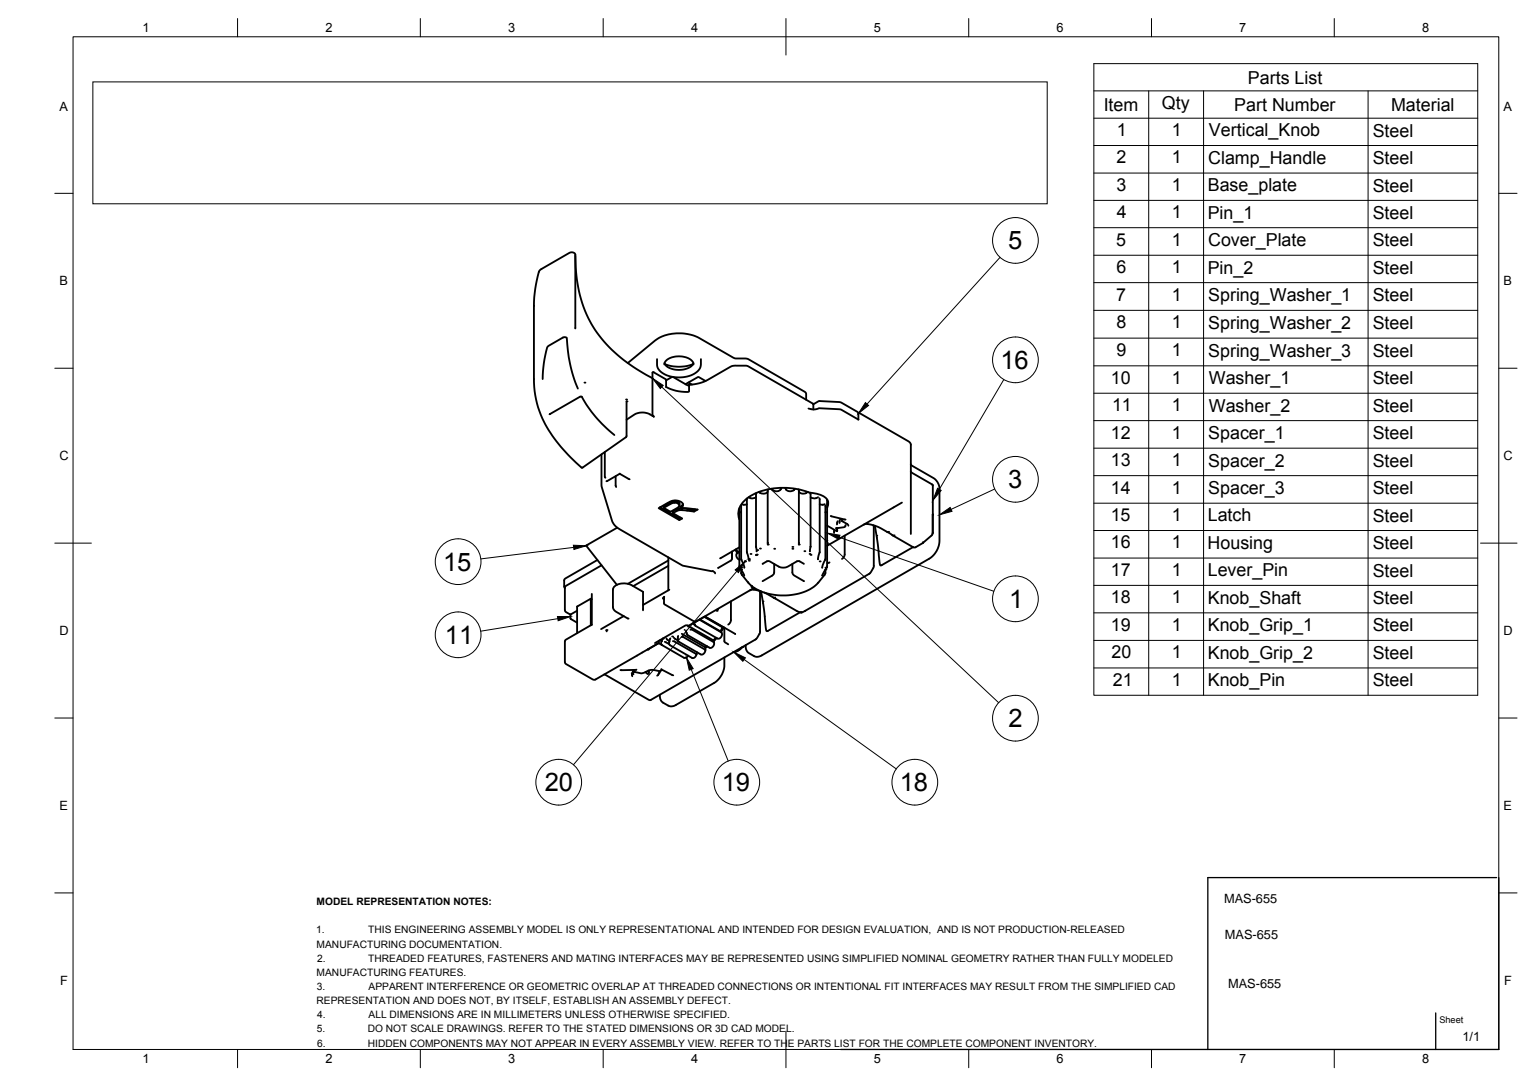
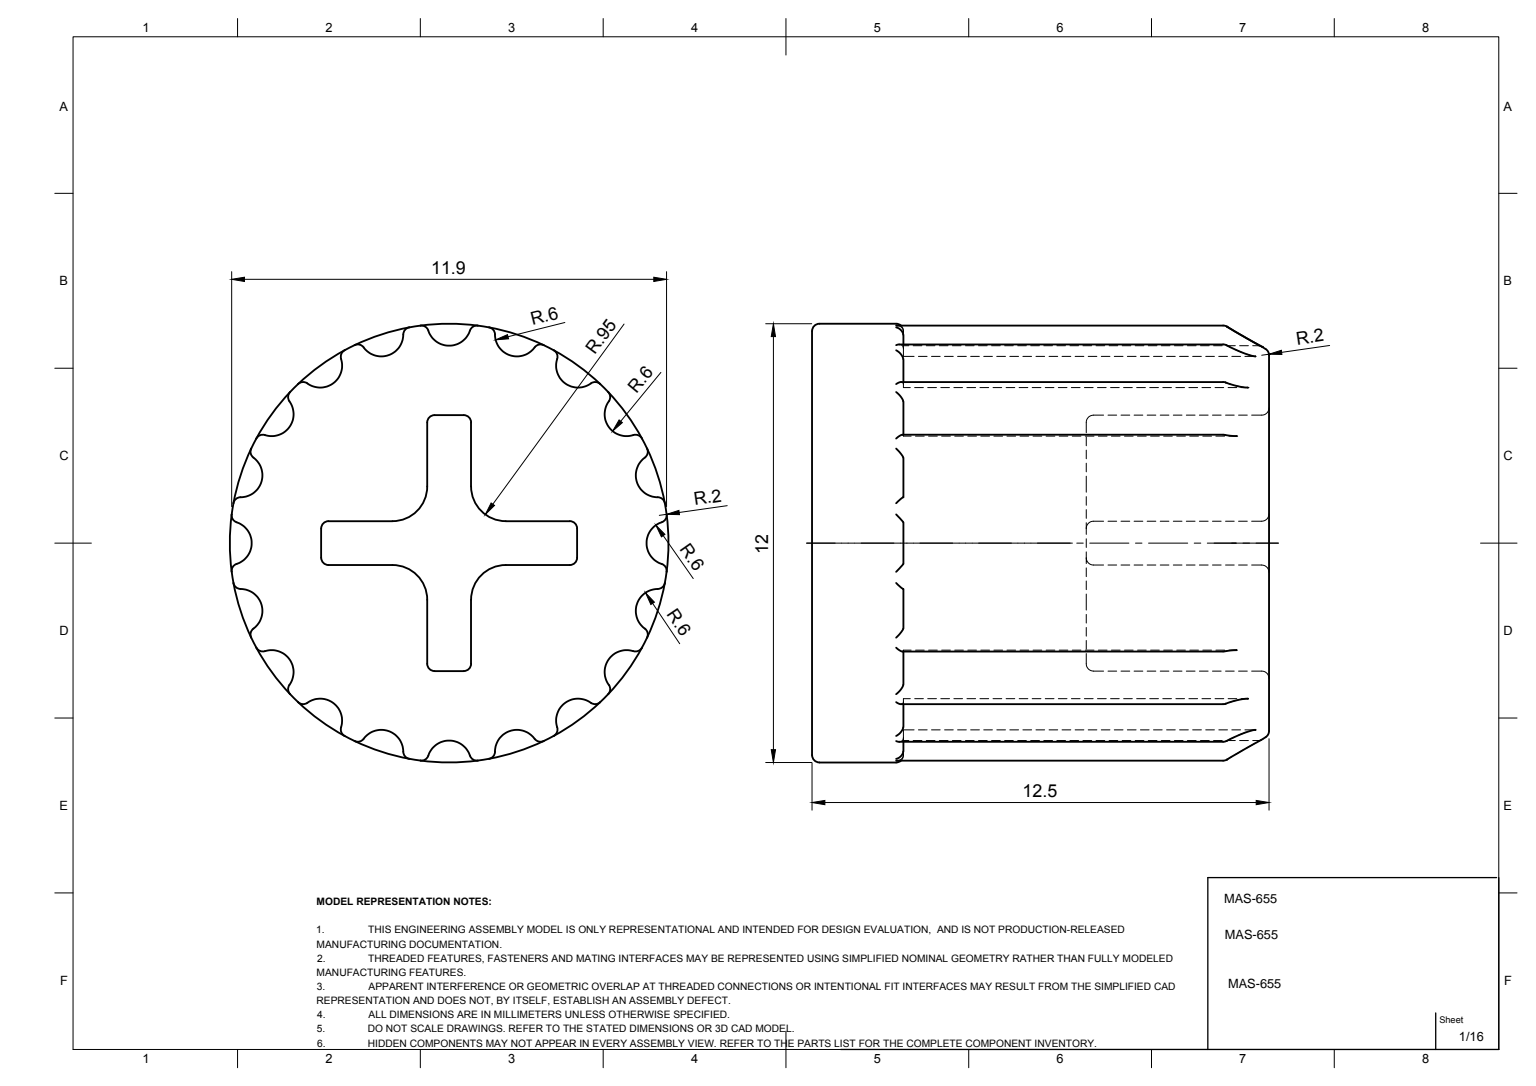
ISO-10303-21;
HEADER;
FILE_DESCRIPTION((''),'2;1');
FILE_NAME('MAS-655','2026-10-09T11:34:15-07:00',(''),(''),'','','');
FILE_SCHEMA (('AUTOMOTIVE_DESIGN { 1 0 10303 214 3 1 1 }'));
ENDSEC;
DATA;
#10 = MECHANICAL_DESIGN_GEOMETRIC_PRESENTATION_REPRESENTATION('',(#628,#629,
#630,#631,#632,#633,#634,#635,#636,#637,#638,#639,#640,#641,#642,#643,#644,
#645,#646,#647,#648),#117170) ;
#11 = ITEM_DEFINED_TRANSFORMATION($,$,#49311,#55076) ;
#12 = ITEM_DEFINED_TRANSFORMATION($,$,#49866,#55077) ;
#13 = ITEM_DEFINED_TRANSFORMATION($,$,#50164,#55078) ;
#14 = ITEM_DEFINED_TRANSFORMATION($,$,#51709,#55079) ;
#15 = ITEM_DEFINED_TRANSFORMATION($,$,#51734,#55080) ;
#16 = ITEM_DEFINED_TRANSFORMATION($,$,#51974,#55081) ;
#17 = ITEM_DEFINED_TRANSFORMATION($,$,#51981,#55082) ;
#18 = ITEM_DEFINED_TRANSFORMATION($,$,#51993,#55083) ;
#19 = ITEM_DEFINED_TRANSFORMATION($,$,#52005,#55084) ;
#20 = ITEM_DEFINED_TRANSFORMATION($,$,#52017,#55085) ;
#21 = ITEM_DEFINED_TRANSFORMATION($,$,#52179,#55086) ;
#22 = ITEM_DEFINED_TRANSFORMATION($,$,#52219,#55087) ;
#23 = ITEM_DEFINED_TRANSFORMATION($,$,#52294,#55088) ;
#24 = ITEM_DEFINED_TRANSFORMATION($,$,#52369,#55089) ;
#25 = ITEM_DEFINED_TRANSFORMATION($,$,#52444,#55090) ;
#26 = ITEM_DEFINED_TRANSFORMATION($,$,#52526,#55091) ;
#27 = ITEM_DEFINED_TRANSFORMATION($,$,#54011,#55092) ;
#28 = ITEM_DEFINED_TRANSFORMATION($,$,#54027,#55093) ;
#29 = ITEM_DEFINED_TRANSFORMATION($,$,#54042,#55094) ;
#30 = ITEM_DEFINED_TRANSFORMATION($,$,#54544,#55095) ;
#31 = ITEM_DEFINED_TRANSFORMATION($,$,#55046,#55096) ;
#32 = (
REPRESENTATION_RELATIONSHIP($,$,#117241,#117240)
REPRESENTATION_RELATIONSHIP_WITH_TRANSFORMATION(#11)
SHAPE_REPRESENTATION_RELATIONSHIP()
) ;
#33 = (
REPRESENTATION_RELATIONSHIP($,$,#117242,#117240)
REPRESENTATION_RELATIONSHIP_WITH_TRANSFORMATION(#12)
SHAPE_REPRESENTATION_RELATIONSHIP()
) ;
#34 = (
REPRESENTATION_RELATIONSHIP($,$,#117243,#117240)
REPRESENTATION_RELATIONSHIP_WITH_TRANSFORMATION(#13)
SHAPE_REPRESENTATION_RELATIONSHIP()
) ;
#35 = (
REPRESENTATION_RELATIONSHIP($,$,#117244,#117240)
REPRESENTATION_RELATIONSHIP_WITH_TRANSFORMATION(#14)
SHAPE_REPRESENTATION_RELATIONSHIP()
) ;
#36 = (
REPRESENTATION_RELATIONSHIP($,$,#117245,#117240)
REPRESENTATION_RELATIONSHIP_WITH_TRANSFORMATION(#15)
SHAPE_REPRESENTATION_RELATIONSHIP()
) ;
#37 = (
REPRESENTATION_RELATIONSHIP($,$,#117246,#117240)
REPRESENTATION_RELATIONSHIP_WITH_TRANSFORMATION(#16)
SHAPE_REPRESENTATION_RELATIONSHIP()
) ;
#38 = (
REPRESENTATION_RELATIONSHIP($,$,#117247,#117240)
REPRESENTATION_RELATIONSHIP_WITH_TRANSFORMATION(#17)
SHAPE_REPRESENTATION_RELATIONSHIP()
) ;
#39 = (
REPRESENTATION_RELATIONSHIP($,$,#117248,#117240)
REPRESENTATION_RELATIONSHIP_WITH_TRANSFORMATION(#18)
SHAPE_REPRESENTATION_RELATIONSHIP()
) ;
#40 = (
REPRESENTATION_RELATIONSHIP($,$,#117249,#117240)
REPRESENTATION_RELATIONSHIP_WITH_TRANSFORMATION(#19)
SHAPE_REPRESENTATION_RELATIONSHIP()
) ;
#41 = (
REPRESENTATION_RELATIONSHIP($,$,#117250,#117240)
REPRESENTATION_RELATIONSHIP_WITH_TRANSFORMATION(#20)
SHAPE_REPRESENTATION_RELATIONSHIP()
) ;
#42 = (
REPRESENTATION_RELATIONSHIP($,$,#117251,#117240)
REPRESENTATION_RELATIONSHIP_WITH_TRANSFORMATION(#21)
SHAPE_REPRESENTATION_RELATIONSHIP()
) ;
#43 = (
REPRESENTATION_RELATIONSHIP($,$,#117252,#117240)
REPRESENTATION_RELATIONSHIP_WITH_TRANSFORMATION(#22)
SHAPE_REPRESENTATION_RELATIONSHIP()
) ;
#44 = (
REPRESENTATION_RELATIONSHIP($,$,#117253,#117240)
REPRESENTATION_RELATIONSHIP_WITH_TRANSFORMATION(#23)
SHAPE_REPRESENTATION_RELATIONSHIP()
) ;
#45 = (
REPRESENTATION_RELATIONSHIP($,$,#117254,#117240)
REPRESENTATION_RELATIONSHIP_WITH_TRANSFORMATION(#24)
SHAPE_REPRESENTATION_RELATIONSHIP()
) ;
#46 = (
REPRESENTATION_RELATIONSHIP($,$,#117255,#117240)
REPRESENTATION_RELATIONSHIP_WITH_TRANSFORMATION(#25)
SHAPE_REPRESENTATION_RELATIONSHIP()
) ;
#47 = (
REPRESENTATION_RELATIONSHIP($,$,#117256,#117240)
REPRESENTATION_RELATIONSHIP_WITH_TRANSFORMATION(#26)
SHAPE_REPRESENTATION_RELATIONSHIP()
) ;
#48 = (
REPRESENTATION_RELATIONSHIP($,$,#117257,#117240)
REPRESENTATION_RELATIONSHIP_WITH_TRANSFORMATION(#27)
SHAPE_REPRESENTATION_RELATIONSHIP()
) ;
#49 = (
REPRESENTATION_RELATIONSHIP($,$,#117258,#117240)
REPRESENTATION_RELATIONSHIP_WITH_TRANSFORMATION(#28)
SHAPE_REPRESENTATION_RELATIONSHIP()
) ;
#50 = (
REPRESENTATION_RELATIONSHIP($,$,#117259,#117240)
REPRESENTATION_RELATIONSHIP_WITH_TRANSFORMATION(#29)
SHAPE_REPRESENTATION_RELATIONSHIP()
) ;
#51 = (
REPRESENTATION_RELATIONSHIP($,$,#117260,#117240)
REPRESENTATION_RELATIONSHIP_WITH_TRANSFORMATION(#30)
SHAPE_REPRESENTATION_RELATIONSHIP()
) ;
#52 = (
REPRESENTATION_RELATIONSHIP($,$,#117261,#117240)
REPRESENTATION_RELATIONSHIP_WITH_TRANSFORMATION(#31)
SHAPE_REPRESENTATION_RELATIONSHIP()
) ;
#53 = CONTEXT_DEPENDENT_SHAPE_REPRESENTATION(#32,#117219) ;
#54 = CONTEXT_DEPENDENT_SHAPE_REPRESENTATION(#33,#117220) ;
#55 = CONTEXT_DEPENDENT_SHAPE_REPRESENTATION(#34,#117221) ;
#56 = CONTEXT_DEPENDENT_SHAPE_REPRESENTATION(#35,#117222) ;
#57 = CONTEXT_DEPENDENT_SHAPE_REPRESENTATION(#36,#117223) ;
#58 = CONTEXT_DEPENDENT_SHAPE_REPRESENTATION(#37,#117224) ;
#59 = CONTEXT_DEPENDENT_SHAPE_REPRESENTATION(#38,#117225) ;
#60 = CONTEXT_DEPENDENT_SHAPE_REPRESENTATION(#39,#117226) ;
#61 = CONTEXT_DEPENDENT_SHAPE_REPRESENTATION(#40,#117227) ;
#62 = CONTEXT_DEPENDENT_SHAPE_REPRESENTATION(#41,#117228) ;
#63 = CONTEXT_DEPENDENT_SHAPE_REPRESENTATION(#42,#117229) ;
#64 = CONTEXT_DEPENDENT_SHAPE_REPRESENTATION(#43,#117230) ;
#65 = CONTEXT_DEPENDENT_SHAPE_REPRESENTATION(#44,#117231) ;
#66 = CONTEXT_DEPENDENT_SHAPE_REPRESENTATION(#45,#117232) ;
#67 = CONTEXT_DEPENDENT_SHAPE_REPRESENTATION(#46,#117233) ;
#68 = CONTEXT_DEPENDENT_SHAPE_REPRESENTATION(#47,#117234) ;
#69 = CONTEXT_DEPENDENT_SHAPE_REPRESENTATION(#48,#117235) ;
#70 = CONTEXT_DEPENDENT_SHAPE_REPRESENTATION(#49,#117236) ;
#71 = CONTEXT_DEPENDENT_SHAPE_REPRESENTATION(#50,#117237) ;
#72 = CONTEXT_DEPENDENT_SHAPE_REPRESENTATION(#51,#117238) ;
#73 = CONTEXT_DEPENDENT_SHAPE_REPRESENTATION(#52,#117239) ;
#74 = NEXT_ASSEMBLY_USAGE_OCCURRENCE('Vertical_Knob:1','Vertical_Knob:1',
'Vertical_Knob:1',#117263,#117264,'Vertical_Knob:1') ;
#75 = NEXT_ASSEMBLY_USAGE_OCCURRENCE('Clamp_Handle:1','Clamp_Handle:1',
'Clamp_Handle:1',#117263,#117265,'Clamp_Handle:1') ;
#76 = NEXT_ASSEMBLY_USAGE_OCCURRENCE('Base_Plate:1','Base_Plate:1',
'Base_Plate:1',#117263,#117266,'Base_Plate:1') ;
#77 = NEXT_ASSEMBLY_USAGE_OCCURRENCE('Pin_1:1','Pin_1:1','Pin_1:1',#117263,
#117267,'Pin_1:1') ;
#78 = NEXT_ASSEMBLY_USAGE_OCCURRENCE('Cover_Plate:1','Cover_Plate:1',
'Cover_Plate:1',#117263,#117268,'Cover_Plate:1') ;
#79 = NEXT_ASSEMBLY_USAGE_OCCURRENCE('Pin_2:1','Pin_2:1','Pin_2:1',#117263,
#117269,'Pin_2:1') ;
#80 = NEXT_ASSEMBLY_USAGE_OCCURRENCE('Spring_Washer_1:1',
'Spring_Washer_1:1','Spring_Washer_1:1',#117263,#117270,
'Spring_Washer_1:1') ;
#81 = NEXT_ASSEMBLY_USAGE_OCCURRENCE('Spring_Washer_2:1',
'Spring_Washer_2:1','Spring_Washer_2:1',#117263,#117271,
'Spring_Washer_2:1') ;
#82 = NEXT_ASSEMBLY_USAGE_OCCURRENCE('Spring_Washer_3:1',
'Spring_Washer_3:1','Spring_Washer_3:1',#117263,#117272,
'Spring_Washer_3:1') ;
#83 = NEXT_ASSEMBLY_USAGE_OCCURRENCE('Washer_1:1','Washer_1:1',
'Washer_1:1',#117263,#117273,'Washer_1:1') ;
#84 = NEXT_ASSEMBLY_USAGE_OCCURRENCE('Washer_2:1','Washer_2:1',
'Washer_2:1',#117263,#117274,'Washer_2:1') ;
#85 = NEXT_ASSEMBLY_USAGE_OCCURRENCE('Spacer_1:1','Spacer_1:1',
'Spacer_1:1',#117263,#117275,'Spacer_1:1') ;
#86 = NEXT_ASSEMBLY_USAGE_OCCURRENCE('Spacer_2:1','Spacer_2:1',
'Spacer_2:1',#117263,#117276,'Spacer_2:1') ;
#87 = NEXT_ASSEMBLY_USAGE_OCCURRENCE('Spacer_3:1','Spacer_3:1',
'Spacer_3:1',#117263,#117277,'Spacer_3:1') ;
#88 = NEXT_ASSEMBLY_USAGE_OCCURRENCE('Latch:1','Latch:1','Latch:1',#117263,
#117278,'Latch:1') ;
#89 = NEXT_ASSEMBLY_USAGE_OCCURRENCE('Housing:1','Housing:1','Housing:1',
#117263,#117279,'Housing:1') ;
#90 = NEXT_ASSEMBLY_USAGE_OCCURRENCE('Lever_Pin:1','Lever_Pin:1',
'Lever_Pin:1',#117263,#117280,'Lever_Pin:1') ;
#91 = NEXT_ASSEMBLY_USAGE_OCCURRENCE('Knob_Shaft:1','Knob_Shaft:1',
'Knob_Shaft:1',#117263,#117281,'Knob_Shaft:1') ;
#92 = NEXT_ASSEMBLY_USAGE_OCCURRENCE('Knob_Grip_1:1','Knob_Grip_1:1',
'Knob_Grip_1:1',#117263,#117282,'Knob_Grip_1:1') ;
#93 = NEXT_ASSEMBLY_USAGE_OCCURRENCE('Knob_Grip_2:1','Knob_Grip_2:1',
'Knob_Grip_2:1',#117263,#117283,'Knob_Grip_2:1') ;
#94 = NEXT_ASSEMBLY_USAGE_OCCURRENCE('Knob_Pin:1','Knob_Pin:1',
'Knob_Pin:1',#117263,#117284,'Knob_Pin:1') ;
#95 = (
BOUNDED_SURFACE()
B_SPLINE_SURFACE(2,2,((#87159,#87160,#87161),(#87162,#87163,#87164),(#87165,
#87166,#87167)),.UNSPECIFIED.,.F.,.F.,.F.)
B_SPLINE_SURFACE_WITH_KNOTS((3,3),(3,3),(2.9656421913598E-12,1.57079632680175),
(-2.44346095279454,-1.57079632680019),.UNSPECIFIED.)
GEOMETRIC_REPRESENTATION_ITEM()
RATIONAL_B_SPLINE_SURFACE(((1.,0.906307787037244,1.),(0.707106781185325,
0.640856382055101,0.707106781185325),(1.,0.906307787037244,1.)))
REPRESENTATION_ITEM('')
SURFACE()
) ;
#96 = (
BOUNDED_SURFACE()
B_SPLINE_SURFACE(2,2,((#87171,#87172,#87173),(#87174,#87175,#87176),(#87177,
#87178,#87179)),.UNSPECIFIED.,.F.,.F.,.F.)
B_SPLINE_SURFACE_WITH_KNOTS((3,3),(3,3),(-1.5707963267996,-4.58626074717158E-12),
(-2.44346095281538,-1.57079632678052),.UNSPECIFIED.)
GEOMETRIC_REPRESENTATION_ITEM()
RATIONAL_B_SPLINE_SURFACE(((1.,0.906307787028686,1.),(0.707106781186676,
0.640856382050274,0.707106781186676),(1.,0.906307787028686,1.)))
REPRESENTATION_ITEM('')
SURFACE()
) ;
#97 = (
BOUNDED_SURFACE()
B_SPLINE_SURFACE(2,2,((#90419,#90420,#90421),(#90422,#90423,#90424),(#90425,
#90426,#90427)),.UNSPECIFIED.,.F.,.F.,.F.)
B_SPLINE_SURFACE_WITH_KNOTS((3,3),(3,3),(-1.57079632679569,0.),(-3.14159265358917,
-1.57079632679587),.UNSPECIFIED.)
GEOMETRIC_REPRESENTATION_ITEM()
RATIONAL_B_SPLINE_SURFACE(((1.,0.707106781187113,1.),(0.707106781186163,
0.500000000000127,0.707106781186163),(1.,0.707106781187113,1.)))
REPRESENTATION_ITEM('')
SURFACE()
) ;
#98 = (
BOUNDED_SURFACE()
B_SPLINE_SURFACE(2,2,((#90597,#90598,#90599),(#90600,#90601,#90602),(#90603,
#90604,#90605)),.UNSPECIFIED.,.F.,.F.,.F.)
B_SPLINE_SURFACE_WITH_KNOTS((3,3),(3,3),(-1.570796326795,2.27222014866972E-13),
(-1.57079632679441,-7.1054273575954E-13),.UNSPECIFIED.)
GEOMETRIC_REPRESENTATION_ITEM()
RATIONAL_B_SPLINE_SURFACE(((1.,0.707106781186971,1.),(0.70710678118641,
0.500000000000203,0.70710678118641),(1.,0.707106781186971,1.)))
REPRESENTATION_ITEM('')
SURFACE()
) ;
#99 = (
BOUNDED_SURFACE()
B_SPLINE_SURFACE(2,2,((#92757,#92758,#92759),(#92760,#92761,#92762),(#92763,
#92764,#92765)),.UNSPECIFIED.,.F.,.F.,.F.)
B_SPLINE_SURFACE_WITH_KNOTS((3,3),(3,3),(-1.57079632680452,-1.25635394189736E-12),
(-2.44346095281043,-1.64859272029811),.UNSPECIFIED.)
GEOMETRIC_REPRESENTATION_ITEM()
RATIONAL_B_SPLINE_SURFACE(((1.,0.922057163080232,1.),(0.707106781183326,
0.651992872652692,0.707106781183326),(1.,0.922057163080232,1.)))
REPRESENTATION_ITEM('')
SURFACE()
) ;
#100 = (
BOUNDED_SURFACE()
B_SPLINE_SURFACE(2,2,((#92794,#92795,#92796,#92797,#92798),(#92799,#92800,
#92801,#92802,#92803),(#92804,#92805,#92806,#92807,#92808)),
 .UNSPECIFIED.,.F.,.F.,.F.)
B_SPLINE_SURFACE_WITH_KNOTS((3,3),(3,2,3),(-3.14159265358979,-1.57079632679397),
(-0.795304873266846,0.,0.795304873266846),.UNSPECIFIED.)
GEOMETRIC_REPRESENTATION_ITEM()
RATIONAL_B_SPLINE_SURFACE(((1.,0.921972639390714,1.,0.921972639390714,1.),
(0.707106781186466,0.651933105381558,0.707106781186466,0.651933105381558,
0.707106781186466),(1.,0.921972639390714,1.,0.921972639390714,1.)))
REPRESENTATION_ITEM('')
SURFACE()
) ;
#101 = (
BOUNDED_SURFACE()
B_SPLINE_SURFACE(2,2,((#97993,#97994,#97995),(#97996,#97997,#97998),(#97999,
#98000,#98001)),.UNSPECIFIED.,.F.,.F.,.F.)
B_SPLINE_SURFACE_WITH_KNOTS((3,3),(3,3),(-1.57079632673965,5.57007752630405E-11),
(4.19220214067588E-12,0.187132086721036),.UNSPECIFIED.)
GEOMETRIC_REPRESENTATION_ITEM()
RATIONAL_B_SPLINE_SURFACE(((1.,0.99562589029583,1.),(0.70710678118639,0.704013818552918,
0.70710678118639),(1.,0.99562589029583,1.)))
REPRESENTATION_ITEM('')
SURFACE()
) ;
#102 = (
BOUNDED_SURFACE()
B_SPLINE_SURFACE(2,2,((#98044,#98045,#98046),(#98047,#98048,#98049),(#98050,
#98051,#98052)),.UNSPECIFIED.,.F.,.F.,.F.)
B_SPLINE_SURFACE_WITH_KNOTS((3,3),(3,3),(-1.57079632677152,2.35301000695734E-11),
(3.55271367856584E-13,0.187132086725463),.UNSPECIFIED.)
GEOMETRIC_REPRESENTATION_ITEM()
RATIONAL_B_SPLINE_SURFACE(((1.,0.995625890295444,1.),(0.707106781186499,
0.704013818552754,0.707106781186499),(1.,0.995625890295444,1.)))
REPRESENTATION_ITEM('')
SURFACE()
) ;
#103 = ELLIPSE('',#49876,30.621208525322,25.4809915026997) ;
#104 = ELLIPSE('',#49877,31.5888201684124,25.5766704752798) ;
#105 = ELLIPSE('',#49879,31.5675675201038,25.5487669653367) ;
#106 = ELLIPSE('',#49885,0.87450775194086,0.752188335062039) ;
#107 = ELLIPSE('',#49887,0.979448682193676,0.842450935309832) ;
#108 = ELLIPSE('',#49892,0.26650610321202,0.226790790063564) ;
#109 = ELLIPSE('',#49893,0.373108544497893,0.31750710609267) ;
#110 = ELLIPSE('',#49894,0.874507751946099,0.752188335070988) ;
#111 = ELLIPSE('',#49899,104.965032228634,60.1468662540866) ;
#112 = ELLIPSE('',#49900,153.912764893179,72.1332927979209) ;
#113 = ELLIPSE('',#49901,107.003369056671,53.394874735838) ;
#114 = ELLIPSE('',#49903,0.944305135734821,0.812323833839972) ;
#115 = ELLIPSE('',#49904,31.6658812357246,25.6468027651175) ;
#116 = ELLIPSE('',#49905,33.3290082029849,26.9991094930833) ;
#117 = ELLIPSE('',#49908,0.373067574458494,0.317497630618124) ;
#118 = ELLIPSE('',#49909,87.539485717233,47.1288613191233) ;
#119 = ELLIPSE('',#49910,28.9052201415572,24.2407648329214) ;
#120 = ELLIPSE('',#49911,33.8387106683363,27.6581069858551) ;
#121 = ELLIPSE('',#49912,32.4705877660237,26.389680540433) ;
#122 = ELLIPSE('',#49913,119.941732153885,63.5628286542732) ;
#123 = ELLIPSE('',#49920,0.266476838896091,0.226784021864154) ;
#124 = ELLIPSE('',#49928,0.266476838896308,0.226784021864664) ;
#125 = ELLIPSE('',#49936,0.120304939822837,0.120009764468753) ;
#126 = ELLIPSE('',#49937,0.120304939823071,0.120009764469075) ;
#127 = ELLIPSE('',#49944,32.9935493519598,26.6864661964081) ;
#128 = ELLIPSE('',#49946,31.5675675494409,25.5487669922883) ;
#129 = ELLIPSE('',#49953,1.04922792860613,0.902582037621626) ;
#130 = ELLIPSE('',#49958,106.937521398911,53.4980353026644) ;
#131 = ELLIPSE('',#49960,171.400384709509,76.7143149375333) ;
#132 = ELLIPSE('',#49962,112.686599872101,62.8742365573781) ;
#133 = ELLIPSE('',#49966,0.124835932303391,0.12) ;
#134 = ELLIPSE('',#49972,106.937521398833,53.4980353026422) ;
#135 = ELLIPSE('',#49973,26.7718235298462,13.2260955102084) ;
#136 = ELLIPSE('',#49974,180.168079206207,78.5747283099703) ;
#137 = ELLIPSE('',#49975,26.5629631306412,13.0416514063261) ;
#138 = ELLIPSE('',#49997,34.0017819463872,27.818723289359) ;
#139 = ELLIPSE('',#49999,33.6804890520093,27.5067870175508) ;
#140 = ELLIPSE('',#50000,32.5228044782183,26.4447063399665) ;
#141 = ELLIPSE('',#50001,32.6276108313175,26.5480371159551) ;
#142 = ELLIPSE('',#50004,33.6121963166486,28.1464718973248) ;
#143 = ELLIPSE('',#50007,34.1688903664586,27.9750858992831) ;
#144 = ELLIPSE('',#50008,32.5764457907704,26.4940988115262) ;
#145 = ELLIPSE('',#50009,121.638689200547,63.8567625922291) ;
#146 = ELLIPSE('',#50011,133.068922302088,67.3695526852953) ;
#147 = ELLIPSE('',#50017,110.759696058364,60.5332237301847) ;
#148 = ELLIPSE('',#50022,26.0480895445502,18.516397692244) ;
#149 = ELLIPSE('',#50026,112.783598469003,61.0762817351653) ;
#150 = ELLIPSE('',#50031,89.0710500040395,47.3896547267835) ;
#151 = ELLIPSE('',#50033,0.159886103339097,0.136070413122481) ;
#152 = ELLIPSE('',#50037,29.4480227809696,24.8646228837011) ;
#153 = ELLIPSE('',#50046,0.76956682169275,0.66192573483117) ;
#154 = ELLIPSE('',#50052,0.159903661928928,0.13607447404265) ;
#155 = ELLIPSE('',#50053,0.266506103215596,0.226790790070262) ;
#156 = ELLIPSE('',#50061,0.129795981335339,0.124487164214877) ;
#157 = ELLIPSE('',#50071,0.769566821716286,0.661925734873078) ;
#158 = ELLIPSE('',#50073,0.874507751919452,0.75218833502354) ;
#159 = ELLIPSE('',#50077,0.210854308776711,0.181549488975955) ;
#160 = ELLIPSE('',#50081,0.874507751937288,0.752188335055131) ;
#161 = ELLIPSE('',#50083,0.97944868220323,0.842450935327434) ;
#162 = ELLIPSE('',#50090,160.893031132199,73.683653149258) ;
#163 = ELLIPSE('',#50091,0.944305135733765,0.812323833838177) ;
#164 = ELLIPSE('',#50093,107.003369056713,53.3948747358502) ;
#165 = ELLIPSE('',#50103,0.129786651823771,0.12448808595579) ;
#166 = ELLIPSE('',#50123,90.0915709695949,47.7382908134221) ;
#167 = ELLIPSE('',#50124,89.6335580246405,47.7081104258241) ;
#168 = ELLIPSE('',#50133,33.329008202931,26.9991094930345) ;
#169 = ELLIPSE('',#50134,32.993549352048,26.6864661964888) ;
#170 = ELLIPSE('',#50146,1.04922792859238,0.902582037596269) ;
#171 = ELLIPSE('',#50166,0.169705627484765,0.12) ;
#172 = ELLIPSE('',#50168,0.169705627484778,0.12) ;
#173 = ELLIPSE('',#50175,0.249814202663062,0.12) ;
#174 = ELLIPSE('',#50177,0.136899613896297,0.12) ;
#175 = ELLIPSE('',#50182,0.169705627484765,0.12) ;
#176 = ELLIPSE('',#50184,0.169705627484778,0.12) ;
#177 = ELLIPSE('',#50186,0.169705627484765,0.12) ;
#178 = ELLIPSE('',#50188,0.169705627484778,0.12) ;
#179 = ELLIPSE('',#50195,0.169705627484765,0.12) ;
#180 = ELLIPSE('',#50197,0.169705627484765,0.12) ;
#181 = ELLIPSE('',#50201,0.169705627484779,0.12) ;
#182 = ELLIPSE('',#50202,0.31357511157033,0.12) ;
#183 = ELLIPSE('',#50204,0.313575111570327,0.12) ;
#184 = ELLIPSE('',#50210,0.169705627484784,0.12) ;
#185 = ELLIPSE('',#50211,0.169705627484784,0.12) ;
#186 = ELLIPSE('',#50213,0.169705627484765,0.12) ;
#187 = ELLIPSE('',#50215,0.169705627484753,0.12) ;
#188 = ELLIPSE('',#50221,0.313575111570327,0.12) ;
#189 = ELLIPSE('',#50222,0.169705627484779,0.12) ;
#190 = ELLIPSE('',#50224,0.31357511157033,0.12) ;
#191 = ELLIPSE('',#50230,0.249814202663065,0.12) ;
#192 = ELLIPSE('',#50233,0.136899613896321,0.12) ;
#193 = ELLIPSE('',#50235,0.169705627484778,0.12) ;
#194 = ELLIPSE('',#50236,0.169705627484778,0.12) ;
#195 = ELLIPSE('',#50238,0.169705627484765,0.12) ;
#196 = ELLIPSE('',#50240,0.169705627484778,0.12) ;
#197 = ELLIPSE('',#50250,1.73726470137952,1.7) ;
#198 = ELLIPSE('',#50251,1.73726470137952,1.7) ;
#199 = ELLIPSE('',#50254,1.73726470137952,1.7) ;
#200 = ELLIPSE('',#50255,1.73726470137952,1.7) ;
#201 = ELLIPSE('',#50326,0.313575111570335,0.12) ;
#202 = ELLIPSE('',#50327,0.169705627484762,0.12) ;
#203 = ELLIPSE('',#50329,0.313575111570314,0.12) ;
#204 = ELLIPSE('',#50333,0.169705627484778,0.12) ;
#205 = ELLIPSE('',#50334,0.169705627484778,0.12) ;
#206 = ELLIPSE('',#50336,0.169705627484765,0.12) ;
#207 = ELLIPSE('',#50338,0.169705627484778,0.12) ;
#208 = ELLIPSE('',#50342,0.169705627484779,0.12) ;
#209 = ELLIPSE('',#50343,0.313575111570343,0.12) ;
#210 = ELLIPSE('',#50345,0.313575111570327,0.12) ;
#211 = ELLIPSE('',#50371,1.73726470137952,1.7) ;
#212 = ELLIPSE('',#50372,1.73726470137952,1.7) ;
#213 = ELLIPSE('',#50373,1.73726470137952,1.7) ;
#214 = ELLIPSE('',#50374,1.73726470137952,1.7) ;
#215 = ELLIPSE('',#50520,4.854121959737,1.) ;
#216 = ELLIPSE('',#50521,4.854121959737,1.) ;
#217 = ELLIPSE('',#50535,4.854121959737,1.) ;
#218 = ELLIPSE('',#50536,4.854121959737,1.) ;
#219 = ELLIPSE('',#50561,8.2520073315529,1.7) ;
#220 = ELLIPSE('',#50562,8.2520073315529,1.7) ;
#221 = ELLIPSE('',#50563,8.2520073315529,1.7) ;
#222 = ELLIPSE('',#50564,8.2520073315529,1.7) ;
#223 = ELLIPSE('',#50565,0.707106781186556,0.5) ;
#224 = ELLIPSE('',#50571,0.509901951359303,0.0999999999999979) ;
#225 = ELLIPSE('',#50645,0.223606797749974,0.0999999999999979) ;
#226 = ELLIPSE('',#50646,0.223606797749982,0.0999999999999979) ;
#227 = ELLIPSE('',#50648,0.141421356237297,0.1) ;
#228 = ELLIPSE('',#50651,0.223606797749982,0.100000000000002) ;
#229 = ELLIPSE('',#50652,0.223606797749974,0.0999999999999979) ;
#230 = ELLIPSE('',#50660,0.1414213562373,0.1) ;
#231 = ELLIPSE('',#50779,0.223606797749974,0.0999999999999934) ;
#232 = ELLIPSE('',#50780,0.223606797749982,0.0999999999999979) ;
#233 = ELLIPSE('',#50783,0.223606797749982,0.0999999999999979) ;
#234 = ELLIPSE('',#50784,0.223606797749974,0.100000000000002) ;
#235 = ELLIPSE('',#51163,1.38924439894499,1.2) ;
#236 = ELLIPSE('',#51164,1.38924439894499,1.2) ;
#237 = ELLIPSE('',#51210,0.141421356237297,0.1) ;
#238 = ELLIPSE('',#51222,0.141421356237292,0.1) ;
#239 = ELLIPSE('',#51349,0.141421356237297,0.1) ;
#240 = ELLIPSE('',#51361,0.141421356237292,0.1) ;
#241 = ELLIPSE('',#51463,0.141421356237297,0.1) ;
#242 = ELLIPSE('',#51475,0.141421356237292,0.1) ;
#243 = ELLIPSE('',#51481,0.141421356237297,0.1) ;
#244 = ELLIPSE('',#51631,1.38924439894499,1.2) ;
#245 = ELLIPSE('',#51632,1.38924439894498,1.2) ;
#246 = ELLIPSE('',#51634,1.38924439894498,1.2) ;
#247 = ELLIPSE('',#51635,1.38924439894498,1.2) ;
#248 = ELLIPSE('',#51636,1.38924439894499,1.2) ;
#249 = ELLIPSE('',#51637,1.38924439894499,1.2) ;
#250 = ELLIPSE('',#51639,1.38924439894499,1.2) ;
#251 = ELLIPSE('',#51640,1.38924439894499,1.2) ;
#252 = ELLIPSE('',#51641,1.38924439894498,1.2) ;
#253 = ELLIPSE('',#51642,1.38924439894498,1.2) ;
#254 = ELLIPSE('',#51644,1.38924439894498,1.20000000000001) ;
#255 = ELLIPSE('',#51645,1.38924439894498,1.20000000000001) ;
#256 = ELLIPSE('',#51650,0.614889130379839,0.499999999999998) ;
#257 = ELLIPSE('',#51654,0.614889130379839,0.499999999999998) ;
#258 = ELLIPSE('',#51660,0.614889130379839,0.499999999999998) ;
#259 = ELLIPSE('',#51664,0.614889130379841,0.499999999999998) ;
#260 = ELLIPSE('',#51673,4.7762432936358,0.499999999999998) ;
#261 = ELLIPSE('',#51675,4.7762432936358,0.499999999999998) ;
#262 = ELLIPSE('',#51683,4.7762432936358,0.499999999999998) ;
#263 = ELLIPSE('',#51706,4.7762432936358,0.499999999999998) ;
#264 = ELLIPSE('',#51711,0.141421356237302,0.1) ;
#265 = ELLIPSE('',#51712,0.108239220029239,0.1) ;
#266 = ELLIPSE('',#51714,0.108239220029249,0.1) ;
#267 = ELLIPSE('',#51716,0.141421356237297,0.1) ;
#268 = ELLIPSE('',#51722,0.141421356237317,0.1) ;
#269 = ELLIPSE('',#51771,0.141421356237322,0.1) ;
#270 = ELLIPSE('',#51774,0.141421356237322,0.1) ;
#271 = ELLIPSE('',#51814,0.31622776601682,0.0999999999999979) ;
#272 = ELLIPSE('',#51815,0.31622776601682,0.0999999999999979) ;
#273 = ELLIPSE('',#51816,0.316227766016848,0.0999999999999979) ;
#274 = ELLIPSE('',#51817,0.316227766016848,0.0999999999999979) ;
#275 = ELLIPSE('',#51820,0.316227766016848,0.0999999999999979) ;
#276 = ELLIPSE('',#51821,0.316227766016848,0.0999999999999979) ;
#277 = ELLIPSE('',#51822,0.316227766016837,0.0999999999999979) ;
#278 = ELLIPSE('',#51823,0.316227766016837,0.0999999999999979) ;
#279 = ELLIPSE('',#51826,0.100574612243464,0.1) ;
#280 = ELLIPSE('',#51856,0.102331928648948,0.1) ;
#281 = ELLIPSE('',#51857,0.10057461224346,0.1) ;
#282 = ELLIPSE('',#51862,0.102331928648948,0.1) ;
#283 = ELLIPSE('',#52024,0.281780056072118,0.249999999999999) ;
#284 = ELLIPSE('',#52025,0.281780056072094,0.249999999999999) ;
#285 = ELLIPSE('',#52032,0.446542271235336,0.249999999999999) ;
#286 = ELLIPSE('',#52033,0.446542271235336,0.249999999999999) ;
#287 = ELLIPSE('',#52034,0.446542271235316,0.249999999999999) ;
#288 = ELLIPSE('',#52035,0.446542271235316,0.249999999999999) ;
#289 = ELLIPSE('',#52043,0.281780056072103,0.249999999999999) ;
#290 = ELLIPSE('',#52044,0.281780056072118,0.249999999999999) ;
#291 = ELLIPSE('',#52053,0.281780056072118,0.249999999999999) ;
#292 = ELLIPSE('',#52054,0.281780056072094,0.249999999999999) ;
#293 = ELLIPSE('',#52061,0.446542271235316,0.249999999999999) ;
#294 = ELLIPSE('',#52062,0.446542271235316,0.249999999999999) ;
#295 = ELLIPSE('',#52063,0.446542271235321,0.249999999999999) ;
#296 = ELLIPSE('',#52064,0.446542271235321,0.249999999999999) ;
#297 = ELLIPSE('',#52073,0.281780056072103,0.249999999999999) ;
#298 = ELLIPSE('',#52074,0.281780056072118,0.249999999999999) ;
#299 = ELLIPSE('',#52082,0.281780056072103,0.249999999999999) ;
#300 = ELLIPSE('',#52083,0.281780056072118,0.249999999999999) ;
#301 = ELLIPSE('',#52091,0.446542271235316,0.249999999999999) ;
#302 = ELLIPSE('',#52092,0.446542271235316,0.249999999999999) ;
#303 = ELLIPSE('',#52093,0.446542271235321,0.249999999999999) ;
#304 = ELLIPSE('',#52094,0.446542271235321,0.249999999999999) ;
#305 = ELLIPSE('',#52102,0.281780056072118,0.249999999999999) ;
#306 = ELLIPSE('',#52103,0.281780056072094,0.249999999999999) ;
#307 = ELLIPSE('',#52112,0.281780056072103,0.249999999999999) ;
#308 = ELLIPSE('',#52113,0.281780056072118,0.249999999999999) ;
#309 = ELLIPSE('',#52120,0.446542271235336,0.249999999999999) ;
#310 = ELLIPSE('',#52121,0.446542271235336,0.249999999999999) ;
#311 = ELLIPSE('',#52122,0.446542271235316,0.249999999999999) ;
#312 = ELLIPSE('',#52123,0.446542271235316,0.249999999999999) ;
#313 = ELLIPSE('',#52132,0.281780056072118,0.249999999999999) ;
#314 = ELLIPSE('',#52133,0.281780056072094,0.249999999999999) ;
#315 = ELLIPSE('',#52193,0.14142135623731,0.1) ;
#316 = ELLIPSE('',#52209,0.141421356237297,0.1) ;
#317 = ELLIPSE('',#52230,0.141421356237297,0.1) ;
#318 = ELLIPSE('',#52231,0.141421356237322,0.1) ;
#319 = ELLIPSE('',#52233,0.141421356237322,0.1) ;
#320 = ELLIPSE('',#52235,0.141421356237297,0.1) ;
#321 = ELLIPSE('',#52237,0.141421356237322,0.1) ;
#322 = ELLIPSE('',#52239,0.141421356237297,0.1) ;
#323 = ELLIPSE('',#52241,0.141421356237297,0.1) ;
#324 = ELLIPSE('',#52242,0.141421356237297,0.1) ;
#325 = ELLIPSE('',#52244,0.141421356237322,0.1) ;
#326 = ELLIPSE('',#52247,0.141421356237297,0.1) ;
#327 = ELLIPSE('',#52249,0.141421356237322,0.1) ;
#328 = ELLIPSE('',#52251,0.141421356237297,0.1) ;
#329 = ELLIPSE('',#52262,0.141421356237272,0.1) ;
#330 = ELLIPSE('',#52263,0.141421356237347,0.1) ;
#331 = ELLIPSE('',#52265,0.141421356237347,0.1) ;
#332 = ELLIPSE('',#52267,0.141421356237272,0.1) ;
#333 = ELLIPSE('',#52269,0.141421356237297,0.1) ;
#334 = ELLIPSE('',#52271,0.141421356237322,0.1) ;
#335 = ELLIPSE('',#52273,0.141421356237347,0.1) ;
#336 = ELLIPSE('',#52275,0.141421356237272,0.1) ;
#337 = ELLIPSE('',#52277,0.141421356237347,0.1) ;
#338 = ELLIPSE('',#52279,0.141421356237272,0.1) ;
#339 = ELLIPSE('',#52281,0.141421356237297,0.1) ;
#340 = ELLIPSE('',#52283,0.141421356237322,0.1) ;
#341 = ELLIPSE('',#52296,0.141421356237297,0.1) ;
#342 = ELLIPSE('',#52297,0.141421356237322,0.1) ;
#343 = ELLIPSE('',#52299,0.141421356237322,0.1) ;
#344 = ELLIPSE('',#52301,0.141421356237297,0.1) ;
#345 = ELLIPSE('',#52303,0.141421356237322,0.1) ;
#346 = ELLIPSE('',#52305,0.141421356237297,0.1) ;
#347 = ELLIPSE('',#52307,0.141421356237322,0.1) ;
#348 = ELLIPSE('',#52309,0.141421356237297,0.1) ;
#349 = ELLIPSE('',#52311,0.141421356237322,0.1) ;
#350 = ELLIPSE('',#52313,0.141421356237297,0.1) ;
#351 = ELLIPSE('',#52315,0.141421356237322,0.1) ;
#352 = ELLIPSE('',#52317,0.141421356237297,0.1) ;
#353 = ELLIPSE('',#52336,0.141421356237297,0.1) ;
#354 = ELLIPSE('',#52337,0.141421356237322,0.1) ;
#355 = ELLIPSE('',#52339,0.141421356237322,0.1) ;
#356 = ELLIPSE('',#52341,0.141421356237297,0.1) ;
#357 = ELLIPSE('',#52343,0.141421356237322,0.1) ;
#358 = ELLIPSE('',#52345,0.141421356237297,0.1) ;
#359 = ELLIPSE('',#52347,0.141421356237297,0.1) ;
#360 = ELLIPSE('',#52348,0.141421356237297,0.1) ;
#361 = ELLIPSE('',#52350,0.141421356237322,0.1) ;
#362 = ELLIPSE('',#52353,0.141421356237297,0.1) ;
#363 = ELLIPSE('',#52355,0.141421356237322,0.1) ;
#364 = ELLIPSE('',#52357,0.141421356237297,0.1) ;
#365 = ELLIPSE('',#52371,0.141421356237294,0.1) ;
#366 = ELLIPSE('',#52372,0.141421356237322,0.1) ;
#367 = ELLIPSE('',#52374,0.141421356237325,0.1) ;
#368 = ELLIPSE('',#52376,0.141421356237297,0.1) ;
#369 = ELLIPSE('',#52378,0.141421356237322,0.1) ;
#370 = ELLIPSE('',#52380,0.141421356237297,0.1) ;
#371 = ELLIPSE('',#52382,0.141421356237322,0.1) ;
#372 = ELLIPSE('',#52384,0.141421356237294,0.1) ;
#373 = ELLIPSE('',#52386,0.141421356237325,0.1) ;
#374 = ELLIPSE('',#52388,0.141421356237297,0.1) ;
#375 = ELLIPSE('',#52390,0.141421356237322,0.1) ;
#376 = ELLIPSE('',#52392,0.141421356237297,0.1) ;
#377 = ELLIPSE('',#52411,0.141421356237297,0.1) ;
#378 = ELLIPSE('',#52412,0.141421356237322,0.1) ;
#379 = ELLIPSE('',#52414,0.141421356237322,0.1) ;
#380 = ELLIPSE('',#52416,0.141421356237297,0.1) ;
#381 = ELLIPSE('',#52418,0.141421356237322,0.1) ;
#382 = ELLIPSE('',#52420,0.141421356237297,0.1) ;
#383 = ELLIPSE('',#52422,0.141421356237297,0.1) ;
#384 = ELLIPSE('',#52423,0.141421356237297,0.1) ;
#385 = ELLIPSE('',#52425,0.141421356237322,0.1) ;
#386 = ELLIPSE('',#52428,0.141421356237297,0.1) ;
#387 = ELLIPSE('',#52430,0.141421356237322,0.1) ;
#388 = ELLIPSE('',#52432,0.141421356237297,0.1) ;
#389 = ELLIPSE('',#52464,0.170018381359192,0.0999999999999989) ;
#390 = ELLIPSE('',#52466,0.146308748884013,0.0499999999999989) ;
#391 = ELLIPSE('',#52481,0.170018381359207,0.100000000000008) ;
#392 = ELLIPSE('',#52483,0.146308748884017,0.0499999999999989) ;
#393 = ELLIPSE('',#52506,0.0707106781186453,0.05) ;
#394 = ELLIPSE('',#52515,0.0964689069078737,0.05) ;
#395 = ELLIPSE('',#52555,0.105759245252314,0.090533850109107) ;
#396 = ELLIPSE('',#52556,0.105759245244956,0.0905338500956946) ;
#397 = ELLIPSE('',#52573,0.634821045649877,0.44) ;
#398 = ELLIPSE('',#52575,0.499397396869427,0.2) ;
#399 = ELLIPSE('',#52590,0.335751501918208,0.111374721424487) ;
#400 = ELLIPSE('',#52593,0.784766199683495,0.4) ;
#401 = ELLIPSE('',#52594,24.8257930386904,0.4) ;
#402 = ELLIPSE('',#52595,0.424264068711929,0.3) ;
#403 = ELLIPSE('',#52596,6.4346717087976,4.55) ;
#404 = ELLIPSE('',#52598,0.354400902933385,0.100000000000016) ;
#405 = ELLIPSE('',#52599,0.354400902933385,0.100000000000016) ;
#406 = ELLIPSE('',#52600,0.354400902933389,0.100000000000016) ;
#407 = ELLIPSE('',#52601,0.354400902933389,0.100000000000016) ;
#408 = ELLIPSE('',#52605,0.76367532368147,0.54) ;
#409 = ELLIPSE('',#52606,0.617737808459213,0.299999999999998) ;
#410 = ELLIPSE('',#52614,0.354400902933389,0.100000000000016) ;
#411 = ELLIPSE('',#52615,0.354400902933389,0.100000000000016) ;
#412 = ELLIPSE('',#52616,0.354400902933385,0.0999999999999801) ;
#413 = ELLIPSE('',#52617,0.354400902933385,0.0999999999999801) ;
#414 = ELLIPSE('',#52621,0.617737808459213,0.300000000000002) ;
#415 = ELLIPSE('',#52622,0.76367532368147,0.54) ;
#416 = ELLIPSE('',#52628,0.141421356237298,0.1) ;
#417 = ELLIPSE('',#52631,0.277848879788995,0.239999999999938) ;
#418 = ELLIPSE('',#52632,0.277848879788997,0.240000000000009) ;
#419 = ELLIPSE('',#52639,0.141421356237298,0.1) ;
#420 = ELLIPSE('',#52640,0.141421356237298,0.1) ;
#421 = ELLIPSE('',#52647,0.339411254969547,0.24) ;
#422 = ELLIPSE('',#52650,0.243578652595007,0.24) ;
#423 = ELLIPSE('',#52652,0.0577110041499885,0.04) ;
#424 = ELLIPSE('',#52655,0.577110041499878,0.399999999999996) ;
#425 = ELLIPSE('',#52668,0.424264068711929,0.3) ;
#426 = ELLIPSE('',#52700,0.344580851516853,0.222253203953467) ;
#427 = ELLIPSE('',#52708,0.141421356237297,0.1) ;
#428 = ELLIPSE('',#52747,0.141421356237322,0.1) ;
#429 = ELLIPSE('',#52767,1.13357840487546,0.749999999999993) ;
#430 = ELLIPSE('',#52768,1.20208152801713,0.85) ;
#431 = ELLIPSE('',#52771,0.223606797749978,0.100000000000016) ;
#432 = ELLIPSE('',#52772,0.282842712474619,0.2) ;
#433 = ELLIPSE('',#52774,0.10069443430648,0.100017256319563) ;
#434 = ELLIPSE('',#52805,0.282842712474618,0.2) ;
#435 = ELLIPSE('',#52806,0.223606797749975,0.100000000000016) ;
#436 = ELLIPSE('',#52810,0.70710678118655,0.5) ;
#437 = ELLIPSE('',#52811,0.640312423743287,0.399999999999992) ;
#438 = ELLIPSE('',#52813,0.846312901686476,0.400595643005874) ;
#439 = ELLIPSE('',#52814,0.862858514657635,0.518233232113999) ;
#440 = ELLIPSE('',#52815,0.640312423743287,0.399999999999992) ;
#441 = ELLIPSE('',#52816,0.70710678118655,0.5) ;
#442 = ELLIPSE('',#52818,0.412310562561758,0.4) ;
#443 = ELLIPSE('',#52820,1.34350288425444,0.95) ;
#444 = ELLIPSE('',#52825,0.141421356237322,0.1) ;
#445 = ELLIPSE('',#52829,0.141421356237322,0.1) ;
#446 = ELLIPSE('',#52836,0.223606797749974,0.0999999999999979) ;
#447 = ELLIPSE('',#52837,0.223606797749986,0.0999999999999979) ;
#448 = ELLIPSE('',#52967,0.258478364700829,0.0999999999999979) ;
#449 = ELLIPSE('',#52969,0.311144765372046,0.199999999999998) ;
#450 = ELLIPSE('',#52993,0.624999999999997,0.4) ;
#451 = ELLIPSE('',#53004,0.51747248987523,0.4999999999999) ;
#452 = ELLIPSE('',#53007,0.202758751010048,0.200000000000102) ;
#453 = ELLIPSE('',#53010,1.06510302057801,0.999999999999996) ;
#454 = ELLIPSE('',#53041,0.499999999999995,0.4) ;
#455 = ELLIPSE('',#53084,0.499999999999995,0.4) ;
#456 = ELLIPSE('',#53153,0.110950450383119,0.1) ;
#457 = ELLIPSE('',#53155,0.693271231193088,0.499999999999992) ;
#458 = ELLIPSE('',#53183,0.421637021355679,0.399999999999901) ;
#459 = ELLIPSE('',#53187,0.105409255339058,0.100000000000106) ;
#460 = ELLIPSE('',#53189,1.1595018087284,1.1) ;
#461 = ELLIPSE('',#53225,0.141421356237293,0.1) ;
#462 = ELLIPSE('',#53250,0.10597392847322,0.1) ;
#463 = ELLIPSE('',#53279,0.800390529679108,0.5) ;
#464 = ELLIPSE('',#53281,0.883883476483187,0.5) ;
#465 = ELLIPSE('',#53287,0.210818510677909,0.200000000000016) ;
#466 = ELLIPSE('',#53289,0.120185042515483,0.0999999999999979) ;
#467 = ELLIPSE('',#53291,0.21081851067789,0.199999999999998) ;
#468 = ELLIPSE('',#53293,0.120185042515479,0.0999999999999979) ;
#469 = ELLIPSE('',#53311,0.316227766016838,0.3) ;
#470 = ELLIPSE('',#53317,6.48266920334518,6.15) ;
#471 = ELLIPSE('',#53320,1.21037184369102,0.749999999999993) ;
#472 = ELLIPSE('',#53322,0.141421356237311,0.1) ;
#473 = ELLIPSE('',#53323,0.112603250061041,0.1) ;
#474 = ELLIPSE('',#53325,0.17320508075689,0.1) ;
#475 = ELLIPSE('',#53326,0.173205080756888,0.1) ;
#476 = ELLIPSE('',#53334,0.704171845621267,0.200000000000013) ;
#477 = ELLIPSE('',#53337,24.8233760798141,0.2) ;
#478 = ELLIPSE('',#53340,0.860232526704269,0.5) ;
#479 = ELLIPSE('',#53341,0.18370348154524,0.0706876553262425) ;
#480 = ELLIPSE('',#53343,0.989949493661167,0.7) ;
#481 = ELLIPSE('',#53347,0.777817459305202,0.55) ;
#482 = ELLIPSE('',#53348,0.930053761886906,0.75) ;
#483 = ELLIPSE('',#53349,0.930053761886906,0.75) ;
#484 = ELLIPSE('',#53358,0.675321117625136,0.479717269382621) ;
#485 = ELLIPSE('',#53360,6.4346717087976,4.55) ;
#486 = ELLIPSE('',#53363,0.461579895576042,0.2) ;
#487 = ELLIPSE('',#53367,0.282842712474621,0.2) ;
#488 = ELLIPSE('',#53373,0.565685424949227,0.399999999999992) ;
#489 = ELLIPSE('',#53379,6.48266920334518,6.15) ;
#490 = ELLIPSE('',#53401,0.100694440756805,0.100017263171969) ;
#491 = ELLIPSE('',#53406,0.108636037740531,0.1) ;
#492 = ELLIPSE('',#53416,0.179117445565849,0.1) ;
#493 = ELLIPSE('',#53419,0.179117445565765,0.1) ;
#494 = ELLIPSE('',#53421,0.265520995084799,0.1) ;
#495 = ELLIPSE('',#53429,0.179117445565772,0.1) ;
#496 = ELLIPSE('',#53431,0.265520995084877,0.1) ;
#497 = ELLIPSE('',#53433,0.179117445565864,0.1) ;
#498 = ELLIPSE('',#53440,0.179117445565776,0.1) ;
#499 = ELLIPSE('',#53441,0.141421356237291,0.1) ;
#500 = ELLIPSE('',#53443,0.265520995084917,0.1) ;
#501 = ELLIPSE('',#53445,0.179117445565779,0.1) ;
#502 = ELLIPSE('',#53447,0.141421356237298,0.1) ;
#503 = ELLIPSE('',#53449,0.14142135623732,0.1) ;
#504 = ELLIPSE('',#53451,0.141421356237322,0.1) ;
#505 = ELLIPSE('',#53459,0.141421356237284,0.1) ;
#506 = ELLIPSE('',#53460,0.141421356237347,0.1) ;
#507 = ELLIPSE('',#53462,0.141421356237322,0.1) ;
#508 = ELLIPSE('',#53464,0.141421356237297,0.1) ;
#509 = ELLIPSE('',#53470,0.141421356237321,0.1) ;
#510 = ELLIPSE('',#53471,0.17911744556577,0.1) ;
#511 = ELLIPSE('',#53473,0.141421356237297,0.1) ;
#512 = ELLIPSE('',#53475,0.141421356237325,0.1) ;
#513 = ELLIPSE('',#53477,0.141421356237269,0.1) ;
#514 = ELLIPSE('',#53479,0.17911744556575,0.1) ;
#515 = ELLIPSE('',#53481,0.265520995084842,0.1) ;
#516 = ELLIPSE('',#53489,0.141421356237322,0.1) ;
#517 = ELLIPSE('',#53490,0.141421356237297,0.1) ;
#518 = ELLIPSE('',#53492,0.141421356237297,0.1) ;
#519 = ELLIPSE('',#53494,0.141421356237322,0.1) ;
#520 = ELLIPSE('',#53500,0.179117445565841,0.1) ;
#521 = ELLIPSE('',#53501,0.265520995084931,0.1) ;
#522 = ELLIPSE('',#53503,0.141421356237301,0.1) ;
#523 = ELLIPSE('',#53511,0.141421356237312,0.1) ;
#524 = ELLIPSE('',#53513,0.141421356237306,0.1) ;
#525 = ELLIPSE('',#53521,0.141421356237327,0.1) ;
#526 = ELLIPSE('',#53523,0.179117445565764,0.1) ;
#527 = ELLIPSE('',#53534,0.141421356237301,0.1) ;
#528 = ELLIPSE('',#53535,0.179117445565841,0.1) ;
#529 = ELLIPSE('',#53543,0.141421356237313,0.1) ;
#530 = ELLIPSE('',#53545,0.141421356237306,0.1) ;
#531 = ELLIPSE('',#53553,0.141421356237327,0.1) ;
#532 = ELLIPSE('',#53555,0.179117445565764,0.1) ;
#533 = ELLIPSE('',#53557,0.265520995084931,0.1) ;
#534 = ELLIPSE('',#53569,0.179117445565845,0.1) ;
#535 = ELLIPSE('',#53571,0.265520995084763,0.1) ;
#536 = ELLIPSE('',#53573,0.179117445565757,0.1) ;
#537 = ELLIPSE('',#53577,0.179117445565837,0.1) ;
#538 = ELLIPSE('',#53579,0.179117445565763,0.1) ;
#539 = ELLIPSE('',#53580,0.265520995084739,0.1) ;
#540 = ELLIPSE('',#53587,0.179117445565766,0.1) ;
#541 = ELLIPSE('',#53588,0.265520995084941,0.1) ;
#542 = ELLIPSE('',#53590,0.179117445565779,0.1) ;
#543 = ELLIPSE('',#53592,0.141421356237327,0.1) ;
#544 = ELLIPSE('',#53594,0.141421356237297,0.1) ;
#545 = ELLIPSE('',#53596,0.141421356237347,0.1) ;
#546 = ELLIPSE('',#53598,0.141421356237294,0.1) ;
#547 = ELLIPSE('',#53610,0.14142135623731,0.1) ;
#548 = ELLIPSE('',#53611,0.141421356237284,0.1) ;
#549 = ELLIPSE('',#53613,0.141421356237322,0.1) ;
#550 = ELLIPSE('',#53615,0.141421356237297,0.1) ;
#551 = ELLIPSE('',#53619,0.141421356237325,0.1) ;
#552 = ELLIPSE('',#53620,0.141421356237319,0.1) ;
#553 = ELLIPSE('',#53622,0.141421356237303,0.1) ;
#554 = ELLIPSE('',#53624,0.179117445565787,0.1) ;
#555 = ELLIPSE('',#53626,0.265520995084743,0.1) ;
#556 = ELLIPSE('',#53628,0.179117445565783,0.1) ;
#557 = ELLIPSE('',#53630,0.141421356237323,0.1) ;
#558 = ELLIPSE('',#53635,0.141421356237297,0.1) ;
#559 = ELLIPSE('',#53636,0.141421356237322,0.1) ;
#560 = ELLIPSE('',#53638,0.141421356237322,0.1) ;
#561 = ELLIPSE('',#53640,0.141421356237322,0.1) ;
#562 = ELLIPSE('',#53644,0.141421356237324,0.1) ;
#563 = ELLIPSE('',#53646,0.179117445565837,0.1) ;
#564 = ELLIPSE('',#53648,0.265520995084907,0.1) ;
#565 = ELLIPSE('',#53650,0.17911744556577,0.1) ;
#566 = ELLIPSE('',#53652,0.141421356237293,0.1) ;
#567 = ELLIPSE('',#53669,0.141421356237314,0.1) ;
#568 = ELLIPSE('',#53670,0.141421356237323,0.1) ;
#569 = ELLIPSE('',#53673,0.141421356237324,0.1) ;
#570 = ELLIPSE('',#53675,0.179117445565837,0.1) ;
#571 = ELLIPSE('',#53677,0.265520995084885,0.1) ;
#572 = ELLIPSE('',#53679,0.179117445565777,0.1) ;
#573 = ELLIPSE('',#53681,0.141421356237293,0.1) ;
#574 = ELLIPSE('',#53750,0.554752251915545,0.5) ;
#575 = ELLIPSE('',#53770,1.17924764150709,0.999999999999996) ;
#576 = ELLIPSE('',#53781,6.09138736249799,4.05) ;
#577 = ELLIPSE('',#53794,6.09138736249799,4.05) ;
#578 = ELLIPSE('',#53808,1.04166666666667,0.5) ;
#579 = ELLIPSE('',#53810,1.17924764150709,0.999999999999997) ;
#580 = ELLIPSE('',#53811,0.800390529679107,0.5) ;
#581 = ELLIPSE('',#53814,1.17924764150709,0.999999999999997) ;
#582 = ELLIPSE('',#53815,0.800390529679107,0.5) ;
#583 = ELLIPSE('',#53817,0.883883476483178,0.5) ;
#584 = ELLIPSE('',#53821,1.17924764150709,0.999999999999996) ;
#585 = ELLIPSE('',#53822,0.800390529679108,0.5) ;
#586 = SHAPE_REPRESENTATION_RELATIONSHIP('SRR','None',#117241,#607) ;
#587 = SHAPE_REPRESENTATION_RELATIONSHIP('SRR','None',#117242,#608) ;
#588 = SHAPE_REPRESENTATION_RELATIONSHIP('SRR','None',#117243,#609) ;
#589 = SHAPE_REPRESENTATION_RELATIONSHIP('SRR','None',#117244,#610) ;
#590 = SHAPE_REPRESENTATION_RELATIONSHIP('SRR','None',#117245,#611) ;
#591 = SHAPE_REPRESENTATION_RELATIONSHIP('SRR','None',#117246,#612) ;
#592 = SHAPE_REPRESENTATION_RELATIONSHIP('SRR','None',#117247,#613) ;
#593 = SHAPE_REPRESENTATION_RELATIONSHIP('SRR','None',#117248,#614) ;
#594 = SHAPE_REPRESENTATION_RELATIONSHIP('SRR','None',#117249,#615) ;
#595 = SHAPE_REPRESENTATION_RELATIONSHIP('SRR','None',#117250,#616) ;
#596 = SHAPE_REPRESENTATION_RELATIONSHIP('SRR','None',#117251,#617) ;
#597 = SHAPE_REPRESENTATION_RELATIONSHIP('SRR','None',#117252,#618) ;
#598 = SHAPE_REPRESENTATION_RELATIONSHIP('SRR','None',#117253,#619) ;
#599 = SHAPE_REPRESENTATION_RELATIONSHIP('SRR','None',#117254,#620) ;
#600 = SHAPE_REPRESENTATION_RELATIONSHIP('SRR','None',#117255,#621) ;
#601 = SHAPE_REPRESENTATION_RELATIONSHIP('SRR','None',#117256,#622) ;
#602 = SHAPE_REPRESENTATION_RELATIONSHIP('SRR','None',#117257,#623) ;
#603 = SHAPE_REPRESENTATION_RELATIONSHIP('SRR','None',#117258,#624) ;
#604 = SHAPE_REPRESENTATION_RELATIONSHIP('SRR','None',#117259,#625) ;
#605 = SHAPE_REPRESENTATION_RELATIONSHIP('SRR','None',#117260,#626) ;
#606 = SHAPE_REPRESENTATION_RELATIONSHIP('SRR','None',#117261,#627) ;
#607 = ADVANCED_BREP_SHAPE_REPRESENTATION('',(#649),#117149) ;
#608 = ADVANCED_BREP_SHAPE_REPRESENTATION('',(#650),#117150) ;
#609 = ADVANCED_BREP_SHAPE_REPRESENTATION('',(#651),#117151) ;
#610 = ADVANCED_BREP_SHAPE_REPRESENTATION('',(#652),#117152) ;
#611 = ADVANCED_BREP_SHAPE_REPRESENTATION('',(#653),#117153) ;
#612 = ADVANCED_BREP_SHAPE_REPRESENTATION('',(#654),#117154) ;
#613 = ADVANCED_BREP_SHAPE_REPRESENTATION('',(#655),#117155) ;
#614 = ADVANCED_BREP_SHAPE_REPRESENTATION('',(#656),#117156) ;
#615 = ADVANCED_BREP_SHAPE_REPRESENTATION('',(#657),#117157) ;
#616 = ADVANCED_BREP_SHAPE_REPRESENTATION('',(#658),#117158) ;
#617 = ADVANCED_BREP_SHAPE_REPRESENTATION('',(#659),#117159) ;
#618 = ADVANCED_BREP_SHAPE_REPRESENTATION('',(#660),#117160) ;
#619 = ADVANCED_BREP_SHAPE_REPRESENTATION('',(#661),#117161) ;
#620 = ADVANCED_BREP_SHAPE_REPRESENTATION('',(#662),#117162) ;
#621 = ADVANCED_BREP_SHAPE_REPRESENTATION('',(#663),#117163) ;
#622 = ADVANCED_BREP_SHAPE_REPRESENTATION('',(#664),#117164) ;
#623 = ADVANCED_BREP_SHAPE_REPRESENTATION('',(#665),#117165) ;
#624 = ADVANCED_BREP_SHAPE_REPRESENTATION('',(#666),#117166) ;
#625 = ADVANCED_BREP_SHAPE_REPRESENTATION('',(#667),#117167) ;
#626 = ADVANCED_BREP_SHAPE_REPRESENTATION('',(#668),#117168) ;
#627 = ADVANCED_BREP_SHAPE_REPRESENTATION('',(#669),#117169) ;
#628 = STYLED_ITEM('',(#117355),#649) ;
#629 = STYLED_ITEM('',(#117355),#650) ;
#630 = STYLED_ITEM('',(#117355),#651) ;
#631 = STYLED_ITEM('',(#117355),#652) ;
#632 = STYLED_ITEM('',(#117355),#653) ;
#633 = STYLED_ITEM('',(#117355),#654) ;
#634 = STYLED_ITEM('',(#117355),#655) ;
#635 = STYLED_ITEM('',(#117355),#656) ;
#636 = STYLED_ITEM('',(#117355),#657) ;
#637 = STYLED_ITEM('',(#117355),#658) ;
#638 = STYLED_ITEM('',(#117355),#659) ;
#639 = STYLED_ITEM('',(#117355),#660) ;
#640 = STYLED_ITEM('',(#117355),#661) ;
#641 = STYLED_ITEM('',(#117355),#662) ;
#642 = STYLED_ITEM('',(#117355),#663) ;
#643 = STYLED_ITEM('',(#117355),#664) ;
#644 = STYLED_ITEM('',(#117355),#665) ;
#645 = STYLED_ITEM('',(#117355),#666) ;
#646 = STYLED_ITEM('',(#117355),#667) ;
#647 = STYLED_ITEM('',(#117355),#668) ;
#648 = STYLED_ITEM('',(#117355),#669) ;
#649 = MANIFOLD_SOLID_BREP('Body1',#49057) ;
#650 = MANIFOLD_SOLID_BREP('Body1',#49058) ;
#651 = MANIFOLD_SOLID_BREP('Body1',#49059) ;
#652 = MANIFOLD_SOLID_BREP('Body1',#49060) ;
#653 = MANIFOLD_SOLID_BREP('Body1',#49061) ;
#654 = MANIFOLD_SOLID_BREP('Body1',#49062) ;
#655 = MANIFOLD_SOLID_BREP('Body1',#49063) ;
#656 = MANIFOLD_SOLID_BREP('Body1',#49064) ;
#657 = MANIFOLD_SOLID_BREP('Body1',#49065) ;
#658 = MANIFOLD_SOLID_BREP('Body1',#49066) ;
#659 = MANIFOLD_SOLID_BREP('Body1',#49067) ;
#660 = MANIFOLD_SOLID_BREP('Body1',#49068) ;
#661 = MANIFOLD_SOLID_BREP('Body1',#49069) ;
#662 = MANIFOLD_SOLID_BREP('Body1',#49070) ;
#663 = MANIFOLD_SOLID_BREP('Body1',#49071) ;
#664 = MANIFOLD_SOLID_BREP('Body1',#49072) ;
#665 = MANIFOLD_SOLID_BREP('Body1',#49073) ;
#666 = MANIFOLD_SOLID_BREP('Body1',#49074) ;
#667 = MANIFOLD_SOLID_BREP('Body1',#49075) ;
#668 = MANIFOLD_SOLID_BREP('Body1',#49076) ;
#669 = MANIFOLD_SOLID_BREP('Body1',#49077) ;
#670 = FACE_BOUND('',#14042,.T.) ;
#671 = FACE_BOUND('',#14121,.T.) ;
#672 = FACE_BOUND('',#14122,.T.) ;
#673 = FACE_BOUND('',#14123,.T.) ;
#674 = FACE_BOUND('',#14124,.T.) ;
#675 = FACE_BOUND('',#14239,.T.) ;
#676 = FACE_BOUND('',#14240,.T.) ;
#677 = FACE_BOUND('',#14304,.T.) ;
#678 = FACE_BOUND('',#14305,.T.) ;
#679 = FACE_BOUND('',#14322,.T.) ;
#680 = FACE_BOUND('',#14408,.T.) ;
#681 = FACE_BOUND('',#14409,.T.) ;
#682 = FACE_BOUND('',#14410,.T.) ;
#683 = FACE_BOUND('',#14411,.T.) ;
#684 = FACE_BOUND('',#14412,.T.) ;
#685 = FACE_BOUND('',#14413,.T.) ;
#686 = FACE_BOUND('',#14414,.T.) ;
#687 = FACE_BOUND('',#14415,.T.) ;
#688 = FACE_BOUND('',#14416,.T.) ;
#689 = FACE_BOUND('',#14417,.T.) ;
#690 = FACE_BOUND('',#14418,.T.) ;
#691 = FACE_BOUND('',#14419,.T.) ;
#692 = FACE_BOUND('',#14420,.T.) ;
#693 = FACE_BOUND('',#14421,.T.) ;
#694 = FACE_BOUND('',#14422,.T.) ;
#695 = FACE_BOUND('',#14423,.T.) ;
#696 = FACE_BOUND('',#14424,.T.) ;
#697 = FACE_BOUND('',#14425,.T.) ;
#698 = FACE_BOUND('',#14447,.T.) ;
#699 = FACE_BOUND('',#14453,.T.) ;
#700 = FACE_BOUND('',#14454,.T.) ;
#701 = FACE_BOUND('',#14455,.T.) ;
#702 = FACE_BOUND('',#14456,.T.) ;
#703 = FACE_BOUND('',#14457,.T.) ;
#704 = FACE_BOUND('',#14458,.T.) ;
#705 = FACE_BOUND('',#14459,.T.) ;
#706 = FACE_BOUND('',#14460,.T.) ;
#707 = FACE_BOUND('',#14461,.T.) ;
#708 = FACE_BOUND('',#14462,.T.) ;
#709 = FACE_BOUND('',#14463,.T.) ;
#710 = FACE_BOUND('',#14464,.T.) ;
#711 = FACE_BOUND('',#14465,.T.) ;
#712 = FACE_BOUND('',#14466,.T.) ;
#713 = FACE_BOUND('',#14496,.T.) ;
#714 = FACE_BOUND('',#14502,.T.) ;
#715 = FACE_BOUND('',#14505,.T.) ;
#716 = FACE_BOUND('',#14509,.T.) ;
#717 = FACE_BOUND('',#14512,.T.) ;
#718 = FACE_BOUND('',#15017,.T.) ;
#719 = FACE_BOUND('',#15025,.T.) ;
#720 = FACE_BOUND('',#15032,.T.) ;
#721 = FACE_BOUND('',#15038,.T.) ;
#722 = FACE_BOUND('',#15126,.T.) ;
#723 = FACE_BOUND('',#15127,.T.) ;
#724 = FACE_BOUND('',#15128,.T.) ;
#725 = FACE_BOUND('',#15129,.T.) ;
#726 = FACE_BOUND('',#15130,.T.) ;
#727 = FACE_BOUND('',#15135,.T.) ;
#728 = FACE_BOUND('',#15136,.T.) ;
#729 = FACE_BOUND('',#15258,.T.) ;
#730 = FACE_BOUND('',#15263,.T.) ;
#731 = FACE_BOUND('',#15267,.T.) ;
#732 = FACE_BOUND('',#15270,.T.) ;
#733 = FACE_BOUND('',#15331,.T.) ;
#734 = FACE_BOUND('',#15393,.T.) ;
#735 = FACE_BOUND('',#15452,.T.) ;
#736 = FACE_BOUND('',#15495,.T.) ;
#737 = FACE_BOUND('',#15539,.T.) ;
#738 = FACE_BOUND('',#15575,.T.) ;
#739 = FACE_BOUND('',#15577,.T.) ;
#740 = FACE_BOUND('',#15578,.T.) ;
#741 = FACE_BOUND('',#15718,.T.) ;
#742 = FACE_BOUND('',#15719,.T.) ;
#743 = FACE_BOUND('',#15720,.T.) ;
#744 = FACE_BOUND('',#15721,.T.) ;
#745 = FACE_BOUND('',#15722,.T.) ;
#746 = FACE_BOUND('',#15723,.T.) ;
#747 = FACE_BOUND('',#15724,.T.) ;
#748 = FACE_BOUND('',#15886,.T.) ;
#749 = FACE_BOUND('',#15887,.T.) ;
#750 = FACE_BOUND('',#15891,.T.) ;
#751 = FACE_BOUND('',#15930,.T.) ;
#752 = FACE_BOUND('',#15931,.T.) ;
#753 = FACE_BOUND('',#15932,.T.) ;
#754 = FACE_BOUND('',#15963,.T.) ;
#755 = FACE_BOUND('',#15973,.T.) ;
#756 = FACE_BOUND('',#15976,.T.) ;
#757 = FACE_BOUND('',#16106,.T.) ;
#758 = FACE_BOUND('',#16107,.T.) ;
#759 = FACE_BOUND('',#16108,.T.) ;
#760 = FACE_BOUND('',#16262,.T.) ;
#761 = FACE_BOUND('',#16411,.T.) ;
#762 = FACE_BOUND('',#16420,.T.) ;
#763 = FACE_BOUND('',#16423,.T.) ;
#764 = FACE_BOUND('',#16425,.T.) ;
#765 = FACE_BOUND('',#16427,.T.) ;
#766 = FACE_BOUND('',#16715,.T.) ;
#767 = FACE_BOUND('',#16718,.T.) ;
#768 = FACE_BOUND('',#16720,.T.) ;
#769 = FACE_BOUND('',#16722,.T.) ;
#770 = FACE_BOUND('',#17019,.T.) ;
#771 = FACE_BOUND('',#17020,.T.) ;
#772 = FACE_BOUND('',#17021,.T.) ;
#773 = CONICAL_SURFACE('',#49762,5.625,0.558599315343563) ;
#774 = B_SPLINE_CURVE_WITH_KNOTS('',3,(#70344,#70345,#70346,#70347,#70348,
#70349,#70350,#70351,#70352,#70353,#70354,#70355,#70356,#70357,#70358,#70359,
#70360,#70361,#70362,#70363,#70364,#70365,#70366,#70367,#70368,#70369,#70370,
#70371,#70372,#70373,#70374,#70375,#70376,#70377,#70378,#70379,#70380,#70381,
#70382,#70383,#70384,#70385,#70386,#70387,#70388,#70389,#70390,#70391,#70392,
#70393,#70394,#70395,#70396,#70397,#70398,#70399,#70400,#70401,#70402,#70403,
#70404,#70405,#70406,#70407,#70408,#70409,#70410,#70411,#70412,#70413,#70414,
#70415,#70416,#70417,#70418,#70419,#70420,#70421,#70422,#70423,#70424,#70425,
#70426,#70427,#70428,#70429,#70430,#70431),.UNSPECIFIED.,.F.,.F.,(4,3,3,
3,3,3,3,3,3,3,3,3,3,3,3,3,3,3,3,3,3,3,3,3,3,3,3,3,3,4),(-0.886548021255927,
-0.866020543548015,-0.85169317239197,-0.845493065840103,-0.808981660034209,
-0.804435696364636,-0.793163090763113,-0.783892247515284,-0.778078363126709,
-0.774199582871934,-0.763350099380766,-0.757877841764194,-0.753807164984933,
-0.753076248451023,-0.744625414255735,-0.742798718670203,-0.736893863257229,
-0.732522509684251,-0.728117623171179,-0.724865268798491,-0.722246227513741,
-0.711109540545207,-0.704984345704586,-0.701711705949509,-0.681173329351425,
-0.671410018653926,-0.651499699186982,-0.640118813275259,-0.619305464345444,
-0.599057470751597),.UNSPECIFIED.) ;
#775 = B_SPLINE_CURVE_WITH_KNOTS('',3,(#70432,#70433,#70434,#70435,#70436,
#70437,#70438,#70439,#70440,#70441,#70442,#70443,#70444,#70445,#70446,#70447,
#70448,#70449,#70450,#70451,#70452,#70453,#70454,#70455,#70456,#70457,#70458,
#70459,#70460,#70461,#70462,#70463,#70464,#70465,#70466,#70467,#70468,#70469,
#70470,#70471,#70472,#70473,#70474,#70475,#70476,#70477,#70478,#70479,#70480,
#70481,#70482,#70483,#70484,#70485,#70486,#70487,#70488,#70489,#70490,#70491,
#70492,#70493,#70494,#70495,#70496,#70497,#70498,#70499,#70500,#70501,#70502,
#70503,#70504,#70505,#70506,#70507,#70508,#70509,#70510,#70511,#70512,#70513,
#70514,#70515,#70516,#70517,#70518,#70519,#70520,#70521,#70522,#70523,#70524,
#70525,#70526,#70527,#70528,#70529,#70530,#70531,#70532,#70533,#70534),
 .UNSPECIFIED.,.F.,.F.,(4,3,3,3,3,3,3,3,3,3,3,3,3,3,3,3,3,3,3,3,3,3,3,3,
3,3,3,3,3,3,3,3,3,3,4),(0.599057470828701,0.615298120440717,0.630942941477274,
0.640127549392609,0.652806522977644,0.665132753910298,0.676916585880226,
0.681197628036496,0.691465147697467,0.700856798218276,0.701732667358439,
0.711232361509187,0.720303122206591,0.722267706680382,0.729879902279182,
0.732535226341353,0.738884690099024,0.742802746002325,0.74911482874544,
0.753070265663297,0.760745074540522,0.763337785324268,0.77242917331783,
0.781938963322013,0.783872824646211,0.793256044991626,0.803051435018297,
0.804407863968155,0.816263178412735,0.828482331000289,0.841197645853686,
0.845477942612041,0.861112429390543,0.877369654187312,0.886548021255484),
 .UNSPECIFIED.) ;
#776 = B_SPLINE_CURVE_WITH_KNOTS('',3,(#70636,#70637,#70638,#70639,#70640,
#70641,#70642,#70643,#70644,#70645,#70646,#70647,#70648,#70649,#70650,#70651,
#70652,#70653,#70654,#70655,#70656,#70657,#70658,#70659,#70660,#70661,#70662,
#70663,#70664,#70665,#70666,#70667,#70668,#70669,#70670,#70671,#70672,#70673,
#70674,#70675,#70676,#70677,#70678,#70679,#70680,#70681,#70682,#70683,#70684,
#70685,#70686,#70687,#70688,#70689,#70690,#70691,#70692,#70693,#70694,#70695,
#70696,#70697,#70698,#70699,#70700,#70701,#70702,#70703,#70704,#70705,#70706,
#70707,#70708,#70709,#70710,#70711,#70712,#70713,#70714,#70715,#70716,#70717,
#70718,#70719,#70720,#70721,#70722,#70723,#70724,#70725,#70726,#70727,#70728,
#70729,#70730,#70731,#70732,#70733,#70734,#70735,#70736,#70737,#70738),
 .UNSPECIFIED.,.F.,.F.,(4,3,3,3,3,3,3,3,3,3,3,3,3,3,3,3,3,3,3,3,3,3,3,3,
3,3,3,3,3,3,3,3,3,3,4),(-0.886548021255908,-0.85656200124965,-0.850026819726932,
-0.84552111160629,-0.818797995447373,-0.814748789578144,-0.809615111606091,
-0.804479243671707,-0.803419323869529,-0.79434065594564,-0.786062741228933,
-0.777784826512226,-0.769788161614651,-0.763365298601152,-0.756898169483173,
-0.751589110728878,-0.748585034020594,-0.747944605577357,-0.743298812044044,
-0.742232977096382,-0.736337056382533,-0.729968012731944,-0.727476816747177,
-0.722258382596352,-0.714591862386322,-0.712000866477793,-0.704984345704397,
-0.701741062663608,-0.687720687939676,-0.681207485515591,-0.671410018653668,
-0.652269418497491,-0.640136959183649,-0.619305464345044,-0.599057470751579),
 .UNSPECIFIED.) ;
#777 = B_SPLINE_CURVE_WITH_KNOTS('',3,(#70739,#70740,#70741,#70742,#70743,
#70744,#70745,#70746,#70747,#70748,#70749,#70750,#70751,#70752,#70753),
 .UNSPECIFIED.,.F.,.F.,(4,1,1,1,1,1,1,1,1,1,1,1,4),(0.599057470748727,0.64012754939261,
0.681197628036493,0.701732667358435,0.712000187019406,0.722267706680377,
0.747936505832804,0.76333778532426,0.804407863968143,0.809541623798628,
0.814675383629114,0.845477942612026,0.886548021255909),.UNSPECIFIED.) ;
#778 = B_SPLINE_CURVE_WITH_KNOTS('',3,(#70855,#70856,#70857,#70858,#70859,
#70860,#70861,#70862,#70863,#70864,#70865,#70866,#70867,#70868,#70869),
 .UNSPECIFIED.,.F.,.F.,(4,1,1,1,1,1,1,1,1,1,1,1,4),(-1.15463223446652,-1.11356235392859,
-1.07249247339066,-1.0519575331217,-1.03142259285273,-1.02115512271825,
-1.01088765258376,-1.00062018244928,-0.990352712314799,-0.969817772045833,
-0.949282831776868,-0.908212951238937,-0.867143070701024),.UNSPECIFIED.) ;
#779 = B_SPLINE_CURVE_WITH_KNOTS('',3,(#70870,#70871,#70872,#70873,#70874,
#70875,#70876,#70877,#70878,#70879,#70880,#70881,#70882,#70883,#70884,#70885,
#70886,#70887,#70888,#70889,#70890,#70891,#70892,#70893,#70894,#70895,#70896,
#70897,#70898,#70899,#70900,#70901,#70902,#70903,#70904,#70905,#70906,#70907,
#70908,#70909,#70910,#70911,#70912,#70913,#70914,#70915,#70916,#70917,#70918,
#70919,#70920,#70921,#70922,#70923,#70924,#70925,#70926,#70927,#70928,#70929,
#70930,#70931,#70932,#70933,#70934,#70935,#70936,#70937,#70938,#70939,#70940,
#70941,#70942,#70943,#70944,#70945,#70946,#70947,#70948,#70949,#70950,#70951,
#70952,#70953,#70954,#70955,#70956,#70957,#70958,#70959,#70960,#70961,#70962,
#70963,#70964,#70965,#70966,#70967,#70968,#70969,#70970,#70971,#70972),
 .UNSPECIFIED.,.F.,.F.,(4,3,3,3,3,3,3,3,3,3,3,3,3,3,3,3,3,3,3,3,3,3,3,3,
3,3,3,3,3,3,3,3,3,3,4),(0.867143070701496,0.88348027656878,0.899207678557921,
0.908212951238937,0.920868217474062,0.93317273149953,0.944935984179887,
0.949282831776868,0.95955030191135,0.968956555049588,0.969817772045833,
0.979310937859832,0.988375034212218,0.990352712314798,0.997960594090661,
1.00062018244928,1.00697043075183,1.01088765258376,1.01719943353249,1.02115512271825,
1.02883039234673,1.03142259285273,1.04051400153883,1.05002381110541,1.05195753312169,
1.06134071200587,1.07113605612072,1.07249247339066,1.08434800661934,1.09656739397206,
1.10928297177777,1.11356235392859,1.12919562860283,1.14545149693943,1.15463223446608),
 .UNSPECIFIED.) ;
#780 = B_SPLINE_CURVE_WITH_KNOTS('',3,(#71075,#71076,#71077,#71078,#71079,
#71080,#71081,#71082,#71083),.UNSPECIFIED.,.F.,.F.,(4,1,1,1,1,1,4),(-0.411832935461353,
-0.370762950184382,-0.32969296490741,-0.309157972268924,-0.288622979630438,
-0.278355483311195,-0.268092192038243),.UNSPECIFIED.) ;
#781 = B_SPLINE_CURVE_WITH_KNOTS('',3,(#71084,#71085,#71086,#71087,#71088,
#71089,#71090,#71091,#71092,#71093),.UNSPECIFIED.,.F.,.F.,(4,2,1,1,1,1,
4),(-0.268087986585571,-0.257816585743201,-0.247549389803151,-0.227014997923051,
-0.206480606042951,-0.165411822282751,-0.124343038522569),.UNSPECIFIED.) ;
#782 = B_SPLINE_CURVE_WITH_KNOTS('',3,(#71094,#71095,#71096,#71097,#71098,
#71099,#71100,#71101,#71102,#71103,#71104,#71105,#71106,#71107,#71108,#71109,
#71110,#71111,#71112,#71113,#71114,#71115,#71116,#71117,#71118,#71119,#71120,
#71121,#71122,#71123,#71124,#71125,#71126,#71127,#71128,#71129,#71130,#71131,
#71132,#71133,#71134,#71135,#71136,#71137,#71138,#71139,#71140,#71141,#71142,
#71143,#71144,#71145,#71146,#71147,#71148,#71149,#71150,#71151,#71152,#71153,
#71154,#71155,#71156,#71157,#71158,#71159,#71160,#71161,#71162,#71163,#71164,
#71165,#71166,#71167,#71168,#71169,#71170,#71171,#71172,#71173,#71174,#71175,
#71176,#71177,#71178,#71179,#71180,#71181,#71182,#71183,#71184,#71185,#71186,
#71187,#71188,#71189,#71190,#71191,#71192,#71193,#71194,#71195,#71196),
 .UNSPECIFIED.,.F.,.F.,(4,3,3,3,3,3,3,3,3,3,3,3,3,3,3,3,3,3,3,3,3,3,3,3,
3,3,3,3,3,3,3,3,3,3,4),(0.124343038523051,0.140680308431655,0.156407764717396,
0.165413023799523,0.178068277230974,0.190372779140203,0.202136018930834,
0.206483009076495,0.216750505395738,0.226156738905456,0.227018001714981,
0.236511182380948,0.245575293706971,0.247552994353466,0.25516079885379,
0.257820490672709,0.264170716687648,0.268087986991952,0.274399785478541,
0.278355483311195,0.286030903500035,0.288622979630438,0.297714437508149,
0.307224296648561,0.309157972268924,0.318541007588984,0.328336197211916,
0.32969296490741,0.341549046953001,0.353769017763909,0.366485239447413,
0.370762950184382,0.386395556645212,0.402650777555412,0.411832935460906),
 .UNSPECIFIED.) ;
#783 = B_SPLINE_CURVE_WITH_KNOTS('',3,(#71293,#71294,#71295,#71296,#71297,
#71298,#71299,#71300,#71301,#71302,#71303,#71304,#71305,#71306,#71307,#71308,
#71309,#71310,#71311,#71312,#71313,#71314,#71315,#71316,#71317,#71318,#71319,
#71320,#71321,#71322,#71323,#71324,#71325,#71326,#71327,#71328,#71329,#71330,
#71331,#71332,#71333,#71334,#71335,#71336,#71337,#71338,#71339,#71340,#71341,
#71342,#71343,#71344,#71345,#71346,#71347,#71348,#71349,#71350,#71351,#71352,
#71353,#71354,#71355,#71356,#71357,#71358,#71359,#71360,#71361,#71362,#71363,
#71364,#71365,#71366,#71367,#71368,#71369,#71370,#71371,#71372,#71373,#71374,
#71375,#71376,#71377,#71378,#71379,#71380,#71381,#71382,#71383,#71384,#71385,
#71386,#71387,#71388,#71389,#71390,#71391,#71392,#71393,#71394,#71395,#71396,
#71397,#71398,#71399,#71400,#71401,#71402,#71403,#71404,#71405,#71406,#71407,
#71408,#71409,#71410),.UNSPECIFIED.,.F.,.F.,(4,3,3,3,3,3,3,3,3,3,3,3,3,
3,3,3,3,3,3,3,3,3,3,3,3,3,3,3,3,3,3,3,3,3,3,3,3,3,3,4),(-0.477703831735214,
-0.454370643331098,-0.441181670393938,-0.436642153009234,-0.419200933510066,
-0.415005716588499,-0.398974103759707,-0.395554960231289,-0.394574174536507,
-0.380610876858235,-0.378136361334893,-0.375012123153041,-0.368939677179199,
-0.360083437747083,-0.354460833860627,-0.348053020150135,-0.340898396750089,
-0.339739884687549,-0.333958883265811,-0.329511911359018,-0.328177881844074,
-0.323681740140828,-0.319864746381499,-0.313388628374842,-0.305652785221246,
-0.303121846558283,-0.29897808935245,-0.292853793170735,-0.27960979488877,
-0.276868043426208,-0.273343591995159,-0.272324458736955,-0.256566521937693,
-0.251801543361572,-0.233103219355294,-0.229693343333032,-0.22673609613777,
-0.210005147820851,-0.192797532028038,-0.190214667974652),.UNSPECIFIED.) ;
#784 = B_SPLINE_CURVE_WITH_KNOTS('',3,(#71411,#71412,#71413,#71414,#71415,
#71416,#71417,#71418,#71419,#71420,#71421,#71422,#71423,#71424),
 .UNSPECIFIED.,.F.,.F.,(4,1,1,1,1,1,1,1,1,1,1,4),(0.190214667974634,0.251819488780472,
0.272354429049085,0.292889369317698,0.303156839452004,0.313424309586311,
0.323691779720617,0.354494190123537,0.375029130392149,0.395564070660762,
0.436633951197988,0.477703831735214),.UNSPECIFIED.) ;
#785 = B_SPLINE_CURVE_WITH_KNOTS('',3,(#71526,#71527,#71528,#71529,#71530,
#71531,#71532,#71533,#71534,#71535,#71536,#71537,#71538,#71539,#71540,#71541,
#71542,#71543,#71544,#71545,#71546,#71547,#71548,#71549,#71550,#71551,#71552,
#71553,#71554,#71555,#71556,#71557,#71558,#71559,#71560,#71561,#71562,#71563,
#71564,#71565,#71566,#71567,#71568,#71569,#71570,#71571,#71572,#71573,#71574,
#71575,#71576,#71577,#71578,#71579,#71580,#71581,#71582,#71583,#71584,#71585,
#71586,#71587,#71588,#71589,#71590,#71591,#71592,#71593,#71594,#71595,#71596,
#71597,#71598,#71599,#71600,#71601,#71602,#71603,#71604,#71605,#71606,#71607,
#71608,#71609,#71610,#71611,#71612,#71613,#71614,#71615,#71616,#71617,#71618,
#71619,#71620,#71621,#71622,#71623,#71624,#71625,#71626,#71627,#71628),
 .UNSPECIFIED.,.F.,.F.,(4,3,3,3,3,3,3,3,3,3,3,3,3,3,3,3,3,3,3,3,3,3,3,3,
3,3,3,3,3,3,3,3,3,3,4),(-0.88654802125593,-0.856559921133392,-0.850026819726776,
-0.845521107818283,-0.818795307853085,-0.814748784266003,-0.809615106409565,
-0.804479238719332,-0.803419323869451,-0.794340522423511,-0.786062674467852,
-0.777784826512192,-0.769787867667373,-0.763365294944202,-0.756898169483178,
-0.751589194764963,-0.748585034020606,-0.747944599813433,-0.743298958411371,
-0.742232977096391,-0.736337056382542,-0.729968873694819,-0.72747681674717,
-0.72225837506046,-0.714591851231898,-0.712000858187692,-0.704984345704301,
-0.70174105366968,-0.687720677804165,-0.681207476307132,-0.671410018653507,
-0.65226935125413,-0.640136953755786,-0.619305464344787,-0.599057470751606),
 .UNSPECIFIED.) ;
#786 = B_SPLINE_CURVE_WITH_KNOTS('',3,(#71629,#71630,#71631,#71632,#71633,
#71634,#71635,#71636,#71637,#71638,#71639,#71640,#71641,#71642,#71643),
 .UNSPECIFIED.,.F.,.F.,(4,1,1,1,1,1,1,1,1,1,1,1,4),(0.599057470748751,0.640127549392634,
0.681197628036517,0.701732667358458,0.712000187019429,0.7222677066804,0.747936505832826,
0.763337785324282,0.804407863968165,0.80954162379865,0.814675383629136,
0.845477942612048,0.88654802125593),.UNSPECIFIED.) ;
#787 = B_SPLINE_CURVE_WITH_KNOTS('',3,(#71745,#71746,#71747,#71748,#71749,
#71750,#71751,#71752,#71753,#71754,#71755,#71756,#71757,#71758,#71759,#71760,
#71761,#71762,#71763,#71764,#71765,#71766,#71767,#71768,#71769,#71770,#71771,
#71772,#71773,#71774,#71775,#71776,#71777,#71778,#71779,#71780,#71781,#71782,
#71783,#71784,#71785,#71786,#71787,#71788,#71789,#71790,#71791,#71792,#71793,
#71794,#71795,#71796,#71797,#71798,#71799,#71800,#71801,#71802,#71803,#71804,
#71805,#71806,#71807,#71808,#71809,#71810,#71811,#71812,#71813,#71814,#71815,
#71816,#71817,#71818,#71819,#71820,#71821,#71822,#71823,#71824,#71825,#71826,
#71827,#71828,#71829,#71830,#71831,#71832,#71833,#71834,#71835,#71836,#71837,
#71838,#71839,#71840,#71841,#71842,#71843,#71844,#71845,#71846,#71847),
 .UNSPECIFIED.,.F.,.F.,(4,3,3,3,3,3,3,3,3,3,3,3,3,3,3,3,3,3,3,3,3,3,3,3,
3,3,3,3,3,3,3,3,3,3,4),(-0.886548021255932,-0.856559926135766,-0.850026819726765,
-0.845521107827399,-0.818795314317799,-0.814748784278784,-0.809615106422069,
-0.804479238731248,-0.803419323869445,-0.794340522744604,-0.786062674628396,
-0.777784826512188,-0.769787868374517,-0.763365294952999,-0.756898169483175,
-0.751589194563149,-0.748585034020601,-0.747944599827302,-0.743298958059412,
-0.742232977096372,-0.736337056382513,-0.729968871625694,-0.727476816747115,
-0.72225837507861,-0.714591851258856,-0.712000858207665,-0.704984345704104,
-0.701741053691342,-0.687720677828186,-0.681207476329301,-0.671410018653206,
-0.652269351415935,-0.640136953768839,-0.619305464344328,-0.599057470751597),
 .UNSPECIFIED.) ;
#788 = B_SPLINE_CURVE_WITH_KNOTS('',3,(#71848,#71849,#71850,#71851,#71852,
#71853,#71854,#71855,#71856,#71857,#71858,#71859,#71860,#71861,#71862),
 .UNSPECIFIED.,.F.,.F.,(4,1,1,1,1,1,1,1,1,1,1,1,4),(0.599057470748744,0.640127549392629,
0.681197628036513,0.701732667358455,0.712000187019426,0.722267706680398,
0.747936505832825,0.763337785324282,0.804407863968166,0.809541623798652,
0.814675383629137,0.84547794261205,0.886548021255935),.UNSPECIFIED.) ;
#789 = B_SPLINE_CURVE_WITH_KNOTS('',3,(#71964,#71965,#71966,#71967,#71968,
#71969,#71970,#71971,#71972,#71973,#71974,#71975,#71976,#71977,#71978,#71979,
#71980,#71981,#71982,#71983,#71984,#71985,#71986,#71987,#71988,#71989,#71990,
#71991,#71992,#71993,#71994,#71995,#71996,#71997,#71998,#71999,#72000,#72001,
#72002,#72003,#72004,#72005,#72006,#72007,#72008,#72009,#72010,#72011,#72012,
#72013,#72014,#72015,#72016,#72017,#72018,#72019,#72020,#72021,#72022,#72023,
#72024,#72025,#72026,#72027,#72028,#72029,#72030,#72031,#72032,#72033,#72034,
#72035,#72036,#72037,#72038,#72039,#72040,#72041,#72042,#72043,#72044,#72045,
#72046,#72047,#72048,#72049,#72050,#72051,#72052,#72053,#72054),
 .UNSPECIFIED.,.F.,.F.,(4,3,3,3,3,3,3,3,3,3,3,3,3,3,3,3,3,3,3,3,3,3,3,3,
3,3,3,3,3,3,4),(-1.15463223446653,-1.1341178340239,-1.12022883800639,-1.11360343358128,
-1.07254719690285,-1.05532975113685,-1.05201126806733,-1.04611234292978,
-1.04174078600302,-1.03146911237729,-1.02733004480818,-1.02513884232791,
-1.0228904427285,-1.01804576856663,-1.01603397735204,-1.01032624264144,
-1.00510701775925,-0.998953323245803,-0.99679388229667,-0.990336102906064,
-0.982532688656496,-0.980075180629686,-0.975907225267637,-0.969811398153971,
-0.950272727910358,-0.949277530134206,-0.926594479609855,-0.908211294032182,
-0.903665232052998,-0.873530848284397,-0.867143070669774),.UNSPECIFIED.) ;
#790 = B_SPLINE_CURVE_WITH_KNOTS('',3,(#72055,#72056,#72057,#72058,#72059,
#72060,#72061,#72062,#72063,#72064,#72065,#72066,#72067,#72068,#72069),
 .UNSPECIFIED.,.F.,.F.,(4,1,1,1,1,1,1,1,1,1,1,1,4),(0.867143070669756,0.908212951212153,
0.949282831754549,0.969817772025747,0.980085242161346,0.990352712296945,
1.01602138763594,1.03142259283934,1.04169006297494,1.05195753311054,1.07249247338174,
1.11356235392413,1.15463223446653),.UNSPECIFIED.) ;
#791 = B_SPLINE_CURVE_WITH_KNOTS('',3,(#72171,#72172,#72173,#72174,#72175,
#72176,#72177,#72178,#72179,#72180,#72181,#72182,#72183,#72184,#72185),
 .UNSPECIFIED.,.F.,.F.,(4,1,1,1,1,1,1,1,1,1,1,1,4),(-0.411832935461242,
-0.370762950184276,-0.329692964907306,-0.309157972268821,-0.298890475949579,
-0.288622979630336,-0.273221735151472,-0.247552994353366,-0.237285498034123,
-0.227018001714881,-0.206483009076396,-0.165413023799426,-0.124343038522472),
 .UNSPECIFIED.) ;
#792 = B_SPLINE_CURVE_WITH_KNOTS('',3,(#72186,#72187,#72188,#72189,#72190,
#72191,#72192,#72193,#72194,#72195,#72196,#72197,#72198,#72199,#72200),
 .UNSPECIFIED.,.F.,.F.,(4,1,1,1,1,1,1,1,1,1,1,1,4),(0.124343038522454,0.165413023799424,
0.206483009076393,0.227018001714878,0.23728549803412,0.247552994353363,
0.273221735151469,0.288622979630332,0.298890475949574,0.309157972268817,
0.329692964907302,0.370762950184271,0.41183293546124),.UNSPECIFIED.) ;
#793 = B_SPLINE_CURVE_WITH_KNOTS('',3,(#72296,#72297,#72298,#72299,#72300,
#72301,#72302,#72303,#72304,#72305,#72306,#72307,#72308,#72309,#72310,#72311,
#72312,#72313,#72314,#72315,#72316,#72317,#72318,#72319,#72320,#72321,#72322,
#72323,#72324,#72325,#72326,#72327,#72328,#72329,#72330,#72331,#72332,#72333,
#72334,#72335,#72336,#72337,#72338,#72339,#72340,#72341,#72342,#72343,#72344,
#72345,#72346,#72347,#72348,#72349,#72350,#72351,#72352,#72353,#72354,#72355,
#72356,#72357,#72358,#72359,#72360,#72361,#72362,#72363,#72364,#72365,#72366,
#72367,#72368,#72369,#72370,#72371,#72372,#72373,#72374,#72375,#72376,#72377,
#72378,#72379,#72380,#72381,#72382,#72383),.UNSPECIFIED.,.F.,.F.,(4,3,3,
3,3,3,3,3,3,3,3,3,3,3,3,3,3,3,3,3,3,3,3,3,3,3,3,3,3,4),(-0.477703831735207,
-0.453614605110258,-0.443230345021846,-0.436675004882822,-0.395618787860206,
-0.378433001370195,-0.375082879002063,-0.364812392178865,-0.354540709068515,
-0.350401876328947,-0.348213627724221,-0.34440122597587,-0.339813935131242,
-0.339105559341817,-0.333397652452776,-0.328177881844085,-0.322023624791636,
-0.319864746381504,-0.313407649569444,-0.305604236787224,-0.303146716277064,
-0.298978089352453,-0.29288292803837,-0.273343591995163,-0.272349038216806,
-0.249678142342238,-0.231282783565101,-0.226736096137766,-0.196808788304168,
-0.190214667976269),.UNSPECIFIED.) ;
#794 = B_SPLINE_CURVE_WITH_KNOTS('',3,(#72384,#72385,#72386,#72387,#72388,
#72389,#72390,#72391,#72392,#72393,#72394,#72395,#72396,#72397,#72398),
 .UNSPECIFIED.,.F.,.F.,(4,1,1,1,1,1,1,1,1,1,1,1,4),(0.19021466797625,0.231284548513244,
0.272354429050238,0.292889369318735,0.303156839452983,0.313424309587232,
0.339092984922853,0.354494190124226,0.364761660258474,0.375029130392723,
0.395564070661219,0.436633951198213,0.477703831735207),.UNSPECIFIED.) ;
#795 = B_SPLINE_CURVE_WITH_KNOTS('',3,(#72404,#72405,#72406,#72407,#72408,
#72409,#72410,#72411,#72412,#72413,#72414,#72415,#72416,#72417),
 .UNSPECIFIED.,.F.,.F.,(4,2,2,2,2,2,4),(-0.000285103889769581,0.,0.00872930952732865,
0.0170606390707464,0.0258600808710477,0.0324403480688856,0.0341876342319972),
 .UNSPECIFIED.) ;
#796 = B_SPLINE_CURVE_WITH_KNOTS('',3,(#72421,#72422,#72423,#72424,#72425,
#72426,#72427,#72428,#72429,#72430,#72431,#72432),.UNSPECIFIED.,.F.,.F.,
(4,2,2,2,2,4),(0.,0.00612475744370298,0.0140348469016774,0.0236318332037711,
0.0338613775546519,0.0341436529593686),.UNSPECIFIED.) ;
#797 = B_SPLINE_CURVE_WITH_KNOTS('',3,(#72503,#72504,#72505,#72506,#72507,
#72508,#72509,#72510,#72511,#72512,#72513,#72514,#72515,#72516,#72517,#72518,
#72519,#72520,#72521,#72522,#72523,#72524,#72525,#72526,#72527,#72528,#72529,
#72530,#72531,#72532,#72533,#72534,#72535,#72536,#72537,#72538,#72539,#72540,
#72541,#72542,#72543,#72544,#72545,#72546,#72547,#72548,#72549,#72550,#72551,
#72552,#72553,#72554,#72555,#72556,#72557,#72558,#72559,#72560,#72561,#72562,
#72563,#72564,#72565,#72566,#72567,#72568,#72569,#72570,#72571,#72572,#72573,
#72574,#72575,#72576,#72577,#72578,#72579,#72580,#72581,#72582,#72583,#72584,
#72585,#72586,#72587,#72588,#72589,#72590,#72591,#72592,#72593,#72594,#72595,
#72596,#72597,#72598,#72599,#72600,#72601,#72602,#72603,#72604,#72605,#72606,
#72607,#72608,#72609,#72610,#72611,#72612,#72613,#72614),.UNSPECIFIED.,
 .F.,.F.,(4,3,3,3,3,3,3,3,3,3,3,3,3,3,3,3,3,3,3,3,3,3,3,3,3,3,3,3,3,3,3,
3,3,3,3,3,3,4),(-0.886548021255927,-0.863182140298643,-0.850026819726694,
-0.845485034834745,-0.828030597997826,-0.823995246256633,-0.807954076785211,
-0.804397382367369,-0.803419323869412,-0.789454447123549,-0.78719953786741,
-0.783854574530306,-0.777784826512168,-0.768895955447484,-0.763303798695202,
-0.756898169483172,-0.749793713751161,-0.748585034020601,-0.74223297709638,
-0.736710121550931,-0.736337056382528,-0.732525933237352,-0.727476816747137,
-0.722225326154133,-0.714703999684171,-0.7119635411798,-0.704984345704188,
-0.70169442338794,-0.687771632725246,-0.681167700475735,-0.671410018653332,
-0.660643601956556,-0.641874291222971,-0.639974533150539,-0.620382689790686,
-0.619305464344523,-0.602967164401198,-0.599057470751627),.UNSPECIFIED.) ;
#798 = B_SPLINE_CURVE_WITH_KNOTS('',3,(#72615,#72616,#72617,#72618,#72619,
#72620,#72621,#72622,#72623,#72624,#72625,#72626,#72627,#72628),
 .UNSPECIFIED.,.F.,.F.,(4,1,1,1,1,1,1,1,1,1,1,4),(0.599057470748752,0.660662588714575,
0.681197628036517,0.701732667358458,0.712000187019428,0.722267706680399,
0.732535226341369,0.763337785324281,0.783872824646222,0.804407863968163,
0.845477942612046,0.886548021255928),.UNSPECIFIED.) ;
#799 = B_SPLINE_CURVE_WITH_KNOTS('',3,(#72632,#72633,#72634,#72635,#72636,
#72637,#72638,#72639,#72640,#72641,#72642,#72643),.UNSPECIFIED.,.F.,.F.,
(4,2,2,2,2,4),(0.,0.00612475744371704,0.0140348469017579,0.0236318332042238,
0.0338613775553621,0.0341436529609325),.UNSPECIFIED.) ;
#800 = B_SPLINE_CURVE_WITH_KNOTS('',3,(#72646,#72647,#72648,#72649,#72650,
#72651),.UNSPECIFIED.,.F.,.F.,(4,2,4),(0.027568167455487,0.0309707637796999,
0.0317834882745698),.UNSPECIFIED.) ;
#801 = B_SPLINE_CURVE_WITH_KNOTS('',3,(#72654,#72655,#72656,#72657,#72658,
#72659),.UNSPECIFIED.,.F.,.F.,(4,2,4),(0.0987440670458636,0.10214723221737,
0.102957912597527),.UNSPECIFIED.) ;
#802 = B_SPLINE_CURVE_WITH_KNOTS('',3,(#72663,#72664,#72665,#72666,#72667,
#72668,#72669,#72670,#72671,#72672,#72673,#72674,#72675,#72676),
 .UNSPECIFIED.,.F.,.F.,(4,2,2,2,2,2,4),(-0.000285103882378192,0.,0.00872930953448812,
0.0170606390834788,0.0258600808806183,0.0324403480767969,0.0341876342336229),
 .UNSPECIFIED.) ;
#803 = B_SPLINE_CURVE_WITH_KNOTS('',3,(#72682,#72683,#72684,#72685,#72686,
#72687,#72688,#72689,#72690,#72691,#72692,#72693,#72694,#72695),
 .UNSPECIFIED.,.F.,.F.,(4,2,2,2,2,2,4),(-0.000285103883943185,2.27041150636931E-14,
0.00872930953329209,0.0170606390813087,0.0258600808790012,0.0324403480754976,
0.0341876342333561),.UNSPECIFIED.) ;
#804 = B_SPLINE_CURVE_WITH_KNOTS('',3,(#72698,#72699,#72700,#72701,#72702,
#72703),.UNSPECIFIED.,.F.,.F.,(4,2,4),(0.0275681674553535,0.0309707637795716,
0.0317834882743947),.UNSPECIFIED.) ;
#805 = B_SPLINE_CURVE_WITH_KNOTS('',3,(#72706,#72707,#72708,#72709,#72710,
#72711),.UNSPECIFIED.,.F.,.F.,(4,2,4),(0.0987440670452405,0.102147232216738,
0.102957912596903),.UNSPECIFIED.) ;
#806 = B_SPLINE_CURVE_WITH_KNOTS('',3,(#72715,#72716,#72717,#72718,#72719,
#72720,#72721,#72722,#72723,#72724,#72725,#72726),.UNSPECIFIED.,.F.,.F.,
(4,2,2,2,2,4),(0.,0.00612475744371102,0.0140348469017037,0.0236318332038197,
0.0338613775547199,0.0341436529588805),.UNSPECIFIED.) ;
#807 = B_SPLINE_CURVE_WITH_KNOTS('',3,(#72729,#72730,#72731,#72732,#72733,
#72734),.UNSPECIFIED.,.F.,.F.,(4,2,4),(0.0275681674555189,0.0309707637797563,
0.0317834882746156),.UNSPECIFIED.) ;
#808 = B_SPLINE_CURVE_WITH_KNOTS('',3,(#72737,#72738,#72739,#72740,#72741,
#72742),.UNSPECIFIED.,.F.,.F.,(4,2,4),(0.0987440670463347,0.102147232217918,
0.102957912598071),.UNSPECIFIED.) ;
#809 = B_SPLINE_CURVE_WITH_KNOTS('',3,(#72813,#72814,#72815,#72816,#72817,
#72818,#72819,#72820,#72821,#72822,#72823,#72824,#72825,#72826,#72827,#72828,
#72829,#72830,#72831,#72832,#72833,#72834,#72835,#72836,#72837,#72838,#72839,
#72840,#72841,#72842,#72843,#72844,#72845,#72846,#72847,#72848,#72849,#72850,
#72851,#72852,#72853,#72854,#72855,#72856,#72857,#72858,#72859,#72860,#72861,
#72862,#72863,#72864,#72865,#72866,#72867,#72868,#72869,#72870,#72871,#72872,
#72873,#72874,#72875,#72876,#72877,#72878,#72879,#72880,#72881,#72882,#72883,
#72884,#72885,#72886,#72887,#72888,#72889,#72890,#72891,#72892,#72893,#72894,
#72895,#72896,#72897,#72898,#72899,#72900,#72901,#72902,#72903,#72904,#72905,
#72906,#72907,#72908,#72909,#72910,#72911,#72912,#72913,#72914,#72915,#72916,
#72917,#72918,#72919,#72920,#72921,#72922,#72923,#72924),.UNSPECIFIED.,
 .F.,.F.,(4,3,3,3,3,3,3,3,3,3,3,3,3,3,3,3,3,3,3,3,3,3,3,3,3,3,3,3,3,3,3,
3,3,3,3,3,3,4),(-0.886548021255915,-0.863182183022991,-0.850026819726918,
-0.845485033904693,-0.828030709545769,-0.823993850862195,-0.807952761446644,
-0.804397379038152,-0.803419323869518,-0.789454453599431,-0.78719888115785,
-0.783854569044938,-0.777784826512226,-0.768895988020034,-0.763303790457395,
-0.756898169483171,-0.749793571369931,-0.748585034020596,-0.742232977096394,
-0.73671041200043,-0.736337056382546,-0.732525922194933,-0.727476816747194,
-0.722225315602094,-0.714704063959347,-0.711963531357458,-0.704984345704372,
-0.701694414342138,-0.687771578704614,-0.681167693161271,-0.671410018653635,
-0.66064359619164,-0.641874296603296,-0.639974530268315,-0.62038268997317,
-0.61930546434499,-0.602967220633359,-0.599057470751585),.UNSPECIFIED.) ;
#810 = B_SPLINE_CURVE_WITH_KNOTS('',3,(#72925,#72926,#72927,#72928,#72929,
#72930,#72931,#72932,#72933,#72934,#72935,#72936,#72937,#72938),
 .UNSPECIFIED.,.F.,.F.,(4,1,1,1,1,1,1,1,1,1,1,4),(0.599057470748733,0.660662588714558,
0.681197628036499,0.701732667358441,0.712000187019412,0.722267706680383,
0.732535226341354,0.763337785324266,0.783872824646208,0.804407863968149,
0.845477942612033,0.886548021255916),.UNSPECIFIED.) ;
#811 = B_SPLINE_CURVE_WITH_KNOTS('',3,(#72942,#72943,#72944,#72945,#72946,
#72947,#72948,#72949,#72950,#72951,#72952,#72953),.UNSPECIFIED.,.F.,.F.,
(4,2,2,2,2,4),(0.,0.00612475744370553,0.0140348469016906,0.0236318332038693,
0.0338613775548128,0.0341436529592063),.UNSPECIFIED.) ;
#812 = B_SPLINE_CURVE_WITH_KNOTS('',3,(#72957,#72958,#72959,#72960,#72961,
#72962,#72963,#72964,#72965,#72966,#72967,#72968,#72969,#72970),
 .UNSPECIFIED.,.F.,.F.,(4,2,2,2,2,2,4),(-0.000285103891090118,0.,0.00872930952749538,
0.0170606390711773,0.0258600808714152,0.0324403480692667,0.0341876342322289),
 .UNSPECIFIED.) ;
#813 = B_SPLINE_CURVE_WITH_KNOTS('',3,(#72976,#72977,#72978,#72979,#72980,
#72981,#72982,#72983,#72984,#72985,#72986,#72987,#72988,#72989),
 .UNSPECIFIED.,.F.,.F.,(4,2,2,2,2,2,4),(-0.000285103883294333,0.,0.00872930953430471,
0.0170606390832003,0.0258600808804658,0.0324403480767586,0.0341876342335693),
 .UNSPECIFIED.) ;
#814 = B_SPLINE_CURVE_WITH_KNOTS('',3,(#72992,#72993,#72994,#72995,#72996,
#72997),.UNSPECIFIED.,.F.,.F.,(4,2,4),(0.0275681674553505,0.030970763779561,
0.0317834882744106),.UNSPECIFIED.) ;
#815 = B_SPLINE_CURVE_WITH_KNOTS('',3,(#73000,#73001,#73002,#73003,#73004,
#73005),.UNSPECIFIED.,.F.,.F.,(4,2,4),(0.0987440670468542,0.102147232218389,
0.102957912598554),.UNSPECIFIED.) ;
#816 = B_SPLINE_CURVE_WITH_KNOTS('',3,(#73009,#73010,#73011,#73012,#73013,
#73014,#73015,#73016,#73017,#73018,#73019,#73020),.UNSPECIFIED.,.F.,.F.,
(4,2,2,2,2,4),(0.,0.0061247574437008,0.0140348469016623,0.0236318332037904,
0.0338613775546856,0.0341436529591702),.UNSPECIFIED.) ;
#817 = B_SPLINE_CURVE_WITH_KNOTS('',3,(#73023,#73024,#73025,#73026,#73027,
#73028),.UNSPECIFIED.,.F.,.F.,(4,2,4),(0.0275681674553572,0.0309707637795828,
0.0317834882744022),.UNSPECIFIED.) ;
#818 = B_SPLINE_CURVE_WITH_KNOTS('',3,(#73031,#73032,#73033,#73034,#73035,
#73036),.UNSPECIFIED.,.F.,.F.,(4,2,4),(0.0987440670462714,0.102147232217851,
0.102957912597979),.UNSPECIFIED.) ;
#819 = B_SPLINE_CURVE_WITH_KNOTS('',3,(#73112,#73113,#73114,#73115,#73116,
#73117,#73118,#73119,#73120,#73121,#73122,#73123,#73124,#73125,#73126),
 .UNSPECIFIED.,.F.,.F.,(4,1,1,1,1,1,1,1,1,1,1,1,4),(-1.1546322344665,-1.11356235393268,
-1.07249247339886,-1.05195753313195,-1.03142259286504,-1.02115512273159,
-1.01088765259813,-1.00062018246467,-0.99035271233122,-0.969817772064309,
-0.949282831797399,-0.908212951263578,-0.867143070729775),.UNSPECIFIED.) ;
#820 = B_SPLINE_CURVE_WITH_KNOTS('',3,(#73127,#73128,#73129,#73130,#73131,
#73132,#73133,#73134,#73135,#73136,#73137,#73138,#73139,#73140,#73141,#73142,
#73143,#73144,#73145,#73146,#73147,#73148,#73149,#73150,#73151,#73152,#73153,
#73154,#73155,#73156,#73157,#73158,#73159,#73160,#73161,#73162,#73163,#73164,
#73165,#73166,#73167,#73168,#73169,#73170,#73171,#73172,#73173,#73174,#73175,
#73176,#73177,#73178,#73179,#73180,#73181,#73182,#73183,#73184,#73185,#73186,
#73187,#73188,#73189,#73190,#73191,#73192,#73193,#73194,#73195,#73196,#73197,
#73198,#73199,#73200,#73201,#73202,#73203,#73204,#73205,#73206,#73207,#73208,
#73209,#73210,#73211,#73212,#73213,#73214,#73215,#73216,#73217,#73218,#73219,
#73220,#73221,#73222,#73223,#73224,#73225,#73226,#73227,#73228,#73229),
 .UNSPECIFIED.,.F.,.F.,(4,3,3,3,3,3,3,3,3,3,3,3,3,3,3,3,3,3,3,3,3,3,3,3,
3,3,3,3,3,3,3,3,3,3,4),(0.86714307073025,0.883480214507125,0.899207563799762,
0.908212951263578,0.920868221979847,0.933172739853617,0.944935995976013,
0.949282831797399,0.959550301930854,0.968956551813585,0.969817772064309,
0.979310938211651,0.988375034947783,0.99035271233122,0.997960594527763,
1.00062018246467,1.0069704296549,1.01088765259813,1.01719943327265,1.02115512273159,
1.02883039102215,1.03142259286504,1.04051400057577,1.05002380913911,1.05195753313195,
1.06134071109721,1.07113605430996,1.07249247339886,1.08434800851963,1.09656739803681,
1.10928297864463,1.11356235393268,1.12919557822945,1.14545138845601,1.15463223446606),
 .UNSPECIFIED.) ;
#821 = B_SPLINE_CURVE_WITH_KNOTS('',3,(#73233,#73234,#73235,#73236,#73237,
#73238,#73239,#73240,#73241,#73242,#73243,#73244),.UNSPECIFIED.,.F.,.F.,
(4,2,2,2,2,4),(0.,0.00612475744371958,0.0140348469017581,0.0236318332039418,
0.0338613775548876,0.034143652959597),.UNSPECIFIED.) ;
#822 = B_SPLINE_CURVE_WITH_KNOTS('',3,(#73248,#73249,#73250,#73251,#73252,
#73253,#73254,#73255,#73256,#73257,#73258,#73259,#73260,#73261),
 .UNSPECIFIED.,.F.,.F.,(4,2,2,2,2,2,4),(-0.000285103884839838,0.,0.00872930953208846,
0.0170606390791463,0.0258600808772505,0.0324403480739367,0.0341876342326163),
 .UNSPECIFIED.) ;
#823 = B_SPLINE_CURVE_WITH_KNOTS('',3,(#73267,#73268,#73269,#73270,#73271,
#73272,#73273,#73274,#73275,#73276,#73277,#73278,#73279,#73280),
 .UNSPECIFIED.,.F.,.F.,(4,2,2,2,2,2,4),(-0.000285103882893919,6.72676974886044E-15,
0.00872930953393735,0.017060639082469,0.0258600808798638,0.032440348076175,
0.0341876342333578),.UNSPECIFIED.) ;
#824 = B_SPLINE_CURVE_WITH_KNOTS('',3,(#73283,#73284,#73285,#73286,#73287,
#73288),.UNSPECIFIED.,.F.,.F.,(4,2,4),(0.0275681674553702,0.0309707637796163,
0.0317834882744124),.UNSPECIFIED.) ;
#825 = B_SPLINE_CURVE_WITH_KNOTS('',3,(#73291,#73292,#73293,#73294,#73295,
#73296),.UNSPECIFIED.,.F.,.F.,(4,2,4),(0.0987440670462461,0.102147232217778,
0.102957912597939),.UNSPECIFIED.) ;
#826 = B_SPLINE_CURVE_WITH_KNOTS('',3,(#73300,#73301,#73302,#73303,#73304,
#73305,#73306,#73307,#73308,#73309,#73310,#73311),.UNSPECIFIED.,.F.,.F.,
(4,2,2,2,2,4),(0.,0.00612475744372758,0.0140348469017917,0.0236318332039519,
0.0338613775547788,0.0341436529598709),.UNSPECIFIED.) ;
#827 = B_SPLINE_CURVE_WITH_KNOTS('',3,(#73314,#73315,#73316,#73317,#73318,
#73319),.UNSPECIFIED.,.F.,.F.,(4,2,4),(0.0275681674553604,0.0309707637795872,
0.0317834882744037),.UNSPECIFIED.) ;
#828 = B_SPLINE_CURVE_WITH_KNOTS('',3,(#73322,#73323,#73324,#73325,#73326,
#73327),.UNSPECIFIED.,.F.,.F.,(4,2,4),(0.0987440670453332,0.102147232216817,
0.102957912596973),.UNSPECIFIED.) ;
#829 = B_SPLINE_CURVE_WITH_KNOTS('',3,(#73403,#73404,#73405,#73406,#73407,
#73408,#73409,#73410,#73411,#73412,#73413,#73414,#73415,#73416,#73417),
 .UNSPECIFIED.,.F.,.F.,(4,1,1,1,1,1,1,1,1,1,1,1,4),(-0.411832935461112,
-0.37076295018414,-0.329692964907169,-0.309157972268683,-0.298890475949441,
-0.288622979630198,-0.262954238832091,-0.247552994353227,-0.237285498033984,
-0.227018001714741,-0.206483009076255,-0.165413023799284,-0.124343038522328),
 .UNSPECIFIED.) ;
#830 = B_SPLINE_CURVE_WITH_KNOTS('',3,(#73418,#73419,#73420,#73421,#73422,
#73423,#73424,#73425,#73426,#73427,#73428,#73429,#73430,#73431,#73432),
 .UNSPECIFIED.,.F.,.F.,(4,1,1,1,1,1,1,1,1,1,1,1,4),(0.124343038522312,0.165413023799283,
0.206483009076254,0.22701800171474,0.237285498033983,0.247552994353225,
0.26295423883209,0.288622979630197,0.29889047594944,0.309157972268682,0.329692964907168,
0.370762950184139,0.411832935461111),.UNSPECIFIED.) ;
#831 = B_SPLINE_CURVE_WITH_KNOTS('',3,(#73436,#73437,#73438,#73439,#73440,
#73441,#73442,#73443,#73444,#73445,#73446,#73447),.UNSPECIFIED.,.F.,.F.,
(4,2,2,2,2,4),(0.,0.00612475744370097,0.0140348469016502,0.0236318332037224,
0.0338613775545817,0.0341436529591511),.UNSPECIFIED.) ;
#832 = B_SPLINE_CURVE_WITH_KNOTS('',3,(#73451,#73452,#73453,#73454,#73455,
#73456,#73457,#73458,#73459,#73460,#73461,#73462,#73463,#73464),
 .UNSPECIFIED.,.F.,.F.,(4,2,2,2,2,2,4),(-0.00028510389012683,2.52045563239878E-14,
0.00872930952634134,0.0170606390690788,0.0258600808700429,0.0324403480682151,
0.0341876342326173),.UNSPECIFIED.) ;
#833 = B_SPLINE_CURVE_WITH_KNOTS('',3,(#73470,#73471,#73472,#73473,#73474,
#73475,#73476,#73477,#73478,#73479,#73480,#73481,#73482,#73483),
 .UNSPECIFIED.,.F.,.F.,(4,2,2,2,2,2,4),(-0.000285103881470846,0.,0.00872930953485893,
0.0170606390840687,0.0258600808810181,0.032440348077114,0.0341876342334867),
 .UNSPECIFIED.) ;
#834 = B_SPLINE_CURVE_WITH_KNOTS('',3,(#73486,#73487,#73488,#73489,#73490,
#73491),.UNSPECIFIED.,.F.,.F.,(4,2,4),(0.0275681674553353,0.030970763779553,
0.0317834882743904),.UNSPECIFIED.) ;
#835 = B_SPLINE_CURVE_WITH_KNOTS('',3,(#73494,#73495,#73496,#73497,#73498,
#73499),.UNSPECIFIED.,.F.,.F.,(4,2,4),(0.0987440670457375,0.10214723221726,
0.102957912597412),.UNSPECIFIED.) ;
#836 = B_SPLINE_CURVE_WITH_KNOTS('',3,(#73503,#73504,#73505,#73506,#73507,
#73508,#73509,#73510,#73511,#73512,#73513,#73514),.UNSPECIFIED.,.F.,.F.,
(4,2,2,2,2,4),(0.,0.00612475744369581,0.014034846901649,0.0236318332038529,
0.0338613775546785,0.0341436529596609),.UNSPECIFIED.) ;
#837 = B_SPLINE_CURVE_WITH_KNOTS('',3,(#73517,#73518,#73519,#73520,#73521,
#73522),.UNSPECIFIED.,.F.,.F.,(4,2,4),(0.0275681674554589,0.0309707637797025,
0.0317834882745042),.UNSPECIFIED.) ;
#838 = B_SPLINE_CURVE_WITH_KNOTS('',3,(#73525,#73526,#73527,#73528,#73529,
#73530),.UNSPECIFIED.,.F.,.F.,(4,2,4),(0.098744067045831,0.102147232217366,
0.102957912597521),.UNSPECIFIED.) ;
#839 = B_SPLINE_CURVE_WITH_KNOTS('',3,(#73606,#73607,#73608,#73609,#73610,
#73611,#73612,#73613,#73614,#73615,#73616,#73617,#73618,#73619,#73620,#73621,
#73622,#73623,#73624,#73625,#73626,#73627,#73628,#73629,#73630,#73631,#73632,
#73633,#73634,#73635,#73636,#73637,#73638,#73639,#73640,#73641,#73642,#73643,
#73644,#73645,#73646,#73647,#73648,#73649,#73650,#73651,#73652,#73653,#73654,
#73655,#73656,#73657,#73658,#73659,#73660,#73661,#73662,#73663,#73664,#73665,
#73666,#73667,#73668,#73669,#73670,#73671,#73672,#73673,#73674,#73675,#73676,
#73677,#73678,#73679,#73680,#73681,#73682,#73683,#73684,#73685,#73686,#73687,
#73688,#73689,#73690,#73691,#73692,#73693),.UNSPECIFIED.,.F.,.F.,(4,3,3,
3,3,3,3,3,3,3,3,3,3,3,3,3,3,3,3,3,3,3,3,3,3,3,3,3,3,4),(-0.477703831735363,
-0.45718942947788,-0.443230571702975,-0.436675027220398,-0.395618819134948,
-0.378433420479109,-0.375082910242375,-0.364812420917539,-0.354540733105092,
-0.350401894405927,-0.348213670695578,-0.345961980835223,-0.341117222395463,
-0.339105573036344,-0.333397647574564,-0.328177881844221,-0.322023234625397,
-0.319864746381625,-0.31340764305829,-0.30560393863315,-0.303146705918973,
-0.298978089352453,-0.292882915418747,-0.273343591995043,-0.272349024384765,
-0.249678001030715,-0.231282775402659,-0.226736096137401,-0.196809892828657,
-0.190214667987186),.UNSPECIFIED.) ;
#840 = B_SPLINE_CURVE_WITH_KNOTS('',3,(#73694,#73695,#73696,#73697,#73698,
#73699,#73700,#73701,#73702,#73703,#73704,#73705,#73706,#73707,#73708),
 .UNSPECIFIED.,.F.,.F.,(4,1,1,1,1,1,1,1,1,1,1,1,4),(0.19021466798717,0.231284548522626,
0.272354429058083,0.292889369325811,0.303156839459675,0.313424309593539,
0.339092984928199,0.354494190128995,0.364761660262859,0.375029130396723,
0.395564070664451,0.436633951199908,0.477703831735364),.UNSPECIFIED.) ;
#841 = B_SPLINE_CURVE_WITH_KNOTS('',3,(#73712,#73713,#73714,#73715,#73716,
#73717,#73718,#73719,#73720,#73721,#73722,#73723),.UNSPECIFIED.,.F.,.F.,
(4,2,2,2,2,4),(0.,0.0061247574437173,0.0140348469017339,0.0236318332039063,
0.0338613775548282,0.0341436529591761),.UNSPECIFIED.) ;
#842 = B_SPLINE_CURVE_WITH_KNOTS('',3,(#73727,#73728,#73729,#73730,#73731,
#73732,#73733,#73734,#73735,#73736,#73737,#73738,#73739,#73740),
 .UNSPECIFIED.,.F.,.F.,(4,2,2,2,2,2,4),(-0.000285103881352186,0.,0.00872930953547832,
0.0170606390851658,0.0258600808817554,0.0324403480776579,0.0341876342332736),
 .UNSPECIFIED.) ;
#843 = B_SPLINE_CURVE_WITH_KNOTS('',3,(#73746,#73747,#73748,#73749,#73750,
#73751,#73752,#73753,#73754,#73755,#73756,#73757,#73758,#73759),
 .UNSPECIFIED.,.F.,.F.,(4,2,2,2,2,2,4),(-0.000285103880786882,0.,0.00872930953571026,
0.0170606390855883,0.025860080882109,0.0324403480779487,0.034187634233573),
 .UNSPECIFIED.) ;
#844 = B_SPLINE_CURVE_WITH_KNOTS('',3,(#73762,#73763,#73764,#73765,#73766,
#73767),.UNSPECIFIED.,.F.,.F.,(4,2,4),(0.0275681674553793,0.0309707637795965,
0.0317834882744089),.UNSPECIFIED.) ;
#845 = B_SPLINE_CURVE_WITH_KNOTS('',3,(#73770,#73771,#73772,#73773,#73774,
#73775),.UNSPECIFIED.,.F.,.F.,(4,2,4),(0.0987440670459561,0.102147232217522,
0.102957912597634),.UNSPECIFIED.) ;
#846 = B_SPLINE_CURVE_WITH_KNOTS('',3,(#73779,#73780,#73781,#73782,#73783,
#73784,#73785,#73786,#73787,#73788,#73789,#73790),.UNSPECIFIED.,.F.,.F.,
(4,2,2,2,2,4),(0.,0.00612475744370604,0.0140348469017081,0.0236318332039229,
0.0338613775549312,0.0341436529594248),.UNSPECIFIED.) ;
#847 = B_SPLINE_CURVE_WITH_KNOTS('',3,(#73793,#73794,#73795,#73796,#73797,
#73798),.UNSPECIFIED.,.F.,.F.,(4,2,4),(0.0275681674554173,0.0309707637796397,
0.0317834882744546),.UNSPECIFIED.) ;
#848 = B_SPLINE_CURVE_WITH_KNOTS('',3,(#73801,#73802,#73803,#73804,#73805,
#73806),.UNSPECIFIED.,.F.,.F.,(4,2,4),(0.0987440670461074,0.102147232217608,
0.10295791259778),.UNSPECIFIED.) ;
#849 = B_SPLINE_CURVE_WITH_KNOTS('',3,(#73882,#73883,#73884,#73885,#73886,
#73887,#73888,#73889,#73890,#73891,#73892,#73893,#73894,#73895,#73896,#73897,
#73898,#73899,#73900,#73901,#73902,#73903,#73904,#73905,#73906,#73907,#73908,
#73909,#73910,#73911,#73912,#73913,#73914,#73915,#73916,#73917,#73918,#73919,
#73920,#73921,#73922,#73923,#73924,#73925,#73926,#73927,#73928,#73929,#73930,
#73931,#73932,#73933,#73934,#73935,#73936,#73937,#73938,#73939,#73940,#73941,
#73942,#73943,#73944,#73945,#73946,#73947,#73948,#73949,#73950,#73951,#73952,
#73953,#73954,#73955,#73956,#73957,#73958,#73959,#73960,#73961,#73962,#73963,
#73964,#73965,#73966,#73967,#73968,#73969,#73970,#73971,#73972,#73973,#73974,
#73975,#73976,#73977,#73978,#73979,#73980,#73981,#73982,#73983,#73984),
 .UNSPECIFIED.,.F.,.F.,(4,3,3,3,3,3,3,3,3,3,3,3,3,3,3,3,3,3,3,3,3,3,3,3,
3,3,3,3,3,3,3,3,3,3,4),(-0.886548021255922,-0.855653870250158,-0.85002681972678,
-0.845470505946487,-0.822368676399289,-0.804396442083867,-0.803419323869455,
-0.783862639207905,-0.777784826512195,-0.773600413563503,-0.765740334199066,
-0.763343542875113,-0.756898169483182,-0.750967673087341,-0.748585034020608,
-0.742943881897718,-0.742232977096396,-0.737660156503543,-0.73633705638255,
-0.730852789241292,-0.727476816747186,-0.722234803402179,-0.714862413628147,
-0.70697932438281,-0.704984345704348,-0.69423844792319,-0.682180041289652,
-0.681161690517635,-0.676013453381874,-0.67141001865358,-0.670871987902952,
-0.64753741444397,-0.64008354109392,-0.619305464344901,-0.599057470751608),
 .UNSPECIFIED.) ;
#850 = B_SPLINE_CURVE_WITH_KNOTS('',3,(#73985,#73986,#73987,#73988,#73989,
#73990,#73991,#73992,#73993,#73994,#73995,#73996,#73997,#73998,#73999),
 .UNSPECIFIED.,.F.,.F.,(4,1,1,1,1,1,1,1,1,1,1,1,4),(0.599057470748756,0.640127549392637,
0.670930108375547,0.676063868206032,0.681197628036518,0.722267706680398,
0.737668986171854,0.763337785324279,0.77360530498525,0.78387282464622,0.80440786396816,
0.845477942612041,0.886548021255922),.UNSPECIFIED.) ;
#851 = B_SPLINE_CURVE_WITH_KNOTS('',3,(#74003,#74004,#74005,#74006,#74007,
#74008,#74009,#74010,#74011,#74012,#74013,#74014),.UNSPECIFIED.,.F.,.F.,
(4,2,2,2,2,4),(0.,0.00612475744371223,0.0140348469017155,0.0236318332039426,
0.0338613775549202,0.0341436529594837),.UNSPECIFIED.) ;
#852 = B_SPLINE_CURVE_WITH_KNOTS('',3,(#74018,#74019,#74020,#74021,#74022,
#74023,#74024,#74025,#74026,#74027,#74028,#74029,#74030,#74031),
 .UNSPECIFIED.,.F.,.F.,(4,2,2,2,2,2,4),(-0.000285103883765505,0.,0.00872930953291526,
0.0170606390807207,0.0258600808785664,0.0324403480751399,0.0341876342333296),
 .UNSPECIFIED.) ;
#853 = B_SPLINE_CURVE_WITH_KNOTS('',3,(#74037,#74038,#74039,#74040,#74041,
#74042,#74043,#74044,#74045,#74046,#74047,#74048,#74049,#74050),
 .UNSPECIFIED.,.F.,.F.,(4,2,2,2,2,2,4),(-0.000285103876031147,0.,0.00872930954136664,
0.0170606390955509,0.0258600808893367,0.0324403480837712,0.0341876342338359),
 .UNSPECIFIED.) ;
#854 = B_SPLINE_CURVE_WITH_KNOTS('',3,(#74053,#74054,#74055,#74056,#74057,
#74058),.UNSPECIFIED.,.F.,.F.,(4,2,4),(0.0275681674554096,0.0309707637796443,
0.0317834882744809),.UNSPECIFIED.) ;
#855 = B_SPLINE_CURVE_WITH_KNOTS('',3,(#74061,#74062,#74063,#74064,#74065,
#74066),.UNSPECIFIED.,.F.,.F.,(4,2,4),(0.0987440670458425,0.102147232217394,
0.102957912597541),.UNSPECIFIED.) ;
#856 = B_SPLINE_CURVE_WITH_KNOTS('',3,(#74070,#74071,#74072,#74073,#74074,
#74075,#74076,#74077,#74078,#74079,#74080,#74081),.UNSPECIFIED.,.F.,.F.,
(4,2,2,2,2,4),(0.,0.00612475744370653,0.014034846901692,0.0236318332038886,
0.0338613775548516,0.0341436529594063),.UNSPECIFIED.) ;
#857 = B_SPLINE_CURVE_WITH_KNOTS('',3,(#74084,#74085,#74086,#74087,#74088,
#74089),.UNSPECIFIED.,.F.,.F.,(4,2,4),(0.0275681674553618,0.0309707637795795,
0.0317834882744105),.UNSPECIFIED.) ;
#858 = B_SPLINE_CURVE_WITH_KNOTS('',3,(#74092,#74093,#74094,#74095,#74096,
#74097),.UNSPECIFIED.,.F.,.F.,(4,2,4),(0.0987440670458198,0.102147232217339,
0.102957912597487),.UNSPECIFIED.) ;
#859 = B_SPLINE_CURVE_WITH_KNOTS('',3,(#74168,#74169,#74170,#74171,#74172,
#74173,#74174,#74175,#74176,#74177,#74178,#74179,#74180,#74181,#74182,#74183,
#74184,#74185,#74186,#74187,#74188,#74189,#74190,#74191,#74192,#74193,#74194,
#74195,#74196,#74197,#74198,#74199,#74200,#74201,#74202,#74203,#74204,#74205,
#74206,#74207,#74208,#74209,#74210,#74211,#74212,#74213,#74214,#74215,#74216,
#74217,#74218,#74219,#74220,#74221,#74222,#74223,#74224,#74225,#74226,#74227,
#74228,#74229,#74230,#74231,#74232,#74233,#74234,#74235,#74236,#74237,#74238,
#74239,#74240,#74241,#74242,#74243,#74244,#74245,#74246,#74247,#74248,#74249,
#74250,#74251,#74252,#74253,#74254,#74255,#74256,#74257,#74258,#74259,#74260,
#74261,#74262,#74263,#74264,#74265,#74266,#74267,#74268,#74269,#74270,#74271,
#74272,#74273,#74274,#74275,#74276,#74277,#74278,#74279),.UNSPECIFIED.,
 .F.,.F.,(4,3,3,3,3,3,3,3,3,3,3,3,3,3,3,3,3,3,3,3,3,3,3,3,3,3,3,3,3,3,3,
3,3,3,3,3,3,4),(-0.886548021255907,-0.863182318004303,-0.850026819727067,
-0.845485030967072,-0.828031061920953,-0.823989441594979,-0.807948605086144,
-0.804397368521845,-0.803419323869594,-0.789454474081531,-0.787196805980162,
-0.783854551717749,-0.777784826512269,-0.768896090894216,-0.763303764436096,
-0.75689816948318,-0.749793121745379,-0.748585034020595,-0.742232977096377,
-0.736711329196858,-0.736337056382526,-0.732525887314632,-0.727476816747158,
-0.722225282270684,-0.714704266959016,-0.711963500330866,-0.704984345704295,
-0.701694385768342,-0.687771408069272,-0.681167670056181,-0.671410018653506,
-0.660643577981008,-0.641874313618654,-0.639974521162902,-0.620382690534388,
-0.619305464344796,-0.602967398208329,-0.599057470751573),.UNSPECIFIED.) ;
#860 = B_SPLINE_CURVE_WITH_KNOTS('',3,(#74280,#74281,#74282,#74283,#74284,
#74285,#74286,#74287,#74288,#74289,#74290,#74291,#74292,#74293),
 .UNSPECIFIED.,.F.,.F.,(4,1,1,1,1,1,1,1,1,1,1,4),(0.59905747074872,0.660662588714547,
0.681197628036489,0.701732667358431,0.712000187019402,0.722267706680373,
0.732535226341344,0.763337785324257,0.783872824646199,0.804407863968141,
0.845477942612025,0.886548021255909),.UNSPECIFIED.) ;
#861 = B_SPLINE_CURVE_WITH_KNOTS('',3,(#74297,#74298,#74299,#74300,#74301,
#74302,#74303,#74304,#74305,#74306,#74307,#74308),.UNSPECIFIED.,.F.,.F.,
(4,2,2,2,2,4),(0.,0.00612475744372648,0.0140348469017703,0.0236318332038679,
0.0338613775547147,0.0341436529599871),.UNSPECIFIED.) ;
#862 = B_SPLINE_CURVE_WITH_KNOTS('',3,(#74312,#74313,#74314,#74315,#74316,
#74317,#74318,#74319,#74320,#74321,#74322,#74323,#74324,#74325),
 .UNSPECIFIED.,.F.,.F.,(4,2,2,2,2,2,4),(-0.000285103885038181,0.,0.00872930953219139,
0.0170606390794635,0.0258600808776587,0.0324403480744031,0.0341876342331678),
 .UNSPECIFIED.) ;
#863 = B_SPLINE_CURVE_WITH_KNOTS('',3,(#74331,#74332,#74333,#74334,#74335,
#74336,#74337,#74338,#74339,#74340,#74341,#74342,#74343,#74344),
 .UNSPECIFIED.,.F.,.F.,(4,2,2,2,2,2,4),(-0.000285103884159099,0.,0.00872930953339573,
0.0170606390816542,0.0258600808793018,0.0324403480757735,0.0341876342333799),
 .UNSPECIFIED.) ;
#864 = B_SPLINE_CURVE_WITH_KNOTS('',3,(#74347,#74348,#74349,#74350,#74351,
#74352),.UNSPECIFIED.,.F.,.F.,(4,2,4),(0.0275681674553244,0.0309707637795474,
0.0317834882743744),.UNSPECIFIED.) ;
#865 = B_SPLINE_CURVE_WITH_KNOTS('',3,(#74355,#74356,#74357,#74358,#74359,
#74360),.UNSPECIFIED.,.F.,.F.,(4,2,4),(0.0987440670455209,0.10214723221702,
0.102957912597177),.UNSPECIFIED.) ;
#866 = B_SPLINE_CURVE_WITH_KNOTS('',3,(#74364,#74365,#74366,#74367,#74368,
#74369,#74370,#74371,#74372,#74373,#74374,#74375),.UNSPECIFIED.,.F.,.F.,
(4,2,2,2,2,4),(0.,0.00612475744370874,0.0140348469017083,0.0236318332038301,
0.0338613775547143,0.0341436529591838),.UNSPECIFIED.) ;
#867 = B_SPLINE_CURVE_WITH_KNOTS('',3,(#74378,#74379,#74380,#74381,#74382,
#74383),.UNSPECIFIED.,.F.,.F.,(4,2,4),(0.0275681674553622,0.0309707637796043,
0.0317834882744653),.UNSPECIFIED.) ;
#868 = B_SPLINE_CURVE_WITH_KNOTS('',3,(#74386,#74387,#74388,#74389,#74390,
#74391),.UNSPECIFIED.,.F.,.F.,(4,2,4),(0.0987440670462907,0.102147232217805,
0.102957912597974),.UNSPECIFIED.) ;
#869 = B_SPLINE_CURVE_WITH_KNOTS('',3,(#74467,#74468,#74469,#74470,#74471,
#74472,#74473,#74474,#74475,#74476,#74477,#74478,#74479,#74480,#74481,#74482,
#74483,#74484,#74485,#74486,#74487,#74488,#74489,#74490,#74491,#74492,#74493,
#74494,#74495,#74496,#74497,#74498,#74499,#74500,#74501,#74502,#74503,#74504,
#74505,#74506,#74507,#74508,#74509,#74510,#74511,#74512,#74513,#74514,#74515,
#74516,#74517,#74518,#74519,#74520,#74521,#74522,#74523,#74524,#74525,#74526,
#74527,#74528,#74529,#74530,#74531,#74532,#74533,#74534,#74535,#74536,#74537,
#74538,#74539,#74540,#74541,#74542,#74543,#74544,#74545,#74546,#74547,#74548,
#74549,#74550,#74551,#74552,#74553,#74554),.UNSPECIFIED.,.F.,.F.,(4,3,3,
3,3,3,3,3,3,3,3,3,3,3,3,3,3,3,3,3,3,3,3,3,3,3,3,3,3,4),(-1.15463223446657,
-1.13411784956101,-1.12022914538744,-1.11360346465544,-1.07254724042576,
-1.05201131155961,-1.04611218888535,-1.04174082602754,-1.03146914587479,
-1.02708078581791,-1.02476147151778,-1.02289044034752,-1.01804574952196,
-1.01603399648863,-1.01032623594513,-1.00510701775931,-0.998952781220051,
-0.996793882296726,-0.990336093963219,-0.982532274474594,-0.980075166341655,
-0.975907225267658,-0.969811380724416,-0.950272727910345,-0.949277511016964,
-0.926594285022028,-0.908211282780506,-0.903665232052903,-0.873532453171296,
-0.867143070761121),.UNSPECIFIED.) ;
#870 = B_SPLINE_CURVE_WITH_KNOTS('',3,(#74555,#74556,#74557,#74558,#74559,
#74560,#74561,#74562,#74563,#74564,#74565,#74566,#74567,#74568,#74569),
 .UNSPECIFIED.,.F.,.F.,(4,1,1,1,1,1,1,1,1,1,1,1,4),(0.867143070761104,0.908212951290456,
0.949282831819809,0.969817772084486,0.980085242216824,0.990352712349162,
1.01602138768001,1.03142259287851,1.04169006301085,1.05195753314319,1.07249247340787,
1.11356235393722,1.15463223446657),.UNSPECIFIED.) ;
#871 = B_SPLINE_CURVE_WITH_KNOTS('',3,(#74573,#74574,#74575,#74576,#74577,
#74578,#74579,#74580,#74581,#74582,#74583,#74584),.UNSPECIFIED.,.F.,.F.,
(4,2,2,2,2,4),(0.,0.0061247574437176,0.0140348469017413,0.02363183320368,
0.0338613775544456,0.0341436529587641),.UNSPECIFIED.) ;
#872 = B_SPLINE_CURVE_WITH_KNOTS('',3,(#74588,#74589,#74590,#74591,#74592,
#74593,#74594,#74595,#74596,#74597,#74598,#74599,#74600,#74601),
 .UNSPECIFIED.,.F.,.F.,(4,2,2,2,2,2,4),(-0.000285103884421192,0.,0.00872930953257869,
0.0170606390801584,0.0258600808781175,0.0324403480747261,0.0341876342330866),
 .UNSPECIFIED.) ;
#873 = B_SPLINE_CURVE_WITH_KNOTS('',3,(#74607,#74608,#74609,#74610,#74611,
#74612,#74613,#74614,#74615,#74616,#74617,#74618,#74619,#74620),
 .UNSPECIFIED.,.F.,.F.,(4,2,2,2,2,2,4),(-0.000285103889744773,0.,0.00872930952671932,
0.0170606390697499,0.0258600808702053,0.0324403480681302,0.0341876342317),
 .UNSPECIFIED.) ;
#874 = B_SPLINE_CURVE_WITH_KNOTS('',3,(#74623,#74624,#74625,#74626,#74627,
#74628),.UNSPECIFIED.,.F.,.F.,(4,2,4),(0.0275681674553669,0.0309707637795839,
0.0317834882744089),.UNSPECIFIED.) ;
#875 = B_SPLINE_CURVE_WITH_KNOTS('',3,(#74631,#74632,#74633,#74634,#74635,
#74636),.UNSPECIFIED.,.F.,.F.,(4,2,4),(0.0987440670462967,0.102147232217882,
0.102957912598016),.UNSPECIFIED.) ;
#876 = B_SPLINE_CURVE_WITH_KNOTS('',3,(#74640,#74641,#74642,#74643,#74644,
#74645,#74646,#74647,#74648,#74649,#74650,#74651),.UNSPECIFIED.,.F.,.F.,
(4,2,2,2,2,4),(0.,0.00612475744371255,0.0140348469017152,0.0236318332037933,
0.0338613775546911,0.0341436529587335),.UNSPECIFIED.) ;
#877 = B_SPLINE_CURVE_WITH_KNOTS('',3,(#74654,#74655,#74656,#74657,#74658,
#74659),.UNSPECIFIED.,.F.,.F.,(4,2,4),(0.0275681674553678,0.0309707637795747,
0.031783488274427),.UNSPECIFIED.) ;
#878 = B_SPLINE_CURVE_WITH_KNOTS('',3,(#74662,#74663,#74664,#74665,#74666,
#74667),.UNSPECIFIED.,.F.,.F.,(4,2,4),(0.0987440670465932,0.102147232218164,
0.102957912598333),.UNSPECIFIED.) ;
#879 = B_SPLINE_CURVE_WITH_KNOTS('',3,(#74743,#74744,#74745,#74746,#74747,
#74748,#74749,#74750,#74751,#74752,#74753,#74754,#74755,#74756,#74757),
 .UNSPECIFIED.,.F.,.F.,(4,1,1,1,1,1,1,1,1,1,1,1,4),(-0.411832935461185,
-0.37076295018422,-0.32969296490725,-0.309157972268765,-0.298890475949523,
-0.28862297963028,-0.273221735151417,-0.247552994353311,-0.237285498034068,
-0.227018001714826,-0.206483009076341,-0.165413023799371,-0.124343038522417),
 .UNSPECIFIED.) ;
#880 = B_SPLINE_CURVE_WITH_KNOTS('',3,(#74758,#74759,#74760,#74761,#74762,
#74763,#74764,#74765,#74766,#74767,#74768,#74769,#74770,#74771,#74772),
 .UNSPECIFIED.,.F.,.F.,(4,1,1,1,1,1,1,1,1,1,1,1,4),(0.1243430385224,0.165413023799369,
0.206483009076339,0.227018001714824,0.237285498034067,0.247552994353309,
0.273221735151415,0.288622979630279,0.298890475949521,0.309157972268764,
0.329692964907249,0.370762950184219,0.411832935461188),.UNSPECIFIED.) ;
#881 = B_SPLINE_CURVE_WITH_KNOTS('',3,(#74776,#74777,#74778,#74779,#74780,
#74781,#74782,#74783,#74784,#74785,#74786,#74787),.UNSPECIFIED.,.F.,.F.,
(4,2,2,2,2,4),(0.,0.00612475744369689,0.0140348469016405,0.0236318332037292,
0.0338613775545991,0.0341436529587365),.UNSPECIFIED.) ;
#882 = B_SPLINE_CURVE_WITH_KNOTS('',3,(#74791,#74792,#74793,#74794,#74795,
#74796,#74797,#74798,#74799,#74800,#74801,#74802,#74803,#74804),
 .UNSPECIFIED.,.F.,.F.,(4,2,2,2,2,2,4),(-0.000285103884298923,0.,0.00872930953326711,
0.0170606390812955,0.0258600808788128,0.0324403480752013,0.0341876342326143),
 .UNSPECIFIED.) ;
#883 = B_SPLINE_CURVE_WITH_KNOTS('',3,(#74810,#74811,#74812,#74813,#74814,
#74815,#74816,#74817,#74818,#74819,#74820,#74821,#74822,#74823),
 .UNSPECIFIED.,.F.,.F.,(4,2,2,2,2,2,4),(-0.000285103883452685,0.,0.00872930953447474,
0.0170606390835385,0.0258600808807064,0.0324403480769824,0.0341876342336455),
 .UNSPECIFIED.) ;
#884 = B_SPLINE_CURVE_WITH_KNOTS('',3,(#74826,#74827,#74828,#74829,#74830,
#74831),.UNSPECIFIED.,.F.,.F.,(4,2,4),(0.027568167455528,0.0309707637797636,
0.0317834882746252),.UNSPECIFIED.) ;
#885 = B_SPLINE_CURVE_WITH_KNOTS('',3,(#74834,#74835,#74836,#74837,#74838,
#74839),.UNSPECIFIED.,.F.,.F.,(4,2,4),(0.0987440670463977,0.10214723221798,
0.102957912598135),.UNSPECIFIED.) ;
#886 = B_SPLINE_CURVE_WITH_KNOTS('',3,(#74843,#74844,#74845,#74846,#74847,
#74848,#74849,#74850,#74851,#74852,#74853,#74854),.UNSPECIFIED.,.F.,.F.,
(4,2,2,2,2,4),(0.,0.00612475744370791,0.0140348469017071,0.0236318332038692,
0.0338613775547471,0.0341436529596501),.UNSPECIFIED.) ;
#887 = B_SPLINE_CURVE_WITH_KNOTS('',3,(#74857,#74858,#74859,#74860,#74861,
#74862),.UNSPECIFIED.,.F.,.F.,(4,2,4),(0.0275681674553135,0.0309707637795262,
0.0317834882743389),.UNSPECIFIED.) ;
#888 = B_SPLINE_CURVE_WITH_KNOTS('',3,(#74865,#74866,#74867,#74868,#74869,
#74870),.UNSPECIFIED.,.F.,.F.,(4,2,4),(0.0987440670454317,0.102147232216938,
0.102957912597103),.UNSPECIFIED.) ;
#889 = B_SPLINE_CURVE_WITH_KNOTS('',3,(#74946,#74947,#74948,#74949,#74950,
#74951,#74952,#74953,#74954,#74955,#74956,#74957,#74958,#74959,#74960,#74961,
#74962,#74963,#74964,#74965,#74966,#74967,#74968,#74969,#74970,#74971,#74972,
#74973,#74974,#74975,#74976,#74977,#74978,#74979,#74980,#74981,#74982,#74983,
#74984,#74985,#74986,#74987,#74988,#74989,#74990,#74991,#74992,#74993,#74994,
#74995,#74996,#74997,#74998,#74999,#75000,#75001,#75002,#75003,#75004,#75005,
#75006,#75007,#75008,#75009,#75010,#75011,#75012,#75013,#75014,#75015,#75016,
#75017,#75018,#75019,#75020,#75021,#75022,#75023,#75024,#75025,#75026,#75027,
#75028,#75029,#75030,#75031,#75032,#75033,#75034,#75035,#75036),
 .UNSPECIFIED.,.F.,.F.,(4,3,3,3,3,3,3,3,3,3,3,3,3,3,3,3,3,3,3,3,3,3,3,3,
3,3,3,3,3,3,4),(-0.477703831735242,-0.457189426261555,-0.443230506420269,
-0.436675020787869,-0.395618810128837,-0.378433299612694,-0.375082901246212,
-0.369185298823285,-0.364812412641861,-0.354540726183523,-0.350401889199105,
-0.348213658304538,-0.345961981360179,-0.341117226356061,-0.339105569093216,
-0.333397648976201,-0.328177881844107,-0.322023347030127,-0.319864746381521,
-0.313407644934347,-0.305604024516391,-0.30314670890323,-0.29897808935244,
-0.292882919054629,-0.273343591995118,-0.272349028370288,-0.249678041716392,
-0.231282777755435,-0.22673609613766,-0.196809574226464,-0.190214667985449),
 .UNSPECIFIED.) ;
#890 = B_SPLINE_CURVE_WITH_KNOTS('',3,(#75037,#75038,#75039,#75040,#75041,
#75042,#75043,#75044,#75045,#75046,#75047,#75048,#75049,#75050,#75051),
 .UNSPECIFIED.,.F.,.F.,(4,1,1,1,1,1,1,1,1,1,1,1,4),(0.190214667985433,0.23128454852112,
0.272354429056807,0.29288936932465,0.303156839458572,0.313424309592494,
0.339092984927298,0.354494190128181,0.364761660262103,0.375029130396024,
0.395564070663868,0.436633951199555,0.477703831735242),.UNSPECIFIED.) ;
#891 = B_SPLINE_CURVE_WITH_KNOTS('',3,(#75055,#75056,#75057,#75058,#75059,
#75060,#75061,#75062,#75063,#75064,#75065,#75066),.UNSPECIFIED.,.F.,.F.,
(4,2,2,2,2,4),(0.,0.00612475744370239,0.0140348469016695,0.0236318332040214,
0.0338613775551618,0.0341436529601212),.UNSPECIFIED.) ;
#892 = B_SPLINE_CURVE_WITH_KNOTS('',3,(#75070,#75071,#75072,#75073,#75074,
#75075,#75076,#75077,#75078,#75079,#75080,#75081,#75082,#75083),
 .UNSPECIFIED.,.F.,.F.,(4,2,2,2,2,2,4),(-0.000285103889775932,0.,0.00872930952735993,
0.0170606390708911,0.0258600808712746,0.0324403480691489,0.0341876342324684),
 .UNSPECIFIED.) ;
#893 = B_SPLINE_CURVE_WITH_KNOTS('',3,(#75086,#75087,#75088,#75089,#75090,
#75091),.UNSPECIFIED.,.F.,.F.,(4,2,4),(0.0275681674554672,0.0309707637796864,
0.031783488274549),.UNSPECIFIED.) ;
#894 = B_SPLINE_CURVE_WITH_KNOTS('',3,(#75094,#75095,#75096,#75097,#75098,
#75099),.UNSPECIFIED.,.F.,.F.,(4,2,4),(0.0987440670467281,0.102147232218267,
0.102957912598433),.UNSPECIFIED.) ;
#895 = B_SPLINE_CURVE_WITH_KNOTS('',3,(#75340,#75341,#75342,#75343),
 .UNSPECIFIED.,.F.,.F.,(4,4),(0.,0.0304960917345408),.UNSPECIFIED.) ;
#896 = B_SPLINE_CURVE_WITH_KNOTS('',3,(#75345,#75346,#75347,#75348,#75349,
#75350),.UNSPECIFIED.,.F.,.F.,(4,2,4),(0.0304960917345408,0.0307213705840096,
0.0308468428281894),.UNSPECIFIED.) ;
#897 = B_SPLINE_CURVE_WITH_KNOTS('',3,(#75351,#75352,#75353,#75354,#75355,
#75356),.UNSPECIFIED.,.F.,.F.,(4,2,4),(-0.0308468428281894,-0.0307213705840096,
0.),.UNSPECIFIED.) ;
#898 = B_SPLINE_CURVE_WITH_KNOTS('',3,(#75428,#75429,#75430,#75431,#75432,
#75433,#75434,#75435,#75436,#75437),.UNSPECIFIED.,.F.,.F.,(4,2,2,2,4),(-9.50158063795107E-5,
-3.3802014536195E-10,0.0116383704253253,0.0168222452993766,0.0213033382245776),
 .UNSPECIFIED.) ;
#899 = B_SPLINE_CURVE_WITH_KNOTS('',3,(#75438,#75439,#75440,#75441,#75442),
 .UNSPECIFIED.,.F.,.F.,(4,1,4),(0.0251851760390954,0.0320842381312984,0.0449179333838473),
 .UNSPECIFIED.) ;
#900 = B_SPLINE_CURVE_WITH_KNOTS('',3,(#75443,#75444,#75445,#75446,#75447,
#75448),.UNSPECIFIED.,.F.,.F.,(4,1,1,4),(0.,0.5,0.714285714285714,1.),
 .UNSPECIFIED.) ;
#901 = B_SPLINE_CURVE_WITH_KNOTS('',3,(#75474,#75475,#75476,#75477,#75478),
 .UNSPECIFIED.,.F.,.F.,(4,1,4),(-0.0228171701215865,-0.0097787952834712,
0.),.UNSPECIFIED.) ;
#902 = B_SPLINE_CURVE_WITH_KNOTS('',3,(#75479,#75480,#75481,#75482,#75483,
#75484,#75485,#75486,#75487,#75488,#75489,#75490,#75491,#75492,#75493,#75494,
#75495,#75496,#75497),.UNSPECIFIED.,.F.,.F.,(4,3,3,3,3,3,4),(7.84710342600197E-9,
0.00635871960742978,0.00765411709399715,0.0097787952834712,0.0153829015724535,
0.0211032796709813,0.0228171889947661),.UNSPECIFIED.) ;
#903 = B_SPLINE_CURVE_WITH_KNOTS('',3,(#75516,#75517,#75518,#75519,#75520),
 .UNSPECIFIED.,.F.,.F.,(4,1,4),(-1.,-0.571428571428571,0.),
 .UNSPECIFIED.) ;
#904 = B_SPLINE_CURVE_WITH_KNOTS('',3,(#75589,#75590,#75591,#75592),
 .UNSPECIFIED.,.F.,.F.,(4,4),(-1.19261278278549,0.),.UNSPECIFIED.) ;
#905 = B_SPLINE_CURVE_WITH_KNOTS('',3,(#75595,#75596,#75597,#75598),
 .UNSPECIFIED.,.F.,.F.,(4,4),(0.,1.19261278278549),.UNSPECIFIED.) ;
#906 = B_SPLINE_CURVE_WITH_KNOTS('',3,(#75630,#75631,#75632,#75633,#75634,
#75635),.UNSPECIFIED.,.F.,.F.,(4,1,1,4),(-0.0977650255444303,-0.0698321611031645,
-0.0418992966618987,0.),.UNSPECIFIED.) ;
#907 = B_SPLINE_CURVE_WITH_KNOTS('',3,(#75638,#75639,#75640,#75641,#75642,
#75643),.UNSPECIFIED.,.F.,.F.,(4,1,1,4),(0.,0.0418992966618987,0.0698321611031645,
0.0977650255444303),.UNSPECIFIED.) ;
#908 = B_SPLINE_CURVE_WITH_KNOTS('',3,(#75698,#75699,#75700,#75701),
 .UNSPECIFIED.,.F.,.F.,(4,4),(-1.35181237759077,-5.11404103536248E-14),
 .UNSPECIFIED.) ;
#909 = B_SPLINE_CURVE_WITH_KNOTS('',3,(#75702,#75703,#75704,#75705),
 .UNSPECIFIED.,.F.,.F.,(4,4),(5.11404103536248E-14,1.35181237759077),
 .UNSPECIFIED.) ;
#910 = B_SPLINE_CURVE_WITH_KNOTS('',3,(#75737,#75738,#75739,#75740,#75741,
#75742),.UNSPECIFIED.,.F.,.F.,(4,1,1,4),(-0.0921161357255624,-0.0657972398039731,
-0.0394783438823839,0.),.UNSPECIFIED.) ;
#911 = B_SPLINE_CURVE_WITH_KNOTS('',3,(#75745,#75746,#75747,#75748,#75749,
#75750),.UNSPECIFIED.,.F.,.F.,(4,1,1,4),(0.,0.0394783438823839,0.0657972398039731,
0.0921161357255624),.UNSPECIFIED.) ;
#912 = B_SPLINE_CURVE_WITH_KNOTS('',3,(#75812,#75813,#75814,#75815,#75816,
#75817,#75818),.UNSPECIFIED.,.F.,.F.,(4,1,1,1,4),(-1.,-0.857142857142857,
-0.571428571428571,-0.285714285714286,0.),.UNSPECIFIED.) ;
#913 = B_SPLINE_CURVE_WITH_KNOTS('',3,(#75829,#75830,#75831,#75832),
 .UNSPECIFIED.,.F.,.F.,(4,4),(-1.19778613661182,0.),.UNSPECIFIED.) ;
#914 = B_SPLINE_CURVE_WITH_KNOTS('',3,(#75854,#75855,#75856,#75857,#75858),
 .UNSPECIFIED.,.F.,.F.,(4,1,4),(-1.5574419802933,-0.667475134411416,0.),
 .UNSPECIFIED.) ;
#915 = B_SPLINE_CURVE_WITH_KNOTS('',3,(#75864,#75865,#75866,#75867,#75868,
#75869,#75870),.UNSPECIFIED.,.F.,.F.,(4,1,1,1,4),(3.75975382637766E-15,
0.0255939875922149,0.051187975184426,0.0639849689805315,0.0895789565727426),
 .UNSPECIFIED.) ;
#916 = B_SPLINE_CURVE_WITH_KNOTS('',3,(#75872,#75873,#75874,#75875,#75876),
 .UNSPECIFIED.,.F.,.F.,(4,1,4),(-1.52552518986177,-0.653796509940758,0.),
 .UNSPECIFIED.) ;
#917 = B_SPLINE_CURVE_WITH_KNOTS('',3,(#75878,#75879,#75880,#75881,#75882),
 .UNSPECIFIED.,.F.,.F.,(4,1,4),(-1.19232799652366,-0.510997712795854,0.),
 .UNSPECIFIED.) ;
#918 = B_SPLINE_CURVE_WITH_KNOTS('',3,(#75900,#75901,#75902,#75903,#75904,
#75905),.UNSPECIFIED.,.F.,.F.,(4,1,1,4),(0.,0.0345437068826219,0.0575728448043699,
0.0806019827261179),.UNSPECIFIED.) ;
#919 = B_SPLINE_CURVE_WITH_KNOTS('',3,(#75909,#75910,#75911,#75912,#75913),
 .UNSPECIFIED.,.F.,.F.,(4,1,4),(0.,0.0235485345716834,0.0549465806672613),
 .UNSPECIFIED.) ;
#920 = B_SPLINE_CURVE_WITH_KNOTS('',3,(#75916,#75917,#75918,#75919,#75920,
#75921),.UNSPECIFIED.,.F.,.F.,(4,1,1,4),(4.3103929042364E-51,0.0368724376954248,
0.061454062825708,0.0860356879559912),.UNSPECIFIED.) ;
#921 = B_SPLINE_CURVE_WITH_KNOTS('',3,(#75924,#75925,#75926,#75927,#75928,
#75929),.UNSPECIFIED.,.F.,.F.,(4,2,4),(-0.0257669909600073,0.,0.011519137396051),
 .UNSPECIFIED.) ;
#922 = B_SPLINE_CURVE_WITH_KNOTS('',3,(#75935,#75936,#75937,#75938,#75939,
#75940,#75941),.UNSPECIFIED.,.F.,.F.,(4,1,1,1,4),(-0.0425072330863067,-0.030362309347362,
-0.0212536165431535,-0.00910869280420873,-1.83791533766654E-16),
 .UNSPECIFIED.) ;
#923 = B_SPLINE_CURVE_WITH_KNOTS('',3,(#75945,#75946,#75947,#75948,#75949),
 .UNSPECIFIED.,.F.,.F.,(4,1,4),(-0.0304168573334205,-0.0130357960000373,
0.),.UNSPECIFIED.) ;
#924 = B_SPLINE_CURVE_WITH_KNOTS('',3,(#76012,#76013,#76014,#76015),
 .UNSPECIFIED.,.F.,.F.,(4,4),(-0.465795144410571,-0.11054487910679),
 .UNSPECIFIED.) ;
#925 = B_SPLINE_CURVE_WITH_KNOTS('',3,(#76047,#76048,#76049,#76050,#76051,
#76052),.UNSPECIFIED.,.F.,.F.,(4,1,1,4),(-0.0806019827261179,-0.0575728448043699,
-0.0345437068826219,0.),.UNSPECIFIED.) ;
#926 = B_SPLINE_CURVE_WITH_KNOTS('',3,(#76084,#76085,#76086,#76087,#76088),
 .UNSPECIFIED.,.F.,.F.,(4,1,4),(-0.0549465806672613,-0.0235485345716834,
0.),.UNSPECIFIED.) ;
#927 = B_SPLINE_CURVE_WITH_KNOTS('',3,(#76112,#76113,#76114,#76115),
 .UNSPECIFIED.,.F.,.F.,(4,4),(0.,0.963640330286854),.UNSPECIFIED.) ;
#928 = B_SPLINE_CURVE_WITH_KNOTS('',3,(#76146,#76147,#76148,#76149,#76150,
#76151),.UNSPECIFIED.,.F.,.F.,(4,1,1,4),(-0.0860356879559912,-0.061454062825708,
-0.0368724376954248,-4.3103929042364E-51),.UNSPECIFIED.) ;
#929 = B_SPLINE_CURVE_WITH_KNOTS('',3,(#76167,#76168,#76169,#76170,#76171,
#76172),.UNSPECIFIED.,.F.,.F.,(4,1,1,4),(0.,0.285714285714286,0.571428571428571,
1.),.UNSPECIFIED.) ;
#930 = B_SPLINE_CURVE_WITH_KNOTS('',3,(#76184,#76185,#76186,#76187),
 .UNSPECIFIED.,.F.,.F.,(4,4),(0.11054487910679,0.465795144410571),
 .UNSPECIFIED.) ;
#931 = B_SPLINE_CURVE_WITH_KNOTS('',3,(#76219,#76220,#76221,#76222,#76223,
#76224,#76225,#76226,#76227,#76228,#76229,#76230,#76231,#76232,#76233,#76234),
 .UNSPECIFIED.,.F.,.F.,(4,3,3,3,3,4),(-0.000158808056872058,0.,0.00496233024236406,
0.00971437347025351,0.0143645688442801,0.0189647476919275),
 .UNSPECIFIED.) ;
#932 = B_SPLINE_CURVE_WITH_KNOTS('',3,(#76238,#76239,#76240,#76241,#76242,
#76243,#76244,#76245,#76246,#76247,#76248,#76249,#76250,#76251),
 .UNSPECIFIED.,.F.,.F.,(4,2,2,2,2,2,4),(-0.000100608577474137,3.68347560433932E-11,
0.00487642669195541,0.00843616962847088,0.0110941564927162,0.012526922262663,
0.0139424786869335),.UNSPECIFIED.) ;
#933 = B_SPLINE_CURVE_WITH_KNOTS('',5,(#76349,#76350,#76351,#76352,#76353,
#76354,#76355,#76356,#76357),.UNSPECIFIED.,.F.,.F.,(6,1,1,1,6),(-0.568009935219888,
-0.5,-0.4,-0.3,-0.202504416334422),.UNSPECIFIED.) ;
#934 = B_SPLINE_CURVE_WITH_KNOTS('',5,(#76385,#76386,#76387,#76388,#76389,
#76390,#76391,#76392,#76393,#76394),.UNSPECIFIED.,.F.,.F.,(6,1,1,1,1,6),
(-0.970637147863782,-0.9,-0.8,-0.7,-0.6,-0.568009935219903),
 .UNSPECIFIED.) ;
#935 = B_SPLINE_CURVE_WITH_KNOTS('',3,(#76432,#76433,#76434,#76435,#76436,
#76437,#76438),.UNSPECIFIED.,.F.,.F.,(4,1,1,1,4),(-1.,-0.857142857142857,
-0.571428571428571,-0.285714285714286,0.),.UNSPECIFIED.) ;
#936 = B_SPLINE_CURVE_WITH_KNOTS('',5,(#76493,#76494,#76495,#76496,#76497,
#76498,#76499,#76500,#76501,#76502),.UNSPECIFIED.,.F.,.F.,(6,1,1,1,1,6),
(0.504846387196225,0.6,0.7,0.8,0.9,0.98854312859838),.UNSPECIFIED.) ;
#937 = B_SPLINE_CURVE_WITH_KNOTS('',3,(#76625,#76626,#76627,#76628,#76629,
#76630,#76631,#76632,#76633,#76634,#76635,#76636,#76637,#76638,#76639,#76640,
#76641,#76642,#76643,#76644,#76645,#76646,#76647,#76648,#76649),
 .UNSPECIFIED.,.F.,.F.,(4,3,3,3,3,3,3,3,4),(-0.000166044934212311,0.,0.00279435046699232,
0.00557076822786895,0.00922713992765633,0.0104440756657821,0.014060635831078,
0.0150050171466993,0.0194197313345285),.UNSPECIFIED.) ;
#938 = B_SPLINE_CURVE_WITH_KNOTS('',3,(#76675,#76676,#76677,#76678,#76679),
 .UNSPECIFIED.,.F.,.F.,(4,1,4),(0.,0.66747373630185,1.55743871803765),
 .UNSPECIFIED.) ;
#939 = B_SPLINE_CURVE_WITH_KNOTS('',3,(#76771,#76772,#76773,#76774,#76775,
#76776),.UNSPECIFIED.,.F.,.F.,(4,2,4),(0.,0.0885040710835739,0.177008142167353),
 .UNSPECIFIED.) ;
#940 = B_SPLINE_CURVE_WITH_KNOTS('',3,(#76795,#76796,#76797,#76798,#76799,
#76800,#76801,#76802,#76803,#76804,#76805,#76806,#76807,#76808),
 .UNSPECIFIED.,.F.,.F.,(4,2,2,2,2,2,4),(-0.0904118247922396,-0.0900035304718211,
-0.0717391824762992,-0.0592522695262226,-0.052421636870123,-0.0483060494744438,
-0.0450017652359281),.UNSPECIFIED.) ;
#941 = B_SPLINE_CURVE_WITH_KNOTS('',3,(#76811,#76812,#76813,#76814,#76815,
#76816,#76817,#76818,#76819,#76820,#76821,#76822,#76823,#76824),
 .UNSPECIFIED.,.F.,.F.,(4,2,2,2,2,2,4),(-0.000229805914918867,0.,0.0057259760846815,
0.0111063849697663,0.0162643432934294,0.0200672254121506,0.0233750704027966),
 .UNSPECIFIED.) ;
#942 = B_SPLINE_CURVE_WITH_KNOTS('',3,(#76853,#76854,#76855,#76856,#76857),
 .UNSPECIFIED.,.F.,.F.,(4,1,4),(0.,0.571428571428571,1.),.UNSPECIFIED.) ;
#943 = B_SPLINE_CURVE_WITH_KNOTS('',3,(#76916,#76917,#76918,#76919,#76920,
#76921),.UNSPECIFIED.,.F.,.F.,(4,1,1,4),(0.,0.285714285714286,0.571428571428571,
1.),.UNSPECIFIED.) ;
#944 = B_SPLINE_CURVE_WITH_KNOTS('',3,(#77040,#77041,#77042,#77043,#77044,
#77045,#77046,#77047,#77048,#77049,#77050,#77051,#77052,#77053),
 .UNSPECIFIED.,.F.,.F.,(4,2,2,2,2,2,4),(-0.000109725029838064,0.,0.00573281981816143,
0.011229162404333,0.0168245500650057,0.0201739980781553,0.0234334300413515),
 .UNSPECIFIED.) ;
#945 = B_SPLINE_CURVE_WITH_KNOTS('',3,(#77151,#77152,#77153,#77154,#77155,
#77156,#77157,#77158,#77159,#77160),.UNSPECIFIED.,.F.,.F.,(4,2,2,2,4),(-0.0827921863495745,
-0.0783024654164144,-0.0738127444832543,-0.0678611473372446,-0.061909550191235),
 .UNSPECIFIED.) ;
#946 = B_SPLINE_CURVE_WITH_KNOTS('',3,(#77234,#77235,#77236,#77237,#77238,
#77239,#77240,#77241,#77242,#77243,#77244,#77245),.UNSPECIFIED.,.F.,.F.,
(4,2,2,2,2,4),(0.,0.00262343669493822,0.00608267202291995,0.0109373875288971,
0.016217047415382,0.021823180377612),.UNSPECIFIED.) ;
#947 = B_SPLINE_CURVE_WITH_KNOTS('',3,(#77306,#77307,#77308,#77309,#77310),
 .UNSPECIFIED.,.F.,.F.,(4,1,4),(-0.0345437068826239,-0.017271853441312,
0.),.UNSPECIFIED.) ;
#948 = B_SPLINE_CURVE_WITH_KNOTS('',3,(#77395,#77396,#77397,#77398,#77399,
#77400),.UNSPECIFIED.,.F.,.F.,(4,1,1,4),(-0.0368724376954292,-0.0263374554967351,
-0.0158024732980411,0.),.UNSPECIFIED.) ;
#949 = B_SPLINE_CURVE_WITH_KNOTS('',3,(#77401,#77402,#77403,#77404,#77405,
#77406),.UNSPECIFIED.,.F.,.F.,(4,1,1,4),(0.,0.0158024732980411,0.0263374554967351,
0.0368724376954292),.UNSPECIFIED.) ;
#950 = B_SPLINE_CURVE_WITH_KNOTS('',3,(#77431,#77432,#77433,#77434),
 .UNSPECIFIED.,.F.,.F.,(4,4),(0.,0.971129055990219),.UNSPECIFIED.) ;
#951 = B_SPLINE_CURVE_WITH_KNOTS('',3,(#77463,#77464,#77465,#77466,#77467),
 .UNSPECIFIED.,.F.,.F.,(4,1,4),(-0.0235485345716821,-0.0100922291021495,
0.),.UNSPECIFIED.) ;
#952 = B_SPLINE_CURVE_WITH_KNOTS('',3,(#77468,#77469,#77470,#77471,#77472),
 .UNSPECIFIED.,.F.,.F.,(4,1,4),(0.,0.0100922291021495,0.0235485345716821),
 .UNSPECIFIED.) ;
#953 = B_SPLINE_CURVE_WITH_KNOTS('',3,(#77511,#77512,#77513,#77514,#77515,
#77516),.UNSPECIFIED.,.F.,.F.,(4,1,1,4),(-0.0394783438823839,-0.0225590536470765,
-0.0112795268235383,0.),.UNSPECIFIED.) ;
#954 = B_SPLINE_CURVE_WITH_KNOTS('',3,(#77519,#77520,#77521,#77522,#77523,
#77524),.UNSPECIFIED.,.F.,.F.,(4,1,1,4),(0.,0.0112795268235383,0.0225590536470765,
0.0394783438823839),.UNSPECIFIED.) ;
#955 = B_SPLINE_CURVE_WITH_KNOTS('',3,(#77545,#77546,#77547,#77548),
 .UNSPECIFIED.,.F.,.F.,(4,4),(-1.34425818567182,0.),.UNSPECIFIED.) ;
#956 = B_SPLINE_CURVE_WITH_KNOTS('',3,(#77551,#77552,#77553,#77554),
 .UNSPECIFIED.,.F.,.F.,(4,4),(0.,1.34425818567182),.UNSPECIFIED.) ;
#957 = B_SPLINE_CURVE_WITH_KNOTS('',3,(#77619,#77620,#77621,#77622,#77623,
#77624,#77625),.UNSPECIFIED.,.F.,.F.,(4,1,1,1,4),(-0.0418992966619001,-0.0359136828530572,
-0.0239424552353715,-0.0119712276176857,0.),.UNSPECIFIED.) ;
#958 = B_SPLINE_CURVE_WITH_KNOTS('',3,(#77648,#77649,#77650,#77651),
 .UNSPECIFIED.,.F.,.F.,(4,4),(0.,1.19778613661182),.UNSPECIFIED.) ;
#959 = B_SPLINE_CURVE_WITH_KNOTS('',3,(#77748,#77749,#77750,#77751,#77752),
 .UNSPECIFIED.,.F.,.F.,(4,1,4),(-0.0247639318112814,-0.0106131136334063,
0.),.UNSPECIFIED.) ;
#960 = B_SPLINE_CURVE_WITH_KNOTS('',3,(#77798,#77799,#77800,#77801),
 .UNSPECIFIED.,.F.,.F.,(4,4),(0.0229372865431325,1.40205259514116),
 .UNSPECIFIED.) ;
#961 = B_SPLINE_CURVE_WITH_KNOTS('',3,(#77804,#77805,#77806,#77807,#77808,
#77809,#77810),.UNSPECIFIED.,.F.,.F.,(4,3,4),(-0.978678731718532,-0.545479769376514,
-0.539016918864981),.UNSPECIFIED.) ;
#962 = B_SPLINE_CURVE_WITH_KNOTS('',3,(#77878,#77879,#77880,#77881,#77882,
#77883,#77884),.UNSPECIFIED.,.F.,.F.,(4,1,1,1,4),(-0.0418992966619021,-0.0299280690442158,
-0.0179568414265295,-0.00598561380884316,0.),.UNSPECIFIED.) ;
#963 = B_SPLINE_CURVE_WITH_KNOTS('',3,(#77887,#77888,#77889,#77890,#77891,
#77892,#77893),.UNSPECIFIED.,.F.,.F.,(4,1,1,1,4),(0.,0.285714285714286,
0.571428571428571,0.857142857142857,1.),.UNSPECIFIED.) ;
#964 = B_SPLINE_CURVE_WITH_KNOTS('',3,(#77914,#77915,#77916,#77917),
 .UNSPECIFIED.,.F.,.F.,(4,4),(-1.20789221798527,0.),.UNSPECIFIED.) ;
#965 = B_SPLINE_CURVE_WITH_KNOTS('',3,(#77918,#77919,#77920,#77921),
 .UNSPECIFIED.,.F.,.F.,(4,4),(0.,1.20789221798527),.UNSPECIFIED.) ;
#966 = B_SPLINE_CURVE_WITH_KNOTS('',3,(#77961,#77962,#77963,#77964,#77965,
#77966),.UNSPECIFIED.,.F.,.F.,(4,1,1,4),(-0.0251311022767196,-0.0224490289603943,
-0.0149660193069295,0.),.UNSPECIFIED.) ;
#967 = B_SPLINE_CURVE_WITH_KNOTS('',3,(#77970,#77971,#77972,#77973,#77974,
#77975,#77976),.UNSPECIFIED.,.F.,.F.,(4,1,1,1,4),(-1.,-0.785714285714286,
-0.5,-0.285714285714286,0.),.UNSPECIFIED.) ;
#968 = B_SPLINE_CURVE_WITH_KNOTS('',3,(#77979,#77980,#77981,#77982,#77983),
 .UNSPECIFIED.,.F.,.F.,(4,1,4),(-0.0523810675742533,-0.0374150482673238,
-0.027172373910007),.UNSPECIFIED.) ;
#969 = B_SPLINE_CURVE_WITH_KNOTS('',3,(#78021,#78022,#78023,#78024),
 .UNSPECIFIED.,.F.,.F.,(4,4),(0.0231068825027873,1.41003451675495),
 .UNSPECIFIED.) ;
#970 = B_SPLINE_CURVE_WITH_KNOTS('',3,(#78027,#78028,#78029,#78030),
 .UNSPECIFIED.,.F.,.F.,(4,4),(-1.41003451675495,-0.0231068825027873),
 .UNSPECIFIED.) ;
#971 = B_SPLINE_CURVE_WITH_KNOTS('',3,(#78093,#78094,#78095,#78096,#78097,
#78098),.UNSPECIFIED.,.F.,.F.,(4,1,1,4),(-0.0977650255444333,-0.0698321611031666,
-0.0418992966619,0.),.UNSPECIFIED.) ;
#972 = B_SPLINE_CURVE_WITH_KNOTS('',3,(#78101,#78102,#78103,#78104,#78105,
#78106),.UNSPECIFIED.,.F.,.F.,(4,1,1,4),(0.,0.0418992966619,0.0698321611031666,
0.0977650255444333),.UNSPECIFIED.) ;
#973 = B_SPLINE_CURVE_WITH_KNOTS('',3,(#78127,#78128,#78129,#78130),
 .UNSPECIFIED.,.F.,.F.,(4,4),(-1.20265740584169,0.),.UNSPECIFIED.) ;
#974 = B_SPLINE_CURVE_WITH_KNOTS('',3,(#78131,#78132,#78133,#78134),
 .UNSPECIFIED.,.F.,.F.,(4,4),(0.,1.20265740584169),.UNSPECIFIED.) ;
#975 = B_SPLINE_CURVE_WITH_KNOTS('',3,(#78186,#78187,#78188,#78189,#78190),
 .UNSPECIFIED.,.F.,.F.,(4,1,4),(0.,0.0104089910116412,0.0242876456938294),
 .UNSPECIFIED.) ;
#976 = B_SPLINE_CURVE_WITH_KNOTS('',3,(#78192,#78193,#78194,#78195,#78196),
 .UNSPECIFIED.,.F.,.F.,(4,1,4),(-1.16825744734596,-0.500681763148267,0.),
 .UNSPECIFIED.) ;
#977 = B_SPLINE_CURVE_WITH_KNOTS('',3,(#78198,#78199,#78200,#78201,#78202),
 .UNSPECIFIED.,.F.,.F.,(4,1,4),(-1.52552518986177,-0.653796509940757,0.),
 .UNSPECIFIED.) ;
#978 = B_SPLINE_CURVE_WITH_KNOTS('',3,(#78204,#78205,#78206,#78207,#78208,
#78209,#78210),.UNSPECIFIED.,.F.,.F.,(4,1,1,1,4),(0.,0.0255939875922127,
0.038390981388319,0.0639849689805316,0.0895789565727443),.UNSPECIFIED.) ;
#979 = B_SPLINE_CURVE_WITH_KNOTS('',3,(#78216,#78217,#78218,#78219,#78220),
 .UNSPECIFIED.,.F.,.F.,(4,1,4),(-1.55743871803765,-0.66747373630185,0.),
 .UNSPECIFIED.) ;
#980 = B_SPLINE_CURVE_WITH_KNOTS('',3,(#78226,#78227,#78228,#78229,#78230,
#78231,#78232),.UNSPECIFIED.,.F.,.F.,(4,1,1,1,4),(-0.0459218921195416,-0.0328013515139583,
-0.0229609460597708,-0.00984040545418749,0.),.UNSPECIFIED.) ;
#981 = B_SPLINE_CURVE_WITH_KNOTS('',3,(#78234,#78235,#78236,#78237),
 .UNSPECIFIED.,.F.,.F.,(4,4),(-1.13243225761785,-0.0170557641123888),
 .UNSPECIFIED.) ;
#982 = B_SPLINE_CURVE_WITH_KNOTS('',3,(#78239,#78240,#78241,#78242,#78243),
 .UNSPECIFIED.,.F.,.F.,(4,1,4),(-0.0245704597956453,-0.0105301970552765,
0.),.UNSPECIFIED.) ;
#983 = B_SPLINE_CURVE_WITH_KNOTS('',3,(#78247,#78248,#78249,#78250,#78251,
#78252,#78253),.UNSPECIFIED.,.F.,.F.,(4,1,1,1,4),(-0.0493631644051633,-0.0352594031465452,
-0.0211556418879271,-0.0141037612586181,0.),.UNSPECIFIED.) ;
#984 = B_SPLINE_CURVE_WITH_KNOTS('',3,(#78255,#78256,#78257,#78258),
 .UNSPECIFIED.,.F.,.F.,(4,4),(-1.02674783308136,-0.019875255616694),
 .UNSPECIFIED.) ;
#985 = B_SPLINE_CURVE_WITH_KNOTS('',3,(#78260,#78261,#78262,#78263,#78264),
 .UNSPECIFIED.,.F.,.F.,(4,1,4),(-0.0315062771267664,-0.0180035869295808,
0.),.UNSPECIFIED.) ;
#986 = B_SPLINE_CURVE_WITH_KNOTS('',3,(#78306,#78307,#78308,#78309,#78310,
#78311,#78312),.UNSPECIFIED.,.F.,.F.,(4,1,1,1,4),(0.,0.285714285714286,
0.5,0.785714285714286,1.),.UNSPECIFIED.) ;
#987 = B_SPLINE_CURVE_WITH_KNOTS('',3,(#78395,#78396,#78397,#78398,#78399),
 .UNSPECIFIED.,.F.,.F.,(4,1,4),(-1.,-0.571428571428571,0.),
 .UNSPECIFIED.) ;
#988 = B_SPLINE_CURVE_WITH_KNOTS('',3,(#78445,#78446,#78447,#78448),
 .UNSPECIFIED.,.F.,.F.,(4,4),(-1.03467847166523,-0.020008660331873),
 .UNSPECIFIED.) ;
#989 = B_SPLINE_CURVE_WITH_KNOTS('',3,(#78449,#78450,#78451,#78452),
 .UNSPECIFIED.,.F.,.F.,(4,4),(0.020008660331873,1.03467846891799),
 .UNSPECIFIED.) ;
#990 = B_SPLINE_CURVE_WITH_KNOTS('',3,(#78491,#78492,#78493,#78494,#78495,
#78496,#78497),.UNSPECIFIED.,.F.,.F.,(4,1,1,1,4),(0.,0.00984040545418749,
0.0229609460597708,0.0328013515139583,0.0459218921195416),.UNSPECIFIED.) ;
#991 = B_SPLINE_CURVE_WITH_KNOTS('',3,(#78547,#78548,#78549,#78550),
 .UNSPECIFIED.,.F.,.F.,(4,4),(-1.12511677037933,-0.0169663179244005),
 .UNSPECIFIED.) ;
#992 = B_SPLINE_CURVE_WITH_KNOTS('',3,(#78610,#78611,#78612,#78613),
 .UNSPECIFIED.,.F.,.F.,(4,4),(0.019875255616694,1.02674783308136),
 .UNSPECIFIED.) ;
#993 = B_SPLINE_CURVE_WITH_KNOTS('',3,(#78678,#78679,#78680,#78681,#78682,
#78683,#78684,#78685,#78686,#78687,#78688,#78689),.UNSPECIFIED.,.F.,.F.,
(4,2,2,2,2,4),(-0.0228953324052163,-0.0161953944372489,-0.0102387878782572,
-0.00528256227931829,-0.00262036469686939,0.),.UNSPECIFIED.) ;
#994 = B_SPLINE_CURVE_WITH_KNOTS('',3,(#78694,#78695,#78696,#78697,#78698,
#78699),.UNSPECIFIED.,.F.,.F.,(4,2,4),(-0.129892307653464,0.,0.00748019188171517),
 .UNSPECIFIED.) ;
#995 = B_SPLINE_CURVE_WITH_KNOTS('',3,(#78941,#78942,#78943,#78944,#78945,
#78946,#78947),.UNSPECIFIED.,.F.,.F.,(4,1,1,1,4),(0.,0.285714285714286,
0.571428571428571,0.857142857142857,1.),.UNSPECIFIED.) ;
#996 = B_SPLINE_CURVE_WITH_KNOTS('',5,(#78975,#78976,#78977,#78978,#78979,
#78980,#78981,#78982,#78983,#78984),.UNSPECIFIED.,.F.,.F.,(6,1,1,1,1,6),
(0.568009935219903,0.6,0.7,0.8,0.9,0.970637147863782),.UNSPECIFIED.) ;
#997 = B_SPLINE_CURVE_WITH_KNOTS('',3,(#79011,#79012,#79013,#79014,#79015),
 .UNSPECIFIED.,.F.,.F.,(4,1,4),(0.,0.500681763148267,1.16825744734596),
 .UNSPECIFIED.) ;
#998 = B_SPLINE_CURVE_WITH_KNOTS('',3,(#79250,#79251,#79252,#79253,#79254,
#79255,#79256,#79257,#79258,#79259),.UNSPECIFIED.,.F.,.F.,(4,2,2,2,4),(-0.000984424941950333,
0.,0.0304393222729151,0.0604225486602068,0.0620633422654789),
 .UNSPECIFIED.) ;
#999 = B_SPLINE_CURVE_WITH_KNOTS('',3,(#79261,#79262,#79263,#79264,#79265,
#79266,#79267,#79268,#79269,#79270,#79271,#79272,#79273,#79274),
 .UNSPECIFIED.,.F.,.F.,(4,2,2,2,2,2,4),(-8.82336995782881E-5,0.,0.00475115835790631,
0.00873436624242474,0.0121992039700031,0.0140206649989405,0.0158413354962278),
 .UNSPECIFIED.) ;
#1000 = B_SPLINE_CURVE_WITH_KNOTS('',3,(#79276,#79277,#79278,#79279,#79280,
#79281,#79282,#79283,#79284,#79285,#79286,#79287,#79288,#79289,#79290,#79291,
#79292,#79293,#79294,#79295,#79296,#79297,#79298,#79299,#79300,#79301,#79302,
#79303,#79304,#79305,#79306,#79307,#79308,#79309),.UNSPECIFIED.,.F.,.F.,
(4,3,3,3,3,3,3,3,3,3,3,4),(-0.0604222015446389,-0.0550499926507643,-0.0493561418638026,
-0.0430468116754606,-0.0361516451437183,-0.0304393667102573,-0.0296323735440378,
-0.0222243385537494,-0.0158108328697019,-0.00982069491557987,-0.00433261667194647,
-2.33582884381498E-7),.UNSPECIFIED.) ;
#1001 = B_SPLINE_CURVE_WITH_KNOTS('',3,(#79310,#79311,#79312,#79313,#79314,
#79315,#79316,#79317,#79318,#79319,#79320,#79321,#79322,#79323),
 .UNSPECIFIED.,.F.,.F.,(4,2,2,2,2,2,4),(-0.0211454388250223,-0.0210285224813978,
-0.0147156589259276,-0.00942919902689826,-0.00482563543048829,-0.00241277839740307,
0.),.UNSPECIFIED.) ;
#1002 = B_SPLINE_CURVE_WITH_KNOTS('',3,(#79366,#79367,#79368,#79369,#79370,
#79371),.UNSPECIFIED.,.F.,.F.,(4,2,4),(-0.0604383125048107,-0.0340909276764841,
-5.87690718515846E-9),.UNSPECIFIED.) ;
#1003 = B_SPLINE_CURVE_WITH_KNOTS('',3,(#79373,#79374,#79375,#79376,#79377,
#79378,#79379,#79380,#79381,#79382,#79383,#79384,#79385,#79386,#79387,#79388,
#79389,#79390,#79391,#79392,#79393,#79394,#79395,#79396,#79397),
 .UNSPECIFIED.,.F.,.F.,(4,3,3,3,3,3,3,3,4),(0.,0.142857141665404,0.284233095225632,
0.427830830943624,0.571428566661616,0.709082623356265,0.846526517857094,
0.983993345114335,1.00000000203212),.UNSPECIFIED.) ;
#1004 = B_SPLINE_CURVE_WITH_KNOTS('',3,(#79399,#79400,#79401,#79402,#79403,
#79404,#79405,#79406),.UNSPECIFIED.,.F.,.F.,(4,2,2,4),(-6.37514627733282E-5,
0.0340909276764841,0.0604383336928468,0.061399226101535),.UNSPECIFIED.) ;
#1005 = B_SPLINE_CURVE_WITH_KNOTS('',3,(#79407,#79408,#79409,#79410,#79411,
#79412,#79413,#79414,#79415,#79416,#79417,#79418,#79419,#79420),
 .UNSPECIFIED.,.F.,.F.,(4,2,2,2,2,2,4),(-0.0211453713160809,-0.0210284730514246,
-0.0147152918429848,-0.00942861499076061,-0.00482456947936517,-0.00241227801516162,
0.),.UNSPECIFIED.) ;
#1006 = B_SPLINE_CURVE_WITH_KNOTS('',3,(#79472,#79473,#79474,#79475,#79476,
#79477,#79478,#79479,#79480,#79481),.UNSPECIFIED.,.F.,.F.,(4,2,2,2,4),(-0.0016406621045341,
0.,0.032656775096122,0.0751675585986371,0.0752925833074644),
 .UNSPECIFIED.) ;
#1007 = B_SPLINE_CURVE_WITH_KNOTS('',3,(#79483,#79484,#79485,#79486,#79487,
#79488,#79489,#79490,#79491,#79492,#79493,#79494,#79495,#79496,#79497,#79498,
#79499,#79500,#79501,#79502,#79503,#79504,#79505,#79506),.UNSPECIFIED.,
 .F.,.F.,(4,2,2,2,2,2,2,2,2,2,2,4),(-0.0405465275427285,-0.0399836298810584,
-0.0342707961683927,-0.0296950430028694,-0.0224465576618196,-0.012906803650382,
-0.0107060635347755,-0.00880130672328058,-0.00614814155262501,-0.00435008553811397,
-0.00226833765470988,0.),.UNSPECIFIED.) ;
#1008 = B_SPLINE_CURVE_WITH_KNOTS('',3,(#79507,#79508,#79509,#79510,#79511,
#79512,#79513,#79514,#79515,#79516,#79517,#79518,#79519,#79520,#79521,#79522,
#79523,#79524,#79525,#79526,#79527,#79528,#79529,#79530,#79531,#79532,#79533,
#79534,#79535,#79536,#79537,#79538,#79539,#79540),.UNSPECIFIED.,.F.,.F.,
(4,3,3,3,3,3,3,3,3,3,3,4),(-0.0751671270593557,-0.0670063003644427,-0.058330620968889,
-0.0493174041305417,-0.0396504587769834,-0.032656775096122,-0.0326552412924559,
-0.0240593424052777,-0.0160879007308648,-0.00858318314202981,-0.00158464448525019,
-1.06159176561375E-7),.UNSPECIFIED.) ;
#1009 = B_SPLINE_CURVE_WITH_KNOTS('',3,(#79607,#79608,#79609,#79610,#79611,
#79612),.UNSPECIFIED.,.F.,.F.,(4,2,4),(-0.0457309983059805,-0.0235600635035843,
-3.22828420435411E-7),.UNSPECIFIED.) ;
#1010 = B_SPLINE_CURVE_WITH_KNOTS('',3,(#79614,#79615,#79616,#79617,#79618,
#79619,#79620,#79621,#79622,#79623),.UNSPECIFIED.,.F.,.F.,(4,2,2,2,4),(-0.00096080851771424,
0.,0.0235600635035843,0.0457311162964727,0.0467303873666823),
 .UNSPECIFIED.) ;
#1011 = B_SPLINE_CURVE_WITH_KNOTS('',3,(#79624,#79625,#79626,#79627,#79628,
#79629,#79630,#79631,#79632,#79633,#79634,#79635,#79636,#79637),
 .UNSPECIFIED.,.F.,.F.,(4,2,2,2,2,2,4),(-8.774851074935E-5,0.,0.00473869223690591,
0.00870703996733189,0.0121629886280889,0.0139740750814815,0.0157851260614204),
 .UNSPECIFIED.) ;
#1012 = B_SPLINE_CURVE_WITH_KNOTS('',3,(#79688,#79689,#79690,#79691,#79692,
#79693,#79694,#79695,#79696,#79697,#79698,#79699,#79700,#79701,#79702,#79703,
#79704,#79705,#79706,#79707,#79708,#79709,#79710,#79711,#79712,#79713,#79714,
#79715),.UNSPECIFIED.,.F.,.F.,(4,3,3,3,3,3,3,3,3,4),(-0.0432143735368821,
-0.0386255934136773,-0.0334465535042506,-0.027720164402335,-0.0217199035575619,
-0.0210041587704275,-0.0147723605623817,-0.00929676450395368,-0.00452143288898869,
-8.08181800291421E-8),.UNSPECIFIED.) ;
#1013 = B_SPLINE_CURVE_WITH_KNOTS('',3,(#79716,#79717,#79718,#79719,#79720,
#79721,#79722,#79723,#79724,#79725),.UNSPECIFIED.,.F.,.F.,(4,2,2,2,4),(-0.000999294135844071,
0.,0.0217198699392343,0.0432144526123464,0.0441989132427654),
 .UNSPECIFIED.) ;
#1014 = B_SPLINE_CURVE_WITH_KNOTS('',3,(#79752,#79753,#79754,#79755,#79756,
#79757),.UNSPECIFIED.,.F.,.F.,(4,2,4),(1.8183290160026E-14,0.0307388136698783,
0.0544948017664183),.UNSPECIFIED.) ;
#1015 = B_SPLINE_CURVE_WITH_KNOTS('',3,(#79763,#79764,#79765,#79766,#79767,
#79768,#79769,#79770),.UNSPECIFIED.,.F.,.F.,(4,2,2,4),(-0.000903812556791651,
0.,0.0126332411015006,0.0312371936251197),.UNSPECIFIED.) ;
#1016 = B_SPLINE_CURVE_WITH_KNOTS('',3,(#79772,#79773,#79774,#79775,#79776,
#79777,#79778,#79779,#79780,#79781),.UNSPECIFIED.,.F.,.F.,(4,2,2,2,4),(-0.000668949496694549,
0.,0.0150950300818429,0.0294213468333971,0.0303251295908459),
 .UNSPECIFIED.) ;
#1017 = B_SPLINE_CURVE_WITH_KNOTS('',3,(#79783,#79784,#79785,#79786,#79787,
#79788,#79789,#79790,#79791,#79792),.UNSPECIFIED.,.F.,.F.,(4,2,2,2,4),(-0.00020740379149845,
0.,0.0232646742763639,0.0410522705936588,0.041721226167804),
 .UNSPECIFIED.) ;
#1018 = B_SPLINE_CURVE_WITH_KNOTS('',3,(#79794,#79795,#79796,#79797,#79798,
#79799,#79800,#79801),.UNSPECIFIED.,.F.,.F.,(4,2,2,4),(-4.75212523545475E-5,
0.0386336727204952,0.0678747004384468,0.0680821984481714),.UNSPECIFIED.) ;
#1019 = B_SPLINE_CURVE_WITH_KNOTS('',3,(#79809,#79810,#79811,#79812,#79813,
#79814),.UNSPECIFIED.,.F.,.F.,(4,2,4),(0.000722157276979357,0.0318468005485353,
0.0667305959449343),.UNSPECIFIED.) ;
#1020 = B_SPLINE_CURVE_WITH_KNOTS('',3,(#79816,#79817,#79818,#79819,#79820,
#79821,#79822,#79823),.UNSPECIFIED.,.F.,.F.,(4,2,2,4),(-0.0369647188766498,
0.,0.0196661092474417,0.0345442295414817),.UNSPECIFIED.) ;
#1021 = B_SPLINE_CURVE_WITH_KNOTS('',3,(#79825,#79826,#79827,#79828,#79829,
#79830,#79831,#79832),.UNSPECIFIED.,.F.,.F.,(4,2,2,4),(0.00145417557171005,
0.0398009040484053,0.0884506599106943,0.125182168962163),.UNSPECIFIED.) ;
#1022 = B_SPLINE_CURVE_WITH_KNOTS('',3,(#79834,#79835,#79836,#79837,#79838,
#79839,#79840,#79841),.UNSPECIFIED.,.F.,.F.,(4,1,2,1,4),(0.000848899917498889,
0.021868453247988,0.0364474220799808,0.0505556257289287,0.070263889237609),
 .UNSPECIFIED.) ;
#1023 = B_SPLINE_CURVE_WITH_KNOTS('',3,(#79843,#79844,#79845,#79846,#79847,
#79848),.UNSPECIFIED.,.F.,.F.,(4,2,4),(0.000832214192100071,0.0289083223985083,
0.0574703491509667),.UNSPECIFIED.) ;
#1024 = B_SPLINE_CURVE_WITH_KNOTS('',3,(#79850,#79851,#79852,#79853,#79854,
#79855,#79856,#79857),.UNSPECIFIED.,.F.,.F.,(4,1,2,1,4),(0.00109423153353252,
0.0104867604235457,0.0262169010588733,0.0371127510104888,0.052624276685899),
 .UNSPECIFIED.) ;
#1025 = B_SPLINE_CURVE_WITH_KNOTS('',3,(#79859,#79860,#79861,#79862,#79863,
#79864),.UNSPECIFIED.,.F.,.F.,(4,2,4),(4.70742900094273E-5,0.0453812948763195,
0.0781603595086036),.UNSPECIFIED.) ;
#1026 = B_SPLINE_CURVE_WITH_KNOTS('',3,(#79877,#79878,#79879,#79880,#79881,
#79882,#79883,#79884,#79885,#79886,#79887,#79888,#79889,#79890,#79891,#79892,
#79893,#79894,#79895,#79896,#79897,#79898),.UNSPECIFIED.,.F.,.F.,(4,2,2,
2,2,2,2,2,2,2,4),(-0.0189100268387207,-0.0188225261357837,-0.0160937127726661,
-0.0140628523915856,-0.0113357098457601,-0.010804126006901,-0.00937481072638454,
-0.00663134068272864,-0.00468727656071559,-0.00196623445923168,0.),
 .UNSPECIFIED.) ;
#1027 = B_SPLINE_CURVE_WITH_KNOTS('',3,(#79905,#79906,#79907,#79908,#79909,
#79910,#79911,#79912,#79913,#79914,#79915,#79916,#79917,#79918,#79919,#79920,
#79921,#79922,#79923,#79924,#79925,#79926),.UNSPECIFIED.,.F.,.F.,(4,2,2,
2,2,2,2,2,2,2,4),(-0.0189091510353225,-0.0188216583950064,-0.0160930867214601,
-0.0140631747980082,-0.0113361362872527,-0.010803887239561,-0.00937541792678878,
-0.00663206984589378,-0.00468769926487486,-0.00196659271288638,0.),
 .UNSPECIFIED.) ;
#1028 = B_SPLINE_CURVE_WITH_KNOTS('',3,(#79969,#79970,#79971,#79972,#79973,
#79974,#79975,#79976,#79977,#79978,#79979,#79980,#79981,#79982,#79983,#79984,
#79985,#79986,#79987,#79988,#79989,#79990,#79991,#79992,#79993,#79994,#79995,
#79996,#79997,#79998,#79999,#80000,#80001,#80002),.UNSPECIFIED.,.F.,.F.,
(4,3,3,3,3,3,3,3,3,3,3,4),(-0.0189104384936197,-0.0188229339990635,-0.0160940759188526,
-0.0140627008849462,-0.011335536637837,-0.0108042382537074,-0.00937452533081662,
-0.00663104829102613,-0.00468707787444879,-0.00196605255282242,-9.10972545172394E-5,
0.),.UNSPECIFIED.) ;
#1029 = B_SPLINE_CURVE_WITH_KNOTS('',3,(#80003,#80004,#80005,#80006,#80007,
#80008),.UNSPECIFIED.,.F.,.F.,(4,2,4),(-0.0678747004384468,-0.0386336727204952,
9.931359662603E-16),.UNSPECIFIED.) ;
#1030 = B_SPLINE_CURVE_WITH_KNOTS('',3,(#80060,#80061,#80062,#80063,#80064,
#80065,#80066,#80067,#80068,#80069,#80070,#80071,#80072,#80073,#80074,#80075,
#80076,#80077,#80078,#80079,#80080,#80081,#80082,#80083,#80084,#80085,#80086,
#80087,#80088,#80089,#80090,#80091,#80092,#80093),.UNSPECIFIED.,.F.,.F.,
(4,3,3,3,3,3,3,3,3,3,3,4),(-0.0189231987523393,-0.0188355768250839,-0.016103896315164,
-0.0140579962341654,-0.0113294935982673,-0.0108077177394999,-0.00936568511698275,
-0.00662104306256861,-0.00468092840563795,-0.00196078713666773,-0.000132076778823899,
0.),.UNSPECIFIED.) ;
#1031 = B_SPLINE_CURVE_WITH_KNOTS('',3,(#80094,#80095,#80096,#80097,#80098,
#80099,#80100,#80101,#80102,#80103,#80104,#80105,#80106,#80107,#80108,#80109,
#80110,#80111,#80112,#80113,#80114,#80115,#80116,#80117,#80118),
 .UNSPECIFIED.,.F.,.F.,(4,3,3,3,3,3,3,3,4),(-0.041052254598462,-0.0353947710294345,
-0.0290069620103994,-0.0232649417665907,-0.0232646742763639,-0.0157599768214883,
-0.00879512539945639,-0.00239829329457513,-6.62284045196766E-9),
 .UNSPECIFIED.) ;
#1032 = B_SPLINE_CURVE_WITH_KNOTS('',3,(#80151,#80152,#80153,#80154,#80155,
#80156),.UNSPECIFIED.,.F.,.F.,(4,2,4),(-0.0792555822118552,-0.0453812948763195,
2.08166817117217E-17),.UNSPECIFIED.) ;
#1033 = B_SPLINE_CURVE_WITH_KNOTS('',3,(#80158,#80159,#80160,#80161,#80162,
#80163,#80164,#80165,#80166,#80167,#80168,#80169,#80170,#80171),
 .UNSPECIFIED.,.F.,.F.,(4,2,2,2,2,2,4),(-8.7816797165505E-5,0.,0.00473925006253047,
0.00870923522712718,0.0121658095680286,0.0139774248519991,0.0157888885985204),
 .UNSPECIFIED.) ;
#1034 = B_SPLINE_CURVE_WITH_KNOTS('',3,(#80223,#80224,#80225,#80226,#80227,
#80228,#80229,#80230,#80231,#80232,#80233,#80234,#80235,#80236,#80237,#80238,
#80239,#80240,#80241,#80242,#80243,#80244,#80245,#80246,#80247,#80248,#80249,
#80250,#80251,#80252,#80253,#80254,#80255,#80256),.UNSPECIFIED.,.F.,.F.,
(4,3,3,3,3,3,3,3,3,3,3,4),(-8.77394398539964E-5,0.,0.00273498567989683,
0.00479398440821394,0.00752394270229122,0.00803717040806658,0.00949060351895224,
0.0122365053916693,0.0141734575442573,0.0168931630703535,0.0187358978034301,
0.0188493460956781),.UNSPECIFIED.) ;
#1035 = B_SPLINE_CURVE_WITH_KNOTS('',3,(#80257,#80258,#80259,#80260,#80261,
#80262),.UNSPECIFIED.,.F.,.F.,(4,2,4),(-0.029421301615743,-0.0150950300818429,
-3.73770280713704E-8),.UNSPECIFIED.) ;
#1036 = B_SPLINE_CURVE_WITH_KNOTS('',3,(#80309,#80310,#80311,#80312,#80313,
#80314,#80315,#80316,#80317,#80318,#80319,#80320,#80321,#80322,#80323,#80324,
#80325,#80326,#80327,#80328,#80329,#80330),.UNSPECIFIED.,.F.,.F.,(4,3,3,
3,3,3,3,4),(-0.0312400832992503,-0.0246244522927767,-0.0173572943526231,
-0.0126332423749213,-0.011908506553527,-0.00595425844831785,-0.000527709717726606,
-1.03431087073348E-8),.UNSPECIFIED.) ;
#1037 = B_SPLINE_CURVE_WITH_KNOTS('',3,(#80386,#80387,#80388,#80389,#80390,
#80391,#80392,#80393),.UNSPECIFIED.,.F.,.F.,(4,1,2,1,4),(-0.0534565259379121,
-0.0371127510104888,-0.0262169010588733,-0.0104867604235457,6.07153216596483E-15),
 .UNSPECIFIED.) ;
#1038 = B_SPLINE_CURVE_WITH_KNOTS('',3,(#80394,#80395,#80396,#80397,#80398,
#80399,#80400,#80401,#80402,#80403,#80404,#80405,#80406,#80407,#80408,#80409,
#80410,#80411,#80412,#80413,#80414,#80415,#80416,#80417,#80418,#80419,#80420,
#80421,#80422,#80423,#80424,#80425,#80426,#80427),.UNSPECIFIED.,.F.,.F.,
(4,3,3,3,3,3,3,3,3,3,3,4),(-0.0189309682305329,-0.0188432744075911,-0.0161088065138652,
-0.0140551360522483,-0.0113261441011701,-0.0108100283879569,-0.0108098271232967,
-0.00936033610026891,-0.00661505228534929,-0.00467721248496698,-0.00195726652153048,
0.),.UNSPECIFIED.) ;
#1039 = B_SPLINE_CURVE_WITH_KNOTS('',3,(#80459,#80460,#80461,#80462,#80463,
#80464,#80465,#80466,#80467,#80468,#80469,#80470,#80471,#80472,#80473,#80474,
#80475,#80476,#80477,#80478,#80479,#80480,#80481,#80482,#80483,#80484,#80485,
#80486,#80487,#80488,#80489,#80490,#80491,#80492,#80493,#80494,#80495,#80496,
#80497,#80498),.UNSPECIFIED.,.F.,.F.,(4,3,3,3,3,3,3,3,3,3,3,3,3,4),(-0.0583191426684248,
-0.0515202234042521,-0.0455591618953523,-0.0399214617427771,-0.034414844098878,
-0.0316615352769285,-0.0302848808659537,-0.0294521489819769,-0.028908226454979,
-0.0238511390677379,-0.0185352795979771,-0.0127504766938683,-0.00631797168678906,
1.19054072156493E-14),.UNSPECIFIED.) ;
#1040 = B_SPLINE_CURVE_WITH_KNOTS('',3,(#80499,#80500,#80501,#80502,#80503,
#80504,#80505,#80506,#80507,#80508,#80509,#80510,#80511,#80512,#80513,#80514,
#80515,#80516,#80517,#80518,#80519,#80520,#80521,#80522,#80523,#80524,#80525,
#80526,#80527,#80528,#80529,#80530,#80531,#80532),.UNSPECIFIED.,.F.,.F.,
(4,3,3,3,3,3,3,3,3,3,3,4),(-8.77110797273226E-5,0.,0.00273520643559201,
0.00478983254758793,0.00751988059915136,0.0080349187065388,0.00803514813958154,
0.00948541104957732,0.0122325784356822,0.0141688418023582,0.0168884919204612,
0.0188461231184326),.UNSPECIFIED.) ;
#1041 = B_SPLINE_CURVE_WITH_KNOTS('',3,(#80574,#80575,#80576,#80577,#80578,
#80579,#80580,#80581),.UNSPECIFIED.,.F.,.F.,(4,1,2,1,4),(-0.0717179312023507,
-0.0505556257289287,-0.0364474220799808,-0.021868453247988,1.21551489931584E-15),
 .UNSPECIFIED.) ;
#1042 = B_SPLINE_CURVE_WITH_KNOTS('',3,(#80582,#80583,#80584,#80585,#80586,
#80587,#80588,#80589,#80590,#80591,#80592,#80593,#80594,#80595,#80596,#80597,
#80598,#80599,#80600,#80601,#80602,#80603,#80604,#80605,#80606,#80607,#80608,
#80609,#80610,#80611,#80612,#80613,#80614,#80615,#80616,#80617,#80618),
 .UNSPECIFIED.,.F.,.F.,(4,3,3,3,3,3,3,3,3,3,3,3,4),(-0.0189757898193099,
-0.0188876825104194,-0.016141250710988,-0.0140385129384437,-0.0113059119834885,
-0.0108221873966673,-0.0108220365581979,-0.00932947344905913,-0.00658072601880498,
-0.00465582700007615,-0.00270420596151227,-0.00193828076950875,0.),
 .UNSPECIFIED.) ;
#1043 = B_SPLINE_CURVE_WITH_KNOTS('',3,(#80668,#80669,#80670,#80671,#80672,
#80673),.UNSPECIFIED.,.F.,.F.,(4,2,4),(-0.0884477485126169,-0.0398009040484053,
3.34298561055327E-14),.UNSPECIFIED.) ;
#1044 = B_SPLINE_CURVE_WITH_KNOTS('',3,(#80674,#80675,#80676,#80677,#80678,
#80679,#80680,#80681,#80682,#80683,#80684,#80685,#80686,#80687),
 .UNSPECIFIED.,.F.,.F.,(4,2,2,2,2,2,4),(-0.000257748868228079,0.,0.0227861491765853,
0.0430952613497541,0.0513731219354545,0.0545021507438859,0.0573049792139941),
 .UNSPECIFIED.) ;
#1045 = B_SPLINE_CURVE_WITH_KNOTS('',3,(#80729,#80730,#80731,#80732,#80733,
#80734),.UNSPECIFIED.,.F.,.F.,(4,2,4),(-0.0352658770408685,-0.0196661092474417,
3.06681289893858E-7),.UNSPECIFIED.) ;
#1046 = B_SPLINE_CURVE_WITH_KNOTS('',3,(#80735,#80736,#80737,#80738,#80739,
#80740,#80741,#80742,#80743,#80744,#80745,#80746,#80747,#80748,#80749,#80750,
#80751,#80752,#80753,#80754,#80755,#80756,#80757,#80758,#80759,#80760,#80761,
#80762,#80763,#80764,#80765),.UNSPECIFIED.,.F.,.F.,(4,3,3,3,3,3,3,3,3,3,
4),(-0.0189255450014105,-0.0188379011808369,-0.0161048586406479,-0.0140571373249443,
-0.0113284598467218,-0.010808352019202,-0.00936407769447349,-0.00661884257235523,
-0.00467981132905438,-0.00195973370921565,0.),.UNSPECIFIED.) ;
#1047 = B_SPLINE_CURVE_WITH_KNOTS('',3,(#80796,#80797,#80798,#80799,#80800,
#80801,#80802,#80803,#80804,#80805,#80806,#80807,#80808,#80809,#80810,#80811,
#80812,#80813,#80814,#80815,#80816,#80817,#80818,#80819,#80820,#80821,#80822,
#80823,#80824,#80825,#80826,#80827,#80828,#80829),.UNSPECIFIED.,.F.,.F.,
(4,3,3,3,3,3,3,3,3,3,3,4),(-0.0669038356909525,-0.0556776653306576,-0.0448761350683132,
-0.0383614116366248,-0.0351040499207806,-0.0332964637419825,-0.0320905242267506,
-0.0318466882049363,-0.0219526243138846,-0.0116986697167936,-0.000861115342412766,
0.),.UNSPECIFIED.) ;
#1048 = B_SPLINE_CURVE_WITH_KNOTS('',3,(#80843,#80844,#80845,#80846,#80847,
#80848),.UNSPECIFIED.,.F.,.F.,(4,2,4),(5.55111512312578E-17,0.0224201537133612,
0.0402049184529),.UNSPECIFIED.) ;
#1049 = B_SPLINE_CURVE_WITH_KNOTS('',3,(#80862,#80863,#80864,#80865,#80866,
#80867),.UNSPECIFIED.,.F.,.F.,(4,2,4),(9.61380643681049E-9,0.033998052296077,
0.0714229819360441),.UNSPECIFIED.) ;
#1050 = B_SPLINE_CURVE_WITH_KNOTS('',3,(#80892,#80893,#80894,#80895,#80896,
#80897),.UNSPECIFIED.,.F.,.F.,(4,2,4),(5.83560977318598E-15,0.0377278926030736,
0.066283338281117),.UNSPECIFIED.) ;
#1051 = B_SPLINE_CURVE_WITH_KNOTS('',3,(#80910,#80911,#80912,#80913,#80914,
#80915),.UNSPECIFIED.,.F.,.F.,(4,2,4),(-2.77555756156289E-17,0.0199847249930681,
0.0352638829354677),.UNSPECIFIED.) ;
#1052 = B_SPLINE_CURVE_WITH_KNOTS('',3,(#80928,#80929,#80930,#80931,#80932,
#80933,#80934,#80935,#80936,#80937,#80938,#80939,#80940,#80941,#80942,#80943,
#80944,#80945,#80946,#80947,#80948,#80949,#80950,#80951,#80952,#80953,#80954,
#80955,#80956,#80957,#80958,#80959,#80960,#80961),.UNSPECIFIED.,.F.,.F.,
(4,3,3,3,3,3,3,3,3,3,3,4),(-4.8815118613983E-15,0.0033937817965806,0.00647026806505026,
0.00922156932779166,0.0105972199591624,0.0112850452748477,0.0117100374865891,
0.0119728705905331,0.0145178026139032,0.0173664913107944,0.0204777162912316,
0.023335857822899),.UNSPECIFIED.) ;
#1053 = B_SPLINE_CURVE_WITH_KNOTS('',3,(#80974,#80975,#80976,#80977,#80978,
#80979),.UNSPECIFIED.,.F.,.F.,(4,2,4),(-3.37568514807661E-14,0.0112807751130659,
0.0278959164324805),.UNSPECIFIED.) ;
#1054 = B_SPLINE_CURVE_WITH_KNOTS('',3,(#81026,#81027,#81028,#81029,#81030,
#81031,#81032,#81033),.UNSPECIFIED.,.F.,.F.,(4,1,2,1,4),(-0.0331275497757554,
-0.0275093508272253,-0.0175825659440626,-0.0105495395664116,-0.000960732822002768),
 .UNSPECIFIED.) ;
#1055 = B_SPLINE_CURVE_WITH_KNOTS('',3,(#81034,#81035,#81036,#81037,#81038,
#81039,#81040,#81041,#81042,#81043,#81044,#81045,#81046,#81047),
 .UNSPECIFIED.,.F.,.F.,(4,2,2,2,2,2,4),(-8.76821873054501E-5,0.,0.00473755893099621,
0.0087048318969467,0.0121603865659108,0.0139701425181185,0.0157799606242108),
 .UNSPECIFIED.) ;
#1056 = B_SPLINE_CURVE_WITH_KNOTS('',3,(#81049,#81050,#81051,#81052,#81053,
#81054,#81055,#81056),.UNSPECIFIED.,.F.,.F.,(4,1,2,1,4),(-6.50365178378404E-14,
0.0105495395664116,0.0175825659440626,0.0275093508272253,0.0341272074160004),
 .UNSPECIFIED.) ;
#1057 = B_SPLINE_CURVE_WITH_KNOTS('',3,(#81057,#81058,#81059,#81060,#81061,
#81062,#81063,#81064,#81065,#81066,#81067,#81068,#81069,#81070),
 .UNSPECIFIED.,.F.,.F.,(4,2,2,2,2,2,4),(-0.0211469908685138,-0.0210301208681755,
-0.0147166592526885,-0.00942972110677525,-0.00482452106724603,-0.00241229268713677,
0.),.UNSPECIFIED.) ;
#1058 = B_SPLINE_CURVE_WITH_KNOTS('',3,(#81073,#81074,#81075,#81076,#81077,
#81078,#81079,#81080,#81081,#81082,#81083,#81084,#81085,#81086,#81087,#81088),
 .UNSPECIFIED.,.F.,.F.,(4,2,2,2,2,2,2,4),(0.,0.226168647000758,0.452278992039162,
0.678340117421019,0.90457233447104,1.13067979945043,1.35690435214638,1.57080531075693),
 .UNSPECIFIED.) ;
#1059 = B_SPLINE_CURVE_WITH_KNOTS('',3,(#81096,#81097,#81098,#81099,#81100,
#81101,#81102,#81103,#81104,#81105,#81106,#81107,#81108,#81109,#81110,#81111,
#81112,#81113,#81114,#81115,#81116,#81117),.UNSPECIFIED.,.F.,.F.,(4,2,2,
2,2,2,2,2,2,2,4),(-0.018909573318621,-0.0188220768043535,-0.016093251639432,
-0.0140630190939924,-0.0113315789493842,-0.0108040023625357,-0.00937512502025987,
-0.006640358962904,-0.00468749542006272,-0.00270182786113088,0.),
 .UNSPECIFIED.) ;
#1060 = B_SPLINE_CURVE_WITH_KNOTS('',3,(#81162,#81163,#81164,#81165,#81166,
#81167,#81168,#81169,#81170,#81171,#81172,#81173,#81174,#81175,#81176,#81177,
#81178,#81179,#81180,#81181,#81182,#81183,#81184,#81185,#81186,#81187,#81188,
#81189,#81190,#81191,#81192,#81193,#81194,#81195,#81196,#81197,#81198,#81199,
#81200,#81201,#81202,#81203,#81204),.UNSPECIFIED.,.F.,.F.,(4,3,3,3,3,3,
3,3,3,3,3,3,3,3,4),(-8.68229099727415E-16,0.00603095577270896,0.0112970853615661,
0.0160979596706912,0.0206419392505884,0.0248678312070903,0.0270954741281374,
0.0275760705491088,0.0325996412774412,0.0378159722742326,0.0426458767484477,
0.0483565421817521,0.054471144104918,0.0614210976336497,0.062393728839361),
 .UNSPECIFIED.) ;
#1061 = B_SPLINE_CURVE_WITH_KNOTS('',3,(#81206,#81207,#81208,#81209,#81210,
#81211,#81212),.UNSPECIFIED.,.F.,.F.,(4,1,2,4),(-0.0622686948925872,-0.0412193079076597,
-0.0271030272865255,-0.00164197031784536),.UNSPECIFIED.) ;
#1062 = B_SPLINE_CURVE_WITH_KNOTS('',3,(#81213,#81214,#81215,#81216,#81217,
#81218,#81219,#81220,#81221,#81222,#81223,#81224,#81225,#81226),
 .UNSPECIFIED.,.F.,.F.,(4,2,2,2,2,2,4),(-0.0264075038978238,-0.0262264477757636,
-0.0165688239045476,-0.00981534868988691,-0.00481983637094454,-0.0024018084974946,
0.),.UNSPECIFIED.) ;
#1063 = B_SPLINE_CURVE_WITH_KNOTS('',3,(#81284,#81285,#81286,#81287,#81288,
#81289,#81290,#81291,#81292,#81293,#81294,#81295,#81296,#81297,#81298,#81299,
#81300,#81301,#81302,#81303,#81304,#81305,#81306,#81307,#81308,#81309,#81310,
#81311,#81312,#81313,#81314,#81315,#81316,#81317,#81318,#81319,#81320,#81321,
#81322,#81323,#81324,#81325,#81326,#81327,#81328,#81329,#81330,#81331,#81332,
#81333,#81334,#81335),.UNSPECIFIED.,.F.,.F.,(4,3,3,3,3,3,3,3,3,3,3,3,3,
3,3,3,3,4),(0.,0.00450947947892499,0.00841902259411946,0.00901895895784998,
0.0124006553358025,0.015294160794407,0.0180109586247333,0.0204951745201462,
0.0225457444696602,0.0225473973946249,0.0251046180458128,0.0269891467103356,
0.0296981883061816,0.0314308960260463,0.0349082131518329,0.0386648400573158,
0.0430428695384302,0.0447561439731784),.UNSPECIFIED.) ;
#1064 = B_SPLINE_CURVE_WITH_KNOTS('',3,(#81337,#81338,#81339,#81340,#81341,
#81342,#81343,#81344,#81345),.UNSPECIFIED.,.F.,.F.,(4,1,1,2,1,4),(-0.043116371938142,
-0.0314308960260463,-0.0269891467103356,-0.0225473973946249,-0.00901895895784998,
-0.00098511887011706),.UNSPECIFIED.) ;
#1065 = B_SPLINE_CURVE_WITH_KNOTS('',3,(#81346,#81347,#81348,#81349,#81350,
#81351,#81352,#81353,#81354,#81355,#81356,#81357,#81358,#81359,#81360,#81361,
#81362,#81363,#81364,#81365,#81366,#81367,#81368,#81369,#81370,#81371,#81372,
#81373,#81374,#81375,#81376,#81377,#81378,#81379,#81380,#81381,#81382,#81383,
#81384,#81385),.UNSPECIFIED.,.F.,.F.,(4,3,3,3,3,3,3,3,3,3,3,3,3,4),(-8.77879354781158E-5,
0.,0.00252798145936727,0.00273454309078326,0.00480081491969721,0.00753353483528674,
0.00804095404153383,0.00804321999015075,0.00949906978678616,0.0122336738715351,
0.0134513299663313,0.0141810106313358,0.0169048836436778,0.0188547055635755),
 .UNSPECIFIED.) ;
#1066 = B_SPLINE_CURVE_WITH_KNOTS('',3,(#81426,#81427,#81428,#81429,#81430,
#81431,#81432,#81433,#81434,#81435,#81436,#81437,#81438,#81439,#81440,#81441,
#81442,#81443,#81444,#81445,#81446,#81447,#81448,#81449,#81450,#81451,#81452,
#81453,#81454,#81455,#81456,#81457,#81458,#81459,#81460,#81461,#81462,#81463,
#81464,#81465,#81466,#81467,#81468,#81469,#81470,#81471),.UNSPECIFIED.,
 .F.,.F.,(4,3,3,3,3,3,3,3,3,3,3,3,3,3,3,4),(-3.8936437845742E-15,0.00412980358625654,
0.0073953121092872,0.0102645357852797,0.0129835018205587,0.0147513580827983,
0.0156352862139181,0.0161055136169195,0.0164277850761292,0.0165192143450379,
0.0190242492168354,0.0217091716190259,0.024723772049841,0.0271062306444131,
0.0309150163721508,0.0328614318196219),.UNSPECIFIED.) ;
#1067 = B_SPLINE_CURVE_WITH_KNOTS('',3,(#81472,#81473,#81474,#81475,#81476,
#81477,#81478,#81479),.UNSPECIFIED.,.F.,.F.,(4,1,2,1,4),(-0.0318767983081372,
-0.0263234394910323,-0.016516450998148,-0.00990987059888721,-0.0010005474151551),
 .UNSPECIFIED.) ;
#1068 = B_SPLINE_CURVE_WITH_KNOTS('',3,(#81510,#81511,#81512,#81513,#81514,
#81515),.UNSPECIFIED.,.F.,.F.,(4,2,4),(-0.0535332247771704,-0.0307388136698783,
-6.37552332398931E-5),.UNSPECIFIED.) ;
#1069 = B_SPLINE_CURVE_WITH_KNOTS('',3,(#81614,#81615,#81616,#81617,#81618,
#81619,#81620,#81621,#81622,#81623,#81624,#81625,#81626,#81627,#81628,#81629,
#81630,#81631,#81632,#81633),.UNSPECIFIED.,.F.,.F.,(4,2,2,2,2,2,2,2,2,4),
(-0.0576966986557776,-0.0574332020643026,-0.0527195345357808,-0.0451607359259123,
-0.0302726022898489,-0.0168228643688311,-0.0103578801382715,-0.00596969171523668,
-0.00327048355186457,0.),.UNSPECIFIED.) ;
#1070 = B_SPLINE_CURVE_WITH_KNOTS('',3,(#81686,#81687,#81688,#81689,#81690,
#81691,#81692,#81693,#81694,#81695),.UNSPECIFIED.,.F.,.F.,(4,2,2,2,4),(-0.0715962154387296,
-0.0714230469344481,-0.033998052296077,0.,0.000721914453027042),
 .UNSPECIFIED.) ;
#1071 = B_SPLINE_CURVE_WITH_KNOTS('',3,(#81696,#81697,#81698,#81699,#81700,
#81701,#81702,#81703,#81704,#81705,#81706,#81707,#81708,#81709,#81710,#81711,
#81712,#81713,#81714,#81715,#81716,#81717,#81718,#81719,#81720,#81721,#81722,
#81723,#81724,#81725,#81726,#81727,#81728,#81729),.UNSPECIFIED.,.F.,.F.,
(4,3,3,3,3,3,3,3,3,3,3,4),(-8.76499876818703E-5,0.,0.00273272879714876,
0.00478109970919887,0.00750990480829954,0.00803013500119809,0.00947451694969623,
0.0122195242547994,0.0141591392154495,0.0168794617448153,0.0187493114075714,
0.0188393055184181),.UNSPECIFIED.) ;
#1072 = B_SPLINE_CURVE_WITH_KNOTS('',3,(#81771,#81772,#81773,#81774,#81775,
#81776),.UNSPECIFIED.,.F.,.F.,(4,2,4),(-0.0409268414934542,-0.0402049350827121,
-0.0322019631637999),.UNSPECIFIED.) ;
#1073 = B_SPLINE_CURVE_WITH_KNOTS('',3,(#81777,#81778,#81779,#81780,#81781,
#81782,#81783,#81784,#81785,#81786,#81787,#81788,#81789,#81790),
 .UNSPECIFIED.,.F.,.F.,(4,2,2,2,2,2,4),(-0.0287724923583598,-0.0286527043683762,
-0.0151123592994182,-0.00653065970956893,-0.00288793000485767,-0.00137884937746232,
0.),.UNSPECIFIED.) ;
#1074 = B_SPLINE_CURVE_WITH_KNOTS('',3,(#81838,#81839,#81840,#81841,#81842,
#81843,#81844,#81845),.UNSPECIFIED.,.F.,.F.,(4,2,2,4),(-0.0689415808684068,
-0.0452350077421772,0.,0.00145402880520905),.UNSPECIFIED.) ;
#1075 = B_SPLINE_CURVE_WITH_KNOTS('',3,(#81847,#81848,#81849,#81850,#81851,
#81852,#81853,#81854,#81855,#81856,#81857,#81858,#81859,#81860),
 .UNSPECIFIED.,.F.,.F.,(4,2,2,2,2,2,4),(-8.81034153357365E-5,0.,0.00474653617288703,
0.00872474084759045,0.0121859542723517,0.0140038756503188,0.0158211901338128),
 .UNSPECIFIED.) ;
#1076 = B_SPLINE_CURVE_WITH_KNOTS('',3,(#81861,#81862,#81863,#81864,#81865,
#81866),.UNSPECIFIED.,.F.,.F.,(4,2,4),(1.07296738594995E-7,0.0452350077421772,
0.100520135955306),.UNSPECIFIED.) ;
#1077 = B_SPLINE_CURVE_WITH_KNOTS('',3,(#81918,#81919,#81920,#81921,#81922,
#81923,#81924,#81925,#81926,#81927),.UNSPECIFIED.,.F.,.F.,(4,2,2,2,4),(-0.0870620753300636,
-0.0856081292457083,-0.0435056845362515,0.,0.000848777061136591),
 .UNSPECIFIED.) ;
#1078 = B_SPLINE_CURVE_WITH_KNOTS('',3,(#81929,#81930,#81931,#81932,#81933,
#81934,#81935,#81936,#81937,#81938,#81939,#81940,#81941,#81942,#81943,#81944,
#81945,#81946,#81947,#81948,#81949,#81950,#81951,#81952,#81953,#81954,#81955,
#81956,#81957,#81958,#81959,#81960,#81961,#81962),.UNSPECIFIED.,.F.,.F.,
(4,3,3,3,3,3,3,3,3,3,3,4),(-0.0189318067161962,-0.0188441055189667,-0.0161139390575287,
-0.0140548164804191,-0.0113247732297175,-0.0108100655848069,-0.00935972898436879,
-0.00661354647959299,-0.00467678954238819,-0.00195798115489982,-0.000183016470591954,
0.),.UNSPECIFIED.) ;
#1079 = B_SPLINE_CURVE_WITH_KNOTS('',3,(#81963,#81964,#81965,#81966,#81967,
#81968),.UNSPECIFIED.,.F.,.F.,(4,2,4),(7.47511594064578E-8,0.0435056845362515,
0.0856079410889234),.UNSPECIFIED.) ;
#1080 = B_SPLINE_CURVE_WITH_KNOTS('',3,(#82020,#82021,#82022,#82023,#82024,
#82025,#82026,#82027,#82028,#82029),.UNSPECIFIED.,.F.,.F.,(4,2,2,2,4),(-0.0691265383481362,
-0.0682776647009788,-0.0338448162467367,0.,0.000832239105180238),
 .UNSPECIFIED.) ;
#1081 = B_SPLINE_CURVE_WITH_KNOTS('',3,(#82031,#82032,#82033,#82034,#82035,
#82036,#82037,#82038,#82039,#82040,#82041,#82042,#82043,#82044,#82045,#82046,
#82047,#82048,#82049,#82050,#82051,#82052,#82053,#82054,#82055,#82056,#82057,
#82058,#82059,#82060,#82061,#82062,#82063,#82064),.UNSPECIFIED.,.F.,.F.,
(4,3,3,3,3,3,3,3,3,3,3,4),(-8.7701944723502E-5,0.,0.00273259197152701,0.00478857188803212,
0.00751836784307051,0.00803421626080498,0.00948384878366692,0.0122297141375811,
0.0141674461840516,0.0168870659675853,0.0186680252920398,0.0188451300988223),
 .UNSPECIFIED.) ;
#1082 = B_SPLINE_CURVE_WITH_KNOTS('',3,(#82065,#82066,#82067,#82068,#82069,
#82070),.UNSPECIFIED.,.F.,.F.,(4,2,4),(4.92710764161277E-8,0.0338448162467367,
0.0682776016463813),.UNSPECIFIED.) ;
#1083 = B_SPLINE_CURVE_WITH_KNOTS('',3,(#82122,#82123,#82124,#82125,#82126,
#82127,#82128,#82129,#82130,#82131),.UNSPECIFIED.,.F.,.F.,(4,2,2,2,4),(-0.0663005130080268,
-0.065468485698588,-0.0321085924337593,0.,0.00109408852437443),
 .UNSPECIFIED.) ;
#1084 = B_SPLINE_CURVE_WITH_KNOTS('',3,(#82133,#82134,#82135,#82136,#82137,
#82138,#82139,#82140,#82141,#82142,#82143,#82144,#82145,#82146),
 .UNSPECIFIED.,.F.,.F.,(4,2,2,2,2,2,4),(-0.02115345221426,-0.0210364437818934,
-0.0147219471919079,-0.0094328410561899,-0.0048279676271279,-0.00241386739955191,
0.),.UNSPECIFIED.) ;
#1085 = B_SPLINE_CURVE_WITH_KNOTS('',3,(#82147,#82148,#82149,#82150,#82151,
#82152),.UNSPECIFIED.,.F.,.F.,(4,2,4),(2.55629243344565E-7,0.0321085924337593,
0.0654684152026825),.UNSPECIFIED.) ;
#1086 = B_SPLINE_CURVE_WITH_KNOTS('',3,(#82194,#82195,#82196,#82197,#82198,
#82199,#82200,#82201),.UNSPECIFIED.,.F.,.F.,(4,2,2,4),(-0.0866902249621159,
-0.085595699976472,-0.0490110014082998,4.70756737529766E-5),
 .UNSPECIFIED.) ;
#1087 = B_SPLINE_CURVE_WITH_KNOTS('',3,(#82203,#82204,#82205,#82206,#82207,
#82208,#82209,#82210,#82211,#82212,#82213,#82214,#82215,#82216,#82217,#82218,
#82219,#82220,#82221,#82222,#82223,#82224),.UNSPECIFIED.,.F.,.F.,(4,2,2,
2,2,2,2,2,2,2,4),(-0.0189091497005805,-0.0188216570693507,-0.0160930875609983,
-0.0140631752914572,-0.0113361432619141,-0.0108038868757659,-0.00937541885348054,
-0.0066320839853287,-0.00468769990948291,-0.00196658907698825,0.),
 .UNSPECIFIED.) ;
#1088 = B_SPLINE_CURVE_WITH_KNOTS('',3,(#82225,#82226,#82227,#82228,#82229,
#82230,#82231,#82232,#82233,#82234,#82235,#82236,#82237,#82238,#82239,#82240,
#82241,#82242,#82243,#82244,#82245,#82246,#82247,#82248,#82249),
 .UNSPECIFIED.,.F.,.F.,(4,3,3,3,3,3,3,3,4),(1.57509957900154E-9,0.0132911426638058,
0.0269830849249619,0.0413877831821161,0.0490109714954551,0.0505389692183738,
0.0629605951743031,0.07447082612909,0.0855956752503445),.UNSPECIFIED.) ;
#1089 = B_SPLINE_CURVE_WITH_KNOTS('',3,(#82306,#82307,#82308,#82309,#82310,
#82311),.UNSPECIFIED.,.F.,.F.,(4,2,4),(-0.0278988061061053,-0.0112807751130659,
-0.000904379645874189),.UNSPECIFIED.) ;
#1090 = B_SPLINE_CURVE_WITH_KNOTS('',3,(#82312,#82313,#82314,#82315,#82316,
#82317,#82318,#82319,#82320,#82321,#82322,#82323,#82324,#82325),
 .UNSPECIFIED.,.F.,.F.,(4,2,2,2,2,2,4),(-0.0211430029019927,-0.0210263115451312,
-0.0147124541559798,-0.00942707088034509,-0.00482159977281412,-0.00241097745669264,
0.),.UNSPECIFIED.) ;
#1091 = B_SPLINE_CURVE_WITH_KNOTS('',3,(#82359,#82360,#82361,#82362,#82363,
#82364),.UNSPECIFIED.,.F.,.F.,(4,2,4),(-0.0224313406438007,-0.0119728599231917,
-0.000668626710861112),.UNSPECIFIED.) ;
#1092 = B_SPLINE_CURVE_WITH_KNOTS('',3,(#82365,#82366,#82367,#82368,#82369,
#82370,#82371,#82372,#82373,#82374,#82375,#82376,#82377,#82378,#82379,#82380,
#82381,#82382,#82383,#82384,#82385,#82386,#82387,#82388,#82389,#82390,#82391,
#82392,#82393,#82394,#82395),.UNSPECIFIED.,.F.,.F.,(4,3,3,3,3,3,3,3,3,3,
4),(-8.7628829834679E-5,0.,0.00273270250618685,0.00477794884587875,0.00750683894428588,
0.00802843590815977,0.00947056618272019,0.0122165071757717,0.0141556306430289,
0.0168758245379607,0.0188368670291837),.UNSPECIFIED.) ;
#1093 = B_SPLINE_CURVE_WITH_KNOTS('',3,(#82427,#82428,#82429,#82430,#82431,
#82432),.UNSPECIFIED.,.F.,.F.,(4,2,4),(-0.0345946589883076,-0.0199847249930681,
-0.000207524979791521),.UNSPECIFIED.) ;
#1094 = B_SPLINE_CURVE_WITH_KNOTS('',3,(#82433,#82434,#82435,#82436,#82437,
#82438,#82439,#82440,#82441,#82442,#82443,#82444,#82445,#82446,#82447,#82448,
#82449,#82450,#82451,#82452,#82453,#82454,#82455,#82456,#82457,#82458,#82459,
#82460,#82461,#82462,#82463),.UNSPECIFIED.,.F.,.F.,(4,3,3,3,3,3,3,3,3,3,
4),(-8.75050552364877E-5,0.,0.00272897052667188,0.00476026345104745,0.00748754551043703,
0.00801874653963784,0.00944846844817684,0.0121921607137149,0.0141359453584198,
0.0168569193374903,0.0188230526768059),.UNSPECIFIED.) ;
#1095 = B_SPLINE_CURVE_WITH_KNOTS('',3,(#82494,#82495,#82496,#82497,#82498,
#82499),.UNSPECIFIED.,.F.,.F.,(4,2,4),(-0.0660759331217695,-0.0377278926030736,
-4.752274878301E-5),.UNSPECIFIED.) ;
#1096 = B_SPLINE_CURVE_WITH_KNOTS('',3,(#83139,#83140,#83141,#83142,#83143,
#83144),.UNSPECIFIED.,.F.,.F.,(4,2,4),(-0.019402604569559,-0.0117562819132928,
0.),.UNSPECIFIED.) ;
#1097 = B_SPLINE_CURVE_WITH_KNOTS('',3,(#83148,#83149,#83150,#83151,#83152,
#83153),.UNSPECIFIED.,.F.,.F.,(4,2,4),(-0.069955828573411,-0.0581995466601174,
-0.0505532240038506),.UNSPECIFIED.) ;
#1098 = B_SPLINE_CURVE_WITH_KNOTS('',3,(#83283,#83284,#83285,#83286,#83287,
#83288),.UNSPECIFIED.,.F.,.F.,(4,2,4),(-0.069955828573407,-0.0581995466601109,
-0.05055322400384),.UNSPECIFIED.) ;
#1099 = B_SPLINE_CURVE_WITH_KNOTS('',3,(#83307,#83308,#83309,#83310,#83311,
#83312),.UNSPECIFIED.,.F.,.F.,(4,2,4),(-0.0194026045695706,-0.0117562819132982,
3.46944695195361E-18),.UNSPECIFIED.) ;
#1100 = B_SPLINE_CURVE_WITH_KNOTS('',3,(#83317,#83318,#83319,#83320,#83321,
#83322),.UNSPECIFIED.,.F.,.F.,(4,2,4),(-0.0699558285734111,-0.0581995466601248,
-0.0505532240038628),.UNSPECIFIED.) ;
#1101 = B_SPLINE_CURVE_WITH_KNOTS('',3,(#83345,#83346,#83347,#83348,#83349,
#83350),.UNSPECIFIED.,.F.,.F.,(4,2,4),(-0.019402604569559,-0.0117562819132928,
0.),.UNSPECIFIED.) ;
#1102 = B_SPLINE_CURVE_WITH_KNOTS('',3,(#83408,#83409,#83410,#83411,#83412,
#83413,#83414,#83415,#83416,#83417,#83418,#83419,#83420,#83421,#83422,#83423,
#83424,#83425),.UNSPECIFIED.,.T.,.F.,(4,1,1,1,1,1,1,1,1,1,1,1,1,1,1,4),
(-1.24903384766071,-1.07060044085204,-0.892167034043367,-0.713733627234693,
-0.53530022042602,-0.356866813617347,-0.178433406808673,0.0594778022695577,
0.118955604539115,0.178433406808673,0.356866813617347,0.53530022042602,
0.713733627234693,0.892167034043367,1.07060044085204,1.24903384766071),
 .UNSPECIFIED.) ;
#1103 = B_SPLINE_CURVE_WITH_KNOTS('',3,(#83662,#83663,#83664,#83665,#83666),
 .UNSPECIFIED.,.F.,.F.,(4,1,4),(-1.,-0.571428571428571,0.),
 .UNSPECIFIED.) ;
#1104 = B_SPLINE_CURVE_WITH_KNOTS('',3,(#83668,#83669,#83670,#83671,#83672,
#83673,#83674,#83675,#83676,#83677,#83678,#83679,#83680,#83681,#83682,#83683,
#83684,#83685),.UNSPECIFIED.,.F.,.F.,(4,1,1,1,1,1,1,1,1,1,1,1,1,1,1,4),
(-1.24887231172908,-1.07060044085204,-0.892167034043367,-0.713733627234693,
-0.53530022042602,-0.356866813617347,-0.178433406808673,-0.118955604539115,
-0.0594778022695577,0.178433406808673,0.356866813617347,0.53530022042602,
0.713733627234693,0.892167034043367,1.07060044085204,1.24854837899851),
 .UNSPECIFIED.) ;
#1105 = B_SPLINE_CURVE_WITH_KNOTS('',3,(#83738,#83739,#83740,#83741,#83742),
 .UNSPECIFIED.,.F.,.F.,(4,1,4),(0.270884354171361,0.773477463983206,1.5707963267949),
 .UNSPECIFIED.) ;
#1106 = B_SPLINE_CURVE_WITH_KNOTS('',3,(#83747,#83748,#83749,#83750,#83751),
 .UNSPECIFIED.,.F.,.F.,(4,1,4),(-1.57079632679489,-0.972068585273428,-0.27088435417137),
 .UNSPECIFIED.) ;
#1107 = B_SPLINE_CURVE_WITH_KNOTS('',3,(#83787,#83788,#83789,#83790,#83791),
 .UNSPECIFIED.,.F.,.F.,(4,1,4),(-1.57079632679489,-0.972068585274832,-0.27088435417136),
 .UNSPECIFIED.) ;
#1108 = B_SPLINE_CURVE_WITH_KNOTS('',3,(#83795,#83796,#83797,#83798,#83799),
 .UNSPECIFIED.,.F.,.F.,(4,1,4),(0.270884354171619,0.773477463983786,1.57079632679491),
 .UNSPECIFIED.) ;
#1109 = B_SPLINE_CURVE_WITH_KNOTS('',3,(#83835,#83836,#83837,#83838,#83839,
#83840,#83841,#83842,#83843,#83844),.UNSPECIFIED.,.F.,.F.,(4,2,2,2,4),(0.,
0.00788303309691765,0.0119497367126136,0.015825892091812,0.0158931850550275),
 .UNSPECIFIED.) ;
#1110 = B_SPLINE_CURVE_WITH_KNOTS('',3,(#83846,#83847,#83848,#83849,#83850,
#83851,#83852,#83853,#83854,#83855),.UNSPECIFIED.,.F.,.F.,(4,2,2,2,4),(-6.67745037823238E-5,
0.,0.00368652269857415,0.00752108608922011,0.0157260861811032),
 .UNSPECIFIED.) ;
#1111 = B_SPLINE_CURVE_WITH_KNOTS('',3,(#83862,#83863,#83864,#83865,#83866,
#83867,#83868,#83869,#83870,#83871),.UNSPECIFIED.,.F.,.F.,(4,2,2,2,4),(0.,
0.00788283137687036,0.0119495587275004,0.0158257190872389,0.0158930122581911),
 .UNSPECIFIED.) ;
#1112 = B_SPLINE_CURVE_WITH_KNOTS('',3,(#83873,#83874,#83875,#83876,#83877,
#83878,#83879,#83880,#83881,#83882),.UNSPECIFIED.,.F.,.F.,(4,2,2,2,4),(-6.70889521711013E-5,
0.,0.00367906803762835,0.00750255358812287,0.0157699191065211),
 .UNSPECIFIED.) ;
#1113 = B_SPLINE_CURVE_WITH_KNOTS('',3,(#83899,#83900,#83901,#83902,#83903,
#83904,#83905,#83906,#83907,#83908,#83909,#83910,#83911,#83912,#83913,#83914,
#83915,#83916),.UNSPECIFIED.,.F.,.F.,(4,2,2,2,2,2,2,2,4),(0.,0.326127356006603,
0.557344647137824,0.584626694347595,0.59984323350605,0.617644550039615,
0.641541852563963,0.664074855441484,0.685580709784321),.UNSPECIFIED.) ;
#1114 = B_SPLINE_CURVE_WITH_KNOTS('',3,(#83918,#83919,#83920,#83921,#83922,
#83923,#83924,#83925,#83926,#83927,#83928,#83929,#83930,#83931,#83932,#83933,
#83934,#83935),.UNSPECIFIED.,.F.,.F.,(4,2,2,2,2,2,2,2,4),(0.,0.0178986748860247,
0.030596894439968,0.0425739990891357,0.0508039795031799,0.0591630839826922,
0.0794036544378079,0.265037314904174,0.418714241056143),.UNSPECIFIED.) ;
#1115 = B_SPLINE_CURVE_WITH_KNOTS('',3,(#83943,#83944,#83945,#83946,#83947,
#83948,#83949,#83950,#83951,#83952,#83953,#83954,#83955,#83956,#83957,#83958,
#83959,#83960),.UNSPECIFIED.,.F.,.F.,(4,2,2,2,2,2,2,2,4),(0.,0.326124834738013,
0.55734519302541,0.584627517143732,0.599844487527337,0.617646472342995,
0.641544788167125,0.664078789501966,0.685585439526425),.UNSPECIFIED.) ;
#1116 = B_SPLINE_CURVE_WITH_KNOTS('',3,(#83962,#83963,#83964,#83965,#83966,
#83967,#83968,#83969,#83970,#83971,#83972,#83973,#83974,#83975,#83976,#83977,
#83978,#83979),.UNSPECIFIED.,.F.,.F.,(4,2,2,2,2,2,2,2,4),(0.,0.0178988264704468,
0.0305964768111414,0.0425728428045337,0.0508022993033077,0.0591609218800705,
0.0794005119967651,0.26502301977072,0.418693046005869),.UNSPECIFIED.) ;
#1117 = B_SPLINE_CURVE_WITH_KNOTS('',3,(#83987,#83988,#83989,#83990),
 .UNSPECIFIED.,.F.,.F.,(4,4),(-0.400732539131533,-0.390705386116278),
 .UNSPECIFIED.) ;
#1118 = B_SPLINE_CURVE_WITH_KNOTS('',3,(#83994,#83995,#83996,#83997,#83998),
 .UNSPECIFIED.,.F.,.F.,(4,1,4),(-0.0173570618196939,-0.00867853090984697,
0.),.UNSPECIFIED.) ;
#1119 = B_SPLINE_CURVE_WITH_KNOTS('',3,(#84003,#84004,#84005,#84006,#84007,
#84008,#84009,#84010,#84011,#84012,#84013,#84014,#84015),.UNSPECIFIED.,
 .F.,.F.,(4,2,2,2,3,4),(-0.0524538649298037,-0.0454382448332118,-0.0301309134460882,
-0.0150654567230441,0.,0.00806831493386506),.UNSPECIFIED.) ;
#1120 = B_SPLINE_CURVE_WITH_KNOTS('',3,(#84062,#84063,#84064,#84065,#84066,
#84067,#84068,#84069,#84070,#84071,#84072,#84073,#84074,#84075,#84076,#84077,
#84078,#84079,#84080),.UNSPECIFIED.,.F.,.F.,(4,3,3,3,3,3,4),(0.390705386116286,
0.392851683870094,0.394821897685454,0.396624148064999,0.39837845519803,
0.400094449296349,0.400732539131533),.UNSPECIFIED.) ;
#1121 = B_SPLINE_CURVE_WITH_KNOTS('',3,(#84111,#84112,#84113,#84114,#84115),
 .UNSPECIFIED.,.F.,.F.,(4,1,4),(0.,0.00867853090984697,0.0173570618196939),
 .UNSPECIFIED.) ;
#1122 = B_SPLINE_CURVE_WITH_KNOTS('',3,(#84138,#84139,#84140,#84141,#84142,
#84143,#84144,#84145,#84146,#84147,#84148,#84149),.UNSPECIFIED.,.F.,.F.,
(4,2,2,2,2,4),(-0.13141454633876,-0.123346231404894,-0.108280774681851,
-0.0932153179588078,-0.0779079865716814,-0.0708923664750809),
 .UNSPECIFIED.) ;
#1123 = B_SPLINE_CURVE_WITH_KNOTS('',3,(#84151,#84152,#84153,#84154,#84155),
 .UNSPECIFIED.,.F.,.F.,(4,1,4),(0.276503853136672,0.620020769070722,1.),
 .UNSPECIFIED.) ;
#1124 = B_SPLINE_CURVE_WITH_KNOTS('',3,(#86302,#86303,#86304,#86305,#86306),
 .UNSPECIFIED.,.F.,.F.,(4,1,4),(-1.,-0.622952086196121,-0.276501380066297),
 .UNSPECIFIED.) ;
#1125 = B_SPLINE_CURVE_WITH_KNOTS('',3,(#86308,#86309,#86310,#86311,#86312),
 .UNSPECIFIED.,.F.,.F.,(4,1,4),(-1.,-0.622952086196224,-0.276501383761116),
 .UNSPECIFIED.) ;
#1126 = B_SPLINE_CURVE_WITH_KNOTS('',3,(#86316,#86317,#86318,#86319,#86320),
 .UNSPECIFIED.,.F.,.F.,(4,1,4),(0.27650384808904,0.620020769070722,1.),
 .UNSPECIFIED.) ;
#1127 = B_SPLINE_CURVE_WITH_KNOTS('',3,(#86615,#86616,#86617,#86618,#86619,
#86620,#86621,#86622,#86623,#86624),.UNSPECIFIED.,.F.,.F.,(4,2,2,2,4),(-0.0453895164641597,
-0.0415954731675521,-0.0378014298709444,-0.0340366298274179,-0.0302718297838914),
 .UNSPECIFIED.) ;
#1128 = B_SPLINE_CURVE_WITH_KNOTS('',3,(#86641,#86642,#86643,#86644,#86645,
#86646,#86647,#86648,#86649,#86650),.UNSPECIFIED.,.F.,.F.,(4,2,2,2,4),(-0.0302718297838915,
-0.0265011188029211,-0.0227304078219508,-0.0189422746940918,-0.0151541415662328),
 .UNSPECIFIED.) ;
#1129 = B_SPLINE_CURVE_WITH_KNOTS('',3,(#86717,#86718,#86719,#86720,#86721,
#86722,#86723,#86724,#86725,#86726),.UNSPECIFIED.,.F.,.F.,(4,2,2,2,4),(0.13378524314305,
0.14497374491656,0.1561177263117,0.167229804836174,0.17832206951723),
 .UNSPECIFIED.) ;
#1130 = B_SPLINE_CURVE_WITH_KNOTS('',3,(#86730,#86731,#86732,#86733,#86734,
#86735,#86736,#86737,#86738,#86739),.UNSPECIFIED.,.F.,.F.,(4,2,2,2,4),(0.,
0.0110922646810569,0.0222043432055302,0.0333483246006708,0.0445368263741803),
 .UNSPECIFIED.) ;
#1131 = B_SPLINE_CURVE_WITH_KNOTS('',3,(#86743,#86744,#86745,#86746,#86747,
#86748,#86749,#86750,#86751,#86752),.UNSPECIFIED.,.F.,.F.,(4,2,2,2,4),(0.13378524314305,
0.14497374491656,0.1561177263117,0.167229804836174,0.17832206951723),
 .UNSPECIFIED.) ;
#1132 = B_SPLINE_CURVE_WITH_KNOTS('',3,(#86756,#86757,#86758,#86759,#86760,
#86761,#86762,#86763,#86764,#86765),.UNSPECIFIED.,.F.,.F.,(4,2,2,2,4),(0.,
0.0110922646810569,0.0222043432055302,0.0333483246006708,0.0445368263741803),
 .UNSPECIFIED.) ;
#1133 = B_SPLINE_CURVE_WITH_KNOTS('',3,(#86771,#86772,#86773,#86774,#86775,
#86776,#86777,#86778,#86779,#86780),.UNSPECIFIED.,.F.,.F.,(4,2,2,2,4),(0.,
0.0110922646810569,0.0222043432055302,0.0333483246006708,0.0445368263741803),
 .UNSPECIFIED.) ;
#1134 = B_SPLINE_CURVE_WITH_KNOTS('',3,(#86784,#86785,#86786,#86787,#86788,
#86789,#86790,#86791,#86792,#86793),.UNSPECIFIED.,.F.,.F.,(4,2,2,2,4),(0.133785243143047,
0.144973744916557,0.156117726311698,0.167229804836173,0.17832206951723),
 .UNSPECIFIED.) ;
#1135 = B_SPLINE_CURVE_WITH_KNOTS('',3,(#86797,#86798,#86799,#86800,#86801,
#86802,#86803,#86804,#86805,#86806),.UNSPECIFIED.,.F.,.F.,(4,2,2,2,4),(0.,
0.0110922646810577,0.022204343205532,0.0333483246006734,0.0445368263741838),
 .UNSPECIFIED.) ;
#1136 = B_SPLINE_CURVE_WITH_KNOTS('',3,(#86809,#86810,#86811,#86812,#86813,
#86814,#86815,#86816,#86817,#86818),.UNSPECIFIED.,.F.,.F.,(4,2,2,2,4),(0.13378524314305,
0.14497374491656,0.1561177263117,0.167229804836174,0.17832206951723),
 .UNSPECIFIED.) ;
#1137 = B_SPLINE_CURVE_WITH_KNOTS('',3,(#86823,#86824,#86825,#86826,#86827,
#86828,#86829,#86830,#86831,#86832),.UNSPECIFIED.,.F.,.F.,(4,2,2,2,4),(0.,
0.0110922646810577,0.022204343205532,0.0333483246006734,0.0445368263741838),
 .UNSPECIFIED.) ;
#1138 = B_SPLINE_CURVE_WITH_KNOTS('',3,(#86836,#86837,#86838,#86839,#86840,
#86841,#86842,#86843,#86844,#86845),.UNSPECIFIED.,.F.,.F.,(4,2,2,2,4),(0.13378524314305,
0.14497374491656,0.1561177263117,0.167229804836174,0.17832206951723),
 .UNSPECIFIED.) ;
#1139 = B_SPLINE_CURVE_WITH_KNOTS('',3,(#86849,#86850,#86851,#86852,#86853,
#86854,#86855,#86856,#86857,#86858),.UNSPECIFIED.,.F.,.F.,(4,2,2,2,4),(0.,
0.0110922646810569,0.0222043432055302,0.0333483246006708,0.0445368263741803),
 .UNSPECIFIED.) ;
#1140 = B_SPLINE_CURVE_WITH_KNOTS('',3,(#86861,#86862,#86863,#86864,#86865,
#86866,#86867,#86868,#86869,#86870),.UNSPECIFIED.,.F.,.F.,(4,2,2,2,4),(0.133785243143047,
0.144973744916557,0.156117726311698,0.167229804836173,0.17832206951723),
 .UNSPECIFIED.) ;
#1141 = B_SPLINE_CURVE_WITH_KNOTS('',3,(#86875,#86876,#86877,#86878,#86879,
#86880,#86881,#86882,#86883,#86884),.UNSPECIFIED.,.F.,.F.,(4,2,2,2,4),(0.,
0.0110922646810569,0.0222043432055302,0.0333483246006708,0.0445368263741803),
 .UNSPECIFIED.) ;
#1142 = B_SPLINE_CURVE_WITH_KNOTS('',3,(#86888,#86889,#86890,#86891,#86892,
#86893,#86894,#86895,#86896,#86897),.UNSPECIFIED.,.F.,.F.,(4,2,2,2,4),(0.133785243143047,
0.144973744916557,0.156117726311698,0.167229804836173,0.17832206951723),
 .UNSPECIFIED.) ;
#1143 = B_SPLINE_CURVE_WITH_KNOTS('',3,(#86901,#86902,#86903,#86904,#86905,
#86906,#86907,#86908,#86909,#86910),.UNSPECIFIED.,.F.,.F.,(4,2,2,2,4),(0.,
0.0110922646810577,0.022204343205532,0.0333483246006734,0.0445368263741838),
 .UNSPECIFIED.) ;
#1144 = B_SPLINE_CURVE_WITH_KNOTS('',3,(#86913,#86914,#86915,#86916,#86917,
#86918,#86919,#86920,#86921,#86922),.UNSPECIFIED.,.F.,.F.,(4,2,2,2,4),(0.13378524314305,
0.14497374491656,0.1561177263117,0.167229804836174,0.17832206951723),
 .UNSPECIFIED.) ;
#1145 = B_SPLINE_CURVE_WITH_KNOTS('',3,(#87209,#87210,#87211,#87212,#87213,
#87214),.UNSPECIFIED.,.F.,.F.,(4,2,4),(0.0376778444829456,0.0409098759506884,
0.0446641096906363),.UNSPECIFIED.) ;
#1146 = B_SPLINE_CURVE_WITH_KNOTS('',3,(#87217,#87218,#87219,#87220),
 .UNSPECIFIED.,.F.,.F.,(4,4),(0.,0.0422101666362959),.UNSPECIFIED.) ;
#1147 = B_SPLINE_CURVE_WITH_KNOTS('',3,(#87225,#87226,#87227,#87228),
 .UNSPECIFIED.,.F.,.F.,(4,4),(-0.0422101666362958,0.),.UNSPECIFIED.) ;
#1148 = B_SPLINE_CURVE_WITH_KNOTS('',3,(#87235,#87236,#87237,#87238,#87239,
#87240),.UNSPECIFIED.,.F.,.F.,(4,2,4),(0.0148851463516941,0.0186393800916421,
0.021871411559383),.UNSPECIFIED.) ;
#1149 = B_SPLINE_CURVE_WITH_KNOTS('',3,(#89080,#89081,#89082,#89083,#89084,
#89085,#89086,#89087,#89088,#89089,#89090,#89091,#89092),.UNSPECIFIED.,
 .F.,.F.,(4,1,1,1,1,1,1,1,1,1,4),(0.,0.1,0.2,0.3,0.4,0.5,0.6,0.7,0.8,0.9,
1.),.UNSPECIFIED.) ;
#1150 = B_SPLINE_CURVE_WITH_KNOTS('',3,(#89094,#89095,#89096,#89097,#89098,
#89099),.UNSPECIFIED.,.F.,.F.,(4,1,1,4),(0.,0.333333333333333,0.666666666666667,
1.),.UNSPECIFIED.) ;
#1151 = B_SPLINE_CURVE_WITH_KNOTS('',3,(#89101,#89102,#89103,#89104,#89105,
#89106,#89107,#89108,#89109,#89110,#89111,#89112,#89113,#89114,#89115,#89116,
#89117,#89118,#89119,#89120,#89121,#89122,#89123,#89124,#89125,#89126,#89127,
#89128,#89129,#89130,#89131,#89132,#89133,#89134,#89135,#89136,#89137,#89138,
#89139,#89140,#89141,#89142,#89143,#89144,#89145,#89146,#89147,#89148,#89149,
#89150,#89151,#89152,#89153,#89154,#89155,#89156,#89157,#89158,#89159,#89160,
#89161,#89162,#89163,#89164),.UNSPECIFIED.,.F.,.F.,(4,3,3,3,3,3,3,3,3,3,
3,3,3,3,3,3,3,3,3,3,3,4),(0.50000000000002,0.540931884362004,0.549999476969566,
0.57785534140829,0.599999449142665,0.630623423732254,0.650001938995543,
0.670121368703304,0.699999961337087,0.726319366023772,0.749998804879715,
0.764743070246695,0.800000000093043,0.800090168326521,0.850000141966713,
0.856761721866945,0.899999993071106,0.902358829665644,0.942091717824869,
0.950000243206862,0.977692918008602,1.),.UNSPECIFIED.) ;
#1152 = B_SPLINE_CURVE_WITH_KNOTS('',3,(#89245,#89246,#89247,#89248,#89249,
#89250,#89251,#89252,#89253,#89254,#89255,#89256,#89257),.UNSPECIFIED.,
 .F.,.F.,(4,1,1,1,1,1,1,1,1,1,4),(0.,0.1,0.2,0.3,0.4,0.5,0.6,0.7,0.8,0.9,
1.),.UNSPECIFIED.) ;
#1153 = B_SPLINE_CURVE_WITH_KNOTS('',3,(#89260,#89261,#89262,#89263,#89264,
#89265,#89266,#89267,#89268,#89269,#89270,#89271,#89272,#89273,#89274,#89275,
#89276,#89277,#89278,#89279,#89280,#89281,#89282,#89283,#89284,#89285,#89286,
#89287,#89288,#89289,#89290,#89291,#89292,#89293,#89294,#89295,#89296,#89297,
#89298,#89299,#89300,#89301,#89302,#89303,#89304,#89305,#89306,#89307,#89308,
#89309,#89310,#89311,#89312,#89313,#89314,#89315,#89316,#89317,#89318,#89319,
#89320,#89321,#89322,#89323,#89324,#89325,#89326),.UNSPECIFIED.,.F.,.F.,
(4,3,3,3,3,3,3,3,3,3,3,3,3,3,3,3,3,3,3,3,3,3,4),(0.,0.029211291026702,0.0500008174088028,
0.060544943773545,0.0938972400757973,0.100000166665901,0.130378684246365,
0.15000088015134,0.174071006839537,0.199999777732466,0.221649421518731,
0.249999425571877,0.25898085613298,0.293770381915345,0.299999713862244,
0.331057161559401,0.350001769846541,0.368733440803518,0.400000309272562,
0.412905090819267,0.450000017037755,0.479639534628252,0.50000000000002),
 .UNSPECIFIED.) ;
#1154 = B_SPLINE_CURVE_WITH_KNOTS('',3,(#89406,#89407,#89408,#89409,#89410,
#89411),.UNSPECIFIED.,.F.,.F.,(4,1,1,4),(0.,0.333333333333333,0.666666666666667,
0.999999901148969),.UNSPECIFIED.) ;
#1155 = B_SPLINE_CURVE_WITH_KNOTS('',3,(#89413,#89414,#89415,#89416,#89417,
#89418,#89419,#89420,#89421,#89422,#89423,#89424,#89425,#89426,#89427,#89428,
#89429,#89430,#89431,#89432,#89433,#89434,#89435,#89436,#89437,#89438,#89439,
#89440,#89441,#89442,#89443,#89444,#89445,#89446,#89447,#89448,#89449,#89450,
#89451,#89452,#89453,#89454,#89455),.UNSPECIFIED.,.F.,.F.,(4,3,3,3,3,3,
3,3,3,3,3,3,3,3,4),(0.740046669567313,0.763099290859212,0.784481908360721,
0.811421669815631,0.819140541376942,0.832121780979733,0.85502513103706,
0.889660371947781,0.913260537792704,0.914933018320988,0.935388557500039,
0.955946024091937,0.975439020158076,0.993845115294604,0.999999999999939),
 .UNSPECIFIED.) ;
#1156 = B_SPLINE_CURVE_WITH_KNOTS('',3,(#89457,#89458,#89459,#89460,#89461,
#89462,#89463,#89464,#89465,#89466,#89467,#89468,#89469,#89470,#89471,#89472,
#89473,#89474,#89475,#89476,#89477,#89478,#89479,#89480,#89481,#89482,#89483,
#89484,#89485,#89486,#89487,#89488,#89489,#89490,#89491,#89492,#89493,#89494,
#89495,#89496,#89497,#89498,#89499,#89500,#89501,#89502,#89503,#89504,#89505,
#89506,#89507,#89508,#89509,#89510,#89511,#89512,#89513,#89514,#89515,#89516,
#89517,#89518,#89519,#89520,#89521,#89522,#89523,#89524,#89525,#89526,#89527,
#89528,#89529,#89530,#89531,#89532,#89533,#89534,#89535,#89536,#89537,#89538,
#89539,#89540,#89541,#89542,#89543,#89544,#89545,#89546,#89547,#89548,#89549,
#89550,#89551,#89552,#89553,#89554,#89555,#89556),.UNSPECIFIED.,.F.,.F.,
(4,3,3,3,3,3,3,3,3,3,3,3,3,3,3,3,3,3,3,3,3,3,3,3,3,3,3,3,3,3,3,3,3,4),(9.43012544827459E-8,
0.031864058797589,0.0647840362122895,0.0990069909892971,0.125039338268755,
0.134916637559053,0.176959063913584,0.215046371604815,0.260170220267245,
0.265136830208005,0.318040825054938,0.360663273489004,0.363657546998835,
0.400621818895941,0.438082955214945,0.468825159061875,0.473202770514011,
0.511546102075598,0.546372378738656,0.578100024548857,0.583032295575111,
0.622265622394134,0.665621014897703,0.680754237084197,0.720780686822075,
0.771027763058629,0.790928228827376,0.813100495945339,0.85149915167859,
0.888624363758942,0.922410481952504,0.955205742315633,0.986814689647663,
1.),.UNSPECIFIED.) ;
#1157 = B_SPLINE_CURVE_WITH_KNOTS('',3,(#89625,#89626,#89627,#89628,#89629,
#89630,#89631,#89632,#89633,#89634,#89635),.UNSPECIFIED.,.F.,.F.,(4,1,1,
1,1,1,1,1,4),(0.,0.125,0.25,0.375,0.5,0.625,0.75,0.875,1.),
 .UNSPECIFIED.) ;
#1158 = B_SPLINE_CURVE_WITH_KNOTS('',3,(#89638,#89639,#89640,#89641,#89642,
#89643,#89644,#89645,#89646,#89647,#89648,#89649,#89650,#89651,#89652,#89653,
#89654,#89655,#89656,#89657,#89658,#89659,#89660,#89661,#89662,#89663,#89664,
#89665,#89666,#89667,#89668,#89669,#89670,#89671,#89672,#89673,#89674,#89675,
#89676,#89677,#89678,#89679,#89680,#89681,#89682,#89683,#89684,#89685,#89686,
#89687,#89688,#89689,#89690,#89691,#89692,#89693,#89694,#89695,#89696,#89697,
#89698,#89699,#89700,#89701,#89702,#89703,#89704,#89705,#89706,#89707,#89708,
#89709,#89710,#89711,#89712,#89713,#89714,#89715,#89716,#89717,#89718,#89719,
#89720,#89721,#89722,#89723,#89724,#89725,#89726,#89727,#89728,#89729,#89730,
#89731,#89732,#89733,#89734,#89735,#89736,#89737),.UNSPECIFIED.,.F.,.F.,
(4,3,3,3,3,3,3,3,3,3,3,3,3,3,3,3,3,3,3,3,3,3,3,3,3,3,3,3,3,3,3,3,3,4),(0.,
0.0234163840184272,0.0478392774354898,0.0735929525966121,0.101260672275236,
0.13215515581021,0.161611085696521,0.205091291829831,0.208484168145554,
0.238318416362703,0.265116005993426,0.265187074007494,0.29019218665116,
0.318308090975454,0.345050056035187,0.357100347629798,0.373722767756927,
0.405591170427141,0.433846469730387,0.445335557423208,0.48217444472529,
0.505617857135101,0.514408471114612,0.542613244205269,0.568369687650452,
0.581008652375286,0.593348553719565,0.615767486536519,0.638648003192484,
0.659516414041665,0.663954602269109,0.699207373791262,0.730123470459489,
0.740046655839865),.UNSPECIFIED.) ;
#1159 = B_SPLINE_CURVE_WITH_KNOTS('',3,(#89805,#89806,#89807,#89808,#89809,
#89810),.UNSPECIFIED.,.F.,.F.,(4,1,1,4),(0.,0.333333333333333,0.666666666666667,
1.),.UNSPECIFIED.) ;
#1160 = B_SPLINE_CURVE_WITH_KNOTS('',3,(#89812,#89813,#89814,#89815,#89816,
#89817,#89818,#89819,#89820,#89821,#89822,#89823,#89824,#89825,#89826,#89827,
#89828,#89829,#89830,#89831,#89832,#89833,#89834,#89835,#89836,#89837,#89838,
#89839,#89840,#89841,#89842,#89843,#89844,#89845,#89846,#89847,#89848,#89849,
#89850,#89851,#89852,#89853,#89854,#89855,#89856,#89857,#89858,#89859,#89860,
#89861,#89862,#89863,#89864,#89865,#89866,#89867,#89868,#89869,#89870,#89871,
#89872),.UNSPECIFIED.,.F.,.F.,(4,3,3,3,3,3,3,3,3,3,3,3,3,3,3,3,3,3,3,3,
4),(0.499999999999957,0.543426929556171,0.562498466595099,0.582529420733352,
0.623146114415814,0.624999981287924,0.663596929285891,0.687501639134093,
0.717594346195301,0.749999793833349,0.754935239198527,0.789630090278152,
0.812500138729425,0.825709594031802,0.866465848423957,0.875000628872866,
0.911531406767164,0.937498440919157,0.946944182542892,0.977771956059037,
1.),.UNSPECIFIED.) ;
#1161 = B_SPLINE_CURVE_WITH_KNOTS('',3,(#89894,#89895,#89896,#89897,#89898),
 .UNSPECIFIED.,.F.,.F.,(4,1,4),(0.,0.0298071351389365,0.0685496713495228),
 .UNSPECIFIED.) ;
#1162 = B_SPLINE_CURVE_WITH_KNOTS('',3,(#89901,#89902,#89903,#89904,#89905),
 .UNSPECIFIED.,.F.,.F.,(4,1,4),(0.,0.0298071351389365,0.0685496713495228),
 .UNSPECIFIED.) ;
#1163 = B_SPLINE_CURVE_WITH_KNOTS('',3,(#89917,#89918,#89919,#89920,#89921),
 .UNSPECIFIED.,.F.,.F.,(4,1,4),(0.,0.0263673128827931,0.0523427870633456),
 .UNSPECIFIED.) ;
#1164 = B_SPLINE_CURVE_WITH_KNOTS('',3,(#89924,#89925,#89926,#89927,#89928),
 .UNSPECIFIED.,.F.,.F.,(4,1,4),(0.,0.0263673128827931,0.0523427870633456),
 .UNSPECIFIED.) ;
#1165 = B_SPLINE_CURVE_WITH_KNOTS('',3,(#89940,#89941,#89942,#89943,#89944),
 .UNSPECIFIED.,.F.,.F.,(4,1,4),(0.,0.0190758281807941,0.0379545209982657),
 .UNSPECIFIED.) ;
#1166 = B_SPLINE_CURVE_WITH_KNOTS('',3,(#89947,#89948,#89949,#89950,#89951),
 .UNSPECIFIED.,.F.,.F.,(4,1,4),(0.,0.0190758281807941,0.0379545209982657),
 .UNSPECIFIED.) ;
#1167 = B_SPLINE_CURVE_WITH_KNOTS('',3,(#89963,#89964,#89965,#89966,#89967),
 .UNSPECIFIED.,.F.,.F.,(4,1,4),(0.,0.0205128997765721,0.0398218276255599),
 .UNSPECIFIED.) ;
#1168 = B_SPLINE_CURVE_WITH_KNOTS('',3,(#89970,#89971,#89972,#89973,#89974),
 .UNSPECIFIED.,.F.,.F.,(4,1,4),(0.,0.0205128997765721,0.0398218276255599),
 .UNSPECIFIED.) ;
#1169 = B_SPLINE_CURVE_WITH_KNOTS('',3,(#89986,#89987,#89988,#89989,#89990),
 .UNSPECIFIED.,.F.,.F.,(4,1,4),(0.,0.0323852950215525,0.0574227556854303),
 .UNSPECIFIED.) ;
#1170 = B_SPLINE_CURVE_WITH_KNOTS('',3,(#89993,#89994,#89995,#89996,#89997),
 .UNSPECIFIED.,.F.,.F.,(4,1,4),(0.,0.0323852950215525,0.0574227556854303),
 .UNSPECIFIED.) ;
#1171 = B_SPLINE_CURVE_WITH_KNOTS('',3,(#90033,#90034,#90035,#90036,#90037),
 .UNSPECIFIED.,.F.,.F.,(4,1,4),(0.,0.011955158932918,0.0295605475166918),
 .UNSPECIFIED.) ;
#1172 = B_SPLINE_CURVE_WITH_KNOTS('',3,(#90040,#90041,#90042,#90043,#90044),
 .UNSPECIFIED.,.F.,.F.,(4,1,4),(0.,0.011955158932918,0.0295605475166918),
 .UNSPECIFIED.) ;
#1173 = B_SPLINE_CURVE_WITH_KNOTS('',3,(#90056,#90057,#90058,#90059,#90060),
 .UNSPECIFIED.,.F.,.F.,(4,1,4),(0.,0.0135228484064754,0.0263579081616444),
 .UNSPECIFIED.) ;
#1174 = B_SPLINE_CURVE_WITH_KNOTS('',3,(#90063,#90064,#90065,#90066,#90067),
 .UNSPECIFIED.,.F.,.F.,(4,1,4),(0.,0.0135228484064754,0.0263579081616444),
 .UNSPECIFIED.) ;
#1175 = B_SPLINE_CURVE_WITH_KNOTS('',3,(#90079,#90080,#90081,#90082,#90083),
 .UNSPECIFIED.,.F.,.F.,(4,1,4),(0.,0.0216058216755205,0.0381303842659523),
 .UNSPECIFIED.) ;
#1176 = B_SPLINE_CURVE_WITH_KNOTS('',3,(#90086,#90087,#90088,#90089,#90090),
 .UNSPECIFIED.,.F.,.F.,(4,1,4),(0.,0.0216058216755205,0.0381303842659523),
 .UNSPECIFIED.) ;
#1177 = B_SPLINE_CURVE_WITH_KNOTS('',3,(#90102,#90103,#90104,#90105,#90106),
 .UNSPECIFIED.,.F.,.F.,(4,1,4),(0.,0.0381782469542568,0.0670753371474822),
 .UNSPECIFIED.) ;
#1178 = B_SPLINE_CURVE_WITH_KNOTS('',3,(#90109,#90110,#90111,#90112,#90113),
 .UNSPECIFIED.,.F.,.F.,(4,1,4),(0.,0.0381782469542568,0.0670753371474822),
 .UNSPECIFIED.) ;
#1179 = B_SPLINE_CURVE_WITH_KNOTS('',3,(#90143,#90144,#90145,#90146,#90147),
 .UNSPECIFIED.,.F.,.F.,(4,1,4),(0.,0.0329095469988702,0.0691336974954879),
 .UNSPECIFIED.) ;
#1180 = B_SPLINE_CURVE_WITH_KNOTS('',3,(#90150,#90151,#90152,#90153,#90154),
 .UNSPECIFIED.,.F.,.F.,(4,1,4),(0.,0.0329095469988702,0.0691336974954879),
 .UNSPECIFIED.) ;
#1181 = B_SPLINE_CURVE_WITH_KNOTS('',3,(#90166,#90167,#90168,#90169,#90170),
 .UNSPECIFIED.,.F.,.F.,(4,1,4),(0.,0.0210301296927785,0.0377156586265697),
 .UNSPECIFIED.) ;
#1182 = B_SPLINE_CURVE_WITH_KNOTS('',3,(#90173,#90174,#90175,#90176,#90177),
 .UNSPECIFIED.,.F.,.F.,(4,1,4),(0.,0.0210301296927785,0.0377156586265697),
 .UNSPECIFIED.) ;
#1183 = B_SPLINE_CURVE_WITH_KNOTS('',3,(#90189,#90190,#90191,#90192,#90193),
 .UNSPECIFIED.,.F.,.F.,(4,1,4),(0.,0.0424180496051088,0.0942055476140892),
 .UNSPECIFIED.) ;
#1184 = B_SPLINE_CURVE_WITH_KNOTS('',3,(#90196,#90197,#90198,#90199,#90200),
 .UNSPECIFIED.,.F.,.F.,(4,1,4),(0.,0.0424180496051088,0.0942055476140892),
 .UNSPECIFIED.) ;
#1185 = B_SPLINE_CURVE_WITH_KNOTS('',3,(#90212,#90213,#90214,#90215,#90216),
 .UNSPECIFIED.,.F.,.F.,(4,1,4),(0.,0.0398228695438388,0.0783699334705556),
 .UNSPECIFIED.) ;
#1186 = B_SPLINE_CURVE_WITH_KNOTS('',3,(#90219,#90220,#90221,#90222,#90223),
 .UNSPECIFIED.,.F.,.F.,(4,1,4),(0.,0.0398228695438388,0.0783699334705556),
 .UNSPECIFIED.) ;
#1187 = B_SPLINE_CURVE_WITH_KNOTS('',3,(#90235,#90236,#90237,#90238,#90239),
 .UNSPECIFIED.,.F.,.F.,(4,1,4),(0.,0.0313133324080373,0.063168759987351),
 .UNSPECIFIED.) ;
#1188 = B_SPLINE_CURVE_WITH_KNOTS('',3,(#90242,#90243,#90244,#90245,#90246),
 .UNSPECIFIED.,.F.,.F.,(4,1,4),(0.,0.0313133324080373,0.063168759987351),
 .UNSPECIFIED.) ;
#1189 = B_SPLINE_CURVE_WITH_KNOTS('',3,(#90258,#90259,#90260,#90261,#90262),
 .UNSPECIFIED.,.F.,.F.,(4,1,4),(0.,0.0290828541577381,0.0592932101613289),
 .UNSPECIFIED.) ;
#1190 = B_SPLINE_CURVE_WITH_KNOTS('',3,(#90265,#90266,#90267,#90268,#90269),
 .UNSPECIFIED.,.F.,.F.,(4,1,4),(0.,0.0290828541577381,0.0592932101613289),
 .UNSPECIFIED.) ;
#1191 = B_SPLINE_CURVE_WITH_KNOTS('',3,(#90281,#90282,#90283,#90284,#90285),
 .UNSPECIFIED.,.F.,.F.,(4,1,4),(0.,0.0471458586470647,0.0823534588635132),
 .UNSPECIFIED.) ;
#1192 = B_SPLINE_CURVE_WITH_KNOTS('',3,(#90288,#90289,#90290,#90291,#90292),
 .UNSPECIFIED.,.F.,.F.,(4,1,4),(0.,0.0471458586470647,0.0823534588635132),
 .UNSPECIFIED.) ;
#1193 = B_SPLINE_CURVE_WITH_KNOTS('',3,(#90383,#90384,#90385,#90386,#90387,
#90388),.UNSPECIFIED.,.F.,.F.,(4,2,4),(-0.0646894582084791,-0.0581995466601206,
-0.0505532240038533),.UNSPECIFIED.) ;
#1194 = B_SPLINE_CURVE_WITH_KNOTS('',3,(#90391,#90392,#90393,#90394,#90395,
#90396),.UNSPECIFIED.,.F.,.F.,(4,2,4),(-0.0279464003917075,-0.0162728575198495,
-0.00636479267613269),.UNSPECIFIED.) ;
#1195 = B_SPLINE_CURVE_WITH_KNOTS('',3,(#90404,#90405,#90406,#90407,#90408,
#90409,#90410,#90411),.UNSPECIFIED.,.F.,.F.,(4,2,2,4),(-0.0463941724255825,
-0.0363335959367585,-0.0244739336232673,6.93889390390723E-18),
 .UNSPECIFIED.) ;
#1196 = B_SPLINE_CURVE_WITH_KNOTS('',3,(#90438,#90439,#90440,#90441),
 .UNSPECIFIED.,.F.,.F.,(4,4),(-0.00233157716846821,0.),.UNSPECIFIED.) ;
#1197 = B_SPLINE_CURVE_WITH_KNOTS('',3,(#90466,#90467,#90468,#90469,#90470,
#90471,#90472,#90473,#90474,#90475,#90476,#90477,#90478,#90479,#90480,#90481,
#90482,#90483,#90484,#90485,#90486,#90487,#90488,#90489,#90490,#90491,#90492,
#90493),.UNSPECIFIED.,.F.,.F.,(4,3,3,3,3,3,3,3,3,4),(3.21026029059551E-8,
0.00464707931025668,0.00929415862051336,0.0137678334300167,0.0156388310171345,
0.0187179653523303,0.0232666593299545,0.0251479586559353,0.0296888345732088,
0.0316724821582484),.UNSPECIFIED.) ;
#1198 = B_SPLINE_CURVE_WITH_KNOTS('',3,(#90495,#90496,#90497,#90498),
 .UNSPECIFIED.,.F.,.F.,(4,4),(0.000498023522427242,0.00742046561384795),
 .UNSPECIFIED.) ;
#1199 = B_SPLINE_CURVE_WITH_KNOTS('',3,(#90499,#90500,#90501,#90502,#90503,
#90504,#90505),.UNSPECIFIED.,.F.,.F.,(4,3,4),(0.00742046561384795,0.0146643599521495,
0.0162549092688308),.UNSPECIFIED.) ;
#1200 = B_SPLINE_CURVE_WITH_KNOTS('',3,(#90552,#90553,#90554,#90555,#90556,
#90557),.UNSPECIFIED.,.F.,.F.,(4,2,4),(0.,0.00166959259478934,0.00333900921077541),
 .UNSPECIFIED.) ;
#1201 = B_SPLINE_CURVE_WITH_KNOTS('',3,(#90565,#90566,#90567,#90568,#90569,
#90570,#90571,#90572,#90573,#90574,#90575,#90576,#90577),.UNSPECIFIED.,
 .F.,.F.,(4,3,3,3,4),(-0.0247314244030886,-0.0245013764734994,-0.0199768571653589,
-0.0156201260570807,-0.0140088579916689),.UNSPECIFIED.) ;
#1202 = B_SPLINE_CURVE_WITH_KNOTS('',3,(#90579,#90580,#90581,#90582,#90583,
#90584),.UNSPECIFIED.,.F.,.F.,(4,2,4),(-0.00524067245577225,-0.00262950955895225,
0.),.UNSPECIFIED.) ;
#1203 = B_SPLINE_CURVE_WITH_KNOTS('',3,(#90585,#90586,#90587,#90588,#90589,
#90590),.UNSPECIFIED.,.F.,.F.,(4,2,4),(-0.0208077196740842,-0.0103104127273635,
-0.000111699617630046),.UNSPECIFIED.) ;
#1204 = B_SPLINE_CURVE_WITH_KNOTS('',3,(#90620,#90621,#90622,#90623,#90624,
#90625),.UNSPECIFIED.,.F.,.F.,(4,2,4),(-0.167893988576184,-0.139678911984281,
-0.12132773760924),.UNSPECIFIED.) ;
#1205 = B_SPLINE_CURVE_WITH_KNOTS('',3,(#90711,#90712,#90713,#90714,#90715,
#90716,#90717,#90718,#90719,#90720,#90721,#90722),.UNSPECIFIED.,.F.,.F.,
(4,2,2,2,2,4),(-0.103468456759814,-0.102439814165996,-0.0469583320002097,
-0.0291854860033449,-0.010865621464627,0.),.UNSPECIFIED.) ;
#1206 = B_SPLINE_CURVE_WITH_KNOTS('',3,(#90724,#90725,#90726,#90727,#90728,
#90729,#90730,#90731,#90732,#90733,#90734,#90735,#90736,#90737,#90738,#90739,
#90740,#90741,#90742,#90743,#90744,#90745,#90746,#90747,#90748,#90749,#90750,
#90751),.UNSPECIFIED.,.F.,.F.,(4,3,3,3,3,3,3,3,3,4),(-0.0929261016547975,
-0.0912735545557092,-0.0896210074566209,-0.0863159132584443,-0.0797057248620911,
-0.073095536465738,-0.0532649712766785,-0.0268242176912658,-0.0234862530524168,
-0.00123315546009042),.UNSPECIFIED.) ;
#1207 = B_SPLINE_CURVE_WITH_KNOTS('',3,(#90757,#90758,#90759,#90760,#90761,
#90762),.UNSPECIFIED.,.F.,.F.,(4,2,4),(-0.0160009459236279,-0.00787429008612065,
-7.73645268326029E-6),.UNSPECIFIED.) ;
#1208 = B_SPLINE_CURVE_WITH_KNOTS('',3,(#90764,#90765,#90766,#90767,#90768,
#90769,#90770,#90771),.UNSPECIFIED.,.F.,.F.,(4,2,2,4),(2.69755551674642E-5,
0.0275748103794202,0.0564582935792714,0.0567967509721843),.UNSPECIFIED.) ;
#1209 = B_SPLINE_CURVE_WITH_KNOTS('',3,(#90777,#90778,#90779,#90780,#90781),
 .UNSPECIFIED.,.F.,.F.,(4,1,4),(-0.0267801877362277,-0.0114772233155261,
0.),.UNSPECIFIED.) ;
#1210 = B_SPLINE_CURVE_WITH_KNOTS('',3,(#90890,#90891,#90892,#90893,#90894,
#90895),.UNSPECIFIED.,.F.,.F.,(4,2,4),(0.,0.0518624644373431,0.0522283064773341),
 .UNSPECIFIED.) ;
#1211 = B_SPLINE_CURVE_WITH_KNOTS('',3,(#90896,#90897,#90898,#90899,#90900,
#90901),.UNSPECIFIED.,.F.,.F.,(4,2,4),(-0.0522283064773341,-0.0518624644373431,
0.),.UNSPECIFIED.) ;
#1212 = B_SPLINE_CURVE_WITH_KNOTS('',3,(#91009,#91010,#91011,#91012),
 .UNSPECIFIED.,.F.,.F.,(4,4),(-0.051862464436985,-0.00040498540622502),
 .UNSPECIFIED.) ;
#1213 = B_SPLINE_CURVE_WITH_KNOTS('',3,(#91013,#91014,#91015,#91016,#91017,
#91018),.UNSPECIFIED.,.F.,.F.,(4,2,4),(-0.00040498540622502,0.,0.000365842040355155),
 .UNSPECIFIED.) ;
#1214 = B_SPLINE_CURVE_WITH_KNOTS('',3,(#91020,#91021,#91022,#91023,#91024,
#91025),.UNSPECIFIED.,.F.,.F.,(4,2,4),(-0.000365842040355155,0.,0.000404915206456683),
 .UNSPECIFIED.) ;
#1215 = B_SPLINE_CURVE_WITH_KNOTS('',3,(#91026,#91027,#91028,#91029),
 .UNSPECIFIED.,.F.,.F.,(4,4),(0.000404915206456683,0.051862464436985),
 .UNSPECIFIED.) ;
#1216 = B_SPLINE_CURVE_WITH_KNOTS('',3,(#91099,#91100,#91101,#91102,#91103,
#91104,#91105,#91106,#91107,#91108),.UNSPECIFIED.,.F.,.F.,(4,2,2,2,4),(-0.0248690759606685,
-0.024715611553566,-0.0142883199095518,-0.00605736591428742,0.),
 .UNSPECIFIED.) ;
#1217 = B_SPLINE_CURVE_WITH_KNOTS('',3,(#91148,#91149,#91150,#91151,#91152,
#91153),.UNSPECIFIED.,.F.,.F.,(4,2,4),(-0.0617997712808834,-0.0284087068830499,
0.),.UNSPECIFIED.) ;
#1218 = B_SPLINE_CURVE_WITH_KNOTS('',3,(#91310,#91311,#91312,#91313,#91314),
 .UNSPECIFIED.,.F.,.F.,(4,1,4),(0.0402140666257685,0.0595744748887569,0.0856917518795941),
 .UNSPECIFIED.) ;
#1219 = B_SPLINE_CURVE_WITH_KNOTS('',3,(#91315,#91316,#91317,#91318),
 .UNSPECIFIED.,.F.,.F.,(4,4),(-0.00119196920320868,0.00853666604048891),
 .UNSPECIFIED.) ;
#1220 = B_SPLINE_CURVE_WITH_KNOTS('',3,(#91335,#91336,#91337,#91338,#91339,
#91340,#91341,#91342,#91343,#91344,#91345,#91346,#91347,#91348,#91349,#91350),
 .UNSPECIFIED.,.F.,.F.,(4,2,2,2,2,2,2,4),(0.0209336302119049,0.0225603262737206,
0.0248958150254002,0.0295087749195171,0.0344155207767142,0.0391677058630032,
0.0437345723765867,0.0438833919350602),.UNSPECIFIED.) ;
#1221 = B_SPLINE_CURVE_WITH_KNOTS('',3,(#91398,#91399,#91400,#91401,#91402,
#91403),.UNSPECIFIED.,.F.,.F.,(4,2,4),(-0.0194026045695604,-0.0117562819132907,
0.),.UNSPECIFIED.) ;
#1222 = B_SPLINE_CURVE_WITH_KNOTS('',3,(#91489,#91490,#91491,#91492,#91493,
#91494,#91495,#91496,#91497,#91498,#91499,#91500),.UNSPECIFIED.,.F.,.F.,
(4,2,2,2,2,4),(-0.029993636019315,-0.0220228924152891,-0.0132531560003494,
-0.00562260137335941,1.54323775980458E-12,7.5349547761283E-5),
 .UNSPECIFIED.) ;
#1223 = B_SPLINE_CURVE_WITH_KNOTS('',3,(#91501,#91502,#91503,#91504,#91505,
#91506),.UNSPECIFIED.,.F.,.F.,(4,1,1,4),(-0.184560397797916,-0.166722152241299,
-0.156528869066089,-0.148883906684682),.UNSPECIFIED.) ;
#1224 = B_SPLINE_CURVE_WITH_KNOTS('',3,(#91507,#91508,#91509,#91510,#91511),
 .UNSPECIFIED.,.F.,.F.,(4,1,4),(0.148883906684682,0.156528869066089,0.159545911357215),
 .UNSPECIFIED.) ;
#1225 = B_SPLINE_CURVE_WITH_KNOTS('',3,(#91555,#91556,#91557,#91558,#91559,
#91560),.UNSPECIFIED.,.F.,.F.,(4,2,4),(-0.0663145530984604,0.,0.000424263177439857),
 .UNSPECIFIED.) ;
#1226 = B_SPLINE_CURVE_WITH_KNOTS('',3,(#91562,#91563,#91564,#91565,#91566,
#91567),.UNSPECIFIED.,.F.,.F.,(4,2,4),(-0.000424263177439857,0.,0.00584465807886479),
 .UNSPECIFIED.) ;
#1227 = B_SPLINE_CURVE_WITH_KNOTS('',3,(#91568,#91569,#91570,#91571),
 .UNSPECIFIED.,.F.,.F.,(4,4),(0.00584465807886479,0.0663145530984604),
 .UNSPECIFIED.) ;
#1228 = B_SPLINE_CURVE_WITH_KNOTS('',3,(#91617,#91618,#91619,#91620),
 .UNSPECIFIED.,.F.,.F.,(4,4),(-0.0254449718282482,0.),.UNSPECIFIED.) ;
#1229 = B_SPLINE_CURVE_WITH_KNOTS('',3,(#91623,#91624,#91625,#91626),
 .UNSPECIFIED.,.F.,.F.,(4,4),(0.,0.0254449718282482),.UNSPECIFIED.) ;
#1230 = B_SPLINE_CURVE_WITH_KNOTS('',3,(#91685,#91686,#91687,#91688,#91689,
#91690,#91691,#91692,#91693,#91694),.UNSPECIFIED.,.F.,.F.,(4,2,2,2,4),(0.,
0.00873255283564249,0.0137119265240959,0.0174485463463235,0.0174926355298175),
 .UNSPECIFIED.) ;
#1231 = B_SPLINE_CURVE_WITH_KNOTS('',3,(#91698,#91699,#91700,#91701,#91702,
#91703),.UNSPECIFIED.,.F.,.F.,(4,2,4),(-0.00554349508612338,-0.00278303954230401,
-7.86527024303811E-6),.UNSPECIFIED.) ;
#1232 = B_SPLINE_CURVE_WITH_KNOTS('',3,(#91793,#91794,#91795,#91796,#91797,
#91798,#91799,#91800,#91801,#91802,#91803,#91804,#91805,#91806,#91807,#91808,
#91809,#91810,#91811),.UNSPECIFIED.,.F.,.F.,(4,3,3,3,3,3,4),(0.,0.00467491259865511,
0.00948510350195526,0.0145483091112081,0.0197594621886094,0.025280122058927,
0.0297379259389668),.UNSPECIFIED.) ;
#1233 = B_SPLINE_CURVE_WITH_KNOTS('',3,(#91813,#91814,#91815,#91816,#91817,
#91818,#91819),.UNSPECIFIED.,.F.,.F.,(4,3,4),(0.0297379259389668,0.0299720828361244,
0.0300731157523127),.UNSPECIFIED.) ;
#1234 = B_SPLINE_CURVE_WITH_KNOTS('',3,(#91821,#91822,#91823,#91824,#91825,
#91826),.UNSPECIFIED.,.F.,.F.,(4,2,4),(-0.0300731157523127,-0.0299720828361244,
-0.0297216886550733),.UNSPECIFIED.) ;
#1235 = B_SPLINE_CURVE_WITH_KNOTS('',3,(#91827,#91828,#91829,#91830),
 .UNSPECIFIED.,.F.,.F.,(4,4),(-0.0297216886550733,0.),.UNSPECIFIED.) ;
#1236 = B_SPLINE_CURVE_WITH_KNOTS('',3,(#91931,#91932,#91933,#91934,#91935,
#91936,#91937,#91938,#91939,#91940),.UNSPECIFIED.,.F.,.F.,(4,2,2,2,4),(-0.0174676169376883,
-0.0173982625003064,-0.00856749914223533,-0.00158802779347854,0.),
 .UNSPECIFIED.) ;
#1237 = B_SPLINE_CURVE_WITH_KNOTS('',3,(#91946,#91947,#91948,#91949),
 .UNSPECIFIED.,.F.,.F.,(4,4),(1.33431567541952E-15,0.0171168860941288),
 .UNSPECIFIED.) ;
#1238 = B_SPLINE_CURVE_WITH_KNOTS('',3,(#91961,#91962,#91963,#91964,#91965,
#91966,#91967,#91968),.UNSPECIFIED.,.F.,.F.,(4,2,2,4),(-0.0256452708673575,
-0.0124292433503726,-0.00476507154092581,-9.48509615022065E-6),
 .UNSPECIFIED.) ;
#1239 = B_SPLINE_CURVE_WITH_KNOTS('',3,(#91983,#91984,#91985,#91986,#91987,
#91988,#91989,#91990,#91991,#91992,#91993,#91994,#91995,#91996),
 .UNSPECIFIED.,.F.,.F.,(4,2,2,2,2,2,4),(0.0354537163355204,0.0383240848475325,
0.0418682032589909,0.0476210418726295,0.057789083784607,0.0709074326710473,
0.0712608101152448),.UNSPECIFIED.) ;
#1240 = B_SPLINE_CURVE_WITH_KNOTS('',3,(#92000,#92001,#92002,#92003,#92004,
#92005,#92006,#92007,#92008,#92009,#92010,#92011,#92012,#92013),
 .UNSPECIFIED.,.F.,.F.,(4,2,2,2,2,2,4),(-0.0354537163167348,-0.0325833478064478,
-0.0290392293972437,-0.0232863907872553,-0.013118348881858,0.,0.000353377444176431),
 .UNSPECIFIED.) ;
#1241 = B_SPLINE_CURVE_WITH_KNOTS('',3,(#92066,#92067,#92068,#92069,#92070,
#92071,#92072,#92073,#92074,#92075,#92076,#92077,#92078,#92079,#92080,#92081,
#92082,#92083,#92084,#92085,#92086,#92087),.UNSPECIFIED.,.F.,.F.,(4,3,3,
3,3,3,3,4),(-0.0477209576750425,-0.0468497353395086,-0.0434194841369138,
-0.0391915106912518,-0.0334700977178844,-0.0309360218424187,-0.0293311245511305,
-0.0287682560648015),.UNSPECIFIED.) ;
#1242 = B_SPLINE_CURVE_WITH_KNOTS('',3,(#92227,#92228,#92229,#92230,#92231,
#92232),.UNSPECIFIED.,.F.,.F.,(4,2,4),(0.,0.0117562819132905,0.0194026045695574),
 .UNSPECIFIED.) ;
#1243 = B_SPLINE_CURVE_WITH_KNOTS('',3,(#92236,#92237,#92238,#92239,#92240,
#92241),.UNSPECIFIED.,.F.,.F.,(4,2,4),(0.0505532240038504,0.0581995466601177,
0.0699558285734079),.UNSPECIFIED.) ;
#1244 = B_SPLINE_CURVE_WITH_KNOTS('',3,(#92268,#92269,#92270,#92271,#92272,
#92273,#92274),.UNSPECIFIED.,.F.,.F.,(4,3,4),(-0.129427938726121,-0.00760184093280492,
-9.99999994838463E-7),.UNSPECIFIED.) ;
#1245 = B_SPLINE_CURVE_WITH_KNOTS('',3,(#92411,#92412,#92413,#92414,#92415,
#92416),.UNSPECIFIED.,.F.,.F.,(4,2,4),(-0.0699558285734104,-0.0581995466601188,
-0.0505532240038526),.UNSPECIFIED.) ;
#1246 = B_SPLINE_CURVE_WITH_KNOTS('',3,(#92435,#92436,#92437,#92438,#92439,
#92440),.UNSPECIFIED.,.F.,.F.,(4,2,4),(-0.0194026045695577,-0.0117562819132915,
0.),.UNSPECIFIED.) ;
#1247 = B_SPLINE_CURVE_WITH_KNOTS('',3,(#92443,#92444,#92445,#92446,#92447,
#92448),.UNSPECIFIED.,.F.,.F.,(4,2,4),(-0.0194026045695576,-0.01175628191329,
0.),.UNSPECIFIED.) ;
#1248 = B_SPLINE_CURVE_WITH_KNOTS('',3,(#92558,#92559,#92560,#92561,#92562,
#92563,#92564,#92565),.UNSPECIFIED.,.F.,.F.,(4,1,1,1,1,4),(-0.0400607966507765,
-0.0286148547505547,-0.0171689128503328,-0.0114459419002219,-0.00572297095011093,
-9.19824141439016E-31),.UNSPECIFIED.) ;
#1249 = B_SPLINE_CURVE_WITH_KNOTS('',3,(#92568,#92569,#92570,#92571,#92572,
#92573,#92574,#92575),.UNSPECIFIED.,.F.,.F.,(4,1,1,1,1,4),(9.19824141439016E-31,
0.00572297095011093,0.0114459419002219,0.0171689128503328,0.0286148547505547,
0.0400607966507765),.UNSPECIFIED.) ;
#1250 = B_SPLINE_CURVE_WITH_KNOTS('',3,(#92582,#92583,#92584,#92585,#92586,
#92587,#92588,#92589,#92590,#92591,#92592,#92593,#92594,#92595,#92596,#92597,
#92598,#92599,#92600),.UNSPECIFIED.,.F.,.F.,(4,3,3,3,3,3,4),(0.0252869589686981,
0.0279002827276299,0.0312075970894694,0.0359392781305207,0.0430930520183015,
0.0490510238207101,0.049573752749312),.UNSPECIFIED.) ;
#1251 = B_SPLINE_CURVE_WITH_KNOTS('',3,(#92669,#92670,#92671,#92672,#92673,
#92674,#92675,#92676,#92677,#92678,#92679,#92680,#92681,#92682),
 .UNSPECIFIED.,.F.,.F.,(4,2,2,2,2,2,4),(-0.0293717278535513,-0.0114851593454505,
-0.00300187054344729,-0.00150093527172364,-0.00075046763586182,-0.000375233817930908,
3.46944695195361E-18),.UNSPECIFIED.) ;
#1252 = B_SPLINE_CURVE_WITH_KNOTS('',3,(#92810,#92811,#92812,#92813,#92814,
#92815,#92816,#92817,#92818,#92819,#92820,#92821,#92822,#92823,#92824,#92825,
#92826,#92827,#92828,#92829,#92830,#92831,#92832,#92833,#92834),
 .UNSPECIFIED.,.F.,.F.,(4,3,3,3,3,3,3,3,4),(6.85291849789822E-5,0.00224825149847016,
0.00410846025809801,0.00699382185291758,0.00799199065054034,0.0109464436869959,
0.0118449474474184,0.014171090431278,0.0157080392133692),.UNSPECIFIED.) ;
#1253 = B_SPLINE_CURVE_WITH_KNOTS('',3,(#92835,#92836,#92837,#92838),
 .UNSPECIFIED.,.F.,.F.,(4,4),(-7.29056287534871E-5,6.85291849789822E-5),
 .UNSPECIFIED.) ;
#1254 = B_SPLINE_CURVE_WITH_KNOTS('',3,(#92897,#92898,#92899,#92900),
 .UNSPECIFIED.,.F.,.F.,(4,4),(2.15310365171961E-15,0.0294983491188769),
 .UNSPECIFIED.) ;
#1255 = B_SPLINE_CURVE_WITH_KNOTS('',3,(#92936,#92937,#92938,#92939,#92940,
#92941,#92942,#92943,#92944,#92945,#92946,#92947,#92948,#92949,#92950,#92951,
#92952,#92953,#92954,#92955,#92956,#92957,#92958,#92959,#92960),
 .UNSPECIFIED.,.F.,.F.,(4,3,3,3,3,3,3,3,4),(8.270742692011E-19,0.0056026191517687,
0.0117794878631444,0.0162039536314463,0.0221619695143852,0.0231485051877804,
0.0273176591774019,0.0314713233612342,0.0324079072628925),.UNSPECIFIED.) ;
#1256 = B_SPLINE_CURVE_WITH_KNOTS('',3,(#92963,#92964,#92965,#92966,#92967,
#92968),.UNSPECIFIED.,.F.,.F.,(4,1,1,4),(-0.0324079072628925,-0.0231485051877804,
-0.0162039536314463,-8.270742692011E-19),.UNSPECIFIED.) ;
#1257 = B_SPLINE_CURVE_WITH_KNOTS('',3,(#93034,#93035,#93036,#93037,#93038,
#93039,#93040,#93041,#93042,#93043,#93044,#93045,#93046,#93047,#93048,#93049,
#93050,#93051,#93052,#93053,#93054,#93055,#93056,#93057,#93058),
 .UNSPECIFIED.,.F.,.F.,(4,3,3,3,3,3,3,3,4),(0.,0.00415188905280238,0.00832027739506051,
0.00925932038092611,0.0152172958024042,0.0162038106666207,0.0224596241657163,
0.0281435224497628,0.032407621333235),.UNSPECIFIED.) ;
#1258 = B_SPLINE_CURVE_WITH_KNOTS('',3,(#93062,#93063,#93064,#93065,#93066,
#93067),.UNSPECIFIED.,.F.,.F.,(4,1,1,4),(-0.0324076213332414,-0.0162038106666207,
-0.00925932038092611,0.),.UNSPECIFIED.) ;
#1259 = B_SPLINE_CURVE_WITH_KNOTS('',3,(#93111,#93112,#93113,#93114,#93115),
 .UNSPECIFIED.,.F.,.F.,(4,1,4),(-0.0294932405228361,-0.0126399602240726,
0.),.UNSPECIFIED.) ;
#1260 = B_SPLINE_CURVE_WITH_KNOTS('',3,(#93116,#93117,#93118,#93119,#93120),
 .UNSPECIFIED.,.F.,.F.,(4,1,4),(0.,0.0126399602240726,0.0294932405228361),
 .UNSPECIFIED.) ;
#1261 = B_SPLINE_CURVE_WITH_KNOTS('',3,(#93255,#93256,#93257,#93258,#93259),
 .UNSPECIFIED.,.F.,.F.,(4,1,4),(-0.0294932405474481,-0.0168532803128275,
0.),.UNSPECIFIED.) ;
#1262 = B_SPLINE_CURVE_WITH_KNOTS('',3,(#93261,#93262,#93263,#93264,#93265),
 .UNSPECIFIED.,.F.,.F.,(4,1,4),(0.,0.0168532803128275,0.0294932405474481),
 .UNSPECIFIED.) ;
#1263 = B_SPLINE_CURVE_WITH_KNOTS('',3,(#93300,#93301,#93302,#93303),
 .UNSPECIFIED.,.F.,.F.,(4,4),(0.,0.0936141811972385),.UNSPECIFIED.) ;
#1264 = B_SPLINE_CURVE_WITH_KNOTS('',3,(#93679,#93680,#93681,#93682),
 .UNSPECIFIED.,.F.,.F.,(4,4),(-0.0294983491188769,-2.15310365171961E-15),
 .UNSPECIFIED.) ;
#1265 = B_SPLINE_CURVE_WITH_KNOTS('',3,(#93820,#93821,#93822,#93823,#93824,
#93825,#93826,#93827,#93828,#93829,#93830,#93831,#93832,#93833,#93834,#93835,
#93836,#93837,#93838,#93839,#93840,#93841,#93842),.UNSPECIFIED.,.F.,.F.,
(4,2,1,1,1,1,1,1,1,1,1,1,1,1,1,1,1,1,1,4),(-0.158000078699635,-0.148000078699544,
-0.12685721031389,-0.116285776121063,-0.105714341928236,-0.105053627291185,
-0.104392912654133,-0.100428624831823,-0.0951429077354094,-0.0845714735425825,
-0.079285756446169,-0.0766428978979623,-0.0759821832609106,-0.0753214686238589,
-0.0746607539868073,-0.0740000393497556,-0.0634286051569287,-0.0422857367712749,
-0.0211428683856211,-0.0100909341248642),.UNSPECIFIED.) ;
#1266 = B_SPLINE_CURVE_WITH_KNOTS('',3,(#93846,#93847,#93848,#93849,#93850,
#93851,#93852,#93853,#93854,#93855,#93856),.UNSPECIFIED.,.F.,.F.,(4,1,1,
1,1,1,2,4),(-0.208459662581221,-0.179372878146882,-0.155976415779898,-0.124781132623918,
-0.0935858494679386,-0.062390566311959,0.,0.0100000000000179),
 .UNSPECIFIED.) ;
#1267 = B_SPLINE_CURVE_WITH_KNOTS('',3,(#93872,#93873,#93874,#93875,#93876,
#93877,#93878,#93879,#93880,#93881,#93882,#93883,#93884,#93885,#93886,#93887),
 .UNSPECIFIED.,.F.,.F.,(4,2,1,1,1,1,1,1,1,1,1,1,4),(-0.168369812149447,
-0.158369812149344,-0.135745553270846,-0.113121294392348,-0.107465229672724,
-0.101809164953099,-0.0961531002334749,-0.0904970355138505,-0.084840970794226,
-0.0791849060746015,-0.0678727766353526,-0.0226242588783568,-0.0102825850151437),
 .UNSPECIFIED.) ;
#1268 = B_SPLINE_CURVE_WITH_KNOTS('',3,(#93891,#93892,#93893,#93894,#93895,
#93896,#93897,#93898,#93899,#93900,#93901),.UNSPECIFIED.,.F.,.F.,(4,1,1,
1,1,1,2,4),(-0.206302611384505,-0.177449514196477,-0.154303925388241,-0.123443140310593,
-0.0925823552329445,-0.0617215701552963,0.,0.0100000000001109),
 .UNSPECIFIED.) ;
#1269 = B_SPLINE_CURVE_WITH_KNOTS('',3,(#94047,#94048,#94049,#94050,#94051),
 .UNSPECIFIED.,.F.,.F.,(4,1,4),(-0.045647970439003,-0.0195634159024299,
0.),.UNSPECIFIED.) ;
#1270 = B_SPLINE_CURVE_WITH_KNOTS('',3,(#94052,#94053,#94054,#94055,#94056,
#94057,#94058,#94059,#94060,#94061,#94062,#94063,#94064,#94065,#94066,#94067,
#94068,#94069,#94070,#94071,#94072,#94073,#94074,#94075,#94076,#94077,#94078,
#94079),.UNSPECIFIED.,.F.,.F.,(4,3,3,3,3,3,3,3,3,4),(0.,0.00537990329643797,
0.0110107587247129,0.017075331585266,0.0195634159024299,0.0256456020000555,
0.0315029066657429,0.0371776636413155,0.0425892624415814,0.045647970439003),
 .UNSPECIFIED.) ;
#1271 = B_SPLINE_CURVE_WITH_KNOTS('',3,(#94152,#94153,#94154,#94155),
 .UNSPECIFIED.,.F.,.F.,(4,4),(-0.0171168860941288,-1.33431567541952E-15),
 .UNSPECIFIED.) ;
#1272 = B_SPLINE_CURVE_WITH_KNOTS('',3,(#94179,#94180,#94181,#94182,#94183,
#94184,#94185,#94186,#94187,#94188,#94189,#94190,#94191),.UNSPECIFIED.,
 .F.,.F.,(4,3,3,3,4),(0.530502305869095,0.542967004358727,0.555197283003313,
0.567168185545784,0.569716944924395),.UNSPECIFIED.) ;
#1273 = B_SPLINE_CURVE_WITH_KNOTS('',3,(#94243,#94244,#94245,#94246),
 .UNSPECIFIED.,.F.,.F.,(4,4),(0.0564440131838686,0.109806780005479),
 .UNSPECIFIED.) ;
#1274 = B_SPLINE_CURVE_WITH_KNOTS('',3,(#94317,#94318,#94319,#94320,#94321,
#94322,#94323,#94324,#94325,#94326,#94327,#94328,#94329,#94330,#94331,#94332,
#94333,#94334,#94335,#94336,#94337,#94338,#94339,#94340,#94341,#94342,#94343,
#94344),.UNSPECIFIED.,.F.,.F.,(4,3,3,3,3,3,3,3,3,4),(1.1236943236576E-6,
0.00317388582283794,0.00628350468964704,0.00935335072246934,0.0114772233155261,
0.0148928133883393,0.0183304301194573,0.0217988007428664,0.0253473022429601,
0.0267801877362277),.UNSPECIFIED.) ;
#1275 = B_SPLINE_CURVE_WITH_KNOTS('',3,(#94412,#94413,#94414,#94415,#94416,
#94417,#94418,#94419,#94420,#94421,#94422,#94423),.UNSPECIFIED.,.F.,.F.,
(4,2,2,2,2,4),(0.,0.00818348889632409,0.0162723371528994,0.0205125633057343,
0.0248544226127729,0.0249813220785652),.UNSPECIFIED.) ;
#1276 = B_SPLINE_CURVE_WITH_KNOTS('',3,(#94424,#94425,#94426,#94427,#94428),
 .UNSPECIFIED.,.F.,.F.,(4,1,4),(-0.0856917518795941,-0.0595744748887569,
-0.0334715043589776),.UNSPECIFIED.) ;
#1277 = B_SPLINE_CURVE_WITH_KNOTS('',3,(#94433,#94434,#94435,#94436),
 .UNSPECIFIED.,.F.,.F.,(4,4),(0.,0.0936131112963941),.UNSPECIFIED.) ;
#1278 = B_SPLINE_CURVE_WITH_KNOTS('',3,(#94440,#94441,#94442,#94443),
 .UNSPECIFIED.,.F.,.F.,(4,4),(0.,0.0936141814749616),.UNSPECIFIED.) ;
#1279 = B_SPLINE_CURVE_WITH_KNOTS('',3,(#94541,#94542,#94543,#94544,#94545,
#94546,#94547,#94548,#94549,#94550,#94551,#94552,#94553,#94554,#94555,#94556,
#94557,#94558),.UNSPECIFIED.,.F.,.F.,(4,2,2,2,2,2,2,2,4),(-0.0223129172590684,
-0.0168544066118854,-0.0114714787709719,-0.0065572365263978,-0.00563951438992895,
-0.0049148380277049,-0.00389243501027995,-0.00207747054762647,-9.5473990429501E-7),
 .UNSPECIFIED.) ;
#1280 = B_SPLINE_CURVE_WITH_KNOTS('',3,(#94673,#94674,#94675,#94676,#94677,
#94678,#94679,#94680,#94681,#94682),.UNSPECIFIED.,.F.,.F.,(4,2,2,2,4),(-0.0146631250948371,
-0.00714591699534451,-0.00307413779860312,-0.00137081844245783,-2.36480237567184E-5),
 .UNSPECIFIED.) ;
#1281 = B_SPLINE_CURVE_WITH_KNOTS('',3,(#94794,#94795,#94796,#94797),
 .UNSPECIFIED.,.F.,.F.,(4,4),(-0.341768486244514,-0.318230893672861),
 .UNSPECIFIED.) ;
#1282 = B_SPLINE_CURVE_WITH_KNOTS('',3,(#94800,#94801,#94802,#94803),
 .UNSPECIFIED.,.F.,.F.,(4,4),(0.318228890765255,0.341768504405115),
 .UNSPECIFIED.) ;
#1283 = B_SPLINE_CURVE_WITH_KNOTS('',3,(#94810,#94811,#94812,#94813,#94814,
#94815,#94816,#94817,#94818,#94819,#94820,#94821,#94822),.UNSPECIFIED.,
 .F.,.F.,(4,3,3,3,4),(0.110165078811181,0.122187579457333,0.134390211284239,
0.146912945246986,0.149379717866476),.UNSPECIFIED.) ;
#1284 = B_SPLINE_CURVE_WITH_KNOTS('',3,(#94880,#94881,#94882,#94883,#94884,
#94885,#94886),.UNSPECIFIED.,.F.,.F.,(4,3,4),(-0.143004044169051,-0.0211094711173082,
-9.99999994338863E-7),.UNSPECIFIED.) ;
#1285 = B_SPLINE_CURVE_WITH_KNOTS('',3,(#94957,#94958,#94959,#94960,#94961,
#94962,#94963,#94964,#94965,#94966,#94967,#94968,#94969,#94970),
 .UNSPECIFIED.,.F.,.F.,(4,2,2,2,2,2,4),(-0.000104155204377971,-3.86217593415514E-11,
0.00490122913929789,0.009484123212302,0.014276465079669,0.0171575682197624,
0.0199062496531735),.UNSPECIFIED.) ;
#1286 = B_SPLINE_CURVE_WITH_KNOTS('',3,(#95025,#95026,#95027,#95028,#95029,
#95030,#95031,#95032,#95033,#95034),.UNSPECIFIED.,.F.,.F.,(4,1,1,1,1,1,
1,4),(-0.0100926828333812,0.0417412101282966,0.0676581566091356,0.0935751030899745,
0.106533576330394,0.119492049570813,0.132450522811233,0.161355759040101),
 .UNSPECIFIED.) ;
#1287 = B_SPLINE_CURVE_WITH_KNOTS('',3,(#95036,#95037,#95038,#95039,#95040,
#95041,#95042,#95043,#95044,#95045,#95046,#95047,#95048,#95049),
 .UNSPECIFIED.,.F.,.F.,(4,2,2,2,2,2,4),(-0.00010162007045407,0.,0.00486299775130735,
0.00944029817878617,0.014181595291943,0.0169882395959943,0.0196725193024137),
 .UNSPECIFIED.) ;
#1288 = B_SPLINE_CURVE_WITH_KNOTS('',3,(#95050,#95051,#95052,#95053,#95054,
#95055,#95056,#95057,#95058,#95059,#95060,#95061,#95062,#95063,#95064,#95065,
#95066,#95067,#95068,#95069,#95070,#95071,#95072,#95073,#95074,#95075,#95076,
#95077,#95078,#95079,#95080,#95081,#95082,#95083,#95084,#95085,#95086,#95087,
#95088,#95089,#95090,#95091,#95092,#95093,#95094,#95095,#95096,#95097,#95098,
#95099,#95100,#95101,#95102,#95103,#95104,#95105,#95106,#95107,#95108,#95109,
#95110,#95111,#95112,#95113,#95114,#95115,#95116,#95117,#95118,#95119,#95120,
#95121,#95122,#95123,#95124,#95125,#95126,#95127,#95128,#95129,#95130,#95131,
#95132,#95133,#95134,#95135,#95136,#95137,#95138,#95139,#95140,#95141,#95142,
#95143,#95144,#95145,#95146,#95147,#95148,#95149,#95150,#95151,#95152,#95153,
#95154,#95155),.UNSPECIFIED.,.F.,.F.,(4,3,3,3,3,3,3,3,3,3,3,3,3,3,3,3,3,
3,3,3,3,3,3,3,3,3,3,3,3,3,3,3,3,3,3,4),(-0.171325942532491,-0.165652411514985,
-0.160023962991389,-0.154439365331305,-0.148893369077348,-0.143356525209383,
-0.137846834510568,-0.132450522811233,-0.128972714613851,-0.125830929486734,
-0.12198716027631,-0.119492049570813,-0.114252996717646,-0.109668825471125,
-0.107349770539937,-0.105445902026418,-0.101635560910071,-0.097921982835525,
-0.0947866325002212,-0.0930504505530208,-0.0883568045689103,-0.0833681805307477,
-0.0778844727423146,-0.0775796267454788,-0.0727306918766619,-0.068184815437146,
-0.0667474756601821,-0.0611266349681567,-0.0551249595064378,-0.0486421623061817,
-0.04256147562346,-0.0393563002552848,-0.0299724411047558,-0.0185906216435956,
-0.000936915493295949,3.33115559203421E-6),.UNSPECIFIED.) ;
#1289 = B_SPLINE_CURVE_WITH_KNOTS('',3,(#95160,#95161,#95162,#95163,#95164,
#95165,#95166,#95167,#95168,#95169,#95170,#95171,#95172,#95173),
 .UNSPECIFIED.,.F.,.F.,(4,2,2,2,2,2,4),(-0.0178788923403474,-0.0177845502863682,
-0.0133934732125181,-0.00931791430816039,-0.00505589452225569,-0.00246766909513425,
0.),.UNSPECIFIED.) ;
#1290 = B_SPLINE_CURVE_WITH_KNOTS('',3,(#95231,#95232,#95233,#95234,#95235,
#95236,#95237,#95238,#95239,#95240,#95241),.UNSPECIFIED.,.F.,.F.,(4,1,1,
1,1,1,1,1,4),(-0.195028884511668,-0.161022259696524,-0.146383872451384,
-0.117107097961104,-0.0878303234708248,-0.073191936225685,-0.0585535489805452,
-0.0292767744902657,1.38391897109284E-14),.UNSPECIFIED.) ;
#1291 = B_SPLINE_CURVE_WITH_KNOTS('',3,(#95243,#95244,#95245,#95246,#95247,
#95248,#95249,#95250,#95251,#95252,#95253),.UNSPECIFIED.,.F.,.F.,(4,1,1,
1,1,1,1,1,4),(0.0100076242561881,0.0292767744902657,0.0585535489805452,
0.073191936225685,0.0878303234708248,0.117107097961104,0.146383872451384,
0.161022259696524,0.204937421431943),.UNSPECIFIED.) ;
#1292 = B_SPLINE_CURVE_WITH_KNOTS('',3,(#95254,#95255,#95256,#95257,#95258,
#95259,#95260,#95261,#95262,#95263,#95264,#95265,#95266,#95267),
 .UNSPECIFIED.,.F.,.F.,(4,2,2,2,2,2,4),(-0.017736256622245,-0.0176440568681958,
-0.0132953764850671,-0.00922540700529897,-0.00498067116082595,-0.0024336851353481,
0.),.UNSPECIFIED.) ;
#1293 = B_SPLINE_CURVE_WITH_KNOTS('',3,(#95384,#95385,#95386,#95387,#95388,
#95389,#95390,#95391,#95392,#95393,#95394,#95395,#95396,#95397,#95398,#95399),
 .UNSPECIFIED.,.F.,.F.,(4,1,1,1,1,1,1,1,1,1,1,1,1,4),(0.01000334021752,
0.0295575519591679,0.059115103918338,0.088672655877508,0.118230207836678,
0.119153881335402,0.120077554834126,0.121924901831574,0.125619595826471,
0.133008983816263,0.140398371806056,0.144093065800952,0.147787759795848,
0.206902863714188),.UNSPECIFIED.) ;
#1294 = B_SPLINE_CURVE_WITH_KNOTS('',3,(#95401,#95402,#95403,#95404,#95405,
#95406,#95407,#95408,#95409,#95410,#95411,#95412,#95413,#95414),
 .UNSPECIFIED.,.F.,.F.,(4,2,2,2,2,2,4),(-0.0176827121873784,-0.0175909062599249,
-0.0132508379959276,-0.00918624532464143,-0.00495893130814665,-0.0024252092698044,
0.),.UNSPECIFIED.) ;
#1295 = B_SPLINE_CURVE_WITH_KNOTS('',3,(#95416,#95417,#95418,#95419,#95420,
#95421,#95422,#95423,#95424,#95425,#95426,#95427,#95428,#95429,#95430,#95431,
#95432,#95433,#95434,#95435,#95436,#95437,#95438,#95439,#95440,#95441,#95442,
#95443,#95444,#95445,#95446,#95447,#95448,#95449,#95450,#95451,#95452,#95453,
#95454,#95455,#95456,#95457,#95458,#95459,#95460,#95461,#95462,#95463,#95464,
#95465,#95466,#95467,#95468,#95469,#95470,#95471,#95472,#95473,#95474,#95475,
#95476,#95477,#95478,#95479,#95480,#95481,#95482,#95483,#95484,#95485,#95486,
#95487,#95488,#95489,#95490,#95491,#95492,#95493,#95494,#95495,#95496,#95497,
#95498,#95499,#95500,#95501,#95502,#95503,#95504,#95505,#95506,#95507,#95508,
#95509,#95510,#95511,#95512,#95513,#95514,#95515,#95516,#95517,#95518,#95519,
#95520,#95521),.UNSPECIFIED.,.F.,.F.,(4,3,3,3,3,3,3,3,3,3,3,3,3,3,3,3,3,
3,3,3,3,3,3,3,3,3,3,3,3,3,3,3,3,3,3,4),(-0.197162523347665,-0.185428221805325,
-0.172815072988371,-0.162883491013023,-0.154392034322415,-0.147787759795848,
-0.144093065800952,-0.140386955559284,-0.137815595832713,-0.133734101190473,
-0.130078332958677,-0.123836669195403,-0.121279913284718,-0.119931182187908,
-0.118936648793649,-0.117861366913671,-0.111884404652618,-0.105224027606823,
-0.0981642867190361,-0.0928694810531958,-0.0898789028134254,-0.0874314612044946,
-0.0809167123108539,-0.0769850640556748,-0.0673619310487152,-0.0631518103581704,
-0.0595014740038858,-0.0579656444507446,-0.0507199388944013,-0.0432381492298856,
-0.0354523555092146,-0.0296634974360258,-0.0257462330660413,-0.0158461536836325,
-0.00541231684862231,2.12204013797473E-15),.UNSPECIFIED.) ;
#1296 = B_SPLINE_CURVE_WITH_KNOTS('',3,(#95522,#95523,#95524,#95525,#95526,
#95527,#95528,#95529,#95530,#95531,#95532,#95533,#95534,#95535),
 .UNSPECIFIED.,.F.,.F.,(4,2,2,2,2,2,4),(-0.0178405879764861,-0.0177469544214278,
-0.0133665397468608,-0.00928874858233894,-0.00503211426553545,-0.00245657296492195,
0.),.UNSPECIFIED.) ;
#1297 = B_SPLINE_CURVE_WITH_KNOTS('',3,(#95559,#95560,#95561,#95562,#95563,
#95564,#95565,#95566,#95567,#95568,#95569,#95570,#95571,#95572),
 .UNSPECIFIED.,.F.,.F.,(4,2,2,2,2,2,4),(-0.000105117782515234,0.,0.00493324992095991,
0.00954507006010922,0.0143873118328074,0.0173002157143566,0.0200732442869903),
 .UNSPECIFIED.) ;
#1298 = B_SPLINE_CURVE_WITH_KNOTS('',3,(#95639,#95640,#95641,#95642,#95643,
#95644,#95645,#95646,#95647,#95648,#95649,#95650,#95651,#95652,#95653,#95654,
#95655,#95656,#95657,#95658,#95659,#95660,#95661,#95662,#95663,#95664,#95665,
#95666,#95667,#95668,#95669,#95670,#95671,#95672,#95673,#95674,#95675,#95676,
#95677,#95678,#95679,#95680,#95681,#95682,#95683,#95684,#95685,#95686,#95687,
#95688,#95689,#95690,#95691,#95692,#95693,#95694,#95695,#95696,#95697,#95698,
#95699,#95700,#95701,#95702,#95703,#95704,#95705,#95706,#95707,#95708,#95709,
#95710,#95711,#95712,#95713,#95714,#95715,#95716,#95717,#95718,#95719,#95720,
#95721,#95722,#95723,#95724,#95725,#95726,#95727,#95728,#95729,#95730,#95731,
#95732,#95733,#95734,#95735,#95736,#95737,#95738,#95739,#95740,#95741,#95742,
#95743,#95744,#95745,#95746,#95747,#95748,#95749,#95750,#95751,#95752,#95753),
 .UNSPECIFIED.,.F.,.F.,(4,3,3,3,3,3,3,3,3,3,3,3,3,3,3,3,3,3,3,3,3,3,3,3,
3,3,3,3,3,3,3,3,3,3,3,3,3,3,4),(-0.177215824581903,-0.17030695155021,-0.163618926693659,
-0.157169053165717,-0.152969641660887,-0.150909770118349,-0.149305581657313,
-0.143934851050869,-0.138734177892587,-0.133779971680493,-0.131601954446486,
-0.126404873939755,-0.124975937434575,-0.123838209813924,-0.123095140176218,
-0.119886853024125,-0.116610406055776,-0.113180338591535,-0.109502458713641,
-0.105676366361172,-0.102113043504167,-0.0987197845521641,-0.0967028274534084,
-0.0925150665588207,-0.0881219492072544,-0.0833340779411559,-0.0809205515762085,
-0.080118735865623,-0.0767815667188522,-0.0723071648618782,-0.0689908285233252,
-0.0628516389877999,-0.0566815075547967,-0.0496779741197332,-0.0422255974286259,
-0.0327088895574629,-0.0209856075626229,-0.00903256831842716,8.12739771206159E-6),
 .UNSPECIFIED.) ;
#1299 = B_SPLINE_CURVE_WITH_KNOTS('',3,(#95755,#95756,#95757,#95758,#95759,
#95760,#95761,#95762,#95763,#95764,#95765,#95766,#95767),.UNSPECIFIED.,
 .F.,.F.,(4,1,1,1,1,1,1,1,1,1,4),(-0.010282001904707,0.043288805662896,
0.0566815075547967,0.0633778585007471,0.0700742094466975,0.0767705603926478,
0.080118735865623,0.0968596132304989,0.1236450170143,0.150430420798102,
0.167188433543675),.UNSPECIFIED.) ;
#1300 = B_SPLINE_CURVE_WITH_KNOTS('',3,(#95768,#95769,#95770,#95771,#95772,
#95773,#95774,#95775,#95776,#95777,#95778,#95779,#95780,#95781),
 .UNSPECIFIED.,.F.,.F.,(4,2,2,2,2,2,4),(-0.000101449588089462,0.,0.00483514941605568,
0.00939524326714808,0.0141515681069081,0.0169776746522734,0.0196788154735788),
 .UNSPECIFIED.) ;
#1301 = B_SPLINE_CURVE_WITH_KNOTS('',3,(#95813,#95814,#95815,#95816,#95817,
#95818,#95819,#95820,#95821,#95822,#95823,#95824,#95825,#95826,#95827,#95828,
#95829,#95830,#95831,#95832,#95833,#95834,#95835,#95836,#95837,#95838,#95839,
#95840,#95841,#95842,#95843,#95844,#95845,#95846,#95847,#95848,#95849,#95850,
#95851,#95852,#95853,#95854,#95855,#95856,#95857,#95858,#95859,#95860,#95861,
#95862,#95863,#95864,#95865,#95866,#95867,#95868,#95869,#95870,#95871,#95872,
#95873,#95874,#95875,#95876,#95877,#95878,#95879,#95880,#95881,#95882,#95883,
#95884,#95885,#95886,#95887,#95888,#95889,#95890,#95891,#95892,#95893,#95894,
#95895,#95896,#95897,#95898,#95899,#95900,#95901,#95902,#95903,#95904,#95905,
#95906,#95907,#95908,#95909,#95910,#95911,#95912,#95913,#95914,#95915,#95916,
#95917,#95918,#95919,#95920,#95921,#95922,#95923,#95924,#95925,#95926,#95927,
#95928,#95929,#95930,#95931,#95932,#95933,#95934,#95935,#95936,#95937,#95938,
#95939,#95940,#95941,#95942,#95943,#95944,#95945,#95946,#95947,#95948,#95949,
#95950,#95951,#95952,#95953,#95954,#95955,#95956,#95957,#95958,#95959,#95960,
#95961,#95962,#95963),.UNSPECIFIED.,.F.,.F.,(4,3,3,3,3,3,3,3,3,3,3,3,3,
3,3,3,3,3,3,3,3,3,3,3,3,3,3,3,3,3,3,3,3,3,3,3,3,3,3,3,3,3,3,3,3,3,3,3,3,
3,4),(-1.41081590854242E-13,0.0103491921525447,0.0211841901626651,0.0241620336586163,
0.0346906689700701,0.043243695236957,0.0509049151551453,0.0579592044052852,
0.0640311579531103,0.0672167264441228,0.0701609156160853,0.074589955199646,
0.0784184868981158,0.080000656512071,0.0822470185965856,0.0846286186319091,
0.0882902149729238,0.0901096689174299,0.0910088738799008,0.0929106796275256,
0.094767296982211,0.0956149406062722,0.0964897141933299,0.0980072157210099,
0.0995495458830169,0.101158309464652,0.101720958003161,0.102190952996405,
0.103858756677589,0.10544844525405,0.106942574357921,0.107537144758825,
0.109524324640222,0.111493613001422,0.11271545936729,0.113638792421966,
0.117087933645678,0.117401478085021,0.120526599485897,0.123807081707708,
0.127250293897731,0.13085310602188,0.134301105123365,0.135464756099362,
0.136301990452286,0.142360570616147,0.148621853955712,0.153529476394735,
0.155984145694832,0.157726358513963,0.158437098833759),.UNSPECIFIED.) ;
#1302 = B_SPLINE_CURVE_WITH_KNOTS('',3,(#95990,#95991,#95992,#95993,#95994,
#95995,#95996,#95997,#95998,#95999,#96000,#96001,#96002,#96003,#96004,#96005,
#96006,#96007,#96008,#96009,#96010,#96011,#96012,#96013,#96014,#96015,#96016,
#96017,#96018,#96019,#96020,#96021,#96022,#96023,#96024,#96025,#96026,#96027,
#96028,#96029,#96030,#96031,#96032,#96033,#96034,#96035,#96036,#96037,#96038,
#96039,#96040,#96041,#96042,#96043,#96044,#96045,#96046,#96047,#96048,#96049,
#96050,#96051,#96052,#96053,#96054,#96055,#96056,#96057,#96058,#96059,#96060,
#96061,#96062,#96063,#96064,#96065,#96066,#96067,#96068,#96069,#96070,#96071,
#96072,#96073,#96074),.UNSPECIFIED.,.F.,.F.,(4,3,3,3,3,3,3,3,3,3,3,3,3,
3,3,3,3,3,3,3,3,3,3,3,3,3,3,3,4),(7.39226184629487E-5,0.0136598058106041,
0.0271262719666971,0.0405296849046172,0.0524208783693001,0.0614937185449666,
0.0634789335509413,0.0767258083011943,0.0880944587633485,0.0913698481542741,
0.0927499368255514,0.100385237169618,0.108120428760434,0.115978104732835,
0.121432471043905,0.126347332023278,0.134910688538487,0.143620005971135,
0.151284213182461,0.153901104284404,0.155875512280353,0.15796612950932,
0.16550652664177,0.171821397754491,0.177387753248743,0.180427948441218,
0.190045700231785,0.202346657648098,0.216025495543537),.UNSPECIFIED.) ;
#1303 = B_SPLINE_CURVE_WITH_KNOTS('',3,(#96592,#96593,#96594,#96595,#96596,
#96597,#96598,#96599,#96600,#96601,#96602,#96603,#96604,#96605),
 .UNSPECIFIED.,.F.,.F.,(4,2,2,2,2,2,4),(-0.0176214355467283,-0.017530501859727,
-0.0132488502937593,-0.00923793408389468,-0.00503892175603895,-0.00245939376250771,
0.),.UNSPECIFIED.) ;
#1304 = B_SPLINE_CURVE_WITH_KNOTS('',3,(#96607,#96608,#96609,#96610,#96611,
#96612,#96613,#96614,#96615,#96616,#96617,#96618,#96619,#96620,#96621,#96622,
#96623,#96624,#96625,#96626,#96627,#96628,#96629,#96630,#96631,#96632,#96633,
#96634,#96635,#96636,#96637,#96638,#96639,#96640,#96641,#96642,#96643,#96644,
#96645,#96646,#96647,#96648,#96649,#96650,#96651,#96652,#96653,#96654,#96655,
#96656,#96657,#96658,#96659,#96660,#96661,#96662,#96663,#96664,#96665,#96666,
#96667,#96668,#96669,#96670,#96671,#96672,#96673,#96674,#96675,#96676,#96677,
#96678,#96679,#96680,#96681,#96682,#96683,#96684,#96685,#96686,#96687,#96688,
#96689,#96690,#96691,#96692,#96693,#96694,#96695,#96696,#96697,#96698,#96699,
#96700,#96701,#96702,#96703,#96704,#96705,#96706,#96707,#96708,#96709,#96710,
#96711,#96712,#96713,#96714,#96715,#96716,#96717,#96718,#96719,#96720,#96721,
#96722,#96723,#96724,#96725,#96726,#96727,#96728,#96729,#96730,#96731,#96732,
#96733,#96734,#96735,#96736,#96737,#96738,#96739,#96740,#96741,#96742),
 .UNSPECIFIED.,.F.,.F.,(4,3,3,3,3,3,3,3,3,3,3,3,3,3,3,3,3,3,3,3,3,3,3,3,
3,3,3,3,3,3,3,3,3,3,3,3,3,3,3,3,3,3,3,3,3,4),(-3.27226604903845E-14,0.0160117966439575,
0.0211428683856211,0.031714302578448,0.0407823893134045,0.0422857367712749,
0.0492754087599505,0.0557982959251203,0.0617950682355224,0.0634286051569287,
0.0681480760224011,0.0725110490107089,0.0740000393497556,0.0746607539868073,
0.0766428978979623,0.0778912092473952,0.079285756446169,0.0837839956329802,
0.0845714735425825,0.088007436305928,0.091295323036963,0.0942668433925865,
0.0951429077354094,0.0974554089650903,0.0994724153333818,0.100919062094076,
0.103024026638316,0.104392912654133,0.105053627291185,0.105714341928236,
0.107788014864766,0.110048891466238,0.112101300019925,0.114621057440101,
0.116285776121063,0.118457056421753,0.120715341329924,0.123028442844287,
0.125415872099653,0.12685721031389,0.131314440274099,0.135828076616338,
0.140391856397832,0.145055869455185,0.148000078699544,0.148109584576875),
 .UNSPECIFIED.) ;
#1305 = B_SPLINE_CURVE_WITH_KNOTS('',3,(#96743,#96744,#96745,#96746,#96747,
#96748,#96749,#96750,#96751,#96752,#96753,#96754,#96755,#96756),
 .UNSPECIFIED.,.F.,.F.,(4,2,2,2,2,2,4),(-0.0175852662160816,-0.0174945942492549,
-0.0132202758144662,-0.00921513953873651,-0.00502788279858528,-0.00245503564383476,
0.),.UNSPECIFIED.) ;
#1306 = B_SPLINE_CURVE_WITH_KNOTS('',3,(#96760,#96761,#96762,#96763,#96764,
#96765,#96766,#96767,#96768,#96769,#96770,#96771,#96772,#96773),
 .UNSPECIFIED.,.F.,.F.,(4,2,2,2,2,2,4),(-0.0199785618144753,-0.0171739150053981,
-0.0142340627298171,-0.00945030384531014,-0.0048741475451923,0.,0.000102743923195659),
 .UNSPECIFIED.) ;
#1307 = B_SPLINE_CURVE_WITH_KNOTS('',3,(#96781,#96782,#96783,#96784,#96785,
#96786,#96787,#96788,#96789,#96790,#96791,#96792,#96793,#96794),
 .UNSPECIFIED.,.F.,.F.,(4,2,2,2,2,2,4),(-0.000102391965205721,0.,0.00486346247839452,
0.00942960119761456,0.0141914129216922,0.0171211331600819,0.019918128305216),
 .UNSPECIFIED.) ;
#1308 = B_SPLINE_CURVE_WITH_KNOTS('',3,(#96872,#96873,#96874,#96875,#96876,
#96877,#96878,#96879,#96880),.UNSPECIFIED.,.F.,.F.,(4,1,1,1,1,1,4),(0.000114312075647494,
0.062390566311959,0.0935858494679386,0.124781132623918,0.155976415779898,
0.179372878146882,0.218366982091857),.UNSPECIFIED.) ;
#1309 = B_SPLINE_CURVE_WITH_KNOTS('',3,(#97020,#97021,#97022,#97023,#97024,
#97025,#97026,#97027,#97028,#97029,#97030,#97031,#97032,#97033),
 .UNSPECIFIED.,.F.,.F.,(4,2,2,2,2,2,4),(-0.0176806146939217,-0.0175891900945432,
-0.0132974964292661,-0.00928060348132365,-0.00506273387556004,-0.00246851070493003,
0.),.UNSPECIFIED.) ;
#1310 = B_SPLINE_CURVE_WITH_KNOTS('',3,(#97034,#97035,#97036,#97037,#97038,
#97039,#97040,#97041,#97042,#97043,#97044,#97045,#97046,#97047),
 .UNSPECIFIED.,.F.,.F.,(4,2,2,2,2,2,4),(-0.0175931989203968,-0.0175024032743514,
-0.0132245503122902,-0.00921679814022863,-0.00502740345754487,-0.00245476268172447,
0.),.UNSPECIFIED.) ;
#1311 = B_SPLINE_CURVE_WITH_KNOTS('',3,(#97058,#97059,#97060,#97061,#97062,
#97063,#97064,#97065,#97066,#97067,#97068,#97069,#97070,#97071),
 .UNSPECIFIED.,.F.,.F.,(4,2,2,2,2,2,4),(-0.000101340840706905,0.,0.00484233032281562,
0.0094210889116318,0.0145740257047924,0.0180441794667034,0.02136133766618),
 .UNSPECIFIED.) ;
#1312 = B_SPLINE_CURVE_WITH_KNOTS('',3,(#97173,#97174,#97175,#97176,#97177,
#97178,#97179,#97180,#97181,#97182,#97183,#97184,#97185,#97186),
 .UNSPECIFIED.,.F.,.F.,(4,2,2,2,2,2,4),(-0.000102734018361801,0.,0.00489034565378813,
0.00951254000304755,0.0146727528261873,0.0181007070879955,0.0213700605851311),
 .UNSPECIFIED.) ;
#1313 = B_SPLINE_CURVE_WITH_KNOTS('',3,(#97247,#97248,#97249,#97250,#97251,
#97252,#97253,#97254,#97255,#97256,#97257,#97258,#97259,#97260,#97261,#97262,
#97263,#97264,#97265,#97266,#97267,#97268,#97269,#97270,#97271,#97272,#97273,
#97274,#97275,#97276,#97277,#97278,#97279,#97280,#97281,#97282,#97283,#97284,
#97285,#97286,#97287,#97288,#97289,#97290,#97291,#97292,#97293,#97294,#97295),
 .UNSPECIFIED.,.F.,.F.,(4,3,3,3,3,3,3,3,3,3,3,3,3,3,3,3,4),(0.,0.032673883783352,
0.0500024738644771,0.0672069534204982,0.104457829903168,0.14643552926833,
0.209150107398444,0.250248878590514,0.289222712534637,0.299999453075335,
0.329665056211051,0.350002030405379,0.370262793003315,0.400000667676969,
0.418641417258019,0.450001086263869,0.499999999999957),.UNSPECIFIED.) ;
#1314 = B_SPLINE_CURVE_WITH_KNOTS('',3,(#97573,#97574,#97575,#97576,#97577,
#97578,#97579,#97580,#97581,#97582,#97583,#97584,#97585,#97586,#97587,#97588),
 .UNSPECIFIED.,.F.,.F.,(4,3,3,3,3,4),(-0.0789300037689148,-0.0785665817449109,
-0.0585416501678468,-0.0389601328135845,-0.0194590440039062,0.),
 .UNSPECIFIED.) ;
#1315 = B_SPLINE_CURVE_WITH_KNOTS('',3,(#97600,#97601,#97602,#97603,#97604,
#97605,#97606,#97607,#97608,#97609,#97610,#97611,#97612,#97613,#97614,#97615),
 .UNSPECIFIED.,.F.,.F.,(4,3,3,3,3,4),(-0.000440517445296823,0.,0.0197956662855006,
0.0393399095404366,0.0588657095784546,0.0783818325119316),.UNSPECIFIED.) ;
#1316 = B_SPLINE_CURVE_WITH_KNOTS('',3,(#97720,#97721,#97722,#97723),
 .UNSPECIFIED.,.F.,.F.,(4,4),(-0.0936131112963942,0.),.UNSPECIFIED.) ;
#1317 = B_SPLINE_CURVE_WITH_KNOTS('',3,(#97725,#97726,#97727,#97728),
 .UNSPECIFIED.,.F.,.F.,(4,4),(0.,0.0936131112963942),.UNSPECIFIED.) ;
#1318 = B_SPLINE_CURVE_WITH_KNOTS('',3,(#97771,#97772,#97773,#97774,#97775,
#97776,#97777,#97778,#97779,#97780,#97781,#97782,#97783,#97784,#97785,#97786),
 .UNSPECIFIED.,.F.,.F.,(4,3,3,3,3,4),(-0.000440517445296842,0.,0.0197956662855012,
0.0393399095404381,0.0588657095784568,0.0783818325119346),.UNSPECIFIED.) ;
#1319 = B_SPLINE_CURVE_WITH_KNOTS('',3,(#97810,#97811,#97812,#97813),
 .UNSPECIFIED.,.F.,.F.,(4,4),(-0.0936141814749616,0.),.UNSPECIFIED.) ;
#1320 = B_SPLINE_CURVE_WITH_KNOTS('',3,(#97820,#97821,#97822,#97823,#97824,
#97825,#97826,#97827,#97828,#97829,#97830,#97831,#97832,#97833,#97834,#97835),
 .UNSPECIFIED.,.F.,.F.,(4,3,3,3,3,4),(-0.0788196095195842,-0.0783791073898761,
-0.0585841293455798,-0.0390405655905564,-0.019515444411231,0.),
 .UNSPECIFIED.) ;
#1321 = B_SPLINE_CURVE_WITH_KNOTS('',3,(#97891,#97892,#97893,#97894),
 .UNSPECIFIED.,.F.,.F.,(4,4),(-0.0936131112963941,0.),.UNSPECIFIED.) ;
#1322 = B_SPLINE_CURVE_WITH_KNOTS('',3,(#97926,#97927,#97928,#97929),
 .UNSPECIFIED.,.F.,.F.,(4,4),(-0.0936141811972385,0.),.UNSPECIFIED.) ;
#1323 = B_SPLINE_CURVE_WITH_KNOTS('',3,(#97936,#97937,#97938,#97939,#97940,
#97941,#97942,#97943,#97944,#97945,#97946,#97947,#97948,#97949,#97950,#97951),
 .UNSPECIFIED.,.F.,.F.,(4,3,3,3,3,4),(-0.0788196095195841,-0.0783791073898759,
-0.0585841293455797,-0.0390405655905564,-0.019515444411231,0.),
 .UNSPECIFIED.) ;
#1324 = B_SPLINE_CURVE_WITH_KNOTS('',3,(#98190,#98191,#98192,#98193,#98194,
#98195),.UNSPECIFIED.,.F.,.F.,(4,2,4),(-0.0699558285734079,-0.0581995466601182,
-0.0505532240038504),.UNSPECIFIED.) ;
#1325 = B_SPLINE_CURVE_WITH_KNOTS('',3,(#98212,#98213,#98214,#98215,#98216,
#98217),.UNSPECIFIED.,.F.,.F.,(4,2,4),(-0.0194026045695574,-0.0117562819132905,
0.),.UNSPECIFIED.) ;
#1326 = B_SPLINE_CURVE_WITH_KNOTS('',3,(#98320,#98321,#98322,#98323,#98324,
#98325),.UNSPECIFIED.,.F.,.F.,(4,2,4),(-0.0279464003916688,-0.0169330751594897,
0.),.UNSPECIFIED.) ;
#1327 = B_SPLINE_CURVE_WITH_KNOTS('',3,(#98446,#98447,#98448,#98449,#98450,
#98451),.UNSPECIFIED.,.F.,.F.,(4,2,4),(-0.0161351759984767,-0.00635867011347371,
0.),.UNSPECIFIED.) ;
#1328 = B_SPLINE_CURVE_WITH_KNOTS('',3,(#98481,#98482,#98483,#98484,#98485,
#98486),.UNSPECIFIED.,.F.,.F.,(4,2,4),(-0.0161351760106074,-0.00635867011825523,
0.),.UNSPECIFIED.) ;
#1329 = B_SPLINE_CURVE_WITH_KNOTS('',3,(#98755,#98756,#98757,#98758,#98759,
#98760,#98761,#98762,#98763,#98764,#98765,#98766,#98767,#98768,#98769,#98770,
#98771,#98772,#98773,#98774,#98775,#98776,#98777,#98778,#98779,#98780,#98781,
#98782,#98783,#98784,#98785,#98786,#98787,#98788,#98789,#98790,#98791,#98792,
#98793,#98794,#98795,#98796,#98797,#98798,#98799,#98800,#98801,#98802,#98803,
#98804,#98805,#98806,#98807,#98808,#98809,#98810,#98811,#98812,#98813,#98814,
#98815,#98816,#98817,#98818,#98819,#98820,#98821,#98822,#98823,#98824,#98825,
#98826,#98827,#98828,#98829,#98830,#98831,#98832,#98833,#98834),
 .UNSPECIFIED.,.F.,.F.,(4,2,2,2,2,2,2,2,2,2,2,2,2,2,2,2,2,2,2,2,2,2,2,2,
2,2,2,2,2,2,2,2,2,2,2,2,2,2,2,4),(-0.552597174673262,-0.552087978909823,
-0.543418802839412,-0.530986321926872,-0.515688074017889,-0.48901852632236,
-0.475795340291992,-0.469803806354904,-0.464827465085121,-0.456763485566357,
-0.446125790999932,-0.412222627640349,-0.396458552376544,-0.387367130961374,
-0.378547259036367,-0.364712615477276,-0.330180734182639,-0.312888098213682,
-0.306688567552087,-0.301731961915121,-0.294013236156573,-0.284057413245719,
-0.255750077060834,-0.235801635191627,-0.226007051069487,-0.217361674208648,
-0.205388809034252,-0.190982053575729,-0.163245460668606,-0.148987082829673,
-0.143002701370855,-0.137919038363949,-0.129466900901552,-0.118084610051148,
-0.0761832714464343,-0.0655381220499832,-0.0569431610964917,-0.0461350849955365,
-0.0209625497341524,-0.00261038353153479),.UNSPECIFIED.) ;
#1330 = B_SPLINE_CURVE_WITH_KNOTS('',3,(#98837,#98838,#98839,#98840,#98841,
#98842,#98843,#98844,#98845,#98846,#98847,#98848,#98849,#98850,#98851,#98852,
#98853,#98854,#98855,#98856,#98857,#98858,#98859,#98860,#98861,#98862,#98863,
#98864,#98865,#98866,#98867,#98868,#98869,#98870,#98871,#98872,#98873,#98874,
#98875,#98876,#98877,#98878,#98879,#98880,#98881,#98882,#98883,#98884,#98885,
#98886),.UNSPECIFIED.,.F.,.F.,(4,2,2,2,2,2,2,2,2,2,2,2,2,2,2,2,2,2,2,2,
2,2,2,2,4),(-1.74405659608,-1.74024862573011,-1.7354490695973,-1.69761675650509,
-1.68391129329674,-1.67222759893424,-1.66298762114359,-1.6513941256668,
-1.6159137516185,-1.59065618245596,-1.58351862500578,-1.57860240737983,
-1.57213220939518,-1.537477246215,-1.51410228040979,-1.50437755876619,-1.49602419307963,
-1.48490892270242,-1.45580246644061,-1.43518707323026,-1.42657793655706,
-1.41966295247194,-1.41491213816115,-1.40875298679861,-1.40019423751868),
 .UNSPECIFIED.) ;
#1331 = B_SPLINE_CURVE_WITH_KNOTS('',3,(#98891,#98892,#98893,#98894,#98895,
#98896,#98897,#98898,#98899,#98900,#98901,#98902,#98903,#98904,#98905,#98906,
#98907,#98908,#98909,#98910,#98911,#98912,#98913,#98914,#98915,#98916,#98917,
#98918,#98919,#98920,#98921,#98922,#98923,#98924,#98925,#98926,#98927,#98928,
#98929,#98930,#98931,#98932,#98933,#98934,#98935,#98936,#98937,#98938,#98939,
#98940,#98941,#98942,#98943,#98944,#98945,#98946,#98947,#98948,#98949,#98950,
#98951,#98952,#98953,#98954,#98955,#98956,#98957,#98958,#98959,#98960,#98961,
#98962,#98963,#98964,#98965,#98966,#98967,#98968,#98969,#98970,#98971,#98972,
#98973,#98974,#98975,#98976,#98977,#98978,#98979,#98980,#98981,#98982,#98983,
#98984,#98985,#98986,#98987,#98988,#98989,#98990,#98991,#98992,#98993,#98994,
#98995,#98996,#98997,#98998,#98999,#99000,#99001,#99002,#99003,#99004,#99005,
#99006,#99007,#99008,#99009,#99010,#99011,#99012,#99013,#99014,#99015,#99016,
#99017,#99018,#99019,#99020,#99021,#99022,#99023,#99024,#99025,#99026,#99027,
#99028,#99029,#99030,#99031,#99032),.UNSPECIFIED.,.F.,.F.,(4,2,2,2,2,2,
2,2,2,2,2,2,2,2,2,2,2,2,2,2,2,2,2,2,2,2,2,2,2,2,2,2,2,2,2,2,2,2,2,2,2,2,
2,2,2,2,2,2,2,2,2,2,2,2,2,2,2,2,2,2,2,2,2,2,2,2,2,2,2,2,4),(-1.60817871985196,
-1.60188697181691,-1.56617428509184,-1.54984087223545,-1.53688654692764,
-1.52815941900595,-1.51880035364366,-1.50119252756857,-1.46500106568252,
-1.45686511127176,-1.45016915517214,-1.4452730535428,-1.43827422610191,
-1.410720873795,-1.38068642007219,-1.37024130049903,-1.36171438017231,-1.35090239215872,
-1.31818186378263,-1.29333652168782,-1.28676822558853,-1.28186617089387,
-1.27471523608405,-1.25426210693583,-1.22954377855377,-1.21768281934354,
-1.20715919419871,-1.19863292932375,-1.18790517373592,-1.15426873354839,
-1.13057394980088,-1.12379973616585,-1.11890417570126,-1.11198677312076,
-1.08351739597117,-1.05355856892254,-1.04333843073385,-1.03479834540627,
-1.0238910563505,-0.996287106129177,-0.976227453852334,-0.964288354181759,
-0.958706935650863,-0.953530612564683,-0.944174280916242,-0.930866568317175,
-0.891101252113233,-0.880607430471217,-0.872083906506385,-0.861333132529412,
-0.836212201841313,-0.803368395572518,-0.796967637358088,-0.792061871113417,
-0.784846056910506,-0.775799271108273,-0.753119298036319,-0.728813193822705,
-0.717960451683399,-0.709427961265852,-0.69900655346212,-0.687320352856108,
-0.663461993928104,-0.641640554378349,-0.634492327931047,-0.62958458215972,
-0.622992165537731,-0.615037058215324,-0.580754809747541,-0.561631838713906,
-0.552597174673262),.UNSPECIFIED.) ;
#1332 = B_SPLINE_CURVE_WITH_KNOTS('',3,(#99033,#99034,#99035,#99036,#99037,
#99038,#99039,#99040,#99041,#99042,#99043,#99044,#99045,#99046,#99047,#99048,
#99049,#99050,#99051,#99052,#99053,#99054,#99055,#99056,#99057,#99058,#99059,
#99060,#99061,#99062,#99063,#99064,#99065,#99066,#99067,#99068,#99069,#99070,
#99071,#99072,#99073,#99074,#99075,#99076,#99077,#99078,#99079,#99080,#99081,
#99082,#99083,#99084,#99085,#99086,#99087,#99088,#99089,#99090,#99091,#99092,
#99093,#99094,#99095,#99096,#99097,#99098,#99099,#99100,#99101,#99102,#99103,
#99104,#99105,#99106,#99107,#99108,#99109,#99110,#99111,#99112,#99113,#99114,
#99115,#99116,#99117,#99118,#99119,#99120,#99121,#99122,#99123,#99124,#99125,
#99126,#99127,#99128,#99129,#99130,#99131,#99132,#99133,#99134,#99135,#99136,
#99137,#99138,#99139,#99140,#99141,#99142,#99143,#99144,#99145,#99146,#99147,
#99148,#99149,#99150,#99151,#99152,#99153,#99154,#99155,#99156,#99157,#99158,
#99159,#99160,#99161,#99162,#99163,#99164,#99165,#99166,#99167,#99168,#99169,
#99170,#99171,#99172,#99173,#99174),.UNSPECIFIED.,.F.,.F.,(4,2,2,2,2,2,
2,2,2,2,2,2,2,2,2,2,2,2,2,2,2,2,2,2,2,2,2,2,2,2,2,2,2,2,2,2,2,2,2,2,2,2,
2,2,2,2,2,2,2,2,2,2,2,2,2,2,2,2,2,2,2,2,2,2,2,2,2,2,2,2,4),(-1.40019423751868,
-1.39059856461891,-1.35667598468847,-1.34290959713784,-1.33402342554946,
-1.32475733166678,-1.30815172066439,-1.27149851334997,-1.26331601166393,
-1.25658126033718,-1.25163113413534,-1.24446124954234,-1.22317299546722,
-1.19893660798004,-1.18715522406132,-1.17666499379619,-1.16809990650696,
-1.1572276585662,-1.12501053474387,-1.10009161766894,-1.09338700792244,
-1.08848701787225,-1.08148107106248,-1.05412084897453,-1.02341461347077,
-1.01315335487947,-1.00465968991157,-0.993932385879927,-0.961647123834745,
-0.936270329728169,-0.929746618015904,-0.92485572071812,-0.917705462014288,
-0.896911887819304,-0.872394270882754,-0.856049781705572,-0.846849723712218,
-0.838025885909813,-0.824390338136546,-0.790915249737361,-0.772823406769396,
-0.766455259867575,-0.761540972127907,-0.754256062725515,-0.745085604668567,
-0.721717226155916,-0.698227847610382,-0.687432671047302,-0.678903412564833,
-0.668436939858761,-0.637290397758027,-0.610963216220392,-0.603901842352647,
-0.599004302864263,-0.592366007013439,-0.56867953784493,-0.534621186939995,
-0.523939302554265,-0.515418012823645,-0.504864049701461,-0.492948449919942,
-0.467963543295212,-0.447868495117718,-0.440716118091854,-0.435815634952121,
-0.429254383948027,-0.40396129016647,-0.371801441673548,-0.360942278777566,
-0.35241374076114,-0.344414753026734),.UNSPECIFIED.) ;
#1333 = B_SPLINE_CURVE_WITH_KNOTS('',3,(#99180,#99181,#99182,#99183,#99184,
#99185,#99186,#99187),.UNSPECIFIED.,.F.,.F.,(4,1,1,1,1,4),(21.9911559755827,
22.8773584072894,23.848998189505,24.8206379717207,25.7922777539364,26.2282473494963),
 .UNSPECIFIED.) ;
#1334 = B_SPLINE_CURVE_WITH_KNOTS('',3,(#99188,#99189,#99190,#99191,#99192,
#99193,#99194,#99195,#99196,#99197,#99198,#99199,#99200,#99201,#99202,#99203,
#99204,#99205,#99206,#99207,#99208,#99209,#99210,#99211,#99212,#99213,#99214,
#99215,#99216,#99217,#99218,#99219,#99220,#99221,#99222,#99223,#99224,#99225,
#99226,#99227,#99228,#99229,#99230,#99231,#99232,#99233,#99234,#99235,#99236,
#99237),.UNSPECIFIED.,.F.,.F.,(4,2,2,2,2,2,2,2,2,2,2,2,2,2,2,2,2,2,2,2,
2,2,2,2,4),(-1.95186686044663,-1.9451727728085,-1.93967548024574,-1.93493962460603,
-1.92792572995927,-1.90152501587077,-1.87059969230919,-1.86007646778741,
-1.85155154543861,-1.84082680150995,-1.80717942800767,-1.78322121868641,
-1.77657104095611,-1.77167346878357,-1.76462252246752,-1.73795912356653,
-1.70712279558588,-1.69668728374485,-1.68816018090868,-1.67733734324366,
-1.64474656626435,-1.6204670242381,-1.61360536890348,-1.60871139946509,
-1.60817871985196),.UNSPECIFIED.) ;
#1335 = B_SPLINE_CURVE_WITH_KNOTS('',3,(#99239,#99240,#99241,#99242,#99243,
#99244,#99245,#99246,#99247,#99248,#99249,#99250,#99251,#99252,#99253,#99254,
#99255,#99256,#99257,#99258,#99259,#99260,#99261,#99262,#99263,#99264,#99265,
#99266,#99267,#99268,#99269,#99270,#99271,#99272,#99273,#99274,#99275,#99276,
#99277,#99278,#99279,#99280,#99281,#99282,#99283,#99284,#99285,#99286,#99287,
#99288),.UNSPECIFIED.,.F.,.F.,(4,2,2,2,2,2,2,2,2,2,2,2,2,2,2,2,2,2,2,2,
2,2,2,2,4),(-0.344414753026734,-0.342008927015211,-0.330348848139387,-0.306608071890107,
-0.284590171653946,-0.277445774946498,-0.272544248501529,-0.265971783203178,
-0.240098440585068,-0.20869911101062,-0.197899738456524,-0.189367850672706,
-0.179070471921566,-0.14943964187475,-0.120798932996502,-0.113894953777187,
-0.109001470737898,-0.102221682855731,-0.0939417781600824,-0.0750956593381936,
-0.0453269004351953,-0.0345663159816099,-0.0260362888104047,-0.0179340362145887,
-0.000450587274275642),.UNSPECIFIED.) ;
#1336 = B_SPLINE_CURVE_WITH_KNOTS('',3,(#99289,#99290,#99291,#99292,#99293,
#99294,#99295,#99296,#99297),.UNSPECIFIED.,.F.,.F.,(4,1,1,1,1,1,4),(21.991153076628,
22.3032518321271,23.2748916143428,24.2465313965585,25.2181711787741,26.1898109609898,
26.2282235152758),.UNSPECIFIED.) ;
#1337 = B_SPLINE_CURVE_WITH_KNOTS('',3,(#99303,#99304,#99305,#99306,#99307,
#99308,#99309,#99310,#99311,#99312,#99313,#99314,#99315,#99316,#99317,#99318,
#99319,#99320,#99321,#99322,#99323,#99324,#99325,#99326,#99327,#99328,#99329,
#99330,#99331,#99332,#99333,#99334,#99335,#99336,#99337,#99338,#99339,#99340,
#99341,#99342,#99343,#99344,#99345,#99346,#99347,#99348,#99349,#99350,#99351,
#99352,#99353,#99354,#99355,#99356,#99357,#99358,#99359,#99360,#99361,#99362,
#99363,#99364,#99365,#99366,#99367,#99368,#99369,#99370,#99371,#99372,#99373,
#99374,#99375,#99376,#99377,#99378,#99379,#99380,#99381,#99382,#99383,#99384,
#99385,#99386,#99387,#99388,#99389,#99390,#99391,#99392,#99393,#99394,#99395,
#99396,#99397,#99398,#99399,#99400,#99401,#99402,#99403,#99404,#99405,#99406,
#99407,#99408,#99409,#99410,#99411,#99412,#99413,#99414,#99415,#99416,#99417,
#99418,#99419,#99420),.UNSPECIFIED.,.F.,.F.,(4,3,3,3,3,3,3,3,3,3,3,3,3,
3,3,3,3,3,3,3,3,3,3,3,3,3,3,3,3,3,3,3,3,3,3,3,3,3,3,4),(28.2743338823083,
28.3918577143769,28.5096434298568,28.627852053642,28.7071971005834,28.8171687317807,
28.9269585285024,29.0366468598356,29.1462735902616,29.2558784995052,29.3655762062641,
29.4753180348027,29.5852552742705,29.6788368827991,29.788799074535,29.8985797766649,
30.0082592302568,30.1178773128371,30.2274738174318,30.337163559117,30.4468976537998,
30.5568276341267,30.6504766650147,30.7603622112468,30.8700658671167,30.9796680949326,
31.0892089139856,31.1987282589466,31.3083416196759,31.4179996566885,31.5278550625658,
31.6221164472304,31.7332153421388,31.8431388376641,31.9529583560026,32.0627135252056,
32.1747620455285,32.2845571568611,32.3977323816792,32.5109076064973),
 .UNSPECIFIED.) ;
#1338 = B_SPLINE_CURVE_WITH_KNOTS('',3,(#99421,#99422,#99423,#99424,#99425,
#99426),.UNSPECIFIED.,.F.,.F.,(4,1,1,4),(26.2282473494963,26.763917536152,
27.7355573183677,28.2743338823083),.UNSPECIFIED.) ;
#1339 = B_SPLINE_CURVE_WITH_KNOTS('',3,(#99428,#99429,#99430,#99431,#99432,
#99433),.UNSPECIFIED.,.F.,.F.,(4,1,1,4),(26.2282235152758,27.1614507432055,
28.1330905254212,28.2743338823083),.UNSPECIFIED.) ;
#1340 = B_SPLINE_CURVE_WITH_KNOTS('',3,(#99434,#99435,#99436,#99437,#99438,
#99439,#99440,#99441,#99442,#99443,#99444,#99445,#99446,#99447,#99448,#99449,
#99450,#99451,#99452,#99453,#99454,#99455,#99456,#99457,#99458,#99459,#99460,
#99461,#99462,#99463,#99464,#99465,#99466,#99467,#99468,#99469,#99470,#99471,
#99472,#99473,#99474,#99475,#99476,#99477,#99478,#99479,#99480,#99481,#99482,
#99483,#99484,#99485,#99486,#99487,#99488,#99489,#99490,#99491,#99492,#99493,
#99494,#99495,#99496,#99497,#99498,#99499,#99500,#99501,#99502,#99503,#99504,
#99505,#99506,#99507,#99508,#99509,#99510,#99511,#99512,#99513,#99514,#99515,
#99516,#99517,#99518,#99519,#99520,#99521,#99522,#99523,#99524,#99525,#99526,
#99527,#99528,#99529,#99530,#99531,#99532,#99533),.UNSPECIFIED.,.F.,.F.,
(4,2,2,2,2,2,2,2,2,2,2,2,2,2,2,2,2,2,2,2,2,2,2,2,2,2,2,2,2,2,2,2,2,2,2,
2,2,2,2,2,2,2,2,2,2,2,2,2,2,4),(0.71239184097541,0.712394397109961,0.721192745130405,
0.734671500759373,0.752082681774165,0.785389301747164,0.792361482669575,
0.797255532613846,0.803969694657684,0.812137997382168,0.848691796614872,
0.866018595123892,0.875338577534295,0.884075623393995,0.897136442047152,
0.913687074888232,0.949536070553263,0.956049447834536,0.960945375490526,
0.968005360973277,0.976776672286265,0.997997587656753,1.02408233804888,
1.03492929727984,1.04346381630968,1.05372425154729,1.08322460952202,1.11212627116881,
1.11900052456233,1.12389412033395,1.13070424102562,1.13903754049952,1.1581264104363,
1.18716937335988,1.19807583912576,1.20661269099351,1.21682479433147,1.24642058771588,
1.27539968756184,1.28226660540231,1.28715951003292,1.293974316854,1.30231588418635,
1.3214434868297,1.35042743331143,1.36133490544489,1.36987153696253,1.38008212757361,
1.40961316219556,1.42438117464762),.UNSPECIFIED.) ;
#1341 = B_SPLINE_CURVE_WITH_KNOTS('',3,(#99539,#99540,#99541,#99542,#99543,
#99544,#99545,#99546),.UNSPECIFIED.,.F.,.F.,(4,1,1,1,1,4),(-27.2059139020388,
-26.2342741198231,-25.2626343376075,-24.2909945553918,-23.3193547731761,
-22.9423101986588),.UNSPECIFIED.) ;
#1342 = B_SPLINE_CURVE_WITH_KNOTS('',3,(#99548,#99549,#99550,#99551,#99552,
#99553,#99554,#99555,#99556,#99557,#99558,#99559,#99560,#99561,#99562,#99563,
#99564,#99565,#99566,#99567,#99568,#99569,#99570,#99571,#99572,#99573,#99574,
#99575,#99576,#99577,#99578,#99579,#99580,#99581,#99582,#99583,#99584,#99585,
#99586,#99587,#99588,#99589,#99590,#99591,#99592,#99593,#99594,#99595,#99596,
#99597,#99598,#99599,#99600,#99601,#99602,#99603,#99604,#99605,#99606,#99607,
#99608,#99609,#99610,#99611,#99612,#99613,#99614,#99615,#99616,#99617,#99618,
#99619,#99620,#99621,#99622,#99623,#99624,#99625,#99626,#99627,#99628,#99629,
#99630,#99631,#99632,#99633,#99634,#99635,#99636,#99637,#99638,#99639,#99640,
#99641,#99642,#99643,#99644,#99645,#99646,#99647,#99648,#99649,#99650,#99651,
#99652,#99653,#99654,#99655,#99656,#99657,#99658,#99659,#99660,#99661,#99662,
#99663,#99664,#99665,#99666,#99667,#99668,#99669,#99670,#99671,#99672,#99673,
#99674,#99675,#99676,#99677,#99678,#99679,#99680,#99681,#99682,#99683,#99684,
#99685,#99686,#99687,#99688,#99689,#99690,#99691,#99692,#99693,#99694,#99695,
#99696,#99697,#99698,#99699,#99700,#99701,#99702,#99703,#99704,#99705,#99706,
#99707,#99708,#99709,#99710,#99711,#99712,#99713,#99714,#99715,#99716,#99717,
#99718,#99719,#99720,#99721,#99722,#99723,#99724,#99725,#99726,#99727,#99728,
#99729,#99730,#99731,#99732,#99733,#99734,#99735,#99736,#99737,#99738,#99739,
#99740),.UNSPECIFIED.,.F.,.F.,(4,3,3,3,3,3,3,3,3,3,3,3,3,3,3,3,3,3,3,3,
3,3,3,3,3,3,3,3,3,3,3,3,3,3,3,3,3,3,3,3,3,3,3,3,3,3,3,3,3,3,3,3,3,3,3,3,
3,3,3,3,3,3,3,3,4),(-22.9423049617328,-22.8359148801892,-22.7294989965987,
-22.6229467860948,-22.5163206965427,-22.4094948198208,-22.3477149909605,
-22.2419915581329,-22.1337520144594,-22.0282967847123,-21.9229011330953,
-21.8175296898858,-21.7071660696005,-21.601672616691,-21.496111283468,-21.3903880127637,
-21.3760752087448,-21.2703449398838,-21.1621062507144,-21.0566433996443,
-20.9512398559663,-20.8458602624753,-20.7355040534888,-20.6300018920914,
-20.5244316643326,-20.4186992962299,-20.4044354265291,-20.2987232478075,
-20.1904822973707,-20.0850383870169,-19.9796540446497,-19.8742938798852,
-19.7639193209922,-19.6584369302253,-19.5528865727019,-19.4471740767142,
-19.4327956443134,-19.3270755254136,-19.2188355674991,-19.1133834622704,
-19.0079908543491,-18.9026223676423,-18.7922557412562,-18.6867649852429,
-18.5812062554424,-18.4754854358354,-18.4611558620978,-18.3554360769796,
-18.2471960773424,-18.1417442640643,-18.0363519316643,-17.9309837035316,
-17.8206167976192,-17.7151262543179,-17.6095677211043,-17.5038470738284,
-17.4895160798821,-17.385308618441,-17.2812327055803,-17.1772506824177,
-17.0733250178827,-16.9693644269059,-16.8653930128412,-16.7612777927426,
-16.6591196549159),.UNSPECIFIED.) ;
#1343 = B_SPLINE_CURVE_WITH_KNOTS('',3,(#99742,#99743,#99744,#99745,#99746,
#99747,#99748,#99749,#99750,#99751,#99752,#99753,#99754,#99755,#99756,#99757,
#99758,#99759,#99760,#99761,#99762,#99763,#99764,#99765,#99766,#99767,#99768,
#99769,#99770,#99771,#99772,#99773,#99774,#99775,#99776,#99777,#99778,#99779,
#99780,#99781,#99782,#99783,#99784,#99785,#99786,#99787,#99788,#99789,#99790,
#99791,#99792,#99793,#99794,#99795,#99796,#99797,#99798,#99799,#99800,#99801,
#99802,#99803,#99804,#99805,#99806,#99807,#99808,#99809,#99810,#99811,#99812,
#99813,#99814,#99815,#99816,#99817,#99818,#99819,#99820,#99821,#99822,#99823,
#99824,#99825,#99826,#99827,#99828,#99829,#99830,#99831,#99832,#99833,#99834,
#99835,#99836,#99837,#99838,#99839,#99840,#99841,#99842,#99843,#99844,#99845,
#99846,#99847,#99848,#99849,#99850,#99851,#99852,#99853,#99854,#99855,#99856,
#99857,#99858,#99859,#99860,#99861,#99862,#99863,#99864,#99865,#99866,#99867,
#99868,#99869,#99870,#99871,#99872,#99873,#99874,#99875,#99876,#99877,#99878,
#99879,#99880,#99881,#99882,#99883,#99884,#99885,#99886,#99887,#99888,#99889,
#99890,#99891,#99892,#99893,#99894,#99895,#99896,#99897,#99898,#99899,#99900,
#99901,#99902,#99903,#99904,#99905,#99906,#99907,#99908,#99909,#99910,#99911,
#99912,#99913,#99914,#99915,#99916,#99917,#99918,#99919,#99920,#99921,#99922,
#99923,#99924,#99925,#99926,#99927,#99928,#99929,#99930,#99931,#99932,#99933,
#99934),.UNSPECIFIED.,.F.,.F.,(4,3,3,3,3,3,3,3,3,3,3,3,3,3,3,3,3,3,3,3,
3,3,3,3,3,3,3,3,3,3,3,3,3,3,3,3,3,3,3,3,3,3,3,3,3,3,3,3,3,3,3,3,3,3,3,3,
3,3,3,3,3,3,3,3,4),(-16.6591196545535,-16.5178762976664,-16.4121571798967,
-16.303917096841,-16.1984659957846,-16.0930743902226,-15.9877069023141,
-15.8773393055983,-15.7718495275461,-15.6662917675439,-15.5605718993772,
-15.5462365154507,-15.4405175111645,-15.3322774139233,-15.2268264264059,
-15.1214349340659,-15.0160675588606,-14.9056998524542,-14.8002101844403,
-14.6946525334436,-14.5889327720487,-14.5745967332351,-14.4688778257925,
-14.3606377164459,-14.2551868319594,-14.1497954446504,-14.0444281762974,
-13.9340603699779,-13.8285708121443,-13.7230132723779,-13.6172936229251,
-13.6029569510194,-13.497238049513,-13.3889979394243,-13.283547057409,-13.1781556712829,
-13.0727884028267,-12.9624205943209,-12.8569310331724,-12.7513734889853,
-12.6456538335856,-12.6313171688037,-12.5255981556417,-12.41735805951,-12.3119070682978,
-12.2065155741889,-12.1011481991378,-11.9907804960004,-11.8852908329427,
-11.7797331885556,-11.6740134360523,-11.6596773865881,-11.5539582669364,
-11.4457181841159,-11.340267082276,-11.2348754763391,-11.1295079884633,
-11.0191403924406,-10.9136506154393,-10.8080928568386,-10.7023729905574,
-10.6880376043724,-10.5637109947364,-10.440558501415,-10.3759343476562),
 .UNSPECIFIED.) ;
#1344 = B_SPLINE_CURVE_WITH_KNOTS('',3,(#99936,#99937,#99938,#99939,#99940,
#99941,#99942,#99943,#99944,#99945,#99946,#99947,#99948,#99949,#99950,#99951,
#99952,#99953,#99954,#99955,#99956,#99957,#99958,#99959,#99960,#99961,#99962,
#99963,#99964,#99965,#99966,#99967,#99968,#99969,#99970,#99971,#99972,#99973,
#99974,#99975,#99976,#99977,#99978,#99979,#99980,#99981,#99982,#99983,#99984,
#99985,#99986,#99987,#99988,#99989,#99990,#99991,#99992,#99993,#99994,#99995,
#99996,#99997,#99998,#99999,#100000,#100001,#100002,#100003,#100004,#100005,
#100006,#100007,#100008,#100009,#100010,#100011,#100012,#100013,#100014,
#100015,#100016,#100017,#100018,#100019,#100020,#100021,#100022,#100023,
#100024,#100025,#100026,#100027,#100028,#100029,#100030,#100031,#100032,
#100033,#100034,#100035,#100036,#100037,#100038,#100039,#100040,#100041,
#100042,#100043,#100044,#100045,#100046,#100047,#100048,#100049,#100050,
#100051,#100052,#100053,#100054,#100055,#100056,#100057,#100058,#100059,
#100060,#100061,#100062,#100063,#100064,#100065,#100066,#100067,#100068,
#100069,#100070,#100071,#100072,#100073,#100074,#100075,#100076,#100077,
#100078,#100079,#100080,#100081,#100082,#100083,#100084,#100085,#100086,
#100087,#100088,#100089,#100090,#100091,#100092,#100093,#100094,#100095,
#100096,#100097,#100098,#100099,#100100,#100101,#100102,#100103,#100104,
#100105,#100106,#100107,#100108,#100109,#100110,#100111,#100112,#100113,
#100114,#100115,#100116,#100117,#100118,#100119,#100120,#100121,#100122,
#100123,#100124,#100125,#100126,#100127,#100128,#100129,#100130,#100131),
 .UNSPECIFIED.,.F.,.F.,(4,3,3,3,3,3,3,3,3,3,3,3,3,3,3,3,3,3,3,3,3,3,3,3,
3,3,3,3,3,3,3,3,3,3,3,3,3,3,3,3,3,3,3,3,3,3,3,3,3,3,3,3,3,3,3,3,3,3,3,3,
3,3,3,3,3,4),(-10.3759343473739,-10.2708182319272,-10.1657261816089,-10.0606224885171,
-9.95540605732621,-9.85012227155168,-9.7446668862292,-9.71639782215672,
-9.61067792538572,-9.50243793970514,-9.39698607994724,-9.291593725295,-9.18622549910132,
-9.07585863431126,-8.97036815335541,-8.86480970328484,-8.75908916785834,
-8.74475803994105,-8.6390379713579,-8.53079800715383,-8.42534592287132,
-8.31995332497796,-8.21458483739726,-8.10421819247929,-7.99872740836975,
-7.89316864110053,-7.7874477710884,-7.77311825772537,-7.66740649115993,
-7.55916548920365,-7.45372175043135,-7.348337490219,-7.24297731831515,-7.13260260761379,
-7.02711998672144,-6.92156932230534,-6.81585641345591,-6.8014784755097,
-6.6957468880536,-6.58750836370865,-6.48204496374827,-6.37664115733222,
-6.27126158683108,-6.16090586344681,-6.05540443841166,-5.9498351926574,
-5.84410414555403,-5.82983869329403,-5.72411618037325,-5.61587652171139,
-5.51042167490583,-5.40502620661422,-5.29965474740967,-5.18929078832684,
-5.08379682173855,-4.9782348034796,-4.87251061123387,-4.85819891107836,
-4.75396836036899,-4.64987198240714,-4.54587213384773,-4.44193130364946,
-4.33797515998441,-4.23400960594329,-4.12994645754084,-4.09274904045272),
 .UNSPECIFIED.) ;
#1345 = B_SPLINE_CURVE_WITH_KNOTS('',3,(#100133,#100134,#100135,#100136,#100137,
#100138,#100139,#100140,#100141,#100142,#100143,#100144,#100145,#100146,
#100147,#100148,#100149,#100150,#100151,#100152,#100153,#100154,#100155,
#100156,#100157,#100158,#100159,#100160,#100161,#100162,#100163,#100164,
#100165,#100166,#100167,#100168,#100169,#100170,#100171,#100172,#100173,
#100174,#100175,#100176,#100177,#100178,#100179,#100180,#100181,#100182,
#100183,#100184,#100185,#100186,#100187,#100188,#100189,#100190,#100191,
#100192,#100193),.UNSPECIFIED.,.F.,.F.,(4,3,3,3,3,3,3,3,3,3,3,3,3,3,3,3,
3,3,3,3,4),(-4.09274904019418,-3.94994229097354,-3.88655912886269,-3.7806981588848,
-3.67247580735508,-3.56688347781595,-3.46135127622131,-3.35584405875722,
-3.24561288072967,-3.13998714819308,-3.03429486644919,-2.92844341909598,
-2.91491934664702,-2.80976849252938,-2.7057785484878,-2.60187950128122,
-2.49803373370174,-2.39195342870279,-2.28805068804784,-2.18088160087689,
-2.07371251370594),.UNSPECIFIED.) ;
#1346 = B_SPLINE_CURVE_WITH_KNOTS('',3,(#100197,#100198,#100199,#100200,#100201),
 .UNSPECIFIED.,.F.,.F.,(4,1,4),(0.,0.971639782215675,1.12201628671505),
 .UNSPECIFIED.) ;
#1347 = B_SPLINE_CURVE_WITH_KNOTS('',3,(#100203,#100204,#100205,#100206,#100207,
#100208,#100209,#100210,#100211,#100212,#100213,#100214,#100215,#100216,
#100217,#100218,#100219,#100220,#100221,#100222,#100223,#100224,#100225,
#100226,#100227,#100228,#100229,#100230,#100231,#100232,#100233,#100234,
#100235,#100236,#100237,#100238,#100239,#100240,#100241,#100242,#100243,
#100244,#100245,#100246,#100247,#100248,#100249,#100250,#100251,#100252,
#100253,#100254,#100255,#100256,#100257,#100258,#100259,#100260,#100261,
#100262,#100263,#100264,#100265,#100266,#100267,#100268,#100269,#100270,
#100271,#100272,#100273,#100274,#100275,#100276,#100277,#100278,#100279,
#100280,#100281,#100282,#100283,#100284,#100285,#100286,#100287,#100288,
#100289,#100290,#100291,#100292,#100293,#100294,#100295,#100296,#100297,
#100298,#100299,#100300,#100301,#100302,#100303,#100304,#100305,#100306,
#100307,#100308,#100309,#100310,#100311,#100312,#100313,#100314,#100315,
#100316,#100317,#100318,#100319,#100320,#100321,#100322,#100323,#100324,
#100325,#100326,#100327,#100328,#100329,#100330,#100331,#100332,#100333,
#100334,#100335,#100336,#100337,#100338,#100339,#100340,#100341,#100342,
#100343,#100344,#100345,#100346,#100347,#100348,#100349,#100350,#100351,
#100352,#100353,#100354,#100355,#100356,#100357,#100358,#100359,#100360,
#100361,#100362,#100363,#100364,#100365,#100366,#100367,#100368,#100369,
#100370,#100371,#100372,#100373,#100374,#100375,#100376,#100377,#100378,
#100379,#100380,#100381,#100382,#100383,#100384,#100385,#100386,#100387,
#100388,#100389,#100390,#100391,#100392,#100393,#100394,#100395),
 .UNSPECIFIED.,.F.,.F.,(4,3,3,3,3,3,3,3,3,3,3,3,3,3,3,3,3,3,3,3,3,3,3,3,
3,3,3,3,3,3,3,3,3,3,3,3,3,3,3,3,3,3,3,3,3,3,3,3,3,3,3,3,3,3,3,3,3,3,3,3,
3,3,3,3,4),(1.12201628671505,1.22572984062012,1.3293396932848,1.43288383968884,
1.53640017806041,1.63999591211869,1.74362768694738,1.84744171560355,1.94327956443135,
2.04897598618115,2.15721890623938,2.2626389507752,2.3679965240157,2.4733270907322,
2.58372515471091,2.68917132531124,2.79468322907709,2.900354428491,2.91491934664702,
3.02076970287158,3.12899338112047,3.2345812937059,3.34011138403074,3.44561879250706,
3.55585387659597,3.66148554028109,3.76718573243698,3.87304781693433,3.8865591288627,
3.99221130516841,4.10045975590715,4.20584169368149,4.31116350983744,4.41646070071832,
4.52689525330833,4.6323142796995,4.73780119575579,4.84345058285624,4.85819891107837,
4.96392234279262,5.0721618866053,5.17761711523643,5.28301276573926,5.38838420783775,
5.49874782920182,5.60424128101974,5.70980261315803,5.81552588279539,5.82983869329404,
5.93556896205594,6.04380765123766,6.14927050221238,6.25467404579622,6.36005363919464,
6.47040984827341,6.57591200958229,6.68148223725401,6.78721460527208,6.80147847550972,
6.90810448169561,7.01457253381657,7.12090167820117,7.22714842106499,7.33336029947649,
7.40520159389472),.UNSPECIFIED.) ;
#1348 = B_SPLINE_CURVE_WITH_KNOTS('',3,(#100397,#100398,#100399,#100400,#100401,
#100402,#100403,#100404,#100405,#100406,#100407,#100408,#100409,#100410,
#100411,#100412,#100413,#100414,#100415,#100416,#100417,#100418,#100419,
#100420,#100421,#100422,#100423,#100424,#100425,#100426,#100427,#100428,
#100429,#100430,#100431,#100432,#100433,#100434,#100435,#100436,#100437,
#100438,#100439,#100440,#100441,#100442,#100443,#100444,#100445,#100446,
#100447,#100448,#100449,#100450,#100451,#100452,#100453,#100454,#100455,
#100456,#100457,#100458,#100459,#100460,#100461,#100462,#100463,#100464,
#100465,#100466,#100467,#100468,#100469,#100470,#100471,#100472,#100473,
#100474,#100475,#100476,#100477,#100478,#100479,#100480,#100481,#100482,
#100483,#100484,#100485,#100486,#100487,#100488,#100489,#100490,#100491,
#100492,#100493,#100494,#100495,#100496,#100497,#100498,#100499,#100500,
#100501,#100502,#100503,#100504,#100505,#100506,#100507,#100508,#100509,
#100510,#100511,#100512,#100513,#100514,#100515,#100516,#100517,#100518,
#100519,#100520,#100521,#100522,#100523,#100524,#100525,#100526,#100527,
#100528,#100529,#100530,#100531,#100532,#100533,#100534,#100535,#100536,
#100537,#100538,#100539,#100540,#100541,#100542,#100543,#100544,#100545,
#100546,#100547,#100548,#100549,#100550,#100551,#100552,#100553,#100554,
#100555,#100556,#100557,#100558,#100559,#100560,#100561,#100562,#100563,
#100564,#100565,#100566,#100567,#100568,#100569,#100570,#100571,#100572,
#100573,#100574,#100575,#100576,#100577,#100578,#100579,#100580,#100581,
#100582,#100583,#100584,#100585,#100586,#100587,#100588,#100589,#100590,
#100591,#100592),.UNSPECIFIED.,.F.,.F.,(4,3,3,3,3,3,3,3,3,3,3,3,3,3,3,3,
3,3,3,3,3,3,3,3,3,3,3,3,3,3,3,3,3,3,3,3,3,3,3,3,3,3,3,3,3,3,3,3,3,3,3,3,
3,3,3,3,3,3,3,3,3,3,3,3,3,4),(7.40520159423053,7.52274823355723,7.64076675914912,
7.75933359401983,7.77311825772539,7.87883837651618,7.98707833444429,8.09253043956017,
8.1979230473676,8.30329153395943,8.41365816045484,8.51914891635246,8.624707646037,
8.73042846552869,8.74475803994107,8.85047782504704,8.95871782468575,9.06416963794981,
9.16956197033504,9.27493019845273,9.38529710437873,9.49078764766358,9.59634618086029,
9.70206682811849,9.71639782215674,9.8221160929373,9.93035628186669,10.0358065051139,
10.1411972239824,10.2465638178459,10.3569322644775,10.4624211405789,10.5679779967512,
10.6736969647547,10.6880376043724,10.7937567221263,10.901996805184,11.0074479062241,
11.1128395117695,11.2182069996615,11.3285745963931,11.4340643744287,11.5396221344144,
11.6453420025645,11.6596773865881,11.7653963908742,11.8736364881154,11.9790874756325,
12.0844789679723,12.1898463431774,12.300214049584,12.4057037175975,12.5112613685939,
12.6169811299884,12.6313171688038,12.7370360762483,12.8452761855947,12.9507270700831,
13.0561184573942,13.1614857257493,13.2718535320668,13.3773430899027,13.4829006296713,
13.5886202791265,13.6029569510194,13.6883869010744),.UNSPECIFIED.) ;
#1349 = B_SPLINE_CURVE_WITH_KNOTS('',3,(#100594,#100595,#100596,#100597,#100598,
#100599,#100600,#100601,#100602,#100603,#100604,#100605,#100606,#100607,
#100608,#100609,#100610,#100611,#100612,#100613,#100614,#100615,#100616,
#100617,#100618,#100619,#100620,#100621,#100622,#100623,#100624,#100625,
#100626,#100627,#100628,#100629,#100630,#100631,#100632,#100633,#100634,
#100635,#100636,#100637,#100638,#100639,#100640,#100641,#100642,#100643,
#100644,#100645,#100646,#100647,#100648,#100649,#100650,#100651,#100652,
#100653,#100654,#100655,#100656,#100657,#100658,#100659,#100660,#100661,
#100662,#100663,#100664,#100665,#100666,#100667,#100668,#100669,#100670,
#100671,#100672,#100673,#100674,#100675,#100676,#100677,#100678,#100679,
#100680,#100681,#100682,#100683,#100684,#100685,#100686,#100687,#100688,
#100689,#100690,#100691,#100692,#100693,#100694,#100695,#100696,#100697,
#100698,#100699,#100700,#100701,#100702,#100703,#100704,#100705,#100706,
#100707,#100708,#100709,#100710,#100711,#100712,#100713,#100714,#100715,
#100716,#100717,#100718,#100719,#100720,#100721,#100722,#100723,#100724,
#100725,#100726,#100727,#100728,#100729,#100730,#100731,#100732,#100733,
#100734,#100735,#100736,#100737,#100738,#100739,#100740,#100741,#100742,
#100743,#100744,#100745,#100746,#100747,#100748,#100749,#100750,#100751,
#100752,#100753,#100754,#100755,#100756,#100757,#100758,#100759,#100760,
#100761,#100762,#100763,#100764,#100765,#100766,#100767,#100768,#100769,
#100770,#100771,#100772,#100773,#100774,#100775,#100776,#100777,#100778,
#100779,#100780,#100781,#100782,#100783,#100784,#100785,#100786),
 .UNSPECIFIED.,.F.,.F.,(4,3,3,3,3,3,3,3,3,3,3,3,3,3,3,3,3,3,3,3,3,3,3,3,
3,3,3,3,3,3,3,3,3,3,3,3,3,3,3,3,3,3,3,3,3,3,3,3,3,3,3,3,3,3,3,3,3,3,3,3,
3,3,3,3,4),(13.6883869014632,13.7928966428815,13.8972545308479,14.001529543701,
14.1057588206298,14.2099794369136,14.314293022429,14.4186584614246,14.5231928822222,
14.5745967332351,14.6803157463967,14.7885558425284,14.8940068337404,14.9993983278492,
15.1047657029,15.2151334060377,15.3206230690952,15.4261807134823,15.5319004659856,
15.5462365154508,15.6519556350861,15.7601957179086,15.865646819732,15.9710384256524,
16.0764059135115,16.1867735095503,16.2922632865352,16.3978210451198,16.5035409113853,
16.5178762976665,16.6235945194864,16.7318347145359,16.8372849174012,16.9426756265115,
17.0480422212251,17.1584106858893,17.2638995893294,17.3694564819601,17.4751754990101,
17.4895160798821,17.5952359766356,17.7034759623184,17.8089278220601,17.9143201766965,
18.019688402875,18.1300552676807,18.2355457486229,18.3411041986802,18.4468247340942,
18.4611558620978,18.5668759305656,18.6751158947841,18.7805679789512,18.8859605767293,
18.9913290641955,19.101695709225,19.2071864932224,19.3127452603802,19.4184661302833,
19.4327956443135,19.5414241997911,19.6498165890499,19.7580693322231,19.8661877984924,
19.9715722082541),.UNSPECIFIED.) ;
#1350 = B_SPLINE_CURVE_WITH_KNOTS('',3,(#100788,#100789,#100790,#100791,#100792,
#100793,#100794,#100795,#100796,#100797,#100798,#100799,#100800,#100801,
#100802,#100803,#100804,#100805,#100806,#100807,#100808,#100809,#100810,
#100811,#100812,#100813,#100814,#100815,#100816,#100817,#100818,#100819,
#100820,#100821,#100822,#100823,#100824,#100825,#100826,#100827,#100828,
#100829,#100830,#100831,#100832,#100833,#100834,#100835,#100836,#100837,
#100838,#100839,#100840,#100841,#100842,#100843,#100844,#100845,#100846,
#100847,#100848,#100849,#100850,#100851,#100852,#100853,#100854,#100855,
#100856,#100857,#100858,#100859,#100860,#100861,#100862,#100863,#100864,
#100865,#100866,#100867,#100868,#100869,#100870,#100871,#100872,#100873,
#100874,#100875,#100876,#100877,#100878,#100879,#100880,#100881,#100882,
#100883,#100884,#100885,#100886,#100887,#100888,#100889,#100890,#100891,
#100892,#100893,#100894,#100895,#100896,#100897,#100898,#100899,#100900,
#100901,#100902,#100903,#100904,#100905,#100906,#100907,#100908,#100909,
#100910,#100911,#100912,#100913,#100914,#100915,#100916,#100917,#100918,
#100919,#100920,#100921,#100922,#100923,#100924,#100925,#100926,#100927,
#100928,#100929,#100930,#100931,#100932,#100933,#100934,#100935,#100936,
#100937,#100938,#100939,#100940,#100941,#100942,#100943,#100944),
 .UNSPECIFIED.,.F.,.F.,(4,3,3,3,3,3,3,3,3,3,3,3,3,3,3,3,3,3,3,3,3,3,3,3,
3,3,3,3,3,3,3,3,3,3,3,3,3,3,3,3,3,3,3,3,3,3,3,3,3,3,3,3,4),(19.971572208661,
20.0845648157855,20.1977995689991,20.3114399446563,20.4044354265292,20.510167013901,
20.6184055382565,20.7238689381274,20.8292727444523,20.9346523148608,21.0450080383318,
21.1505094632704,21.2560787089269,21.361809755931,21.3760752087448,21.4817977206012,
21.5900373793961,21.6954922251061,21.8008876922933,21.9062591503856,22.0166231105293,
22.1221170759983,22.2276790931361,22.3334032842653,22.3477149909605,22.4533638124416,
22.5616126825334,22.666993223323,22.7723143699649,22.8776116177223,22.9880474065858,
23.0934683050467,23.1989577176671,23.304610464124,23.3193547731762,23.4252157407445,
23.5334380925754,23.6390304199759,23.7445626195405,23.850069835088,23.9603010151639,
24.0659267460978,24.1716190263506,24.2774704723827,24.2909945553918,24.3962128895577,
24.5002027571533,24.6041017693643,24.7079475432931,24.8141459646495,24.9180489703703,
25.0253950995445,25.1327412287187),.UNSPECIFIED.) ;
#1351 = B_SPLINE_CURVE_WITH_KNOTS('',3,(#100945,#100946,#100947,#100948),
 .UNSPECIFIED.,.F.,.F.,(4,4),(-0.0366228796273741,0.),.UNSPECIFIED.) ;
#1352 = B_SPLINE_CURVE_WITH_KNOTS('',3,(#100953,#100954,#100955,#100956,#100957,
#100958,#100959,#100960,#100961,#100962,#100963,#100964,#100965,#100966,
#100967,#100968,#100969,#100970,#100971,#100972,#100973,#100974,#100975,
#100976,#100977,#100978,#100979,#100980,#100981,#100982,#100983,#100984,
#100985,#100986,#100987,#100988,#100989,#100990,#100991,#100992,#100993,
#100994,#100995,#100996,#100997,#100998,#100999,#101000,#101001,#101002,
#101003,#101004,#101005,#101006,#101007,#101008,#101009,#101010,#101011,
#101012,#101013,#101014,#101015,#101016,#101017,#101018,#101019,#101020,
#101021,#101022,#101023,#101024,#101025,#101026,#101027,#101028,#101029,
#101030,#101031,#101032,#101033,#101034,#101035,#101036,#101037,#101038,
#101039,#101040,#101041,#101042,#101043,#101044,#101045,#101046,#101047,
#101048),.UNSPECIFIED.,.F.,.F.,(4,2,2,2,2,2,2,2,2,2,2,2,2,2,2,2,2,2,2,2,
2,2,2,2,2,2,2,2,2,2,2,2,2,2,2,2,2,2,2,2,2,2,2,2,2,2,2,4),(0.0026092829850963,
0.0203081228422541,0.0467104773415106,0.0573073440081075,0.0658992178962575,
0.0767494629243784,0.108072536354288,0.132854431634225,0.139607191542061,
0.144557005284787,0.151706565335001,0.183970979646304,0.209620746036483,
0.219934792552778,0.228507886012935,0.239406533000283,0.269303262627802,
0.287812881356171,0.296028645927189,0.302778346521195,0.30767737886147,
0.314632811108762,0.342639844609213,0.372509459836443,0.382881754334163,
0.391370675190917,0.402148795054376,0.42566704672463,0.456307544582424,
0.464617915238406,0.469625184685304,0.475508964095064,0.487990162648659,
0.515911946016534,0.531105983501541,0.543483252563705,0.552143259439136,
0.561701492758515,0.580973981377501,0.61508504263462,0.62302251830787,0.62960410971002,
0.634510358801496,0.641664597586085,0.661399903408521,0.686602160681216,
0.703168776920759,0.71239184097541),.UNSPECIFIED.) ;
#1353 = B_SPLINE_CURVE_WITH_KNOTS('',3,(#101052,#101053,#101054,#101055,#101056,
#101057,#101058,#101059,#101060,#101061,#101062,#101063,#101064,#101065,
#101066,#101067,#101068,#101069,#101070,#101071,#101072,#101073,#101074,
#101075,#101076,#101077,#101078,#101079),.UNSPECIFIED.,.F.,.F.,(4,3,3,3,
3,3,3,3,3,4),(34.5575191899869,34.6694625957267,34.7811806864541,34.8927675157327,
35.0042581797606,35.1156876439035,35.2271277908985,35.3385701031107,35.4501056657722,
35.508675576093),.UNSPECIFIED.) ;
#1354 = B_SPLINE_CURVE_WITH_KNOTS('',3,(#101080,#101081,#101082,#101083,#101084,
#101085,#101086,#101087,#101088,#101089,#101090,#101091,#101092,#101093,
#101094,#101095,#101096,#101097,#101098,#101099,#101100,#101101,#101102,
#101103,#101104,#101105,#101106,#101107,#101108,#101109,#101110,#101111,
#101112,#101113,#101114,#101115,#101116,#101117,#101118,#101119,#101120,
#101121,#101122,#101123,#101124,#101125,#101126,#101127,#101128,#101129,
#101130,#101131,#101132,#101133,#101134,#101135,#101136,#101137,#101138,
#101139,#101140),.UNSPECIFIED.,.F.,.F.,(4,3,3,3,3,3,3,3,3,3,3,3,3,3,3,3,
3,3,3,3,4),(32.5109076064973,32.5937562294461,32.7036643904514,32.8133952660067,
32.9230275064331,33.0326010843926,33.1421558910857,33.2518087048573,33.3615084504932,
33.4714088639723,33.5653960116618,33.6747987943945,33.7840191138006,33.8931380204768,
34.0021964233412,34.111235146482,34.2203746515072,34.3295618237526,34.4389574443397,
34.5370357938774,34.5575191894876),.UNSPECIFIED.) ;
#1355 = B_SPLINE_CURVE_WITH_KNOTS('',3,(#101142,#101143,#101144,#101145,#101146,
#101147,#101148,#101149,#101150,#101151,#101152,#101153,#101154,#101155,
#101156,#101157,#101158,#101159,#101160,#101161,#101162,#101163,#101164,
#101165,#101166,#101167,#101168,#101169,#101170,#101171,#101172,#101173,
#101174,#101175,#101176,#101177,#101178,#101179,#101180,#101181,#101182,
#101183,#101184,#101185,#101186,#101187,#101188,#101189,#101190,#101191,
#101192,#101193,#101194,#101195,#101196,#101197,#101198,#101199,#101200,
#101201,#101202,#101203,#101204,#101205,#101206,#101207,#101208,#101209,
#101210,#101211,#101212,#101213,#101214,#101215,#101216,#101217,#101218,
#101219,#101220,#101221,#101222,#101223,#101224,#101225,#101226),
 .UNSPECIFIED.,.F.,.F.,(4,3,3,3,3,3,3,3,3,3,3,3,3,3,3,3,3,3,3,3,3,3,3,3,
3,3,3,3,4),(-0.37524009580756,-0.357518921288721,-0.353499339011914,-0.330618426268463,
-0.324807985426275,-0.303154818283502,-0.286565543774214,-0.2802937315987,
-0.274975128510897,-0.253676729885043,-0.232669298257941,-0.217166169990548,
-0.20837475042749,-0.204726014152323,-0.184286055371377,-0.17045203706431,
-0.149652213060313,-0.139823936654317,-0.135833669251288,-0.132392599709375,
-0.112098960320059,-0.0918017548146832,-0.0716539883511498,-0.067625436545846,
-0.0641202926150906,-0.0443089210862901,-0.0250693388973895,-0.00603116485857798,
-1.6124231245987E-14),.UNSPECIFIED.) ;
#1356 = B_SPLINE_CURVE_WITH_KNOTS('',3,(#101228,#101229,#101230,#101231),
 .UNSPECIFIED.,.F.,.F.,(4,4),(0.,0.0129523452064985),.UNSPECIFIED.) ;
#1357 = B_SPLINE_CURVE_WITH_KNOTS('',3,(#101232,#101233,#101234,#101235,#101236,
#101237,#101238,#101239,#101240,#101241,#101242,#101243,#101244,#101245,
#101246,#101247,#101248,#101249,#101250,#101251,#101252,#101253,#101254,
#101255,#101256,#101257,#101258,#101259,#101260,#101261,#101262,#101263,
#101264,#101265,#101266,#101267,#101268,#101269,#101270,#101271,#101272,
#101273,#101274,#101275,#101276,#101277,#101278,#101279,#101280,#101281,
#101282,#101283,#101284,#101285,#101286,#101287,#101288,#101289,#101290,
#101291,#101292,#101293,#101294,#101295,#101296,#101297,#101298,#101299,
#101300,#101301,#101302,#101303,#101304,#101305,#101306,#101307,#101308,
#101309,#101310,#101311,#101312,#101313,#101314,#101315,#101316,#101317,
#101318,#101319),.UNSPECIFIED.,.F.,.F.,(4,3,3,3,3,3,3,3,3,3,3,3,3,3,3,3,
3,3,3,3,3,3,3,3,3,3,3,3,3,4),(-0.38016989466375,-0.360311058062006,-0.358093714841499,
-0.34471487570795,-0.336915355012495,-0.332696989994484,-0.312888599506859,
-0.296964105449495,-0.291611990627701,-0.287054657778508,-0.266573287948675,
-0.246125188667504,-0.230967053262615,-0.222333883223211,-0.217980615396263,
-0.196924263842872,-0.185492647047948,-0.16498333041885,-0.154671872267672,
-0.149608894129304,-0.146454177730597,-0.125463903654776,-0.103990194256974,
-0.0825564409435494,-0.0772771397702884,-0.0730031458537735,-0.0510763331729567,
-0.0292998033466994,-0.007759983282897,0.),.UNSPECIFIED.) ;
#1358 = B_SPLINE_CURVE_WITH_KNOTS('',3,(#101445,#101446,#101447,#101448,#101449,
#101450,#101451,#101452,#101453,#101454,#101455,#101456,#101457,#101458,
#101459,#101460,#101461,#101462,#101463,#101464,#101465,#101466,#101467,
#101468,#101469,#101470,#101471,#101472,#101473,#101474,#101475,#101476,
#101477,#101478,#101479,#101480,#101481,#101482,#101483,#101484,#101485,
#101486,#101487,#101488,#101489,#101490,#101491,#101492,#101493,#101494,
#101495,#101496,#101497,#101498,#101499,#101500,#101501,#101502,#101503,
#101504,#101505,#101506,#101507,#101508,#101509,#101510,#101511,#101512,
#101513,#101514,#101515,#101516,#101517,#101518,#101519,#101520,#101521,
#101522,#101523,#101524,#101525,#101526,#101527,#101528,#101529),
 .UNSPECIFIED.,.F.,.F.,(4,3,3,3,3,3,3,3,3,3,3,3,3,3,3,3,3,3,3,3,3,3,3,3,
3,3,3,3,4),(0.,0.0198999736214445,0.022033478855472,0.0414468202729217,
0.0603279893210927,0.0659853869923778,0.0696582620916686,0.0895889830255989,
0.110292888835956,0.130996794646314,0.134529829243006,0.138089195898059,
0.158922736380717,0.179545457140466,0.194222826116571,0.203107891092953,
0.207554446770544,0.227794854702371,0.248829911754691,0.265094672958623,
0.273893002460397,0.277903852040319,0.299536877312563,0.319299235095571,
0.325159379351979,0.330782663134293,0.352647695498619,0.37432272203279,
0.378914100184376),.UNSPECIFIED.) ;
#1359 = B_SPLINE_CURVE_WITH_KNOTS('',3,(#101530,#101531,#101532,#101533),
 .UNSPECIFIED.,.F.,.F.,(4,4),(-0.0129525315802166,0.),.UNSPECIFIED.) ;
#1360 = B_SPLINE_CURVE_WITH_KNOTS('',3,(#101658,#101659,#101660,#101661,#101662,
#101663,#101664,#101665,#101666,#101667,#101668,#101669,#101670,#101671,
#101672,#101673,#101674,#101675,#101676,#101677,#101678,#101679,#101680,
#101681,#101682,#101683,#101684,#101685,#101686,#101687,#101688,#101689,
#101690,#101691,#101692,#101693,#101694,#101695,#101696,#101697,#101698,
#101699,#101700,#101701,#101702,#101703,#101704,#101705,#101706,#101707,
#101708,#101709,#101710,#101711,#101712,#101713,#101714,#101715,#101716,
#101717,#101718,#101719,#101720,#101721,#101722,#101723,#101724,#101725,
#101726,#101727,#101728,#101729,#101730,#101731,#101732,#101733,#101734,
#101735,#101736,#101737,#101738,#101739,#101740,#101741,#101742),
 .UNSPECIFIED.,.F.,.F.,(4,3,3,3,3,3,3,3,3,3,3,3,3,3,3,3,3,3,3,3,3,3,3,3,
3,3,3,3,4),(0.,0.0215677198000641,0.0255184714855182,0.0472519117233337,
0.0675132036694678,0.0732612703991268,0.077959247140824,0.0994876515331383,
0.120942349766413,0.143042324147911,0.147548760546303,0.151258390489377,
0.172167334932419,0.192451590106119,0.209342247292407,0.217998538466851,
0.222762834145278,0.243196176321172,0.263823362943062,0.278366679408141,
0.287113906024107,0.292333781104599,0.312535580645166,0.329444159149797,
0.335387151529194,0.339362863956405,0.35904267418776,0.378722484419115,
0.380169894663675),.UNSPECIFIED.) ;
#1361 = B_SPLINE_CURVE_WITH_KNOTS('',3,(#101754,#101755,#101756,#101757,#101758,
#101759,#101760,#101761,#101762,#101763,#101764,#101765,#101766,#101767,
#101768,#101769),.UNSPECIFIED.,.T.,.F.,(4,1,1,1,1,1,1,1,1,1,1,1,1,4),(-1.37470975898194,
-1.17832265055595,-0.981935542129957,-0.785548433703966,-0.589161325277974,
-0.392774216851983,-0.196387108425991,0.,0.196387108425991,0.589161325277974,
0.785548433703966,0.981935542129957,1.17832265055595,1.37470975898194),
 .UNSPECIFIED.) ;
#1362 = B_SPLINE_CURVE_WITH_KNOTS('',3,(#101778,#101779,#101780,#101781,#101782,
#101783,#101784,#101785,#101786,#101787,#101788,#101789,#101790,#101791,
#101792,#101793),.UNSPECIFIED.,.T.,.F.,(4,1,1,1,1,1,1,1,1,1,1,1,1,4),(-1.37470975898194,
-1.17832265055595,-0.981935542129957,-0.785548433703966,-0.589161325277974,
-0.392774216851983,-0.196387108425991,0.,0.196387108425991,0.589161325277974,
0.785548433703966,0.981935542129957,1.17832265055595,1.37470975898194),
 .UNSPECIFIED.) ;
#1363 = B_SPLINE_CURVE_WITH_KNOTS('',3,(#101881,#101882,#101883,#101884,#101885),
 .UNSPECIFIED.,.F.,.F.,(4,1,4),(-1.,-0.5,0.),.UNSPECIFIED.) ;
#1364 = B_SPLINE_CURVE_WITH_KNOTS('',3,(#101887,#101888,#101889,#101890,#101891,
#101892,#101893),.UNSPECIFIED.,.F.,.F.,(4,1,1,1,4),(-1.37470975898194,-1.17832265055595,
-0.981935542129957,-0.785548433703966,-0.68713324456091),.UNSPECIFIED.) ;
#1365 = B_SPLINE_CURVE_WITH_KNOTS('',3,(#101894,#101895,#101896,#101897,#101898,
#101899,#101900,#101901,#101902,#101903,#101904,#101905,#101906),
 .UNSPECIFIED.,.F.,.F.,(4,1,1,1,1,1,1,1,1,1,4),(-0.68713324456091,-0.589161325277974,
-0.196387108425991,0.,0.196387108425991,0.392774216851983,0.589161325277974,
0.785548433703966,0.981935542129957,1.17832265055595,1.37470975898194),
 .UNSPECIFIED.) ;
#1366 = B_SPLINE_CURVE_WITH_KNOTS('',3,(#101988,#101989,#101990,#101991,#101992),
 .UNSPECIFIED.,.F.,.F.,(4,1,4),(-1.,-0.5,0.),.UNSPECIFIED.) ;
#1367 = B_SPLINE_CURVE_WITH_KNOTS('',3,(#101994,#101995,#101996,#101997,#101998,
#101999,#102000),.UNSPECIFIED.,.F.,.F.,(4,1,1,1,4),(-1.37470975898194,-1.17832265055595,
-0.981935542129957,-0.785548433703966,-0.687210817221056),.UNSPECIFIED.) ;
#1368 = B_SPLINE_CURVE_WITH_KNOTS('',3,(#102001,#102002,#102003,#102004,#102005,
#102006,#102007,#102008,#102009,#102010,#102011,#102012,#102013),
 .UNSPECIFIED.,.F.,.F.,(4,1,1,1,1,1,1,1,1,1,4),(-0.687210817221056,-0.589161325277974,
-0.196387108425991,0.,0.196387108425991,0.392774216851983,0.589161325277974,
0.785548433703966,0.981935542129957,1.17832265055595,1.37470975898194),
 .UNSPECIFIED.) ;
#1369 = B_SPLINE_CURVE_WITH_KNOTS('',3,(#102019,#102020,#102021,#102022,#102023,
#102024,#102025,#102026,#102027,#102028,#102029,#102030,#102031,#102032),
 .UNSPECIFIED.,.F.,.F.,(4,2,2,2,2,2,4),(-0.0559250143496373,-0.0556883945460747,
-0.0495906031992305,-0.0437546843030053,-0.0372885759081072,-0.0322854917709823,
-0.0278441972730634),.UNSPECIFIED.) ;
#1370 = B_SPLINE_CURVE_WITH_KNOTS('',3,(#102035,#102036,#102037,#102038,#102039,
#102040,#102041,#102042,#102043,#102044,#102045,#102046,#102047,#102048),
 .UNSPECIFIED.,.F.,.F.,(4,2,2,2,2,2,4),(-0.000236619804093,0.,0.0060977913471935,
0.0119337102438738,0.018399818639261,0.0234029027767472,0.0278441972749678),
 .UNSPECIFIED.) ;
#1371 = B_SPLINE_CURVE_WITH_KNOTS('',3,(#102053,#102054,#102055,#102056,#102057,
#102058,#102059,#102060,#102061,#102062,#102063,#102064,#102065,#102066,
#102067,#102068),.UNSPECIFIED.,.F.,.F.,(4,3,3,3,3,4),(-0.000437598556087367,
0.,0.00562170475705654,0.0114823251607832,0.0173413775084489,0.0231997078489075),
 .UNSPECIFIED.) ;
#1372 = B_SPLINE_CURVE_WITH_KNOTS('',3,(#102074,#102075,#102076,#102077,#102078,
#102079,#102080,#102081,#102082,#102083,#102084,#102085,#102086,#102087,
#102088,#102089),.UNSPECIFIED.,.F.,.F.,(4,3,3,3,3,4),(-0.046837014255361,
-0.046399415699481,-0.0407777109422933,-0.0349170905383532,-0.0290580381904547,
-0.0231997078497599),.UNSPECIFIED.) ;
#1373 = B_SPLINE_CURVE_WITH_KNOTS('',3,(#102095,#102096,#102097,#102098,#102099,
#102100,#102101,#102102,#102103,#102104,#102105,#102106,#102107,#102108),
 .UNSPECIFIED.,.F.,.F.,(4,2,2,2,2,2,4),(-0.000236619803146698,0.,0.00609779134724104,
0.0119337102438844,0.0183998186389394,0.0234029027761802,0.0278441972742087),
 .UNSPECIFIED.) ;
#1374 = B_SPLINE_CURVE_WITH_KNOTS('',3,(#102114,#102115,#102116,#102117,#102118,
#102119,#102120,#102121,#102122,#102123,#102124,#102125,#102126,#102127),
 .UNSPECIFIED.,.F.,.F.,(4,2,2,2,2,2,4),(-0.0559250143496986,-0.0556883945465552,
-0.0495906031994403,-0.0437546843028884,-0.0372885759079096,-0.0322854917707418,
-0.0278441972727803),.UNSPECIFIED.) ;
#1375 = B_SPLINE_CURVE_WITH_KNOTS('',3,(#102133,#102134,#102135,#102136,#102137,
#102138,#102139,#102140,#102141,#102142,#102143,#102144,#102145,#102146,
#102147,#102148),.UNSPECIFIED.,.F.,.F.,(4,3,3,3,3,4),(-0.000437598556095027,
0.,0.00562170475708189,0.0114823251608833,0.0173413775086171,0.0231997078491342),
 .UNSPECIFIED.) ;
#1376 = B_SPLINE_CURVE_WITH_KNOTS('',3,(#102154,#102155,#102156,#102157,#102158,
#102159,#102160,#102161,#102162,#102163,#102164,#102165,#102166,#102167,
#102168,#102169),.UNSPECIFIED.,.F.,.F.,(4,3,3,3,3,4),(-0.0468370142541051,
-0.0463994156980201,-0.0407777109409428,-0.0349170905371886,-0.0290580381894966,
-0.0231997078490079),.UNSPECIFIED.) ;
#1377 = B_SPLINE_CURVE_WITH_KNOTS('',3,(#102175,#102176,#102177,#102178,#102179,
#102180,#102181,#102182,#102183,#102184,#102185,#102186,#102187,#102188),
 .UNSPECIFIED.,.F.,.F.,(4,2,2,2,2,2,4),(-0.000236619803558265,0.,0.00609779134685418,
0.0119337102431074,0.0183998186379772,0.023402902775095,0.0278441972730209),
 .UNSPECIFIED.) ;
#1378 = B_SPLINE_CURVE_WITH_KNOTS('',3,(#102194,#102195,#102196,#102197,#102198,
#102199,#102200,#102201,#102202,#102203,#102204,#102205,#102206,#102207),
 .UNSPECIFIED.,.F.,.F.,(4,2,2,2,2,2,4),(-0.0559250143504567,-0.0556883945473107,
-0.0495906032000867,-0.0437546843034773,-0.0372885759084374,-0.0322854917711889,
-0.0278441972731474),.UNSPECIFIED.) ;
#1379 = B_SPLINE_CURVE_WITH_KNOTS('',3,(#102213,#102214,#102215,#102216,#102217,
#102218,#102219,#102220,#102221,#102222,#102223,#102224,#102225,#102226,
#102227,#102228),.UNSPECIFIED.,.F.,.F.,(4,3,3,3,3,4),(-0.000437598556114517,
0.,0.00562170475723958,0.0114823251612343,0.0173413775091901,0.0231997078499022),
 .UNSPECIFIED.) ;
#1380 = B_SPLINE_CURVE_WITH_KNOTS('',3,(#102234,#102235,#102236,#102237,#102238,
#102239,#102240,#102241,#102242,#102243,#102244,#102245,#102246,#102247,
#102248,#102249),.UNSPECIFIED.,.F.,.F.,(4,3,3,3,3,4),(-0.0468370142516818,
-0.046399415695612,-0.0407777109388244,-0.034917090535398,-0.0290580381880315,
-0.0231997078478665),.UNSPECIFIED.) ;
#1381 = B_SPLINE_CURVE_WITH_KNOTS('',3,(#102255,#102256,#102257,#102258,#102259,
#102260,#102261,#102262,#102263,#102264,#102265,#102266,#102267,#102268),
 .UNSPECIFIED.,.F.,.F.,(4,2,2,2,2,2,4),(-0.000236619803559768,0.,0.00609779134686269,
0.0119337102430971,0.0183998186379832,0.0234029027750867,0.0278441972729811),
 .UNSPECIFIED.) ;
#1382 = B_SPLINE_CURVE_WITH_KNOTS('',3,(#102274,#102275,#102276,#102277,#102278,
#102279,#102280,#102281,#102282,#102283,#102284,#102285,#102286,#102287),
 .UNSPECIFIED.,.F.,.F.,(4,2,2,2,2,2,4),(-0.0559250143524368,-0.0556883945478243,
-0.0495906032010392,-0.0437546843047665,-0.0372885759096309,-0.0322854917723447,
-0.0278441972742818),.UNSPECIFIED.) ;
#1383 = B_SPLINE_CURVE_WITH_KNOTS('',3,(#102293,#102294,#102295,#102296,#102297,
#102298,#102299,#102300,#102301,#102302,#102303,#102304,#102305,#102306,
#102307,#102308),.UNSPECIFIED.,.F.,.F.,(4,3,3,3,3,4),(-0.000437598556131605,
0.,0.00562170475733242,0.0114823251614144,0.0173413775094361,0.0231997078502398),
 .UNSPECIFIED.) ;
#1384 = B_SPLINE_CURVE_WITH_KNOTS('',3,(#102314,#102315,#102316,#102317,#102318,
#102319,#102320,#102321,#102322,#102323,#102324,#102325,#102326,#102327,
#102328,#102329),.UNSPECIFIED.,.F.,.F.,(4,3,3,3,3,4),(-0.0468370142582233,
-0.0463994157019922,-0.0407777109444557,-0.0349170905401249,-0.0290580381918459,
-0.0231997078507989),.UNSPECIFIED.) ;
#1385 = B_SPLINE_CURVE_WITH_KNOTS('',3,(#102335,#102336,#102337,#102338,#102339,
#102340,#102341,#102342,#102343,#102344,#102345,#102346,#102347,#102348),
 .UNSPECIFIED.,.F.,.F.,(4,2,2,2,2,2,4),(-0.000236619803154501,0.,0.00609779134749395,
0.0119337102444787,0.0183998186399401,0.0234029027774939,0.0278441972757804),
 .UNSPECIFIED.) ;
#1386 = B_SPLINE_CURVE_WITH_KNOTS('',3,(#102354,#102355,#102356,#102357,#102358,
#102359,#102360,#102361,#102362,#102363,#102364,#102365,#102366,#102367),
 .UNSPECIFIED.,.F.,.F.,(4,2,2,2,2,2,4),(-0.0559250143516698,-0.055688394548102,
-0.0495906032010132,-0.0437546843045191,-0.0372885759093257,-0.0322854917720022,
-0.0278441972739074),.UNSPECIFIED.) ;
#1387 = B_SPLINE_CURVE_WITH_KNOTS('',3,(#102373,#102374,#102375,#102376,#102377,
#102378,#102379,#102380,#102381,#102382,#102383,#102384,#102385,#102386,
#102387,#102388),.UNSPECIFIED.,.F.,.F.,(4,3,3,3,3,4),(-0.000437598556150276,
0.,0.00562170475744494,0.0114823251616921,0.0173413775098778,0.0231997078508276),
 .UNSPECIFIED.) ;
#1388 = B_SPLINE_CURVE_WITH_KNOTS('',3,(#102394,#102395,#102396,#102397,#102398,
#102399,#102400,#102401,#102402,#102403,#102404,#102405,#102406,#102407,
#102408,#102409),.UNSPECIFIED.,.F.,.F.,(4,3,3,3,3,4),(-0.0468370142569828,
-0.0463994157014635,-0.0407777109440522,-0.0349170905398014,-0.0290580381915951,
-0.0231997078506218),.UNSPECIFIED.) ;
#1389 = B_SPLINE_CURVE_WITH_KNOTS('',3,(#102415,#102416,#102417,#102418,#102419,
#102420,#102421,#102422,#102423,#102424,#102425,#102426,#102427,#102428),
 .UNSPECIFIED.,.F.,.F.,(4,2,2,2,2,2,4),(-0.000236619804616541,0.,0.00609779134700319,
0.0119337102434886,0.0183998186388943,0.0234029027763847,0.0278441972746185),
 .UNSPECIFIED.) ;
#1390 = B_SPLINE_CURVE_WITH_KNOTS('',3,(#102434,#102435,#102436,#102437,#102438,
#102439,#102440,#102441,#102442,#102443,#102444,#102445,#102446,#102447),
 .UNSPECIFIED.,.F.,.F.,(4,2,2,2,2,2,4),(-0.0559250143475551,-0.0556883945439973,
-0.049590603197355,-0.0437546843013896,-0.037288575906807,-0.0322854917699323,
-0.0278441972722247),.UNSPECIFIED.) ;
#1391 = B_SPLINE_CURVE_WITH_KNOTS('',3,(#102453,#102454,#102455,#102456,#102457,
#102458,#102459,#102460,#102461,#102462,#102463,#102464,#102465,#102466,
#102467,#102468),.UNSPECIFIED.,.F.,.F.,(4,3,3,3,3,4),(-0.000437598556056009,
0.,0.00562170475686937,0.0114823251603833,0.0173413775078316,0.0231997078480834),
 .UNSPECIFIED.) ;
#1392 = B_SPLINE_CURVE_WITH_KNOTS('',3,(#102474,#102475,#102476,#102477,#102478,
#102479,#102480,#102481,#102482,#102483,#102484,#102485,#102486,#102487,
#102488,#102489),.UNSPECIFIED.,.F.,.F.,(4,3,3,3,3,4),(-0.0468370142561097,
-0.0463994157004828,-0.0407777109431283,-0.034917090538975,-0.0290580381908889,
-0.0231997078500392),.UNSPECIFIED.) ;
#1393 = B_SPLINE_CURVE_WITH_KNOTS('',3,(#102495,#102496,#102497,#102498,#102499,
#102500,#102501,#102502,#102503,#102504,#102505,#102506,#102507,#102508),
 .UNSPECIFIED.,.F.,.F.,(4,2,2,2,2,2,4),(-0.000236619804206572,0.,0.00609779134739848,
0.0119337102443252,0.0183998186399927,0.023402902777706,0.0278441972760964),
 .UNSPECIFIED.) ;
#1394 = B_SPLINE_CURVE_WITH_KNOTS('',3,(#102514,#102515,#102516,#102517,#102518,
#102519,#102520,#102521,#102522,#102523,#102524,#102525,#102526,#102527),
 .UNSPECIFIED.,.F.,.F.,(4,2,2,2,2,2,4),(-0.0559250143503367,-0.0556883945467745,
-0.0495906031998185,-0.0437546843034772,-0.0372885759085197,-0.0322854917713411,
-0.0278441972733722),.UNSPECIFIED.) ;
#1395 = B_SPLINE_CURVE_WITH_KNOTS('',3,(#102533,#102534,#102535,#102536,#102537,
#102538,#102539,#102540,#102541,#102542,#102543,#102544,#102545,#102546,
#102547,#102548),.UNSPECIFIED.,.F.,.F.,(4,3,3,3,3,4),(-0.000437598556095159,
0.,0.00562170475710087,0.0114823251609001,0.0173413775086179,0.0231997078491324),
 .UNSPECIFIED.) ;
#1396 = B_SPLINE_CURVE_WITH_KNOTS('',3,(#102554,#102555,#102556,#102557,#102558,
#102559,#102560,#102561,#102562,#102563,#102564,#102565,#102566,#102567,
#102568,#102569),.UNSPECIFIED.,.F.,.F.,(4,3,3,3,3,4),(-0.0468370142542446,
-0.0463994156981747,-0.0407777109410807,-0.0349170905373078,-0.0290580381895938,
-0.0231997078490836),.UNSPECIFIED.) ;
#1397 = B_SPLINE_CURVE_WITH_KNOTS('',3,(#102575,#102576,#102577,#102578,#102579,
#102580,#102581,#102582,#102583,#102584,#102585,#102586,#102587,#102588),
 .UNSPECIFIED.,.F.,.F.,(4,2,2,2,2,2,4),(-0.000236619803563725,0.,0.00609779134693619,
0.0119337102432759,0.0183998186382373,0.0234029027754271,0.027844197273412),
 .UNSPECIFIED.) ;
#1398 = B_SPLINE_CURVE_WITH_KNOTS('',3,(#102594,#102595,#102596,#102597,#102598,
#102599,#102600,#102601,#102602,#102603,#102604,#102605,#102606,#102607),
 .UNSPECIFIED.,.F.,.F.,(4,2,2,2,2,2,4),(-0.0559250143564113,-0.0556883945522011,
-0.0495906032047249,-0.0437546843077159,-0.0372885759119513,-0.0322854917741759,
-0.0278441972757216),.UNSPECIFIED.) ;
#1399 = B_SPLINE_CURVE_WITH_KNOTS('',3,(#102613,#102614,#102615,#102616,#102617,
#102618,#102619,#102620,#102621,#102622,#102623,#102624,#102625,#102626,
#102627,#102628),.UNSPECIFIED.,.F.,.F.,(4,3,3,3,3,4),(-0.000437598556252948,
0.,0.00562170475756358,0.0114823251619473,0.0173413775102792,0.023199707851373),
 .UNSPECIFIED.) ;
#1400 = B_SPLINE_CURVE_WITH_KNOTS('',3,(#102634,#102635,#102636,#102637,#102638,
#102639,#102640,#102641,#102642,#102643,#102644,#102645,#102646,#102647,
#102648,#102649),.UNSPECIFIED.,.F.,.F.,(4,3,3,3,3,4),(-0.0468370142435449,
-0.0463994156880452,-0.0407777109322271,-0.0349170905298351,-0.0290580381834779,
-0.0231997078443083),.UNSPECIFIED.) ;
#1401 = B_SPLINE_CURVE_WITH_KNOTS('',3,(#102655,#102656,#102657,#102658,#102659,
#102660,#102661,#102662,#102663,#102664,#102665,#102666,#102667,#102668),
 .UNSPECIFIED.,.F.,.F.,(4,2,2,2,2,2,4),(-0.000236619803545348,0.,0.00609779134648851,
0.0119337102422953,0.0183998186366923,0.0234029027734222,0.0278441972710204),
 .UNSPECIFIED.) ;
#1402 = B_SPLINE_CURVE_WITH_KNOTS('',3,(#102674,#102675,#102676,#102677,#102678,
#102679,#102680,#102681,#102682,#102683,#102684,#102685,#102686,#102687),
 .UNSPECIFIED.,.F.,.F.,(4,2,2,2,2,2,4),(-0.0559250143495547,-0.0556883945459923,
-0.0495906031991245,-0.0437546843029074,-0.0372885759080479,-0.0322854917709575,
-0.027844197273083),.UNSPECIFIED.) ;
#1403 = B_SPLINE_CURVE_WITH_KNOTS('',3,(#102693,#102694,#102695,#102696,#102697,
#102698,#102699,#102700,#102701,#102702,#102703,#102704,#102705,#102706,
#102707,#102708),.UNSPECIFIED.,.F.,.F.,(4,3,3,3,3,4),(-0.000437598556080383,
0.,0.00562170475701161,0.0114823251606741,0.0173413775082905,0.0231997078487108),
 .UNSPECIFIED.) ;
#1404 = B_SPLINE_CURVE_WITH_KNOTS('',3,(#102714,#102715,#102716,#102717,#102718,
#102719,#102720,#102721,#102722,#102723,#102724,#102725,#102726,#102727,
#102728,#102729),.UNSPECIFIED.,.F.,.F.,(4,3,3,3,3,4),(-0.0468370142410635,
-0.046399415685515,-0.0407777109299654,-0.0349170905279156,-0.0290580381819153,
-0.0231997078430871),.UNSPECIFIED.) ;
#1405 = B_SPLINE_CURVE_WITH_KNOTS('',3,(#102735,#102736,#102737,#102738,#102739,
#102740,#102741,#102742,#102743,#102744,#102745,#102746,#102747,#102748),
 .UNSPECIFIED.,.F.,.F.,(4,2,2,2,2,2,4),(-0.000236619803553881,0.,0.00609779134648714,
0.0119337102422593,0.0183998186365944,0.0234029027733178,0.0278441972709114),
 .UNSPECIFIED.) ;
#1406 = B_SPLINE_CURVE_WITH_KNOTS('',3,(#102754,#102755,#102756,#102757,#102758,
#102759,#102760,#102761,#102762,#102763,#102764,#102765,#102766,#102767),
 .UNSPECIFIED.,.F.,.F.,(4,2,2,2,2,2,4),(-0.0559250143458346,-0.0556883945427038,
-0.0495906031960554,-0.043754684300065,-0.0372885759056522,-0.0322854917688908,
-0.0278441972712752),.UNSPECIFIED.) ;
#1407 = B_SPLINE_CURVE_WITH_KNOTS('',3,(#102773,#102774,#102775,#102776,#102777,
#102778,#102779,#102780,#102781,#102782,#102783,#102784,#102785,#102786,
#102787,#102788),.UNSPECIFIED.,.F.,.F.,(4,3,3,3,3,4),(-0.000437598556037642,
0.,0.00562170475676515,0.0114823251601515,0.0173413775075229,0.0231997078477011),
 .UNSPECIFIED.) ;
#1408 = B_SPLINE_CURVE_WITH_KNOTS('',3,(#102794,#102795,#102796,#102797,#102798,
#102799,#102800,#102801,#102802,#102803,#102804,#102805,#102806,#102807,
#102808,#102809),.UNSPECIFIED.,.F.,.F.,(4,3,3,3,3,4),(-0.0468370142550307,
-0.046399415699245,-0.0407777109420836,-0.0349170905381485,-0.0290580381902572,
-0.023199707849583),.UNSPECIFIED.) ;
#1409 = B_SPLINE_CURVE_WITH_KNOTS('',3,(#102815,#102816,#102817,#102818,#102819,
#102820,#102821,#102822,#102823,#102824,#102825,#102826,#102827,#102828),
 .UNSPECIFIED.,.F.,.F.,(4,2,2,2,2,2,4),(-0.000236619803565948,0.,0.00609779134700125,
0.0119337102434307,0.0183998186384978,0.0234029027757452,0.0278441972737845),
 .UNSPECIFIED.) ;
#1410 = B_SPLINE_CURVE_WITH_KNOTS('',3,(#102834,#102835,#102836,#102837,#102838,
#102839,#102840,#102841,#102842,#102843,#102844,#102845,#102846,#102847),
 .UNSPECIFIED.,.F.,.F.,(4,2,2,2,2,2,4),(-0.0559250143492506,-0.0556883945457476,
-0.049590603198939,-0.0437546843027145,-0.0372885759078682,-0.032285491770796,
-0.0278441972729179),.UNSPECIFIED.) ;
#1411 = B_SPLINE_CURVE_WITH_KNOTS('',3,(#102854,#102855,#102856,#102857,#102858,
#102859,#102860,#102861,#102862,#102863,#102864,#102865,#102866,#102867,
#102868,#102869),.UNSPECIFIED.,.F.,.F.,(4,3,3,3,3,4),(-0.000437598556107252,
0.,0.00562170475708925,0.0114823251608564,0.0173413775085622,0.0231997078490661),
 .UNSPECIFIED.) ;
#1412 = B_SPLINE_CURVE_WITH_KNOTS('',3,(#102875,#102876,#102877,#102878,#102879,
#102880,#102881,#102882,#102883,#102884,#102885,#102886,#102887,#102888,
#102889,#102890),.UNSPECIFIED.,.F.,.F.,(4,3,3,3,3,4),(-0.0468370142553995,
-0.0463994157003126,-0.0407777109430307,-0.0349170905389541,-0.0290580381909493,
-0.0231997078501516),.UNSPECIFIED.) ;
#1413 = B_SPLINE_CURVE_WITH_KNOTS('',3,(#102896,#102897,#102898,#102899,#102900,
#102901,#102902,#102903,#102904,#102905,#102906,#102907,#102908,#102909),
 .UNSPECIFIED.,.F.,.F.,(4,2,2,2,2,2,4),(-0.000236619803559952,0.,0.00609779134694098,
0.0119337102432763,0.0183998186382272,0.0234029027754186,0.0278441972733939),
 .UNSPECIFIED.) ;
#1414 = B_SPLINE_CURVE_WITH_KNOTS('',3,(#102915,#102916,#102917,#102918,#102919,
#102920,#102921,#102922,#102923,#102924,#102925,#102926,#102927,#102928),
 .UNSPECIFIED.,.F.,.F.,(4,2,2,2,2,2,4),(-0.0559250143507825,-0.0556883945467992,
-0.0495906032001226,-0.043754684304009,-0.0372885759090493,-0.032285491771857,
-0.0278441972738728),.UNSPECIFIED.) ;
#1415 = B_SPLINE_CURVE_WITH_KNOTS('',3,(#102934,#102935,#102936,#102937,#102938,
#102939,#102940,#102941,#102942,#102943,#102944,#102945,#102946,#102947,
#102948,#102949),.UNSPECIFIED.,.F.,.F.,(4,3,3,3,3,4),(-0.000437598556095639,
0.,0.00562170475706734,0.0114823251608502,0.0173413775085488,0.0231997078490271),
 .UNSPECIFIED.) ;
#1416 = B_SPLINE_CURVE_WITH_KNOTS('',3,(#102955,#102956,#102957,#102958,#102959,
#102960,#102961,#102962,#102963,#102964,#102965,#102966,#102967,#102968,
#102969,#102970),.UNSPECIFIED.,.F.,.F.,(4,3,3,3,3,4),(-0.0468370142543074,
-0.0463994156982126,-0.0407777109411238,-0.0349170905373201,-0.0290580381896051,
-0.0231997078491063),.UNSPECIFIED.) ;
#1417 = B_SPLINE_CURVE_WITH_KNOTS('',3,(#102976,#102977,#102978,#102979,#102980,
#102981,#102982,#102983,#102984,#102985,#102986,#102987,#102988,#102989),
 .UNSPECIFIED.,.F.,.F.,(4,2,2,2,2,2,4),(-0.000236619803981649,0.,0.00609779134664719,
0.0119337102427236,0.0183998186376455,0.0234029027747974,0.0278441972727449),
 .UNSPECIFIED.) ;
#1418 = B_SPLINE_CURVE_WITH_KNOTS('',3,(#102995,#102996,#102997,#102998,#102999,
#103000,#103001,#103002,#103003,#103004,#103005,#103006,#103007,#103008),
 .UNSPECIFIED.,.F.,.F.,(4,2,2,2,2,2,4),(-0.055925014352087,-0.0556883945480977,
-0.0495906032012405,-0.0437546843049561,-0.0372885759098064,-0.0322854917724869,
-0.0278441972743996),.UNSPECIFIED.) ;
#1419 = B_SPLINE_CURVE_WITH_KNOTS('',3,(#103014,#103015,#103016,#103017,#103018,
#103019,#103020,#103021,#103022,#103023,#103024,#103025,#103026,#103027,
#103028,#103029),.UNSPECIFIED.,.F.,.F.,(4,3,3,3,3,4),(-0.000437598556128711,
0.,0.00562170475726701,0.0114823251612751,0.0173413775092439,0.0231997078500064),
 .UNSPECIFIED.) ;
#1420 = B_SPLINE_CURVE_WITH_KNOTS('',3,(#103035,#103036,#103037,#103038,#103039,
#103040,#103041,#103042,#103043,#103044,#103045,#103046,#103047,#103048,
#103049,#103050),.UNSPECIFIED.,.F.,.F.,(4,3,3,3,3,4),(-0.0468370142525421,
-0.046399415696666,-0.0407777109397685,-0.0349170905362003,-0.029058038188693,
-0.0231997078483865),.UNSPECIFIED.) ;
#1421 = B_SPLINE_CURVE_WITH_KNOTS('',3,(#103056,#103057,#103058,#103059,#103060,
#103061,#103062,#103063,#103064,#103065,#103066,#103067,#103068,#103069),
 .UNSPECIFIED.,.F.,.F.,(4,2,2,2,2,2,4),(-0.000236619803982414,0.,0.00609779134661,
0.0119337102426289,0.0183998186375097,0.0234029027746178,0.0278441972725225),
 .UNSPECIFIED.) ;
#1422 = B_SPLINE_CURVE_WITH_KNOTS('',3,(#103075,#103076,#103077,#103078,#103079,
#103080,#103081,#103082,#103083,#103084,#103085,#103086,#103087,#103088),
 .UNSPECIFIED.,.F.,.F.,(4,2,2,2,2,2,4),(-0.0559250143493171,-0.0556883945461739,
-0.0495906031990541,-0.0437546843026118,-0.037288575907723,-0.0322854917706097,
-0.0278441972727174),.UNSPECIFIED.) ;
#1423 = B_SPLINE_CURVE_WITH_KNOTS('',3,(#103094,#103095,#103096,#103097,#103098,
#103099,#103100,#103101,#103102,#103103,#103104,#103105,#103106,#103107,
#103108,#103109),.UNSPECIFIED.,.F.,.F.,(4,3,3,3,3,4),(-0.000437598556087196,
0.,0.00562170475699019,0.0114823251606472,0.0173413775082489,0.0231997078486377),
 .UNSPECIFIED.) ;
#1424 = B_SPLINE_CURVE_WITH_KNOTS('',3,(#103115,#103116,#103117,#103118,#103119,
#103120,#103121,#103122,#103123,#103124,#103125,#103126,#103127,#103128,
#103129,#103130),.UNSPECIFIED.,.F.,.F.,(4,3,3,3,3,4),(-0.0468370142500863,
-0.0463994156945211,-0.0407777109379294,-0.0349170905346585,-0.0290580381874365,
-0.0231997078474141),.UNSPECIFIED.) ;
#1425 = B_SPLINE_CURVE_WITH_KNOTS('',3,(#103136,#103137,#103138,#103139,#103140,
#103141,#103142,#103143,#103144,#103145,#103146,#103147,#103148,#103149),
 .UNSPECIFIED.,.F.,.F.,(4,2,2,2,2,2,4),(-0.000236619803560014,0.,0.00609779134678491,
0.0119337102429536,0.0183998186377476,0.0234029027747679,0.0278441972725981),
 .UNSPECIFIED.) ;
#1426 = B_SPLINE_CURVE_WITH_KNOTS('',3,(#103155,#103156,#103157,#103158,#103159,
#103160,#103161,#103162,#103163,#103164,#103165,#103166,#103167,#103168),
 .UNSPECIFIED.,.F.,.F.,(4,2,2,2,2,2,4),(-0.0559250143548778,-0.0556883945506748,
-0.0495906032033264,-0.0437546843064839,-0.0372885759109464,-0.0322854917733345,
-0.0278441972750097),.UNSPECIFIED.) ;
#1427 = B_SPLINE_CURVE_WITH_KNOTS('',3,(#103174,#103175,#103176,#103177,#103178,
#103179,#103180,#103181,#103182,#103183,#103184,#103185,#103186,#103187,
#103188,#103189),.UNSPECIFIED.,.F.,.F.,(4,3,3,3,3,4),(-0.000437598556223204,
0.,0.00562170475783914,0.0114823251625445,0.0173413775111918,0.0231997078526027),
 .UNSPECIFIED.) ;
#1428 = B_SPLINE_CURVE_WITH_KNOTS('',3,(#103195,#103196,#103197,#103198,#103199,
#103200,#103201,#103202,#103203,#103204,#103205,#103206,#103207,#103208,
#103209,#103210),.UNSPECIFIED.,.F.,.F.,(4,3,3,3,3,4),(-0.0468370142563843,
-0.046399415700489,-0.0407777109431322,-0.0349170905389995,-0.0290580381909307,
-0.0231997078501088),.UNSPECIFIED.) ;
#1429 = B_SPLINE_CURVE_WITH_KNOTS('',3,(#103216,#103217,#103218,#103219,#103220,
#103221,#103222,#103223,#103224,#103225,#103226,#103227,#103228,#103229),
 .UNSPECIFIED.,.F.,.F.,(4,2,2,2,2,2,4),(-0.000236619804200277,0.,0.00609779134716414,
0.0119337102438048,0.0183998186391783,0.0234029027766296,0.0278441972748296),
 .UNSPECIFIED.) ;
#1430 = B_SPLINE_CURVE_WITH_KNOTS('',3,(#103235,#103236,#103237,#103238,#103239,
#103240,#103241,#103242,#103243,#103244,#103245,#103246,#103247,#103248),
 .UNSPECIFIED.,.F.,.F.,(4,2,2,2,2,2,4),(-0.0559250143496621,-0.0556883945461033,
-0.0495906031992651,-0.0437546843029983,-0.0372885759081094,-0.032285491771005,
-0.02784419727311),.UNSPECIFIED.) ;
#1431 = B_SPLINE_CURVE_WITH_KNOTS('',3,(#103254,#103255,#103256,#103257,#103258,
#103259,#103260,#103261,#103262,#103263,#103264,#103265,#103266,#103267,
#103268,#103269),.UNSPECIFIED.,.F.,.F.,(4,3,3,3,3,4),(-0.000437598556084584,
0.,0.00562170475697965,0.0114823251606079,0.0173413775081775,0.0231997078485472),
 .UNSPECIFIED.) ;
#1432 = B_SPLINE_CURVE_WITH_KNOTS('',3,(#103275,#103276,#103277,#103278,#103279,
#103280,#103281,#103282,#103283,#103284,#103285,#103286,#103287,#103288,
#103289,#103290),.UNSPECIFIED.,.F.,.F.,(4,3,3,3,3,4),(-0.0468370142549382,
-0.0463994156994604,-0.0407777109422707,-0.0349170905383382,-0.0290580381904463,
-0.023199707849757),.UNSPECIFIED.) ;
#1433 = B_SPLINE_CURVE_WITH_KNOTS('',3,(#103296,#103297,#103298,#103299,#103300,
#103301,#103302,#103303,#103304,#103305,#103306,#103307,#103308,#103309),
 .UNSPECIFIED.,.F.,.F.,(4,2,2,2,2,2,4),(-0.000236619803568316,0.,0.00609779134701837,
0.0119337102434465,0.0183998186385035,0.0234029027757473,0.0278441972737745),
 .UNSPECIFIED.) ;
#1434 = B_SPLINE_CURVE_WITH_KNOTS('',3,(#103315,#103316,#103317,#103318,#103319,
#103320,#103321,#103322,#103323,#103324,#103325,#103326,#103327,#103328),
 .UNSPECIFIED.,.F.,.F.,(4,2,2,2,2,2,4),(-0.0559250143499934,-0.0556883945464304,
-0.0495906031995064,-0.0437546843032007,-0.037288575908277,-0.032285491771123,
-0.0278441972731808),.UNSPECIFIED.) ;
#1435 = B_SPLINE_CURVE_WITH_KNOTS('',3,(#103334,#103335,#103336,#103337,#103338,
#103339,#103340,#103341,#103342,#103343,#103344,#103345,#103346,#103347,
#103348,#103349),.UNSPECIFIED.,.F.,.F.,(4,3,3,3,3,4),(-0.000437598556092419,
0.,0.00562170475702671,0.0114823251607112,0.0173413775083605,0.0231997078487915),
 .UNSPECIFIED.) ;
#1436 = B_SPLINE_CURVE_WITH_KNOTS('',3,(#103355,#103356,#103357,#103358,#103359,
#103360,#103361,#103362,#103363,#103364,#103365,#103366,#103367,#103368,
#103369,#103370),.UNSPECIFIED.,.F.,.F.,(4,3,3,3,3,4),(-0.0468370142548351,
-0.0463994156987323,-0.0407777109416122,-0.0349170905377609,-0.0290580381899607,
-0.0231997078493697),.UNSPECIFIED.) ;
#1437 = B_SPLINE_CURVE_WITH_KNOTS('',3,(#103376,#103377,#103378,#103379,#103380,
#103381,#103382,#103383,#103384,#103385,#103386,#103387,#103388,#103389),
 .UNSPECIFIED.,.F.,.F.,(4,2,2,2,2,2,4),(-0.000236619803562033,0.,0.00609779134691358,
0.0119337102432247,0.0183998186381566,0.0234029027753094,0.027844197273255),
 .UNSPECIFIED.) ;
#1438 = B_SPLINE_CURVE_WITH_KNOTS('',3,(#103395,#103396,#103397,#103398,#103399,
#103400,#103401,#103402,#103403,#103404,#103405,#103406,#103407,#103408),
 .UNSPECIFIED.,.F.,.F.,(4,2,2,2,2,2,4),(-0.0559250143503813,-0.0556883945472345,
-0.0495906032000065,-0.0437546843033907,-0.0372885759083472,-0.0322854917711086,
-0.027844197273083),.UNSPECIFIED.) ;
#1439 = B_SPLINE_CURVE_WITH_KNOTS('',3,(#103414,#103415,#103416,#103417,#103418,
#103419,#103420,#103421,#103422,#103423,#103424,#103425,#103426,#103427,
#103428,#103429),.UNSPECIFIED.,.F.,.F.,(4,3,3,3,3,4),(-0.000437598556129241,
0.,0.00562170475730571,0.0114823251613513,0.0173413775093445,0.0231997078501172),
 .UNSPECIFIED.) ;
#1440 = B_SPLINE_CURVE_WITH_KNOTS('',3,(#103435,#103436,#103437,#103438,#103439,
#103440,#103441,#103442,#103443,#103444,#103445,#103446,#103447,#103448,
#103449,#103450),.UNSPECIFIED.,.F.,.F.,(4,3,3,3,3,4),(-0.0468370142515845,
-0.0463994156955989,-0.0407777109388572,-0.0349170905354382,-0.0290580381880585,
-0.0231997078478789),.UNSPECIFIED.) ;
#1441 = B_SPLINE_CURVE_WITH_KNOTS('',3,(#103456,#103457,#103458,#103459,#103460,
#103461,#103462,#103463,#103464,#103465,#103466,#103467,#103468,#103469),
 .UNSPECIFIED.,.F.,.F.,(4,2,2,2,2,2,4),(-0.000236619803559663,0.,0.0060977913468164,
0.0119337102430072,0.0183998186378663,0.0234029027749556,0.0278441972728503),
 .UNSPECIFIED.) ;
#1442 = B_SPLINE_CURVE_WITH_KNOTS('',3,(#103475,#103476,#103477,#103478,#103479,
#103480,#103481,#103482,#103483,#103484,#103485,#103486,#103487,#103488),
 .UNSPECIFIED.,.F.,.F.,(4,2,2,2,2,2,4),(-0.0559250143533661,-0.0556883945491649,
-0.0495906032019838,-0.0437546843053393,-0.0372885759099808,-0.0322854917725361,
-0.0278441972743507),.UNSPECIFIED.) ;
#1443 = B_SPLINE_CURVE_WITH_KNOTS('',3,(#103494,#103495,#103496,#103497,#103498,
#103499,#103500,#103501,#103502,#103503,#103504,#103505,#103506,#103507,
#103508,#103509),.UNSPECIFIED.,.F.,.F.,(4,3,3,3,3,4),(-0.00043759855615984,
0.,0.00562170475737693,0.011482325161534,0.017341377509665,0.0231997078505602),
 .UNSPECIFIED.) ;
#1444 = B_SPLINE_CURVE_WITH_KNOTS('',3,(#103515,#103516,#103517,#103518,#103519,
#103520,#103521,#103522,#103523,#103524,#103525,#103526,#103527,#103528,
#103529,#103530),.UNSPECIFIED.,.F.,.F.,(4,3,3,3,3,4),(-0.0468370142504761,
-0.0463994156944377,-0.0407777109378315,-0.0349170905345851,-0.0290580381873817,
-0.0231997078473671),.UNSPECIFIED.) ;
#1445 = B_SPLINE_CURVE_WITH_KNOTS('',3,(#103536,#103537,#103538,#103539,#103540,
#103541,#103542,#103543,#103544,#103545,#103546,#103547,#103548,#103549),
 .UNSPECIFIED.,.F.,.F.,(4,2,2,2,2,2,4),(-0.000236619803559426,0.,0.00609779134674399,
0.0119337102428204,0.0183998186375428,0.0234029027745216,0.0278441972723019),
 .UNSPECIFIED.) ;
#1446 = B_SPLINE_CURVE_WITH_KNOTS('',3,(#103555,#103556,#103557,#103558,#103559,
#103560,#103561,#103562,#103563,#103564,#103565,#103566,#103567,#103568),
 .UNSPECIFIED.,.F.,.F.,(4,2,2,2,2,2,4),(-0.0559250143520313,-0.0556883945484605,
-0.0495906032013131,-0.0437546843047777,-0.037288575909542,-0.0322854917721873,
-0.0278441972740755),.UNSPECIFIED.) ;
#1447 = B_SPLINE_CURVE_WITH_KNOTS('',3,(#103574,#103575,#103576,#103577,#103578,
#103579,#103580,#103581,#103582,#103583,#103584,#103585,#103586,#103587,
#103588,#103589),.UNSPECIFIED.,.F.,.F.,(4,3,3,3,3,4),(-0.000437598556142791,
0.,0.00562170475737048,0.011482325161532,0.0173413775096432,0.0231997078505159),
 .UNSPECIFIED.) ;
#1448 = B_SPLINE_CURVE_WITH_KNOTS('',3,(#103595,#103596,#103597,#103598,#103599,
#103600,#103601,#103602,#103603,#103604,#103605,#103606,#103607,#103608,
#103609,#103610),.UNSPECIFIED.,.F.,.F.,(4,3,3,3,3,4),(-0.046837014256793,
-0.0463994157012118,-0.0407777109438107,-0.0349170905396121,-0.0290580381914533,
-0.0231997078505249),.UNSPECIFIED.) ;
#1449 = B_SPLINE_CURVE_WITH_KNOTS('',3,(#104026,#104027,#104028,#104029,#104030,
#104031,#104032,#104033,#104034,#104035,#104036,#104037,#104038,#104039),
 .UNSPECIFIED.,.F.,.F.,(4,2,2,2,2,2,4),(-0.0559250143525619,-0.0556883945479474,
-0.0495906032011524,-0.0437546843048812,-0.037288575909754,-0.0322854917724513,
-0.027844197274366),.UNSPECIFIED.) ;
#1450 = B_SPLINE_CURVE_WITH_KNOTS('',3,(#104042,#104043,#104044,#104045,#104046,
#104047,#104048,#104049,#104050,#104051,#104052,#104053,#104054,#104055),
 .UNSPECIFIED.,.F.,.F.,(4,2,2,2,2,2,4),(-0.000236619803144863,0.,0.00609779134711087,
0.0119337102436339,0.0183998186386153,0.0234029027758149,0.0278441972738027),
 .UNSPECIFIED.) ;
#1451 = B_SPLINE_CURVE_WITH_KNOTS('',3,(#104058,#104059,#104060,#104061,#104062,
#104063,#104064,#104065,#104066,#104067,#104068,#104069,#104070,#104071,
#104072,#104073),.UNSPECIFIED.,.F.,.F.,(4,3,3,3,3,4),(-0.000437598556136612,
0.,0.00562170475739987,0.0114823251615695,0.0173413775096577,0.0231997078505359),
 .UNSPECIFIED.) ;
#1452 = B_SPLINE_CURVE_WITH_KNOTS('',3,(#104078,#104079,#104080,#104081,#104082,
#104083,#104084,#104085,#104086,#104087,#104088,#104089,#104090,#104091,
#104092,#104093),.UNSPECIFIED.,.F.,.F.,(4,3,3,3,3,4),(0.,0.00585824217054478,
0.0117172063374487,0.0175777385368331,0.0231993586852603,0.0236369506553383),
 .UNSPECIFIED.) ;
#1453 = B_SPLINE_CURVE_WITH_KNOTS('',3,(#104095,#104096,#104097,#104098,#104099,
#104100,#104101,#104102,#104103,#104104,#104105,#104106,#104107,#104108),
 .UNSPECIFIED.,.F.,.F.,(4,2,2,2,2,2,4),(-0.000236619803563006,0.,0.00609779134689459,
0.0119337102432047,0.0183998186381472,0.0234029027752928,0.027844197273235),
 .UNSPECIFIED.) ;
#1454 = B_SPLINE_CURVE_WITH_KNOTS('',3,(#104111,#104112,#104113,#104114,#104115,
#104116,#104117,#104118,#104119,#104120,#104121,#104122,#104123,#104124,
#104125,#104126),.UNSPECIFIED.,.F.,.F.,(4,3,3,3,3,4),(0.,0.00585824217054169,
0.0117172063374197,0.0175777385367584,0.0231993586851914,0.0236369506552836),
 .UNSPECIFIED.) ;
#1455 = B_SPLINE_CURVE_WITH_KNOTS('',3,(#104128,#104129,#104130,#104131,#104132,
#104133,#104134,#104135,#104136,#104137,#104138,#104139,#104140,#104141),
 .UNSPECIFIED.,.F.,.F.,(4,2,2,2,2,2,4),(-0.055925014352618,-0.0556883945495578,
-0.049590603202043,-0.0437546843051378,-0.0372885759097438,-0.032285491772261,
-0.0278441972740487),.UNSPECIFIED.) ;
#1456 = B_SPLINE_CURVE_WITH_KNOTS('',3,(#104143,#104144,#104145,#104146,#104147,
#104148,#104149,#104150,#104151,#104152,#104153,#104154,#104155,#104156,
#104157,#104158),.UNSPECIFIED.,.F.,.F.,(4,3,3,3,3,4),(-0.000437598556173687,
0.,0.00562170475743059,0.0114823251616519,0.0173413775098334,0.0231997078507846),
 .UNSPECIFIED.) ;
#1457 = B_SPLINE_CURVE_WITH_KNOTS('',3,(#104163,#104164,#104165,#104166,#104167,
#104168,#104169,#104170,#104171,#104172,#104173,#104174,#104175,#104176,
#104177,#104178),.UNSPECIFIED.,.F.,.F.,(4,3,3,3,3,4),(0.,0.0058582421705496,
0.0117172063374621,0.01757773853685,0.0231993586852295,0.0236369506553315),
 .UNSPECIFIED.) ;
#1458 = B_SPLINE_CURVE_WITH_KNOTS('',3,(#104179,#104180,#104181,#104182,#104183,
#104184,#104185,#104186,#104187,#104188,#104189,#104190,#104191,#104192),
 .UNSPECIFIED.,.F.,.F.,(4,2,2,2,2,2,4),(-0.000236619803562956,0.,0.00609779134697842,
0.0119337102433575,0.0183998186383507,0.0234029027755715,0.027844197273593),
 .UNSPECIFIED.) ;
#1459 = B_SPLINE_CURVE_WITH_KNOTS('',3,(#104194,#104195,#104196,#104197,#104198,
#104199,#104200,#104201,#104202,#104203,#104204,#104205,#104206,#104207),
 .UNSPECIFIED.,.F.,.F.,(4,2,2,2,2,2,4),(-0.00023661980356627,0.,0.0060977913470113,
0.0119337102434447,0.0183998186385308,0.0234029027758003,0.027844197273845),
 .UNSPECIFIED.) ;
#1460 = B_SPLINE_CURVE_WITH_KNOTS('',3,(#104208,#104209,#104210,#104211,#104212,
#104213,#104214,#104215,#104216,#104217,#104218,#104219,#104220,#104221,
#104222,#104223),.UNSPECIFIED.,.F.,.F.,(4,3,3,3,3,4),(0.,0.00585824217053873,
0.0117172063374278,0.0175777385368055,0.023199358685178,0.0236369506552736),
 .UNSPECIFIED.) ;
#1461 = B_SPLINE_CURVE_WITH_KNOTS('',3,(#104225,#104226,#104227,#104228,#104229,
#104230,#104231,#104232,#104233,#104234,#104235,#104236,#104237,#104238),
 .UNSPECIFIED.,.F.,.F.,(4,2,2,2,2,2,4),(-0.055925014347253,-0.0556883945436994,
-0.0495906031970911,-0.0437546843011451,-0.0372885759065727,-0.0322854917697116,
-0.0278441972720297),.UNSPECIFIED.) ;
#1462 = B_SPLINE_CURVE_WITH_KNOTS('',3,(#104240,#104241,#104242,#104243,#104244,
#104245,#104246,#104247,#104248,#104249,#104250,#104251,#104252,#104253,
#104254,#104255),.UNSPECIFIED.,.F.,.F.,(4,3,3,3,3,4),(-0.000437598556065294,
0.,0.00562170475696129,0.0114823251605729,0.0173413775081186,0.0231997078484631),
 .UNSPECIFIED.) ;
#1463 = B_SPLINE_CURVE_WITH_KNOTS('',3,(#104260,#104261,#104262,#104263,#104264,
#104265,#104266,#104267,#104268,#104269,#104270,#104271,#104272,#104273,
#104274,#104275),.UNSPECIFIED.,.F.,.F.,(4,3,3,3,3,4),(0.,0.00585824217053423,
0.0117172063374038,0.0175777385367393,0.0231993586850723,0.0236369506551701),
 .UNSPECIFIED.) ;
#1464 = B_SPLINE_CURVE_WITH_KNOTS('',3,(#104276,#104277,#104278,#104279,#104280,
#104281,#104282,#104283,#104284,#104285,#104286,#104287,#104288,#104289),
 .UNSPECIFIED.,.F.,.F.,(4,2,2,2,2,2,4),(-0.00023661980315042,0.,0.00609779134723154,
0.0119337102438925,0.0183998186390206,0.0234029027763186,0.027844197274388),
 .UNSPECIFIED.) ;
#1465 = B_SPLINE_CURVE_WITH_KNOTS('',3,(#104291,#104292,#104293,#104294,#104295,
#104296,#104297,#104298,#104299,#104300,#104301,#104302,#104303,#104304),
 .UNSPECIFIED.,.F.,.F.,(4,2,2,2,2,2,4),(-0.000236619803568179,0.,0.00609779134706943,
0.011933710243561,0.0183998186387449,0.0234029027760718,0.0278441972741583),
 .UNSPECIFIED.) ;
#1466 = B_SPLINE_CURVE_WITH_KNOTS('',3,(#104305,#104306,#104307,#104308,#104309,
#104310,#104311,#104312,#104313,#104314,#104315,#104316,#104317,#104318,
#104319,#104320),.UNSPECIFIED.,.F.,.F.,(4,3,3,3,3,4),(0.,0.00585824217054849,
0.0117172063374606,0.0175777385368388,0.0231993586852149,0.0236369506553345),
 .UNSPECIFIED.) ;
#1467 = B_SPLINE_CURVE_WITH_KNOTS('',3,(#104322,#104323,#104324,#104325,#104326,
#104327,#104328,#104329,#104330,#104331,#104332,#104333,#104334,#104335),
 .UNSPECIFIED.,.F.,.F.,(4,2,2,2,2,2,4),(-0.0559250143497057,-0.0556883945461452,
-0.0495906031993172,-0.0437546843030612,-0.0372885759081806,-0.0322854917710824,
-0.0278441972731839),.UNSPECIFIED.) ;
#1468 = B_SPLINE_CURVE_WITH_KNOTS('',3,(#104337,#104338,#104339,#104340,#104341,
#104342,#104343,#104344,#104345,#104346,#104347,#104348,#104349,#104350,
#104351,#104352),.UNSPECIFIED.,.F.,.F.,(4,3,3,3,3,4),(-0.000437598556084839,
0.,0.00562170475699754,0.0114823251606981,0.0173413775083502,0.0231997078487964),
 .UNSPECIFIED.) ;
#1469 = B_SPLINE_CURVE_WITH_KNOTS('',3,(#104357,#104358,#104359,#104360,#104361,
#104362,#104363,#104364,#104365,#104366,#104367,#104368,#104369,#104370,
#104371,#104372),.UNSPECIFIED.,.F.,.F.,(4,3,3,3,3,4),(0.,0.00585824217054277,
0.0117172063374441,0.0175777385368182,0.0231993586851572,0.0236369506552668),
 .UNSPECIFIED.) ;
#1470 = B_SPLINE_CURVE_WITH_KNOTS('',3,(#104373,#104374,#104375,#104376,#104377,
#104378,#104379,#104380,#104381,#104382,#104383,#104384,#104385,#104386),
 .UNSPECIFIED.,.F.,.F.,(4,2,2,2,2,2,4),(-0.00023661980356187,0.,0.00609779134698056,
0.0119337102433812,0.0183998186384326,0.0234029027756759,0.0278441972736905),
 .UNSPECIFIED.) ;
#1471 = B_SPLINE_CURVE_WITH_KNOTS('',3,(#104388,#104389,#104390,#104391,#104392,
#104393,#104394,#104395,#104396,#104397,#104398,#104399,#104400,#104401),
 .UNSPECIFIED.,.F.,.F.,(4,2,2,2,2,2,4),(-0.000236619803566785,0.,0.00609779134702904,
0.0119337102434475,0.0183998186384865,0.0234029027757207,0.0278441972737459),
 .UNSPECIFIED.) ;
#1472 = B_SPLINE_CURVE_WITH_KNOTS('',3,(#104402,#104403,#104404,#104405,#104406,
#104407,#104408,#104409,#104410,#104411,#104412,#104413,#104414,#104415,
#104416,#104417),.UNSPECIFIED.,.F.,.F.,(4,3,3,3,3,4),(0.,0.00585824217054034,
0.0117172063374279,0.0175777385367946,0.0231993586851777,0.0236369506552812),
 .UNSPECIFIED.) ;
#1473 = B_SPLINE_CURVE_WITH_KNOTS('',3,(#104419,#104420,#104421,#104422,#104423,
#104424,#104425,#104426,#104427,#104428,#104429,#104430,#104431,#104432),
 .UNSPECIFIED.,.F.,.F.,(4,2,2,2,2,2,4),(-0.0559250143501053,-0.0556883945465432,
-0.0495906031996281,-0.0437546843033128,-0.0372885759083777,-0.0322854917712189,
-0.0278441972732712),.UNSPECIFIED.) ;
#1474 = B_SPLINE_CURVE_WITH_KNOTS('',3,(#104434,#104435,#104436,#104437,#104438,
#104439,#104440,#104441,#104442,#104443,#104444,#104445,#104446,#104447,
#104448,#104449),.UNSPECIFIED.,.F.,.F.,(4,3,3,3,3,4),(-0.000437598556096447,
0.,0.00562170475713416,0.0114823251609764,0.0173413775087778,0.0231997078493695),
 .UNSPECIFIED.) ;
#1475 = B_SPLINE_CURVE_WITH_KNOTS('',3,(#104454,#104455,#104456,#104457,#104458,
#104459,#104460,#104461,#104462,#104463,#104464,#104465,#104466,#104467,
#104468,#104469),.UNSPECIFIED.,.F.,.F.,(4,3,3,3,3,4),(0.,0.00585824217053087,
0.0117172063373846,0.0175777385366825,0.0231993586850888,0.0236369506551764),
 .UNSPECIFIED.) ;
#1476 = B_SPLINE_CURVE_WITH_KNOTS('',3,(#104470,#104471,#104472,#104473,#104474,
#104475,#104476,#104477,#104478,#104479,#104480,#104481,#104482,#104483),
 .UNSPECIFIED.,.F.,.F.,(4,2,2,2,2,2,4),(-0.000236619803975554,0.,0.00609779134645292,
0.0119337102422305,0.0183998186368445,0.0234029027737468,0.0278441972714777),
 .UNSPECIFIED.) ;
#1477 = B_SPLINE_CURVE_WITH_KNOTS('',3,(#104485,#104486,#104487,#104488,#104489,
#104490,#104491,#104492,#104493,#104494,#104495,#104496,#104497,#104498),
 .UNSPECIFIED.,.F.,.F.,(4,2,2,2,2,2,4),(-0.000236619803145561,0.,0.00609779134719067,
0.0119337102437602,0.0183998186387406,0.0234029027759312,0.0278441972739105),
 .UNSPECIFIED.) ;
#1478 = B_SPLINE_CURVE_WITH_KNOTS('',3,(#104499,#104500,#104501,#104502,#104503,
#104504,#104505,#104506,#104507,#104508,#104509,#104510,#104511,#104512,
#104513,#104514),.UNSPECIFIED.,.F.,.F.,(4,3,3,3,3,4),(0.,0.00585824217053935,
0.0117172063374137,0.0175777385367471,0.0231993586851797,0.0236369506552624),
 .UNSPECIFIED.) ;
#1479 = B_SPLINE_CURVE_WITH_KNOTS('',3,(#104516,#104517,#104518,#104519,#104520,
#104521,#104522,#104523,#104524,#104525,#104526,#104527,#104528,#104529),
 .UNSPECIFIED.,.F.,.F.,(4,2,2,2,2,2,4),(-0.0559250143516561,-0.0556883945480848,
-0.0495906032009887,-0.0437546843044866,-0.0372885759093485,-0.032285491772039,
-0.0278441972739555),.UNSPECIFIED.) ;
#1480 = B_SPLINE_CURVE_WITH_KNOTS('',3,(#104531,#104532,#104533,#104534,#104535,
#104536,#104537,#104538,#104539,#104540,#104541,#104542,#104543,#104544,
#104545,#104546),.UNSPECIFIED.,.F.,.F.,(4,3,3,3,3,4),(-0.000437598556137922,
0.,0.00562170475738925,0.0114823251615342,0.0173413775096173,0.0231997078504894),
 .UNSPECIFIED.) ;
#1481 = B_SPLINE_CURVE_WITH_KNOTS('',3,(#104551,#104552,#104553,#104554,#104555,
#104556,#104557,#104558,#104559,#104560,#104561,#104562,#104563,#104564,
#104565,#104566),.UNSPECIFIED.,.F.,.F.,(4,3,3,3,3,4),(0.,0.00585824217054286,
0.0117172063374258,0.0175777385367681,0.0231993586851975,0.0236369506552776),
 .UNSPECIFIED.) ;
#1482 = B_SPLINE_CURVE_WITH_KNOTS('',3,(#104567,#104568,#104569,#104570,#104571,
#104572,#104573,#104574,#104575,#104576,#104577,#104578,#104579,#104580),
 .UNSPECIFIED.,.F.,.F.,(4,2,2,2,2,2,4),(-0.000236619803141347,0.,0.00609779134719742,
0.0119337102437761,0.0183998186387667,0.0234029027759622,0.0278441972739489),
 .UNSPECIFIED.) ;
#1483 = B_SPLINE_CURVE_WITH_KNOTS('',3,(#104582,#104583,#104584,#104585,#104586,
#104587,#104588,#104589,#104590,#104591,#104592,#104593,#104594,#104595),
 .UNSPECIFIED.,.F.,.F.,(4,2,2,2,2,2,4),(-0.000236619803560324,0.,0.00609779134688203,
0.0119337102431469,0.0183998186380461,0.0234029027751694,0.0278441972730812),
 .UNSPECIFIED.) ;
#1484 = B_SPLINE_CURVE_WITH_KNOTS('',3,(#104596,#104597,#104598,#104599,#104600,
#104601,#104602,#104603,#104604,#104605,#104606,#104607,#104608,#104609,
#104610,#104611),.UNSPECIFIED.,.F.,.F.,(4,3,3,3,3,4),(0.,0.00585824217053624,
0.0117172063373978,0.017577738536714,0.0231993586851339,0.0236369506552253),
 .UNSPECIFIED.) ;
#1485 = B_SPLINE_CURVE_WITH_KNOTS('',3,(#104613,#104614,#104615,#104616,#104617,
#104618,#104619,#104620,#104621,#104622,#104623,#104624,#104625,#104626),
 .UNSPECIFIED.,.F.,.F.,(4,2,2,2,2,2,4),(-0.0559250143527569,-0.0556883945491825,
-0.0495906032019952,-0.0437546843053732,-0.0372885759100185,-0.0322854917725816,
-0.0278441972744026),.UNSPECIFIED.) ;
#1486 = B_SPLINE_CURVE_WITH_KNOTS('',3,(#104628,#104629,#104630,#104631,#104632,
#104633,#104634,#104635,#104636,#104637,#104638,#104639,#104640,#104641,
#104642,#104643),.UNSPECIFIED.,.F.,.F.,(4,3,3,3,3,4),(-0.000437598556170072,
0.,0.00562170475739005,0.0114823251615356,0.0173413775096278,0.0231997078504878),
 .UNSPECIFIED.) ;
#1487 = B_SPLINE_CURVE_WITH_KNOTS('',3,(#104648,#104649,#104650,#104651,#104652,
#104653,#104654,#104655,#104656,#104657,#104658,#104659,#104660,#104661,
#104662,#104663),.UNSPECIFIED.,.F.,.F.,(4,3,3,3,3,4),(0.,0.00585824217054469,
0.0117172063374513,0.0175777385368039,0.0231993586851361,0.0236369506553527),
 .UNSPECIFIED.) ;
#1488 = B_SPLINE_CURVE_WITH_KNOTS('',3,(#104664,#104665,#104666,#104667,#104668,
#104669,#104670,#104671,#104672,#104673,#104674,#104675,#104676,#104677),
 .UNSPECIFIED.,.F.,.F.,(4,2,2,2,2,2,4),(-0.000236619804202799,0.,0.00609779134737763,
0.0119337102442503,0.0183998186398358,0.0234029027774637,0.0278441972757869),
 .UNSPECIFIED.) ;
#1489 = B_SPLINE_CURVE_WITH_KNOTS('',3,(#104679,#104680,#104681,#104682,#104683,
#104684,#104685,#104686,#104687,#104688,#104689,#104690,#104691,#104692),
 .UNSPECIFIED.,.F.,.F.,(4,2,2,2,2,2,4),(-0.0002366198042002,0.,0.00609779134724177,
0.0119337102439773,0.0183998186394422,0.0234029027769713,0.027844197275244),
 .UNSPECIFIED.) ;
#1490 = B_SPLINE_CURVE_WITH_KNOTS('',3,(#104693,#104694,#104695,#104696,#104697,
#104698,#104699,#104700,#104701,#104702,#104703,#104704,#104705,#104706,
#104707,#104708),.UNSPECIFIED.,.F.,.F.,(4,3,3,3,3,4),(0.,0.00585824217054219,
0.0117172063374448,0.0175777385367976,0.0231993586850719,0.0236369506552122),
 .UNSPECIFIED.) ;
#1491 = B_SPLINE_CURVE_WITH_KNOTS('',3,(#104710,#104711,#104712,#104713,#104714,
#104715,#104716,#104717,#104718,#104719,#104720,#104721,#104722,#104723),
 .UNSPECIFIED.,.F.,.F.,(4,2,2,2,2,2,4),(-0.0559250143475747,-0.0556883945440193,
-0.0495906031973805,-0.0437546843014019,-0.0372885759067931,-0.0322854917699036,
-0.0278441972721905),.UNSPECIFIED.) ;
#1492 = B_SPLINE_CURVE_WITH_KNOTS('',3,(#104725,#104726,#104727,#104728,#104729,
#104730,#104731,#104732,#104733,#104734,#104735,#104736,#104737,#104738,
#104739,#104740),.UNSPECIFIED.,.F.,.F.,(4,3,3,3,3,4),(-0.000437598556074084,
0.,0.00562170475694653,0.0114823251605845,0.0173413775081531,0.0231997078485162),
 .UNSPECIFIED.) ;
#1493 = B_SPLINE_CURVE_WITH_KNOTS('',3,(#104745,#104746,#104747,#104748,#104749,
#104750,#104751,#104752,#104753,#104754,#104755,#104756,#104757,#104758,
#104759,#104760),.UNSPECIFIED.,.F.,.F.,(4,3,3,3,3,4),(0.,0.00585824217053932,
0.0117172063374163,0.0175777385367554,0.0231993586851953,0.0236369506552652),
 .UNSPECIFIED.) ;
#1494 = B_SPLINE_CURVE_WITH_KNOTS('',3,(#104761,#104762,#104763,#104764,#104765,
#104766,#104767,#104768,#104769,#104770,#104771,#104772,#104773,#104774),
 .UNSPECIFIED.,.F.,.F.,(4,2,2,2,2,2,4),(-0.000236619803563584,0.,0.00609779134684538,
0.0119337102430664,0.0183998186379667,0.0234029027750871,0.0278441972729952),
 .UNSPECIFIED.) ;
#1495 = B_SPLINE_CURVE_WITH_KNOTS('',3,(#104776,#104777,#104778,#104779,#104780,
#104781,#104782,#104783,#104784,#104785,#104786,#104787,#104788,#104789),
 .UNSPECIFIED.,.F.,.F.,(4,2,2,2,2,2,4),(-0.000236619803559064,0.,0.00609779134682761,
0.0119337102430243,0.0183998186378634,0.0234029027749327,0.0278441972727837),
 .UNSPECIFIED.) ;
#1496 = B_SPLINE_CURVE_WITH_KNOTS('',3,(#104790,#104791,#104792,#104793,#104794,
#104795,#104796,#104797,#104798,#104799,#104800,#104801,#104802,#104803,
#104804,#104805),.UNSPECIFIED.,.F.,.F.,(4,3,3,3,3,4),(0.,0.00585824217053403,
0.0117172063373908,0.0175777385367026,0.0231993586851274,0.0236369506551984),
 .UNSPECIFIED.) ;
#1497 = B_SPLINE_CURVE_WITH_KNOTS('',3,(#104807,#104808,#104809,#104810,#104811,
#104812,#104813,#104814,#104815,#104816,#104817,#104818,#104819,#104820),
 .UNSPECIFIED.,.F.,.F.,(4,2,2,2,2,2,4),(-0.0559250143495183,-0.0556883945459582,
-0.0495906031991357,-0.0437546843029003,-0.0372885759080418,-0.0322854917709563,
-0.0278441972730646),.UNSPECIFIED.) ;
#1498 = B_SPLINE_CURVE_WITH_KNOTS('',3,(#104822,#104823,#104824,#104825,#104826,
#104827,#104828,#104829,#104830,#104831,#104832,#104833,#104834,#104835,
#104836,#104837),.UNSPECIFIED.,.F.,.F.,(4,3,3,3,3,4),(-0.000437598556092783,
0.,0.00562170475708721,0.0114823251608936,0.0173413775086511,0.0231997078492032),
 .UNSPECIFIED.) ;
#1499 = B_SPLINE_CURVE_WITH_KNOTS('',3,(#104842,#104843,#104844,#104845,#104846,
#104847,#104848,#104849,#104850,#104851,#104852,#104853,#104854,#104855,
#104856,#104857),.UNSPECIFIED.,.F.,.F.,(4,3,3,3,3,4),(0.,0.00585824217054838,
0.0117172063374519,0.0175777385368119,0.0231993586852536,0.0236369506553148),
 .UNSPECIFIED.) ;
#1500 = B_SPLINE_CURVE_WITH_KNOTS('',3,(#104858,#104859,#104860,#104861,#104862,
#104863,#104864,#104865,#104866,#104867,#104868,#104869,#104870,#104871),
 .UNSPECIFIED.,.F.,.F.,(4,2,2,2,2,2,4),(-0.000236619803558096,0.,0.00609779134681664,
0.0119337102430081,0.0183998186378316,0.0234029027748886,0.0278441972727373),
 .UNSPECIFIED.) ;
#1501 = B_SPLINE_CURVE_WITH_KNOTS('',3,(#104873,#104874,#104875,#104876,#104877,
#104878,#104879,#104880,#104881,#104882,#104883,#104884,#104885,#104886),
 .UNSPECIFIED.,.F.,.F.,(4,2,2,2,2,2,4),(-0.000236619803562333,0.,0.00609779134692135,
0.0119337102432951,0.0183998186383094,0.0234029027755172,0.0278441972735094),
 .UNSPECIFIED.) ;
#1502 = B_SPLINE_CURVE_WITH_KNOTS('',3,(#104887,#104888,#104889,#104890,#104891,
#104892,#104893,#104894,#104895,#104896,#104897,#104898,#104899,#104900,
#104901,#104902),.UNSPECIFIED.,.F.,.F.,(4,3,3,3,3,4),(0.,0.00585824217054129,
0.0117172063374373,0.0175777385368199,0.023199358685217,0.0236369506553186),
 .UNSPECIFIED.) ;
#1503 = B_SPLINE_CURVE_WITH_KNOTS('',3,(#104904,#104905,#104906,#104907,#104908,
#104909,#104910,#104911,#104912,#104913,#104914,#104915,#104916,#104917),
 .UNSPECIFIED.,.F.,.F.,(4,2,2,2,2,2,4),(-0.0559250143502032,-0.0556883945466394,
-0.0495906031997328,-0.0437546843034414,-0.0372885759084786,-0.0322854917713055,
-0.0278441972733409),.UNSPECIFIED.) ;
#1504 = B_SPLINE_CURVE_WITH_KNOTS('',3,(#104919,#104920,#104921,#104922,#104923,
#104924,#104925,#104926,#104927,#104928,#104929,#104930,#104931,#104932,
#104933,#104934),.UNSPECIFIED.,.F.,.F.,(4,3,3,3,3,4),(-0.000437598556094846,
0.,0.00562170475708876,0.0114823251608924,0.0173413775086073,0.0231997078491061),
 .UNSPECIFIED.) ;
#1505 = B_SPLINE_CURVE_WITH_KNOTS('',3,(#104936,#104937,#104938,#104939,#104940,
#104941,#104942,#104943,#104944,#104945,#104946,#104947,#104948,#104949,
#104950,#104951),.UNSPECIFIED.,.F.,.F.,(4,3,3,3,3,4),(0.,0.00585824217053639,
0.0117172063374152,0.0175777385367772,0.0231993586851953,0.0236369506552933),
 .UNSPECIFIED.) ;
#1506 = B_SPLINE_CURVE_WITH_KNOTS('',3,(#104952,#104953,#104954,#104955,#104956,
#104957,#104958,#104959,#104960,#104961,#104962,#104963,#104964,#104965),
 .UNSPECIFIED.,.F.,.F.,(4,2,2,2,2,2,4),(-0.000236619803922217,0.,0.00609779134654128,
0.0119337102425373,0.018399818637407,0.0234029027744858,0.0278441972723643),
 .UNSPECIFIED.) ;
#1507 = B_SPLINE_CURVE_WITH_KNOTS('',3,(#104967,#104968,#104969,#104970,#104971,
#104972,#104973,#104974,#104975,#104976,#104977,#104978,#104979,#104980),
 .UNSPECIFIED.,.F.,.F.,(4,2,2,2,2,2,4),(-0.000236619803561269,0.,0.00609779134692068,
0.0119337102432194,0.0183998186381382,0.02340290277528,0.0278441972732167),
 .UNSPECIFIED.) ;
#1508 = B_SPLINE_CURVE_WITH_KNOTS('',3,(#104981,#104982,#104983,#104984,#104985,
#104986,#104987,#104988,#104989,#104990,#104991,#104992,#104993,#104994,
#104995,#104996),.UNSPECIFIED.,.F.,.F.,(4,3,3,3,3,4),(0.,0.00585824217053491,
0.0117172063374156,0.0175777385367886,0.0231993586852222,0.0236369506553088),
 .UNSPECIFIED.) ;
#1509 = B_SPLINE_CURVE_WITH_KNOTS('',3,(#104998,#104999,#105000,#105001,#105002,
#105003,#105004,#105005,#105006,#105007,#105008,#105009,#105010,#105011),
 .UNSPECIFIED.,.F.,.F.,(4,2,2,2,2,2,4),(-0.0559250143500672,-0.0556883945469228,
-0.049590603199785,-0.0437546843032336,-0.0372885759082228,-0.0322854917710044,
-0.0278441972729959),.UNSPECIFIED.) ;
#1510 = B_SPLINE_CURVE_WITH_KNOTS('',3,(#105013,#105014,#105015,#105016,#105017,
#105018,#105019,#105020,#105021,#105022,#105023,#105024,#105025,#105026,
#105027,#105028),.UNSPECIFIED.,.F.,.F.,(4,3,3,3,3,4),(-0.000437598556138437,
0.,0.00562170475741228,0.0114823251616098,0.0173413775097521,0.0231997078506926),
 .UNSPECIFIED.) ;
#1511 = B_SPLINE_CURVE_WITH_KNOTS('',3,(#105034,#105035,#105036,#105037,#105038,
#105039,#105040,#105041,#105042,#105043,#105044,#105045,#105046,#105047),
 .UNSPECIFIED.,.F.,.F.,(4,2,2,2,2,2,4),(-0.0559250143516994,-0.0556883945481287,
-0.0495906032010545,-0.0437546843045533,-0.0372885759093916,-0.0322854917720808,
-0.0278441972739919),.UNSPECIFIED.) ;
#1512 = B_SPLINE_CURVE_WITH_KNOTS('',3,(#105051,#105052,#105053,#105054,#105055,
#105056,#105057,#105058,#105059,#105060,#105061,#105062,#105063,#105064,
#105065,#105066),.UNSPECIFIED.,.F.,.F.,(4,3,3,3,3,4),(-0.000437598556144422,
0.,0.00562170475740183,0.0114823251615895,0.0173413775097444,0.0231997078506806),
 .UNSPECIFIED.) ;
#1513 = B_SPLINE_CURVE_WITH_KNOTS('',3,(#105073,#105074,#105075,#105076,#105077,
#105078,#105079,#105080,#105081,#105082,#105083,#105084,#105085,#105086),
 .UNSPECIFIED.,.F.,.F.,(4,2,2,2,2,2,4),(-0.0559250143435119,-0.0556883945403911,
-0.0495906031940201,-0.0437546842982849,-0.0372885759042276,-0.0322854917677294,
-0.0278441972703399),.UNSPECIFIED.) ;
#1514 = B_SPLINE_CURVE_WITH_KNOTS('',3,(#105090,#105091,#105092,#105093,#105094,
#105095,#105096,#105097,#105098,#105099,#105100,#105101,#105102,#105103,
#105104,#105105),.UNSPECIFIED.,.F.,.F.,(4,3,3,3,3,4),(-0.000437598556018984,
0.,0.00562170475658728,0.0114823251597353,0.0173413775068133,0.0231997078467154),
 .UNSPECIFIED.) ;
#1515 = B_SPLINE_CURVE_WITH_KNOTS('',3,(#105112,#105113,#105114,#105115,#105116,
#105117,#105118,#105119,#105120,#105121,#105122,#105123,#105124,#105125),
 .UNSPECIFIED.,.F.,.F.,(4,2,2,2,2,2,4),(-0.0559250143454541,-0.055688394541913,
-0.0495906031955341,-0.0437546842998321,-0.0372885759055476,-0.0322854917689083,
-0.0278441972713927),.UNSPECIFIED.) ;
#1516 = B_SPLINE_CURVE_WITH_KNOTS('',3,(#105129,#105130,#105131,#105132,#105133,
#105134,#105135,#105136,#105137,#105138,#105139,#105140,#105141,#105142,
#105143,#105144),.UNSPECIFIED.,.F.,.F.,(4,3,3,3,3,4),(-0.000437598556040506,
0.,0.00562170475667276,0.0114823251599514,0.0173413775071961,0.0231997078472556),
 .UNSPECIFIED.) ;
#1517 = B_SPLINE_CURVE_WITH_KNOTS('',3,(#105151,#105152,#105153,#105154,#105155,
#105156,#105157,#105158,#105159,#105160,#105161,#105162,#105163,#105164),
 .UNSPECIFIED.,.F.,.F.,(4,2,2,2,2,2,4),(-0.0559250143503411,-0.0556883945467744,
-0.0495906031998412,-0.0437546843035047,-0.0372885759085466,-0.0322854917713593,
-0.0278441972733858),.UNSPECIFIED.) ;
#1518 = B_SPLINE_CURVE_WITH_KNOTS('',3,(#105168,#105169,#105170,#105171,#105172,
#105173,#105174,#105175,#105176,#105177,#105178,#105179,#105180,#105181,
#105182,#105183),.UNSPECIFIED.,.F.,.F.,(4,3,3,3,3,4),(-0.00043759855609295,
0.,0.00562170475705494,0.0114823251608269,0.0173413775085459,0.0231997078490585),
 .UNSPECIFIED.) ;
#1519 = B_SPLINE_CURVE_WITH_KNOTS('',3,(#105190,#105191,#105192,#105193,#105194,
#105195,#105196,#105197,#105198,#105199,#105200,#105201,#105202,#105203),
 .UNSPECIFIED.,.F.,.F.,(4,2,2,2,2,2,4),(-0.0559250143576788,-0.0556883945534629,
-0.0495906032058708,-0.0437546843087237,-0.0372885759128067,-0.0322854917749087,
-0.027844197276348),.UNSPECIFIED.) ;
#1520 = B_SPLINE_CURVE_WITH_KNOTS('',3,(#105207,#105208,#105209,#105210,#105211,
#105212,#105213,#105214,#105215,#105216,#105217,#105218,#105219,#105220,
#105221,#105222),.UNSPECIFIED.,.F.,.F.,(4,3,3,3,3,4),(-0.000437598556265556,
0.,0.00562170475766576,0.0114823251621366,0.0173413775105401,0.0231997078517073),
 .UNSPECIFIED.) ;
#1521 = B_SPLINE_CURVE_WITH_KNOTS('',3,(#105229,#105230,#105231,#105232,#105233,
#105234,#105235,#105236,#105237,#105238,#105239,#105240,#105241,#105242),
 .UNSPECIFIED.,.F.,.F.,(4,2,2,2,2,2,4),(-0.0559250143546525,-0.0556883945504525,
-0.0495906032031384,-0.0437546843063546,-0.0372885759108327,-0.0322854917732639,
-0.0278441972749651),.UNSPECIFIED.) ;
#1522 = B_SPLINE_CURVE_WITH_KNOTS('',3,(#105246,#105247,#105248,#105249,#105250,
#105251,#105252,#105253,#105254,#105255,#105256,#105257,#105258,#105259,
#105260,#105261),.UNSPECIFIED.,.F.,.F.,(4,3,3,3,3,4),(-0.000437598556211791,
0.,0.00562170475765983,0.011482325162167,0.0173413775106296,0.0231997078518591),
 .UNSPECIFIED.) ;
#1523 = B_SPLINE_CURVE_WITH_KNOTS('',3,(#105268,#105269,#105270,#105271,#105272,
#105273,#105274,#105275,#105276,#105277,#105278,#105279,#105280,#105281),
 .UNSPECIFIED.,.F.,.F.,(4,2,2,2,2,2,4),(-0.0559250143563362,-0.055688394551709,
-0.0495906032045639,-0.0437546843078355,-0.0372885759121675,-0.0322854917744538,
-0.0278441972760254),.UNSPECIFIED.) ;
#1524 = B_SPLINE_CURVE_WITH_KNOTS('',3,(#105285,#105286,#105287,#105288,#105289,
#105290,#105291,#105292,#105293,#105294,#105295,#105296,#105297,#105298,
#105299,#105300),.UNSPECIFIED.,.F.,.F.,(4,3,3,3,3,4),(-0.000437598556225459,
0.,0.00562170475744369,0.0114823251616755,0.0173413775098568,0.0231997078508077),
 .UNSPECIFIED.) ;
#1525 = B_SPLINE_CURVE_WITH_KNOTS('',3,(#105307,#105308,#105309,#105310,#105311,
#105312,#105313,#105314,#105315,#105316,#105317,#105318,#105319,#105320),
 .UNSPECIFIED.,.F.,.F.,(4,2,2,2,2,2,4),(-0.0559250143492567,-0.0556883945456972,
-0.0495906031988905,-0.0437546843027083,-0.0372885759078583,-0.0322854917707879,
-0.0278441972729168),.UNSPECIFIED.) ;
#1526 = B_SPLINE_CURVE_WITH_KNOTS('',3,(#105324,#105325,#105326,#105327,#105328,
#105329,#105330,#105331,#105332,#105333,#105334,#105335,#105336,#105337,
#105338,#105339),.UNSPECIFIED.,.F.,.F.,(4,3,3,3,3,4),(-0.000437598556080345,
0.,0.00562170475697672,0.0114823251606002,0.0173413775081636,0.0231997078485257),
 .UNSPECIFIED.) ;
#1527 = B_SPLINE_CURVE_WITH_KNOTS('',3,(#105346,#105347,#105348,#105349,#105350,
#105351,#105352,#105353,#105354,#105355,#105356,#105357,#105358,#105359),
 .UNSPECIFIED.,.F.,.F.,(4,2,2,2,2,2,4),(-0.055925014349952,-0.0556883945463912,
-0.0495906031994983,-0.0437546843032064,-0.0372885759082967,-0.0322854917711481,
-0.0278441972731949),.UNSPECIFIED.) ;
#1528 = B_SPLINE_CURVE_WITH_KNOTS('',3,(#105363,#105364,#105365,#105366,#105367,
#105368,#105369,#105370,#105371,#105372,#105373,#105374,#105375,#105376,
#105377,#105378),.UNSPECIFIED.,.F.,.F.,(4,3,3,3,3,4),(-0.000437598556096392,
0.,0.005621704757061,0.0114823251608164,0.0173413775085336,0.0231997078490434),
 .UNSPECIFIED.) ;
#1529 = B_SPLINE_CURVE_WITH_KNOTS('',3,(#105473,#105474,#105475,#105476,#105477,
#105478,#105479,#105480,#105481,#105482,#105483,#105484,#105485,#105486,
#105487,#105488,#105489),.UNSPECIFIED.,.T.,.F.,(4,1,1,1,1,1,1,1,1,1,1,1,
1,1,4),(-1.37470975898194,-1.17832265055595,-0.981935542129957,-0.785548433703966,
-0.589161325277974,-0.392774216851983,-0.196387108425991,0.,0.196387108425991,
0.392774216851983,0.589161325277974,0.785548433703966,0.981935542129957,
1.17832265055595,1.37470975898194),.UNSPECIFIED.) ;
#1530 = B_SPLINE_CURVE_WITH_KNOTS('',3,(#105498,#105499,#105500,#105501,#105502,
#105503,#105504,#105505,#105506,#105507,#105508,#105509,#105510,#105511,
#105512,#105513,#105514),.UNSPECIFIED.,.T.,.F.,(4,1,1,1,1,1,1,1,1,1,1,1,
1,1,4),(-1.37470975898194,-1.17832265055595,-0.981935542129957,-0.785548433703966,
-0.589161325277974,-0.392774216851983,-0.196387108425991,0.,0.196387108425991,
0.392774216851983,0.589161325277974,0.785548433703966,0.981935542129957,
1.17832265055595,1.37470975898194),.UNSPECIFIED.) ;
#1531 = B_SPLINE_CURVE_WITH_KNOTS('',3,(#105607,#105608,#105609,#105610,#105611),
 .UNSPECIFIED.,.F.,.F.,(4,1,4),(-1.,-0.5,0.),.UNSPECIFIED.) ;
#1532 = B_SPLINE_CURVE_WITH_KNOTS('',3,(#105613,#105614,#105615,#105616,#105617,
#105618,#105619),.UNSPECIFIED.,.F.,.F.,(4,1,1,1,4),(-1.37470975898194,-1.17832265055595,
-0.981935542129957,-0.785548433703966,-0.687133244560913),.UNSPECIFIED.) ;
#1533 = B_SPLINE_CURVE_WITH_KNOTS('',3,(#105620,#105621,#105622,#105623,#105624,
#105625,#105626,#105627,#105628,#105629,#105630,#105631,#105632,#105633),
 .UNSPECIFIED.,.F.,.F.,(4,1,1,1,1,1,1,1,1,1,1,4),(-0.687133244560913,-0.589161325277974,
-0.392774216851983,-0.196387108425991,0.,0.196387108425991,0.392774216851983,
0.589161325277974,0.785548433703966,0.981935542129957,1.17832265055595,
1.37470975898194),.UNSPECIFIED.) ;
#1534 = B_SPLINE_CURVE_WITH_KNOTS('',3,(#105720,#105721,#105722,#105723,#105724),
 .UNSPECIFIED.,.F.,.F.,(4,1,4),(-1.,-0.5,0.),.UNSPECIFIED.) ;
#1535 = B_SPLINE_CURVE_WITH_KNOTS('',3,(#105726,#105727,#105728,#105729,#105730,
#105731,#105732),.UNSPECIFIED.,.F.,.F.,(4,1,1,1,4),(-1.37470975898194,-1.17832265055595,
-0.981935542129957,-0.785548433703966,-0.687210817221059),.UNSPECIFIED.) ;
#1536 = B_SPLINE_CURVE_WITH_KNOTS('',3,(#105733,#105734,#105735,#105736,#105737,
#105738,#105739,#105740,#105741,#105742,#105743,#105744,#105745,#105746),
 .UNSPECIFIED.,.F.,.F.,(4,1,1,1,1,1,1,1,1,1,1,4),(-0.687210817221059,-0.589161325277974,
-0.392774216851983,-0.196387108425991,0.,0.196387108425991,0.392774216851983,
0.589161325277974,0.785548433703966,0.981935542129957,1.17832265055595,
1.37470975898194),.UNSPECIFIED.) ;
#1537 = B_SPLINE_CURVE_WITH_KNOTS('',3,(#105752,#105753,#105754,#105755,#105756,
#105757,#105758,#105759,#105760,#105761,#105762,#105763,#105764,#105765),
 .UNSPECIFIED.,.F.,.F.,(4,2,2,2,2,2,4),(-0.0559250143496373,-0.0556883945460747,
-0.0495906031992305,-0.0437546843030053,-0.0372885759081072,-0.0322854917709823,
-0.0278441972730634),.UNSPECIFIED.) ;
#1538 = B_SPLINE_CURVE_WITH_KNOTS('',3,(#105768,#105769,#105770,#105771,#105772,
#105773,#105774,#105775,#105776,#105777,#105778,#105779,#105780,#105781),
 .UNSPECIFIED.,.F.,.F.,(4,2,2,2,2,2,4),(-0.000236619804093,0.,0.0060977913471935,
0.0119337102438738,0.018399818639261,0.0234029027767472,0.0278441972749678),
 .UNSPECIFIED.) ;
#1539 = B_SPLINE_CURVE_WITH_KNOTS('',3,(#105786,#105787,#105788,#105789,#105790,
#105791,#105792,#105793,#105794,#105795,#105796,#105797,#105798,#105799,
#105800,#105801),.UNSPECIFIED.,.F.,.F.,(4,3,3,3,3,4),(-0.000437598556087367,
0.,0.00562170475705654,0.0114823251607832,0.0173413775084489,0.0231997078489075),
 .UNSPECIFIED.) ;
#1540 = B_SPLINE_CURVE_WITH_KNOTS('',3,(#105807,#105808,#105809,#105810,#105811,
#105812,#105813,#105814,#105815,#105816,#105817,#105818,#105819,#105820,
#105821,#105822),.UNSPECIFIED.,.F.,.F.,(4,3,3,3,3,4),(-0.046837014255361,
-0.046399415699481,-0.0407777109422933,-0.0349170905383532,-0.0290580381904547,
-0.0231997078497599),.UNSPECIFIED.) ;
#1541 = B_SPLINE_CURVE_WITH_KNOTS('',3,(#105828,#105829,#105830,#105831,#105832,
#105833,#105834,#105835,#105836,#105837,#105838,#105839,#105840,#105841),
 .UNSPECIFIED.,.F.,.F.,(4,2,2,2,2,2,4),(-0.000236619803146698,0.,0.00609779134724104,
0.0119337102438844,0.0183998186389394,0.0234029027761802,0.0278441972742087),
 .UNSPECIFIED.) ;
#1542 = B_SPLINE_CURVE_WITH_KNOTS('',3,(#105847,#105848,#105849,#105850,#105851,
#105852,#105853,#105854,#105855,#105856,#105857,#105858,#105859,#105860),
 .UNSPECIFIED.,.F.,.F.,(4,2,2,2,2,2,4),(-0.0559250143496986,-0.0556883945465552,
-0.0495906031994403,-0.0437546843028884,-0.0372885759079096,-0.0322854917707418,
-0.0278441972727803),.UNSPECIFIED.) ;
#1543 = B_SPLINE_CURVE_WITH_KNOTS('',3,(#105866,#105867,#105868,#105869,#105870,
#105871,#105872,#105873,#105874,#105875,#105876,#105877,#105878,#105879,
#105880,#105881),.UNSPECIFIED.,.F.,.F.,(4,3,3,3,3,4),(-0.000437598556095027,
0.,0.00562170475708189,0.0114823251608833,0.0173413775086171,0.0231997078491342),
 .UNSPECIFIED.) ;
#1544 = B_SPLINE_CURVE_WITH_KNOTS('',3,(#105887,#105888,#105889,#105890,#105891,
#105892,#105893,#105894,#105895,#105896,#105897,#105898,#105899,#105900,
#105901,#105902),.UNSPECIFIED.,.F.,.F.,(4,3,3,3,3,4),(-0.0468370142541051,
-0.0463994156980201,-0.0407777109409428,-0.0349170905371886,-0.0290580381894966,
-0.0231997078490079),.UNSPECIFIED.) ;
#1545 = B_SPLINE_CURVE_WITH_KNOTS('',3,(#105908,#105909,#105910,#105911,#105912,
#105913,#105914,#105915,#105916,#105917,#105918,#105919,#105920,#105921),
 .UNSPECIFIED.,.F.,.F.,(4,2,2,2,2,2,4),(-0.000236619803558265,0.,0.00609779134685418,
0.0119337102431074,0.0183998186379772,0.023402902775095,0.0278441972730209),
 .UNSPECIFIED.) ;
#1546 = B_SPLINE_CURVE_WITH_KNOTS('',3,(#105927,#105928,#105929,#105930,#105931,
#105932,#105933,#105934,#105935,#105936,#105937,#105938,#105939,#105940),
 .UNSPECIFIED.,.F.,.F.,(4,2,2,2,2,2,4),(-0.0559250143504567,-0.0556883945473107,
-0.0495906032000867,-0.0437546843034773,-0.0372885759084374,-0.0322854917711889,
-0.0278441972731474),.UNSPECIFIED.) ;
#1547 = B_SPLINE_CURVE_WITH_KNOTS('',3,(#105946,#105947,#105948,#105949,#105950,
#105951,#105952,#105953,#105954,#105955,#105956,#105957,#105958,#105959,
#105960,#105961),.UNSPECIFIED.,.F.,.F.,(4,3,3,3,3,4),(-0.000437598556114517,
0.,0.00562170475723958,0.0114823251612343,0.0173413775091901,0.0231997078499022),
 .UNSPECIFIED.) ;
#1548 = B_SPLINE_CURVE_WITH_KNOTS('',3,(#105967,#105968,#105969,#105970,#105971,
#105972,#105973,#105974,#105975,#105976,#105977,#105978,#105979,#105980,
#105981,#105982),.UNSPECIFIED.,.F.,.F.,(4,3,3,3,3,4),(-0.0468370142517104,
-0.046399415695612,-0.0407777109388244,-0.034917090535398,-0.0290580381880315,
-0.0231997078478665),.UNSPECIFIED.) ;
#1549 = B_SPLINE_CURVE_WITH_KNOTS('',3,(#105988,#105989,#105990,#105991,#105992,
#105993,#105994,#105995,#105996,#105997,#105998,#105999,#106000,#106001),
 .UNSPECIFIED.,.F.,.F.,(4,2,2,2,2,2,4),(-0.000236619803559768,0.,0.00609779134686269,
0.0119337102430971,0.0183998186379832,0.0234029027750867,0.0278441972729811),
 .UNSPECIFIED.) ;
#1550 = B_SPLINE_CURVE_WITH_KNOTS('',3,(#106007,#106008,#106009,#106010,#106011,
#106012,#106013,#106014,#106015,#106016,#106017,#106018,#106019,#106020),
 .UNSPECIFIED.,.F.,.F.,(4,2,2,2,2,2,4),(-0.0559250143524368,-0.0556883945478243,
-0.0495906032010392,-0.0437546843047665,-0.0372885759096309,-0.0322854917723447,
-0.0278441972742818),.UNSPECIFIED.) ;
#1551 = B_SPLINE_CURVE_WITH_KNOTS('',3,(#106026,#106027,#106028,#106029,#106030,
#106031,#106032,#106033,#106034,#106035,#106036,#106037,#106038,#106039,
#106040,#106041),.UNSPECIFIED.,.F.,.F.,(4,3,3,3,3,4),(-0.000437598556131605,
0.,0.00562170475733242,0.0114823251614144,0.0173413775094361,0.0231997078502398),
 .UNSPECIFIED.) ;
#1552 = B_SPLINE_CURVE_WITH_KNOTS('',3,(#106047,#106048,#106049,#106050,#106051,
#106052,#106053,#106054,#106055,#106056,#106057,#106058,#106059,#106060,
#106061,#106062),.UNSPECIFIED.,.F.,.F.,(4,3,3,3,3,4),(-0.046837014258247,
-0.0463994157019922,-0.0407777109444557,-0.0349170905401249,-0.0290580381918459,
-0.0231997078507989),.UNSPECIFIED.) ;
#1553 = B_SPLINE_CURVE_WITH_KNOTS('',3,(#106068,#106069,#106070,#106071,#106072,
#106073,#106074,#106075,#106076,#106077,#106078,#106079,#106080,#106081),
 .UNSPECIFIED.,.F.,.F.,(4,2,2,2,2,2,4),(-0.000236619803154501,0.,0.00609779134749395,
0.0119337102444787,0.0183998186399401,0.0234029027774939,0.0278441972757804),
 .UNSPECIFIED.) ;
#1554 = B_SPLINE_CURVE_WITH_KNOTS('',3,(#106087,#106088,#106089,#106090,#106091,
#106092,#106093,#106094,#106095,#106096,#106097,#106098,#106099,#106100),
 .UNSPECIFIED.,.F.,.F.,(4,2,2,2,2,2,4),(-0.0559250143516698,-0.055688394548102,
-0.0495906032010132,-0.0437546843045191,-0.0372885759093257,-0.0322854917720022,
-0.0278441972739074),.UNSPECIFIED.) ;
#1555 = B_SPLINE_CURVE_WITH_KNOTS('',3,(#106106,#106107,#106108,#106109,#106110,
#106111,#106112,#106113,#106114,#106115,#106116,#106117,#106118,#106119,
#106120,#106121),.UNSPECIFIED.,.F.,.F.,(4,3,3,3,3,4),(-0.000437598556150276,
0.,0.00562170475744494,0.0114823251616921,0.0173413775098778,0.0231997078508276),
 .UNSPECIFIED.) ;
#1556 = B_SPLINE_CURVE_WITH_KNOTS('',3,(#106127,#106128,#106129,#106130,#106131,
#106132,#106133,#106134,#106135,#106136,#106137,#106138,#106139,#106140,
#106141,#106142),.UNSPECIFIED.,.F.,.F.,(4,3,3,3,3,4),(-0.0468370142569828,
-0.0463994157014635,-0.0407777109440522,-0.0349170905398014,-0.0290580381915951,
-0.0231997078506218),.UNSPECIFIED.) ;
#1557 = B_SPLINE_CURVE_WITH_KNOTS('',3,(#106148,#106149,#106150,#106151,#106152,
#106153,#106154,#106155,#106156,#106157,#106158,#106159,#106160,#106161),
 .UNSPECIFIED.,.F.,.F.,(4,2,2,2,2,2,4),(-0.000236619804616541,0.,0.00609779134700319,
0.0119337102434886,0.0183998186388943,0.0234029027763847,0.0278441972746185),
 .UNSPECIFIED.) ;
#1558 = B_SPLINE_CURVE_WITH_KNOTS('',3,(#106167,#106168,#106169,#106170,#106171,
#106172,#106173,#106174,#106175,#106176,#106177,#106178,#106179,#106180),
 .UNSPECIFIED.,.F.,.F.,(4,2,2,2,2,2,4),(-0.0559250143475551,-0.0556883945439973,
-0.049590603197355,-0.0437546843013896,-0.037288575906807,-0.0322854917699323,
-0.0278441972722247),.UNSPECIFIED.) ;
#1559 = B_SPLINE_CURVE_WITH_KNOTS('',3,(#106186,#106187,#106188,#106189,#106190,
#106191,#106192,#106193,#106194,#106195,#106196,#106197,#106198,#106199,
#106200,#106201),.UNSPECIFIED.,.F.,.F.,(4,3,3,3,3,4),(-0.000437598556056009,
0.,0.00562170475686937,0.0114823251603833,0.0173413775078316,0.0231997078480834),
 .UNSPECIFIED.) ;
#1560 = B_SPLINE_CURVE_WITH_KNOTS('',3,(#106207,#106208,#106209,#106210,#106211,
#106212,#106213,#106214,#106215,#106216,#106217,#106218,#106219,#106220,
#106221,#106222),.UNSPECIFIED.,.F.,.F.,(4,3,3,3,3,4),(-0.0468370142561097,
-0.0463994157004828,-0.0407777109431283,-0.034917090538975,-0.0290580381908889,
-0.0231997078500392),.UNSPECIFIED.) ;
#1561 = B_SPLINE_CURVE_WITH_KNOTS('',3,(#106228,#106229,#106230,#106231,#106232,
#106233,#106234,#106235,#106236,#106237,#106238,#106239,#106240,#106241),
 .UNSPECIFIED.,.F.,.F.,(4,2,2,2,2,2,4),(-0.000236619804206572,0.,0.00609779134739848,
0.0119337102443252,0.0183998186399927,0.023402902777706,0.0278441972760964),
 .UNSPECIFIED.) ;
#1562 = B_SPLINE_CURVE_WITH_KNOTS('',3,(#106247,#106248,#106249,#106250,#106251,
#106252,#106253,#106254,#106255,#106256,#106257,#106258,#106259,#106260),
 .UNSPECIFIED.,.F.,.F.,(4,2,2,2,2,2,4),(-0.0559250143503367,-0.0556883945467745,
-0.0495906031998185,-0.0437546843034772,-0.0372885759085197,-0.0322854917713411,
-0.0278441972733722),.UNSPECIFIED.) ;
#1563 = B_SPLINE_CURVE_WITH_KNOTS('',3,(#106266,#106267,#106268,#106269,#106270,
#106271,#106272,#106273,#106274,#106275,#106276,#106277,#106278,#106279,
#106280,#106281),.UNSPECIFIED.,.F.,.F.,(4,3,3,3,3,4),(-0.000437598556095159,
0.,0.00562170475710087,0.0114823251609001,0.0173413775086179,0.0231997078491324),
 .UNSPECIFIED.) ;
#1564 = B_SPLINE_CURVE_WITH_KNOTS('',3,(#106287,#106288,#106289,#106290,#106291,
#106292,#106293,#106294,#106295,#106296,#106297,#106298,#106299,#106300,
#106301,#106302),.UNSPECIFIED.,.F.,.F.,(4,3,3,3,3,4),(-0.0468370142542446,
-0.0463994156981747,-0.0407777109410807,-0.0349170905373078,-0.0290580381895938,
-0.0231997078490836),.UNSPECIFIED.) ;
#1565 = B_SPLINE_CURVE_WITH_KNOTS('',3,(#106308,#106309,#106310,#106311,#106312,
#106313,#106314,#106315,#106316,#106317,#106318,#106319,#106320,#106321),
 .UNSPECIFIED.,.F.,.F.,(4,2,2,2,2,2,4),(-0.000236619803563725,0.,0.00609779134693619,
0.0119337102432759,0.0183998186382373,0.0234029027754271,0.027844197273412),
 .UNSPECIFIED.) ;
#1566 = B_SPLINE_CURVE_WITH_KNOTS('',3,(#106327,#106328,#106329,#106330,#106331,
#106332,#106333,#106334,#106335,#106336,#106337,#106338,#106339,#106340),
 .UNSPECIFIED.,.F.,.F.,(4,2,2,2,2,2,4),(-0.0559250143564113,-0.0556883945522011,
-0.0495906032047249,-0.0437546843077159,-0.0372885759119513,-0.0322854917741759,
-0.0278441972757216),.UNSPECIFIED.) ;
#1567 = B_SPLINE_CURVE_WITH_KNOTS('',3,(#106346,#106347,#106348,#106349,#106350,
#106351,#106352,#106353,#106354,#106355,#106356,#106357,#106358,#106359,
#106360,#106361),.UNSPECIFIED.,.F.,.F.,(4,3,3,3,3,4),(-0.000437598556252948,
0.,0.00562170475756358,0.0114823251619473,0.0173413775102792,0.023199707851373),
 .UNSPECIFIED.) ;
#1568 = B_SPLINE_CURVE_WITH_KNOTS('',3,(#106367,#106368,#106369,#106370,#106371,
#106372,#106373,#106374,#106375,#106376,#106377,#106378,#106379,#106380,
#106381,#106382),.UNSPECIFIED.,.F.,.F.,(4,3,3,3,3,4),(-0.0468370142435449,
-0.0463994156880452,-0.0407777109322271,-0.0349170905298351,-0.0290580381834779,
-0.0231997078443083),.UNSPECIFIED.) ;
#1569 = B_SPLINE_CURVE_WITH_KNOTS('',3,(#106388,#106389,#106390,#106391,#106392,
#106393,#106394,#106395,#106396,#106397,#106398,#106399,#106400,#106401),
 .UNSPECIFIED.,.F.,.F.,(4,2,2,2,2,2,4),(-0.000236619803545348,0.,0.00609779134648851,
0.0119337102422953,0.0183998186366923,0.0234029027734222,0.0278441972710204),
 .UNSPECIFIED.) ;
#1570 = B_SPLINE_CURVE_WITH_KNOTS('',3,(#106407,#106408,#106409,#106410,#106411,
#106412,#106413,#106414,#106415,#106416,#106417,#106418,#106419,#106420),
 .UNSPECIFIED.,.F.,.F.,(4,2,2,2,2,2,4),(-0.0559250143495547,-0.0556883945459923,
-0.0495906031991245,-0.0437546843029074,-0.0372885759080479,-0.0322854917709575,
-0.027844197273083),.UNSPECIFIED.) ;
#1571 = B_SPLINE_CURVE_WITH_KNOTS('',3,(#106426,#106427,#106428,#106429,#106430,
#106431,#106432,#106433,#106434,#106435,#106436,#106437,#106438,#106439,
#106440,#106441),.UNSPECIFIED.,.F.,.F.,(4,3,3,3,3,4),(-0.000437598556080383,
0.,0.00562170475701161,0.0114823251606741,0.0173413775082905,0.0231997078487108),
 .UNSPECIFIED.) ;
#1572 = B_SPLINE_CURVE_WITH_KNOTS('',3,(#106447,#106448,#106449,#106450,#106451,
#106452,#106453,#106454,#106455,#106456,#106457,#106458,#106459,#106460,
#106461,#106462),.UNSPECIFIED.,.F.,.F.,(4,3,3,3,3,4),(-0.0468370142410635,
-0.046399415685515,-0.0407777109299654,-0.0349170905279156,-0.0290580381819153,
-0.0231997078430871),.UNSPECIFIED.) ;
#1573 = B_SPLINE_CURVE_WITH_KNOTS('',3,(#106468,#106469,#106470,#106471,#106472,
#106473,#106474,#106475,#106476,#106477,#106478,#106479,#106480,#106481),
 .UNSPECIFIED.,.F.,.F.,(4,2,2,2,2,2,4),(-0.000236619803553881,0.,0.00609779134648714,
0.0119337102422593,0.0183998186365944,0.0234029027733178,0.0278441972709114),
 .UNSPECIFIED.) ;
#1574 = B_SPLINE_CURVE_WITH_KNOTS('',3,(#106487,#106488,#106489,#106490,#106491,
#106492,#106493,#106494,#106495,#106496,#106497,#106498,#106499,#106500),
 .UNSPECIFIED.,.F.,.F.,(4,2,2,2,2,2,4),(-0.0559250143458346,-0.0556883945427038,
-0.0495906031960554,-0.043754684300065,-0.0372885759056522,-0.0322854917688908,
-0.0278441972712752),.UNSPECIFIED.) ;
#1575 = B_SPLINE_CURVE_WITH_KNOTS('',3,(#106506,#106507,#106508,#106509,#106510,
#106511,#106512,#106513,#106514,#106515,#106516,#106517,#106518,#106519,
#106520,#106521),.UNSPECIFIED.,.F.,.F.,(4,3,3,3,3,4),(-0.000437598556037642,
0.,0.00562170475676515,0.0114823251601515,0.0173413775075229,0.0231997078477011),
 .UNSPECIFIED.) ;
#1576 = B_SPLINE_CURVE_WITH_KNOTS('',3,(#106527,#106528,#106529,#106530,#106531,
#106532,#106533,#106534,#106535,#106536,#106537,#106538,#106539,#106540,
#106541,#106542),.UNSPECIFIED.,.F.,.F.,(4,3,3,3,3,4),(-0.0468370142550307,
-0.046399415699245,-0.0407777109420836,-0.0349170905381485,-0.0290580381902572,
-0.023199707849583),.UNSPECIFIED.) ;
#1577 = B_SPLINE_CURVE_WITH_KNOTS('',3,(#106548,#106549,#106550,#106551,#106552,
#106553,#106554,#106555,#106556,#106557,#106558,#106559,#106560,#106561),
 .UNSPECIFIED.,.F.,.F.,(4,2,2,2,2,2,4),(-0.000236619803565948,0.,0.00609779134700125,
0.0119337102434307,0.0183998186384978,0.0234029027757452,0.0278441972737845),
 .UNSPECIFIED.) ;
#1578 = B_SPLINE_CURVE_WITH_KNOTS('',3,(#106567,#106568,#106569,#106570,#106571,
#106572,#106573,#106574,#106575,#106576,#106577,#106578,#106579,#106580),
 .UNSPECIFIED.,.F.,.F.,(4,2,2,2,2,2,4),(-0.0559250143492506,-0.0556883945457476,
-0.049590603198939,-0.0437546843027145,-0.0372885759078682,-0.032285491770796,
-0.0278441972729179),.UNSPECIFIED.) ;
#1579 = B_SPLINE_CURVE_WITH_KNOTS('',3,(#106587,#106588,#106589,#106590,#106591,
#106592,#106593,#106594,#106595,#106596,#106597,#106598,#106599,#106600,
#106601,#106602),.UNSPECIFIED.,.F.,.F.,(4,3,3,3,3,4),(-0.000437598556107252,
0.,0.00562170475708925,0.0114823251608564,0.0173413775085622,0.0231997078490661),
 .UNSPECIFIED.) ;
#1580 = B_SPLINE_CURVE_WITH_KNOTS('',3,(#106608,#106609,#106610,#106611,#106612,
#106613,#106614,#106615,#106616,#106617,#106618,#106619,#106620,#106621,
#106622,#106623),.UNSPECIFIED.,.F.,.F.,(4,3,3,3,3,4),(-0.0468370142553995,
-0.0463994157003126,-0.0407777109430307,-0.0349170905389541,-0.0290580381909493,
-0.0231997078501516),.UNSPECIFIED.) ;
#1581 = B_SPLINE_CURVE_WITH_KNOTS('',3,(#106629,#106630,#106631,#106632,#106633,
#106634,#106635,#106636,#106637,#106638,#106639,#106640,#106641,#106642),
 .UNSPECIFIED.,.F.,.F.,(4,2,2,2,2,2,4),(-0.000236619803559952,0.,0.00609779134694098,
0.0119337102432763,0.0183998186382272,0.0234029027754186,0.0278441972733939),
 .UNSPECIFIED.) ;
#1582 = B_SPLINE_CURVE_WITH_KNOTS('',3,(#106648,#106649,#106650,#106651,#106652,
#106653,#106654,#106655,#106656,#106657,#106658,#106659,#106660,#106661),
 .UNSPECIFIED.,.F.,.F.,(4,2,2,2,2,2,4),(-0.0559250143507825,-0.0556883945467992,
-0.0495906032001226,-0.043754684304009,-0.0372885759090493,-0.032285491771857,
-0.0278441972738728),.UNSPECIFIED.) ;
#1583 = B_SPLINE_CURVE_WITH_KNOTS('',3,(#106667,#106668,#106669,#106670,#106671,
#106672,#106673,#106674,#106675,#106676,#106677,#106678,#106679,#106680,
#106681,#106682),.UNSPECIFIED.,.F.,.F.,(4,3,3,3,3,4),(-0.000437598556095639,
0.,0.00562170475706734,0.0114823251608502,0.0173413775085488,0.0231997078490271),
 .UNSPECIFIED.) ;
#1584 = B_SPLINE_CURVE_WITH_KNOTS('',3,(#106688,#106689,#106690,#106691,#106692,
#106693,#106694,#106695,#106696,#106697,#106698,#106699,#106700,#106701,
#106702,#106703),.UNSPECIFIED.,.F.,.F.,(4,3,3,3,3,4),(-0.0468370142543074,
-0.0463994156982126,-0.0407777109411238,-0.0349170905373201,-0.0290580381896051,
-0.0231997078491063),.UNSPECIFIED.) ;
#1585 = B_SPLINE_CURVE_WITH_KNOTS('',3,(#106709,#106710,#106711,#106712,#106713,
#106714,#106715,#106716,#106717,#106718,#106719,#106720,#106721,#106722),
 .UNSPECIFIED.,.F.,.F.,(4,2,2,2,2,2,4),(-0.000236619803981649,0.,0.00609779134664719,
0.0119337102427236,0.0183998186376455,0.0234029027747974,0.0278441972727449),
 .UNSPECIFIED.) ;
#1586 = B_SPLINE_CURVE_WITH_KNOTS('',3,(#106728,#106729,#106730,#106731,#106732,
#106733,#106734,#106735,#106736,#106737,#106738,#106739,#106740,#106741),
 .UNSPECIFIED.,.F.,.F.,(4,2,2,2,2,2,4),(-0.055925014352087,-0.0556883945480977,
-0.0495906032012405,-0.0437546843049561,-0.0372885759098064,-0.0322854917724869,
-0.0278441972743996),.UNSPECIFIED.) ;
#1587 = B_SPLINE_CURVE_WITH_KNOTS('',3,(#106747,#106748,#106749,#106750,#106751,
#106752,#106753,#106754,#106755,#106756,#106757,#106758,#106759,#106760,
#106761,#106762),.UNSPECIFIED.,.F.,.F.,(4,3,3,3,3,4),(-0.000437598556128711,
0.,0.00562170475726701,0.0114823251612751,0.0173413775092439,0.0231997078500064),
 .UNSPECIFIED.) ;
#1588 = B_SPLINE_CURVE_WITH_KNOTS('',3,(#106768,#106769,#106770,#106771,#106772,
#106773,#106774,#106775,#106776,#106777,#106778,#106779,#106780,#106781,
#106782,#106783),.UNSPECIFIED.,.F.,.F.,(4,3,3,3,3,4),(-0.0468370142525421,
-0.046399415696666,-0.0407777109397685,-0.0349170905362003,-0.029058038188693,
-0.0231997078483865),.UNSPECIFIED.) ;
#1589 = B_SPLINE_CURVE_WITH_KNOTS('',3,(#106789,#106790,#106791,#106792,#106793,
#106794,#106795,#106796,#106797,#106798,#106799,#106800,#106801,#106802),
 .UNSPECIFIED.,.F.,.F.,(4,2,2,2,2,2,4),(-0.000236619803982414,0.,0.00609779134661,
0.0119337102426289,0.0183998186375097,0.0234029027746178,0.0278441972725225),
 .UNSPECIFIED.) ;
#1590 = B_SPLINE_CURVE_WITH_KNOTS('',3,(#106808,#106809,#106810,#106811,#106812,
#106813,#106814,#106815,#106816,#106817,#106818,#106819,#106820,#106821),
 .UNSPECIFIED.,.F.,.F.,(4,2,2,2,2,2,4),(-0.0559250143493171,-0.0556883945461739,
-0.0495906031990541,-0.0437546843026118,-0.037288575907723,-0.0322854917706097,
-0.0278441972727174),.UNSPECIFIED.) ;
#1591 = B_SPLINE_CURVE_WITH_KNOTS('',3,(#106827,#106828,#106829,#106830,#106831,
#106832,#106833,#106834,#106835,#106836,#106837,#106838,#106839,#106840,
#106841,#106842),.UNSPECIFIED.,.F.,.F.,(4,3,3,3,3,4),(-0.000437598556087196,
0.,0.00562170475699019,0.0114823251606472,0.0173413775082489,0.0231997078486377),
 .UNSPECIFIED.) ;
#1592 = B_SPLINE_CURVE_WITH_KNOTS('',3,(#106848,#106849,#106850,#106851,#106852,
#106853,#106854,#106855,#106856,#106857,#106858,#106859,#106860,#106861,
#106862,#106863),.UNSPECIFIED.,.F.,.F.,(4,3,3,3,3,4),(-0.0468370142500863,
-0.0463994156945211,-0.0407777109379294,-0.0349170905346585,-0.0290580381874365,
-0.0231997078474141),.UNSPECIFIED.) ;
#1593 = B_SPLINE_CURVE_WITH_KNOTS('',3,(#106869,#106870,#106871,#106872,#106873,
#106874,#106875,#106876,#106877,#106878,#106879,#106880,#106881,#106882),
 .UNSPECIFIED.,.F.,.F.,(4,2,2,2,2,2,4),(-0.000236619803560014,0.,0.00609779134678491,
0.0119337102429536,0.0183998186377476,0.0234029027747679,0.0278441972725981),
 .UNSPECIFIED.) ;
#1594 = B_SPLINE_CURVE_WITH_KNOTS('',3,(#106888,#106889,#106890,#106891,#106892,
#106893,#106894,#106895,#106896,#106897,#106898,#106899,#106900,#106901),
 .UNSPECIFIED.,.F.,.F.,(4,2,2,2,2,2,4),(-0.0559250143548778,-0.0556883945506748,
-0.0495906032033264,-0.0437546843064839,-0.0372885759109464,-0.0322854917733345,
-0.0278441972750097),.UNSPECIFIED.) ;
#1595 = B_SPLINE_CURVE_WITH_KNOTS('',3,(#106907,#106908,#106909,#106910,#106911,
#106912,#106913,#106914,#106915,#106916,#106917,#106918,#106919,#106920,
#106921,#106922),.UNSPECIFIED.,.F.,.F.,(4,3,3,3,3,4),(-0.000437598556223204,
0.,0.00562170475783914,0.0114823251625445,0.0173413775111918,0.0231997078526027),
 .UNSPECIFIED.) ;
#1596 = B_SPLINE_CURVE_WITH_KNOTS('',3,(#106928,#106929,#106930,#106931,#106932,
#106933,#106934,#106935,#106936,#106937,#106938,#106939,#106940,#106941,
#106942,#106943),.UNSPECIFIED.,.F.,.F.,(4,3,3,3,3,4),(-0.0468370142563843,
-0.046399415700489,-0.0407777109431322,-0.0349170905389995,-0.0290580381909307,
-0.0231997078501088),.UNSPECIFIED.) ;
#1597 = B_SPLINE_CURVE_WITH_KNOTS('',3,(#106949,#106950,#106951,#106952,#106953,
#106954,#106955,#106956,#106957,#106958,#106959,#106960,#106961,#106962),
 .UNSPECIFIED.,.F.,.F.,(4,2,2,2,2,2,4),(-0.000236619804200277,0.,0.00609779134716414,
0.0119337102438048,0.0183998186391783,0.0234029027766296,0.0278441972748296),
 .UNSPECIFIED.) ;
#1598 = B_SPLINE_CURVE_WITH_KNOTS('',3,(#106968,#106969,#106970,#106971,#106972,
#106973,#106974,#106975,#106976,#106977,#106978,#106979,#106980,#106981),
 .UNSPECIFIED.,.F.,.F.,(4,2,2,2,2,2,4),(-0.0559250143496621,-0.0556883945461033,
-0.0495906031992651,-0.0437546843029983,-0.0372885759081094,-0.032285491771005,
-0.02784419727311),.UNSPECIFIED.) ;
#1599 = B_SPLINE_CURVE_WITH_KNOTS('',3,(#106987,#106988,#106989,#106990,#106991,
#106992,#106993,#106994,#106995,#106996,#106997,#106998,#106999,#107000,
#107001,#107002),.UNSPECIFIED.,.F.,.F.,(4,3,3,3,3,4),(-0.000437598556084584,
0.,0.00562170475697965,0.0114823251606079,0.0173413775081775,0.0231997078485472),
 .UNSPECIFIED.) ;
#1600 = B_SPLINE_CURVE_WITH_KNOTS('',3,(#107008,#107009,#107010,#107011,#107012,
#107013,#107014,#107015,#107016,#107017,#107018,#107019,#107020,#107021,
#107022,#107023),.UNSPECIFIED.,.F.,.F.,(4,3,3,3,3,4),(-0.0468370142549382,
-0.0463994156994604,-0.0407777109422707,-0.0349170905383382,-0.0290580381904463,
-0.023199707849757),.UNSPECIFIED.) ;
#1601 = B_SPLINE_CURVE_WITH_KNOTS('',3,(#107029,#107030,#107031,#107032,#107033,
#107034,#107035,#107036,#107037,#107038,#107039,#107040,#107041,#107042),
 .UNSPECIFIED.,.F.,.F.,(4,2,2,2,2,2,4),(-0.000236619803568316,0.,0.00609779134701837,
0.0119337102434465,0.0183998186385035,0.0234029027757473,0.0278441972737745),
 .UNSPECIFIED.) ;
#1602 = B_SPLINE_CURVE_WITH_KNOTS('',3,(#107048,#107049,#107050,#107051,#107052,
#107053,#107054,#107055,#107056,#107057,#107058,#107059,#107060,#107061),
 .UNSPECIFIED.,.F.,.F.,(4,2,2,2,2,2,4),(-0.0559250143499934,-0.0556883945464304,
-0.0495906031995064,-0.0437546843032007,-0.037288575908277,-0.032285491771123,
-0.0278441972731808),.UNSPECIFIED.) ;
#1603 = B_SPLINE_CURVE_WITH_KNOTS('',3,(#107067,#107068,#107069,#107070,#107071,
#107072,#107073,#107074,#107075,#107076,#107077,#107078,#107079,#107080,
#107081,#107082),.UNSPECIFIED.,.F.,.F.,(4,3,3,3,3,4),(-0.000437598556092419,
0.,0.00562170475702671,0.0114823251607112,0.0173413775083605,0.0231997078487915),
 .UNSPECIFIED.) ;
#1604 = B_SPLINE_CURVE_WITH_KNOTS('',3,(#107088,#107089,#107090,#107091,#107092,
#107093,#107094,#107095,#107096,#107097,#107098,#107099,#107100,#107101,
#107102,#107103),.UNSPECIFIED.,.F.,.F.,(4,3,3,3,3,4),(-0.0468370142548351,
-0.0463994156987323,-0.0407777109416122,-0.0349170905377609,-0.0290580381899607,
-0.0231997078493697),.UNSPECIFIED.) ;
#1605 = B_SPLINE_CURVE_WITH_KNOTS('',3,(#107109,#107110,#107111,#107112,#107113,
#107114,#107115,#107116,#107117,#107118,#107119,#107120,#107121,#107122),
 .UNSPECIFIED.,.F.,.F.,(4,2,2,2,2,2,4),(-0.000236619803562033,0.,0.00609779134691358,
0.0119337102432247,0.0183998186381566,0.0234029027753094,0.027844197273255),
 .UNSPECIFIED.) ;
#1606 = B_SPLINE_CURVE_WITH_KNOTS('',3,(#107128,#107129,#107130,#107131,#107132,
#107133,#107134,#107135,#107136,#107137,#107138,#107139,#107140,#107141),
 .UNSPECIFIED.,.F.,.F.,(4,2,2,2,2,2,4),(-0.0559250143503813,-0.0556883945472345,
-0.0495906032000065,-0.0437546843033907,-0.0372885759083472,-0.0322854917711086,
-0.027844197273083),.UNSPECIFIED.) ;
#1607 = B_SPLINE_CURVE_WITH_KNOTS('',3,(#107147,#107148,#107149,#107150,#107151,
#107152,#107153,#107154,#107155,#107156,#107157,#107158,#107159,#107160,
#107161,#107162),.UNSPECIFIED.,.F.,.F.,(4,3,3,3,3,4),(-0.000437598556129241,
0.,0.00562170475730571,0.0114823251613513,0.0173413775093445,0.0231997078501172),
 .UNSPECIFIED.) ;
#1608 = B_SPLINE_CURVE_WITH_KNOTS('',3,(#107168,#107169,#107170,#107171,#107172,
#107173,#107174,#107175,#107176,#107177,#107178,#107179,#107180,#107181,
#107182,#107183),.UNSPECIFIED.,.F.,.F.,(4,3,3,3,3,4),(-0.0468370142515845,
-0.0463994156955989,-0.0407777109388572,-0.0349170905354382,-0.0290580381880585,
-0.0231997078478789),.UNSPECIFIED.) ;
#1609 = B_SPLINE_CURVE_WITH_KNOTS('',3,(#107189,#107190,#107191,#107192,#107193,
#107194,#107195,#107196,#107197,#107198,#107199,#107200,#107201,#107202),
 .UNSPECIFIED.,.F.,.F.,(4,2,2,2,2,2,4),(-0.000236619803559663,0.,0.0060977913468164,
0.0119337102430072,0.0183998186378663,0.0234029027749556,0.0278441972728503),
 .UNSPECIFIED.) ;
#1610 = B_SPLINE_CURVE_WITH_KNOTS('',3,(#107208,#107209,#107210,#107211,#107212,
#107213,#107214,#107215,#107216,#107217,#107218,#107219,#107220,#107221),
 .UNSPECIFIED.,.F.,.F.,(4,2,2,2,2,2,4),(-0.0559250143533661,-0.0556883945491649,
-0.0495906032019838,-0.0437546843053393,-0.0372885759099808,-0.0322854917725361,
-0.0278441972743507),.UNSPECIFIED.) ;
#1611 = B_SPLINE_CURVE_WITH_KNOTS('',3,(#107227,#107228,#107229,#107230,#107231,
#107232,#107233,#107234,#107235,#107236,#107237,#107238,#107239,#107240,
#107241,#107242),.UNSPECIFIED.,.F.,.F.,(4,3,3,3,3,4),(-0.00043759855615984,
0.,0.00562170475737693,0.011482325161534,0.017341377509665,0.0231997078505602),
 .UNSPECIFIED.) ;
#1612 = B_SPLINE_CURVE_WITH_KNOTS('',3,(#107248,#107249,#107250,#107251,#107252,
#107253,#107254,#107255,#107256,#107257,#107258,#107259,#107260,#107261,
#107262,#107263),.UNSPECIFIED.,.F.,.F.,(4,3,3,3,3,4),(-0.0468370142504407,
-0.0463994156944377,-0.0407777109378315,-0.0349170905345851,-0.0290580381873817,
-0.0231997078473671),.UNSPECIFIED.) ;
#1613 = B_SPLINE_CURVE_WITH_KNOTS('',3,(#107269,#107270,#107271,#107272,#107273,
#107274,#107275,#107276,#107277,#107278,#107279,#107280,#107281,#107282),
 .UNSPECIFIED.,.F.,.F.,(4,2,2,2,2,2,4),(-0.000236619803559426,0.,0.00609779134674399,
0.0119337102428204,0.0183998186375428,0.0234029027745216,0.0278441972723019),
 .UNSPECIFIED.) ;
#1614 = B_SPLINE_CURVE_WITH_KNOTS('',3,(#107288,#107289,#107290,#107291,#107292,
#107293,#107294,#107295,#107296,#107297,#107298,#107299,#107300,#107301),
 .UNSPECIFIED.,.F.,.F.,(4,2,2,2,2,2,4),(-0.0559250143520313,-0.0556883945484605,
-0.0495906032013131,-0.0437546843047777,-0.037288575909542,-0.0322854917721873,
-0.0278441972740755),.UNSPECIFIED.) ;
#1615 = B_SPLINE_CURVE_WITH_KNOTS('',3,(#107307,#107308,#107309,#107310,#107311,
#107312,#107313,#107314,#107315,#107316,#107317,#107318,#107319,#107320,
#107321,#107322),.UNSPECIFIED.,.F.,.F.,(4,3,3,3,3,4),(-0.000437598556142791,
0.,0.00562170475737048,0.011482325161532,0.0173413775096432,0.0231997078505159),
 .UNSPECIFIED.) ;
#1616 = B_SPLINE_CURVE_WITH_KNOTS('',3,(#107328,#107329,#107330,#107331,#107332,
#107333,#107334,#107335,#107336,#107337,#107338,#107339,#107340,#107341,
#107342,#107343),.UNSPECIFIED.,.F.,.F.,(4,3,3,3,3,4),(-0.046837014256793,
-0.0463994157012118,-0.0407777109438107,-0.0349170905396121,-0.0290580381914533,
-0.0231997078505249),.UNSPECIFIED.) ;
#1617 = B_SPLINE_CURVE_WITH_KNOTS('',3,(#107759,#107760,#107761,#107762,#107763,
#107764,#107765,#107766,#107767,#107768,#107769,#107770,#107771,#107772),
 .UNSPECIFIED.,.F.,.F.,(4,2,2,2,2,2,4),(-0.0559250143525619,-0.0556883945479474,
-0.0495906032011524,-0.0437546843048812,-0.037288575909754,-0.0322854917724513,
-0.027844197274366),.UNSPECIFIED.) ;
#1618 = B_SPLINE_CURVE_WITH_KNOTS('',3,(#107775,#107776,#107777,#107778,#107779,
#107780,#107781,#107782,#107783,#107784,#107785,#107786,#107787,#107788),
 .UNSPECIFIED.,.F.,.F.,(4,2,2,2,2,2,4),(-0.000236619803144863,0.,0.00609779134711087,
0.0119337102436339,0.0183998186386153,0.0234029027758149,0.0278441972738027),
 .UNSPECIFIED.) ;
#1619 = B_SPLINE_CURVE_WITH_KNOTS('',3,(#107791,#107792,#107793,#107794,#107795,
#107796,#107797,#107798,#107799,#107800,#107801,#107802,#107803,#107804,
#107805,#107806),.UNSPECIFIED.,.F.,.F.,(4,3,3,3,3,4),(-0.000437598556136612,
0.,0.00562170475739987,0.0114823251615695,0.0173413775096577,0.0231997078505359),
 .UNSPECIFIED.) ;
#1620 = B_SPLINE_CURVE_WITH_KNOTS('',3,(#107811,#107812,#107813,#107814,#107815,
#107816,#107817,#107818,#107819,#107820,#107821,#107822,#107823,#107824,
#107825,#107826),.UNSPECIFIED.,.F.,.F.,(4,3,3,3,3,4),(0.,0.00585824217054478,
0.0117172063374487,0.0175777385368331,0.0231993586852603,0.0236369506553383),
 .UNSPECIFIED.) ;
#1621 = B_SPLINE_CURVE_WITH_KNOTS('',3,(#107828,#107829,#107830,#107831,#107832,
#107833,#107834,#107835,#107836,#107837,#107838,#107839,#107840,#107841),
 .UNSPECIFIED.,.F.,.F.,(4,2,2,2,2,2,4),(-0.000236619803563006,0.,0.00609779134689459,
0.0119337102432047,0.0183998186381472,0.0234029027752928,0.027844197273235),
 .UNSPECIFIED.) ;
#1622 = B_SPLINE_CURVE_WITH_KNOTS('',3,(#107844,#107845,#107846,#107847,#107848,
#107849,#107850,#107851,#107852,#107853,#107854,#107855,#107856,#107857,
#107858,#107859),.UNSPECIFIED.,.F.,.F.,(4,3,3,3,3,4),(0.,0.00585824217054169,
0.0117172063374197,0.0175777385367584,0.0231993586851914,0.0236369506552836),
 .UNSPECIFIED.) ;
#1623 = B_SPLINE_CURVE_WITH_KNOTS('',3,(#107861,#107862,#107863,#107864,#107865,
#107866,#107867,#107868,#107869,#107870,#107871,#107872,#107873,#107874),
 .UNSPECIFIED.,.F.,.F.,(4,2,2,2,2,2,4),(-0.055925014352618,-0.0556883945495578,
-0.049590603202043,-0.0437546843051378,-0.0372885759097438,-0.032285491772261,
-0.0278441972740487),.UNSPECIFIED.) ;
#1624 = B_SPLINE_CURVE_WITH_KNOTS('',3,(#107876,#107877,#107878,#107879,#107880,
#107881,#107882,#107883,#107884,#107885,#107886,#107887,#107888,#107889,
#107890,#107891),.UNSPECIFIED.,.F.,.F.,(4,3,3,3,3,4),(-0.000437598556173687,
0.,0.00562170475743059,0.0114823251616519,0.0173413775098334,0.0231997078507748),
 .UNSPECIFIED.) ;
#1625 = B_SPLINE_CURVE_WITH_KNOTS('',3,(#107896,#107897,#107898,#107899,#107900,
#107901,#107902,#107903,#107904,#107905,#107906,#107907,#107908,#107909,
#107910,#107911),.UNSPECIFIED.,.F.,.F.,(4,3,3,3,3,4),(0.,0.0058582421705496,
0.0117172063374621,0.01757773853685,0.0231993586852295,0.0236369506553315),
 .UNSPECIFIED.) ;
#1626 = B_SPLINE_CURVE_WITH_KNOTS('',3,(#107912,#107913,#107914,#107915,#107916,
#107917,#107918,#107919,#107920,#107921,#107922,#107923,#107924,#107925),
 .UNSPECIFIED.,.F.,.F.,(4,2,2,2,2,2,4),(-0.000236619803562956,0.,0.00609779134697842,
0.0119337102433575,0.0183998186383507,0.0234029027755715,0.027844197273593),
 .UNSPECIFIED.) ;
#1627 = B_SPLINE_CURVE_WITH_KNOTS('',3,(#107927,#107928,#107929,#107930,#107931,
#107932,#107933,#107934,#107935,#107936,#107937,#107938,#107939,#107940),
 .UNSPECIFIED.,.F.,.F.,(4,2,2,2,2,2,4),(-0.00023661980356627,0.,0.0060977913470113,
0.0119337102434447,0.0183998186385308,0.0234029027758003,0.027844197273845),
 .UNSPECIFIED.) ;
#1628 = B_SPLINE_CURVE_WITH_KNOTS('',3,(#107941,#107942,#107943,#107944,#107945,
#107946,#107947,#107948,#107949,#107950,#107951,#107952,#107953,#107954,
#107955,#107956),.UNSPECIFIED.,.F.,.F.,(4,3,3,3,3,4),(0.,0.00585824217053873,
0.0117172063374278,0.0175777385368055,0.023199358685178,0.0236369506552736),
 .UNSPECIFIED.) ;
#1629 = B_SPLINE_CURVE_WITH_KNOTS('',3,(#107958,#107959,#107960,#107961,#107962,
#107963,#107964,#107965,#107966,#107967,#107968,#107969,#107970,#107971),
 .UNSPECIFIED.,.F.,.F.,(4,2,2,2,2,2,4),(-0.055925014347253,-0.0556883945436994,
-0.0495906031970911,-0.0437546843011451,-0.0372885759065727,-0.0322854917697116,
-0.0278441972720297),.UNSPECIFIED.) ;
#1630 = B_SPLINE_CURVE_WITH_KNOTS('',3,(#107973,#107974,#107975,#107976,#107977,
#107978,#107979,#107980,#107981,#107982,#107983,#107984,#107985,#107986,
#107987,#107988),.UNSPECIFIED.,.F.,.F.,(4,3,3,3,3,4),(-0.000437598556065294,
0.,0.00562170475696129,0.0114823251605729,0.0173413775081186,0.0231997078484631),
 .UNSPECIFIED.) ;
#1631 = B_SPLINE_CURVE_WITH_KNOTS('',3,(#107993,#107994,#107995,#107996,#107997,
#107998,#107999,#108000,#108001,#108002,#108003,#108004,#108005,#108006,
#108007,#108008),.UNSPECIFIED.,.F.,.F.,(4,3,3,3,3,4),(0.,0.00585824217053423,
0.0117172063374038,0.0175777385367393,0.0231993586850723,0.0236369506551701),
 .UNSPECIFIED.) ;
#1632 = B_SPLINE_CURVE_WITH_KNOTS('',3,(#108009,#108010,#108011,#108012,#108013,
#108014,#108015,#108016,#108017,#108018,#108019,#108020,#108021,#108022),
 .UNSPECIFIED.,.F.,.F.,(4,2,2,2,2,2,4),(-0.00023661980315042,0.,0.00609779134723154,
0.0119337102438925,0.0183998186390206,0.0234029027763186,0.027844197274388),
 .UNSPECIFIED.) ;
#1633 = B_SPLINE_CURVE_WITH_KNOTS('',3,(#108024,#108025,#108026,#108027,#108028,
#108029,#108030,#108031,#108032,#108033,#108034,#108035,#108036,#108037),
 .UNSPECIFIED.,.F.,.F.,(4,2,2,2,2,2,4),(-0.000236619803568179,0.,0.00609779134706943,
0.011933710243561,0.0183998186387449,0.0234029027760718,0.0278441972741583),
 .UNSPECIFIED.) ;
#1634 = B_SPLINE_CURVE_WITH_KNOTS('',3,(#108038,#108039,#108040,#108041,#108042,
#108043,#108044,#108045,#108046,#108047,#108048,#108049,#108050,#108051,
#108052,#108053),.UNSPECIFIED.,.F.,.F.,(4,3,3,3,3,4),(0.,0.00585824217054849,
0.0117172063374606,0.0175777385368388,0.0231993586852149,0.0236369506553345),
 .UNSPECIFIED.) ;
#1635 = B_SPLINE_CURVE_WITH_KNOTS('',3,(#108055,#108056,#108057,#108058,#108059,
#108060,#108061,#108062,#108063,#108064,#108065,#108066,#108067,#108068),
 .UNSPECIFIED.,.F.,.F.,(4,2,2,2,2,2,4),(-0.0559250143497057,-0.0556883945461452,
-0.0495906031993172,-0.0437546843030612,-0.0372885759081806,-0.0322854917710824,
-0.0278441972731839),.UNSPECIFIED.) ;
#1636 = B_SPLINE_CURVE_WITH_KNOTS('',3,(#108070,#108071,#108072,#108073,#108074,
#108075,#108076,#108077,#108078,#108079,#108080,#108081,#108082,#108083,
#108084,#108085),.UNSPECIFIED.,.F.,.F.,(4,3,3,3,3,4),(-0.000437598556084839,
0.,0.00562170475699754,0.0114823251606981,0.0173413775083502,0.0231997078487964),
 .UNSPECIFIED.) ;
#1637 = B_SPLINE_CURVE_WITH_KNOTS('',3,(#108090,#108091,#108092,#108093,#108094,
#108095,#108096,#108097,#108098,#108099,#108100,#108101,#108102,#108103,
#108104,#108105),.UNSPECIFIED.,.F.,.F.,(4,3,3,3,3,4),(0.,0.00585824217054277,
0.0117172063374441,0.0175777385368182,0.0231993586851572,0.0236369506552668),
 .UNSPECIFIED.) ;
#1638 = B_SPLINE_CURVE_WITH_KNOTS('',3,(#108106,#108107,#108108,#108109,#108110,
#108111,#108112,#108113,#108114,#108115,#108116,#108117,#108118,#108119),
 .UNSPECIFIED.,.F.,.F.,(4,2,2,2,2,2,4),(-0.00023661980356187,0.,0.00609779134698056,
0.0119337102433812,0.0183998186384326,0.0234029027756759,0.0278441972736905),
 .UNSPECIFIED.) ;
#1639 = B_SPLINE_CURVE_WITH_KNOTS('',3,(#108121,#108122,#108123,#108124,#108125,
#108126,#108127,#108128,#108129,#108130,#108131,#108132,#108133,#108134),
 .UNSPECIFIED.,.F.,.F.,(4,2,2,2,2,2,4),(-0.000236619803566785,0.,0.00609779134702904,
0.0119337102434475,0.0183998186384865,0.0234029027757207,0.0278441972737459),
 .UNSPECIFIED.) ;
#1640 = B_SPLINE_CURVE_WITH_KNOTS('',3,(#108135,#108136,#108137,#108138,#108139,
#108140,#108141,#108142,#108143,#108144,#108145,#108146,#108147,#108148,
#108149,#108150),.UNSPECIFIED.,.F.,.F.,(4,3,3,3,3,4),(0.,0.00585824217054034,
0.0117172063374279,0.0175777385367946,0.0231993586851777,0.0236369506552812),
 .UNSPECIFIED.) ;
#1641 = B_SPLINE_CURVE_WITH_KNOTS('',3,(#108152,#108153,#108154,#108155,#108156,
#108157,#108158,#108159,#108160,#108161,#108162,#108163,#108164,#108165),
 .UNSPECIFIED.,.F.,.F.,(4,2,2,2,2,2,4),(-0.0559250143501053,-0.0556883945465432,
-0.0495906031996281,-0.0437546843033128,-0.0372885759083777,-0.0322854917712189,
-0.0278441972732712),.UNSPECIFIED.) ;
#1642 = B_SPLINE_CURVE_WITH_KNOTS('',3,(#108167,#108168,#108169,#108170,#108171,
#108172,#108173,#108174,#108175,#108176,#108177,#108178,#108179,#108180,
#108181,#108182),.UNSPECIFIED.,.F.,.F.,(4,3,3,3,3,4),(-0.000437598556096447,
0.,0.00562170475713416,0.0114823251609764,0.0173413775087778,0.0231997078493597),
 .UNSPECIFIED.) ;
#1643 = B_SPLINE_CURVE_WITH_KNOTS('',3,(#108187,#108188,#108189,#108190,#108191,
#108192,#108193,#108194,#108195,#108196,#108197,#108198,#108199,#108200,
#108201,#108202),.UNSPECIFIED.,.F.,.F.,(4,3,3,3,3,4),(0.,0.00585824217053087,
0.0117172063373846,0.0175777385366825,0.0231993586850888,0.0236369506551764),
 .UNSPECIFIED.) ;
#1644 = B_SPLINE_CURVE_WITH_KNOTS('',3,(#108203,#108204,#108205,#108206,#108207,
#108208,#108209,#108210,#108211,#108212,#108213,#108214,#108215,#108216),
 .UNSPECIFIED.,.F.,.F.,(4,2,2,2,2,2,4),(-0.000236619803975554,0.,0.00609779134645292,
0.0119337102422305,0.0183998186368445,0.0234029027737468,0.0278441972714777),
 .UNSPECIFIED.) ;
#1645 = B_SPLINE_CURVE_WITH_KNOTS('',3,(#108218,#108219,#108220,#108221,#108222,
#108223,#108224,#108225,#108226,#108227,#108228,#108229,#108230,#108231),
 .UNSPECIFIED.,.F.,.F.,(4,2,2,2,2,2,4),(-0.000236619803145561,0.,0.00609779134719067,
0.0119337102437602,0.0183998186387406,0.0234029027759312,0.0278441972739105),
 .UNSPECIFIED.) ;
#1646 = B_SPLINE_CURVE_WITH_KNOTS('',3,(#108232,#108233,#108234,#108235,#108236,
#108237,#108238,#108239,#108240,#108241,#108242,#108243,#108244,#108245,
#108246,#108247),.UNSPECIFIED.,.F.,.F.,(4,3,3,3,3,4),(0.,0.00585824217053935,
0.0117172063374137,0.0175777385367471,0.0231993586851797,0.0236369506552624),
 .UNSPECIFIED.) ;
#1647 = B_SPLINE_CURVE_WITH_KNOTS('',3,(#108249,#108250,#108251,#108252,#108253,
#108254,#108255,#108256,#108257,#108258,#108259,#108260,#108261,#108262),
 .UNSPECIFIED.,.F.,.F.,(4,2,2,2,2,2,4),(-0.0559250143516561,-0.0556883945480848,
-0.0495906032009887,-0.0437546843044866,-0.0372885759093485,-0.032285491772039,
-0.0278441972739555),.UNSPECIFIED.) ;
#1648 = B_SPLINE_CURVE_WITH_KNOTS('',3,(#108264,#108265,#108266,#108267,#108268,
#108269,#108270,#108271,#108272,#108273,#108274,#108275,#108276,#108277,
#108278,#108279),.UNSPECIFIED.,.F.,.F.,(4,3,3,3,3,4),(-0.000437598556137922,
0.,0.00562170475738925,0.0114823251615342,0.0173413775096173,0.0231997078504894),
 .UNSPECIFIED.) ;
#1649 = B_SPLINE_CURVE_WITH_KNOTS('',3,(#108284,#108285,#108286,#108287,#108288,
#108289,#108290,#108291,#108292,#108293,#108294,#108295,#108296,#108297,
#108298,#108299),.UNSPECIFIED.,.F.,.F.,(4,3,3,3,3,4),(0.,0.00585824217054286,
0.0117172063374258,0.0175777385367681,0.0231993586851975,0.0236369506552776),
 .UNSPECIFIED.) ;
#1650 = B_SPLINE_CURVE_WITH_KNOTS('',3,(#108300,#108301,#108302,#108303,#108304,
#108305,#108306,#108307,#108308,#108309,#108310,#108311,#108312,#108313),
 .UNSPECIFIED.,.F.,.F.,(4,2,2,2,2,2,4),(-0.000236619803141347,0.,0.00609779134719742,
0.0119337102437761,0.0183998186387667,0.0234029027759622,0.0278441972739489),
 .UNSPECIFIED.) ;
#1651 = B_SPLINE_CURVE_WITH_KNOTS('',3,(#108315,#108316,#108317,#108318,#108319,
#108320,#108321,#108322,#108323,#108324,#108325,#108326,#108327,#108328),
 .UNSPECIFIED.,.F.,.F.,(4,2,2,2,2,2,4),(-0.000236619803560324,0.,0.00609779134688203,
0.0119337102431469,0.0183998186380461,0.0234029027751694,0.0278441972730812),
 .UNSPECIFIED.) ;
#1652 = B_SPLINE_CURVE_WITH_KNOTS('',3,(#108329,#108330,#108331,#108332,#108333,
#108334,#108335,#108336,#108337,#108338,#108339,#108340,#108341,#108342,
#108343,#108344),.UNSPECIFIED.,.F.,.F.,(4,3,3,3,3,4),(0.,0.00585824217053624,
0.0117172063373978,0.017577738536714,0.0231993586851339,0.0236369506552253),
 .UNSPECIFIED.) ;
#1653 = B_SPLINE_CURVE_WITH_KNOTS('',3,(#108346,#108347,#108348,#108349,#108350,
#108351,#108352,#108353,#108354,#108355,#108356,#108357,#108358,#108359),
 .UNSPECIFIED.,.F.,.F.,(4,2,2,2,2,2,4),(-0.0559250143527569,-0.0556883945491825,
-0.0495906032019952,-0.0437546843053732,-0.0372885759100185,-0.0322854917725816,
-0.0278441972744026),.UNSPECIFIED.) ;
#1654 = B_SPLINE_CURVE_WITH_KNOTS('',3,(#108361,#108362,#108363,#108364,#108365,
#108366,#108367,#108368,#108369,#108370,#108371,#108372,#108373,#108374,
#108375,#108376),.UNSPECIFIED.,.F.,.F.,(4,3,3,3,3,4),(-0.000437598556170072,
0.,0.00562170475739005,0.0114823251615356,0.0173413775096278,0.0231997078504878),
 .UNSPECIFIED.) ;
#1655 = B_SPLINE_CURVE_WITH_KNOTS('',3,(#108381,#108382,#108383,#108384,#108385,
#108386,#108387,#108388,#108389,#108390,#108391,#108392,#108393,#108394,
#108395,#108396),.UNSPECIFIED.,.F.,.F.,(4,3,3,3,3,4),(0.,0.00585824217054469,
0.0117172063374513,0.0175777385368039,0.0231993586851361,0.0236369506553527),
 .UNSPECIFIED.) ;
#1656 = B_SPLINE_CURVE_WITH_KNOTS('',3,(#108397,#108398,#108399,#108400,#108401,
#108402,#108403,#108404,#108405,#108406,#108407,#108408,#108409,#108410),
 .UNSPECIFIED.,.F.,.F.,(4,2,2,2,2,2,4),(-0.000236619804202799,0.,0.00609779134737763,
0.0119337102442503,0.0183998186398358,0.0234029027774637,0.0278441972757869),
 .UNSPECIFIED.) ;
#1657 = B_SPLINE_CURVE_WITH_KNOTS('',3,(#108412,#108413,#108414,#108415,#108416,
#108417,#108418,#108419,#108420,#108421,#108422,#108423,#108424,#108425),
 .UNSPECIFIED.,.F.,.F.,(4,2,2,2,2,2,4),(-0.0002366198042002,0.,0.00609779134724177,
0.0119337102439773,0.0183998186394422,0.0234029027769713,0.027844197275244),
 .UNSPECIFIED.) ;
#1658 = B_SPLINE_CURVE_WITH_KNOTS('',3,(#108426,#108427,#108428,#108429,#108430,
#108431,#108432,#108433,#108434,#108435,#108436,#108437,#108438,#108439,
#108440,#108441),.UNSPECIFIED.,.F.,.F.,(4,3,3,3,3,4),(0.,0.00585824217054219,
0.0117172063374448,0.0175777385367976,0.0231993586850719,0.0236369506552122),
 .UNSPECIFIED.) ;
#1659 = B_SPLINE_CURVE_WITH_KNOTS('',3,(#108443,#108444,#108445,#108446,#108447,
#108448,#108449,#108450,#108451,#108452,#108453,#108454,#108455,#108456),
 .UNSPECIFIED.,.F.,.F.,(4,2,2,2,2,2,4),(-0.0559250143475747,-0.0556883945440193,
-0.0495906031973805,-0.0437546843014019,-0.0372885759067931,-0.0322854917699036,
-0.0278441972721905),.UNSPECIFIED.) ;
#1660 = B_SPLINE_CURVE_WITH_KNOTS('',3,(#108458,#108459,#108460,#108461,#108462,
#108463,#108464,#108465,#108466,#108467,#108468,#108469,#108470,#108471,
#108472,#108473),.UNSPECIFIED.,.F.,.F.,(4,3,3,3,3,4),(-0.000437598556074084,
0.,0.00562170475694653,0.0114823251605845,0.0173413775081531,0.0231997078485162),
 .UNSPECIFIED.) ;
#1661 = B_SPLINE_CURVE_WITH_KNOTS('',3,(#108478,#108479,#108480,#108481,#108482,
#108483,#108484,#108485,#108486,#108487,#108488,#108489,#108490,#108491,
#108492,#108493),.UNSPECIFIED.,.F.,.F.,(4,3,3,3,3,4),(0.,0.00585824217053932,
0.0117172063374163,0.0175777385367554,0.0231993586851953,0.0236369506552652),
 .UNSPECIFIED.) ;
#1662 = B_SPLINE_CURVE_WITH_KNOTS('',3,(#108494,#108495,#108496,#108497,#108498,
#108499,#108500,#108501,#108502,#108503,#108504,#108505,#108506,#108507),
 .UNSPECIFIED.,.F.,.F.,(4,2,2,2,2,2,4),(-0.000236619803563584,0.,0.00609779134684538,
0.0119337102430664,0.0183998186379667,0.0234029027750871,0.0278441972729952),
 .UNSPECIFIED.) ;
#1663 = B_SPLINE_CURVE_WITH_KNOTS('',3,(#108509,#108510,#108511,#108512,#108513,
#108514,#108515,#108516,#108517,#108518,#108519,#108520,#108521,#108522),
 .UNSPECIFIED.,.F.,.F.,(4,2,2,2,2,2,4),(-0.000236619803559064,0.,0.00609779134682761,
0.0119337102430243,0.0183998186378634,0.0234029027749327,0.0278441972727837),
 .UNSPECIFIED.) ;
#1664 = B_SPLINE_CURVE_WITH_KNOTS('',3,(#108523,#108524,#108525,#108526,#108527,
#108528,#108529,#108530,#108531,#108532,#108533,#108534,#108535,#108536,
#108537,#108538),.UNSPECIFIED.,.F.,.F.,(4,3,3,3,3,4),(0.,0.00585824217053403,
0.0117172063373908,0.0175777385367026,0.0231993586851274,0.0236369506551984),
 .UNSPECIFIED.) ;
#1665 = B_SPLINE_CURVE_WITH_KNOTS('',3,(#108540,#108541,#108542,#108543,#108544,
#108545,#108546,#108547,#108548,#108549,#108550,#108551,#108552,#108553),
 .UNSPECIFIED.,.F.,.F.,(4,2,2,2,2,2,4),(-0.0559250143495183,-0.0556883945459582,
-0.0495906031991357,-0.0437546843029003,-0.0372885759080418,-0.0322854917709563,
-0.0278441972730646),.UNSPECIFIED.) ;
#1666 = B_SPLINE_CURVE_WITH_KNOTS('',3,(#108555,#108556,#108557,#108558,#108559,
#108560,#108561,#108562,#108563,#108564,#108565,#108566,#108567,#108568,
#108569,#108570),.UNSPECIFIED.,.F.,.F.,(4,3,3,3,3,4),(-0.000437598556092783,
0.,0.00562170475708721,0.0114823251608936,0.0173413775086511,0.0231997078492032),
 .UNSPECIFIED.) ;
#1667 = B_SPLINE_CURVE_WITH_KNOTS('',3,(#108575,#108576,#108577,#108578,#108579,
#108580,#108581,#108582,#108583,#108584,#108585,#108586,#108587,#108588,
#108589,#108590),.UNSPECIFIED.,.F.,.F.,(4,3,3,3,3,4),(0.,0.00585824217054838,
0.0117172063374519,0.0175777385368119,0.0231993586852536,0.0236369506553148),
 .UNSPECIFIED.) ;
#1668 = B_SPLINE_CURVE_WITH_KNOTS('',3,(#108591,#108592,#108593,#108594,#108595,
#108596,#108597,#108598,#108599,#108600,#108601,#108602,#108603,#108604),
 .UNSPECIFIED.,.F.,.F.,(4,2,2,2,2,2,4),(-0.000236619803558096,0.,0.00609779134681664,
0.0119337102430081,0.0183998186378316,0.0234029027748886,0.0278441972727373),
 .UNSPECIFIED.) ;
#1669 = B_SPLINE_CURVE_WITH_KNOTS('',3,(#108606,#108607,#108608,#108609,#108610,
#108611,#108612,#108613,#108614,#108615,#108616,#108617,#108618,#108619),
 .UNSPECIFIED.,.F.,.F.,(4,2,2,2,2,2,4),(-0.000236619803562333,0.,0.00609779134692135,
0.0119337102432951,0.0183998186383094,0.0234029027755172,0.0278441972735094),
 .UNSPECIFIED.) ;
#1670 = B_SPLINE_CURVE_WITH_KNOTS('',3,(#108620,#108621,#108622,#108623,#108624,
#108625,#108626,#108627,#108628,#108629,#108630,#108631,#108632,#108633,
#108634,#108635),.UNSPECIFIED.,.F.,.F.,(4,3,3,3,3,4),(0.,0.00585824217054129,
0.0117172063374373,0.0175777385368199,0.023199358685217,0.0236369506553186),
 .UNSPECIFIED.) ;
#1671 = B_SPLINE_CURVE_WITH_KNOTS('',3,(#108637,#108638,#108639,#108640,#108641,
#108642,#108643,#108644,#108645,#108646,#108647,#108648,#108649,#108650),
 .UNSPECIFIED.,.F.,.F.,(4,2,2,2,2,2,4),(-0.0559250143502032,-0.0556883945466394,
-0.0495906031997328,-0.0437546843034414,-0.0372885759084786,-0.0322854917713055,
-0.0278441972733409),.UNSPECIFIED.) ;
#1672 = B_SPLINE_CURVE_WITH_KNOTS('',3,(#108652,#108653,#108654,#108655,#108656,
#108657,#108658,#108659,#108660,#108661,#108662,#108663,#108664,#108665,
#108666,#108667),.UNSPECIFIED.,.F.,.F.,(4,3,3,3,3,4),(-0.000437598556094846,
0.,0.00562170475708876,0.0114823251608924,0.0173413775086073,0.0231997078491061),
 .UNSPECIFIED.) ;
#1673 = B_SPLINE_CURVE_WITH_KNOTS('',3,(#108669,#108670,#108671,#108672,#108673,
#108674,#108675,#108676,#108677,#108678,#108679,#108680,#108681,#108682,
#108683,#108684),.UNSPECIFIED.,.F.,.F.,(4,3,3,3,3,4),(0.,0.00585824217053639,
0.0117172063374152,0.0175777385367772,0.0231993586851953,0.0236369506552933),
 .UNSPECIFIED.) ;
#1674 = B_SPLINE_CURVE_WITH_KNOTS('',3,(#108685,#108686,#108687,#108688,#108689,
#108690,#108691,#108692,#108693,#108694,#108695,#108696,#108697,#108698),
 .UNSPECIFIED.,.F.,.F.,(4,2,2,2,2,2,4),(-0.000236619803922217,0.,0.00609779134654128,
0.0119337102425373,0.018399818637407,0.0234029027744858,0.0278441972723643),
 .UNSPECIFIED.) ;
#1675 = B_SPLINE_CURVE_WITH_KNOTS('',3,(#108700,#108701,#108702,#108703,#108704,
#108705,#108706,#108707,#108708,#108709,#108710,#108711,#108712,#108713),
 .UNSPECIFIED.,.F.,.F.,(4,2,2,2,2,2,4),(-0.000236619803561269,0.,0.00609779134692068,
0.0119337102432194,0.0183998186381382,0.02340290277528,0.0278441972732167),
 .UNSPECIFIED.) ;
#1676 = B_SPLINE_CURVE_WITH_KNOTS('',3,(#108714,#108715,#108716,#108717,#108718,
#108719,#108720,#108721,#108722,#108723,#108724,#108725,#108726,#108727,
#108728,#108729),.UNSPECIFIED.,.F.,.F.,(4,3,3,3,3,4),(0.,0.00585824217053491,
0.0117172063374156,0.0175777385367886,0.0231993586852222,0.0236369506553088),
 .UNSPECIFIED.) ;
#1677 = B_SPLINE_CURVE_WITH_KNOTS('',3,(#108731,#108732,#108733,#108734,#108735,
#108736,#108737,#108738,#108739,#108740,#108741,#108742,#108743,#108744),
 .UNSPECIFIED.,.F.,.F.,(4,2,2,2,2,2,4),(-0.0559250143500672,-0.0556883945469228,
-0.049590603199785,-0.0437546843032336,-0.0372885759082228,-0.0322854917710044,
-0.0278441972729959),.UNSPECIFIED.) ;
#1678 = B_SPLINE_CURVE_WITH_KNOTS('',3,(#108746,#108747,#108748,#108749,#108750,
#108751,#108752,#108753,#108754,#108755,#108756,#108757,#108758,#108759,
#108760,#108761),.UNSPECIFIED.,.F.,.F.,(4,3,3,3,3,4),(-0.000437598556138437,
0.,0.00562170475741228,0.0114823251616098,0.0173413775097521,0.0231997078506926),
 .UNSPECIFIED.) ;
#1679 = B_SPLINE_CURVE_WITH_KNOTS('',3,(#108767,#108768,#108769,#108770,#108771,
#108772,#108773,#108774,#108775,#108776,#108777,#108778,#108779,#108780),
 .UNSPECIFIED.,.F.,.F.,(4,2,2,2,2,2,4),(-0.0559250143516994,-0.0556883945481287,
-0.0495906032010545,-0.0437546843045533,-0.0372885759093916,-0.0322854917720808,
-0.0278441972739919),.UNSPECIFIED.) ;
#1680 = B_SPLINE_CURVE_WITH_KNOTS('',3,(#108784,#108785,#108786,#108787,#108788,
#108789,#108790,#108791,#108792,#108793,#108794,#108795,#108796,#108797,
#108798,#108799),.UNSPECIFIED.,.F.,.F.,(4,3,3,3,3,4),(-0.000437598556144422,
0.,0.00562170475740183,0.0114823251615895,0.0173413775097444,0.0231997078506806),
 .UNSPECIFIED.) ;
#1681 = B_SPLINE_CURVE_WITH_KNOTS('',3,(#108806,#108807,#108808,#108809,#108810,
#108811,#108812,#108813,#108814,#108815,#108816,#108817,#108818,#108819),
 .UNSPECIFIED.,.F.,.F.,(4,2,2,2,2,2,4),(-0.0559250143435119,-0.0556883945403911,
-0.0495906031940201,-0.0437546842982849,-0.0372885759042276,-0.0322854917677294,
-0.0278441972703399),.UNSPECIFIED.) ;
#1682 = B_SPLINE_CURVE_WITH_KNOTS('',3,(#108823,#108824,#108825,#108826,#108827,
#108828,#108829,#108830,#108831,#108832,#108833,#108834,#108835,#108836,
#108837,#108838),.UNSPECIFIED.,.F.,.F.,(4,3,3,3,3,4),(-0.000437598556018984,
0.,0.00562170475658728,0.0114823251597353,0.0173413775068133,0.0231997078467154),
 .UNSPECIFIED.) ;
#1683 = B_SPLINE_CURVE_WITH_KNOTS('',3,(#108845,#108846,#108847,#108848,#108849,
#108850,#108851,#108852,#108853,#108854,#108855,#108856,#108857,#108858),
 .UNSPECIFIED.,.F.,.F.,(4,2,2,2,2,2,4),(-0.0559250143454541,-0.055688394541913,
-0.0495906031955341,-0.0437546842998321,-0.0372885759055476,-0.0322854917689083,
-0.0278441972713927),.UNSPECIFIED.) ;
#1684 = B_SPLINE_CURVE_WITH_KNOTS('',3,(#108862,#108863,#108864,#108865,#108866,
#108867,#108868,#108869,#108870,#108871,#108872,#108873,#108874,#108875,
#108876,#108877),.UNSPECIFIED.,.F.,.F.,(4,3,3,3,3,4),(-0.000437598556040506,
0.,0.00562170475667276,0.0114823251599514,0.0173413775071961,0.0231997078472458),
 .UNSPECIFIED.) ;
#1685 = B_SPLINE_CURVE_WITH_KNOTS('',3,(#108884,#108885,#108886,#108887,#108888,
#108889,#108890,#108891,#108892,#108893,#108894,#108895,#108896,#108897),
 .UNSPECIFIED.,.F.,.F.,(4,2,2,2,2,2,4),(-0.0559250143503411,-0.0556883945467744,
-0.0495906031998412,-0.0437546843035047,-0.0372885759085466,-0.0322854917713593,
-0.0278441972733858),.UNSPECIFIED.) ;
#1686 = B_SPLINE_CURVE_WITH_KNOTS('',3,(#108901,#108902,#108903,#108904,#108905,
#108906,#108907,#108908,#108909,#108910,#108911,#108912,#108913,#108914,
#108915,#108916),.UNSPECIFIED.,.F.,.F.,(4,3,3,3,3,4),(-0.00043759855609295,
0.,0.00562170475705494,0.0114823251608269,0.0173413775085459,0.0231997078490585),
 .UNSPECIFIED.) ;
#1687 = B_SPLINE_CURVE_WITH_KNOTS('',3,(#108923,#108924,#108925,#108926,#108927,
#108928,#108929,#108930,#108931,#108932,#108933,#108934,#108935,#108936),
 .UNSPECIFIED.,.F.,.F.,(4,2,2,2,2,2,4),(-0.0559250143576788,-0.0556883945534629,
-0.0495906032058708,-0.0437546843087237,-0.0372885759128067,-0.0322854917749087,
-0.027844197276348),.UNSPECIFIED.) ;
#1688 = B_SPLINE_CURVE_WITH_KNOTS('',3,(#108940,#108941,#108942,#108943,#108944,
#108945,#108946,#108947,#108948,#108949,#108950,#108951,#108952,#108953,
#108954,#108955),.UNSPECIFIED.,.F.,.F.,(4,3,3,3,3,4),(-0.000437598556265556,
0.,0.00562170475766576,0.0114823251621366,0.0173413775105401,0.0231997078516975),
 .UNSPECIFIED.) ;
#1689 = B_SPLINE_CURVE_WITH_KNOTS('',3,(#108962,#108963,#108964,#108965,#108966,
#108967,#108968,#108969,#108970,#108971,#108972,#108973,#108974,#108975),
 .UNSPECIFIED.,.F.,.F.,(4,2,2,2,2,2,4),(-0.0559250143546525,-0.0556883945504525,
-0.0495906032031384,-0.0437546843063546,-0.0372885759108327,-0.0322854917732639,
-0.0278441972749651),.UNSPECIFIED.) ;
#1690 = B_SPLINE_CURVE_WITH_KNOTS('',3,(#108979,#108980,#108981,#108982,#108983,
#108984,#108985,#108986,#108987,#108988,#108989,#108990,#108991,#108992,
#108993,#108994),.UNSPECIFIED.,.F.,.F.,(4,3,3,3,3,4),(-0.000437598556211791,
0.,0.00562170475765983,0.011482325162167,0.0173413775106296,0.0231997078518591),
 .UNSPECIFIED.) ;
#1691 = B_SPLINE_CURVE_WITH_KNOTS('',3,(#109001,#109002,#109003,#109004,#109005,
#109006,#109007,#109008,#109009,#109010,#109011,#109012,#109013,#109014),
 .UNSPECIFIED.,.F.,.F.,(4,2,2,2,2,2,4),(-0.0559250143563362,-0.055688394551709,
-0.0495906032045639,-0.0437546843078355,-0.0372885759121675,-0.0322854917744538,
-0.0278441972760254),.UNSPECIFIED.) ;
#1692 = B_SPLINE_CURVE_WITH_KNOTS('',3,(#109018,#109019,#109020,#109021,#109022,
#109023,#109024,#109025,#109026,#109027,#109028,#109029,#109030,#109031,
#109032,#109033),.UNSPECIFIED.,.F.,.F.,(4,3,3,3,3,4),(-0.000437598556225459,
0.,0.00562170475744369,0.0114823251616755,0.0173413775098568,0.0231997078508077),
 .UNSPECIFIED.) ;
#1693 = B_SPLINE_CURVE_WITH_KNOTS('',3,(#109040,#109041,#109042,#109043,#109044,
#109045,#109046,#109047,#109048,#109049,#109050,#109051,#109052,#109053),
 .UNSPECIFIED.,.F.,.F.,(4,2,2,2,2,2,4),(-0.0559250143492567,-0.0556883945456972,
-0.0495906031988905,-0.0437546843027083,-0.0372885759078583,-0.0322854917707879,
-0.0278441972729168),.UNSPECIFIED.) ;
#1694 = B_SPLINE_CURVE_WITH_KNOTS('',3,(#109057,#109058,#109059,#109060,#109061,
#109062,#109063,#109064,#109065,#109066,#109067,#109068,#109069,#109070,
#109071,#109072),.UNSPECIFIED.,.F.,.F.,(4,3,3,3,3,4),(-0.000437598556080345,
0.,0.00562170475697672,0.0114823251606002,0.0173413775081636,0.0231997078485257),
 .UNSPECIFIED.) ;
#1695 = B_SPLINE_CURVE_WITH_KNOTS('',3,(#109079,#109080,#109081,#109082,#109083,
#109084,#109085,#109086,#109087,#109088,#109089,#109090,#109091,#109092),
 .UNSPECIFIED.,.F.,.F.,(4,2,2,2,2,2,4),(-0.055925014349952,-0.0556883945463912,
-0.0495906031994983,-0.0437546843032064,-0.0372885759082967,-0.0322854917711481,
-0.0278441972731949),.UNSPECIFIED.) ;
#1696 = B_SPLINE_CURVE_WITH_KNOTS('',3,(#109096,#109097,#109098,#109099,#109100,
#109101,#109102,#109103,#109104,#109105,#109106,#109107,#109108,#109109,
#109110,#109111),.UNSPECIFIED.,.F.,.F.,(4,3,3,3,3,4),(-0.000437598556096392,
0.,0.005621704757061,0.0114823251608164,0.0173413775085336,0.0231997078490336),
 .UNSPECIFIED.) ;
#1697 = B_SPLINE_CURVE_WITH_KNOTS('',3,(#109203,#109204,#109205,#109206,#109207,
#109208,#109209,#109210,#109211,#109212,#109213,#109214,#109215,#109216,
#109217,#109218,#109219,#109220,#109221,#109222,#109223,#109224,#109225,
#109226,#109227,#109228,#109229,#109230,#109231,#109232,#109233,#109234,
#109235,#109236,#109237,#109238,#109239,#109240,#109241,#109242,#109243,
#109244,#109245,#109246,#109247,#109248,#109249,#109250,#109251,#109252,
#109253,#109254,#109255,#109256,#109257,#109258,#109259,#109260,#109261,
#109262,#109263,#109264,#109265,#109266,#109267,#109268,#109269,#109270,
#109271,#109272,#109273,#109274,#109275,#109276,#109277,#109278,#109279,
#109280,#109281,#109282),.UNSPECIFIED.,.F.,.F.,(4,2,2,2,2,2,2,2,2,2,2,2,
2,2,2,2,2,2,2,2,2,2,2,2,2,2,2,2,2,2,2,2,2,2,2,2,2,2,2,4),(-0.552593410761711,
-0.5520841033493,-0.543414800045841,-0.530981645331462,-0.515682120379995,
-0.489011851192856,-0.475791475211459,-0.469800228676837,-0.464823585052418,
-0.456758200675436,-0.446117862199597,-0.412190397885134,-0.396445377902817,
-0.387356530724998,-0.378534621106888,-0.364686037892163,-0.330083411853553,
-0.312869588553632,-0.306676202327231,-0.301718040883505,-0.293987276238174,
-0.28400901338443,-0.255540175710082,-0.235962621045616,-0.226122570338451,
-0.217486499647387,-0.205608163506685,-0.191376706596845,-0.162958816002947,
-0.149015686282994,-0.143020064395438,-0.137940493423511,-0.129517498871141,
-0.118194060456811,-0.0767579974893125,-0.0659012890372971,-0.0573052858902992,
-0.0467033580009995,-0.0196389999660062,-0.00261625130652141),
 .UNSPECIFIED.) ;
#1698 = B_SPLINE_CURVE_WITH_KNOTS('',3,(#109285,#109286,#109287,#109288,#109289,
#109290,#109291,#109292,#109293,#109294,#109295,#109296,#109297,#109298,
#109299,#109300,#109301,#109302,#109303,#109304,#109305,#109306,#109307,
#109308,#109309,#109310,#109311,#109312,#109313,#109314,#109315,#109316,
#109317,#109318,#109319,#109320,#109321,#109322,#109323,#109324,#109325,
#109326,#109327,#109328,#109329,#109330,#109331,#109332),.UNSPECIFIED.,
 .F.,.F.,(4,2,2,2,2,2,2,2,2,2,2,2,2,2,2,2,2,2,2,2,2,2,2,4),(-1.74388914172831,
-1.74010158624316,-1.73533493491195,-1.69713014187374,-1.68355997429145,
-1.67194962285965,-1.66271393068178,-1.65106169492588,-1.61630518110585,
-1.58993773929061,-1.58306967342475,-1.57816077380394,-1.57132637085491,
-1.54363126039316,-1.51548297073149,-1.50527675750718,-1.49695811956463,
-1.48648723066268,-1.44858943711612,-1.42603340225277,-1.41932565863014,
-1.41457975898413,-1.40826951094876,-1.40009241220142),.UNSPECIFIED.) ;
#1699 = B_SPLINE_CURVE_WITH_KNOTS('',3,(#109337,#109338,#109339,#109340,#109341,
#109342,#109343,#109344,#109345,#109346,#109347,#109348,#109349,#109350,
#109351,#109352,#109353,#109354,#109355,#109356,#109357,#109358,#109359,
#109360,#109361,#109362,#109363,#109364,#109365,#109366,#109367,#109368,
#109369,#109370,#109371,#109372,#109373,#109374,#109375,#109376,#109377,
#109378,#109379,#109380,#109381,#109382,#109383,#109384,#109385,#109386,
#109387,#109388,#109389,#109390,#109391,#109392,#109393,#109394,#109395,
#109396,#109397,#109398,#109399,#109400,#109401,#109402,#109403,#109404,
#109405,#109406,#109407,#109408,#109409,#109410,#109411,#109412,#109413,
#109414,#109415,#109416,#109417,#109418,#109419,#109420,#109421,#109422,
#109423,#109424,#109425,#109426,#109427,#109428,#109429,#109430,#109431,
#109432,#109433,#109434,#109435,#109436,#109437,#109438,#109439,#109440,
#109441,#109442,#109443,#109444,#109445,#109446,#109447,#109448,#109449,
#109450,#109451,#109452,#109453,#109454,#109455,#109456,#109457,#109458,
#109459,#109460,#109461,#109462,#109463,#109464,#109465,#109466,#109467,
#109468,#109469,#109470,#109471,#109472,#109473,#109474,#109475,#109476),
 .UNSPECIFIED.,.F.,.F.,(4,2,2,2,2,2,2,2,2,2,2,2,2,2,2,2,2,2,2,2,2,2,2,2,
2,2,2,2,2,2,2,2,2,2,2,2,2,2,2,2,2,2,2,2,2,2,2,2,2,2,2,2,2,2,2,2,2,2,2,2,
2,2,2,2,2,2,2,2,2,4),(-1.60819476001236,-1.60157151108133,-1.57374993060186,
-1.54333520918712,-1.5330944628995,-1.52455732114626,-1.51368106490473,
-1.48363670371605,-1.45716775914122,-1.45034362080875,-1.44544941240374,
-1.43858684897259,-1.40293109993587,-1.38660840131381,-1.37365915712381,
-1.36493247672918,-1.35557163070149,-1.33795142758038,-1.30177252657126,
-1.29363751094972,-1.28694201653805,-1.28204551297269,-1.27504505146196,
-1.24750286398903,-1.21793991752278,-1.20732165243159,-1.1987959811487,
-1.18816616116487,-1.1535726711856,-1.1305629468268,-1.12379029329879,-1.11889461776859,
-1.11197522743769,-1.08352620940999,-1.05355243311613,-1.04333196199694,
-1.03479173415174,-1.02388438639545,-0.996280762100526,-0.97622121148834,
-0.964282134908163,-0.958700667916607,-0.953524190525165,-0.944167265791223,
-0.930858282226715,-0.891097096141751,-0.88060265191729,-0.872078959293447,
-0.861328341297288,-0.836209324457884,-0.803362711467678,-0.796962241119135,
-0.792056336516214,-0.784839695546787,-0.775791460713609,-0.753103628892537,
-0.728807187779854,-0.717955013186807,-0.709422378254332,-0.699000038493792,
-0.687312334031512,-0.663447018063261,-0.64163726390635,-0.634488912403423,
-0.629581096095425,-0.622988562285989,-0.615033268711227,-0.580749247858517,
-0.561627829423672,-0.552593410761711),.UNSPECIFIED.) ;
#1700 = B_SPLINE_CURVE_WITH_KNOTS('',3,(#109477,#109478,#109479,#109480,#109481,
#109482,#109483,#109484,#109485,#109486,#109487,#109488,#109489,#109490,
#109491,#109492,#109493,#109494,#109495,#109496,#109497,#109498,#109499,
#109500,#109501,#109502,#109503,#109504,#109505,#109506,#109507,#109508,
#109509,#109510,#109511,#109512,#109513,#109514,#109515,#109516,#109517,
#109518,#109519,#109520,#109521,#109522,#109523,#109524,#109525,#109526,
#109527,#109528,#109529,#109530,#109531,#109532,#109533,#109534,#109535,
#109536,#109537,#109538,#109539,#109540,#109541,#109542,#109543,#109544,
#109545,#109546,#109547,#109548,#109549,#109550,#109551,#109552,#109553,
#109554,#109555,#109556,#109557,#109558,#109559,#109560,#109561,#109562,
#109563,#109564,#109565,#109566,#109567,#109568,#109569,#109570,#109571,
#109572,#109573,#109574,#109575,#109576,#109577,#109578,#109579,#109580,
#109581,#109582,#109583,#109584,#109585,#109586,#109587,#109588,#109589,
#109590,#109591,#109592,#109593,#109594,#109595,#109596,#109597,#109598,
#109599,#109600,#109601,#109602,#109603,#109604,#109605,#109606,#109607,
#109608,#109609,#109610,#109611,#109612,#109613,#109614,#109615,#109616,
#109617,#109618,#109619,#109620),.UNSPECIFIED.,.F.,.F.,(4,2,2,2,2,2,2,2,
2,2,2,2,2,2,2,2,2,2,2,2,2,2,2,2,2,2,2,2,2,2,2,2,2,2,2,2,2,2,2,2,2,2,2,2,
2,2,2,2,2,2,2,2,2,2,2,2,2,2,2,2,2,2,2,2,2,2,2,2,2,2,2,4),(-1.40009241220142,
-1.39027892404271,-1.35652120621099,-1.3427890502387,-1.33390838723088,
-1.3246360693791,-1.30797596827838,-1.27140299931499,-1.26322847705518,
-1.25649865986203,-1.25154939614112,-1.24437689145958,-1.22365219794817,
-1.19905991057942,-1.18720625527165,-1.17667403901707,-1.16811126913231,
-1.15728955781264,-1.12451282687639,-1.09983755963236,-1.09322146021638,
-1.08831885826578,-1.08120958853904,-1.05752347272841,-1.03479351117752,
-1.02336848189861,-1.01311471325315,-1.00462167080781,-0.993887863487606,
-0.96170664133996,-0.936256142399075,-0.929732827025822,-0.924842413978316,
-0.917692992839221,-0.896900816749588,-0.872386852319312,-0.856044560452436,
-0.846845625567806,-0.838022804779289,-0.824388691598358,-0.790916712807407,
-0.772827844029858,-0.766460546761273,-0.761546789185446,-0.754262465407307,
-0.745092618908703,-0.721724376077324,-0.698241216394806,-0.687447507649216,
-0.678919154709546,-0.668453448578193,-0.640197040220508,-0.610392150786397,
-0.603605311475741,-0.598712180190372,-0.59181667254431,-0.58333495261135,
-0.563541826914644,-0.535576624556928,-0.524668307552705,-0.51613376685688,
-0.505929580557802,-0.476712978209925,-0.447172033827767,-0.440359701789513,
-0.435467268922646,-0.428599990352192,-0.406330629551592,-0.370984619119945,
-0.36043799547759,-0.351912666138791,-0.344447890118419),.UNSPECIFIED.) ;
#1701 = B_SPLINE_CURVE_WITH_KNOTS('',3,(#109626,#109627,#109628,#109629,#109630,
#109631,#109632,#109633),.UNSPECIFIED.,.F.,.F.,(4,1,1,1,1,4),(21.9911559852233,
22.8773584072887,23.8489981895043,24.8206379717199,25.7922777539356,26.2282428538859),
 .UNSPECIFIED.) ;
#1702 = B_SPLINE_CURVE_WITH_KNOTS('',3,(#109634,#109635,#109636,#109637,#109638,
#109639,#109640,#109641,#109642,#109643,#109644,#109645,#109646,#109647,
#109648,#109649,#109650,#109651,#109652,#109653,#109654,#109655,#109656,
#109657,#109658,#109659,#109660,#109661,#109662,#109663,#109664,#109665,
#109666,#109667,#109668,#109669,#109670,#109671,#109672,#109673,#109674,
#109675,#109676,#109677,#109678,#109679,#109680,#109681,#109682,#109683,
#109684,#109685,#109686,#109687),.UNSPECIFIED.,.F.,.F.,(4,2,2,2,2,2,2,2,
2,2,2,2,2,2,2,2,2,2,2,2,2,2,2,2,2,2,4),(-1.95189018697911,-1.94523075986396,
-1.93976018216148,-1.9350625880257,-1.92813522823441,-1.9002619203118,-1.86981700938258,
-1.8595676021692,-1.85103118055753,-1.8401664646119,-1.81373957993934,-1.79279860037804,
-1.78408227826745,-1.77705321706049,-1.77215613141574,-1.76560901647882,
-1.72998813070304,-1.71337217751185,-1.70027829875411,-1.69153273295096,
-1.68221230721063,-1.66491104766538,-1.62833238402752,-1.62016088599395,
-1.61344422315257,-1.60854836482265,-1.60819476001236),.UNSPECIFIED.) ;
#1703 = B_SPLINE_CURVE_WITH_KNOTS('',3,(#109689,#109690,#109691,#109692,#109693,
#109694,#109695,#109696,#109697,#109698,#109699,#109700,#109701,#109702,
#109703,#109704,#109705,#109706,#109707,#109708,#109709,#109710,#109711,
#109712,#109713,#109714,#109715,#109716,#109717,#109718,#109719,#109720,
#109721,#109722,#109723,#109724,#109725,#109726,#109727,#109728,#109729,
#109730,#109731,#109732,#109733,#109734),.UNSPECIFIED.,.F.,.F.,(4,2,2,2,
2,2,2,2,2,2,2,2,2,2,2,2,2,2,2,2,2,2,4),(-0.344447890118419,-0.341211553818979,
-0.316491587765998,-0.284698969180093,-0.277510677721432,-0.272606774376936,
-0.266068464621561,-0.240741588803494,-0.208560897771362,-0.197819047043028,
-0.189289309551728,-0.178943542594523,-0.150329573893438,-0.120559673202142,
-0.113770569004943,-0.108877003813415,-0.101982213749196,-0.0784204016516493,
-0.0446107495584237,-0.0340010178915369,-0.0254774882305537,-0.0173105615643668,
-0.000450519194125924),.UNSPECIFIED.) ;
#1704 = B_SPLINE_CURVE_WITH_KNOTS('',3,(#109735,#109736,#109737,#109738,#109739,
#109740,#109741,#109742,#109743),.UNSPECIFIED.,.F.,.F.,(4,1,1,1,1,1,4),
(21.9911530646648,22.3032518321267,23.2748916143424,24.246531396558,25.2181711787737,
26.1898109609893,26.2282189766792),.UNSPECIFIED.) ;
#1705 = B_SPLINE_CURVE_WITH_KNOTS('',3,(#109749,#109750,#109751,#109752,#109753,
#109754,#109755,#109756,#109757,#109758,#109759,#109760,#109761,#109762,
#109763,#109764,#109765,#109766,#109767,#109768,#109769,#109770,#109771,
#109772,#109773,#109774,#109775,#109776,#109777,#109778,#109779,#109780,
#109781,#109782,#109783,#109784,#109785,#109786,#109787,#109788,#109789,
#109790,#109791,#109792,#109793,#109794,#109795,#109796,#109797,#109798,
#109799,#109800,#109801,#109802,#109803,#109804,#109805,#109806,#109807,
#109808,#109809,#109810,#109811,#109812,#109813,#109814,#109815,#109816,
#109817,#109818,#109819,#109820,#109821,#109822,#109823,#109824,#109825,
#109826,#109827,#109828,#109829,#109830,#109831,#109832,#109833,#109834,
#109835,#109836,#109837,#109838,#109839,#109840,#109841,#109842,#109843,
#109844,#109845,#109846,#109847,#109848,#109849,#109850,#109851,#109852,
#109853,#109854,#109855,#109856,#109857,#109858,#109859,#109860,#109861,
#109862,#109863,#109864,#109865,#109866),.UNSPECIFIED.,.F.,.F.,(4,3,3,3,
3,3,3,3,3,3,3,3,3,3,3,3,3,3,3,3,3,3,3,3,3,3,3,3,3,3,3,3,3,3,3,3,3,3,3,4),
(28.2743338823081,28.3918577636548,28.5096435278108,28.6278521981456,28.7071971005825,
28.8171687217528,28.9269585080325,29.0366468286716,29.1462735481556,29.255878446213,
29.3655761414453,29.4753179582527,29.5852551857474,29.6788368827982,29.7887989434638,
29.8985795120685,30.0082588307296,30.1178767771779,30.2274731446426,30.337162748593,
30.4468967050156,30.5568265477835,30.6504766650138,30.7603623692327,30.8700661842359,
30.9796685717358,31.0892095506955,31.1987290554581,31.3083425744435,31.4180007690804,
31.527856329468,31.6221164472294,31.733214795593,31.8431380171637,31.9529572746322,
32.0627121966772,32.1747599560424,32.2845548564219,32.39772904528,32.5109032341381),
 .UNSPECIFIED.) ;
#1706 = B_SPLINE_CURVE_WITH_KNOTS('',3,(#109867,#109868,#109869,#109870,#109871,
#109872),.UNSPECIFIED.,.F.,.F.,(4,1,1,4),(26.2282428538859,26.7639175361512,
27.7355573183669,28.2743338823081),.UNSPECIFIED.) ;
#1707 = B_SPLINE_CURVE_WITH_KNOTS('',3,(#109874,#109875,#109876,#109877,#109878,
#109879),.UNSPECIFIED.,.F.,.F.,(4,1,1,4),(26.2282189766792,27.161450743205,
28.1330905254206,28.2743338823081),.UNSPECIFIED.) ;
#1708 = B_SPLINE_CURVE_WITH_KNOTS('',3,(#109880,#109881,#109882,#109883,#109884,
#109885,#109886,#109887,#109888,#109889,#109890,#109891,#109892,#109893,
#109894,#109895,#109896,#109897,#109898,#109899,#109900,#109901,#109902,
#109903,#109904,#109905,#109906,#109907,#109908,#109909,#109910,#109911,
#109912,#109913,#109914,#109915,#109916,#109917,#109918,#109919,#109920,
#109921,#109922,#109923,#109924,#109925,#109926,#109927,#109928,#109929,
#109930,#109931,#109932,#109933,#109934,#109935,#109936,#109937,#109938,
#109939,#109940,#109941,#109942,#109943,#109944,#109945,#109946,#109947,
#109948,#109949,#109950,#109951,#109952,#109953,#109954,#109955,#109956,
#109957,#109958,#109959,#109960,#109961,#109962,#109963,#109964,#109965,
#109966,#109967,#109968,#109969,#109970,#109971,#109972,#109973,#109974,
#109975,#109976,#109977,#109978,#109979),.UNSPECIFIED.,.F.,.F.,(4,2,2,2,
2,2,2,2,2,2,2,2,2,2,2,2,2,2,2,2,2,2,2,2,2,2,2,2,2,2,2,2,2,2,2,2,2,2,2,2,
2,2,2,2,2,2,2,2,2,4),(0.712378143918981,0.712379954064215,0.72117831390082,
0.734657145018622,0.752068558527762,0.785373251131307,0.792345568546191,
0.79723963207803,0.803953757521709,0.812122008433253,0.848675628910262,
0.866001748507462,0.875321640069418,0.884058766219068,0.89712011860944,
0.913671889982011,0.949516073360798,0.956030042968438,0.960925950122258,
0.967985280014148,0.976755452934728,0.997970755917627,1.02406159262653,
1.03490881969519,1.0434433464097,1.05370359091221,1.08319754493553,1.11210683471402,
1.11898020632238,1.12387379656926,1.13068482421711,1.13901971639607,1.15811611731338,
1.18714628278811,1.19805288514865,1.20658974636888,1.21680178599216,1.24639735813157,
1.27537558519748,1.28224247880753,1.28713538887,1.2939502869039,1.30229203079242,
1.32142061052155,1.35040203680972,1.36130945627684,1.36984608699719,1.38005675842585,
1.4095946811458,1.42435463577266),.UNSPECIFIED.) ;
#1709 = B_SPLINE_CURVE_WITH_KNOTS('',3,(#109985,#109986,#109987,#109988,#109989,
#109990,#109991,#109992,#109993,#109994,#109995,#109996,#109997,#109998,
#109999,#110000,#110001,#110002,#110003,#110004,#110005,#110006,#110007,
#110008,#110009,#110010,#110011,#110012,#110013,#110014,#110015,#110016,
#110017,#110018,#110019,#110020,#110021,#110022,#110023,#110024,#110025,
#110026,#110027,#110028,#110029,#110030,#110031,#110032,#110033,#110034,
#110035,#110036,#110037,#110038,#110039,#110040,#110041,#110042,#110043,
#110044,#110045,#110046,#110047,#110048,#110049,#110050,#110051,#110052,
#110053,#110054,#110055,#110056,#110057,#110058,#110059,#110060,#110061,
#110062,#110063,#110064,#110065,#110066,#110067,#110068,#110069,#110070,
#110071,#110072,#110073,#110074,#110075,#110076,#110077,#110078),
 .UNSPECIFIED.,.F.,.F.,(4,3,3,3,3,3,3,3,3,3,3,3,3,3,3,3,3,3,3,3,3,3,3,3,
3,3,3,3,3,3,3,4),(10.3764047342417,10.4900645190595,10.5981563505387,10.7061539904157,
10.8140997864379,10.9220360039885,11.0300742467267,11.1381720731464,11.2464519829849,
11.2856830127838,11.3954831058327,11.5060464833154,11.6155542565773,11.7249978887657,
11.8344175025737,11.9458106583537,12.0553714468275,12.1676807862607,12.2799901256938,
12.3895641603662,12.5001557951459,12.6094282845871,12.7186338508099,12.8278130186388,
12.93943407363,13.0487513389406,13.1615242887721,13.2742972386037,13.3839155036222,
13.4933854860546,13.6027340815615,13.6618521794004),.UNSPECIFIED.) ;
#1710 = B_SPLINE_CURVE_WITH_KNOTS('',3,(#110081,#110082,#110083,#110084,#110085,
#110086,#110087,#110088,#110089,#110090,#110091,#110092,#110093,#110094,
#110095,#110096,#110097,#110098,#110099,#110100,#110101,#110102,#110103,
#110104,#110105,#110106,#110107,#110108,#110109,#110110,#110111,#110112,
#110113,#110114,#110115,#110116,#110117,#110118,#110119,#110120,#110121,
#110122,#110123,#110124,#110125,#110126,#110127,#110128,#110129,#110130,
#110131,#110132,#110133,#110134,#110135,#110136,#110137,#110138,#110139,
#110140),.UNSPECIFIED.,.F.,.F.,(4,2,2,2,2,2,2,2,2,2,2,2,2,2,2,2,2,2,2,2,
2,2,2,2,2,2,2,2,2,4),(-6.33424724009888,-6.3305869177302,-6.32541614156915,
-6.30776597142003,-6.28525261227357,-6.27314356015186,-6.2633690855282,
-6.25704102834557,-6.25075796634079,-6.24130885212152,-6.2018848898745,
-6.17573635588415,-6.17042441658865,-6.16711907831754,-6.16370428441967,
-6.15775527423043,-6.13753220062291,-6.11997163190395,-6.09800360015442,
-6.09050748347225,-6.08506535512531,-6.07923638089268,-6.06962378328271,
-6.02913105778434,-6.01429072948881,-6.00777656269078,-6.00256469572425,
-5.99938374041717,-5.99604989891884,-5.99053971230419),.UNSPECIFIED.) ;
#1711 = B_SPLINE_CURVE_WITH_KNOTS('',3,(#110146,#110147,#110148,#110149,#110150,
#110151,#110152,#110153,#110154,#110155,#110156,#110157,#110158,#110159,
#110160,#110161,#110162,#110163,#110164,#110165,#110166,#110167,#110168,
#110169,#110170,#110171,#110172,#110173,#110174,#110175,#110176,#110177,
#110178,#110179,#110180,#110181,#110182,#110183,#110184,#110185,#110186,
#110187,#110188,#110189,#110190,#110191,#110192,#110193,#110194,#110195,
#110196,#110197,#110198,#110199,#110200,#110201,#110202,#110203,#110204,
#110205,#110206,#110207,#110208,#110209,#110210,#110211,#110212,#110213,
#110214,#110215,#110216,#110217,#110218,#110219,#110220,#110221,#110222,
#110223,#110224,#110225,#110226,#110227,#110228,#110229,#110230,#110231,
#110232,#110233,#110234,#110235,#110236,#110237,#110238,#110239,#110240,
#110241,#110242,#110243,#110244,#110245,#110246,#110247,#110248,#110249,
#110250,#110251,#110252,#110253,#110254,#110255,#110256,#110257),
 .UNSPECIFIED.,.F.,.F.,(4,2,2,2,2,2,2,2,2,2,2,2,2,2,2,2,2,2,2,2,2,2,2,2,
2,2,2,2,2,2,2,2,2,2,2,2,2,2,2,2,2,2,2,2,2,2,2,2,2,2,2,2,2,2,2,4),(-0.712477051017104,
-0.692802655493847,-0.683772920129568,-0.677945641814678,-0.672243058678314,
-0.663900351001329,-0.630604780701155,-0.603779896817934,-0.597758211996828,
-0.594319329048754,-0.59103022263903,-0.585743272187226,-0.560611083704649,
-0.525331213931128,-0.51649143220176,-0.510699465027105,-0.504968120500479,
-0.49646209662495,-0.469169926483107,-0.436335484292804,-0.430512931507663,
-0.427114820016612,-0.42379348225532,-0.418345458607985,-0.411507449451325,
-0.39559713149191,-0.357518717259878,-0.349022553353028,-0.343864348052536,
-0.338176905527992,-0.329923428023697,-0.30068061415273,-0.268790936312498,
-0.2632130787766,-0.25986516831537,-0.256495374779357,-0.250812807680856,
-0.227712274654564,-0.190747755479028,-0.182106619482357,-0.176350235475083,
-0.170583038913043,-0.161882552302035,-0.13811727285328,-0.102004110348754,
-0.0962660030206231,-0.0928851028491788,-0.0895501348445353,-0.0840301566912476,
-0.0606491320262799,-0.0405891786089123,-0.0211129520942058,-0.0137273297259265,
-0.00825233034605935,-0.00423882998995977,-0.000487560506064013),
 .UNSPECIFIED.) ;
#1712 = B_SPLINE_CURVE_WITH_KNOTS('',3,(#110258,#110259,#110260,#110261,#110262,
#110263,#110264,#110265,#110266,#110267,#110268,#110269,#110270,#110271,
#110272,#110273,#110274,#110275,#110276,#110277,#110278,#110279,#110280,
#110281,#110282,#110283,#110284,#110285,#110286,#110287,#110288,#110289,
#110290,#110291,#110292,#110293,#110294,#110295,#110296,#110297,#110298,
#110299,#110300,#110301,#110302,#110303,#110304,#110305,#110306,#110307,
#110308,#110309,#110310,#110311,#110312,#110313,#110314,#110315),
 .UNSPECIFIED.,.F.,.F.,(4,3,3,3,3,3,3,3,3,3,3,3,3,3,3,3,3,3,3,4),(13.6618521794004,
13.7711169148501,13.88037702439,13.9897475868547,14.0991785591997,14.2088043877141,
14.2686043515136,14.3782655527654,14.4888462917227,14.5982089574048,14.7075055716608,
14.8167765076852,14.9283102468698,15.0377199986809,15.1503157315523,15.2629114644236,
15.3810391917761,15.4988692888196,15.6162446022961,15.7079632675443),
 .UNSPECIFIED.) ;
#1713 = B_SPLINE_CURVE_WITH_KNOTS('',3,(#110316,#110317,#110318,#110319,#110320,
#110321,#110322,#110323,#110324,#110325,#110326,#110327,#110328,#110329,
#110330,#110331,#110332,#110333,#110334,#110335,#110336,#110337,#110338,
#110339,#110340,#110341,#110342,#110343,#110344,#110345,#110346,#110347,
#110348,#110349,#110350,#110351,#110352,#110353,#110354,#110355,#110356,
#110357,#110358,#110359,#110360,#110361,#110362,#110363,#110364,#110365,
#110366,#110367,#110368,#110369,#110370,#110371,#110372,#110373,#110374,
#110375,#110376,#110377,#110378,#110379,#110380,#110381,#110382,#110383,
#110384,#110385,#110386,#110387,#110388,#110389,#110390,#110391,#110392,
#110393,#110394,#110395,#110396,#110397,#110398,#110399,#110400,#110401,
#110402,#110403,#110404,#110405,#110406,#110407,#110408,#110409,#110410,
#110411,#110412,#110413,#110414,#110415,#110416,#110417,#110418,#110419,
#110420,#110421,#110422,#110423,#110424,#110425,#110426,#110427,#110428,
#110429,#110430,#110431,#110432,#110433,#110434,#110435,#110436,#110437,
#110438,#110439,#110440,#110441,#110442,#110443,#110444,#110445,#110446,
#110447,#110448,#110449,#110450,#110451,#110452,#110453,#110454,#110455,
#110456,#110457,#110458,#110459,#110460,#110461,#110462,#110463,#110464,
#110465,#110466,#110467,#110468,#110469,#110470,#110471,#110472,#110473,
#110474,#110475),.UNSPECIFIED.,.F.,.F.,(4,2,2,2,2,2,2,2,2,2,2,2,2,2,2,2,
2,2,2,2,2,2,2,2,2,2,2,2,2,2,2,2,2,2,2,2,2,2,2,2,2,2,2,2,2,2,2,2,2,2,2,2,
2,2,2,2,2,2,2,2,2,2,2,2,2,2,2,2,2,2,2,2,2,2,2,2,2,2,2,4),(-5.99053971230419,
-5.99047461915376,-5.95863408749524,-5.92969933625071,-5.92114681247369,
-5.915382578984,-5.90955220244452,-5.90062838830993,-5.87701819018997,-5.85236394846719,
-5.84376533328685,-5.8373135536108,-5.83375945007048,-5.83052134715155,
-5.82542463673811,-5.80505229717849,-5.77693764917991,-5.76556984118265,
-5.75625855327928,-5.75035861651557,-5.7447229240835,-5.73656342255167,
-5.69603857832968,-5.68123878905728,-5.67467388255143,-5.66938441896224,
-5.6660855631516,-5.66265149068689,-5.65661618350724,-5.62976488185456,
-5.59655621591346,-5.58823493236518,-5.58255620616837,-5.57744225437469,
-5.56910919109571,-5.52835464098746,-5.51380877876097,-5.50732381078696,
-5.50209177678022,-5.49882403274683,-5.49538334870154,-5.48934624246608,
-5.46251397712469,-5.42923993509709,-5.4209137181702,-5.41521229709611,
-5.41006365996861,-5.40163487145359,-5.36317618148174,-5.34096910239947,
-5.33541870518404,-5.33207440806664,-5.32869619298517,-5.32297321551596,
-5.29245413663171,-5.26226599070794,-5.2539712036158,-5.24827681786533,
-5.24243800882422,-5.23334744843942,-5.20142115753318,-5.17348278738021,
-5.16816968985747,-5.16487583020783,-5.16144680644824,-5.15546548539489,
-5.12795602433186,-5.0955345838297,-5.08709883194831,-5.0813835504828,-5.07558361949721,
-5.06668208643157,-5.03201451159366,-5.00644599200698,-5.00112565663733,
-4.99783192271362,-4.99440511132734,-4.98843793496379,-4.95371727216649,
-4.9350521817335),.UNSPECIFIED.) ;
#1714 = B_SPLINE_CURVE_WITH_KNOTS('',3,(#110480,#110481,#110482,#110483,#110484,
#110485,#110486,#110487,#110488,#110489,#110490,#110491,#110492,#110493,
#110494,#110495,#110496,#110497,#110498,#110499,#110500,#110501,#110502,
#110503,#110504,#110505,#110506,#110507,#110508,#110509,#110510,#110511,
#110512,#110513,#110514,#110515,#110516,#110517,#110518,#110519,#110520,
#110521,#110522,#110523,#110524,#110525,#110526,#110527,#110528,#110529,
#110530,#110531,#110532,#110533,#110534,#110535,#110536,#110537,#110538,
#110539,#110540,#110541,#110542,#110543,#110544,#110545,#110546,#110547,
#110548,#110549,#110550,#110551,#110552,#110553,#110554,#110555,#110556,
#110557,#110558,#110559,#110560,#110561,#110562,#110563,#110564,#110565,
#110566,#110567,#110568,#110569,#110570,#110571,#110572,#110573,#110574,
#110575,#110576,#110577,#110578,#110579,#110580,#110581,#110582,#110583,
#110584,#110585,#110586,#110587,#110588,#110589,#110590,#110591,#110592,
#110593,#110594,#110595,#110596,#110597,#110598,#110599,#110600,#110601,
#110602,#110603,#110604,#110605,#110606,#110607,#110608,#110609,#110610,
#110611,#110612,#110613,#110614,#110615,#110616,#110617,#110618,#110619,
#110620,#110621,#110622,#110623,#110624,#110625,#110626,#110627,#110628,
#110629,#110630,#110631,#110632,#110633,#110634,#110635,#110636,#110637,
#110638,#110639,#110640,#110641,#110642,#110643),.UNSPECIFIED.,.F.,.F.,
(4,2,2,2,2,2,2,2,2,2,2,2,2,2,2,2,2,2,2,2,2,2,2,2,2,2,2,2,2,2,2,2,2,2,2,
2,2,2,2,2,2,2,2,2,2,2,2,2,2,2,2,2,2,2,2,2,2,2,2,2,2,2,2,2,2,2,2,2,2,2,2,
2,2,2,2,2,2,2,2,2,2,4),(-1.76818356378078,-1.76666210863979,-1.76335874747055,
-1.75993953124951,-1.75401304730633,-1.7261788047067,-1.69407326476353,
-1.68558675228945,-1.67985926096194,-1.67406390562458,-1.66520393482846,
-1.63010226962174,-1.60561277861248,-1.59990800700045,-1.59653437101539,
-1.5931919816856,-1.58763889989772,-1.55556687777865,-1.52720892284277,
-1.5186289076951,-1.5128845673421,-1.50710766903938,-1.49834858149115,-1.46232917555678,
-1.43790919774604,-1.43254040047344,-1.42923527159702,-1.42581814563762,
-1.41990211094776,-1.39200096337258,-1.37007954259637,-1.36001416862498,
-1.35150084664892,-1.34576835606398,-1.33997808174755,-1.33114681658688,
-1.29576757956943,-1.27111086695335,-1.2656091204,-1.26227714970592,-1.2588918091262,
-1.25313088766896,-1.22300159181825,-1.19232624188739,-1.1840951061917,
-1.17841204248402,-1.17325077710014,-1.16473296027604,-1.12680166285061,
-1.11081344178922,-1.10395627554512,-1.09849739707728,-1.09517412141265,
-1.09177887023573,-1.08596972878113,-1.05647958053428,-1.02710225847862,
-1.01799436632724,-1.0121526839847,-1.0064613458708,-0.998182189048535,
-0.968373423054622,-0.937279229744221,-0.931613068231424,-0.928247271935606,
-0.924897021545374,-0.919306345738125,-0.912225740972987,-0.89530601260113,
-0.859324571674764,-0.850563538847296,-0.844786048445886,-0.839041581798305,
-0.830462374491692,-0.802250305773277,-0.76995397365888,-0.764423281997596,
-0.761085322112715,-0.75770626514405,-0.751976387823087,-0.72590084049544,
-0.712477051017104),.UNSPECIFIED.) ;
#1715 = B_SPLINE_CURVE_WITH_KNOTS('',3,(#110644,#110645,#110646,#110647,#110648,
#110649,#110650,#110651,#110652,#110653,#110654,#110655,#110656,#110657,
#110658,#110659,#110660,#110661,#110662,#110663,#110664,#110665,#110666,
#110667,#110668,#110669,#110670,#110671,#110672,#110673,#110674,#110675,
#110676,#110677,#110678,#110679,#110680,#110681,#110682,#110683,#110684,
#110685,#110686,#110687,#110688,#110689,#110690,#110691,#110692,#110693,
#110694,#110695,#110696,#110697,#110698,#110699,#110700,#110701,#110702,
#110703,#110704,#110705,#110706,#110707,#110708,#110709,#110710,#110711,
#110712,#110713,#110714,#110715,#110716,#110717,#110718,#110719,#110720,
#110721,#110722,#110723,#110724,#110725,#110726,#110727,#110728,#110729,
#110730,#110731,#110732,#110733,#110734,#110735,#110736,#110737,#110738,
#110739,#110740,#110741,#110742,#110743,#110744,#110745,#110746,#110747,
#110748,#110749,#110750,#110751,#110752,#110753,#110754,#110755,#110756,
#110757,#110758,#110759,#110760,#110761,#110762,#110763,#110764,#110765,
#110766,#110767,#110768,#110769,#110770,#110771,#110772,#110773,#110774,
#110775,#110776,#110777,#110778,#110779,#110780,#110781,#110782,#110783,
#110784,#110785,#110786,#110787,#110788,#110789,#110790,#110791,#110792,
#110793,#110794,#110795,#110796,#110797,#110798,#110799,#110800,#110801,
#110802,#110803,#110804,#110805,#110806,#110807,#110808,#110809),
 .UNSPECIFIED.,.F.,.F.,(4,2,2,2,2,2,2,2,2,2,2,2,2,2,2,2,2,2,2,2,2,2,2,2,
2,2,2,2,2,2,2,2,2,2,2,2,2,2,2,2,2,2,2,2,2,2,2,2,2,2,2,2,2,2,2,2,2,2,2,2,
2,2,2,2,2,2,2,2,2,2,2,2,2,2,2,2,2,2,2,2,2,2,4),(-4.9350521817335,-4.92924063431001,
-4.92044239877843,-4.91465940528696,-4.90892351641425,-4.90038456224455,
-4.86264847290703,-4.84658277607218,-4.8397074909766,-4.83423827443184,
-4.83091341750573,-4.82752198218248,-4.82172782759203,-4.79203898950566,
-4.77112106687337,-4.76130259504078,-4.75294376002215,-4.74724004938001,
-4.74141951950012,-4.73241737215319,-4.69892832381971,-4.6728214363707,
-4.66728213436687,-4.66394329293773,-4.66056834654829,-4.65485352521452,
-4.62426640486569,-4.59411722047284,-4.58582595290027,-4.58013430875787,
-4.57429882728677,-4.56521504374047,-4.53318283650538,-4.50616750618709,
-4.50042352036627,-4.49704259355698,-4.49411219504707,-4.48902115662041,
-4.46748769556528,-4.44020461262813,-4.42900107160256,-4.41979655965162,
-4.41393804178965,-4.40832682243432,-4.40017938091833,-4.35965849168015,
-4.34482640449425,-4.3382611866649,-4.33297664176318,-4.32968873335359,
-4.32625095373141,-4.32023086486532,-4.29342481673317,-4.26015236585617,
-4.25181104174667,-4.24611029313889,-4.24028564120251,-4.23126189696331,
-4.19807637418412,-4.17162792408406,-4.16613041753203,-4.16280001841052,
-4.15941534758802,-4.15365421993062,-4.12354614187762,-4.09338197576611,
-4.08491495060093,-4.0791920594429,-4.07339477872434,-4.06451836754818,
-4.02959475019793,-4.00439138334853,-3.99899340105477,-3.99568309549955,
-3.99227477190073,-3.98639863391994,-3.95113205383628,-3.92694774181241,
-3.91819047658281,-3.91241514624073,-3.90667266451009,-3.89809625365554,
-3.87952612660362),.UNSPECIFIED.) ;
#1716 = B_SPLINE_CURVE_WITH_KNOTS('',3,(#110815,#110816,#110817,#110818,#110819,
#110820,#110821,#110822,#110823,#110824,#110825,#110826,#110827,#110828,
#110829,#110830,#110831,#110832,#110833,#110834,#110835,#110836,#110837,
#110838,#110839,#110840,#110841,#110842,#110843,#110844,#110845,#110846,
#110847,#110848,#110849,#110850,#110851,#110852,#110853,#110854,#110855,
#110856,#110857,#110858,#110859,#110860,#110861,#110862,#110863,#110864,
#110865,#110866,#110867,#110868,#110869,#110870,#110871,#110872,#110873,
#110874,#110875,#110876,#110877,#110878,#110879,#110880,#110881,#110882,
#110883,#110884,#110885,#110886,#110887,#110888,#110889,#110890,#110891,
#110892,#110893,#110894,#110895,#110896,#110897,#110898,#110899,#110900,
#110901,#110902,#110903,#110904,#110905,#110906,#110907,#110908,#110909,
#110910,#110911,#110912,#110913,#110914,#110915,#110916),.UNSPECIFIED.,
 .F.,.F.,(4,2,2,2,2,2,2,2,2,2,2,2,2,2,2,2,2,2,2,2,2,2,2,2,2,2,2,2,2,2,2,
2,2,2,2,2,2,2,2,2,2,2,2,2,2,2,2,2,2,2,4),(-0.712560310195096,-0.696927543742108,
-0.664393756377226,-0.658308473226922,-0.654856627884361,-0.65157642714292,
-0.646335858781874,-0.619824553094956,-0.586138170659426,-0.577149854410368,
-0.571330128691633,-0.565621274854638,-0.557243683240465,-0.52515271781851,
-0.496938482436241,-0.491060214402507,-0.487650558070128,-0.484338641962742,
-0.478937515505729,-0.453679571810099,-0.41884006969134,-0.409954338268172,
-0.404153524304069,-0.398428867282295,-0.389962470359715,-0.360362849023259,
-0.329508722091577,-0.3238157222087,-0.320444136084627,-0.317098690632935,
-0.311532565593602,-0.287426221779339,-0.251506631916206,-0.242737154611523,
-0.236957694377381,-0.231213934171252,-0.222641014264426,-0.194841718838807,
-0.16199081489796,-0.156522544681182,-0.153197069938858,-0.149803377221981,
-0.144003303274408,-0.124995580033334,-0.0846985680180007,-0.075785096394773,
-0.0699791943610914,-0.0642589396352745,-0.0558170987592085,-0.0233685145724937,
-0.000486898249177208),.UNSPECIFIED.) ;
#1717 = B_SPLINE_CURVE_WITH_KNOTS('',3,(#110917,#110918,#110919,#110920,#110921,
#110922,#110923,#110924,#110925,#110926,#110927,#110928,#110929,#110930,
#110931,#110932,#110933,#110934,#110935,#110936,#110937,#110938,#110939,
#110940,#110941,#110942,#110943,#110944,#110945,#110946,#110947,#110948,
#110949,#110950,#110951,#110952,#110953,#110954,#110955,#110956,#110957,
#110958,#110959,#110960,#110961,#110962,#110963,#110964,#110965,#110966,
#110967,#110968,#110969,#110970,#110971,#110972,#110973,#110974),
 .UNSPECIFIED.,.F.,.F.,(4,2,2,2,2,2,2,2,2,2,2,2,2,2,2,2,2,2,2,2,2,2,2,2,
2,2,2,2,4),(-2.11192746243384,-2.10365836072938,-2.10032748721145,-2.09739905319525,
-2.09395618783264,-2.0879135511067,-2.0618322929545,-2.05345777211631,-2.02888579184874,
-2.0200732276697,-2.01428663417168,-2.00855143726169,-2.00002183872159,
-1.96218415944355,-1.94615428816371,-1.93928708674953,-1.93382235705294,
-1.93049802943554,-1.92710441440501,-1.92130264175917,-1.89170157783663,
-1.86141009373834,-1.85279580594553,-1.84704537799896,-1.84127518605679,
-1.83255223671774,-1.79622972800035,-1.77202226703003,-1.76818356378078),
 .UNSPECIFIED.) ;
#1718 = B_SPLINE_CURVE_WITH_KNOTS('',3,(#110975,#110976,#110977,#110978,#110979,
#110980,#110981,#110982,#110983,#110984,#110985,#110986,#110987,#110988,
#110989,#110990,#110991,#110992,#110993,#110994,#110995,#110996,#110997,
#110998,#110999,#111000,#111001,#111002,#111003,#111004,#111005,#111006,
#111007,#111008,#111009,#111010,#111011,#111012,#111013,#111014,#111015,
#111016,#111017,#111018,#111019,#111020,#111021,#111022,#111023,#111024,
#111025,#111026,#111027,#111028,#111029,#111030,#111031,#111032,#111033,
#111034,#111035,#111036,#111037,#111038,#111039,#111040,#111041,#111042,
#111043,#111044,#111045,#111046,#111047,#111048,#111049,#111050,#111051,
#111052,#111053,#111054,#111055,#111056,#111057,#111058,#111059,#111060,
#111061,#111062,#111063,#111064,#111065,#111066,#111067,#111068,#111069,
#111070,#111071,#111072,#111073,#111074,#111075,#111076,#111077,#111078,
#111079,#111080,#111081,#111082,#111083,#111084,#111085,#111086,#111087,
#111088,#111089,#111090,#111091,#111092,#111093,#111094,#111095,#111096,
#111097,#111098,#111099,#111100,#111101,#111102,#111103,#111104,#111105,
#111106,#111107,#111108,#111109,#111110,#111111,#111112,#111113,#111114,
#111115,#111116,#111117,#111118,#111119,#111120,#111121,#111122,#111123,
#111124,#111125,#111126,#111127,#111128,#111129,#111130,#111131,#111132,
#111133,#111134,#111135,#111136,#111137,#111138,#111139,#111140),
 .UNSPECIFIED.,.F.,.F.,(4,2,2,2,2,2,2,2,2,2,2,2,2,2,2,2,2,2,2,2,2,2,2,2,
2,2,2,2,2,2,2,2,2,2,2,2,2,2,2,2,2,2,2,2,2,2,2,2,2,2,2,2,2,2,2,2,2,2,2,2,
2,2,2,2,2,2,2,2,2,2,2,2,2,2,2,2,2,2,2,2,2,2,4),(-3.87952612660362,-3.86062568452188,
-3.84442601515873,-3.83751797114886,-3.83202943311297,-3.82870086247565,
-3.82531413862114,-3.81954303164399,-3.78955091772268,-3.7592912808188,
-3.7508234548549,-3.7451004257672,-3.73930331754311,-3.73042781496521,-3.6954957738308,
-3.67029896598693,-3.66490124106473,-3.661590990245,-3.65818262332641,-3.65230620949632,
-3.62412515274316,-3.5920459744581,-3.58367034575224,-3.57796362120538,
-3.57214672886548,-3.56316448102137,-3.52941186474604,-3.50302060509746,
-3.49774346021087,-3.49445708491337,-3.49101745410518,-3.48498800924908,
-3.4581560142016,-3.42487758809319,-3.41655914447765,-3.41086247708157,
-3.40503275253428,-3.39598133942955,-3.37005366899035,-3.34641573350646,
-3.33797448860644,-3.33161560747389,-3.32810952227488,-3.32490391984474,
-3.319885547723,-3.30123149955326,-3.27984059566937,-3.26413966465563,-3.25247692687625,
-3.24615940815198,-3.24063956259222,-3.23357099957884,-3.21846630144393,
-3.18244798671489,-3.16773500197394,-3.16305806015763,-3.15987674157065,
-3.15621982427784,-3.14908667546599,-3.11755196697434,-3.09237116509003,
-3.08332238548082,-3.07749299246945,-3.07179562991928,-3.06347434404492,
-3.03018176236825,-3.0033288158175,-2.99730399144291,-2.99386520520512,
-2.99057789569833,-2.98529675938854,-2.95999947546801,-2.92493103033546,
-2.91607175218247,-2.91027740623184,-2.90455134575136,-2.89606802224394,
-2.88604934852181,-2.86432142289227,-2.83600264401299,-2.83013743101675,
-2.82673127717738,-2.82399026850942),.UNSPECIFIED.) ;
#1719 = B_SPLINE_CURVE_WITH_KNOTS('',3,(#111145,#111146,#111147,#111148,#111149,
#111150,#111151,#111152,#111153,#111154,#111155,#111156,#111157,#111158,
#111159,#111160,#111161,#111162,#111163,#111164,#111165,#111166,#111167,
#111168,#111169,#111170,#111171,#111172,#111173,#111174,#111175,#111176,
#111177,#111178,#111179,#111180,#111181,#111182,#111183,#111184,#111185,
#111186,#111187,#111188,#111189,#111190,#111191,#111192,#111193,#111194,
#111195,#111196,#111197,#111198,#111199,#111200,#111201,#111202,#111203,
#111204,#111205,#111206,#111207,#111208,#111209,#111210,#111211,#111212,
#111213,#111214,#111215,#111216,#111217,#111218,#111219,#111220,#111221,
#111222,#111223,#111224,#111225,#111226,#111227,#111228,#111229,#111230,
#111231,#111232,#111233,#111234,#111235,#111236,#111237,#111238,#111239,
#111240,#111241,#111242,#111243,#111244,#111245,#111246,#111247,#111248,
#111249,#111250,#111251,#111252,#111253,#111254,#111255,#111256,#111257,
#111258,#111259,#111260,#111261,#111262,#111263,#111264,#111265,#111266,
#111267,#111268,#111269,#111270,#111271,#111272,#111273,#111274,#111275,
#111276,#111277,#111278,#111279,#111280,#111281,#111282,#111283,#111284,
#111285,#111286,#111287,#111288,#111289,#111290,#111291,#111292,#111293,
#111294,#111295,#111296,#111297,#111298,#111299,#111300,#111301,#111302,
#111303,#111304,#111305,#111306),.UNSPECIFIED.,.F.,.F.,(4,2,2,2,2,2,2,2,
2,2,2,2,2,2,2,2,2,2,2,2,2,2,2,2,2,2,2,2,2,2,2,2,2,2,2,2,2,2,2,2,2,2,2,2,
2,2,2,2,2,2,2,2,2,2,2,2,2,2,2,2,2,2,2,2,2,2,2,2,2,2,2,2,2,2,2,2,2,2,2,2,
4),(-1.76829897325153,-1.75460392163481,-1.74611762918806,-1.74038984818434,
-1.73459384330885,-1.72573211997339,-1.69063835242174,-1.66555260637465,
-1.66015783335173,-1.65684745379245,-1.65343685955817,-1.64755255118024,
-1.61942449203402,-1.58730905211199,-1.57892593974264,-1.57321674186153,
-1.56739935178262,-1.55842050573739,-1.52459629337172,-1.49855014186046,
-1.49312071830056,-1.48980351553656,-1.48640137667395,-1.48055862353011,
-1.44508483627295,-1.42100550335908,-1.41226161927158,-1.40648741653162,
-1.40074025349759,-1.39214525728931,-1.35479931095745,-1.33167692340998,
-1.32614191424939,-1.32280313343559,-1.31942525780903,-1.31370051849044,
-1.28319005419036,-1.25297473638803,-1.24467823110622,-1.23898392491907,
-1.2331463645208,-1.22406051627092,-1.19201073794918,-1.16500246036131,
-1.15925695802786,-1.15587482220384,-1.15253997060442,-1.14702422880595,
-1.11462133444451,-1.08535977678247,-1.07730603012133,-1.07165280267554,
-1.06575282050299,-1.0563353966255,-1.02697771227102,-0.998098672414146,
-0.992262514355829,-0.988861694626336,-0.985543012286294,-0.98010727071304,
-0.973289789452838,-0.957461674297307,-0.919211833316843,-0.9107404145102,
-0.905586573923107,-0.899895806731126,-0.891620532261262,-0.861899771527197,
-0.830682611318693,-0.825029788918696,-0.821666696298092,-0.81831367031811,
-0.812709721714768,-0.805606455171284,-0.788590340785238,-0.752797444912451,
-0.74401456566953,-0.738233003103442,-0.732492126687357,-0.723933250484363,
-0.712560310195096),.UNSPECIFIED.) ;
#1720 = B_SPLINE_CURVE_WITH_KNOTS('',3,(#111307,#111308,#111309,#111310,#111311,
#111312,#111313,#111314,#111315,#111316,#111317,#111318,#111319,#111320,
#111321,#111322,#111323,#111324,#111325,#111326,#111327,#111328,#111329,
#111330,#111331,#111332,#111333,#111334,#111335,#111336,#111337,#111338,
#111339,#111340,#111341,#111342,#111343,#111344,#111345,#111346,#111347,
#111348,#111349,#111350,#111351,#111352,#111353,#111354,#111355,#111356,
#111357,#111358,#111359,#111360,#111361,#111362,#111363,#111364,#111365,
#111366,#111367,#111368,#111369,#111370,#111371,#111372,#111373,#111374,
#111375,#111376,#111377,#111378,#111379,#111380,#111381,#111382,#111383,
#111384,#111385,#111386,#111387,#111388,#111389,#111390,#111391,#111392,
#111393,#111394,#111395,#111396,#111397,#111398,#111399,#111400,#111401,
#111402,#111403,#111404,#111405,#111406,#111407,#111408,#111409,#111410,
#111411,#111412,#111413,#111414,#111415,#111416,#111417,#111418,#111419,
#111420,#111421,#111422,#111423,#111424,#111425,#111426,#111427,#111428,
#111429,#111430,#111431,#111432,#111433,#111434,#111435,#111436,#111437,
#111438,#111439,#111440,#111441,#111442,#111443,#111444,#111445,#111446,
#111447,#111448,#111449,#111450,#111451,#111452,#111453,#111454,#111455,
#111456,#111457,#111458,#111459,#111460,#111461,#111462,#111463,#111464,
#111465,#111466,#111467,#111468),.UNSPECIFIED.,.F.,.F.,(4,2,2,2,2,2,2,2,
2,2,2,2,2,2,2,2,2,2,2,2,2,2,2,2,2,2,2,2,2,2,2,2,2,2,2,2,2,2,2,2,2,2,2,2,
2,2,2,2,2,2,2,2,2,2,2,2,2,2,2,2,2,2,2,2,2,2,2,2,2,2,2,2,2,2,2,2,2,2,2,2,
4),(-2.82399026850942,-2.82341890687629,-2.81801132306273,-2.79253919112659,
-2.75799980550302,-2.74908808182721,-2.74328402892283,-2.73756618862353,
-2.72912918990773,-2.69797579532232,-2.66887982531938,-2.66305181517914,
-2.65965324196555,-2.65633440963625,-2.65089498863588,-2.64407077120943,
-2.62821305750453,-2.59003369288838,-2.58155457207929,-2.57640052065259,
-2.57071300498161,-2.56244987304937,-2.53296005495871,-2.50142691207352,
-2.4958106358921,-2.49245568167594,-2.48909648100377,-2.48345980855283,
-2.456974533545,-2.42415276243805,-2.41510756047844,-2.40927853774309,-2.40358016901041,
-2.39525485839727,-2.36196088688736,-2.33510849801988,-2.3290854951205,
-2.32564692129078,-2.32235904506188,-2.31707583991493,-2.31051361107425,
-2.29569318899404,-2.25516488421965,-2.24702024182607,-2.24140908540174,
-2.23554906495507,-2.2263388407737,-2.21512519677322,-2.18779871835891,
-2.16629308856763,-2.16120069777036,-2.15826981502894,-2.15488845048444,
-2.14914429800924,-2.14179899911136,-2.12372082221965,-2.08990279265047,
-2.08092730936326,-2.07511128899889,-2.06940285603707,-2.06101995164008,
-2.02889883164275,-2.00075263773878,-1.99486799858886,-1.99145772928818,
-1.98814835522146,-1.98275634484835,-1.95771002465056,-1.922592074612,-1.91373719119365,
-1.90794342607117,-1.90221626915163,-1.89372810144114,-1.86159458878002,
-1.83377362628468,-1.82784069540986,-1.82442048288859,-1.82111879767998,
-1.81576572041569,-1.79171101232918,-1.76831699902817),.UNSPECIFIED.) ;
#1721 = B_SPLINE_CURVE_WITH_KNOTS('',3,(#111474,#111475,#111476,#111477,#111478,
#111479,#111480,#111481,#111482,#111483,#111484,#111485,#111486,#111487,
#111488,#111489,#111490,#111491,#111492,#111493,#111494,#111495,#111496,
#111497,#111498,#111499,#111500,#111501,#111502,#111503,#111504,#111505,
#111506,#111507,#111508,#111509,#111510,#111511,#111512,#111513,#111514,
#111515,#111516,#111517,#111518,#111519,#111520,#111521,#111522,#111523,
#111524,#111525,#111526,#111527,#111528,#111529,#111530,#111531,#111532,
#111533,#111534,#111535,#111536,#111537,#111538,#111539,#111540,#111541,
#111542,#111543,#111544,#111545,#111546,#111547,#111548,#111549,#111550,
#111551,#111552,#111553,#111554,#111555,#111556,#111557,#111558,#111559,
#111560,#111561,#111562,#111563,#111564,#111565,#111566,#111567,#111568,
#111569,#111570,#111571,#111572,#111573,#111574,#111575,#111576,#111577,
#111578,#111579,#111580,#111581,#111582,#111583,#111584,#111585,#111586,
#111587,#111588),.UNSPECIFIED.,.F.,.F.,(4,3,3,3,3,3,3,3,3,3,3,3,3,3,3,3,
3,3,3,3,3,3,3,3,3,3,3,3,3,3,3,3,3,3,3,3,3,3,4),(40.8407044969695,40.9778004485257,
41.1148964000819,41.2245591175802,41.3351396670066,41.4445029598726,41.5537998679094,
41.6630707648349,41.7746039518741,41.8840128460614,41.9966081795266,42.1092035129918,
42.2188516823835,42.3294340503233,42.4387834441433,42.5480667322124,42.6573243083354,
42.768870887727,42.8782673433037,42.9908889846027,43.1035106259017,43.2130813463413,
43.3236733954001,43.4329445134416,43.5421494364015,43.6513286879563,43.7629509506701,
43.8722700890464,43.985043913929,44.0978177388117,44.2076327245732,44.3172547150156,
44.4267684933025,44.536214279915,44.6456322030823,44.7551374325598,44.8646820423166,
44.9744233938719,45.0774317841423),.UNSPECIFIED.) ;
#1722 = B_SPLINE_CURVE_WITH_KNOTS('',3,(#111589,#111590,#111591,#111592,#111593,
#111594,#111595,#111596,#111597,#111598,#111599,#111600,#111601,#111602,
#111603,#111604,#111605,#111606,#111607,#111608,#111609,#111610,#111611,
#111612,#111613,#111614,#111615,#111616,#111617,#111618,#111619,#111620,
#111621,#111622,#111623,#111624,#111625,#111626,#111627,#111628,#111629,
#111630,#111631,#111632,#111633,#111634,#111635,#111636,#111637,#111638,
#111639,#111640,#111641,#111642,#111643,#111644),.UNSPECIFIED.,.F.,.F.,
(4,2,2,2,2,2,2,2,2,2,2,2,2,2,2,2,2,2,2,2,2,2,2,2,2,2,2,4),(-2.11228412499268,
-2.09589069751274,-2.08616970041209,-2.08037589962005,-2.07463269380149,
-2.0688595433906,-2.06011197044276,-2.0235776218593,-2.0069774997407,-1.99997283546138,
-1.99442747362915,-1.99108766548718,-1.98771301743009,-1.98200388162584,
-1.95133971005555,-1.92190326785172,-1.91330335441766,-1.90755485784521,
-1.9017807039189,-1.8930396354663,-1.85687418159894,-1.83256461598671,-1.82719981502227,
-1.82389505434892,-1.82047618598876,-1.81455254885302,-1.78669711134918,
-1.76829897325153),.UNSPECIFIED.) ;
#1723 = B_SPLINE_CURVE_WITH_KNOTS('',3,(#111645,#111646,#111647,#111648,#111649,
#111650,#111651,#111652,#111653,#111654,#111655,#111656,#111657,#111658,
#111659,#111660,#111661,#111662,#111663,#111664,#111665,#111666,#111667,
#111668,#111669,#111670,#111671,#111672,#111673,#111674,#111675,#111676,
#111677,#111678,#111679,#111680,#111681,#111682,#111683,#111684,#111685,
#111686,#111687,#111688,#111689,#111690,#111691,#111692,#111693,#111694,
#111695,#111696,#111697,#111698,#111699,#111700,#111701,#111702,#111703,
#111704,#111705,#111706,#111707,#111708,#111709,#111710,#111711,#111712,
#111713,#111714,#111715,#111716,#111717,#111718,#111719,#111720,#111721,
#111722,#111723,#111724,#111725,#111726,#111727,#111728,#111729,#111730,
#111731,#111732,#111733,#111734,#111735,#111736,#111737,#111738,#111739,
#111740,#111741,#111742,#111743,#111744,#111745,#111746,#111747,#111748,
#111749,#111750,#111751,#111752,#111753,#111754,#111755,#111756,#111757,
#111758,#111759,#111760,#111761,#111762,#111763,#111764,#111765,#111766,
#111767,#111768,#111769,#111770,#111771,#111772,#111773,#111774,#111775,
#111776,#111777,#111778,#111779,#111780,#111781,#111782,#111783,#111784,
#111785,#111786,#111787,#111788,#111789,#111790,#111791,#111792,#111793,
#111794,#111795,#111796,#111797,#111798,#111799,#111800,#111801,#111802,
#111803,#111804,#111805,#111806,#111807,#111808),.UNSPECIFIED.,.F.,.F.,
(4,2,2,2,2,2,2,2,2,2,2,2,2,2,2,2,2,2,2,2,2,2,2,2,2,2,2,2,2,2,2,2,2,2,2,
2,2,2,2,2,2,2,2,2,2,2,2,2,2,2,2,2,2,2,2,2,2,2,2,2,2,2,2,2,2,2,2,2,2,2,2,
2,2,2,2,2,2,2,2,2,2,4),(-1.76831699902817,-1.75518964805716,-1.7464939967529,
-1.74072931780407,-1.73497502618634,-1.72633662398727,-1.69475416514867,
-1.66661632486612,-1.66073017475442,-1.65731947814099,-1.65401004875575,
-1.64861855660536,-1.62359288966011,-1.58844479684806,-1.57959255588087,
-1.57379900488342,-1.56807094121945,-1.55957925089772,-1.52737702425792,
-1.49966150675423,-1.49370975209278,-1.49028556586819,-1.48698678312783,
-1.48164844322083,-1.45555171790032,-1.42160028807763,-1.41263445446714,
-1.40681995276556,-1.40110964628147,-1.39271766668299,-1.36054972024335,
-1.33248078779257,-1.32658507794482,-1.32317237433183,-1.31986434892612,
-1.3144804660512,-1.28966197107827,-1.25422061233062,-1.24539843861857,
-1.23961009702442,-1.23387658404469,-1.22535624893443,-1.19575074172621,
-1.16505376690443,-1.15934496571757,-1.15597044251782,-1.15262831875543,
-1.14707799948981,-1.12489509543687,-1.08629569001683,-1.07787376642098,
-1.07272788441997,-1.06702884083304,-1.05870563516865,-1.02540582083539,
-0.998547257588233,-0.992520046801463,-0.989080304812647,-0.985794181702154,
-0.980516494618136,-0.97396305824982,-0.959175820696547,-0.918536689606294,
-0.910405236709954,-0.904797500956223,-0.898936632101549,-0.889715679414612,
-0.878483193532081,-0.851054163825655,-0.829681793148376,-0.824590238282511,
-0.821659670394674,-0.818276870565965,-0.812530368884856,-0.805182019449805,
-0.787095435655023,-0.753274574776637,-0.744294657821547,-0.738475350004387,
-0.732763203677629,-0.724373493863662,-0.712529018801462),.UNSPECIFIED.) ;
#1724 = B_SPLINE_CURVE_WITH_KNOTS('',3,(#111816,#111817,#111818,#111819,#111820,
#111821,#111822,#111823),.UNSPECIFIED.,.F.,.F.,(4,1,1,1,1,4),(-27.2059139020381,
-26.2342741198224,-25.2626343376068,-24.2909945553912,-23.3193547731755,
-22.9423101900986),.UNSPECIFIED.) ;
#1725 = B_SPLINE_CURVE_WITH_KNOTS('',3,(#111825,#111826,#111827,#111828,#111829,
#111830,#111831,#111832,#111833,#111834,#111835,#111836,#111837,#111838,
#111839,#111840,#111841,#111842,#111843,#111844,#111845,#111846,#111847,
#111848,#111849,#111850,#111851,#111852,#111853,#111854,#111855,#111856,
#111857,#111858,#111859,#111860,#111861,#111862,#111863,#111864,#111865,
#111866,#111867,#111868,#111869,#111870,#111871,#111872,#111873,#111874,
#111875,#111876,#111877,#111878,#111879,#111880,#111881,#111882,#111883,
#111884,#111885,#111886,#111887,#111888,#111889,#111890,#111891,#111892,
#111893,#111894,#111895,#111896,#111897,#111898,#111899,#111900,#111901,
#111902,#111903,#111904,#111905,#111906,#111907,#111908,#111909,#111910,
#111911,#111912,#111913,#111914,#111915,#111916,#111917,#111918,#111919,
#111920,#111921,#111922,#111923,#111924,#111925,#111926,#111927,#111928,
#111929,#111930,#111931,#111932,#111933,#111934,#111935,#111936,#111937,
#111938,#111939,#111940,#111941,#111942,#111943,#111944,#111945,#111946,
#111947,#111948,#111949,#111950,#111951,#111952,#111953,#111954,#111955,
#111956,#111957,#111958,#111959,#111960,#111961,#111962,#111963,#111964,
#111965,#111966,#111967,#111968,#111969,#111970,#111971,#111972,#111973,
#111974,#111975,#111976,#111977,#111978,#111979,#111980,#111981,#111982,
#111983,#111984,#111985,#111986,#111987,#111988,#111989,#111990,#111991,
#111992,#111993,#111994,#111995,#111996,#111997,#111998,#111999,#112000,
#112001,#112002,#112003,#112004,#112005,#112006,#112007,#112008,#112009,
#112010,#112011,#112012,#112013,#112014,#112015,#112016,#112017),
 .UNSPECIFIED.,.F.,.F.,(4,3,3,3,3,3,3,3,3,3,3,3,3,3,3,3,3,3,3,3,3,3,3,3,
3,3,3,3,3,3,3,3,3,3,3,3,3,3,3,3,3,3,3,3,3,3,3,3,3,3,3,3,3,3,3,3,3,3,3,3,
3,3,3,3,4),(-22.9423049617331,-22.8359146756665,-22.7294985856963,-22.6229461677493,
-22.5163198701347,-22.4094937864604,-22.3477149909599,-22.241991690464,
-22.133752130249,-22.0282970330834,-21.9229015138189,-21.8175302025545,
-21.7071664541019,-21.6016731308017,-21.4961119262998,-21.3903887822451,
-21.3760752087442,-21.270344951488,-21.1621062608681,-21.0566434209101,
-20.95123988815,-20.8458603053796,-20.7355040856669,-20.6300019344483,-20.5244317166851,
-20.4186993582769,-20.4044354265286,-20.2987232088165,-20.1904822632535,
-20.0850383121632,-19.9796539285277,-19.8742937220325,-19.7639192026026,
-19.6584367694276,-19.5528863693,-19.4471738307262,-19.4327956443129,-19.327075538132,
-19.2188355786277,-19.1133834865874,-19.0079908919881,-18.9026224187124,
-18.7922557795586,-18.6867650370827,-18.581206320842,-18.4754855147286,
-18.4611558620973,-18.355436078419,-18.2471960786018,-18.1417442669779,
-18.0363519363068,-17.9309837099735,-17.8206168024505,-17.7151262611044,
-17.609567729898,-17.5038470846879,-17.4895160798816,-17.3853086147757,
-17.2812326981936,-17.1772506712568,-17.0733250028991,-16.9693644080451,
-16.8653929900671,-16.7612777660331,-16.6591196549165),.UNSPECIFIED.) ;
#1726 = B_SPLINE_CURVE_WITH_KNOTS('',3,(#112019,#112020,#112021,#112022,#112023,
#112024,#112025,#112026,#112027,#112028,#112029,#112030,#112031,#112032,
#112033,#112034,#112035,#112036,#112037,#112038,#112039,#112040,#112041,
#112042,#112043,#112044,#112045,#112046,#112047,#112048,#112049,#112050,
#112051,#112052,#112053,#112054,#112055,#112056,#112057,#112058,#112059,
#112060,#112061,#112062,#112063,#112064,#112065,#112066,#112067,#112068,
#112069,#112070,#112071,#112072,#112073,#112074,#112075,#112076,#112077,
#112078,#112079,#112080,#112081,#112082,#112083,#112084,#112085,#112086,
#112087,#112088,#112089,#112090,#112091,#112092,#112093,#112094,#112095,
#112096,#112097,#112098,#112099,#112100,#112101,#112102,#112103,#112104,
#112105,#112106,#112107,#112108,#112109,#112110,#112111,#112112,#112113,
#112114,#112115,#112116,#112117,#112118,#112119,#112120,#112121,#112122,
#112123,#112124,#112125,#112126,#112127,#112128,#112129,#112130,#112131,
#112132,#112133,#112134,#112135,#112136,#112137,#112138,#112139,#112140,
#112141,#112142,#112143,#112144,#112145,#112146,#112147,#112148,#112149,
#112150,#112151,#112152,#112153,#112154,#112155,#112156,#112157,#112158,
#112159,#112160,#112161,#112162,#112163,#112164,#112165,#112166,#112167,
#112168,#112169,#112170,#112171,#112172,#112173,#112174,#112175,#112176,
#112177,#112178,#112179,#112180,#112181,#112182,#112183,#112184,#112185,
#112186,#112187,#112188,#112189,#112190,#112191,#112192,#112193,#112194,
#112195,#112196,#112197,#112198,#112199,#112200,#112201,#112202,#112203,
#112204,#112205,#112206,#112207,#112208,#112209,#112210,#112211),
 .UNSPECIFIED.,.F.,.F.,(4,3,3,3,3,3,3,3,3,3,3,3,3,3,3,3,3,3,3,3,3,3,3,3,
3,3,3,3,3,3,3,3,3,3,3,3,3,3,3,3,3,3,3,3,3,3,3,3,3,3,3,3,3,3,3,3,3,3,3,3,
3,3,3,3,4),(-16.6591196545535,-16.517876297666,-16.4121571817512,-16.3039170984636,
-16.1984659993176,-16.0930743956811,-15.98770690971,-15.8773393111451,-15.7718495350374,
-15.6662917769805,-15.5605719107464,-15.5462365154503,-15.4405175111735,
-15.3322774139311,-15.2268264264337,-15.1214349341175,-15.0160675589399,
-14.9056998525136,-14.8002101845372,-14.6946525335813,-14.5889327722318,
-14.5745967332347,-14.4688778255767,-14.360637716257,-14.2551868315348,
-14.1497954439831,-14.044428175381,-13.9340603692905,-13.8285708111944,
-13.7230132711611,-13.6172936214372,-13.602956951019,-13.4972380492425,
-13.3889979391876,-13.2835470569139,-13.1781556705346,-13.0727884018306,
-12.9624205935738,-12.856931032194,-12.7513734877815,-12.6456538321663,
-12.6313171688034,-12.5255981556858,-12.4173580595486,-12.3119070683704,
-12.2065155742917,-12.1011481992669,-11.9907804960971,-11.8852908330562,
-11.7797331886823,-11.6740134361877,-11.6596773865878,-11.5539582688639,
-11.4457181858024,-11.3402670859034,-11.2348754819066,-11.1295079959672,
-11.0191403980684,-10.9136506229712,-10.8080928662617,-10.7023730018402,
-10.6880376043721,-10.5637109854946,-10.4405584833869,-10.3759343476556),
 .UNSPECIFIED.) ;
#1727 = B_SPLINE_CURVE_WITH_KNOTS('',3,(#112213,#112214,#112215,#112216,#112217,
#112218,#112219,#112220,#112221,#112222,#112223,#112224,#112225,#112226,
#112227,#112228,#112229,#112230,#112231,#112232,#112233,#112234,#112235,
#112236,#112237,#112238,#112239,#112240,#112241,#112242,#112243,#112244,
#112245,#112246,#112247,#112248,#112249,#112250,#112251,#112252,#112253,
#112254,#112255,#112256,#112257,#112258,#112259,#112260,#112261,#112262,
#112263,#112264,#112265,#112266,#112267,#112268,#112269,#112270,#112271,
#112272,#112273,#112274,#112275,#112276,#112277,#112278,#112279,#112280,
#112281,#112282,#112283,#112284,#112285,#112286,#112287,#112288,#112289,
#112290,#112291,#112292,#112293,#112294,#112295,#112296,#112297,#112298,
#112299,#112300,#112301,#112302,#112303,#112304,#112305,#112306,#112307,
#112308,#112309,#112310,#112311,#112312,#112313,#112314,#112315,#112316,
#112317,#112318,#112319,#112320,#112321,#112322,#112323,#112324,#112325,
#112326,#112327,#112328,#112329,#112330,#112331,#112332,#112333,#112334,
#112335,#112336,#112337,#112338,#112339,#112340,#112341,#112342,#112343,
#112344,#112345,#112346,#112347,#112348,#112349,#112350,#112351,#112352,
#112353,#112354,#112355,#112356,#112357,#112358,#112359,#112360,#112361,
#112362,#112363,#112364,#112365,#112366,#112367,#112368,#112369,#112370,
#112371,#112372,#112373,#112374,#112375,#112376,#112377,#112378,#112379,
#112380,#112381,#112382,#112383,#112384,#112385,#112386,#112387,#112388,
#112389,#112390,#112391,#112392,#112393,#112394,#112395,#112396,#112397,
#112398,#112399,#112400,#112401,#112402,#112403,#112404,#112405,#112406,
#112407,#112408),.UNSPECIFIED.,.F.,.F.,(4,3,3,3,3,3,3,3,3,3,3,3,3,3,3,3,
3,3,3,3,3,3,3,3,3,3,3,3,3,3,3,3,3,3,3,3,3,3,3,3,3,3,3,3,3,3,3,3,3,3,3,3,
3,3,3,3,3,3,3,3,3,3,3,3,3,4),(-10.375934347374,-10.270818228235,-10.1657261742581,
-10.0606224775472,-9.95540604281518,-9.8501222535424,-9.74466686480985,
-9.71639782215646,-9.61067792744562,-9.50243794150752,-9.39698608366202,
-9.2915937308619,-9.18622550645682,-9.07585863982782,-8.97036816048045,
-8.86480971195451,-8.75908917797183,-8.74475803994082,-8.63903798481663,
-8.5307980189302,-8.42534594814427,-8.31995336372064,-8.2145848895582,-8.10421823159994,
-7.99872746061479,-7.89316870635468,-7.78744784909512,-7.77311825772517,
-7.66740644868325,-7.55916545203653,-7.45372167107659,-7.34833736890122,
-7.24297715532693,-7.13260248537258,-7.02711982401829,-6.92156911959377,
-6.81585617164976,-6.80147847550953,-6.69574689772163,-6.58750837216816,
-6.48204498251401,-6.37664118662987,-6.27126162688296,-6.16090589348569,
-6.05540447971091,-5.94983524539449,-5.84410420992605,-5.82983869329388,
-5.72411630668951,-5.6158766322381,-5.51042191551005,-5.40502657837274,
-5.29965525121858,-5.18929116618349,-5.0837973325642,-4.97823544750672,
-4.87251138793772,-4.85819891107823,-4.75396818259709,-4.64987162623521,
-4.54587159887065,-4.44193058968034,-4.33797426762636,-4.23400853536007,
-4.12994521022668,-4.09274904045468),.UNSPECIFIED.) ;
#1728 = B_SPLINE_CURVE_WITH_KNOTS('',3,(#112410,#112411,#112412,#112413,#112414,
#112415,#112416,#112417,#112418,#112419,#112420,#112421,#112422,#112423,
#112424,#112425,#112426,#112427,#112428,#112429,#112430,#112431,#112432,
#112433,#112434,#112435,#112436,#112437,#112438,#112439,#112440,#112441,
#112442,#112443,#112444,#112445,#112446,#112447,#112448,#112449,#112450,
#112451,#112452,#112453,#112454,#112455,#112456,#112457,#112458,#112459,
#112460,#112461,#112462,#112463,#112464,#112465,#112466,#112467,#112468,
#112469,#112470),.UNSPECIFIED.,.F.,.F.,(4,3,3,3,3,3,3,3,3,3,3,3,3,3,3,3,
3,3,3,3,4),(-4.09274904019429,-3.94994251714104,-3.88655912886259,-3.78069844242293,
-3.67247605545093,-3.5668839769559,-3.46135201338902,-3.35584502036394,
-3.24561360193469,-3.13998805631316,-3.03429594813686,-2.92844465404552,
-2.91491934664694,-2.80970101248105,-2.70571134479635,-2.60181252142057,
-2.49796692460674,-2.39176836178501,-2.28786550058172,-2.18051908695078,
-2.07317267331984),.UNSPECIFIED.) ;
#1729 = B_SPLINE_CURVE_WITH_KNOTS('',3,(#112472,#112473,#112474,#112475),
 .UNSPECIFIED.,.F.,.F.,(4,4),(-0.0367203712850908,0.),.UNSPECIFIED.) ;
#1730 = B_SPLINE_CURVE_WITH_KNOTS('',3,(#112479,#112480,#112481,#112482,#112483),
 .UNSPECIFIED.,.F.,.F.,(4,1,4),(0.,0.971639782215629,1.12201628671538),
 .UNSPECIFIED.) ;
#1731 = B_SPLINE_CURVE_WITH_KNOTS('',3,(#112485,#112486,#112487,#112488,#112489,
#112490,#112491,#112492,#112493,#112494,#112495,#112496,#112497,#112498,
#112499,#112500,#112501,#112502,#112503,#112504,#112505,#112506,#112507,
#112508,#112509,#112510,#112511,#112512,#112513,#112514,#112515,#112516,
#112517,#112518,#112519,#112520,#112521,#112522,#112523,#112524,#112525,
#112526,#112527,#112528,#112529,#112530,#112531,#112532,#112533,#112534,
#112535,#112536,#112537,#112538,#112539,#112540,#112541,#112542,#112543,
#112544,#112545,#112546,#112547,#112548,#112549,#112550,#112551,#112552,
#112553,#112554,#112555,#112556,#112557,#112558,#112559,#112560,#112561,
#112562,#112563,#112564,#112565,#112566,#112567,#112568,#112569,#112570,
#112571,#112572,#112573,#112574,#112575,#112576,#112577,#112578,#112579,
#112580,#112581,#112582,#112583,#112584,#112585,#112586,#112587,#112588,
#112589,#112590,#112591,#112592,#112593,#112594,#112595,#112596,#112597,
#112598,#112599,#112600,#112601,#112602,#112603,#112604,#112605,#112606,
#112607,#112608,#112609,#112610,#112611,#112612,#112613,#112614,#112615,
#112616,#112617,#112618,#112619,#112620,#112621,#112622,#112623,#112624,
#112625,#112626,#112627,#112628,#112629,#112630,#112631,#112632,#112633,
#112634,#112635,#112636,#112637,#112638,#112639,#112640,#112641,#112642,
#112643,#112644,#112645,#112646,#112647,#112648,#112649,#112650,#112651,
#112652,#112653,#112654,#112655,#112656,#112657,#112658,#112659,#112660,
#112661,#112662,#112663,#112664,#112665,#112666,#112667,#112668,#112669,
#112670,#112671,#112672,#112673,#112674,#112675,#112676,#112677),
 .UNSPECIFIED.,.F.,.F.,(4,3,3,3,3,3,3,3,3,3,3,3,3,3,3,3,3,3,3,3,3,3,3,3,
3,3,3,3,3,3,3,3,3,3,3,3,3,3,3,3,3,3,3,3,3,3,3,3,3,3,3,3,3,3,3,3,3,3,3,3,
3,3,3,3,4),(1.12201628671538,1.22573351984078,1.32934711813555,1.4328950730314,
1.53641527935953,1.64001495378494,1.74365071550474,1.84746877012718,1.94327956443127,
2.0489757773739,2.15721872353302,2.2626385001509,2.36799578538946,2.47332604534675,
2.58372437067179,2.68917019510039,2.79468174011294,2.90035256690749,2.91491934664691,
3.02076955040777,3.12899324771462,3.23458096412644,3.34011084293479,3.44561802516486,
3.55585330108929,3.66148470545172,3.76718462728308,3.8730464282202,3.88655912886256,
3.9922114528047,4.10045988508888,4.20584197472517,4.31116394383356,4.41646128846482,
4.52689569411816,4.6323148743042,4.73780194400129,4.84345148339452,4.8581989110782,
4.96392221077202,5.07216177108725,5.17761686744958,5.28301238591223,5.38838369637743,
5.49874744560654,5.60424076812202,5.70980197184468,5.81552511513283,5.82983869329384,
5.93556895048034,6.04380764110898,6.14927048100083,6.254674013696,6.36005359640275,
6.47040981617943,6.575911967338,6.68148218504262,6.78721454339403,6.80147847550949,
6.90810451976517,7.01457261073179,7.12090179489442,7.22714857804156,7.3333604972507,
7.40520159389494),.UNSPECIFIED.) ;
#1732 = B_SPLINE_CURVE_WITH_KNOTS('',3,(#112679,#112680,#112681,#112682,#112683,
#112684,#112685,#112686,#112687,#112688,#112689,#112690,#112691,#112692,
#112693,#112694,#112695,#112696,#112697,#112698,#112699,#112700,#112701,
#112702,#112703,#112704,#112705,#112706,#112707,#112708,#112709,#112710,
#112711,#112712,#112713,#112714,#112715,#112716,#112717,#112718,#112719,
#112720,#112721,#112722,#112723,#112724,#112725,#112726,#112727,#112728,
#112729,#112730,#112731,#112732,#112733,#112734,#112735,#112736,#112737,
#112738,#112739,#112740,#112741,#112742,#112743,#112744,#112745,#112746,
#112747,#112748,#112749,#112750,#112751,#112752,#112753,#112754,#112755,
#112756,#112757,#112758,#112759,#112760,#112761,#112762,#112763,#112764,
#112765,#112766,#112767,#112768,#112769,#112770,#112771,#112772,#112773,
#112774,#112775,#112776,#112777,#112778,#112779,#112780,#112781,#112782,
#112783,#112784,#112785,#112786,#112787,#112788,#112789,#112790,#112791,
#112792,#112793,#112794,#112795,#112796,#112797,#112798,#112799,#112800,
#112801,#112802,#112803,#112804,#112805,#112806,#112807,#112808,#112809,
#112810,#112811,#112812,#112813,#112814,#112815,#112816,#112817,#112818,
#112819,#112820,#112821,#112822,#112823,#112824,#112825,#112826,#112827,
#112828,#112829,#112830,#112831,#112832,#112833,#112834,#112835,#112836,
#112837,#112838,#112839,#112840,#112841,#112842,#112843,#112844,#112845,
#112846,#112847,#112848,#112849,#112850,#112851,#112852,#112853,#112854,
#112855,#112856,#112857,#112858,#112859,#112860,#112861,#112862,#112863,
#112864,#112865,#112866,#112867,#112868,#112869,#112870,#112871,#112872,
#112873,#112874),.UNSPECIFIED.,.F.,.F.,(4,3,3,3,3,3,3,3,3,3,3,3,3,3,3,3,
3,3,3,3,3,3,3,3,3,3,3,3,3,3,3,3,3,3,3,3,3,3,3,3,3,3,3,3,3,3,3,3,3,3,3,3,
3,3,3,3,3,3,3,3,3,3,3,3,3,4),(7.4052015942302,7.52274829518333,7.64076688448783,
7.75933378391934,7.77311825772513,7.87883836383028,7.98707832334409,8.0925304153057,
8.19792300982544,8.3032914830209,8.41365812225087,8.51914886464601,8.6247075808057,
8.73042838683844,8.74475803994077,8.85047782361075,8.95871782342896,9.06416963504312,
9.16956196570429,9.27493019202703,9.38529709955938,9.49078764089399,9.59634617208882,
9.7020668172867,9.71639782215641,9.82211609691572,9.93035628534776,10.0358065127374,
10.1411972357971,10.2465638338936,10.3569322765132,10.4624211569032,10.5679780173793,
10.6736969896783,10.6880376043721,10.7937567202753,10.9019968035643,11.0074479026982,
11.1128395063224,11.2182069922812,11.3285745908578,11.4340643669531,11.5396221249977,
11.6453419912194,11.6596773865877,11.7653963908656,11.8736364881078,11.9790874756063,
12.0844789679236,12.1898463431023,12.3002140495275,12.405703717505,12.511261368462,
12.6169811298125,12.6313171688033,12.7370360764623,12.8452761857819,12.9507270705053,
13.0561184580582,13.1614857266615,13.2718535327509,13.3773430908484,13.4829006308829,
13.5886202806081,13.602956951019,13.6883869010745),.UNSPECIFIED.) ;
#1733 = B_SPLINE_CURVE_WITH_KNOTS('',3,(#112876,#112877,#112878,#112879,#112880,
#112881,#112882,#112883,#112884,#112885,#112886,#112887,#112888,#112889,
#112890,#112891,#112892,#112893,#112894,#112895,#112896,#112897,#112898,
#112899,#112900,#112901,#112902,#112903,#112904,#112905,#112906,#112907,
#112908,#112909,#112910,#112911,#112912,#112913,#112914,#112915,#112916,
#112917,#112918,#112919,#112920,#112921,#112922,#112923,#112924,#112925,
#112926,#112927,#112928,#112929,#112930,#112931,#112932,#112933,#112934,
#112935,#112936,#112937,#112938,#112939,#112940,#112941,#112942,#112943,
#112944,#112945,#112946,#112947,#112948,#112949,#112950,#112951,#112952,
#112953,#112954,#112955,#112956,#112957,#112958,#112959,#112960,#112961,
#112962,#112963,#112964,#112965,#112966,#112967,#112968,#112969,#112970,
#112971,#112972,#112973,#112974,#112975,#112976,#112977,#112978,#112979,
#112980,#112981,#112982,#112983,#112984,#112985,#112986,#112987,#112988,
#112989,#112990,#112991,#112992,#112993,#112994,#112995,#112996,#112997,
#112998,#112999,#113000,#113001,#113002,#113003,#113004,#113005,#113006,
#113007,#113008,#113009,#113010,#113011,#113012,#113013,#113014,#113015,
#113016,#113017,#113018,#113019,#113020,#113021,#113022,#113023,#113024,
#113025,#113026,#113027,#113028,#113029,#113030,#113031,#113032,#113033,
#113034,#113035,#113036,#113037,#113038,#113039,#113040,#113041,#113042,
#113043,#113044,#113045,#113046,#113047,#113048,#113049,#113050,#113051,
#113052,#113053,#113054,#113055,#113056,#113057,#113058,#113059,#113060,
#113061,#113062,#113063,#113064,#113065,#113066,#113067,#113068),
 .UNSPECIFIED.,.F.,.F.,(4,3,3,3,3,3,3,3,3,3,3,3,3,3,3,3,3,3,3,3,3,3,3,3,
3,3,3,3,3,3,3,3,3,3,3,3,3,3,3,3,3,3,3,3,3,3,3,3,3,3,3,3,3,3,3,3,3,3,3,3,
3,3,3,3,4),(13.6883869014638,13.7928966431387,13.8972545313542,14.0015295444517,
14.10575882162,14.2099794381379,14.3142930238784,14.4186584630941,14.5231928841024,
14.5745967332346,14.6803157463521,14.7885558424894,14.8940068336676,14.9993983277466,
15.1047657027714,15.2151334059411,15.3206230689822,15.4261807133564,15.5319004658512,
15.5462365154503,15.6519556331625,15.7601957162254,15.8656468161126,15.9710384200976,
16.0764059060253,16.1867735039355,16.292263279021,16.397821035719,16.5035409001291,
16.5178762976659,16.62359452377,16.7318347182839,16.8372849254186,16.9426756387808,
17.0480422377219,17.1584106982618,17.2638996058194,17.3694565025261,17.475175523565,
17.4895160798816,17.5952359745804,17.70347596052,17.8089278183545,17.9143201711438,
18.0196883955385,18.1300552621782,18.2355457415161,18.341104190033,18.4468247240073,
18.4611558620972,18.5668759171409,18.6751158830374,18.7805679537426,18.8859605380855,
18.9913290121675,19.1016956702039,19.2071864411105,19.3127451952932,19.4184660524764,
19.4327956443128,19.5414242479478,19.6498166849957,19.7580694756742,19.8661879885317,
19.9715722082541),.UNSPECIFIED.) ;
#1734 = B_SPLINE_CURVE_WITH_KNOTS('',3,(#113070,#113071,#113072,#113073,#113074,
#113075,#113076,#113077,#113078,#113079,#113080,#113081,#113082,#113083,
#113084,#113085,#113086,#113087,#113088,#113089,#113090,#113091,#113092,
#113093,#113094,#113095,#113096,#113097,#113098,#113099,#113100,#113101,
#113102,#113103,#113104,#113105,#113106,#113107,#113108,#113109,#113110,
#113111,#113112,#113113,#113114,#113115,#113116,#113117,#113118,#113119,
#113120,#113121,#113122,#113123,#113124,#113125,#113126,#113127,#113128,
#113129,#113130,#113131,#113132,#113133,#113134,#113135,#113136,#113137,
#113138,#113139,#113140,#113141,#113142,#113143,#113144,#113145,#113146,
#113147,#113148,#113149,#113150,#113151,#113152,#113153,#113154,#113155,
#113156,#113157,#113158,#113159,#113160,#113161,#113162,#113163,#113164,
#113165,#113166,#113167,#113168,#113169,#113170,#113171,#113172,#113173,
#113174,#113175,#113176,#113177,#113178,#113179,#113180,#113181,#113182,
#113183,#113184,#113185,#113186,#113187,#113188,#113189,#113190,#113191,
#113192,#113193,#113194,#113195,#113196,#113197,#113198,#113199,#113200,
#113201,#113202,#113203,#113204,#113205,#113206,#113207,#113208,#113209,
#113210,#113211,#113212,#113213,#113214,#113215,#113216,#113217,#113218,
#113219,#113220,#113221,#113222,#113223,#113224,#113225,#113226),
 .UNSPECIFIED.,.F.,.F.,(4,3,3,3,3,3,3,3,3,3,3,3,3,3,3,3,3,3,3,3,3,3,3,3,
3,3,3,3,3,3,3,3,3,3,3,3,3,3,3,3,3,3,3,3,3,3,3,3,3,3,3,3,4),(19.9715722086605,
20.0845648631634,20.1977996632066,20.3114400836798,20.4044354265285,20.5101670042602,
20.6184055298206,20.7238689194144,20.8292727152366,20.9346522749201,21.0450080083761,
21.1505094220841,21.2560786563325,21.3618096917317,21.3760752087441,21.4817975945836,
21.5900372691306,21.6954919850707,21.8008873214135,21.9062586477675,22.0166227335656,
22.122116566379,22.2276784506292,22.3334025093939,22.3477149909598,22.4533639643363,
22.5616128154412,22.6669935098671,22.7723148103133,22.8776122117521,22.9880478521079,
23.0934689019899,23.1989584650854,23.3046113595733,23.3193547731754,23.4252154579137,
23.5334378450984,23.6390299220907,23.7445618842346,23.8500688759196,23.9603002957875,
24.0659258402978,24.1716179474442,24.2774692406294,24.2909945553911,24.396212889557,
24.5002025561162,24.6041013784337,24.7079469742604,24.8141455378748,24.9180483982882,
25.0253948135031,25.1327412287181),.UNSPECIFIED.) ;
#1735 = B_SPLINE_CURVE_WITH_KNOTS('',3,(#113227,#113228,#113229,#113230),
 .UNSPECIFIED.,.F.,.F.,(4,4),(-0.0367209699986071,0.),.UNSPECIFIED.) ;
#1736 = B_SPLINE_CURVE_WITH_KNOTS('',3,(#113235,#113236,#113237,#113238,#113239,
#113240,#113241,#113242),.UNSPECIFIED.,.F.,.F.,(4,1,1,1,1,4),(-39.7722845163973,
-38.7779774034875,-37.7836702905775,-36.7893631776676,-35.7950560647577,
-35.5086795309852),.UNSPECIFIED.) ;
#1737 = B_SPLINE_CURVE_WITH_KNOTS('',3,(#113244,#113245,#113246,#113247,#113248,
#113249,#113250,#113251,#113252,#113253,#113254,#113255,#113256,#113257,
#113258,#113259,#113260,#113261,#113262,#113263,#113264,#113265,#113266,
#113267,#113268,#113269,#113270,#113271,#113272,#113273,#113274,#113275,
#113276,#113277,#113278,#113279,#113280,#113281,#113282,#113283,#113284,
#113285,#113286,#113287,#113288,#113289,#113290,#113291,#113292,#113293,
#113294,#113295,#113296,#113297,#113298,#113299,#113300,#113301,#113302,
#113303,#113304,#113305,#113306,#113307,#113308,#113309,#113310,#113311,
#113312,#113313,#113314,#113315,#113316,#113317,#113318,#113319,#113320,
#113321,#113322,#113323,#113324,#113325,#113326,#113327,#113328,#113329,
#113330,#113331,#113332,#113333,#113334,#113335,#113336,#113337,#113338,
#113339,#113340,#113341,#113342,#113343,#113344,#113345,#113346,#113347,
#113348,#113349,#113350,#113351,#113352,#113353,#113354,#113355,#113356,
#113357,#113358,#113359,#113360,#113361,#113362,#113363,#113364,#113365,
#113366,#113367,#113368,#113369,#113370,#113371,#113372,#113373,#113374,
#113375,#113376,#113377,#113378,#113379,#113380,#113381,#113382,#113383,
#113384,#113385,#113386,#113387,#113388,#113389,#113390,#113391,#113392,
#113393,#113394,#113395,#113396,#113397,#113398,#113399,#113400,#113401,
#113402,#113403,#113404,#113405,#113406,#113407,#113408,#113409,#113410,
#113411,#113412,#113413,#113414,#113415,#113416,#113417,#113418,#113419,
#113420,#113421,#113422,#113423,#113424,#113425,#113426,#113427,#113428,
#113429,#113430,#113431,#113432,#113433),.UNSPECIFIED.,.F.,.F.,(4,3,3,3,
3,3,3,3,3,3,3,3,3,3,3,3,3,3,3,3,3,3,3,3,3,3,3,3,3,3,3,3,3,3,3,3,3,3,3,3,
3,3,3,3,3,3,3,3,3,3,3,3,3,3,3,3,3,3,3,3,3,3,3,4),(-35.5086755760922,-35.4044022275757,
-35.3001748457792,-35.1959564275686,-35.0916365673699,-34.9872656491195,
-34.8827030128636,-34.8007489518477,-34.6953269562437,-34.590062699299,
-34.4849213620955,-34.3798454078011,-34.2747989300688,-34.1697460662361,
-34.0645822019727,-33.9593555008014,-33.8539493708266,-33.8064418389378,
-33.7010087123129,-33.5957328956943,-33.4905794204482,-33.3854909757382,
-33.280431674028,-33.1753656711069,-33.0701882799077,-32.9649478104766,
-32.859527683096,-32.8121347260278,-32.7067227907937,-32.6014685704431,
-32.4963371822769,-32.3912711160732,-32.2862344494186,-32.1811913035088,
-32.0760369477011,-31.9708196485666,-31.8654226574899,-31.8178276131179,
-31.7124073632301,-31.6071447184869,-31.5020047860233,-31.3969301063105,
-31.2918847704261,-31.1868329129934,-31.0816698418366,-30.9764438127394,
-30.8710381603998,-30.823520500208,-30.7180998986488,-30.6128368710002,
-30.5076965111687,-30.4026213766816,-30.2975755592732,-30.1925231941935,
-30.0873595792423,-29.9821329848799,-29.8767267400281,-29.8292133872981,
-29.7224635603256,-29.6158838669993,-29.5094623746583,-29.4031341758113,
-29.2968586465874,-29.2254902689127),.UNSPECIFIED.) ;
#1738 = B_SPLINE_CURVE_WITH_KNOTS('',3,(#113435,#113436,#113437,#113438,#113439,
#113440,#113441,#113442,#113443,#113444,#113445,#113446,#113447,#113448,
#113449,#113450,#113451,#113452,#113453,#113454,#113455,#113456,#113457,
#113458,#113459,#113460,#113461,#113462,#113463,#113464,#113465,#113466,
#113467,#113468,#113469,#113470,#113471,#113472,#113473,#113474,#113475,
#113476,#113477,#113478,#113479,#113480,#113481,#113482,#113483,#113484,
#113485,#113486,#113487,#113488,#113489,#113490,#113491,#113492,#113493,
#113494,#113495,#113496,#113497,#113498,#113499,#113500,#113501,#113502,
#113503,#113504,#113505,#113506,#113507,#113508,#113509,#113510,#113511,
#113512,#113513,#113514,#113515,#113516,#113517,#113518,#113519,#113520,
#113521,#113522,#113523,#113524,#113525,#113526,#113527,#113528,#113529,
#113530,#113531,#113532,#113533,#113534,#113535,#113536,#113537,#113538,
#113539,#113540,#113541,#113542,#113543,#113544,#113545,#113546,#113547,
#113548,#113549,#113550,#113551,#113552,#113553,#113554,#113555,#113556,
#113557,#113558,#113559,#113560,#113561,#113562,#113563,#113564,#113565,
#113566,#113567,#113568,#113569,#113570,#113571,#113572,#113573,#113574,
#113575,#113576,#113577,#113578,#113579,#113580,#113581,#113582,#113583,
#113584,#113585,#113586,#113587,#113588,#113589,#113590,#113591,#113592,
#113593,#113594,#113595,#113596,#113597,#113598,#113599,#113600,#113601,
#113602,#113603,#113604,#113605,#113606,#113607,#113608,#113609,#113610,
#113611,#113612,#113613,#113614,#113615,#113616,#113617,#113618,#113619,
#113620,#113621,#113622,#113623,#113624),.UNSPECIFIED.,.F.,.F.,(4,3,3,3,
3,3,3,3,3,3,3,3,3,3,3,3,3,3,3,3,3,3,3,3,3,3,3,3,3,3,3,3,3,3,3,3,3,3,3,3,
3,3,3,3,3,3,3,3,3,3,3,3,3,3,3,3,3,3,3,3,3,3,3,4),(-29.2254902685167,-29.1088417077146,
-28.9917385973977,-28.8740574296362,-28.8349062743881,-28.7294867233392,
-28.6242247724242,-28.5190855227818,-28.4140115186036,-28.3089668498783,
-28.2039156501323,-28.0987532177186,-27.9935278174278,-27.8881227719779,
-27.8405991614782,-27.7351796522675,-27.6299177413909,-27.5247785289052,
-27.419704560066,-27.3146599248016,-27.2096087565756,-27.1044463525154,
-26.9992209788055,-26.8938159569209,-26.8462920485682,-26.7408727177183,
-26.6356109889847,-26.5304719633295,-26.4253981841197,-26.3203537409896,
-26.2153027671114,-26.1101405594126,-26.0049153834966,-25.8995105595505,
-25.8519849356583,-25.746565505444,-25.6413036758188,-25.5361645475202,
-25.4310906646418,-25.3260461169799,-25.2209950378678,-25.1158327245988,
-25.0106074427696,-24.9052025134882,-24.8576778227484,-24.7522584043583,
-24.6469965865146,-24.5418574698731,-24.436783598567,-24.331739062374,-24.2266879946087,
-24.1215256924225,-24.0163004215407,-23.9108955028829,-23.8633707098384,
-23.7590253019421,-23.6548572600467,-23.5507881656705,-23.4467805861788,
-23.34279717317,-23.238732933035,-23.1346302543012,-23.0303500238302,-22.9423049621638),
 .UNSPECIFIED.) ;
#1739 = B_SPLINE_CURVE_WITH_KNOTS('',3,(#113626,#113627,#113628,#113629,#113630,
#113631,#113632,#113633,#113634,#113635,#113636,#113637,#113638,#113639,
#113640,#113641,#113642,#113643,#113644,#113645,#113646,#113647,#113648,
#113649,#113650,#113651,#113652,#113653,#113654,#113655,#113656,#113657,
#113658,#113659,#113660,#113661,#113662,#113663,#113664,#113665,#113666,
#113667,#113668,#113669,#113670,#113671,#113672,#113673,#113674,#113675,
#113676,#113677,#113678,#113679,#113680,#113681,#113682,#113683,#113684,
#113685,#113686,#113687,#113688,#113689,#113690,#113691,#113692,#113693,
#113694,#113695,#113696,#113697,#113698,#113699,#113700,#113701,#113702,
#113703,#113704,#113705,#113706,#113707,#113708,#113709,#113710,#113711,
#113712,#113713,#113714,#113715,#113716,#113717,#113718,#113719,#113720,
#113721,#113722,#113723,#113724,#113725,#113726,#113727,#113728,#113729,
#113730,#113731,#113732,#113733,#113734,#113735,#113736,#113737,#113738,
#113739,#113740,#113741,#113742,#113743,#113744,#113745,#113746,#113747,
#113748,#113749,#113750,#113751,#113752,#113753,#113754,#113755,#113756,
#113757,#113758,#113759,#113760,#113761,#113762,#113763,#113764,#113765,
#113766,#113767,#113768,#113769,#113770,#113771,#113772,#113773,#113774,
#113775,#113776,#113777,#113778,#113779,#113780,#113781,#113782,#113783,
#113784,#113785,#113786,#113787,#113788,#113789,#113790,#113791,#113792,
#113793,#113794,#113795,#113796,#113797,#113798,#113799,#113800,#113801,
#113802,#113803,#113804,#113805,#113806,#113807,#113808,#113809,#113810,
#113811,#113812,#113813,#113814,#113815),.UNSPECIFIED.,.F.,.F.,(4,3,3,3,
3,3,3,3,3,3,3,3,3,3,3,3,3,3,3,3,3,3,3,3,3,3,3,3,3,3,3,3,3,3,3,3,3,3,3,3,
3,3,3,3,3,3,3,3,3,3,3,3,3,3,3,3,3,3,3,3,3,3,3,4),(-22.9423049617331,-22.8690635969285,
-22.7636441836932,-22.6583823711868,-22.5532432601264,-22.4481693945498,
-22.3431248642258,-22.2380738024606,-22.1329115064317,-22.0276862418063,
-21.9222813294921,-21.8747564840186,-21.7693370725943,-21.6640752619096,
-21.5589361526772,-21.4538622889313,-21.3488177604379,-21.2437667005001,
-21.1386044062813,-21.0333791434584,-20.9279742329166,-20.8804493711086,
-20.7750299606903,-20.6697681510407,-20.5646290428816,-20.4595551802322,
-20.3545106528565,-20.2494595940563,-20.1442973009971,-20.0390720393482,
-19.93366712999,-19.8861422581987,-19.7807228478555,-19.6754610382638,-19.5703219301372,
-19.4652480675043,-19.3602035401295,-19.2551524813143,-19.1499901882165,
-19.0447649265154,-18.9393600170848,-18.8918351452888,-18.7864157337639,
-18.6811539230014,-18.5760148137255,-18.4709409499573,-18.3658964214628,
-18.2608453615451,-18.1556830673781,-18.0504578046253,-17.9450528941805,
-17.8975280323788,-17.7921086190912,-17.6868468065444,-17.5817076954615,
-17.4766338298734,-17.371589299549,-17.2665382377944,-17.1613759417928,
-17.056150677204,-16.9507457649406,-16.9032209194689,-16.7660415444305,
-16.6591196548236),.UNSPECIFIED.) ;
#1740 = B_SPLINE_CURVE_WITH_KNOTS('',3,(#113817,#113818,#113819,#113820,#113821,
#113822,#113823,#113824,#113825,#113826,#113827,#113828,#113829,#113830,
#113831,#113832,#113833,#113834,#113835,#113836,#113837,#113838,#113839,
#113840,#113841,#113842,#113843,#113844,#113845,#113846,#113847,#113848,
#113849,#113850,#113851,#113852,#113853,#113854,#113855,#113856,#113857,
#113858,#113859,#113860,#113861,#113862,#113863,#113864,#113865,#113866,
#113867,#113868,#113869,#113870,#113871,#113872,#113873,#113874,#113875,
#113876,#113877,#113878,#113879,#113880,#113881,#113882,#113883,#113884,
#113885,#113886,#113887,#113888,#113889,#113890,#113891,#113892,#113893,
#113894,#113895,#113896,#113897,#113898,#113899,#113900,#113901,#113902,
#113903,#113904,#113905,#113906,#113907,#113908,#113909,#113910,#113911,
#113912,#113913,#113914,#113915,#113916,#113917,#113918,#113919,#113920,
#113921,#113922,#113923,#113924,#113925,#113926,#113927,#113928,#113929,
#113930,#113931,#113932,#113933,#113934,#113935,#113936,#113937,#113938,
#113939,#113940,#113941,#113942,#113943,#113944,#113945,#113946,#113947,
#113948,#113949,#113950,#113951,#113952,#113953,#113954,#113955,#113956,
#113957,#113958,#113959,#113960,#113961,#113962,#113963,#113964,#113965,
#113966,#113967,#113968,#113969,#113970,#113971,#113972,#113973,#113974,
#113975,#113976,#113977,#113978,#113979,#113980,#113981,#113982,#113983,
#113984,#113985,#113986,#113987,#113988,#113989,#113990,#113991,#113992,
#113993,#113994,#113995,#113996,#113997,#113998,#113999,#114000,#114001,
#114002,#114003,#114004,#114005,#114006,#114007,#114008,#114009),
 .UNSPECIFIED.,.F.,.F.,(4,3,3,3,3,3,3,3,3,3,3,3,3,3,3,3,3,3,3,3,3,3,3,3,
3,3,3,3,3,3,3,3,3,3,3,3,3,3,3,3,3,3,3,3,3,3,3,3,3,3,3,3,3,3,3,3,3,3,3,3,
3,3,3,3,4),(-16.6591196545535,-16.5552036813066,-16.4513560625145,-16.3475392568374,
-16.2437157711178,-16.1397837879908,-16.0357856707898,-15.9316178772595,
-15.908913806559,-15.8034943869351,-15.698232568139,-15.5930934509645,-15.4880195793859,
-15.3829750431806,-15.2779239756628,-15.1727616741133,-15.0675364040917,
-14.9621314866271,-14.914606693649,-14.8091872634756,-14.7039254338822,
-14.5987863056011,-14.4937124227317,-14.3886678750699,-14.2836167959496,
-14.178454482659,-14.0732292008009,-13.9678242714792,-13.9202995807391,
-13.8148802555112,-13.7096185311161,-13.6044795078905,-13.4994057299235,
-13.3943612868513,-13.2893103118467,-13.1841481012487,-13.0789229214155,
-12.9735180920354,-12.9259924678292,-12.8205729452315,-12.715311024023,
-12.6101718057521,-12.5050978339537,-12.4000531985516,-12.2950020330076,
-12.1898396358509,-12.0846142714686,-11.9792092625234,-11.9316853549192,
-11.8262658092296,-11.7210038624508,-11.6158646151245,-11.5107906121308,
-11.4057459434607,-11.3006947426411,-11.1955323074635,-11.0903069034382,
-10.9849018528082,-10.9373782420093,-10.8292878650851,-10.7159494856573,
-10.6082494155454,-10.5006633351676,-10.3931764397244,-10.375934347374),
 .UNSPECIFIED.) ;
#1741 = B_SPLINE_CURVE_WITH_KNOTS('',3,(#114011,#114012,#114013,#114014,#114015,
#114016,#114017,#114018,#114019,#114020,#114021,#114022,#114023,#114024,
#114025,#114026,#114027,#114028,#114029,#114030,#114031,#114032,#114033,
#114034,#114035,#114036,#114037,#114038,#114039,#114040,#114041,#114042,
#114043,#114044,#114045,#114046,#114047,#114048,#114049,#114050,#114051,
#114052,#114053,#114054,#114055,#114056,#114057,#114058,#114059,#114060,
#114061,#114062,#114063,#114064,#114065,#114066,#114067,#114068,#114069,
#114070,#114071,#114072,#114073,#114074,#114075,#114076,#114077,#114078,
#114079,#114080,#114081,#114082,#114083,#114084,#114085,#114086,#114087,
#114088,#114089,#114090,#114091,#114092,#114093,#114094,#114095,#114096,
#114097,#114098,#114099,#114100,#114101,#114102,#114103,#114104,#114105,
#114106,#114107,#114108,#114109,#114110,#114111,#114112,#114113,#114114,
#114115,#114116,#114117,#114118,#114119,#114120,#114121,#114122,#114123,
#114124,#114125,#114126,#114127,#114128,#114129,#114130,#114131,#114132,
#114133,#114134,#114135,#114136,#114137,#114138,#114139,#114140,#114141,
#114142,#114143,#114144,#114145,#114146,#114147,#114148,#114149,#114150,
#114151,#114152,#114153,#114154,#114155,#114156,#114157,#114158,#114159,
#114160,#114161,#114162,#114163,#114164,#114165,#114166,#114167,#114168,
#114169,#114170,#114171,#114172,#114173,#114174,#114175,#114176,#114177,
#114178,#114179,#114180,#114181,#114182,#114183,#114184,#114185,#114186,
#114187,#114188,#114189,#114190,#114191,#114192,#114193,#114194,#114195,
#114196,#114197,#114198,#114199,#114200),.UNSPECIFIED.,.F.,.F.,(4,3,3,3,
3,3,3,3,3,3,3,3,3,3,3,3,3,3,3,3,3,3,3,3,3,3,3,3,3,3,3,3,3,3,3,3,3,3,3,3,
3,3,3,3,3,3,3,3,3,3,3,3,3,3,3,3,3,3,3,3,3,3,3,4),(-10.3759343470868,-10.2622932374969,
-10.1483592599546,-10.0339564107411,-9.94307112909935,-9.83765038685958,
-9.73238725063561,-9.62724683000794,-9.52217166442452,-9.41712584557071,
-9.31207350868044,-9.20690996627838,-9.10168346994019,-8.99627736106777,
-8.94876401618942,-8.84334386834391,-8.7380813023553,-8.63294141399026,
-8.52786675683356,-8.42282142199786,-8.31776954411901,-8.21260642033977,
-8.107380320142,-8.00197456917108,-7.95445690327949,-7.84904538178143,-7.74379148075398,
-7.63866027140058,-7.53359429667177,-7.42855763429612,-7.32351440552014,
-7.21835983638616,-7.1131422490107,-7.00774485805702,-6.96014979036955,
-6.85471520591697,-6.74943826420544,-6.64428415902488,-6.53919539218959,
-6.43413607566243,-6.329070365056,-6.22389372586801,-6.11865427247152,-6.01323555438736,
-5.96584267745961,-5.86042207933793,-5.75515890094995,-5.65001816767372,
-5.54494252227572,-5.43989605888921,-5.3348429150212,-5.2296783300615,-5.1244506551307,
-5.01904317436125,-4.97153556454968,-4.86758857729089,-4.76381948081389,
-4.66014914956136,-4.55653972806567,-4.45295345014138,-4.34929458304977,
-4.24559519972438,-4.14174369917986,-4.09274904066394),.UNSPECIFIED.) ;
#1742 = B_SPLINE_CURVE_WITH_KNOTS('',3,(#114202,#114203,#114204,#114205,#114206,
#114207,#114208,#114209,#114210,#114211,#114212,#114213,#114214,#114215,
#114216,#114217,#114218,#114219,#114220,#114221,#114222,#114223,#114224,
#114225,#114226,#114227,#114228,#114229,#114230,#114231,#114232,#114233,
#114234,#114235,#114236,#114237,#114238,#114239,#114240,#114241,#114242,
#114243,#114244,#114245,#114246,#114247,#114248,#114249,#114250,#114251,
#114252,#114253,#114254,#114255,#114256,#114257,#114258,#114259,#114260,
#114261,#114262),.UNSPECIFIED.,.F.,.F.,(4,3,3,3,3,3,3,3,3,3,3,3,3,3,3,3,
3,3,3,3,4),(-4.09274904019429,-3.97722845163974,-3.87164849924216,-3.76622632436345,
-3.66092789460631,-3.55569545944398,-3.45049334973295,-3.34528594082316,
-3.23997021120549,-3.13459296743756,-3.02903986465691,-2.98292133872981,
-2.87879939642559,-2.77485099638648,-2.67099903247579,-2.56720584380832,
-2.46343385283584,-2.35957849417104,-2.25568164883975,-2.15160928322696,
-2.07317267331984),.UNSPECIFIED.) ;
#1743 = B_SPLINE_CURVE_WITH_KNOTS('',3,(#114264,#114265,#114266,#114267),
 .UNSPECIFIED.,.F.,.F.,(4,4),(-0.0487081061340111,0.),.UNSPECIFIED.) ;
#1744 = B_SPLINE_CURVE_WITH_KNOTS('',3,(#114271,#114272,#114273,#114274,#114275),
 .UNSPECIFIED.,.F.,.F.,(4,1,4),(0.,0.994307112909918,1.12201628671538),
 .UNSPECIFIED.) ;
#1745 = B_SPLINE_CURVE_WITH_KNOTS('',3,(#114277,#114278,#114279,#114280,#114281,
#114282,#114283,#114284,#114285,#114286,#114287,#114288,#114289,#114290,
#114291,#114292,#114293,#114294,#114295,#114296,#114297,#114298,#114299,
#114300,#114301,#114302,#114303,#114304,#114305,#114306,#114307,#114308,
#114309,#114310,#114311,#114312,#114313,#114314,#114315,#114316,#114317,
#114318,#114319,#114320,#114321,#114322,#114323,#114324,#114325,#114326,
#114327,#114328,#114329,#114330,#114331,#114332,#114333,#114334,#114335,
#114336,#114337,#114338,#114339,#114340,#114341,#114342,#114343,#114344,
#114345,#114346,#114347,#114348,#114349,#114350,#114351,#114352,#114353,
#114354,#114355,#114356,#114357,#114358,#114359,#114360,#114361,#114362,
#114363,#114364,#114365,#114366,#114367,#114368,#114369,#114370,#114371,
#114372,#114373,#114374,#114375,#114376,#114377,#114378,#114379,#114380,
#114381,#114382,#114383,#114384,#114385,#114386,#114387,#114388,#114389,
#114390,#114391,#114392,#114393,#114394,#114395,#114396,#114397,#114398,
#114399,#114400,#114401,#114402,#114403,#114404,#114405,#114406,#114407,
#114408,#114409,#114410,#114411,#114412,#114413,#114414,#114415,#114416,
#114417,#114418,#114419,#114420,#114421,#114422,#114423,#114424,#114425,
#114426,#114427,#114428,#114429,#114430,#114431,#114432,#114433,#114434,
#114435,#114436,#114437,#114438,#114439,#114440,#114441,#114442,#114443,
#114444,#114445,#114446,#114447,#114448,#114449,#114450,#114451,#114452,
#114453,#114454,#114455,#114456,#114457,#114458,#114459,#114460,#114461,
#114462,#114463,#114464,#114465,#114466),.UNSPECIFIED.,.F.,.F.,(4,3,3,3,
3,3,3,3,3,3,3,3,3,3,3,3,3,3,3,3,3,3,3,3,3,3,3,3,3,3,3,3,3,3,3,3,3,3,3,3,
3,3,3,3,3,3,3,3,3,3,3,3,3,3,3,3,3,3,3,3,3,3,3,4),(1.12201628671538,1.23034102910344,
1.33358330420648,1.43674793062772,1.53987315811359,1.64299717167808,1.74622395060981,
1.84951097348011,1.95297061142083,1.98861422581985,2.09399892739112,2.19922262279794,
2.30431881533442,2.40934681168488,2.51434260972737,2.61934216073603,2.72444914077599,
2.82961683585291,2.93496134502189,2.98292133872979,3.08848800174328,3.19389992341939,
3.29919261601425,3.40442212311023,3.50962410932036,3.6148341977006,3.72015679699726,
3.82554331992505,3.93110928046911,3.97722845163972,4.08257777213716,4.18776850937299,
4.29283544498566,4.39783649479165,4.50280768124411,4.60778498265087,4.71287339380203,
4.81802459579896,4.92335594389848,4.97153556454966,5.07695755890264,5.18222181458872,
5.28736315052821,5.39243910355605,5.49748558002122,5.60253844258718,5.70770230559402,
5.81292900551239,5.91833513425313,5.96584267745959,6.07127580375949,6.176551620046,
6.28170509495031,6.38679353931261,6.49185284066994,6.59691884323355,6.70209623407033,
6.80733670313579,6.9127568301494,6.96014979036953,7.07372300911412,7.18702116753589,
7.2998880871726,7.40520159341374),.UNSPECIFIED.) ;
#1746 = B_SPLINE_CURVE_WITH_KNOTS('',3,(#114468,#114469,#114470,#114471,#114472,
#114473,#114474,#114475,#114476,#114477,#114478,#114479,#114480,#114481,
#114482,#114483,#114484,#114485,#114486,#114487,#114488,#114489,#114490,
#114491,#114492,#114493,#114494,#114495,#114496,#114497,#114498,#114499,
#114500,#114501,#114502,#114503,#114504,#114505,#114506,#114507,#114508,
#114509,#114510,#114511,#114512,#114513,#114514,#114515,#114516,#114517,
#114518,#114519,#114520,#114521,#114522,#114523,#114524,#114525,#114526,
#114527,#114528,#114529,#114530,#114531,#114532,#114533,#114534,#114535,
#114536,#114537,#114538,#114539,#114540,#114541,#114542,#114543,#114544,
#114545,#114546,#114547,#114548,#114549,#114550,#114551,#114552,#114553,
#114554,#114555,#114556,#114557,#114558,#114559,#114560,#114561,#114562,
#114563,#114564,#114565,#114566,#114567,#114568,#114569,#114570,#114571,
#114572,#114573,#114574,#114575,#114576,#114577,#114578,#114579,#114580,
#114581,#114582,#114583,#114584,#114585,#114586,#114587,#114588,#114589,
#114590,#114591,#114592,#114593,#114594,#114595,#114596,#114597,#114598,
#114599,#114600,#114601,#114602,#114603,#114604,#114605,#114606,#114607,
#114608,#114609,#114610,#114611,#114612,#114613,#114614,#114615,#114616,
#114617,#114618,#114619,#114620,#114621,#114622,#114623,#114624,#114625,
#114626,#114627,#114628,#114629,#114630,#114631,#114632,#114633,#114634,
#114635,#114636,#114637,#114638,#114639,#114640,#114641,#114642,#114643,
#114644,#114645,#114646,#114647,#114648,#114649,#114650,#114651,#114652,
#114653,#114654,#114655,#114656,#114657),.UNSPECIFIED.,.F.,.F.,(4,3,3,3,
3,3,3,3,3,3,3,3,3,3,3,3,3,3,3,3,3,3,3,3,3,3,3,3,3,3,3,3,3,3,3,3,3,3,3,3,
3,3,3,3,3,3,3,3,3,3,3,3,3,3,3,3,3,3,3,3,3,3,3,4),(7.40520159389494,7.51310671647122,
7.62344426317328,7.73165200870718,7.84305445599332,7.95445690327946,8.05987715300651,
8.16513979758751,8.27027972988675,8.37535440943424,8.4803997451524,8.58545160241827,
8.69061467340867,8.79584070233938,8.90124635451427,8.94876401618939,9.05418461770193,
9.15944764530252,9.26458800508425,9.36966313952041,9.47470895687734,9.57976132190398,
9.68492493680147,9.79015153110949,9.89555777590651,9.94307112909933,10.0484897557137,
10.1537507688988,10.2588890658611,10.3639621086595,10.4690058088096,10.574056034282,
10.6792174905251,10.7844419121692,10.8898459853794,10.9373782420093,11.0427977930361,
11.1480597439288,11.2531989935486,11.3582729977041,11.4633176664064,11.5683688661293,
11.6735312985203,11.7787566987884,11.8841617442156,11.9316853549192,12.0371048641248,
12.1423667749956,12.2475059874759,12.3525799563095,12.4576245915682,12.5626757597885,
12.6678381638428,12.7730635375468,12.8784685594254,12.9259924678291,13.0300394883708,
13.1339455877987,13.2377486448433,13.3414863916629,13.4452303857489,13.5489787431586,
13.652816925385,13.6883869007106),.UNSPECIFIED.) ;
#1747 = B_SPLINE_CURVE_WITH_KNOTS('',3,(#114659,#114660,#114661,#114662,#114663,
#114664,#114665,#114666,#114667,#114668,#114669,#114670,#114671,#114672,
#114673,#114674,#114675,#114676,#114677,#114678,#114679,#114680,#114681,
#114682,#114683,#114684,#114685,#114686,#114687,#114688,#114689,#114690,
#114691,#114692,#114693,#114694,#114695,#114696,#114697,#114698,#114699,
#114700,#114701,#114702,#114703,#114704,#114705,#114706,#114707,#114708,
#114709,#114710,#114711,#114712,#114713,#114714,#114715,#114716,#114717,
#114718,#114719,#114720,#114721,#114722,#114723,#114724,#114725,#114726,
#114727,#114728,#114729,#114730,#114731,#114732,#114733,#114734,#114735,
#114736,#114737,#114738,#114739,#114740,#114741,#114742,#114743,#114744,
#114745,#114746,#114747,#114748,#114749,#114750,#114751,#114752,#114753,
#114754,#114755,#114756,#114757,#114758,#114759,#114760,#114761,#114762,
#114763,#114764,#114765,#114766,#114767,#114768,#114769,#114770,#114771,
#114772,#114773,#114774,#114775,#114776,#114777,#114778,#114779,#114780,
#114781,#114782,#114783,#114784,#114785,#114786,#114787,#114788,#114789,
#114790,#114791,#114792,#114793,#114794,#114795,#114796,#114797,#114798,
#114799,#114800,#114801,#114802,#114803,#114804,#114805,#114806,#114807,
#114808,#114809,#114810,#114811,#114812,#114813,#114814,#114815,#114816,
#114817,#114818,#114819,#114820,#114821,#114822,#114823,#114824,#114825,
#114826,#114827,#114828,#114829,#114830,#114831,#114832,#114833,#114834,
#114835,#114836,#114837,#114838,#114839,#114840,#114841,#114842,#114843,
#114844,#114845,#114846,#114847,#114848),.UNSPECIFIED.,.F.,.F.,(4,3,3,3,
3,3,3,3,3,3,3,3,3,3,3,3,3,3,3,3,3,3,3,3,3,3,3,3,3,3,3,3,3,3,3,3,3,3,3,3,
3,3,3,3,3,3,3,3,3,3,3,3,3,3,3,3,3,3,3,3,3,3,3,4),(13.6883869010745,13.8285226780631,
13.9202995807391,14.0257190109509,14.1309808405734,14.2361199688695,14.3411938517453,
14.4462383994047,14.5512894785142,14.6564517917807,14.7616770736072,14.8670820028861,
14.914606693649,15.0200261120377,15.1252879298801,15.2304270465202,15.3355009178248,
15.4405454540164,15.5455965217802,15.6507588239649,15.7559840948451,15.8613890135014,
15.9089138065589,16.0143332095239,16.1195950115914,16.2247341120157,16.3298079668403,
16.4348524863131,16.5399035371446,16.6450658221904,16.7502910757889,16.8556959771237,
16.9032209194689,17.0086403327036,17.1139021452095,17.2190412562692,17.3241151218452,
17.4291596521685,17.5342107139331,17.6393730099613,17.7445982745861,17.8500031868997,
17.8975280323788,18.0029474438031,18.1082092544879,18.2133483637203,18.3184222274662,
18.4234667559597,18.5285178158973,18.6336801101162,18.738905372939,18.8443102834809,
18.8918351452887,18.9972545557072,19.1025163653571,19.2076554735164,19.3127293361661,
19.417773863542,19.5228249223424,19.6279872154019,19.7332124770511,19.8386173864095,
19.8861422581987,19.9715722082541),.UNSPECIFIED.) ;
#1748 = B_SPLINE_CURVE_WITH_KNOTS('',3,(#114850,#114851,#114852,#114853,#114854,
#114855,#114856,#114857,#114858,#114859,#114860,#114861,#114862,#114863,
#114864,#114865,#114866,#114867,#114868,#114869,#114870,#114871,#114872,
#114873,#114874,#114875,#114876,#114877,#114878,#114879,#114880,#114881,
#114882,#114883,#114884,#114885,#114886,#114887,#114888,#114889,#114890,
#114891,#114892,#114893,#114894,#114895,#114896,#114897,#114898,#114899,
#114900,#114901,#114902,#114903,#114904,#114905,#114906,#114907,#114908,
#114909,#114910,#114911,#114912,#114913,#114914,#114915,#114916,#114917,
#114918,#114919,#114920,#114921,#114922,#114923,#114924,#114925,#114926,
#114927,#114928,#114929,#114930,#114931,#114932,#114933,#114934,#114935,
#114936,#114937,#114938,#114939,#114940,#114941,#114942,#114943,#114944,
#114945,#114946,#114947,#114948,#114949,#114950,#114951,#114952,#114953,
#114954,#114955,#114956,#114957,#114958,#114959,#114960,#114961,#114962,
#114963,#114964,#114965,#114966,#114967,#114968,#114969,#114970,#114971,
#114972,#114973,#114974,#114975,#114976,#114977,#114978,#114979,#114980,
#114981,#114982,#114983,#114984,#114985,#114986,#114987,#114988,#114989,
#114990,#114991,#114992,#114993,#114994,#114995,#114996,#114997,#114998,
#114999,#115000,#115001,#115002,#115003,#115004,#115005,#115006,#115007,
#115008,#115009,#115010,#115011,#115012,#115013,#115014,#115015,#115016,
#115017,#115018,#115019,#115020,#115021,#115022,#115023,#115024,#115025,
#115026,#115027,#115028,#115029,#115030,#115031,#115032,#115033,#115034,
#115035,#115036,#115037,#115038,#115039),.UNSPECIFIED.,.F.,.F.,(4,3,3,3,
3,3,3,3,3,3,3,3,3,3,3,3,3,3,3,3,3,3,3,3,3,3,3,3,3,3,3,3,3,3,3,3,3,3,3,3,
3,3,3,3,3,3,3,3,3,3,3,3,3,3,3,3,3,3,3,3,3,3,3,4),(19.9715722087079,20.0757526573405,
20.1797732687495,20.2837058335539,20.3875878870888,20.4914568929667,20.5954209680976,
20.699433391534,20.8036305474994,20.8804493711086,20.9858687826337,21.0911305933964,
21.1962697026724,21.3013435664408,21.4063880949356,21.5114391548532,21.6166014490203,
21.7218267117734,21.8272316222182,21.8747564840186,21.9801758973058,22.0854377098522,
22.1905768209346,22.2956506865221,22.4006952168461,22.5057462786001,22.6109085746013,
22.7161338391897,22.8215387514525,22.8690635969285,22.9744829992754,23.0797448008656,
23.1848839010226,23.2899577557102,23.3950022751763,23.5000533261311,23.6052156114951,
23.7104408655235,23.8158457674549,23.8633707098384,23.9687901294618,24.0740519482573,
24.1791910654315,24.2842649370099,24.3893094732149,24.4943605407323,24.5995228422816,
24.7047481123027,24.8101530297671,24.8576778227484,24.9630972529186,25.0683590825089,
25.1734982107868,25.2785720936532,25.3836166413118,25.4886677204293,25.5938300337168,
25.6990553155718,25.8044602448903,25.8519849356583,25.9685846308431,26.0848174253634,
26.2004492469501,26.2547575150606),.UNSPECIFIED.) ;
#1749 = B_SPLINE_CURVE_WITH_KNOTS('',3,(#115041,#115042,#115043,#115044,#115045,
#115046,#115047,#115048,#115049,#115050,#115051,#115052,#115053,#115054,
#115055,#115056,#115057,#115058,#115059,#115060,#115061,#115062,#115063,
#115064,#115065,#115066,#115067,#115068,#115069,#115070,#115071,#115072,
#115073,#115074,#115075,#115076,#115077,#115078,#115079,#115080,#115081,
#115082,#115083,#115084,#115085,#115086,#115087,#115088,#115089,#115090,
#115091,#115092,#115093,#115094,#115095,#115096,#115097,#115098,#115099,
#115100,#115101,#115102,#115103,#115104,#115105,#115106,#115107,#115108,
#115109,#115110,#115111,#115112,#115113,#115114,#115115,#115116,#115117,
#115118,#115119,#115120,#115121,#115122,#115123,#115124,#115125,#115126,
#115127,#115128,#115129,#115130,#115131,#115132,#115133,#115134,#115135,
#115136,#115137,#115138,#115139,#115140,#115141,#115142,#115143,#115144,
#115145,#115146,#115147,#115148,#115149,#115150,#115151,#115152,#115153,
#115154,#115155,#115156,#115157,#115158,#115159,#115160,#115161,#115162,
#115163,#115164,#115165,#115166,#115167,#115168,#115169,#115170,#115171,
#115172,#115173,#115174,#115175,#115176,#115177,#115178,#115179,#115180,
#115181,#115182,#115183,#115184,#115185,#115186,#115187,#115188,#115189,
#115190,#115191,#115192,#115193,#115194,#115195,#115196,#115197,#115198,
#115199,#115200,#115201,#115202,#115203,#115204,#115205,#115206,#115207,
#115208,#115209,#115210,#115211,#115212,#115213,#115214,#115215,#115216,
#115217,#115218,#115219,#115220,#115221,#115222,#115223,#115224,#115225,
#115226,#115227,#115228,#115229,#115230),.UNSPECIFIED.,.F.,.F.,(4,3,3,3,
3,3,3,3,3,3,3,3,3,3,3,3,3,3,3,3,3,3,3,3,3,3,3,3,3,3,3,3,3,3,3,3,3,3,3,3,
3,3,3,3,3,3,3,3,3,3,3,3,3,3,3,3,3,3,3,3,3,3,3,4),(26.2547575154336,26.3613465931618,
26.4679789682056,26.5747709772014,26.6816506924515,26.7887463962673,26.8462920485682,
26.9517115711595,27.0569734923618,27.1621127106266,27.2671866824188,27.3722313178148,
27.4772824833525,27.5824448805035,27.68767024488,27.7930752538197,27.8405991614782,
27.9460187071456,28.0512806539019,28.1564199012058,28.2614939041769,28.3665385728247,
28.4715897736222,28.5767522087774,28.6819776127802,28.7873826633883,28.8349062743881,
28.9403248515837,29.0455858266276,29.1507241022328,29.2557971341069,29.3608408337486,
29.4658910691218,29.5710525508493,29.6762770069266,29.7816811279033,29.829213387298,
29.9346341294826,30.039897265652,30.1450376862259,30.2501128517563,30.3551586705575,
30.4602110073962,30.5653745497481,30.6706010460371,30.7760071548619,30.823520500208,
30.9289406478903,31.0342032137143,31.1393431019143,31.2444177589056,31.3494630935756,
31.4545149712888,31.5596780949041,31.6649041949384,31.7703099457485,31.8178276131179,
31.9222753937316,32.0265781783092,32.1307733970436,32.2349210195028,32.3390353788241,
32.4432146412587,32.5379428226133),.UNSPECIFIED.) ;
#1750 = B_SPLINE_CURVE_WITH_KNOTS('',3,(#115232,#115233,#115234,#115235,#115236,
#115237,#115238,#115239,#115240,#115241,#115242,#115243,#115244,#115245,
#115246,#115247,#115248,#115249,#115250,#115251,#115252,#115253,#115254,
#115255,#115256,#115257,#115258,#115259,#115260,#115261,#115262,#115263,
#115264,#115265,#115266,#115267,#115268,#115269,#115270,#115271,#115272,
#115273,#115274,#115275,#115276,#115277,#115278,#115279,#115280,#115281,
#115282,#115283,#115284,#115285,#115286,#115287,#115288,#115289,#115290,
#115291,#115292,#115293,#115294,#115295,#115296,#115297,#115298,#115299,
#115300,#115301,#115302,#115303,#115304,#115305,#115306,#115307,#115308,
#115309,#115310,#115311,#115312,#115313,#115314,#115315,#115316,#115317,
#115318,#115319,#115320,#115321,#115322,#115323,#115324,#115325,#115326,
#115327,#115328,#115329,#115330,#115331,#115332,#115333,#115334,#115335,
#115336,#115337,#115338,#115339,#115340,#115341,#115342,#115343,#115344,
#115345,#115346,#115347,#115348,#115349,#115350,#115351,#115352,#115353,
#115354,#115355,#115356,#115357,#115358,#115359,#115360,#115361,#115362,
#115363,#115364,#115365,#115366,#115367,#115368,#115369,#115370,#115371,
#115372,#115373,#115374,#115375,#115376,#115377,#115378,#115379,#115380,
#115381,#115382,#115383,#115384,#115385,#115386,#115387,#115388),
 .UNSPECIFIED.,.F.,.F.,(4,3,3,3,3,3,3,3,3,3,3,3,3,3,3,3,3,3,3,3,3,3,3,3,
3,3,3,3,3,3,3,3,3,3,3,3,3,3,3,3,3,3,3,3,3,3,3,3,3,3,3,3,4),(32.5379428229721,
32.6678523512312,32.8000400073029,32.8121347260278,32.9175693101144,33.0228462514619,
33.1280003562829,33.2330891227617,33.3381484389358,33.4432141491931,33.5483907880401,
33.6536302410997,33.7590489588567,33.8064418389378,33.9118624358314,34.0171256129785,
34.1222663450006,34.227341989137,34.3323884512563,34.4374415938531,34.5426061775443,
34.6478338512062,34.7532413307192,34.8007489518477,34.9060950858955,35.0112833633988,
35.1163489210678,35.2213492651478,35.3263204169927,35.4312983545223,35.5363884064698,
35.6415418258675,35.7468762517544,35.7950560647576,35.9006360132837,36.0060581843695,
36.1113566104704,36.2165890420641,36.3217911483003,36.4269985538351,36.5323142802526,
36.6376915209163,36.7432446207726,36.7893631776676,36.8934851122297,36.9974335047275,
37.101285461222,37.2050786426096,37.3088506264494,37.412705978262,37.5166028168842,
37.6206751761,37.6991118430775),.UNSPECIFIED.) ;
#1751 = B_SPLINE_CURVE_WITH_KNOTS('',3,(#115389,#115390,#115391,#115392),
 .UNSPECIFIED.,.F.,.F.,(4,4),(-0.0487088993428013,0.),.UNSPECIFIED.) ;
#1752 = B_SPLINE_CURVE_WITH_KNOTS('',3,(#115397,#115398,#115399,#115400,#115401,
#115402,#115403,#115404,#115405,#115406,#115407,#115408,#115409,#115410,
#115411,#115412,#115413,#115414,#115415,#115416,#115417,#115418,#115419,
#115420,#115421,#115422,#115423,#115424,#115425,#115426,#115427,#115428,
#115429,#115430,#115431,#115432,#115433,#115434,#115435,#115436,#115437,
#115438,#115439,#115440,#115441,#115442,#115443,#115444,#115445,#115446,
#115447,#115448,#115449,#115450,#115451,#115452,#115453,#115454,#115455,
#115456,#115457,#115458,#115459,#115460,#115461,#115462,#115463,#115464,
#115465,#115466,#115467,#115468,#115469,#115470,#115471,#115472,#115473,
#115474,#115475,#115476,#115477,#115478,#115479,#115480,#115481,#115482,
#115483,#115484,#115485,#115486,#115487,#115488,#115489,#115490,#115491,
#115492,#115493,#115494,#115495,#115496,#115497,#115498,#115499,#115500,
#115501,#115502,#115503,#115504),.UNSPECIFIED.,.F.,.F.,(4,2,2,2,2,2,2,2,
2,2,2,2,2,2,2,2,2,2,2,2,2,2,2,2,2,2,2,2,2,2,2,2,2,2,2,2,2,2,2,2,2,2,2,2,
2,2,2,2,2,2,2,2,2,4),(-0.712529018801462,-0.692215766132187,-0.664135864238742,
-0.658240027550338,-0.65482564774828,-0.651510806762373,-0.646109027517185,
-0.620883198311623,-0.586121850216688,-0.5772399037717,-0.571437147349492,
-0.565706665075696,-0.557223325800328,-0.547208645040879,-0.525513742714016,
-0.497097727813206,-0.491238951503433,-0.487834075555186,-0.484537915090653,
-0.479163400168952,-0.454304399302376,-0.418678985728483,-0.409866567247856,
-0.404097580583173,-0.398395458960152,-0.389949910340539,-0.360561181362236,
-0.329412523059719,-0.323757230869978,-0.320400114298294,-0.317033346831293,
-0.311416967020911,-0.282511821131457,-0.252233820777348,-0.243100580417461,
-0.237232557741588,-0.231505891629165,-0.22315293004513,-0.189759578067865,
-0.163006081390897,-0.156972073278048,-0.15351761524682,-0.150169378793417,
-0.144734566387307,-0.137933698959475,-0.122196090774211,-0.0850532115423573,
-0.0765779487325186,-0.0714002462994081,-0.0656613420703193,-0.0572626031513613,
-0.0474086202233217,-0.0264640630640861,-0.00352947697862977),
 .UNSPECIFIED.) ;
#1753 = B_SPLINE_CURVE_WITH_KNOTS('',3,(#115508,#115509,#115510,#115511,#115512,
#115513,#115514,#115515,#115516,#115517,#115518,#115519,#115520,#115521,
#115522,#115523,#115524,#115525,#115526,#115527,#115528,#115529,#115530,
#115531,#115532,#115533,#115534,#115535),.UNSPECIFIED.,.F.,.F.,(4,3,3,3,
3,3,3,3,3,4),(47.1238898043947,47.2352837902631,47.3464400309164,47.4574585890731,
47.5683762665546,47.6792297317267,47.7900945032509,47.900961870412,48.0119293664921,
48.0750461904514),.UNSPECIFIED.) ;
#1754 = B_SPLINE_CURVE_WITH_KNOTS('',3,(#115536,#115537,#115538,#115539,#115540,
#115541,#115542,#115543,#115544,#115545,#115546,#115547,#115548,#115549,
#115550,#115551,#115552,#115553,#115554,#115555,#115556,#115557,#115558,
#115559,#115560,#115561,#115562,#115563,#115564,#115565,#115566,#115567,
#115568,#115569,#115570,#115571,#115572,#115573,#115574,#115575,#115576,
#115577,#115578,#115579,#115580,#115581,#115582,#115583,#115584,#115585,
#115586,#115587,#115588,#115589,#115590,#115591,#115592,#115593,#115594,
#115595,#115596),.UNSPECIFIED.,.F.,.F.,(4,3,3,3,3,3,3,3,3,3,3,3,3,3,3,3,
3,3,3,3,4),(45.0774317841423,45.0921248517216,45.2017087476041,45.3122991497326,
45.4215907363396,45.5308188028355,45.6400238367858,45.7516258687472,45.8609770374908,
45.9737045010611,46.0864319646315,46.1954426168905,46.3061046744719,46.4148166958695,
46.5234644023138,46.6320892195687,46.7442516840619,46.8530297571829,46.9668844173622,
47.0807390775415,47.1238898038469),.UNSPECIFIED.) ;
#1755 = B_SPLINE_CURVE_WITH_KNOTS('',3,(#115599,#115600,#115601,#115602,#115603,
#115604,#115605,#115606,#115607,#115608,#115609,#115610,#115611,#115612,
#115613,#115614,#115615,#115616,#115617,#115618,#115619,#115620,#115621,
#115622,#115623,#115624,#115625,#115626,#115627,#115628,#115629,#115630,
#115631,#115632,#115633,#115634,#115635,#115636,#115637,#115638,#115639,
#115640,#115641,#115642,#115643,#115644,#115645,#115646,#115647,#115648,
#115649,#115650,#115651,#115652,#115653,#115654,#115655,#115656,#115657,
#115658,#115659,#115660,#115661,#115662,#115663,#115664,#115665,#115666,
#115667,#115668,#115669,#115670,#115671,#115672,#115673,#115674,#115675,
#115676,#115677,#115678,#115679,#115680,#115681,#115682,#115683,#115684,
#115685,#115686,#115687,#115688,#115689,#115690,#115691,#115692,#115693,
#115694),.UNSPECIFIED.,.F.,.F.,(4,2,2,2,2,2,2,2,2,2,2,2,2,2,2,2,2,2,2,2,
2,2,2,2,2,2,2,2,2,2,2,2,2,2,2,2,2,2,2,2,2,2,2,2,2,2,2,4),(0.0026151563363548,
0.0179899578167905,0.0472044811745065,0.0576295306852423,0.0662273340337798,
0.0770918755822315,0.104350311824498,0.124050281215216,0.132515561685311,
0.139413475602386,0.144360237891016,0.151347291161069,0.179374142514947,
0.209542405261021,0.219879444032952,0.228451041843246,0.239320643288716,
0.269825786465474,0.296023856051,0.302771836078026,0.307671052620665,0.314629037379767,
0.342607736599612,0.37249921285926,0.382872374942502,0.391361215872602,
0.402138206335904,0.425642624421977,0.456294846706203,0.46460630768549,
0.469613781743472,0.475497265298997,0.487976737859294,0.515898642790773,
0.531093292477762,0.54347082513099,0.552130780531028,0.561688755483493,
0.580959665388665,0.615071972976662,0.623009519934321,0.629591131217097,
0.634497357221016,0.641651525729804,0.661384245233401,0.686587476454549,
0.703154313183141,0.712378143918981),.UNSPECIFIED.) ;
#1756 = B_SPLINE_CURVE_WITH_KNOTS('',3,(#115698,#115699,#115700,#115701,#115702,
#115703,#115704,#115705,#115706,#115707,#115708,#115709,#115710,#115711,
#115712,#115713,#115714,#115715,#115716,#115717,#115718,#115719,#115720,
#115721,#115722,#115723,#115724,#115725),.UNSPECIFIED.,.F.,.F.,(4,3,3,3,
3,3,3,3,3,4),(34.557519189987,34.6694584461235,34.7811724399487,34.8927552132247,
35.0042418725079,35.1156673936037,35.2271037225296,35.338542288418,35.4500742527154,
35.508675576092),.UNSPECIFIED.) ;
#1757 = B_SPLINE_CURVE_WITH_KNOTS('',3,(#115726,#115727,#115728,#115729,#115730,
#115731,#115732,#115733,#115734,#115735,#115736,#115737,#115738,#115739,
#115740,#115741,#115742,#115743,#115744,#115745,#115746,#115747,#115748,
#115749,#115750,#115751,#115752,#115753,#115754,#115755,#115756,#115757,
#115758,#115759,#115760,#115761,#115762,#115763,#115764,#115765,#115766,
#115767,#115768,#115769,#115770,#115771,#115772,#115773,#115774,#115775,
#115776,#115777,#115778,#115779,#115780,#115781,#115782,#115783,#115784,
#115785,#115786),.UNSPECIFIED.,.F.,.F.,(4,3,3,3,3,3,3,3,3,3,3,3,3,3,3,3,
3,3,3,3,4),(32.5109032341381,32.5937562294451,32.7036640037873,32.8133945161912,
32.9230264084955,33.0325996547794,33.1421541476789,33.2518066805613,33.3615061631074,
33.4714063488116,33.5653960116607,33.6748026965323,33.7840268426677,33.8931495282482,
34.0022116569275,34.1112540474795,34.2203971020844,34.3295877652005,34.4389867358328,
34.5370357938764,34.5575191894878),.UNSPECIFIED.) ;
#1758 = B_SPLINE_CURVE_WITH_KNOTS('',3,(#115788,#115789,#115790,#115791,#115792,
#115793,#115794,#115795,#115796,#115797,#115798,#115799,#115800,#115801,
#115802,#115803,#115804,#115805,#115806,#115807,#115808,#115809,#115810,
#115811,#115812,#115813,#115814,#115815,#115816,#115817,#115818,#115819,
#115820,#115821,#115822,#115823,#115824,#115825,#115826,#115827,#115828,
#115829,#115830,#115831,#115832,#115833,#115834,#115835,#115836,#115837,
#115838,#115839,#115840,#115841,#115842,#115843,#115844,#115845,#115846,
#115847,#115848,#115849,#115850,#115851,#115852,#115853,#115854,#115855,
#115856,#115857,#115858,#115859,#115860,#115861,#115862,#115863,#115864,
#115865,#115866,#115867,#115868,#115869,#115870,#115871,#115872),
 .UNSPECIFIED.,.F.,.F.,(4,3,3,3,3,3,3,3,3,3,3,3,3,3,3,3,3,3,3,3,3,3,3,3,
3,3,3,3,4),(-0.375230238529917,-0.357518914002748,-0.353499339011933,-0.330618426268482,
-0.324807980319591,-0.303153187739658,-0.286565543905241,-0.280293721854319,
-0.274975125238719,-0.253681437664564,-0.232737497017393,-0.217166132029125,
-0.208374669734109,-0.204725951335004,-0.184285942423822,-0.170452037064323,
-0.149145532431283,-0.139823936654328,-0.135833708785121,-0.132392631626963,
-0.112078350447567,-0.0917069570560497,-0.071654175354626,-0.0676263159013853,
-0.0641204348977771,-0.0443305734284611,-0.0248574443104007,-0.00603170532718953,
0.),.UNSPECIFIED.) ;
#1759 = B_SPLINE_CURVE_WITH_KNOTS('',3,(#115874,#115875,#115876,#115877),
 .UNSPECIFIED.,.F.,.F.,(4,4),(0.,0.0129878021108932),.UNSPECIFIED.) ;
#1760 = B_SPLINE_CURVE_WITH_KNOTS('',3,(#115878,#115879,#115880,#115881,#115882,
#115883,#115884,#115885,#115886,#115887,#115888,#115889,#115890,#115891,
#115892,#115893,#115894,#115895,#115896,#115897,#115898,#115899,#115900,
#115901,#115902,#115903,#115904,#115905,#115906,#115907,#115908,#115909,
#115910,#115911,#115912,#115913,#115914,#115915,#115916,#115917,#115918,
#115919,#115920,#115921,#115922,#115923,#115924,#115925,#115926,#115927,
#115928,#115929,#115930,#115931,#115932,#115933,#115934,#115935,#115936,
#115937,#115938,#115939,#115940,#115941,#115942,#115943,#115944,#115945,
#115946,#115947,#115948,#115949,#115950,#115951,#115952,#115953,#115954,
#115955,#115956,#115957,#115958,#115959,#115960,#115961,#115962,#115963,
#115964,#115965),.UNSPECIFIED.,.F.,.F.,(4,3,3,3,3,3,3,3,3,3,3,3,3,3,3,3,
3,3,3,3,3,3,3,3,3,3,3,3,3,4),(-0.380169894663495,-0.360311041953257,-0.358093714841347,
-0.344714901897815,-0.336915301102773,-0.332696968908371,-0.312888567026539,
-0.296964077029212,-0.291611757449479,-0.287054572082553,-0.266750979851411,
-0.246125107358001,-0.23096699228048,-0.222333842397338,-0.217980610353271,
-0.196924266505527,-0.185492647047918,-0.164983292057223,-0.154671836303647,
-0.149608821797306,-0.146454059323621,-0.125463742568063,-0.104059845569569,
-0.082556275683466,-0.0772769044299627,-0.0730030946602837,-0.0510590776608034,
-0.0291391974875742,-0.0077601331035521,0.),.UNSPECIFIED.) ;
#1761 = B_SPLINE_CURVE_WITH_KNOTS('',3,(#116091,#116092,#116093,#116094,#116095,
#116096,#116097,#116098,#116099,#116100,#116101,#116102,#116103,#116104,
#116105,#116106,#116107,#116108,#116109,#116110,#116111,#116112,#116113,
#116114,#116115,#116116,#116117,#116118,#116119,#116120,#116121,#116122,
#116123,#116124,#116125,#116126,#116127,#116128,#116129,#116130,#116131,
#116132,#116133,#116134,#116135,#116136,#116137,#116138,#116139,#116140,
#116141,#116142,#116143,#116144,#116145,#116146,#116147,#116148,#116149,
#116150,#116151,#116152,#116153,#116154,#116155,#116156,#116157,#116158,
#116159,#116160,#116161,#116162,#116163,#116164,#116165,#116166,#116167,
#116168,#116169,#116170,#116171,#116172,#116173,#116174,#116175,#116176,
#116177,#116178),.UNSPECIFIED.,.F.,.F.,(4,3,3,3,3,3,3,3,3,3,3,3,3,3,3,3,
3,3,3,3,3,3,3,3,3,3,3,3,3,4),(-0.380169894663605,-0.360311041858371,-0.358093714841452,
-0.344714902065716,-0.336915300765293,-0.33269696876484,-0.312888566814864,
-0.296964076844001,-0.291611755955825,-0.287054571535372,-0.266750979273317,
-0.2461251068382,-0.230966991890641,-0.222333842148618,-0.217980610319933,
-0.196924266519412,-0.185492647047962,-0.164983291825849,-0.154671836086734,
-0.149608821363363,-0.146454058645083,-0.125531321942587,-0.104043798334106,
-0.0825562747256238,-0.0772769030728362,-0.0730030943857931,-0.0510590773577688,
-0.0291391975209706,-0.00776013404481242,0.),.UNSPECIFIED.) ;
#1762 = B_SPLINE_CURVE_WITH_KNOTS('',3,(#116179,#116180,#116181,#116182),
 .UNSPECIFIED.,.F.,.F.,(4,4),(-0.0129879181954274,0.),.UNSPECIFIED.) ;
#1763 = B_SPLINE_CURVE_WITH_KNOTS('',3,(#116184,#116185,#116186,#116187,#116188,
#116189,#116190,#116191,#116192,#116193,#116194,#116195,#116196,#116197,
#116198,#116199,#116200,#116201,#116202,#116203,#116204,#116205,#116206,
#116207,#116208,#116209,#116210,#116211,#116212,#116213,#116214,#116215,
#116216,#116217,#116218,#116219,#116220,#116221,#116222,#116223,#116224,
#116225,#116226,#116227,#116228,#116229,#116230,#116231,#116232,#116233,
#116234,#116235,#116236,#116237,#116238,#116239,#116240,#116241,#116242,
#116243,#116244,#116245,#116246,#116247,#116248,#116249,#116250,#116251,
#116252,#116253,#116254,#116255,#116256,#116257,#116258,#116259,#116260,
#116261,#116262,#116263,#116264,#116265,#116266,#116267,#116268),
 .UNSPECIFIED.,.F.,.F.,(4,3,3,3,3,3,3,3,3,3,3,3,3,3,3,3,3,3,3,3,3,3,3,3,
3,3,3,3,4),(-0.375230298695406,-0.357518914044833,-0.353499339011814,-0.330618426268376,
-0.324807980341732,-0.303153187730854,-0.286565543897536,-0.280293721896857,
-0.27497512524351,-0.253681437665961,-0.232737497308779,-0.217166132247661,
-0.208374670197327,-0.204725951707223,-0.184285943084061,-0.170452037064309,
-0.14914553243127,-0.139823936654316,-0.135833708541921,-0.132392631416531,
-0.112078350352873,-0.0917069566471694,-0.0716541742035818,-0.067626310494424,
-0.0641204340447217,-0.0443305720467959,-0.0250908100884248,-0.00603170206196263,
-5.00355929031884E-15),.UNSPECIFIED.) ;
#1764 = B_SPLINE_CURVE_WITH_KNOTS('',3,(#116394,#116395,#116396,#116397,#116398,
#116399,#116400,#116401,#116402,#116403,#116404,#116405,#116406,#116407,
#116408,#116409,#116410,#116411,#116412,#116413,#116414,#116415,#116416,
#116417,#116418,#116419,#116420,#116421,#116422,#116423,#116424,#116425,
#116426,#116427,#116428,#116429,#116430,#116431,#116432,#116433,#116434,
#116435,#116436,#116437,#116438,#116439,#116440,#116441,#116442,#116443,
#116444,#116445,#116446,#116447,#116448,#116449,#116450,#116451,#116452,
#116453,#116454,#116455,#116456,#116457,#116458,#116459,#116460,#116461,
#116462,#116463,#116464,#116465,#116466,#116467,#116468,#116469,#116470,
#116471,#116472,#116473,#116474,#116475,#116476,#116477,#116478,#116479,
#116480,#116481),.UNSPECIFIED.,.F.,.F.,(4,3,3,3,3,3,3,3,3,3,3,3,3,3,3,3,
3,3,3,3,3,3,3,3,3,3,3,3,3,4),(-0.374020018364427,-0.362349077150302,-0.34056398080081,
-0.33345324485073,-0.328206439767411,-0.323553301020776,-0.301861361668488,
-0.285952048119608,-0.279252129425629,-0.275334282185498,-0.254027310368013,
-0.233103842154587,-0.218474594935304,-0.206338981465346,-0.202820931586694,
-0.182410565592875,-0.174586853277452,-0.153875936134864,-0.143831381828718,
-0.13799507666095,-0.134412923455841,-0.114104327564578,-0.0937141935060995,
-0.0736245310869828,-0.0688062389308537,-0.0640039679130607,-0.0442183910804699,
-0.0247594363974842,-0.00595275431251839,0.),.UNSPECIFIED.) ;
#1765 = B_SPLINE_CURVE_WITH_KNOTS('',3,(#116483,#116484,#116485,#116486),
 .UNSPECIFIED.,.F.,.F.,(4,4),(0.,0.0180654173549806),.UNSPECIFIED.) ;
#1766 = B_SPLINE_CURVE_WITH_KNOTS('',3,(#116487,#116488,#116489,#116490,#116491,
#116492,#116493,#116494,#116495,#116496,#116497,#116498,#116499,#116500,
#116501,#116502,#116503,#116504,#116505,#116506,#116507,#116508,#116509,
#116510,#116511,#116512,#116513,#116514,#116515,#116516,#116517,#116518,
#116519,#116520,#116521,#116522,#116523,#116524,#116525,#116526,#116527,
#116528,#116529,#116530,#116531,#116532,#116533,#116534,#116535,#116536,
#116537,#116538,#116539,#116540,#116541,#116542,#116543,#116544,#116545,
#116546,#116547,#116548,#116549,#116550,#116551,#116552,#116553,#116554,
#116555,#116556,#116557,#116558,#116559,#116560,#116561,#116562,#116563,
#116564,#116565,#116566,#116567,#116568,#116569,#116570,#116571,#116572,
#116573,#116574,#116575,#116576,#116577),.UNSPECIFIED.,.F.,.F.,(4,3,3,3,
3,3,3,3,3,3,3,3,3,3,3,3,3,3,3,3,3,3,3,3,3,3,3,3,3,3,4),(-0.380169894663632,
-0.365829779172372,-0.346639954767462,-0.338855951704939,-0.33481170502711,
-0.31500122031449,-0.299335348941147,-0.290828675949366,-0.287130866641693,
-0.266780066890063,-0.246135635921242,-0.232029437966579,-0.224974018565242,
-0.220447300081947,-0.217112258820216,-0.196051485500263,-0.189674249327746,
-0.169242036501509,-0.158592891500461,-0.152820666006991,-0.149331434698219,
-0.145470149822495,-0.124229913596774,-0.102989677371053,-0.0814839825252319,
-0.0765643464165228,-0.0730763435899889,-0.0511173678544621,-0.0291950315550003,
-0.00783050913432987,0.),.UNSPECIFIED.) ;
#1767 = B_SPLINE_CURVE_WITH_KNOTS('',3,(#116750,#116751,#116752,#116753,#116754,
#116755,#116756,#116757,#116758,#116759,#116760,#116761,#116762,#116763,
#116764,#116765,#116766,#116767,#116768,#116769,#116770,#116771,#116772,
#116773,#116774,#116775,#116776,#116777,#116778,#116779,#116780,#116781,
#116782,#116783,#116784,#116785,#116786,#116787,#116788,#116789,#116790,
#116791,#116792,#116793,#116794,#116795,#116796,#116797,#116798,#116799,
#116800,#116801,#116802,#116803,#116804,#116805,#116806,#116807,#116808,
#116809,#116810,#116811,#116812,#116813,#116814,#116815,#116816,#116817,
#116818,#116819,#116820,#116821,#116822,#116823,#116824,#116825,#116826,
#116827,#116828,#116829,#116830,#116831,#116832,#116833,#116834,#116835,
#116836,#116837,#116838,#116839,#116840),.UNSPECIFIED.,.F.,.F.,(4,3,3,3,
3,3,3,3,3,3,3,3,3,3,3,3,3,3,3,3,3,3,3,3,3,3,3,3,3,3,4),(-0.380169894663596,
-0.365829779172345,-0.346639954384228,-0.338855950466618,-0.334811703196154,
-0.315001218246295,-0.299335347131477,-0.290828672854654,-0.287130864274129,
-0.266780064403244,-0.246147831802541,-0.232029436183843,-0.224974014860838,
-0.220447286668042,-0.217112256507811,-0.196051483279599,-0.189674249327752,
-0.169242036096976,-0.158592891228521,-0.152820665783821,-0.149331432694279,
-0.145470149474333,-0.124229912877894,-0.102989676281454,-0.0814839817255933,
-0.0765643433675259,-0.0730763417070937,-0.0511173658980769,-0.0291950301878927,
-0.00783050936092446,0.),.UNSPECIFIED.) ;
#1768 = B_SPLINE_CURVE_WITH_KNOTS('',3,(#116842,#116843,#116844,#116845,#116846,
#116847,#116848,#116849,#116850,#116851,#116852,#116853,#116854,#116855,
#116856,#116857,#116858,#116859,#116860,#116861,#116862,#116863,#116864,
#116865,#116866,#116867,#116868,#116869,#116870,#116871,#116872,#116873,
#116874,#116875,#116876,#116877,#116878,#116879,#116880,#116881,#116882,
#116883,#116884,#116885,#116886,#116887,#116888,#116889,#116890,#116891,
#116892,#116893,#116894,#116895,#116896,#116897,#116898,#116899,#116900,
#116901,#116902,#116903,#116904,#116905,#116906,#116907,#116908,#116909,
#116910,#116911,#116912,#116913,#116914,#116915,#116916,#116917,#116918,
#116919,#116920,#116921,#116922,#116923,#116924,#116925,#116926,#116927,
#116928,#116929),.UNSPECIFIED.,.F.,.F.,(4,3,3,3,3,3,3,3,3,3,3,3,3,3,3,3,
3,3,3,3,3,3,3,3,3,3,3,3,3,4),(-0.374020098293467,-0.362349077150222,-0.340563980758886,
-0.333453244980001,-0.328206442865421,-0.323553301758691,-0.30186136236912,
-0.285952048732665,-0.279252131280905,-0.275334282105171,-0.254027310290031,
-0.233103842618665,-0.218474595283369,-0.206338981920192,-0.202820931774396,
-0.182410566355118,-0.174586853277482,-0.153875936555904,-0.14383138253821,
-0.137995078806115,-0.134412924715841,-0.114130938170206,-0.0938043258732684,
-0.0736245309349631,-0.0688062385263128,-0.0640039679354593,-0.0442183901736035,
-0.0247594340386698,-0.00595275010025783,-2.53963310401108E-15),
 .UNSPECIFIED.) ;
#1769 = B_SPLINE_SURFACE_WITH_KNOTS('',3,3,((#70269,#70270,#70271,#70272,
#70273,#70274,#70275,#70276,#70277,#70278,#70279,#70280,#70281,#70282,#70283),
(#70284,#70285,#70286,#70287,#70288,#70289,#70290,#70291,#70292,#70293,
#70294,#70295,#70296,#70297,#70298),(#70299,#70300,#70301,#70302,#70303,
#70304,#70305,#70306,#70307,#70308,#70309,#70310,#70311,#70312,#70313),
(#70314,#70315,#70316,#70317,#70318,#70319,#70320,#70321,#70322,#70323,
#70324,#70325,#70326,#70327,#70328),(#70329,#70330,#70331,#70332,#70333,
#70334,#70335,#70336,#70337,#70338,#70339,#70340,#70341,#70342,#70343)),
 .UNSPECIFIED.,.F.,.F.,.F.,(4,1,4),(4,1,1,1,1,1,1,1,1,1,1,1,4),(-0.000196888981062193,
0.571428571428571,1.),(0.598860581847638,0.640127549392609,0.681197628036496,
0.701732667358439,0.722267706680382,0.732535226341353,0.742802746002325,
0.753070265663297,0.763337785324268,0.783872824646211,0.804407863968155,
0.845477942612041,0.886744910236546),.UNSPECIFIED.) ;
#1770 = B_SPLINE_SURFACE_WITH_KNOTS('',3,3,((#70561,#70562,#70563,#70564,
#70565,#70566,#70567,#70568,#70569,#70570,#70571,#70572,#70573,#70574,#70575),
(#70576,#70577,#70578,#70579,#70580,#70581,#70582,#70583,#70584,#70585,
#70586,#70587,#70588,#70589,#70590),(#70591,#70592,#70593,#70594,#70595,
#70596,#70597,#70598,#70599,#70600,#70601,#70602,#70603,#70604,#70605),
(#70606,#70607,#70608,#70609,#70610,#70611,#70612,#70613,#70614,#70615,
#70616,#70617,#70618,#70619,#70620),(#70621,#70622,#70623,#70624,#70625,
#70626,#70627,#70628,#70629,#70630,#70631,#70632,#70633,#70634,#70635)),
 .UNSPECIFIED.,.F.,.F.,.F.,(4,1,4),(4,1,1,1,1,1,1,1,1,1,1,1,4),(0.,0.571428571428571,
1.),(0.599057470748727,0.64012754939261,0.681197628036493,0.701732667358435,
0.712000187019406,0.722267706680377,0.747936505832804,0.76333778532426,
0.804407863968143,0.809541623798628,0.814675383629114,0.845477942612026,
0.886548021255909),.UNSPECIFIED.) ;
#1771 = B_SPLINE_SURFACE_WITH_KNOTS('',3,3,((#70780,#70781,#70782,#70783,
#70784,#70785,#70786,#70787,#70788,#70789,#70790,#70791,#70792,#70793,#70794),
(#70795,#70796,#70797,#70798,#70799,#70800,#70801,#70802,#70803,#70804,
#70805,#70806,#70807,#70808,#70809),(#70810,#70811,#70812,#70813,#70814,
#70815,#70816,#70817,#70818,#70819,#70820,#70821,#70822,#70823,#70824),
(#70825,#70826,#70827,#70828,#70829,#70830,#70831,#70832,#70833,#70834,
#70835,#70836,#70837,#70838,#70839),(#70840,#70841,#70842,#70843,#70844,
#70845,#70846,#70847,#70848,#70849,#70850,#70851,#70852,#70853,#70854)),
 .UNSPECIFIED.,.F.,.F.,.F.,(4,1,4),(4,1,1,1,1,1,1,1,1,1,1,1,4),(-0.000196404178126319,
0.571428571428571,1.),(0.866946666522881,0.908212951238937,0.949282831776868,
0.969817772045833,0.990352712314798,1.00062018244928,1.01088765258376,1.02115512271825,
1.03142259285273,1.05195753312169,1.07249247339066,1.11356235392859,1.15482863864465),
 .UNSPECIFIED.) ;
#1772 = B_SPLINE_SURFACE_WITH_KNOTS('',3,3,((#70999,#71000,#71001,#71002,
#71003,#71004,#71005,#71006,#71007,#71008,#71009,#71010,#71011,#71012,#71013),
(#71014,#71015,#71016,#71017,#71018,#71019,#71020,#71021,#71022,#71023,
#71024,#71025,#71026,#71027,#71028),(#71029,#71030,#71031,#71032,#71033,
#71034,#71035,#71036,#71037,#71038,#71039,#71040,#71041,#71042,#71043),
(#71044,#71045,#71046,#71047,#71048,#71049,#71050,#71051,#71052,#71053,
#71054,#71055,#71056,#71057,#71058),(#71059,#71060,#71061,#71062,#71063,
#71064,#71065,#71066,#71067,#71068,#71069,#71070,#71071,#71072,#71073)),
 .UNSPECIFIED.,.F.,.F.,.F.,(4,1,4),(4,1,1,1,1,1,1,1,1,1,1,1,4),(-0.000196418998065374,
0.571428571428571,1.),(0.124146619524486,0.165413023799523,0.206483009076495,
0.227018001714981,0.247552994353466,0.257820490672709,0.268087986991952,
0.278355483311195,0.288622979630438,0.309157972268924,0.32969296490741,
0.370762950184382,0.412029354459418),.UNSPECIFIED.) ;
#1773 = B_SPLINE_SURFACE_WITH_KNOTS('',3,3,((#71223,#71224,#71225,#71226,
#71227,#71228,#71229,#71230,#71231,#71232,#71233,#71234,#71235,#71236),
(#71237,#71238,#71239,#71240,#71241,#71242,#71243,#71244,#71245,#71246,
#71247,#71248,#71249,#71250),(#71251,#71252,#71253,#71254,#71255,#71256,
#71257,#71258,#71259,#71260,#71261,#71262,#71263,#71264),(#71265,#71266,
#71267,#71268,#71269,#71270,#71271,#71272,#71273,#71274,#71275,#71276,#71277,
#71278),(#71279,#71280,#71281,#71282,#71283,#71284,#71285,#71286,#71287,
#71288,#71289,#71290,#71291,#71292)),.UNSPECIFIED.,.F.,.F.,.F.,(4,1,4),
(4,1,1,1,1,1,1,1,1,1,1,4),(0.,0.571428571428571,1.),(0.190214667974634,
0.251819488780472,0.272354429049085,0.292889369317698,0.303156839452004,
0.313424309586311,0.323691779720617,0.354494190123537,0.375029130392149,
0.395564070660762,0.436633951197988,0.477703831735214),.UNSPECIFIED.) ;
#1774 = B_SPLINE_SURFACE_WITH_KNOTS('',3,3,((#71451,#71452,#71453,#71454,
#71455,#71456,#71457,#71458,#71459,#71460,#71461,#71462,#71463,#71464,#71465),
(#71466,#71467,#71468,#71469,#71470,#71471,#71472,#71473,#71474,#71475,
#71476,#71477,#71478,#71479,#71480),(#71481,#71482,#71483,#71484,#71485,
#71486,#71487,#71488,#71489,#71490,#71491,#71492,#71493,#71494,#71495),
(#71496,#71497,#71498,#71499,#71500,#71501,#71502,#71503,#71504,#71505,
#71506,#71507,#71508,#71509,#71510),(#71511,#71512,#71513,#71514,#71515,
#71516,#71517,#71518,#71519,#71520,#71521,#71522,#71523,#71524,#71525)),
 .UNSPECIFIED.,.F.,.F.,.F.,(4,1,4),(4,1,1,1,1,1,1,1,1,1,1,1,4),(0.,0.571428571428571,
1.),(0.599057470748751,0.640127549392634,0.681197628036517,0.701732667358458,
0.712000187019429,0.7222677066804,0.747936505832826,0.763337785324282,0.804407863968165,
0.80954162379865,0.814675383629136,0.845477942612048,0.88654802125593),
 .UNSPECIFIED.) ;
#1775 = B_SPLINE_SURFACE_WITH_KNOTS('',3,3,((#71670,#71671,#71672,#71673,
#71674,#71675,#71676,#71677,#71678,#71679,#71680,#71681,#71682,#71683,#71684),
(#71685,#71686,#71687,#71688,#71689,#71690,#71691,#71692,#71693,#71694,
#71695,#71696,#71697,#71698,#71699),(#71700,#71701,#71702,#71703,#71704,
#71705,#71706,#71707,#71708,#71709,#71710,#71711,#71712,#71713,#71714),
(#71715,#71716,#71717,#71718,#71719,#71720,#71721,#71722,#71723,#71724,
#71725,#71726,#71727,#71728,#71729),(#71730,#71731,#71732,#71733,#71734,
#71735,#71736,#71737,#71738,#71739,#71740,#71741,#71742,#71743,#71744)),
 .UNSPECIFIED.,.F.,.F.,.F.,(4,1,4),(4,1,1,1,1,1,1,1,1,1,1,1,4),(0.,0.571428571428571,
1.),(0.599057470748744,0.640127549392629,0.681197628036513,0.701732667358455,
0.712000187019426,0.722267706680398,0.747936505832825,0.763337785324282,
0.804407863968166,0.809541623798652,0.814675383629137,0.84547794261205,
0.886548021255935),.UNSPECIFIED.) ;
#1776 = B_SPLINE_SURFACE_WITH_KNOTS('',3,3,((#71889,#71890,#71891,#71892,
#71893,#71894,#71895,#71896,#71897,#71898,#71899,#71900,#71901,#71902,#71903),
(#71904,#71905,#71906,#71907,#71908,#71909,#71910,#71911,#71912,#71913,
#71914,#71915,#71916,#71917,#71918),(#71919,#71920,#71921,#71922,#71923,
#71924,#71925,#71926,#71927,#71928,#71929,#71930,#71931,#71932,#71933),
(#71934,#71935,#71936,#71937,#71938,#71939,#71940,#71941,#71942,#71943,
#71944,#71945,#71946,#71947,#71948),(#71949,#71950,#71951,#71952,#71953,
#71954,#71955,#71956,#71957,#71958,#71959,#71960,#71961,#71962,#71963)),
 .UNSPECIFIED.,.F.,.F.,.F.,(4,1,4),(4,1,1,1,1,1,1,1,1,1,1,1,4),(0.,0.571428571428571,
1.),(0.867143070669756,0.908212951212153,0.949282831754549,0.969817772025747,
0.980085242161346,0.990352712296945,1.01602138763594,1.03142259283934,1.04169006297494,
1.05195753311054,1.07249247338174,1.11356235392413,1.15463223446653),
 .UNSPECIFIED.) ;
#1777 = B_SPLINE_SURFACE_WITH_KNOTS('',3,3,((#72096,#72097,#72098,#72099,
#72100,#72101,#72102,#72103,#72104,#72105,#72106,#72107,#72108,#72109,#72110),
(#72111,#72112,#72113,#72114,#72115,#72116,#72117,#72118,#72119,#72120,
#72121,#72122,#72123,#72124,#72125),(#72126,#72127,#72128,#72129,#72130,
#72131,#72132,#72133,#72134,#72135,#72136,#72137,#72138,#72139,#72140),
(#72141,#72142,#72143,#72144,#72145,#72146,#72147,#72148,#72149,#72150,
#72151,#72152,#72153,#72154,#72155),(#72156,#72157,#72158,#72159,#72160,
#72161,#72162,#72163,#72164,#72165,#72166,#72167,#72168,#72169,#72170)),
 .UNSPECIFIED.,.F.,.F.,.F.,(4,1,4),(4,1,1,1,1,1,1,1,1,1,1,1,4),(0.,0.571428571428571,
1.),(0.124343038522454,0.165413023799424,0.206483009076393,0.227018001714878,
0.23728549803412,0.247552994353363,0.273221735151469,0.288622979630332,
0.298890475949574,0.309157972268817,0.329692964907302,0.370762950184271,
0.41183293546124),.UNSPECIFIED.) ;
#1778 = B_SPLINE_SURFACE_WITH_KNOTS('',3,3,((#72221,#72222,#72223,#72224,
#72225,#72226,#72227,#72228,#72229,#72230,#72231,#72232,#72233,#72234,#72235),
(#72236,#72237,#72238,#72239,#72240,#72241,#72242,#72243,#72244,#72245,
#72246,#72247,#72248,#72249,#72250),(#72251,#72252,#72253,#72254,#72255,
#72256,#72257,#72258,#72259,#72260,#72261,#72262,#72263,#72264,#72265),
(#72266,#72267,#72268,#72269,#72270,#72271,#72272,#72273,#72274,#72275,
#72276,#72277,#72278,#72279,#72280),(#72281,#72282,#72283,#72284,#72285,
#72286,#72287,#72288,#72289,#72290,#72291,#72292,#72293,#72294,#72295)),
 .UNSPECIFIED.,.F.,.F.,.F.,(4,1,4),(4,1,1,1,1,1,1,1,1,1,1,1,4),(0.,0.571428571428571,
1.),(0.19021466797625,0.231284548513244,0.272354429050238,0.292889369318735,
0.303156839452983,0.313424309587232,0.339092984922853,0.354494190124226,
0.364761660258474,0.375029130392723,0.395564070661219,0.436633951198213,
0.477703831735207),.UNSPECIFIED.) ;
#1779 = B_SPLINE_SURFACE_WITH_KNOTS('',3,3,((#72433,#72434,#72435,#72436,
#72437,#72438,#72439,#72440,#72441,#72442,#72443,#72444,#72445,#72446),
(#72447,#72448,#72449,#72450,#72451,#72452,#72453,#72454,#72455,#72456,
#72457,#72458,#72459,#72460),(#72461,#72462,#72463,#72464,#72465,#72466,
#72467,#72468,#72469,#72470,#72471,#72472,#72473,#72474),(#72475,#72476,
#72477,#72478,#72479,#72480,#72481,#72482,#72483,#72484,#72485,#72486,#72487,
#72488),(#72489,#72490,#72491,#72492,#72493,#72494,#72495,#72496,#72497,
#72498,#72499,#72500,#72501,#72502)),.UNSPECIFIED.,.F.,.F.,.F.,(4,1,4),
(4,1,1,1,1,1,1,1,1,1,1,4),(0.,0.571428571428571,1.),(0.599057470748752,
0.660662588714575,0.681197628036517,0.701732667358458,0.712000187019428,
0.722267706680399,0.732535226341369,0.763337785324281,0.783872824646222,
0.804407863968163,0.845477942612046,0.886548021255928),.UNSPECIFIED.) ;
#1780 = B_SPLINE_SURFACE_WITH_KNOTS('',3,3,((#72743,#72744,#72745,#72746,
#72747,#72748,#72749,#72750,#72751,#72752,#72753,#72754,#72755,#72756),
(#72757,#72758,#72759,#72760,#72761,#72762,#72763,#72764,#72765,#72766,
#72767,#72768,#72769,#72770),(#72771,#72772,#72773,#72774,#72775,#72776,
#72777,#72778,#72779,#72780,#72781,#72782,#72783,#72784),(#72785,#72786,
#72787,#72788,#72789,#72790,#72791,#72792,#72793,#72794,#72795,#72796,#72797,
#72798),(#72799,#72800,#72801,#72802,#72803,#72804,#72805,#72806,#72807,
#72808,#72809,#72810,#72811,#72812)),.UNSPECIFIED.,.F.,.F.,.F.,(4,1,4),
(4,1,1,1,1,1,1,1,1,1,1,4),(0.,0.571428571428571,1.),(0.599057470748733,
0.660662588714558,0.681197628036499,0.701732667358441,0.712000187019412,
0.722267706680383,0.732535226341354,0.763337785324266,0.783872824646208,
0.804407863968149,0.845477942612033,0.886548021255916),.UNSPECIFIED.) ;
#1781 = B_SPLINE_SURFACE_WITH_KNOTS('',3,3,((#73037,#73038,#73039,#73040,
#73041,#73042,#73043,#73044,#73045,#73046,#73047,#73048,#73049,#73050,#73051),
(#73052,#73053,#73054,#73055,#73056,#73057,#73058,#73059,#73060,#73061,
#73062,#73063,#73064,#73065,#73066),(#73067,#73068,#73069,#73070,#73071,
#73072,#73073,#73074,#73075,#73076,#73077,#73078,#73079,#73080,#73081),
(#73082,#73083,#73084,#73085,#73086,#73087,#73088,#73089,#73090,#73091,
#73092,#73093,#73094,#73095,#73096),(#73097,#73098,#73099,#73100,#73101,
#73102,#73103,#73104,#73105,#73106,#73107,#73108,#73109,#73110,#73111)),
 .UNSPECIFIED.,.F.,.F.,.F.,(4,1,4),(4,1,1,1,1,1,1,1,1,1,1,1,4),(-0.000196399328153213,
0.571428571428571,1.),(0.866946671401604,0.908212951263578,0.949282831797399,
0.969817772064309,0.99035271233122,1.00062018246467,1.01088765259813,1.02115512273159,
1.03142259286504,1.05195753313195,1.07249247339886,1.11356235393268,1.15482863379465),
 .UNSPECIFIED.) ;
#1782 = B_SPLINE_SURFACE_WITH_KNOTS('',3,3,((#73328,#73329,#73330,#73331,
#73332,#73333,#73334,#73335,#73336,#73337,#73338,#73339,#73340,#73341,#73342),
(#73343,#73344,#73345,#73346,#73347,#73348,#73349,#73350,#73351,#73352,
#73353,#73354,#73355,#73356,#73357),(#73358,#73359,#73360,#73361,#73362,
#73363,#73364,#73365,#73366,#73367,#73368,#73369,#73370,#73371,#73372),
(#73373,#73374,#73375,#73376,#73377,#73378,#73379,#73380,#73381,#73382,
#73383,#73384,#73385,#73386,#73387),(#73388,#73389,#73390,#73391,#73392,
#73393,#73394,#73395,#73396,#73397,#73398,#73399,#73400,#73401,#73402)),
 .UNSPECIFIED.,.F.,.F.,.F.,(4,1,4),(4,1,1,1,1,1,1,1,1,1,1,1,4),(0.,0.571428571428571,
1.),(0.124343038522312,0.165413023799283,0.206483009076254,0.22701800171474,
0.237285498033983,0.247552994353225,0.26295423883209,0.288622979630197,
0.29889047594944,0.309157972268682,0.329692964907168,0.370762950184139,
0.411832935461111),.UNSPECIFIED.) ;
#1783 = B_SPLINE_SURFACE_WITH_KNOTS('',3,3,((#73531,#73532,#73533,#73534,
#73535,#73536,#73537,#73538,#73539,#73540,#73541,#73542,#73543,#73544,#73545),
(#73546,#73547,#73548,#73549,#73550,#73551,#73552,#73553,#73554,#73555,
#73556,#73557,#73558,#73559,#73560),(#73561,#73562,#73563,#73564,#73565,
#73566,#73567,#73568,#73569,#73570,#73571,#73572,#73573,#73574,#73575),
(#73576,#73577,#73578,#73579,#73580,#73581,#73582,#73583,#73584,#73585,
#73586,#73587,#73588,#73589,#73590),(#73591,#73592,#73593,#73594,#73595,
#73596,#73597,#73598,#73599,#73600,#73601,#73602,#73603,#73604,#73605)),
 .UNSPECIFIED.,.F.,.F.,.F.,(4,1,4),(4,1,1,1,1,1,1,1,1,1,1,1,4),(0.,0.571428571428571,
1.),(0.19021466798717,0.231284548522626,0.272354429058083,0.292889369325811,
0.303156839459675,0.313424309593539,0.339092984928199,0.354494190128995,
0.364761660262859,0.375029130396723,0.395564070664451,0.436633951199908,
0.477703831735364),.UNSPECIFIED.) ;
#1784 = B_SPLINE_SURFACE_WITH_KNOTS('',3,3,((#73807,#73808,#73809,#73810,
#73811,#73812,#73813,#73814,#73815,#73816,#73817,#73818,#73819,#73820,#73821),
(#73822,#73823,#73824,#73825,#73826,#73827,#73828,#73829,#73830,#73831,
#73832,#73833,#73834,#73835,#73836),(#73837,#73838,#73839,#73840,#73841,
#73842,#73843,#73844,#73845,#73846,#73847,#73848,#73849,#73850,#73851),
(#73852,#73853,#73854,#73855,#73856,#73857,#73858,#73859,#73860,#73861,
#73862,#73863,#73864,#73865,#73866),(#73867,#73868,#73869,#73870,#73871,
#73872,#73873,#73874,#73875,#73876,#73877,#73878,#73879,#73880,#73881)),
 .UNSPECIFIED.,.F.,.F.,.F.,(4,1,4),(4,1,1,1,1,1,1,1,1,1,1,1,4),(0.,0.571428571428571,
1.),(0.599057470748756,0.640127549392637,0.670930108375547,0.676063868206032,
0.681197628036518,0.722267706680398,0.737668986171854,0.763337785324279,
0.77360530498525,0.78387282464622,0.80440786396816,0.845477942612041,0.886548021255922),
 .UNSPECIFIED.) ;
#1785 = B_SPLINE_SURFACE_WITH_KNOTS('',3,3,((#74098,#74099,#74100,#74101,
#74102,#74103,#74104,#74105,#74106,#74107,#74108,#74109,#74110,#74111),
(#74112,#74113,#74114,#74115,#74116,#74117,#74118,#74119,#74120,#74121,
#74122,#74123,#74124,#74125),(#74126,#74127,#74128,#74129,#74130,#74131,
#74132,#74133,#74134,#74135,#74136,#74137,#74138,#74139),(#74140,#74141,
#74142,#74143,#74144,#74145,#74146,#74147,#74148,#74149,#74150,#74151,#74152,
#74153),(#74154,#74155,#74156,#74157,#74158,#74159,#74160,#74161,#74162,
#74163,#74164,#74165,#74166,#74167)),.UNSPECIFIED.,.F.,.F.,.F.,(4,1,4),
(4,1,1,1,1,1,1,1,1,1,1,4),(0.,0.571428571428571,1.),(0.59905747074872,0.660662588714547,
0.681197628036489,0.701732667358431,0.712000187019402,0.722267706680373,
0.732535226341344,0.763337785324257,0.783872824646199,0.804407863968141,
0.845477942612025,0.886548021255909),.UNSPECIFIED.) ;
#1786 = B_SPLINE_SURFACE_WITH_KNOTS('',3,3,((#74392,#74393,#74394,#74395,
#74396,#74397,#74398,#74399,#74400,#74401,#74402,#74403,#74404,#74405,#74406),
(#74407,#74408,#74409,#74410,#74411,#74412,#74413,#74414,#74415,#74416,
#74417,#74418,#74419,#74420,#74421),(#74422,#74423,#74424,#74425,#74426,
#74427,#74428,#74429,#74430,#74431,#74432,#74433,#74434,#74435,#74436),
(#74437,#74438,#74439,#74440,#74441,#74442,#74443,#74444,#74445,#74446,
#74447,#74448,#74449,#74450,#74451),(#74452,#74453,#74454,#74455,#74456,
#74457,#74458,#74459,#74460,#74461,#74462,#74463,#74464,#74465,#74466)),
 .UNSPECIFIED.,.F.,.F.,.F.,(4,1,4),(4,1,1,1,1,1,1,1,1,1,1,1,4),(0.,0.571428571428571,
1.),(0.867143070761104,0.908212951290456,0.949282831819809,0.969817772084486,
0.980085242216824,0.990352712349162,1.01602138768001,1.03142259287851,1.04169006301085,
1.05195753314319,1.07249247340787,1.11356235393722,1.15463223446657),
 .UNSPECIFIED.) ;
#1787 = B_SPLINE_SURFACE_WITH_KNOTS('',3,3,((#74668,#74669,#74670,#74671,
#74672,#74673,#74674,#74675,#74676,#74677,#74678,#74679,#74680,#74681,#74682),
(#74683,#74684,#74685,#74686,#74687,#74688,#74689,#74690,#74691,#74692,
#74693,#74694,#74695,#74696,#74697),(#74698,#74699,#74700,#74701,#74702,
#74703,#74704,#74705,#74706,#74707,#74708,#74709,#74710,#74711,#74712),
(#74713,#74714,#74715,#74716,#74717,#74718,#74719,#74720,#74721,#74722,
#74723,#74724,#74725,#74726,#74727),(#74728,#74729,#74730,#74731,#74732,
#74733,#74734,#74735,#74736,#74737,#74738,#74739,#74740,#74741,#74742)),
 .UNSPECIFIED.,.F.,.F.,.F.,(4,1,4),(4,1,1,1,1,1,1,1,1,1,1,1,4),(0.,0.571428571428571,
1.),(0.1243430385224,0.165413023799369,0.206483009076339,0.227018001714824,
0.237285498034067,0.247552994353309,0.273221735151415,0.288622979630279,
0.298890475949521,0.309157972268764,0.329692964907249,0.370762950184219,
0.411832935461188),.UNSPECIFIED.) ;
#1788 = B_SPLINE_SURFACE_WITH_KNOTS('',3,3,((#74871,#74872,#74873,#74874,
#74875,#74876,#74877,#74878,#74879,#74880,#74881,#74882,#74883,#74884,#74885),
(#74886,#74887,#74888,#74889,#74890,#74891,#74892,#74893,#74894,#74895,
#74896,#74897,#74898,#74899,#74900),(#74901,#74902,#74903,#74904,#74905,
#74906,#74907,#74908,#74909,#74910,#74911,#74912,#74913,#74914,#74915),
(#74916,#74917,#74918,#74919,#74920,#74921,#74922,#74923,#74924,#74925,
#74926,#74927,#74928,#74929,#74930),(#74931,#74932,#74933,#74934,#74935,
#74936,#74937,#74938,#74939,#74940,#74941,#74942,#74943,#74944,#74945)),
 .UNSPECIFIED.,.F.,.F.,.F.,(4,1,4),(4,1,1,1,1,1,1,1,1,1,1,1,4),(0.,0.571428571428571,
1.),(0.190214667985433,0.23128454852112,0.272354429056807,0.29288936932465,
0.303156839458572,0.313424309592494,0.339092984927298,0.354494190128181,
0.364761660262103,0.375029130396024,0.395564070663868,0.436633951199555,
0.477703831735242),.UNSPECIFIED.) ;
#1789 = B_SPLINE_SURFACE_WITH_KNOTS('',3,3,((#75312,#75313,#75314,#75315,
#75316,#75317),(#75318,#75319,#75320,#75321,#75322,#75323),(#75324,#75325,
#75326,#75327,#75328,#75329),(#75330,#75331,#75332,#75333,#75334,#75335)),
 .UNSPECIFIED.,.F.,.F.,.F.,(4,4),(4,2,4),(0.,1.),(-0.0308468428281894,-0.0307213705840096,
0.),.UNSPECIFIED.) ;
#1790 = B_SPLINE_SURFACE_WITH_KNOTS('',3,3,((#75357,#75358,#75359,#75360),
(#75361,#75362,#75363,#75364),(#75365,#75366,#75367,#75368),(#75369,#75370,
#75371,#75372),(#75373,#75374,#75375,#75376)),.UNSPECIFIED.,.F.,.F.,.F.,
(4,1,4),(4,4),(0.,0.571428571428571,1.),(0.,0.00956620372314311),
 .UNSPECIFIED.) ;
#1791 = B_SPLINE_SURFACE_WITH_KNOTS('',3,3,((#75391,#75392,#75393,#75394,
#75395,#75396,#75397),(#75398,#75399,#75400,#75401,#75402,#75403,#75404),
(#75405,#75406,#75407,#75408,#75409,#75410,#75411),(#75412,#75413,#75414,
#75415,#75416,#75417,#75418),(#75419,#75420,#75421,#75422,#75423,#75424,
#75425)),.UNSPECIFIED.,.F.,.F.,.F.,(4,1,4),(4,1,1,1,4),(0.,0.571428571428571,
1.),(-7.39408534400354E-14,0.00962527143933775,0.0224589666918867,0.0320842381312984,
0.0449179333838473),.UNSPECIFIED.) ;
#1792 = B_SPLINE_SURFACE_WITH_KNOTS('',3,3,((#75449,#75450,#75451,#75452,
#75453),(#75454,#75455,#75456,#75457,#75458),(#75459,#75460,#75461,#75462,
#75463),(#75464,#75465,#75466,#75467,#75468),(#75469,#75470,#75471,#75472,
#75473)),.UNSPECIFIED.,.F.,.F.,.F.,(4,1,4),(4,1,4),(0.,0.571428571428571,
1.),(0.,0.0097787952834712,0.0228171889947661),.UNSPECIFIED.) ;
#1793 = B_SPLINE_SURFACE_WITH_KNOTS('',3,1,((#75504,#75505),(#75506,#75507),
(#75508,#75509),(#75510,#75511),(#75512,#75513)),.UNSPECIFIED.,.F.,.F.,
 .F.,(4,1,4),(2,2),(0.,0.571428571428571,1.),(0.,0.72),.UNSPECIFIED.) ;
#1794 = B_SPLINE_SURFACE_WITH_KNOTS('',3,3,((#75521,#75522,#75523,#75524),
(#75525,#75526,#75527,#75528),(#75529,#75530,#75531,#75532),(#75533,#75534,
#75535,#75536)),.UNSPECIFIED.,.F.,.F.,.F.,(4,4),(4,4),(0.,0.520585033056564),
(0.,0.0240718680289287),.UNSPECIFIED.) ;
#1795 = B_SPLINE_SURFACE_WITH_KNOTS('',3,3,((#75540,#75541,#75542,#75543),
(#75544,#75545,#75546,#75547),(#75548,#75549,#75550,#75551),(#75552,#75553,
#75554,#75555),(#75556,#75557,#75558,#75559)),.UNSPECIFIED.,.F.,.F.,.F.,
(4,1,4),(4,4),(0.,0.571428571428571,1.),(0.,0.276406121061607),
 .UNSPECIFIED.) ;
#1796 = B_SPLINE_SURFACE_WITH_KNOTS('',3,3,((#75565,#75566,#75567,#75568),
(#75569,#75570,#75571,#75572),(#75573,#75574,#75575,#75576),(#75577,#75578,
#75579,#75580),(#75581,#75582,#75583,#75584)),.UNSPECIFIED.,.F.,.F.,.F.,
(4,1,4),(4,4),(0.,0.571428571428571,1.),(0.,1.19261278278549),
 .UNSPECIFIED.) ;
#1797 = B_SPLINE_SURFACE_WITH_KNOTS('',3,3,((#75599,#75600,#75601,#75602,
#75603,#75604),(#75605,#75606,#75607,#75608,#75609,#75610),(#75611,#75612,
#75613,#75614,#75615,#75616),(#75617,#75618,#75619,#75620,#75621,#75622),
(#75623,#75624,#75625,#75626,#75627,#75628)),.UNSPECIFIED.,.F.,.F.,.F.,
(4,1,4),(4,1,1,4),(0.,0.571428571428571,1.),(0.,0.0418992966618987,0.0698321611031645,
0.0977650255444303),.UNSPECIFIED.) ;
#1798 = B_SPLINE_SURFACE_WITH_KNOTS('',3,3,((#75650,#75651,#75652,#75653),
(#75654,#75655,#75656,#75657),(#75658,#75659,#75660,#75661),(#75662,#75663,
#75664,#75665),(#75666,#75667,#75668,#75669)),.UNSPECIFIED.,.F.,.F.,.F.,
(4,1,4),(4,4),(0.,0.571428571428571,1.),(0.,0.0709441843098362),
 .UNSPECIFIED.) ;
#1799 = B_SPLINE_SURFACE_WITH_KNOTS('',3,3,((#75675,#75676,#75677,#75678),
(#75679,#75680,#75681,#75682),(#75683,#75684,#75685,#75686),(#75687,#75688,
#75689,#75690),(#75691,#75692,#75693,#75694)),.UNSPECIFIED.,.F.,.F.,.F.,
(4,1,4),(4,4),(0.,0.571428571428571,1.),(5.11404103536248E-14,1.35181237759077),
 .UNSPECIFIED.) ;
#1800 = B_SPLINE_SURFACE_WITH_KNOTS('',3,3,((#75706,#75707,#75708,#75709,
#75710,#75711),(#75712,#75713,#75714,#75715,#75716,#75717),(#75718,#75719,
#75720,#75721,#75722,#75723),(#75724,#75725,#75726,#75727,#75728,#75729),
(#75730,#75731,#75732,#75733,#75734,#75735)),.UNSPECIFIED.,.F.,.F.,.F.,
(4,1,4),(4,1,1,4),(0.,0.571428571428571,1.),(0.,0.0394783438823839,0.0657972398039731,
0.0921161357255624),.UNSPECIFIED.) ;
#1801 = B_SPLINE_SURFACE_WITH_KNOTS('',3,3,((#75757,#75758,#75759,#75760),
(#75761,#75762,#75763,#75764),(#75765,#75766,#75767,#75768),(#75769,#75770,
#75771,#75772),(#75773,#75774,#75775,#75776)),.UNSPECIFIED.,.F.,.F.,.F.,
(4,1,4),(4,4),(-8.29172718649439E-5,0.571428571428571,1.),(-8.29172718649439E-5,
0.0433131895212127),.UNSPECIFIED.) ;
#1802 = B_SPLINE_SURFACE_WITH_KNOTS('',3,1,((#75779,#75780),(#75781,#75782),
(#75783,#75784),(#75785,#75786)),.UNSPECIFIED.,.F.,.F.,.F.,(4,4),(2,2),
(0.,1.),(0.,0.8112),.UNSPECIFIED.) ;
#1803 = B_SPLINE_SURFACE_WITH_KNOTS('',3,1,((#75796,#75797),(#75798,#75799),
(#75800,#75801),(#75802,#75803),(#75804,#75805),(#75806,#75807),(#75808,
#75809)),.UNSPECIFIED.,.F.,.F.,.F.,(4,1,1,1,4),(2,2),(0.,0.285714285714286,
0.571428571428571,0.857142857142857,1.),(0.,0.8112),.UNSPECIFIED.) ;
#1804 = B_SPLINE_SURFACE_WITH_KNOTS('',3,1,((#75819,#75820),(#75821,#75822),
(#75823,#75824),(#75825,#75826)),.UNSPECIFIED.,.F.,.F.,.F.,(4,4),(2,2),
(0.597473964327042,0.930240743465184),(0.,1.50203770750399),
 .UNSPECIFIED.) ;
#1805 = B_SPLINE_SURFACE_WITH_KNOTS('',3,3,((#75967,#75968,#75969,#75970),
(#75971,#75972,#75973,#75974),(#75975,#75976,#75977,#75978),(#75979,#75980,
#75981,#75982),(#75983,#75984,#75985,#75986)),.UNSPECIFIED.,.F.,.F.,.F.,
(4,1,4),(4,4),(-8.18731696806902E-5,0.571428571428571,1.),(-8.18731696802306E-5,
0.0432139508227142),.UNSPECIFIED.) ;
#1806 = B_SPLINE_SURFACE_WITH_KNOTS('',3,3,((#75990,#75991,#75992,#75993),
(#75994,#75995,#75996,#75997),(#75998,#75999,#76000,#76001),(#76002,#76003,
#76004,#76005),(#76006,#76007,#76008,#76009)),.UNSPECIFIED.,.F.,.F.,.F.,
(4,1,4),(4,4),(0.,0.571428571428571,1.),(2.25690506700109E-10,1.07931701789601),
 .UNSPECIFIED.) ;
#1807 = B_SPLINE_SURFACE_WITH_KNOTS('',3,3,((#76016,#76017,#76018,#76019,
#76020,#76021),(#76022,#76023,#76024,#76025,#76026,#76027),(#76028,#76029,
#76030,#76031,#76032,#76033),(#76034,#76035,#76036,#76037,#76038,#76039),
(#76040,#76041,#76042,#76043,#76044,#76045)),.UNSPECIFIED.,.F.,.F.,.F.,
(4,1,4),(4,1,1,4),(0.,0.571428571428571,1.),(0.,0.0345437068826219,0.0575728448043699,
0.0806019827261179),.UNSPECIFIED.) ;
#1808 = B_SPLINE_SURFACE_WITH_KNOTS('',3,3,((#76058,#76059,#76060,#76061,
#76062),(#76063,#76064,#76065,#76066,#76067),(#76068,#76069,#76070,#76071,
#76072),(#76073,#76074,#76075,#76076,#76077),(#76078,#76079,#76080,#76081,
#76082)),.UNSPECIFIED.,.F.,.F.,.F.,(4,1,4),(4,1,4),(0.,0.571428571428571,
1.),(0.,0.0235485345716834,0.0549465806672613),.UNSPECIFIED.) ;
#1809 = B_SPLINE_SURFACE_WITH_KNOTS('',3,3,((#76090,#76091,#76092,#76093),
(#76094,#76095,#76096,#76097),(#76098,#76099,#76100,#76101),(#76102,#76103,
#76104,#76105),(#76106,#76107,#76108,#76109)),.UNSPECIFIED.,.F.,.F.,.F.,
(4,1,4),(4,4),(0.,0.571428571428571,1.),(0.,0.963640330286854),
 .UNSPECIFIED.) ;
#1810 = B_SPLINE_SURFACE_WITH_KNOTS('',3,3,((#76116,#76117,#76118,#76119,
#76120,#76121),(#76122,#76123,#76124,#76125,#76126,#76127),(#76128,#76129,
#76130,#76131,#76132,#76133),(#76134,#76135,#76136,#76137,#76138,#76139),
(#76140,#76141,#76142,#76143,#76144,#76145)),.UNSPECIFIED.,.F.,.F.,.F.,
(4,1,4),(4,1,1,4),(0.,0.571428571428571,1.),(4.3103929042364E-51,0.0368724376954248,
0.061454062825708,0.0860356879559912),.UNSPECIFIED.) ;
#1811 = B_SPLINE_SURFACE_WITH_KNOTS('',3,1,((#76152,#76153),(#76154,#76155),
(#76156,#76157),(#76158,#76159),(#76160,#76161),(#76162,#76163)),
 .UNSPECIFIED.,.F.,.F.,.F.,(4,1,1,4),(2,2),(0.,0.285714285714286,0.571428571428571,
1.),(0.,0.8112),.UNSPECIFIED.) ;
#1812 = B_SPLINE_SURFACE_WITH_KNOTS('',3,1,((#76174,#76175),(#76176,#76177),
(#76178,#76179),(#76180,#76181)),.UNSPECIFIED.,.F.,.F.,.F.,(4,4),(2,2),
(-0.471465822587465,-0.0968327577708928),(0.,1.50198816647678),
 .UNSPECIFIED.) ;
#1813 = B_SPLINE_SURFACE_WITH_KNOTS('',3,1,((#76188,#76189),(#76190,#76191),
(#76192,#76193),(#76194,#76195)),.UNSPECIFIED.,.F.,.F.,.F.,(4,4),(2,2),
(0.,1.),(0.,0.8112),.UNSPECIFIED.) ;
#1814 = B_SPLINE_SURFACE_WITH_KNOTS('',3,3,((#76253,#76254,#76255,#76256),
(#76257,#76258,#76259,#76260),(#76261,#76262,#76263,#76264),(#76265,#76266,
#76267,#76268),(#76269,#76270,#76271,#76272)),.UNSPECIFIED.,.F.,.F.,.F.,
(4,1,4),(4,4),(0.,0.571428571428571,1.),(0.,0.12989230765349),
 .UNSPECIFIED.) ;
#1815 = B_SPLINE_SURFACE_WITH_KNOTS('',3,3,((#76276,#76277,#76278,#76279),
(#76280,#76281,#76282,#76283),(#76284,#76285,#76286,#76287),(#76288,#76289,
#76290,#76291),(#76292,#76293,#76294,#76295)),.UNSPECIFIED.,.F.,.F.,.F.,
(4,1,4),(4,4),(0.,0.571428571428571,1.),(0.,0.233629810933348),
 .UNSPECIFIED.) ;
#1816 = B_SPLINE_SURFACE_WITH_KNOTS('',3,3,((#76299,#76300,#76301,#76302),
(#76303,#76304,#76305,#76306),(#76307,#76308,#76309,#76310),(#76311,#76312,
#76313,#76314),(#76315,#76316,#76317,#76318)),.UNSPECIFIED.,.F.,.F.,.F.,
(4,1,4),(4,4),(0.,0.571428571428571,1.),(0.,0.27640612106161),
 .UNSPECIFIED.) ;
#1817 = B_SPLINE_SURFACE_WITH_KNOTS('',3,3,((#76322,#76323,#76324,#76325,
#76326),(#76327,#76328,#76329,#76330,#76331),(#76332,#76333,#76334,#76335,
#76336),(#76337,#76338,#76339,#76340,#76341),(#76342,#76343,#76344,#76345,
#76346)),.UNSPECIFIED.,.F.,.F.,.F.,(4,1,4),(4,1,4),(0.,0.571428571428571,
1.),(0.,0.510997712795854,1.19232799652366),.UNSPECIFIED.) ;
#1818 = B_SPLINE_SURFACE_WITH_KNOTS('',3,3,((#76358,#76359,#76360,#76361,
#76362),(#76363,#76364,#76365,#76366,#76367),(#76368,#76369,#76370,#76371,
#76372),(#76373,#76374,#76375,#76376,#76377),(#76378,#76379,#76380,#76381,
#76382)),.UNSPECIFIED.,.F.,.F.,.F.,(4,1,4),(4,1,4),(0.,0.571428571428571,
1.),(0.,0.653796509940758,1.52552518986177),.UNSPECIFIED.) ;
#1819 = B_SPLINE_SURFACE_WITH_KNOTS('',3,3,((#76395,#76396,#76397,#76398,
#76399,#76400,#76401),(#76402,#76403,#76404,#76405,#76406,#76407,#76408),
(#76409,#76410,#76411,#76412,#76413,#76414,#76415),(#76416,#76417,#76418,
#76419,#76420,#76421,#76422),(#76423,#76424,#76425,#76426,#76427,#76428,
#76429)),.UNSPECIFIED.,.F.,.F.,.F.,(4,1,4),(4,1,1,1,4),(0.,0.571428571428571,
1.),(3.75975382637766E-15,0.0255939875922149,0.051187975184426,0.0639849689805315,
0.0895789565727426),.UNSPECIFIED.) ;
#1820 = B_SPLINE_SURFACE_WITH_KNOTS('',3,3,((#76443,#76444,#76445,#76446),
(#76447,#76448,#76449,#76450),(#76451,#76452,#76453,#76454),(#76455,#76456,
#76457,#76458),(#76459,#76460,#76461,#76462)),.UNSPECIFIED.,.F.,.F.,.F.,
(4,1,4),(4,4),(0.,0.571428571428571,1.),(0.,0.0677899888308747),
 .UNSPECIFIED.) ;
#1821 = B_SPLINE_SURFACE_WITH_KNOTS('',3,3,((#76466,#76467,#76468,#76469,
#76470),(#76471,#76472,#76473,#76474,#76475),(#76476,#76477,#76478,#76479,
#76480),(#76481,#76482,#76483,#76484,#76485),(#76486,#76487,#76488,#76489,
#76490)),.UNSPECIFIED.,.F.,.F.,.F.,(4,1,4),(4,1,4),(0.,0.571428571428571,
1.),(0.,0.667475134411416,1.5574419802933),.UNSPECIFIED.) ;
#1822 = B_SPLINE_SURFACE_WITH_KNOTS('',3,3,((#76503,#76504,#76505,#76506),
(#76507,#76508,#76509,#76510),(#76511,#76512,#76513,#76514),(#76515,#76516,
#76517,#76518),(#76519,#76520,#76521,#76522)),.UNSPECIFIED.,.F.,.F.,.F.,
(4,1,4),(4,4),(0.,0.571428571428571,1.),(0.,0.175732724220852),
 .UNSPECIFIED.) ;
#1823 = B_SPLINE_SURFACE_WITH_KNOTS('',3,3,((#76526,#76527,#76528,#76529),
(#76530,#76531,#76532,#76533),(#76534,#76535,#76536,#76537),(#76538,#76539,
#76540,#76541),(#76542,#76543,#76544,#76545)),.UNSPECIFIED.,.F.,.F.,.F.,
(4,1,4),(4,4),(0.,0.571428571428571,1.),(0.,1.13812857775824),
 .UNSPECIFIED.) ;
#1824 = B_SPLINE_SURFACE_WITH_KNOTS('',3,3,((#76549,#76550,#76551,#76552),
(#76553,#76554,#76555,#76556),(#76557,#76558,#76559,#76560),(#76561,#76562,
#76563,#76564),(#76565,#76566,#76567,#76568)),.UNSPECIFIED.,.F.,.F.,.F.,
(4,1,4),(4,4),(0.,0.571428571428571,1.),(0.,0.157312634644266),
 .UNSPECIFIED.) ;
#1825 = B_SPLINE_SURFACE_WITH_KNOTS('',3,3,((#76572,#76573,#76574,#76575),
(#76576,#76577,#76578,#76579),(#76580,#76581,#76582,#76583),(#76584,#76585,
#76586,#76587),(#76588,#76589,#76590,#76591)),.UNSPECIFIED.,.F.,.F.,.F.,
(4,1,4),(4,4),(0.,0.571428571428571,1.),(0.,0.0204003555763695),
 .UNSPECIFIED.) ;
#1826 = B_SPLINE_SURFACE_WITH_KNOTS('',3,3,((#76595,#76596,#76597,#76598),
(#76599,#76600,#76601,#76602),(#76603,#76604,#76605,#76606),(#76607,#76608,
#76609,#76610),(#76611,#76612,#76613,#76614)),.UNSPECIFIED.,.F.,.F.,.F.,
(4,1,4),(4,4),(0.,0.571428571428571,1.),(1.90971081540989E-15,0.17464806736394),
 .UNSPECIFIED.) ;
#1827 = B_SPLINE_SURFACE_WITH_KNOTS('',5,1,((#76652,#76653),(#76654,#76655),
(#76656,#76657),(#76658,#76659),(#76660,#76661),(#76662,#76663),(#76664,
#76665),(#76666,#76667),(#76668,#76669),(#76670,#76671)),.UNSPECIFIED.,
 .F.,.F.,.F.,(6,1,1,1,1,6),(2,2),(0.504846387196225,0.6,0.7,0.8,0.9,1.),
(0.,1.5),.UNSPECIFIED.) ;
#1828 = B_SPLINE_SURFACE_WITH_KNOTS('',5,1,((#76685,#76686),(#76687,#76688),
(#76689,#76690),(#76691,#76692),(#76693,#76694),(#76695,#76696),(#76697,
#76698),(#76699,#76700),(#76701,#76702),(#76703,#76704)),.UNSPECIFIED.,
 .F.,.F.,.F.,(6,1,1,1,1,6),(2,2),(0.0836762789821565,0.1,0.2,0.3,0.4,0.447897819536537),
(0.,1.5),.UNSPECIFIED.) ;
#1829 = B_SPLINE_SURFACE_WITH_KNOTS('',5,1,((#76708,#76709),(#76710,#76711),
(#76712,#76713),(#76714,#76715),(#76716,#76717),(#76718,#76719)),
 .UNSPECIFIED.,.F.,.F.,.F.,(6,6),(2,2),(0.0348574618790549,0.0836762789809161),
(0.,1.5),.UNSPECIFIED.) ;
#1830 = B_SPLINE_SURFACE_WITH_KNOTS('',5,1,((#76728,#76729),(#76730,#76731),
(#76732,#76733),(#76734,#76735),(#76736,#76737),(#76738,#76739),(#76740,
#76741),(#76742,#76743),(#76744,#76745),(#76746,#76747),(#76748,#76749),
(#76750,#76751),(#76752,#76753),(#76754,#76755),(#76756,#76757)),
 .UNSPECIFIED.,.F.,.F.,.F.,(6,1,1,1,1,1,1,1,1,1,6),(2,2),(0.,0.1,0.2,0.3,
0.4,0.5,0.6,0.7,0.8,0.9,1.),(0.,0.83184),.UNSPECIFIED.) ;
#1831 = B_SPLINE_SURFACE_WITH_KNOTS('',3,1,((#76761,#76762),(#76763,#76764),
(#76765,#76766),(#76767,#76768)),.UNSPECIFIED.,.F.,.F.,.F.,(4,4),(2,2),
(0.,1.),(0.,0.7656),.UNSPECIFIED.) ;
#1832 = B_SPLINE_SURFACE_WITH_KNOTS('',3,3,((#76825,#76826,#76827,#76828,
#76829),(#76830,#76831,#76832,#76833,#76834),(#76835,#76836,#76837,#76838,
#76839),(#76840,#76841,#76842,#76843,#76844),(#76845,#76846,#76847,#76848,
#76849)),.UNSPECIFIED.,.F.,.F.,.F.,(4,1,4),(4,1,4),(0.,0.571428571428571,
1.),(0.,0.0130357960000373,0.0304168573334205),.UNSPECIFIED.) ;
#1833 = B_SPLINE_SURFACE_WITH_KNOTS('',3,1,((#76866,#76867),(#76868,#76869),
(#76870,#76871),(#76872,#76873),(#76874,#76875)),.UNSPECIFIED.,.F.,.F.,
 .F.,(4,1,4),(2,2),(0.,0.571428571428571,1.),(0.,0.451200000000012),
 .UNSPECIFIED.) ;
#1834 = B_SPLINE_SURFACE_WITH_KNOTS('',3,3,((#76878,#76879,#76880,#76881,
#76882,#76883,#76884),(#76885,#76886,#76887,#76888,#76889,#76890,#76891),
(#76892,#76893,#76894,#76895,#76896,#76897,#76898),(#76899,#76900,#76901,
#76902,#76903,#76904,#76905),(#76906,#76907,#76908,#76909,#76910,#76911,
#76912)),.UNSPECIFIED.,.F.,.F.,.F.,(4,1,4),(4,1,1,1,4),(0.,0.571428571428571,
1.),(1.83791533766654E-16,0.00910869280420873,0.0212536165431535,0.030362309347362,
0.0425072330863067),.UNSPECIFIED.) ;
#1835 = B_SPLINE_SURFACE_WITH_KNOTS('',3,1,((#76932,#76933),(#76934,#76935),
(#76936,#76937),(#76938,#76939),(#76940,#76941),(#76942,#76943)),
 .UNSPECIFIED.,.F.,.F.,.F.,(4,1,1,4),(2,2),(0.,0.285714285714286,0.571428571428571,
1.),(0.,0.4512),.UNSPECIFIED.) ;
#1836 = B_SPLINE_SURFACE_WITH_KNOTS('',3,3,((#76946,#76947,#76948,#76949),
(#76950,#76951,#76952,#76953),(#76954,#76955,#76956,#76957),(#76958,#76959,
#76960,#76961),(#76962,#76963,#76964,#76965)),.UNSPECIFIED.,.F.,.F.,.F.,
(4,1,4),(4,4),(0.,0.571428571428571,1.),(-6.93889390390723E-18,0.369059935722116),
 .UNSPECIFIED.) ;
#1837 = B_SPLINE_SURFACE_WITH_KNOTS('',3,3,((#76974,#76975,#76976,#76977),
(#76978,#76979,#76980,#76981),(#76982,#76983,#76984,#76985),(#76986,#76987,
#76988,#76989),(#76990,#76991,#76992,#76993)),.UNSPECIFIED.,.F.,.F.,.F.,
(4,1,4),(4,4),(0.,0.571428571428571,1.),(0.,0.228081359096226),
 .UNSPECIFIED.) ;
#1838 = B_SPLINE_SURFACE_WITH_KNOTS('',3,3,((#77001,#77002,#77003,#77004,
#77005,#77006,#77007),(#77008,#77009,#77010,#77011,#77012,#77013,#77014),
(#77015,#77016,#77017,#77018,#77019,#77020,#77021),(#77022,#77023,#77024,
#77025,#77026,#77027,#77028),(#77029,#77030,#77031,#77032,#77033,#77034,
#77035)),.UNSPECIFIED.,.F.,.F.,.F.,(4,1,4),(4,3,4),(0.,0.571428571428571,
1.),(-0.011519137396051,0.,0.0257669909600073),.UNSPECIFIED.) ;
#1839 = B_SPLINE_SURFACE_WITH_KNOTS('',3,3,((#77054,#77055,#77056,#77057),
(#77058,#77059,#77060,#77061),(#77062,#77063,#77064,#77065),(#77066,#77067,
#77068,#77069),(#77070,#77071,#77072,#77073)),.UNSPECIFIED.,.F.,.F.,.F.,
(4,1,4),(4,4),(0.,0.571428571428571,1.),(0.,0.366454031313985),
 .UNSPECIFIED.) ;
#1840 = B_SPLINE_SURFACE_WITH_KNOTS('',3,3,((#77077,#77078,#77079,#77080),
(#77081,#77082,#77083,#77084),(#77085,#77086,#77087,#77088),(#77089,#77090,
#77091,#77092),(#77093,#77094,#77095,#77096)),.UNSPECIFIED.,.F.,.F.,.F.,
(4,1,4),(4,4),(0.,0.571428571428571,1.),(0.,0.226379744484658),
 .UNSPECIFIED.) ;
#1841 = B_SPLINE_SURFACE_WITH_KNOTS('',3,3,((#77098,#77099,#77100,#77101),
(#77102,#77103,#77104,#77105),(#77106,#77107,#77108,#77109),(#77110,#77111,
#77112,#77113),(#77114,#77115,#77116,#77117)),.UNSPECIFIED.,.F.,.F.,.F.,
(4,1,4),(4,4),(0.,0.571428571428571,1.),(0.00879814959602052,0.042272992561856),
 .UNSPECIFIED.) ;
#1842 = B_SPLINE_SURFACE_WITH_KNOTS('',3,3,((#77123,#77124,#77125,#77126),
(#77127,#77128,#77129,#77130),(#77131,#77132,#77133,#77134),(#77135,#77136,
#77137,#77138),(#77139,#77140,#77141,#77142)),.UNSPECIFIED.,.F.,.F.,.F.,
(4,1,4),(4,4),(0.,0.571428571428571,1.),(2.80806131699996E-14,0.177284657271612),
 .UNSPECIFIED.) ;
#1843 = B_SPLINE_SURFACE_WITH_KNOTS('',3,3,((#77165,#77166,#77167,#77168),
(#77169,#77170,#77171,#77172),(#77173,#77174,#77175,#77176),(#77177,#77178,
#77179,#77180),(#77181,#77182,#77183,#77184)),.UNSPECIFIED.,.F.,.F.,.F.,
(4,1,4),(4,4),(0.,0.571428571428571,1.),(0.0088422414876098,0.0424839045660454),
 .UNSPECIFIED.) ;
#1844 = B_SPLINE_SURFACE_WITH_KNOTS('',3,3,((#77188,#77189,#77190,#77191),
(#77192,#77193,#77194,#77195),(#77196,#77197,#77198,#77199),(#77200,#77201,
#77202,#77203),(#77204,#77205,#77206,#77207)),.UNSPECIFIED.,.F.,.F.,.F.,
(4,1,4),(4,4),(0.,0.571428571428571,1.),(0.,0.182076134495141),
 .UNSPECIFIED.) ;
#1845 = B_SPLINE_SURFACE_WITH_KNOTS('',3,3,((#77213,#77214,#77215,#77216),
(#77217,#77218,#77219,#77220),(#77221,#77222,#77223,#77224),(#77225,#77226,
#77227,#77228),(#77229,#77230,#77231,#77232)),.UNSPECIFIED.,.F.,.F.,.F.,
(4,1,4),(4,4),(0.,0.571428571428571,1.),(0.,0.0102916147937805),
 .UNSPECIFIED.) ;
#1846 = B_SPLINE_SURFACE_WITH_KNOTS('',3,1,((#77253,#77254),(#77255,#77256),
(#77257,#77258),(#77259,#77260)),.UNSPECIFIED.,.F.,.F.,.F.,(4,4),(2,2),
(0.120318448480489,0.194542293717003),(0.,0.78),.UNSPECIFIED.) ;
#1847 = B_SPLINE_SURFACE_WITH_KNOTS('',3,1,((#77262,#77263),(#77264,#77265),
(#77266,#77267),(#77268,#77269)),.UNSPECIFIED.,.F.,.F.,.F.,(4,4),(2,2),
(0.00785988716405027,0.120318448346505),(0.,0.78),.UNSPECIFIED.) ;
#1848 = B_SPLINE_SURFACE_WITH_KNOTS('',3,3,((#77278,#77279,#77280,#77281,
#77282),(#77283,#77284,#77285,#77286,#77287),(#77288,#77289,#77290,#77291,
#77292),(#77293,#77294,#77295,#77296,#77297),(#77298,#77299,#77300,#77301,
#77302)),.UNSPECIFIED.,.F.,.F.,.F.,(4,1,4),(4,1,4),(0.,0.571428571428571,
1.),(0.,0.017271853441312,0.0345437068826239),.UNSPECIFIED.) ;
#1849 = B_SPLINE_SURFACE_WITH_KNOTS('',3,3,((#77312,#77313,#77314,#77315),
(#77316,#77317,#77318,#77319),(#77320,#77321,#77322,#77323),(#77324,#77325,
#77326,#77327),(#77328,#77329,#77330,#77331)),.UNSPECIFIED.,.F.,.F.,.F.,
(4,1,4),(4,4),(0.,0.571428571428571,1.),(0.,1.07230437897721),
 .UNSPECIFIED.) ;
#1850 = B_SPLINE_SURFACE_WITH_KNOTS('',3,3,((#77335,#77336,#77337,#77338),
(#77339,#77340,#77341,#77342),(#77343,#77344,#77345,#77346),(#77347,#77348,
#77349,#77350),(#77351,#77352,#77353,#77354)),.UNSPECIFIED.,.F.,.F.,.F.,
(4,1,4),(4,4),(0.,0.571428571428571,1.),(0.,0.0184851761370125),
 .UNSPECIFIED.) ;
#1851 = B_SPLINE_SURFACE_WITH_KNOTS('',3,3,((#77362,#77363,#77364,#77365,
#77366,#77367),(#77368,#77369,#77370,#77371,#77372,#77373),(#77374,#77375,
#77376,#77377,#77378,#77379),(#77380,#77381,#77382,#77383,#77384,#77385),
(#77386,#77387,#77388,#77389,#77390,#77391)),.UNSPECIFIED.,.F.,.F.,.F.,
(4,1,4),(4,1,1,4),(0.,0.571428571428571,1.),(0.,0.0158024732980411,0.0263374554967351,
0.0368724376954292),.UNSPECIFIED.) ;
#1852 = B_SPLINE_SURFACE_WITH_KNOTS('',3,3,((#77407,#77408,#77409,#77410),
(#77411,#77412,#77413,#77414),(#77415,#77416,#77417,#77418),(#77419,#77420,
#77421,#77422),(#77423,#77424,#77425,#77426)),.UNSPECIFIED.,.F.,.F.,.F.,
(4,1,4),(4,4),(0.,0.571428571428571,1.),(0.,0.971129055990219),
 .UNSPECIFIED.) ;
#1853 = B_SPLINE_SURFACE_WITH_KNOTS('',3,3,((#77435,#77436,#77437,#77438,
#77439),(#77440,#77441,#77442,#77443,#77444),(#77445,#77446,#77447,#77448,
#77449),(#77450,#77451,#77452,#77453,#77454),(#77455,#77456,#77457,#77458,
#77459)),.UNSPECIFIED.,.F.,.F.,.F.,(4,1,4),(4,1,4),(0.,0.571428571428571,
1.),(0.,0.0100922291021495,0.0235485345716821),.UNSPECIFIED.) ;
#1854 = B_SPLINE_SURFACE_WITH_KNOTS('',3,3,((#77477,#77478,#77479,#77480,
#77481,#77482),(#77483,#77484,#77485,#77486,#77487,#77488),(#77489,#77490,
#77491,#77492,#77493,#77494),(#77495,#77496,#77497,#77498,#77499,#77500),
(#77501,#77502,#77503,#77504,#77505,#77506)),.UNSPECIFIED.,.F.,.F.,.F.,
(4,1,4),(4,1,1,4),(0.,0.571428571428571,1.),(0.,0.0112795268235383,0.0225590536470765,
0.0394783438823839),.UNSPECIFIED.) ;
#1855 = B_SPLINE_SURFACE_WITH_KNOTS('',3,3,((#77525,#77526,#77527,#77528),
(#77529,#77530,#77531,#77532),(#77533,#77534,#77535,#77536),(#77537,#77538,
#77539,#77540),(#77541,#77542,#77543,#77544)),.UNSPECIFIED.,.F.,.F.,.F.,
(4,1,4),(4,4),(0.,0.571428571428571,1.),(0.,1.34425818567182),
 .UNSPECIFIED.) ;
#1856 = B_SPLINE_SURFACE_WITH_KNOTS('',3,3,((#77555,#77556,#77557,#77558),
(#77559,#77560,#77561,#77562),(#77563,#77564,#77565,#77566),(#77567,#77568,
#77569,#77570),(#77571,#77572,#77573,#77574)),.UNSPECIFIED.,.F.,.F.,.F.,
(4,1,4),(4,4),(0.,0.571428571428571,1.),(0.,0.0557418591005873),
 .UNSPECIFIED.) ;
#1857 = B_SPLINE_SURFACE_WITH_KNOTS('',3,3,((#77582,#77583,#77584,#77585,
#77586,#77587,#77588),(#77589,#77590,#77591,#77592,#77593,#77594,#77595),
(#77596,#77597,#77598,#77599,#77600,#77601,#77602),(#77603,#77604,#77605,
#77606,#77607,#77608,#77609),(#77610,#77611,#77612,#77613,#77614,#77615,
#77616)),.UNSPECIFIED.,.F.,.F.,.F.,(4,1,4),(4,1,1,1,4),(0.,0.571428571428571,
1.),(0.,0.0119712276176857,0.0239424552353715,0.0359136828530572,0.0418992966619001),
 .UNSPECIFIED.) ;
#1858 = B_SPLINE_SURFACE_WITH_KNOTS('',3,3,((#77626,#77627,#77628,#77629),
(#77630,#77631,#77632,#77633),(#77634,#77635,#77636,#77637),(#77638,#77639,
#77640,#77641),(#77642,#77643,#77644,#77645)),.UNSPECIFIED.,.F.,.F.,.F.,
(4,1,4),(4,4),(0.,0.571428571428571,1.),(0.,1.19778613661182),
 .UNSPECIFIED.) ;
#1859 = B_SPLINE_SURFACE_WITH_KNOTS('',3,3,((#77652,#77653,#77654,#77655),
(#77656,#77657,#77658,#77659),(#77660,#77661,#77662,#77663),(#77664,#77665,
#77666,#77667),(#77668,#77669,#77670,#77671)),.UNSPECIFIED.,.F.,.F.,.F.,
(4,1,4),(4,4),(0.,0.571428571428571,1.),(0.,0.0185272595354357),
 .UNSPECIFIED.) ;
#1860 = B_SPLINE_SURFACE_WITH_KNOTS('',3,1,((#77680,#77681),(#77682,#77683),
(#77684,#77685),(#77686,#77687),(#77688,#77689),(#77690,#77691),(#77692,
#77693)),.UNSPECIFIED.,.F.,.F.,.F.,(4,3,4),(2,2),(-0.988543128598371,-0.545479769376514,
-0.531340881080732),(0.,1.50198816647678),.UNSPECIFIED.) ;
#1861 = B_SPLINE_SURFACE_WITH_KNOTS('',3,1,((#77695,#77696),(#77697,#77698),
(#77699,#77700),(#77701,#77702),(#77703,#77704),(#77705,#77706)),
 .UNSPECIFIED.,.F.,.F.,.F.,(4,1,1,4),(2,2),(0.,0.285714285714286,0.571428571428571,
1.),(0.,0.8112),.UNSPECIFIED.) ;
#1862 = B_SPLINE_SURFACE_WITH_KNOTS('',3,3,((#77716,#77717,#77718,#77719,
#77720),(#77721,#77722,#77723,#77724,#77725),(#77726,#77727,#77728,#77729,
#77730),(#77731,#77732,#77733,#77734,#77735),(#77736,#77737,#77738,#77739,
#77740)),.UNSPECIFIED.,.F.,.F.,.F.,(4,1,4),(4,1,4),(0.,0.571428571428571,
1.),(0.,0.0106131136334063,0.0247639318112814),.UNSPECIFIED.) ;
#1863 = B_SPLINE_SURFACE_WITH_KNOTS('',3,1,((#77753,#77754),(#77755,#77756),
(#77757,#77758),(#77759,#77760)),.UNSPECIFIED.,.F.,.F.,.F.,(4,4),(2,2),
(0.,1.),(0.,0.1512),.UNSPECIFIED.) ;
#1864 = B_SPLINE_SURFACE_WITH_KNOTS('',3,3,((#77777,#77778,#77779,#77780),
(#77781,#77782,#77783,#77784),(#77785,#77786,#77787,#77788),(#77789,#77790,
#77791,#77792),(#77793,#77794,#77795,#77796)),.UNSPECIFIED.,.F.,.F.,.F.,
(4,1,4),(4,4),(0.,0.571428571428571,1.),(0.0229372865431325,1.40205259514116),
 .UNSPECIFIED.) ;
#1865 = B_SPLINE_SURFACE_WITH_KNOTS('',3,3,((#77811,#77812,#77813,#77814),
(#77815,#77816,#77817,#77818),(#77819,#77820,#77821,#77822),(#77823,#77824,
#77825,#77826),(#77827,#77828,#77829,#77830)),.UNSPECIFIED.,.F.,.F.,.F.,
(4,1,4),(4,4),(0.,0.571428571428571,1.),(0.,0.0557418591005868),
 .UNSPECIFIED.) ;
#1866 = B_SPLINE_SURFACE_WITH_KNOTS('',3,3,((#77842,#77843,#77844,#77845,
#77846,#77847,#77848),(#77849,#77850,#77851,#77852,#77853,#77854,#77855),
(#77856,#77857,#77858,#77859,#77860,#77861,#77862),(#77863,#77864,#77865,
#77866,#77867,#77868,#77869),(#77870,#77871,#77872,#77873,#77874,#77875,
#77876)),.UNSPECIFIED.,.F.,.F.,.F.,(4,1,4),(4,1,1,1,4),(0.,0.571428571428571,
1.),(0.,0.00598561380884316,0.0179568414265295,0.0299280690442158,0.0418992966619021),
 .UNSPECIFIED.) ;
#1867 = B_SPLINE_SURFACE_WITH_KNOTS('',3,3,((#77894,#77895,#77896,#77897),
(#77898,#77899,#77900,#77901),(#77902,#77903,#77904,#77905),(#77906,#77907,
#77908,#77909),(#77910,#77911,#77912,#77913)),.UNSPECIFIED.,.F.,.F.,.F.,
(4,1,4),(4,4),(0.,0.571428571428571,1.),(0.,1.20789221798527),
 .UNSPECIFIED.) ;
#1868 = B_SPLINE_SURFACE_WITH_KNOTS('',3,3,((#77922,#77923,#77924,#77925,
#77926,#77927,#77928),(#77929,#77930,#77931,#77932,#77933,#77934,#77935),
(#77936,#77937,#77938,#77939,#77940,#77941,#77942),(#77943,#77944,#77945,
#77946,#77947,#77948,#77949),(#77950,#77951,#77952,#77953,#77954,#77955,
#77956)),.UNSPECIFIED.,.F.,.F.,.F.,(4,1,4),(4,1,1,1,4),(0.,0.571428571428571,
1.),(0.,0.0149660193069295,0.0224490289603943,0.0374150482673238,0.0523810675742533),
 .UNSPECIFIED.) ;
#1869 = B_SPLINE_SURFACE_WITH_KNOTS('',3,1,((#77984,#77985),(#77986,#77987),
(#77988,#77989),(#77990,#77991),(#77992,#77993),(#77994,#77995),(#77996,
#77997)),.UNSPECIFIED.,.F.,.F.,.F.,(4,1,1,1,4),(2,2),(0.,0.285714285714286,
0.5,0.785714285714286,1.),(0.,0.1512),.UNSPECIFIED.) ;
#1870 = B_SPLINE_SURFACE_WITH_KNOTS('',3,3,((#78000,#78001,#78002,#78003),
(#78004,#78005,#78006,#78007),(#78008,#78009,#78010,#78011),(#78012,#78013,
#78014,#78015),(#78016,#78017,#78018,#78019)),.UNSPECIFIED.,.F.,.F.,.F.,
(4,1,4),(4,4),(0.,0.571428571428571,1.),(0.0231068825027873,1.41003451675495),
 .UNSPECIFIED.) ;
#1871 = B_SPLINE_SURFACE_WITH_KNOTS('',3,3,((#78031,#78032,#78033,#78034),
(#78035,#78036,#78037,#78038),(#78039,#78040,#78041,#78042),(#78043,#78044,
#78045,#78046),(#78047,#78048,#78049,#78050)),.UNSPECIFIED.,.F.,.F.,.F.,
(4,1,4),(4,4),(0.,0.571428571428571,1.),(0.,0.0709441843098284),
 .UNSPECIFIED.) ;
#1872 = B_SPLINE_SURFACE_WITH_KNOTS('',3,3,((#78062,#78063,#78064,#78065,
#78066,#78067),(#78068,#78069,#78070,#78071,#78072,#78073),(#78074,#78075,
#78076,#78077,#78078,#78079),(#78080,#78081,#78082,#78083,#78084,#78085),
(#78086,#78087,#78088,#78089,#78090,#78091)),.UNSPECIFIED.,.F.,.F.,.F.,
(4,1,4),(4,1,1,4),(0.,0.571428571428571,1.),(0.,0.0418992966619,0.0698321611031666,
0.0977650255444333),.UNSPECIFIED.) ;
#1873 = B_SPLINE_SURFACE_WITH_KNOTS('',3,3,((#78107,#78108,#78109,#78110),
(#78111,#78112,#78113,#78114),(#78115,#78116,#78117,#78118),(#78119,#78120,
#78121,#78122),(#78123,#78124,#78125,#78126)),.UNSPECIFIED.,.F.,.F.,.F.,
(4,1,4),(4,4),(0.,0.571428571428571,1.),(0.,1.20265740584169),
 .UNSPECIFIED.) ;
#1874 = B_SPLINE_SURFACE_WITH_KNOTS('',3,1,((#78138,#78139),(#78140,#78141),
(#78142,#78143),(#78144,#78145),(#78146,#78147),(#78148,#78149),(#78150,
#78151)),.UNSPECIFIED.,.F.,.F.,.F.,(4,1,1,1,4),(2,2),(0.,0.285714285714286,
0.571428571428571,0.857142857142857,1.),(0.,0.1512),.UNSPECIFIED.) ;
#1875 = B_SPLINE_SURFACE_WITH_KNOTS('',3,1,((#78154,#78155),(#78156,#78157),
(#78158,#78159),(#78160,#78161),(#78162,#78163),(#78164,#78165),(#78166,
#78167)),.UNSPECIFIED.,.F.,.F.,.F.,(4,3,4),(2,2),(-0.988543128598371,-0.545479769376514,
-0.531340881080732),(0.,1.50198816647678),.UNSPECIFIED.) ;
#1876 = B_SPLINE_SURFACE_WITH_KNOTS('',3,1,((#78171,#78172),(#78173,#78174),
(#78175,#78176),(#78177,#78178)),.UNSPECIFIED.,.F.,.F.,.F.,(4,4),(2,2),
(0.,1.),(0.,0.1512),.UNSPECIFIED.) ;
#1877 = B_SPLINE_SURFACE_WITH_KNOTS('',3,3,((#78268,#78269,#78270,#78271,
#78272,#78273,#78274),(#78275,#78276,#78277,#78278,#78279,#78280,#78281),
(#78282,#78283,#78284,#78285,#78286,#78287,#78288),(#78289,#78290,#78291,
#78292,#78293,#78294,#78295),(#78296,#78297,#78298,#78299,#78300,#78301,
#78302)),.UNSPECIFIED.,.F.,.F.,.F.,(4,1,4),(4,1,1,1,4),(0.,0.571428571428571,
1.),(0.,0.0141037612586181,0.0211556418879271,0.0352594031465452,0.0493631644051633),
 .UNSPECIFIED.) ;
#1878 = B_SPLINE_SURFACE_WITH_KNOTS('',3,1,((#78321,#78322),(#78323,#78324),
(#78325,#78326),(#78327,#78328),(#78329,#78330),(#78331,#78332),(#78333,
#78334)),.UNSPECIFIED.,.F.,.F.,.F.,(4,1,1,1,4),(2,2),(0.,0.285714285714286,
0.5,0.785714285714286,1.),(0.,0.1512),.UNSPECIFIED.) ;
#1879 = B_SPLINE_SURFACE_WITH_KNOTS('',3,3,((#78337,#78338,#78339,#78340,
#78341),(#78342,#78343,#78344,#78345,#78346),(#78347,#78348,#78349,#78350,
#78351),(#78352,#78353,#78354,#78355,#78356),(#78357,#78358,#78359,#78360,
#78361)),.UNSPECIFIED.,.F.,.F.,.F.,(4,1,4),(4,1,4),(0.,0.571428571428571,
1.),(0.,0.0105301970552765,0.0245704597956453),.UNSPECIFIED.) ;
#1880 = B_SPLINE_SURFACE_WITH_KNOTS('',3,3,((#78367,#78368,#78369,#78370,
#78371),(#78372,#78373,#78374,#78375,#78376),(#78377,#78378,#78379,#78380,
#78381),(#78382,#78383,#78384,#78385,#78386),(#78387,#78388,#78389,#78390,
#78391)),.UNSPECIFIED.,.F.,.F.,.F.,(4,1,4),(4,1,4),(0.,0.571428571428571,
1.),(0.,0.0180035869295808,0.0315062771267664),.UNSPECIFIED.) ;
#1881 = B_SPLINE_SURFACE_WITH_KNOTS('',3,1,((#78408,#78409),(#78410,#78411),
(#78412,#78413),(#78414,#78415)),.UNSPECIFIED.,.F.,.F.,.F.,(4,4),(2,2),
(0.,1.),(0.,0.1512),.UNSPECIFIED.) ;
#1882 = B_SPLINE_SURFACE_WITH_KNOTS('',3,3,((#78425,#78426,#78427,#78428),
(#78429,#78430,#78431,#78432),(#78433,#78434,#78435,#78436),(#78437,#78438,
#78439,#78440),(#78441,#78442,#78443,#78444)),.UNSPECIFIED.,.F.,.F.,.F.,
(4,1,4),(4,4),(0.,0.571428571428571,1.),(0.020008660331873,1.03467847166523),
 .UNSPECIFIED.) ;
#1883 = B_SPLINE_SURFACE_WITH_KNOTS('',3,3,((#78453,#78454,#78455,#78456,
#78457,#78458,#78459),(#78460,#78461,#78462,#78463,#78464,#78465,#78466),
(#78467,#78468,#78469,#78470,#78471,#78472,#78473),(#78474,#78475,#78476,
#78477,#78478,#78479,#78480),(#78481,#78482,#78483,#78484,#78485,#78486,
#78487)),.UNSPECIFIED.,.F.,.F.,.F.,(4,1,4),(4,1,1,1,4),(0.,0.571428571428571,
1.),(0.,0.00984040545418749,0.0229609460597708,0.0328013515139583,0.0459218921195416),
 .UNSPECIFIED.) ;
#1884 = B_SPLINE_SURFACE_WITH_KNOTS('',3,1,((#78508,#78509),(#78510,#78511),
(#78512,#78513),(#78514,#78515),(#78516,#78517),(#78518,#78519),(#78520,
#78521)),.UNSPECIFIED.,.F.,.F.,.F.,(4,1,1,1,4),(2,2),(0.,0.285714285714286,
0.5,0.714285714285714,1.),(0.,0.1512),.UNSPECIFIED.) ;
#1885 = B_SPLINE_SURFACE_WITH_KNOTS('',3,3,((#78527,#78528,#78529,#78530),
(#78531,#78532,#78533,#78534),(#78535,#78536,#78537,#78538),(#78539,#78540,
#78541,#78542),(#78543,#78544,#78545,#78546)),.UNSPECIFIED.,.F.,.F.,.F.,
(4,1,4),(4,4),(0.,0.571428571428571,1.),(0.0169663179244005,1.12511677037933),
 .UNSPECIFIED.) ;
#1886 = B_SPLINE_SURFACE_WITH_KNOTS('',3,3,((#78552,#78553,#78554,#78555),
(#78556,#78557,#78558,#78559),(#78560,#78561,#78562,#78563),(#78564,#78565,
#78566,#78567),(#78568,#78569,#78570,#78571)),.UNSPECIFIED.,.F.,.F.,.F.,
(4,1,4),(4,4),(0.,0.571428571428571,1.),(0.0170557641123888,1.13243225761785),
 .UNSPECIFIED.) ;
#1887 = B_SPLINE_SURFACE_WITH_KNOTS('',3,1,((#78575,#78576),(#78577,#78578),
(#78579,#78580),(#78581,#78582),(#78583,#78584)),.UNSPECIFIED.,.F.,.F.,
 .F.,(4,1,4),(2,2),(0.,0.571428571428571,1.),(0.,0.1512),.UNSPECIFIED.) ;
#1888 = B_SPLINE_SURFACE_WITH_KNOTS('',3,3,((#78590,#78591,#78592,#78593),
(#78594,#78595,#78596,#78597),(#78598,#78599,#78600,#78601),(#78602,#78603,
#78604,#78605),(#78606,#78607,#78608,#78609)),.UNSPECIFIED.,.F.,.F.,.F.,
(4,1,4),(4,4),(0.,0.571428571428571,1.),(0.019875255616694,1.02674783308136),
 .UNSPECIFIED.) ;
#1889 = B_SPLINE_SURFACE_WITH_KNOTS('',3,1,((#78616,#78617),(#78618,#78619),
(#78620,#78621),(#78622,#78623),(#78624,#78625),(#78626,#78627),(#78628,
#78629)),.UNSPECIFIED.,.F.,.F.,.F.,(4,3,4),(2,2),(0.241689284630679,0.500017400470172,
0.549213097360471),(0.,1.50203770750399),.UNSPECIFIED.) ;
#1890 = B_SPLINE_SURFACE_WITH_KNOTS('',3,1,((#78632,#78633),(#78634,#78635),
(#78636,#78637),(#78638,#78639)),.UNSPECIFIED.,.F.,.F.,.F.,(4,4),(2,2),
(-0.471465822587465,-0.0968327577708928),(0.,1.50198816647678),
 .UNSPECIFIED.) ;
#1891 = B_SPLINE_SURFACE_WITH_KNOTS('',3,3,((#78641,#78642,#78643,#78644,
#78645,#78646,#78647),(#78648,#78649,#78650,#78651,#78652,#78653,#78654),
(#78655,#78656,#78657,#78658,#78659,#78660,#78661),(#78662,#78663,#78664,
#78665,#78666,#78667,#78668),(#78669,#78670,#78671,#78672,#78673,#78674,
#78675)),.UNSPECIFIED.,.F.,.F.,.F.,(4,1,4),(4,3,4),(0.,0.571428571428571,
1.),(-0.00748019188171517,0.,0.129892307653464),.UNSPECIFIED.) ;
#1892 = B_SPLINE_SURFACE_WITH_KNOTS('',3,3,((#78700,#78701,#78702,#78703),
(#78704,#78705,#78706,#78707),(#78708,#78709,#78710,#78711),(#78712,#78713,
#78714,#78715),(#78716,#78717,#78718,#78719)),.UNSPECIFIED.,.F.,.F.,.F.,
(4,1,4),(4,4),(0.,0.571428571428571,1.),(0.,0.233629810933348),
 .UNSPECIFIED.) ;
#1893 = B_SPLINE_SURFACE_WITH_KNOTS('',5,1,((#78722,#78723),(#78724,#78725),
(#78726,#78727),(#78728,#78729),(#78730,#78731),(#78732,#78733),(#78734,
#78735)),.UNSPECIFIED.,.F.,.F.,.F.,(6,1,6),(2,2),(-0.202504416334417,-0.2,
-0.114745808067944),(0.,0.78),.UNSPECIFIED.) ;
#1894 = B_SPLINE_SURFACE_WITH_KNOTS('',5,1,((#78738,#78739),(#78740,#78741),
(#78742,#78743),(#78744,#78745),(#78746,#78747),(#78748,#78749),(#78750,
#78751)),.UNSPECIFIED.,.F.,.F.,.F.,(6,1,6),(2,2),(-0.114745808067916,-0.1,
-0.040837741884948),(0.,0.78),.UNSPECIFIED.) ;
#1895 = B_SPLINE_SURFACE_WITH_KNOTS('',5,1,((#78753,#78754),(#78755,#78756),
(#78757,#78758),(#78759,#78760),(#78761,#78762),(#78763,#78764)),
 .UNSPECIFIED.,.F.,.F.,.F.,(6,6),(2,2),(-0.0408377418849424,0.),(0.,0.78),
 .UNSPECIFIED.) ;
#1896 = B_SPLINE_SURFACE_WITH_KNOTS('',3,1,((#78776,#78777),(#78778,#78779),
(#78780,#78781),(#78782,#78783),(#78784,#78785),(#78786,#78787)),
 .UNSPECIFIED.,.F.,.F.,.F.,(4,1,1,4),(2,2),(0.,0.5,0.714285714285714,1.),
(0.,0.6912),.UNSPECIFIED.) ;
#1897 = B_SPLINE_SURFACE_WITH_KNOTS('',3,3,((#78788,#78789,#78790,#78791),
(#78792,#78793,#78794,#78795),(#78796,#78797,#78798,#78799),(#78800,#78801,
#78802,#78803),(#78804,#78805,#78806,#78807)),.UNSPECIFIED.,.F.,.F.,.F.,
(4,1,4),(4,4),(0.,0.571428571428571,1.),(0.,0.141072567236982),
 .UNSPECIFIED.) ;
#1898 = B_SPLINE_SURFACE_WITH_KNOTS('',3,3,((#78809,#78810,#78811,#78812),
(#78813,#78814,#78815,#78816),(#78817,#78818,#78819,#78820),(#78821,#78822,
#78823,#78824),(#78825,#78826,#78827,#78828)),.UNSPECIFIED.,.F.,.F.,.F.,
(4,1,4),(4,4),(0.,0.571428571428571,1.),(0.,1.13812857775824),
 .UNSPECIFIED.) ;
#1899 = B_SPLINE_SURFACE_WITH_KNOTS('',3,3,((#78830,#78831,#78832,#78833),
(#78834,#78835,#78836,#78837),(#78838,#78839,#78840,#78841),(#78842,#78843,
#78844,#78845),(#78846,#78847,#78848,#78849)),.UNSPECIFIED.,.F.,.F.,.F.,
(4,1,4),(4,4),(0.,0.571428571428571,1.),(0.,0.175732724220853),
 .UNSPECIFIED.) ;
#1900 = B_SPLINE_SURFACE_WITH_KNOTS('',3,3,((#78851,#78852,#78853,#78854,
#78855),(#78856,#78857,#78858,#78859,#78860),(#78861,#78862,#78863,#78864,
#78865),(#78866,#78867,#78868,#78869,#78870),(#78871,#78872,#78873,#78874,
#78875)),.UNSPECIFIED.,.F.,.F.,.F.,(4,1,4),(4,1,4),(0.,0.571428571428571,
1.),(0.,0.66747373630185,1.55743871803765),.UNSPECIFIED.) ;
#1901 = B_SPLINE_SURFACE_WITH_KNOTS('',3,3,((#78877,#78878,#78879,#78880),
(#78881,#78882,#78883,#78884),(#78885,#78886,#78887,#78888),(#78889,#78890,
#78891,#78892),(#78893,#78894,#78895,#78896)),.UNSPECIFIED.,.F.,.F.,.F.,
(4,1,4),(4,4),(0.,0.571428571428571,1.),(0.,0.0677899888308747),
 .UNSPECIFIED.) ;
#1902 = B_SPLINE_SURFACE_WITH_KNOTS('',3,3,((#78904,#78905,#78906,#78907,
#78908,#78909,#78910),(#78911,#78912,#78913,#78914,#78915,#78916,#78917),
(#78918,#78919,#78920,#78921,#78922,#78923,#78924),(#78925,#78926,#78927,
#78928,#78929,#78930,#78931),(#78932,#78933,#78934,#78935,#78936,#78937,
#78938)),.UNSPECIFIED.,.F.,.F.,.F.,(4,1,4),(4,1,1,1,4),(0.,0.571428571428571,
1.),(0.,0.0255939875922127,0.038390981388319,0.0639849689805316,0.0895789565727443),
 .UNSPECIFIED.) ;
#1903 = B_SPLINE_SURFACE_WITH_KNOTS('',3,3,((#78948,#78949,#78950,#78951,
#78952),(#78953,#78954,#78955,#78956,#78957),(#78958,#78959,#78960,#78961,
#78962),(#78963,#78964,#78965,#78966,#78967),(#78968,#78969,#78970,#78971,
#78972)),.UNSPECIFIED.,.F.,.F.,.F.,(4,1,4),(4,1,4),(0.,0.571428571428571,
1.),(0.,0.653796509940757,1.52552518986177),.UNSPECIFIED.) ;
#1904 = B_SPLINE_SURFACE_WITH_KNOTS('',3,3,((#78985,#78986,#78987,#78988,
#78989),(#78990,#78991,#78992,#78993,#78994),(#78995,#78996,#78997,#78998,
#78999),(#79000,#79001,#79002,#79003,#79004),(#79005,#79006,#79007,#79008,
#79009)),.UNSPECIFIED.,.F.,.F.,.F.,(4,1,4),(4,1,4),(0.,0.571428571428571,
1.),(0.,0.500681763148267,1.16825744734596),.UNSPECIFIED.) ;
#1905 = B_SPLINE_SURFACE_WITH_KNOTS('',3,3,((#79016,#79017,#79018,#79019,
#79020),(#79021,#79022,#79023,#79024,#79025),(#79026,#79027,#79028,#79029,
#79030),(#79031,#79032,#79033,#79034,#79035),(#79036,#79037,#79038,#79039,
#79040)),.UNSPECIFIED.,.F.,.F.,.F.,(4,1,4),(4,1,4),(0.,0.571428571428571,
1.),(0.,0.0104089910116412,0.0242876456938294),.UNSPECIFIED.) ;
#1906 = B_SPLINE_SURFACE_WITH_KNOTS('',3,1,((#79046,#79047),(#79048,#79049),
(#79050,#79051),(#79052,#79053),(#79054,#79055),(#79056,#79057),(#79058,
#79059)),.UNSPECIFIED.,.F.,.F.,.F.,(4,1,1,1,4),(2,2),(0.,0.285714285714286,
0.571428571428571,0.857142857142857,1.),(0.,1.4712),.UNSPECIFIED.) ;
#1907 = B_SPLINE_SURFACE_WITH_KNOTS('',5,1,((#79061,#79062),(#79063,#79064),
(#79065,#79066),(#79067,#79068),(#79069,#79070),(#79071,#79072),(#79073,
#79074),(#79075,#79076),(#79077,#79078),(#79079,#79080)),.UNSPECIFIED.,
 .F.,.F.,.F.,(6,1,1,1,1,6),(2,2),(-1.,-0.9,-0.8,-0.7,-0.6,-0.568009935219903),
(0.,1.5),.UNSPECIFIED.) ;
#1908 = B_SPLINE_SURFACE_WITH_KNOTS('',5,1,((#79082,#79083),(#79084,#79085),
(#79086,#79087),(#79088,#79089),(#79090,#79091),(#79092,#79093),(#79094,
#79095),(#79096,#79097),(#79098,#79099)),.UNSPECIFIED.,.F.,.F.,.F.,(6,1,
1,1,6),(2,2),(-0.568009935219888,-0.5,-0.4,-0.3,-0.202504416334422),(0.,
1.5),.UNSPECIFIED.) ;
#1909 = B_SPLINE_SURFACE_WITH_KNOTS('',3,1,((#79104,#79105),(#79106,#79107),
(#79108,#79109),(#79110,#79111)),.UNSPECIFIED.,.F.,.F.,.F.,(4,4),(2,2),
(-0.0465039596324731,-0.00333818885951975),(0.,0.78),.UNSPECIFIED.) ;
#1910 = B_SPLINE_SURFACE_WITH_KNOTS('',3,1,((#79113,#79114),(#79115,#79116),
(#79117,#79118),(#79119,#79120)),.UNSPECIFIED.,.F.,.F.,.F.,(4,4),(2,2),
(0.,1.),(0.,0.4512),.UNSPECIFIED.) ;
#1911 = B_SPLINE_SURFACE_WITH_KNOTS('',3,1,((#79122,#79123),(#79124,#79125),
(#79126,#79127),(#79128,#79129),(#79130,#79131)),.UNSPECIFIED.,.F.,.F.,
 .F.,(4,1,4),(2,2),(0.,0.571428571428571,1.),(0.,0.8112),.UNSPECIFIED.) ;
#1912 = B_SPLINE_SURFACE_WITH_KNOTS('',3,1,((#79135,#79136),(#79137,#79138),
(#79139,#79140),(#79141,#79142),(#79143,#79144),(#79145,#79146)),
 .UNSPECIFIED.,.F.,.F.,.F.,(4,1,1,4),(2,2),(0.,0.285714285714286,0.571428571428571,
1.),(0.,0.8112),.UNSPECIFIED.) ;
#1913 = B_SPLINE_SURFACE_WITH_KNOTS('',3,1,((#79148,#79149),(#79150,#79151),
(#79152,#79153),(#79154,#79155)),.UNSPECIFIED.,.F.,.F.,.F.,(4,4),(2,2),
(0.,1.),(0.,0.8112),.UNSPECIFIED.) ;
#1914 = B_SPLINE_SURFACE_WITH_KNOTS('',3,1,((#79157,#79158),(#79159,#79160),
(#79161,#79162),(#79163,#79164)),.UNSPECIFIED.,.F.,.F.,.F.,(4,4),(2,2),
(0.,1.),(0.,1.4712),.UNSPECIFIED.) ;
#1915 = B_SPLINE_SURFACE_WITH_KNOTS('',3,1,((#79165,#79166),(#79167,#79168),
(#79169,#79170),(#79171,#79172)),.UNSPECIFIED.,.F.,.F.,.F.,(4,4),(2,2),
(0.597473964327042,0.930240743465184),(0.,1.50203770750399),
 .UNSPECIFIED.) ;
#1916 = B_SPLINE_SURFACE_WITH_KNOTS('',3,1,((#79174,#79175),(#79176,#79177),
(#79178,#79179),(#79180,#79181),(#79182,#79183),(#79184,#79185),(#79186,
#79187)),.UNSPECIFIED.,.F.,.F.,.F.,(4,3,4),(2,2),(0.241689284630679,0.500017400470172,
0.549213097360471),(0.,1.50203770750399),.UNSPECIFIED.) ;
#1917 = B_SPLINE_SURFACE_WITH_KNOTS('',3,3,((#79198,#79199,#79200,#79201,
#79202,#79203,#79204,#79205,#79206,#79207),(#79208,#79209,#79210,#79211,
#79212,#79213,#79214,#79215,#79216,#79217),(#79218,#79219,#79220,#79221,
#79222,#79223,#79224,#79225,#79226,#79227),(#79228,#79229,#79230,#79231,
#79232,#79233,#79234,#79235,#79236,#79237),(#79238,#79239,#79240,#79241,
#79242,#79243,#79244,#79245,#79246,#79247)),.UNSPECIFIED.,.F.,.F.,.F.,(4,
1,4),(4,2,2,2,4),(0.,0.571428571428571,1.),(-0.000984424941950333,0.,0.0304393222729151,
0.0604225486602068,0.0620633422654789),.UNSPECIFIED.) ;
#1918 = B_SPLINE_SURFACE_WITH_KNOTS('',3,3,((#79324,#79325,#79326,#79327,
#79328,#79329,#79330,#79331),(#79332,#79333,#79334,#79335,#79336,#79337,
#79338,#79339),(#79340,#79341,#79342,#79343,#79344,#79345,#79346,#79347),
(#79348,#79349,#79350,#79351,#79352,#79353,#79354,#79355),(#79356,#79357,
#79358,#79359,#79360,#79361,#79362,#79363)),.UNSPECIFIED.,.F.,.F.,.F.,(4,
1,4),(4,2,2,4),(0.,0.571428571428571,1.),(-6.37514627733282E-5,0.0340909276764841,
0.0604383336928468,0.061399226101535),.UNSPECIFIED.) ;
#1919 = B_SPLINE_SURFACE_WITH_KNOTS('',3,3,((#79421,#79422,#79423,#79424,
#79425,#79426,#79427,#79428,#79429,#79430),(#79431,#79432,#79433,#79434,
#79435,#79436,#79437,#79438,#79439,#79440),(#79441,#79442,#79443,#79444,
#79445,#79446,#79447,#79448,#79449,#79450),(#79451,#79452,#79453,#79454,
#79455,#79456,#79457,#79458,#79459,#79460),(#79461,#79462,#79463,#79464,
#79465,#79466,#79467,#79468,#79469,#79470)),.UNSPECIFIED.,.F.,.F.,.F.,(4,
1,4),(4,2,2,2,4),(0.,0.571428571428571,1.),(-0.0016406621045341,0.,0.032656775096122,
0.0751675585986371,0.0752925967203965),.UNSPECIFIED.) ;
#1920 = B_SPLINE_SURFACE_WITH_KNOTS('',3,3,((#79556,#79557,#79558,#79559,
#79560,#79561,#79562,#79563,#79564,#79565),(#79566,#79567,#79568,#79569,
#79570,#79571,#79572,#79573,#79574,#79575),(#79576,#79577,#79578,#79579,
#79580,#79581,#79582,#79583,#79584,#79585),(#79586,#79587,#79588,#79589,
#79590,#79591,#79592,#79593,#79594,#79595),(#79596,#79597,#79598,#79599,
#79600,#79601,#79602,#79603,#79604,#79605)),.UNSPECIFIED.,.F.,.F.,.F.,(4,
1,4),(4,2,2,2,4),(0.,0.571428571428571,1.),(-0.00096080851771424,0.,0.0235600635035843,
0.0457311162964727,0.0467303873666823),.UNSPECIFIED.) ;
#1921 = B_SPLINE_SURFACE_WITH_KNOTS('',3,3,((#79638,#79639,#79640,#79641,
#79642,#79643,#79644,#79645,#79646,#79647),(#79648,#79649,#79650,#79651,
#79652,#79653,#79654,#79655,#79656,#79657),(#79658,#79659,#79660,#79661,
#79662,#79663,#79664,#79665,#79666,#79667),(#79668,#79669,#79670,#79671,
#79672,#79673,#79674,#79675,#79676,#79677),(#79678,#79679,#79680,#79681,
#79682,#79683,#79684,#79685,#79686,#79687)),.UNSPECIFIED.,.F.,.F.,.F.,(4,
1,4),(4,2,2,2,4),(0.,0.571428571428571,1.),(-0.000999294135844071,0.,0.0217198699392343,
0.0432144526123464,0.0441989132427654),.UNSPECIFIED.) ;
#1922 = B_SPLINE_SURFACE_WITH_KNOTS('',3,1,((#79740,#79741),(#79742,#79743),
(#79744,#79745),(#79746,#79747),(#79748,#79749)),.UNSPECIFIED.,.F.,.F.,
 .F.,(4,1,4),(2,2),(0.,0.0323852950215525,0.0574227556854303),(0.,0.0360000000000003),
 .UNSPECIFIED.) ;
#1923 = B_SPLINE_SURFACE_WITH_KNOTS('',3,3,((#79928,#79929,#79930,#79931,
#79932,#79933,#79934,#79935),(#79936,#79937,#79938,#79939,#79940,#79941,
#79942,#79943),(#79944,#79945,#79946,#79947,#79948,#79949,#79950,#79951),
(#79952,#79953,#79954,#79955,#79956,#79957,#79958,#79959),(#79960,#79961,
#79962,#79963,#79964,#79965,#79966,#79967)),.UNSPECIFIED.,.F.,.F.,.F.,(4,
1,4),(4,2,2,4),(0.,0.571428571428571,1.),(-4.75219968878011E-5,0.0386336727204952,
0.0678747004384468,0.0680822294122733),.UNSPECIFIED.) ;
#1924 = B_SPLINE_SURFACE_WITH_KNOTS('',3,3,((#80009,#80010,#80011,#80012,
#80013,#80014,#80015,#80016,#80017,#80018),(#80019,#80020,#80021,#80022,
#80023,#80024,#80025,#80026,#80027,#80028),(#80029,#80030,#80031,#80032,
#80033,#80034,#80035,#80036,#80037,#80038),(#80039,#80040,#80041,#80042,
#80043,#80044,#80045,#80046,#80047,#80048),(#80049,#80050,#80051,#80052,
#80053,#80054,#80055,#80056,#80057,#80058)),.UNSPECIFIED.,.F.,.F.,.F.,(4,
1,4),(4,2,2,2,4),(0.,0.571428571428571,1.),(-0.000207465766990066,0.,0.0232646742763639,
0.0410522705936588,0.041721226167804),.UNSPECIFIED.) ;
#1925 = B_SPLINE_SURFACE_WITH_KNOTS('',3,3,((#80119,#80120,#80121,#80122,
#80123,#80124),(#80125,#80126,#80127,#80128,#80129,#80130),(#80131,#80132,
#80133,#80134,#80135,#80136),(#80137,#80138,#80139,#80140,#80141,#80142),
(#80143,#80144,#80145,#80146,#80147,#80148)),.UNSPECIFIED.,.F.,.F.,.F.,
(4,1,4),(4,2,4),(0.,0.571428571428571,1.),(-2.08166817117217E-17,0.0453812948763195,
0.0792555822118552),.UNSPECIFIED.) ;
#1926 = B_SPLINE_SURFACE_WITH_KNOTS('',3,3,((#80172,#80173,#80174,#80175,
#80176,#80177,#80178,#80179,#80180,#80181),(#80182,#80183,#80184,#80185,
#80186,#80187,#80188,#80189,#80190,#80191),(#80192,#80193,#80194,#80195,
#80196,#80197,#80198,#80199,#80200,#80201),(#80202,#80203,#80204,#80205,
#80206,#80207,#80208,#80209,#80210,#80211),(#80212,#80213,#80214,#80215,
#80216,#80217,#80218,#80219,#80220,#80221)),.UNSPECIFIED.,.F.,.F.,.F.,(4,
1,4),(4,2,2,2,4),(0.,0.571428571428571,1.),(-0.000668949496694549,0.,0.0150950300818429,
0.0294213468333971,0.0303251295908459),.UNSPECIFIED.) ;
#1927 = B_SPLINE_SURFACE_WITH_KNOTS('',3,3,((#80269,#80270,#80271,#80272,
#80273,#80274,#80275,#80276),(#80277,#80278,#80279,#80280,#80281,#80282,
#80283,#80284),(#80285,#80286,#80287,#80288,#80289,#80290,#80291,#80292),
(#80293,#80294,#80295,#80296,#80297,#80298,#80299,#80300),(#80301,#80302,
#80303,#80304,#80305,#80306,#80307,#80308)),.UNSPECIFIED.,.F.,.F.,.F.,(4,
1,4),(4,2,2,4),(0.,0.571428571428571,1.),(-0.000903812556791651,0.,0.0126332411015006,
0.0312404144905361),.UNSPECIFIED.) ;
#1928 = B_SPLINE_SURFACE_WITH_KNOTS('',3,3,((#80345,#80346,#80347,#80348,
#80349,#80350,#80351,#80352),(#80353,#80354,#80355,#80356,#80357,#80358,
#80359,#80360),(#80361,#80362,#80363,#80364,#80365,#80366,#80367,#80368),
(#80369,#80370,#80371,#80372,#80373,#80374,#80375,#80376),(#80377,#80378,
#80379,#80380,#80381,#80382,#80383,#80384)),.UNSPECIFIED.,.F.,.F.,.F.,(4,
1,4),(4,1,2,1,4),(0.,0.571428571428571,1.),(-6.07153216596483E-15,0.0104867604235457,
0.0262169010588733,0.0371127510104888,0.0534565259379121),.UNSPECIFIED.) ;
#1929 = B_SPLINE_SURFACE_WITH_KNOTS('',3,3,((#80428,#80429,#80430,#80431,
#80432,#80433),(#80434,#80435,#80436,#80437,#80438,#80439),(#80440,#80441,
#80442,#80443,#80444,#80445),(#80446,#80447,#80448,#80449,#80450,#80451),
(#80452,#80453,#80454,#80455,#80456,#80457)),.UNSPECIFIED.,.F.,.F.,.F.,
(4,1,4),(4,2,4),(0.,0.571428571428571,1.),(-1.19054072156493E-14,0.0289083223985083,
0.0583191426684248),.UNSPECIFIED.) ;
#1930 = B_SPLINE_SURFACE_WITH_KNOTS('',3,3,((#80533,#80534,#80535,#80536,
#80537,#80538,#80539,#80540),(#80541,#80542,#80543,#80544,#80545,#80546,
#80547,#80548),(#80549,#80550,#80551,#80552,#80553,#80554,#80555,#80556),
(#80557,#80558,#80559,#80560,#80561,#80562,#80563,#80564),(#80565,#80566,
#80567,#80568,#80569,#80570,#80571,#80572)),.UNSPECIFIED.,.F.,.F.,.F.,(4,
1,4),(4,1,2,1,4),(0.,0.571428571428571,1.),(-1.21551489931584E-15,0.021868453247988,
0.0364474220799808,0.0505556257289287,0.0717179312023507),.UNSPECIFIED.) ;
#1931 = B_SPLINE_SURFACE_WITH_KNOTS('',3,3,((#80619,#80620,#80621,#80622,
#80623,#80624,#80625,#80626),(#80627,#80628,#80629,#80630,#80631,#80632,
#80633,#80634),(#80635,#80636,#80637,#80638,#80639,#80640,#80641,#80642),
(#80643,#80644,#80645,#80646,#80647,#80648,#80649,#80650),(#80651,#80652,
#80653,#80654,#80655,#80656,#80657,#80658),(#80659,#80660,#80661,#80662,
#80663,#80664,#80665,#80666)),.UNSPECIFIED.,.F.,.F.,.F.,(4,1,1,4),(4,2,
2,4),(0.,0.142857142857143,0.571428571428571,1.),(-3.34298561055327E-14,
0.0398009040484053,0.0884506599106943,0.125182168962163),.UNSPECIFIED.) ;
#1932 = B_SPLINE_SURFACE_WITH_KNOTS('',3,3,((#80688,#80689,#80690,#80691,
#80692,#80693,#80694,#80695),(#80696,#80697,#80698,#80699,#80700,#80701,
#80702,#80703),(#80704,#80705,#80706,#80707,#80708,#80709,#80710,#80711),
(#80712,#80713,#80714,#80715,#80716,#80717,#80718,#80719),(#80720,#80721,
#80722,#80723,#80724,#80725,#80726,#80727)),.UNSPECIFIED.,.F.,.F.,.F.,(4,
1,4),(4,2,2,4),(0.,0.571428571428571,1.),(-0.0369647188766498,0.,0.0196661092474417,
0.0352658770408685),.UNSPECIFIED.) ;
#1933 = B_SPLINE_SURFACE_WITH_KNOTS('',3,3,((#80766,#80767,#80768,#80769,
#80770,#80771),(#80772,#80773,#80774,#80775,#80776,#80777),(#80778,#80779,
#80780,#80781,#80782,#80783),(#80784,#80785,#80786,#80787,#80788,#80789),
(#80790,#80791,#80792,#80793,#80794,#80795)),.UNSPECIFIED.,.F.,.F.,.F.,
(4,1,4),(4,2,4),(0.,0.571428571428571,1.),(0.,0.0318468005485353,0.0669038356909525),
 .UNSPECIFIED.) ;
#1934 = B_SPLINE_SURFACE_WITH_KNOTS('',3,1,((#80830,#80831),(#80832,#80833),
(#80834,#80835),(#80836,#80837),(#80838,#80839)),.UNSPECIFIED.,.F.,.F.,
 .F.,(4,1,4),(2,2),(0.,0.0210301296927785,0.0377156586265697),(0.,0.0360000000000003),
 .UNSPECIFIED.) ;
#1935 = B_SPLINE_SURFACE_WITH_KNOTS('',3,1,((#80850,#80851),(#80852,#80853),
(#80854,#80855),(#80856,#80857),(#80858,#80859)),.UNSPECIFIED.,.F.,.F.,
 .F.,(4,1,4),(2,2),(0.,0.0329095469988702,0.0691336974954879),(0.,0.0360000000000003),
 .UNSPECIFIED.) ;
#1936 = B_SPLINE_SURFACE_WITH_KNOTS('',3,1,((#80880,#80881),(#80882,#80883),
(#80884,#80885),(#80886,#80887),(#80888,#80889)),.UNSPECIFIED.,.F.,.F.,
 .F.,(4,1,4),(2,2),(0.,0.0381782469542568,0.0670753371474822),(0.,0.0360000000000003),
 .UNSPECIFIED.) ;
#1937 = B_SPLINE_SURFACE_WITH_KNOTS('',3,1,((#80898,#80899),(#80900,#80901),
(#80902,#80903),(#80904,#80905),(#80906,#80907)),.UNSPECIFIED.,.F.,.F.,
 .F.,(4,1,4),(2,2),(0.,0.0216058216755205,0.0381303842659523),(0.,0.0360000000000003),
 .UNSPECIFIED.) ;
#1938 = B_SPLINE_SURFACE_WITH_KNOTS('',3,1,((#80916,#80917),(#80918,#80919),
(#80920,#80921),(#80922,#80923),(#80924,#80925)),.UNSPECIFIED.,.F.,.F.,
 .F.,(4,1,4),(2,2),(0.,0.0135228484064754,0.0263579081616444),(0.,0.0360000000000003),
 .UNSPECIFIED.) ;
#1939 = B_SPLINE_SURFACE_WITH_KNOTS('',3,1,((#80962,#80963),(#80964,#80965),
(#80966,#80967),(#80968,#80969),(#80970,#80971)),.UNSPECIFIED.,.F.,.F.,
 .F.,(4,1,4),(2,2),(0.,0.011955158932918,0.0295605475166918),(0.,0.0360000000000003),
 .UNSPECIFIED.) ;
#1940 = B_SPLINE_SURFACE_WITH_KNOTS('',3,3,((#80984,#80985,#80986,#80987,
#80988,#80989,#80990,#80991),(#80992,#80993,#80994,#80995,#80996,#80997,
#80998,#80999),(#81000,#81001,#81002,#81003,#81004,#81005,#81006,#81007),
(#81008,#81009,#81010,#81011,#81012,#81013,#81014,#81015),(#81016,#81017,
#81018,#81019,#81020,#81021,#81022,#81023)),.UNSPECIFIED.,.F.,.F.,.F.,(4,
1,4),(4,1,2,1,4),(0.,0.571428571428571,1.),(-6.50365178378404E-14,0.0105495395664116,
0.0175825659440626,0.0275093508272253,0.0341272074160004),.UNSPECIFIED.) ;
#1941 = B_SPLINE_SURFACE_WITH_KNOTS('',3,3,((#81119,#81120,#81121,#81122,
#81123,#81124,#81125),(#81126,#81127,#81128,#81129,#81130,#81131,#81132),
(#81133,#81134,#81135,#81136,#81137,#81138,#81139),(#81140,#81141,#81142,
#81143,#81144,#81145,#81146),(#81147,#81148,#81149,#81150,#81151,#81152,
#81153),(#81154,#81155,#81156,#81157,#81158,#81159,#81160)),
 .UNSPECIFIED.,.F.,.F.,.F.,(4,1,1,4),(4,2,1,4),(0.,0.142857142857143,0.571428571428571,
1.),(-8.68229099727415E-16,0.0271030272865255,0.0412193079076597,0.062393728839361),
 .UNSPECIFIED.) ;
#1942 = B_SPLINE_SURFACE_WITH_KNOTS('',3,3,((#81229,#81230,#81231,#81232,
#81233,#81234,#81235,#81236,#81237),(#81238,#81239,#81240,#81241,#81242,
#81243,#81244,#81245,#81246),(#81247,#81248,#81249,#81250,#81251,#81252,
#81253,#81254,#81255),(#81256,#81257,#81258,#81259,#81260,#81261,#81262,
#81263,#81264),(#81265,#81266,#81267,#81268,#81269,#81270,#81271,#81272,
#81273),(#81274,#81275,#81276,#81277,#81278,#81279,#81280,#81281,#81282)),
 .UNSPECIFIED.,.F.,.F.,.F.,(4,1,1,4),(4,1,2,1,1,4),(0.,0.285714285714286,
0.571428571428571,1.),(0.,0.00901895895784998,0.0225473973946249,0.0269891467103356,
0.0314308960260463,0.044761249451505),.UNSPECIFIED.) ;
#1943 = B_SPLINE_SURFACE_WITH_KNOTS('',3,3,((#81386,#81387,#81388,#81389,
#81390,#81391,#81392,#81393),(#81394,#81395,#81396,#81397,#81398,#81399,
#81400,#81401),(#81402,#81403,#81404,#81405,#81406,#81407,#81408,#81409),
(#81410,#81411,#81412,#81413,#81414,#81415,#81416,#81417),(#81418,#81419,
#81420,#81421,#81422,#81423,#81424,#81425)),.UNSPECIFIED.,.F.,.F.,.F.,(4,
1,4),(4,1,2,1,4),(0.,0.571428571428571,1.),(-3.8936437845742E-15,0.00990987059888721,
0.016516450998148,0.0263234394910323,0.0328614318196219),.UNSPECIFIED.) ;
#1944 = B_SPLINE_SURFACE_WITH_KNOTS('',3,3,((#81480,#81481,#81482,#81483,
#81484,#81485),(#81486,#81487,#81488,#81489,#81490,#81491),(#81492,#81493,
#81494,#81495,#81496,#81497),(#81498,#81499,#81500,#81501,#81502,#81503),
(#81504,#81505,#81506,#81507,#81508,#81509)),.UNSPECIFIED.,.F.,.F.,.F.,
(4,1,4),(4,2,4),(0.,0.571428571428571,1.),(-7.30609319335548E-6,0.0307388136698783,
0.0544948017664183),.UNSPECIFIED.) ;
#1945 = B_SPLINE_SURFACE_WITH_KNOTS('',3,3,((#81635,#81636,#81637,#81638,
#81639,#81640,#81641,#81642,#81643,#81644),(#81645,#81646,#81647,#81648,
#81649,#81650,#81651,#81652,#81653,#81654),(#81655,#81656,#81657,#81658,
#81659,#81660,#81661,#81662,#81663,#81664),(#81665,#81666,#81667,#81668,
#81669,#81670,#81671,#81672,#81673,#81674),(#81675,#81676,#81677,#81678,
#81679,#81680,#81681,#81682,#81683,#81684)),.UNSPECIFIED.,.F.,.F.,.F.,(4,
1,4),(4,2,2,2,4),(0.,0.571428571428571,1.),(-0.000721914453027042,0.,0.033998052296077,
0.0714230469344481,0.0715962515154608),.UNSPECIFIED.) ;
#1946 = B_SPLINE_SURFACE_WITH_KNOTS('',3,3,((#81730,#81731,#81732,#81733,
#81734,#81735,#81736,#81737),(#81738,#81739,#81740,#81741,#81742,#81743,
#81744,#81745),(#81746,#81747,#81748,#81749,#81750,#81751,#81752,#81753),
(#81754,#81755,#81756,#81757,#81758,#81759,#81760,#81761),(#81762,#81763,
#81764,#81765,#81766,#81767,#81768,#81769)),.UNSPECIFIED.,.F.,.F.,.F.,(4,
1,4),(4,2,2,4),(0.,0.571428571428571,1.),(5.55111512312578E-17,0.0224201537133612,
0.0402049350827121,0.0409268414934542),.UNSPECIFIED.) ;
#1947 = B_SPLINE_SURFACE_WITH_KNOTS('',3,3,((#81797,#81798,#81799,#81800,
#81801,#81802,#81803,#81804),(#81805,#81806,#81807,#81808,#81809,#81810,
#81811,#81812),(#81813,#81814,#81815,#81816,#81817,#81818,#81819,#81820),
(#81821,#81822,#81823,#81824,#81825,#81826,#81827,#81828),(#81829,#81830,
#81831,#81832,#81833,#81834,#81835,#81836)),.UNSPECIFIED.,.F.,.F.,.F.,(4,
1,4),(4,2,2,4),(0.,0.571428571428571,1.),(-0.00145402880520905,0.,0.0452350077421772,
0.100520135955306),.UNSPECIFIED.) ;
#1948 = B_SPLINE_SURFACE_WITH_KNOTS('',3,3,((#81867,#81868,#81869,#81870,
#81871,#81872,#81873,#81874,#81875,#81876),(#81877,#81878,#81879,#81880,
#81881,#81882,#81883,#81884,#81885,#81886),(#81887,#81888,#81889,#81890,
#81891,#81892,#81893,#81894,#81895,#81896),(#81897,#81898,#81899,#81900,
#81901,#81902,#81903,#81904,#81905,#81906),(#81907,#81908,#81909,#81910,
#81911,#81912,#81913,#81914,#81915,#81916)),.UNSPECIFIED.,.F.,.F.,.F.,(4,
1,4),(4,2,2,2,4),(0.,0.571428571428571,1.),(-0.000848777061136591,0.,0.0435056845362515,
0.0856081292457083,0.0870620753300636),.UNSPECIFIED.) ;
#1949 = B_SPLINE_SURFACE_WITH_KNOTS('',3,3,((#81969,#81970,#81971,#81972,
#81973,#81974,#81975,#81976,#81977,#81978),(#81979,#81980,#81981,#81982,
#81983,#81984,#81985,#81986,#81987,#81988),(#81989,#81990,#81991,#81992,
#81993,#81994,#81995,#81996,#81997,#81998),(#81999,#82000,#82001,#82002,
#82003,#82004,#82005,#82006,#82007,#82008),(#82009,#82010,#82011,#82012,
#82013,#82014,#82015,#82016,#82017,#82018)),.UNSPECIFIED.,.F.,.F.,.F.,(4,
1,4),(4,2,2,2,4),(0.,0.571428571428571,1.),(-0.000832239105180238,0.,0.0338448162467367,
0.0682776647009788,0.0691265383481362),.UNSPECIFIED.) ;
#1950 = B_SPLINE_SURFACE_WITH_KNOTS('',3,3,((#82071,#82072,#82073,#82074,
#82075,#82076,#82077,#82078,#82079,#82080),(#82081,#82082,#82083,#82084,
#82085,#82086,#82087,#82088,#82089,#82090),(#82091,#82092,#82093,#82094,
#82095,#82096,#82097,#82098,#82099,#82100),(#82101,#82102,#82103,#82104,
#82105,#82106,#82107,#82108,#82109,#82110),(#82111,#82112,#82113,#82114,
#82115,#82116,#82117,#82118,#82119,#82120)),.UNSPECIFIED.,.F.,.F.,.F.,(4,
1,4),(4,2,2,2,4),(0.,0.571428571428571,1.),(-0.00109408852437443,0.,0.0321085924337593,
0.065468485698588,0.0663005130080268),.UNSPECIFIED.) ;
#1951 = B_SPLINE_SURFACE_WITH_KNOTS('',3,3,((#82153,#82154,#82155,#82156,
#82157,#82158,#82159,#82160),(#82161,#82162,#82163,#82164,#82165,#82166,
#82167,#82168),(#82169,#82170,#82171,#82172,#82173,#82174,#82175,#82176),
(#82177,#82178,#82179,#82180,#82181,#82182,#82183,#82184),(#82185,#82186,
#82187,#82188,#82189,#82190,#82191,#82192)),.UNSPECIFIED.,.F.,.F.,.F.,(4,
1,4),(4,2,2,4),(0.,0.571428571428571,1.),(-4.70756737529766E-5,0.0490110014082998,
0.085595699976472,0.0866902249621159),.UNSPECIFIED.) ;
#1952 = B_SPLINE_SURFACE_WITH_KNOTS('',3,3,((#82273,#82274,#82275,#82276,
#82277,#82278),(#82279,#82280,#82281,#82282,#82283,#82284),(#82285,#82286,
#82287,#82288,#82289,#82290),(#82291,#82292,#82293,#82294,#82295,#82296),
(#82297,#82298,#82299,#82300,#82301,#82302)),.UNSPECIFIED.,.F.,.F.,.F.,
(4,1,4),(4,2,4),(0.,0.571428571428571,1.),(-3.37568514807661E-14,0.0112807751130659,
0.0278988061061053),.UNSPECIFIED.) ;
#1953 = B_SPLINE_SURFACE_WITH_KNOTS('',3,3,((#82328,#82329,#82330,#82331,
#82332,#82333),(#82334,#82335,#82336,#82337,#82338,#82339),(#82340,#82341,
#82342,#82343,#82344,#82345),(#82346,#82347,#82348,#82349,#82350,#82351),
(#82352,#82353,#82354,#82355,#82356,#82357)),.UNSPECIFIED.,.F.,.F.,.F.,
(4,1,4),(4,2,4),(0.,0.571428571428571,1.),(-4.8815118613983E-15,0.0119728599231917,
0.023335857822899),.UNSPECIFIED.) ;
#1954 = B_SPLINE_SURFACE_WITH_KNOTS('',3,3,((#82396,#82397,#82398,#82399,
#82400,#82401),(#82402,#82403,#82404,#82405,#82406,#82407),(#82408,#82409,
#82410,#82411,#82412,#82413),(#82414,#82415,#82416,#82417,#82418,#82419),
(#82420,#82421,#82422,#82423,#82424,#82425)),.UNSPECIFIED.,.F.,.F.,.F.,
(4,1,4),(4,2,4),(0.,0.571428571428571,1.),(-2.77555756156289E-17,0.0199847249930681,
0.0352638829354677),.UNSPECIFIED.) ;
#1955 = B_SPLINE_SURFACE_WITH_KNOTS('',3,3,((#82464,#82465,#82466,#82467,
#82468,#82469),(#82470,#82471,#82472,#82473,#82474,#82475),(#82476,#82477,
#82478,#82479,#82480,#82481),(#82482,#82483,#82484,#82485,#82486,#82487),
(#82488,#82489,#82490,#82491,#82492,#82493)),.UNSPECIFIED.,.F.,.F.,.F.,
(4,1,4),(4,2,4),(-2.09809871143395E-6,0.571428571428571,1.00000209810189),
(-7.54436050495102E-6,0.0377278926030736,0.066283338281117),
 .UNSPECIFIED.) ;
#1956 = B_SPLINE_SURFACE_WITH_KNOTS('',3,1,((#82502,#82503),(#82504,#82505),
(#82506,#82507),(#82508,#82509),(#82510,#82511)),.UNSPECIFIED.,.F.,.F.,
 .F.,(4,1,4),(2,2),(0.,0.0398228695438388,0.0783699334705556),(0.,0.0360000000000003),
 .UNSPECIFIED.) ;
#1957 = B_SPLINE_SURFACE_WITH_KNOTS('',3,1,((#82514,#82515),(#82516,#82517),
(#82518,#82519),(#82520,#82521),(#82522,#82523)),.UNSPECIFIED.,.F.,.F.,
 .F.,(4,1,4),(2,2),(0.,0.0313133324080373,0.063168759987351),(0.,0.0360000000000003),
 .UNSPECIFIED.) ;
#1958 = B_SPLINE_SURFACE_WITH_KNOTS('',3,1,((#82525,#82526),(#82527,#82528),
(#82529,#82530),(#82531,#82532),(#82533,#82534)),.UNSPECIFIED.,.F.,.F.,
 .F.,(4,1,4),(2,2),(0.,0.0290828541577381,0.0592932101613289),(0.,0.0360000000000003),
 .UNSPECIFIED.) ;
#1959 = B_SPLINE_SURFACE_WITH_KNOTS('',3,1,((#82536,#82537),(#82538,#82539),
(#82540,#82541),(#82542,#82543),(#82544,#82545)),.UNSPECIFIED.,.F.,.F.,
 .F.,(4,1,4),(2,2),(0.,0.0471458586470647,0.0823534588635132),(0.,0.0360000000000003),
 .UNSPECIFIED.) ;
#1960 = B_SPLINE_SURFACE_WITH_KNOTS('',3,1,((#82958,#82959),(#82960,#82961),
(#82962,#82963),(#82964,#82965),(#82966,#82967)),.UNSPECIFIED.,.F.,.F.,
 .F.,(4,1,4),(2,2),(0.,0.0298071351389365,0.0685496713495228),(0.,0.0360000000000003),
 .UNSPECIFIED.) ;
#1961 = B_SPLINE_SURFACE_WITH_KNOTS('',3,1,((#82969,#82970),(#82971,#82972),
(#82973,#82974),(#82975,#82976),(#82977,#82978)),.UNSPECIFIED.,.F.,.F.,
 .F.,(4,1,4),(2,2),(0.,0.0263673128827931,0.0523427870633456),(0.,0.0360000000000003),
 .UNSPECIFIED.) ;
#1962 = B_SPLINE_SURFACE_WITH_KNOTS('',3,1,((#82980,#82981),(#82982,#82983),
(#82984,#82985),(#82986,#82987),(#82988,#82989)),.UNSPECIFIED.,.F.,.F.,
 .F.,(4,1,4),(2,2),(0.,0.0190758281807941,0.0379545209982657),(0.,0.0360000000000003),
 .UNSPECIFIED.) ;
#1963 = B_SPLINE_SURFACE_WITH_KNOTS('',3,1,((#82991,#82992),(#82993,#82994),
(#82995,#82996),(#82997,#82998),(#82999,#83000)),.UNSPECIFIED.,.F.,.F.,
 .F.,(4,1,4),(2,2),(0.,0.0205128997765721,0.0398218276255599),(0.,0.0360000000000003),
 .UNSPECIFIED.) ;
#1964 = B_SPLINE_SURFACE_WITH_KNOTS('',3,1,((#83001,#83002),(#83003,#83004),
(#83005,#83006),(#83007,#83008),(#83009,#83010)),.UNSPECIFIED.,.F.,.F.,
 .F.,(4,1,4),(2,2),(0.,0.0424180496051088,0.0942055476140892),(0.,0.0360000000000003),
 .UNSPECIFIED.) ;
#1965 = B_SPLINE_SURFACE_WITH_KNOTS('',3,3,((#83571,#83572,#83573,#83574,
#83575,#83576,#83577,#83578,#83579,#83580,#83581,#83582,#83583,#83584,#83585,
#83586,#83587,#83588),(#83589,#83590,#83591,#83592,#83593,#83594,#83595,
#83596,#83597,#83598,#83599,#83600,#83601,#83602,#83603,#83604,#83605,#83606),
(#83607,#83608,#83609,#83610,#83611,#83612,#83613,#83614,#83615,#83616,
#83617,#83618,#83619,#83620,#83621,#83622,#83623,#83624),(#83625,#83626,
#83627,#83628,#83629,#83630,#83631,#83632,#83633,#83634,#83635,#83636,#83637,
#83638,#83639,#83640,#83641,#83642),(#83643,#83644,#83645,#83646,#83647,
#83648,#83649,#83650,#83651,#83652,#83653,#83654,#83655,#83656,#83657,#83658,
#83659,#83660)),.UNSPECIFIED.,.F.,.T.,.F.,(4,1,4),(4,1,1,1,1,1,1,1,1,1,
1,1,1,1,1,4),(0.,0.571428571428571,1.),(-1.24903384766071,-1.07060044085204,
-0.892167034043367,-0.713733627234693,-0.53530022042602,-0.356866813617347,
-0.178433406808673,0.0594778022695577,0.118955604539115,0.178433406808673,
0.356866813617347,0.53530022042602,0.713733627234693,0.892167034043367,
1.07060044085204,1.24903384766071),.UNSPECIFIED.) ;
#1966 = B_SPLINE_SURFACE_WITH_KNOTS('',3,3,((#84017,#84018,#84019,#84020),
(#84021,#84022,#84023,#84024),(#84025,#84026,#84027,#84028),(#84029,#84030,
#84031,#84032),(#84033,#84034,#84035,#84036)),.UNSPECIFIED.,.F.,.F.,.F.,
(4,1,4),(4,4),(0.,0.5,1.),(1.57079632679485,1.68822329689356),
 .UNSPECIFIED.) ;
#1967 = B_SPLINE_SURFACE_WITH_KNOTS('',3,3,((#84040,#84041,#84042,#84043),
(#84044,#84045,#84046,#84047),(#84048,#84049,#84050,#84051),(#84052,#84053,
#84054,#84055),(#84056,#84057,#84058,#84059)),.UNSPECIFIED.,.F.,.F.,.F.,
(4,1,4),(4,4),(0.,0.5,1.00076388698133),(0.38994149913495,0.401496426112861),
 .UNSPECIFIED.) ;
#1968 = B_SPLINE_SURFACE_WITH_KNOTS('',3,3,((#84085,#84086,#84087,#84088,
#84089),(#84090,#84091,#84092,#84093,#84094),(#84095,#84096,#84097,#84098,
#84099),(#84100,#84101,#84102,#84103,#84104),(#84105,#84106,#84107,#84108,
#84109)),.UNSPECIFIED.,.F.,.F.,.F.,(4,1,4),(4,1,4),(0.,0.5,1.),(0.,0.00867853090984697,
0.0173570618196939),.UNSPECIFIED.) ;
#1969 = B_SPLINE_SURFACE_WITH_KNOTS('',3,3,((#84251,#84252,#84253,#84254),
(#84255,#84256,#84257,#84258),(#84259,#84260,#84261,#84262),(#84263,#84264,
#84265,#84266),(#84267,#84268,#84269,#84270)),.UNSPECIFIED.,.F.,.F.,.F.,
(4,1,4),(4,4),(0.,0.571428571428571,1.),(-1.11022302462516E-16,1.5707963267949),
 .UNSPECIFIED.) ;
#1970 = B_SPLINE_SURFACE_WITH_KNOTS('',3,3,((#84279,#84280,#84281,#84282),
(#84283,#84284,#84285,#84286),(#84287,#84288,#84289,#84290),(#84291,#84292,
#84293,#84294),(#84295,#84296,#84297,#84298)),.UNSPECIFIED.,.F.,.F.,.F.,
(4,1,4),(4,4),(0.,0.571428571428571,1.),(-8.77933589643389E-15,1.5707963267949),
 .UNSPECIFIED.) ;
#1971 = B_SPLINE_SURFACE_WITH_KNOTS('',3,3,((#84547,#84548,#84549,#84550),
(#84551,#84552,#84553,#84554),(#84555,#84556,#84557,#84558),(#84559,#84560,
#84561,#84562),(#84563,#84564,#84565,#84566)),.UNSPECIFIED.,.F.,.F.,.F.,
(4,1,4),(4,4),(0.,0.571428571428571,1.),(-6.90310534513333E-14,1.5707963267949),
 .UNSPECIFIED.) ;
#1972 = B_SPLINE_SURFACE_WITH_KNOTS('',3,3,((#84575,#84576,#84577,#84578),
(#84579,#84580,#84581,#84582),(#84583,#84584,#84585,#84586),(#84587,#84588,
#84589,#84590),(#84591,#84592,#84593,#84594)),.UNSPECIFIED.,.F.,.F.,.F.,
(4,1,4),(4,4),(0.,0.571428571428571,1.),(-1.5707963267949,1.68448774068473E-13),
 .UNSPECIFIED.) ;
#1973 = B_SPLINE_SURFACE_WITH_KNOTS('',3,3,((#85979,#85980,#85981,#85982,
#85983,#85984),(#85985,#85986,#85987,#85988,#85989,#85990),(#85991,#85992,
#85993,#85994,#85995,#85996),(#85997,#85998,#85999,#86000,#86001,#86002),
(#86003,#86004,#86005,#86006,#86007,#86008)),.UNSPECIFIED.,.F.,.F.,.F.,
(4,1,4),(4,1,1,4),(-0.000538086234182272,0.5,1.00053808622348),(-0.000538086234182344,
0.448798950512828,0.897597901025655,1.5707963267949),.UNSPECIFIED.) ;
#1974 = B_SPLINE_SURFACE_WITH_KNOTS('',3,3,((#86013,#86014,#86015,#86016,
#86017),(#86018,#86019,#86020,#86021,#86022),(#86023,#86024,#86025,#86026,
#86027),(#86028,#86029,#86030,#86031,#86032),(#86033,#86034,#86035,#86036,
#86037)),.UNSPECIFIED.,.F.,.F.,.F.,(4,1,4),(4,1,4),(-0.00316978173158919,
0.5,1.00316978173188),(-0.00316978173188948,0.673198425769238,1.5707963267949),
 .UNSPECIFIED.) ;
#1975 = B_SPLINE_SURFACE_WITH_KNOTS('',3,3,((#86046,#86047,#86048,#86049,
#86050),(#86051,#86052,#86053,#86054,#86055),(#86056,#86057,#86058,#86059,
#86060),(#86061,#86062,#86063,#86064,#86065),(#86066,#86067,#86068,#86069,
#86070)),.UNSPECIFIED.,.F.,.F.,.F.,(4,1,4),(4,1,4),(-0.00317101823526472,
0.5,1.00317101819783),(-0.00317101823526462,0.673198425769241,1.5707963267949),
 .UNSPECIFIED.) ;
#1976 = B_SPLINE_SURFACE_WITH_KNOTS('',3,3,((#86079,#86080,#86081,#86082,
#86083),(#86084,#86085,#86086,#86087,#86088),(#86089,#86090,#86091,#86092,
#86093),(#86094,#86095,#86096,#86097,#86098),(#86099,#86100,#86101,#86102,
#86103)),.UNSPECIFIED.,.F.,.F.,.F.,(4,1,4),(4,1,4),(-0.00317180722397545,
0.5,1.00317180718751),(-0.00317180722396792,0.673198425769246,1.5707963267949),
 .UNSPECIFIED.) ;
#1977 = B_SPLINE_SURFACE_WITH_KNOTS('',3,3,((#86113,#86114,#86115,#86116,
#86117,#86118),(#86119,#86120,#86121,#86122,#86123,#86124),(#86125,#86126,
#86127,#86128,#86129,#86130),(#86131,#86132,#86133,#86134,#86135,#86136),
(#86137,#86138,#86139,#86140,#86141,#86142)),.UNSPECIFIED.,.F.,.F.,.F.,
(4,1,4),(4,1,1,4),(0.,0.571428571428571,1.00028292742608),(-0.000282927426077196,
0.673198425769239,1.12199737628207,1.57107925422097),.UNSPECIFIED.) ;
#1978 = B_SPLINE_SURFACE_WITH_KNOTS('',3,3,((#86147,#86148,#86149,#86150,
#86151),(#86152,#86153,#86154,#86155,#86156),(#86157,#86158,#86159,#86160,
#86161),(#86162,#86163,#86164,#86165,#86166),(#86167,#86168,#86169,#86170,
#86171)),.UNSPECIFIED.,.F.,.F.,.F.,(4,1,4),(4,1,4),(-0.000895493577093496,
0.571428571428571,1.00047285387642),(-1.57169182037199,-0.897597901025654,
0.000895493577097937),.UNSPECIFIED.) ;
#1979 = B_SPLINE_SURFACE_WITH_KNOTS('',3,3,((#86182,#86183,#86184,#86185,
#86186,#86187),(#86188,#86189,#86190,#86191,#86192,#86193),(#86194,#86195,
#86196,#86197,#86198,#86199),(#86200,#86201,#86202,#86203,#86204,#86205),
(#86206,#86207,#86208,#86209,#86210,#86211)),.UNSPECIFIED.,.F.,.F.,.F.,
(4,1,4),(4,1,1,4),(0.,0.571428571428571,1.00028282366511),(-0.000282823665114463,
0.67319842576924,1.12199737628207,1.57107915046001),.UNSPECIFIED.) ;
#1980 = B_SPLINE_SURFACE_WITH_KNOTS('',3,3,((#86216,#86217,#86218,#86219,
#86220),(#86221,#86222,#86223,#86224,#86225),(#86226,#86227,#86228,#86229,
#86230),(#86231,#86232,#86233,#86234,#86235),(#86236,#86237,#86238,#86239,
#86240)),.UNSPECIFIED.,.F.,.F.,.F.,(4,1,4),(4,1,4),(-0.00089808555193699,
0.571428571428571,1.00047258665151),(-1.57169441234684,-0.897597901025656,
0.000898085551936612),.UNSPECIFIED.) ;
#1981 = B_SPLINE_SURFACE_WITH_KNOTS('',3,3,((#86321,#86322,#86323,#86324,
#86325),(#86326,#86327,#86328,#86329,#86330),(#86331,#86332,#86333,#86334,
#86335),(#86336,#86337,#86338,#86339,#86340),(#86341,#86342,#86343,#86344,
#86345)),.UNSPECIFIED.,.F.,.F.,.F.,(4,1,4),(4,1,4),(0.232659879271761,0.620020769070722,
1.),(0.173726017404586,0.773477463983206,1.5707963267949),.UNSPECIFIED.) ;
#1982 = B_SPLINE_SURFACE_WITH_KNOTS('',3,3,((#86346,#86347,#86348,#86349,
#86350),(#86351,#86352,#86353,#86354,#86355),(#86356,#86357,#86358,#86359,
#86360),(#86361,#86362,#86363,#86364,#86365),(#86366,#86367,#86368,#86369,
#86370)),.UNSPECIFIED.,.F.,.F.,.F.,(4,1,4),(4,1,4),(0.229110535172741,0.622952086196121,
1.),(-1.57079632679489,-0.972068585274832,-0.173764929914751),
 .UNSPECIFIED.) ;
#1983 = B_SPLINE_SURFACE_WITH_KNOTS('',3,3,((#86371,#86372,#86373,#86374,
#86375),(#86376,#86377,#86378,#86379,#86380),(#86381,#86382,#86383,#86384,
#86385),(#86386,#86387,#86388,#86389,#86390),(#86391,#86392,#86393,#86394,
#86395)),.UNSPECIFIED.,.F.,.F.,.F.,(4,1,4),(4,1,4),(0.2291096770137,0.622952086196224,
1.),(-1.57079632679489,-0.972068585273428,-0.173764929911475),
 .UNSPECIFIED.) ;
#1984 = B_SPLINE_SURFACE_WITH_KNOTS('',3,3,((#86397,#86398,#86399,#86400,
#86401),(#86402,#86403,#86404,#86405,#86406),(#86407,#86408,#86409,#86410,
#86411),(#86412,#86413,#86414,#86415,#86416),(#86417,#86418,#86419,#86420,
#86421)),.UNSPECIFIED.,.F.,.F.,.F.,(4,1,4),(4,1,4),(0.232660620324116,0.620020769070722,
1.),(0.173725984876902,0.773477463983786,1.57079632679491),
 .UNSPECIFIED.) ;
#1985 = B_SPLINE_SURFACE_WITH_KNOTS('',3,3,((#86423,#86424,#86425,#86426,
#86427,#86428),(#86429,#86430,#86431,#86432,#86433,#86434),(#86435,#86436,
#86437,#86438,#86439,#86440),(#86441,#86442,#86443,#86444,#86445,#86446),
(#86447,#86448,#86449,#86450,#86451,#86452)),.UNSPECIFIED.,.F.,.F.,.F.,
(4,1,4),(4,1,1,4),(-0.026021099187187,0.5,1.00149490139021),(-1.59681742598208,
-0.897597901025652,-0.448798950512825,0.0260210991871885),.UNSPECIFIED.) ;
#1986 = B_SPLINE_SURFACE_WITH_KNOTS('',3,3,((#86454,#86455,#86456,#86457,
#86458),(#86459,#86460,#86461,#86462,#86463),(#86464,#86465,#86466,#86467,
#86468),(#86469,#86470,#86471,#86472,#86473),(#86474,#86475,#86476,#86477,
#86478)),.UNSPECIFIED.,.F.,.F.,.F.,(4,1,4),(4,1,4),(-0.0540331686418731,
0.5,1.00272533009723),(-0.0540331686418767,0.673198425769243,1.62482949543678),
 .UNSPECIFIED.) ;
#1987 = B_SPLINE_SURFACE_WITH_KNOTS('',3,3,((#86479,#86480,#86481,#86482,
#86483,#86484),(#86485,#86486,#86487,#86488,#86489,#86490),(#86491,#86492,
#86493,#86494,#86495,#86496),(#86497,#86498,#86499,#86500,#86501,#86502),
(#86503,#86504,#86505,#86506,#86507,#86508)),.UNSPECIFIED.,.F.,.F.,.F.,
(4,1,4),(4,1,1,4),(-0.0260423511979298,0.5,1.00147848522175),(-0.0260423511979351,
0.448798950512826,0.897597901025657,1.59683867799283),.UNSPECIFIED.) ;
#1988 = B_SPLINE_SURFACE_WITH_KNOTS('',3,3,((#86509,#86510,#86511,#86512,
#86513,#86514),(#86515,#86516,#86517,#86518,#86519,#86520),(#86521,#86522,
#86523,#86524,#86525,#86526),(#86527,#86528,#86529,#86530,#86531,#86532),
(#86533,#86534,#86535,#86536,#86537,#86538)),.UNSPECIFIED.,.F.,.F.,.F.,
(4,1,4),(4,1,1,4),(-0.0260371921793241,0.5,1.00148247115979),(-1.59683351897421,
-0.897597901025653,-0.448798950512826,0.0260371921793241),.UNSPECIFIED.) ;
#1989 = B_SPLINE_SURFACE_WITH_KNOTS('',3,3,((#87076,#87077,#87078,#87079,
#87080),(#87081,#87082,#87083,#87084,#87085),(#87086,#87087,#87088,#87089,
#87090),(#87091,#87092,#87093,#87094,#87095),(#87096,#87097,#87098,#87099,
#87100)),.UNSPECIFIED.,.F.,.F.,.F.,(4,1,4),(4,1,4),(-0.000337535876093274,
0.5,1.00033753587942),(-1.5707963267949,-0.897597901025655,0.000337535879419949),
 .UNSPECIFIED.) ;
#1990 = B_SPLINE_SURFACE_WITH_KNOTS('',3,3,((#87116,#87117,#87118,#87119,
#87120),(#87121,#87122,#87123,#87124,#87125),(#87126,#87127,#87128,#87129,
#87130),(#87131,#87132,#87133,#87134,#87135),(#87136,#87137,#87138,#87139,
#87140)),.UNSPECIFIED.,.F.,.F.,.F.,(4,1,4),(4,1,4),(-0.000337608092631786,
0.5,1.00033760812633),(-1.5707963267949,-0.897597901025655,0.000337608126388777),
 .UNSPECIFIED.) ;
#1991 = B_SPLINE_SURFACE_WITH_KNOTS('',3,3,((#87541,#87542,#87543,#87544),
(#87545,#87546,#87547,#87548),(#87549,#87550,#87551,#87552),(#87553,#87554,
#87555,#87556),(#87557,#87558,#87559,#87560)),.UNSPECIFIED.,.F.,.F.,.F.,
(4,1,4),(4,4),(-0.0153229911164263,0.571428571428571,1.01526317510374),
(-1.5707963267949,0.0153229911164264),.UNSPECIFIED.) ;
#1992 = B_SPLINE_SURFACE_WITH_KNOTS('',3,3,((#87577,#87578,#87579,#87580,
#87581),(#87582,#87583,#87584,#87585,#87586),(#87587,#87588,#87589,#87590,
#87591),(#87592,#87593,#87594,#87595,#87596),(#87597,#87598,#87599,#87600,
#87601)),.UNSPECIFIED.,.F.,.F.,.F.,(4,1,4),(4,1,4),(-0.00114528587145135,
0.571428571428571,1.00114914004475),(-1.5707963267949,-0.897597901025655,
0.00114914004475158),.UNSPECIFIED.) ;
#1993 = B_SPLINE_SURFACE_WITH_KNOTS('',3,3,((#87624,#87625,#87626,#87627),
(#87628,#87629,#87630,#87631),(#87632,#87633,#87634,#87635),(#87636,#87637,
#87638,#87639),(#87640,#87641,#87642,#87643)),.UNSPECIFIED.,.F.,.F.,.F.,
(4,1,4),(4,4),(-0.0153229910814027,0.571428571428571,1.0152631750376),(-1.5707963267949,
0.0153229910814969),.UNSPECIFIED.) ;
#1994 = B_SPLINE_SURFACE_WITH_KNOTS('',3,3,((#87665,#87666,#87667,#87668),
(#87669,#87670,#87671,#87672),(#87673,#87674,#87675,#87676),(#87677,#87678,
#87679,#87680),(#87681,#87682,#87683,#87684)),.UNSPECIFIED.,.F.,.F.,.F.,
(4,1,4),(4,4),(-0.0153229913038913,0.571428571428571,1.01526317545535),
(-1.5707963267949,0.0153229913038913),.UNSPECIFIED.) ;
#1995 = B_SPLINE_SURFACE_WITH_KNOTS('',3,3,((#87701,#87702,#87703,#87704,
#87705),(#87706,#87707,#87708,#87709,#87710),(#87711,#87712,#87713,#87714,
#87715),(#87716,#87717,#87718,#87719,#87720),(#87721,#87722,#87723,#87724,
#87725)),.UNSPECIFIED.,.F.,.F.,.F.,(4,1,4),(4,1,4),(-0.00114514914518223,
0.571428571428571,1.00114900336214),(-1.5707963267949,-0.897597901025655,
0.0011490033621433),.UNSPECIFIED.) ;
#1996 = B_SPLINE_SURFACE_WITH_KNOTS('',3,3,((#87751,#87752,#87753,#87754),
(#87755,#87756,#87757,#87758),(#87759,#87760,#87761,#87762),(#87763,#87764,
#87765,#87766),(#87767,#87768,#87769,#87770)),.UNSPECIFIED.,.F.,.F.,.F.,
(4,1,4),(4,4),(-0.0153229913446253,0.571428571428571,1.01526317558427),
(-1.5707963267949,0.0153229913446253),.UNSPECIFIED.) ;
#1997 = B_SPLINE_SURFACE_WITH_KNOTS('',3,3,((#87789,#87790,#87791,#87792),
(#87793,#87794,#87795,#87796),(#87797,#87798,#87799,#87800),(#87801,#87802,
#87803,#87804),(#87805,#87806,#87807,#87808)),.UNSPECIFIED.,.F.,.F.,.F.,
(4,1,4),(4,4),(-0.0153229910815485,0.571428571428571,1.01526317509188),
(-1.5707963267949,0.0153229910815485),.UNSPECIFIED.) ;
#1998 = B_SPLINE_SURFACE_WITH_KNOTS('',3,3,((#87828,#87829,#87830,#87831,
#87832),(#87833,#87834,#87835,#87836,#87837),(#87838,#87839,#87840,#87841,
#87842),(#87843,#87844,#87845,#87846,#87847),(#87848,#87849,#87850,#87851,
#87852)),.UNSPECIFIED.,.F.,.F.,.F.,(4,1,4),(4,1,4),(-0.00114539327423229,
0.571428571428571,1.00114924740985),(-1.5707963267949,-0.897597901025655,
0.00114924740985024),.UNSPECIFIED.) ;
#1999 = B_SPLINE_SURFACE_WITH_KNOTS('',3,3,((#87875,#87876,#87877,#87878),
(#87879,#87880,#87881,#87882),(#87883,#87884,#87885,#87886),(#87887,#87888,
#87889,#87890),(#87891,#87892,#87893,#87894)),.UNSPECIFIED.,.F.,.F.,.F.,
(4,1,4),(4,4),(-0.0153229911159153,0.571428571428571,1.01526317510136),
(-1.5707963267949,0.0153229911159153),.UNSPECIFIED.) ;
#2000 = B_SPLINE_SURFACE_WITH_KNOTS('',3,3,((#87916,#87917,#87918,#87919),
(#87920,#87921,#87922,#87923),(#87924,#87925,#87926,#87927),(#87928,#87929,
#87930,#87931),(#87932,#87933,#87934,#87935)),.UNSPECIFIED.,.F.,.F.,.F.,
(4,1,4),(4,4),(-0.0153229913444723,0.571428571428571,1.01526317558858),
(-1.5707963267949,0.0153229913444723),.UNSPECIFIED.) ;
#2001 = B_SPLINE_SURFACE_WITH_KNOTS('',3,3,((#87952,#87953,#87954,#87955,
#87956),(#87957,#87958,#87959,#87960,#87961),(#87962,#87963,#87964,#87965,
#87966),(#87967,#87968,#87969,#87970,#87971),(#87972,#87973,#87974,#87975,
#87976)),.UNSPECIFIED.,.F.,.F.,.F.,(4,1,4),(4,1,4),(-0.00114528587149614,
0.571428571428571,1.00114914004187),(-1.5707963267949,-0.897597901025655,
0.00114914004186756),.UNSPECIFIED.) ;
#2002 = B_SPLINE_SURFACE_WITH_KNOTS('',3,3,((#88002,#88003,#88004,#88005),
(#88006,#88007,#88008,#88009),(#88010,#88011,#88012,#88013),(#88014,#88015,
#88016,#88017),(#88018,#88019,#88020,#88021)),.UNSPECIFIED.,.F.,.F.,.F.,
(4,1,4),(4,4),(-0.0153229913034765,0.571428571428571,1.01526317551047),
(-1.5707963267949,0.0153229913034765),.UNSPECIFIED.) ;
#2003 = B_SPLINE_SURFACE_WITH_KNOTS('',3,3,((#88809,#88810,#88811,#88812,
#88813,#88814),(#88815,#88816,#88817,#88818,#88819,#88820),(#88821,#88822,
#88823,#88824,#88825,#88826),(#88827,#88828,#88829,#88830,#88831,#88832),
(#88833,#88834,#88835,#88836,#88837,#88838)),.UNSPECIFIED.,.F.,.F.,.F.,
(4,1,4),(4,1,1,4),(-0.00263861939634921,0.571428571428571,1.),(4.70975036097816,
5.38558740615393,5.83438635666676,6.28582392658612),.UNSPECIFIED.) ;
#2004 = B_SPLINE_SURFACE_WITH_KNOTS('',3,3,((#88875,#88876,#88877,#88878,
#88879),(#88880,#88881,#88882,#88883,#88884),(#88885,#88886,#88887,#88888,
#88889),(#88890,#88891,#88892,#88893,#88894),(#88895,#88896,#88897,#88898,
#88899)),.UNSPECIFIED.,.F.,.F.,.F.,(4,1,4),(4,1,4),(-0.00515447126046521,
0.571428571428571,1.00290951547842),(-0.00515447124447774,0.673198425769152,
1.5759507980487),.UNSPECIFIED.) ;
#2005 = B_SPLINE_SURFACE_WITH_KNOTS('',3,3,((#89000,#89001,#89002,#89003,
#89004,#89005,#89006,#89007,#89008,#89009,#89010,#89011,#89012),(#89013,
#89014,#89015,#89016,#89017,#89018,#89019,#89020,#89021,#89022,#89023,#89024,
#89025),(#89026,#89027,#89028,#89029,#89030,#89031,#89032,#89033,#89034,
#89035,#89036,#89037,#89038),(#89039,#89040,#89041,#89042,#89043,#89044,
#89045,#89046,#89047,#89048,#89049,#89050,#89051),(#89052,#89053,#89054,
#89055,#89056,#89057,#89058,#89059,#89060,#89061,#89062,#89063,#89064),
(#89065,#89066,#89067,#89068,#89069,#89070,#89071,#89072,#89073,#89074,
#89075,#89076,#89077)),.UNSPECIFIED.,.F.,.F.,.F.,(4,1,1,4),(4,1,1,1,1,1,
1,1,1,1,4),(0.,0.333333333333333,0.666666666666667,1.),(0.,0.1,0.2,0.3,
0.4,0.5,0.6,0.7,0.8,0.9,1.),.UNSPECIFIED.) ;
#2006 = B_SPLINE_SURFACE_WITH_KNOTS('',3,3,((#89166,#89167,#89168,#89169,
#89170,#89171),(#89172,#89173,#89174,#89175,#89176,#89177),(#89178,#89179,
#89180,#89181,#89182,#89183),(#89184,#89185,#89186,#89187,#89188,#89189),
(#89190,#89191,#89192,#89193,#89194,#89195),(#89196,#89197,#89198,#89199,
#89200,#89201),(#89202,#89203,#89204,#89205,#89206,#89207),(#89208,#89209,
#89210,#89211,#89212,#89213),(#89214,#89215,#89216,#89217,#89218,#89219),
(#89220,#89221,#89222,#89223,#89224,#89225),(#89226,#89227,#89228,#89229,
#89230,#89231),(#89232,#89233,#89234,#89235,#89236,#89237),(#89238,#89239,
#89240,#89241,#89242,#89243)),.UNSPECIFIED.,.F.,.F.,.F.,(4,1,1,1,1,1,1,
1,1,1,4),(4,1,1,4),(0.,0.1,0.2,0.3,0.4,0.5,0.6,0.7,0.8,0.9,1.),(0.,0.333333333333333,
0.666666666666667,1.),.UNSPECIFIED.) ;
#2007 = B_SPLINE_SURFACE_WITH_KNOTS('',3,3,((#89327,#89328,#89329,#89330,
#89331,#89332,#89333,#89334,#89335,#89336,#89337,#89338,#89339),(#89340,
#89341,#89342,#89343,#89344,#89345,#89346,#89347,#89348,#89349,#89350,#89351,
#89352),(#89353,#89354,#89355,#89356,#89357,#89358,#89359,#89360,#89361,
#89362,#89363,#89364,#89365),(#89366,#89367,#89368,#89369,#89370,#89371,
#89372,#89373,#89374,#89375,#89376,#89377,#89378),(#89379,#89380,#89381,
#89382,#89383,#89384,#89385,#89386,#89387,#89388,#89389,#89390,#89391),
(#89392,#89393,#89394,#89395,#89396,#89397,#89398,#89399,#89400,#89401,
#89402,#89403,#89404)),.UNSPECIFIED.,.F.,.F.,.F.,(4,1,1,4),(4,1,1,1,1,1,
1,1,1,1,4),(0.,0.333333333333333,0.666666666666667,1.),(0.,0.1,0.2,0.3,
0.4,0.5,0.6,0.7,0.8,0.9,1.),.UNSPECIFIED.) ;
#2008 = B_SPLINE_SURFACE_WITH_KNOTS('',3,3,((#89558,#89559,#89560,#89561,
#89562,#89563),(#89564,#89565,#89566,#89567,#89568,#89569),(#89570,#89571,
#89572,#89573,#89574,#89575),(#89576,#89577,#89578,#89579,#89580,#89581),
(#89582,#89583,#89584,#89585,#89586,#89587),(#89588,#89589,#89590,#89591,
#89592,#89593),(#89594,#89595,#89596,#89597,#89598,#89599),(#89600,#89601,
#89602,#89603,#89604,#89605),(#89606,#89607,#89608,#89609,#89610,#89611),
(#89612,#89613,#89614,#89615,#89616,#89617),(#89618,#89619,#89620,#89621,
#89622,#89623)),.UNSPECIFIED.,.F.,.F.,.F.,(4,1,1,1,1,1,1,1,4),(4,1,1,4),
(0.,0.125,0.25,0.375,0.5,0.625,0.75,0.875,1.),(0.,0.333333333333333,0.666666666666667,
1.),.UNSPECIFIED.) ;
#2009 = B_SPLINE_SURFACE_WITH_KNOTS('',3,3,((#89738,#89739,#89740,#89741,
#89742,#89743,#89744,#89745,#89746,#89747,#89748),(#89749,#89750,#89751,
#89752,#89753,#89754,#89755,#89756,#89757,#89758,#89759),(#89760,#89761,
#89762,#89763,#89764,#89765,#89766,#89767,#89768,#89769,#89770),(#89771,
#89772,#89773,#89774,#89775,#89776,#89777,#89778,#89779,#89780,#89781),
(#89782,#89783,#89784,#89785,#89786,#89787,#89788,#89789,#89790,#89791,
#89792),(#89793,#89794,#89795,#89796,#89797,#89798,#89799,#89800,#89801,
#89802,#89803)),.UNSPECIFIED.,.F.,.F.,.F.,(4,1,1,4),(4,1,1,1,1,1,1,1,4),
(0.,0.333333333333333,0.666666666666667,1.),(0.,0.125,0.25,0.375,0.5,0.625,
0.75,0.875,1.),.UNSPECIFIED.) ;
#2010 = B_SPLINE_SURFACE_WITH_KNOTS('',3,1,((#89883,#89884),(#89885,#89886),
(#89887,#89888),(#89889,#89890),(#89891,#89892)),.UNSPECIFIED.,.F.,.F.,
 .F.,(4,1,4),(2,2),(0.,0.0298071351389365,0.0685496713495228),(0.,0.0359999999999998),
 .UNSPECIFIED.) ;
#2011 = B_SPLINE_SURFACE_WITH_KNOTS('',3,1,((#89906,#89907),(#89908,#89909),
(#89910,#89911),(#89912,#89913),(#89914,#89915)),.UNSPECIFIED.,.F.,.F.,
 .F.,(4,1,4),(2,2),(0.,0.0263673128827931,0.0523427870633456),(0.,0.0359999999999998),
 .UNSPECIFIED.) ;
#2012 = B_SPLINE_SURFACE_WITH_KNOTS('',3,1,((#89929,#89930),(#89931,#89932),
(#89933,#89934),(#89935,#89936),(#89937,#89938)),.UNSPECIFIED.,.F.,.F.,
 .F.,(4,1,4),(2,2),(0.,0.0190758281807941,0.0379545209982657),(0.,0.0359999999999998),
 .UNSPECIFIED.) ;
#2013 = B_SPLINE_SURFACE_WITH_KNOTS('',3,1,((#89952,#89953),(#89954,#89955),
(#89956,#89957),(#89958,#89959),(#89960,#89961)),.UNSPECIFIED.,.F.,.F.,
 .F.,(4,1,4),(2,2),(0.,0.0205128997765721,0.0398218276255599),(0.,0.0359999999999998),
 .UNSPECIFIED.) ;
#2014 = B_SPLINE_SURFACE_WITH_KNOTS('',3,1,((#89975,#89976),(#89977,#89978),
(#89979,#89980),(#89981,#89982),(#89983,#89984)),.UNSPECIFIED.,.F.,.F.,
 .F.,(4,1,4),(2,2),(0.,0.0323852950215525,0.0574227556854303),(0.,0.0359999999999998),
 .UNSPECIFIED.) ;
#2015 = B_SPLINE_SURFACE_WITH_KNOTS('',3,1,((#90022,#90023),(#90024,#90025),
(#90026,#90027),(#90028,#90029),(#90030,#90031)),.UNSPECIFIED.,.F.,.F.,
 .F.,(4,1,4),(2,2),(0.,0.011955158932918,0.0295605475166918),(0.,0.0359999999999998),
 .UNSPECIFIED.) ;
#2016 = B_SPLINE_SURFACE_WITH_KNOTS('',3,1,((#90045,#90046),(#90047,#90048),
(#90049,#90050),(#90051,#90052),(#90053,#90054)),.UNSPECIFIED.,.F.,.F.,
 .F.,(4,1,4),(2,2),(0.,0.0135228484064754,0.0263579081616444),(0.,0.0359999999999998),
 .UNSPECIFIED.) ;
#2017 = B_SPLINE_SURFACE_WITH_KNOTS('',3,1,((#90068,#90069),(#90070,#90071),
(#90072,#90073),(#90074,#90075),(#90076,#90077)),.UNSPECIFIED.,.F.,.F.,
 .F.,(4,1,4),(2,2),(0.,0.0216058216755205,0.0381303842659523),(0.,0.0359999999999998),
 .UNSPECIFIED.) ;
#2018 = B_SPLINE_SURFACE_WITH_KNOTS('',3,1,((#90091,#90092),(#90093,#90094),
(#90095,#90096),(#90097,#90098),(#90099,#90100)),.UNSPECIFIED.,.F.,.F.,
 .F.,(4,1,4),(2,2),(0.,0.0381782469542568,0.0670753371474822),(0.,0.0359999999999998),
 .UNSPECIFIED.) ;
#2019 = B_SPLINE_SURFACE_WITH_KNOTS('',3,1,((#90132,#90133),(#90134,#90135),
(#90136,#90137),(#90138,#90139),(#90140,#90141)),.UNSPECIFIED.,.F.,.F.,
 .F.,(4,1,4),(2,2),(0.,0.0329095469988702,0.0691336974954879),(0.,0.0359999999999998),
 .UNSPECIFIED.) ;
#2020 = B_SPLINE_SURFACE_WITH_KNOTS('',3,1,((#90155,#90156),(#90157,#90158),
(#90159,#90160),(#90161,#90162),(#90163,#90164)),.UNSPECIFIED.,.F.,.F.,
 .F.,(4,1,4),(2,2),(0.,0.0210301296927785,0.0377156586265697),(0.,0.0359999999999998),
 .UNSPECIFIED.) ;
#2021 = B_SPLINE_SURFACE_WITH_KNOTS('',3,1,((#90178,#90179),(#90180,#90181),
(#90182,#90183),(#90184,#90185),(#90186,#90187)),.UNSPECIFIED.,.F.,.F.,
 .F.,(4,1,4),(2,2),(0.,0.0424180496051088,0.0942055476140892),(0.,0.0359999999999998),
 .UNSPECIFIED.) ;
#2022 = B_SPLINE_SURFACE_WITH_KNOTS('',3,1,((#90201,#90202),(#90203,#90204),
(#90205,#90206),(#90207,#90208),(#90209,#90210)),.UNSPECIFIED.,.F.,.F.,
 .F.,(4,1,4),(2,2),(0.,0.0398228695438388,0.0783699334705556),(0.,0.0359999999999998),
 .UNSPECIFIED.) ;
#2023 = B_SPLINE_SURFACE_WITH_KNOTS('',3,1,((#90224,#90225),(#90226,#90227),
(#90228,#90229),(#90230,#90231),(#90232,#90233)),.UNSPECIFIED.,.F.,.F.,
 .F.,(4,1,4),(2,2),(0.,0.0313133324080373,0.063168759987351),(0.,0.0359999999999998),
 .UNSPECIFIED.) ;
#2024 = B_SPLINE_SURFACE_WITH_KNOTS('',3,1,((#90247,#90248),(#90249,#90250),
(#90251,#90252),(#90253,#90254),(#90255,#90256)),.UNSPECIFIED.,.F.,.F.,
 .F.,(4,1,4),(2,2),(0.,0.0290828541577381,0.0592932101613289),(0.,0.0359999999999998),
 .UNSPECIFIED.) ;
#2025 = B_SPLINE_SURFACE_WITH_KNOTS('',3,1,((#90270,#90271),(#90272,#90273),
(#90274,#90275),(#90276,#90277),(#90278,#90279)),.UNSPECIFIED.,.F.,.F.,
 .F.,(4,1,4),(2,2),(0.,0.0471458586470647,0.0823534588635132),(0.,0.0359999999999998),
 .UNSPECIFIED.) ;
#2026 = B_SPLINE_SURFACE_WITH_KNOTS('',3,1,((#90354,#90355),(#90356,#90357),
(#90358,#90359),(#90360,#90361)),.UNSPECIFIED.,.F.,.F.,.F.,(4,4),(2,2),
(0.,1.),(0.,0.456),.UNSPECIFIED.) ;
#2027 = B_SPLINE_SURFACE_WITH_KNOTS('',3,1,((#90370,#90371),(#90372,#90373),
(#90374,#90375),(#90376,#90377),(#90378,#90379),(#90380,#90381)),
 .UNSPECIFIED.,.F.,.F.,.F.,(4,2,4),(2,2),(-0.0699558285734109,-0.0581995466601206,
-0.0505532240038533),(0.,1.14),.UNSPECIFIED.) ;
#2028 = B_SPLINE_SURFACE_WITH_KNOTS('',3,3,((#90444,#90445,#90446,#90447),
(#90448,#90449,#90450,#90451),(#90452,#90453,#90454,#90455),(#90456,#90457,
#90458,#90459),(#90460,#90461,#90462,#90463)),.UNSPECIFIED.,.F.,.F.,.F.,
(4,1,4),(4,4),(0.,0.5,1.),(-0.156907118032788,-0.139899380964935),
 .UNSPECIFIED.) ;
#2029 = B_SPLINE_SURFACE_WITH_KNOTS('',3,3,((#90525,#90526,#90527,#90528,
#90529),(#90530,#90531,#90532,#90533,#90534),(#90535,#90536,#90537,#90538,
#90539),(#90540,#90541,#90542,#90543,#90544),(#90545,#90546,#90547,#90548,
#90549)),.UNSPECIFIED.,.F.,.F.,.F.,(4,1,4),(4,1,4),(0.,0.5,1.00016791794751),
(4.71222106243701,5.16843353557162,5.77649294248775),.UNSPECIFIED.) ;
#2030 = B_SPLINE_SURFACE_WITH_KNOTS('',3,3,((#90642,#90643,#90644,#90645,
#90646,#90647,#90648,#90649,#90650,#90651,#90652),(#90653,#90654,#90655,
#90656,#90657,#90658,#90659,#90660,#90661,#90662,#90663),(#90664,#90665,
#90666,#90667,#90668,#90669,#90670,#90671,#90672,#90673,#90674),(#90675,
#90676,#90677,#90678,#90679,#90680,#90681,#90682,#90683,#90684,#90685),
(#90686,#90687,#90688,#90689,#90690,#90691,#90692,#90693,#90694,#90695,
#90696),(#90697,#90698,#90699,#90700,#90701,#90702,#90703,#90704,#90705,
#90706,#90707)),.UNSPECIFIED.,.F.,.F.,.F.,(4,1,1,4),(4,1,1,1,1,1,1,1,4),
(0.,0.285714285714286,0.571428571428571,1.55420651718688),(0.000383464105853098,
0.0268242176912658,0.0532649712766785,0.073095536465738,0.0797057248620911,
0.0863159132584443,0.0896210074566209,0.0912735545557092,0.0929261016547975),
 .UNSPECIFIED.) ;
#2031 = B_SPLINE_SURFACE_WITH_KNOTS('',3,3,((#90799,#90800,#90801,#90802,
#90803),(#90804,#90805,#90806,#90807,#90808),(#90809,#90810,#90811,#90812,
#90813),(#90814,#90815,#90816,#90817,#90818),(#90819,#90820,#90821,#90822,
#90823)),.UNSPECIFIED.,.F.,.F.,.F.,(4,1,4),(4,1,4),(-0.000290474503729989,
0.5,1.00029047450393),(-0.000290474503928144,0.897597901025654,1.5707963267949),
 .UNSPECIFIED.) ;
#2032 = B_SPLINE_SURFACE_WITH_KNOTS('',3,3,((#90840,#90841,#90842,#90843),
(#90844,#90845,#90846,#90847),(#90848,#90849,#90850,#90851),(#90852,#90853,
#90854,#90855),(#90856,#90857,#90858,#90859)),.UNSPECIFIED.,.F.,.F.,.F.,
(4,1,4),(4,4),(-0.000506016721647412,0.5,1.),(-5.54544584248221,-4.71188296366304),
 .UNSPECIFIED.) ;
#2033 = B_SPLINE_SURFACE_WITH_KNOTS('',3,3,((#90865,#90866,#90867,#90868,
#90869,#90870),(#90871,#90872,#90873,#90874,#90875,#90876),(#90877,#90878,
#90879,#90880,#90881,#90882),(#90883,#90884,#90885,#90886,#90887,#90888)),
 .UNSPECIFIED.,.F.,.F.,.F.,(4,4),(4,2,4),(0.,1.),(0.,0.0518624644373431,
0.0522283064773341),.UNSPECIFIED.) ;
#2034 = B_SPLINE_SURFACE_WITH_KNOTS('',3,3,((#90918,#90919,#90920,#90921,
#90922),(#90923,#90924,#90925,#90926,#90927),(#90928,#90929,#90930,#90931,
#90932),(#90933,#90934,#90935,#90936,#90937),(#90938,#90939,#90940,#90941,
#90942)),.UNSPECIFIED.,.F.,.F.,.F.,(4,1,4),(4,1,4),(-0.000419225650178164,
0.5,1.00041922565031),(-1.5707963267949,-0.67319842576924,0.0004192256503168),
 .UNSPECIFIED.) ;
#2035 = B_SPLINE_SURFACE_WITH_KNOTS('',3,3,((#90959,#90960,#90961,#90962),
(#90963,#90964,#90965,#90966),(#90967,#90968,#90969,#90970),(#90971,#90972,
#90973,#90974),(#90975,#90976,#90977,#90978)),.UNSPECIFIED.,.F.,.F.,.F.,
(4,1,4),(4,4),(-0.000506016735097035,0.5,1.),(-1.57130234353,-0.737739464683826),
 .UNSPECIFIED.) ;
#2036 = B_SPLINE_SURFACE_WITH_KNOTS('',3,3,((#90984,#90985,#90986,#90987,
#90988,#90989),(#90990,#90991,#90992,#90993,#90994,#90995),(#90996,#90997,
#90998,#90999,#91000,#91001),(#91002,#91003,#91004,#91005,#91006,#91007)),
 .UNSPECIFIED.,.F.,.F.,.F.,(4,4),(4,2,4),(0.,1.),(-0.000365842040355155,
0.,0.051862464436985),.UNSPECIFIED.) ;
#2037 = B_SPLINE_SURFACE_WITH_KNOTS('',3,3,((#91063,#91064,#91065,#91066),
(#91067,#91068,#91069,#91070),(#91071,#91072,#91073,#91074),(#91075,#91076,
#91077,#91078),(#91079,#91080,#91081,#91082)),.UNSPECIFIED.,.F.,.F.,.F.,
(4,1,4),(4,4),(-0.0189222038896959,0.571428571428571,1.01886279511128),
(-0.0189222038896219,1.5707963267949),.UNSPECIFIED.) ;
#2038 = B_SPLINE_SURFACE_WITH_KNOTS('',3,3,((#91155,#91156,#91157,#91158,
#91159),(#91160,#91161,#91162,#91163,#91164),(#91165,#91166,#91167,#91168,
#91169),(#91170,#91171,#91172,#91173,#91174),(#91175,#91176,#91177,#91178,
#91179)),.UNSPECIFIED.,.F.,.F.,.F.,(4,1,4),(4,1,4),(0.,0.5,1.00066906930274),
(-0.000669069302958659,0.785398163397612,1.57146539609819),
 .UNSPECIFIED.) ;
#2039 = B_SPLINE_SURFACE_WITH_KNOTS('',3,3,((#91445,#91446,#91447,#91448,
#91449,#91450),(#91451,#91452,#91453,#91454,#91455,#91456),(#91457,#91458,
#91459,#91460,#91461,#91462),(#91463,#91464,#91465,#91466,#91467,#91468),
(#91469,#91470,#91471,#91472,#91473,#91474),(#91475,#91476,#91477,#91478,
#91479,#91480),(#91481,#91482,#91483,#91484,#91485,#91486)),
 .UNSPECIFIED.,.F.,.F.,.F.,(4,1,1,1,4),(4,1,1,4),(0.,0.285714285714286,
0.5,0.785714285714286,1.),(0.148883906684682,0.156528869066089,0.166722152241299,
0.184560397797916),.UNSPECIFIED.) ;
#2040 = B_SPLINE_SURFACE_WITH_KNOTS('',3,3,((#91524,#91525,#91526,#91527,
#91528,#91529),(#91530,#91531,#91532,#91533,#91534,#91535),(#91536,#91537,
#91538,#91539,#91540,#91541),(#91542,#91543,#91544,#91545,#91546,#91547),
(#91548,#91549,#91550,#91551,#91552,#91553)),.UNSPECIFIED.,.F.,.F.,.F.,
(4,1,4),(4,2,4),(0.,0.571428571428571,1.),(-0.0663145530984604,0.,0.000424263177439857),
 .UNSPECIFIED.) ;
#2041 = B_SPLINE_SURFACE_WITH_KNOTS('',3,3,((#91596,#91597,#91598,#91599),
(#91600,#91601,#91602,#91603),(#91604,#91605,#91606,#91607),(#91608,#91609,
#91610,#91611),(#91612,#91613,#91614,#91615)),.UNSPECIFIED.,.F.,.F.,.F.,
(4,1,4),(4,4),(0.,0.571428571428571,1.),(0.,0.0254449718282482),
 .UNSPECIFIED.) ;
#2042 = B_SPLINE_SURFACE_WITH_KNOTS('',3,3,((#91627,#91628,#91629,#91630),
(#91631,#91632,#91633,#91634),(#91635,#91636,#91637,#91638),(#91639,#91640,
#91641,#91642),(#91643,#91644,#91645,#91646)),.UNSPECIFIED.,.F.,.F.,.F.,
(4,1,4),(4,4),(-0.00104348049004246,0.571428571428571,1.),(0.861856499795871,
1.57183980728496),.UNSPECIFIED.) ;
#2043 = B_SPLINE_SURFACE_WITH_KNOTS('',3,3,((#91658,#91659,#91660,#91661,
#91662),(#91663,#91664,#91665,#91666,#91667),(#91668,#91669,#91670,#91671,
#91672),(#91673,#91674,#91675,#91676,#91677),(#91678,#91679,#91680,#91681,
#91682)),.UNSPECIFIED.,.F.,.F.,.F.,(4,1,4),(4,1,4),(-0.000590521380405756,
0.571428571428571,1.),(-1.57138684817531,-1.12581647705762,-0.531919489361454),
 .UNSPECIFIED.) ;
#2044 = B_SPLINE_SURFACE_WITH_KNOTS('',3,3,((#91765,#91766,#91767,#91768,
#91769,#91770),(#91771,#91772,#91773,#91774,#91775,#91776),(#91777,#91778,
#91779,#91780,#91781,#91782),(#91783,#91784,#91785,#91786,#91787,#91788)),
 .UNSPECIFIED.,.F.,.F.,.F.,(4,4),(4,2,4),(-0.000170891015070361,1.),(-0.0300731157523127,
-0.0299720828361244,0.000170254829587993),.UNSPECIFIED.) ;
#2045 = B_SPLINE_SURFACE_WITH_KNOTS('',3,3,((#91831,#91832,#91833,#91834),
(#91835,#91836,#91837,#91838),(#91839,#91840,#91841,#91842),(#91843,#91844,
#91845,#91846),(#91847,#91848,#91849,#91850)),.UNSPECIFIED.,.F.,.F.,.F.,
(4,1,4),(4,4),(0.,0.571428571428571,1.),(1.13982531580781,1.57079632679494),
 .UNSPECIFIED.) ;
#2046 = B_SPLINE_SURFACE_WITH_KNOTS('',3,3,((#91862,#91863,#91864,#91865),
(#91866,#91867,#91868,#91869),(#91870,#91871,#91872,#91873),(#91874,#91875,
#91876,#91877),(#91878,#91879,#91880,#91881)),.UNSPECIFIED.,.F.,.F.,.F.,
(4,1,4),(4,4),(0.,0.571428571428571,1.0003523080326),(-1.57114863482751,
-0.92694290996995),.UNSPECIFIED.) ;
#2047 = B_SPLINE_SURFACE_WITH_KNOTS('',3,3,((#91887,#91888,#91889,#91890),
(#91891,#91892,#91893,#91894),(#91895,#91896,#91897,#91898),(#91899,#91900,
#91901,#91902),(#91903,#91904,#91905,#91906)),.UNSPECIFIED.,.F.,.F.,.F.,
(4,1,4),(4,4),(0.,0.571428571428571,1.),(4.14247343901052E-16,0.0173725716234068),
 .UNSPECIFIED.) ;
#2048 = B_SPLINE_SURFACE_WITH_KNOTS('',3,3,((#91912,#91913,#91914,#91915),
(#91916,#91917,#91918,#91919),(#91920,#91921,#91922,#91923),(#91924,#91925,
#91926,#91927)),.UNSPECIFIED.,.F.,.F.,.F.,(4,4),(4,4),(0.,1.00246533549981),
(-0.64596644429237,0.00246533549982144),.UNSPECIFIED.) ;
#2049 = B_SPLINE_SURFACE_WITH_KNOTS('',3,3,((#92031,#92032,#92033,#92034),
(#92035,#92036,#92037,#92038),(#92039,#92040,#92041,#92042),(#92043,#92044,
#92045,#92046),(#92047,#92048,#92049,#92050)),.UNSPECIFIED.,.F.,.F.,.F.,
(4,1,4),(4,4),(0.,0.571428571428571,1.),(-1.57079632679486,1.0162123752053E-13),
 .UNSPECIFIED.) ;
#2050 = B_SPLINE_SURFACE_WITH_KNOTS('',3,3,((#92500,#92501,#92502,#92503,
#92504,#92505,#92506,#92507),(#92508,#92509,#92510,#92511,#92512,#92513,
#92514,#92515),(#92516,#92517,#92518,#92519,#92520,#92521,#92522,#92523),
(#92524,#92525,#92526,#92527,#92528,#92529,#92530,#92531),(#92532,#92533,
#92534,#92535,#92536,#92537,#92538,#92539),(#92540,#92541,#92542,#92543,
#92544,#92545,#92546,#92547),(#92548,#92549,#92550,#92551,#92552,#92553,
#92554,#92555)),.UNSPECIFIED.,.F.,.F.,.F.,(4,1,1,1,4),(4,1,1,1,1,4),(0.,
0.285714285714286,0.5,0.785714285714286,1.),(9.19824141439016E-31,0.00572297095011093,
0.0114459419002219,0.0171689128503328,0.0286148547505547,0.0400607966507765),
 .UNSPECIFIED.) ;
#2051 = B_SPLINE_SURFACE_WITH_KNOTS('',3,3,((#92697,#92698,#92699,#92700,
#92701,#92702,#92703),(#92704,#92705,#92706,#92707,#92708,#92709,#92710),
(#92711,#92712,#92713,#92714,#92715,#92716,#92717),(#92718,#92719,#92720,
#92721,#92722,#92723,#92724),(#92725,#92726,#92727,#92728,#92729,#92730,
#92731),(#92732,#92733,#92734,#92735,#92736,#92737,#92738),(#92739,#92740,
#92741,#92742,#92743,#92744,#92745)),.UNSPECIFIED.,.F.,.F.,.F.,(4,1,1,1,
4),(4,1,1,1,4),(0.,0.285714285714286,0.5,0.785714285714286,1.),(-8.67361737988406E-17,
0.224399475256413,0.448798950512826,0.897597901025653,1.57079632679489),
 .UNSPECIFIED.) ;
#2052 = B_SPLINE_SURFACE_WITH_KNOTS('',3,3,((#92902,#92903,#92904,#92905,
#92906,#92907),(#92908,#92909,#92910,#92911,#92912,#92913),(#92914,#92915,
#92916,#92917,#92918,#92919),(#92920,#92921,#92922,#92923,#92924,#92925),
(#92926,#92927,#92928,#92929,#92930,#92931)),.UNSPECIFIED.,.F.,.F.,.F.,
(4,1,4),(4,1,1,4),(0.,0.571428571428571,1.),(8.270742692011E-19,0.0162039536314463,
0.0231485051877804,0.0324079072628925),.UNSPECIFIED.) ;
#2053 = B_SPLINE_SURFACE_WITH_KNOTS('',3,3,((#93002,#93003,#93004,#93005,
#93006,#93007),(#93008,#93009,#93010,#93011,#93012,#93013),(#93014,#93015,
#93016,#93017,#93018,#93019),(#93020,#93021,#93022,#93023,#93024,#93025),
(#93026,#93027,#93028,#93029,#93030,#93031)),.UNSPECIFIED.,.F.,.F.,.F.,
(4,1,4),(4,1,1,4),(0.,0.571428571428571,1.),(0.,0.00925932038092611,0.0162038106666207,
0.0324076213332414),.UNSPECIFIED.) ;
#2054 = B_SPLINE_SURFACE_WITH_KNOTS('',3,3,((#93084,#93085,#93086,#93087,
#93088),(#93089,#93090,#93091,#93092,#93093),(#93094,#93095,#93096,#93097,
#93098),(#93099,#93100,#93101,#93102,#93103),(#93104,#93105,#93106,#93107,
#93108)),.UNSPECIFIED.,.F.,.F.,.F.,(4,1,4),(4,1,4),(0.,0.571428571428571,
1.),(0.,0.0126399602240726,0.0294932405228361),.UNSPECIFIED.) ;
#2055 = B_SPLINE_SURFACE_WITH_KNOTS('',3,3,((#93121,#93122,#93123,#93124),
(#93125,#93126,#93127,#93128),(#93129,#93130,#93131,#93132),(#93133,#93134,
#93135,#93136),(#93137,#93138,#93139,#93140)),.UNSPECIFIED.,.F.,.F.,.F.,
(4,1,4),(4,4),(-0.00114393799377549,0.571428571428571,1.),(0.914253278585075,
1.57194026478868),.UNSPECIFIED.) ;
#2056 = B_SPLINE_SURFACE_WITH_KNOTS('',3,3,((#93229,#93230,#93231,#93232,
#93233),(#93234,#93235,#93236,#93237,#93238),(#93239,#93240,#93241,#93242,
#93243),(#93244,#93245,#93246,#93247,#93248),(#93249,#93250,#93251,#93252,
#93253)),.UNSPECIFIED.,.F.,.F.,.F.,(4,1,4),(4,1,4),(0.,0.571428571428571,
1.),(0.,0.0168532803128275,0.0294932405474481),.UNSPECIFIED.) ;
#2057 = B_SPLINE_SURFACE_WITH_KNOTS('',3,3,((#93266,#93267,#93268,#93269),
(#93270,#93271,#93272,#93273),(#93274,#93275,#93276,#93277),(#93278,#93279,
#93280,#93281),(#93282,#93283,#93284,#93285)),.UNSPECIFIED.,.F.,.F.,.F.,
(4,1,4),(4,4),(-0.00114393799175905,0.571428571428571,1.),(-1.57194026478668,
-0.914253278587085),.UNSPECIFIED.) ;
#2058 = B_SPLINE_SURFACE_WITH_KNOTS('',3,3,((#93481,#93482,#93483,#93484,
#93485),(#93486,#93487,#93488,#93489,#93490),(#93491,#93492,#93493,#93494,
#93495),(#93496,#93497,#93498,#93499,#93500),(#93501,#93502,#93503,#93504,
#93505),(#93506,#93507,#93508,#93509,#93510),(#93511,#93512,#93513,#93514,
#93515)),.UNSPECIFIED.,.F.,.F.,.F.,(4,1,1,1,4),(4,1,4),(-0.000276284474482355,
0.285714285714286,0.5,0.785714285714286,1.00025438918361),(0.67448655303988,
1.05876467846844,1.57107261127047),.UNSPECIFIED.) ;
#2059 = B_SPLINE_SURFACE_WITH_KNOTS('',3,3,((#93561,#93562,#93563,#93564),
(#93565,#93566,#93567,#93568),(#93569,#93570,#93571,#93572),(#93573,#93574,
#93575,#93576),(#93577,#93578,#93579,#93580),(#93581,#93582,#93583,#93584)),
 .UNSPECIFIED.,.F.,.F.,.F.,(4,1,1,4),(4,4),(-0.000163798824285399,0.285714285714286,
0.571428571428571,1.00148567620286),(-1.57228200299773,-0.871178949794101),
 .UNSPECIFIED.) ;
#2060 = B_SPLINE_SURFACE_WITH_KNOTS('',3,3,((#93592,#93593,#93594,#93595),
(#93596,#93597,#93598,#93599),(#93600,#93601,#93602,#93603),(#93604,#93605,
#93606,#93607),(#93608,#93609,#93610,#93611),(#93612,#93613,#93614,#93615),
(#93616,#93617,#93618,#93619)),.UNSPECIFIED.,.F.,.F.,.F.,(4,1,1,1,4),(4,
4),(-0.000162614260257949,0.285714285714286,0.5,0.714285714285714,1.0005808683447),
(-0.873245494341663,-0.0772155251815629),.UNSPECIFIED.) ;
#2061 = B_SPLINE_SURFACE_WITH_KNOTS('',3,3,((#93623,#93624,#93625,#93626),
(#93627,#93628,#93629,#93630),(#93631,#93632,#93633,#93634),(#93635,#93636,
#93637,#93638),(#93639,#93640,#93641,#93642),(#93643,#93644,#93645,#93646),
(#93647,#93648,#93649,#93650)),.UNSPECIFIED.,.F.,.F.,.F.,(4,1,1,1,4),(4,
4),(0.,0.285714285714286,0.5,0.714285714285714,1.),(0.0777963935263006,
0.648820263581669),.UNSPECIFIED.) ;
#2062 = B_SPLINE_SURFACE_WITH_KNOTS('',3,3,((#93654,#93655,#93656,#93657),
(#93658,#93659,#93660,#93661),(#93662,#93663,#93664,#93665),(#93666,#93667,
#93668,#93669),(#93670,#93671,#93672,#93673),(#93674,#93675,#93676,#93677)),
 .UNSPECIFIED.,.F.,.F.,.F.,(4,1,1,4),(4,4),(0.,0.285714285714286,0.571428571428571,
1.),(2.15310365171961E-15,0.0294983491188769),.UNSPECIFIED.) ;
#2063 = B_SPLINE_SURFACE_WITH_KNOTS('',3,3,((#93937,#93938,#93939,#93940,
#93941,#93942),(#93943,#93944,#93945,#93946,#93947,#93948),(#93949,#93950,
#93951,#93952,#93953,#93954),(#93955,#93956,#93957,#93958,#93959,#93960),
(#93961,#93962,#93963,#93964,#93965,#93966)),.UNSPECIFIED.,.F.,.F.,.F.,
(4,1,4),(4,1,1,4),(-0.00069658220300701,0.571428571428571,1.),(-0.00069658220300276,
0.673198425769244,1.12199737628207,1.57149290899785),.UNSPECIFIED.) ;
#2064 = B_SPLINE_SURFACE_WITH_KNOTS('',3,3,((#93975,#93976,#93977,#93978,
#93979,#93980),(#93981,#93982,#93983,#93984,#93985,#93986),(#93987,#93988,
#93989,#93990,#93991,#93992),(#93993,#93994,#93995,#93996,#93997,#93998),
(#93999,#94000,#94001,#94002,#94003,#94004)),.UNSPECIFIED.,.F.,.F.,.F.,
(4,1,4),(4,1,1,4),(-0.00069647979888005,0.571428571428571,1.),(-1.57149280659377,
-1.12199737628207,-0.673198425769238,0.000696479798882929),
 .UNSPECIFIED.) ;
#2065 = B_SPLINE_SURFACE_WITH_KNOTS('',3,3,((#94019,#94020,#94021,#94022,
#94023),(#94024,#94025,#94026,#94027,#94028),(#94029,#94030,#94031,#94032,
#94033),(#94034,#94035,#94036,#94037,#94038),(#94039,#94040,#94041,#94042,
#94043)),.UNSPECIFIED.,.F.,.F.,.F.,(4,1,4),(4,1,4),(-0.00194122259541691,
0.571428571428571,1.),(-0.00194122259541691,0.0195634159024299,0.0475891930344199),
 .UNSPECIFIED.) ;
#2066 = B_SPLINE_SURFACE_WITH_KNOTS('',3,3,((#94109,#94110,#94111,#94112),
(#94113,#94114,#94115,#94116),(#94117,#94118,#94119,#94120),(#94121,#94122,
#94123,#94124),(#94125,#94126,#94127,#94128)),.UNSPECIFIED.,.F.,.F.,.F.,
(4,1,4),(4,4),(-0.00567875718055857,0.571428571428571,1.),(0.562190624368961,
1.57647508397548),.UNSPECIFIED.) ;
#2067 = B_SPLINE_SURFACE_WITH_KNOTS('',3,3,((#94132,#94133,#94134,#94135),
(#94136,#94137,#94138,#94139),(#94140,#94141,#94142,#94143),(#94144,#94145,
#94146,#94147),(#94148,#94149,#94150,#94151)),.UNSPECIFIED.,.F.,.F.,.F.,
(4,1,4),(4,4),(0.,0.571428571428571,1.),(1.33431567541952E-15,0.0171168860941288),
 .UNSPECIFIED.) ;
#2068 = B_SPLINE_SURFACE_WITH_KNOTS('',3,3,((#94222,#94223,#94224,#94225),
(#94226,#94227,#94228,#94229),(#94230,#94231,#94232,#94233),(#94234,#94235,
#94236,#94237),(#94238,#94239,#94240,#94241)),.UNSPECIFIED.,.F.,.F.,.F.,
(4,1,4),(4,4),(0.,0.5,1.),(0.0461307304951755,0.109806780005479),
 .UNSPECIFIED.) ;
#2069 = B_SPLINE_SURFACE_WITH_KNOTS('',3,3,((#94251,#94252,#94253,#94254),
(#94255,#94256,#94257,#94258),(#94259,#94260,#94261,#94262),(#94263,#94264,
#94265,#94266),(#94267,#94268,#94269,#94270),(#94271,#94272,#94273,#94274),
(#94275,#94276,#94277,#94278)),.UNSPECIFIED.,.F.,.F.,.F.,(4,1,1,1,4),(4,
4),(0.,0.285714285714286,0.5,0.785714285714286,1.),(-2.1768822796151,-1.66773041364303),
 .UNSPECIFIED.) ;
#2070 = B_SPLINE_SURFACE_WITH_KNOTS('',3,3,((#94280,#94281,#94282,#94283,
#94284),(#94285,#94286,#94287,#94288,#94289),(#94290,#94291,#94292,#94293,
#94294),(#94295,#94296,#94297,#94298,#94299),(#94300,#94301,#94302,#94303,
#94304),(#94305,#94306,#94307,#94308,#94309),(#94310,#94311,#94312,#94313,
#94314)),.UNSPECIFIED.,.F.,.F.,.F.,(4,1,1,1,4),(4,1,4),(-0.000518096114479414,
0.285714285714286,0.5,0.785714285714286,1.),(-0.00050344375524984,0.0114772233155261,
0.0272982838507071),.UNSPECIFIED.) ;
#2071 = B_SPLINE_SURFACE_WITH_KNOTS('',3,3,((#94345,#94346,#94347,#94348),
(#94349,#94350,#94351,#94352),(#94353,#94354,#94355,#94356),(#94357,#94358,
#94359,#94360),(#94361,#94362,#94363,#94364),(#94365,#94366,#94367,#94368),
(#94369,#94370,#94371,#94372)),.UNSPECIFIED.,.F.,.F.,.F.,(4,1,1,1,4),(4,
4),(0.,0.285714285714286,0.5,0.785714285714286,1.),(-1.27744058344438,-1.20367640622073),
 .UNSPECIFIED.) ;
#2072 = B_SPLINE_SURFACE_WITH_KNOTS('',3,3,((#94376,#94377,#94378,#94379,
#94380),(#94381,#94382,#94383,#94384,#94385),(#94386,#94387,#94388,#94389,
#94390),(#94391,#94392,#94393,#94394,#94395),(#94396,#94397,#94398,#94399,
#94400),(#94401,#94402,#94403,#94404,#94405),(#94406,#94407,#94408,#94409,
#94410)),.UNSPECIFIED.,.F.,.F.,.F.,(4,1,1,1,4),(4,1,4),(0.,0.285714285714286,
0.5,0.785714285714286,1.),(0.0334571978979197,0.0595744748887569,0.0856917518795941),
 .UNSPECIFIED.) ;
#2073 = B_SPLINE_SURFACE_WITH_KNOTS('',3,3,((#94449,#94450,#94451,#94452),
(#94453,#94454,#94455,#94456),(#94457,#94458,#94459,#94460),(#94461,#94462,
#94463,#94464),(#94465,#94466,#94467,#94468),(#94469,#94470,#94471,#94472),
(#94473,#94474,#94475,#94476)),.UNSPECIFIED.,.F.,.F.,.F.,(4,1,1,1,4),(4,
4),(0.,0.285714285714286,0.5,0.785714285714286,1.),(-1.56238538892354,-0.785398163397404),
 .UNSPECIFIED.) ;
#2074 = B_SPLINE_SURFACE_WITH_KNOTS('',3,3,((#94487,#94488,#94489,#94490),
(#94491,#94492,#94493,#94494),(#94495,#94496,#94497,#94498),(#94499,#94500,
#94501,#94502),(#94503,#94504,#94505,#94506),(#94507,#94508,#94509,#94510),
(#94511,#94512,#94513,#94514)),.UNSPECIFIED.,.F.,.F.,.F.,(4,1,1,1,4),(4,
4),(-0.000154725634345458,0.285714285714286,0.5,0.785714285714286,1.00006609114655),
(-1.2305075083907,-0.785243437762843),.UNSPECIFIED.) ;
#2075 = B_SPLINE_SURFACE_WITH_KNOTS('',3,3,((#94519,#94520,#94521,#94522),
(#94523,#94524,#94525,#94526),(#94527,#94528,#94529,#94530),(#94531,#94532,
#94533,#94534),(#94535,#94536,#94537,#94538)),.UNSPECIFIED.,.F.,.F.,.F.,
(4,1,4),(4,4),(0.,0.5,1.),(1.2303527827561,1.54388796055314),
 .UNSPECIFIED.) ;
#2076 = B_SPLINE_SURFACE_WITH_KNOTS('',3,3,((#94635,#94636,#94637,#94638),
(#94639,#94640,#94641,#94642),(#94643,#94644,#94645,#94646),(#94647,#94648,
#94649,#94650)),.UNSPECIFIED.,.F.,.F.,.F.,(4,4),(4,4),(0.,1.),(-0.263885209381218,
-1.85090356762827E-14),.UNSPECIFIED.) ;
#2077 = B_SPLINE_SURFACE_WITH_KNOTS('',3,3,((#94651,#94652,#94653,#94654),
(#94655,#94656,#94657,#94658),(#94659,#94660,#94661,#94662),(#94663,#94664,
#94665,#94666)),.UNSPECIFIED.,.F.,.F.,.F.,(4,4),(4,4),(0.,1.00201261903925),
(-0.00201261903924553,0.787410782436316),.UNSPECIFIED.) ;
#2078 = B_SPLINE_SURFACE_WITH_KNOTS('',3,3,((#94688,#94689,#94690,#94691,
#94692,#94693,#94694,#94695,#94696),(#94697,#94698,#94699,#94700,#94701,
#94702,#94703,#94704,#94705),(#94706,#94707,#94708,#94709,#94710,#94711,
#94712,#94713,#94714),(#94715,#94716,#94717,#94718,#94719,#94720,#94721,
#94722,#94723),(#94724,#94725,#94726,#94727,#94728,#94729,#94730,#94731,
#94732)),.UNSPECIFIED.,.F.,.F.,.F.,(4,1,4),(4,1,1,1,1,1,4),(0.,0.5,1.),
(-0.0334031852475255,-0.0321676440171422,-0.0309321027867588,-0.0284610203259921,
-0.0161056080221584,-0.00869236063985824,0.00119196920320868),
 .UNSPECIFIED.) ;
#2079 = B_SPLINE_SURFACE_WITH_KNOTS('',3,3,((#94736,#94737,#94738,#94739,
#94740,#94741,#94742,#94743,#94744,#94745),(#94746,#94747,#94748,#94749,
#94750,#94751,#94752,#94753,#94754,#94755),(#94756,#94757,#94758,#94759,
#94760,#94761,#94762,#94763,#94764,#94765),(#94766,#94767,#94768,#94769,
#94770,#94771,#94772,#94773,#94774,#94775)),.UNSPECIFIED.,.F.,.F.,.F.,(4,
4),(4,1,1,1,1,1,1,4),(0.,1.00026349704058),(0.047946162077175,0.048285659180944,
0.048625156284713,0.0493041504922509,0.0506621389073269,0.0513411331148649,
0.0520201273224029,0.0577155780232905),.UNSPECIFIED.) ;
#2080 = B_SPLINE_SURFACE_WITH_KNOTS('',5,1,((#94850,#94851),(#94852,#94853),
(#94854,#94855),(#94856,#94857),(#94858,#94859),(#94860,#94861),(#94862,
#94863),(#94864,#94865),(#94866,#94867),(#94868,#94869),(#94870,#94871),
(#94872,#94873),(#94874,#94875),(#94876,#94877),(#94878,#94879)),
 .UNSPECIFIED.,.F.,.F.,.F.,(6,1,1,1,1,1,1,1,1,1,6),(2,2),(-1.,-0.9,-0.8,
-0.7,-0.6,-0.5,-0.4,-0.3,-0.2,-0.1,0.),(0.,0.7668),.UNSPECIFIED.) ;
#2081 = B_SPLINE_SURFACE_WITH_KNOTS('',3,3,((#94974,#94975,#94976,#94977,
#94978,#94979,#94980,#94981,#94982,#94983),(#94984,#94985,#94986,#94987,
#94988,#94989,#94990,#94991,#94992,#94993),(#94994,#94995,#94996,#94997,
#94998,#94999,#95000,#95001,#95002,#95003),(#95004,#95005,#95006,#95007,
#95008,#95009,#95010,#95011,#95012,#95013),(#95014,#95015,#95016,#95017,
#95018,#95019,#95020,#95021,#95022,#95023)),.UNSPECIFIED.,.F.,.F.,.F.,(4,
1,4),(4,1,1,1,1,1,1,4),(0.,0.571428571428571,1.),(-0.0100926828333812,0.0417412101282966,
0.0676581566091356,0.0935751030899745,0.106533576330394,0.119492049570813,
0.132450522811233,0.171325942532491),.UNSPECIFIED.) ;
#2082 = B_SPLINE_SURFACE_WITH_KNOTS('',3,3,((#95175,#95176,#95177,#95178,
#95179,#95180,#95181,#95182,#95183,#95184,#95185),(#95186,#95187,#95188,
#95189,#95190,#95191,#95192,#95193,#95194,#95195,#95196),(#95197,#95198,
#95199,#95200,#95201,#95202,#95203,#95204,#95205,#95206,#95207),(#95208,
#95209,#95210,#95211,#95212,#95213,#95214,#95215,#95216,#95217,#95218),
(#95219,#95220,#95221,#95222,#95223,#95224,#95225,#95226,#95227,#95228,
#95229)),.UNSPECIFIED.,.F.,.F.,.F.,(4,1,4),(4,1,1,1,1,1,1,1,4),(0.,0.571428571428571,
1.),(-1.38391897109284E-14,0.0292767744902657,0.0585535489805452,0.073191936225685,
0.0878303234708248,0.117107097961104,0.146383872451384,0.161022259696524,
0.204937421431943),.UNSPECIFIED.) ;
#2083 = B_SPLINE_SURFACE_WITH_KNOTS('',3,3,((#95302,#95303,#95304,#95305,
#95306,#95307,#95308,#95309,#95310,#95311,#95312,#95313,#95314,#95315,#95316,
#95317),(#95318,#95319,#95320,#95321,#95322,#95323,#95324,#95325,#95326,
#95327,#95328,#95329,#95330,#95331,#95332,#95333),(#95334,#95335,#95336,
#95337,#95338,#95339,#95340,#95341,#95342,#95343,#95344,#95345,#95346,#95347,
#95348,#95349),(#95350,#95351,#95352,#95353,#95354,#95355,#95356,#95357,
#95358,#95359,#95360,#95361,#95362,#95363,#95364,#95365),(#95366,#95367,
#95368,#95369,#95370,#95371,#95372,#95373,#95374,#95375,#95376,#95377,#95378,
#95379,#95380,#95381)),.UNSPECIFIED.,.F.,.F.,.F.,(4,1,4),(4,1,1,1,1,1,1,
1,1,1,1,1,1,4),(0.,0.571428571428571,1.),(-2.12204013797473E-15,0.0295575519591679,
0.059115103918338,0.088672655877508,0.118230207836678,0.119153881335402,
0.120077554834126,0.121924901831574,0.125619595826471,0.133008983816263,
0.140398371806056,0.144093065800952,0.147787759795848,0.206902863714188),
 .UNSPECIFIED.) ;
#2084 = B_SPLINE_SURFACE_WITH_KNOTS('',3,3,((#95573,#95574,#95575,#95576,
#95577,#95578,#95579,#95580,#95581,#95582,#95583,#95584,#95585),(#95586,
#95587,#95588,#95589,#95590,#95591,#95592,#95593,#95594,#95595,#95596,#95597,
#95598),(#95599,#95600,#95601,#95602,#95603,#95604,#95605,#95606,#95607,
#95608,#95609,#95610,#95611),(#95612,#95613,#95614,#95615,#95616,#95617,
#95618,#95619,#95620,#95621,#95622,#95623,#95624),(#95625,#95626,#95627,
#95628,#95629,#95630,#95631,#95632,#95633,#95634,#95635,#95636,#95637)),
 .UNSPECIFIED.,.F.,.F.,.F.,(4,1,4),(4,1,1,1,1,1,1,1,1,1,4),(0.,0.571428571428571,
1.),(-0.010282001904707,0.043288805662896,0.0566815075547967,0.0633778585007471,
0.0700742094466975,0.0767705603926478,0.080118735865623,0.0968596132304989,
0.1236450170143,0.150430420798102,0.177215824581903),.UNSPECIFIED.) ;
#2085 = B_SPLINE_SURFACE_WITH_KNOTS('',3,1,((#95791,#95792),(#95793,#95794),
(#95795,#95796),(#95797,#95798),(#95799,#95800),(#95801,#95802),(#95803,
#95804),(#95805,#95806),(#95807,#95808),(#95809,#95810)),.UNSPECIFIED.,
 .F.,.F.,.F.,(4,3,3,4),(2,2),(0.158459382483081,0.476662334259652,0.810817235783357,
1.),(0.,0.0359999999999998),.UNSPECIFIED.) ;
#2086 = B_SPLINE_SURFACE_WITH_KNOTS('',3,1,((#95968,#95969),(#95970,#95971),
(#95972,#95973),(#95974,#95975),(#95976,#95977),(#95978,#95979),(#95980,
#95981),(#95982,#95983),(#95984,#95985),(#95986,#95987)),.UNSPECIFIED.,
 .F.,.F.,.F.,(4,3,3,4),(2,2),(-1.,-0.68247429487388,-0.37617247715991,-0.15436867748257),
(0.,0.0359999999999998),.UNSPECIFIED.) ;
#2087 = B_SPLINE_SURFACE_WITH_KNOTS('',3,3,((#96454,#96455,#96456,#96457,
#96458,#96459,#96460,#96461,#96462,#96463,#96464,#96465,#96466,#96467,#96468,
#96469,#96470,#96471,#96472,#96473,#96474,#96475,#96476),(#96477,#96478,
#96479,#96480,#96481,#96482,#96483,#96484,#96485,#96486,#96487,#96488,#96489,
#96490,#96491,#96492,#96493,#96494,#96495,#96496,#96497,#96498,#96499),
(#96500,#96501,#96502,#96503,#96504,#96505,#96506,#96507,#96508,#96509,
#96510,#96511,#96512,#96513,#96514,#96515,#96516,#96517,#96518,#96519,#96520,
#96521,#96522),(#96523,#96524,#96525,#96526,#96527,#96528,#96529,#96530,
#96531,#96532,#96533,#96534,#96535,#96536,#96537,#96538,#96539,#96540,#96541,
#96542,#96543,#96544,#96545),(#96546,#96547,#96548,#96549,#96550,#96551,
#96552,#96553,#96554,#96555,#96556,#96557,#96558,#96559,#96560,#96561,#96562,
#96563,#96564,#96565,#96566,#96567,#96568),(#96569,#96570,#96571,#96572,
#96573,#96574,#96575,#96576,#96577,#96578,#96579,#96580,#96581,#96582,#96583,
#96584,#96585,#96586,#96587,#96588,#96589,#96590,#96591)),.UNSPECIFIED.,
 .F.,.F.,.F.,(4,1,1,4),(4,1,1,1,1,1,1,1,1,1,1,1,1,1,1,1,1,1,2,4),(0.,0.285714285714286,
0.571428571428571,1.),(-3.27226604903845E-14,0.0211428683856211,0.0422857367712749,
0.0634286051569287,0.0740000393497556,0.0746607539868073,0.0753214686238589,
0.0759821832609106,0.0766428978979623,0.079285756446169,0.0845714735425825,
0.0951429077354094,0.100428624831823,0.104392912654133,0.105053627291185,
0.105714341928236,0.116285776121063,0.12685721031389,0.148000078699544,
0.158000078699635),.UNSPECIFIED.) ;
#2088 = B_SPLINE_SURFACE_WITH_KNOTS('',3,3,((#96795,#96796,#96797,#96798,
#96799,#96800,#96801,#96802,#96803,#96804,#96805),(#96806,#96807,#96808,
#96809,#96810,#96811,#96812,#96813,#96814,#96815,#96816),(#96817,#96818,
#96819,#96820,#96821,#96822,#96823,#96824,#96825,#96826,#96827),(#96828,
#96829,#96830,#96831,#96832,#96833,#96834,#96835,#96836,#96837,#96838),
(#96839,#96840,#96841,#96842,#96843,#96844,#96845,#96846,#96847,#96848,
#96849),(#96850,#96851,#96852,#96853,#96854,#96855,#96856,#96857,#96858,
#96859,#96860),(#96861,#96862,#96863,#96864,#96865,#96866,#96867,#96868,
#96869,#96870,#96871)),.UNSPECIFIED.,.F.,.F.,.F.,(4,1,1,1,4),(4,2,1,1,1,
1,1,4),(0.,0.285714285714286,0.571428571428571,0.857142857142857,1.),(-0.0100000000000179,
0.,0.062390566311959,0.0935858494679386,0.124781132623918,0.155976415779898,
0.179372878146882,0.218366982091857),.UNSPECIFIED.) ;
#2089 = B_SPLINE_SURFACE_WITH_KNOTS('',3,1,((#96881,#96882),(#96883,#96884),
(#96885,#96886),(#96887,#96888),(#96889,#96890),(#96891,#96892),(#96893,
#96894),(#96895,#96896),(#96897,#96898),(#96899,#96900)),.UNSPECIFIED.,
 .F.,.F.,.F.,(4,3,3,4),(2,2),(-1.,-0.727595954149532,-0.403941852861304,
-0.18399442225235),(0.,0.0359999999999998),.UNSPECIFIED.) ;
#2090 = B_SPLINE_SURFACE_WITH_KNOTS('',3,1,((#96904,#96905),(#96906,#96907),
(#96908,#96909),(#96910,#96911),(#96912,#96913),(#96914,#96915),(#96916,
#96917),(#96918,#96919),(#96920,#96921),(#96922,#96923)),.UNSPECIFIED.,
 .F.,.F.,.F.,(4,3,3,4),(2,2),(0.185322868216722,0.499244287262782,0.821195447612718,
1.),(0.,0.0359999999999998),.UNSPECIFIED.) ;
#2091 = B_SPLINE_SURFACE_WITH_KNOTS('',3,3,((#96924,#96925,#96926,#96927,
#96928,#96929,#96930,#96931,#96932,#96933,#96934,#96935,#96936,#96937,#96938,
#96939),(#96940,#96941,#96942,#96943,#96944,#96945,#96946,#96947,#96948,
#96949,#96950,#96951,#96952,#96953,#96954,#96955),(#96956,#96957,#96958,
#96959,#96960,#96961,#96962,#96963,#96964,#96965,#96966,#96967,#96968,#96969,
#96970,#96971),(#96972,#96973,#96974,#96975,#96976,#96977,#96978,#96979,
#96980,#96981,#96982,#96983,#96984,#96985,#96986,#96987),(#96988,#96989,
#96990,#96991,#96992,#96993,#96994,#96995,#96996,#96997,#96998,#96999,#97000,
#97001,#97002,#97003),(#97004,#97005,#97006,#97007,#97008,#97009,#97010,
#97011,#97012,#97013,#97014,#97015,#97016,#97017,#97018,#97019)),
 .UNSPECIFIED.,.F.,.F.,.F.,(4,1,1,4),(4,1,1,1,1,1,1,1,1,1,1,2,4),(0.,0.285714285714286,
0.571428571428571,1.),(-1.41081590854242E-13,0.0226242588783568,0.0678727766353526,
0.0791849060746015,0.084840970794226,0.0904970355138505,0.0961531002334749,
0.101809164953099,0.107465229672724,0.113121294392348,0.135745553270846,
0.158369812149344,0.168369812149447),.UNSPECIFIED.) ;
#2092 = B_SPLINE_SURFACE_WITH_KNOTS('',3,3,((#97074,#97075,#97076,#97077,
#97078,#97079,#97080,#97081,#97082,#97083,#97084),(#97085,#97086,#97087,
#97088,#97089,#97090,#97091,#97092,#97093,#97094,#97095),(#97096,#97097,
#97098,#97099,#97100,#97101,#97102,#97103,#97104,#97105,#97106),(#97107,
#97108,#97109,#97110,#97111,#97112,#97113,#97114,#97115,#97116,#97117),
(#97118,#97119,#97120,#97121,#97122,#97123,#97124,#97125,#97126,#97127,
#97128),(#97129,#97130,#97131,#97132,#97133,#97134,#97135,#97136,#97137,
#97138,#97139),(#97140,#97141,#97142,#97143,#97144,#97145,#97146,#97147,
#97148,#97149,#97150),(#97151,#97152,#97153,#97154,#97155,#97156,#97157,
#97158,#97159,#97160,#97161),(#97162,#97163,#97164,#97165,#97166,#97167,
#97168,#97169,#97170,#97171,#97172)),.UNSPECIFIED.,.F.,.F.,.F.,(4,1,1,1,
1,1,4),(4,2,1,1,1,1,1,4),(0.,0.285714285714286,0.5,0.785714285714286,0.857142857142857,
0.928571428571429,1.),(-0.0100000000001109,0.,0.0617215701552963,0.0925823552329445,
0.123443140310593,0.154303925388241,0.177449514196477,0.216025495543537),
 .UNSPECIFIED.) ;
#2093 = B_SPLINE_SURFACE_WITH_KNOTS('',3,3,((#97617,#97618,#97619,#97620,
#97621,#97622),(#97623,#97624,#97625,#97626,#97627,#97628),(#97629,#97630,
#97631,#97632,#97633,#97634),(#97635,#97636,#97637,#97638,#97639,#97640),
(#97641,#97642,#97643,#97644,#97645,#97646),(#97647,#97648,#97649,#97650,
#97651,#97652),(#97653,#97654,#97655,#97656,#97657,#97658),(#97659,#97660,
#97661,#97662,#97663,#97664),(#97665,#97666,#97667,#97668,#97669,#97670),
(#97671,#97672,#97673,#97674,#97675,#97676),(#97677,#97678,#97679,#97680,
#97681,#97682),(#97683,#97684,#97685,#97686,#97687,#97688),(#97689,#97690,
#97691,#97692,#97693,#97694)),.UNSPECIFIED.,.F.,.F.,.F.,(4,1,1,1,1,1,1,
1,1,1,4),(4,1,1,4),(0.,0.1,0.2,0.3,0.4,0.5,0.6,0.7,0.8,0.9,1.),(0.,0.333333333333333,
0.666666666666667,1.),.UNSPECIFIED.) ;
#2094 = B_SPLINE_SURFACE_WITH_KNOTS('',3,3,((#97698,#97699,#97700,#97701),
(#97702,#97703,#97704,#97705),(#97706,#97707,#97708,#97709),(#97710,#97711,
#97712,#97713),(#97714,#97715,#97716,#97717)),.UNSPECIFIED.,.F.,.F.,.F.,
(4,1,4),(4,4),(0.,0.5,1.),(0.,0.0936131112963942),.UNSPECIFIED.) ;
#2095 = B_SPLINE_SURFACE_WITH_KNOTS('',3,3,((#97741,#97742,#97743,#97744),
(#97745,#97746,#97747,#97748),(#97749,#97750,#97751,#97752),(#97753,#97754,
#97755,#97756),(#97757,#97758,#97759,#97760)),.UNSPECIFIED.,.F.,.F.,.F.,
(4,1,4),(4,4),(-9.85495485568073E-5,0.5,1.),(-1.38376278961886,-0.927196668453033),
 .UNSPECIFIED.) ;
#2096 = B_SPLINE_SURFACE_WITH_KNOTS('',3,3,((#97787,#97788,#97789,#97790),
(#97791,#97792,#97793,#97794),(#97795,#97796,#97797,#97798),(#97799,#97800,
#97801,#97802),(#97803,#97804,#97805,#97806)),.UNSPECIFIED.,.F.,.F.,.F.,
(4,1,4),(4,4),(0.,0.5,1.),(0.,0.0936141814749616),.UNSPECIFIED.) ;
#2097 = B_SPLINE_SURFACE_WITH_KNOTS('',3,3,((#97838,#97839,#97840,#97841,
#97842,#97843),(#97844,#97845,#97846,#97847,#97848,#97849),(#97850,#97851,
#97852,#97853,#97854,#97855),(#97856,#97857,#97858,#97859,#97860,#97861),
(#97862,#97863,#97864,#97865,#97866,#97867)),.UNSPECIFIED.,.F.,.F.,.F.,
(4,1,4),(4,1,1,4),(-0.00794987368555094,0.571428571428571,1.),(-0.858804741536017,
-0.12155069540721,0.364652086221628,0.858804741536017),.UNSPECIFIED.) ;
#2098 = B_SPLINE_SURFACE_WITH_KNOTS('',3,3,((#97869,#97870,#97871,#97872),
(#97873,#97874,#97875,#97876),(#97877,#97878,#97879,#97880),(#97881,#97882,
#97883,#97884),(#97885,#97886,#97887,#97888)),.UNSPECIFIED.,.F.,.F.,.F.,
(4,1,4),(4,4),(0.,0.5,1.),(0.,0.0936131112963941),.UNSPECIFIED.) ;
#2099 = B_SPLINE_SURFACE_WITH_KNOTS('',3,3,((#97903,#97904,#97905,#97906),
(#97907,#97908,#97909,#97910),(#97911,#97912,#97913,#97914),(#97915,#97916,
#97917,#97918),(#97919,#97920,#97921,#97922)),.UNSPECIFIED.,.F.,.F.,.F.,
(4,1,4),(4,4),(0.,0.5,1.),(0.,0.0936141811972385),.UNSPECIFIED.) ;
#2100 = B_SPLINE_SURFACE_WITH_KNOTS('',3,3,((#97954,#97955,#97956,#97957,
#97958,#97959),(#97960,#97961,#97962,#97963,#97964,#97965),(#97966,#97967,
#97968,#97969,#97970,#97971),(#97972,#97973,#97974,#97975,#97976,#97977),
(#97978,#97979,#97980,#97981,#97982,#97983)),.UNSPECIFIED.,.F.,.F.,.F.,
(4,1,4),(4,1,1,4),(-0.00795694173847245,0.571428571428571,1.),(-0.858811809588939,
-0.12155069540721,0.364652086221628,0.858811809588939),.UNSPECIFIED.) ;
#2101 = B_SPLINE_SURFACE_WITH_KNOTS('',3,3,((#98022,#98023,#98024,#98025),
(#98026,#98027,#98028,#98029),(#98030,#98031,#98032,#98033),(#98034,#98035,
#98036,#98037),(#98038,#98039,#98040,#98041)),.UNSPECIFIED.,.F.,.F.,.F.,
(4,1,4),(4,4),(-0.00025082614922299,0.5,1.),(0.643250282643994,1.18620111781914),
 .UNSPECIFIED.) ;
#2102 = B_SPLINE_SURFACE_WITH_KNOTS('',3,3,((#98054,#98055,#98056,#98057),
(#98058,#98059,#98060,#98061),(#98062,#98063,#98064,#98065),(#98066,#98067,
#98068,#98069),(#98070,#98071,#98072,#98073)),.UNSPECIFIED.,.F.,.F.,.F.,
(4,1,4),(4,4),(-9.85495485873771E-5,0.5,1.),(-1.38376278961876,-0.927196668453042),
 .UNSPECIFIED.) ;
#2103 = B_SPLINE_SURFACE_WITH_KNOTS('',3,3,((#98091,#98092,#98093,#98094),
(#98095,#98096,#98097,#98098),(#98099,#98100,#98101,#98102),(#98103,#98104,
#98105,#98106),(#98107,#98108,#98109,#98110)),.UNSPECIFIED.,.F.,.F.,.F.,
(4,1,4),(4,4),(-0.0018031252703055,0.5,1.),(0.641697983523243,1.57259945206521),
 .UNSPECIFIED.) ;
#2104 = B_SPLINE_SURFACE_WITH_KNOTS('',3,1,((#98176,#98177),(#98178,#98179),
(#98180,#98181),(#98182,#98183),(#98184,#98185),(#98186,#98187)),
 .UNSPECIFIED.,.F.,.F.,.F.,(4,2,4),(2,2),(-0.0699558285734079,-0.0581995466601177,
-0.0505532240038504),(0.,1.14),.UNSPECIFIED.) ;
#2105 = B_SPLINE_SURFACE_WITH_KNOTS('',3,1,((#98200,#98201),(#98202,#98203),
(#98204,#98205),(#98206,#98207),(#98208,#98209),(#98210,#98211)),
 .UNSPECIFIED.,.F.,.F.,.F.,(4,2,4),(2,2),(-0.0194026045695574,-0.0117562819132905,
0.),(0.,1.14),.UNSPECIFIED.) ;
#2106 = B_SPLINE_SURFACE_WITH_KNOTS('',3,1,((#98307,#98308),(#98309,#98310),
(#98311,#98312),(#98313,#98314),(#98315,#98316),(#98317,#98318)),
 .UNSPECIFIED.,.F.,.F.,.F.,(4,2,4),(2,2),(-0.0699558285734104,-0.0581995466601188,
-0.0505532240038526),(0.,1.14),.UNSPECIFIED.) ;
#2107 = B_SPLINE_SURFACE_WITH_KNOTS('',3,1,((#98433,#98434),(#98435,#98436),
(#98437,#98438),(#98439,#98440),(#98441,#98442),(#98443,#98444)),
 .UNSPECIFIED.,.F.,.F.,.F.,(4,2,4),(2,2),(-0.0194026045695577,-0.0117562819132915,
0.),(0.,1.14),.UNSPECIFIED.) ;
#2108 = B_SPLINE_SURFACE_WITH_KNOTS('',3,1,((#98468,#98469),(#98470,#98471),
(#98472,#98473),(#98474,#98475),(#98476,#98477),(#98478,#98479)),
 .UNSPECIFIED.,.F.,.F.,.F.,(4,2,4),(2,2),(-0.0194026045695576,-0.0117562819132903,
0.),(0.,1.14),.UNSPECIFIED.) ;
#2109 = B_SPLINE_SURFACE_WITH_KNOTS('',3,3,((#101320,#101321,#101322,#101323,
#101324,#101325,#101326,#101327,#101328,#101329,#101330,#101331,#101332,
#101333,#101334,#101335,#101336,#101337,#101338,#101339,#101340,#101341,
#101342,#101343,#101344,#101345,#101346,#101347,#101348,#101349,#101350),
(#101351,#101352,#101353,#101354,#101355,#101356,#101357,#101358,#101359,
#101360,#101361,#101362,#101363,#101364,#101365,#101366,#101367,#101368,
#101369,#101370,#101371,#101372,#101373,#101374,#101375,#101376,#101377,
#101378,#101379,#101380,#101381),(#101382,#101383,#101384,#101385,#101386,
#101387,#101388,#101389,#101390,#101391,#101392,#101393,#101394,#101395,
#101396,#101397,#101398,#101399,#101400,#101401,#101402,#101403,#101404,
#101405,#101406,#101407,#101408,#101409,#101410,#101411,#101412),(#101413,
#101414,#101415,#101416,#101417,#101418,#101419,#101420,#101421,#101422,
#101423,#101424,#101425,#101426,#101427,#101428,#101429,#101430,#101431,
#101432,#101433,#101434,#101435,#101436,#101437,#101438,#101439,#101440,
#101441,#101442,#101443)),.UNSPECIFIED.,.F.,.F.,.F.,(4,4),(4,1,1,1,1,1,
1,1,1,1,1,1,1,1,1,1,1,1,1,1,1,1,1,1,1,1,1,1,4),(-0.0003307145317139,0.0332819478446879),
(8.30276167405425,9.27440145626992,10.2460412384856,11.2176810207013,12.1893208029169,
13.1609605851326,14.1326003673483,15.104240149564,16.0758799317796,17.0475197139953,
18.019159496211,18.9907992784267,19.9624390606423,20.934078842858,21.9057186250737,
22.8773584072894,23.848998189505,24.8206379717207,25.7922777539364,26.763917536152,
27.7355573183677,28.7071971005834,29.6788368827991,30.6504766650147,31.6221164472304,
32.5937562294461,33.5653960116618,34.5370357938774,35.5090062906248),
 .UNSPECIFIED.) ;
#2110 = B_SPLINE_SURFACE_WITH_KNOTS('',3,3,((#101534,#101535,#101536,#101537,
#101538,#101539,#101540,#101541,#101542,#101543,#101544,#101545,#101546,
#101547,#101548,#101549,#101550,#101551,#101552,#101553,#101554,#101555,
#101556,#101557,#101558,#101559,#101560,#101561,#101562,#101563,#101564),
(#101565,#101566,#101567,#101568,#101569,#101570,#101571,#101572,#101573,
#101574,#101575,#101576,#101577,#101578,#101579,#101580,#101581,#101582,
#101583,#101584,#101585,#101586,#101587,#101588,#101589,#101590,#101591,
#101592,#101593,#101594,#101595),(#101596,#101597,#101598,#101599,#101600,
#101601,#101602,#101603,#101604,#101605,#101606,#101607,#101608,#101609,
#101610,#101611,#101612,#101613,#101614,#101615,#101616,#101617,#101618,
#101619,#101620,#101621,#101622,#101623,#101624,#101625,#101626),(#101627,
#101628,#101629,#101630,#101631,#101632,#101633,#101634,#101635,#101636,
#101637,#101638,#101639,#101640,#101641,#101642,#101643,#101644,#101645,
#101646,#101647,#101648,#101649,#101650,#101651,#101652,#101653,#101654,
#101655,#101656,#101657)),.UNSPECIFIED.,.F.,.F.,.F.,(4,4),(4,1,1,1,1,1,
1,1,1,1,1,1,1,1,1,1,1,1,1,1,1,1,1,1,1,1,1,1,4),(-0.000267659600955013,0.0333309127327678),
(11.6148788829061,12.5868540099704,13.5584937921861,14.5301335744018,15.5017733566174,
16.4734131388331,17.4450529210488,18.4166927032644,19.3883324854801,20.3599722676958,
21.3316120499115,22.3032518321271,23.2748916143428,24.2465313965585,25.2181711787741,
26.1898109609898,27.1614507432055,28.1330905254212,29.1047303076368,30.0763700898525,
31.0480098720682,32.0196496542838,32.9912894364995,33.9629292187152,34.9345690009309,
35.9062087831465,36.8778485653622,37.8494883475779,38.8211281297935),
 .UNSPECIFIED.) ;
#2111 = B_SPLINE_SURFACE_WITH_KNOTS('',3,3,((#101800,#101801,#101802,#101803,
#101804,#101805,#101806,#101807,#101808,#101809,#101810,#101811,#101812,
#101813,#101814,#101815),(#101816,#101817,#101818,#101819,#101820,#101821,
#101822,#101823,#101824,#101825,#101826,#101827,#101828,#101829,#101830,
#101831),(#101832,#101833,#101834,#101835,#101836,#101837,#101838,#101839,
#101840,#101841,#101842,#101843,#101844,#101845,#101846,#101847),(#101848,
#101849,#101850,#101851,#101852,#101853,#101854,#101855,#101856,#101857,
#101858,#101859,#101860,#101861,#101862,#101863),(#101864,#101865,#101866,
#101867,#101868,#101869,#101870,#101871,#101872,#101873,#101874,#101875,
#101876,#101877,#101878,#101879)),.UNSPECIFIED.,.F.,.T.,.F.,(4,1,4),(4,
1,1,1,1,1,1,1,1,1,1,1,1,4),(0.,0.5,1.),(-1.37470975898194,-1.17832265055595,
-0.981935542129957,-0.785548433703966,-0.589161325277974,-0.196387108425991,
0.,0.196387108425991,0.392774216851983,0.589161325277974,0.785548433703966,
0.981935542129957,1.17832265055595,1.37470975898194),.UNSPECIFIED.) ;
#2112 = B_SPLINE_SURFACE_WITH_KNOTS('',3,3,((#101907,#101908,#101909,#101910,
#101911,#101912,#101913,#101914,#101915,#101916,#101917,#101918,#101919,
#101920,#101921,#101922),(#101923,#101924,#101925,#101926,#101927,#101928,
#101929,#101930,#101931,#101932,#101933,#101934,#101935,#101936,#101937,
#101938),(#101939,#101940,#101941,#101942,#101943,#101944,#101945,#101946,
#101947,#101948,#101949,#101950,#101951,#101952,#101953,#101954),(#101955,
#101956,#101957,#101958,#101959,#101960,#101961,#101962,#101963,#101964,
#101965,#101966,#101967,#101968,#101969,#101970),(#101971,#101972,#101973,
#101974,#101975,#101976,#101977,#101978,#101979,#101980,#101981,#101982,
#101983,#101984,#101985,#101986)),.UNSPECIFIED.,.F.,.T.,.F.,(4,1,4),(4,
1,1,1,1,1,1,1,1,1,1,1,1,4),(0.,0.5,1.),(-1.37470975898194,-1.17832265055595,
-0.981935542129957,-0.785548433703966,-0.589161325277974,-0.196387108425991,
0.,0.196387108425991,0.392774216851983,0.589161325277974,0.785548433703966,
0.981935542129957,1.17832265055595,1.37470975898194),.UNSPECIFIED.) ;
#2113 = B_SPLINE_SURFACE_WITH_KNOTS('',3,3,((#105521,#105522,#105523,#105524,
#105525,#105526,#105527,#105528,#105529,#105530,#105531,#105532,#105533,
#105534,#105535,#105536,#105537),(#105538,#105539,#105540,#105541,#105542,
#105543,#105544,#105545,#105546,#105547,#105548,#105549,#105550,#105551,
#105552,#105553,#105554),(#105555,#105556,#105557,#105558,#105559,#105560,
#105561,#105562,#105563,#105564,#105565,#105566,#105567,#105568,#105569,
#105570,#105571),(#105572,#105573,#105574,#105575,#105576,#105577,#105578,
#105579,#105580,#105581,#105582,#105583,#105584,#105585,#105586,#105587,
#105588),(#105589,#105590,#105591,#105592,#105593,#105594,#105595,#105596,
#105597,#105598,#105599,#105600,#105601,#105602,#105603,#105604,#105605)),
 .UNSPECIFIED.,.F.,.T.,.F.,(4,1,4),(4,1,1,1,1,1,1,1,1,1,1,1,1,1,4),(0.,
0.5,1.),(-1.37470975898194,-1.17832265055595,-0.981935542129957,-0.785548433703966,
-0.589161325277974,-0.392774216851983,-0.196387108425991,0.,0.196387108425991,
0.392774216851983,0.589161325277974,0.785548433703966,0.981935542129957,
1.17832265055595,1.37470975898194),.UNSPECIFIED.) ;
#2114 = B_SPLINE_SURFACE_WITH_KNOTS('',3,3,((#105634,#105635,#105636,#105637,
#105638,#105639,#105640,#105641,#105642,#105643,#105644,#105645,#105646,
#105647,#105648,#105649,#105650),(#105651,#105652,#105653,#105654,#105655,
#105656,#105657,#105658,#105659,#105660,#105661,#105662,#105663,#105664,
#105665,#105666,#105667),(#105668,#105669,#105670,#105671,#105672,#105673,
#105674,#105675,#105676,#105677,#105678,#105679,#105680,#105681,#105682,
#105683,#105684),(#105685,#105686,#105687,#105688,#105689,#105690,#105691,
#105692,#105693,#105694,#105695,#105696,#105697,#105698,#105699,#105700,
#105701),(#105702,#105703,#105704,#105705,#105706,#105707,#105708,#105709,
#105710,#105711,#105712,#105713,#105714,#105715,#105716,#105717,#105718)),
 .UNSPECIFIED.,.F.,.T.,.F.,(4,1,4),(4,1,1,1,1,1,1,1,1,1,1,1,1,1,4),(0.,
0.5,1.),(-1.37470975898194,-1.17832265055595,-0.981935542129957,-0.785548433703966,
-0.589161325277974,-0.392774216851983,-0.196387108425991,0.,0.196387108425991,
0.392774216851983,0.589161325277974,0.785548433703966,0.981935542129957,
1.17832265055595,1.37470975898194),.UNSPECIFIED.) ;
#2115 = B_SPLINE_SURFACE_WITH_KNOTS('',3,3,((#115966,#115967,#115968,#115969,
#115970,#115971,#115972,#115973,#115974,#115975,#115976,#115977,#115978,
#115979,#115980,#115981,#115982,#115983,#115984,#115985,#115986,#115987,
#115988,#115989,#115990,#115991,#115992,#115993,#115994,#115995,#115996),
(#115997,#115998,#115999,#116000,#116001,#116002,#116003,#116004,#116005,
#116006,#116007,#116008,#116009,#116010,#116011,#116012,#116013,#116014,
#116015,#116016,#116017,#116018,#116019,#116020,#116021,#116022,#116023,
#116024,#116025,#116026,#116027),(#116028,#116029,#116030,#116031,#116032,
#116033,#116034,#116035,#116036,#116037,#116038,#116039,#116040,#116041,
#116042,#116043,#116044,#116045,#116046,#116047,#116048,#116049,#116050,
#116051,#116052,#116053,#116054,#116055,#116056,#116057,#116058),(#116059,
#116060,#116061,#116062,#116063,#116064,#116065,#116066,#116067,#116068,
#116069,#116070,#116071,#116072,#116073,#116074,#116075,#116076,#116077,
#116078,#116079,#116080,#116081,#116082,#116083,#116084,#116085,#116086,
#116087,#116088,#116089)),.UNSPECIFIED.,.F.,.F.,.F.,(4,4),(4,1,1,1,1,1,
1,1,1,1,1,1,1,1,1,1,1,1,1,1,1,1,1,1,1,1,1,1,4),(-0.000330953812216286,0.0332825271993837),
(8.30276167405401,9.27440145626965,10.2460412384853,11.2176810207009,12.1893208029166,
13.1609605851322,14.1326003673479,15.1042401495635,16.0758799317792,17.0475197139948,
18.0191594962104,18.9907992784261,19.9624390606417,20.9340788428574,21.905718625073,
22.8773584072887,23.8489981895043,24.8206379717199,25.7922777539356,26.7639175361512,
27.7355573183669,28.7071971005825,29.6788368827982,30.6504766650138,31.6221164472294,
32.5937562294451,33.5653960116607,34.5370357938764,35.5090065299042),
 .UNSPECIFIED.) ;
#2116 = B_SPLINE_SURFACE_WITH_KNOTS('',3,3,((#116269,#116270,#116271,#116272,
#116273,#116274,#116275,#116276,#116277,#116278,#116279,#116280,#116281,
#116282,#116283,#116284,#116285,#116286,#116287,#116288,#116289,#116290,
#116291,#116292,#116293,#116294,#116295,#116296,#116297,#116298,#116299),
(#116300,#116301,#116302,#116303,#116304,#116305,#116306,#116307,#116308,
#116309,#116310,#116311,#116312,#116313,#116314,#116315,#116316,#116317,
#116318,#116319,#116320,#116321,#116322,#116323,#116324,#116325,#116326,
#116327,#116328,#116329,#116330),(#116331,#116332,#116333,#116334,#116335,
#116336,#116337,#116338,#116339,#116340,#116341,#116342,#116343,#116344,
#116345,#116346,#116347,#116348,#116349,#116350,#116351,#116352,#116353,
#116354,#116355,#116356,#116357,#116358,#116359,#116360,#116361),(#116362,
#116363,#116364,#116365,#116366,#116367,#116368,#116369,#116370,#116371,
#116372,#116373,#116374,#116375,#116376,#116377,#116378,#116379,#116380,
#116381,#116382,#116383,#116384,#116385,#116386,#116387,#116388,#116389,
#116390,#116391,#116392)),.UNSPECIFIED.,.F.,.F.,.F.,(4,4),(4,1,1,1,1,1,
1,1,1,1,1,1,1,1,1,1,1,1,1,1,1,1,1,1,1,1,1,1,4),(-0.000267929854482752,0.0333311607245051),
(11.6148786349143,12.5868540099703,13.5584937921859,14.5301335744016,15.5017733566172,
16.4734131388329,17.4450529210485,18.4166927032641,19.3883324854798,20.3599722676954,
21.3316120499111,22.3032518321267,23.2748916143424,24.246531396558,25.2181711787737,
26.1898109609893,27.161450743205,28.1330905254206,29.1047303076363,30.0763700898519,
31.0480098720675,32.0196496542832,32.9912894364988,33.9629292187145,34.9345690009301,
35.9062087831458,36.8778485653614,37.8494883475771,38.8211281297927),
 .UNSPECIFIED.) ;
#2117 = B_SPLINE_SURFACE_WITH_KNOTS('',3,3,((#116578,#116579,#116580,#116581,
#116582,#116583,#116584,#116585,#116586,#116587,#116588,#116589,#116590,
#116591,#116592,#116593,#116594,#116595,#116596,#116597,#116598,#116599,
#116600,#116601,#116602,#116603,#116604,#116605,#116606,#116607,#116608,
#116609,#116610,#116611,#116612,#116613,#116614,#116615,#116616,#116617,
#116618,#116619,#116620),(#116621,#116622,#116623,#116624,#116625,#116626,
#116627,#116628,#116629,#116630,#116631,#116632,#116633,#116634,#116635,
#116636,#116637,#116638,#116639,#116640,#116641,#116642,#116643,#116644,
#116645,#116646,#116647,#116648,#116649,#116650,#116651,#116652,#116653,
#116654,#116655,#116656,#116657,#116658,#116659,#116660,#116661,#116662,
#116663),(#116664,#116665,#116666,#116667,#116668,#116669,#116670,#116671,
#116672,#116673,#116674,#116675,#116676,#116677,#116678,#116679,#116680,
#116681,#116682,#116683,#116684,#116685,#116686,#116687,#116688,#116689,
#116690,#116691,#116692,#116693,#116694,#116695,#116696,#116697,#116698,
#116699,#116700,#116701,#116702,#116703,#116704,#116705,#116706),(#116707,
#116708,#116709,#116710,#116711,#116712,#116713,#116714,#116715,#116716,
#116717,#116718,#116719,#116720,#116721,#116722,#116723,#116724,#116725,
#116726,#116727,#116728,#116729,#116730,#116731,#116732,#116733,#116734,
#116735,#116736,#116737,#116738,#116739,#116740,#116741,#116742,#116743,
#116744,#116745,#116746,#116747,#116748,#116749)),.UNSPECIFIED.,.F.,.F.,
 .F.,(4,4),(4,1,1,1,1,1,1,1,1,1,1,1,1,1,1,1,1,1,1,1,1,1,1,1,1,1,1,1,1,1,
1,1,1,1,1,1,1,1,1,1,4),(-0.00035408581260011,0.0333043091341808),(8.30276167405401,
9.29706878696395,10.2913758998739,11.2856830127838,12.2799901256938,13.2742972386037,
14.2686043515136,15.2629114644236,16.2572185773335,17.2515256902434,18.2458328031534,
19.2401399160633,20.2344470289732,21.2287541418832,22.2230612547931,23.217368367703,
24.211675480613,25.2059825935229,26.2002897064328,27.1945968193428,28.1889039322527,
29.1832110451626,30.1775181580726,31.1718252709825,32.1661323838924,33.1604394968024,
34.1547466097123,35.1490537226222,36.1433608355322,37.1376679484421,38.1319750613521,
39.126282174262,40.1205892871719,41.1148964000819,42.1092035129918,43.1035106259017,
44.0978177388117,45.0921248517216,46.0864319646315,47.0807390775415,48.075400276264),
 .UNSPECIFIED.) ;
#2118 = B_SPLINE_SURFACE_WITH_KNOTS('',3,3,((#116930,#116931,#116932,#116933,
#116934,#116935,#116936,#116937,#116938,#116939,#116940,#116941,#116942,
#116943,#116944,#116945,#116946,#116947,#116948,#116949,#116950,#116951,
#116952,#116953,#116954,#116955,#116956,#116957,#116958,#116959,#116960,
#116961,#116962,#116963,#116964,#116965,#116966,#116967,#116968,#116969,
#116970,#116971,#116972),(#116973,#116974,#116975,#116976,#116977,#116978,
#116979,#116980,#116981,#116982,#116983,#116984,#116985,#116986,#116987,
#116988,#116989,#116990,#116991,#116992,#116993,#116994,#116995,#116996,
#116997,#116998,#116999,#117000,#117001,#117002,#117003,#117004,#117005,
#117006,#117007,#117008,#117009,#117010,#117011,#117012,#117013,#117014,
#117015),(#117016,#117017,#117018,#117019,#117020,#117021,#117022,#117023,
#117024,#117025,#117026,#117027,#117028,#117029,#117030,#117031,#117032,
#117033,#117034,#117035,#117036,#117037,#117038,#117039,#117040,#117041,
#117042,#117043,#117044,#117045,#117046,#117047,#117048,#117049,#117050,
#117051,#117052,#117053,#117054,#117055,#117056,#117057,#117058),(#117059,
#117060,#117061,#117062,#117063,#117064,#117065,#117066,#117067,#117068,
#117069,#117070,#117071,#117072,#117073,#117074,#117075,#117076,#117077,
#117078,#117079,#117080,#117081,#117082,#117083,#117084,#117085,#117086,
#117087,#117088,#117089,#117090,#117091,#117092,#117093,#117094,#117095,
#117096,#117097,#117098,#117099,#117100,#117101)),.UNSPECIFIED.,.F.,.F.,
 .F.,(4,4),(4,1,1,1,1,1,1,1,1,1,1,1,1,1,1,1,1,1,1,1,1,1,1,1,1,1,1,1,1,1,
1,1,1,1,1,1,1,1,1,1,4),(-0.00029211499150135,0.0333604038950206),(11.6148493917438,
12.6095213406646,13.6038284535745,14.5981355664844,15.5924426793944,16.5867497923043,
17.5810569052142,18.5753640181242,19.5696711310341,20.563978243944,21.558285356854,
22.5525924697639,23.5468995826738,24.5412066955838,25.5355138084937,26.5298209214036,
27.5241280343136,28.5184351472235,29.5127422601335,30.5070493730434,31.5013564859533,
32.4956635988633,33.4899707117732,34.4842778246831,35.4785849375931,36.472892050503,
37.4671991634129,38.4615062763229,39.4558133892328,40.4501205021427,41.4444276150527,
42.4387347279626,43.4330418408725,44.4273489537825,45.4216560666924,46.4159631796023,
47.4102702925123,48.4045774054222,49.3988845183321,50.3931916312421,51.387498744152),
 .UNSPECIFIED.) ;
#2119 = SPHERICAL_SURFACE('',#49407,0.2) ;
#2120 = SPHERICAL_SURFACE('',#49409,0.2) ;
#2121 = SPHERICAL_SURFACE('',#49411,0.2) ;
#2122 = SPHERICAL_SURFACE('',#49413,0.2) ;
#2123 = SPHERICAL_SURFACE('',#49415,0.2) ;
#2124 = SPHERICAL_SURFACE('',#49417,0.2) ;
#2125 = SPHERICAL_SURFACE('',#49419,0.2) ;
#2126 = SPHERICAL_SURFACE('',#49421,0.2) ;
#2127 = SPHERICAL_SURFACE('',#49442,0.199999999999992) ;
#2128 = SPHERICAL_SURFACE('',#49446,0.199999999999996) ;
#2129 = SPHERICAL_SURFACE('',#49450,0.199999999999982) ;
#2130 = SPHERICAL_SURFACE('',#49456,0.19999999999999) ;
#2131 = SPHERICAL_SURFACE('',#49460,0.199999999999987) ;
#2132 = SPHERICAL_SURFACE('',#49464,0.199999999999985) ;
#2133 = SPHERICAL_SURFACE('',#49468,0.199999999999991) ;
#2134 = SPHERICAL_SURFACE('',#49474,0.199999999999996) ;
#2135 = SPHERICAL_SURFACE('',#49478,0.199999999999987) ;
#2136 = SPHERICAL_SURFACE('',#49482,0.200000000000018) ;
#2137 = SPHERICAL_SURFACE('',#49486,0.200000000000018) ;
#2138 = SPHERICAL_SURFACE('',#49492,0.200000000000001) ;
#2139 = SPHERICAL_SURFACE('',#49496,0.199999999999999) ;
#2140 = SPHERICAL_SURFACE('',#49500,0.200000000000007) ;
#2141 = SPHERICAL_SURFACE('',#49504,0.200000000000012) ;
#2142 = SPHERICAL_SURFACE('',#49510,0.200000000000011) ;
#2143 = SPHERICAL_SURFACE('',#49514,0.199999999999993) ;
#2144 = SPHERICAL_SURFACE('',#49518,0.200000000000016) ;
#2145 = SPHERICAL_SURFACE('',#49522,0.200000000000006) ;
#2146 = SPHERICAL_SURFACE('',#49528,0.199999999999982) ;
#2147 = SPHERICAL_SURFACE('',#49532,0.199999999999997) ;
#2148 = SPHERICAL_SURFACE('',#49536,0.199999999999999) ;
#2149 = SPHERICAL_SURFACE('',#49540,0.200000000000023) ;
#2150 = SPHERICAL_SURFACE('',#49546,0.199999999999992) ;
#2151 = SPHERICAL_SURFACE('',#49550,0.199999999999988) ;
#2152 = SPHERICAL_SURFACE('',#49554,0.199999999999997) ;
#2153 = SPHERICAL_SURFACE('',#49558,0.200000000000027) ;
#2154 = SPHERICAL_SURFACE('',#49564,0.199999999999997) ;
#2155 = SPHERICAL_SURFACE('',#49568,0.199999999999974) ;
#2156 = SPHERICAL_SURFACE('',#49572,0.200000000000024) ;
#2157 = SPHERICAL_SURFACE('',#49576,0.199999999999994) ;
#2158 = SPHERICAL_SURFACE('',#49582,0.199999999999997) ;
#2159 = SPHERICAL_SURFACE('',#49586,0.199999999999995) ;
#2160 = SPHERICAL_SURFACE('',#49590,0.200000000000031) ;
#2161 = SPHERICAL_SURFACE('',#49594,0.199999999999985) ;
#2162 = SPHERICAL_SURFACE('',#49600,0.199999999999994) ;
#2163 = SPHERICAL_SURFACE('',#49604,0.199999999999995) ;
#2164 = SPHERICAL_SURFACE('',#49608,0.199999999999986) ;
#2165 = SPHERICAL_SURFACE('',#49612,0.199999999999968) ;
#2166 = SPHERICAL_SURFACE('',#49618,0.199999999999996) ;
#2167 = SPHERICAL_SURFACE('',#49985,0.119999999999985) ;
#2168 = SPHERICAL_SURFACE('',#49991,0.119999999999999) ;
#2169 = SPHERICAL_SURFACE('',#50056,0.120000000000007) ;
#2170 = SPHERICAL_SURFACE('',#50063,0.12) ;
#2171 = SPHERICAL_SURFACE('',#50098,0.120000000000005) ;
#2172 = SPHERICAL_SURFACE('',#50107,0.12) ;
#2173 = SPHERICAL_SURFACE('',#50111,0.12) ;
#2174 = SPHERICAL_SURFACE('',#50117,0.120000000000021) ;
#2175 = SPHERICAL_SURFACE('',#50136,0.119999999999985) ;
#2176 = SPHERICAL_SURFACE('',#50592,0.100000000000016) ;
#2177 = SPHERICAL_SURFACE('',#50601,0.1) ;
#2178 = SPHERICAL_SURFACE('',#50628,0.1) ;
#2179 = SPHERICAL_SURFACE('',#50730,0.1) ;
#2180 = SPHERICAL_SURFACE('',#50732,0.1) ;
#2181 = SPHERICAL_SURFACE('',#50807,0.1) ;
#2182 = SPHERICAL_SURFACE('',#50815,0.1) ;
#2183 = SPHERICAL_SURFACE('',#50849,0.1) ;
#2184 = SPHERICAL_SURFACE('',#50857,0.1) ;
#2185 = SPHERICAL_SURFACE('',#50880,0.1) ;
#2186 = SPHERICAL_SURFACE('',#50968,0.100000000000016) ;
#2187 = SPHERICAL_SURFACE('',#50971,0.0999999999999979) ;
#2188 = SPHERICAL_SURFACE('',#51016,0.0999999999999979) ;
#2189 = SPHERICAL_SURFACE('',#51028,0.0999999999999979) ;
#2190 = SPHERICAL_SURFACE('',#51263,0.0999999999999979) ;
#2191 = SPHERICAL_SURFACE('',#51290,0.100000000000016) ;
#2192 = SPHERICAL_SURFACE('',#51717,0.100000000000016) ;
#2193 = SPHERICAL_SURFACE('',#51742,0.1) ;
#2194 = SPHERICAL_SURFACE('',#51744,0.1) ;
#2195 = SPHERICAL_SURFACE('',#52027,0.120000000000005) ;
#2196 = SPHERICAL_SURFACE('',#52056,0.120000000000005) ;
#2197 = SPHERICAL_SURFACE('',#52086,0.120000000000005) ;
#2198 = SPHERICAL_SURFACE('',#52115,0.120000000000005) ;
#2199 = SPHERICAL_SURFACE('',#52180,0.0999999999999979) ;
#2200 = SPHERICAL_SURFACE('',#52184,0.100000000000016) ;
#2201 = SPHERICAL_SURFACE('',#52188,0.100000000000016) ;
#2202 = SPHERICAL_SURFACE('',#52195,0.0999999999999979) ;
#2203 = SPHERICAL_SURFACE('',#52199,0.0999999999999979) ;
#2204 = SPHERICAL_SURFACE('',#52445,0.0499999999999989) ;
#2205 = SPHERICAL_SURFACE('',#52449,0.0499999999999989) ;
#2206 = SPHERICAL_SURFACE('',#52454,0.0499999999999901) ;
#2207 = SPHERICAL_SURFACE('',#52470,0.0499999999999945) ;
#2208 = SPHERICAL_SURFACE('',#52496,0.0499999999999989) ;
#2209 = SPHERICAL_SURFACE('',#52500,0.0499999999999989) ;
#2210 = SPHERICAL_SURFACE('',#52507,0.0499999999999989) ;
#2211 = SPHERICAL_SURFACE('',#52703,0.0999999999999979) ;
#2212 = SPHERICAL_SURFACE('',#52848,0.0999999999999979) ;
#2213 = SPHERICAL_SURFACE('',#52943,0.0999999999999979) ;
#2214 = SPHERICAL_SURFACE('',#53751,0.500000000000009) ;
#2215 = SPHERICAL_SURFACE('',#53766,0.500000000000009) ;
#2216 = PLANE('',#49358) ;
#2217 = PLANE('',#49423) ;
#2218 = PLANE('',#49426) ;
#2219 = PLANE('',#49429) ;
#2220 = PLANE('',#49432) ;
#2221 = PLANE('',#49435) ;
#2222 = PLANE('',#49438) ;
#2223 = PLANE('',#49441) ;
#2224 = PLANE('',#49768) ;
#2225 = PLANE('',#49783) ;
#2226 = PLANE('',#49796) ;
#2227 = PLANE('',#49842) ;
#2228 = PLANE('',#49843) ;
#2229 = PLANE('',#49844) ;
#2230 = PLANE('',#49845) ;
#2231 = PLANE('',#49846) ;
#2232 = PLANE('',#49847) ;
#2233 = PLANE('',#49848) ;
#2234 = PLANE('',#49849) ;
#2235 = PLANE('',#49850) ;
#2236 = PLANE('',#49851) ;
#2237 = PLANE('',#49852) ;
#2238 = PLANE('',#49853) ;
#2239 = PLANE('',#49854) ;
#2240 = PLANE('',#49855) ;
#2241 = PLANE('',#49856) ;
#2242 = PLANE('',#49857) ;
#2243 = PLANE('',#49858) ;
#2244 = PLANE('',#49859) ;
#2245 = PLANE('',#49860) ;
#2246 = PLANE('',#49861) ;
#2247 = PLANE('',#49862) ;
#2248 = PLANE('',#49863) ;
#2249 = PLANE('',#49864) ;
#2250 = PLANE('',#49865) ;
#2251 = PLANE('',#49874) ;
#2252 = PLANE('',#49895) ;
#2253 = PLANE('',#49896) ;
#2254 = PLANE('',#49929) ;
#2255 = PLANE('',#49976) ;
#2256 = PLANE('',#49977) ;
#2257 = PLANE('',#49980) ;
#2258 = PLANE('',#50023) ;
#2259 = PLANE('',#50027) ;
#2260 = PLANE('',#50041) ;
#2261 = PLANE('',#50055) ;
#2262 = PLANE('',#50088) ;
#2263 = PLANE('',#50089) ;
#2264 = PLANE('',#50094) ;
#2265 = PLANE('',#50095) ;
#2266 = PLANE('',#50128) ;
#2267 = PLANE('',#50129) ;
#2268 = PLANE('',#50130) ;
#2269 = PLANE('',#50135) ;
#2270 = PLANE('',#50154) ;
#2271 = PLANE('',#50155) ;
#2272 = PLANE('',#50156) ;
#2273 = PLANE('',#50157) ;
#2274 = PLANE('',#50158) ;
#2275 = PLANE('',#50159) ;
#2276 = PLANE('',#50161) ;
#2277 = PLANE('',#50170) ;
#2278 = PLANE('',#50171) ;
#2279 = PLANE('',#50172) ;
#2280 = PLANE('',#50173) ;
#2281 = PLANE('',#50190) ;
#2282 = PLANE('',#50191) ;
#2283 = PLANE('',#50192) ;
#2284 = PLANE('',#50193) ;
#2285 = PLANE('',#50199) ;
#2286 = PLANE('',#50206) ;
#2287 = PLANE('',#50207) ;
#2288 = PLANE('',#50208) ;
#2289 = PLANE('',#50217) ;
#2290 = PLANE('',#50218) ;
#2291 = PLANE('',#50219) ;
#2292 = PLANE('',#50226) ;
#2293 = PLANE('',#50227) ;
#2294 = PLANE('',#50228) ;
#2295 = PLANE('',#50245) ;
#2296 = PLANE('',#50246) ;
#2297 = PLANE('',#50247) ;
#2298 = PLANE('',#50248) ;
#2299 = PLANE('',#50249) ;
#2300 = PLANE('',#50331) ;
#2301 = PLANE('',#50340) ;
#2302 = PLANE('',#50347) ;
#2303 = PLANE('',#50348) ;
#2304 = PLANE('',#50354) ;
#2305 = PLANE('',#50366) ;
#2306 = PLANE('',#50477) ;
#2307 = PLANE('',#50481) ;
#2308 = PLANE('',#50484) ;
#2309 = PLANE('',#50487) ;
#2310 = PLANE('',#50490) ;
#2311 = PLANE('',#50493) ;
#2312 = PLANE('',#50503) ;
#2313 = PLANE('',#50519) ;
#2314 = PLANE('',#50525) ;
#2315 = PLANE('',#50534) ;
#2316 = PLANE('',#50540) ;
#2317 = PLANE('',#50555) ;
#2318 = PLANE('',#50560) ;
#2319 = PLANE('',#50633) ;
#2320 = PLANE('',#50638) ;
#2321 = PLANE('',#50649) ;
#2322 = PLANE('',#50658) ;
#2323 = PLANE('',#50678) ;
#2324 = PLANE('',#50681) ;
#2325 = PLANE('',#50684) ;
#2326 = PLANE('',#50687) ;
#2327 = PLANE('',#50690) ;
#2328 = PLANE('',#50693) ;
#2329 = PLANE('',#50736) ;
#2330 = PLANE('',#50739) ;
#2331 = PLANE('',#50742) ;
#2332 = PLANE('',#50745) ;
#2333 = PLANE('',#50787) ;
#2334 = PLANE('',#50817) ;
#2335 = PLANE('',#50820) ;
#2336 = PLANE('',#50823) ;
#2337 = PLANE('',#50826) ;
#2338 = PLANE('',#50829) ;
#2339 = PLANE('',#50859) ;
#2340 = PLANE('',#50862) ;
#2341 = PLANE('',#50865) ;
#2342 = PLANE('',#50868) ;
#2343 = PLANE('',#50871) ;
#2344 = PLANE('',#50881) ;
#2345 = PLANE('',#50886) ;
#2346 = PLANE('',#50908) ;
#2347 = PLANE('',#50911) ;
#2348 = PLANE('',#50914) ;
#2349 = PLANE('',#50917) ;
#2350 = PLANE('',#50920) ;
#2351 = PLANE('',#50926) ;
#2352 = PLANE('',#50950) ;
#2353 = PLANE('',#50960) ;
#2354 = PLANE('',#51002) ;
#2355 = PLANE('',#51012) ;
#2356 = PLANE('',#51054) ;
#2357 = PLANE('',#51165) ;
#2358 = PLANE('',#51168) ;
#2359 = PLANE('',#51173) ;
#2360 = PLANE('',#51178) ;
#2361 = PLANE('',#51181) ;
#2362 = PLANE('',#51184) ;
#2363 = PLANE('',#51187) ;
#2364 = PLANE('',#51190) ;
#2365 = PLANE('',#51193) ;
#2366 = PLANE('',#51196) ;
#2367 = PLANE('',#51199) ;
#2368 = PLANE('',#51213) ;
#2369 = PLANE('',#51214) ;
#2370 = PLANE('',#51223) ;
#2371 = PLANE('',#51261) ;
#2372 = PLANE('',#51262) ;
#2373 = PLANE('',#51303) ;
#2374 = PLANE('',#51304) ;
#2375 = PLANE('',#51313) ;
#2376 = PLANE('',#51323) ;
#2377 = PLANE('',#51352) ;
#2378 = PLANE('',#51353) ;
#2379 = PLANE('',#51362) ;
#2380 = PLANE('',#51390) ;
#2381 = PLANE('',#51391) ;
#2382 = PLANE('',#51392) ;
#2383 = PLANE('',#51393) ;
#2384 = PLANE('',#51394) ;
#2385 = PLANE('',#51396) ;
#2386 = PLANE('',#51398) ;
#2387 = PLANE('',#51443) ;
#2388 = PLANE('',#51444) ;
#2389 = PLANE('',#51445) ;
#2390 = PLANE('',#51446) ;
#2391 = PLANE('',#51464) ;
#2392 = PLANE('',#51465) ;
#2393 = PLANE('',#51467) ;
#2394 = PLANE('',#51571) ;
#2395 = PLANE('',#51594) ;
#2396 = PLANE('',#51612) ;
#2397 = PLANE('',#51622) ;
#2398 = PLANE('',#51624) ;
#2399 = PLANE('',#51626) ;
#2400 = PLANE('',#51627) ;
#2401 = PLANE('',#51628) ;
#2402 = PLANE('',#51629) ;
#2403 = PLANE('',#51630) ;
#2404 = PLANE('',#51671) ;
#2405 = PLANE('',#51676) ;
#2406 = PLANE('',#51681) ;
#2407 = PLANE('',#51684) ;
#2408 = PLANE('',#51685) ;
#2409 = PLANE('',#51686) ;
#2410 = PLANE('',#51687) ;
#2411 = PLANE('',#51688) ;
#2412 = PLANE('',#51689) ;
#2413 = PLANE('',#51690) ;
#2414 = PLANE('',#51691) ;
#2415 = PLANE('',#51692) ;
#2416 = PLANE('',#51693) ;
#2417 = PLANE('',#51694) ;
#2418 = PLANE('',#51695) ;
#2419 = PLANE('',#51696) ;
#2420 = PLANE('',#51697) ;
#2421 = PLANE('',#51698) ;
#2422 = PLANE('',#51699) ;
#2423 = PLANE('',#51700) ;
#2424 = PLANE('',#51704) ;
#2425 = PLANE('',#51705) ;
#2426 = PLANE('',#51708) ;
#2427 = PLANE('',#51726) ;
#2428 = PLANE('',#51727) ;
#2429 = PLANE('',#51728) ;
#2430 = PLANE('',#51729) ;
#2431 = PLANE('',#51730) ;
#2432 = PLANE('',#51731) ;
#2433 = PLANE('',#51732) ;
#2434 = PLANE('',#51733) ;
#2435 = PLANE('',#51746) ;
#2436 = PLANE('',#51757) ;
#2437 = PLANE('',#51760) ;
#2438 = PLANE('',#51775) ;
#2439 = PLANE('',#51785) ;
#2440 = PLANE('',#51799) ;
#2441 = PLANE('',#51810) ;
#2442 = PLANE('',#51824) ;
#2443 = PLANE('',#51834) ;
#2444 = PLANE('',#51846) ;
#2445 = PLANE('',#51849) ;
#2446 = PLANE('',#51852) ;
#2447 = PLANE('',#51854) ;
#2448 = PLANE('',#51861) ;
#2449 = PLANE('',#51863) ;
#2450 = PLANE('',#51864) ;
#2451 = PLANE('',#51876) ;
#2452 = PLANE('',#51886) ;
#2453 = PLANE('',#51896) ;
#2454 = PLANE('',#51906) ;
#2455 = PLANE('',#51916) ;
#2456 = PLANE('',#51926) ;
#2457 = PLANE('',#51936) ;
#2458 = PLANE('',#51946) ;
#2459 = PLANE('',#51948) ;
#2460 = PLANE('',#51951) ;
#2461 = PLANE('',#51954) ;
#2462 = PLANE('',#51957) ;
#2463 = PLANE('',#51959) ;
#2464 = PLANE('',#51960) ;
#2465 = PLANE('',#51961) ;
#2466 = PLANE('',#51963) ;
#2467 = PLANE('',#51964) ;
#2468 = PLANE('',#51966) ;
#2469 = PLANE('',#51967) ;
#2470 = PLANE('',#51968) ;
#2471 = PLANE('',#51969) ;
#2472 = PLANE('',#51970) ;
#2473 = PLANE('',#51971) ;
#2474 = PLANE('',#51972) ;
#2475 = PLANE('',#51973) ;
#2476 = PLANE('',#51975) ;
#2477 = PLANE('',#51976) ;
#2478 = PLANE('',#51977) ;
#2479 = PLANE('',#51978) ;
#2480 = PLANE('',#51979) ;
#2481 = PLANE('',#51980) ;
#2482 = PLANE('',#51992) ;
#2483 = PLANE('',#52004) ;
#2484 = PLANE('',#52012) ;
#2485 = PLANE('',#52016) ;
#2486 = PLANE('',#52142) ;
#2487 = PLANE('',#52143) ;
#2488 = PLANE('',#52145) ;
#2489 = PLANE('',#52147) ;
#2490 = PLANE('',#52149) ;
#2491 = PLANE('',#52151) ;
#2492 = PLANE('',#52153) ;
#2493 = PLANE('',#52162) ;
#2494 = PLANE('',#52163) ;
#2495 = PLANE('',#52164) ;
#2496 = PLANE('',#52165) ;
#2497 = PLANE('',#52166) ;
#2498 = PLANE('',#52167) ;
#2499 = PLANE('',#52177) ;
#2500 = PLANE('',#52178) ;
#2501 = PLANE('',#52213) ;
#2502 = PLANE('',#52214) ;
#2503 = PLANE('',#52215) ;
#2504 = PLANE('',#52216) ;
#2505 = PLANE('',#52217) ;
#2506 = PLANE('',#52218) ;
#2507 = PLANE('',#52228) ;
#2508 = PLANE('',#52253) ;
#2509 = PLANE('',#52254) ;
#2510 = PLANE('',#52255) ;
#2511 = PLANE('',#52256) ;
#2512 = PLANE('',#52257) ;
#2513 = PLANE('',#52258) ;
#2514 = PLANE('',#52259) ;
#2515 = PLANE('',#52285) ;
#2516 = PLANE('',#52286) ;
#2517 = PLANE('',#52287) ;
#2518 = PLANE('',#52288) ;
#2519 = PLANE('',#52291) ;
#2520 = PLANE('',#52292) ;
#2521 = PLANE('',#52293) ;
#2522 = PLANE('',#52319) ;
#2523 = PLANE('',#52320) ;
#2524 = PLANE('',#52321) ;
#2525 = PLANE('',#52322) ;
#2526 = PLANE('',#52323) ;
#2527 = PLANE('',#52324) ;
#2528 = PLANE('',#52325) ;
#2529 = PLANE('',#52334) ;
#2530 = PLANE('',#52359) ;
#2531 = PLANE('',#52360) ;
#2532 = PLANE('',#52361) ;
#2533 = PLANE('',#52362) ;
#2534 = PLANE('',#52366) ;
#2535 = PLANE('',#52367) ;
#2536 = PLANE('',#52368) ;
#2537 = PLANE('',#52394) ;
#2538 = PLANE('',#52395) ;
#2539 = PLANE('',#52396) ;
#2540 = PLANE('',#52397) ;
#2541 = PLANE('',#52398) ;
#2542 = PLANE('',#52399) ;
#2543 = PLANE('',#52400) ;
#2544 = PLANE('',#52409) ;
#2545 = PLANE('',#52434) ;
#2546 = PLANE('',#52435) ;
#2547 = PLANE('',#52436) ;
#2548 = PLANE('',#52437) ;
#2549 = PLANE('',#52441) ;
#2550 = PLANE('',#52442) ;
#2551 = PLANE('',#52443) ;
#2552 = PLANE('',#52491) ;
#2553 = PLANE('',#52492) ;
#2554 = PLANE('',#52493) ;
#2555 = PLANE('',#52494) ;
#2556 = PLANE('',#52495) ;
#2557 = PLANE('',#52520) ;
#2558 = PLANE('',#52521) ;
#2559 = PLANE('',#52522) ;
#2560 = PLANE('',#52523) ;
#2561 = PLANE('',#52524) ;
#2562 = PLANE('',#52525) ;
#2563 = PLANE('',#52532) ;
#2564 = PLANE('',#52533) ;
#2565 = PLANE('',#52534) ;
#2566 = PLANE('',#52535) ;
#2567 = PLANE('',#52536) ;
#2568 = PLANE('',#52537) ;
#2569 = PLANE('',#52538) ;
#2570 = PLANE('',#52539) ;
#2571 = PLANE('',#52540) ;
#2572 = PLANE('',#52541) ;
#2573 = PLANE('',#52542) ;
#2574 = PLANE('',#52543) ;
#2575 = PLANE('',#52544) ;
#2576 = PLANE('',#52569) ;
#2577 = PLANE('',#52572) ;
#2578 = PLANE('',#52586) ;
#2579 = PLANE('',#52589) ;
#2580 = PLANE('',#52591) ;
#2581 = PLANE('',#52592) ;
#2582 = PLANE('',#52609) ;
#2583 = PLANE('',#52623) ;
#2584 = PLANE('',#52638) ;
#2585 = PLANE('',#52641) ;
#2586 = PLANE('',#52642) ;
#2587 = PLANE('',#52648) ;
#2588 = PLANE('',#52654) ;
#2589 = PLANE('',#52658) ;
#2590 = PLANE('',#52667) ;
#2591 = PLANE('',#52696) ;
#2592 = PLANE('',#52699) ;
#2593 = PLANE('',#52735) ;
#2594 = PLANE('',#52743) ;
#2595 = PLANE('',#52753) ;
#2596 = PLANE('',#52795) ;
#2597 = PLANE('',#52798) ;
#2598 = PLANE('',#52819) ;
#2599 = PLANE('',#52821) ;
#2600 = PLANE('',#52833) ;
#2601 = PLANE('',#52834) ;
#2602 = PLANE('',#52843) ;
#2603 = PLANE('',#52862) ;
#2604 = PLANE('',#52927) ;
#2605 = PLANE('',#52941) ;
#2606 = PLANE('',#52942) ;
#2607 = PLANE('',#52990) ;
#2608 = PLANE('',#52992) ;
#2609 = PLANE('',#52996) ;
#2610 = PLANE('',#52999) ;
#2611 = PLANE('',#53005) ;
#2612 = PLANE('',#53093) ;
#2613 = PLANE('',#53097) ;
#2614 = PLANE('',#53098) ;
#2615 = PLANE('',#53099) ;
#2616 = PLANE('',#53100) ;
#2617 = PLANE('',#53101) ;
#2618 = PLANE('',#53106) ;
#2619 = PLANE('',#53143) ;
#2620 = PLANE('',#53150) ;
#2621 = PLANE('',#53214) ;
#2622 = PLANE('',#53217) ;
#2623 = PLANE('',#53220) ;
#2624 = PLANE('',#53269) ;
#2625 = PLANE('',#53270) ;
#2626 = PLANE('',#53272) ;
#2627 = PLANE('',#53278) ;
#2628 = PLANE('',#53280) ;
#2629 = PLANE('',#53285) ;
#2630 = PLANE('',#53286) ;
#2631 = PLANE('',#53314) ;
#2632 = PLANE('',#53316) ;
#2633 = PLANE('',#53327) ;
#2634 = PLANE('',#53328) ;
#2635 = PLANE('',#53329) ;
#2636 = PLANE('',#53350) ;
#2637 = PLANE('',#53359) ;
#2638 = PLANE('',#53368) ;
#2639 = PLANE('',#53372) ;
#2640 = PLANE('',#53374) ;
#2641 = PLANE('',#53375) ;
#2642 = PLANE('',#53380) ;
#2643 = PLANE('',#53382) ;
#2644 = PLANE('',#53384) ;
#2645 = PLANE('',#53387) ;
#2646 = PLANE('',#53393) ;
#2647 = PLANE('',#53394) ;
#2648 = PLANE('',#53395) ;
#2649 = PLANE('',#53396) ;
#2650 = PLANE('',#53407) ;
#2651 = PLANE('',#53408) ;
#2652 = PLANE('',#53409) ;
#2653 = PLANE('',#53410) ;
#2654 = PLANE('',#53411) ;
#2655 = PLANE('',#53412) ;
#2656 = PLANE('',#53413) ;
#2657 = PLANE('',#53414) ;
#2658 = PLANE('',#53423) ;
#2659 = PLANE('',#53424) ;
#2660 = PLANE('',#53425) ;
#2661 = PLANE('',#53426) ;
#2662 = PLANE('',#53427) ;
#2663 = PLANE('',#53436) ;
#2664 = PLANE('',#53437) ;
#2665 = PLANE('',#53438) ;
#2666 = PLANE('',#53453) ;
#2667 = PLANE('',#53454) ;
#2668 = PLANE('',#53455) ;
#2669 = PLANE('',#53456) ;
#2670 = PLANE('',#53457) ;
#2671 = PLANE('',#53466) ;
#2672 = PLANE('',#53467) ;
#2673 = PLANE('',#53468) ;
#2674 = PLANE('',#53483) ;
#2675 = PLANE('',#53484) ;
#2676 = PLANE('',#53485) ;
#2677 = PLANE('',#53486) ;
#2678 = PLANE('',#53487) ;
#2679 = PLANE('',#53496) ;
#2680 = PLANE('',#53497) ;
#2681 = PLANE('',#53498) ;
#2682 = PLANE('',#53525) ;
#2683 = PLANE('',#53528) ;
#2684 = PLANE('',#53529) ;
#2685 = PLANE('',#53530) ;
#2686 = PLANE('',#53531) ;
#2687 = PLANE('',#53532) ;
#2688 = PLANE('',#53561) ;
#2689 = PLANE('',#53562) ;
#2690 = PLANE('',#53563) ;
#2691 = PLANE('',#53564) ;
#2692 = PLANE('',#53565) ;
#2693 = PLANE('',#53566) ;
#2694 = PLANE('',#53575) ;
#2695 = PLANE('',#53584) ;
#2696 = PLANE('',#53585) ;
#2697 = PLANE('',#53600) ;
#2698 = PLANE('',#53601) ;
#2699 = PLANE('',#53602) ;
#2700 = PLANE('',#53603) ;
#2701 = PLANE('',#53617) ;
#2702 = PLANE('',#53632) ;
#2703 = PLANE('',#53633) ;
#2704 = PLANE('',#53664) ;
#2705 = PLANE('',#53666) ;
#2706 = PLANE('',#53667) ;
#2707 = PLANE('',#53691) ;
#2708 = PLANE('',#53692) ;
#2709 = PLANE('',#53693) ;
#2710 = PLANE('',#53695) ;
#2711 = PLANE('',#53696) ;
#2712 = PLANE('',#53697) ;
#2713 = PLANE('',#53698) ;
#2714 = PLANE('',#53699) ;
#2715 = PLANE('',#53700) ;
#2716 = PLANE('',#53701) ;
#2717 = PLANE('',#53702) ;
#2718 = PLANE('',#53703) ;
#2719 = PLANE('',#53706) ;
#2720 = PLANE('',#53709) ;
#2721 = PLANE('',#53712) ;
#2722 = PLANE('',#53713) ;
#2723 = PLANE('',#53714) ;
#2724 = PLANE('',#53715) ;
#2725 = PLANE('',#53719) ;
#2726 = PLANE('',#53720) ;
#2727 = PLANE('',#53721) ;
#2728 = PLANE('',#53722) ;
#2729 = PLANE('',#53723) ;
#2730 = PLANE('',#53724) ;
#2731 = PLANE('',#53725) ;
#2732 = PLANE('',#53726) ;
#2733 = PLANE('',#53727) ;
#2734 = PLANE('',#53730) ;
#2735 = PLANE('',#53731) ;
#2736 = PLANE('',#53732) ;
#2737 = PLANE('',#53735) ;
#2738 = PLANE('',#53736) ;
#2739 = PLANE('',#53737) ;
#2740 = PLANE('',#53738) ;
#2741 = PLANE('',#53739) ;
#2742 = PLANE('',#53742) ;
#2743 = PLANE('',#53744) ;
#2744 = PLANE('',#53745) ;
#2745 = PLANE('',#53746) ;
#2746 = PLANE('',#53747) ;
#2747 = PLANE('',#53748) ;
#2748 = PLANE('',#53824) ;
#2749 = PLANE('',#53826) ;
#2750 = PLANE('',#53828) ;
#2751 = PLANE('',#53829) ;
#2752 = PLANE('',#53834) ;
#2753 = PLANE('',#53837) ;
#2754 = PLANE('',#53838) ;
#2755 = PLANE('',#53841) ;
#2756 = PLANE('',#53844) ;
#2757 = PLANE('',#53845) ;
#2758 = PLANE('',#53846) ;
#2759 = PLANE('',#53848) ;
#2760 = PLANE('',#53853) ;
#2761 = PLANE('',#53856) ;
#2762 = PLANE('',#53859) ;
#2763 = PLANE('',#53862) ;
#2764 = PLANE('',#53865) ;
#2765 = PLANE('',#53866) ;
#2766 = PLANE('',#53869) ;
#2767 = PLANE('',#53872) ;
#2768 = PLANE('',#53875) ;
#2769 = PLANE('',#53878) ;
#2770 = PLANE('',#53881) ;
#2771 = PLANE('',#53884) ;
#2772 = PLANE('',#53885) ;
#2773 = PLANE('',#53886) ;
#2774 = PLANE('',#53889) ;
#2775 = PLANE('',#53892) ;
#2776 = PLANE('',#53897) ;
#2777 = PLANE('',#53900) ;
#2778 = PLANE('',#53901) ;
#2779 = PLANE('',#53904) ;
#2780 = PLANE('',#53907) ;
#2781 = PLANE('',#53908) ;
#2782 = PLANE('',#53911) ;
#2783 = PLANE('',#53914) ;
#2784 = PLANE('',#53915) ;
#2785 = PLANE('',#53916) ;
#2786 = PLANE('',#53917) ;
#2787 = PLANE('',#53920) ;
#2788 = PLANE('',#53923) ;
#2789 = PLANE('',#53924) ;
#2790 = PLANE('',#53925) ;
#2791 = PLANE('',#53928) ;
#2792 = PLANE('',#53931) ;
#2793 = PLANE('',#53932) ;
#2794 = PLANE('',#53935) ;
#2795 = PLANE('',#53936) ;
#2796 = PLANE('',#53937) ;
#2797 = PLANE('',#53938) ;
#2798 = PLANE('',#53939) ;
#2799 = PLANE('',#53942) ;
#2800 = PLANE('',#53946) ;
#2801 = PLANE('',#53947) ;
#2802 = PLANE('',#53950) ;
#2803 = PLANE('',#53953) ;
#2804 = PLANE('',#53954) ;
#2805 = PLANE('',#53957) ;
#2806 = PLANE('',#53960) ;
#2807 = PLANE('',#53963) ;
#2808 = PLANE('',#53964) ;
#2809 = PLANE('',#53965) ;
#2810 = PLANE('',#53968) ;
#2811 = PLANE('',#53969) ;
#2812 = PLANE('',#53970) ;
#2813 = PLANE('',#53971) ;
#2814 = PLANE('',#53972) ;
#2815 = PLANE('',#53973) ;
#2816 = PLANE('',#53974) ;
#2817 = PLANE('',#53975) ;
#2818 = PLANE('',#53976) ;
#2819 = PLANE('',#53978) ;
#2820 = PLANE('',#53980) ;
#2821 = PLANE('',#53981) ;
#2822 = PLANE('',#53985) ;
#2823 = PLANE('',#53987) ;
#2824 = PLANE('',#53988) ;
#2825 = PLANE('',#53989) ;
#2826 = PLANE('',#53990) ;
#2827 = PLANE('',#53991) ;
#2828 = PLANE('',#53993) ;
#2829 = PLANE('',#53995) ;
#2830 = PLANE('',#53996) ;
#2831 = PLANE('',#53999) ;
#2832 = PLANE('',#54001) ;
#2833 = PLANE('',#54003) ;
#2834 = PLANE('',#54004) ;
#2835 = PLANE('',#54006) ;
#2836 = PLANE('',#54007) ;
#2837 = PLANE('',#54008) ;
#2838 = PLANE('',#54009) ;
#2839 = PLANE('',#54010) ;
#2840 = PLANE('',#54012) ;
#2841 = PLANE('',#54013) ;
#2842 = PLANE('',#54014) ;
#2843 = PLANE('',#54015) ;
#2844 = PLANE('',#54016) ;
#2845 = PLANE('',#54017) ;
#2846 = PLANE('',#54018) ;
#2847 = PLANE('',#54019) ;
#2848 = PLANE('',#54020) ;
#2849 = PLANE('',#54021) ;
#2850 = PLANE('',#54022) ;
#2851 = PLANE('',#54023) ;
#2852 = PLANE('',#54024) ;
#2853 = PLANE('',#54025) ;
#2854 = PLANE('',#54026) ;
#2855 = PLANE('',#54039) ;
#2856 = PLANE('',#54040) ;
#2857 = PLANE('',#54041) ;
#2858 = PLANE('',#54047) ;
#2859 = PLANE('',#54052) ;
#2860 = PLANE('',#54053) ;
#2861 = PLANE('',#54055) ;
#2862 = PLANE('',#54217) ;
#2863 = PLANE('',#54220) ;
#2864 = PLANE('',#54223) ;
#2865 = PLANE('',#54226) ;
#2866 = PLANE('',#54229) ;
#2867 = PLANE('',#54232) ;
#2868 = PLANE('',#54235) ;
#2869 = PLANE('',#54238) ;
#2870 = PLANE('',#54241) ;
#2871 = PLANE('',#54244) ;
#2872 = PLANE('',#54247) ;
#2873 = PLANE('',#54250) ;
#2874 = PLANE('',#54253) ;
#2875 = PLANE('',#54256) ;
#2876 = PLANE('',#54259) ;
#2877 = PLANE('',#54262) ;
#2878 = PLANE('',#54265) ;
#2879 = PLANE('',#54268) ;
#2880 = PLANE('',#54271) ;
#2881 = PLANE('',#54274) ;
#2882 = PLANE('',#54277) ;
#2883 = PLANE('',#54279) ;
#2884 = PLANE('',#54281) ;
#2885 = PLANE('',#54283) ;
#2886 = PLANE('',#54285) ;
#2887 = PLANE('',#54287) ;
#2888 = PLANE('',#54289) ;
#2889 = PLANE('',#54291) ;
#2890 = PLANE('',#54293) ;
#2891 = PLANE('',#54295) ;
#2892 = PLANE('',#54297) ;
#2893 = PLANE('',#54299) ;
#2894 = PLANE('',#54301) ;
#2895 = PLANE('',#54303) ;
#2896 = PLANE('',#54305) ;
#2897 = PLANE('',#54307) ;
#2898 = PLANE('',#54309) ;
#2899 = PLANE('',#54311) ;
#2900 = PLANE('',#54313) ;
#2901 = PLANE('',#54319) ;
#2902 = PLANE('',#54363) ;
#2903 = PLANE('',#54365) ;
#2904 = PLANE('',#54367) ;
#2905 = PLANE('',#54369) ;
#2906 = PLANE('',#54371) ;
#2907 = PLANE('',#54373) ;
#2908 = PLANE('',#54375) ;
#2909 = PLANE('',#54377) ;
#2910 = PLANE('',#54379) ;
#2911 = PLANE('',#54381) ;
#2912 = PLANE('',#54383) ;
#2913 = PLANE('',#54385) ;
#2914 = PLANE('',#54387) ;
#2915 = PLANE('',#54389) ;
#2916 = PLANE('',#54391) ;
#2917 = PLANE('',#54393) ;
#2918 = PLANE('',#54395) ;
#2919 = PLANE('',#54397) ;
#2920 = PLANE('',#54399) ;
#2921 = PLANE('',#54401) ;
#2922 = PLANE('',#54504) ;
#2923 = PLANE('',#54506) ;
#2924 = PLANE('',#54507) ;
#2925 = PLANE('',#54508) ;
#2926 = PLANE('',#54510) ;
#2927 = PLANE('',#54511) ;
#2928 = PLANE('',#54513) ;
#2929 = PLANE('',#54514) ;
#2930 = PLANE('',#54516) ;
#2931 = PLANE('',#54517) ;
#2932 = PLANE('',#54519) ;
#2933 = PLANE('',#54520) ;
#2934 = PLANE('',#54522) ;
#2935 = PLANE('',#54523) ;
#2936 = PLANE('',#54525) ;
#2937 = PLANE('',#54526) ;
#2938 = PLANE('',#54528) ;
#2939 = PLANE('',#54529) ;
#2940 = PLANE('',#54531) ;
#2941 = PLANE('',#54532) ;
#2942 = PLANE('',#54549) ;
#2943 = PLANE('',#54554) ;
#2944 = PLANE('',#54555) ;
#2945 = PLANE('',#54557) ;
#2946 = PLANE('',#54719) ;
#2947 = PLANE('',#54722) ;
#2948 = PLANE('',#54725) ;
#2949 = PLANE('',#54728) ;
#2950 = PLANE('',#54731) ;
#2951 = PLANE('',#54734) ;
#2952 = PLANE('',#54737) ;
#2953 = PLANE('',#54740) ;
#2954 = PLANE('',#54743) ;
#2955 = PLANE('',#54746) ;
#2956 = PLANE('',#54749) ;
#2957 = PLANE('',#54752) ;
#2958 = PLANE('',#54755) ;
#2959 = PLANE('',#54758) ;
#2960 = PLANE('',#54761) ;
#2961 = PLANE('',#54764) ;
#2962 = PLANE('',#54767) ;
#2963 = PLANE('',#54770) ;
#2964 = PLANE('',#54773) ;
#2965 = PLANE('',#54776) ;
#2966 = PLANE('',#54779) ;
#2967 = PLANE('',#54781) ;
#2968 = PLANE('',#54783) ;
#2969 = PLANE('',#54785) ;
#2970 = PLANE('',#54787) ;
#2971 = PLANE('',#54789) ;
#2972 = PLANE('',#54791) ;
#2973 = PLANE('',#54793) ;
#2974 = PLANE('',#54795) ;
#2975 = PLANE('',#54797) ;
#2976 = PLANE('',#54799) ;
#2977 = PLANE('',#54801) ;
#2978 = PLANE('',#54803) ;
#2979 = PLANE('',#54805) ;
#2980 = PLANE('',#54807) ;
#2981 = PLANE('',#54809) ;
#2982 = PLANE('',#54811) ;
#2983 = PLANE('',#54813) ;
#2984 = PLANE('',#54815) ;
#2985 = PLANE('',#54821) ;
#2986 = PLANE('',#54865) ;
#2987 = PLANE('',#54867) ;
#2988 = PLANE('',#54869) ;
#2989 = PLANE('',#54871) ;
#2990 = PLANE('',#54873) ;
#2991 = PLANE('',#54875) ;
#2992 = PLANE('',#54877) ;
#2993 = PLANE('',#54879) ;
#2994 = PLANE('',#54881) ;
#2995 = PLANE('',#54883) ;
#2996 = PLANE('',#54885) ;
#2997 = PLANE('',#54887) ;
#2998 = PLANE('',#54889) ;
#2999 = PLANE('',#54891) ;
#3000 = PLANE('',#54893) ;
#3001 = PLANE('',#54895) ;
#3002 = PLANE('',#54897) ;
#3003 = PLANE('',#54899) ;
#3004 = PLANE('',#54901) ;
#3005 = PLANE('',#54903) ;
#3006 = PLANE('',#55006) ;
#3007 = PLANE('',#55008) ;
#3008 = PLANE('',#55009) ;
#3009 = PLANE('',#55010) ;
#3010 = PLANE('',#55012) ;
#3011 = PLANE('',#55013) ;
#3012 = PLANE('',#55015) ;
#3013 = PLANE('',#55016) ;
#3014 = PLANE('',#55018) ;
#3015 = PLANE('',#55019) ;
#3016 = PLANE('',#55021) ;
#3017 = PLANE('',#55022) ;
#3018 = PLANE('',#55024) ;
#3019 = PLANE('',#55025) ;
#3020 = PLANE('',#55027) ;
#3021 = PLANE('',#55028) ;
#3022 = PLANE('',#55030) ;
#3023 = PLANE('',#55031) ;
#3024 = PLANE('',#55033) ;
#3025 = PLANE('',#55034) ;
#3026 = PLANE('',#55070) ;
#3027 = PLANE('',#55071) ;
#3028 = PLANE('',#55072) ;
#3029 = PLANE('',#55073) ;
#3030 = PLANE('',#55074) ;
#3031 = PLANE('',#55075) ;
#3032 = LINE('',#69895,#6246) ;
#3033 = LINE('',#69899,#6247) ;
#3034 = LINE('',#69903,#6248) ;
#3035 = LINE('',#69907,#6249) ;
#3036 = LINE('',#69911,#6250) ;
#3037 = LINE('',#69915,#6251) ;
#3038 = LINE('',#69919,#6252) ;
#3039 = LINE('',#69923,#6253) ;
#3040 = LINE('',#69927,#6254) ;
#3041 = LINE('',#69931,#6255) ;
#3042 = LINE('',#69935,#6256) ;
#3043 = LINE('',#69939,#6257) ;
#3044 = LINE('',#69943,#6258) ;
#3045 = LINE('',#69947,#6259) ;
#3046 = LINE('',#69951,#6260) ;
#3047 = LINE('',#69955,#6261) ;
#3048 = LINE('',#69959,#6262) ;
#3049 = LINE('',#69963,#6263) ;
#3050 = LINE('',#69967,#6264) ;
#3051 = LINE('',#69971,#6265) ;
#3052 = LINE('',#69975,#6266) ;
#3053 = LINE('',#69979,#6267) ;
#3054 = LINE('',#69983,#6268) ;
#3055 = LINE('',#69987,#6269) ;
#3056 = LINE('',#69991,#6270) ;
#3057 = LINE('',#69995,#6271) ;
#3058 = LINE('',#69999,#6272) ;
#3059 = LINE('',#70003,#6273) ;
#3060 = LINE('',#70007,#6274) ;
#3061 = LINE('',#70011,#6275) ;
#3062 = LINE('',#70015,#6276) ;
#3063 = LINE('',#70019,#6277) ;
#3064 = LINE('',#70023,#6278) ;
#3065 = LINE('',#70027,#6279) ;
#3066 = LINE('',#70031,#6280) ;
#3067 = LINE('',#70035,#6281) ;
#3068 = LINE('',#70039,#6282) ;
#3069 = LINE('',#70043,#6283) ;
#3070 = LINE('',#70047,#6284) ;
#3071 = LINE('',#70051,#6285) ;
#3072 = LINE('',#70055,#6286) ;
#3073 = LINE('',#70063,#6287) ;
#3074 = LINE('',#70066,#6288) ;
#3075 = LINE('',#70072,#6289) ;
#3076 = LINE('',#70075,#6290) ;
#3077 = LINE('',#70085,#6291) ;
#3078 = LINE('',#70086,#6292) ;
#3079 = LINE('',#70091,#6293) ;
#3080 = LINE('',#70094,#6294) ;
#3081 = LINE('',#70100,#6295) ;
#3082 = LINE('',#70103,#6296) ;
#3083 = LINE('',#70113,#6297) ;
#3084 = LINE('',#70114,#6298) ;
#3085 = LINE('',#70119,#6299) ;
#3086 = LINE('',#70122,#6300) ;
#3087 = LINE('',#70128,#6301) ;
#3088 = LINE('',#70131,#6302) ;
#3089 = LINE('',#70141,#6303) ;
#3090 = LINE('',#70142,#6304) ;
#3091 = LINE('',#70147,#6305) ;
#3092 = LINE('',#70150,#6306) ;
#3093 = LINE('',#70163,#6307) ;
#3094 = LINE('',#70164,#6308) ;
#3095 = LINE('',#70168,#6309) ;
#3096 = LINE('',#70169,#6310) ;
#3097 = LINE('',#70188,#6311) ;
#3098 = LINE('',#70190,#6312) ;
#3099 = LINE('',#70191,#6313) ;
#3100 = LINE('',#70194,#6314) ;
#3101 = LINE('',#70198,#6315) ;
#3102 = LINE('',#70199,#6316) ;
#3103 = LINE('',#70202,#6317) ;
#3104 = LINE('',#70206,#6318) ;
#3105 = LINE('',#70207,#6319) ;
#3106 = LINE('',#70210,#6320) ;
#3107 = LINE('',#70214,#6321) ;
#3108 = LINE('',#70215,#6322) ;
#3109 = LINE('',#70218,#6323) ;
#3110 = LINE('',#70222,#6324) ;
#3111 = LINE('',#70223,#6325) ;
#3112 = LINE('',#70226,#6326) ;
#3113 = LINE('',#70230,#6327) ;
#3114 = LINE('',#70231,#6328) ;
#3115 = LINE('',#70234,#6329) ;
#3116 = LINE('',#72403,#6330) ;
#3117 = LINE('',#72420,#6331) ;
#3118 = LINE('',#72631,#6332) ;
#3119 = LINE('',#72662,#6333) ;
#3120 = LINE('',#72681,#6334) ;
#3121 = LINE('',#72714,#6335) ;
#3122 = LINE('',#72941,#6336) ;
#3123 = LINE('',#72956,#6337) ;
#3124 = LINE('',#72975,#6338) ;
#3125 = LINE('',#73008,#6339) ;
#3126 = LINE('',#73232,#6340) ;
#3127 = LINE('',#73247,#6341) ;
#3128 = LINE('',#73266,#6342) ;
#3129 = LINE('',#73299,#6343) ;
#3130 = LINE('',#73435,#6344) ;
#3131 = LINE('',#73450,#6345) ;
#3132 = LINE('',#73469,#6346) ;
#3133 = LINE('',#73502,#6347) ;
#3134 = LINE('',#73711,#6348) ;
#3135 = LINE('',#73726,#6349) ;
#3136 = LINE('',#73745,#6350) ;
#3137 = LINE('',#73778,#6351) ;
#3138 = LINE('',#74002,#6352) ;
#3139 = LINE('',#74017,#6353) ;
#3140 = LINE('',#74036,#6354) ;
#3141 = LINE('',#74069,#6355) ;
#3142 = LINE('',#74296,#6356) ;
#3143 = LINE('',#74311,#6357) ;
#3144 = LINE('',#74330,#6358) ;
#3145 = LINE('',#74363,#6359) ;
#3146 = LINE('',#74572,#6360) ;
#3147 = LINE('',#74587,#6361) ;
#3148 = LINE('',#74606,#6362) ;
#3149 = LINE('',#74639,#6363) ;
#3150 = LINE('',#74775,#6364) ;
#3151 = LINE('',#74790,#6365) ;
#3152 = LINE('',#74809,#6366) ;
#3153 = LINE('',#74842,#6367) ;
#3154 = LINE('',#75054,#6368) ;
#3155 = LINE('',#75069,#6369) ;
#3156 = LINE('',#75142,#6370) ;
#3157 = LINE('',#75154,#6371) ;
#3158 = LINE('',#75158,#6372) ;
#3159 = LINE('',#75162,#6373) ;
#3160 = LINE('',#75166,#6374) ;
#3161 = LINE('',#75170,#6375) ;
#3162 = LINE('',#75174,#6376) ;
#3163 = LINE('',#75178,#6377) ;
#3164 = LINE('',#75182,#6378) ;
#3165 = LINE('',#75186,#6379) ;
#3166 = LINE('',#75190,#6380) ;
#3167 = LINE('',#75194,#6381) ;
#3168 = LINE('',#75197,#6382) ;
#3169 = LINE('',#75200,#6383) ;
#3170 = LINE('',#75203,#6384) ;
#3171 = LINE('',#75216,#6385) ;
#3172 = LINE('',#75217,#6386) ;
#3173 = LINE('',#75220,#6387) ;
#3174 = LINE('',#75223,#6388) ;
#3175 = LINE('',#75230,#6389) ;
#3176 = LINE('',#75253,#6390) ;
#3177 = LINE('',#75261,#6391) ;
#3178 = LINE('',#75263,#6392) ;
#3179 = LINE('',#75264,#6393) ;
#3180 = LINE('',#75272,#6394) ;
#3181 = LINE('',#75278,#6395) ;
#3182 = LINE('',#75280,#6396) ;
#3183 = LINE('',#75282,#6397) ;
#3184 = LINE('',#75283,#6398) ;
#3185 = LINE('',#75285,#6399) ;
#3186 = LINE('',#75389,#6400) ;
#3187 = LINE('',#75390,#6401) ;
#3188 = LINE('',#75500,#6402) ;
#3189 = LINE('',#75502,#6403) ;
#3190 = LINE('',#75503,#6404) ;
#3191 = LINE('',#75515,#6405) ;
#3192 = LINE('',#75648,#6406) ;
#3193 = LINE('',#75649,#6407) ;
#3194 = LINE('',#75755,#6408) ;
#3195 = LINE('',#75756,#6409) ;
#3196 = LINE('',#75788,#6410) ;
#3197 = LINE('',#75791,#6411) ;
#3198 = LINE('',#75794,#6412) ;
#3199 = LINE('',#75795,#6413) ;
#3200 = LINE('',#75811,#6414) ;
#3201 = LINE('',#75828,#6415) ;
#3202 = LINE('',#75836,#6416) ;
#3203 = LINE('',#75840,#6417) ;
#3204 = LINE('',#75842,#6418) ;
#3205 = LINE('',#75862,#6419) ;
#3206 = LINE('',#75890,#6420) ;
#3207 = LINE('',#75894,#6421) ;
#3208 = LINE('',#75907,#6422) ;
#3209 = LINE('',#75943,#6423) ;
#3210 = LINE('',#75955,#6424) ;
#3211 = LINE('',#75958,#6425) ;
#3212 = LINE('',#75965,#6426) ;
#3213 = LINE('',#76057,#6427) ;
#3214 = LINE('',#76165,#6428) ;
#3215 = LINE('',#76173,#6429) ;
#3216 = LINE('',#76183,#6430) ;
#3217 = LINE('',#76197,#6431) ;
#3218 = LINE('',#76201,#6432) ;
#3219 = LINE('',#76202,#6433) ;
#3220 = LINE('',#76210,#6434) ;
#3221 = LINE('',#76215,#6435) ;
#3222 = LINE('',#76252,#6436) ;
#3223 = LINE('',#76442,#6437) ;
#3224 = LINE('',#76620,#6438) ;
#3225 = LINE('',#76624,#6439) ;
#3226 = LINE('',#76673,#6440) ;
#3227 = LINE('',#76680,#6441) ;
#3228 = LINE('',#76683,#6442) ;
#3229 = LINE('',#76706,#6443) ;
#3230 = LINE('',#76721,#6444) ;
#3231 = LINE('',#76724,#6445) ;
#3232 = LINE('',#76726,#6446) ;
#3233 = LINE('',#76759,#6447) ;
#3234 = LINE('',#76770,#6448) ;
#3235 = LINE('',#76779,#6449) ;
#3236 = LINE('',#76780,#6450) ;
#3237 = LINE('',#76783,#6451) ;
#3238 = LINE('',#76784,#6452) ;
#3239 = LINE('',#76787,#6453) ;
#3240 = LINE('',#76791,#6454) ;
#3241 = LINE('',#76792,#6455) ;
#3242 = LINE('',#76876,#6456) ;
#3243 = LINE('',#76877,#6457) ;
#3244 = LINE('',#76944,#6458) ;
#3245 = LINE('',#76945,#6459) ;
#3246 = LINE('',#76997,#6460) ;
#3247 = LINE('',#76998,#6461) ;
#3248 = LINE('',#77000,#6462) ;
#3249 = LINE('',#77161,#6463) ;
#3250 = LINE('',#77162,#6464) ;
#3251 = LINE('',#77164,#6465) ;
#3252 = LINE('',#77212,#6466) ;
#3253 = LINE('',#77249,#6467) ;
#3254 = LINE('',#77251,#6468) ;
#3255 = LINE('',#77261,#6469) ;
#3256 = LINE('',#77270,#6470) ;
#3257 = LINE('',#77273,#6471) ;
#3258 = LINE('',#77276,#6472) ;
#3259 = LINE('',#77361,#6473) ;
#3260 = LINE('',#77474,#6474) ;
#3261 = LINE('',#77475,#6475) ;
#3262 = LINE('',#77581,#6476) ;
#3263 = LINE('',#77678,#6477) ;
#3264 = LINE('',#77679,#6478) ;
#3265 = LINE('',#77694,#6479) ;
#3266 = LINE('',#77707,#6480) ;
#3267 = LINE('',#77761,#6481) ;
#3268 = LINE('',#77762,#6482) ;
#3269 = LINE('',#77775,#6483) ;
#3270 = LINE('',#77776,#6484) ;
#3271 = LINE('',#77840,#6485) ;
#3272 = LINE('',#77841,#6486) ;
#3273 = LINE('',#77998,#6487) ;
#3274 = LINE('',#77999,#6488) ;
#3275 = LINE('',#78060,#6489) ;
#3276 = LINE('',#78061,#6490) ;
#3277 = LINE('',#78136,#6491) ;
#3278 = LINE('',#78137,#6492) ;
#3279 = LINE('',#78152,#6493) ;
#3280 = LINE('',#78153,#6494) ;
#3281 = LINE('',#78168,#6495) ;
#3282 = LINE('',#78170,#6496) ;
#3283 = LINE('',#78184,#6497) ;
#3284 = LINE('',#78212,#6498) ;
#3285 = LINE('',#78245,#6499) ;
#3286 = LINE('',#78265,#6500) ;
#3287 = LINE('',#78335,#6501) ;
#3288 = LINE('',#78336,#6502) ;
#3289 = LINE('',#78416,#6503) ;
#3290 = LINE('',#78417,#6504) ;
#3291 = LINE('',#78522,#6505) ;
#3292 = LINE('',#78523,#6506) ;
#3293 = LINE('',#78525,#6507) ;
#3294 = LINE('',#78526,#6508) ;
#3295 = LINE('',#78574,#6509) ;
#3296 = LINE('',#78585,#6510) ;
#3297 = LINE('',#78586,#6511) ;
#3298 = LINE('',#78588,#6512) ;
#3299 = LINE('',#78589,#6513) ;
#3300 = LINE('',#78615,#6514) ;
#3301 = LINE('',#78736,#6515) ;
#3302 = LINE('',#78737,#6516) ;
#3303 = LINE('',#78752,#6517) ;
#3304 = LINE('',#78765,#6518) ;
#3305 = LINE('',#78768,#6519) ;
#3306 = LINE('',#78769,#6520) ;
#3307 = LINE('',#78903,#6521) ;
#3308 = LINE('',#79044,#6522) ;
#3309 = LINE('',#79045,#6523) ;
#3310 = LINE('',#79060,#6524) ;
#3311 = LINE('',#79081,#6525) ;
#3312 = LINE('',#79102,#6526) ;
#3313 = LINE('',#79103,#6527) ;
#3314 = LINE('',#79112,#6528) ;
#3315 = LINE('',#79121,#6529) ;
#3316 = LINE('',#79132,#6530) ;
#3317 = LINE('',#79133,#6531) ;
#3318 = LINE('',#79147,#6532) ;
#3319 = LINE('',#79156,#6533) ;
#3320 = LINE('',#79189,#6534) ;
#3321 = LINE('',#79192,#6535) ;
#3322 = LINE('',#79194,#6536) ;
#3323 = LINE('',#79543,#6537) ;
#3324 = LINE('',#79546,#6538) ;
#3325 = LINE('',#79549,#6539) ;
#3326 = LINE('',#79551,#6540) ;
#3327 = LINE('',#79554,#6541) ;
#3328 = LINE('',#79555,#6542) ;
#3329 = LINE('',#79728,#6543) ;
#3330 = LINE('',#79730,#6544) ;
#3331 = LINE('',#79731,#6545) ;
#3332 = LINE('',#79734,#6546) ;
#3333 = LINE('',#79735,#6547) ;
#3334 = LINE('',#79738,#6548) ;
#3335 = LINE('',#79739,#6549) ;
#3336 = LINE('',#79751,#6550) ;
#3337 = LINE('',#79761,#6551) ;
#3338 = LINE('',#79803,#6552) ;
#3339 = LINE('',#79805,#6553) ;
#3340 = LINE('',#79807,#6554) ;
#3341 = LINE('',#79866,#6555) ;
#3342 = LINE('',#79868,#6556) ;
#3343 = LINE('',#79870,#6557) ;
#3344 = LINE('',#79871,#6558) ;
#3345 = LINE('',#79876,#6559) ;
#3346 = LINE('',#79902,#6560) ;
#3347 = LINE('',#79927,#6561) ;
#3348 = LINE('',#80266,#6562) ;
#3349 = LINE('',#80334,#6563) ;
#3350 = LINE('',#80337,#6564) ;
#3351 = LINE('',#80341,#6565) ;
#3352 = LINE('',#80344,#6566) ;
#3353 = LINE('',#80841,#6567) ;
#3354 = LINE('',#80849,#6568) ;
#3355 = LINE('',#80861,#6569) ;
#3356 = LINE('',#80870,#6570) ;
#3357 = LINE('',#80871,#6571) ;
#3358 = LINE('',#80874,#6572) ;
#3359 = LINE('',#80875,#6573) ;
#3360 = LINE('',#80878,#6574) ;
#3361 = LINE('',#80879,#6575) ;
#3362 = LINE('',#80891,#6576) ;
#3363 = LINE('',#80909,#6577) ;
#3364 = LINE('',#80927,#6578) ;
#3365 = LINE('',#80973,#6579) ;
#3366 = LINE('',#80982,#6580) ;
#3367 = LINE('',#80983,#6581) ;
#3368 = LINE('',#81090,#6582) ;
#3369 = LINE('',#81095,#6583) ;
#3370 = LINE('',#81228,#6584) ;
#3371 = LINE('',#81520,#6585) ;
#3372 = LINE('',#81524,#6586) ;
#3373 = LINE('',#81528,#6587) ;
#3374 = LINE('',#81530,#6588) ;
#3375 = LINE('',#81533,#6589) ;
#3376 = LINE('',#81534,#6590) ;
#3377 = LINE('',#81537,#6591) ;
#3378 = LINE('',#81539,#6592) ;
#3379 = LINE('',#81540,#6593) ;
#3380 = LINE('',#81543,#6594) ;
#3381 = LINE('',#81544,#6595) ;
#3382 = LINE('',#81549,#6596) ;
#3383 = LINE('',#81553,#6597) ;
#3384 = LINE('',#81557,#6598) ;
#3385 = LINE('',#81559,#6599) ;
#3386 = LINE('',#81563,#6600) ;
#3387 = LINE('',#81565,#6601) ;
#3388 = LINE('',#81568,#6602) ;
#3389 = LINE('',#81569,#6603) ;
#3390 = LINE('',#81572,#6604) ;
#3391 = LINE('',#81574,#6605) ;
#3392 = LINE('',#81575,#6606) ;
#3393 = LINE('',#81578,#6607) ;
#3394 = LINE('',#81579,#6608) ;
#3395 = LINE('',#81584,#6609) ;
#3396 = LINE('',#81588,#6610) ;
#3397 = LINE('',#81592,#6611) ;
#3398 = LINE('',#81594,#6612) ;
#3399 = LINE('',#81597,#6613) ;
#3400 = LINE('',#81598,#6614) ;
#3401 = LINE('',#81601,#6615) ;
#3402 = LINE('',#81603,#6616) ;
#3403 = LINE('',#81604,#6617) ;
#3404 = LINE('',#81607,#6618) ;
#3405 = LINE('',#81608,#6619) ;
#3406 = LINE('',#81613,#6620) ;
#3407 = LINE('',#81795,#6621) ;
#3408 = LINE('',#82252,#6622) ;
#3409 = LINE('',#82256,#6623) ;
#3410 = LINE('',#82260,#6624) ;
#3411 = LINE('',#82263,#6625) ;
#3412 = LINE('',#82266,#6626) ;
#3413 = LINE('',#82269,#6627) ;
#3414 = LINE('',#82271,#6628) ;
#3415 = LINE('',#82272,#6629) ;
#3416 = LINE('',#82327,#6630) ;
#3417 = LINE('',#82501,#6631) ;
#3418 = LINE('',#82512,#6632) ;
#3419 = LINE('',#82513,#6633) ;
#3420 = LINE('',#82524,#6634) ;
#3421 = LINE('',#82535,#6635) ;
#3422 = LINE('',#82546,#6636) ;
#3423 = LINE('',#82548,#6637) ;
#3424 = LINE('',#82550,#6638) ;
#3425 = LINE('',#82552,#6639) ;
#3426 = LINE('',#82557,#6640) ;
#3427 = LINE('',#82559,#6641) ;
#3428 = LINE('',#82561,#6642) ;
#3429 = LINE('',#82565,#6643) ;
#3430 = LINE('',#82569,#6644) ;
#3431 = LINE('',#82571,#6645) ;
#3432 = LINE('',#82576,#6646) ;
#3433 = LINE('',#82578,#6647) ;
#3434 = LINE('',#82582,#6648) ;
#3435 = LINE('',#82586,#6649) ;
#3436 = LINE('',#82588,#6650) ;
#3437 = LINE('',#82590,#6651) ;
#3438 = LINE('',#82594,#6652) ;
#3439 = LINE('',#82598,#6653) ;
#3440 = LINE('',#82602,#6654) ;
#3441 = LINE('',#82606,#6655) ;
#3442 = LINE('',#82610,#6656) ;
#3443 = LINE('',#82614,#6657) ;
#3444 = LINE('',#82618,#6658) ;
#3445 = LINE('',#82622,#6659) ;
#3446 = LINE('',#82626,#6660) ;
#3447 = LINE('',#82630,#6661) ;
#3448 = LINE('',#82634,#6662) ;
#3449 = LINE('',#82640,#6663) ;
#3450 = LINE('',#82646,#6664) ;
#3451 = LINE('',#82650,#6665) ;
#3452 = LINE('',#82654,#6666) ;
#3453 = LINE('',#82656,#6667) ;
#3454 = LINE('',#82657,#6668) ;
#3455 = LINE('',#82660,#6669) ;
#3456 = LINE('',#82662,#6670) ;
#3457 = LINE('',#82663,#6671) ;
#3458 = LINE('',#82668,#6672) ;
#3459 = LINE('',#82672,#6673) ;
#3460 = LINE('',#82676,#6674) ;
#3461 = LINE('',#82678,#6675) ;
#3462 = LINE('',#82682,#6676) ;
#3463 = LINE('',#82686,#6677) ;
#3464 = LINE('',#82688,#6678) ;
#3465 = LINE('',#82691,#6679) ;
#3466 = LINE('',#82694,#6680) ;
#3467 = LINE('',#82696,#6681) ;
#3468 = LINE('',#82698,#6682) ;
#3469 = LINE('',#82700,#6683) ;
#3470 = LINE('',#82702,#6684) ;
#3471 = LINE('',#82706,#6685) ;
#3472 = LINE('',#82710,#6686) ;
#3473 = LINE('',#82714,#6687) ;
#3474 = LINE('',#82718,#6688) ;
#3475 = LINE('',#82722,#6689) ;
#3476 = LINE('',#82728,#6690) ;
#3477 = LINE('',#82730,#6691) ;
#3478 = LINE('',#82734,#6692) ;
#3479 = LINE('',#82738,#6693) ;
#3480 = LINE('',#82740,#6694) ;
#3481 = LINE('',#82744,#6695) ;
#3482 = LINE('',#82748,#6696) ;
#3483 = LINE('',#82751,#6697) ;
#3484 = LINE('',#82756,#6698) ;
#3485 = LINE('',#82758,#6699) ;
#3486 = LINE('',#82762,#6700) ;
#3487 = LINE('',#82766,#6701) ;
#3488 = LINE('',#82768,#6702) ;
#3489 = LINE('',#82772,#6703) ;
#3490 = LINE('',#82776,#6704) ;
#3491 = LINE('',#82779,#6705) ;
#3492 = LINE('',#82782,#6706) ;
#3493 = LINE('',#82784,#6707) ;
#3494 = LINE('',#82786,#6708) ;
#3495 = LINE('',#82788,#6709) ;
#3496 = LINE('',#82790,#6710) ;
#3497 = LINE('',#82792,#6711) ;
#3498 = LINE('',#82796,#6712) ;
#3499 = LINE('',#82800,#6713) ;
#3500 = LINE('',#82804,#6714) ;
#3501 = LINE('',#82807,#6715) ;
#3502 = LINE('',#82812,#6716) ;
#3503 = LINE('',#82816,#6717) ;
#3504 = LINE('',#82820,#6718) ;
#3505 = LINE('',#82824,#6719) ;
#3506 = LINE('',#82828,#6720) ;
#3507 = LINE('',#82832,#6721) ;
#3508 = LINE('',#82834,#6722) ;
#3509 = LINE('',#82836,#6723) ;
#3510 = LINE('',#82838,#6724) ;
#3511 = LINE('',#82839,#6725) ;
#3512 = LINE('',#82846,#6726) ;
#3513 = LINE('',#82848,#6727) ;
#3514 = LINE('',#82850,#6728) ;
#3515 = LINE('',#82854,#6729) ;
#3516 = LINE('',#82858,#6730) ;
#3517 = LINE('',#82862,#6731) ;
#3518 = LINE('',#82866,#6732) ;
#3519 = LINE('',#82868,#6733) ;
#3520 = LINE('',#82870,#6734) ;
#3521 = LINE('',#82871,#6735) ;
#3522 = LINE('',#82880,#6736) ;
#3523 = LINE('',#82884,#6737) ;
#3524 = LINE('',#82888,#6738) ;
#3525 = LINE('',#82891,#6739) ;
#3526 = LINE('',#82896,#6740) ;
#3527 = LINE('',#82900,#6741) ;
#3528 = LINE('',#82904,#6742) ;
#3529 = LINE('',#82906,#6743) ;
#3530 = LINE('',#82910,#6744) ;
#3531 = LINE('',#82914,#6745) ;
#3532 = LINE('',#82916,#6746) ;
#3533 = LINE('',#82919,#6747) ;
#3534 = LINE('',#82922,#6748) ;
#3535 = LINE('',#82924,#6749) ;
#3536 = LINE('',#82926,#6750) ;
#3537 = LINE('',#82927,#6751) ;
#3538 = LINE('',#82934,#6752) ;
#3539 = LINE('',#82943,#6753) ;
#3540 = LINE('',#82946,#6754) ;
#3541 = LINE('',#82948,#6755) ;
#3542 = LINE('',#82955,#6756) ;
#3543 = LINE('',#82968,#6757) ;
#3544 = LINE('',#82979,#6758) ;
#3545 = LINE('',#82990,#6759) ;
#3546 = LINE('',#83024,#6760) ;
#3547 = LINE('',#83033,#6761) ;
#3548 = LINE('',#83041,#6762) ;
#3549 = LINE('',#83045,#6763) ;
#3550 = LINE('',#83047,#6764) ;
#3551 = LINE('',#83049,#6765) ;
#3552 = LINE('',#83051,#6766) ;
#3553 = LINE('',#83053,#6767) ;
#3554 = LINE('',#83057,#6768) ;
#3555 = LINE('',#83061,#6769) ;
#3556 = LINE('',#83065,#6770) ;
#3557 = LINE('',#83067,#6771) ;
#3558 = LINE('',#83071,#6772) ;
#3559 = LINE('',#83075,#6773) ;
#3560 = LINE('',#83077,#6774) ;
#3561 = LINE('',#83079,#6775) ;
#3562 = LINE('',#83083,#6776) ;
#3563 = LINE('',#83087,#6777) ;
#3564 = LINE('',#83089,#6778) ;
#3565 = LINE('',#83093,#6779) ;
#3566 = LINE('',#83097,#6780) ;
#3567 = LINE('',#83103,#6781) ;
#3568 = LINE('',#83109,#6782) ;
#3569 = LINE('',#83113,#6783) ;
#3570 = LINE('',#83117,#6784) ;
#3571 = LINE('',#83121,#6785) ;
#3572 = LINE('',#83125,#6786) ;
#3573 = LINE('',#83129,#6787) ;
#3574 = LINE('',#83133,#6788) ;
#3575 = LINE('',#83137,#6789) ;
#3576 = LINE('',#83146,#6790) ;
#3577 = LINE('',#83155,#6791) ;
#3578 = LINE('',#83159,#6792) ;
#3579 = LINE('',#83162,#6793) ;
#3580 = LINE('',#83167,#6794) ;
#3581 = LINE('',#83169,#6795) ;
#3582 = LINE('',#83173,#6796) ;
#3583 = LINE('',#83177,#6797) ;
#3584 = LINE('',#83179,#6798) ;
#3585 = LINE('',#83183,#6799) ;
#3586 = LINE('',#83187,#6800) ;
#3587 = LINE('',#83191,#6801) ;
#3588 = LINE('',#83199,#6802) ;
#3589 = LINE('',#83201,#6803) ;
#3590 = LINE('',#83205,#6804) ;
#3591 = LINE('',#83209,#6805) ;
#3592 = LINE('',#83213,#6806) ;
#3593 = LINE('',#83217,#6807) ;
#3594 = LINE('',#83221,#6808) ;
#3595 = LINE('',#83225,#6809) ;
#3596 = LINE('',#83227,#6810) ;
#3597 = LINE('',#83228,#6811) ;
#3598 = LINE('',#83233,#6812) ;
#3599 = LINE('',#83237,#6813) ;
#3600 = LINE('',#83241,#6814) ;
#3601 = LINE('',#83245,#6815) ;
#3602 = LINE('',#83249,#6816) ;
#3603 = LINE('',#83253,#6817) ;
#3604 = LINE('',#83255,#6818) ;
#3605 = LINE('',#83257,#6819) ;
#3606 = LINE('',#83263,#6820) ;
#3607 = LINE('',#83267,#6821) ;
#3608 = LINE('',#83271,#6822) ;
#3609 = LINE('',#83274,#6823) ;
#3610 = LINE('',#83277,#6824) ;
#3611 = LINE('',#83279,#6825) ;
#3612 = LINE('',#83281,#6826) ;
#3613 = LINE('',#83290,#6827) ;
#3614 = LINE('',#83294,#6828) ;
#3615 = LINE('',#83298,#6829) ;
#3616 = LINE('',#83302,#6830) ;
#3617 = LINE('',#83306,#6831) ;
#3618 = LINE('',#83315,#6832) ;
#3619 = LINE('',#83324,#6833) ;
#3620 = LINE('',#83326,#6834) ;
#3621 = LINE('',#83330,#6835) ;
#3622 = LINE('',#83334,#6836) ;
#3623 = LINE('',#83338,#6837) ;
#3624 = LINE('',#83342,#6838) ;
#3625 = LINE('',#83344,#6839) ;
#3626 = LINE('',#83355,#6840) ;
#3627 = LINE('',#83359,#6841) ;
#3628 = LINE('',#83363,#6842) ;
#3629 = LINE('',#83367,#6843) ;
#3630 = LINE('',#83369,#6844) ;
#3631 = LINE('',#83373,#6845) ;
#3632 = LINE('',#83377,#6846) ;
#3633 = LINE('',#83378,#6847) ;
#3634 = LINE('',#83383,#6848) ;
#3635 = LINE('',#83387,#6849) ;
#3636 = LINE('',#83391,#6850) ;
#3637 = LINE('',#83395,#6851) ;
#3638 = LINE('',#83397,#6852) ;
#3639 = LINE('',#83401,#6853) ;
#3640 = LINE('',#83405,#6854) ;
#3641 = LINE('',#83406,#6855) ;
#3642 = LINE('',#83438,#6856) ;
#3643 = LINE('',#83439,#6857) ;
#3644 = LINE('',#83450,#6858) ;
#3645 = LINE('',#83451,#6859) ;
#3646 = LINE('',#83462,#6860) ;
#3647 = LINE('',#83463,#6861) ;
#3648 = LINE('',#83474,#6862) ;
#3649 = LINE('',#83475,#6863) ;
#3650 = LINE('',#83486,#6864) ;
#3651 = LINE('',#83487,#6865) ;
#3652 = LINE('',#83498,#6866) ;
#3653 = LINE('',#83499,#6867) ;
#3654 = LINE('',#83507,#6868) ;
#3655 = LINE('',#83509,#6869) ;
#3656 = LINE('',#83513,#6870) ;
#3657 = LINE('',#83515,#6871) ;
#3658 = LINE('',#83516,#6872) ;
#3659 = LINE('',#83519,#6873) ;
#3660 = LINE('',#83523,#6874) ;
#3661 = LINE('',#83524,#6875) ;
#3662 = LINE('',#83527,#6876) ;
#3663 = LINE('',#83531,#6877) ;
#3664 = LINE('',#83532,#6878) ;
#3665 = LINE('',#83535,#6879) ;
#3666 = LINE('',#83539,#6880) ;
#3667 = LINE('',#83540,#6881) ;
#3668 = LINE('',#83543,#6882) ;
#3669 = LINE('',#83547,#6883) ;
#3670 = LINE('',#83548,#6884) ;
#3671 = LINE('',#83551,#6885) ;
#3672 = LINE('',#83555,#6886) ;
#3673 = LINE('',#83557,#6887) ;
#3674 = LINE('',#83559,#6888) ;
#3675 = LINE('',#83562,#6889) ;
#3676 = LINE('',#83569,#6890) ;
#3677 = LINE('',#83686,#6891) ;
#3678 = LINE('',#83702,#6892) ;
#3679 = LINE('',#83714,#6893) ;
#3680 = LINE('',#83721,#6894) ;
#3681 = LINE('',#83723,#6895) ;
#3682 = LINE('',#83727,#6896) ;
#3683 = LINE('',#83730,#6897) ;
#3684 = LINE('',#83743,#6898) ;
#3685 = LINE('',#83745,#6899) ;
#3686 = LINE('',#83752,#6900) ;
#3687 = LINE('',#83763,#6901) ;
#3688 = LINE('',#83770,#6902) ;
#3689 = LINE('',#83772,#6903) ;
#3690 = LINE('',#83776,#6904) ;
#3691 = LINE('',#83779,#6905) ;
#3692 = LINE('',#83793,#6906) ;
#3693 = LINE('',#83800,#6907) ;
#3694 = LINE('',#83801,#6908) ;
#3695 = LINE('',#83811,#6909) ;
#3696 = LINE('',#83819,#6910) ;
#3697 = LINE('',#83826,#6911) ;
#3698 = LINE('',#83830,#6912) ;
#3699 = LINE('',#83832,#6913) ;
#3700 = LINE('',#83834,#6914) ;
#3701 = LINE('',#83857,#6915) ;
#3702 = LINE('',#83859,#6916) ;
#3703 = LINE('',#83861,#6917) ;
#3704 = LINE('',#83884,#6918) ;
#3705 = LINE('',#83886,#6919) ;
#3706 = LINE('',#83888,#6920) ;
#3707 = LINE('',#83891,#6921) ;
#3708 = LINE('',#83896,#6922) ;
#3709 = LINE('',#83938,#6923) ;
#3710 = LINE('',#83940,#6924) ;
#3711 = LINE('',#83983,#6925) ;
#3712 = LINE('',#83992,#6926) ;
#3713 = LINE('',#83999,#6927) ;
#3714 = LINE('',#84084,#6928) ;
#3715 = LINE('',#84128,#6929) ;
#3716 = LINE('',#84136,#6930) ;
#3717 = LINE('',#84165,#6931) ;
#3718 = LINE('',#84177,#6932) ;
#3719 = LINE('',#84178,#6933) ;
#3720 = LINE('',#84192,#6934) ;
#3721 = LINE('',#84194,#6935) ;
#3722 = LINE('',#84202,#6936) ;
#3723 = LINE('',#84203,#6937) ;
#3724 = LINE('',#84208,#6938) ;
#3725 = LINE('',#84209,#6939) ;
#3726 = LINE('',#84216,#6940) ;
#3727 = LINE('',#84223,#6941) ;
#3728 = LINE('',#84226,#6942) ;
#3729 = LINE('',#84229,#6943) ;
#3730 = LINE('',#84233,#6944) ;
#3731 = LINE('',#84236,#6945) ;
#3732 = LINE('',#84238,#6946) ;
#3733 = LINE('',#84249,#6947) ;
#3734 = LINE('',#84250,#6948) ;
#3735 = LINE('',#84275,#6949) ;
#3736 = LINE('',#84278,#6950) ;
#3737 = LINE('',#84308,#6951) ;
#3738 = LINE('',#84309,#6952) ;
#3739 = LINE('',#84315,#6953) ;
#3740 = LINE('',#84316,#6954) ;
#3741 = LINE('',#84324,#6955) ;
#3742 = LINE('',#84332,#6956) ;
#3743 = LINE('',#84340,#6957) ;
#3744 = LINE('',#84346,#6958) ;
#3745 = LINE('',#84349,#6959) ;
#3746 = LINE('',#84351,#6960) ;
#3747 = LINE('',#84352,#6961) ;
#3748 = LINE('',#84355,#6962) ;
#3749 = LINE('',#84359,#6963) ;
#3750 = LINE('',#84360,#6964) ;
#3751 = LINE('',#84363,#6965) ;
#3752 = LINE('',#84367,#6966) ;
#3753 = LINE('',#84368,#6967) ;
#3754 = LINE('',#84371,#6968) ;
#3755 = LINE('',#84375,#6969) ;
#3756 = LINE('',#84376,#6970) ;
#3757 = LINE('',#84379,#6971) ;
#3758 = LINE('',#84383,#6972) ;
#3759 = LINE('',#84384,#6973) ;
#3760 = LINE('',#84387,#6974) ;
#3761 = LINE('',#84391,#6975) ;
#3762 = LINE('',#84392,#6976) ;
#3763 = LINE('',#84397,#6977) ;
#3764 = LINE('',#84406,#6978) ;
#3765 = LINE('',#84414,#6979) ;
#3766 = LINE('',#84422,#6980) ;
#3767 = LINE('',#84430,#6981) ;
#3768 = LINE('',#84435,#6982) ;
#3769 = LINE('',#84444,#6983) ;
#3770 = LINE('',#84452,#6984) ;
#3771 = LINE('',#84459,#6985) ;
#3772 = LINE('',#84462,#6986) ;
#3773 = LINE('',#84465,#6987) ;
#3774 = LINE('',#84466,#6988) ;
#3775 = LINE('',#84469,#6989) ;
#3776 = LINE('',#84473,#6990) ;
#3777 = LINE('',#84474,#6991) ;
#3778 = LINE('',#84477,#6992) ;
#3779 = LINE('',#84481,#6993) ;
#3780 = LINE('',#84482,#6994) ;
#3781 = LINE('',#84485,#6995) ;
#3782 = LINE('',#84489,#6996) ;
#3783 = LINE('',#84490,#6997) ;
#3784 = LINE('',#84506,#6998) ;
#3785 = LINE('',#84514,#6999) ;
#3786 = LINE('',#84522,#7000) ;
#3787 = LINE('',#84530,#7001) ;
#3788 = LINE('',#84536,#7002) ;
#3789 = LINE('',#84540,#7003) ;
#3790 = LINE('',#84545,#7004) ;
#3791 = LINE('',#84546,#7005) ;
#3792 = LINE('',#84573,#7006) ;
#3793 = LINE('',#84574,#7007) ;
#3794 = LINE('',#84600,#7008) ;
#3795 = LINE('',#84603,#7009) ;
#3796 = LINE('',#84604,#7010) ;
#3797 = LINE('',#84614,#7011) ;
#3798 = LINE('',#84619,#7012) ;
#3799 = LINE('',#84628,#7013) ;
#3800 = LINE('',#84636,#7014) ;
#3801 = LINE('',#84643,#7015) ;
#3802 = LINE('',#84653,#7016) ;
#3803 = LINE('',#84655,#7017) ;
#3804 = LINE('',#84656,#7018) ;
#3805 = LINE('',#84659,#7019) ;
#3806 = LINE('',#84663,#7020) ;
#3807 = LINE('',#84664,#7021) ;
#3808 = LINE('',#84667,#7022) ;
#3809 = LINE('',#84671,#7023) ;
#3810 = LINE('',#84672,#7024) ;
#3811 = LINE('',#84675,#7025) ;
#3812 = LINE('',#84679,#7026) ;
#3813 = LINE('',#84680,#7027) ;
#3814 = LINE('',#84683,#7028) ;
#3815 = LINE('',#84687,#7029) ;
#3816 = LINE('',#84688,#7030) ;
#3817 = LINE('',#84698,#7031) ;
#3818 = LINE('',#84703,#7032) ;
#3819 = LINE('',#84712,#7033) ;
#3820 = LINE('',#84720,#7034) ;
#3821 = LINE('',#84727,#7035) ;
#3822 = LINE('',#84737,#7036) ;
#3823 = LINE('',#84739,#7037) ;
#3824 = LINE('',#84740,#7038) ;
#3825 = LINE('',#84743,#7039) ;
#3826 = LINE('',#84747,#7040) ;
#3827 = LINE('',#84748,#7041) ;
#3828 = LINE('',#84751,#7042) ;
#3829 = LINE('',#84755,#7043) ;
#3830 = LINE('',#84756,#7044) ;
#3831 = LINE('',#84759,#7045) ;
#3832 = LINE('',#84763,#7046) ;
#3833 = LINE('',#84764,#7047) ;
#3834 = LINE('',#84767,#7048) ;
#3835 = LINE('',#84771,#7049) ;
#3836 = LINE('',#84772,#7050) ;
#3837 = LINE('',#84778,#7051) ;
#3838 = LINE('',#84786,#7052) ;
#3839 = LINE('',#84788,#7053) ;
#3840 = LINE('',#84796,#7054) ;
#3841 = LINE('',#84805,#7055) ;
#3842 = LINE('',#84813,#7056) ;
#3843 = LINE('',#84821,#7057) ;
#3844 = LINE('',#84827,#7058) ;
#3845 = LINE('',#84830,#7059) ;
#3846 = LINE('',#84831,#7060) ;
#3847 = LINE('',#84834,#7061) ;
#3848 = LINE('',#84838,#7062) ;
#3849 = LINE('',#84839,#7063) ;
#3850 = LINE('',#84842,#7064) ;
#3851 = LINE('',#84846,#7065) ;
#3852 = LINE('',#84847,#7066) ;
#3853 = LINE('',#84850,#7067) ;
#3854 = LINE('',#84854,#7068) ;
#3855 = LINE('',#84855,#7069) ;
#3856 = LINE('',#84858,#7070) ;
#3857 = LINE('',#84861,#7071) ;
#3858 = LINE('',#84863,#7072) ;
#3859 = LINE('',#84872,#7073) ;
#3860 = LINE('',#84874,#7074) ;
#3861 = LINE('',#84876,#7075) ;
#3862 = LINE('',#84877,#7076) ;
#3863 = LINE('',#84883,#7077) ;
#3864 = LINE('',#84895,#7078) ;
#3865 = LINE('',#84897,#7079) ;
#3866 = LINE('',#84906,#7080) ;
#3867 = LINE('',#84908,#7081) ;
#3868 = LINE('',#84910,#7082) ;
#3869 = LINE('',#84912,#7083) ;
#3870 = LINE('',#84927,#7084) ;
#3871 = LINE('',#84929,#7085) ;
#3872 = LINE('',#84931,#7086) ;
#3873 = LINE('',#84932,#7087) ;
#3874 = LINE('',#84959,#7088) ;
#3875 = LINE('',#84971,#7089) ;
#3876 = LINE('',#84973,#7090) ;
#3877 = LINE('',#84976,#7091) ;
#3878 = LINE('',#84978,#7092) ;
#3879 = LINE('',#84980,#7093) ;
#3880 = LINE('',#84985,#7094) ;
#3881 = LINE('',#85000,#7095) ;
#3882 = LINE('',#85002,#7096) ;
#3883 = LINE('',#85004,#7097) ;
#3884 = LINE('',#85005,#7098) ;
#3885 = LINE('',#85038,#7099) ;
#3886 = LINE('',#85045,#7100) ;
#3887 = LINE('',#85047,#7101) ;
#3888 = LINE('',#85050,#7102) ;
#3889 = LINE('',#85052,#7103) ;
#3890 = LINE('',#85054,#7104) ;
#3891 = LINE('',#85058,#7105) ;
#3892 = LINE('',#85087,#7106) ;
#3893 = LINE('',#85093,#7107) ;
#3894 = LINE('',#85111,#7108) ;
#3895 = LINE('',#85119,#7109) ;
#3896 = LINE('',#85131,#7110) ;
#3897 = LINE('',#85143,#7111) ;
#3898 = LINE('',#85151,#7112) ;
#3899 = LINE('',#85159,#7113) ;
#3900 = LINE('',#85167,#7114) ;
#3901 = LINE('',#85175,#7115) ;
#3902 = LINE('',#85183,#7116) ;
#3903 = LINE('',#85191,#7117) ;
#3904 = LINE('',#85197,#7118) ;
#3905 = LINE('',#85205,#7119) ;
#3906 = LINE('',#85206,#7120) ;
#3907 = LINE('',#85208,#7121) ;
#3908 = LINE('',#85213,#7122) ;
#3909 = LINE('',#85214,#7123) ;
#3910 = LINE('',#85224,#7124) ;
#3911 = LINE('',#85226,#7125) ;
#3912 = LINE('',#85227,#7126) ;
#3913 = LINE('',#85230,#7127) ;
#3914 = LINE('',#85234,#7128) ;
#3915 = LINE('',#85235,#7129) ;
#3916 = LINE('',#85238,#7130) ;
#3917 = LINE('',#85242,#7131) ;
#3918 = LINE('',#85246,#7132) ;
#3919 = LINE('',#85247,#7133) ;
#3920 = LINE('',#85250,#7134) ;
#3921 = LINE('',#85254,#7135) ;
#3922 = LINE('',#85258,#7136) ;
#3923 = LINE('',#85259,#7137) ;
#3924 = LINE('',#85262,#7138) ;
#3925 = LINE('',#85266,#7139) ;
#3926 = LINE('',#85267,#7140) ;
#3927 = LINE('',#85270,#7141) ;
#3928 = LINE('',#85274,#7142) ;
#3929 = LINE('',#85275,#7143) ;
#3930 = LINE('',#85278,#7144) ;
#3931 = LINE('',#85282,#7145) ;
#3932 = LINE('',#85283,#7146) ;
#3933 = LINE('',#85286,#7147) ;
#3934 = LINE('',#85290,#7148) ;
#3935 = LINE('',#85291,#7149) ;
#3936 = LINE('',#85294,#7150) ;
#3937 = LINE('',#85298,#7151) ;
#3938 = LINE('',#85299,#7152) ;
#3939 = LINE('',#85302,#7153) ;
#3940 = LINE('',#85306,#7154) ;
#3941 = LINE('',#85307,#7155) ;
#3942 = LINE('',#85310,#7156) ;
#3943 = LINE('',#85313,#7157) ;
#3944 = LINE('',#85321,#7158) ;
#3945 = LINE('',#85324,#7159) ;
#3946 = LINE('',#85334,#7160) ;
#3947 = LINE('',#85338,#7161) ;
#3948 = LINE('',#85339,#7162) ;
#3949 = LINE('',#85342,#7163) ;
#3950 = LINE('',#85344,#7164) ;
#3951 = LINE('',#85346,#7165) ;
#3952 = LINE('',#85350,#7166) ;
#3953 = LINE('',#85359,#7167) ;
#3954 = LINE('',#85360,#7168) ;
#3955 = LINE('',#85374,#7169) ;
#3956 = LINE('',#85382,#7170) ;
#3957 = LINE('',#85390,#7171) ;
#3958 = LINE('',#85398,#7172) ;
#3959 = LINE('',#85406,#7173) ;
#3960 = LINE('',#85408,#7174) ;
#3961 = LINE('',#85409,#7175) ;
#3962 = LINE('',#85411,#7176) ;
#3963 = LINE('',#85413,#7177) ;
#3964 = LINE('',#85414,#7178) ;
#3965 = LINE('',#85416,#7179) ;
#3966 = LINE('',#85417,#7180) ;
#3967 = LINE('',#85419,#7181) ;
#3968 = LINE('',#85420,#7182) ;
#3969 = LINE('',#85422,#7183) ;
#3970 = LINE('',#85423,#7184) ;
#3971 = LINE('',#85425,#7185) ;
#3972 = LINE('',#85426,#7186) ;
#3973 = LINE('',#85428,#7187) ;
#3974 = LINE('',#85444,#7188) ;
#3975 = LINE('',#85446,#7189) ;
#3976 = LINE('',#85447,#7190) ;
#3977 = LINE('',#85458,#7191) ;
#3978 = LINE('',#85465,#7192) ;
#3979 = LINE('',#85480,#7193) ;
#3980 = LINE('',#85482,#7194) ;
#3981 = LINE('',#85483,#7195) ;
#3982 = LINE('',#85485,#7196) ;
#3983 = LINE('',#85487,#7197) ;
#3984 = LINE('',#85488,#7198) ;
#3985 = LINE('',#85496,#7199) ;
#3986 = LINE('',#85499,#7200) ;
#3987 = LINE('',#85507,#7201) ;
#3988 = LINE('',#85508,#7202) ;
#3989 = LINE('',#85514,#7203) ;
#3990 = LINE('',#85517,#7204) ;
#3991 = LINE('',#85524,#7205) ;
#3992 = LINE('',#85526,#7206) ;
#3993 = LINE('',#85549,#7207) ;
#3994 = LINE('',#85552,#7208) ;
#3995 = LINE('',#85561,#7209) ;
#3996 = LINE('',#85565,#7210) ;
#3997 = LINE('',#85566,#7211) ;
#3998 = LINE('',#85569,#7212) ;
#3999 = LINE('',#85571,#7213) ;
#4000 = LINE('',#85573,#7214) ;
#4001 = LINE('',#85577,#7215) ;
#4002 = LINE('',#85586,#7216) ;
#4003 = LINE('',#85587,#7217) ;
#4004 = LINE('',#85613,#7218) ;
#4005 = LINE('',#85616,#7219) ;
#4006 = LINE('',#85618,#7220) ;
#4007 = LINE('',#85619,#7221) ;
#4008 = LINE('',#85621,#7222) ;
#4009 = LINE('',#85623,#7223) ;
#4010 = LINE('',#85624,#7224) ;
#4011 = LINE('',#85626,#7225) ;
#4012 = LINE('',#85628,#7226) ;
#4013 = LINE('',#85629,#7227) ;
#4014 = LINE('',#85631,#7228) ;
#4015 = LINE('',#85633,#7229) ;
#4016 = LINE('',#85634,#7230) ;
#4017 = LINE('',#85636,#7231) ;
#4018 = LINE('',#85643,#7232) ;
#4019 = LINE('',#85646,#7233) ;
#4020 = LINE('',#85691,#7234) ;
#4021 = LINE('',#85699,#7235) ;
#4022 = LINE('',#85701,#7236) ;
#4023 = LINE('',#85703,#7237) ;
#4024 = LINE('',#85704,#7238) ;
#4025 = LINE('',#85706,#7239) ;
#4026 = LINE('',#85708,#7240) ;
#4027 = LINE('',#85710,#7241) ;
#4028 = LINE('',#85711,#7242) ;
#4029 = LINE('',#85713,#7243) ;
#4030 = LINE('',#85714,#7244) ;
#4031 = LINE('',#85716,#7245) ;
#4032 = LINE('',#85718,#7246) ;
#4033 = LINE('',#85720,#7247) ;
#4034 = LINE('',#85722,#7248) ;
#4035 = LINE('',#85723,#7249) ;
#4036 = LINE('',#85734,#7250) ;
#4037 = LINE('',#85745,#7251) ;
#4038 = LINE('',#85748,#7252) ;
#4039 = LINE('',#85757,#7253) ;
#4040 = LINE('',#85758,#7254) ;
#4041 = LINE('',#85761,#7255) ;
#4042 = LINE('',#85765,#7256) ;
#4043 = LINE('',#85766,#7257) ;
#4044 = LINE('',#85769,#7258) ;
#4045 = LINE('',#85770,#7259) ;
#4046 = LINE('',#85774,#7260) ;
#4047 = LINE('',#85806,#7261) ;
#4048 = LINE('',#85814,#7262) ;
#4049 = LINE('',#85822,#7263) ;
#4050 = LINE('',#85879,#7264) ;
#4051 = LINE('',#85885,#7265) ;
#4052 = LINE('',#85902,#7266) ;
#4053 = LINE('',#85919,#7267) ;
#4054 = LINE('',#85937,#7268) ;
#4055 = LINE('',#85948,#7269) ;
#4056 = LINE('',#85969,#7270) ;
#4057 = LINE('',#85970,#7271) ;
#4058 = LINE('',#85972,#7272) ;
#4059 = LINE('',#86111,#7273) ;
#4060 = LINE('',#86176,#7274) ;
#4061 = LINE('',#86180,#7275) ;
#4062 = LINE('',#86245,#7276) ;
#4063 = LINE('',#86250,#7277) ;
#4064 = LINE('',#86253,#7278) ;
#4065 = LINE('',#86256,#7279) ;
#4066 = LINE('',#86261,#7280) ;
#4067 = LINE('',#86264,#7281) ;
#4068 = LINE('',#86269,#7282) ;
#4069 = LINE('',#86272,#7283) ;
#4070 = LINE('',#86277,#7284) ;
#4071 = LINE('',#86278,#7285) ;
#4072 = LINE('',#86280,#7286) ;
#4073 = LINE('',#86283,#7287) ;
#4074 = LINE('',#86284,#7288) ;
#4075 = LINE('',#86288,#7289) ;
#4076 = LINE('',#86289,#7290) ;
#4077 = LINE('',#86293,#7291) ;
#4078 = LINE('',#86313,#7292) ;
#4079 = LINE('',#86315,#7293) ;
#4080 = LINE('',#86540,#7294) ;
#4081 = LINE('',#86546,#7295) ;
#4082 = LINE('',#86550,#7296) ;
#4083 = LINE('',#86554,#7297) ;
#4084 = LINE('',#86557,#7298) ;
#4085 = LINE('',#86560,#7299) ;
#4086 = LINE('',#86563,#7300) ;
#4087 = LINE('',#86575,#7301) ;
#4088 = LINE('',#86576,#7302) ;
#4089 = LINE('',#86581,#7303) ;
#4090 = LINE('',#86582,#7304) ;
#4091 = LINE('',#86584,#7305) ;
#4092 = LINE('',#86585,#7306) ;
#4093 = LINE('',#86588,#7307) ;
#4094 = LINE('',#86590,#7308) ;
#4095 = LINE('',#86591,#7309) ;
#4096 = LINE('',#86594,#7310) ;
#4097 = LINE('',#86595,#7311) ;
#4098 = LINE('',#86596,#7312) ;
#4099 = LINE('',#86599,#7313) ;
#4100 = LINE('',#86600,#7314) ;
#4101 = LINE('',#86603,#7315) ;
#4102 = LINE('',#86604,#7316) ;
#4103 = LINE('',#86606,#7317) ;
#4104 = LINE('',#86608,#7318) ;
#4105 = LINE('',#86626,#7319) ;
#4106 = LINE('',#86629,#7320) ;
#4107 = LINE('',#86634,#7321) ;
#4108 = LINE('',#86637,#7322) ;
#4109 = LINE('',#86652,#7323) ;
#4110 = LINE('',#86654,#7324) ;
#4111 = LINE('',#86661,#7325) ;
#4112 = LINE('',#86665,#7326) ;
#4113 = LINE('',#86667,#7327) ;
#4114 = LINE('',#86669,#7328) ;
#4115 = LINE('',#86671,#7329) ;
#4116 = LINE('',#86673,#7330) ;
#4117 = LINE('',#86677,#7331) ;
#4118 = LINE('',#86681,#7332) ;
#4119 = LINE('',#86685,#7333) ;
#4120 = LINE('',#86689,#7334) ;
#4121 = LINE('',#86691,#7335) ;
#4122 = LINE('',#86693,#7336) ;
#4123 = LINE('',#86695,#7337) ;
#4124 = LINE('',#86697,#7338) ;
#4125 = LINE('',#86699,#7339) ;
#4126 = LINE('',#86701,#7340) ;
#4127 = LINE('',#86703,#7341) ;
#4128 = LINE('',#86705,#7342) ;
#4129 = LINE('',#86709,#7343) ;
#4130 = LINE('',#86713,#7344) ;
#4131 = LINE('',#86728,#7345) ;
#4132 = LINE('',#86741,#7346) ;
#4133 = LINE('',#86754,#7347) ;
#4134 = LINE('',#86766,#7348) ;
#4135 = LINE('',#86769,#7349) ;
#4136 = LINE('',#86782,#7350) ;
#4137 = LINE('',#86795,#7351) ;
#4138 = LINE('',#86808,#7352) ;
#4139 = LINE('',#86821,#7353) ;
#4140 = LINE('',#86834,#7354) ;
#4141 = LINE('',#86847,#7355) ;
#4142 = LINE('',#86860,#7356) ;
#4143 = LINE('',#86873,#7357) ;
#4144 = LINE('',#86886,#7358) ;
#4145 = LINE('',#86899,#7359) ;
#4146 = LINE('',#86912,#7360) ;
#4147 = LINE('',#86925,#7361) ;
#4148 = LINE('',#86929,#7362) ;
#4149 = LINE('',#86930,#7363) ;
#4150 = LINE('',#86933,#7364) ;
#4151 = LINE('',#86939,#7365) ;
#4152 = LINE('',#86941,#7366) ;
#4153 = LINE('',#86943,#7367) ;
#4154 = LINE('',#86945,#7368) ;
#4155 = LINE('',#86947,#7369) ;
#4156 = LINE('',#86949,#7370) ;
#4157 = LINE('',#86951,#7371) ;
#4158 = LINE('',#86953,#7372) ;
#4159 = LINE('',#86955,#7373) ;
#4160 = LINE('',#86959,#7374) ;
#4161 = LINE('',#86963,#7375) ;
#4162 = LINE('',#86967,#7376) ;
#4163 = LINE('',#86971,#7377) ;
#4164 = LINE('',#86973,#7378) ;
#4165 = LINE('',#86975,#7379) ;
#4166 = LINE('',#86977,#7380) ;
#4167 = LINE('',#86979,#7381) ;
#4168 = LINE('',#86985,#7382) ;
#4169 = LINE('',#86988,#7383) ;
#4170 = LINE('',#86991,#7384) ;
#4171 = LINE('',#86993,#7385) ;
#4172 = LINE('',#86995,#7386) ;
#4173 = LINE('',#86996,#7387) ;
#4174 = LINE('',#87001,#7388) ;
#4175 = LINE('',#87008,#7389) ;
#4176 = LINE('',#87010,#7390) ;
#4177 = LINE('',#87011,#7391) ;
#4178 = LINE('',#87025,#7392) ;
#4179 = LINE('',#87026,#7393) ;
#4180 = LINE('',#87029,#7394) ;
#4181 = LINE('',#87031,#7395) ;
#4182 = LINE('',#87032,#7396) ;
#4183 = LINE('',#87037,#7397) ;
#4184 = LINE('',#87050,#7398) ;
#4185 = LINE('',#87051,#7399) ;
#4186 = LINE('',#87053,#7400) ;
#4187 = LINE('',#87065,#7401) ;
#4188 = LINE('',#87068,#7402) ;
#4189 = LINE('',#87072,#7403) ;
#4190 = LINE('',#87073,#7404) ;
#4191 = LINE('',#87112,#7405) ;
#4192 = LINE('',#87115,#7406) ;
#4193 = LINE('',#87149,#7407) ;
#4194 = LINE('',#87151,#7408) ;
#4195 = LINE('',#87152,#7409) ;
#4196 = LINE('',#87157,#7410) ;
#4197 = LINE('',#87182,#7411) ;
#4198 = LINE('',#87184,#7412) ;
#4199 = LINE('',#87191,#7413) ;
#4200 = LINE('',#87199,#7414) ;
#4201 = LINE('',#87203,#7415) ;
#4202 = LINE('',#87204,#7416) ;
#4203 = LINE('',#87206,#7417) ;
#4204 = LINE('',#87223,#7418) ;
#4205 = LINE('',#87229,#7419) ;
#4206 = LINE('',#87233,#7420) ;
#4207 = LINE('',#87242,#7421) ;
#4208 = LINE('',#87245,#7422) ;
#4209 = LINE('',#87251,#7423) ;
#4210 = LINE('',#87254,#7424) ;
#4211 = LINE('',#87257,#7425) ;
#4212 = LINE('',#87259,#7426) ;
#4213 = LINE('',#87272,#7427) ;
#4214 = LINE('',#87273,#7428) ;
#4215 = LINE('',#87288,#7429) ;
#4216 = LINE('',#87289,#7430) ;
#4217 = LINE('',#87304,#7431) ;
#4218 = LINE('',#87305,#7432) ;
#4219 = LINE('',#87320,#7433) ;
#4220 = LINE('',#87321,#7434) ;
#4221 = LINE('',#87336,#7435) ;
#4222 = LINE('',#87337,#7436) ;
#4223 = LINE('',#87352,#7437) ;
#4224 = LINE('',#87353,#7438) ;
#4225 = LINE('',#87368,#7439) ;
#4226 = LINE('',#87369,#7440) ;
#4227 = LINE('',#87384,#7441) ;
#4228 = LINE('',#87385,#7442) ;
#4229 = LINE('',#87391,#7443) ;
#4230 = LINE('',#87393,#7444) ;
#4231 = LINE('',#87396,#7445) ;
#4232 = LINE('',#87398,#7446) ;
#4233 = LINE('',#87401,#7447) ;
#4234 = LINE('',#87403,#7448) ;
#4235 = LINE('',#87406,#7449) ;
#4236 = LINE('',#87408,#7450) ;
#4237 = LINE('',#87413,#7451) ;
#4238 = LINE('',#87415,#7452) ;
#4239 = LINE('',#87417,#7453) ;
#4240 = LINE('',#87418,#7454) ;
#4241 = LINE('',#87420,#7455) ;
#4242 = LINE('',#87421,#7456) ;
#4243 = LINE('',#87423,#7457) ;
#4244 = LINE('',#87425,#7458) ;
#4245 = LINE('',#87427,#7459) ;
#4246 = LINE('',#87429,#7460) ;
#4247 = LINE('',#87432,#7461) ;
#4248 = LINE('',#87435,#7462) ;
#4249 = LINE('',#87437,#7463) ;
#4250 = LINE('',#87439,#7464) ;
#4251 = LINE('',#87441,#7465) ;
#4252 = LINE('',#87443,#7466) ;
#4253 = LINE('',#87449,#7467) ;
#4254 = LINE('',#87451,#7468) ;
#4255 = LINE('',#87453,#7469) ;
#4256 = LINE('',#87454,#7470) ;
#4257 = LINE('',#87457,#7471) ;
#4258 = LINE('',#87459,#7472) ;
#4259 = LINE('',#87460,#7473) ;
#4260 = LINE('',#87463,#7474) ;
#4261 = LINE('',#87465,#7475) ;
#4262 = LINE('',#87466,#7476) ;
#4263 = LINE('',#87468,#7477) ;
#4264 = LINE('',#87469,#7478) ;
#4265 = LINE('',#87485,#7479) ;
#4266 = LINE('',#87490,#7480) ;
#4267 = LINE('',#87505,#7481) ;
#4268 = LINE('',#87510,#7482) ;
#4269 = LINE('',#87521,#7483) ;
#4270 = LINE('',#87529,#7484) ;
#4271 = LINE('',#87568,#7485) ;
#4272 = LINE('',#87569,#7486) ;
#4273 = LINE('',#87613,#7487) ;
#4274 = LINE('',#87614,#7488) ;
#4275 = LINE('',#87651,#7489) ;
#4276 = LINE('',#87652,#7490) ;
#4277 = LINE('',#87654,#7491) ;
#4278 = LINE('',#87655,#7492) ;
#4279 = LINE('',#87692,#7493) ;
#4280 = LINE('',#87693,#7494) ;
#4281 = LINE('',#87737,#7495) ;
#4282 = LINE('',#87738,#7496) ;
#4283 = LINE('',#87740,#7497) ;
#4284 = LINE('',#87741,#7498) ;
#4285 = LINE('',#87778,#7499) ;
#4286 = LINE('',#87779,#7500) ;
#4287 = LINE('',#87816,#7501) ;
#4288 = LINE('',#87817,#7502) ;
#4289 = LINE('',#87819,#7503) ;
#4290 = LINE('',#87820,#7504) ;
#4291 = LINE('',#87864,#7505) ;
#4292 = LINE('',#87865,#7506) ;
#4293 = LINE('',#87902,#7507) ;
#4294 = LINE('',#87903,#7508) ;
#4295 = LINE('',#87905,#7509) ;
#4296 = LINE('',#87906,#7510) ;
#4297 = LINE('',#87943,#7511) ;
#4298 = LINE('',#87944,#7512) ;
#4299 = LINE('',#87988,#7513) ;
#4300 = LINE('',#87989,#7514) ;
#4301 = LINE('',#87991,#7515) ;
#4302 = LINE('',#87992,#7516) ;
#4303 = LINE('',#88029,#7517) ;
#4304 = LINE('',#88030,#7518) ;
#4305 = LINE('',#88032,#7519) ;
#4306 = LINE('',#88033,#7520) ;
#4307 = LINE('',#88035,#7521) ;
#4308 = LINE('',#88036,#7522) ;
#4309 = LINE('',#88038,#7523) ;
#4310 = LINE('',#88039,#7524) ;
#4311 = LINE('',#88041,#7525) ;
#4312 = LINE('',#88042,#7526) ;
#4313 = LINE('',#88044,#7527) ;
#4314 = LINE('',#88045,#7528) ;
#4315 = LINE('',#88047,#7529) ;
#4316 = LINE('',#88048,#7530) ;
#4317 = LINE('',#88050,#7531) ;
#4318 = LINE('',#88051,#7532) ;
#4319 = LINE('',#88053,#7533) ;
#4320 = LINE('',#88055,#7534) ;
#4321 = LINE('',#88057,#7535) ;
#4322 = LINE('',#88059,#7536) ;
#4323 = LINE('',#88061,#7537) ;
#4324 = LINE('',#88063,#7538) ;
#4325 = LINE('',#88065,#7539) ;
#4326 = LINE('',#88067,#7540) ;
#4327 = LINE('',#88069,#7541) ;
#4328 = LINE('',#88071,#7542) ;
#4329 = LINE('',#88073,#7543) ;
#4330 = LINE('',#88078,#7544) ;
#4331 = LINE('',#88079,#7545) ;
#4332 = LINE('',#88081,#7546) ;
#4333 = LINE('',#88082,#7547) ;
#4334 = LINE('',#88084,#7548) ;
#4335 = LINE('',#88086,#7549) ;
#4336 = LINE('',#88087,#7550) ;
#4337 = LINE('',#88089,#7551) ;
#4338 = LINE('',#88090,#7552) ;
#4339 = LINE('',#88092,#7553) ;
#4340 = LINE('',#88093,#7554) ;
#4341 = LINE('',#88095,#7555) ;
#4342 = LINE('',#88096,#7556) ;
#4343 = LINE('',#88109,#7557) ;
#4344 = LINE('',#88143,#7558) ;
#4345 = LINE('',#88145,#7559) ;
#4346 = LINE('',#88148,#7560) ;
#4347 = LINE('',#88149,#7561) ;
#4348 = LINE('',#88165,#7562) ;
#4349 = LINE('',#88166,#7563) ;
#4350 = LINE('',#88168,#7564) ;
#4351 = LINE('',#88169,#7565) ;
#4352 = LINE('',#88174,#7566) ;
#4353 = LINE('',#88175,#7567) ;
#4354 = LINE('',#88177,#7568) ;
#4355 = LINE('',#88178,#7569) ;
#4356 = LINE('',#88181,#7570) ;
#4357 = LINE('',#88183,#7571) ;
#4358 = LINE('',#88186,#7572) ;
#4359 = LINE('',#88187,#7573) ;
#4360 = LINE('',#88189,#7574) ;
#4361 = LINE('',#88190,#7575) ;
#4362 = LINE('',#88192,#7576) ;
#4363 = LINE('',#88193,#7577) ;
#4364 = LINE('',#88195,#7578) ;
#4365 = LINE('',#88197,#7579) ;
#4366 = LINE('',#88213,#7580) ;
#4367 = LINE('',#88221,#7581) ;
#4368 = LINE('',#88225,#7582) ;
#4369 = LINE('',#88229,#7583) ;
#4370 = LINE('',#88232,#7584) ;
#4371 = LINE('',#88235,#7585) ;
#4372 = LINE('',#88238,#7586) ;
#4373 = LINE('',#88241,#7587) ;
#4374 = LINE('',#88244,#7588) ;
#4375 = LINE('',#88247,#7589) ;
#4376 = LINE('',#88250,#7590) ;
#4377 = LINE('',#88254,#7591) ;
#4378 = LINE('',#88258,#7592) ;
#4379 = LINE('',#88262,#7593) ;
#4380 = LINE('',#88264,#7594) ;
#4381 = LINE('',#88267,#7595) ;
#4382 = LINE('',#88268,#7596) ;
#4383 = LINE('',#88271,#7597) ;
#4384 = LINE('',#88273,#7598) ;
#4385 = LINE('',#88277,#7599) ;
#4386 = LINE('',#88279,#7600) ;
#4387 = LINE('',#88283,#7601) ;
#4388 = LINE('',#88285,#7602) ;
#4389 = LINE('',#88288,#7603) ;
#4390 = LINE('',#88289,#7604) ;
#4391 = LINE('',#88292,#7605) ;
#4392 = LINE('',#88294,#7606) ;
#4393 = LINE('',#88295,#7607) ;
#4394 = LINE('',#88298,#7608) ;
#4395 = LINE('',#88299,#7609) ;
#4396 = LINE('',#88302,#7610) ;
#4397 = LINE('',#88303,#7611) ;
#4398 = LINE('',#88306,#7612) ;
#4399 = LINE('',#88307,#7613) ;
#4400 = LINE('',#88310,#7614) ;
#4401 = LINE('',#88311,#7615) ;
#4402 = LINE('',#88314,#7616) ;
#4403 = LINE('',#88315,#7617) ;
#4404 = LINE('',#88322,#7618) ;
#4405 = LINE('',#88326,#7619) ;
#4406 = LINE('',#88330,#7620) ;
#4407 = LINE('',#88333,#7621) ;
#4408 = LINE('',#88336,#7622) ;
#4409 = LINE('',#88339,#7623) ;
#4410 = LINE('',#88342,#7624) ;
#4411 = LINE('',#88344,#7625) ;
#4412 = LINE('',#88347,#7626) ;
#4413 = LINE('',#88351,#7627) ;
#4414 = LINE('',#88355,#7628) ;
#4415 = LINE('',#88359,#7629) ;
#4416 = LINE('',#88363,#7630) ;
#4417 = LINE('',#88367,#7631) ;
#4418 = LINE('',#88371,#7632) ;
#4419 = LINE('',#88373,#7633) ;
#4420 = LINE('',#88376,#7634) ;
#4421 = LINE('',#88377,#7635) ;
#4422 = LINE('',#88379,#7636) ;
#4423 = LINE('',#88381,#7637) ;
#4424 = LINE('',#88383,#7638) ;
#4425 = LINE('',#88388,#7639) ;
#4426 = LINE('',#88390,#7640) ;
#4427 = LINE('',#88396,#7641) ;
#4428 = LINE('',#88400,#7642) ;
#4429 = LINE('',#88404,#7643) ;
#4430 = LINE('',#88407,#7644) ;
#4431 = LINE('',#88410,#7645) ;
#4432 = LINE('',#88413,#7646) ;
#4433 = LINE('',#88416,#7647) ;
#4434 = LINE('',#88419,#7648) ;
#4435 = LINE('',#88422,#7649) ;
#4436 = LINE('',#88425,#7650) ;
#4437 = LINE('',#88428,#7651) ;
#4438 = LINE('',#88430,#7652) ;
#4439 = LINE('',#88434,#7653) ;
#4440 = LINE('',#88436,#7654) ;
#4441 = LINE('',#88440,#7655) ;
#4442 = LINE('',#88442,#7656) ;
#4443 = LINE('',#88446,#7657) ;
#4444 = LINE('',#88448,#7658) ;
#4445 = LINE('',#88452,#7659) ;
#4446 = LINE('',#88454,#7660) ;
#4447 = LINE('',#88458,#7661) ;
#4448 = LINE('',#88460,#7662) ;
#4449 = LINE('',#88463,#7663) ;
#4450 = LINE('',#88464,#7664) ;
#4451 = LINE('',#88467,#7665) ;
#4452 = LINE('',#88469,#7666) ;
#4453 = LINE('',#88470,#7667) ;
#4454 = LINE('',#88473,#7668) ;
#4455 = LINE('',#88474,#7669) ;
#4456 = LINE('',#88477,#7670) ;
#4457 = LINE('',#88478,#7671) ;
#4458 = LINE('',#88481,#7672) ;
#4459 = LINE('',#88482,#7673) ;
#4460 = LINE('',#88485,#7674) ;
#4461 = LINE('',#88486,#7675) ;
#4462 = LINE('',#88489,#7676) ;
#4463 = LINE('',#88490,#7677) ;
#4464 = LINE('',#88502,#7678) ;
#4465 = LINE('',#88510,#7679) ;
#4466 = LINE('',#88515,#7680) ;
#4467 = LINE('',#88519,#7681) ;
#4468 = LINE('',#88523,#7682) ;
#4469 = LINE('',#88527,#7683) ;
#4470 = LINE('',#88530,#7684) ;
#4471 = LINE('',#88534,#7685) ;
#4472 = LINE('',#88538,#7686) ;
#4473 = LINE('',#88542,#7687) ;
#4474 = LINE('',#88544,#7688) ;
#4475 = LINE('',#88547,#7689) ;
#4476 = LINE('',#88548,#7690) ;
#4477 = LINE('',#88551,#7691) ;
#4478 = LINE('',#88553,#7692) ;
#4479 = LINE('',#88556,#7693) ;
#4480 = LINE('',#88558,#7694) ;
#4481 = LINE('',#88562,#7695) ;
#4482 = LINE('',#88565,#7696) ;
#4483 = LINE('',#88567,#7697) ;
#4484 = LINE('',#88569,#7698) ;
#4485 = LINE('',#88571,#7699) ;
#4486 = LINE('',#88578,#7700) ;
#4487 = LINE('',#88580,#7701) ;
#4488 = LINE('',#88586,#7702) ;
#4489 = LINE('',#88590,#7703) ;
#4490 = LINE('',#88594,#7704) ;
#4491 = LINE('',#88597,#7705) ;
#4492 = LINE('',#88600,#7706) ;
#4493 = LINE('',#88603,#7707) ;
#4494 = LINE('',#88606,#7708) ;
#4495 = LINE('',#88609,#7709) ;
#4496 = LINE('',#88612,#7710) ;
#4497 = LINE('',#88615,#7711) ;
#4498 = LINE('',#88618,#7712) ;
#4499 = LINE('',#88620,#7713) ;
#4500 = LINE('',#88624,#7714) ;
#4501 = LINE('',#88626,#7715) ;
#4502 = LINE('',#88630,#7716) ;
#4503 = LINE('',#88632,#7717) ;
#4504 = LINE('',#88636,#7718) ;
#4505 = LINE('',#88638,#7719) ;
#4506 = LINE('',#88642,#7720) ;
#4507 = LINE('',#88644,#7721) ;
#4508 = LINE('',#88648,#7722) ;
#4509 = LINE('',#88650,#7723) ;
#4510 = LINE('',#88653,#7724) ;
#4511 = LINE('',#88654,#7725) ;
#4512 = LINE('',#88657,#7726) ;
#4513 = LINE('',#88659,#7727) ;
#4514 = LINE('',#88660,#7728) ;
#4515 = LINE('',#88663,#7729) ;
#4516 = LINE('',#88664,#7730) ;
#4517 = LINE('',#88667,#7731) ;
#4518 = LINE('',#88668,#7732) ;
#4519 = LINE('',#88671,#7733) ;
#4520 = LINE('',#88672,#7734) ;
#4521 = LINE('',#88675,#7735) ;
#4522 = LINE('',#88676,#7736) ;
#4523 = LINE('',#88679,#7737) ;
#4524 = LINE('',#88680,#7738) ;
#4525 = LINE('',#88692,#7739) ;
#4526 = LINE('',#88700,#7740) ;
#4527 = LINE('',#88705,#7741) ;
#4528 = LINE('',#88709,#7742) ;
#4529 = LINE('',#88713,#7743) ;
#4530 = LINE('',#88717,#7744) ;
#4531 = LINE('',#88720,#7745) ;
#4532 = LINE('',#88724,#7746) ;
#4533 = LINE('',#88728,#7747) ;
#4534 = LINE('',#88732,#7748) ;
#4535 = LINE('',#88734,#7749) ;
#4536 = LINE('',#88737,#7750) ;
#4537 = LINE('',#88738,#7751) ;
#4538 = LINE('',#88741,#7752) ;
#4539 = LINE('',#88743,#7753) ;
#4540 = LINE('',#88746,#7754) ;
#4541 = LINE('',#88748,#7755) ;
#4542 = LINE('',#88752,#7756) ;
#4543 = LINE('',#88755,#7757) ;
#4544 = LINE('',#88757,#7758) ;
#4545 = LINE('',#88759,#7759) ;
#4546 = LINE('',#88761,#7760) ;
#4547 = LINE('',#88768,#7761) ;
#4548 = LINE('',#88770,#7762) ;
#4549 = LINE('',#88788,#7763) ;
#4550 = LINE('',#88789,#7764) ;
#4551 = LINE('',#88798,#7765) ;
#4552 = LINE('',#88799,#7766) ;
#4553 = LINE('',#88848,#7767) ;
#4554 = LINE('',#88849,#7768) ;
#4555 = LINE('',#88851,#7769) ;
#4556 = LINE('',#88852,#7770) ;
#4557 = LINE('',#88861,#7771) ;
#4558 = LINE('',#88862,#7772) ;
#4559 = LINE('',#88864,#7773) ;
#4560 = LINE('',#88865,#7774) ;
#4561 = LINE('',#88909,#7775) ;
#4562 = LINE('',#88910,#7776) ;
#4563 = LINE('',#88912,#7777) ;
#4564 = LINE('',#88913,#7778) ;
#4565 = LINE('',#88915,#7779) ;
#4566 = LINE('',#88916,#7780) ;
#4567 = LINE('',#88918,#7781) ;
#4568 = LINE('',#88919,#7782) ;
#4569 = LINE('',#88921,#7783) ;
#4570 = LINE('',#88922,#7784) ;
#4571 = LINE('',#88924,#7785) ;
#4572 = LINE('',#88925,#7786) ;
#4573 = LINE('',#88946,#7787) ;
#4574 = LINE('',#88947,#7788) ;
#4575 = LINE('',#88950,#7789) ;
#4576 = LINE('',#88952,#7790) ;
#4577 = LINE('',#88962,#7791) ;
#4578 = LINE('',#88963,#7792) ;
#4579 = LINE('',#88966,#7793) ;
#4580 = LINE('',#88967,#7794) ;
#4581 = LINE('',#88973,#7795) ;
#4582 = LINE('',#88974,#7796) ;
#4583 = LINE('',#88979,#7797) ;
#4584 = LINE('',#88980,#7798) ;
#4585 = LINE('',#88985,#7799) ;
#4586 = LINE('',#88986,#7800) ;
#4587 = LINE('',#88988,#7801) ;
#4588 = LINE('',#88991,#7802) ;
#4589 = LINE('',#88992,#7803) ;
#4590 = LINE('',#88993,#7804) ;
#4591 = LINE('',#88995,#7805) ;
#4592 = LINE('',#89877,#7806) ;
#4593 = LINE('',#89879,#7807) ;
#4594 = LINE('',#89881,#7808) ;
#4595 = LINE('',#89882,#7809) ;
#4596 = LINE('',#89900,#7810) ;
#4597 = LINE('',#89923,#7811) ;
#4598 = LINE('',#89946,#7812) ;
#4599 = LINE('',#89969,#7813) ;
#4600 = LINE('',#89992,#7814) ;
#4601 = LINE('',#90000,#7815) ;
#4602 = LINE('',#90002,#7816) ;
#4603 = LINE('',#90003,#7817) ;
#4604 = LINE('',#90005,#7818) ;
#4605 = LINE('',#90006,#7819) ;
#4606 = LINE('',#90010,#7820) ;
#4607 = LINE('',#90012,#7821) ;
#4608 = LINE('',#90014,#7822) ;
#4609 = LINE('',#90015,#7823) ;
#4610 = LINE('',#90018,#7824) ;
#4611 = LINE('',#90020,#7825) ;
#4612 = LINE('',#90021,#7826) ;
#4613 = LINE('',#90039,#7827) ;
#4614 = LINE('',#90062,#7828) ;
#4615 = LINE('',#90085,#7829) ;
#4616 = LINE('',#90108,#7830) ;
#4617 = LINE('',#90116,#7831) ;
#4618 = LINE('',#90118,#7832) ;
#4619 = LINE('',#90119,#7833) ;
#4620 = LINE('',#90122,#7834) ;
#4621 = LINE('',#90124,#7835) ;
#4622 = LINE('',#90125,#7836) ;
#4623 = LINE('',#90128,#7837) ;
#4624 = LINE('',#90130,#7838) ;
#4625 = LINE('',#90131,#7839) ;
#4626 = LINE('',#90149,#7840) ;
#4627 = LINE('',#90172,#7841) ;
#4628 = LINE('',#90195,#7842) ;
#4629 = LINE('',#90218,#7843) ;
#4630 = LINE('',#90241,#7844) ;
#4631 = LINE('',#90264,#7845) ;
#4632 = LINE('',#90287,#7846) ;
#4633 = LINE('',#90295,#7847) ;
#4634 = LINE('',#90297,#7848) ;
#4635 = LINE('',#90298,#7849) ;
#4636 = LINE('',#90301,#7850) ;
#4637 = LINE('',#90303,#7851) ;
#4638 = LINE('',#90304,#7852) ;
#4639 = LINE('',#90306,#7853) ;
#4640 = LINE('',#90307,#7854) ;
#4641 = LINE('',#90312,#7855) ;
#4642 = LINE('',#90314,#7856) ;
#4643 = LINE('',#90318,#7857) ;
#4644 = LINE('',#90322,#7858) ;
#4645 = LINE('',#90326,#7859) ;
#4646 = LINE('',#90332,#7860) ;
#4647 = LINE('',#90336,#7861) ;
#4648 = LINE('',#90340,#7862) ;
#4649 = LINE('',#90344,#7863) ;
#4650 = LINE('',#90348,#7864) ;
#4651 = LINE('',#90352,#7865) ;
#4652 = LINE('',#90353,#7866) ;
#4653 = LINE('',#90366,#7867) ;
#4654 = LINE('',#90369,#7868) ;
#4655 = LINE('',#90390,#7869) ;
#4656 = LINE('',#90417,#7870) ;
#4657 = LINE('',#90418,#7871) ;
#4658 = LINE('',#90442,#7872) ;
#4659 = LINE('',#90443,#7873) ;
#4660 = LINE('',#90509,#7874) ;
#4661 = LINE('',#90511,#7875) ;
#4662 = LINE('',#90513,#7876) ;
#4663 = LINE('',#90515,#7877) ;
#4664 = LINE('',#90516,#7878) ;
#4665 = LINE('',#90519,#7879) ;
#4666 = LINE('',#90523,#7880) ;
#4667 = LINE('',#90524,#7881) ;
#4668 = LINE('',#90595,#7882) ;
#4669 = LINE('',#90596,#7883) ;
#4670 = LINE('',#90615,#7884) ;
#4671 = LINE('',#90616,#7885) ;
#4672 = LINE('',#90630,#7886) ;
#4673 = LINE('',#90632,#7887) ;
#4674 = LINE('',#90633,#7888) ;
#4675 = LINE('',#90636,#7889) ;
#4676 = LINE('',#90640,#7890) ;
#4677 = LINE('',#90641,#7891) ;
#4678 = LINE('',#90709,#7892) ;
#4679 = LINE('',#90754,#7893) ;
#4680 = LINE('',#90775,#7894) ;
#4681 = LINE('',#90785,#7895) ;
#4682 = LINE('',#90787,#7896) ;
#4683 = LINE('',#90789,#7897) ;
#4684 = LINE('',#90791,#7898) ;
#4685 = LINE('',#90795,#7899) ;
#4686 = LINE('',#90798,#7900) ;
#4687 = LINE('',#90838,#7901) ;
#4688 = LINE('',#90839,#7902) ;
#4689 = LINE('',#90904,#7903) ;
#4690 = LINE('',#90907,#7904) ;
#4691 = LINE('',#90910,#7905) ;
#4692 = LINE('',#90912,#7906) ;
#4693 = LINE('',#90916,#7907) ;
#4694 = LINE('',#90957,#7908) ;
#4695 = LINE('',#90958,#7909) ;
#4696 = LINE('',#91032,#7910) ;
#4697 = LINE('',#91034,#7911) ;
#4698 = LINE('',#91038,#7912) ;
#4699 = LINE('',#91042,#7913) ;
#4700 = LINE('',#91043,#7914) ;
#4701 = LINE('',#91045,#7915) ;
#4702 = LINE('',#91047,#7916) ;
#4703 = LINE('',#91051,#7917) ;
#4704 = LINE('',#91052,#7918) ;
#4705 = LINE('',#91055,#7919) ;
#4706 = LINE('',#91059,#7920) ;
#4707 = LINE('',#91062,#7921) ;
#4708 = LINE('',#91091,#7922) ;
#4709 = LINE('',#91094,#7923) ;
#4710 = LINE('',#91097,#7924) ;
#4711 = LINE('',#91110,#7925) ;
#4712 = LINE('',#91113,#7926) ;
#4713 = LINE('',#91116,#7927) ;
#4714 = LINE('',#91118,#7928) ;
#4715 = LINE('',#91120,#7929) ;
#4716 = LINE('',#91122,#7930) ;
#4717 = LINE('',#91126,#7931) ;
#4718 = LINE('',#91129,#7932) ;
#4719 = LINE('',#91131,#7933) ;
#4720 = LINE('',#91135,#7934) ;
#4721 = LINE('',#91139,#7935) ;
#4722 = LINE('',#91142,#7936) ;
#4723 = LINE('',#91145,#7937) ;
#4724 = LINE('',#91154,#7938) ;
#4725 = LINE('',#91189,#7939) ;
#4726 = LINE('',#91190,#7940) ;
#4727 = LINE('',#91193,#7941) ;
#4728 = LINE('',#91197,#7942) ;
#4729 = LINE('',#91198,#7943) ;
#4730 = LINE('',#91201,#7944) ;
#4731 = LINE('',#91205,#7945) ;
#4732 = LINE('',#91207,#7946) ;
#4733 = LINE('',#91209,#7947) ;
#4734 = LINE('',#91211,#7948) ;
#4735 = LINE('',#91212,#7949) ;
#4736 = LINE('',#91222,#7950) ;
#4737 = LINE('',#91225,#7951) ;
#4738 = LINE('',#91228,#7952) ;
#4739 = LINE('',#91231,#7953) ;
#4740 = LINE('',#91233,#7954) ;
#4741 = LINE('',#91235,#7955) ;
#4742 = LINE('',#91248,#7956) ;
#4743 = LINE('',#91260,#7957) ;
#4744 = LINE('',#91271,#7958) ;
#4745 = LINE('',#91272,#7959) ;
#4746 = LINE('',#91279,#7960) ;
#4747 = LINE('',#91282,#7961) ;
#4748 = LINE('',#91284,#7962) ;
#4749 = LINE('',#91286,#7963) ;
#4750 = LINE('',#91288,#7964) ;
#4751 = LINE('',#91290,#7965) ;
#4752 = LINE('',#91291,#7966) ;
#4753 = LINE('',#91294,#7967) ;
#4754 = LINE('',#91298,#7968) ;
#4755 = LINE('',#91302,#7969) ;
#4756 = LINE('',#91304,#7970) ;
#4757 = LINE('',#91306,#7971) ;
#4758 = LINE('',#91330,#7972) ;
#4759 = LINE('',#91331,#7973) ;
#4760 = LINE('',#91360,#7974) ;
#4761 = LINE('',#91361,#7975) ;
#4762 = LINE('',#91378,#7976) ;
#4763 = LINE('',#91379,#7977) ;
#4764 = LINE('',#91387,#7978) ;
#4765 = LINE('',#91388,#7979) ;
#4766 = LINE('',#91393,#7980) ;
#4767 = LINE('',#91394,#7981) ;
#4768 = LINE('',#91408,#7982) ;
#4769 = LINE('',#91412,#7983) ;
#4770 = LINE('',#91416,#7984) ;
#4771 = LINE('',#91418,#7985) ;
#4772 = LINE('',#91420,#7986) ;
#4773 = LINE('',#91428,#7987) ;
#4774 = LINE('',#91432,#7988) ;
#4775 = LINE('',#91433,#7989) ;
#4776 = LINE('',#91439,#7990) ;
#4777 = LINE('',#91443,#7991) ;
#4778 = LINE('',#91516,#7992) ;
#4779 = LINE('',#91520,#7993) ;
#4780 = LINE('',#91523,#7994) ;
#4781 = LINE('',#91574,#7995) ;
#4782 = LINE('',#91576,#7996) ;
#4783 = LINE('',#91577,#7997) ;
#4784 = LINE('',#91589,#7998) ;
#4785 = LINE('',#91595,#7999) ;
#4786 = LINE('',#91656,#8000) ;
#4787 = LINE('',#91657,#8001) ;
#4788 = LINE('',#91713,#8002) ;
#4789 = LINE('',#91721,#8003) ;
#4790 = LINE('',#91732,#8004) ;
#4791 = LINE('',#91733,#8005) ;
#4792 = LINE('',#91739,#8006) ;
#4793 = LINE('',#91743,#8007) ;
#4794 = LINE('',#91744,#8008) ;
#4795 = LINE('',#91747,#8009) ;
#4796 = LINE('',#91751,#8010) ;
#4797 = LINE('',#91753,#8011) ;
#4798 = LINE('',#91755,#8012) ;
#4799 = LINE('',#91756,#8013) ;
#4800 = LINE('',#91759,#8014) ;
#4801 = LINE('',#91764,#8015) ;
#4802 = LINE('',#91860,#8016) ;
#4803 = LINE('',#91861,#8017) ;
#4804 = LINE('',#91944,#8018) ;
#4805 = LINE('',#91952,#8019) ;
#4806 = LINE('',#91955,#8020) ;
#4807 = LINE('',#91957,#8021) ;
#4808 = LINE('',#91959,#8022) ;
#4809 = LINE('',#91970,#8023) ;
#4810 = LINE('',#91973,#8024) ;
#4811 = LINE('',#91976,#8025) ;
#4812 = LINE('',#91982,#8026) ;
#4813 = LINE('',#92016,#8027) ;
#4814 = LINE('',#92019,#8028) ;
#4815 = LINE('',#92022,#8029) ;
#4816 = LINE('',#92025,#8030) ;
#4817 = LINE('',#92028,#8031) ;
#4818 = LINE('',#92029,#8032) ;
#4819 = LINE('',#92088,#8033) ;
#4820 = LINE('',#92089,#8034) ;
#4821 = LINE('',#92092,#8035) ;
#4822 = LINE('',#92094,#8036) ;
#4823 = LINE('',#92096,#8037) ;
#4824 = LINE('',#92098,#8038) ;
#4825 = LINE('',#92099,#8039) ;
#4826 = LINE('',#92102,#8040) ;
#4827 = LINE('',#92106,#8041) ;
#4828 = LINE('',#92109,#8042) ;
#4829 = LINE('',#92118,#8043) ;
#4830 = LINE('',#92119,#8044) ;
#4831 = LINE('',#92121,#8045) ;
#4832 = LINE('',#92122,#8046) ;
#4833 = LINE('',#92133,#8047) ;
#4834 = LINE('',#92134,#8048) ;
#4835 = LINE('',#92136,#8049) ;
#4836 = LINE('',#92137,#8050) ;
#4837 = LINE('',#92139,#8051) ;
#4838 = LINE('',#92140,#8052) ;
#4839 = LINE('',#92143,#8053) ;
#4840 = LINE('',#92147,#8054) ;
#4841 = LINE('',#92151,#8055) ;
#4842 = LINE('',#92155,#8056) ;
#4843 = LINE('',#92159,#8057) ;
#4844 = LINE('',#92161,#8058) ;
#4845 = LINE('',#92163,#8059) ;
#4846 = LINE('',#92165,#8060) ;
#4847 = LINE('',#92167,#8061) ;
#4848 = LINE('',#92171,#8062) ;
#4849 = LINE('',#92175,#8063) ;
#4850 = LINE('',#92179,#8064) ;
#4851 = LINE('',#92183,#8065) ;
#4852 = LINE('',#92187,#8066) ;
#4853 = LINE('',#92191,#8067) ;
#4854 = LINE('',#92193,#8068) ;
#4855 = LINE('',#92195,#8069) ;
#4856 = LINE('',#92199,#8070) ;
#4857 = LINE('',#92203,#8071) ;
#4858 = LINE('',#92207,#8072) ;
#4859 = LINE('',#92211,#8073) ;
#4860 = LINE('',#92215,#8074) ;
#4861 = LINE('',#92217,#8075) ;
#4862 = LINE('',#92219,#8076) ;
#4863 = LINE('',#92221,#8077) ;
#4864 = LINE('',#92223,#8078) ;
#4865 = LINE('',#92225,#8079) ;
#4866 = LINE('',#92234,#8080) ;
#4867 = LINE('',#92243,#8081) ;
#4868 = LINE('',#92245,#8082) ;
#4869 = LINE('',#92247,#8083) ;
#4870 = LINE('',#92251,#8084) ;
#4871 = LINE('',#92255,#8085) ;
#4872 = LINE('',#92257,#8086) ;
#4873 = LINE('',#92261,#8087) ;
#4874 = LINE('',#92263,#8088) ;
#4875 = LINE('',#92267,#8089) ;
#4876 = LINE('',#92276,#8090) ;
#4877 = LINE('',#92278,#8091) ;
#4878 = LINE('',#92280,#8092) ;
#4879 = LINE('',#92290,#8093) ;
#4880 = LINE('',#92294,#8094) ;
#4881 = LINE('',#92296,#8095) ;
#4882 = LINE('',#92300,#8096) ;
#4883 = LINE('',#92304,#8097) ;
#4884 = LINE('',#92306,#8098) ;
#4885 = LINE('',#92310,#8099) ;
#4886 = LINE('',#92314,#8100) ;
#4887 = LINE('',#92316,#8101) ;
#4888 = LINE('',#92318,#8102) ;
#4889 = LINE('',#92322,#8103) ;
#4890 = LINE('',#92326,#8104) ;
#4891 = LINE('',#92330,#8105) ;
#4892 = LINE('',#92334,#8106) ;
#4893 = LINE('',#92335,#8107) ;
#4894 = LINE('',#92341,#8108) ;
#4895 = LINE('',#92345,#8109) ;
#4896 = LINE('',#92347,#8110) ;
#4897 = LINE('',#92351,#8111) ;
#4898 = LINE('',#92357,#8112) ;
#4899 = LINE('',#92358,#8113) ;
#4900 = LINE('',#92363,#8114) ;
#4901 = LINE('',#92367,#8115) ;
#4902 = LINE('',#92371,#8116) ;
#4903 = LINE('',#92374,#8117) ;
#4904 = LINE('',#92381,#8118) ;
#4905 = LINE('',#92385,#8119) ;
#4906 = LINE('',#92387,#8120) ;
#4907 = LINE('',#92391,#8121) ;
#4908 = LINE('',#92395,#8122) ;
#4909 = LINE('',#92399,#8123) ;
#4910 = LINE('',#92403,#8124) ;
#4911 = LINE('',#92404,#8125) ;
#4912 = LINE('',#92409,#8126) ;
#4913 = LINE('',#92418,#8127) ;
#4914 = LINE('',#92422,#8128) ;
#4915 = LINE('',#92426,#8129) ;
#4916 = LINE('',#92430,#8130) ;
#4917 = LINE('',#92434,#8131) ;
#4918 = LINE('',#92449,#8132) ;
#4919 = LINE('',#92451,#8133) ;
#4920 = LINE('',#92453,#8134) ;
#4921 = LINE('',#92457,#8135) ;
#4922 = LINE('',#92461,#8136) ;
#4923 = LINE('',#92465,#8137) ;
#4924 = LINE('',#92469,#8138) ;
#4925 = LINE('',#92470,#8139) ;
#4926 = LINE('',#92475,#8140) ;
#4927 = LINE('',#92479,#8141) ;
#4928 = LINE('',#92481,#8142) ;
#4929 = LINE('',#92485,#8143) ;
#4930 = LINE('',#92489,#8144) ;
#4931 = LINE('',#92493,#8145) ;
#4932 = LINE('',#92497,#8146) ;
#4933 = LINE('',#92498,#8147) ;
#4934 = LINE('',#92578,#8148) ;
#4935 = LINE('',#92579,#8149) ;
#4936 = LINE('',#92609,#8150) ;
#4937 = LINE('',#92611,#8151) ;
#4938 = LINE('',#92614,#8152) ;
#4939 = LINE('',#92617,#8153) ;
#4940 = LINE('',#92620,#8154) ;
#4941 = LINE('',#92621,#8155) ;
#4942 = LINE('',#92623,#8156) ;
#4943 = LINE('',#92624,#8157) ;
#4944 = LINE('',#92626,#8158) ;
#4945 = LINE('',#92628,#8159) ;
#4946 = LINE('',#92630,#8160) ;
#4947 = LINE('',#92631,#8161) ;
#4948 = LINE('',#92641,#8162) ;
#4949 = LINE('',#92644,#8163) ;
#4950 = LINE('',#92655,#8164) ;
#4951 = LINE('',#92656,#8165) ;
#4952 = LINE('',#92664,#8166) ;
#4953 = LINE('',#92665,#8167) ;
#4954 = LINE('',#92684,#8168) ;
#4955 = LINE('',#92687,#8169) ;
#4956 = LINE('',#92695,#8170) ;
#4957 = LINE('',#92696,#8171) ;
#4958 = LINE('',#92772,#8172) ;
#4959 = LINE('',#92778,#8173) ;
#4960 = LINE('',#92780,#8174) ;
#4961 = LINE('',#92781,#8175) ;
#4962 = LINE('',#92785,#8176) ;
#4963 = LINE('',#92793,#8177) ;
#4964 = LINE('',#92841,#8178) ;
#4965 = LINE('',#92843,#8179) ;
#4966 = LINE('',#92847,#8180) ;
#4967 = LINE('',#92849,#8181) ;
#4968 = LINE('',#92851,#8182) ;
#4969 = LINE('',#92855,#8183) ;
#4970 = LINE('',#92859,#8184) ;
#4971 = LINE('',#92860,#8185) ;
#4972 = LINE('',#92863,#8186) ;
#4973 = LINE('',#92867,#8187) ;
#4974 = LINE('',#92869,#8188) ;
#4975 = LINE('',#92873,#8189) ;
#4976 = LINE('',#92877,#8190) ;
#4977 = LINE('',#92880,#8191) ;
#4978 = LINE('',#92883,#8192) ;
#4979 = LINE('',#92887,#8193) ;
#4980 = LINE('',#92888,#8194) ;
#4981 = LINE('',#92891,#8195) ;
#4982 = LINE('',#92973,#8196) ;
#4983 = LINE('',#92974,#8197) ;
#4984 = LINE('',#92988,#8198) ;
#4985 = LINE('',#92989,#8199) ;
#4986 = LINE('',#93076,#8200) ;
#4987 = LINE('',#93077,#8201) ;
#4988 = LINE('',#93082,#8202) ;
#4989 = LINE('',#93083,#8203) ;
#4990 = LINE('',#93145,#8204) ;
#4991 = LINE('',#93150,#8205) ;
#4992 = LINE('',#93151,#8206) ;
#4993 = LINE('',#93159,#8207) ;
#4994 = LINE('',#93165,#8208) ;
#4995 = LINE('',#93170,#8209) ;
#4996 = LINE('',#93171,#8210) ;
#4997 = LINE('',#93176,#8211) ;
#4998 = LINE('',#93177,#8212) ;
#4999 = LINE('',#93188,#8213) ;
#5000 = LINE('',#93189,#8214) ;
#5001 = LINE('',#93200,#8215) ;
#5002 = LINE('',#93201,#8216) ;
#5003 = LINE('',#93212,#8217) ;
#5004 = LINE('',#93213,#8218) ;
#5005 = LINE('',#93221,#8219) ;
#5006 = LINE('',#93222,#8220) ;
#5007 = LINE('',#93227,#8221) ;
#5008 = LINE('',#93228,#8222) ;
#5009 = LINE('',#93291,#8223) ;
#5010 = LINE('',#93292,#8224) ;
#5011 = LINE('',#93296,#8225) ;
#5012 = LINE('',#93299,#8226) ;
#5013 = LINE('',#93306,#8227) ;
#5014 = LINE('',#93309,#8228) ;
#5015 = LINE('',#93311,#8229) ;
#5016 = LINE('',#93312,#8230) ;
#5017 = LINE('',#93314,#8231) ;
#5018 = LINE('',#93316,#8232) ;
#5019 = LINE('',#93319,#8233) ;
#5020 = LINE('',#93322,#8234) ;
#5021 = LINE('',#93324,#8235) ;
#5022 = LINE('',#93326,#8236) ;
#5023 = LINE('',#93327,#8237) ;
#5024 = LINE('',#93329,#8238) ;
#5025 = LINE('',#93332,#8239) ;
#5026 = LINE('',#93333,#8240) ;
#5027 = LINE('',#93334,#8241) ;
#5028 = LINE('',#93336,#8242) ;
#5029 = LINE('',#93339,#8243) ;
#5030 = LINE('',#93346,#8244) ;
#5031 = LINE('',#93349,#8245) ;
#5032 = LINE('',#93352,#8246) ;
#5033 = LINE('',#93354,#8247) ;
#5034 = LINE('',#93355,#8248) ;
#5035 = LINE('',#93361,#8249) ;
#5036 = LINE('',#93381,#8250) ;
#5037 = LINE('',#93382,#8251) ;
#5038 = LINE('',#93388,#8252) ;
#5039 = LINE('',#93391,#8253) ;
#5040 = LINE('',#93399,#8254) ;
#5041 = LINE('',#93400,#8255) ;
#5042 = LINE('',#93405,#8256) ;
#5043 = LINE('',#93406,#8257) ;
#5044 = LINE('',#93411,#8258) ;
#5045 = LINE('',#93412,#8259) ;
#5046 = LINE('',#93417,#8260) ;
#5047 = LINE('',#93418,#8261) ;
#5048 = LINE('',#93429,#8262) ;
#5049 = LINE('',#93430,#8263) ;
#5050 = LINE('',#93433,#8264) ;
#5051 = LINE('',#93436,#8265) ;
#5052 = LINE('',#93439,#8266) ;
#5053 = LINE('',#93441,#8267) ;
#5054 = LINE('',#93445,#8268) ;
#5055 = LINE('',#93447,#8269) ;
#5056 = LINE('',#93451,#8270) ;
#5057 = LINE('',#93455,#8271) ;
#5058 = LINE('',#93458,#8272) ;
#5059 = LINE('',#93461,#8273) ;
#5060 = LINE('',#93465,#8274) ;
#5061 = LINE('',#93467,#8275) ;
#5062 = LINE('',#93469,#8276) ;
#5063 = LINE('',#93471,#8277) ;
#5064 = LINE('',#93472,#8278) ;
#5065 = LINE('',#93473,#8279) ;
#5066 = LINE('',#93474,#8280) ;
#5067 = LINE('',#93479,#8281) ;
#5068 = LINE('',#93520,#8282) ;
#5069 = LINE('',#93528,#8283) ;
#5070 = LINE('',#93536,#8284) ;
#5071 = LINE('',#93544,#8285) ;
#5072 = LINE('',#93552,#8286) ;
#5073 = LINE('',#93560,#8287) ;
#5074 = LINE('',#93591,#8288) ;
#5075 = LINE('',#93694,#8289) ;
#5076 = LINE('',#93705,#8290) ;
#5077 = LINE('',#93714,#8291) ;
#5078 = LINE('',#93715,#8292) ;
#5079 = LINE('',#93719,#8293) ;
#5080 = LINE('',#93721,#8294) ;
#5081 = LINE('',#93723,#8295) ;
#5082 = LINE('',#93725,#8296) ;
#5083 = LINE('',#93730,#8297) ;
#5084 = LINE('',#93735,#8298) ;
#5085 = LINE('',#93742,#8299) ;
#5086 = LINE('',#93750,#8300) ;
#5087 = LINE('',#93761,#8301) ;
#5088 = LINE('',#93768,#8302) ;
#5089 = LINE('',#93775,#8303) ;
#5090 = LINE('',#93778,#8304) ;
#5091 = LINE('',#93787,#8305) ;
#5092 = LINE('',#93795,#8306) ;
#5093 = LINE('',#93801,#8307) ;
#5094 = LINE('',#93804,#8308) ;
#5095 = LINE('',#93808,#8309) ;
#5096 = LINE('',#93812,#8310) ;
#5097 = LINE('',#93816,#8311) ;
#5098 = LINE('',#93844,#8312) ;
#5099 = LINE('',#93858,#8313) ;
#5100 = LINE('',#93860,#8314) ;
#5101 = LINE('',#93862,#8315) ;
#5102 = LINE('',#93863,#8316) ;
#5103 = LINE('',#93866,#8317) ;
#5104 = LINE('',#93868,#8318) ;
#5105 = LINE('',#93870,#8319) ;
#5106 = LINE('',#93889,#8320) ;
#5107 = LINE('',#93902,#8321) ;
#5108 = LINE('',#93905,#8322) ;
#5109 = LINE('',#93909,#8323) ;
#5110 = LINE('',#93911,#8324) ;
#5111 = LINE('',#93915,#8325) ;
#5112 = LINE('',#93916,#8326) ;
#5113 = LINE('',#93918,#8327) ;
#5114 = LINE('',#93924,#8328) ;
#5115 = LINE('',#93928,#8329) ;
#5116 = LINE('',#93930,#8330) ;
#5117 = LINE('',#93932,#8331) ;
#5118 = LINE('',#93933,#8332) ;
#5119 = LINE('',#93935,#8333) ;
#5120 = LINE('',#93936,#8334) ;
#5121 = LINE('',#94015,#8335) ;
#5122 = LINE('',#94018,#8336) ;
#5123 = LINE('',#94087,#8337) ;
#5124 = LINE('',#94088,#8338) ;
#5125 = LINE('',#94093,#8339) ;
#5126 = LINE('',#94094,#8340) ;
#5127 = LINE('',#94096,#8341) ;
#5128 = LINE('',#94097,#8342) ;
#5129 = LINE('',#94102,#8343) ;
#5130 = LINE('',#94103,#8344) ;
#5131 = LINE('',#94107,#8345) ;
#5132 = LINE('',#94108,#8346) ;
#5133 = LINE('',#94158,#8347) ;
#5134 = LINE('',#94161,#8348) ;
#5135 = LINE('',#94163,#8349) ;
#5136 = LINE('',#94165,#8350) ;
#5137 = LINE('',#94168,#8351) ;
#5138 = LINE('',#94171,#8352) ;
#5139 = LINE('',#94178,#8353) ;
#5140 = LINE('',#94195,#8354) ;
#5141 = LINE('',#94200,#8355) ;
#5142 = LINE('',#94204,#8356) ;
#5143 = LINE('',#94207,#8357) ;
#5144 = LINE('',#94209,#8358) ;
#5145 = LINE('',#94211,#8359) ;
#5146 = LINE('',#94213,#8360) ;
#5147 = LINE('',#94214,#8361) ;
#5148 = LINE('',#94217,#8362) ;
#5149 = LINE('',#94218,#8363) ;
#5150 = LINE('',#94220,#8364) ;
#5151 = LINE('',#94221,#8365) ;
#5152 = LINE('',#94430,#8366) ;
#5153 = LINE('',#94438,#8367) ;
#5154 = LINE('',#94445,#8368) ;
#5155 = LINE('',#94448,#8369) ;
#5156 = LINE('',#94485,#8370) ;
#5157 = LINE('',#94486,#8371) ;
#5158 = LINE('',#94561,#8372) ;
#5159 = LINE('',#94565,#8373) ;
#5160 = LINE('',#94567,#8374) ;
#5161 = LINE('',#94569,#8375) ;
#5162 = LINE('',#94572,#8376) ;
#5163 = LINE('',#94573,#8377) ;
#5164 = LINE('',#94576,#8378) ;
#5165 = LINE('',#94580,#8379) ;
#5166 = LINE('',#94582,#8380) ;
#5167 = LINE('',#94584,#8381) ;
#5168 = LINE('',#94588,#8382) ;
#5169 = LINE('',#94590,#8383) ;
#5170 = LINE('',#94592,#8384) ;
#5171 = LINE('',#94594,#8385) ;
#5172 = LINE('',#94595,#8386) ;
#5173 = LINE('',#94598,#8387) ;
#5174 = LINE('',#94600,#8388) ;
#5175 = LINE('',#94604,#8389) ;
#5176 = LINE('',#94606,#8390) ;
#5177 = LINE('',#94608,#8391) ;
#5178 = LINE('',#94610,#8392) ;
#5179 = LINE('',#94612,#8393) ;
#5180 = LINE('',#94614,#8394) ;
#5181 = LINE('',#94617,#8395) ;
#5182 = LINE('',#94620,#8396) ;
#5183 = LINE('',#94622,#8397) ;
#5184 = LINE('',#94624,#8398) ;
#5185 = LINE('',#94625,#8399) ;
#5186 = LINE('',#94628,#8400) ;
#5187 = LINE('',#94632,#8401) ;
#5188 = LINE('',#94672,#8402) ;
#5189 = LINE('',#94686,#8403) ;
#5190 = LINE('',#94734,#8404) ;
#5191 = LINE('',#94778,#8405) ;
#5192 = LINE('',#94780,#8406) ;
#5193 = LINE('',#94783,#8407) ;
#5194 = LINE('',#94787,#8408) ;
#5195 = LINE('',#94788,#8409) ;
#5196 = LINE('',#94790,#8410) ;
#5197 = LINE('',#94791,#8411) ;
#5198 = LINE('',#94798,#8412) ;
#5199 = LINE('',#94805,#8413) ;
#5200 = LINE('',#94808,#8414) ;
#5201 = LINE('',#94826,#8415) ;
#5202 = LINE('',#94828,#8416) ;
#5203 = LINE('',#94833,#8417) ;
#5204 = LINE('',#94835,#8418) ;
#5205 = LINE('',#94837,#8419) ;
#5206 = LINE('',#94838,#8420) ;
#5207 = LINE('',#94839,#8421) ;
#5208 = LINE('',#94843,#8422) ;
#5209 = LINE('',#94846,#8423) ;
#5210 = LINE('',#94848,#8424) ;
#5211 = LINE('',#94849,#8425) ;
#5212 = LINE('',#94891,#8426) ;
#5213 = LINE('',#94895,#8427) ;
#5214 = LINE('',#94899,#8428) ;
#5215 = LINE('',#94900,#8429) ;
#5216 = LINE('',#94903,#8430) ;
#5217 = LINE('',#94904,#8431) ;
#5218 = LINE('',#94906,#8432) ;
#5219 = LINE('',#94909,#8433) ;
#5220 = LINE('',#94911,#8434) ;
#5221 = LINE('',#94915,#8435) ;
#5222 = LINE('',#94918,#8436) ;
#5223 = LINE('',#94919,#8437) ;
#5224 = LINE('',#94929,#8438) ;
#5225 = LINE('',#94932,#8439) ;
#5226 = LINE('',#94934,#8440) ;
#5227 = LINE('',#94935,#8441) ;
#5228 = LINE('',#94938,#8442) ;
#5229 = LINE('',#94940,#8443) ;
#5230 = LINE('',#94941,#8444) ;
#5231 = LINE('',#94943,#8445) ;
#5232 = LINE('',#94944,#8446) ;
#5233 = LINE('',#94946,#8447) ;
#5234 = LINE('',#94948,#8448) ;
#5235 = LINE('',#94950,#8449) ;
#5236 = LINE('',#94955,#8450) ;
#5237 = LINE('',#94972,#8451) ;
#5238 = LINE('',#95158,#8452) ;
#5239 = LINE('',#95174,#8453) ;
#5240 = LINE('',#95270,#8454) ;
#5241 = LINE('',#95272,#8455) ;
#5242 = LINE('',#95276,#8456) ;
#5243 = LINE('',#95278,#8457) ;
#5244 = LINE('',#95281,#8458) ;
#5245 = LINE('',#95282,#8459) ;
#5246 = LINE('',#95285,#8460) ;
#5247 = LINE('',#95287,#8461) ;
#5248 = LINE('',#95288,#8462) ;
#5249 = LINE('',#95291,#8463) ;
#5250 = LINE('',#95292,#8464) ;
#5251 = LINE('',#95295,#8465) ;
#5252 = LINE('',#95296,#8466) ;
#5253 = LINE('',#95299,#8467) ;
#5254 = LINE('',#95300,#8468) ;
#5255 = LINE('',#95538,#8469) ;
#5256 = LINE('',#95541,#8470) ;
#5257 = LINE('',#95544,#8471) ;
#5258 = LINE('',#95547,#8472) ;
#5259 = LINE('',#95550,#8473) ;
#5260 = LINE('',#95552,#8474) ;
#5261 = LINE('',#95556,#8475) ;
#5262 = LINE('',#95558,#8476) ;
#5263 = LINE('',#95783,#8477) ;
#5264 = LINE('',#95784,#8478) ;
#5265 = LINE('',#95787,#8479) ;
#5266 = LINE('',#95789,#8480) ;
#5267 = LINE('',#95790,#8481) ;
#5268 = LINE('',#95812,#8482) ;
#5269 = LINE('',#95966,#8483) ;
#5270 = LINE('',#95967,#8484) ;
#5271 = LINE('',#95989,#8485) ;
#5272 = LINE('',#96079,#8486) ;
#5273 = LINE('',#96083,#8487) ;
#5274 = LINE('',#96087,#8488) ;
#5275 = LINE('',#96090,#8489) ;
#5276 = LINE('',#96093,#8490) ;
#5277 = LINE('',#96096,#8491) ;
#5278 = LINE('',#96099,#8492) ;
#5279 = LINE('',#96101,#8493) ;
#5280 = LINE('',#96105,#8494) ;
#5281 = LINE('',#96107,#8495) ;
#5282 = LINE('',#96111,#8496) ;
#5283 = LINE('',#96113,#8497) ;
#5284 = LINE('',#96116,#8498) ;
#5285 = LINE('',#96117,#8499) ;
#5286 = LINE('',#96120,#8500) ;
#5287 = LINE('',#96122,#8501) ;
#5288 = LINE('',#96123,#8502) ;
#5289 = LINE('',#96126,#8503) ;
#5290 = LINE('',#96127,#8504) ;
#5291 = LINE('',#96130,#8505) ;
#5292 = LINE('',#96131,#8506) ;
#5293 = LINE('',#96134,#8507) ;
#5294 = LINE('',#96135,#8508) ;
#5295 = LINE('',#96140,#8509) ;
#5296 = LINE('',#96144,#8510) ;
#5297 = LINE('',#96148,#8511) ;
#5298 = LINE('',#96150,#8512) ;
#5299 = LINE('',#96154,#8513) ;
#5300 = LINE('',#96156,#8514) ;
#5301 = LINE('',#96159,#8515) ;
#5302 = LINE('',#96160,#8516) ;
#5303 = LINE('',#96163,#8517) ;
#5304 = LINE('',#96165,#8518) ;
#5305 = LINE('',#96166,#8519) ;
#5306 = LINE('',#96169,#8520) ;
#5307 = LINE('',#96170,#8521) ;
#5308 = LINE('',#96175,#8522) ;
#5309 = LINE('',#96179,#8523) ;
#5310 = LINE('',#96183,#8524) ;
#5311 = LINE('',#96186,#8525) ;
#5312 = LINE('',#96189,#8526) ;
#5313 = LINE('',#96192,#8527) ;
#5314 = LINE('',#96195,#8528) ;
#5315 = LINE('',#96197,#8529) ;
#5316 = LINE('',#96201,#8530) ;
#5317 = LINE('',#96203,#8531) ;
#5318 = LINE('',#96207,#8532) ;
#5319 = LINE('',#96209,#8533) ;
#5320 = LINE('',#96212,#8534) ;
#5321 = LINE('',#96213,#8535) ;
#5322 = LINE('',#96216,#8536) ;
#5323 = LINE('',#96218,#8537) ;
#5324 = LINE('',#96219,#8538) ;
#5325 = LINE('',#96222,#8539) ;
#5326 = LINE('',#96223,#8540) ;
#5327 = LINE('',#96226,#8541) ;
#5328 = LINE('',#96227,#8542) ;
#5329 = LINE('',#96230,#8543) ;
#5330 = LINE('',#96231,#8544) ;
#5331 = LINE('',#96236,#8545) ;
#5332 = LINE('',#96240,#8546) ;
#5333 = LINE('',#96244,#8547) ;
#5334 = LINE('',#96246,#8548) ;
#5335 = LINE('',#96250,#8549) ;
#5336 = LINE('',#96252,#8550) ;
#5337 = LINE('',#96255,#8551) ;
#5338 = LINE('',#96256,#8552) ;
#5339 = LINE('',#96259,#8553) ;
#5340 = LINE('',#96261,#8554) ;
#5341 = LINE('',#96262,#8555) ;
#5342 = LINE('',#96265,#8556) ;
#5343 = LINE('',#96266,#8557) ;
#5344 = LINE('',#96271,#8558) ;
#5345 = LINE('',#96275,#8559) ;
#5346 = LINE('',#96279,#8560) ;
#5347 = LINE('',#96282,#8561) ;
#5348 = LINE('',#96285,#8562) ;
#5349 = LINE('',#96288,#8563) ;
#5350 = LINE('',#96297,#8564) ;
#5351 = LINE('',#96299,#8565) ;
#5352 = LINE('',#96303,#8566) ;
#5353 = LINE('',#96305,#8567) ;
#5354 = LINE('',#96309,#8568) ;
#5355 = LINE('',#96312,#8569) ;
#5356 = LINE('',#96321,#8570) ;
#5357 = LINE('',#96323,#8571) ;
#5358 = LINE('',#96327,#8572) ;
#5359 = LINE('',#96329,#8573) ;
#5360 = LINE('',#96332,#8574) ;
#5361 = LINE('',#96333,#8575) ;
#5362 = LINE('',#96336,#8576) ;
#5363 = LINE('',#96338,#8577) ;
#5364 = LINE('',#96339,#8578) ;
#5365 = LINE('',#96342,#8579) ;
#5366 = LINE('',#96346,#8580) ;
#5367 = LINE('',#96347,#8581) ;
#5368 = LINE('',#96350,#8582) ;
#5369 = LINE('',#96351,#8583) ;
#5370 = LINE('',#96354,#8584) ;
#5371 = LINE('',#96355,#8585) ;
#5372 = LINE('',#96358,#8586) ;
#5373 = LINE('',#96359,#8587) ;
#5374 = LINE('',#96364,#8588) ;
#5375 = LINE('',#96368,#8589) ;
#5376 = LINE('',#96372,#8590) ;
#5377 = LINE('',#96375,#8591) ;
#5378 = LINE('',#96384,#8592) ;
#5379 = LINE('',#96386,#8593) ;
#5380 = LINE('',#96390,#8594) ;
#5381 = LINE('',#96393,#8595) ;
#5382 = LINE('',#96396,#8596) ;
#5383 = LINE('',#96399,#8597) ;
#5384 = LINE('',#96408,#8598) ;
#5385 = LINE('',#96410,#8599) ;
#5386 = LINE('',#96414,#8600) ;
#5387 = LINE('',#96416,#8601) ;
#5388 = LINE('',#96420,#8602) ;
#5389 = LINE('',#96422,#8603) ;
#5390 = LINE('',#96425,#8604) ;
#5391 = LINE('',#96426,#8605) ;
#5392 = LINE('',#96429,#8606) ;
#5393 = LINE('',#96432,#8607) ;
#5394 = LINE('',#96435,#8608) ;
#5395 = LINE('',#96436,#8609) ;
#5396 = LINE('',#96439,#8610) ;
#5397 = LINE('',#96440,#8611) ;
#5398 = LINE('',#96443,#8612) ;
#5399 = LINE('',#96444,#8613) ;
#5400 = LINE('',#96447,#8614) ;
#5401 = LINE('',#96448,#8615) ;
#5402 = LINE('',#96451,#8616) ;
#5403 = LINE('',#96452,#8617) ;
#5404 = LINE('',#96759,#8618) ;
#5405 = LINE('',#96901,#8619) ;
#5406 = LINE('',#96903,#8620) ;
#5407 = LINE('',#97054,#8621) ;
#5408 = LINE('',#97057,#8622) ;
#5409 = LINE('',#97073,#8623) ;
#5410 = LINE('',#97189,#8624) ;
#5411 = LINE('',#97191,#8625) ;
#5412 = LINE('',#97195,#8626) ;
#5413 = LINE('',#97198,#8627) ;
#5414 = LINE('',#97202,#8628) ;
#5415 = LINE('',#97205,#8629) ;
#5416 = LINE('',#97208,#8630) ;
#5417 = LINE('',#97212,#8631) ;
#5418 = LINE('',#97216,#8632) ;
#5419 = LINE('',#97220,#8633) ;
#5420 = LINE('',#97223,#8634) ;
#5421 = LINE('',#97224,#8635) ;
#5422 = LINE('',#97226,#8636) ;
#5423 = LINE('',#97228,#8637) ;
#5424 = LINE('',#97233,#8638) ;
#5425 = LINE('',#97237,#8639) ;
#5426 = LINE('',#97242,#8640) ;
#5427 = LINE('',#97245,#8641) ;
#5428 = LINE('',#97297,#8642) ;
#5429 = LINE('',#97301,#8643) ;
#5430 = LINE('',#97303,#8644) ;
#5431 = LINE('',#97305,#8645) ;
#5432 = LINE('',#97306,#8646) ;
#5433 = LINE('',#97309,#8647) ;
#5434 = LINE('',#97311,#8648) ;
#5435 = LINE('',#97313,#8649) ;
#5436 = LINE('',#97315,#8650) ;
#5437 = LINE('',#97317,#8651) ;
#5438 = LINE('',#97319,#8652) ;
#5439 = LINE('',#97320,#8653) ;
#5440 = LINE('',#97328,#8654) ;
#5441 = LINE('',#97331,#8655) ;
#5442 = LINE('',#97333,#8656) ;
#5443 = LINE('',#97338,#8657) ;
#5444 = LINE('',#97342,#8658) ;
#5445 = LINE('',#97352,#8659) ;
#5446 = LINE('',#97354,#8660) ;
#5447 = LINE('',#97356,#8661) ;
#5448 = LINE('',#97363,#8662) ;
#5449 = LINE('',#97367,#8663) ;
#5450 = LINE('',#97371,#8664) ;
#5451 = LINE('',#97376,#8665) ;
#5452 = LINE('',#97396,#8666) ;
#5453 = LINE('',#97398,#8667) ;
#5454 = LINE('',#97399,#8668) ;
#5455 = LINE('',#97401,#8669) ;
#5456 = LINE('',#97403,#8670) ;
#5457 = LINE('',#97409,#8671) ;
#5458 = LINE('',#97413,#8672) ;
#5459 = LINE('',#97429,#8673) ;
#5460 = LINE('',#97431,#8674) ;
#5461 = LINE('',#97437,#8675) ;
#5462 = LINE('',#97439,#8676) ;
#5463 = LINE('',#97441,#8677) ;
#5464 = LINE('',#97443,#8678) ;
#5465 = LINE('',#97447,#8679) ;
#5466 = LINE('',#97454,#8680) ;
#5467 = LINE('',#97455,#8681) ;
#5468 = LINE('',#97458,#8682) ;
#5469 = LINE('',#97462,#8683) ;
#5470 = LINE('',#97466,#8684) ;
#5471 = LINE('',#97467,#8685) ;
#5472 = LINE('',#97469,#8686) ;
#5473 = LINE('',#97472,#8687) ;
#5474 = LINE('',#97476,#8688) ;
#5475 = LINE('',#97477,#8689) ;
#5476 = LINE('',#97480,#8690) ;
#5477 = LINE('',#97484,#8691) ;
#5478 = LINE('',#97485,#8692) ;
#5479 = LINE('',#97488,#8693) ;
#5480 = LINE('',#97489,#8694) ;
#5481 = LINE('',#97492,#8695) ;
#5482 = LINE('',#97493,#8696) ;
#5483 = LINE('',#97496,#8697) ;
#5484 = LINE('',#97500,#8698) ;
#5485 = LINE('',#97504,#8699) ;
#5486 = LINE('',#97505,#8700) ;
#5487 = LINE('',#97507,#8701) ;
#5488 = LINE('',#97511,#8702) ;
#5489 = LINE('',#97513,#8703) ;
#5490 = LINE('',#97514,#8704) ;
#5491 = LINE('',#97517,#8705) ;
#5492 = LINE('',#97518,#8706) ;
#5493 = LINE('',#97521,#8707) ;
#5494 = LINE('',#97522,#8708) ;
#5495 = LINE('',#97524,#8709) ;
#5496 = LINE('',#97527,#8710) ;
#5497 = LINE('',#97529,#8711) ;
#5498 = LINE('',#97531,#8712) ;
#5499 = LINE('',#97532,#8713) ;
#5500 = LINE('',#97535,#8714) ;
#5501 = LINE('',#97538,#8715) ;
#5502 = LINE('',#97540,#8716) ;
#5503 = LINE('',#97542,#8717) ;
#5504 = LINE('',#97546,#8718) ;
#5505 = LINE('',#97551,#8719) ;
#5506 = LINE('',#97553,#8720) ;
#5507 = LINE('',#97554,#8721) ;
#5508 = LINE('',#97555,#8722) ;
#5509 = LINE('',#97559,#8723) ;
#5510 = LINE('',#97562,#8724) ;
#5511 = LINE('',#97564,#8725) ;
#5512 = LINE('',#97567,#8726) ;
#5513 = LINE('',#97590,#8727) ;
#5514 = LINE('',#97697,#8728) ;
#5515 = LINE('',#97735,#8729) ;
#5516 = LINE('',#97765,#8730) ;
#5517 = LINE('',#97818,#8731) ;
#5518 = LINE('',#97902,#8732) ;
#5519 = LINE('',#97934,#8733) ;
#5520 = LINE('',#97989,#8734) ;
#5521 = LINE('',#98004,#8735) ;
#5522 = LINE('',#98009,#8736) ;
#5523 = LINE('',#98018,#8737) ;
#5524 = LINE('',#98021,#8738) ;
#5525 = LINE('',#98083,#8739) ;
#5526 = LINE('',#98084,#8740) ;
#5527 = LINE('',#98087,#8741) ;
#5528 = LINE('',#98090,#8742) ;
#5529 = LINE('',#98117,#8743) ;
#5530 = LINE('',#98118,#8744) ;
#5531 = LINE('',#98120,#8745) ;
#5532 = LINE('',#98121,#8746) ;
#5533 = LINE('',#98123,#8747) ;
#5534 = LINE('',#98125,#8748) ;
#5535 = LINE('',#98127,#8749) ;
#5536 = LINE('',#98133,#8750) ;
#5537 = LINE('',#98134,#8751) ;
#5538 = LINE('',#98136,#8752) ;
#5539 = LINE('',#98137,#8753) ;
#5540 = LINE('',#98140,#8754) ;
#5541 = LINE('',#98142,#8755) ;
#5542 = LINE('',#98143,#8756) ;
#5543 = LINE('',#98147,#8757) ;
#5544 = LINE('',#98150,#8758) ;
#5545 = LINE('',#98151,#8759) ;
#5546 = LINE('',#98154,#8760) ;
#5547 = LINE('',#98155,#8761) ;
#5548 = LINE('',#98159,#8762) ;
#5549 = LINE('',#98162,#8763) ;
#5550 = LINE('',#98163,#8764) ;
#5551 = LINE('',#98167,#8765) ;
#5552 = LINE('',#98170,#8766) ;
#5553 = LINE('',#98171,#8767) ;
#5554 = LINE('',#98174,#8768) ;
#5555 = LINE('',#98175,#8769) ;
#5556 = LINE('',#98189,#8770) ;
#5557 = LINE('',#98198,#8771) ;
#5558 = LINE('',#98199,#8772) ;
#5559 = LINE('',#98219,#8773) ;
#5560 = LINE('',#98221,#8774) ;
#5561 = LINE('',#98227,#8775) ;
#5562 = LINE('',#98231,#8776) ;
#5563 = LINE('',#98233,#8777) ;
#5564 = LINE('',#98234,#8778) ;
#5565 = LINE('',#98238,#8779) ;
#5566 = LINE('',#98241,#8780) ;
#5567 = LINE('',#98242,#8781) ;
#5568 = LINE('',#98246,#8782) ;
#5569 = LINE('',#98249,#8783) ;
#5570 = LINE('',#98250,#8784) ;
#5571 = LINE('',#98255,#8785) ;
#5572 = LINE('',#98256,#8786) ;
#5573 = LINE('',#98259,#8787) ;
#5574 = LINE('',#98260,#8788) ;
#5575 = LINE('',#98264,#8789) ;
#5576 = LINE('',#98267,#8790) ;
#5577 = LINE('',#98268,#8791) ;
#5578 = LINE('',#98271,#8792) ;
#5579 = LINE('',#98272,#8793) ;
#5580 = LINE('',#98276,#8794) ;
#5581 = LINE('',#98279,#8795) ;
#5582 = LINE('',#98280,#8796) ;
#5583 = LINE('',#98283,#8797) ;
#5584 = LINE('',#98288,#8798) ;
#5585 = LINE('',#98289,#8799) ;
#5586 = LINE('',#98290,#8800) ;
#5587 = LINE('',#98294,#8801) ;
#5588 = LINE('',#98297,#8802) ;
#5589 = LINE('',#98298,#8803) ;
#5590 = LINE('',#98302,#8804) ;
#5591 = LINE('',#98305,#8805) ;
#5592 = LINE('',#98306,#8806) ;
#5593 = LINE('',#98326,#8807) ;
#5594 = LINE('',#98331,#8808) ;
#5595 = LINE('',#98332,#8809) ;
#5596 = LINE('',#98335,#8810) ;
#5597 = LINE('',#98336,#8811) ;
#5598 = LINE('',#98340,#8812) ;
#5599 = LINE('',#98343,#8813) ;
#5600 = LINE('',#98344,#8814) ;
#5601 = LINE('',#98346,#8815) ;
#5602 = LINE('',#98349,#8816) ;
#5603 = LINE('',#98350,#8817) ;
#5604 = LINE('',#98355,#8818) ;
#5605 = LINE('',#98356,#8819) ;
#5606 = LINE('',#98359,#8820) ;
#5607 = LINE('',#98360,#8821) ;
#5608 = LINE('',#98361,#8822) ;
#5609 = LINE('',#98365,#8823) ;
#5610 = LINE('',#98368,#8824) ;
#5611 = LINE('',#98369,#8825) ;
#5612 = LINE('',#98376,#8826) ;
#5613 = LINE('',#98377,#8827) ;
#5614 = LINE('',#98380,#8828) ;
#5615 = LINE('',#98381,#8829) ;
#5616 = LINE('',#98385,#8830) ;
#5617 = LINE('',#98388,#8831) ;
#5618 = LINE('',#98389,#8832) ;
#5619 = LINE('',#98392,#8833) ;
#5620 = LINE('',#98393,#8834) ;
#5621 = LINE('',#98397,#8835) ;
#5622 = LINE('',#98400,#8836) ;
#5623 = LINE('',#98401,#8837) ;
#5624 = LINE('',#98405,#8838) ;
#5625 = LINE('',#98408,#8839) ;
#5626 = LINE('',#98409,#8840) ;
#5627 = LINE('',#98412,#8841) ;
#5628 = LINE('',#98413,#8842) ;
#5629 = LINE('',#98417,#8843) ;
#5630 = LINE('',#98420,#8844) ;
#5631 = LINE('',#98421,#8845) ;
#5632 = LINE('',#98425,#8846) ;
#5633 = LINE('',#98427,#8847) ;
#5634 = LINE('',#98431,#8848) ;
#5635 = LINE('',#98432,#8849) ;
#5636 = LINE('',#98452,#8850) ;
#5637 = LINE('',#98455,#8851) ;
#5638 = LINE('',#98456,#8852) ;
#5639 = LINE('',#98460,#8853) ;
#5640 = LINE('',#98463,#8854) ;
#5641 = LINE('',#98464,#8855) ;
#5642 = LINE('',#98487,#8856) ;
#5643 = LINE('',#98490,#8857) ;
#5644 = LINE('',#98491,#8858) ;
#5645 = LINE('',#98494,#8859) ;
#5646 = LINE('',#98495,#8860) ;
#5647 = LINE('',#98499,#8861) ;
#5648 = LINE('',#98502,#8862) ;
#5649 = LINE('',#98503,#8863) ;
#5650 = LINE('',#98507,#8864) ;
#5651 = LINE('',#98509,#8865) ;
#5652 = LINE('',#98514,#8866) ;
#5653 = LINE('',#98517,#8867) ;
#5654 = LINE('',#98518,#8868) ;
#5655 = LINE('',#98521,#8869) ;
#5656 = LINE('',#98522,#8870) ;
#5657 = LINE('',#98525,#8871) ;
#5658 = LINE('',#98526,#8872) ;
#5659 = LINE('',#98529,#8873) ;
#5660 = LINE('',#98530,#8874) ;
#5661 = LINE('',#98533,#8875) ;
#5662 = LINE('',#98534,#8876) ;
#5663 = LINE('',#98538,#8877) ;
#5664 = LINE('',#98542,#8878) ;
#5665 = LINE('',#98546,#8879) ;
#5666 = LINE('',#98549,#8880) ;
#5667 = LINE('',#98550,#8881) ;
#5668 = LINE('',#98553,#8882) ;
#5669 = LINE('',#98554,#8883) ;
#5670 = LINE('',#98558,#8884) ;
#5671 = LINE('',#98561,#8885) ;
#5672 = LINE('',#98562,#8886) ;
#5673 = LINE('',#98566,#8887) ;
#5674 = LINE('',#98568,#8888) ;
#5675 = LINE('',#98573,#8889) ;
#5676 = LINE('',#98576,#8890) ;
#5677 = LINE('',#98577,#8891) ;
#5678 = LINE('',#98581,#8892) ;
#5679 = LINE('',#98584,#8893) ;
#5680 = LINE('',#98585,#8894) ;
#5681 = LINE('',#98589,#8895) ;
#5682 = LINE('',#98591,#8896) ;
#5683 = LINE('',#98597,#8897) ;
#5684 = LINE('',#98600,#8898) ;
#5685 = LINE('',#98601,#8899) ;
#5686 = LINE('',#98604,#8900) ;
#5687 = LINE('',#98605,#8901) ;
#5688 = LINE('',#98607,#8902) ;
#5689 = LINE('',#98608,#8903) ;
#5690 = LINE('',#98610,#8904) ;
#5691 = LINE('',#98612,#8905) ;
#5692 = LINE('',#98613,#8906) ;
#5693 = LINE('',#98616,#8907) ;
#5694 = LINE('',#98618,#8908) ;
#5695 = LINE('',#98620,#8909) ;
#5696 = LINE('',#98622,#8910) ;
#5697 = LINE('',#98624,#8911) ;
#5698 = LINE('',#98631,#8912) ;
#5699 = LINE('',#98634,#8913) ;
#5700 = LINE('',#98636,#8914) ;
#5701 = LINE('',#98639,#8915) ;
#5702 = LINE('',#98642,#8916) ;
#5703 = LINE('',#98645,#8917) ;
#5704 = LINE('',#98649,#8918) ;
#5705 = LINE('',#98652,#8919) ;
#5706 = LINE('',#98654,#8920) ;
#5707 = LINE('',#98656,#8921) ;
#5708 = LINE('',#98658,#8922) ;
#5709 = LINE('',#98660,#8923) ;
#5710 = LINE('',#98663,#8924) ;
#5711 = LINE('',#98666,#8925) ;
#5712 = LINE('',#98667,#8926) ;
#5713 = LINE('',#98676,#8927) ;
#5714 = LINE('',#98678,#8928) ;
#5715 = LINE('',#98680,#8929) ;
#5716 = LINE('',#98681,#8930) ;
#5717 = LINE('',#98684,#8931) ;
#5718 = LINE('',#98686,#8932) ;
#5719 = LINE('',#98687,#8933) ;
#5720 = LINE('',#98690,#8934) ;
#5721 = LINE('',#98692,#8935) ;
#5722 = LINE('',#98693,#8936) ;
#5723 = LINE('',#98696,#8937) ;
#5724 = LINE('',#98698,#8938) ;
#5725 = LINE('',#98699,#8939) ;
#5726 = LINE('',#98702,#8940) ;
#5727 = LINE('',#98704,#8941) ;
#5728 = LINE('',#98705,#8942) ;
#5729 = LINE('',#98708,#8943) ;
#5730 = LINE('',#98710,#8944) ;
#5731 = LINE('',#98711,#8945) ;
#5732 = LINE('',#98714,#8946) ;
#5733 = LINE('',#98716,#8947) ;
#5734 = LINE('',#98717,#8948) ;
#5735 = LINE('',#98719,#8949) ;
#5736 = LINE('',#98721,#8950) ;
#5737 = LINE('',#98725,#8951) ;
#5738 = LINE('',#98727,#8952) ;
#5739 = LINE('',#98729,#8953) ;
#5740 = LINE('',#98730,#8954) ;
#5741 = LINE('',#98733,#8955) ;
#5742 = LINE('',#98734,#8956) ;
#5743 = LINE('',#98736,#8957) ;
#5744 = LINE('',#98737,#8958) ;
#5745 = LINE('',#98740,#8959) ;
#5746 = LINE('',#98742,#8960) ;
#5747 = LINE('',#98743,#8961) ;
#5748 = LINE('',#98745,#8962) ;
#5749 = LINE('',#98746,#8963) ;
#5750 = LINE('',#98753,#8964) ;
#5751 = LINE('',#98890,#8965) ;
#5752 = LINE('',#99178,#8966) ;
#5753 = LINE('',#99301,#8967) ;
#5754 = LINE('',#102051,#8968) ;
#5755 = LINE('',#102069,#8969) ;
#5756 = LINE('',#102093,#8970) ;
#5757 = LINE('',#102109,#8971) ;
#5758 = LINE('',#102131,#8972) ;
#5759 = LINE('',#102149,#8973) ;
#5760 = LINE('',#102173,#8974) ;
#5761 = LINE('',#102189,#8975) ;
#5762 = LINE('',#102211,#8976) ;
#5763 = LINE('',#102229,#8977) ;
#5764 = LINE('',#102253,#8978) ;
#5765 = LINE('',#102269,#8979) ;
#5766 = LINE('',#102291,#8980) ;
#5767 = LINE('',#102309,#8981) ;
#5768 = LINE('',#102333,#8982) ;
#5769 = LINE('',#102349,#8983) ;
#5770 = LINE('',#102371,#8984) ;
#5771 = LINE('',#102389,#8985) ;
#5772 = LINE('',#102413,#8986) ;
#5773 = LINE('',#102429,#8987) ;
#5774 = LINE('',#102451,#8988) ;
#5775 = LINE('',#102469,#8989) ;
#5776 = LINE('',#102493,#8990) ;
#5777 = LINE('',#102509,#8991) ;
#5778 = LINE('',#102531,#8992) ;
#5779 = LINE('',#102549,#8993) ;
#5780 = LINE('',#102573,#8994) ;
#5781 = LINE('',#102589,#8995) ;
#5782 = LINE('',#102611,#8996) ;
#5783 = LINE('',#102629,#8997) ;
#5784 = LINE('',#102653,#8998) ;
#5785 = LINE('',#102669,#8999) ;
#5786 = LINE('',#102691,#9000) ;
#5787 = LINE('',#102709,#9001) ;
#5788 = LINE('',#102733,#9002) ;
#5789 = LINE('',#102749,#9003) ;
#5790 = LINE('',#102771,#9004) ;
#5791 = LINE('',#102789,#9005) ;
#5792 = LINE('',#102813,#9006) ;
#5793 = LINE('',#102829,#9007) ;
#5794 = LINE('',#102851,#9008) ;
#5795 = LINE('',#102853,#9009) ;
#5796 = LINE('',#102893,#9010) ;
#5797 = LINE('',#102895,#9011) ;
#5798 = LINE('',#102931,#9012) ;
#5799 = LINE('',#102933,#9013) ;
#5800 = LINE('',#102973,#9014) ;
#5801 = LINE('',#102975,#9015) ;
#5802 = LINE('',#103011,#9016) ;
#5803 = LINE('',#103013,#9017) ;
#5804 = LINE('',#103053,#9018) ;
#5805 = LINE('',#103055,#9019) ;
#5806 = LINE('',#103091,#9020) ;
#5807 = LINE('',#103093,#9021) ;
#5808 = LINE('',#103133,#9022) ;
#5809 = LINE('',#103135,#9023) ;
#5810 = LINE('',#103171,#9024) ;
#5811 = LINE('',#103173,#9025) ;
#5812 = LINE('',#103213,#9026) ;
#5813 = LINE('',#103215,#9027) ;
#5814 = LINE('',#103251,#9028) ;
#5815 = LINE('',#103253,#9029) ;
#5816 = LINE('',#103293,#9030) ;
#5817 = LINE('',#103295,#9031) ;
#5818 = LINE('',#103331,#9032) ;
#5819 = LINE('',#103333,#9033) ;
#5820 = LINE('',#103373,#9034) ;
#5821 = LINE('',#103375,#9035) ;
#5822 = LINE('',#103411,#9036) ;
#5823 = LINE('',#103413,#9037) ;
#5824 = LINE('',#103453,#9038) ;
#5825 = LINE('',#103455,#9039) ;
#5826 = LINE('',#103491,#9040) ;
#5827 = LINE('',#103493,#9041) ;
#5828 = LINE('',#103533,#9042) ;
#5829 = LINE('',#103535,#9043) ;
#5830 = LINE('',#103571,#9044) ;
#5831 = LINE('',#103573,#9045) ;
#5832 = LINE('',#103612,#9046) ;
#5833 = LINE('',#103613,#9047) ;
#5834 = LINE('',#103616,#9048) ;
#5835 = LINE('',#103618,#9049) ;
#5836 = LINE('',#103619,#9050) ;
#5837 = LINE('',#103622,#9051) ;
#5838 = LINE('',#103626,#9052) ;
#5839 = LINE('',#103627,#9053) ;
#5840 = LINE('',#103630,#9054) ;
#5841 = LINE('',#103634,#9055) ;
#5842 = LINE('',#103635,#9056) ;
#5843 = LINE('',#103638,#9057) ;
#5844 = LINE('',#103642,#9058) ;
#5845 = LINE('',#103643,#9059) ;
#5846 = LINE('',#103646,#9060) ;
#5847 = LINE('',#103650,#9061) ;
#5848 = LINE('',#103651,#9062) ;
#5849 = LINE('',#103654,#9063) ;
#5850 = LINE('',#103658,#9064) ;
#5851 = LINE('',#103659,#9065) ;
#5852 = LINE('',#103662,#9066) ;
#5853 = LINE('',#103666,#9067) ;
#5854 = LINE('',#103667,#9068) ;
#5855 = LINE('',#103670,#9069) ;
#5856 = LINE('',#103674,#9070) ;
#5857 = LINE('',#103675,#9071) ;
#5858 = LINE('',#103678,#9072) ;
#5859 = LINE('',#103682,#9073) ;
#5860 = LINE('',#103683,#9074) ;
#5861 = LINE('',#103686,#9075) ;
#5862 = LINE('',#103690,#9076) ;
#5863 = LINE('',#103691,#9077) ;
#5864 = LINE('',#103694,#9078) ;
#5865 = LINE('',#103698,#9079) ;
#5866 = LINE('',#103699,#9080) ;
#5867 = LINE('',#103702,#9081) ;
#5868 = LINE('',#103706,#9082) ;
#5869 = LINE('',#103707,#9083) ;
#5870 = LINE('',#103710,#9084) ;
#5871 = LINE('',#103714,#9085) ;
#5872 = LINE('',#103715,#9086) ;
#5873 = LINE('',#103718,#9087) ;
#5874 = LINE('',#103722,#9088) ;
#5875 = LINE('',#103723,#9089) ;
#5876 = LINE('',#103726,#9090) ;
#5877 = LINE('',#103730,#9091) ;
#5878 = LINE('',#103731,#9092) ;
#5879 = LINE('',#103734,#9093) ;
#5880 = LINE('',#103738,#9094) ;
#5881 = LINE('',#103739,#9095) ;
#5882 = LINE('',#103742,#9096) ;
#5883 = LINE('',#103746,#9097) ;
#5884 = LINE('',#103747,#9098) ;
#5885 = LINE('',#103750,#9099) ;
#5886 = LINE('',#103754,#9100) ;
#5887 = LINE('',#103755,#9101) ;
#5888 = LINE('',#103758,#9102) ;
#5889 = LINE('',#103762,#9103) ;
#5890 = LINE('',#103763,#9104) ;
#5891 = LINE('',#103766,#9105) ;
#5892 = LINE('',#103770,#9106) ;
#5893 = LINE('',#103771,#9107) ;
#5894 = LINE('',#103774,#9108) ;
#5895 = LINE('',#103906,#9109) ;
#5896 = LINE('',#103909,#9110) ;
#5897 = LINE('',#103912,#9111) ;
#5898 = LINE('',#103915,#9112) ;
#5899 = LINE('',#103918,#9113) ;
#5900 = LINE('',#103921,#9114) ;
#5901 = LINE('',#103924,#9115) ;
#5902 = LINE('',#103927,#9116) ;
#5903 = LINE('',#103930,#9117) ;
#5904 = LINE('',#103933,#9118) ;
#5905 = LINE('',#103936,#9119) ;
#5906 = LINE('',#103939,#9120) ;
#5907 = LINE('',#103942,#9121) ;
#5908 = LINE('',#103945,#9122) ;
#5909 = LINE('',#103948,#9123) ;
#5910 = LINE('',#103951,#9124) ;
#5911 = LINE('',#103954,#9125) ;
#5912 = LINE('',#103957,#9126) ;
#5913 = LINE('',#103960,#9127) ;
#5914 = LINE('',#103963,#9128) ;
#5915 = LINE('',#103966,#9129) ;
#5916 = LINE('',#103969,#9130) ;
#5917 = LINE('',#103972,#9131) ;
#5918 = LINE('',#103975,#9132) ;
#5919 = LINE('',#103978,#9133) ;
#5920 = LINE('',#103981,#9134) ;
#5921 = LINE('',#103984,#9135) ;
#5922 = LINE('',#103987,#9136) ;
#5923 = LINE('',#103990,#9137) ;
#5924 = LINE('',#103993,#9138) ;
#5925 = LINE('',#103996,#9139) ;
#5926 = LINE('',#103999,#9140) ;
#5927 = LINE('',#104002,#9141) ;
#5928 = LINE('',#104005,#9142) ;
#5929 = LINE('',#104008,#9143) ;
#5930 = LINE('',#104011,#9144) ;
#5931 = LINE('',#104014,#9145) ;
#5932 = LINE('',#104017,#9146) ;
#5933 = LINE('',#104020,#9147) ;
#5934 = LINE('',#104023,#9148) ;
#5935 = LINE('',#104074,#9149) ;
#5936 = LINE('',#104077,#9150) ;
#5937 = LINE('',#104110,#9151) ;
#5938 = LINE('',#104162,#9152) ;
#5939 = LINE('',#104259,#9153) ;
#5940 = LINE('',#104356,#9154) ;
#5941 = LINE('',#104453,#9155) ;
#5942 = LINE('',#104550,#9156) ;
#5943 = LINE('',#104647,#9157) ;
#5944 = LINE('',#104744,#9158) ;
#5945 = LINE('',#104841,#9159) ;
#5946 = LINE('',#105050,#9160) ;
#5947 = LINE('',#105089,#9161) ;
#5948 = LINE('',#105128,#9162) ;
#5949 = LINE('',#105167,#9163) ;
#5950 = LINE('',#105206,#9164) ;
#5951 = LINE('',#105245,#9165) ;
#5952 = LINE('',#105284,#9166) ;
#5953 = LINE('',#105323,#9167) ;
#5954 = LINE('',#105362,#9168) ;
#5955 = LINE('',#105384,#9169) ;
#5956 = LINE('',#105385,#9170) ;
#5957 = LINE('',#105387,#9171) ;
#5958 = LINE('',#105389,#9172) ;
#5959 = LINE('',#105392,#9173) ;
#5960 = LINE('',#105393,#9174) ;
#5961 = LINE('',#105395,#9175) ;
#5962 = LINE('',#105396,#9176) ;
#5963 = LINE('',#105399,#9177) ;
#5964 = LINE('',#105400,#9178) ;
#5965 = LINE('',#105402,#9179) ;
#5966 = LINE('',#105403,#9180) ;
#5967 = LINE('',#105406,#9181) ;
#5968 = LINE('',#105407,#9182) ;
#5969 = LINE('',#105409,#9183) ;
#5970 = LINE('',#105410,#9184) ;
#5971 = LINE('',#105413,#9185) ;
#5972 = LINE('',#105414,#9186) ;
#5973 = LINE('',#105416,#9187) ;
#5974 = LINE('',#105417,#9188) ;
#5975 = LINE('',#105420,#9189) ;
#5976 = LINE('',#105421,#9190) ;
#5977 = LINE('',#105423,#9191) ;
#5978 = LINE('',#105424,#9192) ;
#5979 = LINE('',#105427,#9193) ;
#5980 = LINE('',#105428,#9194) ;
#5981 = LINE('',#105430,#9195) ;
#5982 = LINE('',#105431,#9196) ;
#5983 = LINE('',#105434,#9197) ;
#5984 = LINE('',#105435,#9198) ;
#5985 = LINE('',#105437,#9199) ;
#5986 = LINE('',#105438,#9200) ;
#5987 = LINE('',#105441,#9201) ;
#5988 = LINE('',#105442,#9202) ;
#5989 = LINE('',#105444,#9203) ;
#5990 = LINE('',#105445,#9204) ;
#5991 = LINE('',#105448,#9205) ;
#5992 = LINE('',#105449,#9206) ;
#5993 = LINE('',#105451,#9207) ;
#5994 = LINE('',#105463,#9208) ;
#5995 = LINE('',#105784,#9209) ;
#5996 = LINE('',#105802,#9210) ;
#5997 = LINE('',#105826,#9211) ;
#5998 = LINE('',#105842,#9212) ;
#5999 = LINE('',#105864,#9213) ;
#6000 = LINE('',#105882,#9214) ;
#6001 = LINE('',#105906,#9215) ;
#6002 = LINE('',#105922,#9216) ;
#6003 = LINE('',#105944,#9217) ;
#6004 = LINE('',#105962,#9218) ;
#6005 = LINE('',#105986,#9219) ;
#6006 = LINE('',#106002,#9220) ;
#6007 = LINE('',#106024,#9221) ;
#6008 = LINE('',#106042,#9222) ;
#6009 = LINE('',#106066,#9223) ;
#6010 = LINE('',#106082,#9224) ;
#6011 = LINE('',#106104,#9225) ;
#6012 = LINE('',#106122,#9226) ;
#6013 = LINE('',#106146,#9227) ;
#6014 = LINE('',#106162,#9228) ;
#6015 = LINE('',#106184,#9229) ;
#6016 = LINE('',#106202,#9230) ;
#6017 = LINE('',#106226,#9231) ;
#6018 = LINE('',#106242,#9232) ;
#6019 = LINE('',#106264,#9233) ;
#6020 = LINE('',#106282,#9234) ;
#6021 = LINE('',#106306,#9235) ;
#6022 = LINE('',#106322,#9236) ;
#6023 = LINE('',#106344,#9237) ;
#6024 = LINE('',#106362,#9238) ;
#6025 = LINE('',#106386,#9239) ;
#6026 = LINE('',#106402,#9240) ;
#6027 = LINE('',#106424,#9241) ;
#6028 = LINE('',#106442,#9242) ;
#6029 = LINE('',#106466,#9243) ;
#6030 = LINE('',#106482,#9244) ;
#6031 = LINE('',#106504,#9245) ;
#6032 = LINE('',#106522,#9246) ;
#6033 = LINE('',#106546,#9247) ;
#6034 = LINE('',#106562,#9248) ;
#6035 = LINE('',#106584,#9249) ;
#6036 = LINE('',#106586,#9250) ;
#6037 = LINE('',#106626,#9251) ;
#6038 = LINE('',#106628,#9252) ;
#6039 = LINE('',#106664,#9253) ;
#6040 = LINE('',#106666,#9254) ;
#6041 = LINE('',#106706,#9255) ;
#6042 = LINE('',#106708,#9256) ;
#6043 = LINE('',#106744,#9257) ;
#6044 = LINE('',#106746,#9258) ;
#6045 = LINE('',#106786,#9259) ;
#6046 = LINE('',#106788,#9260) ;
#6047 = LINE('',#106824,#9261) ;
#6048 = LINE('',#106826,#9262) ;
#6049 = LINE('',#106866,#9263) ;
#6050 = LINE('',#106868,#9264) ;
#6051 = LINE('',#106904,#9265) ;
#6052 = LINE('',#106906,#9266) ;
#6053 = LINE('',#106946,#9267) ;
#6054 = LINE('',#106948,#9268) ;
#6055 = LINE('',#106984,#9269) ;
#6056 = LINE('',#106986,#9270) ;
#6057 = LINE('',#107026,#9271) ;
#6058 = LINE('',#107028,#9272) ;
#6059 = LINE('',#107064,#9273) ;
#6060 = LINE('',#107066,#9274) ;
#6061 = LINE('',#107106,#9275) ;
#6062 = LINE('',#107108,#9276) ;
#6063 = LINE('',#107144,#9277) ;
#6064 = LINE('',#107146,#9278) ;
#6065 = LINE('',#107186,#9279) ;
#6066 = LINE('',#107188,#9280) ;
#6067 = LINE('',#107224,#9281) ;
#6068 = LINE('',#107226,#9282) ;
#6069 = LINE('',#107266,#9283) ;
#6070 = LINE('',#107268,#9284) ;
#6071 = LINE('',#107304,#9285) ;
#6072 = LINE('',#107306,#9286) ;
#6073 = LINE('',#107345,#9287) ;
#6074 = LINE('',#107346,#9288) ;
#6075 = LINE('',#107349,#9289) ;
#6076 = LINE('',#107351,#9290) ;
#6077 = LINE('',#107352,#9291) ;
#6078 = LINE('',#107355,#9292) ;
#6079 = LINE('',#107359,#9293) ;
#6080 = LINE('',#107360,#9294) ;
#6081 = LINE('',#107363,#9295) ;
#6082 = LINE('',#107367,#9296) ;
#6083 = LINE('',#107368,#9297) ;
#6084 = LINE('',#107371,#9298) ;
#6085 = LINE('',#107375,#9299) ;
#6086 = LINE('',#107376,#9300) ;
#6087 = LINE('',#107379,#9301) ;
#6088 = LINE('',#107383,#9302) ;
#6089 = LINE('',#107384,#9303) ;
#6090 = LINE('',#107387,#9304) ;
#6091 = LINE('',#107391,#9305) ;
#6092 = LINE('',#107392,#9306) ;
#6093 = LINE('',#107395,#9307) ;
#6094 = LINE('',#107399,#9308) ;
#6095 = LINE('',#107400,#9309) ;
#6096 = LINE('',#107403,#9310) ;
#6097 = LINE('',#107407,#9311) ;
#6098 = LINE('',#107408,#9312) ;
#6099 = LINE('',#107411,#9313) ;
#6100 = LINE('',#107415,#9314) ;
#6101 = LINE('',#107416,#9315) ;
#6102 = LINE('',#107419,#9316) ;
#6103 = LINE('',#107423,#9317) ;
#6104 = LINE('',#107424,#9318) ;
#6105 = LINE('',#107427,#9319) ;
#6106 = LINE('',#107431,#9320) ;
#6107 = LINE('',#107432,#9321) ;
#6108 = LINE('',#107435,#9322) ;
#6109 = LINE('',#107439,#9323) ;
#6110 = LINE('',#107440,#9324) ;
#6111 = LINE('',#107443,#9325) ;
#6112 = LINE('',#107447,#9326) ;
#6113 = LINE('',#107448,#9327) ;
#6114 = LINE('',#107451,#9328) ;
#6115 = LINE('',#107455,#9329) ;
#6116 = LINE('',#107456,#9330) ;
#6117 = LINE('',#107459,#9331) ;
#6118 = LINE('',#107463,#9332) ;
#6119 = LINE('',#107464,#9333) ;
#6120 = LINE('',#107467,#9334) ;
#6121 = LINE('',#107471,#9335) ;
#6122 = LINE('',#107472,#9336) ;
#6123 = LINE('',#107475,#9337) ;
#6124 = LINE('',#107479,#9338) ;
#6125 = LINE('',#107480,#9339) ;
#6126 = LINE('',#107483,#9340) ;
#6127 = LINE('',#107487,#9341) ;
#6128 = LINE('',#107488,#9342) ;
#6129 = LINE('',#107491,#9343) ;
#6130 = LINE('',#107495,#9344) ;
#6131 = LINE('',#107496,#9345) ;
#6132 = LINE('',#107499,#9346) ;
#6133 = LINE('',#107503,#9347) ;
#6134 = LINE('',#107504,#9348) ;
#6135 = LINE('',#107507,#9349) ;
#6136 = LINE('',#107639,#9350) ;
#6137 = LINE('',#107642,#9351) ;
#6138 = LINE('',#107645,#9352) ;
#6139 = LINE('',#107648,#9353) ;
#6140 = LINE('',#107651,#9354) ;
#6141 = LINE('',#107654,#9355) ;
#6142 = LINE('',#107657,#9356) ;
#6143 = LINE('',#107660,#9357) ;
#6144 = LINE('',#107663,#9358) ;
#6145 = LINE('',#107666,#9359) ;
#6146 = LINE('',#107669,#9360) ;
#6147 = LINE('',#107672,#9361) ;
#6148 = LINE('',#107675,#9362) ;
#6149 = LINE('',#107678,#9363) ;
#6150 = LINE('',#107681,#9364) ;
#6151 = LINE('',#107684,#9365) ;
#6152 = LINE('',#107687,#9366) ;
#6153 = LINE('',#107690,#9367) ;
#6154 = LINE('',#107693,#9368) ;
#6155 = LINE('',#107696,#9369) ;
#6156 = LINE('',#107699,#9370) ;
#6157 = LINE('',#107702,#9371) ;
#6158 = LINE('',#107705,#9372) ;
#6159 = LINE('',#107708,#9373) ;
#6160 = LINE('',#107711,#9374) ;
#6161 = LINE('',#107714,#9375) ;
#6162 = LINE('',#107717,#9376) ;
#6163 = LINE('',#107720,#9377) ;
#6164 = LINE('',#107723,#9378) ;
#6165 = LINE('',#107726,#9379) ;
#6166 = LINE('',#107729,#9380) ;
#6167 = LINE('',#107732,#9381) ;
#6168 = LINE('',#107735,#9382) ;
#6169 = LINE('',#107738,#9383) ;
#6170 = LINE('',#107741,#9384) ;
#6171 = LINE('',#107744,#9385) ;
#6172 = LINE('',#107747,#9386) ;
#6173 = LINE('',#107750,#9387) ;
#6174 = LINE('',#107753,#9388) ;
#6175 = LINE('',#107756,#9389) ;
#6176 = LINE('',#107807,#9390) ;
#6177 = LINE('',#107810,#9391) ;
#6178 = LINE('',#107843,#9392) ;
#6179 = LINE('',#107895,#9393) ;
#6180 = LINE('',#107992,#9394) ;
#6181 = LINE('',#108089,#9395) ;
#6182 = LINE('',#108186,#9396) ;
#6183 = LINE('',#108283,#9397) ;
#6184 = LINE('',#108380,#9398) ;
#6185 = LINE('',#108477,#9399) ;
#6186 = LINE('',#108574,#9400) ;
#6187 = LINE('',#108783,#9401) ;
#6188 = LINE('',#108822,#9402) ;
#6189 = LINE('',#108861,#9403) ;
#6190 = LINE('',#108900,#9404) ;
#6191 = LINE('',#108939,#9405) ;
#6192 = LINE('',#108978,#9406) ;
#6193 = LINE('',#109017,#9407) ;
#6194 = LINE('',#109056,#9408) ;
#6195 = LINE('',#109095,#9409) ;
#6196 = LINE('',#109117,#9410) ;
#6197 = LINE('',#109118,#9411) ;
#6198 = LINE('',#109120,#9412) ;
#6199 = LINE('',#109122,#9413) ;
#6200 = LINE('',#109125,#9414) ;
#6201 = LINE('',#109126,#9415) ;
#6202 = LINE('',#109128,#9416) ;
#6203 = LINE('',#109129,#9417) ;
#6204 = LINE('',#109132,#9418) ;
#6205 = LINE('',#109133,#9419) ;
#6206 = LINE('',#109135,#9420) ;
#6207 = LINE('',#109136,#9421) ;
#6208 = LINE('',#109139,#9422) ;
#6209 = LINE('',#109140,#9423) ;
#6210 = LINE('',#109142,#9424) ;
#6211 = LINE('',#109143,#9425) ;
#6212 = LINE('',#109146,#9426) ;
#6213 = LINE('',#109147,#9427) ;
#6214 = LINE('',#109149,#9428) ;
#6215 = LINE('',#109150,#9429) ;
#6216 = LINE('',#109153,#9430) ;
#6217 = LINE('',#109154,#9431) ;
#6218 = LINE('',#109156,#9432) ;
#6219 = LINE('',#109157,#9433) ;
#6220 = LINE('',#109160,#9434) ;
#6221 = LINE('',#109161,#9435) ;
#6222 = LINE('',#109163,#9436) ;
#6223 = LINE('',#109164,#9437) ;
#6224 = LINE('',#109167,#9438) ;
#6225 = LINE('',#109168,#9439) ;
#6226 = LINE('',#109170,#9440) ;
#6227 = LINE('',#109171,#9441) ;
#6228 = LINE('',#109174,#9442) ;
#6229 = LINE('',#109175,#9443) ;
#6230 = LINE('',#109177,#9444) ;
#6231 = LINE('',#109178,#9445) ;
#6232 = LINE('',#109181,#9446) ;
#6233 = LINE('',#109182,#9447) ;
#6234 = LINE('',#109184,#9448) ;
#6235 = LINE('',#109196,#9449) ;
#6236 = LINE('',#109201,#9450) ;
#6237 = LINE('',#109336,#9451) ;
#6238 = LINE('',#109624,#9452) ;
#6239 = LINE('',#109747,#9453) ;
#6240 = LINE('',#109983,#9454) ;
#6241 = LINE('',#110144,#9455) ;
#6242 = LINE('',#110479,#9456) ;
#6243 = LINE('',#110813,#9457) ;
#6244 = LINE('',#111144,#9458) ;
#6245 = LINE('',#111472,#9459) ;
#6246 = VECTOR('',#55111,6.) ;
#6247 = VECTOR('',#55114,10.) ;
#6248 = VECTOR('',#55117,10.) ;
#6249 = VECTOR('',#55120,10.) ;
#6250 = VECTOR('',#55123,10.) ;
#6251 = VECTOR('',#55126,10.) ;
#6252 = VECTOR('',#55129,10.) ;
#6253 = VECTOR('',#55132,10.) ;
#6254 = VECTOR('',#55135,10.) ;
#6255 = VECTOR('',#55138,10.) ;
#6256 = VECTOR('',#55141,10.) ;
#6257 = VECTOR('',#55144,10.) ;
#6258 = VECTOR('',#55147,10.) ;
#6259 = VECTOR('',#55150,10.) ;
#6260 = VECTOR('',#55153,10.) ;
#6261 = VECTOR('',#55156,10.) ;
#6262 = VECTOR('',#55159,10.) ;
#6263 = VECTOR('',#55162,10.) ;
#6264 = VECTOR('',#55165,10.) ;
#6265 = VECTOR('',#55168,10.) ;
#6266 = VECTOR('',#55171,10.) ;
#6267 = VECTOR('',#55174,10.) ;
#6268 = VECTOR('',#55177,10.) ;
#6269 = VECTOR('',#55180,10.) ;
#6270 = VECTOR('',#55183,10.) ;
#6271 = VECTOR('',#55186,10.) ;
#6272 = VECTOR('',#55189,10.) ;
#6273 = VECTOR('',#55192,10.) ;
#6274 = VECTOR('',#55195,10.) ;
#6275 = VECTOR('',#55198,10.) ;
#6276 = VECTOR('',#55201,10.) ;
#6277 = VECTOR('',#55204,10.) ;
#6278 = VECTOR('',#55207,10.) ;
#6279 = VECTOR('',#55210,10.) ;
#6280 = VECTOR('',#55213,10.) ;
#6281 = VECTOR('',#55216,10.) ;
#6282 = VECTOR('',#55219,10.) ;
#6283 = VECTOR('',#55222,10.) ;
#6284 = VECTOR('',#55225,10.) ;
#6285 = VECTOR('',#55228,10.) ;
#6286 = VECTOR('',#55231,10.) ;
#6287 = VECTOR('',#55240,10.) ;
#6288 = VECTOR('',#55243,10.) ;
#6289 = VECTOR('',#55248,10.) ;
#6290 = VECTOR('',#55251,10.) ;
#6291 = VECTOR('',#55264,10.) ;
#6292 = VECTOR('',#55265,10.) ;
#6293 = VECTOR('',#55270,10.) ;
#6294 = VECTOR('',#55273,10.) ;
#6295 = VECTOR('',#55278,10.) ;
#6296 = VECTOR('',#55281,10.) ;
#6297 = VECTOR('',#55294,10.) ;
#6298 = VECTOR('',#55295,10.) ;
#6299 = VECTOR('',#55300,10.) ;
#6300 = VECTOR('',#55303,10.) ;
#6301 = VECTOR('',#55308,10.) ;
#6302 = VECTOR('',#55311,10.) ;
#6303 = VECTOR('',#55324,10.) ;
#6304 = VECTOR('',#55325,10.) ;
#6305 = VECTOR('',#55330,10.) ;
#6306 = VECTOR('',#55333,10.) ;
#6307 = VECTOR('',#55348,10.) ;
#6308 = VECTOR('',#55349,10.) ;
#6309 = VECTOR('',#55354,10.) ;
#6310 = VECTOR('',#55355,10.) ;
#6311 = VECTOR('',#55390,10.) ;
#6312 = VECTOR('',#55391,10.) ;
#6313 = VECTOR('',#55392,10.) ;
#6314 = VECTOR('',#55395,10.) ;
#6315 = VECTOR('',#55400,10.) ;
#6316 = VECTOR('',#55401,10.) ;
#6317 = VECTOR('',#55404,10.) ;
#6318 = VECTOR('',#55409,10.) ;
#6319 = VECTOR('',#55410,10.) ;
#6320 = VECTOR('',#55413,10.) ;
#6321 = VECTOR('',#55418,10.) ;
#6322 = VECTOR('',#55419,10.) ;
#6323 = VECTOR('',#55422,10.) ;
#6324 = VECTOR('',#55427,10.) ;
#6325 = VECTOR('',#55428,10.) ;
#6326 = VECTOR('',#55431,10.) ;
#6327 = VECTOR('',#55436,10.) ;
#6328 = VECTOR('',#55437,10.) ;
#6329 = VECTOR('',#55440,10.) ;
#6330 = VECTOR('',#55811,10.) ;
#6331 = VECTOR('',#55814,10.) ;
#6332 = VECTOR('',#55817,10.) ;
#6333 = VECTOR('',#55824,10.) ;
#6334 = VECTOR('',#55831,10.) ;
#6335 = VECTOR('',#55838,10.) ;
#6336 = VECTOR('',#55845,10.) ;
#6337 = VECTOR('',#55848,10.) ;
#6338 = VECTOR('',#55855,10.) ;
#6339 = VECTOR('',#55862,10.) ;
#6340 = VECTOR('',#55869,10.) ;
#6341 = VECTOR('',#55872,10.) ;
#6342 = VECTOR('',#55879,10.) ;
#6343 = VECTOR('',#55886,10.) ;
#6344 = VECTOR('',#55893,10.) ;
#6345 = VECTOR('',#55896,10.) ;
#6346 = VECTOR('',#55903,10.) ;
#6347 = VECTOR('',#55910,10.) ;
#6348 = VECTOR('',#55917,10.) ;
#6349 = VECTOR('',#55920,10.) ;
#6350 = VECTOR('',#55927,10.) ;
#6351 = VECTOR('',#55934,10.) ;
#6352 = VECTOR('',#55941,10.) ;
#6353 = VECTOR('',#55944,10.) ;
#6354 = VECTOR('',#55951,10.) ;
#6355 = VECTOR('',#55958,10.) ;
#6356 = VECTOR('',#55965,10.) ;
#6357 = VECTOR('',#55968,10.) ;
#6358 = VECTOR('',#55975,10.) ;
#6359 = VECTOR('',#55982,10.) ;
#6360 = VECTOR('',#55989,10.) ;
#6361 = VECTOR('',#55992,10.) ;
#6362 = VECTOR('',#55999,10.) ;
#6363 = VECTOR('',#56006,10.) ;
#6364 = VECTOR('',#56013,10.) ;
#6365 = VECTOR('',#56016,10.) ;
#6366 = VECTOR('',#56023,10.) ;
#6367 = VECTOR('',#56030,10.) ;
#6368 = VECTOR('',#56037,10.) ;
#6369 = VECTOR('',#56040,10.) ;
#6370 = VECTOR('',#56127,5.625) ;
#6371 = VECTOR('',#56142,10.) ;
#6372 = VECTOR('',#56145,10.) ;
#6373 = VECTOR('',#56148,10.) ;
#6374 = VECTOR('',#56151,10.) ;
#6375 = VECTOR('',#56154,10.) ;
#6376 = VECTOR('',#56157,10.) ;
#6377 = VECTOR('',#56160,10.) ;
#6378 = VECTOR('',#56163,10.) ;
#6379 = VECTOR('',#56166,10.) ;
#6380 = VECTOR('',#56169,10.) ;
#6381 = VECTOR('',#56172,10.) ;
#6382 = VECTOR('',#56175,10.) ;
#6383 = VECTOR('',#56178,10.) ;
#6384 = VECTOR('',#56183,10.) ;
#6385 = VECTOR('',#56204,10.) ;
#6386 = VECTOR('',#56205,10.) ;
#6387 = VECTOR('',#56208,10.) ;
#6388 = VECTOR('',#56213,10.) ;
#6389 = VECTOR('',#56224,10.) ;
#6390 = VECTOR('',#56267,10.) ;
#6391 = VECTOR('',#56278,10.) ;
#6392 = VECTOR('',#56281,10.) ;
#6393 = VECTOR('',#56282,10.) ;
#6394 = VECTOR('',#56293,10.) ;
#6395 = VECTOR('',#56302,10.) ;
#6396 = VECTOR('',#56305,10.) ;
#6397 = VECTOR('',#56308,10.) ;
#6398 = VECTOR('',#56309,10.) ;
#6399 = VECTOR('',#56312,10.) ;
#6400 = VECTOR('',#56379,10.) ;
#6401 = VECTOR('',#56380,10.) ;
#6402 = VECTOR('',#56383,10.) ;
#6403 = VECTOR('',#56384,10.) ;
#6404 = VECTOR('',#56385,10.) ;
#6405 = VECTOR('',#56386,10.) ;
#6406 = VECTOR('',#56407,10.) ;
#6407 = VECTOR('',#56408,10.) ;
#6408 = VECTOR('',#56423,10.) ;
#6409 = VECTOR('',#56424,10.) ;
#6410 = VECTOR('',#56429,10.) ;
#6411 = VECTOR('',#56432,10.) ;
#6412 = VECTOR('',#56435,10.) ;
#6413 = VECTOR('',#56436,10.) ;
#6414 = VECTOR('',#56437,10.) ;
#6415 = VECTOR('',#56438,10.) ;
#6416 = VECTOR('',#56441,10.) ;
#6417 = VECTOR('',#56444,10.) ;
#6418 = VECTOR('',#56445,10.) ;
#6419 = VECTOR('',#56458,10.) ;
#6420 = VECTOR('',#56465,10.) ;
#6421 = VECTOR('',#56468,10.) ;
#6422 = VECTOR('',#56473,10.) ;
#6423 = VECTOR('',#56480,10.) ;
#6424 = VECTOR('',#56485,10.) ;
#6425 = VECTOR('',#56488,10.) ;
#6426 = VECTOR('',#56495,10.) ;
#6427 = VECTOR('',#56510,10.) ;
#6428 = VECTOR('',#56515,10.) ;
#6429 = VECTOR('',#56516,10.) ;
#6430 = VECTOR('',#56517,10.) ;
#6431 = VECTOR('',#56518,10.) ;
#6432 = VECTOR('',#56523,10.) ;
#6433 = VECTOR('',#56524,10.) ;
#6434 = VECTOR('',#56535,2.) ;
#6435 = VECTOR('',#56540,10.) ;
#6436 = VECTOR('',#56549,10.) ;
#6437 = VECTOR('',#56572,10.) ;
#6438 = VECTOR('',#56601,10.) ;
#6439 = VECTOR('',#56606,10.) ;
#6440 = VECTOR('',#56611,10.) ;
#6441 = VECTOR('',#56612,10.) ;
#6442 = VECTOR('',#56615,10.) ;
#6443 = VECTOR('',#56618,10.) ;
#6444 = VECTOR('',#56621,10.) ;
#6445 = VECTOR('',#56624,10.) ;
#6446 = VECTOR('',#56625,10.) ;
#6447 = VECTOR('',#56628,10.) ;
#6448 = VECTOR('',#56631,10.) ;
#6449 = VECTOR('',#56634,10.) ;
#6450 = VECTOR('',#56635,10.) ;
#6451 = VECTOR('',#56638,10.) ;
#6452 = VECTOR('',#56639,10.) ;
#6453 = VECTOR('',#56642,10.) ;
#6454 = VECTOR('',#56647,10.) ;
#6455 = VECTOR('',#56648,10.) ;
#6456 = VECTOR('',#56665,10.) ;
#6457 = VECTOR('',#56666,10.) ;
#6458 = VECTOR('',#56681,10.) ;
#6459 = VECTOR('',#56682,10.) ;
#6460 = VECTOR('',#56697,10.) ;
#6461 = VECTOR('',#56698,10.) ;
#6462 = VECTOR('',#56701,10.) ;
#6463 = VECTOR('',#56726,10.) ;
#6464 = VECTOR('',#56727,10.) ;
#6465 = VECTOR('',#56730,10.) ;
#6466 = VECTOR('',#56741,10.) ;
#6467 = VECTOR('',#56746,10.) ;
#6468 = VECTOR('',#56747,10.) ;
#6469 = VECTOR('',#56750,10.) ;
#6470 = VECTOR('',#56751,10.) ;
#6471 = VECTOR('',#56754,10.) ;
#6472 = VECTOR('',#56757,10.) ;
#6473 = VECTOR('',#56776,10.) ;
#6474 = VECTOR('',#56787,10.) ;
#6475 = VECTOR('',#56788,10.) ;
#6476 = VECTOR('',#56805,10.) ;
#6477 = VECTOR('',#56818,10.) ;
#6478 = VECTOR('',#56819,10.) ;
#6479 = VECTOR('',#56820,10.) ;
#6480 = VECTOR('',#56821,10.) ;
#6481 = VECTOR('',#56838,10.) ;
#6482 = VECTOR('',#56839,10.) ;
#6483 = VECTOR('',#56854,10.) ;
#6484 = VECTOR('',#56855,10.) ;
#6485 = VECTOR('',#56868,10.) ;
#6486 = VECTOR('',#56869,10.) ;
#6487 = VECTOR('',#56878,10.) ;
#6488 = VECTOR('',#56879,10.) ;
#6489 = VECTOR('',#56892,10.) ;
#6490 = VECTOR('',#56893,10.) ;
#6491 = VECTOR('',#56898,10.) ;
#6492 = VECTOR('',#56899,10.) ;
#6493 = VECTOR('',#56900,10.) ;
#6494 = VECTOR('',#56901,10.) ;
#6495 = VECTOR('',#56902,10.) ;
#6496 = VECTOR('',#56905,10.) ;
#6497 = VECTOR('',#56910,10.) ;
#6498 = VECTOR('',#56911,10.) ;
#6499 = VECTOR('',#56918,10.) ;
#6500 = VECTOR('',#56919,10.) ;
#6501 = VECTOR('',#56936,10.) ;
#6502 = VECTOR('',#56937,10.) ;
#6503 = VECTOR('',#56956,10.) ;
#6504 = VECTOR('',#56957,10.) ;
#6505 = VECTOR('',#56980,10.) ;
#6506 = VECTOR('',#56981,10.) ;
#6507 = VECTOR('',#56984,10.) ;
#6508 = VECTOR('',#56985,10.) ;
#6509 = VECTOR('',#56992,10.) ;
#6510 = VECTOR('',#56993,10.) ;
#6511 = VECTOR('',#56994,10.) ;
#6512 = VECTOR('',#56997,10.) ;
#6513 = VECTOR('',#56998,10.) ;
#6514 = VECTOR('',#57001,10.) ;
#6515 = VECTOR('',#57016,10.) ;
#6516 = VECTOR('',#57017,10.) ;
#6517 = VECTOR('',#57018,10.) ;
#6518 = VECTOR('',#57019,10.) ;
#6519 = VECTOR('',#57022,10.) ;
#6520 = VECTOR('',#57023,10.) ;
#6521 = VECTOR('',#57050,10.) ;
#6522 = VECTOR('',#57063,10.) ;
#6523 = VECTOR('',#57064,10.) ;
#6524 = VECTOR('',#57065,10.) ;
#6525 = VECTOR('',#57066,10.) ;
#6526 = VECTOR('',#57069,10.) ;
#6527 = VECTOR('',#57070,10.) ;
#6528 = VECTOR('',#57071,10.) ;
#6529 = VECTOR('',#57072,10.) ;
#6530 = VECTOR('',#57073,10.) ;
#6531 = VECTOR('',#57074,10.) ;
#6532 = VECTOR('',#57077,10.) ;
#6533 = VECTOR('',#57078,10.) ;
#6534 = VECTOR('',#57083,10.) ;
#6535 = VECTOR('',#57088,10.) ;
#6536 = VECTOR('',#57091,10.) ;
#6537 = VECTOR('',#57100,10.) ;
#6538 = VECTOR('',#57103,10.) ;
#6539 = VECTOR('',#57106,10.) ;
#6540 = VECTOR('',#57107,10.) ;
#6541 = VECTOR('',#57112,10.) ;
#6542 = VECTOR('',#57113,10.) ;
#6543 = VECTOR('',#57116,10.) ;
#6544 = VECTOR('',#57117,10.) ;
#6545 = VECTOR('',#57118,10.) ;
#6546 = VECTOR('',#57121,10.) ;
#6547 = VECTOR('',#57122,10.) ;
#6548 = VECTOR('',#57125,10.) ;
#6549 = VECTOR('',#57126,10.) ;
#6550 = VECTOR('',#57127,10.) ;
#6551 = VECTOR('',#57130,10.) ;
#6552 = VECTOR('',#57131,10.) ;
#6553 = VECTOR('',#57132,10.) ;
#6554 = VECTOR('',#57133,10.) ;
#6555 = VECTOR('',#57134,10.) ;
#6556 = VECTOR('',#57135,10.) ;
#6557 = VECTOR('',#57136,10.) ;
#6558 = VECTOR('',#57137,10.) ;
#6559 = VECTOR('',#57142,10.) ;
#6560 = VECTOR('',#57147,10.) ;
#6561 = VECTOR('',#57150,10.) ;
#6562 = VECTOR('',#57155,10.) ;
#6563 = VECTOR('',#57164,10.) ;
#6564 = VECTOR('',#57167,10.) ;
#6565 = VECTOR('',#57172,10.) ;
#6566 = VECTOR('',#57177,10.) ;
#6567 = VECTOR('',#57178,10.) ;
#6568 = VECTOR('',#57179,10.) ;
#6569 = VECTOR('',#57180,10.) ;
#6570 = VECTOR('',#57183,10.) ;
#6571 = VECTOR('',#57184,10.) ;
#6572 = VECTOR('',#57187,10.) ;
#6573 = VECTOR('',#57188,10.) ;
#6574 = VECTOR('',#57191,10.) ;
#6575 = VECTOR('',#57192,10.) ;
#6576 = VECTOR('',#57193,10.) ;
#6577 = VECTOR('',#57194,10.) ;
#6578 = VECTOR('',#57195,10.) ;
#6579 = VECTOR('',#57196,10.) ;
#6580 = VECTOR('',#57199,10.) ;
#6581 = VECTOR('',#57200,10.) ;
#6582 = VECTOR('',#57203,10.) ;
#6583 = VECTOR('',#57208,10.) ;
#6584 = VECTOR('',#57213,10.) ;
#6585 = VECTOR('',#57218,10.) ;
#6586 = VECTOR('',#57221,10.) ;
#6587 = VECTOR('',#57226,10.) ;
#6588 = VECTOR('',#57227,10.) ;
#6589 = VECTOR('',#57232,10.) ;
#6590 = VECTOR('',#57233,10.) ;
#6591 = VECTOR('',#57236,10.) ;
#6592 = VECTOR('',#57237,10.) ;
#6593 = VECTOR('',#57238,10.) ;
#6594 = VECTOR('',#57241,10.) ;
#6595 = VECTOR('',#57242,10.) ;
#6596 = VECTOR('',#57247,10.) ;
#6597 = VECTOR('',#57250,10.) ;
#6598 = VECTOR('',#57255,10.) ;
#6599 = VECTOR('',#57256,10.) ;
#6600 = VECTOR('',#57261,10.) ;
#6601 = VECTOR('',#57262,10.) ;
#6602 = VECTOR('',#57267,10.) ;
#6603 = VECTOR('',#57268,10.) ;
#6604 = VECTOR('',#57271,10.) ;
#6605 = VECTOR('',#57272,10.) ;
#6606 = VECTOR('',#57273,10.) ;
#6607 = VECTOR('',#57276,10.) ;
#6608 = VECTOR('',#57277,10.) ;
#6609 = VECTOR('',#57282,10.) ;
#6610 = VECTOR('',#57285,10.) ;
#6611 = VECTOR('',#57290,10.) ;
#6612 = VECTOR('',#57291,10.) ;
#6613 = VECTOR('',#57296,10.) ;
#6614 = VECTOR('',#57297,10.) ;
#6615 = VECTOR('',#57300,10.) ;
#6616 = VECTOR('',#57301,10.) ;
#6617 = VECTOR('',#57302,10.) ;
#6618 = VECTOR('',#57305,10.) ;
#6619 = VECTOR('',#57306,10.) ;
#6620 = VECTOR('',#57311,10.) ;
#6621 = VECTOR('',#57318,10.) ;
#6622 = VECTOR('',#57323,10.) ;
#6623 = VECTOR('',#57326,10.) ;
#6624 = VECTOR('',#57331,10.) ;
#6625 = VECTOR('',#57334,10.) ;
#6626 = VECTOR('',#57337,10.) ;
#6627 = VECTOR('',#57340,10.) ;
#6628 = VECTOR('',#57343,10.) ;
#6629 = VECTOR('',#57344,10.) ;
#6630 = VECTOR('',#57349,10.) ;
#6631 = VECTOR('',#57352,10.) ;
#6632 = VECTOR('',#57353,10.) ;
#6633 = VECTOR('',#57354,10.) ;
#6634 = VECTOR('',#57355,10.) ;
#6635 = VECTOR('',#57356,10.) ;
#6636 = VECTOR('',#57357,10.) ;
#6637 = VECTOR('',#57360,10.) ;
#6638 = VECTOR('',#57363,10.) ;
#6639 = VECTOR('',#57366,10.) ;
#6640 = VECTOR('',#57371,10.) ;
#6641 = VECTOR('',#57372,10.) ;
#6642 = VECTOR('',#57373,10.) ;
#6643 = VECTOR('',#57376,10.) ;
#6644 = VECTOR('',#57379,10.) ;
#6645 = VECTOR('',#57380,10.) ;
#6646 = VECTOR('',#57385,10.) ;
#6647 = VECTOR('',#57386,10.) ;
#6648 = VECTOR('',#57389,10.) ;
#6649 = VECTOR('',#57392,10.) ;
#6650 = VECTOR('',#57393,10.) ;
#6651 = VECTOR('',#57394,10.) ;
#6652 = VECTOR('',#57397,10.) ;
#6653 = VECTOR('',#57400,10.) ;
#6654 = VECTOR('',#57403,10.) ;
#6655 = VECTOR('',#57406,10.) ;
#6656 = VECTOR('',#57409,10.) ;
#6657 = VECTOR('',#57412,10.) ;
#6658 = VECTOR('',#57415,10.) ;
#6659 = VECTOR('',#57418,10.) ;
#6660 = VECTOR('',#57421,10.) ;
#6661 = VECTOR('',#57424,10.) ;
#6662 = VECTOR('',#57427,10.) ;
#6663 = VECTOR('',#57432,10.) ;
#6664 = VECTOR('',#57437,10.) ;
#6665 = VECTOR('',#57440,10.) ;
#6666 = VECTOR('',#57443,10.) ;
#6667 = VECTOR('',#57444,10.) ;
#6668 = VECTOR('',#57445,10.) ;
#6669 = VECTOR('',#57446,10.) ;
#6670 = VECTOR('',#57447,10.) ;
#6671 = VECTOR('',#57448,10.) ;
#6672 = VECTOR('',#57451,10.) ;
#6673 = VECTOR('',#57454,10.) ;
#6674 = VECTOR('',#57457,10.) ;
#6675 = VECTOR('',#57458,10.) ;
#6676 = VECTOR('',#57461,10.) ;
#6677 = VECTOR('',#57464,10.) ;
#6678 = VECTOR('',#57465,10.) ;
#6679 = VECTOR('',#57468,10.) ;
#6680 = VECTOR('',#57469,10.) ;
#6681 = VECTOR('',#57470,10.) ;
#6682 = VECTOR('',#57471,10.) ;
#6683 = VECTOR('',#57472,10.) ;
#6684 = VECTOR('',#57473,10.) ;
#6685 = VECTOR('',#57476,10.) ;
#6686 = VECTOR('',#57479,10.) ;
#6687 = VECTOR('',#57482,10.) ;
#6688 = VECTOR('',#57485,10.) ;
#6689 = VECTOR('',#57488,10.) ;
#6690 = VECTOR('',#57493,10.) ;
#6691 = VECTOR('',#57494,10.) ;
#6692 = VECTOR('',#57497,10.) ;
#6693 = VECTOR('',#57500,10.) ;
#6694 = VECTOR('',#57501,10.) ;
#6695 = VECTOR('',#57504,10.) ;
#6696 = VECTOR('',#57507,10.) ;
#6697 = VECTOR('',#57510,10.) ;
#6698 = VECTOR('',#57513,10.) ;
#6699 = VECTOR('',#57514,10.) ;
#6700 = VECTOR('',#57517,10.) ;
#6701 = VECTOR('',#57520,10.) ;
#6702 = VECTOR('',#57521,10.) ;
#6703 = VECTOR('',#57524,10.) ;
#6704 = VECTOR('',#57527,10.) ;
#6705 = VECTOR('',#57530,10.) ;
#6706 = VECTOR('',#57531,10.) ;
#6707 = VECTOR('',#57532,10.) ;
#6708 = VECTOR('',#57533,10.) ;
#6709 = VECTOR('',#57534,10.) ;
#6710 = VECTOR('',#57535,10.) ;
#6711 = VECTOR('',#57536,10.) ;
#6712 = VECTOR('',#57539,10.) ;
#6713 = VECTOR('',#57542,10.) ;
#6714 = VECTOR('',#57545,10.) ;
#6715 = VECTOR('',#57548,10.) ;
#6716 = VECTOR('',#57551,10.) ;
#6717 = VECTOR('',#57554,10.) ;
#6718 = VECTOR('',#57557,10.) ;
#6719 = VECTOR('',#57560,10.) ;
#6720 = VECTOR('',#57563,10.) ;
#6721 = VECTOR('',#57566,10.) ;
#6722 = VECTOR('',#57567,10.) ;
#6723 = VECTOR('',#57568,10.) ;
#6724 = VECTOR('',#57569,10.) ;
#6725 = VECTOR('',#57570,10.) ;
#6726 = VECTOR('',#57575,10.) ;
#6727 = VECTOR('',#57576,10.) ;
#6728 = VECTOR('',#57577,10.) ;
#6729 = VECTOR('',#57580,10.) ;
#6730 = VECTOR('',#57583,10.) ;
#6731 = VECTOR('',#57586,10.) ;
#6732 = VECTOR('',#57589,10.) ;
#6733 = VECTOR('',#57590,10.) ;
#6734 = VECTOR('',#57591,10.) ;
#6735 = VECTOR('',#57592,10.) ;
#6736 = VECTOR('',#57599,10.) ;
#6737 = VECTOR('',#57602,10.) ;
#6738 = VECTOR('',#57605,10.) ;
#6739 = VECTOR('',#57608,10.) ;
#6740 = VECTOR('',#57611,10.) ;
#6741 = VECTOR('',#57614,10.) ;
#6742 = VECTOR('',#57617,10.) ;
#6743 = VECTOR('',#57618,10.) ;
#6744 = VECTOR('',#57621,10.) ;
#6745 = VECTOR('',#57624,10.) ;
#6746 = VECTOR('',#57625,10.) ;
#6747 = VECTOR('',#57628,10.) ;
#6748 = VECTOR('',#57629,10.) ;
#6749 = VECTOR('',#57630,10.) ;
#6750 = VECTOR('',#57631,10.) ;
#6751 = VECTOR('',#57632,10.) ;
#6752 = VECTOR('',#57645,10.) ;
#6753 = VECTOR('',#57660,10.) ;
#6754 = VECTOR('',#57665,10.) ;
#6755 = VECTOR('',#57668,10.) ;
#6756 = VECTOR('',#57681,10.) ;
#6757 = VECTOR('',#57686,10.) ;
#6758 = VECTOR('',#57687,10.) ;
#6759 = VECTOR('',#57688,10.) ;
#6760 = VECTOR('',#57705,2.) ;
#6761 = VECTOR('',#57718,2.99999999999999) ;
#6762 = VECTOR('',#57727,10.) ;
#6763 = VECTOR('',#57730,10.) ;
#6764 = VECTOR('',#57731,10.) ;
#6765 = VECTOR('',#57732,10.) ;
#6766 = VECTOR('',#57733,10.) ;
#6767 = VECTOR('',#57734,10.) ;
#6768 = VECTOR('',#57737,10.) ;
#6769 = VECTOR('',#57740,10.) ;
#6770 = VECTOR('',#57743,10.) ;
#6771 = VECTOR('',#57744,10.) ;
#6772 = VECTOR('',#57747,10.) ;
#6773 = VECTOR('',#57750,10.) ;
#6774 = VECTOR('',#57751,10.) ;
#6775 = VECTOR('',#57752,10.) ;
#6776 = VECTOR('',#57755,10.) ;
#6777 = VECTOR('',#57758,10.) ;
#6778 = VECTOR('',#57759,10.) ;
#6779 = VECTOR('',#57762,10.) ;
#6780 = VECTOR('',#57765,10.) ;
#6781 = VECTOR('',#57770,10.) ;
#6782 = VECTOR('',#57775,10.) ;
#6783 = VECTOR('',#57778,10.) ;
#6784 = VECTOR('',#57781,10.) ;
#6785 = VECTOR('',#57784,10.) ;
#6786 = VECTOR('',#57787,10.) ;
#6787 = VECTOR('',#57790,10.) ;
#6788 = VECTOR('',#57793,10.) ;
#6789 = VECTOR('',#57796,10.) ;
#6790 = VECTOR('',#57797,10.) ;
#6791 = VECTOR('',#57798,10.) ;
#6792 = VECTOR('',#57801,10.) ;
#6793 = VECTOR('',#57804,10.) ;
#6794 = VECTOR('',#57807,10.) ;
#6795 = VECTOR('',#57808,10.) ;
#6796 = VECTOR('',#57811,10.) ;
#6797 = VECTOR('',#57814,10.) ;
#6798 = VECTOR('',#57815,10.) ;
#6799 = VECTOR('',#57818,10.) ;
#6800 = VECTOR('',#57821,10.) ;
#6801 = VECTOR('',#57824,10.) ;
#6802 = VECTOR('',#57831,10.) ;
#6803 = VECTOR('',#57832,10.) ;
#6804 = VECTOR('',#57835,10.) ;
#6805 = VECTOR('',#57838,10.) ;
#6806 = VECTOR('',#57841,10.) ;
#6807 = VECTOR('',#57844,10.) ;
#6808 = VECTOR('',#57847,10.) ;
#6809 = VECTOR('',#57850,10.) ;
#6810 = VECTOR('',#57851,10.) ;
#6811 = VECTOR('',#57852,10.) ;
#6812 = VECTOR('',#57855,10.) ;
#6813 = VECTOR('',#57858,10.) ;
#6814 = VECTOR('',#57861,10.) ;
#6815 = VECTOR('',#57864,10.) ;
#6816 = VECTOR('',#57867,10.) ;
#6817 = VECTOR('',#57870,10.) ;
#6818 = VECTOR('',#57871,10.) ;
#6819 = VECTOR('',#57872,10.) ;
#6820 = VECTOR('',#57877,10.) ;
#6821 = VECTOR('',#57880,10.) ;
#6822 = VECTOR('',#57883,10.) ;
#6823 = VECTOR('',#57886,10.) ;
#6824 = VECTOR('',#57887,10.) ;
#6825 = VECTOR('',#57888,10.) ;
#6826 = VECTOR('',#57889,10.) ;
#6827 = VECTOR('',#57890,10.) ;
#6828 = VECTOR('',#57893,10.) ;
#6829 = VECTOR('',#57896,10.) ;
#6830 = VECTOR('',#57899,10.) ;
#6831 = VECTOR('',#57902,10.) ;
#6832 = VECTOR('',#57903,10.) ;
#6833 = VECTOR('',#57904,10.) ;
#6834 = VECTOR('',#57905,10.) ;
#6835 = VECTOR('',#57908,10.) ;
#6836 = VECTOR('',#57911,10.) ;
#6837 = VECTOR('',#57914,10.) ;
#6838 = VECTOR('',#57917,10.) ;
#6839 = VECTOR('',#57918,10.) ;
#6840 = VECTOR('',#57921,10.) ;
#6841 = VECTOR('',#57924,10.) ;
#6842 = VECTOR('',#57927,10.) ;
#6843 = VECTOR('',#57930,10.) ;
#6844 = VECTOR('',#57931,10.) ;
#6845 = VECTOR('',#57934,10.) ;
#6846 = VECTOR('',#57937,10.) ;
#6847 = VECTOR('',#57938,10.) ;
#6848 = VECTOR('',#57941,10.) ;
#6849 = VECTOR('',#57944,10.) ;
#6850 = VECTOR('',#57947,10.) ;
#6851 = VECTOR('',#57950,10.) ;
#6852 = VECTOR('',#57951,10.) ;
#6853 = VECTOR('',#57954,10.) ;
#6854 = VECTOR('',#57957,10.) ;
#6855 = VECTOR('',#57958,10.) ;
#6856 = VECTOR('',#57973,10.) ;
#6857 = VECTOR('',#57974,10.) ;
#6858 = VECTOR('',#57987,10.) ;
#6859 = VECTOR('',#57988,10.) ;
#6860 = VECTOR('',#58001,10.) ;
#6861 = VECTOR('',#58002,10.) ;
#6862 = VECTOR('',#58015,10.) ;
#6863 = VECTOR('',#58016,10.) ;
#6864 = VECTOR('',#58029,10.) ;
#6865 = VECTOR('',#58030,10.) ;
#6866 = VECTOR('',#58043,10.) ;
#6867 = VECTOR('',#58044,10.) ;
#6868 = VECTOR('',#58055,10.) ;
#6869 = VECTOR('',#58056,10.) ;
#6870 = VECTOR('',#58059,10.) ;
#6871 = VECTOR('',#58060,10.) ;
#6872 = VECTOR('',#58061,10.) ;
#6873 = VECTOR('',#58064,10.) ;
#6874 = VECTOR('',#58069,10.) ;
#6875 = VECTOR('',#58070,10.) ;
#6876 = VECTOR('',#58073,10.) ;
#6877 = VECTOR('',#58078,10.) ;
#6878 = VECTOR('',#58079,10.) ;
#6879 = VECTOR('',#58082,10.) ;
#6880 = VECTOR('',#58087,10.) ;
#6881 = VECTOR('',#58088,10.) ;
#6882 = VECTOR('',#58091,10.) ;
#6883 = VECTOR('',#58096,10.) ;
#6884 = VECTOR('',#58097,10.) ;
#6885 = VECTOR('',#58100,10.) ;
#6886 = VECTOR('',#58105,10.) ;
#6887 = VECTOR('',#58106,10.) ;
#6888 = VECTOR('',#58107,10.) ;
#6889 = VECTOR('',#58110,10.) ;
#6890 = VECTOR('',#58119,3.) ;
#6891 = VECTOR('',#58122,10.) ;
#6892 = VECTOR('',#58143,2.) ;
#6893 = VECTOR('',#58158,1.85) ;
#6894 = VECTOR('',#58165,10.) ;
#6895 = VECTOR('',#58166,10.) ;
#6896 = VECTOR('',#58169,10.) ;
#6897 = VECTOR('',#58172,10.) ;
#6898 = VECTOR('',#58181,10.) ;
#6899 = VECTOR('',#58182,10.) ;
#6900 = VECTOR('',#58183,10.) ;
#6901 = VECTOR('',#58196,1.85) ;
#6902 = VECTOR('',#58203,10.) ;
#6903 = VECTOR('',#58204,10.) ;
#6904 = VECTOR('',#58207,10.) ;
#6905 = VECTOR('',#58210,10.) ;
#6906 = VECTOR('',#58219,10.) ;
#6907 = VECTOR('',#58220,10.) ;
#6908 = VECTOR('',#58221,10.) ;
#6909 = VECTOR('',#58234,10.) ;
#6910 = VECTOR('',#58245,10.) ;
#6911 = VECTOR('',#58254,10.) ;
#6912 = VECTOR('',#58257,10.) ;
#6913 = VECTOR('',#58258,10.) ;
#6914 = VECTOR('',#58259,10.) ;
#6915 = VECTOR('',#58260,10.) ;
#6916 = VECTOR('',#58261,10.) ;
#6917 = VECTOR('',#58262,10.) ;
#6918 = VECTOR('',#58263,10.) ;
#6919 = VECTOR('',#58264,10.) ;
#6920 = VECTOR('',#58265,10.) ;
#6921 = VECTOR('',#58268,10.) ;
#6922 = VECTOR('',#58275,10.) ;
#6923 = VECTOR('',#58280,10.) ;
#6924 = VECTOR('',#58281,10.) ;
#6925 = VECTOR('',#58286,10.) ;
#6926 = VECTOR('',#58289,10.) ;
#6927 = VECTOR('',#58290,10.) ;
#6928 = VECTOR('',#58309,10.) ;
#6929 = VECTOR('',#58330,10.) ;
#6930 = VECTOR('',#58341,10.) ;
#6931 = VECTOR('',#58358,10.) ;
#6932 = VECTOR('',#58375,10.) ;
#6933 = VECTOR('',#58376,10.) ;
#6934 = VECTOR('',#58395,10.) ;
#6935 = VECTOR('',#58398,10.) ;
#6936 = VECTOR('',#58409,10.) ;
#6937 = VECTOR('',#58410,10.) ;
#6938 = VECTOR('',#58415,10.) ;
#6939 = VECTOR('',#58416,10.) ;
#6940 = VECTOR('',#58427,10.) ;
#6941 = VECTOR('',#58436,10.) ;
#6942 = VECTOR('',#58441,10.) ;
#6943 = VECTOR('',#58444,10.) ;
#6944 = VECTOR('',#58449,10.) ;
#6945 = VECTOR('',#58452,10.) ;
#6946 = VECTOR('',#58455,10.) ;
#6947 = VECTOR('',#58468,10.) ;
#6948 = VECTOR('',#58469,10.) ;
#6949 = VECTOR('',#58476,10.) ;
#6950 = VECTOR('',#58481,10.) ;
#6951 = VECTOR('',#58492,10.) ;
#6952 = VECTOR('',#58493,10.) ;
#6953 = VECTOR('',#58502,10.) ;
#6954 = VECTOR('',#58503,10.) ;
#6955 = VECTOR('',#58514,10.) ;
#6956 = VECTOR('',#58525,10.) ;
#6957 = VECTOR('',#58536,10.) ;
#6958 = VECTOR('',#58545,10.) ;
#6959 = VECTOR('',#58548,10.) ;
#6960 = VECTOR('',#58549,10.) ;
#6961 = VECTOR('',#58550,10.) ;
#6962 = VECTOR('',#58553,10.) ;
#6963 = VECTOR('',#58558,10.) ;
#6964 = VECTOR('',#58559,10.) ;
#6965 = VECTOR('',#58562,10.) ;
#6966 = VECTOR('',#58567,10.) ;
#6967 = VECTOR('',#58568,10.) ;
#6968 = VECTOR('',#58571,10.) ;
#6969 = VECTOR('',#58576,10.) ;
#6970 = VECTOR('',#58577,10.) ;
#6971 = VECTOR('',#58580,10.) ;
#6972 = VECTOR('',#58585,10.) ;
#6973 = VECTOR('',#58586,10.) ;
#6974 = VECTOR('',#58589,10.) ;
#6975 = VECTOR('',#58594,10.) ;
#6976 = VECTOR('',#58595,10.) ;
#6977 = VECTOR('',#58600,10.) ;
#6978 = VECTOR('',#58613,10.) ;
#6979 = VECTOR('',#58624,10.) ;
#6980 = VECTOR('',#58635,10.) ;
#6981 = VECTOR('',#58646,10.) ;
#6982 = VECTOR('',#58651,10.) ;
#6983 = VECTOR('',#58664,10.) ;
#6984 = VECTOR('',#58675,10.) ;
#6985 = VECTOR('',#58686,10.) ;
#6986 = VECTOR('',#58689,10.) ;
#6987 = VECTOR('',#58692,10.) ;
#6988 = VECTOR('',#58693,10.) ;
#6989 = VECTOR('',#58696,10.) ;
#6990 = VECTOR('',#58701,10.) ;
#6991 = VECTOR('',#58702,10.) ;
#6992 = VECTOR('',#58705,10.) ;
#6993 = VECTOR('',#58710,10.) ;
#6994 = VECTOR('',#58711,10.) ;
#6995 = VECTOR('',#58714,10.) ;
#6996 = VECTOR('',#58719,10.) ;
#6997 = VECTOR('',#58720,10.) ;
#6998 = VECTOR('',#58741,10.) ;
#6999 = VECTOR('',#58752,10.) ;
#7000 = VECTOR('',#58763,10.) ;
#7001 = VECTOR('',#58774,10.) ;
#7002 = VECTOR('',#58783,10.) ;
#7003 = VECTOR('',#58788,10.) ;
#7004 = VECTOR('',#58793,10.) ;
#7005 = VECTOR('',#58794,10.) ;
#7006 = VECTOR('',#58803,10.) ;
#7007 = VECTOR('',#58804,10.) ;
#7008 = VECTOR('',#58813,10.) ;
#7009 = VECTOR('',#58816,10.) ;
#7010 = VECTOR('',#58817,10.) ;
#7011 = VECTOR('',#58830,10.) ;
#7012 = VECTOR('',#58835,10.) ;
#7013 = VECTOR('',#58848,10.) ;
#7014 = VECTOR('',#58859,10.) ;
#7015 = VECTOR('',#58868,10.) ;
#7016 = VECTOR('',#58883,10.) ;
#7017 = VECTOR('',#58884,10.) ;
#7018 = VECTOR('',#58885,10.) ;
#7019 = VECTOR('',#58888,10.) ;
#7020 = VECTOR('',#58893,10.) ;
#7021 = VECTOR('',#58894,10.) ;
#7022 = VECTOR('',#58897,10.) ;
#7023 = VECTOR('',#58902,10.) ;
#7024 = VECTOR('',#58903,10.) ;
#7025 = VECTOR('',#58906,10.) ;
#7026 = VECTOR('',#58911,10.) ;
#7027 = VECTOR('',#58912,10.) ;
#7028 = VECTOR('',#58915,10.) ;
#7029 = VECTOR('',#58920,10.) ;
#7030 = VECTOR('',#58921,10.) ;
#7031 = VECTOR('',#58934,10.) ;
#7032 = VECTOR('',#58939,10.) ;
#7033 = VECTOR('',#58952,10.) ;
#7034 = VECTOR('',#58963,10.) ;
#7035 = VECTOR('',#58972,10.) ;
#7036 = VECTOR('',#58987,10.) ;
#7037 = VECTOR('',#58988,10.) ;
#7038 = VECTOR('',#58989,10.) ;
#7039 = VECTOR('',#58992,10.) ;
#7040 = VECTOR('',#58997,10.) ;
#7041 = VECTOR('',#58998,10.) ;
#7042 = VECTOR('',#59001,10.) ;
#7043 = VECTOR('',#59006,10.) ;
#7044 = VECTOR('',#59007,10.) ;
#7045 = VECTOR('',#59010,10.) ;
#7046 = VECTOR('',#59015,10.) ;
#7047 = VECTOR('',#59016,10.) ;
#7048 = VECTOR('',#59019,10.) ;
#7049 = VECTOR('',#59024,10.) ;
#7050 = VECTOR('',#59025,10.) ;
#7051 = VECTOR('',#59034,10.) ;
#7052 = VECTOR('',#59047,10.) ;
#7053 = VECTOR('',#59050,10.) ;
#7054 = VECTOR('',#59061,10.) ;
#7055 = VECTOR('',#59074,10.) ;
#7056 = VECTOR('',#59085,10.) ;
#7057 = VECTOR('',#59096,10.) ;
#7058 = VECTOR('',#59105,10.) ;
#7059 = VECTOR('',#59108,10.) ;
#7060 = VECTOR('',#59109,10.) ;
#7061 = VECTOR('',#59112,10.) ;
#7062 = VECTOR('',#59117,10.) ;
#7063 = VECTOR('',#59118,10.) ;
#7064 = VECTOR('',#59121,10.) ;
#7065 = VECTOR('',#59126,10.) ;
#7066 = VECTOR('',#59127,10.) ;
#7067 = VECTOR('',#59130,10.) ;
#7068 = VECTOR('',#59135,10.) ;
#7069 = VECTOR('',#59136,10.) ;
#7070 = VECTOR('',#59139,10.) ;
#7071 = VECTOR('',#59144,10.) ;
#7072 = VECTOR('',#59147,10.) ;
#7073 = VECTOR('',#59158,10.) ;
#7074 = VECTOR('',#59159,10.) ;
#7075 = VECTOR('',#59160,10.) ;
#7076 = VECTOR('',#59161,10.) ;
#7077 = VECTOR('',#59170,10.) ;
#7078 = VECTOR('',#59189,10.) ;
#7079 = VECTOR('',#59192,10.) ;
#7080 = VECTOR('',#59207,10.) ;
#7081 = VECTOR('',#59210,10.) ;
#7082 = VECTOR('',#59213,10.) ;
#7083 = VECTOR('',#59216,10.) ;
#7084 = VECTOR('',#59237,10.) ;
#7085 = VECTOR('',#59238,10.) ;
#7086 = VECTOR('',#59239,10.) ;
#7087 = VECTOR('',#59240,10.) ;
#7088 = VECTOR('',#59289,10.) ;
#7089 = VECTOR('',#59308,10.) ;
#7090 = VECTOR('',#59311,10.) ;
#7091 = VECTOR('',#59316,10.) ;
#7092 = VECTOR('',#59319,10.) ;
#7093 = VECTOR('',#59322,10.) ;
#7094 = VECTOR('',#59331,10.) ;
#7095 = VECTOR('',#59352,10.) ;
#7096 = VECTOR('',#59353,10.) ;
#7097 = VECTOR('',#59354,10.) ;
#7098 = VECTOR('',#59355,10.) ;
#7099 = VECTOR('',#59414,10.) ;
#7100 = VECTOR('',#59425,10.) ;
#7101 = VECTOR('',#59428,10.) ;
#7102 = VECTOR('',#59433,10.) ;
#7103 = VECTOR('',#59436,10.) ;
#7104 = VECTOR('',#59439,10.) ;
#7105 = VECTOR('',#59446,10.) ;
#7106 = VECTOR('',#59491,10.) ;
#7107 = VECTOR('',#59500,10.) ;
#7108 = VECTOR('',#59531,10.) ;
#7109 = VECTOR('',#59542,10.) ;
#7110 = VECTOR('',#59559,10.) ;
#7111 = VECTOR('',#59576,10.) ;
#7112 = VECTOR('',#59587,10.) ;
#7113 = VECTOR('',#59598,10.) ;
#7114 = VECTOR('',#59609,10.) ;
#7115 = VECTOR('',#59620,10.) ;
#7116 = VECTOR('',#59631,10.) ;
#7117 = VECTOR('',#59642,10.) ;
#7118 = VECTOR('',#59651,10.) ;
#7119 = VECTOR('',#59662,10.) ;
#7120 = VECTOR('',#59663,10.) ;
#7121 = VECTOR('',#59666,10.) ;
#7122 = VECTOR('',#59671,10.) ;
#7123 = VECTOR('',#59672,10.) ;
#7124 = VECTOR('',#59687,10.) ;
#7125 = VECTOR('',#59688,10.) ;
#7126 = VECTOR('',#59689,10.) ;
#7127 = VECTOR('',#59692,10.) ;
#7128 = VECTOR('',#59697,0.600000000000005) ;
#7129 = VECTOR('',#59698,10.) ;
#7130 = VECTOR('',#59701,0.600000000000005) ;
#7131 = VECTOR('',#59706,10.) ;
#7132 = VECTOR('',#59711,10.) ;
#7133 = VECTOR('',#59712,10.) ;
#7134 = VECTOR('',#59715,0.600000000000023) ;
#7135 = VECTOR('',#59720,0.600000000000023) ;
#7136 = VECTOR('',#59725,10.) ;
#7137 = VECTOR('',#59726,10.) ;
#7138 = VECTOR('',#59729,10.) ;
#7139 = VECTOR('',#59734,10.) ;
#7140 = VECTOR('',#59735,10.) ;
#7141 = VECTOR('',#59738,10.) ;
#7142 = VECTOR('',#59743,10.) ;
#7143 = VECTOR('',#59744,10.) ;
#7144 = VECTOR('',#59747,10.) ;
#7145 = VECTOR('',#59752,10.) ;
#7146 = VECTOR('',#59753,10.) ;
#7147 = VECTOR('',#59756,10.) ;
#7148 = VECTOR('',#59761,10.) ;
#7149 = VECTOR('',#59762,10.) ;
#7150 = VECTOR('',#59765,10.) ;
#7151 = VECTOR('',#59770,10.) ;
#7152 = VECTOR('',#59771,10.) ;
#7153 = VECTOR('',#59774,10.) ;
#7154 = VECTOR('',#59779,10.) ;
#7155 = VECTOR('',#59780,10.) ;
#7156 = VECTOR('',#59783,10.) ;
#7157 = VECTOR('',#59788,10.) ;
#7158 = VECTOR('',#59797,10.) ;
#7159 = VECTOR('',#59800,10.) ;
#7160 = VECTOR('',#59815,10.) ;
#7161 = VECTOR('',#59820,10.) ;
#7162 = VECTOR('',#59821,10.) ;
#7163 = VECTOR('',#59824,10.) ;
#7164 = VECTOR('',#59825,10.) ;
#7165 = VECTOR('',#59826,10.) ;
#7166 = VECTOR('',#59831,10.) ;
#7167 = VECTOR('',#59846,10.) ;
#7168 = VECTOR('',#59847,10.) ;
#7169 = VECTOR('',#59866,10.) ;
#7170 = VECTOR('',#59877,10.) ;
#7171 = VECTOR('',#59888,10.) ;
#7172 = VECTOR('',#59899,10.) ;
#7173 = VECTOR('',#59910,10.) ;
#7174 = VECTOR('',#59913,10.) ;
#7175 = VECTOR('',#59914,10.) ;
#7176 = VECTOR('',#59917,10.) ;
#7177 = VECTOR('',#59920,10.) ;
#7178 = VECTOR('',#59921,10.) ;
#7179 = VECTOR('',#59924,10.) ;
#7180 = VECTOR('',#59925,10.) ;
#7181 = VECTOR('',#59928,10.) ;
#7182 = VECTOR('',#59929,10.) ;
#7183 = VECTOR('',#59932,10.) ;
#7184 = VECTOR('',#59933,10.) ;
#7185 = VECTOR('',#59936,10.) ;
#7186 = VECTOR('',#59937,10.) ;
#7187 = VECTOR('',#59940,10.) ;
#7188 = VECTOR('',#59963,10.) ;
#7189 = VECTOR('',#59966,10.) ;
#7190 = VECTOR('',#59967,10.) ;
#7191 = VECTOR('',#59984,10.) ;
#7192 = VECTOR('',#59995,10.) ;
#7193 = VECTOR('',#60024,10.) ;
#7194 = VECTOR('',#60027,10.) ;
#7195 = VECTOR('',#60028,10.) ;
#7196 = VECTOR('',#60031,10.) ;
#7197 = VECTOR('',#60034,10.) ;
#7198 = VECTOR('',#60035,10.) ;
#7199 = VECTOR('',#60044,10.) ;
#7200 = VECTOR('',#60047,10.) ;
#7201 = VECTOR('',#60060,10.) ;
#7202 = VECTOR('',#60061,10.) ;
#7203 = VECTOR('',#60066,10.) ;
#7204 = VECTOR('',#60069,10.) ;
#7205 = VECTOR('',#60082,10.) ;
#7206 = VECTOR('',#60085,10.) ;
#7207 = VECTOR('',#60124,10.) ;
#7208 = VECTOR('',#60127,10.) ;
#7209 = VECTOR('',#60142,10.) ;
#7210 = VECTOR('',#60147,10.) ;
#7211 = VECTOR('',#60148,10.) ;
#7212 = VECTOR('',#60151,10.) ;
#7213 = VECTOR('',#60152,10.) ;
#7214 = VECTOR('',#60153,10.) ;
#7215 = VECTOR('',#60158,10.) ;
#7216 = VECTOR('',#60173,10.) ;
#7217 = VECTOR('',#60174,10.) ;
#7218 = VECTOR('',#60209,10.) ;
#7219 = VECTOR('',#60214,10.) ;
#7220 = VECTOR('',#60217,10.) ;
#7221 = VECTOR('',#60218,10.) ;
#7222 = VECTOR('',#60221,10.) ;
#7223 = VECTOR('',#60224,10.) ;
#7224 = VECTOR('',#60225,10.) ;
#7225 = VECTOR('',#60228,10.) ;
#7226 = VECTOR('',#60231,10.) ;
#7227 = VECTOR('',#60232,10.) ;
#7228 = VECTOR('',#60235,10.) ;
#7229 = VECTOR('',#60238,10.) ;
#7230 = VECTOR('',#60239,10.) ;
#7231 = VECTOR('',#60242,10.) ;
#7232 = VECTOR('',#60255,10.) ;
#7233 = VECTOR('',#60260,10.) ;
#7234 = VECTOR('',#60321,10.) ;
#7235 = VECTOR('',#60332,10.) ;
#7236 = VECTOR('',#60335,10.) ;
#7237 = VECTOR('',#60338,10.) ;
#7238 = VECTOR('',#60339,10.) ;
#7239 = VECTOR('',#60342,10.) ;
#7240 = VECTOR('',#60345,10.) ;
#7241 = VECTOR('',#60348,10.) ;
#7242 = VECTOR('',#60349,10.) ;
#7243 = VECTOR('',#60352,10.) ;
#7244 = VECTOR('',#60353,10.) ;
#7245 = VECTOR('',#60356,10.) ;
#7246 = VECTOR('',#60359,10.) ;
#7247 = VECTOR('',#60362,10.) ;
#7248 = VECTOR('',#60365,10.) ;
#7249 = VECTOR('',#60366,10.) ;
#7250 = VECTOR('',#60383,2.5) ;
#7251 = VECTOR('',#60396,10.) ;
#7252 = VECTOR('',#60399,10.) ;
#7253 = VECTOR('',#60414,10.) ;
#7254 = VECTOR('',#60415,10.) ;
#7255 = VECTOR('',#60418,10.) ;
#7256 = VECTOR('',#60421,10.) ;
#7257 = VECTOR('',#60422,10.) ;
#7258 = VECTOR('',#60425,10.) ;
#7259 = VECTOR('',#60426,10.) ;
#7260 = VECTOR('',#60431,10.) ;
#7261 = VECTOR('',#60492,10.) ;
#7262 = VECTOR('',#60503,2.5) ;
#7263 = VECTOR('',#60514,2.) ;
#7264 = VECTOR('',#60623,10.) ;
#7265 = VECTOR('',#60632,10.) ;
#7266 = VECTOR('',#60655,2.8) ;
#7267 = VECTOR('',#60676,2.8) ;
#7268 = VECTOR('',#60701,2.) ;
#7269 = VECTOR('',#60714,2.79999999999999) ;
#7270 = VECTOR('',#60749,10.) ;
#7271 = VECTOR('',#60750,10.) ;
#7272 = VECTOR('',#60753,10.) ;
#7273 = VECTOR('',#60800,10.) ;
#7274 = VECTOR('',#60817,10.) ;
#7275 = VECTOR('',#60822,10.) ;
#7276 = VECTOR('',#60839,10.) ;
#7277 = VECTOR('',#60846,10.) ;
#7278 = VECTOR('',#60849,10.) ;
#7279 = VECTOR('',#60854,10.) ;
#7280 = VECTOR('',#60861,10.) ;
#7281 = VECTOR('',#60866,10.) ;
#7282 = VECTOR('',#60873,10.) ;
#7283 = VECTOR('',#60878,10.) ;
#7284 = VECTOR('',#60885,10.) ;
#7285 = VECTOR('',#60886,10.) ;
#7286 = VECTOR('',#60889,10.) ;
#7287 = VECTOR('',#60894,10.) ;
#7288 = VECTOR('',#60895,10.) ;
#7289 = VECTOR('',#60902,10.) ;
#7290 = VECTOR('',#60903,10.) ;
#7291 = VECTOR('',#60910,10.) ;
#7292 = VECTOR('',#60929,10.) ;
#7293 = VECTOR('',#60932,10.) ;
#7294 = VECTOR('',#60941,10.) ;
#7295 = VECTOR('',#60948,10.) ;
#7296 = VECTOR('',#60951,10.) ;
#7297 = VECTOR('',#60956,10.) ;
#7298 = VECTOR('',#60959,10.) ;
#7299 = VECTOR('',#60962,10.) ;
#7300 = VECTOR('',#60965,10.) ;
#7301 = VECTOR('',#60978,10.) ;
#7302 = VECTOR('',#60979,10.) ;
#7303 = VECTOR('',#60984,10.) ;
#7304 = VECTOR('',#60985,10.) ;
#7305 = VECTOR('',#60988,10.) ;
#7306 = VECTOR('',#60989,10.) ;
#7307 = VECTOR('',#60992,10.) ;
#7308 = VECTOR('',#60993,10.) ;
#7309 = VECTOR('',#60994,10.) ;
#7310 = VECTOR('',#60997,10.) ;
#7311 = VECTOR('',#60998,10.) ;
#7312 = VECTOR('',#60999,10.) ;
#7313 = VECTOR('',#61002,10.) ;
#7314 = VECTOR('',#61003,10.) ;
#7315 = VECTOR('',#61006,10.) ;
#7316 = VECTOR('',#61007,10.) ;
#7317 = VECTOR('',#61010,10.) ;
#7318 = VECTOR('',#61013,10.) ;
#7319 = VECTOR('',#61022,10.) ;
#7320 = VECTOR('',#61025,10.) ;
#7321 = VECTOR('',#61030,10.) ;
#7322 = VECTOR('',#61033,10.) ;
#7323 = VECTOR('',#61036,10.) ;
#7324 = VECTOR('',#61039,10.) ;
#7325 = VECTOR('',#61050,10.) ;
#7326 = VECTOR('',#61053,10.) ;
#7327 = VECTOR('',#61054,10.) ;
#7328 = VECTOR('',#61055,10.) ;
#7329 = VECTOR('',#61056,10.) ;
#7330 = VECTOR('',#61057,10.) ;
#7331 = VECTOR('',#61060,10.) ;
#7332 = VECTOR('',#61063,10.) ;
#7333 = VECTOR('',#61066,10.) ;
#7334 = VECTOR('',#61069,10.) ;
#7335 = VECTOR('',#61070,10.) ;
#7336 = VECTOR('',#61071,10.) ;
#7337 = VECTOR('',#61072,10.) ;
#7338 = VECTOR('',#61073,10.) ;
#7339 = VECTOR('',#61074,10.) ;
#7340 = VECTOR('',#61075,10.) ;
#7341 = VECTOR('',#61076,10.) ;
#7342 = VECTOR('',#61077,10.) ;
#7343 = VECTOR('',#61080,10.) ;
#7344 = VECTOR('',#61083,10.) ;
#7345 = VECTOR('',#61086,10.) ;
#7346 = VECTOR('',#61087,10.) ;
#7347 = VECTOR('',#61088,10.) ;
#7348 = VECTOR('',#61089,10.) ;
#7349 = VECTOR('',#61090,10.) ;
#7350 = VECTOR('',#61091,10.) ;
#7351 = VECTOR('',#61092,10.) ;
#7352 = VECTOR('',#61093,10.) ;
#7353 = VECTOR('',#61094,10.) ;
#7354 = VECTOR('',#61095,10.) ;
#7355 = VECTOR('',#61096,10.) ;
#7356 = VECTOR('',#61097,10.) ;
#7357 = VECTOR('',#61098,10.) ;
#7358 = VECTOR('',#61099,10.) ;
#7359 = VECTOR('',#61100,10.) ;
#7360 = VECTOR('',#61101,10.) ;
#7361 = VECTOR('',#61104,10.) ;
#7362 = VECTOR('',#61109,10.) ;
#7363 = VECTOR('',#61110,10.) ;
#7364 = VECTOR('',#61113,10.) ;
#7365 = VECTOR('',#61120,10.) ;
#7366 = VECTOR('',#61121,10.) ;
#7367 = VECTOR('',#61122,10.) ;
#7368 = VECTOR('',#61123,10.) ;
#7369 = VECTOR('',#61124,10.) ;
#7370 = VECTOR('',#61125,10.) ;
#7371 = VECTOR('',#61126,10.) ;
#7372 = VECTOR('',#61127,10.) ;
#7373 = VECTOR('',#61128,10.) ;
#7374 = VECTOR('',#61131,10.) ;
#7375 = VECTOR('',#61134,10.) ;
#7376 = VECTOR('',#61137,10.) ;
#7377 = VECTOR('',#61140,10.) ;
#7378 = VECTOR('',#61141,10.) ;
#7379 = VECTOR('',#61142,10.) ;
#7380 = VECTOR('',#61143,10.) ;
#7381 = VECTOR('',#61144,10.) ;
#7382 = VECTOR('',#61149,10.) ;
#7383 = VECTOR('',#61152,10.) ;
#7384 = VECTOR('',#61153,10.) ;
#7385 = VECTOR('',#61154,10.) ;
#7386 = VECTOR('',#61155,10.) ;
#7387 = VECTOR('',#61156,10.) ;
#7388 = VECTOR('',#61161,10.) ;
#7389 = VECTOR('',#61170,10.) ;
#7390 = VECTOR('',#61173,10.) ;
#7391 = VECTOR('',#61174,10.) ;
#7392 = VECTOR('',#61193,10.) ;
#7393 = VECTOR('',#61194,10.) ;
#7394 = VECTOR('',#61197,10.) ;
#7395 = VECTOR('',#61198,10.) ;
#7396 = VECTOR('',#61199,10.) ;
#7397 = VECTOR('',#61206,10.) ;
#7398 = VECTOR('',#61225,10.) ;
#7399 = VECTOR('',#61226,10.) ;
#7400 = VECTOR('',#61229,10.) ;
#7401 = VECTOR('',#61248,10.) ;
#7402 = VECTOR('',#61251,10.) ;
#7403 = VECTOR('',#61256,10.) ;
#7404 = VECTOR('',#61257,10.) ;
#7405 = VECTOR('',#61274,10.) ;
#7406 = VECTOR('',#61277,10.) ;
#7407 = VECTOR('',#61288,10.) ;
#7408 = VECTOR('',#61289,10.) ;
#7409 = VECTOR('',#61290,10.) ;
#7410 = VECTOR('',#61297,10.) ;
#7411 = VECTOR('',#61308,10.) ;
#7412 = VECTOR('',#61311,10.) ;
#7413 = VECTOR('',#61320,10.) ;
#7414 = VECTOR('',#61331,10.) ;
#7415 = VECTOR('',#61338,10.) ;
#7416 = VECTOR('',#61339,10.) ;
#7417 = VECTOR('',#61342,10.) ;
#7418 = VECTOR('',#61349,10.) ;
#7419 = VECTOR('',#61350,10.) ;
#7420 = VECTOR('',#61357,10.) ;
#7421 = VECTOR('',#61362,10.) ;
#7422 = VECTOR('',#61365,10.) ;
#7423 = VECTOR('',#61376,10.) ;
#7424 = VECTOR('',#61379,10.) ;
#7425 = VECTOR('',#61384,10.) ;
#7426 = VECTOR('',#61387,10.) ;
#7427 = VECTOR('',#61404,10.) ;
#7428 = VECTOR('',#61405,10.) ;
#7429 = VECTOR('',#61426,10.) ;
#7430 = VECTOR('',#61427,10.) ;
#7431 = VECTOR('',#61448,10.) ;
#7432 = VECTOR('',#61449,10.) ;
#7433 = VECTOR('',#61470,10.) ;
#7434 = VECTOR('',#61471,10.) ;
#7435 = VECTOR('',#61492,10.) ;
#7436 = VECTOR('',#61493,10.) ;
#7437 = VECTOR('',#61514,10.) ;
#7438 = VECTOR('',#61515,10.) ;
#7439 = VECTOR('',#61536,10.) ;
#7440 = VECTOR('',#61537,10.) ;
#7441 = VECTOR('',#61558,10.) ;
#7442 = VECTOR('',#61559,10.) ;
#7443 = VECTOR('',#61570,1.2) ;
#7444 = VECTOR('',#61573,1.2) ;
#7445 = VECTOR('',#61578,1.2) ;
#7446 = VECTOR('',#61581,1.2) ;
#7447 = VECTOR('',#61586,1.2) ;
#7448 = VECTOR('',#61589,1.2) ;
#7449 = VECTOR('',#61594,1.2) ;
#7450 = VECTOR('',#61597,1.2) ;
#7451 = VECTOR('',#61602,10.) ;
#7452 = VECTOR('',#61603,10.) ;
#7453 = VECTOR('',#61604,10.) ;
#7454 = VECTOR('',#61605,10.) ;
#7455 = VECTOR('',#61608,10.) ;
#7456 = VECTOR('',#61609,10.) ;
#7457 = VECTOR('',#61612,10.) ;
#7458 = VECTOR('',#61615,10.) ;
#7459 = VECTOR('',#61618,10.) ;
#7460 = VECTOR('',#61621,10.) ;
#7461 = VECTOR('',#61626,10.) ;
#7462 = VECTOR('',#61631,10.) ;
#7463 = VECTOR('',#61634,10.) ;
#7464 = VECTOR('',#61637,10.) ;
#7465 = VECTOR('',#61640,10.) ;
#7466 = VECTOR('',#61643,10.) ;
#7467 = VECTOR('',#61650,10.) ;
#7468 = VECTOR('',#61651,10.) ;
#7469 = VECTOR('',#61652,10.) ;
#7470 = VECTOR('',#61653,10.) ;
#7471 = VECTOR('',#61656,10.) ;
#7472 = VECTOR('',#61657,10.) ;
#7473 = VECTOR('',#61658,10.) ;
#7474 = VECTOR('',#61661,10.) ;
#7475 = VECTOR('',#61662,10.) ;
#7476 = VECTOR('',#61663,10.) ;
#7477 = VECTOR('',#61666,10.) ;
#7478 = VECTOR('',#61667,10.) ;
#7479 = VECTOR('',#61688,2.) ;
#7480 = VECTOR('',#61695,2.4) ;
#7481 = VECTOR('',#61714,2.49999999999999) ;
#7482 = VECTOR('',#61721,2.69999999999999) ;
#7483 = VECTOR('',#61736,2.5) ;
#7484 = VECTOR('',#61747,3.) ;
#7485 = VECTOR('',#61770,10.) ;
#7486 = VECTOR('',#61771,10.) ;
#7487 = VECTOR('',#61792,10.) ;
#7488 = VECTOR('',#61793,10.) ;
#7489 = VECTOR('',#61812,10.) ;
#7490 = VECTOR('',#61813,10.) ;
#7491 = VECTOR('',#61816,10.) ;
#7492 = VECTOR('',#61817,10.) ;
#7493 = VECTOR('',#61836,10.) ;
#7494 = VECTOR('',#61837,10.) ;
#7495 = VECTOR('',#61858,10.) ;
#7496 = VECTOR('',#61859,10.) ;
#7497 = VECTOR('',#61862,10.) ;
#7498 = VECTOR('',#61863,10.) ;
#7499 = VECTOR('',#61882,10.) ;
#7500 = VECTOR('',#61883,10.) ;
#7501 = VECTOR('',#61902,10.) ;
#7502 = VECTOR('',#61903,10.) ;
#7503 = VECTOR('',#61906,10.) ;
#7504 = VECTOR('',#61907,10.) ;
#7505 = VECTOR('',#61928,10.) ;
#7506 = VECTOR('',#61929,10.) ;
#7507 = VECTOR('',#61948,10.) ;
#7508 = VECTOR('',#61949,10.) ;
#7509 = VECTOR('',#61952,10.) ;
#7510 = VECTOR('',#61953,10.) ;
#7511 = VECTOR('',#61972,10.) ;
#7512 = VECTOR('',#61973,10.) ;
#7513 = VECTOR('',#61994,10.) ;
#7514 = VECTOR('',#61995,10.) ;
#7515 = VECTOR('',#61998,10.) ;
#7516 = VECTOR('',#61999,10.) ;
#7517 = VECTOR('',#62018,10.) ;
#7518 = VECTOR('',#62019,10.) ;
#7519 = VECTOR('',#62022,10.) ;
#7520 = VECTOR('',#62023,10.) ;
#7521 = VECTOR('',#62026,10.) ;
#7522 = VECTOR('',#62027,10.) ;
#7523 = VECTOR('',#62030,10.) ;
#7524 = VECTOR('',#62031,10.) ;
#7525 = VECTOR('',#62034,10.) ;
#7526 = VECTOR('',#62035,10.) ;
#7527 = VECTOR('',#62038,10.) ;
#7528 = VECTOR('',#62039,10.) ;
#7529 = VECTOR('',#62042,10.) ;
#7530 = VECTOR('',#62043,10.) ;
#7531 = VECTOR('',#62046,10.) ;
#7532 = VECTOR('',#62047,10.) ;
#7533 = VECTOR('',#62050,10.) ;
#7534 = VECTOR('',#62053,10.) ;
#7535 = VECTOR('',#62056,10.) ;
#7536 = VECTOR('',#62059,10.) ;
#7537 = VECTOR('',#62062,10.) ;
#7538 = VECTOR('',#62065,10.) ;
#7539 = VECTOR('',#62068,10.) ;
#7540 = VECTOR('',#62071,10.) ;
#7541 = VECTOR('',#62074,10.) ;
#7542 = VECTOR('',#62077,10.) ;
#7543 = VECTOR('',#62080,10.) ;
#7544 = VECTOR('',#62087,10.) ;
#7545 = VECTOR('',#62088,10.) ;
#7546 = VECTOR('',#62091,10.) ;
#7547 = VECTOR('',#62092,10.) ;
#7548 = VECTOR('',#62095,10.) ;
#7549 = VECTOR('',#62098,10.) ;
#7550 = VECTOR('',#62099,10.) ;
#7551 = VECTOR('',#62102,10.) ;
#7552 = VECTOR('',#62103,10.) ;
#7553 = VECTOR('',#62106,10.) ;
#7554 = VECTOR('',#62107,10.) ;
#7555 = VECTOR('',#62110,10.) ;
#7556 = VECTOR('',#62111,10.) ;
#7557 = VECTOR('',#62132,1.99999999999999) ;
#7558 = VECTOR('',#62175,10.) ;
#7559 = VECTOR('',#62176,10.) ;
#7560 = VECTOR('',#62181,10.) ;
#7561 = VECTOR('',#62182,10.) ;
#7562 = VECTOR('',#62201,10.) ;
#7563 = VECTOR('',#62202,10.) ;
#7564 = VECTOR('',#62205,10.) ;
#7565 = VECTOR('',#62206,10.) ;
#7566 = VECTOR('',#62211,10.) ;
#7567 = VECTOR('',#62212,10.) ;
#7568 = VECTOR('',#62215,10.) ;
#7569 = VECTOR('',#62216,10.) ;
#7570 = VECTOR('',#62219,10.) ;
#7571 = VECTOR('',#62220,10.) ;
#7572 = VECTOR('',#62225,10.) ;
#7573 = VECTOR('',#62226,10.) ;
#7574 = VECTOR('',#62229,10.) ;
#7575 = VECTOR('',#62230,10.) ;
#7576 = VECTOR('',#62233,10.) ;
#7577 = VECTOR('',#62234,10.) ;
#7578 = VECTOR('',#62237,10.) ;
#7579 = VECTOR('',#62240,10.) ;
#7580 = VECTOR('',#62263,2.) ;
#7581 = VECTOR('',#62272,10.) ;
#7582 = VECTOR('',#62275,10.) ;
#7583 = VECTOR('',#62280,10.) ;
#7584 = VECTOR('',#62283,10.) ;
#7585 = VECTOR('',#62286,10.) ;
#7586 = VECTOR('',#62289,10.) ;
#7587 = VECTOR('',#62292,10.) ;
#7588 = VECTOR('',#62295,10.) ;
#7589 = VECTOR('',#62298,10.) ;
#7590 = VECTOR('',#62301,10.) ;
#7591 = VECTOR('',#62304,10.) ;
#7592 = VECTOR('',#62307,10.) ;
#7593 = VECTOR('',#62312,10.) ;
#7594 = VECTOR('',#62313,10.) ;
#7595 = VECTOR('',#62318,10.) ;
#7596 = VECTOR('',#62319,10.) ;
#7597 = VECTOR('',#62322,10.) ;
#7598 = VECTOR('',#62323,10.) ;
#7599 = VECTOR('',#62328,10.) ;
#7600 = VECTOR('',#62329,10.) ;
#7601 = VECTOR('',#62334,10.) ;
#7602 = VECTOR('',#62335,10.) ;
#7603 = VECTOR('',#62340,10.) ;
#7604 = VECTOR('',#62341,10.) ;
#7605 = VECTOR('',#62344,10.) ;
#7606 = VECTOR('',#62345,10.) ;
#7607 = VECTOR('',#62346,10.) ;
#7608 = VECTOR('',#62349,10.) ;
#7609 = VECTOR('',#62350,10.) ;
#7610 = VECTOR('',#62353,10.) ;
#7611 = VECTOR('',#62354,10.) ;
#7612 = VECTOR('',#62357,10.) ;
#7613 = VECTOR('',#62358,10.) ;
#7614 = VECTOR('',#62361,10.) ;
#7615 = VECTOR('',#62362,10.) ;
#7616 = VECTOR('',#62365,10.) ;
#7617 = VECTOR('',#62366,10.) ;
#7618 = VECTOR('',#62373,10.) ;
#7619 = VECTOR('',#62376,10.) ;
#7620 = VECTOR('',#62381,10.) ;
#7621 = VECTOR('',#62384,10.) ;
#7622 = VECTOR('',#62387,10.) ;
#7623 = VECTOR('',#62390,10.) ;
#7624 = VECTOR('',#62393,10.) ;
#7625 = VECTOR('',#62396,10.) ;
#7626 = VECTOR('',#62399,10.) ;
#7627 = VECTOR('',#62404,10.) ;
#7628 = VECTOR('',#62409,10.) ;
#7629 = VECTOR('',#62414,10.) ;
#7630 = VECTOR('',#62419,10.) ;
#7631 = VECTOR('',#62424,10.) ;
#7632 = VECTOR('',#62429,10.) ;
#7633 = VECTOR('',#62430,10.) ;
#7634 = VECTOR('',#62435,10.) ;
#7635 = VECTOR('',#62436,10.) ;
#7636 = VECTOR('',#62439,10.) ;
#7637 = VECTOR('',#62442,10.) ;
#7638 = VECTOR('',#62445,10.) ;
#7639 = VECTOR('',#62454,10.) ;
#7640 = VECTOR('',#62457,10.) ;
#7641 = VECTOR('',#62464,10.) ;
#7642 = VECTOR('',#62467,10.) ;
#7643 = VECTOR('',#62472,10.) ;
#7644 = VECTOR('',#62475,10.) ;
#7645 = VECTOR('',#62478,10.) ;
#7646 = VECTOR('',#62481,10.) ;
#7647 = VECTOR('',#62484,10.) ;
#7648 = VECTOR('',#62487,10.) ;
#7649 = VECTOR('',#62490,10.) ;
#7650 = VECTOR('',#62493,10.) ;
#7651 = VECTOR('',#62496,10.) ;
#7652 = VECTOR('',#62497,10.) ;
#7653 = VECTOR('',#62502,10.) ;
#7654 = VECTOR('',#62503,10.) ;
#7655 = VECTOR('',#62508,10.) ;
#7656 = VECTOR('',#62509,10.) ;
#7657 = VECTOR('',#62514,10.) ;
#7658 = VECTOR('',#62515,10.) ;
#7659 = VECTOR('',#62520,10.) ;
#7660 = VECTOR('',#62521,10.) ;
#7661 = VECTOR('',#62526,10.) ;
#7662 = VECTOR('',#62527,10.) ;
#7663 = VECTOR('',#62532,10.) ;
#7664 = VECTOR('',#62533,10.) ;
#7665 = VECTOR('',#62536,10.) ;
#7666 = VECTOR('',#62537,10.) ;
#7667 = VECTOR('',#62538,10.) ;
#7668 = VECTOR('',#62541,10.) ;
#7669 = VECTOR('',#62542,10.) ;
#7670 = VECTOR('',#62545,10.) ;
#7671 = VECTOR('',#62546,10.) ;
#7672 = VECTOR('',#62549,10.) ;
#7673 = VECTOR('',#62550,10.) ;
#7674 = VECTOR('',#62553,10.) ;
#7675 = VECTOR('',#62554,10.) ;
#7676 = VECTOR('',#62557,10.) ;
#7677 = VECTOR('',#62558,10.) ;
#7678 = VECTOR('',#62573,2.49999999999999) ;
#7679 = VECTOR('',#62582,10.) ;
#7680 = VECTOR('',#62589,10.) ;
#7681 = VECTOR('',#62594,10.) ;
#7682 = VECTOR('',#62599,10.) ;
#7683 = VECTOR('',#62604,10.) ;
#7684 = VECTOR('',#62607,10.) ;
#7685 = VECTOR('',#62610,10.) ;
#7686 = VECTOR('',#62613,10.) ;
#7687 = VECTOR('',#62618,10.) ;
#7688 = VECTOR('',#62619,10.) ;
#7689 = VECTOR('',#62624,10.) ;
#7690 = VECTOR('',#62625,10.) ;
#7691 = VECTOR('',#62628,10.) ;
#7692 = VECTOR('',#62629,10.) ;
#7693 = VECTOR('',#62634,10.) ;
#7694 = VECTOR('',#62635,10.) ;
#7695 = VECTOR('',#62640,10.) ;
#7696 = VECTOR('',#62645,10.) ;
#7697 = VECTOR('',#62648,10.) ;
#7698 = VECTOR('',#62651,10.) ;
#7699 = VECTOR('',#62654,10.) ;
#7700 = VECTOR('',#62665,10.) ;
#7701 = VECTOR('',#62668,10.) ;
#7702 = VECTOR('',#62675,10.) ;
#7703 = VECTOR('',#62678,10.) ;
#7704 = VECTOR('',#62683,10.) ;
#7705 = VECTOR('',#62686,10.) ;
#7706 = VECTOR('',#62689,10.) ;
#7707 = VECTOR('',#62692,10.) ;
#7708 = VECTOR('',#62695,10.) ;
#7709 = VECTOR('',#62698,10.) ;
#7710 = VECTOR('',#62701,10.) ;
#7711 = VECTOR('',#62704,10.) ;
#7712 = VECTOR('',#62707,10.) ;
#7713 = VECTOR('',#62708,10.) ;
#7714 = VECTOR('',#62713,10.) ;
#7715 = VECTOR('',#62714,10.) ;
#7716 = VECTOR('',#62719,10.) ;
#7717 = VECTOR('',#62720,10.) ;
#7718 = VECTOR('',#62725,10.) ;
#7719 = VECTOR('',#62726,10.) ;
#7720 = VECTOR('',#62731,10.) ;
#7721 = VECTOR('',#62732,10.) ;
#7722 = VECTOR('',#62737,10.) ;
#7723 = VECTOR('',#62738,10.) ;
#7724 = VECTOR('',#62743,10.) ;
#7725 = VECTOR('',#62744,10.) ;
#7726 = VECTOR('',#62747,10.) ;
#7727 = VECTOR('',#62748,10.) ;
#7728 = VECTOR('',#62749,10.) ;
#7729 = VECTOR('',#62752,10.) ;
#7730 = VECTOR('',#62753,10.) ;
#7731 = VECTOR('',#62756,10.) ;
#7732 = VECTOR('',#62757,10.) ;
#7733 = VECTOR('',#62760,10.) ;
#7734 = VECTOR('',#62761,10.) ;
#7735 = VECTOR('',#62764,10.) ;
#7736 = VECTOR('',#62765,10.) ;
#7737 = VECTOR('',#62768,10.) ;
#7738 = VECTOR('',#62769,10.) ;
#7739 = VECTOR('',#62784,2.5) ;
#7740 = VECTOR('',#62793,10.) ;
#7741 = VECTOR('',#62800,10.) ;
#7742 = VECTOR('',#62805,10.) ;
#7743 = VECTOR('',#62810,10.) ;
#7744 = VECTOR('',#62815,10.) ;
#7745 = VECTOR('',#62818,10.) ;
#7746 = VECTOR('',#62821,10.) ;
#7747 = VECTOR('',#62824,10.) ;
#7748 = VECTOR('',#62829,10.) ;
#7749 = VECTOR('',#62830,10.) ;
#7750 = VECTOR('',#62835,10.) ;
#7751 = VECTOR('',#62836,10.) ;
#7752 = VECTOR('',#62839,10.) ;
#7753 = VECTOR('',#62840,10.) ;
#7754 = VECTOR('',#62845,10.) ;
#7755 = VECTOR('',#62846,10.) ;
#7756 = VECTOR('',#62851,10.) ;
#7757 = VECTOR('',#62856,10.) ;
#7758 = VECTOR('',#62859,10.) ;
#7759 = VECTOR('',#62862,10.) ;
#7760 = VECTOR('',#62865,10.) ;
#7761 = VECTOR('',#62876,10.) ;
#7762 = VECTOR('',#62879,10.) ;
#7763 = VECTOR('',#62902,10.) ;
#7764 = VECTOR('',#62903,10.) ;
#7765 = VECTOR('',#62914,10.) ;
#7766 = VECTOR('',#62915,10.) ;
#7767 = VECTOR('',#62936,10.) ;
#7768 = VECTOR('',#62937,10.) ;
#7769 = VECTOR('',#62940,10.) ;
#7770 = VECTOR('',#62941,10.) ;
#7771 = VECTOR('',#62952,10.) ;
#7772 = VECTOR('',#62953,10.) ;
#7773 = VECTOR('',#62956,10.) ;
#7774 = VECTOR('',#62957,10.) ;
#7775 = VECTOR('',#62978,10.) ;
#7776 = VECTOR('',#62979,10.) ;
#7777 = VECTOR('',#62982,10.) ;
#7778 = VECTOR('',#62983,10.) ;
#7779 = VECTOR('',#62986,10.) ;
#7780 = VECTOR('',#62987,10.) ;
#7781 = VECTOR('',#62990,10.) ;
#7782 = VECTOR('',#62991,10.) ;
#7783 = VECTOR('',#62994,10.) ;
#7784 = VECTOR('',#62995,10.) ;
#7785 = VECTOR('',#62998,10.) ;
#7786 = VECTOR('',#62999,10.) ;
#7787 = VECTOR('',#63028,10.) ;
#7788 = VECTOR('',#63029,10.) ;
#7789 = VECTOR('',#63032,10.) ;
#7790 = VECTOR('',#63033,10.) ;
#7791 = VECTOR('',#63046,10.) ;
#7792 = VECTOR('',#63047,10.) ;
#7793 = VECTOR('',#63050,10.) ;
#7794 = VECTOR('',#63051,10.) ;
#7795 = VECTOR('',#63058,10.) ;
#7796 = VECTOR('',#63059,10.) ;
#7797 = VECTOR('',#63064,10.) ;
#7798 = VECTOR('',#63065,10.) ;
#7799 = VECTOR('',#63070,10.) ;
#7800 = VECTOR('',#63071,10.) ;
#7801 = VECTOR('',#63074,10.) ;
#7802 = VECTOR('',#63077,10.) ;
#7803 = VECTOR('',#63078,10.) ;
#7804 = VECTOR('',#63079,10.) ;
#7805 = VECTOR('',#63082,10.) ;
#7806 = VECTOR('',#63103,10.) ;
#7807 = VECTOR('',#63104,10.) ;
#7808 = VECTOR('',#63105,10.) ;
#7809 = VECTOR('',#63106,10.) ;
#7810 = VECTOR('',#63107,10.) ;
#7811 = VECTOR('',#63108,10.) ;
#7812 = VECTOR('',#63109,10.) ;
#7813 = VECTOR('',#63110,10.) ;
#7814 = VECTOR('',#63111,10.) ;
#7815 = VECTOR('',#63114,10.) ;
#7816 = VECTOR('',#63115,10.) ;
#7817 = VECTOR('',#63116,10.) ;
#7818 = VECTOR('',#63119,10.) ;
#7819 = VECTOR('',#63120,10.) ;
#7820 = VECTOR('',#63123,10.) ;
#7821 = VECTOR('',#63124,10.) ;
#7822 = VECTOR('',#63125,10.) ;
#7823 = VECTOR('',#63126,10.) ;
#7824 = VECTOR('',#63129,10.) ;
#7825 = VECTOR('',#63130,10.) ;
#7826 = VECTOR('',#63131,10.) ;
#7827 = VECTOR('',#63132,10.) ;
#7828 = VECTOR('',#63133,10.) ;
#7829 = VECTOR('',#63134,10.) ;
#7830 = VECTOR('',#63135,10.) ;
#7831 = VECTOR('',#63138,10.) ;
#7832 = VECTOR('',#63139,10.) ;
#7833 = VECTOR('',#63140,10.) ;
#7834 = VECTOR('',#63143,10.) ;
#7835 = VECTOR('',#63144,10.) ;
#7836 = VECTOR('',#63145,10.) ;
#7837 = VECTOR('',#63148,10.) ;
#7838 = VECTOR('',#63149,10.) ;
#7839 = VECTOR('',#63150,9.99999999999999) ;
#7840 = VECTOR('',#63151,10.) ;
#7841 = VECTOR('',#63152,10.) ;
#7842 = VECTOR('',#63153,10.) ;
#7843 = VECTOR('',#63154,10.) ;
#7844 = VECTOR('',#63155,10.) ;
#7845 = VECTOR('',#63156,10.) ;
#7846 = VECTOR('',#63157,10.) ;
#7847 = VECTOR('',#63160,10.) ;
#7848 = VECTOR('',#63161,10.) ;
#7849 = VECTOR('',#63162,10.) ;
#7850 = VECTOR('',#63165,10.) ;
#7851 = VECTOR('',#63166,10.) ;
#7852 = VECTOR('',#63167,10.) ;
#7853 = VECTOR('',#63170,10.) ;
#7854 = VECTOR('',#63171,10.) ;
#7855 = VECTOR('',#63176,10.) ;
#7856 = VECTOR('',#63177,10.) ;
#7857 = VECTOR('',#63180,10.) ;
#7858 = VECTOR('',#63183,10.) ;
#7859 = VECTOR('',#63186,10.) ;
#7860 = VECTOR('',#63191,10.) ;
#7861 = VECTOR('',#63194,10.) ;
#7862 = VECTOR('',#63197,10.) ;
#7863 = VECTOR('',#63200,10.) ;
#7864 = VECTOR('',#63203,10.) ;
#7865 = VECTOR('',#63206,10.) ;
#7866 = VECTOR('',#63207,10.) ;
#7867 = VECTOR('',#63210,10.) ;
#7868 = VECTOR('',#63213,10.) ;
#7869 = VECTOR('',#63214,10.) ;
#7870 = VECTOR('',#63227,10.) ;
#7871 = VECTOR('',#63228,10.) ;
#7872 = VECTOR('',#63239,10.) ;
#7873 = VECTOR('',#63240,10.) ;
#7874 = VECTOR('',#63245,10.) ;
#7875 = VECTOR('',#63246,10.) ;
#7876 = VECTOR('',#63247,10.) ;
#7877 = VECTOR('',#63248,10.) ;
#7878 = VECTOR('',#63249,10.) ;
#7879 = VECTOR('',#63252,10.) ;
#7880 = VECTOR('',#63257,10.) ;
#7881 = VECTOR('',#63258,10.) ;
#7882 = VECTOR('',#63269,10.) ;
#7883 = VECTOR('',#63270,10.) ;
#7884 = VECTOR('',#63281,10.) ;
#7885 = VECTOR('',#63282,10.) ;
#7886 = VECTOR('',#63291,10.) ;
#7887 = VECTOR('',#63292,10.) ;
#7888 = VECTOR('',#63293,10.) ;
#7889 = VECTOR('',#63296,10.) ;
#7890 = VECTOR('',#63301,10.) ;
#7891 = VECTOR('',#63302,10.) ;
#7892 = VECTOR('',#63303,10.) ;
#7893 = VECTOR('',#63308,10.) ;
#7894 = VECTOR('',#63313,10.) ;
#7895 = VECTOR('',#63316,10.) ;
#7896 = VECTOR('',#63317,10.) ;
#7897 = VECTOR('',#63318,10.) ;
#7898 = VECTOR('',#63319,10.) ;
#7899 = VECTOR('',#63322,10.) ;
#7900 = VECTOR('',#63325,10.) ;
#7901 = VECTOR('',#63340,10.) ;
#7902 = VECTOR('',#63341,10.) ;
#7903 = VECTOR('',#63350,10.) ;
#7904 = VECTOR('',#63353,10.) ;
#7905 = VECTOR('',#63356,10.) ;
#7906 = VECTOR('',#63357,10.) ;
#7907 = VECTOR('',#63362,10.) ;
#7908 = VECTOR('',#63379,10.) ;
#7909 = VECTOR('',#63380,10.) ;
#7910 = VECTOR('',#63389,10.) ;
#7911 = VECTOR('',#63390,10.) ;
#7912 = VECTOR('',#63393,10.) ;
#7913 = VECTOR('',#63396,10.) ;
#7914 = VECTOR('',#63397,10.) ;
#7915 = VECTOR('',#63398,10.) ;
#7916 = VECTOR('',#63399,10.) ;
#7917 = VECTOR('',#63402,10.) ;
#7918 = VECTOR('',#63403,10.) ;
#7919 = VECTOR('',#63406,10.) ;
#7920 = VECTOR('',#63411,10.) ;
#7921 = VECTOR('',#63414,10.) ;
#7922 = VECTOR('',#63423,10.) ;
#7923 = VECTOR('',#63426,10.) ;
#7924 = VECTOR('',#63429,10.) ;
#7925 = VECTOR('',#63430,10.) ;
#7926 = VECTOR('',#63433,10.) ;
#7927 = VECTOR('',#63436,10.) ;
#7928 = VECTOR('',#63437,10.) ;
#7929 = VECTOR('',#63438,10.) ;
#7930 = VECTOR('',#63439,10.) ;
#7931 = VECTOR('',#63442,10.) ;
#7932 = VECTOR('',#63445,10.) ;
#7933 = VECTOR('',#63448,10.) ;
#7934 = VECTOR('',#63453,10.) ;
#7935 = VECTOR('',#63458,10.) ;
#7936 = VECTOR('',#63461,10.) ;
#7937 = VECTOR('',#63464,10.) ;
#7938 = VECTOR('',#63467,10.) ;
#7939 = VECTOR('',#63478,10.) ;
#7940 = VECTOR('',#63479,10.) ;
#7941 = VECTOR('',#63482,10.) ;
#7942 = VECTOR('',#63485,10.) ;
#7943 = VECTOR('',#63486,10.) ;
#7944 = VECTOR('',#63489,10.) ;
#7945 = VECTOR('',#63494,10.) ;
#7946 = VECTOR('',#63495,10.) ;
#7947 = VECTOR('',#63496,10.) ;
#7948 = VECTOR('',#63497,10.) ;
#7949 = VECTOR('',#63498,10.) ;
#7950 = VECTOR('',#63511,10.) ;
#7951 = VECTOR('',#63514,10.) ;
#7952 = VECTOR('',#63517,10.) ;
#7953 = VECTOR('',#63520,10.) ;
#7954 = VECTOR('',#63521,10.) ;
#7955 = VECTOR('',#63522,10.) ;
#7956 = VECTOR('',#63541,10.) ;
#7957 = VECTOR('',#63558,10.) ;
#7958 = VECTOR('',#63571,10.) ;
#7959 = VECTOR('',#63572,10.) ;
#7960 = VECTOR('',#63583,10.) ;
#7961 = VECTOR('',#63586,10.) ;
#7962 = VECTOR('',#63587,10.) ;
#7963 = VECTOR('',#63588,10.) ;
#7964 = VECTOR('',#63589,10.) ;
#7965 = VECTOR('',#63590,10.) ;
#7966 = VECTOR('',#63591,10.) ;
#7967 = VECTOR('',#63594,10.) ;
#7968 = VECTOR('',#63599,10.) ;
#7969 = VECTOR('',#63602,10.) ;
#7970 = VECTOR('',#63603,10.) ;
#7971 = VECTOR('',#63604,10.) ;
#7972 = VECTOR('',#63621,10.) ;
#7973 = VECTOR('',#63622,10.) ;
#7974 = VECTOR('',#63635,10.) ;
#7975 = VECTOR('',#63636,10.) ;
#7976 = VECTOR('',#63657,10.) ;
#7977 = VECTOR('',#63658,10.) ;
#7978 = VECTOR('',#63669,10.) ;
#7979 = VECTOR('',#63670,10.) ;
#7980 = VECTOR('',#63675,10.) ;
#7981 = VECTOR('',#63676,10.) ;
#7982 = VECTOR('',#63685,10.) ;
#7983 = VECTOR('',#63688,10.) ;
#7984 = VECTOR('',#63691,10.) ;
#7985 = VECTOR('',#63692,10.) ;
#7986 = VECTOR('',#63693,10.) ;
#7987 = VECTOR('',#63702,10.) ;
#7988 = VECTOR('',#63707,10.) ;
#7989 = VECTOR('',#63708,10.) ;
#7990 = VECTOR('',#63713,10.) ;
#7991 = VECTOR('',#63716,10.) ;
#7992 = VECTOR('',#63723,10.) ;
#7993 = VECTOR('',#63728,10.) ;
#7994 = VECTOR('',#63731,10.) ;
#7995 = VECTOR('',#63734,10.) ;
#7996 = VECTOR('',#63735,10.) ;
#7997 = VECTOR('',#63736,0.999999999999996) ;
#7998 = VECTOR('',#63751,10.) ;
#7999 = VECTOR('',#63760,10.) ;
#8000 = VECTOR('',#63773,10.) ;
#8001 = VECTOR('',#63774,10.) ;
#8002 = VECTOR('',#63791,10.) ;
#8003 = VECTOR('',#63802,10.) ;
#8004 = VECTOR('',#63815,9.99999999999999) ;
#8005 = VECTOR('',#63816,9.99999999999999) ;
#8006 = VECTOR('',#63825,10.) ;
#8007 = VECTOR('',#63830,10.) ;
#8008 = VECTOR('',#63831,10.) ;
#8009 = VECTOR('',#63834,10.) ;
#8010 = VECTOR('',#63839,10.) ;
#8011 = VECTOR('',#63840,10.) ;
#8012 = VECTOR('',#63841,10.) ;
#8013 = VECTOR('',#63842,10.) ;
#8014 = VECTOR('',#63845,10.) ;
#8015 = VECTOR('',#63852,10.) ;
#8016 = VECTOR('',#63865,10.) ;
#8017 = VECTOR('',#63866,10.) ;
#8018 = VECTOR('',#63885,10.) ;
#8019 = VECTOR('',#63888,10.) ;
#8020 = VECTOR('',#63891,10.) ;
#8021 = VECTOR('',#63892,10.) ;
#8022 = VECTOR('',#63893,10.) ;
#8023 = VECTOR('',#63894,10.) ;
#8024 = VECTOR('',#63899,10.) ;
#8025 = VECTOR('',#63902,10.) ;
#8026 = VECTOR('',#63909,10.) ;
#8027 = VECTOR('',#63916,10.) ;
#8028 = VECTOR('',#63921,10.) ;
#8029 = VECTOR('',#63924,10.) ;
#8030 = VECTOR('',#63927,10.) ;
#8031 = VECTOR('',#63930,10.) ;
#8032 = VECTOR('',#63931,10.) ;
#8033 = VECTOR('',#63950,10.) ;
#8034 = VECTOR('',#63951,10.) ;
#8035 = VECTOR('',#63954,10.) ;
#8036 = VECTOR('',#63955,10.) ;
#8037 = VECTOR('',#63956,10.) ;
#8038 = VECTOR('',#63957,10.) ;
#8039 = VECTOR('',#63958,10.) ;
#8040 = VECTOR('',#63961,10.) ;
#8041 = VECTOR('',#63966,10.) ;
#8042 = VECTOR('',#63969,10.) ;
#8043 = VECTOR('',#63980,10.) ;
#8044 = VECTOR('',#63981,10.) ;
#8045 = VECTOR('',#63984,10.) ;
#8046 = VECTOR('',#63985,10.) ;
#8047 = VECTOR('',#63998,10.) ;
#8048 = VECTOR('',#63999,10.) ;
#8049 = VECTOR('',#64002,10.) ;
#8050 = VECTOR('',#64003,10.) ;
#8051 = VECTOR('',#64006,10.) ;
#8052 = VECTOR('',#64007,10.) ;
#8053 = VECTOR('',#64010,10.) ;
#8054 = VECTOR('',#64013,10.) ;
#8055 = VECTOR('',#64016,10.) ;
#8056 = VECTOR('',#64019,10.) ;
#8057 = VECTOR('',#64022,10.) ;
#8058 = VECTOR('',#64023,10.) ;
#8059 = VECTOR('',#64024,10.) ;
#8060 = VECTOR('',#64025,10.) ;
#8061 = VECTOR('',#64026,10.) ;
#8062 = VECTOR('',#64029,10.) ;
#8063 = VECTOR('',#64032,10.) ;
#8064 = VECTOR('',#64035,10.) ;
#8065 = VECTOR('',#64038,10.) ;
#8066 = VECTOR('',#64041,10.) ;
#8067 = VECTOR('',#64044,10.) ;
#8068 = VECTOR('',#64045,10.) ;
#8069 = VECTOR('',#64046,10.) ;
#8070 = VECTOR('',#64049,10.) ;
#8071 = VECTOR('',#64052,10.) ;
#8072 = VECTOR('',#64055,10.) ;
#8073 = VECTOR('',#64058,10.) ;
#8074 = VECTOR('',#64061,10.) ;
#8075 = VECTOR('',#64062,10.) ;
#8076 = VECTOR('',#64063,10.) ;
#8077 = VECTOR('',#64064,10.) ;
#8078 = VECTOR('',#64065,10.) ;
#8079 = VECTOR('',#64066,10.) ;
#8080 = VECTOR('',#64067,10.) ;
#8081 = VECTOR('',#64068,10.) ;
#8082 = VECTOR('',#64069,10.) ;
#8083 = VECTOR('',#64070,10.) ;
#8084 = VECTOR('',#64073,10.) ;
#8085 = VECTOR('',#64076,10.) ;
#8086 = VECTOR('',#64077,10.) ;
#8087 = VECTOR('',#64080,9.99999999999999) ;
#8088 = VECTOR('',#64081,10.) ;
#8089 = VECTOR('',#64084,10.) ;
#8090 = VECTOR('',#64085,10.) ;
#8091 = VECTOR('',#64086,10.) ;
#8092 = VECTOR('',#64087,10.) ;
#8093 = VECTOR('',#64096,10.) ;
#8094 = VECTOR('',#64099,10.) ;
#8095 = VECTOR('',#64100,10.) ;
#8096 = VECTOR('',#64103,10.) ;
#8097 = VECTOR('',#64106,10.) ;
#8098 = VECTOR('',#64107,10.) ;
#8099 = VECTOR('',#64110,10.) ;
#8100 = VECTOR('',#64113,10.) ;
#8101 = VECTOR('',#64114,10.) ;
#8102 = VECTOR('',#64115,10.) ;
#8103 = VECTOR('',#64118,10.) ;
#8104 = VECTOR('',#64121,10.) ;
#8105 = VECTOR('',#64124,10.) ;
#8106 = VECTOR('',#64127,10.) ;
#8107 = VECTOR('',#64128,10.) ;
#8108 = VECTOR('',#64133,10.) ;
#8109 = VECTOR('',#64136,10.) ;
#8110 = VECTOR('',#64137,10.) ;
#8111 = VECTOR('',#64140,10.) ;
#8112 = VECTOR('',#64145,10.) ;
#8113 = VECTOR('',#64146,10.) ;
#8114 = VECTOR('',#64149,10.) ;
#8115 = VECTOR('',#64152,10.) ;
#8116 = VECTOR('',#64155,10.) ;
#8117 = VECTOR('',#64158,10.) ;
#8118 = VECTOR('',#64163,10.) ;
#8119 = VECTOR('',#64166,10.) ;
#8120 = VECTOR('',#64167,10.) ;
#8121 = VECTOR('',#64170,10.) ;
#8122 = VECTOR('',#64173,10.) ;
#8123 = VECTOR('',#64176,10.) ;
#8124 = VECTOR('',#64179,10.) ;
#8125 = VECTOR('',#64180,10.) ;
#8126 = VECTOR('',#64183,10.) ;
#8127 = VECTOR('',#64184,10.) ;
#8128 = VECTOR('',#64187,10.) ;
#8129 = VECTOR('',#64190,10.) ;
#8130 = VECTOR('',#64193,10.) ;
#8131 = VECTOR('',#64196,10.) ;
#8132 = VECTOR('',#64197,10.) ;
#8133 = VECTOR('',#64198,10.) ;
#8134 = VECTOR('',#64199,10.) ;
#8135 = VECTOR('',#64202,10.) ;
#8136 = VECTOR('',#64205,10.) ;
#8137 = VECTOR('',#64208,10.) ;
#8138 = VECTOR('',#64211,10.) ;
#8139 = VECTOR('',#64212,10.) ;
#8140 = VECTOR('',#64215,10.) ;
#8141 = VECTOR('',#64218,10.) ;
#8142 = VECTOR('',#64219,10.) ;
#8143 = VECTOR('',#64222,10.) ;
#8144 = VECTOR('',#64225,10.) ;
#8145 = VECTOR('',#64228,10.) ;
#8146 = VECTOR('',#64231,10.) ;
#8147 = VECTOR('',#64232,10.) ;
#8148 = VECTOR('',#64241,10.) ;
#8149 = VECTOR('',#64242,10.) ;
#8150 = VECTOR('',#64257,10.) ;
#8151 = VECTOR('',#64260,10.) ;
#8152 = VECTOR('',#64263,10.) ;
#8153 = VECTOR('',#64266,10.) ;
#8154 = VECTOR('',#64269,10.) ;
#8155 = VECTOR('',#64270,10.) ;
#8156 = VECTOR('',#64271,10.) ;
#8157 = VECTOR('',#64272,10.) ;
#8158 = VECTOR('',#64275,10.) ;
#8159 = VECTOR('',#64276,10.) ;
#8160 = VECTOR('',#64277,10.) ;
#8161 = VECTOR('',#64278,10.) ;
#8162 = VECTOR('',#64289,10.) ;
#8163 = VECTOR('',#64292,10.) ;
#8164 = VECTOR('',#64305,10.) ;
#8165 = VECTOR('',#64306,10.) ;
#8166 = VECTOR('',#64317,10.) ;
#8167 = VECTOR('',#64318,10.) ;
#8168 = VECTOR('',#64321,10.) ;
#8169 = VECTOR('',#64324,10.) ;
#8170 = VECTOR('',#64335,10.) ;
#8171 = VECTOR('',#64336,10.) ;
#8172 = VECTOR('',#64359,10.) ;
#8173 = VECTOR('',#64368,10.) ;
#8174 = VECTOR('',#64371,10.) ;
#8175 = VECTOR('',#64372,10.) ;
#8176 = VECTOR('',#64377,10.) ;
#8177 = VECTOR('',#64388,10.) ;
#8178 = VECTOR('',#64391,10.) ;
#8179 = VECTOR('',#64392,10.) ;
#8180 = VECTOR('',#64397,10.) ;
#8181 = VECTOR('',#64398,10.) ;
#8182 = VECTOR('',#64399,10.) ;
#8183 = VECTOR('',#64404,10.) ;
#8184 = VECTOR('',#64409,10.) ;
#8185 = VECTOR('',#64410,10.) ;
#8186 = VECTOR('',#64413,10.) ;
#8187 = VECTOR('',#64418,10.) ;
#8188 = VECTOR('',#64419,9.99999999999999) ;
#8189 = VECTOR('',#64422,10.) ;
#8190 = VECTOR('',#64425,10.) ;
#8191 = VECTOR('',#64428,10.) ;
#8192 = VECTOR('',#64431,10.) ;
#8193 = VECTOR('',#64436,10.) ;
#8194 = VECTOR('',#64437,10.) ;
#8195 = VECTOR('',#64440,0.999999999999996) ;
#8196 = VECTOR('',#64457,10.) ;
#8197 = VECTOR('',#64458,10.) ;
#8198 = VECTOR('',#64473,10.) ;
#8199 = VECTOR('',#64474,10.) ;
#8200 = VECTOR('',#64505,10.) ;
#8201 = VECTOR('',#64506,10.) ;
#8202 = VECTOR('',#64511,10.) ;
#8203 = VECTOR('',#64512,10.) ;
#8204 = VECTOR('',#64521,10.) ;
#8205 = VECTOR('',#64526,10.) ;
#8206 = VECTOR('',#64527,10.) ;
#8207 = VECTOR('',#64538,10.) ;
#8208 = VECTOR('',#64547,10.) ;
#8209 = VECTOR('',#64552,10.) ;
#8210 = VECTOR('',#64553,10.) ;
#8211 = VECTOR('',#64558,10.) ;
#8212 = VECTOR('',#64559,10.) ;
#8213 = VECTOR('',#64572,10.) ;
#8214 = VECTOR('',#64573,10.) ;
#8215 = VECTOR('',#64586,10.) ;
#8216 = VECTOR('',#64587,10.) ;
#8217 = VECTOR('',#64600,10.) ;
#8218 = VECTOR('',#64601,10.) ;
#8219 = VECTOR('',#64612,10.) ;
#8220 = VECTOR('',#64613,10.) ;
#8221 = VECTOR('',#64618,10.) ;
#8222 = VECTOR('',#64619,10.) ;
#8223 = VECTOR('',#64628,10.) ;
#8224 = VECTOR('',#64629,10.) ;
#8225 = VECTOR('',#64634,10.) ;
#8226 = VECTOR('',#64637,10.) ;
#8227 = VECTOR('',#64640,10.) ;
#8228 = VECTOR('',#64643,10.) ;
#8229 = VECTOR('',#64646,10.) ;
#8230 = VECTOR('',#64647,10.) ;
#8231 = VECTOR('',#64650,10.) ;
#8232 = VECTOR('',#64653,10.) ;
#8233 = VECTOR('',#64656,10.) ;
#8234 = VECTOR('',#64659,10.) ;
#8235 = VECTOR('',#64662,10.) ;
#8236 = VECTOR('',#64663,10.) ;
#8237 = VECTOR('',#64664,10.) ;
#8238 = VECTOR('',#64667,10.) ;
#8239 = VECTOR('',#64670,10.) ;
#8240 = VECTOR('',#64671,10.) ;
#8241 = VECTOR('',#64672,10.) ;
#8242 = VECTOR('',#64675,10.) ;
#8243 = VECTOR('',#64678,10.) ;
#8244 = VECTOR('',#64685,10.) ;
#8245 = VECTOR('',#64688,10.) ;
#8246 = VECTOR('',#64691,10.) ;
#8247 = VECTOR('',#64692,10.) ;
#8248 = VECTOR('',#64693,10.) ;
#8249 = VECTOR('',#64700,10.) ;
#8250 = VECTOR('',#64723,10.) ;
#8251 = VECTOR('',#64724,10.) ;
#8252 = VECTOR('',#64729,10.) ;
#8253 = VECTOR('',#64732,10.) ;
#8254 = VECTOR('',#64743,10.) ;
#8255 = VECTOR('',#64744,10.) ;
#8256 = VECTOR('',#64749,10.) ;
#8257 = VECTOR('',#64750,10.) ;
#8258 = VECTOR('',#64755,10.) ;
#8259 = VECTOR('',#64756,10.) ;
#8260 = VECTOR('',#64761,10.) ;
#8261 = VECTOR('',#64762,10.) ;
#8262 = VECTOR('',#64775,10.) ;
#8263 = VECTOR('',#64776,10.) ;
#8264 = VECTOR('',#64779,10.) ;
#8265 = VECTOR('',#64782,10.) ;
#8266 = VECTOR('',#64785,10.) ;
#8267 = VECTOR('',#64786,10.) ;
#8268 = VECTOR('',#64789,10.) ;
#8269 = VECTOR('',#64790,10.) ;
#8270 = VECTOR('',#64793,10.) ;
#8271 = VECTOR('',#64796,10.) ;
#8272 = VECTOR('',#64799,10.) ;
#8273 = VECTOR('',#64802,10.) ;
#8274 = VECTOR('',#64807,10.) ;
#8275 = VECTOR('',#64808,10.) ;
#8276 = VECTOR('',#64809,10.) ;
#8277 = VECTOR('',#64810,10.) ;
#8278 = VECTOR('',#64811,10.) ;
#8279 = VECTOR('',#64812,10.) ;
#8280 = VECTOR('',#64813,10.) ;
#8281 = VECTOR('',#64818,10.) ;
#8282 = VECTOR('',#64827,10.) ;
#8283 = VECTOR('',#64838,10.) ;
#8284 = VECTOR('',#64849,10.) ;
#8285 = VECTOR('',#64860,10.) ;
#8286 = VECTOR('',#64871,10.) ;
#8287 = VECTOR('',#64882,9.99999999999999) ;
#8288 = VECTOR('',#64891,10.) ;
#8289 = VECTOR('',#64920,10.) ;
#8290 = VECTOR('',#64937,10.) ;
#8291 = VECTOR('',#64952,10.) ;
#8292 = VECTOR('',#64953,10.) ;
#8293 = VECTOR('',#64960,10.) ;
#8294 = VECTOR('',#64963,10.) ;
#8295 = VECTOR('',#64966,10.) ;
#8296 = VECTOR('',#64969,10.) ;
#8297 = VECTOR('',#64976,10.) ;
#8298 = VECTOR('',#64983,10.) ;
#8299 = VECTOR('',#64994,10.) ;
#8300 = VECTOR('',#65005,10.) ;
#8301 = VECTOR('',#65024,10.) ;
#8302 = VECTOR('',#65033,10.) ;
#8303 = VECTOR('',#65040,10.) ;
#8304 = VECTOR('',#65043,10.) ;
#8305 = VECTOR('',#65056,10.) ;
#8306 = VECTOR('',#65067,10.) ;
#8307 = VECTOR('',#65076,10.) ;
#8308 = VECTOR('',#65081,10.) ;
#8309 = VECTOR('',#65086,10.) ;
#8310 = VECTOR('',#65089,10.) ;
#8311 = VECTOR('',#65092,10.) ;
#8312 = VECTOR('',#65095,10.) ;
#8313 = VECTOR('',#65096,10.) ;
#8314 = VECTOR('',#65097,10.) ;
#8315 = VECTOR('',#65098,10.) ;
#8316 = VECTOR('',#65099,10.) ;
#8317 = VECTOR('',#65100,10.) ;
#8318 = VECTOR('',#65101,10.) ;
#8319 = VECTOR('',#65102,10.) ;
#8320 = VECTOR('',#65103,10.) ;
#8321 = VECTOR('',#65104,10.) ;
#8322 = VECTOR('',#65107,10.) ;
#8323 = VECTOR('',#65112,10.) ;
#8324 = VECTOR('',#65113,10.) ;
#8325 = VECTOR('',#65118,10.) ;
#8326 = VECTOR('',#65119,10.) ;
#8327 = VECTOR('',#65120,10.) ;
#8328 = VECTOR('',#65127,10.) ;
#8329 = VECTOR('',#65132,10.) ;
#8330 = VECTOR('',#65133,10.) ;
#8331 = VECTOR('',#65134,10.) ;
#8332 = VECTOR('',#65135,10.) ;
#8333 = VECTOR('',#65138,10.) ;
#8334 = VECTOR('',#65139,10.) ;
#8335 = VECTOR('',#65158,10.) ;
#8336 = VECTOR('',#65161,10.) ;
#8337 = VECTOR('',#65174,9.99999999999999) ;
#8338 = VECTOR('',#65175,9.99999999999999) ;
#8339 = VECTOR('',#65180,10.) ;
#8340 = VECTOR('',#65181,10.) ;
#8341 = VECTOR('',#65184,10.) ;
#8342 = VECTOR('',#65185,10.) ;
#8343 = VECTOR('',#65190,10.) ;
#8344 = VECTOR('',#65191,10.) ;
#8345 = VECTOR('',#65196,9.99999999999999) ;
#8346 = VECTOR('',#65197,10.) ;
#8347 = VECTOR('',#65204,10.) ;
#8348 = VECTOR('',#65207,10.) ;
#8349 = VECTOR('',#65210,10.) ;
#8350 = VECTOR('',#65213,10.) ;
#8351 = VECTOR('',#65216,10.) ;
#8352 = VECTOR('',#65219,10.) ;
#8353 = VECTOR('',#65226,10.) ;
#8354 = VECTOR('',#65229,10.) ;
#8355 = VECTOR('',#65236,10.) ;
#8356 = VECTOR('',#65239,10.) ;
#8357 = VECTOR('',#65244,10.) ;
#8358 = VECTOR('',#65245,10.) ;
#8359 = VECTOR('',#65246,10.) ;
#8360 = VECTOR('',#65247,10.) ;
#8361 = VECTOR('',#65248,10.) ;
#8362 = VECTOR('',#65251,10.) ;
#8363 = VECTOR('',#65252,10.) ;
#8364 = VECTOR('',#65255,10.) ;
#8365 = VECTOR('',#65256,10.) ;
#8366 = VECTOR('',#65275,10.) ;
#8367 = VECTOR('',#65278,10.) ;
#8368 = VECTOR('',#65279,10.) ;
#8369 = VECTOR('',#65282,10.) ;
#8370 = VECTOR('',#65293,10.) ;
#8371 = VECTOR('',#65294,10.) ;
#8372 = VECTOR('',#65305,10.) ;
#8373 = VECTOR('',#65308,10.) ;
#8374 = VECTOR('',#65309,10.) ;
#8375 = VECTOR('',#65310,10.) ;
#8376 = VECTOR('',#65313,10.) ;
#8377 = VECTOR('',#65314,10.) ;
#8378 = VECTOR('',#65315,10.) ;
#8379 = VECTOR('',#65318,10.) ;
#8380 = VECTOR('',#65319,10.) ;
#8381 = VECTOR('',#65320,10.) ;
#8382 = VECTOR('',#65323,10.) ;
#8383 = VECTOR('',#65324,10.) ;
#8384 = VECTOR('',#65325,10.) ;
#8385 = VECTOR('',#65326,9.99999999999999) ;
#8386 = VECTOR('',#65327,10.) ;
#8387 = VECTOR('',#65328,10.) ;
#8388 = VECTOR('',#65329,10.) ;
#8389 = VECTOR('',#65332,10.) ;
#8390 = VECTOR('',#65333,10.) ;
#8391 = VECTOR('',#65334,10.) ;
#8392 = VECTOR('',#65335,9.99999999999999) ;
#8393 = VECTOR('',#65336,10.) ;
#8394 = VECTOR('',#65337,10.) ;
#8395 = VECTOR('',#65340,10.) ;
#8396 = VECTOR('',#65341,10.) ;
#8397 = VECTOR('',#65342,10.) ;
#8398 = VECTOR('',#65343,10.) ;
#8399 = VECTOR('',#65344,10.) ;
#8400 = VECTOR('',#65349,10.) ;
#8401 = VECTOR('',#65354,10.) ;
#8402 = VECTOR('',#65365,9.99999999999999) ;
#8403 = VECTOR('',#65370,10.) ;
#8404 = VECTOR('',#65373,10.) ;
#8405 = VECTOR('',#65378,10.) ;
#8406 = VECTOR('',#65381,10.) ;
#8407 = VECTOR('',#65384,10.) ;
#8408 = VECTOR('',#65389,10.) ;
#8409 = VECTOR('',#65390,10.) ;
#8410 = VECTOR('',#65393,10.) ;
#8411 = VECTOR('',#65394,10.) ;
#8412 = VECTOR('',#65397,10.) ;
#8413 = VECTOR('',#65400,10.) ;
#8414 = VECTOR('',#65403,10.) ;
#8415 = VECTOR('',#65410,10.) ;
#8416 = VECTOR('',#65413,10.) ;
#8417 = VECTOR('',#65418,10.) ;
#8418 = VECTOR('',#65419,10.) ;
#8419 = VECTOR('',#65420,10.) ;
#8420 = VECTOR('',#65421,10.) ;
#8421 = VECTOR('',#65422,10.) ;
#8422 = VECTOR('',#65427,10.) ;
#8423 = VECTOR('',#65430,10.) ;
#8424 = VECTOR('',#65431,10.) ;
#8425 = VECTOR('',#65432,10.) ;
#8426 = VECTOR('',#65437,10.) ;
#8427 = VECTOR('',#65442,10.) ;
#8428 = VECTOR('',#65447,10.) ;
#8429 = VECTOR('',#65448,10.) ;
#8430 = VECTOR('',#65451,10.) ;
#8431 = VECTOR('',#65452,10.) ;
#8432 = VECTOR('',#65455,9.99999999999999) ;
#8433 = VECTOR('',#65458,9.99999999999999) ;
#8434 = VECTOR('',#65459,10.) ;
#8435 = VECTOR('',#65462,10.) ;
#8436 = VECTOR('',#65465,10.) ;
#8437 = VECTOR('',#65466,10.) ;
#8438 = VECTOR('',#65485,9.99999999999999) ;
#8439 = VECTOR('',#65488,10.) ;
#8440 = VECTOR('',#65489,10.) ;
#8441 = VECTOR('',#65490,10.) ;
#8442 = VECTOR('',#65493,10.) ;
#8443 = VECTOR('',#65494,10.) ;
#8444 = VECTOR('',#65495,10.) ;
#8445 = VECTOR('',#65498,10.) ;
#8446 = VECTOR('',#65499,10.) ;
#8447 = VECTOR('',#65502,10.) ;
#8448 = VECTOR('',#65505,10.) ;
#8449 = VECTOR('',#65508,10.) ;
#8450 = VECTOR('',#65513,10.) ;
#8451 = VECTOR('',#65514,10.) ;
#8452 = VECTOR('',#65519,10.) ;
#8453 = VECTOR('',#65520,10.) ;
#8454 = VECTOR('',#65523,10.) ;
#8455 = VECTOR('',#65524,10.) ;
#8456 = VECTOR('',#65529,10.) ;
#8457 = VECTOR('',#65530,10.) ;
#8458 = VECTOR('',#65535,10.) ;
#8459 = VECTOR('',#65536,10.) ;
#8460 = VECTOR('',#65539,10.) ;
#8461 = VECTOR('',#65540,10.) ;
#8462 = VECTOR('',#65541,10.) ;
#8463 = VECTOR('',#65544,10.) ;
#8464 = VECTOR('',#65545,10.) ;
#8465 = VECTOR('',#65548,10.) ;
#8466 = VECTOR('',#65549,10.) ;
#8467 = VECTOR('',#65552,10.) ;
#8468 = VECTOR('',#65553,10.) ;
#8469 = VECTOR('',#65558,10.) ;
#8470 = VECTOR('',#65561,10.) ;
#8471 = VECTOR('',#65564,10.) ;
#8472 = VECTOR('',#65567,10.) ;
#8473 = VECTOR('',#65570,10.) ;
#8474 = VECTOR('',#65571,10.) ;
#8475 = VECTOR('',#65576,10.) ;
#8476 = VECTOR('',#65577,10.) ;
#8477 = VECTOR('',#65580,10.) ;
#8478 = VECTOR('',#65581,10.) ;
#8479 = VECTOR('',#65584,10.) ;
#8480 = VECTOR('',#65585,10.) ;
#8481 = VECTOR('',#65586,10.) ;
#8482 = VECTOR('',#65587,10.) ;
#8483 = VECTOR('',#65590,10.) ;
#8484 = VECTOR('',#65591,10.) ;
#8485 = VECTOR('',#65592,10.) ;
#8486 = VECTOR('',#65597,10.) ;
#8487 = VECTOR('',#65600,10.) ;
#8488 = VECTOR('',#65605,10.) ;
#8489 = VECTOR('',#65608,10.) ;
#8490 = VECTOR('',#65611,9.99999999999999) ;
#8491 = VECTOR('',#65614,9.99999999999999) ;
#8492 = VECTOR('',#65617,10.) ;
#8493 = VECTOR('',#65618,10.) ;
#8494 = VECTOR('',#65623,10.) ;
#8495 = VECTOR('',#65624,10.) ;
#8496 = VECTOR('',#65629,10.) ;
#8497 = VECTOR('',#65630,10.) ;
#8498 = VECTOR('',#65635,10.) ;
#8499 = VECTOR('',#65636,10.) ;
#8500 = VECTOR('',#65639,10.) ;
#8501 = VECTOR('',#65640,10.) ;
#8502 = VECTOR('',#65641,10.) ;
#8503 = VECTOR('',#65644,10.) ;
#8504 = VECTOR('',#65645,10.) ;
#8505 = VECTOR('',#65648,10.) ;
#8506 = VECTOR('',#65649,10.) ;
#8507 = VECTOR('',#65652,10.) ;
#8508 = VECTOR('',#65653,10.) ;
#8509 = VECTOR('',#65658,10.) ;
#8510 = VECTOR('',#65661,10.) ;
#8511 = VECTOR('',#65666,10.) ;
#8512 = VECTOR('',#65667,10.) ;
#8513 = VECTOR('',#65672,10.) ;
#8514 = VECTOR('',#65673,10.) ;
#8515 = VECTOR('',#65678,10.) ;
#8516 = VECTOR('',#65679,10.) ;
#8517 = VECTOR('',#65682,10.) ;
#8518 = VECTOR('',#65683,10.) ;
#8519 = VECTOR('',#65684,10.) ;
#8520 = VECTOR('',#65687,10.) ;
#8521 = VECTOR('',#65688,10.) ;
#8522 = VECTOR('',#65693,10.) ;
#8523 = VECTOR('',#65696,10.) ;
#8524 = VECTOR('',#65701,10.) ;
#8525 = VECTOR('',#65704,10.) ;
#8526 = VECTOR('',#65707,10.) ;
#8527 = VECTOR('',#65710,10.) ;
#8528 = VECTOR('',#65713,10.) ;
#8529 = VECTOR('',#65714,10.) ;
#8530 = VECTOR('',#65719,10.) ;
#8531 = VECTOR('',#65720,10.) ;
#8532 = VECTOR('',#65725,10.) ;
#8533 = VECTOR('',#65726,10.) ;
#8534 = VECTOR('',#65731,10.) ;
#8535 = VECTOR('',#65732,10.) ;
#8536 = VECTOR('',#65735,10.) ;
#8537 = VECTOR('',#65736,10.) ;
#8538 = VECTOR('',#65737,10.) ;
#8539 = VECTOR('',#65740,10.) ;
#8540 = VECTOR('',#65741,10.) ;
#8541 = VECTOR('',#65744,10.) ;
#8542 = VECTOR('',#65745,10.) ;
#8543 = VECTOR('',#65748,10.) ;
#8544 = VECTOR('',#65749,10.) ;
#8545 = VECTOR('',#65754,10.) ;
#8546 = VECTOR('',#65757,10.) ;
#8547 = VECTOR('',#65762,10.) ;
#8548 = VECTOR('',#65763,10.) ;
#8549 = VECTOR('',#65768,10.) ;
#8550 = VECTOR('',#65769,10.) ;
#8551 = VECTOR('',#65774,10.) ;
#8552 = VECTOR('',#65775,10.) ;
#8553 = VECTOR('',#65778,10.) ;
#8554 = VECTOR('',#65779,10.) ;
#8555 = VECTOR('',#65780,10.) ;
#8556 = VECTOR('',#65783,10.) ;
#8557 = VECTOR('',#65784,10.) ;
#8558 = VECTOR('',#65789,9.99999999999999) ;
#8559 = VECTOR('',#65792,9.99999999999999) ;
#8560 = VECTOR('',#65797,10.) ;
#8561 = VECTOR('',#65800,10.) ;
#8562 = VECTOR('',#65803,10.) ;
#8563 = VECTOR('',#65806,10.) ;
#8564 = VECTOR('',#65817,10.) ;
#8565 = VECTOR('',#65818,10.) ;
#8566 = VECTOR('',#65823,10.) ;
#8567 = VECTOR('',#65824,10.) ;
#8568 = VECTOR('',#65829,10.) ;
#8569 = VECTOR('',#65832,10.) ;
#8570 = VECTOR('',#65843,10.) ;
#8571 = VECTOR('',#65844,10.) ;
#8572 = VECTOR('',#65849,10.) ;
#8573 = VECTOR('',#65850,10.) ;
#8574 = VECTOR('',#65855,10.) ;
#8575 = VECTOR('',#65856,10.) ;
#8576 = VECTOR('',#65859,10.) ;
#8577 = VECTOR('',#65860,10.) ;
#8578 = VECTOR('',#65861,10.) ;
#8579 = VECTOR('',#65864,10.) ;
#8580 = VECTOR('',#65869,10.) ;
#8581 = VECTOR('',#65870,10.) ;
#8582 = VECTOR('',#65873,10.) ;
#8583 = VECTOR('',#65874,10.) ;
#8584 = VECTOR('',#65877,10.) ;
#8585 = VECTOR('',#65878,10.) ;
#8586 = VECTOR('',#65881,10.) ;
#8587 = VECTOR('',#65882,9.99999999999999) ;
#8588 = VECTOR('',#65887,10.) ;
#8589 = VECTOR('',#65890,10.) ;
#8590 = VECTOR('',#65895,10.) ;
#8591 = VECTOR('',#65898,10.) ;
#8592 = VECTOR('',#65909,10.) ;
#8593 = VECTOR('',#65910,10.) ;
#8594 = VECTOR('',#65915,10.) ;
#8595 = VECTOR('',#65918,10.) ;
#8596 = VECTOR('',#65921,10.) ;
#8597 = VECTOR('',#65924,10.) ;
#8598 = VECTOR('',#65935,10.) ;
#8599 = VECTOR('',#65936,10.) ;
#8600 = VECTOR('',#65941,10.) ;
#8601 = VECTOR('',#65942,10.) ;
#8602 = VECTOR('',#65947,10.) ;
#8603 = VECTOR('',#65948,10.) ;
#8604 = VECTOR('',#65953,9.99999999999999) ;
#8605 = VECTOR('',#65954,9.99999999999999) ;
#8606 = VECTOR('',#65957,10.) ;
#8607 = VECTOR('',#65960,10.) ;
#8608 = VECTOR('',#65963,10.) ;
#8609 = VECTOR('',#65964,10.) ;
#8610 = VECTOR('',#65967,10.) ;
#8611 = VECTOR('',#65968,10.) ;
#8612 = VECTOR('',#65971,10.) ;
#8613 = VECTOR('',#65972,10.) ;
#8614 = VECTOR('',#65975,10.) ;
#8615 = VECTOR('',#65976,9.99999999999999) ;
#8616 = VECTOR('',#65979,10.) ;
#8617 = VECTOR('',#65980,10.) ;
#8618 = VECTOR('',#65985,10.) ;
#8619 = VECTOR('',#66000,10.) ;
#8620 = VECTOR('',#66003,10.) ;
#8621 = VECTOR('',#66012,10.) ;
#8622 = VECTOR('',#66017,10.) ;
#8623 = VECTOR('',#66020,10.) ;
#8624 = VECTOR('',#66025,10.) ;
#8625 = VECTOR('',#66028,10.) ;
#8626 = VECTOR('',#66031,10.) ;
#8627 = VECTOR('',#66034,10.) ;
#8628 = VECTOR('',#66039,9.99999999999999) ;
#8629 = VECTOR('',#66042,9.99999999999999) ;
#8630 = VECTOR('',#66045,10.) ;
#8631 = VECTOR('',#66050,10.) ;
#8632 = VECTOR('',#66055,10.) ;
#8633 = VECTOR('',#66060,10.) ;
#8634 = VECTOR('',#66065,10.) ;
#8635 = VECTOR('',#66066,10.) ;
#8636 = VECTOR('',#66069,10.) ;
#8637 = VECTOR('',#66072,10.) ;
#8638 = VECTOR('',#66077,10.) ;
#8639 = VECTOR('',#66080,10.) ;
#8640 = VECTOR('',#66085,10.) ;
#8641 = VECTOR('',#66088,10.) ;
#8642 = VECTOR('',#66089,10.) ;
#8643 = VECTOR('',#66092,10.) ;
#8644 = VECTOR('',#66093,10.) ;
#8645 = VECTOR('',#66094,10.) ;
#8646 = VECTOR('',#66095,10.) ;
#8647 = VECTOR('',#66096,10.) ;
#8648 = VECTOR('',#66097,10.) ;
#8649 = VECTOR('',#66098,10.) ;
#8650 = VECTOR('',#66099,10.) ;
#8651 = VECTOR('',#66100,10.) ;
#8652 = VECTOR('',#66101,10.) ;
#8653 = VECTOR('',#66102,10.) ;
#8654 = VECTOR('',#66115,10.) ;
#8655 = VECTOR('',#66120,10.) ;
#8656 = VECTOR('',#66123,10.) ;
#8657 = VECTOR('',#66128,10.) ;
#8658 = VECTOR('',#66135,10.) ;
#8659 = VECTOR('',#66154,10.) ;
#8660 = VECTOR('',#66157,10.) ;
#8661 = VECTOR('',#66160,10.) ;
#8662 = VECTOR('',#66171,10.) ;
#8663 = VECTOR('',#66178,10.) ;
#8664 = VECTOR('',#66181,10.) ;
#8665 = VECTOR('',#66190,10.) ;
#8666 = VECTOR('',#66225,10.) ;
#8667 = VECTOR('',#66228,10.) ;
#8668 = VECTOR('',#66229,10.) ;
#8669 = VECTOR('',#66232,10.) ;
#8670 = VECTOR('',#66235,10.) ;
#8671 = VECTOR('',#66242,10.) ;
#8672 = VECTOR('',#66247,10.) ;
#8673 = VECTOR('',#66276,10.) ;
#8674 = VECTOR('',#66279,10.) ;
#8675 = VECTOR('',#66290,10.) ;
#8676 = VECTOR('',#66293,10.) ;
#8677 = VECTOR('',#66296,10.) ;
#8678 = VECTOR('',#66299,10.) ;
#8679 = VECTOR('',#66306,10.) ;
#8680 = VECTOR('',#66317,10.) ;
#8681 = VECTOR('',#66318,10.) ;
#8682 = VECTOR('',#66321,10.) ;
#8683 = VECTOR('',#66324,10.) ;
#8684 = VECTOR('',#66327,10.) ;
#8685 = VECTOR('',#66328,10.) ;
#8686 = VECTOR('',#66331,10.) ;
#8687 = VECTOR('',#66334,10.) ;
#8688 = VECTOR('',#66339,10.) ;
#8689 = VECTOR('',#66340,10.) ;
#8690 = VECTOR('',#66343,10.) ;
#8691 = VECTOR('',#66348,10.) ;
#8692 = VECTOR('',#66349,10.) ;
#8693 = VECTOR('',#66352,10.) ;
#8694 = VECTOR('',#66353,10.) ;
#8695 = VECTOR('',#66356,10.) ;
#8696 = VECTOR('',#66357,10.) ;
#8697 = VECTOR('',#66360,10.) ;
#8698 = VECTOR('',#66365,10.) ;
#8699 = VECTOR('',#66370,10.) ;
#8700 = VECTOR('',#66371,10.) ;
#8701 = VECTOR('',#66374,10.) ;
#8702 = VECTOR('',#66379,10.) ;
#8703 = VECTOR('',#66380,10.) ;
#8704 = VECTOR('',#66381,10.) ;
#8705 = VECTOR('',#66384,10.) ;
#8706 = VECTOR('',#66385,10.) ;
#8707 = VECTOR('',#66388,10.) ;
#8708 = VECTOR('',#66389,10.) ;
#8709 = VECTOR('',#66392,10.) ;
#8710 = VECTOR('',#66397,10.) ;
#8711 = VECTOR('',#66398,10.) ;
#8712 = VECTOR('',#66399,10.) ;
#8713 = VECTOR('',#66400,10.) ;
#8714 = VECTOR('',#66403,10.) ;
#8715 = VECTOR('',#66406,10.) ;
#8716 = VECTOR('',#66409,10.) ;
#8717 = VECTOR('',#66412,10.) ;
#8718 = VECTOR('',#66417,0.4) ;
#8719 = VECTOR('',#66426,10.) ;
#8720 = VECTOR('',#66429,10.) ;
#8721 = VECTOR('',#66430,10.) ;
#8722 = VECTOR('',#66431,10.) ;
#8723 = VECTOR('',#66436,10.) ;
#8724 = VECTOR('',#66441,10.) ;
#8725 = VECTOR('',#66444,10.) ;
#8726 = VECTOR('',#66449,10.) ;
#8727 = VECTOR('',#66458,10.) ;
#8728 = VECTOR('',#66477,10.) ;
#8729 = VECTOR('',#66490,10.) ;
#8730 = VECTOR('',#66505,10.) ;
#8731 = VECTOR('',#66518,10.) ;
#8732 = VECTOR('',#66539,10.) ;
#8733 = VECTOR('',#66546,10.) ;
#8734 = VECTOR('',#66559,10.) ;
#8735 = VECTOR('',#66570,10.) ;
#8736 = VECTOR('',#66575,10.) ;
#8737 = VECTOR('',#66586,10.) ;
#8738 = VECTOR('',#66589,10.) ;
#8739 = VECTOR('',#66606,10.) ;
#8740 = VECTOR('',#66607,10.) ;
#8741 = VECTOR('',#66610,10.) ;
#8742 = VECTOR('',#66613,10.) ;
#8743 = VECTOR('',#66622,10.) ;
#8744 = VECTOR('',#66623,10.) ;
#8745 = VECTOR('',#66626,10.) ;
#8746 = VECTOR('',#66627,10.) ;
#8747 = VECTOR('',#66630,10.) ;
#8748 = VECTOR('',#66633,10.) ;
#8749 = VECTOR('',#66636,10.) ;
#8750 = VECTOR('',#66647,10.) ;
#8751 = VECTOR('',#66648,10.) ;
#8752 = VECTOR('',#66651,10.) ;
#8753 = VECTOR('',#66652,10.) ;
#8754 = VECTOR('',#66655,10.) ;
#8755 = VECTOR('',#66656,10.) ;
#8756 = VECTOR('',#66657,10.) ;
#8757 = VECTOR('',#66662,10.) ;
#8758 = VECTOR('',#66665,10.) ;
#8759 = VECTOR('',#66666,10.) ;
#8760 = VECTOR('',#66669,10.) ;
#8761 = VECTOR('',#66670,10.) ;
#8762 = VECTOR('',#66675,10.) ;
#8763 = VECTOR('',#66678,10.) ;
#8764 = VECTOR('',#66679,10.) ;
#8765 = VECTOR('',#66684,10.) ;
#8766 = VECTOR('',#66687,10.) ;
#8767 = VECTOR('',#66688,10.) ;
#8768 = VECTOR('',#66691,10.) ;
#8769 = VECTOR('',#66692,10.) ;
#8770 = VECTOR('',#66693,10.) ;
#8771 = VECTOR('',#66696,10.) ;
#8772 = VECTOR('',#66697,10.) ;
#8773 = VECTOR('',#66700,10.) ;
#8774 = VECTOR('',#66703,10.) ;
#8775 = VECTOR('',#66710,2.6) ;
#8776 = VECTOR('',#66715,10.) ;
#8777 = VECTOR('',#66716,10.) ;
#8778 = VECTOR('',#66717,10.) ;
#8779 = VECTOR('',#66722,10.) ;
#8780 = VECTOR('',#66725,10.) ;
#8781 = VECTOR('',#66726,10.) ;
#8782 = VECTOR('',#66731,10.) ;
#8783 = VECTOR('',#66734,10.) ;
#8784 = VECTOR('',#66735,10.) ;
#8785 = VECTOR('',#66740,10.) ;
#8786 = VECTOR('',#66741,10.) ;
#8787 = VECTOR('',#66744,10.) ;
#8788 = VECTOR('',#66745,10.) ;
#8789 = VECTOR('',#66750,10.) ;
#8790 = VECTOR('',#66753,10.) ;
#8791 = VECTOR('',#66754,10.) ;
#8792 = VECTOR('',#66757,10.) ;
#8793 = VECTOR('',#66758,10.) ;
#8794 = VECTOR('',#66763,10.) ;
#8795 = VECTOR('',#66766,10.) ;
#8796 = VECTOR('',#66767,10.) ;
#8797 = VECTOR('',#66770,2.49999999999999) ;
#8798 = VECTOR('',#66775,10.) ;
#8799 = VECTOR('',#66776,10.) ;
#8800 = VECTOR('',#66777,10.) ;
#8801 = VECTOR('',#66782,10.) ;
#8802 = VECTOR('',#66785,10.) ;
#8803 = VECTOR('',#66786,10.) ;
#8804 = VECTOR('',#66791,10.) ;
#8805 = VECTOR('',#66794,10.) ;
#8806 = VECTOR('',#66795,10.) ;
#8807 = VECTOR('',#66796,10.) ;
#8808 = VECTOR('',#66801,10.) ;
#8809 = VECTOR('',#66802,10.) ;
#8810 = VECTOR('',#66805,10.) ;
#8811 = VECTOR('',#66806,10.) ;
#8812 = VECTOR('',#66811,10.) ;
#8813 = VECTOR('',#66814,10.) ;
#8814 = VECTOR('',#66815,10.) ;
#8815 = VECTOR('',#66818,10.) ;
#8816 = VECTOR('',#66821,10.) ;
#8817 = VECTOR('',#66822,10.) ;
#8818 = VECTOR('',#66827,10.) ;
#8819 = VECTOR('',#66828,10.) ;
#8820 = VECTOR('',#66831,10.) ;
#8821 = VECTOR('',#66832,10.) ;
#8822 = VECTOR('',#66833,10.) ;
#8823 = VECTOR('',#66838,10.) ;
#8824 = VECTOR('',#66841,10.) ;
#8825 = VECTOR('',#66842,10.) ;
#8826 = VECTOR('',#66851,10.) ;
#8827 = VECTOR('',#66852,10.) ;
#8828 = VECTOR('',#66855,10.) ;
#8829 = VECTOR('',#66856,10.) ;
#8830 = VECTOR('',#66861,10.) ;
#8831 = VECTOR('',#66864,10.) ;
#8832 = VECTOR('',#66865,10.) ;
#8833 = VECTOR('',#66868,10.) ;
#8834 = VECTOR('',#66869,10.) ;
#8835 = VECTOR('',#66874,10.) ;
#8836 = VECTOR('',#66877,10.) ;
#8837 = VECTOR('',#66878,10.) ;
#8838 = VECTOR('',#66883,10.) ;
#8839 = VECTOR('',#66886,10.) ;
#8840 = VECTOR('',#66887,10.) ;
#8841 = VECTOR('',#66890,10.) ;
#8842 = VECTOR('',#66891,10.) ;
#8843 = VECTOR('',#66896,10.) ;
#8844 = VECTOR('',#66899,10.) ;
#8845 = VECTOR('',#66900,10.) ;
#8846 = VECTOR('',#66905,10.) ;
#8847 = VECTOR('',#66908,10.) ;
#8848 = VECTOR('',#66913,10.) ;
#8849 = VECTOR('',#66914,10.) ;
#8850 = VECTOR('',#66915,10.) ;
#8851 = VECTOR('',#66918,10.) ;
#8852 = VECTOR('',#66919,10.) ;
#8853 = VECTOR('',#66924,10.) ;
#8854 = VECTOR('',#66927,10.) ;
#8855 = VECTOR('',#66928,10.) ;
#8856 = VECTOR('',#66935,10.) ;
#8857 = VECTOR('',#66938,10.) ;
#8858 = VECTOR('',#66939,10.) ;
#8859 = VECTOR('',#66942,10.) ;
#8860 = VECTOR('',#66943,10.) ;
#8861 = VECTOR('',#66948,10.) ;
#8862 = VECTOR('',#66951,10.) ;
#8863 = VECTOR('',#66952,10.) ;
#8864 = VECTOR('',#66957,10.) ;
#8865 = VECTOR('',#66960,10.) ;
#8866 = VECTOR('',#66967,10.) ;
#8867 = VECTOR('',#66970,10.) ;
#8868 = VECTOR('',#66971,10.) ;
#8869 = VECTOR('',#66974,10.) ;
#8870 = VECTOR('',#66975,10.) ;
#8871 = VECTOR('',#66978,10.) ;
#8872 = VECTOR('',#66979,10.) ;
#8873 = VECTOR('',#66982,10.) ;
#8874 = VECTOR('',#66983,10.) ;
#8875 = VECTOR('',#66986,10.) ;
#8876 = VECTOR('',#66987,10.) ;
#8877 = VECTOR('',#66992,10.) ;
#8878 = VECTOR('',#66997,10.) ;
#8879 = VECTOR('',#67002,10.) ;
#8880 = VECTOR('',#67005,10.) ;
#8881 = VECTOR('',#67006,10.) ;
#8882 = VECTOR('',#67009,10.) ;
#8883 = VECTOR('',#67010,10.) ;
#8884 = VECTOR('',#67015,10.) ;
#8885 = VECTOR('',#67018,10.) ;
#8886 = VECTOR('',#67019,10.) ;
#8887 = VECTOR('',#67024,10.) ;
#8888 = VECTOR('',#67027,10.) ;
#8889 = VECTOR('',#67034,10.) ;
#8890 = VECTOR('',#67037,10.) ;
#8891 = VECTOR('',#67038,10.) ;
#8892 = VECTOR('',#67043,10.) ;
#8893 = VECTOR('',#67046,10.) ;
#8894 = VECTOR('',#67047,10.) ;
#8895 = VECTOR('',#67052,10.) ;
#8896 = VECTOR('',#67055,10.) ;
#8897 = VECTOR('',#67064,10.) ;
#8898 = VECTOR('',#67067,10.) ;
#8899 = VECTOR('',#67068,10.) ;
#8900 = VECTOR('',#67073,10.) ;
#8901 = VECTOR('',#67074,10.) ;
#8902 = VECTOR('',#67077,10.) ;
#8903 = VECTOR('',#67078,10.) ;
#8904 = VECTOR('',#67081,10.) ;
#8905 = VECTOR('',#67084,10.) ;
#8906 = VECTOR('',#67085,10.) ;
#8907 = VECTOR('',#67090,10.) ;
#8908 = VECTOR('',#67093,10.) ;
#8909 = VECTOR('',#67096,10.) ;
#8910 = VECTOR('',#67099,10.) ;
#8911 = VECTOR('',#67102,10.) ;
#8912 = VECTOR('',#67113,10.) ;
#8913 = VECTOR('',#67118,10.) ;
#8914 = VECTOR('',#67121,10.) ;
#8915 = VECTOR('',#67126,10.) ;
#8916 = VECTOR('',#67131,10.) ;
#8917 = VECTOR('',#67136,10.) ;
#8918 = VECTOR('',#67143,10.) ;
#8919 = VECTOR('',#67148,2.) ;
#8920 = VECTOR('',#67151,10.) ;
#8921 = VECTOR('',#67154,10.) ;
#8922 = VECTOR('',#67157,10.) ;
#8923 = VECTOR('',#67160,10.) ;
#8924 = VECTOR('',#67165,10.) ;
#8925 = VECTOR('',#67170,10.) ;
#8926 = VECTOR('',#67171,10.) ;
#8927 = VECTOR('',#67184,10.) ;
#8928 = VECTOR('',#67185,10.) ;
#8929 = VECTOR('',#67186,10.) ;
#8930 = VECTOR('',#67187,10.) ;
#8931 = VECTOR('',#67190,10.) ;
#8932 = VECTOR('',#67191,10.) ;
#8933 = VECTOR('',#67192,10.) ;
#8934 = VECTOR('',#67195,10.) ;
#8935 = VECTOR('',#67196,10.) ;
#8936 = VECTOR('',#67197,10.) ;
#8937 = VECTOR('',#67200,10.) ;
#8938 = VECTOR('',#67201,10.) ;
#8939 = VECTOR('',#67202,10.) ;
#8940 = VECTOR('',#67205,10.) ;
#8941 = VECTOR('',#67206,10.) ;
#8942 = VECTOR('',#67207,10.) ;
#8943 = VECTOR('',#67210,10.) ;
#8944 = VECTOR('',#67211,10.) ;
#8945 = VECTOR('',#67212,10.) ;
#8946 = VECTOR('',#67215,10.) ;
#8947 = VECTOR('',#67216,10.) ;
#8948 = VECTOR('',#67217,10.) ;
#8949 = VECTOR('',#67220,10.) ;
#8950 = VECTOR('',#67223,10.) ;
#8951 = VECTOR('',#67226,10.) ;
#8952 = VECTOR('',#67227,10.) ;
#8953 = VECTOR('',#67228,10.) ;
#8954 = VECTOR('',#67229,10.) ;
#8955 = VECTOR('',#67232,10.) ;
#8956 = VECTOR('',#67233,10.) ;
#8957 = VECTOR('',#67234,10.) ;
#8958 = VECTOR('',#67235,10.) ;
#8959 = VECTOR('',#67238,10.) ;
#8960 = VECTOR('',#67239,10.) ;
#8961 = VECTOR('',#67240,10.) ;
#8962 = VECTOR('',#67243,10.) ;
#8963 = VECTOR('',#67244,10.) ;
#8964 = VECTOR('',#67253,1.67775) ;
#8965 = VECTOR('',#67258,1.67775) ;
#8966 = VECTOR('',#67261,1.67775) ;
#8967 = VECTOR('',#67264,1.67775) ;
#8968 = VECTOR('',#67321,10.) ;
#8969 = VECTOR('',#67322,10.) ;
#8970 = VECTOR('',#67331,10.) ;
#8971 = VECTOR('',#67332,10.) ;
#8972 = VECTOR('',#67341,10.) ;
#8973 = VECTOR('',#67342,10.) ;
#8974 = VECTOR('',#67351,10.) ;
#8975 = VECTOR('',#67352,10.) ;
#8976 = VECTOR('',#67361,10.) ;
#8977 = VECTOR('',#67362,10.) ;
#8978 = VECTOR('',#67371,10.) ;
#8979 = VECTOR('',#67372,10.) ;
#8980 = VECTOR('',#67381,10.) ;
#8981 = VECTOR('',#67382,9.99999999999999) ;
#8982 = VECTOR('',#67391,9.99999999999999) ;
#8983 = VECTOR('',#67392,9.99999999999999) ;
#8984 = VECTOR('',#67401,9.99999999999999) ;
#8985 = VECTOR('',#67402,9.99999999999999) ;
#8986 = VECTOR('',#67411,9.99999999999999) ;
#8987 = VECTOR('',#67412,9.99999999999999) ;
#8988 = VECTOR('',#67421,10.) ;
#8989 = VECTOR('',#67422,10.) ;
#8990 = VECTOR('',#67431,10.) ;
#8991 = VECTOR('',#67432,10.) ;
#8992 = VECTOR('',#67441,10.) ;
#8993 = VECTOR('',#67442,10.) ;
#8994 = VECTOR('',#67451,10.) ;
#8995 = VECTOR('',#67452,10.) ;
#8996 = VECTOR('',#67461,10.) ;
#8997 = VECTOR('',#67462,10.) ;
#8998 = VECTOR('',#67471,10.) ;
#8999 = VECTOR('',#67472,10.) ;
#9000 = VECTOR('',#67481,10.) ;
#9001 = VECTOR('',#67482,10.) ;
#9002 = VECTOR('',#67491,10.) ;
#9003 = VECTOR('',#67492,10.) ;
#9004 = VECTOR('',#67501,9.99999999999999) ;
#9005 = VECTOR('',#67502,9.99999999999999) ;
#9006 = VECTOR('',#67511,9.99999999999999) ;
#9007 = VECTOR('',#67512,9.99999999999999) ;
#9008 = VECTOR('',#67521,10.) ;
#9009 = VECTOR('',#67522,10.) ;
#9010 = VECTOR('',#67531,10.) ;
#9011 = VECTOR('',#67532,10.) ;
#9012 = VECTOR('',#67541,10.) ;
#9013 = VECTOR('',#67542,10.) ;
#9014 = VECTOR('',#67551,10.) ;
#9015 = VECTOR('',#67552,10.) ;
#9016 = VECTOR('',#67561,10.) ;
#9017 = VECTOR('',#67562,10.) ;
#9018 = VECTOR('',#67571,10.) ;
#9019 = VECTOR('',#67572,10.) ;
#9020 = VECTOR('',#67581,9.99999999999999) ;
#9021 = VECTOR('',#67582,9.99999999999999) ;
#9022 = VECTOR('',#67591,9.99999999999999) ;
#9023 = VECTOR('',#67592,9.99999999999999) ;
#9024 = VECTOR('',#67601,9.99999999999999) ;
#9025 = VECTOR('',#67602,9.99999999999999) ;
#9026 = VECTOR('',#67611,9.99999999999999) ;
#9027 = VECTOR('',#67612,9.99999999999999) ;
#9028 = VECTOR('',#67621,10.) ;
#9029 = VECTOR('',#67622,10.) ;
#9030 = VECTOR('',#67631,10.) ;
#9031 = VECTOR('',#67632,10.) ;
#9032 = VECTOR('',#67641,10.) ;
#9033 = VECTOR('',#67642,10.) ;
#9034 = VECTOR('',#67651,10.) ;
#9035 = VECTOR('',#67652,10.) ;
#9036 = VECTOR('',#67661,10.) ;
#9037 = VECTOR('',#67662,10.) ;
#9038 = VECTOR('',#67671,10.) ;
#9039 = VECTOR('',#67672,10.) ;
#9040 = VECTOR('',#67681,9.99999999999999) ;
#9041 = VECTOR('',#67682,9.99999999999999) ;
#9042 = VECTOR('',#67691,9.99999999999999) ;
#9043 = VECTOR('',#67692,9.99999999999999) ;
#9044 = VECTOR('',#67701,9.99999999999999) ;
#9045 = VECTOR('',#67702,9.99999999999999) ;
#9046 = VECTOR('',#67711,9.99999999999999) ;
#9047 = VECTOR('',#67712,9.99999999999999) ;
#9048 = VECTOR('',#67715,10.) ;
#9049 = VECTOR('',#67716,10.) ;
#9050 = VECTOR('',#67717,10.) ;
#9051 = VECTOR('',#67720,10.) ;
#9052 = VECTOR('',#67725,10.) ;
#9053 = VECTOR('',#67726,10.) ;
#9054 = VECTOR('',#67729,10.) ;
#9055 = VECTOR('',#67734,10.) ;
#9056 = VECTOR('',#67735,10.) ;
#9057 = VECTOR('',#67738,10.) ;
#9058 = VECTOR('',#67743,10.) ;
#9059 = VECTOR('',#67744,10.) ;
#9060 = VECTOR('',#67747,10.) ;
#9061 = VECTOR('',#67752,10.) ;
#9062 = VECTOR('',#67753,10.) ;
#9063 = VECTOR('',#67756,10.) ;
#9064 = VECTOR('',#67761,10.) ;
#9065 = VECTOR('',#67762,10.) ;
#9066 = VECTOR('',#67765,10.) ;
#9067 = VECTOR('',#67770,10.) ;
#9068 = VECTOR('',#67771,9.99999999999999) ;
#9069 = VECTOR('',#67774,10.) ;
#9070 = VECTOR('',#67779,10.) ;
#9071 = VECTOR('',#67780,9.99999999999999) ;
#9072 = VECTOR('',#67783,10.) ;
#9073 = VECTOR('',#67788,10.) ;
#9074 = VECTOR('',#67789,9.99999999999999) ;
#9075 = VECTOR('',#67792,10.) ;
#9076 = VECTOR('',#67797,10.) ;
#9077 = VECTOR('',#67798,9.99999999999999) ;
#9078 = VECTOR('',#67801,10.) ;
#9079 = VECTOR('',#67806,10.) ;
#9080 = VECTOR('',#67807,10.) ;
#9081 = VECTOR('',#67810,10.) ;
#9082 = VECTOR('',#67815,10.) ;
#9083 = VECTOR('',#67816,10.) ;
#9084 = VECTOR('',#67819,10.) ;
#9085 = VECTOR('',#67824,10.) ;
#9086 = VECTOR('',#67825,10.) ;
#9087 = VECTOR('',#67828,10.) ;
#9088 = VECTOR('',#67833,10.) ;
#9089 = VECTOR('',#67834,10.) ;
#9090 = VECTOR('',#67837,10.) ;
#9091 = VECTOR('',#67842,10.) ;
#9092 = VECTOR('',#67843,10.) ;
#9093 = VECTOR('',#67846,10.) ;
#9094 = VECTOR('',#67851,10.) ;
#9095 = VECTOR('',#67852,10.) ;
#9096 = VECTOR('',#67855,10.) ;
#9097 = VECTOR('',#67860,10.) ;
#9098 = VECTOR('',#67861,9.99999999999999) ;
#9099 = VECTOR('',#67864,10.) ;
#9100 = VECTOR('',#67869,10.) ;
#9101 = VECTOR('',#67870,9.99999999999999) ;
#9102 = VECTOR('',#67873,10.) ;
#9103 = VECTOR('',#67878,10.) ;
#9104 = VECTOR('',#67879,9.99999999999999) ;
#9105 = VECTOR('',#67882,10.) ;
#9106 = VECTOR('',#67887,10.) ;
#9107 = VECTOR('',#67888,9.99999999999999) ;
#9108 = VECTOR('',#67891,10.) ;
#9109 = VECTOR('',#68068,10.) ;
#9110 = VECTOR('',#68071,10.) ;
#9111 = VECTOR('',#68074,9.99999999999999) ;
#9112 = VECTOR('',#68077,9.99999999999999) ;
#9113 = VECTOR('',#68080,10.) ;
#9114 = VECTOR('',#68083,10.) ;
#9115 = VECTOR('',#68086,10.) ;
#9116 = VECTOR('',#68089,10.) ;
#9117 = VECTOR('',#68092,10.) ;
#9118 = VECTOR('',#68095,10.) ;
#9119 = VECTOR('',#68098,10.) ;
#9120 = VECTOR('',#68101,10.) ;
#9121 = VECTOR('',#68104,9.99999999999999) ;
#9122 = VECTOR('',#68107,9.99999999999999) ;
#9123 = VECTOR('',#68110,9.99999999999999) ;
#9124 = VECTOR('',#68113,9.99999999999999) ;
#9125 = VECTOR('',#68116,10.) ;
#9126 = VECTOR('',#68119,10.) ;
#9127 = VECTOR('',#68122,10.) ;
#9128 = VECTOR('',#68125,10.) ;
#9129 = VECTOR('',#68128,10.) ;
#9130 = VECTOR('',#68131,10.) ;
#9131 = VECTOR('',#68134,9.99999999999999) ;
#9132 = VECTOR('',#68137,9.99999999999999) ;
#9133 = VECTOR('',#68140,9.99999999999999) ;
#9134 = VECTOR('',#68143,9.99999999999999) ;
#9135 = VECTOR('',#68146,10.) ;
#9136 = VECTOR('',#68149,10.) ;
#9137 = VECTOR('',#68152,10.) ;
#9138 = VECTOR('',#68155,10.) ;
#9139 = VECTOR('',#68158,10.) ;
#9140 = VECTOR('',#68161,10.) ;
#9141 = VECTOR('',#68164,9.99999999999999) ;
#9142 = VECTOR('',#68167,9.99999999999999) ;
#9143 = VECTOR('',#68170,9.99999999999999) ;
#9144 = VECTOR('',#68173,9.99999999999999) ;
#9145 = VECTOR('',#68176,10.) ;
#9146 = VECTOR('',#68179,10.) ;
#9147 = VECTOR('',#68182,10.) ;
#9148 = VECTOR('',#68185,10.) ;
#9149 = VECTOR('',#68192,10.) ;
#9150 = VECTOR('',#68195,10.) ;
#9151 = VECTOR('',#68198,10.) ;
#9152 = VECTOR('',#68205,10.) ;
#9153 = VECTOR('',#68214,9.99999999999999) ;
#9154 = VECTOR('',#68223,9.99999999999999) ;
#9155 = VECTOR('',#68232,10.) ;
#9156 = VECTOR('',#68241,10.) ;
#9157 = VECTOR('',#68250,10.) ;
#9158 = VECTOR('',#68259,10.) ;
#9159 = VECTOR('',#68268,9.99999999999999) ;
#9160 = VECTOR('',#68293,9.99999999999999) ;
#9161 = VECTOR('',#68306,10.) ;
#9162 = VECTOR('',#68319,10.) ;
#9163 = VECTOR('',#68332,10.) ;
#9164 = VECTOR('',#68345,10.) ;
#9165 = VECTOR('',#68358,9.99999999999999) ;
#9166 = VECTOR('',#68371,9.99999999999999) ;
#9167 = VECTOR('',#68384,10.) ;
#9168 = VECTOR('',#68397,10.) ;
#9169 = VECTOR('',#68408,10.) ;
#9170 = VECTOR('',#68409,10.) ;
#9171 = VECTOR('',#68412,10.) ;
#9172 = VECTOR('',#68415,10.) ;
#9173 = VECTOR('',#68420,10.) ;
#9174 = VECTOR('',#68421,10.) ;
#9175 = VECTOR('',#68424,10.) ;
#9176 = VECTOR('',#68425,10.) ;
#9177 = VECTOR('',#68430,10.) ;
#9178 = VECTOR('',#68431,10.) ;
#9179 = VECTOR('',#68434,10.) ;
#9180 = VECTOR('',#68435,10.) ;
#9181 = VECTOR('',#68440,10.) ;
#9182 = VECTOR('',#68441,10.) ;
#9183 = VECTOR('',#68444,10.) ;
#9184 = VECTOR('',#68445,10.) ;
#9185 = VECTOR('',#68450,10.) ;
#9186 = VECTOR('',#68451,10.) ;
#9187 = VECTOR('',#68454,10.) ;
#9188 = VECTOR('',#68455,10.) ;
#9189 = VECTOR('',#68460,10.) ;
#9190 = VECTOR('',#68461,10.) ;
#9191 = VECTOR('',#68464,10.) ;
#9192 = VECTOR('',#68465,10.) ;
#9193 = VECTOR('',#68470,10.) ;
#9194 = VECTOR('',#68471,10.) ;
#9195 = VECTOR('',#68474,10.) ;
#9196 = VECTOR('',#68475,10.) ;
#9197 = VECTOR('',#68480,10.) ;
#9198 = VECTOR('',#68481,10.) ;
#9199 = VECTOR('',#68484,10.) ;
#9200 = VECTOR('',#68485,10.) ;
#9201 = VECTOR('',#68490,10.) ;
#9202 = VECTOR('',#68491,10.) ;
#9203 = VECTOR('',#68494,10.) ;
#9204 = VECTOR('',#68495,10.) ;
#9205 = VECTOR('',#68500,10.) ;
#9206 = VECTOR('',#68501,10.) ;
#9207 = VECTOR('',#68504,10.) ;
#9208 = VECTOR('',#68527,2.) ;
#9209 = VECTOR('',#68566,10.) ;
#9210 = VECTOR('',#68567,10.) ;
#9211 = VECTOR('',#68576,10.) ;
#9212 = VECTOR('',#68577,10.) ;
#9213 = VECTOR('',#68586,10.) ;
#9214 = VECTOR('',#68587,10.) ;
#9215 = VECTOR('',#68596,10.) ;
#9216 = VECTOR('',#68597,10.) ;
#9217 = VECTOR('',#68606,10.) ;
#9218 = VECTOR('',#68607,10.) ;
#9219 = VECTOR('',#68616,10.) ;
#9220 = VECTOR('',#68617,10.) ;
#9221 = VECTOR('',#68626,10.) ;
#9222 = VECTOR('',#68627,9.99999999999999) ;
#9223 = VECTOR('',#68636,9.99999999999999) ;
#9224 = VECTOR('',#68637,9.99999999999999) ;
#9225 = VECTOR('',#68646,9.99999999999999) ;
#9226 = VECTOR('',#68647,9.99999999999999) ;
#9227 = VECTOR('',#68656,9.99999999999999) ;
#9228 = VECTOR('',#68657,9.99999999999999) ;
#9229 = VECTOR('',#68666,10.) ;
#9230 = VECTOR('',#68667,10.) ;
#9231 = VECTOR('',#68676,10.) ;
#9232 = VECTOR('',#68677,10.) ;
#9233 = VECTOR('',#68686,10.) ;
#9234 = VECTOR('',#68687,10.) ;
#9235 = VECTOR('',#68696,10.) ;
#9236 = VECTOR('',#68697,10.) ;
#9237 = VECTOR('',#68706,10.) ;
#9238 = VECTOR('',#68707,10.) ;
#9239 = VECTOR('',#68716,10.) ;
#9240 = VECTOR('',#68717,10.) ;
#9241 = VECTOR('',#68726,10.) ;
#9242 = VECTOR('',#68727,10.) ;
#9243 = VECTOR('',#68736,10.) ;
#9244 = VECTOR('',#68737,10.) ;
#9245 = VECTOR('',#68746,9.99999999999999) ;
#9246 = VECTOR('',#68747,9.99999999999999) ;
#9247 = VECTOR('',#68756,9.99999999999999) ;
#9248 = VECTOR('',#68757,9.99999999999999) ;
#9249 = VECTOR('',#68766,10.) ;
#9250 = VECTOR('',#68767,10.) ;
#9251 = VECTOR('',#68776,10.) ;
#9252 = VECTOR('',#68777,10.) ;
#9253 = VECTOR('',#68786,10.) ;
#9254 = VECTOR('',#68787,10.) ;
#9255 = VECTOR('',#68796,10.) ;
#9256 = VECTOR('',#68797,10.) ;
#9257 = VECTOR('',#68806,10.) ;
#9258 = VECTOR('',#68807,10.) ;
#9259 = VECTOR('',#68816,10.) ;
#9260 = VECTOR('',#68817,10.) ;
#9261 = VECTOR('',#68826,9.99999999999999) ;
#9262 = VECTOR('',#68827,9.99999999999999) ;
#9263 = VECTOR('',#68836,9.99999999999999) ;
#9264 = VECTOR('',#68837,9.99999999999999) ;
#9265 = VECTOR('',#68846,9.99999999999999) ;
#9266 = VECTOR('',#68847,9.99999999999999) ;
#9267 = VECTOR('',#68856,9.99999999999999) ;
#9268 = VECTOR('',#68857,9.99999999999999) ;
#9269 = VECTOR('',#68866,10.) ;
#9270 = VECTOR('',#68867,10.) ;
#9271 = VECTOR('',#68876,10.) ;
#9272 = VECTOR('',#68877,10.) ;
#9273 = VECTOR('',#68886,10.) ;
#9274 = VECTOR('',#68887,10.) ;
#9275 = VECTOR('',#68896,10.) ;
#9276 = VECTOR('',#68897,10.) ;
#9277 = VECTOR('',#68906,10.) ;
#9278 = VECTOR('',#68907,10.) ;
#9279 = VECTOR('',#68916,10.) ;
#9280 = VECTOR('',#68917,10.) ;
#9281 = VECTOR('',#68926,9.99999999999999) ;
#9282 = VECTOR('',#68927,9.99999999999999) ;
#9283 = VECTOR('',#68936,9.99999999999999) ;
#9284 = VECTOR('',#68937,9.99999999999999) ;
#9285 = VECTOR('',#68946,9.99999999999999) ;
#9286 = VECTOR('',#68947,9.99999999999999) ;
#9287 = VECTOR('',#68956,9.99999999999999) ;
#9288 = VECTOR('',#68957,9.99999999999999) ;
#9289 = VECTOR('',#68960,10.) ;
#9290 = VECTOR('',#68961,10.) ;
#9291 = VECTOR('',#68962,10.) ;
#9292 = VECTOR('',#68965,10.) ;
#9293 = VECTOR('',#68970,10.) ;
#9294 = VECTOR('',#68971,10.) ;
#9295 = VECTOR('',#68974,10.) ;
#9296 = VECTOR('',#68979,10.) ;
#9297 = VECTOR('',#68980,10.) ;
#9298 = VECTOR('',#68983,10.) ;
#9299 = VECTOR('',#68988,10.) ;
#9300 = VECTOR('',#68989,10.) ;
#9301 = VECTOR('',#68992,10.) ;
#9302 = VECTOR('',#68997,10.) ;
#9303 = VECTOR('',#68998,10.) ;
#9304 = VECTOR('',#69001,10.) ;
#9305 = VECTOR('',#69006,10.) ;
#9306 = VECTOR('',#69007,10.) ;
#9307 = VECTOR('',#69010,10.) ;
#9308 = VECTOR('',#69015,10.) ;
#9309 = VECTOR('',#69016,9.99999999999999) ;
#9310 = VECTOR('',#69019,10.) ;
#9311 = VECTOR('',#69024,10.) ;
#9312 = VECTOR('',#69025,9.99999999999999) ;
#9313 = VECTOR('',#69028,10.) ;
#9314 = VECTOR('',#69033,10.) ;
#9315 = VECTOR('',#69034,9.99999999999999) ;
#9316 = VECTOR('',#69037,10.) ;
#9317 = VECTOR('',#69042,10.) ;
#9318 = VECTOR('',#69043,9.99999999999999) ;
#9319 = VECTOR('',#69046,10.) ;
#9320 = VECTOR('',#69051,10.) ;
#9321 = VECTOR('',#69052,10.) ;
#9322 = VECTOR('',#69055,10.) ;
#9323 = VECTOR('',#69060,10.) ;
#9324 = VECTOR('',#69061,10.) ;
#9325 = VECTOR('',#69064,10.) ;
#9326 = VECTOR('',#69069,10.) ;
#9327 = VECTOR('',#69070,10.) ;
#9328 = VECTOR('',#69073,10.) ;
#9329 = VECTOR('',#69078,10.) ;
#9330 = VECTOR('',#69079,10.) ;
#9331 = VECTOR('',#69082,10.) ;
#9332 = VECTOR('',#69087,10.) ;
#9333 = VECTOR('',#69088,10.) ;
#9334 = VECTOR('',#69091,10.) ;
#9335 = VECTOR('',#69096,10.) ;
#9336 = VECTOR('',#69097,10.) ;
#9337 = VECTOR('',#69100,10.) ;
#9338 = VECTOR('',#69105,10.) ;
#9339 = VECTOR('',#69106,9.99999999999999) ;
#9340 = VECTOR('',#69109,10.) ;
#9341 = VECTOR('',#69114,10.) ;
#9342 = VECTOR('',#69115,9.99999999999999) ;
#9343 = VECTOR('',#69118,10.) ;
#9344 = VECTOR('',#69123,10.) ;
#9345 = VECTOR('',#69124,9.99999999999999) ;
#9346 = VECTOR('',#69127,10.) ;
#9347 = VECTOR('',#69132,10.) ;
#9348 = VECTOR('',#69133,9.99999999999999) ;
#9349 = VECTOR('',#69136,10.) ;
#9350 = VECTOR('',#69313,10.) ;
#9351 = VECTOR('',#69316,10.) ;
#9352 = VECTOR('',#69319,9.99999999999999) ;
#9353 = VECTOR('',#69322,9.99999999999999) ;
#9354 = VECTOR('',#69325,10.) ;
#9355 = VECTOR('',#69328,10.) ;
#9356 = VECTOR('',#69331,10.) ;
#9357 = VECTOR('',#69334,10.) ;
#9358 = VECTOR('',#69337,10.) ;
#9359 = VECTOR('',#69340,10.) ;
#9360 = VECTOR('',#69343,10.) ;
#9361 = VECTOR('',#69346,10.) ;
#9362 = VECTOR('',#69349,9.99999999999999) ;
#9363 = VECTOR('',#69352,9.99999999999999) ;
#9364 = VECTOR('',#69355,9.99999999999999) ;
#9365 = VECTOR('',#69358,9.99999999999999) ;
#9366 = VECTOR('',#69361,10.) ;
#9367 = VECTOR('',#69364,10.) ;
#9368 = VECTOR('',#69367,10.) ;
#9369 = VECTOR('',#69370,10.) ;
#9370 = VECTOR('',#69373,10.) ;
#9371 = VECTOR('',#69376,10.) ;
#9372 = VECTOR('',#69379,9.99999999999999) ;
#9373 = VECTOR('',#69382,9.99999999999999) ;
#9374 = VECTOR('',#69385,9.99999999999999) ;
#9375 = VECTOR('',#69388,9.99999999999999) ;
#9376 = VECTOR('',#69391,10.) ;
#9377 = VECTOR('',#69394,10.) ;
#9378 = VECTOR('',#69397,10.) ;
#9379 = VECTOR('',#69400,10.) ;
#9380 = VECTOR('',#69403,10.) ;
#9381 = VECTOR('',#69406,10.) ;
#9382 = VECTOR('',#69409,9.99999999999999) ;
#9383 = VECTOR('',#69412,9.99999999999999) ;
#9384 = VECTOR('',#69415,9.99999999999999) ;
#9385 = VECTOR('',#69418,9.99999999999999) ;
#9386 = VECTOR('',#69421,10.) ;
#9387 = VECTOR('',#69424,10.) ;
#9388 = VECTOR('',#69427,10.) ;
#9389 = VECTOR('',#69430,10.) ;
#9390 = VECTOR('',#69437,10.) ;
#9391 = VECTOR('',#69440,10.) ;
#9392 = VECTOR('',#69443,10.) ;
#9393 = VECTOR('',#69450,10.) ;
#9394 = VECTOR('',#69459,9.99999999999999) ;
#9395 = VECTOR('',#69468,9.99999999999999) ;
#9396 = VECTOR('',#69477,10.) ;
#9397 = VECTOR('',#69486,10.) ;
#9398 = VECTOR('',#69495,10.) ;
#9399 = VECTOR('',#69504,10.) ;
#9400 = VECTOR('',#69513,9.99999999999999) ;
#9401 = VECTOR('',#69538,9.99999999999999) ;
#9402 = VECTOR('',#69551,10.) ;
#9403 = VECTOR('',#69564,10.) ;
#9404 = VECTOR('',#69577,10.) ;
#9405 = VECTOR('',#69590,10.) ;
#9406 = VECTOR('',#69603,9.99999999999999) ;
#9407 = VECTOR('',#69616,9.99999999999999) ;
#9408 = VECTOR('',#69629,10.) ;
#9409 = VECTOR('',#69642,10.) ;
#9410 = VECTOR('',#69653,10.) ;
#9411 = VECTOR('',#69654,10.) ;
#9412 = VECTOR('',#69657,10.) ;
#9413 = VECTOR('',#69660,10.) ;
#9414 = VECTOR('',#69665,10.) ;
#9415 = VECTOR('',#69666,10.) ;
#9416 = VECTOR('',#69669,10.) ;
#9417 = VECTOR('',#69670,10.) ;
#9418 = VECTOR('',#69675,10.) ;
#9419 = VECTOR('',#69676,10.) ;
#9420 = VECTOR('',#69679,10.) ;
#9421 = VECTOR('',#69680,10.) ;
#9422 = VECTOR('',#69685,10.) ;
#9423 = VECTOR('',#69686,10.) ;
#9424 = VECTOR('',#69689,10.) ;
#9425 = VECTOR('',#69690,10.) ;
#9426 = VECTOR('',#69695,10.) ;
#9427 = VECTOR('',#69696,10.) ;
#9428 = VECTOR('',#69699,10.) ;
#9429 = VECTOR('',#69700,10.) ;
#9430 = VECTOR('',#69705,10.) ;
#9431 = VECTOR('',#69706,10.) ;
#9432 = VECTOR('',#69709,10.) ;
#9433 = VECTOR('',#69710,10.) ;
#9434 = VECTOR('',#69715,10.) ;
#9435 = VECTOR('',#69716,10.) ;
#9436 = VECTOR('',#69719,10.) ;
#9437 = VECTOR('',#69720,10.) ;
#9438 = VECTOR('',#69725,10.) ;
#9439 = VECTOR('',#69726,10.) ;
#9440 = VECTOR('',#69729,10.) ;
#9441 = VECTOR('',#69730,10.) ;
#9442 = VECTOR('',#69735,10.) ;
#9443 = VECTOR('',#69736,10.) ;
#9444 = VECTOR('',#69739,10.) ;
#9445 = VECTOR('',#69740,10.) ;
#9446 = VECTOR('',#69745,10.) ;
#9447 = VECTOR('',#69746,10.) ;
#9448 = VECTOR('',#69749,10.) ;
#9449 = VECTOR('',#69772,2.) ;
#9450 = VECTOR('',#69777,1.67774999999999) ;
#9451 = VECTOR('',#69782,1.67774999999999) ;
#9452 = VECTOR('',#69785,1.67774999999999) ;
#9453 = VECTOR('',#69788,1.67774999999999) ;
#9454 = VECTOR('',#69791,1.67774999999999) ;
#9455 = VECTOR('',#69796,1.67774999999999) ;
#9456 = VECTOR('',#69799,1.67774999999999) ;
#9457 = VECTOR('',#69802,1.67774999999999) ;
#9458 = VECTOR('',#69805,1.67774999999999) ;
#9459 = VECTOR('',#69808,1.67774999999999) ;
#9460 = CYLINDRICAL_SURFACE('',#49316,6.) ;
#9461 = CYLINDRICAL_SURFACE('',#49359,0.2) ;
#9462 = CYLINDRICAL_SURFACE('',#49362,0.2) ;
#9463 = CYLINDRICAL_SURFACE('',#49369,0.2) ;
#9464 = CYLINDRICAL_SURFACE('',#49371,0.2) ;
#9465 = CYLINDRICAL_SURFACE('',#49374,0.2) ;
#9466 = CYLINDRICAL_SURFACE('',#49381,0.2) ;
#9467 = CYLINDRICAL_SURFACE('',#49383,0.2) ;
#9468 = CYLINDRICAL_SURFACE('',#49386,0.2) ;
#9469 = CYLINDRICAL_SURFACE('',#49393,0.2) ;
#9470 = CYLINDRICAL_SURFACE('',#49395,0.2) ;
#9471 = CYLINDRICAL_SURFACE('',#49403,0.2) ;
#9472 = CYLINDRICAL_SURFACE('',#49405,0.2) ;
#9473 = CYLINDRICAL_SURFACE('',#49424,0.2) ;
#9474 = CYLINDRICAL_SURFACE('',#49427,0.2) ;
#9475 = CYLINDRICAL_SURFACE('',#49430,0.95) ;
#9476 = CYLINDRICAL_SURFACE('',#49433,0.2) ;
#9477 = CYLINDRICAL_SURFACE('',#49436,0.2) ;
#9478 = CYLINDRICAL_SURFACE('',#49439,0.95) ;
#9479 = CYLINDRICAL_SURFACE('',#49624,0.2) ;
#9480 = CYLINDRICAL_SURFACE('',#49625,0.2) ;
#9481 = CYLINDRICAL_SURFACE('',#49626,0.2) ;
#9482 = CYLINDRICAL_SURFACE('',#49629,0.2) ;
#9483 = CYLINDRICAL_SURFACE('',#49632,0.2) ;
#9484 = CYLINDRICAL_SURFACE('',#49635,0.2) ;
#9485 = CYLINDRICAL_SURFACE('',#49638,0.2) ;
#9486 = CYLINDRICAL_SURFACE('',#49639,0.2) ;
#9487 = CYLINDRICAL_SURFACE('',#49642,0.2) ;
#9488 = CYLINDRICAL_SURFACE('',#49645,0.2) ;
#9489 = CYLINDRICAL_SURFACE('',#49648,0.2) ;
#9490 = CYLINDRICAL_SURFACE('',#49649,0.2) ;
#9491 = CYLINDRICAL_SURFACE('',#49652,0.2) ;
#9492 = CYLINDRICAL_SURFACE('',#49655,0.2) ;
#9493 = CYLINDRICAL_SURFACE('',#49658,0.2) ;
#9494 = CYLINDRICAL_SURFACE('',#49659,0.2) ;
#9495 = CYLINDRICAL_SURFACE('',#49662,0.2) ;
#9496 = CYLINDRICAL_SURFACE('',#49665,0.2) ;
#9497 = CYLINDRICAL_SURFACE('',#49668,0.2) ;
#9498 = CYLINDRICAL_SURFACE('',#49669,0.2) ;
#9499 = CYLINDRICAL_SURFACE('',#49672,0.2) ;
#9500 = CYLINDRICAL_SURFACE('',#49675,0.2) ;
#9501 = CYLINDRICAL_SURFACE('',#49678,0.2) ;
#9502 = CYLINDRICAL_SURFACE('',#49679,0.2) ;
#9503 = CYLINDRICAL_SURFACE('',#49682,0.2) ;
#9504 = CYLINDRICAL_SURFACE('',#49685,0.2) ;
#9505 = CYLINDRICAL_SURFACE('',#49688,0.2) ;
#9506 = CYLINDRICAL_SURFACE('',#49689,0.2) ;
#9507 = CYLINDRICAL_SURFACE('',#49692,0.2) ;
#9508 = CYLINDRICAL_SURFACE('',#49695,0.2) ;
#9509 = CYLINDRICAL_SURFACE('',#49698,0.2) ;
#9510 = CYLINDRICAL_SURFACE('',#49699,0.2) ;
#9511 = CYLINDRICAL_SURFACE('',#49702,0.2) ;
#9512 = CYLINDRICAL_SURFACE('',#49705,0.2) ;
#9513 = CYLINDRICAL_SURFACE('',#49708,0.2) ;
#9514 = CYLINDRICAL_SURFACE('',#49709,0.2) ;
#9515 = CYLINDRICAL_SURFACE('',#49712,0.2) ;
#9516 = CYLINDRICAL_SURFACE('',#49715,0.2) ;
#9517 = CYLINDRICAL_SURFACE('',#49718,0.2) ;
#9518 = CYLINDRICAL_SURFACE('',#49719,0.2) ;
#9519 = CYLINDRICAL_SURFACE('',#49722,0.599999999999996) ;
#9520 = CYLINDRICAL_SURFACE('',#49724,0.599999999999996) ;
#9521 = CYLINDRICAL_SURFACE('',#49726,0.599999999999996) ;
#9522 = CYLINDRICAL_SURFACE('',#49728,0.599999999999996) ;
#9523 = CYLINDRICAL_SURFACE('',#49730,0.599999999999996) ;
#9524 = CYLINDRICAL_SURFACE('',#49732,0.599999999999996) ;
#9525 = CYLINDRICAL_SURFACE('',#49734,0.599999999999996) ;
#9526 = CYLINDRICAL_SURFACE('',#49736,0.599999999999996) ;
#9527 = CYLINDRICAL_SURFACE('',#49738,0.599999999999996) ;
#9528 = CYLINDRICAL_SURFACE('',#49740,0.599999999999996) ;
#9529 = CYLINDRICAL_SURFACE('',#49742,0.599999999999996) ;
#9530 = CYLINDRICAL_SURFACE('',#49744,0.599999999999996) ;
#9531 = CYLINDRICAL_SURFACE('',#49746,0.599999999999996) ;
#9532 = CYLINDRICAL_SURFACE('',#49748,0.599999999999996) ;
#9533 = CYLINDRICAL_SURFACE('',#49750,0.599999999999996) ;
#9534 = CYLINDRICAL_SURFACE('',#49752,0.599999999999996) ;
#9535 = CYLINDRICAL_SURFACE('',#49754,0.599999999999996) ;
#9536 = CYLINDRICAL_SURFACE('',#49756,0.599999999999996) ;
#9537 = CYLINDRICAL_SURFACE('',#49758,0.599999999999996) ;
#9538 = CYLINDRICAL_SURFACE('',#49760,0.599999999999996) ;
#9539 = CYLINDRICAL_SURFACE('',#49781,0.2) ;
#9540 = CYLINDRICAL_SURFACE('',#49787,0.2) ;
#9541 = CYLINDRICAL_SURFACE('',#49793,0.95) ;
#9542 = CYLINDRICAL_SURFACE('',#49794,0.2) ;
#9543 = CYLINDRICAL_SURFACE('',#49801,0.95) ;
#9544 = CYLINDRICAL_SURFACE('',#49802,0.2) ;
#9545 = CYLINDRICAL_SURFACE('',#49811,0.2) ;
#9546 = CYLINDRICAL_SURFACE('',#49815,0.2) ;
#9547 = CYLINDRICAL_SURFACE('',#49816,0.2) ;
#9548 = CYLINDRICAL_SURFACE('',#49822,0.2) ;
#9549 = CYLINDRICAL_SURFACE('',#49827,0.2) ;
#9550 = CYLINDRICAL_SURFACE('',#49828,0.2) ;
#9551 = CYLINDRICAL_SURFACE('',#49833,0.2) ;
#9552 = CYLINDRICAL_SURFACE('',#49837,0.2) ;
#9553 = CYLINDRICAL_SURFACE('',#49838,0.2) ;
#9554 = CYLINDRICAL_SURFACE('',#49839,0.2) ;
#9555 = CYLINDRICAL_SURFACE('',#49840,0.2) ;
#9556 = CYLINDRICAL_SURFACE('',#49841,0.2) ;
#9557 = CYLINDRICAL_SURFACE('',#49872,0.12) ;
#9558 = CYLINDRICAL_SURFACE('',#49883,0.12) ;
#9559 = CYLINDRICAL_SURFACE('',#49890,0.12) ;
#9560 = CYLINDRICAL_SURFACE('',#49917,0.12) ;
#9561 = CYLINDRICAL_SURFACE('',#49924,0.12) ;
#9562 = CYLINDRICAL_SURFACE('',#49933,2.) ;
#9563 = CYLINDRICAL_SURFACE('',#49935,0.12) ;
#9564 = CYLINDRICAL_SURFACE('',#49940,0.12) ;
#9565 = CYLINDRICAL_SURFACE('',#49950,0.12) ;
#9566 = CYLINDRICAL_SURFACE('',#49965,0.12) ;
#9567 = CYLINDRICAL_SURFACE('',#49967,0.12) ;
#9568 = CYLINDRICAL_SURFACE('',#49970,33.2107853000911) ;
#9569 = CYLINDRICAL_SURFACE('',#49978,3.6) ;
#9570 = CYLINDRICAL_SURFACE('',#50002,0.12) ;
#9571 = CYLINDRICAL_SURFACE('',#50003,0.12) ;
#9572 = CYLINDRICAL_SURFACE('',#50015,0.12) ;
#9573 = CYLINDRICAL_SURFACE('',#50016,0.12) ;
#9574 = CYLINDRICAL_SURFACE('',#50021,0.12) ;
#9575 = CYLINDRICAL_SURFACE('',#50025,34.9868507372267) ;
#9576 = CYLINDRICAL_SURFACE('',#50034,0.12) ;
#9577 = CYLINDRICAL_SURFACE('',#50040,0.12) ;
#9578 = CYLINDRICAL_SURFACE('',#50047,0.12) ;
#9579 = CYLINDRICAL_SURFACE('',#50054,0.12) ;
#9580 = CYLINDRICAL_SURFACE('',#50069,0.12) ;
#9581 = CYLINDRICAL_SURFACE('',#50074,0.12) ;
#9582 = CYLINDRICAL_SURFACE('',#50084,0.12) ;
#9583 = CYLINDRICAL_SURFACE('',#50087,0.12) ;
#9584 = CYLINDRICAL_SURFACE('',#50122,0.12) ;
#9585 = CYLINDRICAL_SURFACE('',#50125,0.12) ;
#9586 = CYLINDRICAL_SURFACE('',#50126,0.12) ;
#9587 = CYLINDRICAL_SURFACE('',#50127,0.12) ;
#9588 = CYLINDRICAL_SURFACE('',#50147,0.12) ;
#9589 = CYLINDRICAL_SURFACE('',#50153,0.12) ;
#9590 = CYLINDRICAL_SURFACE('',#50162,3.6) ;
#9591 = CYLINDRICAL_SURFACE('',#50163,3.6) ;
#9592 = CYLINDRICAL_SURFACE('',#50165,0.12) ;
#9593 = CYLINDRICAL_SURFACE('',#50167,0.12) ;
#9594 = CYLINDRICAL_SURFACE('',#50169,0.12) ;
#9595 = CYLINDRICAL_SURFACE('',#50174,0.12) ;
#9596 = CYLINDRICAL_SURFACE('',#50176,0.12) ;
#9597 = CYLINDRICAL_SURFACE('',#50178,0.12) ;
#9598 = CYLINDRICAL_SURFACE('',#50180,0.12) ;
#9599 = CYLINDRICAL_SURFACE('',#50183,0.12) ;
#9600 = CYLINDRICAL_SURFACE('',#50185,0.12) ;
#9601 = CYLINDRICAL_SURFACE('',#50187,0.12) ;
#9602 = CYLINDRICAL_SURFACE('',#50189,0.12) ;
#9603 = CYLINDRICAL_SURFACE('',#50194,0.12) ;
#9604 = CYLINDRICAL_SURFACE('',#50196,0.12) ;
#9605 = CYLINDRICAL_SURFACE('',#50198,0.12) ;
#9606 = CYLINDRICAL_SURFACE('',#50200,0.12) ;
#9607 = CYLINDRICAL_SURFACE('',#50203,0.12) ;
#9608 = CYLINDRICAL_SURFACE('',#50205,0.12) ;
#9609 = CYLINDRICAL_SURFACE('',#50209,0.12) ;
#9610 = CYLINDRICAL_SURFACE('',#50212,0.12) ;
#9611 = CYLINDRICAL_SURFACE('',#50214,0.12) ;
#9612 = CYLINDRICAL_SURFACE('',#50216,0.12) ;
#9613 = CYLINDRICAL_SURFACE('',#50220,0.12) ;
#9614 = CYLINDRICAL_SURFACE('',#50223,0.12) ;
#9615 = CYLINDRICAL_SURFACE('',#50225,0.12) ;
#9616 = CYLINDRICAL_SURFACE('',#50229,0.12) ;
#9617 = CYLINDRICAL_SURFACE('',#50231,0.12) ;
#9618 = CYLINDRICAL_SURFACE('',#50234,0.12) ;
#9619 = CYLINDRICAL_SURFACE('',#50237,0.12) ;
#9620 = CYLINDRICAL_SURFACE('',#50239,0.12) ;
#9621 = CYLINDRICAL_SURFACE('',#50241,0.12) ;
#9622 = CYLINDRICAL_SURFACE('',#50243,0.12) ;
#9623 = CYLINDRICAL_SURFACE('',#50244,0.12) ;
#9624 = CYLINDRICAL_SURFACE('',#50325,0.12) ;
#9625 = CYLINDRICAL_SURFACE('',#50328,0.12) ;
#9626 = CYLINDRICAL_SURFACE('',#50330,0.12) ;
#9627 = CYLINDRICAL_SURFACE('',#50332,0.12) ;
#9628 = CYLINDRICAL_SURFACE('',#50335,0.12) ;
#9629 = CYLINDRICAL_SURFACE('',#50337,0.12) ;
#9630 = CYLINDRICAL_SURFACE('',#50339,0.12) ;
#9631 = CYLINDRICAL_SURFACE('',#50341,0.12) ;
#9632 = CYLINDRICAL_SURFACE('',#50344,0.12) ;
#9633 = CYLINDRICAL_SURFACE('',#50346,0.12) ;
#9634 = CYLINDRICAL_SURFACE('',#50356,2.) ;
#9635 = CYLINDRICAL_SURFACE('',#50361,2.99999999999999) ;
#9636 = CYLINDRICAL_SURFACE('',#50441,0.1) ;
#9637 = CYLINDRICAL_SURFACE('',#50447,0.1) ;
#9638 = CYLINDRICAL_SURFACE('',#50453,0.1) ;
#9639 = CYLINDRICAL_SURFACE('',#50459,0.1) ;
#9640 = CYLINDRICAL_SURFACE('',#50465,0.1) ;
#9641 = CYLINDRICAL_SURFACE('',#50471,0.1) ;
#9642 = CYLINDRICAL_SURFACE('',#50479,2.) ;
#9643 = CYLINDRICAL_SURFACE('',#50482,2.) ;
#9644 = CYLINDRICAL_SURFACE('',#50485,2.6) ;
#9645 = CYLINDRICAL_SURFACE('',#50488,2.) ;
#9646 = CYLINDRICAL_SURFACE('',#50491,2.) ;
#9647 = CYLINDRICAL_SURFACE('',#50498,3.) ;
#9648 = CYLINDRICAL_SURFACE('',#50509,2.) ;
#9649 = CYLINDRICAL_SURFACE('',#50516,1.85) ;
#9650 = CYLINDRICAL_SURFACE('',#50531,1.85) ;
#9651 = CYLINDRICAL_SURFACE('',#50545,0.1) ;
#9652 = CYLINDRICAL_SURFACE('',#50550,0.1) ;
#9653 = CYLINDRICAL_SURFACE('',#50558,0.1) ;
#9654 = CYLINDRICAL_SURFACE('',#50566,0.1) ;
#9655 = CYLINDRICAL_SURFACE('',#50568,0.4) ;
#9656 = CYLINDRICAL_SURFACE('',#50573,0.4) ;
#9657 = CYLINDRICAL_SURFACE('',#50576,0.4) ;
#9658 = CYLINDRICAL_SURFACE('',#50577,0.1) ;
#9659 = CYLINDRICAL_SURFACE('',#50583,0.1) ;
#9660 = CYLINDRICAL_SURFACE('',#50588,0.1) ;
#9661 = CYLINDRICAL_SURFACE('',#50590,0.4) ;
#9662 = CYLINDRICAL_SURFACE('',#50591,1.7) ;
#9663 = CYLINDRICAL_SURFACE('',#50596,0.1) ;
#9664 = CYLINDRICAL_SURFACE('',#50605,0.1) ;
#9665 = CYLINDRICAL_SURFACE('',#50614,0.1) ;
#9666 = CYLINDRICAL_SURFACE('',#50615,0.1) ;
#9667 = CYLINDRICAL_SURFACE('',#50620,0.1) ;
#9668 = CYLINDRICAL_SURFACE('',#50621,0.1) ;
#9669 = CYLINDRICAL_SURFACE('',#50626,0.1) ;
#9670 = CYLINDRICAL_SURFACE('',#50631,0.1) ;
#9671 = CYLINDRICAL_SURFACE('',#50634,0.1) ;
#9672 = CYLINDRICAL_SURFACE('',#50636,0.1) ;
#9673 = CYLINDRICAL_SURFACE('',#50643,0.1) ;
#9674 = CYLINDRICAL_SURFACE('',#50647,0.1) ;
#9675 = CYLINDRICAL_SURFACE('',#50653,0.1) ;
#9676 = CYLINDRICAL_SURFACE('',#50659,0.1) ;
#9677 = CYLINDRICAL_SURFACE('',#50661,0.1) ;
#9678 = CYLINDRICAL_SURFACE('',#50667,0.1) ;
#9679 = CYLINDRICAL_SURFACE('',#50672,0.1) ;
#9680 = CYLINDRICAL_SURFACE('',#50676,0.1) ;
#9681 = CYLINDRICAL_SURFACE('',#50679,0.1) ;
#9682 = CYLINDRICAL_SURFACE('',#50682,0.1) ;
#9683 = CYLINDRICAL_SURFACE('',#50685,0.1) ;
#9684 = CYLINDRICAL_SURFACE('',#50688,0.1) ;
#9685 = CYLINDRICAL_SURFACE('',#50691,0.1) ;
#9686 = CYLINDRICAL_SURFACE('',#50694,0.1) ;
#9687 = CYLINDRICAL_SURFACE('',#50700,0.1) ;
#9688 = CYLINDRICAL_SURFACE('',#50705,0.1) ;
#9689 = CYLINDRICAL_SURFACE('',#50710,0.1) ;
#9690 = CYLINDRICAL_SURFACE('',#50715,0.1) ;
#9691 = CYLINDRICAL_SURFACE('',#50717,0.1) ;
#9692 = CYLINDRICAL_SURFACE('',#50723,0.1) ;
#9693 = CYLINDRICAL_SURFACE('',#50728,0.1) ;
#9694 = CYLINDRICAL_SURFACE('',#50734,0.1) ;
#9695 = CYLINDRICAL_SURFACE('',#50737,0.1) ;
#9696 = CYLINDRICAL_SURFACE('',#50740,0.1) ;
#9697 = CYLINDRICAL_SURFACE('',#50743,0.1) ;
#9698 = CYLINDRICAL_SURFACE('',#50754,0.1) ;
#9699 = CYLINDRICAL_SURFACE('',#50759,0.1) ;
#9700 = CYLINDRICAL_SURFACE('',#50764,0.1) ;
#9701 = CYLINDRICAL_SURFACE('',#50769,0.1) ;
#9702 = CYLINDRICAL_SURFACE('',#50774,0.1) ;
#9703 = CYLINDRICAL_SURFACE('',#50775,0.1) ;
#9704 = CYLINDRICAL_SURFACE('',#50777,0.1) ;
#9705 = CYLINDRICAL_SURFACE('',#50781,0.1) ;
#9706 = CYLINDRICAL_SURFACE('',#50785,0.1) ;
#9707 = CYLINDRICAL_SURFACE('',#50792,0.1) ;
#9708 = CYLINDRICAL_SURFACE('',#50794,0.1) ;
#9709 = CYLINDRICAL_SURFACE('',#50800,0.1) ;
#9710 = CYLINDRICAL_SURFACE('',#50805,0.1) ;
#9711 = CYLINDRICAL_SURFACE('',#50809,0.1) ;
#9712 = CYLINDRICAL_SURFACE('',#50818,0.1) ;
#9713 = CYLINDRICAL_SURFACE('',#50821,0.1) ;
#9714 = CYLINDRICAL_SURFACE('',#50824,0.1) ;
#9715 = CYLINDRICAL_SURFACE('',#50827,0.1) ;
#9716 = CYLINDRICAL_SURFACE('',#50834,0.1) ;
#9717 = CYLINDRICAL_SURFACE('',#50836,0.1) ;
#9718 = CYLINDRICAL_SURFACE('',#50842,0.1) ;
#9719 = CYLINDRICAL_SURFACE('',#50847,0.1) ;
#9720 = CYLINDRICAL_SURFACE('',#50851,0.1) ;
#9721 = CYLINDRICAL_SURFACE('',#50860,0.1) ;
#9722 = CYLINDRICAL_SURFACE('',#50863,0.1) ;
#9723 = CYLINDRICAL_SURFACE('',#50866,0.1) ;
#9724 = CYLINDRICAL_SURFACE('',#50869,0.1) ;
#9725 = CYLINDRICAL_SURFACE('',#50872,0.1) ;
#9726 = CYLINDRICAL_SURFACE('',#50874,0.1) ;
#9727 = CYLINDRICAL_SURFACE('',#50882,0.1) ;
#9728 = CYLINDRICAL_SURFACE('',#50887,0.1) ;
#9729 = CYLINDRICAL_SURFACE('',#50892,0.1) ;
#9730 = CYLINDRICAL_SURFACE('',#50897,0.1) ;
#9731 = CYLINDRICAL_SURFACE('',#50902,0.1) ;
#9732 = CYLINDRICAL_SURFACE('',#50907,0.1) ;
#9733 = CYLINDRICAL_SURFACE('',#50909,0.1) ;
#9734 = CYLINDRICAL_SURFACE('',#50912,0.1) ;
#9735 = CYLINDRICAL_SURFACE('',#50915,0.1) ;
#9736 = CYLINDRICAL_SURFACE('',#50918,0.1) ;
#9737 = CYLINDRICAL_SURFACE('',#50921,0.1) ;
#9738 = CYLINDRICAL_SURFACE('',#50930,0.1) ;
#9739 = CYLINDRICAL_SURFACE('',#50939,0.1) ;
#9740 = CYLINDRICAL_SURFACE('',#50940,0.1) ;
#9741 = CYLINDRICAL_SURFACE('',#50941,0.1) ;
#9742 = CYLINDRICAL_SURFACE('',#50946,0.1) ;
#9743 = CYLINDRICAL_SURFACE('',#50947,0.1) ;
#9744 = CYLINDRICAL_SURFACE('',#50948,0.1) ;
#9745 = CYLINDRICAL_SURFACE('',#50949,0.1) ;
#9746 = CYLINDRICAL_SURFACE('',#50951,0.1) ;
#9747 = CYLINDRICAL_SURFACE('',#50967,0.1) ;
#9748 = CYLINDRICAL_SURFACE('',#50974,0.1) ;
#9749 = CYLINDRICAL_SURFACE('',#50983,0.1) ;
#9750 = CYLINDRICAL_SURFACE('',#50984,0.1) ;
#9751 = CYLINDRICAL_SURFACE('',#50993,0.1) ;
#9752 = CYLINDRICAL_SURFACE('',#50994,0.1) ;
#9753 = CYLINDRICAL_SURFACE('',#50995,0.1) ;
#9754 = CYLINDRICAL_SURFACE('',#50996,0.1) ;
#9755 = CYLINDRICAL_SURFACE('',#50997,0.1) ;
#9756 = CYLINDRICAL_SURFACE('',#50998,0.1) ;
#9757 = CYLINDRICAL_SURFACE('',#50999,0.1) ;
#9758 = CYLINDRICAL_SURFACE('',#51000,0.1) ;
#9759 = CYLINDRICAL_SURFACE('',#51001,0.1) ;
#9760 = CYLINDRICAL_SURFACE('',#51003,0.1) ;
#9761 = CYLINDRICAL_SURFACE('',#51019,0.1) ;
#9762 = CYLINDRICAL_SURFACE('',#51023,0.1) ;
#9763 = CYLINDRICAL_SURFACE('',#51031,0.1) ;
#9764 = CYLINDRICAL_SURFACE('',#51040,0.1) ;
#9765 = CYLINDRICAL_SURFACE('',#51041,0.1) ;
#9766 = CYLINDRICAL_SURFACE('',#51046,0.1) ;
#9767 = CYLINDRICAL_SURFACE('',#51047,0.1) ;
#9768 = CYLINDRICAL_SURFACE('',#51048,0.1) ;
#9769 = CYLINDRICAL_SURFACE('',#51049,0.1) ;
#9770 = CYLINDRICAL_SURFACE('',#51050,0.1) ;
#9771 = CYLINDRICAL_SURFACE('',#51051,0.1) ;
#9772 = CYLINDRICAL_SURFACE('',#51052,0.1) ;
#9773 = CYLINDRICAL_SURFACE('',#51053,0.1) ;
#9774 = CYLINDRICAL_SURFACE('',#51055,0.1) ;
#9775 = CYLINDRICAL_SURFACE('',#51064,0.1) ;
#9776 = CYLINDRICAL_SURFACE('',#51070,0.1) ;
#9777 = CYLINDRICAL_SURFACE('',#51075,0.1) ;
#9778 = CYLINDRICAL_SURFACE('',#51080,0.1) ;
#9779 = CYLINDRICAL_SURFACE('',#51084,0.1) ;
#9780 = CYLINDRICAL_SURFACE('',#51089,0.1) ;
#9781 = CYLINDRICAL_SURFACE('',#51094,0.1) ;
#9782 = CYLINDRICAL_SURFACE('',#51099,0.1) ;
#9783 = CYLINDRICAL_SURFACE('',#51107,0.1) ;
#9784 = CYLINDRICAL_SURFACE('',#51115,0.1) ;
#9785 = CYLINDRICAL_SURFACE('',#51120,0.1) ;
#9786 = CYLINDRICAL_SURFACE('',#51125,0.1) ;
#9787 = CYLINDRICAL_SURFACE('',#51130,0.1) ;
#9788 = CYLINDRICAL_SURFACE('',#51135,0.1) ;
#9789 = CYLINDRICAL_SURFACE('',#51140,0.1) ;
#9790 = CYLINDRICAL_SURFACE('',#51145,0.1) ;
#9791 = CYLINDRICAL_SURFACE('',#51150,0.1) ;
#9792 = CYLINDRICAL_SURFACE('',#51155,0.1) ;
#9793 = CYLINDRICAL_SURFACE('',#51156,0.1) ;
#9794 = CYLINDRICAL_SURFACE('',#51157,0.1) ;
#9795 = CYLINDRICAL_SURFACE('',#51162,1.2) ;
#9796 = CYLINDRICAL_SURFACE('',#51166,0.6) ;
#9797 = CYLINDRICAL_SURFACE('',#51169,0.600000000000005) ;
#9798 = CYLINDRICAL_SURFACE('',#51171,2.49999999999996) ;
#9799 = CYLINDRICAL_SURFACE('',#51174,2.49999999999999) ;
#9800 = CYLINDRICAL_SURFACE('',#51176,0.600000000000023) ;
#9801 = CYLINDRICAL_SURFACE('',#51179,0.6) ;
#9802 = CYLINDRICAL_SURFACE('',#51182,0.6) ;
#9803 = CYLINDRICAL_SURFACE('',#51185,4.) ;
#9804 = CYLINDRICAL_SURFACE('',#51188,4.) ;
#9805 = CYLINDRICAL_SURFACE('',#51191,4.) ;
#9806 = CYLINDRICAL_SURFACE('',#51194,0.6) ;
#9807 = CYLINDRICAL_SURFACE('',#51197,0.6) ;
#9808 = CYLINDRICAL_SURFACE('',#51200,0.1) ;
#9809 = CYLINDRICAL_SURFACE('',#51202,0.1) ;
#9810 = CYLINDRICAL_SURFACE('',#51209,0.1) ;
#9811 = CYLINDRICAL_SURFACE('',#51211,1.) ;
#9812 = CYLINDRICAL_SURFACE('',#51216,0.1) ;
#9813 = CYLINDRICAL_SURFACE('',#51221,0.1) ;
#9814 = CYLINDRICAL_SURFACE('',#51232,0.1) ;
#9815 = CYLINDRICAL_SURFACE('',#51237,0.1) ;
#9816 = CYLINDRICAL_SURFACE('',#51242,0.1) ;
#9817 = CYLINDRICAL_SURFACE('',#51247,0.1) ;
#9818 = CYLINDRICAL_SURFACE('',#51252,0.1) ;
#9819 = CYLINDRICAL_SURFACE('',#51253,0.1) ;
#9820 = CYLINDRICAL_SURFACE('',#51254,0.1) ;
#9821 = CYLINDRICAL_SURFACE('',#51255,0.1) ;
#9822 = CYLINDRICAL_SURFACE('',#51256,0.1) ;
#9823 = CYLINDRICAL_SURFACE('',#51257,0.1) ;
#9824 = CYLINDRICAL_SURFACE('',#51258,0.1) ;
#9825 = CYLINDRICAL_SURFACE('',#51259,0.1) ;
#9826 = CYLINDRICAL_SURFACE('',#51260,0.1) ;
#9827 = CYLINDRICAL_SURFACE('',#51271,0.1) ;
#9828 = CYLINDRICAL_SURFACE('',#51272,0.1) ;
#9829 = CYLINDRICAL_SURFACE('',#51280,0.1) ;
#9830 = CYLINDRICAL_SURFACE('',#51285,0.1) ;
#9831 = CYLINDRICAL_SURFACE('',#51289,0.1) ;
#9832 = CYLINDRICAL_SURFACE('',#51296,0.1) ;
#9833 = CYLINDRICAL_SURFACE('',#51297,0.1) ;
#9834 = CYLINDRICAL_SURFACE('',#51298,0.1) ;
#9835 = CYLINDRICAL_SURFACE('',#51299,0.1) ;
#9836 = CYLINDRICAL_SURFACE('',#51300,0.1) ;
#9837 = CYLINDRICAL_SURFACE('',#51301,0.1) ;
#9838 = CYLINDRICAL_SURFACE('',#51302,0.1) ;
#9839 = CYLINDRICAL_SURFACE('',#51305,0.1) ;
#9840 = CYLINDRICAL_SURFACE('',#51312,0.1) ;
#9841 = CYLINDRICAL_SURFACE('',#51314,0.1) ;
#9842 = CYLINDRICAL_SURFACE('',#51321,0.1) ;
#9843 = CYLINDRICAL_SURFACE('',#51322,1.) ;
#9844 = CYLINDRICAL_SURFACE('',#51327,0.1) ;
#9845 = CYLINDRICAL_SURFACE('',#51331,0.1) ;
#9846 = CYLINDRICAL_SURFACE('',#51335,0.1) ;
#9847 = CYLINDRICAL_SURFACE('',#51339,0.1) ;
#9848 = CYLINDRICAL_SURFACE('',#51340,0.1) ;
#9849 = CYLINDRICAL_SURFACE('',#51341,0.1) ;
#9850 = CYLINDRICAL_SURFACE('',#51348,0.1) ;
#9851 = CYLINDRICAL_SURFACE('',#51350,1.) ;
#9852 = CYLINDRICAL_SURFACE('',#51355,0.1) ;
#9853 = CYLINDRICAL_SURFACE('',#51360,0.1) ;
#9854 = CYLINDRICAL_SURFACE('',#51379,0.1) ;
#9855 = CYLINDRICAL_SURFACE('',#51380,0.1) ;
#9856 = CYLINDRICAL_SURFACE('',#51381,0.1) ;
#9857 = CYLINDRICAL_SURFACE('',#51382,0.1) ;
#9858 = CYLINDRICAL_SURFACE('',#51383,0.1) ;
#9859 = CYLINDRICAL_SURFACE('',#51384,0.1) ;
#9860 = CYLINDRICAL_SURFACE('',#51385,0.1) ;
#9861 = CYLINDRICAL_SURFACE('',#51386,0.1) ;
#9862 = CYLINDRICAL_SURFACE('',#51387,0.1) ;
#9863 = CYLINDRICAL_SURFACE('',#51388,0.1) ;
#9864 = CYLINDRICAL_SURFACE('',#51389,0.1) ;
#9865 = CYLINDRICAL_SURFACE('',#51395,0.1) ;
#9866 = CYLINDRICAL_SURFACE('',#51397,0.1) ;
#9867 = CYLINDRICAL_SURFACE('',#51427,0.1) ;
#9868 = CYLINDRICAL_SURFACE('',#51432,0.1) ;
#9869 = CYLINDRICAL_SURFACE('',#51433,0.1) ;
#9870 = CYLINDRICAL_SURFACE('',#51434,0.1) ;
#9871 = CYLINDRICAL_SURFACE('',#51435,0.1) ;
#9872 = CYLINDRICAL_SURFACE('',#51436,0.1) ;
#9873 = CYLINDRICAL_SURFACE('',#51437,0.1) ;
#9874 = CYLINDRICAL_SURFACE('',#51438,0.1) ;
#9875 = CYLINDRICAL_SURFACE('',#51439,0.1) ;
#9876 = CYLINDRICAL_SURFACE('',#51440,0.1) ;
#9877 = CYLINDRICAL_SURFACE('',#51441,0.1) ;
#9878 = CYLINDRICAL_SURFACE('',#51442,0.1) ;
#9879 = CYLINDRICAL_SURFACE('',#51450,2.5) ;
#9880 = CYLINDRICAL_SURFACE('',#51455,0.1) ;
#9881 = CYLINDRICAL_SURFACE('',#51462,0.1) ;
#9882 = CYLINDRICAL_SURFACE('',#51468,0.1) ;
#9883 = CYLINDRICAL_SURFACE('',#51474,0.1) ;
#9884 = CYLINDRICAL_SURFACE('',#51476,1.) ;
#9885 = CYLINDRICAL_SURFACE('',#51480,0.1) ;
#9886 = CYLINDRICAL_SURFACE('',#51485,0.1) ;
#9887 = CYLINDRICAL_SURFACE('',#51489,0.1) ;
#9888 = CYLINDRICAL_SURFACE('',#51493,0.1) ;
#9889 = CYLINDRICAL_SURFACE('',#51497,0.1) ;
#9890 = CYLINDRICAL_SURFACE('',#51498,0.1) ;
#9891 = CYLINDRICAL_SURFACE('',#51499,0.1) ;
#9892 = CYLINDRICAL_SURFACE('',#51504,2.5) ;
#9893 = CYLINDRICAL_SURFACE('',#51509,2.) ;
#9894 = CYLINDRICAL_SURFACE('',#51510,0.1) ;
#9895 = CYLINDRICAL_SURFACE('',#51515,0.1) ;
#9896 = CYLINDRICAL_SURFACE('',#51519,0.1) ;
#9897 = CYLINDRICAL_SURFACE('',#51525,0.1) ;
#9898 = CYLINDRICAL_SURFACE('',#51531,0.1) ;
#9899 = CYLINDRICAL_SURFACE('',#51535,0.1) ;
#9900 = CYLINDRICAL_SURFACE('',#51539,0.1) ;
#9901 = CYLINDRICAL_SURFACE('',#51543,0.1) ;
#9902 = CYLINDRICAL_SURFACE('',#51547,0.1) ;
#9903 = CYLINDRICAL_SURFACE('',#51551,0.1) ;
#9904 = CYLINDRICAL_SURFACE('',#51555,0.1) ;
#9905 = CYLINDRICAL_SURFACE('',#51558,0.6) ;
#9906 = CYLINDRICAL_SURFACE('',#51562,0.1) ;
#9907 = CYLINDRICAL_SURFACE('',#51567,0.1) ;
#9908 = CYLINDRICAL_SURFACE('',#51577,2.8) ;
#9909 = CYLINDRICAL_SURFACE('',#51588,2.8) ;
#9910 = CYLINDRICAL_SURFACE('',#51599,2.) ;
#9911 = CYLINDRICAL_SURFACE('',#51606,2.79999999999999) ;
#9912 = CYLINDRICAL_SURFACE('',#51623,0.6) ;
#9913 = CYLINDRICAL_SURFACE('',#51625,0.6) ;
#9914 = CYLINDRICAL_SURFACE('',#51647,1.2) ;
#9915 = CYLINDRICAL_SURFACE('',#51651,1.2) ;
#9916 = CYLINDRICAL_SURFACE('',#51655,1.2) ;
#9917 = CYLINDRICAL_SURFACE('',#51656,1.2) ;
#9918 = CYLINDRICAL_SURFACE('',#51657,1.2) ;
#9919 = CYLINDRICAL_SURFACE('',#51661,1.2) ;
#9920 = CYLINDRICAL_SURFACE('',#51665,1.2) ;
#9921 = CYLINDRICAL_SURFACE('',#51666,1.2) ;
#9922 = CYLINDRICAL_SURFACE('',#51667,0.5) ;
#9923 = CYLINDRICAL_SURFACE('',#51669,0.5) ;
#9924 = CYLINDRICAL_SURFACE('',#51672,0.5) ;
#9925 = CYLINDRICAL_SURFACE('',#51674,0.5) ;
#9926 = CYLINDRICAL_SURFACE('',#51677,0.5) ;
#9927 = CYLINDRICAL_SURFACE('',#51679,0.5) ;
#9928 = CYLINDRICAL_SURFACE('',#51682,0.5) ;
#9929 = CYLINDRICAL_SURFACE('',#51701,1.7) ;
#9930 = CYLINDRICAL_SURFACE('',#51702,1.7) ;
#9931 = CYLINDRICAL_SURFACE('',#51703,1.7) ;
#9932 = CYLINDRICAL_SURFACE('',#51707,0.5) ;
#9933 = CYLINDRICAL_SURFACE('',#51710,0.1) ;
#9934 = CYLINDRICAL_SURFACE('',#51713,0.1) ;
#9935 = CYLINDRICAL_SURFACE('',#51715,0.1) ;
#9936 = CYLINDRICAL_SURFACE('',#51721,0.1) ;
#9937 = CYLINDRICAL_SURFACE('',#51723,0.1) ;
#9938 = CYLINDRICAL_SURFACE('',#51725,0.1) ;
#9939 = CYLINDRICAL_SURFACE('',#51735,0.1) ;
#9940 = CYLINDRICAL_SURFACE('',#51737,0.1) ;
#9941 = CYLINDRICAL_SURFACE('',#51740,0.1) ;
#9942 = CYLINDRICAL_SURFACE('',#51755,0.1) ;
#9943 = CYLINDRICAL_SURFACE('',#51758,0.1) ;
#9944 = CYLINDRICAL_SURFACE('',#51769,0.1) ;
#9945 = CYLINDRICAL_SURFACE('',#51772,0.1) ;
#9946 = CYLINDRICAL_SURFACE('',#51784,0.5) ;
#9947 = CYLINDRICAL_SURFACE('',#51786,0.1) ;
#9948 = CYLINDRICAL_SURFACE('',#51788,0.1) ;
#9949 = CYLINDRICAL_SURFACE('',#51797,0.5) ;
#9950 = CYLINDRICAL_SURFACE('',#51798,0.1) ;
#9951 = CYLINDRICAL_SURFACE('',#51807,0.5) ;
#9952 = CYLINDRICAL_SURFACE('',#51808,0.1) ;
#9953 = CYLINDRICAL_SURFACE('',#51811,0.1) ;
#9954 = CYLINDRICAL_SURFACE('',#51818,0.2) ;
#9955 = CYLINDRICAL_SURFACE('',#51825,0.1) ;
#9956 = CYLINDRICAL_SURFACE('',#51827,0.1) ;
#9957 = CYLINDRICAL_SURFACE('',#51832,0.2) ;
#9958 = CYLINDRICAL_SURFACE('',#51833,0.1) ;
#9959 = CYLINDRICAL_SURFACE('',#51835,0.1) ;
#9960 = CYLINDRICAL_SURFACE('',#51841,0.1) ;
#9961 = CYLINDRICAL_SURFACE('',#51845,1.45266329058736) ;
#9962 = CYLINDRICAL_SURFACE('',#51850,3.) ;
#9963 = CYLINDRICAL_SURFACE('',#51855,0.1) ;
#9964 = CYLINDRICAL_SURFACE('',#51858,0.1) ;
#9965 = CYLINDRICAL_SURFACE('',#51859,0.1) ;
#9966 = CYLINDRICAL_SURFACE('',#51860,0.1) ;
#9967 = CYLINDRICAL_SURFACE('',#51865,0.1) ;
#9968 = CYLINDRICAL_SURFACE('',#51866,0.1) ;
#9969 = CYLINDRICAL_SURFACE('',#51871,0.3) ;
#9970 = CYLINDRICAL_SURFACE('',#51881,0.3) ;
#9971 = CYLINDRICAL_SURFACE('',#51891,0.3) ;
#9972 = CYLINDRICAL_SURFACE('',#51901,0.3) ;
#9973 = CYLINDRICAL_SURFACE('',#51911,0.3) ;
#9974 = CYLINDRICAL_SURFACE('',#51921,0.3) ;
#9975 = CYLINDRICAL_SURFACE('',#51931,0.3) ;
#9976 = CYLINDRICAL_SURFACE('',#51941,0.3) ;
#9977 = CYLINDRICAL_SURFACE('',#51947,1.19999999999999) ;
#9978 = CYLINDRICAL_SURFACE('',#51949,1.19999999999999) ;
#9979 = CYLINDRICAL_SURFACE('',#51950,1.19999999999999) ;
#9980 = CYLINDRICAL_SURFACE('',#51952,1.19999999999999) ;
#9981 = CYLINDRICAL_SURFACE('',#51953,1.19999999999999) ;
#9982 = CYLINDRICAL_SURFACE('',#51955,1.19999999999999) ;
#9983 = CYLINDRICAL_SURFACE('',#51956,1.19999999999999) ;
#9984 = CYLINDRICAL_SURFACE('',#51958,1.19999999999999) ;
#9985 = CYLINDRICAL_SURFACE('',#51962,2.4) ;
#9986 = CYLINDRICAL_SURFACE('',#51965,1.45266329058736) ;
#9987 = CYLINDRICAL_SURFACE('',#51988,2.) ;
#9988 = CYLINDRICAL_SURFACE('',#51990,2.4) ;
#9989 = CYLINDRICAL_SURFACE('',#52000,2.49999999999999) ;
#9990 = CYLINDRICAL_SURFACE('',#52002,2.69999999999999) ;
#9991 = CYLINDRICAL_SURFACE('',#52010,2.5) ;
#9992 = CYLINDRICAL_SURFACE('',#52014,3.) ;
#9993 = CYLINDRICAL_SURFACE('',#52026,0.12) ;
#9994 = CYLINDRICAL_SURFACE('',#52036,0.12) ;
#9995 = CYLINDRICAL_SURFACE('',#52045,0.12) ;
#9996 = CYLINDRICAL_SURFACE('',#52046,0.12) ;
#9997 = CYLINDRICAL_SURFACE('',#52055,0.12) ;
#9998 = CYLINDRICAL_SURFACE('',#52065,0.12) ;
#9999 = CYLINDRICAL_SURFACE('',#52066,0.12) ;
#10000 = CYLINDRICAL_SURFACE('',#52075,0.12) ;
#10001 = CYLINDRICAL_SURFACE('',#52084,0.12) ;
#10002 = CYLINDRICAL_SURFACE('',#52085,0.12) ;
#10003 = CYLINDRICAL_SURFACE('',#52095,0.12) ;
#10004 = CYLINDRICAL_SURFACE('',#52104,0.12) ;
#10005 = CYLINDRICAL_SURFACE('',#52105,0.12) ;
#10006 = CYLINDRICAL_SURFACE('',#52114,0.12) ;
#10007 = CYLINDRICAL_SURFACE('',#52124,0.12) ;
#10008 = CYLINDRICAL_SURFACE('',#52125,0.12) ;
#10009 = CYLINDRICAL_SURFACE('',#52134,0.12) ;
#10010 = CYLINDRICAL_SURFACE('',#52135,0.12) ;
#10011 = CYLINDRICAL_SURFACE('',#52136,0.12) ;
#10012 = CYLINDRICAL_SURFACE('',#52137,0.12) ;
#10013 = CYLINDRICAL_SURFACE('',#52138,0.12) ;
#10014 = CYLINDRICAL_SURFACE('',#52139,0.12) ;
#10015 = CYLINDRICAL_SURFACE('',#52140,0.12) ;
#10016 = CYLINDRICAL_SURFACE('',#52141,0.12) ;
#10017 = CYLINDRICAL_SURFACE('',#52144,0.25) ;
#10018 = CYLINDRICAL_SURFACE('',#52146,0.25) ;
#10019 = CYLINDRICAL_SURFACE('',#52148,0.25) ;
#10020 = CYLINDRICAL_SURFACE('',#52150,0.25) ;
#10021 = CYLINDRICAL_SURFACE('',#52152,0.25) ;
#10022 = CYLINDRICAL_SURFACE('',#52155,0.25) ;
#10023 = CYLINDRICAL_SURFACE('',#52156,0.25) ;
#10024 = CYLINDRICAL_SURFACE('',#52157,0.25) ;
#10025 = CYLINDRICAL_SURFACE('',#52158,0.25) ;
#10026 = CYLINDRICAL_SURFACE('',#52159,0.25) ;
#10027 = CYLINDRICAL_SURFACE('',#52160,0.25) ;
#10028 = CYLINDRICAL_SURFACE('',#52161,0.25) ;
#10029 = CYLINDRICAL_SURFACE('',#52171,1.99999999999999) ;
#10030 = CYLINDRICAL_SURFACE('',#52192,0.1) ;
#10031 = CYLINDRICAL_SURFACE('',#52194,0.1) ;
#10032 = CYLINDRICAL_SURFACE('',#52203,0.1) ;
#10033 = CYLINDRICAL_SURFACE('',#52204,0.1) ;
#10034 = CYLINDRICAL_SURFACE('',#52205,0.1) ;
#10035 = CYLINDRICAL_SURFACE('',#52207,0.1) ;
#10036 = CYLINDRICAL_SURFACE('',#52208,0.1) ;
#10037 = CYLINDRICAL_SURFACE('',#52210,0.1) ;
#10038 = CYLINDRICAL_SURFACE('',#52211,0.1) ;
#10039 = CYLINDRICAL_SURFACE('',#52212,0.1) ;
#10040 = CYLINDRICAL_SURFACE('',#52225,2.) ;
#10041 = CYLINDRICAL_SURFACE('',#52229,0.1) ;
#10042 = CYLINDRICAL_SURFACE('',#52232,0.1) ;
#10043 = CYLINDRICAL_SURFACE('',#52234,0.1) ;
#10044 = CYLINDRICAL_SURFACE('',#52236,0.1) ;
#10045 = CYLINDRICAL_SURFACE('',#52238,0.1) ;
#10046 = CYLINDRICAL_SURFACE('',#52240,0.1) ;
#10047 = CYLINDRICAL_SURFACE('',#52243,0.1) ;
#10048 = CYLINDRICAL_SURFACE('',#52245,0.1) ;
#10049 = CYLINDRICAL_SURFACE('',#52246,0.1) ;
#10050 = CYLINDRICAL_SURFACE('',#52248,0.1) ;
#10051 = CYLINDRICAL_SURFACE('',#52250,0.1) ;
#10052 = CYLINDRICAL_SURFACE('',#52252,0.1) ;
#10053 = CYLINDRICAL_SURFACE('',#52261,0.1) ;
#10054 = CYLINDRICAL_SURFACE('',#52264,0.1) ;
#10055 = CYLINDRICAL_SURFACE('',#52266,0.1) ;
#10056 = CYLINDRICAL_SURFACE('',#52268,0.1) ;
#10057 = CYLINDRICAL_SURFACE('',#52270,0.1) ;
#10058 = CYLINDRICAL_SURFACE('',#52272,0.1) ;
#10059 = CYLINDRICAL_SURFACE('',#52274,0.1) ;
#10060 = CYLINDRICAL_SURFACE('',#52276,0.1) ;
#10061 = CYLINDRICAL_SURFACE('',#52278,0.1) ;
#10062 = CYLINDRICAL_SURFACE('',#52280,0.1) ;
#10063 = CYLINDRICAL_SURFACE('',#52282,0.1) ;
#10064 = CYLINDRICAL_SURFACE('',#52284,0.1) ;
#10065 = CYLINDRICAL_SURFACE('',#52295,0.1) ;
#10066 = CYLINDRICAL_SURFACE('',#52298,0.1) ;
#10067 = CYLINDRICAL_SURFACE('',#52300,0.1) ;
#10068 = CYLINDRICAL_SURFACE('',#52302,0.1) ;
#10069 = CYLINDRICAL_SURFACE('',#52304,0.1) ;
#10070 = CYLINDRICAL_SURFACE('',#52306,0.1) ;
#10071 = CYLINDRICAL_SURFACE('',#52308,0.1) ;
#10072 = CYLINDRICAL_SURFACE('',#52310,0.1) ;
#10073 = CYLINDRICAL_SURFACE('',#52312,0.1) ;
#10074 = CYLINDRICAL_SURFACE('',#52314,0.1) ;
#10075 = CYLINDRICAL_SURFACE('',#52316,0.1) ;
#10076 = CYLINDRICAL_SURFACE('',#52318,0.1) ;
#10077 = CYLINDRICAL_SURFACE('',#52331,2.49999999999999) ;
#10078 = CYLINDRICAL_SURFACE('',#52335,0.1) ;
#10079 = CYLINDRICAL_SURFACE('',#52338,0.1) ;
#10080 = CYLINDRICAL_SURFACE('',#52340,0.1) ;
#10081 = CYLINDRICAL_SURFACE('',#52342,0.1) ;
#10082 = CYLINDRICAL_SURFACE('',#52344,0.1) ;
#10083 = CYLINDRICAL_SURFACE('',#52346,0.1) ;
#10084 = CYLINDRICAL_SURFACE('',#52349,0.1) ;
#10085 = CYLINDRICAL_SURFACE('',#52351,0.1) ;
#10086 = CYLINDRICAL_SURFACE('',#52352,0.1) ;
#10087 = CYLINDRICAL_SURFACE('',#52354,0.1) ;
#10088 = CYLINDRICAL_SURFACE('',#52356,0.1) ;
#10089 = CYLINDRICAL_SURFACE('',#52358,0.1) ;
#10090 = CYLINDRICAL_SURFACE('',#52370,0.1) ;
#10091 = CYLINDRICAL_SURFACE('',#52373,0.1) ;
#10092 = CYLINDRICAL_SURFACE('',#52375,0.1) ;
#10093 = CYLINDRICAL_SURFACE('',#52377,0.1) ;
#10094 = CYLINDRICAL_SURFACE('',#52379,0.1) ;
#10095 = CYLINDRICAL_SURFACE('',#52381,0.1) ;
#10096 = CYLINDRICAL_SURFACE('',#52383,0.1) ;
#10097 = CYLINDRICAL_SURFACE('',#52385,0.1) ;
#10098 = CYLINDRICAL_SURFACE('',#52387,0.1) ;
#10099 = CYLINDRICAL_SURFACE('',#52389,0.1) ;
#10100 = CYLINDRICAL_SURFACE('',#52391,0.1) ;
#10101 = CYLINDRICAL_SURFACE('',#52393,0.1) ;
#10102 = CYLINDRICAL_SURFACE('',#52406,2.5) ;
#10103 = CYLINDRICAL_SURFACE('',#52410,0.1) ;
#10104 = CYLINDRICAL_SURFACE('',#52413,0.1) ;
#10105 = CYLINDRICAL_SURFACE('',#52415,0.1) ;
#10106 = CYLINDRICAL_SURFACE('',#52417,0.1) ;
#10107 = CYLINDRICAL_SURFACE('',#52419,0.1) ;
#10108 = CYLINDRICAL_SURFACE('',#52421,0.1) ;
#10109 = CYLINDRICAL_SURFACE('',#52424,0.1) ;
#10110 = CYLINDRICAL_SURFACE('',#52426,0.1) ;
#10111 = CYLINDRICAL_SURFACE('',#52427,0.1) ;
#10112 = CYLINDRICAL_SURFACE('',#52429,0.1) ;
#10113 = CYLINDRICAL_SURFACE('',#52431,0.1) ;
#10114 = CYLINDRICAL_SURFACE('',#52433,0.1) ;
#10115 = CYLINDRICAL_SURFACE('',#52453,0.05) ;
#10116 = CYLINDRICAL_SURFACE('',#52458,0.05) ;
#10117 = CYLINDRICAL_SURFACE('',#52468,0.05) ;
#10118 = CYLINDRICAL_SURFACE('',#52469,0.05) ;
#10119 = CYLINDRICAL_SURFACE('',#52474,0.05) ;
#10120 = CYLINDRICAL_SURFACE('',#52475,0.05) ;
#10121 = CYLINDRICAL_SURFACE('',#52485,0.05) ;
#10122 = CYLINDRICAL_SURFACE('',#52486,0.05) ;
#10123 = CYLINDRICAL_SURFACE('',#52487,0.05) ;
#10124 = CYLINDRICAL_SURFACE('',#52488,0.05) ;
#10125 = CYLINDRICAL_SURFACE('',#52489,0.05) ;
#10126 = CYLINDRICAL_SURFACE('',#52490,0.05) ;
#10127 = CYLINDRICAL_SURFACE('',#52504,0.05) ;
#10128 = CYLINDRICAL_SURFACE('',#52505,0.05) ;
#10129 = CYLINDRICAL_SURFACE('',#52511,0.05) ;
#10130 = CYLINDRICAL_SURFACE('',#52512,0.05) ;
#10131 = CYLINDRICAL_SURFACE('',#52514,0.05) ;
#10132 = CYLINDRICAL_SURFACE('',#52516,0.05) ;
#10133 = CYLINDRICAL_SURFACE('',#52518,0.05) ;
#10134 = CYLINDRICAL_SURFACE('',#52561,0.24) ;
#10135 = CYLINDRICAL_SURFACE('',#52566,0.24) ;
#10136 = CYLINDRICAL_SURFACE('',#52570,0.4) ;
#10137 = CYLINDRICAL_SURFACE('',#52576,0.24) ;
#10138 = CYLINDRICAL_SURFACE('',#52581,0.24) ;
#10139 = CYLINDRICAL_SURFACE('',#52587,0.4) ;
#10140 = CYLINDRICAL_SURFACE('',#52602,0.24) ;
#10141 = CYLINDRICAL_SURFACE('',#52607,0.3) ;
#10142 = CYLINDRICAL_SURFACE('',#52611,0.1) ;
#10143 = CYLINDRICAL_SURFACE('',#52618,0.24) ;
#10144 = CYLINDRICAL_SURFACE('',#52627,0.1) ;
#10145 = CYLINDRICAL_SURFACE('',#52629,0.1) ;
#10146 = CYLINDRICAL_SURFACE('',#52634,0.24) ;
#10147 = CYLINDRICAL_SURFACE('',#52636,0.24) ;
#10148 = CYLINDRICAL_SURFACE('',#52644,0.1) ;
#10149 = CYLINDRICAL_SURFACE('',#52646,0.24) ;
#10150 = CYLINDRICAL_SURFACE('',#52653,0.24) ;
#10151 = CYLINDRICAL_SURFACE('',#52656,0.2) ;
#10152 = CYLINDRICAL_SURFACE('',#52664,0.24) ;
#10153 = CYLINDRICAL_SURFACE('',#52665,0.1) ;
#10154 = CYLINDRICAL_SURFACE('',#52674,0.24) ;
#10155 = CYLINDRICAL_SURFACE('',#52675,0.1) ;
#10156 = CYLINDRICAL_SURFACE('',#52684,0.3) ;
#10157 = CYLINDRICAL_SURFACE('',#52689,0.3) ;
#10158 = CYLINDRICAL_SURFACE('',#52695,0.3) ;
#10159 = CYLINDRICAL_SURFACE('',#52697,0.1) ;
#10160 = CYLINDRICAL_SURFACE('',#52702,0.75) ;
#10161 = CYLINDRICAL_SURFACE('',#52707,0.1) ;
#10162 = CYLINDRICAL_SURFACE('',#52713,0.1) ;
#10163 = CYLINDRICAL_SURFACE('',#52723,0.1) ;
#10164 = CYLINDRICAL_SURFACE('',#52729,0.1) ;
#10165 = CYLINDRICAL_SURFACE('',#52730,0.1) ;
#10166 = CYLINDRICAL_SURFACE('',#52741,0.1) ;
#10167 = CYLINDRICAL_SURFACE('',#52744,0.1) ;
#10168 = CYLINDRICAL_SURFACE('',#52748,1.50000000000013) ;
#10169 = CYLINDRICAL_SURFACE('',#52751,0.1) ;
#10170 = CYLINDRICAL_SURFACE('',#52759,0.1) ;
#10171 = CYLINDRICAL_SURFACE('',#52763,0.1) ;
#10172 = CYLINDRICAL_SURFACE('',#52769,0.1) ;
#10173 = CYLINDRICAL_SURFACE('',#52777,0.1) ;
#10174 = CYLINDRICAL_SURFACE('',#52782,0.1) ;
#10175 = CYLINDRICAL_SURFACE('',#52788,0.1) ;
#10176 = CYLINDRICAL_SURFACE('',#52793,0.700000000000003) ;
#10177 = CYLINDRICAL_SURFACE('',#52796,3.89999999999982) ;
#10178 = CYLINDRICAL_SURFACE('',#52799,3.89999999999997) ;
#10179 = CYLINDRICAL_SURFACE('',#52801,0.1) ;
#10180 = CYLINDRICAL_SURFACE('',#52807,0.1) ;
#10181 = CYLINDRICAL_SURFACE('',#52817,0.4) ;
#10182 = CYLINDRICAL_SURFACE('',#52822,0.1) ;
#10183 = CYLINDRICAL_SURFACE('',#52824,0.1) ;
#10184 = CYLINDRICAL_SURFACE('',#52828,0.1) ;
#10185 = CYLINDRICAL_SURFACE('',#52830,0.1) ;
#10186 = CYLINDRICAL_SURFACE('',#52831,2.) ;
#10187 = CYLINDRICAL_SURFACE('',#52842,0.1) ;
#10188 = CYLINDRICAL_SURFACE('',#52844,0.1) ;
#10189 = CYLINDRICAL_SURFACE('',#52846,0.1) ;
#10190 = CYLINDRICAL_SURFACE('',#52852,0.1) ;
#10191 = CYLINDRICAL_SURFACE('',#52853,0.1) ;
#10192 = CYLINDRICAL_SURFACE('',#52859,0.1) ;
#10193 = CYLINDRICAL_SURFACE('',#52860,0.1) ;
#10194 = CYLINDRICAL_SURFACE('',#52861,0.1) ;
#10195 = CYLINDRICAL_SURFACE('',#52930,0.1) ;
#10196 = CYLINDRICAL_SURFACE('',#52936,0.1) ;
#10197 = CYLINDRICAL_SURFACE('',#52938,2.9) ;
#10198 = CYLINDRICAL_SURFACE('',#52939,3.99999999999997) ;
#10199 = CYLINDRICAL_SURFACE('',#52947,0.1) ;
#10200 = CYLINDRICAL_SURFACE('',#52953,0.1) ;
#10201 = CYLINDRICAL_SURFACE('',#52959,0.1) ;
#10202 = CYLINDRICAL_SURFACE('',#52960,0.1) ;
#10203 = CYLINDRICAL_SURFACE('',#52966,0.1) ;
#10204 = CYLINDRICAL_SURFACE('',#52976,0.1) ;
#10205 = CYLINDRICAL_SURFACE('',#52981,0.1) ;
#10206 = CYLINDRICAL_SURFACE('',#52982,0.1) ;
#10207 = CYLINDRICAL_SURFACE('',#52983,0.1) ;
#10208 = CYLINDRICAL_SURFACE('',#52988,0.1) ;
#10209 = CYLINDRICAL_SURFACE('',#52994,0.599999999999915) ;
#10210 = CYLINDRICAL_SURFACE('',#52997,1.) ;
#10211 = CYLINDRICAL_SURFACE('',#53003,0.499999999999901) ;
#10212 = CYLINDRICAL_SURFACE('',#53006,0.200000000000106) ;
#10213 = CYLINDRICAL_SURFACE('',#53008,0.999999999999996) ;
#10214 = CYLINDRICAL_SURFACE('',#53013,0.1) ;
#10215 = CYLINDRICAL_SURFACE('',#53020,0.1) ;
#10216 = CYLINDRICAL_SURFACE('',#53036,0.1) ;
#10217 = CYLINDRICAL_SURFACE('',#53037,0.1) ;
#10218 = CYLINDRICAL_SURFACE('',#53042,0.1) ;
#10219 = CYLINDRICAL_SURFACE('',#53043,0.1) ;
#10220 = CYLINDRICAL_SURFACE('',#53048,0.1) ;
#10221 = CYLINDRICAL_SURFACE('',#53053,0.1) ;
#10222 = CYLINDRICAL_SURFACE('',#53054,0.1) ;
#10223 = CYLINDRICAL_SURFACE('',#53056,0.1) ;
#10224 = CYLINDRICAL_SURFACE('',#53062,0.1) ;
#10225 = CYLINDRICAL_SURFACE('',#53068,0.1) ;
#10226 = CYLINDRICAL_SURFACE('',#53074,0.1) ;
#10227 = CYLINDRICAL_SURFACE('',#53080,0.1) ;
#10228 = CYLINDRICAL_SURFACE('',#53081,0.1) ;
#10229 = CYLINDRICAL_SURFACE('',#53085,0.1) ;
#10230 = CYLINDRICAL_SURFACE('',#53087,0.5) ;
#10231 = CYLINDRICAL_SURFACE('',#53089,0.5) ;
#10232 = CYLINDRICAL_SURFACE('',#53090,0.4) ;
#10233 = CYLINDRICAL_SURFACE('',#53092,0.199999999999996) ;
#10234 = CYLINDRICAL_SURFACE('',#53094,0.200000000000031) ;
#10235 = CYLINDRICAL_SURFACE('',#53095,0.4) ;
#10236 = CYLINDRICAL_SURFACE('',#53103,0.1) ;
#10237 = CYLINDRICAL_SURFACE('',#53107,0.1) ;
#10238 = CYLINDRICAL_SURFACE('',#53120,0.1) ;
#10239 = CYLINDRICAL_SURFACE('',#53121,0.1) ;
#10240 = CYLINDRICAL_SURFACE('',#53128,0.1) ;
#10241 = CYLINDRICAL_SURFACE('',#53129,0.1) ;
#10242 = CYLINDRICAL_SURFACE('',#53131,0.1) ;
#10243 = CYLINDRICAL_SURFACE('',#53133,0.1) ;
#10244 = CYLINDRICAL_SURFACE('',#53139,0.1) ;
#10245 = CYLINDRICAL_SURFACE('',#53141,0.500000000000007) ;
#10246 = CYLINDRICAL_SURFACE('',#53148,0.500000000000007) ;
#10247 = CYLINDRICAL_SURFACE('',#53151,0.1) ;
#10248 = CYLINDRICAL_SURFACE('',#53156,0.1) ;
#10249 = CYLINDRICAL_SURFACE('',#53160,0.1) ;
#10250 = CYLINDRICAL_SURFACE('',#53165,0.1) ;
#10251 = CYLINDRICAL_SURFACE('',#53170,0.1) ;
#10252 = CYLINDRICAL_SURFACE('',#53175,0.1) ;
#10253 = CYLINDRICAL_SURFACE('',#53180,0.1) ;
#10254 = CYLINDRICAL_SURFACE('',#53184,0.1) ;
#10255 = CYLINDRICAL_SURFACE('',#53193,0.1) ;
#10256 = CYLINDRICAL_SURFACE('',#53198,0.1) ;
#10257 = CYLINDRICAL_SURFACE('',#53206,0.1) ;
#10258 = CYLINDRICAL_SURFACE('',#53210,0.1) ;
#10259 = CYLINDRICAL_SURFACE('',#53215,1.50000000000004) ;
#10260 = CYLINDRICAL_SURFACE('',#53218,1.) ;
#10261 = CYLINDRICAL_SURFACE('',#53219,0.600000000000129) ;
#10262 = CYLINDRICAL_SURFACE('',#53221,0.600000000000129) ;
#10263 = CYLINDRICAL_SURFACE('',#53222,0.1) ;
#10264 = CYLINDRICAL_SURFACE('',#53224,0.1) ;
#10265 = CYLINDRICAL_SURFACE('',#53226,0.1) ;
#10266 = CYLINDRICAL_SURFACE('',#53231,0.1) ;
#10267 = CYLINDRICAL_SURFACE('',#53235,0.1) ;
#10268 = CYLINDRICAL_SURFACE('',#53240,0.1) ;
#10269 = CYLINDRICAL_SURFACE('',#53244,0.1) ;
#10270 = CYLINDRICAL_SURFACE('',#53249,0.1) ;
#10271 = CYLINDRICAL_SURFACE('',#53251,0.1) ;
#10272 = CYLINDRICAL_SURFACE('',#53258,0.1) ;
#10273 = CYLINDRICAL_SURFACE('',#53263,0.1) ;
#10274 = CYLINDRICAL_SURFACE('',#53268,0.1) ;
#10275 = CYLINDRICAL_SURFACE('',#53271,0.75) ;
#10276 = CYLINDRICAL_SURFACE('',#53276,0.5) ;
#10277 = CYLINDRICAL_SURFACE('',#53283,0.4) ;
#10278 = CYLINDRICAL_SURFACE('',#53295,0.1) ;
#10279 = CYLINDRICAL_SURFACE('',#53302,0.1) ;
#10280 = CYLINDRICAL_SURFACE('',#53303,0.1) ;
#10281 = CYLINDRICAL_SURFACE('',#53305,0.1) ;
#10282 = CYLINDRICAL_SURFACE('',#53306,0.1) ;
#10283 = CYLINDRICAL_SURFACE('',#53308,0.1) ;
#10284 = CYLINDRICAL_SURFACE('',#53312,0.4) ;
#10285 = CYLINDRICAL_SURFACE('',#53315,0.75) ;
#10286 = CYLINDRICAL_SURFACE('',#53318,0.75) ;
#10287 = CYLINDRICAL_SURFACE('',#53321,0.1) ;
#10288 = CYLINDRICAL_SURFACE('',#53324,0.1) ;
#10289 = CYLINDRICAL_SURFACE('',#53331,0.2) ;
#10290 = CYLINDRICAL_SURFACE('',#53338,0.2) ;
#10291 = CYLINDRICAL_SURFACE('',#53339,0.5) ;
#10292 = CYLINDRICAL_SURFACE('',#53344,0.2) ;
#10293 = CYLINDRICAL_SURFACE('',#53357,0.75) ;
#10294 = CYLINDRICAL_SURFACE('',#53361,0.2) ;
#10295 = CYLINDRICAL_SURFACE('',#53365,0.2) ;
#10296 = CYLINDRICAL_SURFACE('',#53366,0.2) ;
#10297 = CYLINDRICAL_SURFACE('',#53371,0.2) ;
#10298 = CYLINDRICAL_SURFACE('',#53376,0.75) ;
#10299 = CYLINDRICAL_SURFACE('',#53377,6.15) ;
#10300 = CYLINDRICAL_SURFACE('',#53381,0.75) ;
#10301 = CYLINDRICAL_SURFACE('',#53383,0.75) ;
#10302 = CYLINDRICAL_SURFACE('',#53385,3.6) ;
#10303 = CYLINDRICAL_SURFACE('',#53388,3.6) ;
#10304 = CYLINDRICAL_SURFACE('',#53391,3.6) ;
#10305 = CYLINDRICAL_SURFACE('',#53402,0.1) ;
#10306 = CYLINDRICAL_SURFACE('',#53405,0.1) ;
#10307 = CYLINDRICAL_SURFACE('',#53415,0.1) ;
#10308 = CYLINDRICAL_SURFACE('',#53417,0.1) ;
#10309 = CYLINDRICAL_SURFACE('',#53418,0.1) ;
#10310 = CYLINDRICAL_SURFACE('',#53420,0.1) ;
#10311 = CYLINDRICAL_SURFACE('',#53422,0.1) ;
#10312 = CYLINDRICAL_SURFACE('',#53428,0.1) ;
#10313 = CYLINDRICAL_SURFACE('',#53430,0.1) ;
#10314 = CYLINDRICAL_SURFACE('',#53432,0.1) ;
#10315 = CYLINDRICAL_SURFACE('',#53434,0.1) ;
#10316 = CYLINDRICAL_SURFACE('',#53435,0.1) ;
#10317 = CYLINDRICAL_SURFACE('',#53439,0.1) ;
#10318 = CYLINDRICAL_SURFACE('',#53442,0.1) ;
#10319 = CYLINDRICAL_SURFACE('',#53444,0.1) ;
#10320 = CYLINDRICAL_SURFACE('',#53446,0.1) ;
#10321 = CYLINDRICAL_SURFACE('',#53448,0.1) ;
#10322 = CYLINDRICAL_SURFACE('',#53450,0.1) ;
#10323 = CYLINDRICAL_SURFACE('',#53452,0.1) ;
#10324 = CYLINDRICAL_SURFACE('',#53458,0.1) ;
#10325 = CYLINDRICAL_SURFACE('',#53461,0.1) ;
#10326 = CYLINDRICAL_SURFACE('',#53463,0.1) ;
#10327 = CYLINDRICAL_SURFACE('',#53465,0.1) ;
#10328 = CYLINDRICAL_SURFACE('',#53469,0.1) ;
#10329 = CYLINDRICAL_SURFACE('',#53472,0.1) ;
#10330 = CYLINDRICAL_SURFACE('',#53474,0.1) ;
#10331 = CYLINDRICAL_SURFACE('',#53476,0.1) ;
#10332 = CYLINDRICAL_SURFACE('',#53478,0.1) ;
#10333 = CYLINDRICAL_SURFACE('',#53480,0.1) ;
#10334 = CYLINDRICAL_SURFACE('',#53482,0.1) ;
#10335 = CYLINDRICAL_SURFACE('',#53488,0.1) ;
#10336 = CYLINDRICAL_SURFACE('',#53491,0.1) ;
#10337 = CYLINDRICAL_SURFACE('',#53493,0.1) ;
#10338 = CYLINDRICAL_SURFACE('',#53495,0.1) ;
#10339 = CYLINDRICAL_SURFACE('',#53499,0.1) ;
#10340 = CYLINDRICAL_SURFACE('',#53502,0.1) ;
#10341 = CYLINDRICAL_SURFACE('',#53504,0.1) ;
#10342 = CYLINDRICAL_SURFACE('',#53510,0.1) ;
#10343 = CYLINDRICAL_SURFACE('',#53512,0.1) ;
#10344 = CYLINDRICAL_SURFACE('',#53514,0.1) ;
#10345 = CYLINDRICAL_SURFACE('',#53520,0.1) ;
#10346 = CYLINDRICAL_SURFACE('',#53522,0.1) ;
#10347 = CYLINDRICAL_SURFACE('',#53524,0.1) ;
#10348 = CYLINDRICAL_SURFACE('',#53526,0.299999999999963) ;
#10349 = CYLINDRICAL_SURFACE('',#53533,0.1) ;
#10350 = CYLINDRICAL_SURFACE('',#53536,0.1) ;
#10351 = CYLINDRICAL_SURFACE('',#53542,0.1) ;
#10352 = CYLINDRICAL_SURFACE('',#53544,0.1) ;
#10353 = CYLINDRICAL_SURFACE('',#53546,0.1) ;
#10354 = CYLINDRICAL_SURFACE('',#53552,0.1) ;
#10355 = CYLINDRICAL_SURFACE('',#53554,0.1) ;
#10356 = CYLINDRICAL_SURFACE('',#53556,0.1) ;
#10357 = CYLINDRICAL_SURFACE('',#53558,0.1) ;
#10358 = CYLINDRICAL_SURFACE('',#53559,0.299999999999963) ;
#10359 = CYLINDRICAL_SURFACE('',#53567,0.1) ;
#10360 = CYLINDRICAL_SURFACE('',#53568,0.1) ;
#10361 = CYLINDRICAL_SURFACE('',#53570,0.1) ;
#10362 = CYLINDRICAL_SURFACE('',#53572,0.1) ;
#10363 = CYLINDRICAL_SURFACE('',#53574,0.1) ;
#10364 = CYLINDRICAL_SURFACE('',#53576,0.1) ;
#10365 = CYLINDRICAL_SURFACE('',#53578,0.1) ;
#10366 = CYLINDRICAL_SURFACE('',#53581,0.1) ;
#10367 = CYLINDRICAL_SURFACE('',#53582,0.1) ;
#10368 = CYLINDRICAL_SURFACE('',#53583,0.1) ;
#10369 = CYLINDRICAL_SURFACE('',#53586,0.1) ;
#10370 = CYLINDRICAL_SURFACE('',#53589,0.1) ;
#10371 = CYLINDRICAL_SURFACE('',#53591,0.1) ;
#10372 = CYLINDRICAL_SURFACE('',#53593,0.1) ;
#10373 = CYLINDRICAL_SURFACE('',#53595,0.1) ;
#10374 = CYLINDRICAL_SURFACE('',#53597,0.1) ;
#10375 = CYLINDRICAL_SURFACE('',#53599,0.1) ;
#10376 = CYLINDRICAL_SURFACE('',#53609,0.1) ;
#10377 = CYLINDRICAL_SURFACE('',#53612,0.1) ;
#10378 = CYLINDRICAL_SURFACE('',#53614,0.1) ;
#10379 = CYLINDRICAL_SURFACE('',#53616,0.1) ;
#10380 = CYLINDRICAL_SURFACE('',#53618,0.1) ;
#10381 = CYLINDRICAL_SURFACE('',#53621,0.1) ;
#10382 = CYLINDRICAL_SURFACE('',#53623,0.1) ;
#10383 = CYLINDRICAL_SURFACE('',#53625,0.1) ;
#10384 = CYLINDRICAL_SURFACE('',#53627,0.1) ;
#10385 = CYLINDRICAL_SURFACE('',#53629,0.1) ;
#10386 = CYLINDRICAL_SURFACE('',#53631,0.1) ;
#10387 = CYLINDRICAL_SURFACE('',#53634,0.1) ;
#10388 = CYLINDRICAL_SURFACE('',#53637,0.1) ;
#10389 = CYLINDRICAL_SURFACE('',#53639,0.1) ;
#10390 = CYLINDRICAL_SURFACE('',#53641,0.1) ;
#10391 = CYLINDRICAL_SURFACE('',#53642,0.1) ;
#10392 = CYLINDRICAL_SURFACE('',#53645,0.1) ;
#10393 = CYLINDRICAL_SURFACE('',#53647,0.1) ;
#10394 = CYLINDRICAL_SURFACE('',#53649,0.1) ;
#10395 = CYLINDRICAL_SURFACE('',#53651,0.1) ;
#10396 = CYLINDRICAL_SURFACE('',#53653,0.1) ;
#10397 = CYLINDRICAL_SURFACE('',#53658,0.1) ;
#10398 = CYLINDRICAL_SURFACE('',#53662,0.1) ;
#10399 = CYLINDRICAL_SURFACE('',#53665,0.699999999999972) ;
#10400 = CYLINDRICAL_SURFACE('',#53668,0.1) ;
#10401 = CYLINDRICAL_SURFACE('',#53671,0.1) ;
#10402 = CYLINDRICAL_SURFACE('',#53674,0.1) ;
#10403 = CYLINDRICAL_SURFACE('',#53676,0.1) ;
#10404 = CYLINDRICAL_SURFACE('',#53678,0.1) ;
#10405 = CYLINDRICAL_SURFACE('',#53680,0.1) ;
#10406 = CYLINDRICAL_SURFACE('',#53685,0.1) ;
#10407 = CYLINDRICAL_SURFACE('',#53686,0.1) ;
#10408 = CYLINDRICAL_SURFACE('',#53690,0.1) ;
#10409 = CYLINDRICAL_SURFACE('',#53694,0.699999999999972) ;
#10410 = CYLINDRICAL_SURFACE('',#53707,2.99999999999998) ;
#10411 = CYLINDRICAL_SURFACE('',#53710,1.60000000000004) ;
#10412 = CYLINDRICAL_SURFACE('',#53717,0.500000000000043) ;
#10413 = CYLINDRICAL_SURFACE('',#53728,1.5) ;
#10414 = CYLINDRICAL_SURFACE('',#53733,0.399999999999992) ;
#10415 = CYLINDRICAL_SURFACE('',#53740,0.4) ;
#10416 = CYLINDRICAL_SURFACE('',#53743,0.4) ;
#10417 = CYLINDRICAL_SURFACE('',#53749,0.5) ;
#10418 = CYLINDRICAL_SURFACE('',#53758,0.5) ;
#10419 = CYLINDRICAL_SURFACE('',#53764,0.5) ;
#10420 = CYLINDRICAL_SURFACE('',#53765,0.5) ;
#10421 = CYLINDRICAL_SURFACE('',#53771,0.5) ;
#10422 = CYLINDRICAL_SURFACE('',#53777,0.5) ;
#10423 = CYLINDRICAL_SURFACE('',#53787,0.5) ;
#10424 = CYLINDRICAL_SURFACE('',#53790,0.5) ;
#10425 = CYLINDRICAL_SURFACE('',#53795,0.5) ;
#10426 = CYLINDRICAL_SURFACE('',#53801,0.5) ;
#10427 = CYLINDRICAL_SURFACE('',#53802,0.5) ;
#10428 = CYLINDRICAL_SURFACE('',#53807,0.5) ;
#10429 = CYLINDRICAL_SURFACE('',#53816,0.5) ;
#10430 = CYLINDRICAL_SURFACE('',#53818,0.5) ;
#10431 = CYLINDRICAL_SURFACE('',#53823,0.5) ;
#10432 = CYLINDRICAL_SURFACE('',#53825,4.06491106406736) ;
#10433 = CYLINDRICAL_SURFACE('',#53827,1.) ;
#10434 = CYLINDRICAL_SURFACE('',#53830,0.500000000000043) ;
#10435 = CYLINDRICAL_SURFACE('',#53832,4.06491106406736) ;
#10436 = CYLINDRICAL_SURFACE('',#53833,4.06491106406736) ;
#10437 = CYLINDRICAL_SURFACE('',#53835,0.200000000000031) ;
#10438 = CYLINDRICAL_SURFACE('',#53839,0.199999999999996) ;
#10439 = CYLINDRICAL_SURFACE('',#53842,0.199999999999996) ;
#10440 = CYLINDRICAL_SURFACE('',#53847,0.200000000000031) ;
#10441 = CYLINDRICAL_SURFACE('',#53850,0.2) ;
#10442 = CYLINDRICAL_SURFACE('',#53851,2.6) ;
#10443 = CYLINDRICAL_SURFACE('',#53854,0.200000000000001) ;
#10444 = CYLINDRICAL_SURFACE('',#53857,0.199999999999996) ;
#10445 = CYLINDRICAL_SURFACE('',#53860,0.199999999999996) ;
#10446 = CYLINDRICAL_SURFACE('',#53863,0.199999999999996) ;
#10447 = CYLINDRICAL_SURFACE('',#53867,0.199999999999996) ;
#10448 = CYLINDRICAL_SURFACE('',#53870,2.49999999999999) ;
#10449 = CYLINDRICAL_SURFACE('',#53873,0.199999999999995) ;
#10450 = CYLINDRICAL_SURFACE('',#53876,0.199999999999996) ;
#10451 = CYLINDRICAL_SURFACE('',#53879,0.199999999999996) ;
#10452 = CYLINDRICAL_SURFACE('',#53882,0.199999999999996) ;
#10453 = CYLINDRICAL_SURFACE('',#53887,0.100000000000016) ;
#10454 = CYLINDRICAL_SURFACE('',#53890,0.0999999999999979) ;
#10455 = CYLINDRICAL_SURFACE('',#53893,0.100000000000051) ;
#10456 = CYLINDRICAL_SURFACE('',#53895,0.199999999999996) ;
#10457 = CYLINDRICAL_SURFACE('',#53898,0.199999999999996) ;
#10458 = CYLINDRICAL_SURFACE('',#53902,0.199999999999996) ;
#10459 = CYLINDRICAL_SURFACE('',#53905,0.199999999999996) ;
#10460 = CYLINDRICAL_SURFACE('',#53909,0.199999999999996) ;
#10461 = CYLINDRICAL_SURFACE('',#53912,0.199999999999996) ;
#10462 = CYLINDRICAL_SURFACE('',#53918,0.199999999999995) ;
#10463 = CYLINDRICAL_SURFACE('',#53921,0.199999999999996) ;
#10464 = CYLINDRICAL_SURFACE('',#53926,0.199999999999996) ;
#10465 = CYLINDRICAL_SURFACE('',#53929,0.200000000000031) ;
#10466 = CYLINDRICAL_SURFACE('',#53933,0.199999999999996) ;
#10467 = CYLINDRICAL_SURFACE('',#53940,0.200000000000031) ;
#10468 = CYLINDRICAL_SURFACE('',#53944,0.199999999999996) ;
#10469 = CYLINDRICAL_SURFACE('',#53948,0.199999999999996) ;
#10470 = CYLINDRICAL_SURFACE('',#53951,0.199999999999996) ;
#10471 = CYLINDRICAL_SURFACE('',#53955,0.0999999999999973) ;
#10472 = CYLINDRICAL_SURFACE('',#53958,0.0999999999999979) ;
#10473 = CYLINDRICAL_SURFACE('',#53961,0.100000000000004) ;
#10474 = CYLINDRICAL_SURFACE('',#53966,0.199999999999996) ;
#10475 = CYLINDRICAL_SURFACE('',#53977,0.500000000000114) ;
#10476 = CYLINDRICAL_SURFACE('',#53979,0.500000000000025) ;
#10477 = CYLINDRICAL_SURFACE('',#53984,0.199999999999996) ;
#10478 = CYLINDRICAL_SURFACE('',#53986,4.49999999999997) ;
#10479 = CYLINDRICAL_SURFACE('',#53992,1.) ;
#10480 = CYLINDRICAL_SURFACE('',#53994,1.) ;
#10481 = CYLINDRICAL_SURFACE('',#53997,1.) ;
#10482 = CYLINDRICAL_SURFACE('',#53998,2.) ;
#10483 = CYLINDRICAL_SURFACE('',#54000,4.06491106406736) ;
#10484 = CYLINDRICAL_SURFACE('',#54002,4.05) ;
#10485 = CYLINDRICAL_SURFACE('',#54005,4.05) ;
#10486 = CYLINDRICAL_SURFACE('',#54028,1.67775) ;
#10487 = CYLINDRICAL_SURFACE('',#54030,1.67775) ;
#10488 = CYLINDRICAL_SURFACE('',#54031,1.67775) ;
#10489 = CYLINDRICAL_SURFACE('',#54032,1.67775) ;
#10490 = CYLINDRICAL_SURFACE('',#54033,1.9635) ;
#10491 = CYLINDRICAL_SURFACE('',#54037,1.67775) ;
#10492 = CYLINDRICAL_SURFACE('',#54060,0.15) ;
#10493 = CYLINDRICAL_SURFACE('',#54064,0.15) ;
#10494 = CYLINDRICAL_SURFACE('',#54068,0.15) ;
#10495 = CYLINDRICAL_SURFACE('',#54072,0.15) ;
#10496 = CYLINDRICAL_SURFACE('',#54076,0.15) ;
#10497 = CYLINDRICAL_SURFACE('',#54080,0.15) ;
#10498 = CYLINDRICAL_SURFACE('',#54084,0.15) ;
#10499 = CYLINDRICAL_SURFACE('',#54088,0.15) ;
#10500 = CYLINDRICAL_SURFACE('',#54092,0.15) ;
#10501 = CYLINDRICAL_SURFACE('',#54096,0.15) ;
#10502 = CYLINDRICAL_SURFACE('',#54100,0.15) ;
#10503 = CYLINDRICAL_SURFACE('',#54104,0.15) ;
#10504 = CYLINDRICAL_SURFACE('',#54108,0.15) ;
#10505 = CYLINDRICAL_SURFACE('',#54112,0.15) ;
#10506 = CYLINDRICAL_SURFACE('',#54116,0.15) ;
#10507 = CYLINDRICAL_SURFACE('',#54120,0.15) ;
#10508 = CYLINDRICAL_SURFACE('',#54124,0.15) ;
#10509 = CYLINDRICAL_SURFACE('',#54128,0.15) ;
#10510 = CYLINDRICAL_SURFACE('',#54132,0.15) ;
#10511 = CYLINDRICAL_SURFACE('',#54136,0.15) ;
#10512 = CYLINDRICAL_SURFACE('',#54140,0.15) ;
#10513 = CYLINDRICAL_SURFACE('',#54144,0.15) ;
#10514 = CYLINDRICAL_SURFACE('',#54148,0.15) ;
#10515 = CYLINDRICAL_SURFACE('',#54152,0.15) ;
#10516 = CYLINDRICAL_SURFACE('',#54156,0.15) ;
#10517 = CYLINDRICAL_SURFACE('',#54160,0.15) ;
#10518 = CYLINDRICAL_SURFACE('',#54164,0.15) ;
#10519 = CYLINDRICAL_SURFACE('',#54168,0.15) ;
#10520 = CYLINDRICAL_SURFACE('',#54172,0.15) ;
#10521 = CYLINDRICAL_SURFACE('',#54176,0.15) ;
#10522 = CYLINDRICAL_SURFACE('',#54180,0.15) ;
#10523 = CYLINDRICAL_SURFACE('',#54184,0.15) ;
#10524 = CYLINDRICAL_SURFACE('',#54188,0.15) ;
#10525 = CYLINDRICAL_SURFACE('',#54192,0.15) ;
#10526 = CYLINDRICAL_SURFACE('',#54196,0.15) ;
#10527 = CYLINDRICAL_SURFACE('',#54200,0.15) ;
#10528 = CYLINDRICAL_SURFACE('',#54204,0.15) ;
#10529 = CYLINDRICAL_SURFACE('',#54208,0.15) ;
#10530 = CYLINDRICAL_SURFACE('',#54212,0.15) ;
#10531 = CYLINDRICAL_SURFACE('',#54216,0.15) ;
#10532 = CYLINDRICAL_SURFACE('',#54218,0.500000000000003) ;
#10533 = CYLINDRICAL_SURFACE('',#54221,5.1) ;
#10534 = CYLINDRICAL_SURFACE('',#54224,0.500000000000003) ;
#10535 = CYLINDRICAL_SURFACE('',#54227,5.1) ;
#10536 = CYLINDRICAL_SURFACE('',#54230,0.500000000000003) ;
#10537 = CYLINDRICAL_SURFACE('',#54233,5.1) ;
#10538 = CYLINDRICAL_SURFACE('',#54236,0.500000000000003) ;
#10539 = CYLINDRICAL_SURFACE('',#54239,5.1) ;
#10540 = CYLINDRICAL_SURFACE('',#54242,0.500000000000003) ;
#10541 = CYLINDRICAL_SURFACE('',#54245,5.1) ;
#10542 = CYLINDRICAL_SURFACE('',#54248,0.500000000000003) ;
#10543 = CYLINDRICAL_SURFACE('',#54251,5.1) ;
#10544 = CYLINDRICAL_SURFACE('',#54254,0.500000000000003) ;
#10545 = CYLINDRICAL_SURFACE('',#54257,5.1) ;
#10546 = CYLINDRICAL_SURFACE('',#54260,0.500000000000003) ;
#10547 = CYLINDRICAL_SURFACE('',#54263,5.1) ;
#10548 = CYLINDRICAL_SURFACE('',#54266,0.500000000000003) ;
#10549 = CYLINDRICAL_SURFACE('',#54269,5.1) ;
#10550 = CYLINDRICAL_SURFACE('',#54272,0.500000000000003) ;
#10551 = CYLINDRICAL_SURFACE('',#54275,5.1) ;
#10552 = CYLINDRICAL_SURFACE('',#54405,0.15) ;
#10553 = CYLINDRICAL_SURFACE('',#54406,0.15) ;
#10554 = CYLINDRICAL_SURFACE('',#54407,0.15) ;
#10555 = CYLINDRICAL_SURFACE('',#54409,0.15) ;
#10556 = CYLINDRICAL_SURFACE('',#54410,0.15) ;
#10557 = CYLINDRICAL_SURFACE('',#54411,0.15) ;
#10558 = CYLINDRICAL_SURFACE('',#54413,0.15) ;
#10559 = CYLINDRICAL_SURFACE('',#54414,0.15) ;
#10560 = CYLINDRICAL_SURFACE('',#54415,0.15) ;
#10561 = CYLINDRICAL_SURFACE('',#54417,0.15) ;
#10562 = CYLINDRICAL_SURFACE('',#54418,0.15) ;
#10563 = CYLINDRICAL_SURFACE('',#54419,0.15) ;
#10564 = CYLINDRICAL_SURFACE('',#54421,0.15) ;
#10565 = CYLINDRICAL_SURFACE('',#54422,0.15) ;
#10566 = CYLINDRICAL_SURFACE('',#54423,0.15) ;
#10567 = CYLINDRICAL_SURFACE('',#54425,0.15) ;
#10568 = CYLINDRICAL_SURFACE('',#54426,0.15) ;
#10569 = CYLINDRICAL_SURFACE('',#54427,0.15) ;
#10570 = CYLINDRICAL_SURFACE('',#54429,0.15) ;
#10571 = CYLINDRICAL_SURFACE('',#54430,0.15) ;
#10572 = CYLINDRICAL_SURFACE('',#54431,0.15) ;
#10573 = CYLINDRICAL_SURFACE('',#54433,0.15) ;
#10574 = CYLINDRICAL_SURFACE('',#54434,0.15) ;
#10575 = CYLINDRICAL_SURFACE('',#54435,0.15) ;
#10576 = CYLINDRICAL_SURFACE('',#54437,0.15) ;
#10577 = CYLINDRICAL_SURFACE('',#54438,0.15) ;
#10578 = CYLINDRICAL_SURFACE('',#54439,0.15) ;
#10579 = CYLINDRICAL_SURFACE('',#54441,0.15) ;
#10580 = CYLINDRICAL_SURFACE('',#54442,0.15) ;
#10581 = CYLINDRICAL_SURFACE('',#54443,0.15) ;
#10582 = CYLINDRICAL_SURFACE('',#54445,0.15) ;
#10583 = CYLINDRICAL_SURFACE('',#54450,0.15) ;
#10584 = CYLINDRICAL_SURFACE('',#54456,0.15) ;
#10585 = CYLINDRICAL_SURFACE('',#54462,0.15) ;
#10586 = CYLINDRICAL_SURFACE('',#54468,0.15) ;
#10587 = CYLINDRICAL_SURFACE('',#54474,0.15) ;
#10588 = CYLINDRICAL_SURFACE('',#54480,0.15) ;
#10589 = CYLINDRICAL_SURFACE('',#54486,0.15) ;
#10590 = CYLINDRICAL_SURFACE('',#54492,0.15) ;
#10591 = CYLINDRICAL_SURFACE('',#54498,0.15) ;
#10592 = CYLINDRICAL_SURFACE('',#54503,5.1) ;
#10593 = CYLINDRICAL_SURFACE('',#54505,0.500000000000003) ;
#10594 = CYLINDRICAL_SURFACE('',#54509,0.500000000000003) ;
#10595 = CYLINDRICAL_SURFACE('',#54512,0.500000000000003) ;
#10596 = CYLINDRICAL_SURFACE('',#54515,0.500000000000003) ;
#10597 = CYLINDRICAL_SURFACE('',#54518,0.500000000000003) ;
#10598 = CYLINDRICAL_SURFACE('',#54521,0.500000000000003) ;
#10599 = CYLINDRICAL_SURFACE('',#54524,0.500000000000003) ;
#10600 = CYLINDRICAL_SURFACE('',#54527,0.500000000000003) ;
#10601 = CYLINDRICAL_SURFACE('',#54530,0.500000000000003) ;
#10602 = CYLINDRICAL_SURFACE('',#54533,0.500000000000003) ;
#10603 = CYLINDRICAL_SURFACE('',#54534,5.1) ;
#10604 = CYLINDRICAL_SURFACE('',#54535,5.1) ;
#10605 = CYLINDRICAL_SURFACE('',#54536,5.1) ;
#10606 = CYLINDRICAL_SURFACE('',#54537,5.1) ;
#10607 = CYLINDRICAL_SURFACE('',#54538,5.1) ;
#10608 = CYLINDRICAL_SURFACE('',#54539,5.1) ;
#10609 = CYLINDRICAL_SURFACE('',#54540,5.1) ;
#10610 = CYLINDRICAL_SURFACE('',#54541,5.1) ;
#10611 = CYLINDRICAL_SURFACE('',#54542,5.1) ;
#10612 = CYLINDRICAL_SURFACE('',#54543,2.) ;
#10613 = CYLINDRICAL_SURFACE('',#54562,0.15) ;
#10614 = CYLINDRICAL_SURFACE('',#54566,0.15) ;
#10615 = CYLINDRICAL_SURFACE('',#54570,0.15) ;
#10616 = CYLINDRICAL_SURFACE('',#54574,0.15) ;
#10617 = CYLINDRICAL_SURFACE('',#54578,0.15) ;
#10618 = CYLINDRICAL_SURFACE('',#54582,0.15) ;
#10619 = CYLINDRICAL_SURFACE('',#54586,0.15) ;
#10620 = CYLINDRICAL_SURFACE('',#54590,0.15) ;
#10621 = CYLINDRICAL_SURFACE('',#54594,0.15) ;
#10622 = CYLINDRICAL_SURFACE('',#54598,0.15) ;
#10623 = CYLINDRICAL_SURFACE('',#54602,0.15) ;
#10624 = CYLINDRICAL_SURFACE('',#54606,0.15) ;
#10625 = CYLINDRICAL_SURFACE('',#54610,0.15) ;
#10626 = CYLINDRICAL_SURFACE('',#54614,0.15) ;
#10627 = CYLINDRICAL_SURFACE('',#54618,0.15) ;
#10628 = CYLINDRICAL_SURFACE('',#54622,0.15) ;
#10629 = CYLINDRICAL_SURFACE('',#54626,0.15) ;
#10630 = CYLINDRICAL_SURFACE('',#54630,0.15) ;
#10631 = CYLINDRICAL_SURFACE('',#54634,0.15) ;
#10632 = CYLINDRICAL_SURFACE('',#54638,0.15) ;
#10633 = CYLINDRICAL_SURFACE('',#54642,0.15) ;
#10634 = CYLINDRICAL_SURFACE('',#54646,0.15) ;
#10635 = CYLINDRICAL_SURFACE('',#54650,0.15) ;
#10636 = CYLINDRICAL_SURFACE('',#54654,0.15) ;
#10637 = CYLINDRICAL_SURFACE('',#54658,0.15) ;
#10638 = CYLINDRICAL_SURFACE('',#54662,0.15) ;
#10639 = CYLINDRICAL_SURFACE('',#54666,0.15) ;
#10640 = CYLINDRICAL_SURFACE('',#54670,0.15) ;
#10641 = CYLINDRICAL_SURFACE('',#54674,0.15) ;
#10642 = CYLINDRICAL_SURFACE('',#54678,0.15) ;
#10643 = CYLINDRICAL_SURFACE('',#54682,0.15) ;
#10644 = CYLINDRICAL_SURFACE('',#54686,0.15) ;
#10645 = CYLINDRICAL_SURFACE('',#54690,0.15) ;
#10646 = CYLINDRICAL_SURFACE('',#54694,0.15) ;
#10647 = CYLINDRICAL_SURFACE('',#54698,0.15) ;
#10648 = CYLINDRICAL_SURFACE('',#54702,0.15) ;
#10649 = CYLINDRICAL_SURFACE('',#54706,0.15) ;
#10650 = CYLINDRICAL_SURFACE('',#54710,0.15) ;
#10651 = CYLINDRICAL_SURFACE('',#54714,0.15) ;
#10652 = CYLINDRICAL_SURFACE('',#54718,0.15) ;
#10653 = CYLINDRICAL_SURFACE('',#54720,0.500000000000003) ;
#10654 = CYLINDRICAL_SURFACE('',#54723,5.1) ;
#10655 = CYLINDRICAL_SURFACE('',#54726,0.500000000000003) ;
#10656 = CYLINDRICAL_SURFACE('',#54729,5.1) ;
#10657 = CYLINDRICAL_SURFACE('',#54732,0.500000000000003) ;
#10658 = CYLINDRICAL_SURFACE('',#54735,5.1) ;
#10659 = CYLINDRICAL_SURFACE('',#54738,0.500000000000003) ;
#10660 = CYLINDRICAL_SURFACE('',#54741,5.1) ;
#10661 = CYLINDRICAL_SURFACE('',#54744,0.500000000000003) ;
#10662 = CYLINDRICAL_SURFACE('',#54747,5.1) ;
#10663 = CYLINDRICAL_SURFACE('',#54750,0.500000000000003) ;
#10664 = CYLINDRICAL_SURFACE('',#54753,5.1) ;
#10665 = CYLINDRICAL_SURFACE('',#54756,0.500000000000003) ;
#10666 = CYLINDRICAL_SURFACE('',#54759,5.1) ;
#10667 = CYLINDRICAL_SURFACE('',#54762,0.500000000000003) ;
#10668 = CYLINDRICAL_SURFACE('',#54765,5.1) ;
#10669 = CYLINDRICAL_SURFACE('',#54768,0.500000000000003) ;
#10670 = CYLINDRICAL_SURFACE('',#54771,5.1) ;
#10671 = CYLINDRICAL_SURFACE('',#54774,0.500000000000003) ;
#10672 = CYLINDRICAL_SURFACE('',#54777,5.1) ;
#10673 = CYLINDRICAL_SURFACE('',#54907,0.15) ;
#10674 = CYLINDRICAL_SURFACE('',#54908,0.15) ;
#10675 = CYLINDRICAL_SURFACE('',#54909,0.15) ;
#10676 = CYLINDRICAL_SURFACE('',#54911,0.15) ;
#10677 = CYLINDRICAL_SURFACE('',#54912,0.15) ;
#10678 = CYLINDRICAL_SURFACE('',#54913,0.15) ;
#10679 = CYLINDRICAL_SURFACE('',#54915,0.15) ;
#10680 = CYLINDRICAL_SURFACE('',#54916,0.15) ;
#10681 = CYLINDRICAL_SURFACE('',#54917,0.15) ;
#10682 = CYLINDRICAL_SURFACE('',#54919,0.15) ;
#10683 = CYLINDRICAL_SURFACE('',#54920,0.15) ;
#10684 = CYLINDRICAL_SURFACE('',#54921,0.15) ;
#10685 = CYLINDRICAL_SURFACE('',#54923,0.15) ;
#10686 = CYLINDRICAL_SURFACE('',#54924,0.15) ;
#10687 = CYLINDRICAL_SURFACE('',#54925,0.15) ;
#10688 = CYLINDRICAL_SURFACE('',#54927,0.15) ;
#10689 = CYLINDRICAL_SURFACE('',#54928,0.15) ;
#10690 = CYLINDRICAL_SURFACE('',#54929,0.15) ;
#10691 = CYLINDRICAL_SURFACE('',#54931,0.15) ;
#10692 = CYLINDRICAL_SURFACE('',#54932,0.15) ;
#10693 = CYLINDRICAL_SURFACE('',#54933,0.15) ;
#10694 = CYLINDRICAL_SURFACE('',#54935,0.15) ;
#10695 = CYLINDRICAL_SURFACE('',#54936,0.15) ;
#10696 = CYLINDRICAL_SURFACE('',#54937,0.15) ;
#10697 = CYLINDRICAL_SURFACE('',#54939,0.15) ;
#10698 = CYLINDRICAL_SURFACE('',#54940,0.15) ;
#10699 = CYLINDRICAL_SURFACE('',#54941,0.15) ;
#10700 = CYLINDRICAL_SURFACE('',#54943,0.15) ;
#10701 = CYLINDRICAL_SURFACE('',#54944,0.15) ;
#10702 = CYLINDRICAL_SURFACE('',#54945,0.15) ;
#10703 = CYLINDRICAL_SURFACE('',#54947,0.15) ;
#10704 = CYLINDRICAL_SURFACE('',#54952,0.15) ;
#10705 = CYLINDRICAL_SURFACE('',#54958,0.15) ;
#10706 = CYLINDRICAL_SURFACE('',#54964,0.15) ;
#10707 = CYLINDRICAL_SURFACE('',#54970,0.15) ;
#10708 = CYLINDRICAL_SURFACE('',#54976,0.15) ;
#10709 = CYLINDRICAL_SURFACE('',#54982,0.15) ;
#10710 = CYLINDRICAL_SURFACE('',#54988,0.15) ;
#10711 = CYLINDRICAL_SURFACE('',#54994,0.15) ;
#10712 = CYLINDRICAL_SURFACE('',#55000,0.15) ;
#10713 = CYLINDRICAL_SURFACE('',#55005,5.1) ;
#10714 = CYLINDRICAL_SURFACE('',#55007,0.500000000000003) ;
#10715 = CYLINDRICAL_SURFACE('',#55011,0.500000000000003) ;
#10716 = CYLINDRICAL_SURFACE('',#55014,0.500000000000003) ;
#10717 = CYLINDRICAL_SURFACE('',#55017,0.500000000000003) ;
#10718 = CYLINDRICAL_SURFACE('',#55020,0.500000000000003) ;
#10719 = CYLINDRICAL_SURFACE('',#55023,0.500000000000003) ;
#10720 = CYLINDRICAL_SURFACE('',#55026,0.500000000000003) ;
#10721 = CYLINDRICAL_SURFACE('',#55029,0.500000000000003) ;
#10722 = CYLINDRICAL_SURFACE('',#55032,0.500000000000003) ;
#10723 = CYLINDRICAL_SURFACE('',#55035,0.500000000000003) ;
#10724 = CYLINDRICAL_SURFACE('',#55036,5.1) ;
#10725 = CYLINDRICAL_SURFACE('',#55037,5.1) ;
#10726 = CYLINDRICAL_SURFACE('',#55038,5.1) ;
#10727 = CYLINDRICAL_SURFACE('',#55039,5.1) ;
#10728 = CYLINDRICAL_SURFACE('',#55040,5.1) ;
#10729 = CYLINDRICAL_SURFACE('',#55041,5.1) ;
#10730 = CYLINDRICAL_SURFACE('',#55042,5.1) ;
#10731 = CYLINDRICAL_SURFACE('',#55043,5.1) ;
#10732 = CYLINDRICAL_SURFACE('',#55044,5.1) ;
#10733 = CYLINDRICAL_SURFACE('',#55045,2.) ;
#10734 = CYLINDRICAL_SURFACE('',#55047,1.67774999999999) ;
#10735 = CYLINDRICAL_SURFACE('',#55049,1.67774999999999) ;
#10736 = CYLINDRICAL_SURFACE('',#55050,1.67774999999999) ;
#10737 = CYLINDRICAL_SURFACE('',#55051,1.67774999999999) ;
#10738 = CYLINDRICAL_SURFACE('',#55052,1.67774999999999) ;
#10739 = CYLINDRICAL_SURFACE('',#55054,1.67774999999999) ;
#10740 = CYLINDRICAL_SURFACE('',#55055,1.67774999999999) ;
#10741 = CYLINDRICAL_SURFACE('',#55056,1.67774999999999) ;
#10742 = CYLINDRICAL_SURFACE('',#55057,1.67774999999999) ;
#10743 = CYLINDRICAL_SURFACE('',#55058,1.67774999999999) ;
#10744 = CYLINDRICAL_SURFACE('',#55059,1.9635) ;
#10745 = CYLINDRICAL_SURFACE('',#55066,1.67774999999999) ;
#10746 = CYLINDRICAL_SURFACE('',#55068,1.67774999999999) ;
#10747 = FACE_OUTER_BOUND('',#13839,.T.) ;
#10748 = FACE_OUTER_BOUND('',#13840,.T.) ;
#10749 = FACE_OUTER_BOUND('',#13841,.T.) ;
#10750 = FACE_OUTER_BOUND('',#13842,.T.) ;
#10751 = FACE_OUTER_BOUND('',#13843,.T.) ;
#10752 = FACE_OUTER_BOUND('',#13844,.T.) ;
#10753 = FACE_OUTER_BOUND('',#13845,.T.) ;
#10754 = FACE_OUTER_BOUND('',#13846,.T.) ;
#10755 = FACE_OUTER_BOUND('',#13847,.T.) ;
#10756 = FACE_OUTER_BOUND('',#13848,.T.) ;
#10757 = FACE_OUTER_BOUND('',#13849,.T.) ;
#10758 = FACE_OUTER_BOUND('',#13850,.T.) ;
#10759 = FACE_OUTER_BOUND('',#13851,.T.) ;
#10760 = FACE_OUTER_BOUND('',#13852,.T.) ;
#10761 = FACE_OUTER_BOUND('',#13853,.T.) ;
#10762 = FACE_OUTER_BOUND('',#13854,.T.) ;
#10763 = FACE_OUTER_BOUND('',#13855,.T.) ;
#10764 = FACE_OUTER_BOUND('',#13856,.T.) ;
#10765 = FACE_OUTER_BOUND('',#13857,.T.) ;
#10766 = FACE_OUTER_BOUND('',#13858,.T.) ;
#10767 = FACE_OUTER_BOUND('',#13859,.T.) ;
#10768 = FACE_OUTER_BOUND('',#13860,.T.) ;
#10769 = FACE_OUTER_BOUND('',#13861,.T.) ;
#10770 = FACE_OUTER_BOUND('',#13862,.T.) ;
#10771 = FACE_OUTER_BOUND('',#13863,.T.) ;
#10772 = FACE_OUTER_BOUND('',#13864,.T.) ;
#10773 = FACE_OUTER_BOUND('',#13865,.T.) ;
#10774 = FACE_OUTER_BOUND('',#13866,.T.) ;
#10775 = FACE_OUTER_BOUND('',#13867,.T.) ;
#10776 = FACE_OUTER_BOUND('',#13868,.T.) ;
#10777 = FACE_OUTER_BOUND('',#13869,.T.) ;
#10778 = FACE_OUTER_BOUND('',#13870,.T.) ;
#10779 = FACE_OUTER_BOUND('',#13871,.T.) ;
#10780 = FACE_OUTER_BOUND('',#13872,.T.) ;
#10781 = FACE_OUTER_BOUND('',#13873,.T.) ;
#10782 = FACE_OUTER_BOUND('',#13874,.T.) ;
#10783 = FACE_OUTER_BOUND('',#13875,.T.) ;
#10784 = FACE_OUTER_BOUND('',#13876,.T.) ;
#10785 = FACE_OUTER_BOUND('',#13877,.T.) ;
#10786 = FACE_OUTER_BOUND('',#13878,.T.) ;
#10787 = FACE_OUTER_BOUND('',#13879,.T.) ;
#10788 = FACE_OUTER_BOUND('',#13880,.T.) ;
#10789 = FACE_OUTER_BOUND('',#13881,.T.) ;
#10790 = FACE_OUTER_BOUND('',#13882,.T.) ;
#10791 = FACE_OUTER_BOUND('',#13883,.T.) ;
#10792 = FACE_OUTER_BOUND('',#13884,.T.) ;
#10793 = FACE_OUTER_BOUND('',#13885,.T.) ;
#10794 = FACE_OUTER_BOUND('',#13886,.T.) ;
#10795 = FACE_OUTER_BOUND('',#13887,.T.) ;
#10796 = FACE_OUTER_BOUND('',#13888,.T.) ;
#10797 = FACE_OUTER_BOUND('',#13889,.T.) ;
#10798 = FACE_OUTER_BOUND('',#13890,.T.) ;
#10799 = FACE_OUTER_BOUND('',#13891,.T.) ;
#10800 = FACE_OUTER_BOUND('',#13892,.T.) ;
#10801 = FACE_OUTER_BOUND('',#13893,.T.) ;
#10802 = FACE_OUTER_BOUND('',#13894,.T.) ;
#10803 = FACE_OUTER_BOUND('',#13895,.T.) ;
#10804 = FACE_OUTER_BOUND('',#13896,.T.) ;
#10805 = FACE_OUTER_BOUND('',#13897,.T.) ;
#10806 = FACE_OUTER_BOUND('',#13898,.T.) ;
#10807 = FACE_OUTER_BOUND('',#13899,.T.) ;
#10808 = FACE_OUTER_BOUND('',#13900,.T.) ;
#10809 = FACE_OUTER_BOUND('',#13901,.T.) ;
#10810 = FACE_OUTER_BOUND('',#13902,.T.) ;
#10811 = FACE_OUTER_BOUND('',#13903,.T.) ;
#10812 = FACE_OUTER_BOUND('',#13904,.T.) ;
#10813 = FACE_OUTER_BOUND('',#13905,.T.) ;
#10814 = FACE_OUTER_BOUND('',#13906,.T.) ;
#10815 = FACE_OUTER_BOUND('',#13907,.T.) ;
#10816 = FACE_OUTER_BOUND('',#13908,.T.) ;
#10817 = FACE_OUTER_BOUND('',#13909,.T.) ;
#10818 = FACE_OUTER_BOUND('',#13910,.T.) ;
#10819 = FACE_OUTER_BOUND('',#13911,.T.) ;
#10820 = FACE_OUTER_BOUND('',#13912,.T.) ;
#10821 = FACE_OUTER_BOUND('',#13913,.T.) ;
#10822 = FACE_OUTER_BOUND('',#13914,.T.) ;
#10823 = FACE_OUTER_BOUND('',#13915,.T.) ;
#10824 = FACE_OUTER_BOUND('',#13916,.T.) ;
#10825 = FACE_OUTER_BOUND('',#13917,.T.) ;
#10826 = FACE_OUTER_BOUND('',#13918,.T.) ;
#10827 = FACE_OUTER_BOUND('',#13919,.T.) ;
#10828 = FACE_OUTER_BOUND('',#13920,.T.) ;
#10829 = FACE_OUTER_BOUND('',#13921,.T.) ;
#10830 = FACE_OUTER_BOUND('',#13922,.T.) ;
#10831 = FACE_OUTER_BOUND('',#13923,.T.) ;
#10832 = FACE_OUTER_BOUND('',#13924,.T.) ;
#10833 = FACE_OUTER_BOUND('',#13925,.T.) ;
#10834 = FACE_OUTER_BOUND('',#13926,.T.) ;
#10835 = FACE_OUTER_BOUND('',#13927,.T.) ;
#10836 = FACE_OUTER_BOUND('',#13928,.T.) ;
#10837 = FACE_OUTER_BOUND('',#13929,.T.) ;
#10838 = FACE_OUTER_BOUND('',#13930,.T.) ;
#10839 = FACE_OUTER_BOUND('',#13931,.T.) ;
#10840 = FACE_OUTER_BOUND('',#13932,.T.) ;
#10841 = FACE_OUTER_BOUND('',#13933,.T.) ;
#10842 = FACE_OUTER_BOUND('',#13934,.T.) ;
#10843 = FACE_OUTER_BOUND('',#13935,.T.) ;
#10844 = FACE_OUTER_BOUND('',#13936,.T.) ;
#10845 = FACE_OUTER_BOUND('',#13937,.T.) ;
#10846 = FACE_OUTER_BOUND('',#13938,.T.) ;
#10847 = FACE_OUTER_BOUND('',#13939,.T.) ;
#10848 = FACE_OUTER_BOUND('',#13940,.T.) ;
#10849 = FACE_OUTER_BOUND('',#13941,.T.) ;
#10850 = FACE_OUTER_BOUND('',#13942,.T.) ;
#10851 = FACE_OUTER_BOUND('',#13943,.T.) ;
#10852 = FACE_OUTER_BOUND('',#13944,.T.) ;
#10853 = FACE_OUTER_BOUND('',#13945,.T.) ;
#10854 = FACE_OUTER_BOUND('',#13946,.T.) ;
#10855 = FACE_OUTER_BOUND('',#13947,.T.) ;
#10856 = FACE_OUTER_BOUND('',#13948,.T.) ;
#10857 = FACE_OUTER_BOUND('',#13949,.T.) ;
#10858 = FACE_OUTER_BOUND('',#13950,.T.) ;
#10859 = FACE_OUTER_BOUND('',#13951,.T.) ;
#10860 = FACE_OUTER_BOUND('',#13952,.T.) ;
#10861 = FACE_OUTER_BOUND('',#13953,.T.) ;
#10862 = FACE_OUTER_BOUND('',#13954,.T.) ;
#10863 = FACE_OUTER_BOUND('',#13955,.T.) ;
#10864 = FACE_OUTER_BOUND('',#13956,.T.) ;
#10865 = FACE_OUTER_BOUND('',#13957,.T.) ;
#10866 = FACE_OUTER_BOUND('',#13958,.T.) ;
#10867 = FACE_OUTER_BOUND('',#13959,.T.) ;
#10868 = FACE_OUTER_BOUND('',#13960,.T.) ;
#10869 = FACE_OUTER_BOUND('',#13961,.T.) ;
#10870 = FACE_OUTER_BOUND('',#13962,.T.) ;
#10871 = FACE_OUTER_BOUND('',#13963,.T.) ;
#10872 = FACE_OUTER_BOUND('',#13964,.T.) ;
#10873 = FACE_OUTER_BOUND('',#13965,.T.) ;
#10874 = FACE_OUTER_BOUND('',#13966,.T.) ;
#10875 = FACE_OUTER_BOUND('',#13967,.T.) ;
#10876 = FACE_OUTER_BOUND('',#13968,.T.) ;
#10877 = FACE_OUTER_BOUND('',#13969,.T.) ;
#10878 = FACE_OUTER_BOUND('',#13970,.T.) ;
#10879 = FACE_OUTER_BOUND('',#13971,.T.) ;
#10880 = FACE_OUTER_BOUND('',#13972,.T.) ;
#10881 = FACE_OUTER_BOUND('',#13973,.T.) ;
#10882 = FACE_OUTER_BOUND('',#13974,.T.) ;
#10883 = FACE_OUTER_BOUND('',#13975,.T.) ;
#10884 = FACE_OUTER_BOUND('',#13976,.T.) ;
#10885 = FACE_OUTER_BOUND('',#13977,.T.) ;
#10886 = FACE_OUTER_BOUND('',#13978,.T.) ;
#10887 = FACE_OUTER_BOUND('',#13979,.T.) ;
#10888 = FACE_OUTER_BOUND('',#13980,.T.) ;
#10889 = FACE_OUTER_BOUND('',#13981,.T.) ;
#10890 = FACE_OUTER_BOUND('',#13982,.T.) ;
#10891 = FACE_OUTER_BOUND('',#13983,.T.) ;
#10892 = FACE_OUTER_BOUND('',#13984,.T.) ;
#10893 = FACE_OUTER_BOUND('',#13985,.T.) ;
#10894 = FACE_OUTER_BOUND('',#13986,.T.) ;
#10895 = FACE_OUTER_BOUND('',#13987,.T.) ;
#10896 = FACE_OUTER_BOUND('',#13988,.T.) ;
#10897 = FACE_OUTER_BOUND('',#13989,.T.) ;
#10898 = FACE_OUTER_BOUND('',#13990,.T.) ;
#10899 = FACE_OUTER_BOUND('',#13991,.T.) ;
#10900 = FACE_OUTER_BOUND('',#13992,.T.) ;
#10901 = FACE_OUTER_BOUND('',#13993,.T.) ;
#10902 = FACE_OUTER_BOUND('',#13994,.T.) ;
#10903 = FACE_OUTER_BOUND('',#13995,.T.) ;
#10904 = FACE_OUTER_BOUND('',#13996,.T.) ;
#10905 = FACE_OUTER_BOUND('',#13997,.T.) ;
#10906 = FACE_OUTER_BOUND('',#13998,.T.) ;
#10907 = FACE_OUTER_BOUND('',#13999,.T.) ;
#10908 = FACE_OUTER_BOUND('',#14000,.T.) ;
#10909 = FACE_OUTER_BOUND('',#14001,.T.) ;
#10910 = FACE_OUTER_BOUND('',#14002,.T.) ;
#10911 = FACE_OUTER_BOUND('',#14003,.T.) ;
#10912 = FACE_OUTER_BOUND('',#14004,.T.) ;
#10913 = FACE_OUTER_BOUND('',#14005,.T.) ;
#10914 = FACE_OUTER_BOUND('',#14006,.T.) ;
#10915 = FACE_OUTER_BOUND('',#14007,.T.) ;
#10916 = FACE_OUTER_BOUND('',#14008,.T.) ;
#10917 = FACE_OUTER_BOUND('',#14009,.T.) ;
#10918 = FACE_OUTER_BOUND('',#14010,.T.) ;
#10919 = FACE_OUTER_BOUND('',#14011,.T.) ;
#10920 = FACE_OUTER_BOUND('',#14012,.T.) ;
#10921 = FACE_OUTER_BOUND('',#14013,.T.) ;
#10922 = FACE_OUTER_BOUND('',#14014,.T.) ;
#10923 = FACE_OUTER_BOUND('',#14015,.T.) ;
#10924 = FACE_OUTER_BOUND('',#14016,.T.) ;
#10925 = FACE_OUTER_BOUND('',#14017,.T.) ;
#10926 = FACE_OUTER_BOUND('',#14018,.T.) ;
#10927 = FACE_OUTER_BOUND('',#14019,.T.) ;
#10928 = FACE_OUTER_BOUND('',#14020,.T.) ;
#10929 = FACE_OUTER_BOUND('',#14021,.T.) ;
#10930 = FACE_OUTER_BOUND('',#14022,.T.) ;
#10931 = FACE_OUTER_BOUND('',#14023,.T.) ;
#10932 = FACE_OUTER_BOUND('',#14024,.T.) ;
#10933 = FACE_OUTER_BOUND('',#14025,.T.) ;
#10934 = FACE_OUTER_BOUND('',#14026,.T.) ;
#10935 = FACE_OUTER_BOUND('',#14027,.T.) ;
#10936 = FACE_OUTER_BOUND('',#14028,.T.) ;
#10937 = FACE_OUTER_BOUND('',#14029,.T.) ;
#10938 = FACE_OUTER_BOUND('',#14030,.T.) ;
#10939 = FACE_OUTER_BOUND('',#14031,.T.) ;
#10940 = FACE_OUTER_BOUND('',#14032,.T.) ;
#10941 = FACE_OUTER_BOUND('',#14033,.T.) ;
#10942 = FACE_OUTER_BOUND('',#14034,.T.) ;
#10943 = FACE_OUTER_BOUND('',#14035,.T.) ;
#10944 = FACE_OUTER_BOUND('',#14036,.T.) ;
#10945 = FACE_OUTER_BOUND('',#14037,.T.) ;
#10946 = FACE_OUTER_BOUND('',#14038,.T.) ;
#10947 = FACE_OUTER_BOUND('',#14039,.T.) ;
#10948 = FACE_OUTER_BOUND('',#14040,.T.) ;
#10949 = FACE_OUTER_BOUND('',#14041,.T.) ;
#10950 = FACE_OUTER_BOUND('',#14043,.T.) ;
#10951 = FACE_OUTER_BOUND('',#14044,.T.) ;
#10952 = FACE_OUTER_BOUND('',#14045,.T.) ;
#10953 = FACE_OUTER_BOUND('',#14046,.T.) ;
#10954 = FACE_OUTER_BOUND('',#14047,.T.) ;
#10955 = FACE_OUTER_BOUND('',#14048,.T.) ;
#10956 = FACE_OUTER_BOUND('',#14049,.T.) ;
#10957 = FACE_OUTER_BOUND('',#14050,.T.) ;
#10958 = FACE_OUTER_BOUND('',#14051,.T.) ;
#10959 = FACE_OUTER_BOUND('',#14052,.T.) ;
#10960 = FACE_OUTER_BOUND('',#14053,.T.) ;
#10961 = FACE_OUTER_BOUND('',#14054,.T.) ;
#10962 = FACE_OUTER_BOUND('',#14055,.T.) ;
#10963 = FACE_OUTER_BOUND('',#14056,.T.) ;
#10964 = FACE_OUTER_BOUND('',#14057,.T.) ;
#10965 = FACE_OUTER_BOUND('',#14058,.T.) ;
#10966 = FACE_OUTER_BOUND('',#14059,.T.) ;
#10967 = FACE_OUTER_BOUND('',#14060,.T.) ;
#10968 = FACE_OUTER_BOUND('',#14061,.T.) ;
#10969 = FACE_OUTER_BOUND('',#14062,.T.) ;
#10970 = FACE_OUTER_BOUND('',#14063,.T.) ;
#10971 = FACE_OUTER_BOUND('',#14064,.T.) ;
#10972 = FACE_OUTER_BOUND('',#14065,.T.) ;
#10973 = FACE_OUTER_BOUND('',#14066,.T.) ;
#10974 = FACE_OUTER_BOUND('',#14067,.T.) ;
#10975 = FACE_OUTER_BOUND('',#14068,.T.) ;
#10976 = FACE_OUTER_BOUND('',#14069,.T.) ;
#10977 = FACE_OUTER_BOUND('',#14070,.T.) ;
#10978 = FACE_OUTER_BOUND('',#14071,.T.) ;
#10979 = FACE_OUTER_BOUND('',#14072,.T.) ;
#10980 = FACE_OUTER_BOUND('',#14073,.T.) ;
#10981 = FACE_OUTER_BOUND('',#14074,.T.) ;
#10982 = FACE_OUTER_BOUND('',#14075,.T.) ;
#10983 = FACE_OUTER_BOUND('',#14076,.T.) ;
#10984 = FACE_OUTER_BOUND('',#14077,.T.) ;
#10985 = FACE_OUTER_BOUND('',#14078,.T.) ;
#10986 = FACE_OUTER_BOUND('',#14079,.T.) ;
#10987 = FACE_OUTER_BOUND('',#14080,.T.) ;
#10988 = FACE_OUTER_BOUND('',#14081,.T.) ;
#10989 = FACE_OUTER_BOUND('',#14082,.T.) ;
#10990 = FACE_OUTER_BOUND('',#14083,.T.) ;
#10991 = FACE_OUTER_BOUND('',#14084,.T.) ;
#10992 = FACE_OUTER_BOUND('',#14085,.T.) ;
#10993 = FACE_OUTER_BOUND('',#14086,.T.) ;
#10994 = FACE_OUTER_BOUND('',#14087,.T.) ;
#10995 = FACE_OUTER_BOUND('',#14088,.T.) ;
#10996 = FACE_OUTER_BOUND('',#14089,.T.) ;
#10997 = FACE_OUTER_BOUND('',#14090,.T.) ;
#10998 = FACE_OUTER_BOUND('',#14091,.T.) ;
#10999 = FACE_OUTER_BOUND('',#14092,.T.) ;
#11000 = FACE_OUTER_BOUND('',#14093,.T.) ;
#11001 = FACE_OUTER_BOUND('',#14094,.T.) ;
#11002 = FACE_OUTER_BOUND('',#14095,.T.) ;
#11003 = FACE_OUTER_BOUND('',#14096,.T.) ;
#11004 = FACE_OUTER_BOUND('',#14097,.T.) ;
#11005 = FACE_OUTER_BOUND('',#14098,.T.) ;
#11006 = FACE_OUTER_BOUND('',#14099,.T.) ;
#11007 = FACE_OUTER_BOUND('',#14100,.T.) ;
#11008 = FACE_OUTER_BOUND('',#14101,.T.) ;
#11009 = FACE_OUTER_BOUND('',#14102,.T.) ;
#11010 = FACE_OUTER_BOUND('',#14103,.T.) ;
#11011 = FACE_OUTER_BOUND('',#14104,.T.) ;
#11012 = FACE_OUTER_BOUND('',#14105,.T.) ;
#11013 = FACE_OUTER_BOUND('',#14106,.T.) ;
#11014 = FACE_OUTER_BOUND('',#14107,.T.) ;
#11015 = FACE_OUTER_BOUND('',#14108,.T.) ;
#11016 = FACE_OUTER_BOUND('',#14109,.T.) ;
#11017 = FACE_OUTER_BOUND('',#14110,.T.) ;
#11018 = FACE_OUTER_BOUND('',#14111,.T.) ;
#11019 = FACE_OUTER_BOUND('',#14112,.T.) ;
#11020 = FACE_OUTER_BOUND('',#14113,.T.) ;
#11021 = FACE_OUTER_BOUND('',#14114,.T.) ;
#11022 = FACE_OUTER_BOUND('',#14115,.T.) ;
#11023 = FACE_OUTER_BOUND('',#14116,.T.) ;
#11024 = FACE_OUTER_BOUND('',#14117,.T.) ;
#11025 = FACE_OUTER_BOUND('',#14118,.T.) ;
#11026 = FACE_OUTER_BOUND('',#14119,.T.) ;
#11027 = FACE_OUTER_BOUND('',#14120,.T.) ;
#11028 = FACE_OUTER_BOUND('',#14125,.T.) ;
#11029 = FACE_OUTER_BOUND('',#14126,.T.) ;
#11030 = FACE_OUTER_BOUND('',#14127,.T.) ;
#11031 = FACE_OUTER_BOUND('',#14128,.T.) ;
#11032 = FACE_OUTER_BOUND('',#14129,.T.) ;
#11033 = FACE_OUTER_BOUND('',#14130,.T.) ;
#11034 = FACE_OUTER_BOUND('',#14131,.T.) ;
#11035 = FACE_OUTER_BOUND('',#14132,.T.) ;
#11036 = FACE_OUTER_BOUND('',#14133,.T.) ;
#11037 = FACE_OUTER_BOUND('',#14134,.T.) ;
#11038 = FACE_OUTER_BOUND('',#14135,.T.) ;
#11039 = FACE_OUTER_BOUND('',#14136,.T.) ;
#11040 = FACE_OUTER_BOUND('',#14137,.T.) ;
#11041 = FACE_OUTER_BOUND('',#14138,.T.) ;
#11042 = FACE_OUTER_BOUND('',#14139,.T.) ;
#11043 = FACE_OUTER_BOUND('',#14140,.T.) ;
#11044 = FACE_OUTER_BOUND('',#14141,.T.) ;
#11045 = FACE_OUTER_BOUND('',#14142,.T.) ;
#11046 = FACE_OUTER_BOUND('',#14143,.T.) ;
#11047 = FACE_OUTER_BOUND('',#14144,.T.) ;
#11048 = FACE_OUTER_BOUND('',#14145,.T.) ;
#11049 = FACE_OUTER_BOUND('',#14146,.T.) ;
#11050 = FACE_OUTER_BOUND('',#14147,.T.) ;
#11051 = FACE_OUTER_BOUND('',#14148,.T.) ;
#11052 = FACE_OUTER_BOUND('',#14149,.T.) ;
#11053 = FACE_OUTER_BOUND('',#14150,.T.) ;
#11054 = FACE_OUTER_BOUND('',#14151,.T.) ;
#11055 = FACE_OUTER_BOUND('',#14152,.T.) ;
#11056 = FACE_OUTER_BOUND('',#14153,.T.) ;
#11057 = FACE_OUTER_BOUND('',#14154,.T.) ;
#11058 = FACE_OUTER_BOUND('',#14155,.T.) ;
#11059 = FACE_OUTER_BOUND('',#14156,.T.) ;
#11060 = FACE_OUTER_BOUND('',#14157,.T.) ;
#11061 = FACE_OUTER_BOUND('',#14158,.T.) ;
#11062 = FACE_OUTER_BOUND('',#14159,.T.) ;
#11063 = FACE_OUTER_BOUND('',#14160,.T.) ;
#11064 = FACE_OUTER_BOUND('',#14161,.T.) ;
#11065 = FACE_OUTER_BOUND('',#14162,.T.) ;
#11066 = FACE_OUTER_BOUND('',#14163,.T.) ;
#11067 = FACE_OUTER_BOUND('',#14164,.T.) ;
#11068 = FACE_OUTER_BOUND('',#14165,.T.) ;
#11069 = FACE_OUTER_BOUND('',#14166,.T.) ;
#11070 = FACE_OUTER_BOUND('',#14167,.T.) ;
#11071 = FACE_OUTER_BOUND('',#14168,.T.) ;
#11072 = FACE_OUTER_BOUND('',#14169,.T.) ;
#11073 = FACE_OUTER_BOUND('',#14170,.T.) ;
#11074 = FACE_OUTER_BOUND('',#14171,.T.) ;
#11075 = FACE_OUTER_BOUND('',#14172,.T.) ;
#11076 = FACE_OUTER_BOUND('',#14173,.T.) ;
#11077 = FACE_OUTER_BOUND('',#14174,.T.) ;
#11078 = FACE_OUTER_BOUND('',#14175,.T.) ;
#11079 = FACE_OUTER_BOUND('',#14176,.T.) ;
#11080 = FACE_OUTER_BOUND('',#14177,.T.) ;
#11081 = FACE_OUTER_BOUND('',#14178,.T.) ;
#11082 = FACE_OUTER_BOUND('',#14179,.T.) ;
#11083 = FACE_OUTER_BOUND('',#14180,.T.) ;
#11084 = FACE_OUTER_BOUND('',#14181,.T.) ;
#11085 = FACE_OUTER_BOUND('',#14182,.T.) ;
#11086 = FACE_OUTER_BOUND('',#14183,.T.) ;
#11087 = FACE_OUTER_BOUND('',#14184,.T.) ;
#11088 = FACE_OUTER_BOUND('',#14185,.T.) ;
#11089 = FACE_OUTER_BOUND('',#14186,.T.) ;
#11090 = FACE_OUTER_BOUND('',#14187,.T.) ;
#11091 = FACE_OUTER_BOUND('',#14188,.T.) ;
#11092 = FACE_OUTER_BOUND('',#14189,.T.) ;
#11093 = FACE_OUTER_BOUND('',#14190,.T.) ;
#11094 = FACE_OUTER_BOUND('',#14191,.T.) ;
#11095 = FACE_OUTER_BOUND('',#14192,.T.) ;
#11096 = FACE_OUTER_BOUND('',#14193,.T.) ;
#11097 = FACE_OUTER_BOUND('',#14194,.T.) ;
#11098 = FACE_OUTER_BOUND('',#14195,.T.) ;
#11099 = FACE_OUTER_BOUND('',#14196,.T.) ;
#11100 = FACE_OUTER_BOUND('',#14197,.T.) ;
#11101 = FACE_OUTER_BOUND('',#14198,.T.) ;
#11102 = FACE_OUTER_BOUND('',#14199,.T.) ;
#11103 = FACE_OUTER_BOUND('',#14200,.T.) ;
#11104 = FACE_OUTER_BOUND('',#14201,.T.) ;
#11105 = FACE_OUTER_BOUND('',#14202,.T.) ;
#11106 = FACE_OUTER_BOUND('',#14203,.T.) ;
#11107 = FACE_OUTER_BOUND('',#14204,.T.) ;
#11108 = FACE_OUTER_BOUND('',#14205,.T.) ;
#11109 = FACE_OUTER_BOUND('',#14206,.T.) ;
#11110 = FACE_OUTER_BOUND('',#14207,.T.) ;
#11111 = FACE_OUTER_BOUND('',#14208,.T.) ;
#11112 = FACE_OUTER_BOUND('',#14209,.T.) ;
#11113 = FACE_OUTER_BOUND('',#14210,.T.) ;
#11114 = FACE_OUTER_BOUND('',#14211,.T.) ;
#11115 = FACE_OUTER_BOUND('',#14212,.T.) ;
#11116 = FACE_OUTER_BOUND('',#14213,.T.) ;
#11117 = FACE_OUTER_BOUND('',#14214,.T.) ;
#11118 = FACE_OUTER_BOUND('',#14215,.T.) ;
#11119 = FACE_OUTER_BOUND('',#14216,.T.) ;
#11120 = FACE_OUTER_BOUND('',#14217,.T.) ;
#11121 = FACE_OUTER_BOUND('',#14218,.T.) ;
#11122 = FACE_OUTER_BOUND('',#14219,.T.) ;
#11123 = FACE_OUTER_BOUND('',#14220,.T.) ;
#11124 = FACE_OUTER_BOUND('',#14221,.T.) ;
#11125 = FACE_OUTER_BOUND('',#14222,.T.) ;
#11126 = FACE_OUTER_BOUND('',#14223,.T.) ;
#11127 = FACE_OUTER_BOUND('',#14224,.T.) ;
#11128 = FACE_OUTER_BOUND('',#14225,.T.) ;
#11129 = FACE_OUTER_BOUND('',#14226,.T.) ;
#11130 = FACE_OUTER_BOUND('',#14227,.T.) ;
#11131 = FACE_OUTER_BOUND('',#14228,.T.) ;
#11132 = FACE_OUTER_BOUND('',#14229,.T.) ;
#11133 = FACE_OUTER_BOUND('',#14230,.T.) ;
#11134 = FACE_OUTER_BOUND('',#14231,.T.) ;
#11135 = FACE_OUTER_BOUND('',#14232,.T.) ;
#11136 = FACE_OUTER_BOUND('',#14233,.T.) ;
#11137 = FACE_OUTER_BOUND('',#14234,.T.) ;
#11138 = FACE_OUTER_BOUND('',#14235,.T.) ;
#11139 = FACE_OUTER_BOUND('',#14236,.T.) ;
#11140 = FACE_OUTER_BOUND('',#14237,.T.) ;
#11141 = FACE_OUTER_BOUND('',#14238,.T.) ;
#11142 = FACE_OUTER_BOUND('',#14241,.T.) ;
#11143 = FACE_OUTER_BOUND('',#14242,.T.) ;
#11144 = FACE_OUTER_BOUND('',#14243,.T.) ;
#11145 = FACE_OUTER_BOUND('',#14244,.T.) ;
#11146 = FACE_OUTER_BOUND('',#14245,.T.) ;
#11147 = FACE_OUTER_BOUND('',#14246,.T.) ;
#11148 = FACE_OUTER_BOUND('',#14247,.T.) ;
#11149 = FACE_OUTER_BOUND('',#14248,.T.) ;
#11150 = FACE_OUTER_BOUND('',#14249,.T.) ;
#11151 = FACE_OUTER_BOUND('',#14250,.T.) ;
#11152 = FACE_OUTER_BOUND('',#14251,.T.) ;
#11153 = FACE_OUTER_BOUND('',#14252,.T.) ;
#11154 = FACE_OUTER_BOUND('',#14253,.T.) ;
#11155 = FACE_OUTER_BOUND('',#14254,.T.) ;
#11156 = FACE_OUTER_BOUND('',#14255,.T.) ;
#11157 = FACE_OUTER_BOUND('',#14256,.T.) ;
#11158 = FACE_OUTER_BOUND('',#14257,.T.) ;
#11159 = FACE_OUTER_BOUND('',#14258,.T.) ;
#11160 = FACE_OUTER_BOUND('',#14259,.T.) ;
#11161 = FACE_OUTER_BOUND('',#14260,.T.) ;
#11162 = FACE_OUTER_BOUND('',#14261,.T.) ;
#11163 = FACE_OUTER_BOUND('',#14262,.T.) ;
#11164 = FACE_OUTER_BOUND('',#14263,.T.) ;
#11165 = FACE_OUTER_BOUND('',#14264,.T.) ;
#11166 = FACE_OUTER_BOUND('',#14265,.T.) ;
#11167 = FACE_OUTER_BOUND('',#14266,.T.) ;
#11168 = FACE_OUTER_BOUND('',#14267,.T.) ;
#11169 = FACE_OUTER_BOUND('',#14268,.T.) ;
#11170 = FACE_OUTER_BOUND('',#14269,.T.) ;
#11171 = FACE_OUTER_BOUND('',#14270,.T.) ;
#11172 = FACE_OUTER_BOUND('',#14271,.T.) ;
#11173 = FACE_OUTER_BOUND('',#14272,.T.) ;
#11174 = FACE_OUTER_BOUND('',#14273,.T.) ;
#11175 = FACE_OUTER_BOUND('',#14274,.T.) ;
#11176 = FACE_OUTER_BOUND('',#14275,.T.) ;
#11177 = FACE_OUTER_BOUND('',#14276,.T.) ;
#11178 = FACE_OUTER_BOUND('',#14277,.T.) ;
#11179 = FACE_OUTER_BOUND('',#14278,.T.) ;
#11180 = FACE_OUTER_BOUND('',#14279,.T.) ;
#11181 = FACE_OUTER_BOUND('',#14280,.T.) ;
#11182 = FACE_OUTER_BOUND('',#14281,.T.) ;
#11183 = FACE_OUTER_BOUND('',#14282,.T.) ;
#11184 = FACE_OUTER_BOUND('',#14283,.T.) ;
#11185 = FACE_OUTER_BOUND('',#14284,.T.) ;
#11186 = FACE_OUTER_BOUND('',#14285,.T.) ;
#11187 = FACE_OUTER_BOUND('',#14286,.T.) ;
#11188 = FACE_OUTER_BOUND('',#14287,.T.) ;
#11189 = FACE_OUTER_BOUND('',#14288,.T.) ;
#11190 = FACE_OUTER_BOUND('',#14289,.T.) ;
#11191 = FACE_OUTER_BOUND('',#14290,.T.) ;
#11192 = FACE_OUTER_BOUND('',#14291,.T.) ;
#11193 = FACE_OUTER_BOUND('',#14292,.T.) ;
#11194 = FACE_OUTER_BOUND('',#14293,.T.) ;
#11195 = FACE_OUTER_BOUND('',#14294,.T.) ;
#11196 = FACE_OUTER_BOUND('',#14295,.T.) ;
#11197 = FACE_OUTER_BOUND('',#14296,.T.) ;
#11198 = FACE_OUTER_BOUND('',#14297,.T.) ;
#11199 = FACE_OUTER_BOUND('',#14298,.T.) ;
#11200 = FACE_OUTER_BOUND('',#14299,.T.) ;
#11201 = FACE_OUTER_BOUND('',#14300,.T.) ;
#11202 = FACE_OUTER_BOUND('',#14301,.T.) ;
#11203 = FACE_OUTER_BOUND('',#14302,.T.) ;
#11204 = FACE_OUTER_BOUND('',#14303,.T.) ;
#11205 = FACE_OUTER_BOUND('',#14306,.T.) ;
#11206 = FACE_OUTER_BOUND('',#14307,.T.) ;
#11207 = FACE_OUTER_BOUND('',#14308,.T.) ;
#11208 = FACE_OUTER_BOUND('',#14309,.T.) ;
#11209 = FACE_OUTER_BOUND('',#14310,.T.) ;
#11210 = FACE_OUTER_BOUND('',#14311,.T.) ;
#11211 = FACE_OUTER_BOUND('',#14312,.T.) ;
#11212 = FACE_OUTER_BOUND('',#14313,.T.) ;
#11213 = FACE_OUTER_BOUND('',#14314,.T.) ;
#11214 = FACE_OUTER_BOUND('',#14315,.T.) ;
#11215 = FACE_OUTER_BOUND('',#14316,.T.) ;
#11216 = FACE_OUTER_BOUND('',#14317,.T.) ;
#11217 = FACE_OUTER_BOUND('',#14318,.T.) ;
#11218 = FACE_OUTER_BOUND('',#14319,.T.) ;
#11219 = FACE_OUTER_BOUND('',#14320,.T.) ;
#11220 = FACE_OUTER_BOUND('',#14321,.T.) ;
#11221 = FACE_OUTER_BOUND('',#14323,.T.) ;
#11222 = FACE_OUTER_BOUND('',#14324,.T.) ;
#11223 = FACE_OUTER_BOUND('',#14325,.T.) ;
#11224 = FACE_OUTER_BOUND('',#14326,.T.) ;
#11225 = FACE_OUTER_BOUND('',#14327,.T.) ;
#11226 = FACE_OUTER_BOUND('',#14328,.T.) ;
#11227 = FACE_OUTER_BOUND('',#14329,.T.) ;
#11228 = FACE_OUTER_BOUND('',#14330,.T.) ;
#11229 = FACE_OUTER_BOUND('',#14331,.T.) ;
#11230 = FACE_OUTER_BOUND('',#14332,.T.) ;
#11231 = FACE_OUTER_BOUND('',#14333,.T.) ;
#11232 = FACE_OUTER_BOUND('',#14334,.T.) ;
#11233 = FACE_OUTER_BOUND('',#14335,.T.) ;
#11234 = FACE_OUTER_BOUND('',#14336,.T.) ;
#11235 = FACE_OUTER_BOUND('',#14337,.T.) ;
#11236 = FACE_OUTER_BOUND('',#14338,.T.) ;
#11237 = FACE_OUTER_BOUND('',#14339,.T.) ;
#11238 = FACE_OUTER_BOUND('',#14340,.T.) ;
#11239 = FACE_OUTER_BOUND('',#14341,.T.) ;
#11240 = FACE_OUTER_BOUND('',#14342,.T.) ;
#11241 = FACE_OUTER_BOUND('',#14343,.T.) ;
#11242 = FACE_OUTER_BOUND('',#14344,.T.) ;
#11243 = FACE_OUTER_BOUND('',#14345,.T.) ;
#11244 = FACE_OUTER_BOUND('',#14346,.T.) ;
#11245 = FACE_OUTER_BOUND('',#14347,.T.) ;
#11246 = FACE_OUTER_BOUND('',#14348,.T.) ;
#11247 = FACE_OUTER_BOUND('',#14349,.T.) ;
#11248 = FACE_OUTER_BOUND('',#14350,.T.) ;
#11249 = FACE_OUTER_BOUND('',#14351,.T.) ;
#11250 = FACE_OUTER_BOUND('',#14352,.T.) ;
#11251 = FACE_OUTER_BOUND('',#14353,.T.) ;
#11252 = FACE_OUTER_BOUND('',#14354,.T.) ;
#11253 = FACE_OUTER_BOUND('',#14355,.T.) ;
#11254 = FACE_OUTER_BOUND('',#14356,.T.) ;
#11255 = FACE_OUTER_BOUND('',#14357,.T.) ;
#11256 = FACE_OUTER_BOUND('',#14358,.T.) ;
#11257 = FACE_OUTER_BOUND('',#14359,.T.) ;
#11258 = FACE_OUTER_BOUND('',#14360,.T.) ;
#11259 = FACE_OUTER_BOUND('',#14361,.T.) ;
#11260 = FACE_OUTER_BOUND('',#14362,.T.) ;
#11261 = FACE_OUTER_BOUND('',#14363,.T.) ;
#11262 = FACE_OUTER_BOUND('',#14364,.T.) ;
#11263 = FACE_OUTER_BOUND('',#14365,.T.) ;
#11264 = FACE_OUTER_BOUND('',#14366,.T.) ;
#11265 = FACE_OUTER_BOUND('',#14367,.T.) ;
#11266 = FACE_OUTER_BOUND('',#14368,.T.) ;
#11267 = FACE_OUTER_BOUND('',#14369,.T.) ;
#11268 = FACE_OUTER_BOUND('',#14370,.T.) ;
#11269 = FACE_OUTER_BOUND('',#14371,.T.) ;
#11270 = FACE_OUTER_BOUND('',#14372,.T.) ;
#11271 = FACE_OUTER_BOUND('',#14373,.T.) ;
#11272 = FACE_OUTER_BOUND('',#14374,.T.) ;
#11273 = FACE_OUTER_BOUND('',#14375,.T.) ;
#11274 = FACE_OUTER_BOUND('',#14376,.T.) ;
#11275 = FACE_OUTER_BOUND('',#14377,.T.) ;
#11276 = FACE_OUTER_BOUND('',#14378,.T.) ;
#11277 = FACE_OUTER_BOUND('',#14379,.T.) ;
#11278 = FACE_OUTER_BOUND('',#14380,.T.) ;
#11279 = FACE_OUTER_BOUND('',#14381,.T.) ;
#11280 = FACE_OUTER_BOUND('',#14382,.T.) ;
#11281 = FACE_OUTER_BOUND('',#14383,.T.) ;
#11282 = FACE_OUTER_BOUND('',#14384,.T.) ;
#11283 = FACE_OUTER_BOUND('',#14385,.T.) ;
#11284 = FACE_OUTER_BOUND('',#14386,.T.) ;
#11285 = FACE_OUTER_BOUND('',#14387,.T.) ;
#11286 = FACE_OUTER_BOUND('',#14388,.T.) ;
#11287 = FACE_OUTER_BOUND('',#14389,.T.) ;
#11288 = FACE_OUTER_BOUND('',#14390,.T.) ;
#11289 = FACE_OUTER_BOUND('',#14391,.T.) ;
#11290 = FACE_OUTER_BOUND('',#14392,.T.) ;
#11291 = FACE_OUTER_BOUND('',#14393,.T.) ;
#11292 = FACE_OUTER_BOUND('',#14394,.T.) ;
#11293 = FACE_OUTER_BOUND('',#14395,.T.) ;
#11294 = FACE_OUTER_BOUND('',#14396,.T.) ;
#11295 = FACE_OUTER_BOUND('',#14397,.T.) ;
#11296 = FACE_OUTER_BOUND('',#14398,.T.) ;
#11297 = FACE_OUTER_BOUND('',#14399,.T.) ;
#11298 = FACE_OUTER_BOUND('',#14400,.T.) ;
#11299 = FACE_OUTER_BOUND('',#14401,.T.) ;
#11300 = FACE_OUTER_BOUND('',#14402,.T.) ;
#11301 = FACE_OUTER_BOUND('',#14403,.T.) ;
#11302 = FACE_OUTER_BOUND('',#14404,.T.) ;
#11303 = FACE_OUTER_BOUND('',#14405,.T.) ;
#11304 = FACE_OUTER_BOUND('',#14406,.T.) ;
#11305 = FACE_OUTER_BOUND('',#14407,.T.) ;
#11306 = FACE_OUTER_BOUND('',#14426,.T.) ;
#11307 = FACE_OUTER_BOUND('',#14427,.T.) ;
#11308 = FACE_OUTER_BOUND('',#14428,.T.) ;
#11309 = FACE_OUTER_BOUND('',#14429,.T.) ;
#11310 = FACE_OUTER_BOUND('',#14430,.T.) ;
#11311 = FACE_OUTER_BOUND('',#14431,.T.) ;
#11312 = FACE_OUTER_BOUND('',#14432,.T.) ;
#11313 = FACE_OUTER_BOUND('',#14433,.T.) ;
#11314 = FACE_OUTER_BOUND('',#14434,.T.) ;
#11315 = FACE_OUTER_BOUND('',#14435,.T.) ;
#11316 = FACE_OUTER_BOUND('',#14436,.T.) ;
#11317 = FACE_OUTER_BOUND('',#14437,.T.) ;
#11318 = FACE_OUTER_BOUND('',#14438,.T.) ;
#11319 = FACE_OUTER_BOUND('',#14439,.T.) ;
#11320 = FACE_OUTER_BOUND('',#14440,.T.) ;
#11321 = FACE_OUTER_BOUND('',#14441,.T.) ;
#11322 = FACE_OUTER_BOUND('',#14442,.T.) ;
#11323 = FACE_OUTER_BOUND('',#14443,.T.) ;
#11324 = FACE_OUTER_BOUND('',#14444,.T.) ;
#11325 = FACE_OUTER_BOUND('',#14445,.T.) ;
#11326 = FACE_OUTER_BOUND('',#14446,.T.) ;
#11327 = FACE_OUTER_BOUND('',#14448,.T.) ;
#11328 = FACE_OUTER_BOUND('',#14449,.T.) ;
#11329 = FACE_OUTER_BOUND('',#14450,.T.) ;
#11330 = FACE_OUTER_BOUND('',#14451,.T.) ;
#11331 = FACE_OUTER_BOUND('',#14452,.T.) ;
#11332 = FACE_OUTER_BOUND('',#14467,.T.) ;
#11333 = FACE_OUTER_BOUND('',#14468,.T.) ;
#11334 = FACE_OUTER_BOUND('',#14469,.T.) ;
#11335 = FACE_OUTER_BOUND('',#14470,.T.) ;
#11336 = FACE_OUTER_BOUND('',#14471,.T.) ;
#11337 = FACE_OUTER_BOUND('',#14472,.T.) ;
#11338 = FACE_OUTER_BOUND('',#14473,.T.) ;
#11339 = FACE_OUTER_BOUND('',#14474,.T.) ;
#11340 = FACE_OUTER_BOUND('',#14475,.T.) ;
#11341 = FACE_OUTER_BOUND('',#14476,.T.) ;
#11342 = FACE_OUTER_BOUND('',#14477,.T.) ;
#11343 = FACE_OUTER_BOUND('',#14478,.T.) ;
#11344 = FACE_OUTER_BOUND('',#14479,.T.) ;
#11345 = FACE_OUTER_BOUND('',#14480,.T.) ;
#11346 = FACE_OUTER_BOUND('',#14481,.T.) ;
#11347 = FACE_OUTER_BOUND('',#14482,.T.) ;
#11348 = FACE_OUTER_BOUND('',#14483,.T.) ;
#11349 = FACE_OUTER_BOUND('',#14484,.T.) ;
#11350 = FACE_OUTER_BOUND('',#14485,.T.) ;
#11351 = FACE_OUTER_BOUND('',#14486,.T.) ;
#11352 = FACE_OUTER_BOUND('',#14487,.T.) ;
#11353 = FACE_OUTER_BOUND('',#14488,.T.) ;
#11354 = FACE_OUTER_BOUND('',#14489,.T.) ;
#11355 = FACE_OUTER_BOUND('',#14490,.T.) ;
#11356 = FACE_OUTER_BOUND('',#14491,.T.) ;
#11357 = FACE_OUTER_BOUND('',#14492,.T.) ;
#11358 = FACE_OUTER_BOUND('',#14493,.T.) ;
#11359 = FACE_OUTER_BOUND('',#14494,.T.) ;
#11360 = FACE_OUTER_BOUND('',#14495,.T.) ;
#11361 = FACE_OUTER_BOUND('',#14497,.T.) ;
#11362 = FACE_OUTER_BOUND('',#14498,.T.) ;
#11363 = FACE_OUTER_BOUND('',#14499,.T.) ;
#11364 = FACE_OUTER_BOUND('',#14500,.T.) ;
#11365 = FACE_OUTER_BOUND('',#14501,.T.) ;
#11366 = FACE_OUTER_BOUND('',#14503,.T.) ;
#11367 = FACE_OUTER_BOUND('',#14504,.T.) ;
#11368 = FACE_OUTER_BOUND('',#14506,.T.) ;
#11369 = FACE_OUTER_BOUND('',#14507,.T.) ;
#11370 = FACE_OUTER_BOUND('',#14508,.T.) ;
#11371 = FACE_OUTER_BOUND('',#14510,.T.) ;
#11372 = FACE_OUTER_BOUND('',#14511,.T.) ;
#11373 = FACE_OUTER_BOUND('',#14513,.T.) ;
#11374 = FACE_OUTER_BOUND('',#14514,.T.) ;
#11375 = FACE_OUTER_BOUND('',#14515,.T.) ;
#11376 = FACE_OUTER_BOUND('',#14516,.T.) ;
#11377 = FACE_OUTER_BOUND('',#14517,.T.) ;
#11378 = FACE_OUTER_BOUND('',#14518,.T.) ;
#11379 = FACE_OUTER_BOUND('',#14519,.T.) ;
#11380 = FACE_OUTER_BOUND('',#14520,.T.) ;
#11381 = FACE_OUTER_BOUND('',#14521,.T.) ;
#11382 = FACE_OUTER_BOUND('',#14522,.T.) ;
#11383 = FACE_OUTER_BOUND('',#14523,.T.) ;
#11384 = FACE_OUTER_BOUND('',#14524,.T.) ;
#11385 = FACE_OUTER_BOUND('',#14525,.T.) ;
#11386 = FACE_OUTER_BOUND('',#14526,.T.) ;
#11387 = FACE_OUTER_BOUND('',#14527,.T.) ;
#11388 = FACE_OUTER_BOUND('',#14528,.T.) ;
#11389 = FACE_OUTER_BOUND('',#14529,.T.) ;
#11390 = FACE_OUTER_BOUND('',#14530,.T.) ;
#11391 = FACE_OUTER_BOUND('',#14531,.T.) ;
#11392 = FACE_OUTER_BOUND('',#14532,.T.) ;
#11393 = FACE_OUTER_BOUND('',#14533,.T.) ;
#11394 = FACE_OUTER_BOUND('',#14534,.T.) ;
#11395 = FACE_OUTER_BOUND('',#14535,.T.) ;
#11396 = FACE_OUTER_BOUND('',#14536,.T.) ;
#11397 = FACE_OUTER_BOUND('',#14537,.T.) ;
#11398 = FACE_OUTER_BOUND('',#14538,.T.) ;
#11399 = FACE_OUTER_BOUND('',#14539,.T.) ;
#11400 = FACE_OUTER_BOUND('',#14540,.T.) ;
#11401 = FACE_OUTER_BOUND('',#14541,.T.) ;
#11402 = FACE_OUTER_BOUND('',#14542,.T.) ;
#11403 = FACE_OUTER_BOUND('',#14543,.T.) ;
#11404 = FACE_OUTER_BOUND('',#14544,.T.) ;
#11405 = FACE_OUTER_BOUND('',#14545,.T.) ;
#11406 = FACE_OUTER_BOUND('',#14546,.T.) ;
#11407 = FACE_OUTER_BOUND('',#14547,.T.) ;
#11408 = FACE_OUTER_BOUND('',#14548,.T.) ;
#11409 = FACE_OUTER_BOUND('',#14549,.T.) ;
#11410 = FACE_OUTER_BOUND('',#14550,.T.) ;
#11411 = FACE_OUTER_BOUND('',#14551,.T.) ;
#11412 = FACE_OUTER_BOUND('',#14552,.T.) ;
#11413 = FACE_OUTER_BOUND('',#14553,.T.) ;
#11414 = FACE_OUTER_BOUND('',#14554,.T.) ;
#11415 = FACE_OUTER_BOUND('',#14555,.T.) ;
#11416 = FACE_OUTER_BOUND('',#14556,.T.) ;
#11417 = FACE_OUTER_BOUND('',#14557,.T.) ;
#11418 = FACE_OUTER_BOUND('',#14558,.T.) ;
#11419 = FACE_OUTER_BOUND('',#14559,.T.) ;
#11420 = FACE_OUTER_BOUND('',#14560,.T.) ;
#11421 = FACE_OUTER_BOUND('',#14561,.T.) ;
#11422 = FACE_OUTER_BOUND('',#14562,.T.) ;
#11423 = FACE_OUTER_BOUND('',#14563,.T.) ;
#11424 = FACE_OUTER_BOUND('',#14564,.T.) ;
#11425 = FACE_OUTER_BOUND('',#14565,.T.) ;
#11426 = FACE_OUTER_BOUND('',#14566,.T.) ;
#11427 = FACE_OUTER_BOUND('',#14567,.T.) ;
#11428 = FACE_OUTER_BOUND('',#14568,.T.) ;
#11429 = FACE_OUTER_BOUND('',#14569,.T.) ;
#11430 = FACE_OUTER_BOUND('',#14570,.T.) ;
#11431 = FACE_OUTER_BOUND('',#14571,.T.) ;
#11432 = FACE_OUTER_BOUND('',#14572,.T.) ;
#11433 = FACE_OUTER_BOUND('',#14573,.T.) ;
#11434 = FACE_OUTER_BOUND('',#14574,.T.) ;
#11435 = FACE_OUTER_BOUND('',#14575,.T.) ;
#11436 = FACE_OUTER_BOUND('',#14576,.T.) ;
#11437 = FACE_OUTER_BOUND('',#14577,.T.) ;
#11438 = FACE_OUTER_BOUND('',#14578,.T.) ;
#11439 = FACE_OUTER_BOUND('',#14579,.T.) ;
#11440 = FACE_OUTER_BOUND('',#14580,.T.) ;
#11441 = FACE_OUTER_BOUND('',#14581,.T.) ;
#11442 = FACE_OUTER_BOUND('',#14582,.T.) ;
#11443 = FACE_OUTER_BOUND('',#14583,.T.) ;
#11444 = FACE_OUTER_BOUND('',#14584,.T.) ;
#11445 = FACE_OUTER_BOUND('',#14585,.T.) ;
#11446 = FACE_OUTER_BOUND('',#14586,.T.) ;
#11447 = FACE_OUTER_BOUND('',#14587,.T.) ;
#11448 = FACE_OUTER_BOUND('',#14588,.T.) ;
#11449 = FACE_OUTER_BOUND('',#14589,.T.) ;
#11450 = FACE_OUTER_BOUND('',#14590,.T.) ;
#11451 = FACE_OUTER_BOUND('',#14591,.T.) ;
#11452 = FACE_OUTER_BOUND('',#14592,.T.) ;
#11453 = FACE_OUTER_BOUND('',#14593,.T.) ;
#11454 = FACE_OUTER_BOUND('',#14594,.T.) ;
#11455 = FACE_OUTER_BOUND('',#14595,.T.) ;
#11456 = FACE_OUTER_BOUND('',#14596,.T.) ;
#11457 = FACE_OUTER_BOUND('',#14597,.T.) ;
#11458 = FACE_OUTER_BOUND('',#14598,.T.) ;
#11459 = FACE_OUTER_BOUND('',#14599,.T.) ;
#11460 = FACE_OUTER_BOUND('',#14600,.T.) ;
#11461 = FACE_OUTER_BOUND('',#14601,.T.) ;
#11462 = FACE_OUTER_BOUND('',#14602,.T.) ;
#11463 = FACE_OUTER_BOUND('',#14603,.T.) ;
#11464 = FACE_OUTER_BOUND('',#14604,.T.) ;
#11465 = FACE_OUTER_BOUND('',#14605,.T.) ;
#11466 = FACE_OUTER_BOUND('',#14606,.T.) ;
#11467 = FACE_OUTER_BOUND('',#14607,.T.) ;
#11468 = FACE_OUTER_BOUND('',#14608,.T.) ;
#11469 = FACE_OUTER_BOUND('',#14609,.T.) ;
#11470 = FACE_OUTER_BOUND('',#14610,.T.) ;
#11471 = FACE_OUTER_BOUND('',#14611,.T.) ;
#11472 = FACE_OUTER_BOUND('',#14612,.T.) ;
#11473 = FACE_OUTER_BOUND('',#14613,.T.) ;
#11474 = FACE_OUTER_BOUND('',#14614,.T.) ;
#11475 = FACE_OUTER_BOUND('',#14615,.T.) ;
#11476 = FACE_OUTER_BOUND('',#14616,.T.) ;
#11477 = FACE_OUTER_BOUND('',#14617,.T.) ;
#11478 = FACE_OUTER_BOUND('',#14618,.T.) ;
#11479 = FACE_OUTER_BOUND('',#14619,.T.) ;
#11480 = FACE_OUTER_BOUND('',#14620,.T.) ;
#11481 = FACE_OUTER_BOUND('',#14621,.T.) ;
#11482 = FACE_OUTER_BOUND('',#14622,.T.) ;
#11483 = FACE_OUTER_BOUND('',#14623,.T.) ;
#11484 = FACE_OUTER_BOUND('',#14624,.T.) ;
#11485 = FACE_OUTER_BOUND('',#14625,.T.) ;
#11486 = FACE_OUTER_BOUND('',#14626,.T.) ;
#11487 = FACE_OUTER_BOUND('',#14627,.T.) ;
#11488 = FACE_OUTER_BOUND('',#14628,.T.) ;
#11489 = FACE_OUTER_BOUND('',#14629,.T.) ;
#11490 = FACE_OUTER_BOUND('',#14630,.T.) ;
#11491 = FACE_OUTER_BOUND('',#14631,.T.) ;
#11492 = FACE_OUTER_BOUND('',#14632,.T.) ;
#11493 = FACE_OUTER_BOUND('',#14633,.T.) ;
#11494 = FACE_OUTER_BOUND('',#14634,.T.) ;
#11495 = FACE_OUTER_BOUND('',#14635,.T.) ;
#11496 = FACE_OUTER_BOUND('',#14636,.T.) ;
#11497 = FACE_OUTER_BOUND('',#14637,.T.) ;
#11498 = FACE_OUTER_BOUND('',#14638,.T.) ;
#11499 = FACE_OUTER_BOUND('',#14639,.T.) ;
#11500 = FACE_OUTER_BOUND('',#14640,.T.) ;
#11501 = FACE_OUTER_BOUND('',#14641,.T.) ;
#11502 = FACE_OUTER_BOUND('',#14642,.T.) ;
#11503 = FACE_OUTER_BOUND('',#14643,.T.) ;
#11504 = FACE_OUTER_BOUND('',#14644,.T.) ;
#11505 = FACE_OUTER_BOUND('',#14645,.T.) ;
#11506 = FACE_OUTER_BOUND('',#14646,.T.) ;
#11507 = FACE_OUTER_BOUND('',#14647,.T.) ;
#11508 = FACE_OUTER_BOUND('',#14648,.T.) ;
#11509 = FACE_OUTER_BOUND('',#14649,.T.) ;
#11510 = FACE_OUTER_BOUND('',#14650,.T.) ;
#11511 = FACE_OUTER_BOUND('',#14651,.T.) ;
#11512 = FACE_OUTER_BOUND('',#14652,.T.) ;
#11513 = FACE_OUTER_BOUND('',#14653,.T.) ;
#11514 = FACE_OUTER_BOUND('',#14654,.T.) ;
#11515 = FACE_OUTER_BOUND('',#14655,.T.) ;
#11516 = FACE_OUTER_BOUND('',#14656,.T.) ;
#11517 = FACE_OUTER_BOUND('',#14657,.T.) ;
#11518 = FACE_OUTER_BOUND('',#14658,.T.) ;
#11519 = FACE_OUTER_BOUND('',#14659,.T.) ;
#11520 = FACE_OUTER_BOUND('',#14660,.T.) ;
#11521 = FACE_OUTER_BOUND('',#14661,.T.) ;
#11522 = FACE_OUTER_BOUND('',#14662,.T.) ;
#11523 = FACE_OUTER_BOUND('',#14663,.T.) ;
#11524 = FACE_OUTER_BOUND('',#14664,.T.) ;
#11525 = FACE_OUTER_BOUND('',#14665,.T.) ;
#11526 = FACE_OUTER_BOUND('',#14666,.T.) ;
#11527 = FACE_OUTER_BOUND('',#14667,.T.) ;
#11528 = FACE_OUTER_BOUND('',#14668,.T.) ;
#11529 = FACE_OUTER_BOUND('',#14669,.T.) ;
#11530 = FACE_OUTER_BOUND('',#14670,.T.) ;
#11531 = FACE_OUTER_BOUND('',#14671,.T.) ;
#11532 = FACE_OUTER_BOUND('',#14672,.T.) ;
#11533 = FACE_OUTER_BOUND('',#14673,.T.) ;
#11534 = FACE_OUTER_BOUND('',#14674,.T.) ;
#11535 = FACE_OUTER_BOUND('',#14675,.T.) ;
#11536 = FACE_OUTER_BOUND('',#14676,.T.) ;
#11537 = FACE_OUTER_BOUND('',#14677,.T.) ;
#11538 = FACE_OUTER_BOUND('',#14678,.T.) ;
#11539 = FACE_OUTER_BOUND('',#14679,.T.) ;
#11540 = FACE_OUTER_BOUND('',#14680,.T.) ;
#11541 = FACE_OUTER_BOUND('',#14681,.T.) ;
#11542 = FACE_OUTER_BOUND('',#14682,.T.) ;
#11543 = FACE_OUTER_BOUND('',#14683,.T.) ;
#11544 = FACE_OUTER_BOUND('',#14684,.T.) ;
#11545 = FACE_OUTER_BOUND('',#14685,.T.) ;
#11546 = FACE_OUTER_BOUND('',#14686,.T.) ;
#11547 = FACE_OUTER_BOUND('',#14687,.T.) ;
#11548 = FACE_OUTER_BOUND('',#14688,.T.) ;
#11549 = FACE_OUTER_BOUND('',#14689,.T.) ;
#11550 = FACE_OUTER_BOUND('',#14690,.T.) ;
#11551 = FACE_OUTER_BOUND('',#14691,.T.) ;
#11552 = FACE_OUTER_BOUND('',#14692,.T.) ;
#11553 = FACE_OUTER_BOUND('',#14693,.T.) ;
#11554 = FACE_OUTER_BOUND('',#14694,.T.) ;
#11555 = FACE_OUTER_BOUND('',#14695,.T.) ;
#11556 = FACE_OUTER_BOUND('',#14696,.T.) ;
#11557 = FACE_OUTER_BOUND('',#14697,.T.) ;
#11558 = FACE_OUTER_BOUND('',#14698,.T.) ;
#11559 = FACE_OUTER_BOUND('',#14699,.T.) ;
#11560 = FACE_OUTER_BOUND('',#14700,.T.) ;
#11561 = FACE_OUTER_BOUND('',#14701,.T.) ;
#11562 = FACE_OUTER_BOUND('',#14702,.T.) ;
#11563 = FACE_OUTER_BOUND('',#14703,.T.) ;
#11564 = FACE_OUTER_BOUND('',#14704,.T.) ;
#11565 = FACE_OUTER_BOUND('',#14705,.T.) ;
#11566 = FACE_OUTER_BOUND('',#14706,.T.) ;
#11567 = FACE_OUTER_BOUND('',#14707,.T.) ;
#11568 = FACE_OUTER_BOUND('',#14708,.T.) ;
#11569 = FACE_OUTER_BOUND('',#14709,.T.) ;
#11570 = FACE_OUTER_BOUND('',#14710,.T.) ;
#11571 = FACE_OUTER_BOUND('',#14711,.T.) ;
#11572 = FACE_OUTER_BOUND('',#14712,.T.) ;
#11573 = FACE_OUTER_BOUND('',#14713,.T.) ;
#11574 = FACE_OUTER_BOUND('',#14714,.T.) ;
#11575 = FACE_OUTER_BOUND('',#14715,.T.) ;
#11576 = FACE_OUTER_BOUND('',#14716,.T.) ;
#11577 = FACE_OUTER_BOUND('',#14717,.T.) ;
#11578 = FACE_OUTER_BOUND('',#14718,.T.) ;
#11579 = FACE_OUTER_BOUND('',#14719,.T.) ;
#11580 = FACE_OUTER_BOUND('',#14720,.T.) ;
#11581 = FACE_OUTER_BOUND('',#14721,.T.) ;
#11582 = FACE_OUTER_BOUND('',#14722,.T.) ;
#11583 = FACE_OUTER_BOUND('',#14723,.T.) ;
#11584 = FACE_OUTER_BOUND('',#14724,.T.) ;
#11585 = FACE_OUTER_BOUND('',#14725,.T.) ;
#11586 = FACE_OUTER_BOUND('',#14726,.T.) ;
#11587 = FACE_OUTER_BOUND('',#14727,.T.) ;
#11588 = FACE_OUTER_BOUND('',#14728,.T.) ;
#11589 = FACE_OUTER_BOUND('',#14729,.T.) ;
#11590 = FACE_OUTER_BOUND('',#14730,.T.) ;
#11591 = FACE_OUTER_BOUND('',#14731,.T.) ;
#11592 = FACE_OUTER_BOUND('',#14732,.T.) ;
#11593 = FACE_OUTER_BOUND('',#14733,.T.) ;
#11594 = FACE_OUTER_BOUND('',#14734,.T.) ;
#11595 = FACE_OUTER_BOUND('',#14735,.T.) ;
#11596 = FACE_OUTER_BOUND('',#14736,.T.) ;
#11597 = FACE_OUTER_BOUND('',#14737,.T.) ;
#11598 = FACE_OUTER_BOUND('',#14738,.T.) ;
#11599 = FACE_OUTER_BOUND('',#14739,.T.) ;
#11600 = FACE_OUTER_BOUND('',#14740,.T.) ;
#11601 = FACE_OUTER_BOUND('',#14741,.T.) ;
#11602 = FACE_OUTER_BOUND('',#14742,.T.) ;
#11603 = FACE_OUTER_BOUND('',#14743,.T.) ;
#11604 = FACE_OUTER_BOUND('',#14744,.T.) ;
#11605 = FACE_OUTER_BOUND('',#14745,.T.) ;
#11606 = FACE_OUTER_BOUND('',#14746,.T.) ;
#11607 = FACE_OUTER_BOUND('',#14747,.T.) ;
#11608 = FACE_OUTER_BOUND('',#14748,.T.) ;
#11609 = FACE_OUTER_BOUND('',#14749,.T.) ;
#11610 = FACE_OUTER_BOUND('',#14750,.T.) ;
#11611 = FACE_OUTER_BOUND('',#14751,.T.) ;
#11612 = FACE_OUTER_BOUND('',#14752,.T.) ;
#11613 = FACE_OUTER_BOUND('',#14753,.T.) ;
#11614 = FACE_OUTER_BOUND('',#14754,.T.) ;
#11615 = FACE_OUTER_BOUND('',#14755,.T.) ;
#11616 = FACE_OUTER_BOUND('',#14756,.T.) ;
#11617 = FACE_OUTER_BOUND('',#14757,.T.) ;
#11618 = FACE_OUTER_BOUND('',#14758,.T.) ;
#11619 = FACE_OUTER_BOUND('',#14759,.T.) ;
#11620 = FACE_OUTER_BOUND('',#14760,.T.) ;
#11621 = FACE_OUTER_BOUND('',#14761,.T.) ;
#11622 = FACE_OUTER_BOUND('',#14762,.T.) ;
#11623 = FACE_OUTER_BOUND('',#14763,.T.) ;
#11624 = FACE_OUTER_BOUND('',#14764,.T.) ;
#11625 = FACE_OUTER_BOUND('',#14765,.T.) ;
#11626 = FACE_OUTER_BOUND('',#14766,.T.) ;
#11627 = FACE_OUTER_BOUND('',#14767,.T.) ;
#11628 = FACE_OUTER_BOUND('',#14768,.T.) ;
#11629 = FACE_OUTER_BOUND('',#14769,.T.) ;
#11630 = FACE_OUTER_BOUND('',#14770,.T.) ;
#11631 = FACE_OUTER_BOUND('',#14771,.T.) ;
#11632 = FACE_OUTER_BOUND('',#14772,.T.) ;
#11633 = FACE_OUTER_BOUND('',#14773,.T.) ;
#11634 = FACE_OUTER_BOUND('',#14774,.T.) ;
#11635 = FACE_OUTER_BOUND('',#14775,.T.) ;
#11636 = FACE_OUTER_BOUND('',#14776,.T.) ;
#11637 = FACE_OUTER_BOUND('',#14777,.T.) ;
#11638 = FACE_OUTER_BOUND('',#14778,.T.) ;
#11639 = FACE_OUTER_BOUND('',#14779,.T.) ;
#11640 = FACE_OUTER_BOUND('',#14780,.T.) ;
#11641 = FACE_OUTER_BOUND('',#14781,.T.) ;
#11642 = FACE_OUTER_BOUND('',#14782,.T.) ;
#11643 = FACE_OUTER_BOUND('',#14783,.T.) ;
#11644 = FACE_OUTER_BOUND('',#14784,.T.) ;
#11645 = FACE_OUTER_BOUND('',#14785,.T.) ;
#11646 = FACE_OUTER_BOUND('',#14786,.T.) ;
#11647 = FACE_OUTER_BOUND('',#14787,.T.) ;
#11648 = FACE_OUTER_BOUND('',#14788,.T.) ;
#11649 = FACE_OUTER_BOUND('',#14789,.T.) ;
#11650 = FACE_OUTER_BOUND('',#14790,.T.) ;
#11651 = FACE_OUTER_BOUND('',#14791,.T.) ;
#11652 = FACE_OUTER_BOUND('',#14792,.T.) ;
#11653 = FACE_OUTER_BOUND('',#14793,.T.) ;
#11654 = FACE_OUTER_BOUND('',#14794,.T.) ;
#11655 = FACE_OUTER_BOUND('',#14795,.T.) ;
#11656 = FACE_OUTER_BOUND('',#14796,.T.) ;
#11657 = FACE_OUTER_BOUND('',#14797,.T.) ;
#11658 = FACE_OUTER_BOUND('',#14798,.T.) ;
#11659 = FACE_OUTER_BOUND('',#14799,.T.) ;
#11660 = FACE_OUTER_BOUND('',#14800,.T.) ;
#11661 = FACE_OUTER_BOUND('',#14801,.T.) ;
#11662 = FACE_OUTER_BOUND('',#14802,.T.) ;
#11663 = FACE_OUTER_BOUND('',#14803,.T.) ;
#11664 = FACE_OUTER_BOUND('',#14804,.T.) ;
#11665 = FACE_OUTER_BOUND('',#14805,.T.) ;
#11666 = FACE_OUTER_BOUND('',#14806,.T.) ;
#11667 = FACE_OUTER_BOUND('',#14807,.T.) ;
#11668 = FACE_OUTER_BOUND('',#14808,.T.) ;
#11669 = FACE_OUTER_BOUND('',#14809,.T.) ;
#11670 = FACE_OUTER_BOUND('',#14810,.T.) ;
#11671 = FACE_OUTER_BOUND('',#14811,.T.) ;
#11672 = FACE_OUTER_BOUND('',#14812,.T.) ;
#11673 = FACE_OUTER_BOUND('',#14813,.T.) ;
#11674 = FACE_OUTER_BOUND('',#14814,.T.) ;
#11675 = FACE_OUTER_BOUND('',#14815,.T.) ;
#11676 = FACE_OUTER_BOUND('',#14816,.T.) ;
#11677 = FACE_OUTER_BOUND('',#14817,.T.) ;
#11678 = FACE_OUTER_BOUND('',#14818,.T.) ;
#11679 = FACE_OUTER_BOUND('',#14819,.T.) ;
#11680 = FACE_OUTER_BOUND('',#14820,.T.) ;
#11681 = FACE_OUTER_BOUND('',#14821,.T.) ;
#11682 = FACE_OUTER_BOUND('',#14822,.T.) ;
#11683 = FACE_OUTER_BOUND('',#14823,.T.) ;
#11684 = FACE_OUTER_BOUND('',#14824,.T.) ;
#11685 = FACE_OUTER_BOUND('',#14825,.T.) ;
#11686 = FACE_OUTER_BOUND('',#14826,.T.) ;
#11687 = FACE_OUTER_BOUND('',#14827,.T.) ;
#11688 = FACE_OUTER_BOUND('',#14828,.T.) ;
#11689 = FACE_OUTER_BOUND('',#14829,.T.) ;
#11690 = FACE_OUTER_BOUND('',#14830,.T.) ;
#11691 = FACE_OUTER_BOUND('',#14831,.T.) ;
#11692 = FACE_OUTER_BOUND('',#14832,.T.) ;
#11693 = FACE_OUTER_BOUND('',#14833,.T.) ;
#11694 = FACE_OUTER_BOUND('',#14834,.T.) ;
#11695 = FACE_OUTER_BOUND('',#14835,.T.) ;
#11696 = FACE_OUTER_BOUND('',#14836,.T.) ;
#11697 = FACE_OUTER_BOUND('',#14837,.T.) ;
#11698 = FACE_OUTER_BOUND('',#14838,.T.) ;
#11699 = FACE_OUTER_BOUND('',#14839,.T.) ;
#11700 = FACE_OUTER_BOUND('',#14840,.T.) ;
#11701 = FACE_OUTER_BOUND('',#14841,.T.) ;
#11702 = FACE_OUTER_BOUND('',#14842,.T.) ;
#11703 = FACE_OUTER_BOUND('',#14843,.T.) ;
#11704 = FACE_OUTER_BOUND('',#14844,.T.) ;
#11705 = FACE_OUTER_BOUND('',#14845,.T.) ;
#11706 = FACE_OUTER_BOUND('',#14846,.T.) ;
#11707 = FACE_OUTER_BOUND('',#14847,.T.) ;
#11708 = FACE_OUTER_BOUND('',#14848,.T.) ;
#11709 = FACE_OUTER_BOUND('',#14849,.T.) ;
#11710 = FACE_OUTER_BOUND('',#14850,.T.) ;
#11711 = FACE_OUTER_BOUND('',#14851,.T.) ;
#11712 = FACE_OUTER_BOUND('',#14852,.T.) ;
#11713 = FACE_OUTER_BOUND('',#14853,.T.) ;
#11714 = FACE_OUTER_BOUND('',#14854,.T.) ;
#11715 = FACE_OUTER_BOUND('',#14855,.T.) ;
#11716 = FACE_OUTER_BOUND('',#14856,.T.) ;
#11717 = FACE_OUTER_BOUND('',#14857,.T.) ;
#11718 = FACE_OUTER_BOUND('',#14858,.T.) ;
#11719 = FACE_OUTER_BOUND('',#14859,.T.) ;
#11720 = FACE_OUTER_BOUND('',#14860,.T.) ;
#11721 = FACE_OUTER_BOUND('',#14861,.T.) ;
#11722 = FACE_OUTER_BOUND('',#14862,.T.) ;
#11723 = FACE_OUTER_BOUND('',#14863,.T.) ;
#11724 = FACE_OUTER_BOUND('',#14864,.T.) ;
#11725 = FACE_OUTER_BOUND('',#14865,.T.) ;
#11726 = FACE_OUTER_BOUND('',#14866,.T.) ;
#11727 = FACE_OUTER_BOUND('',#14867,.T.) ;
#11728 = FACE_OUTER_BOUND('',#14868,.T.) ;
#11729 = FACE_OUTER_BOUND('',#14869,.T.) ;
#11730 = FACE_OUTER_BOUND('',#14870,.T.) ;
#11731 = FACE_OUTER_BOUND('',#14871,.T.) ;
#11732 = FACE_OUTER_BOUND('',#14872,.T.) ;
#11733 = FACE_OUTER_BOUND('',#14873,.T.) ;
#11734 = FACE_OUTER_BOUND('',#14874,.T.) ;
#11735 = FACE_OUTER_BOUND('',#14875,.T.) ;
#11736 = FACE_OUTER_BOUND('',#14876,.T.) ;
#11737 = FACE_OUTER_BOUND('',#14877,.T.) ;
#11738 = FACE_OUTER_BOUND('',#14878,.T.) ;
#11739 = FACE_OUTER_BOUND('',#14879,.T.) ;
#11740 = FACE_OUTER_BOUND('',#14880,.T.) ;
#11741 = FACE_OUTER_BOUND('',#14881,.T.) ;
#11742 = FACE_OUTER_BOUND('',#14882,.T.) ;
#11743 = FACE_OUTER_BOUND('',#14883,.T.) ;
#11744 = FACE_OUTER_BOUND('',#14884,.T.) ;
#11745 = FACE_OUTER_BOUND('',#14885,.T.) ;
#11746 = FACE_OUTER_BOUND('',#14886,.T.) ;
#11747 = FACE_OUTER_BOUND('',#14887,.T.) ;
#11748 = FACE_OUTER_BOUND('',#14888,.T.) ;
#11749 = FACE_OUTER_BOUND('',#14889,.T.) ;
#11750 = FACE_OUTER_BOUND('',#14890,.T.) ;
#11751 = FACE_OUTER_BOUND('',#14891,.T.) ;
#11752 = FACE_OUTER_BOUND('',#14892,.T.) ;
#11753 = FACE_OUTER_BOUND('',#14893,.T.) ;
#11754 = FACE_OUTER_BOUND('',#14894,.T.) ;
#11755 = FACE_OUTER_BOUND('',#14895,.T.) ;
#11756 = FACE_OUTER_BOUND('',#14896,.T.) ;
#11757 = FACE_OUTER_BOUND('',#14897,.T.) ;
#11758 = FACE_OUTER_BOUND('',#14898,.T.) ;
#11759 = FACE_OUTER_BOUND('',#14899,.T.) ;
#11760 = FACE_OUTER_BOUND('',#14900,.T.) ;
#11761 = FACE_OUTER_BOUND('',#14901,.T.) ;
#11762 = FACE_OUTER_BOUND('',#14902,.T.) ;
#11763 = FACE_OUTER_BOUND('',#14903,.T.) ;
#11764 = FACE_OUTER_BOUND('',#14904,.T.) ;
#11765 = FACE_OUTER_BOUND('',#14905,.T.) ;
#11766 = FACE_OUTER_BOUND('',#14906,.T.) ;
#11767 = FACE_OUTER_BOUND('',#14907,.T.) ;
#11768 = FACE_OUTER_BOUND('',#14908,.T.) ;
#11769 = FACE_OUTER_BOUND('',#14909,.T.) ;
#11770 = FACE_OUTER_BOUND('',#14910,.T.) ;
#11771 = FACE_OUTER_BOUND('',#14911,.T.) ;
#11772 = FACE_OUTER_BOUND('',#14912,.T.) ;
#11773 = FACE_OUTER_BOUND('',#14913,.T.) ;
#11774 = FACE_OUTER_BOUND('',#14914,.T.) ;
#11775 = FACE_OUTER_BOUND('',#14915,.T.) ;
#11776 = FACE_OUTER_BOUND('',#14916,.T.) ;
#11777 = FACE_OUTER_BOUND('',#14917,.T.) ;
#11778 = FACE_OUTER_BOUND('',#14918,.T.) ;
#11779 = FACE_OUTER_BOUND('',#14919,.T.) ;
#11780 = FACE_OUTER_BOUND('',#14920,.T.) ;
#11781 = FACE_OUTER_BOUND('',#14921,.T.) ;
#11782 = FACE_OUTER_BOUND('',#14922,.T.) ;
#11783 = FACE_OUTER_BOUND('',#14923,.T.) ;
#11784 = FACE_OUTER_BOUND('',#14924,.T.) ;
#11785 = FACE_OUTER_BOUND('',#14925,.T.) ;
#11786 = FACE_OUTER_BOUND('',#14926,.T.) ;
#11787 = FACE_OUTER_BOUND('',#14927,.T.) ;
#11788 = FACE_OUTER_BOUND('',#14928,.T.) ;
#11789 = FACE_OUTER_BOUND('',#14929,.T.) ;
#11790 = FACE_OUTER_BOUND('',#14930,.T.) ;
#11791 = FACE_OUTER_BOUND('',#14931,.T.) ;
#11792 = FACE_OUTER_BOUND('',#14932,.T.) ;
#11793 = FACE_OUTER_BOUND('',#14933,.T.) ;
#11794 = FACE_OUTER_BOUND('',#14934,.T.) ;
#11795 = FACE_OUTER_BOUND('',#14935,.T.) ;
#11796 = FACE_OUTER_BOUND('',#14936,.T.) ;
#11797 = FACE_OUTER_BOUND('',#14937,.T.) ;
#11798 = FACE_OUTER_BOUND('',#14938,.T.) ;
#11799 = FACE_OUTER_BOUND('',#14939,.T.) ;
#11800 = FACE_OUTER_BOUND('',#14940,.T.) ;
#11801 = FACE_OUTER_BOUND('',#14941,.T.) ;
#11802 = FACE_OUTER_BOUND('',#14942,.T.) ;
#11803 = FACE_OUTER_BOUND('',#14943,.T.) ;
#11804 = FACE_OUTER_BOUND('',#14944,.T.) ;
#11805 = FACE_OUTER_BOUND('',#14945,.T.) ;
#11806 = FACE_OUTER_BOUND('',#14946,.T.) ;
#11807 = FACE_OUTER_BOUND('',#14947,.T.) ;
#11808 = FACE_OUTER_BOUND('',#14948,.T.) ;
#11809 = FACE_OUTER_BOUND('',#14949,.T.) ;
#11810 = FACE_OUTER_BOUND('',#14950,.T.) ;
#11811 = FACE_OUTER_BOUND('',#14951,.T.) ;
#11812 = FACE_OUTER_BOUND('',#14952,.T.) ;
#11813 = FACE_OUTER_BOUND('',#14953,.T.) ;
#11814 = FACE_OUTER_BOUND('',#14954,.T.) ;
#11815 = FACE_OUTER_BOUND('',#14955,.T.) ;
#11816 = FACE_OUTER_BOUND('',#14956,.T.) ;
#11817 = FACE_OUTER_BOUND('',#14957,.T.) ;
#11818 = FACE_OUTER_BOUND('',#14958,.T.) ;
#11819 = FACE_OUTER_BOUND('',#14959,.T.) ;
#11820 = FACE_OUTER_BOUND('',#14960,.T.) ;
#11821 = FACE_OUTER_BOUND('',#14961,.T.) ;
#11822 = FACE_OUTER_BOUND('',#14962,.T.) ;
#11823 = FACE_OUTER_BOUND('',#14963,.T.) ;
#11824 = FACE_OUTER_BOUND('',#14964,.T.) ;
#11825 = FACE_OUTER_BOUND('',#14965,.T.) ;
#11826 = FACE_OUTER_BOUND('',#14966,.T.) ;
#11827 = FACE_OUTER_BOUND('',#14967,.T.) ;
#11828 = FACE_OUTER_BOUND('',#14968,.T.) ;
#11829 = FACE_OUTER_BOUND('',#14969,.T.) ;
#11830 = FACE_OUTER_BOUND('',#14970,.T.) ;
#11831 = FACE_OUTER_BOUND('',#14971,.T.) ;
#11832 = FACE_OUTER_BOUND('',#14972,.T.) ;
#11833 = FACE_OUTER_BOUND('',#14973,.T.) ;
#11834 = FACE_OUTER_BOUND('',#14974,.T.) ;
#11835 = FACE_OUTER_BOUND('',#14975,.T.) ;
#11836 = FACE_OUTER_BOUND('',#14976,.T.) ;
#11837 = FACE_OUTER_BOUND('',#14977,.T.) ;
#11838 = FACE_OUTER_BOUND('',#14978,.T.) ;
#11839 = FACE_OUTER_BOUND('',#14979,.T.) ;
#11840 = FACE_OUTER_BOUND('',#14980,.T.) ;
#11841 = FACE_OUTER_BOUND('',#14981,.T.) ;
#11842 = FACE_OUTER_BOUND('',#14982,.T.) ;
#11843 = FACE_OUTER_BOUND('',#14983,.T.) ;
#11844 = FACE_OUTER_BOUND('',#14984,.T.) ;
#11845 = FACE_OUTER_BOUND('',#14985,.T.) ;
#11846 = FACE_OUTER_BOUND('',#14986,.T.) ;
#11847 = FACE_OUTER_BOUND('',#14987,.T.) ;
#11848 = FACE_OUTER_BOUND('',#14988,.T.) ;
#11849 = FACE_OUTER_BOUND('',#14989,.T.) ;
#11850 = FACE_OUTER_BOUND('',#14990,.T.) ;
#11851 = FACE_OUTER_BOUND('',#14991,.T.) ;
#11852 = FACE_OUTER_BOUND('',#14992,.T.) ;
#11853 = FACE_OUTER_BOUND('',#14993,.T.) ;
#11854 = FACE_OUTER_BOUND('',#14994,.T.) ;
#11855 = FACE_OUTER_BOUND('',#14995,.T.) ;
#11856 = FACE_OUTER_BOUND('',#14996,.T.) ;
#11857 = FACE_OUTER_BOUND('',#14997,.T.) ;
#11858 = FACE_OUTER_BOUND('',#14998,.T.) ;
#11859 = FACE_OUTER_BOUND('',#14999,.T.) ;
#11860 = FACE_OUTER_BOUND('',#15000,.T.) ;
#11861 = FACE_OUTER_BOUND('',#15001,.T.) ;
#11862 = FACE_OUTER_BOUND('',#15002,.T.) ;
#11863 = FACE_OUTER_BOUND('',#15003,.T.) ;
#11864 = FACE_OUTER_BOUND('',#15004,.T.) ;
#11865 = FACE_OUTER_BOUND('',#15005,.T.) ;
#11866 = FACE_OUTER_BOUND('',#15006,.T.) ;
#11867 = FACE_OUTER_BOUND('',#15007,.T.) ;
#11868 = FACE_OUTER_BOUND('',#15008,.T.) ;
#11869 = FACE_OUTER_BOUND('',#15009,.T.) ;
#11870 = FACE_OUTER_BOUND('',#15010,.T.) ;
#11871 = FACE_OUTER_BOUND('',#15011,.T.) ;
#11872 = FACE_OUTER_BOUND('',#15012,.T.) ;
#11873 = FACE_OUTER_BOUND('',#15013,.T.) ;
#11874 = FACE_OUTER_BOUND('',#15014,.T.) ;
#11875 = FACE_OUTER_BOUND('',#15015,.T.) ;
#11876 = FACE_OUTER_BOUND('',#15016,.T.) ;
#11877 = FACE_OUTER_BOUND('',#15018,.T.) ;
#11878 = FACE_OUTER_BOUND('',#15019,.T.) ;
#11879 = FACE_OUTER_BOUND('',#15020,.T.) ;
#11880 = FACE_OUTER_BOUND('',#15021,.T.) ;
#11881 = FACE_OUTER_BOUND('',#15022,.T.) ;
#11882 = FACE_OUTER_BOUND('',#15023,.T.) ;
#11883 = FACE_OUTER_BOUND('',#15024,.T.) ;
#11884 = FACE_OUTER_BOUND('',#15026,.T.) ;
#11885 = FACE_OUTER_BOUND('',#15027,.T.) ;
#11886 = FACE_OUTER_BOUND('',#15028,.T.) ;
#11887 = FACE_OUTER_BOUND('',#15029,.T.) ;
#11888 = FACE_OUTER_BOUND('',#15030,.T.) ;
#11889 = FACE_OUTER_BOUND('',#15031,.T.) ;
#11890 = FACE_OUTER_BOUND('',#15033,.T.) ;
#11891 = FACE_OUTER_BOUND('',#15034,.T.) ;
#11892 = FACE_OUTER_BOUND('',#15035,.T.) ;
#11893 = FACE_OUTER_BOUND('',#15036,.T.) ;
#11894 = FACE_OUTER_BOUND('',#15037,.T.) ;
#11895 = FACE_OUTER_BOUND('',#15039,.T.) ;
#11896 = FACE_OUTER_BOUND('',#15040,.T.) ;
#11897 = FACE_OUTER_BOUND('',#15041,.T.) ;
#11898 = FACE_OUTER_BOUND('',#15042,.T.) ;
#11899 = FACE_OUTER_BOUND('',#15043,.T.) ;
#11900 = FACE_OUTER_BOUND('',#15044,.T.) ;
#11901 = FACE_OUTER_BOUND('',#15045,.T.) ;
#11902 = FACE_OUTER_BOUND('',#15046,.T.) ;
#11903 = FACE_OUTER_BOUND('',#15047,.T.) ;
#11904 = FACE_OUTER_BOUND('',#15048,.T.) ;
#11905 = FACE_OUTER_BOUND('',#15049,.T.) ;
#11906 = FACE_OUTER_BOUND('',#15050,.T.) ;
#11907 = FACE_OUTER_BOUND('',#15051,.T.) ;
#11908 = FACE_OUTER_BOUND('',#15052,.T.) ;
#11909 = FACE_OUTER_BOUND('',#15053,.T.) ;
#11910 = FACE_OUTER_BOUND('',#15054,.T.) ;
#11911 = FACE_OUTER_BOUND('',#15055,.T.) ;
#11912 = FACE_OUTER_BOUND('',#15056,.T.) ;
#11913 = FACE_OUTER_BOUND('',#15057,.T.) ;
#11914 = FACE_OUTER_BOUND('',#15058,.T.) ;
#11915 = FACE_OUTER_BOUND('',#15059,.T.) ;
#11916 = FACE_OUTER_BOUND('',#15060,.T.) ;
#11917 = FACE_OUTER_BOUND('',#15061,.T.) ;
#11918 = FACE_OUTER_BOUND('',#15062,.T.) ;
#11919 = FACE_OUTER_BOUND('',#15063,.T.) ;
#11920 = FACE_OUTER_BOUND('',#15064,.T.) ;
#11921 = FACE_OUTER_BOUND('',#15065,.T.) ;
#11922 = FACE_OUTER_BOUND('',#15066,.T.) ;
#11923 = FACE_OUTER_BOUND('',#15067,.T.) ;
#11924 = FACE_OUTER_BOUND('',#15068,.T.) ;
#11925 = FACE_OUTER_BOUND('',#15069,.T.) ;
#11926 = FACE_OUTER_BOUND('',#15070,.T.) ;
#11927 = FACE_OUTER_BOUND('',#15071,.T.) ;
#11928 = FACE_OUTER_BOUND('',#15072,.T.) ;
#11929 = FACE_OUTER_BOUND('',#15073,.T.) ;
#11930 = FACE_OUTER_BOUND('',#15074,.T.) ;
#11931 = FACE_OUTER_BOUND('',#15075,.T.) ;
#11932 = FACE_OUTER_BOUND('',#15076,.T.) ;
#11933 = FACE_OUTER_BOUND('',#15077,.T.) ;
#11934 = FACE_OUTER_BOUND('',#15078,.T.) ;
#11935 = FACE_OUTER_BOUND('',#15079,.T.) ;
#11936 = FACE_OUTER_BOUND('',#15080,.T.) ;
#11937 = FACE_OUTER_BOUND('',#15081,.T.) ;
#11938 = FACE_OUTER_BOUND('',#15082,.T.) ;
#11939 = FACE_OUTER_BOUND('',#15083,.T.) ;
#11940 = FACE_OUTER_BOUND('',#15084,.T.) ;
#11941 = FACE_OUTER_BOUND('',#15085,.T.) ;
#11942 = FACE_OUTER_BOUND('',#15086,.T.) ;
#11943 = FACE_OUTER_BOUND('',#15087,.T.) ;
#11944 = FACE_OUTER_BOUND('',#15088,.T.) ;
#11945 = FACE_OUTER_BOUND('',#15089,.T.) ;
#11946 = FACE_OUTER_BOUND('',#15090,.T.) ;
#11947 = FACE_OUTER_BOUND('',#15091,.T.) ;
#11948 = FACE_OUTER_BOUND('',#15092,.T.) ;
#11949 = FACE_OUTER_BOUND('',#15093,.T.) ;
#11950 = FACE_OUTER_BOUND('',#15094,.T.) ;
#11951 = FACE_OUTER_BOUND('',#15095,.T.) ;
#11952 = FACE_OUTER_BOUND('',#15096,.T.) ;
#11953 = FACE_OUTER_BOUND('',#15097,.T.) ;
#11954 = FACE_OUTER_BOUND('',#15098,.T.) ;
#11955 = FACE_OUTER_BOUND('',#15099,.T.) ;
#11956 = FACE_OUTER_BOUND('',#15100,.T.) ;
#11957 = FACE_OUTER_BOUND('',#15101,.T.) ;
#11958 = FACE_OUTER_BOUND('',#15102,.T.) ;
#11959 = FACE_OUTER_BOUND('',#15103,.T.) ;
#11960 = FACE_OUTER_BOUND('',#15104,.T.) ;
#11961 = FACE_OUTER_BOUND('',#15105,.T.) ;
#11962 = FACE_OUTER_BOUND('',#15106,.T.) ;
#11963 = FACE_OUTER_BOUND('',#15107,.T.) ;
#11964 = FACE_OUTER_BOUND('',#15108,.T.) ;
#11965 = FACE_OUTER_BOUND('',#15109,.T.) ;
#11966 = FACE_OUTER_BOUND('',#15110,.T.) ;
#11967 = FACE_OUTER_BOUND('',#15111,.T.) ;
#11968 = FACE_OUTER_BOUND('',#15112,.T.) ;
#11969 = FACE_OUTER_BOUND('',#15113,.T.) ;
#11970 = FACE_OUTER_BOUND('',#15114,.T.) ;
#11971 = FACE_OUTER_BOUND('',#15115,.T.) ;
#11972 = FACE_OUTER_BOUND('',#15116,.T.) ;
#11973 = FACE_OUTER_BOUND('',#15117,.T.) ;
#11974 = FACE_OUTER_BOUND('',#15118,.T.) ;
#11975 = FACE_OUTER_BOUND('',#15119,.T.) ;
#11976 = FACE_OUTER_BOUND('',#15120,.T.) ;
#11977 = FACE_OUTER_BOUND('',#15121,.T.) ;
#11978 = FACE_OUTER_BOUND('',#15122,.T.) ;
#11979 = FACE_OUTER_BOUND('',#15123,.T.) ;
#11980 = FACE_OUTER_BOUND('',#15124,.T.) ;
#11981 = FACE_OUTER_BOUND('',#15125,.T.) ;
#11982 = FACE_OUTER_BOUND('',#15131,.T.) ;
#11983 = FACE_OUTER_BOUND('',#15132,.T.) ;
#11984 = FACE_OUTER_BOUND('',#15133,.T.) ;
#11985 = FACE_OUTER_BOUND('',#15134,.T.) ;
#11986 = FACE_OUTER_BOUND('',#15137,.T.) ;
#11987 = FACE_OUTER_BOUND('',#15138,.T.) ;
#11988 = FACE_OUTER_BOUND('',#15139,.T.) ;
#11989 = FACE_OUTER_BOUND('',#15140,.T.) ;
#11990 = FACE_OUTER_BOUND('',#15141,.T.) ;
#11991 = FACE_OUTER_BOUND('',#15142,.T.) ;
#11992 = FACE_OUTER_BOUND('',#15143,.T.) ;
#11993 = FACE_OUTER_BOUND('',#15144,.T.) ;
#11994 = FACE_OUTER_BOUND('',#15145,.T.) ;
#11995 = FACE_OUTER_BOUND('',#15146,.T.) ;
#11996 = FACE_OUTER_BOUND('',#15147,.T.) ;
#11997 = FACE_OUTER_BOUND('',#15148,.T.) ;
#11998 = FACE_OUTER_BOUND('',#15149,.T.) ;
#11999 = FACE_OUTER_BOUND('',#15150,.T.) ;
#12000 = FACE_OUTER_BOUND('',#15151,.T.) ;
#12001 = FACE_OUTER_BOUND('',#15152,.T.) ;
#12002 = FACE_OUTER_BOUND('',#15153,.T.) ;
#12003 = FACE_OUTER_BOUND('',#15154,.T.) ;
#12004 = FACE_OUTER_BOUND('',#15155,.T.) ;
#12005 = FACE_OUTER_BOUND('',#15156,.T.) ;
#12006 = FACE_OUTER_BOUND('',#15157,.T.) ;
#12007 = FACE_OUTER_BOUND('',#15158,.T.) ;
#12008 = FACE_OUTER_BOUND('',#15159,.T.) ;
#12009 = FACE_OUTER_BOUND('',#15160,.T.) ;
#12010 = FACE_OUTER_BOUND('',#15161,.T.) ;
#12011 = FACE_OUTER_BOUND('',#15162,.T.) ;
#12012 = FACE_OUTER_BOUND('',#15163,.T.) ;
#12013 = FACE_OUTER_BOUND('',#15164,.T.) ;
#12014 = FACE_OUTER_BOUND('',#15165,.T.) ;
#12015 = FACE_OUTER_BOUND('',#15166,.T.) ;
#12016 = FACE_OUTER_BOUND('',#15167,.T.) ;
#12017 = FACE_OUTER_BOUND('',#15168,.T.) ;
#12018 = FACE_OUTER_BOUND('',#15169,.T.) ;
#12019 = FACE_OUTER_BOUND('',#15170,.T.) ;
#12020 = FACE_OUTER_BOUND('',#15171,.T.) ;
#12021 = FACE_OUTER_BOUND('',#15172,.T.) ;
#12022 = FACE_OUTER_BOUND('',#15173,.T.) ;
#12023 = FACE_OUTER_BOUND('',#15174,.T.) ;
#12024 = FACE_OUTER_BOUND('',#15175,.T.) ;
#12025 = FACE_OUTER_BOUND('',#15176,.T.) ;
#12026 = FACE_OUTER_BOUND('',#15177,.T.) ;
#12027 = FACE_OUTER_BOUND('',#15178,.T.) ;
#12028 = FACE_OUTER_BOUND('',#15179,.T.) ;
#12029 = FACE_OUTER_BOUND('',#15180,.T.) ;
#12030 = FACE_OUTER_BOUND('',#15181,.T.) ;
#12031 = FACE_OUTER_BOUND('',#15182,.T.) ;
#12032 = FACE_OUTER_BOUND('',#15183,.T.) ;
#12033 = FACE_OUTER_BOUND('',#15184,.T.) ;
#12034 = FACE_OUTER_BOUND('',#15185,.T.) ;
#12035 = FACE_OUTER_BOUND('',#15186,.T.) ;
#12036 = FACE_OUTER_BOUND('',#15187,.T.) ;
#12037 = FACE_OUTER_BOUND('',#15188,.T.) ;
#12038 = FACE_OUTER_BOUND('',#15189,.T.) ;
#12039 = FACE_OUTER_BOUND('',#15190,.T.) ;
#12040 = FACE_OUTER_BOUND('',#15191,.T.) ;
#12041 = FACE_OUTER_BOUND('',#15192,.T.) ;
#12042 = FACE_OUTER_BOUND('',#15193,.T.) ;
#12043 = FACE_OUTER_BOUND('',#15194,.T.) ;
#12044 = FACE_OUTER_BOUND('',#15195,.T.) ;
#12045 = FACE_OUTER_BOUND('',#15196,.T.) ;
#12046 = FACE_OUTER_BOUND('',#15197,.T.) ;
#12047 = FACE_OUTER_BOUND('',#15198,.T.) ;
#12048 = FACE_OUTER_BOUND('',#15199,.T.) ;
#12049 = FACE_OUTER_BOUND('',#15200,.T.) ;
#12050 = FACE_OUTER_BOUND('',#15201,.T.) ;
#12051 = FACE_OUTER_BOUND('',#15202,.T.) ;
#12052 = FACE_OUTER_BOUND('',#15203,.T.) ;
#12053 = FACE_OUTER_BOUND('',#15204,.T.) ;
#12054 = FACE_OUTER_BOUND('',#15205,.T.) ;
#12055 = FACE_OUTER_BOUND('',#15206,.T.) ;
#12056 = FACE_OUTER_BOUND('',#15207,.T.) ;
#12057 = FACE_OUTER_BOUND('',#15208,.T.) ;
#12058 = FACE_OUTER_BOUND('',#15209,.T.) ;
#12059 = FACE_OUTER_BOUND('',#15210,.T.) ;
#12060 = FACE_OUTER_BOUND('',#15211,.T.) ;
#12061 = FACE_OUTER_BOUND('',#15212,.T.) ;
#12062 = FACE_OUTER_BOUND('',#15213,.T.) ;
#12063 = FACE_OUTER_BOUND('',#15214,.T.) ;
#12064 = FACE_OUTER_BOUND('',#15215,.T.) ;
#12065 = FACE_OUTER_BOUND('',#15216,.T.) ;
#12066 = FACE_OUTER_BOUND('',#15217,.T.) ;
#12067 = FACE_OUTER_BOUND('',#15218,.T.) ;
#12068 = FACE_OUTER_BOUND('',#15219,.T.) ;
#12069 = FACE_OUTER_BOUND('',#15220,.T.) ;
#12070 = FACE_OUTER_BOUND('',#15221,.T.) ;
#12071 = FACE_OUTER_BOUND('',#15222,.T.) ;
#12072 = FACE_OUTER_BOUND('',#15223,.T.) ;
#12073 = FACE_OUTER_BOUND('',#15224,.T.) ;
#12074 = FACE_OUTER_BOUND('',#15225,.T.) ;
#12075 = FACE_OUTER_BOUND('',#15226,.T.) ;
#12076 = FACE_OUTER_BOUND('',#15227,.T.) ;
#12077 = FACE_OUTER_BOUND('',#15228,.T.) ;
#12078 = FACE_OUTER_BOUND('',#15229,.T.) ;
#12079 = FACE_OUTER_BOUND('',#15230,.T.) ;
#12080 = FACE_OUTER_BOUND('',#15231,.T.) ;
#12081 = FACE_OUTER_BOUND('',#15232,.T.) ;
#12082 = FACE_OUTER_BOUND('',#15233,.T.) ;
#12083 = FACE_OUTER_BOUND('',#15234,.T.) ;
#12084 = FACE_OUTER_BOUND('',#15235,.T.) ;
#12085 = FACE_OUTER_BOUND('',#15236,.T.) ;
#12086 = FACE_OUTER_BOUND('',#15237,.T.) ;
#12087 = FACE_OUTER_BOUND('',#15238,.T.) ;
#12088 = FACE_OUTER_BOUND('',#15239,.T.) ;
#12089 = FACE_OUTER_BOUND('',#15240,.T.) ;
#12090 = FACE_OUTER_BOUND('',#15241,.T.) ;
#12091 = FACE_OUTER_BOUND('',#15242,.T.) ;
#12092 = FACE_OUTER_BOUND('',#15243,.T.) ;
#12093 = FACE_OUTER_BOUND('',#15244,.T.) ;
#12094 = FACE_OUTER_BOUND('',#15245,.T.) ;
#12095 = FACE_OUTER_BOUND('',#15246,.T.) ;
#12096 = FACE_OUTER_BOUND('',#15247,.T.) ;
#12097 = FACE_OUTER_BOUND('',#15248,.T.) ;
#12098 = FACE_OUTER_BOUND('',#15249,.T.) ;
#12099 = FACE_OUTER_BOUND('',#15250,.T.) ;
#12100 = FACE_OUTER_BOUND('',#15251,.T.) ;
#12101 = FACE_OUTER_BOUND('',#15252,.T.) ;
#12102 = FACE_OUTER_BOUND('',#15253,.T.) ;
#12103 = FACE_OUTER_BOUND('',#15254,.T.) ;
#12104 = FACE_OUTER_BOUND('',#15255,.T.) ;
#12105 = FACE_OUTER_BOUND('',#15256,.T.) ;
#12106 = FACE_OUTER_BOUND('',#15257,.T.) ;
#12107 = FACE_OUTER_BOUND('',#15259,.T.) ;
#12108 = FACE_OUTER_BOUND('',#15260,.T.) ;
#12109 = FACE_OUTER_BOUND('',#15261,.T.) ;
#12110 = FACE_OUTER_BOUND('',#15262,.T.) ;
#12111 = FACE_OUTER_BOUND('',#15264,.T.) ;
#12112 = FACE_OUTER_BOUND('',#15265,.T.) ;
#12113 = FACE_OUTER_BOUND('',#15266,.T.) ;
#12114 = FACE_OUTER_BOUND('',#15268,.T.) ;
#12115 = FACE_OUTER_BOUND('',#15269,.T.) ;
#12116 = FACE_OUTER_BOUND('',#15271,.T.) ;
#12117 = FACE_OUTER_BOUND('',#15272,.T.) ;
#12118 = FACE_OUTER_BOUND('',#15273,.T.) ;
#12119 = FACE_OUTER_BOUND('',#15274,.T.) ;
#12120 = FACE_OUTER_BOUND('',#15275,.T.) ;
#12121 = FACE_OUTER_BOUND('',#15276,.T.) ;
#12122 = FACE_OUTER_BOUND('',#15277,.T.) ;
#12123 = FACE_OUTER_BOUND('',#15278,.T.) ;
#12124 = FACE_OUTER_BOUND('',#15279,.T.) ;
#12125 = FACE_OUTER_BOUND('',#15280,.T.) ;
#12126 = FACE_OUTER_BOUND('',#15281,.T.) ;
#12127 = FACE_OUTER_BOUND('',#15282,.T.) ;
#12128 = FACE_OUTER_BOUND('',#15283,.T.) ;
#12129 = FACE_OUTER_BOUND('',#15284,.T.) ;
#12130 = FACE_OUTER_BOUND('',#15285,.T.) ;
#12131 = FACE_OUTER_BOUND('',#15286,.T.) ;
#12132 = FACE_OUTER_BOUND('',#15287,.T.) ;
#12133 = FACE_OUTER_BOUND('',#15288,.T.) ;
#12134 = FACE_OUTER_BOUND('',#15289,.T.) ;
#12135 = FACE_OUTER_BOUND('',#15290,.T.) ;
#12136 = FACE_OUTER_BOUND('',#15291,.T.) ;
#12137 = FACE_OUTER_BOUND('',#15292,.T.) ;
#12138 = FACE_OUTER_BOUND('',#15293,.T.) ;
#12139 = FACE_OUTER_BOUND('',#15294,.T.) ;
#12140 = FACE_OUTER_BOUND('',#15295,.T.) ;
#12141 = FACE_OUTER_BOUND('',#15296,.T.) ;
#12142 = FACE_OUTER_BOUND('',#15297,.T.) ;
#12143 = FACE_OUTER_BOUND('',#15298,.T.) ;
#12144 = FACE_OUTER_BOUND('',#15299,.T.) ;
#12145 = FACE_OUTER_BOUND('',#15300,.T.) ;
#12146 = FACE_OUTER_BOUND('',#15301,.T.) ;
#12147 = FACE_OUTER_BOUND('',#15302,.T.) ;
#12148 = FACE_OUTER_BOUND('',#15303,.T.) ;
#12149 = FACE_OUTER_BOUND('',#15304,.T.) ;
#12150 = FACE_OUTER_BOUND('',#15305,.T.) ;
#12151 = FACE_OUTER_BOUND('',#15306,.T.) ;
#12152 = FACE_OUTER_BOUND('',#15307,.T.) ;
#12153 = FACE_OUTER_BOUND('',#15308,.T.) ;
#12154 = FACE_OUTER_BOUND('',#15309,.T.) ;
#12155 = FACE_OUTER_BOUND('',#15310,.T.) ;
#12156 = FACE_OUTER_BOUND('',#15311,.T.) ;
#12157 = FACE_OUTER_BOUND('',#15312,.T.) ;
#12158 = FACE_OUTER_BOUND('',#15313,.T.) ;
#12159 = FACE_OUTER_BOUND('',#15314,.T.) ;
#12160 = FACE_OUTER_BOUND('',#15315,.T.) ;
#12161 = FACE_OUTER_BOUND('',#15316,.T.) ;
#12162 = FACE_OUTER_BOUND('',#15317,.T.) ;
#12163 = FACE_OUTER_BOUND('',#15318,.T.) ;
#12164 = FACE_OUTER_BOUND('',#15319,.T.) ;
#12165 = FACE_OUTER_BOUND('',#15320,.T.) ;
#12166 = FACE_OUTER_BOUND('',#15321,.T.) ;
#12167 = FACE_OUTER_BOUND('',#15322,.T.) ;
#12168 = FACE_OUTER_BOUND('',#15323,.T.) ;
#12169 = FACE_OUTER_BOUND('',#15324,.T.) ;
#12170 = FACE_OUTER_BOUND('',#15325,.T.) ;
#12171 = FACE_OUTER_BOUND('',#15326,.T.) ;
#12172 = FACE_OUTER_BOUND('',#15327,.T.) ;
#12173 = FACE_OUTER_BOUND('',#15328,.T.) ;
#12174 = FACE_OUTER_BOUND('',#15329,.T.) ;
#12175 = FACE_OUTER_BOUND('',#15330,.T.) ;
#12176 = FACE_OUTER_BOUND('',#15332,.T.) ;
#12177 = FACE_OUTER_BOUND('',#15333,.T.) ;
#12178 = FACE_OUTER_BOUND('',#15334,.T.) ;
#12179 = FACE_OUTER_BOUND('',#15335,.T.) ;
#12180 = FACE_OUTER_BOUND('',#15336,.T.) ;
#12181 = FACE_OUTER_BOUND('',#15337,.T.) ;
#12182 = FACE_OUTER_BOUND('',#15338,.T.) ;
#12183 = FACE_OUTER_BOUND('',#15339,.T.) ;
#12184 = FACE_OUTER_BOUND('',#15340,.T.) ;
#12185 = FACE_OUTER_BOUND('',#15341,.T.) ;
#12186 = FACE_OUTER_BOUND('',#15342,.T.) ;
#12187 = FACE_OUTER_BOUND('',#15343,.T.) ;
#12188 = FACE_OUTER_BOUND('',#15344,.T.) ;
#12189 = FACE_OUTER_BOUND('',#15345,.T.) ;
#12190 = FACE_OUTER_BOUND('',#15346,.T.) ;
#12191 = FACE_OUTER_BOUND('',#15347,.T.) ;
#12192 = FACE_OUTER_BOUND('',#15348,.T.) ;
#12193 = FACE_OUTER_BOUND('',#15349,.T.) ;
#12194 = FACE_OUTER_BOUND('',#15350,.T.) ;
#12195 = FACE_OUTER_BOUND('',#15351,.T.) ;
#12196 = FACE_OUTER_BOUND('',#15352,.T.) ;
#12197 = FACE_OUTER_BOUND('',#15353,.T.) ;
#12198 = FACE_OUTER_BOUND('',#15354,.T.) ;
#12199 = FACE_OUTER_BOUND('',#15355,.T.) ;
#12200 = FACE_OUTER_BOUND('',#15356,.T.) ;
#12201 = FACE_OUTER_BOUND('',#15357,.T.) ;
#12202 = FACE_OUTER_BOUND('',#15358,.T.) ;
#12203 = FACE_OUTER_BOUND('',#15359,.T.) ;
#12204 = FACE_OUTER_BOUND('',#15360,.T.) ;
#12205 = FACE_OUTER_BOUND('',#15361,.T.) ;
#12206 = FACE_OUTER_BOUND('',#15362,.T.) ;
#12207 = FACE_OUTER_BOUND('',#15363,.T.) ;
#12208 = FACE_OUTER_BOUND('',#15364,.T.) ;
#12209 = FACE_OUTER_BOUND('',#15365,.T.) ;
#12210 = FACE_OUTER_BOUND('',#15366,.T.) ;
#12211 = FACE_OUTER_BOUND('',#15367,.T.) ;
#12212 = FACE_OUTER_BOUND('',#15368,.T.) ;
#12213 = FACE_OUTER_BOUND('',#15369,.T.) ;
#12214 = FACE_OUTER_BOUND('',#15370,.T.) ;
#12215 = FACE_OUTER_BOUND('',#15371,.T.) ;
#12216 = FACE_OUTER_BOUND('',#15372,.T.) ;
#12217 = FACE_OUTER_BOUND('',#15373,.T.) ;
#12218 = FACE_OUTER_BOUND('',#15374,.T.) ;
#12219 = FACE_OUTER_BOUND('',#15375,.T.) ;
#12220 = FACE_OUTER_BOUND('',#15376,.T.) ;
#12221 = FACE_OUTER_BOUND('',#15377,.T.) ;
#12222 = FACE_OUTER_BOUND('',#15378,.T.) ;
#12223 = FACE_OUTER_BOUND('',#15379,.T.) ;
#12224 = FACE_OUTER_BOUND('',#15380,.T.) ;
#12225 = FACE_OUTER_BOUND('',#15381,.T.) ;
#12226 = FACE_OUTER_BOUND('',#15382,.T.) ;
#12227 = FACE_OUTER_BOUND('',#15383,.T.) ;
#12228 = FACE_OUTER_BOUND('',#15384,.T.) ;
#12229 = FACE_OUTER_BOUND('',#15385,.T.) ;
#12230 = FACE_OUTER_BOUND('',#15386,.T.) ;
#12231 = FACE_OUTER_BOUND('',#15387,.T.) ;
#12232 = FACE_OUTER_BOUND('',#15388,.T.) ;
#12233 = FACE_OUTER_BOUND('',#15389,.T.) ;
#12234 = FACE_OUTER_BOUND('',#15390,.T.) ;
#12235 = FACE_OUTER_BOUND('',#15391,.T.) ;
#12236 = FACE_OUTER_BOUND('',#15392,.T.) ;
#12237 = FACE_OUTER_BOUND('',#15394,.T.) ;
#12238 = FACE_OUTER_BOUND('',#15395,.T.) ;
#12239 = FACE_OUTER_BOUND('',#15396,.T.) ;
#12240 = FACE_OUTER_BOUND('',#15397,.T.) ;
#12241 = FACE_OUTER_BOUND('',#15398,.T.) ;
#12242 = FACE_OUTER_BOUND('',#15399,.T.) ;
#12243 = FACE_OUTER_BOUND('',#15400,.T.) ;
#12244 = FACE_OUTER_BOUND('',#15401,.T.) ;
#12245 = FACE_OUTER_BOUND('',#15402,.T.) ;
#12246 = FACE_OUTER_BOUND('',#15403,.T.) ;
#12247 = FACE_OUTER_BOUND('',#15404,.T.) ;
#12248 = FACE_OUTER_BOUND('',#15405,.T.) ;
#12249 = FACE_OUTER_BOUND('',#15406,.T.) ;
#12250 = FACE_OUTER_BOUND('',#15407,.T.) ;
#12251 = FACE_OUTER_BOUND('',#15408,.T.) ;
#12252 = FACE_OUTER_BOUND('',#15409,.T.) ;
#12253 = FACE_OUTER_BOUND('',#15410,.T.) ;
#12254 = FACE_OUTER_BOUND('',#15411,.T.) ;
#12255 = FACE_OUTER_BOUND('',#15412,.T.) ;
#12256 = FACE_OUTER_BOUND('',#15413,.T.) ;
#12257 = FACE_OUTER_BOUND('',#15414,.T.) ;
#12258 = FACE_OUTER_BOUND('',#15415,.T.) ;
#12259 = FACE_OUTER_BOUND('',#15416,.T.) ;
#12260 = FACE_OUTER_BOUND('',#15417,.T.) ;
#12261 = FACE_OUTER_BOUND('',#15418,.T.) ;
#12262 = FACE_OUTER_BOUND('',#15419,.T.) ;
#12263 = FACE_OUTER_BOUND('',#15420,.T.) ;
#12264 = FACE_OUTER_BOUND('',#15421,.T.) ;
#12265 = FACE_OUTER_BOUND('',#15422,.T.) ;
#12266 = FACE_OUTER_BOUND('',#15423,.T.) ;
#12267 = FACE_OUTER_BOUND('',#15424,.T.) ;
#12268 = FACE_OUTER_BOUND('',#15425,.T.) ;
#12269 = FACE_OUTER_BOUND('',#15426,.T.) ;
#12270 = FACE_OUTER_BOUND('',#15427,.T.) ;
#12271 = FACE_OUTER_BOUND('',#15428,.T.) ;
#12272 = FACE_OUTER_BOUND('',#15429,.T.) ;
#12273 = FACE_OUTER_BOUND('',#15430,.T.) ;
#12274 = FACE_OUTER_BOUND('',#15431,.T.) ;
#12275 = FACE_OUTER_BOUND('',#15432,.T.) ;
#12276 = FACE_OUTER_BOUND('',#15433,.T.) ;
#12277 = FACE_OUTER_BOUND('',#15434,.T.) ;
#12278 = FACE_OUTER_BOUND('',#15435,.T.) ;
#12279 = FACE_OUTER_BOUND('',#15436,.T.) ;
#12280 = FACE_OUTER_BOUND('',#15437,.T.) ;
#12281 = FACE_OUTER_BOUND('',#15438,.T.) ;
#12282 = FACE_OUTER_BOUND('',#15439,.T.) ;
#12283 = FACE_OUTER_BOUND('',#15440,.T.) ;
#12284 = FACE_OUTER_BOUND('',#15441,.T.) ;
#12285 = FACE_OUTER_BOUND('',#15442,.T.) ;
#12286 = FACE_OUTER_BOUND('',#15443,.T.) ;
#12287 = FACE_OUTER_BOUND('',#15444,.T.) ;
#12288 = FACE_OUTER_BOUND('',#15445,.T.) ;
#12289 = FACE_OUTER_BOUND('',#15446,.T.) ;
#12290 = FACE_OUTER_BOUND('',#15447,.T.) ;
#12291 = FACE_OUTER_BOUND('',#15448,.T.) ;
#12292 = FACE_OUTER_BOUND('',#15449,.T.) ;
#12293 = FACE_OUTER_BOUND('',#15450,.T.) ;
#12294 = FACE_OUTER_BOUND('',#15451,.T.) ;
#12295 = FACE_OUTER_BOUND('',#15453,.T.) ;
#12296 = FACE_OUTER_BOUND('',#15454,.T.) ;
#12297 = FACE_OUTER_BOUND('',#15455,.T.) ;
#12298 = FACE_OUTER_BOUND('',#15456,.T.) ;
#12299 = FACE_OUTER_BOUND('',#15457,.T.) ;
#12300 = FACE_OUTER_BOUND('',#15458,.T.) ;
#12301 = FACE_OUTER_BOUND('',#15459,.T.) ;
#12302 = FACE_OUTER_BOUND('',#15460,.T.) ;
#12303 = FACE_OUTER_BOUND('',#15461,.T.) ;
#12304 = FACE_OUTER_BOUND('',#15462,.T.) ;
#12305 = FACE_OUTER_BOUND('',#15463,.T.) ;
#12306 = FACE_OUTER_BOUND('',#15464,.T.) ;
#12307 = FACE_OUTER_BOUND('',#15465,.T.) ;
#12308 = FACE_OUTER_BOUND('',#15466,.T.) ;
#12309 = FACE_OUTER_BOUND('',#15467,.T.) ;
#12310 = FACE_OUTER_BOUND('',#15468,.T.) ;
#12311 = FACE_OUTER_BOUND('',#15469,.T.) ;
#12312 = FACE_OUTER_BOUND('',#15470,.T.) ;
#12313 = FACE_OUTER_BOUND('',#15471,.T.) ;
#12314 = FACE_OUTER_BOUND('',#15472,.T.) ;
#12315 = FACE_OUTER_BOUND('',#15473,.T.) ;
#12316 = FACE_OUTER_BOUND('',#15474,.T.) ;
#12317 = FACE_OUTER_BOUND('',#15475,.T.) ;
#12318 = FACE_OUTER_BOUND('',#15476,.T.) ;
#12319 = FACE_OUTER_BOUND('',#15477,.T.) ;
#12320 = FACE_OUTER_BOUND('',#15478,.T.) ;
#12321 = FACE_OUTER_BOUND('',#15479,.T.) ;
#12322 = FACE_OUTER_BOUND('',#15480,.T.) ;
#12323 = FACE_OUTER_BOUND('',#15481,.T.) ;
#12324 = FACE_OUTER_BOUND('',#15482,.T.) ;
#12325 = FACE_OUTER_BOUND('',#15483,.T.) ;
#12326 = FACE_OUTER_BOUND('',#15484,.T.) ;
#12327 = FACE_OUTER_BOUND('',#15485,.T.) ;
#12328 = FACE_OUTER_BOUND('',#15486,.T.) ;
#12329 = FACE_OUTER_BOUND('',#15487,.T.) ;
#12330 = FACE_OUTER_BOUND('',#15488,.T.) ;
#12331 = FACE_OUTER_BOUND('',#15489,.T.) ;
#12332 = FACE_OUTER_BOUND('',#15490,.T.) ;
#12333 = FACE_OUTER_BOUND('',#15491,.T.) ;
#12334 = FACE_OUTER_BOUND('',#15492,.T.) ;
#12335 = FACE_OUTER_BOUND('',#15493,.T.) ;
#12336 = FACE_OUTER_BOUND('',#15494,.T.) ;
#12337 = FACE_OUTER_BOUND('',#15496,.T.) ;
#12338 = FACE_OUTER_BOUND('',#15497,.T.) ;
#12339 = FACE_OUTER_BOUND('',#15498,.T.) ;
#12340 = FACE_OUTER_BOUND('',#15499,.T.) ;
#12341 = FACE_OUTER_BOUND('',#15500,.T.) ;
#12342 = FACE_OUTER_BOUND('',#15501,.T.) ;
#12343 = FACE_OUTER_BOUND('',#15502,.T.) ;
#12344 = FACE_OUTER_BOUND('',#15503,.T.) ;
#12345 = FACE_OUTER_BOUND('',#15504,.T.) ;
#12346 = FACE_OUTER_BOUND('',#15505,.T.) ;
#12347 = FACE_OUTER_BOUND('',#15506,.T.) ;
#12348 = FACE_OUTER_BOUND('',#15507,.T.) ;
#12349 = FACE_OUTER_BOUND('',#15508,.T.) ;
#12350 = FACE_OUTER_BOUND('',#15509,.T.) ;
#12351 = FACE_OUTER_BOUND('',#15510,.T.) ;
#12352 = FACE_OUTER_BOUND('',#15511,.T.) ;
#12353 = FACE_OUTER_BOUND('',#15512,.T.) ;
#12354 = FACE_OUTER_BOUND('',#15513,.T.) ;
#12355 = FACE_OUTER_BOUND('',#15514,.T.) ;
#12356 = FACE_OUTER_BOUND('',#15515,.T.) ;
#12357 = FACE_OUTER_BOUND('',#15516,.T.) ;
#12358 = FACE_OUTER_BOUND('',#15517,.T.) ;
#12359 = FACE_OUTER_BOUND('',#15518,.T.) ;
#12360 = FACE_OUTER_BOUND('',#15519,.T.) ;
#12361 = FACE_OUTER_BOUND('',#15520,.T.) ;
#12362 = FACE_OUTER_BOUND('',#15521,.T.) ;
#12363 = FACE_OUTER_BOUND('',#15522,.T.) ;
#12364 = FACE_OUTER_BOUND('',#15523,.T.) ;
#12365 = FACE_OUTER_BOUND('',#15524,.T.) ;
#12366 = FACE_OUTER_BOUND('',#15525,.T.) ;
#12367 = FACE_OUTER_BOUND('',#15526,.T.) ;
#12368 = FACE_OUTER_BOUND('',#15527,.T.) ;
#12369 = FACE_OUTER_BOUND('',#15528,.T.) ;
#12370 = FACE_OUTER_BOUND('',#15529,.T.) ;
#12371 = FACE_OUTER_BOUND('',#15530,.T.) ;
#12372 = FACE_OUTER_BOUND('',#15531,.T.) ;
#12373 = FACE_OUTER_BOUND('',#15532,.T.) ;
#12374 = FACE_OUTER_BOUND('',#15533,.T.) ;
#12375 = FACE_OUTER_BOUND('',#15534,.T.) ;
#12376 = FACE_OUTER_BOUND('',#15535,.T.) ;
#12377 = FACE_OUTER_BOUND('',#15536,.T.) ;
#12378 = FACE_OUTER_BOUND('',#15537,.T.) ;
#12379 = FACE_OUTER_BOUND('',#15538,.T.) ;
#12380 = FACE_OUTER_BOUND('',#15540,.T.) ;
#12381 = FACE_OUTER_BOUND('',#15541,.T.) ;
#12382 = FACE_OUTER_BOUND('',#15542,.T.) ;
#12383 = FACE_OUTER_BOUND('',#15543,.T.) ;
#12384 = FACE_OUTER_BOUND('',#15544,.T.) ;
#12385 = FACE_OUTER_BOUND('',#15545,.T.) ;
#12386 = FACE_OUTER_BOUND('',#15546,.T.) ;
#12387 = FACE_OUTER_BOUND('',#15547,.T.) ;
#12388 = FACE_OUTER_BOUND('',#15548,.T.) ;
#12389 = FACE_OUTER_BOUND('',#15549,.T.) ;
#12390 = FACE_OUTER_BOUND('',#15550,.T.) ;
#12391 = FACE_OUTER_BOUND('',#15551,.T.) ;
#12392 = FACE_OUTER_BOUND('',#15552,.T.) ;
#12393 = FACE_OUTER_BOUND('',#15553,.T.) ;
#12394 = FACE_OUTER_BOUND('',#15554,.T.) ;
#12395 = FACE_OUTER_BOUND('',#15555,.T.) ;
#12396 = FACE_OUTER_BOUND('',#15556,.T.) ;
#12397 = FACE_OUTER_BOUND('',#15557,.T.) ;
#12398 = FACE_OUTER_BOUND('',#15558,.T.) ;
#12399 = FACE_OUTER_BOUND('',#15559,.T.) ;
#12400 = FACE_OUTER_BOUND('',#15560,.T.) ;
#12401 = FACE_OUTER_BOUND('',#15561,.T.) ;
#12402 = FACE_OUTER_BOUND('',#15562,.T.) ;
#12403 = FACE_OUTER_BOUND('',#15563,.T.) ;
#12404 = FACE_OUTER_BOUND('',#15564,.T.) ;
#12405 = FACE_OUTER_BOUND('',#15565,.T.) ;
#12406 = FACE_OUTER_BOUND('',#15566,.T.) ;
#12407 = FACE_OUTER_BOUND('',#15567,.T.) ;
#12408 = FACE_OUTER_BOUND('',#15568,.T.) ;
#12409 = FACE_OUTER_BOUND('',#15569,.T.) ;
#12410 = FACE_OUTER_BOUND('',#15570,.T.) ;
#12411 = FACE_OUTER_BOUND('',#15571,.T.) ;
#12412 = FACE_OUTER_BOUND('',#15572,.T.) ;
#12413 = FACE_OUTER_BOUND('',#15573,.T.) ;
#12414 = FACE_OUTER_BOUND('',#15574,.T.) ;
#12415 = FACE_OUTER_BOUND('',#15576,.T.) ;
#12416 = FACE_OUTER_BOUND('',#15579,.T.) ;
#12417 = FACE_OUTER_BOUND('',#15580,.T.) ;
#12418 = FACE_OUTER_BOUND('',#15581,.T.) ;
#12419 = FACE_OUTER_BOUND('',#15582,.T.) ;
#12420 = FACE_OUTER_BOUND('',#15583,.T.) ;
#12421 = FACE_OUTER_BOUND('',#15584,.T.) ;
#12422 = FACE_OUTER_BOUND('',#15585,.T.) ;
#12423 = FACE_OUTER_BOUND('',#15586,.T.) ;
#12424 = FACE_OUTER_BOUND('',#15587,.T.) ;
#12425 = FACE_OUTER_BOUND('',#15588,.T.) ;
#12426 = FACE_OUTER_BOUND('',#15589,.T.) ;
#12427 = FACE_OUTER_BOUND('',#15590,.T.) ;
#12428 = FACE_OUTER_BOUND('',#15591,.T.) ;
#12429 = FACE_OUTER_BOUND('',#15592,.T.) ;
#12430 = FACE_OUTER_BOUND('',#15593,.T.) ;
#12431 = FACE_OUTER_BOUND('',#15594,.T.) ;
#12432 = FACE_OUTER_BOUND('',#15595,.T.) ;
#12433 = FACE_OUTER_BOUND('',#15596,.T.) ;
#12434 = FACE_OUTER_BOUND('',#15597,.T.) ;
#12435 = FACE_OUTER_BOUND('',#15598,.T.) ;
#12436 = FACE_OUTER_BOUND('',#15599,.T.) ;
#12437 = FACE_OUTER_BOUND('',#15600,.T.) ;
#12438 = FACE_OUTER_BOUND('',#15601,.T.) ;
#12439 = FACE_OUTER_BOUND('',#15602,.T.) ;
#12440 = FACE_OUTER_BOUND('',#15603,.T.) ;
#12441 = FACE_OUTER_BOUND('',#15604,.T.) ;
#12442 = FACE_OUTER_BOUND('',#15605,.T.) ;
#12443 = FACE_OUTER_BOUND('',#15606,.T.) ;
#12444 = FACE_OUTER_BOUND('',#15607,.T.) ;
#12445 = FACE_OUTER_BOUND('',#15608,.T.) ;
#12446 = FACE_OUTER_BOUND('',#15609,.T.) ;
#12447 = FACE_OUTER_BOUND('',#15610,.T.) ;
#12448 = FACE_OUTER_BOUND('',#15611,.T.) ;
#12449 = FACE_OUTER_BOUND('',#15612,.T.) ;
#12450 = FACE_OUTER_BOUND('',#15613,.T.) ;
#12451 = FACE_OUTER_BOUND('',#15614,.T.) ;
#12452 = FACE_OUTER_BOUND('',#15615,.T.) ;
#12453 = FACE_OUTER_BOUND('',#15616,.T.) ;
#12454 = FACE_OUTER_BOUND('',#15617,.T.) ;
#12455 = FACE_OUTER_BOUND('',#15618,.T.) ;
#12456 = FACE_OUTER_BOUND('',#15619,.T.) ;
#12457 = FACE_OUTER_BOUND('',#15620,.T.) ;
#12458 = FACE_OUTER_BOUND('',#15621,.T.) ;
#12459 = FACE_OUTER_BOUND('',#15622,.T.) ;
#12460 = FACE_OUTER_BOUND('',#15623,.T.) ;
#12461 = FACE_OUTER_BOUND('',#15624,.T.) ;
#12462 = FACE_OUTER_BOUND('',#15625,.T.) ;
#12463 = FACE_OUTER_BOUND('',#15626,.T.) ;
#12464 = FACE_OUTER_BOUND('',#15627,.T.) ;
#12465 = FACE_OUTER_BOUND('',#15628,.T.) ;
#12466 = FACE_OUTER_BOUND('',#15629,.T.) ;
#12467 = FACE_OUTER_BOUND('',#15630,.T.) ;
#12468 = FACE_OUTER_BOUND('',#15631,.T.) ;
#12469 = FACE_OUTER_BOUND('',#15632,.T.) ;
#12470 = FACE_OUTER_BOUND('',#15633,.T.) ;
#12471 = FACE_OUTER_BOUND('',#15634,.T.) ;
#12472 = FACE_OUTER_BOUND('',#15635,.T.) ;
#12473 = FACE_OUTER_BOUND('',#15636,.T.) ;
#12474 = FACE_OUTER_BOUND('',#15637,.T.) ;
#12475 = FACE_OUTER_BOUND('',#15638,.T.) ;
#12476 = FACE_OUTER_BOUND('',#15639,.T.) ;
#12477 = FACE_OUTER_BOUND('',#15640,.T.) ;
#12478 = FACE_OUTER_BOUND('',#15641,.T.) ;
#12479 = FACE_OUTER_BOUND('',#15642,.T.) ;
#12480 = FACE_OUTER_BOUND('',#15643,.T.) ;
#12481 = FACE_OUTER_BOUND('',#15644,.T.) ;
#12482 = FACE_OUTER_BOUND('',#15645,.T.) ;
#12483 = FACE_OUTER_BOUND('',#15646,.T.) ;
#12484 = FACE_OUTER_BOUND('',#15647,.T.) ;
#12485 = FACE_OUTER_BOUND('',#15648,.T.) ;
#12486 = FACE_OUTER_BOUND('',#15649,.T.) ;
#12487 = FACE_OUTER_BOUND('',#15650,.T.) ;
#12488 = FACE_OUTER_BOUND('',#15651,.T.) ;
#12489 = FACE_OUTER_BOUND('',#15652,.T.) ;
#12490 = FACE_OUTER_BOUND('',#15653,.T.) ;
#12491 = FACE_OUTER_BOUND('',#15654,.T.) ;
#12492 = FACE_OUTER_BOUND('',#15655,.T.) ;
#12493 = FACE_OUTER_BOUND('',#15656,.T.) ;
#12494 = FACE_OUTER_BOUND('',#15657,.T.) ;
#12495 = FACE_OUTER_BOUND('',#15658,.T.) ;
#12496 = FACE_OUTER_BOUND('',#15659,.T.) ;
#12497 = FACE_OUTER_BOUND('',#15660,.T.) ;
#12498 = FACE_OUTER_BOUND('',#15661,.T.) ;
#12499 = FACE_OUTER_BOUND('',#15662,.T.) ;
#12500 = FACE_OUTER_BOUND('',#15663,.T.) ;
#12501 = FACE_OUTER_BOUND('',#15664,.T.) ;
#12502 = FACE_OUTER_BOUND('',#15665,.T.) ;
#12503 = FACE_OUTER_BOUND('',#15666,.T.) ;
#12504 = FACE_OUTER_BOUND('',#15667,.T.) ;
#12505 = FACE_OUTER_BOUND('',#15668,.T.) ;
#12506 = FACE_OUTER_BOUND('',#15669,.T.) ;
#12507 = FACE_OUTER_BOUND('',#15670,.T.) ;
#12508 = FACE_OUTER_BOUND('',#15671,.T.) ;
#12509 = FACE_OUTER_BOUND('',#15672,.T.) ;
#12510 = FACE_OUTER_BOUND('',#15673,.T.) ;
#12511 = FACE_OUTER_BOUND('',#15674,.T.) ;
#12512 = FACE_OUTER_BOUND('',#15675,.T.) ;
#12513 = FACE_OUTER_BOUND('',#15676,.T.) ;
#12514 = FACE_OUTER_BOUND('',#15677,.T.) ;
#12515 = FACE_OUTER_BOUND('',#15678,.T.) ;
#12516 = FACE_OUTER_BOUND('',#15679,.T.) ;
#12517 = FACE_OUTER_BOUND('',#15680,.T.) ;
#12518 = FACE_OUTER_BOUND('',#15681,.T.) ;
#12519 = FACE_OUTER_BOUND('',#15682,.T.) ;
#12520 = FACE_OUTER_BOUND('',#15683,.T.) ;
#12521 = FACE_OUTER_BOUND('',#15684,.T.) ;
#12522 = FACE_OUTER_BOUND('',#15685,.T.) ;
#12523 = FACE_OUTER_BOUND('',#15686,.T.) ;
#12524 = FACE_OUTER_BOUND('',#15687,.T.) ;
#12525 = FACE_OUTER_BOUND('',#15688,.T.) ;
#12526 = FACE_OUTER_BOUND('',#15689,.T.) ;
#12527 = FACE_OUTER_BOUND('',#15690,.T.) ;
#12528 = FACE_OUTER_BOUND('',#15691,.T.) ;
#12529 = FACE_OUTER_BOUND('',#15692,.T.) ;
#12530 = FACE_OUTER_BOUND('',#15693,.T.) ;
#12531 = FACE_OUTER_BOUND('',#15694,.T.) ;
#12532 = FACE_OUTER_BOUND('',#15695,.T.) ;
#12533 = FACE_OUTER_BOUND('',#15696,.T.) ;
#12534 = FACE_OUTER_BOUND('',#15697,.T.) ;
#12535 = FACE_OUTER_BOUND('',#15698,.T.) ;
#12536 = FACE_OUTER_BOUND('',#15699,.T.) ;
#12537 = FACE_OUTER_BOUND('',#15700,.T.) ;
#12538 = FACE_OUTER_BOUND('',#15701,.T.) ;
#12539 = FACE_OUTER_BOUND('',#15702,.T.) ;
#12540 = FACE_OUTER_BOUND('',#15703,.T.) ;
#12541 = FACE_OUTER_BOUND('',#15704,.T.) ;
#12542 = FACE_OUTER_BOUND('',#15705,.T.) ;
#12543 = FACE_OUTER_BOUND('',#15706,.T.) ;
#12544 = FACE_OUTER_BOUND('',#15707,.T.) ;
#12545 = FACE_OUTER_BOUND('',#15708,.T.) ;
#12546 = FACE_OUTER_BOUND('',#15709,.T.) ;
#12547 = FACE_OUTER_BOUND('',#15710,.T.) ;
#12548 = FACE_OUTER_BOUND('',#15711,.T.) ;
#12549 = FACE_OUTER_BOUND('',#15712,.T.) ;
#12550 = FACE_OUTER_BOUND('',#15713,.T.) ;
#12551 = FACE_OUTER_BOUND('',#15714,.T.) ;
#12552 = FACE_OUTER_BOUND('',#15715,.T.) ;
#12553 = FACE_OUTER_BOUND('',#15716,.T.) ;
#12554 = FACE_OUTER_BOUND('',#15717,.T.) ;
#12555 = FACE_OUTER_BOUND('',#15725,.T.) ;
#12556 = FACE_OUTER_BOUND('',#15726,.T.) ;
#12557 = FACE_OUTER_BOUND('',#15727,.T.) ;
#12558 = FACE_OUTER_BOUND('',#15728,.T.) ;
#12559 = FACE_OUTER_BOUND('',#15729,.T.) ;
#12560 = FACE_OUTER_BOUND('',#15730,.T.) ;
#12561 = FACE_OUTER_BOUND('',#15731,.T.) ;
#12562 = FACE_OUTER_BOUND('',#15732,.T.) ;
#12563 = FACE_OUTER_BOUND('',#15733,.T.) ;
#12564 = FACE_OUTER_BOUND('',#15734,.T.) ;
#12565 = FACE_OUTER_BOUND('',#15735,.T.) ;
#12566 = FACE_OUTER_BOUND('',#15736,.T.) ;
#12567 = FACE_OUTER_BOUND('',#15737,.T.) ;
#12568 = FACE_OUTER_BOUND('',#15738,.T.) ;
#12569 = FACE_OUTER_BOUND('',#15739,.T.) ;
#12570 = FACE_OUTER_BOUND('',#15740,.T.) ;
#12571 = FACE_OUTER_BOUND('',#15741,.T.) ;
#12572 = FACE_OUTER_BOUND('',#15742,.T.) ;
#12573 = FACE_OUTER_BOUND('',#15743,.T.) ;
#12574 = FACE_OUTER_BOUND('',#15744,.T.) ;
#12575 = FACE_OUTER_BOUND('',#15745,.T.) ;
#12576 = FACE_OUTER_BOUND('',#15746,.T.) ;
#12577 = FACE_OUTER_BOUND('',#15747,.T.) ;
#12578 = FACE_OUTER_BOUND('',#15748,.T.) ;
#12579 = FACE_OUTER_BOUND('',#15749,.T.) ;
#12580 = FACE_OUTER_BOUND('',#15750,.T.) ;
#12581 = FACE_OUTER_BOUND('',#15751,.T.) ;
#12582 = FACE_OUTER_BOUND('',#15752,.T.) ;
#12583 = FACE_OUTER_BOUND('',#15753,.T.) ;
#12584 = FACE_OUTER_BOUND('',#15754,.T.) ;
#12585 = FACE_OUTER_BOUND('',#15755,.T.) ;
#12586 = FACE_OUTER_BOUND('',#15756,.T.) ;
#12587 = FACE_OUTER_BOUND('',#15757,.T.) ;
#12588 = FACE_OUTER_BOUND('',#15758,.T.) ;
#12589 = FACE_OUTER_BOUND('',#15759,.T.) ;
#12590 = FACE_OUTER_BOUND('',#15760,.T.) ;
#12591 = FACE_OUTER_BOUND('',#15761,.T.) ;
#12592 = FACE_OUTER_BOUND('',#15762,.T.) ;
#12593 = FACE_OUTER_BOUND('',#15763,.T.) ;
#12594 = FACE_OUTER_BOUND('',#15764,.T.) ;
#12595 = FACE_OUTER_BOUND('',#15765,.T.) ;
#12596 = FACE_OUTER_BOUND('',#15766,.T.) ;
#12597 = FACE_OUTER_BOUND('',#15767,.T.) ;
#12598 = FACE_OUTER_BOUND('',#15768,.T.) ;
#12599 = FACE_OUTER_BOUND('',#15769,.T.) ;
#12600 = FACE_OUTER_BOUND('',#15770,.T.) ;
#12601 = FACE_OUTER_BOUND('',#15771,.T.) ;
#12602 = FACE_OUTER_BOUND('',#15772,.T.) ;
#12603 = FACE_OUTER_BOUND('',#15773,.T.) ;
#12604 = FACE_OUTER_BOUND('',#15774,.T.) ;
#12605 = FACE_OUTER_BOUND('',#15775,.T.) ;
#12606 = FACE_OUTER_BOUND('',#15776,.T.) ;
#12607 = FACE_OUTER_BOUND('',#15777,.T.) ;
#12608 = FACE_OUTER_BOUND('',#15778,.T.) ;
#12609 = FACE_OUTER_BOUND('',#15779,.T.) ;
#12610 = FACE_OUTER_BOUND('',#15780,.T.) ;
#12611 = FACE_OUTER_BOUND('',#15781,.T.) ;
#12612 = FACE_OUTER_BOUND('',#15782,.T.) ;
#12613 = FACE_OUTER_BOUND('',#15783,.T.) ;
#12614 = FACE_OUTER_BOUND('',#15784,.T.) ;
#12615 = FACE_OUTER_BOUND('',#15785,.T.) ;
#12616 = FACE_OUTER_BOUND('',#15786,.T.) ;
#12617 = FACE_OUTER_BOUND('',#15787,.T.) ;
#12618 = FACE_OUTER_BOUND('',#15788,.T.) ;
#12619 = FACE_OUTER_BOUND('',#15789,.T.) ;
#12620 = FACE_OUTER_BOUND('',#15790,.T.) ;
#12621 = FACE_OUTER_BOUND('',#15791,.T.) ;
#12622 = FACE_OUTER_BOUND('',#15792,.T.) ;
#12623 = FACE_OUTER_BOUND('',#15793,.T.) ;
#12624 = FACE_OUTER_BOUND('',#15794,.T.) ;
#12625 = FACE_OUTER_BOUND('',#15795,.T.) ;
#12626 = FACE_OUTER_BOUND('',#15796,.T.) ;
#12627 = FACE_OUTER_BOUND('',#15797,.T.) ;
#12628 = FACE_OUTER_BOUND('',#15798,.T.) ;
#12629 = FACE_OUTER_BOUND('',#15799,.T.) ;
#12630 = FACE_OUTER_BOUND('',#15800,.T.) ;
#12631 = FACE_OUTER_BOUND('',#15801,.T.) ;
#12632 = FACE_OUTER_BOUND('',#15802,.T.) ;
#12633 = FACE_OUTER_BOUND('',#15803,.T.) ;
#12634 = FACE_OUTER_BOUND('',#15804,.T.) ;
#12635 = FACE_OUTER_BOUND('',#15805,.T.) ;
#12636 = FACE_OUTER_BOUND('',#15806,.T.) ;
#12637 = FACE_OUTER_BOUND('',#15807,.T.) ;
#12638 = FACE_OUTER_BOUND('',#15808,.T.) ;
#12639 = FACE_OUTER_BOUND('',#15809,.T.) ;
#12640 = FACE_OUTER_BOUND('',#15810,.T.) ;
#12641 = FACE_OUTER_BOUND('',#15811,.T.) ;
#12642 = FACE_OUTER_BOUND('',#15812,.T.) ;
#12643 = FACE_OUTER_BOUND('',#15813,.T.) ;
#12644 = FACE_OUTER_BOUND('',#15814,.T.) ;
#12645 = FACE_OUTER_BOUND('',#15815,.T.) ;
#12646 = FACE_OUTER_BOUND('',#15816,.T.) ;
#12647 = FACE_OUTER_BOUND('',#15817,.T.) ;
#12648 = FACE_OUTER_BOUND('',#15818,.T.) ;
#12649 = FACE_OUTER_BOUND('',#15819,.T.) ;
#12650 = FACE_OUTER_BOUND('',#15820,.T.) ;
#12651 = FACE_OUTER_BOUND('',#15821,.T.) ;
#12652 = FACE_OUTER_BOUND('',#15822,.T.) ;
#12653 = FACE_OUTER_BOUND('',#15823,.T.) ;
#12654 = FACE_OUTER_BOUND('',#15824,.T.) ;
#12655 = FACE_OUTER_BOUND('',#15825,.T.) ;
#12656 = FACE_OUTER_BOUND('',#15826,.T.) ;
#12657 = FACE_OUTER_BOUND('',#15827,.T.) ;
#12658 = FACE_OUTER_BOUND('',#15828,.T.) ;
#12659 = FACE_OUTER_BOUND('',#15829,.T.) ;
#12660 = FACE_OUTER_BOUND('',#15830,.T.) ;
#12661 = FACE_OUTER_BOUND('',#15831,.T.) ;
#12662 = FACE_OUTER_BOUND('',#15832,.T.) ;
#12663 = FACE_OUTER_BOUND('',#15833,.T.) ;
#12664 = FACE_OUTER_BOUND('',#15834,.T.) ;
#12665 = FACE_OUTER_BOUND('',#15835,.T.) ;
#12666 = FACE_OUTER_BOUND('',#15836,.T.) ;
#12667 = FACE_OUTER_BOUND('',#15837,.T.) ;
#12668 = FACE_OUTER_BOUND('',#15838,.T.) ;
#12669 = FACE_OUTER_BOUND('',#15839,.T.) ;
#12670 = FACE_OUTER_BOUND('',#15840,.T.) ;
#12671 = FACE_OUTER_BOUND('',#15841,.T.) ;
#12672 = FACE_OUTER_BOUND('',#15842,.T.) ;
#12673 = FACE_OUTER_BOUND('',#15843,.T.) ;
#12674 = FACE_OUTER_BOUND('',#15844,.T.) ;
#12675 = FACE_OUTER_BOUND('',#15845,.T.) ;
#12676 = FACE_OUTER_BOUND('',#15846,.T.) ;
#12677 = FACE_OUTER_BOUND('',#15847,.T.) ;
#12678 = FACE_OUTER_BOUND('',#15848,.T.) ;
#12679 = FACE_OUTER_BOUND('',#15849,.T.) ;
#12680 = FACE_OUTER_BOUND('',#15850,.T.) ;
#12681 = FACE_OUTER_BOUND('',#15851,.T.) ;
#12682 = FACE_OUTER_BOUND('',#15852,.T.) ;
#12683 = FACE_OUTER_BOUND('',#15853,.T.) ;
#12684 = FACE_OUTER_BOUND('',#15854,.T.) ;
#12685 = FACE_OUTER_BOUND('',#15855,.T.) ;
#12686 = FACE_OUTER_BOUND('',#15856,.T.) ;
#12687 = FACE_OUTER_BOUND('',#15857,.T.) ;
#12688 = FACE_OUTER_BOUND('',#15858,.T.) ;
#12689 = FACE_OUTER_BOUND('',#15859,.T.) ;
#12690 = FACE_OUTER_BOUND('',#15860,.T.) ;
#12691 = FACE_OUTER_BOUND('',#15861,.T.) ;
#12692 = FACE_OUTER_BOUND('',#15862,.T.) ;
#12693 = FACE_OUTER_BOUND('',#15863,.T.) ;
#12694 = FACE_OUTER_BOUND('',#15864,.T.) ;
#12695 = FACE_OUTER_BOUND('',#15865,.T.) ;
#12696 = FACE_OUTER_BOUND('',#15866,.T.) ;
#12697 = FACE_OUTER_BOUND('',#15867,.T.) ;
#12698 = FACE_OUTER_BOUND('',#15868,.T.) ;
#12699 = FACE_OUTER_BOUND('',#15869,.T.) ;
#12700 = FACE_OUTER_BOUND('',#15870,.T.) ;
#12701 = FACE_OUTER_BOUND('',#15871,.T.) ;
#12702 = FACE_OUTER_BOUND('',#15872,.T.) ;
#12703 = FACE_OUTER_BOUND('',#15873,.T.) ;
#12704 = FACE_OUTER_BOUND('',#15874,.T.) ;
#12705 = FACE_OUTER_BOUND('',#15875,.T.) ;
#12706 = FACE_OUTER_BOUND('',#15876,.T.) ;
#12707 = FACE_OUTER_BOUND('',#15877,.T.) ;
#12708 = FACE_OUTER_BOUND('',#15878,.T.) ;
#12709 = FACE_OUTER_BOUND('',#15879,.T.) ;
#12710 = FACE_OUTER_BOUND('',#15880,.T.) ;
#12711 = FACE_OUTER_BOUND('',#15881,.T.) ;
#12712 = FACE_OUTER_BOUND('',#15882,.T.) ;
#12713 = FACE_OUTER_BOUND('',#15883,.T.) ;
#12714 = FACE_OUTER_BOUND('',#15884,.T.) ;
#12715 = FACE_OUTER_BOUND('',#15885,.T.) ;
#12716 = FACE_OUTER_BOUND('',#15888,.T.) ;
#12717 = FACE_OUTER_BOUND('',#15889,.T.) ;
#12718 = FACE_OUTER_BOUND('',#15890,.T.) ;
#12719 = FACE_OUTER_BOUND('',#15892,.T.) ;
#12720 = FACE_OUTER_BOUND('',#15893,.T.) ;
#12721 = FACE_OUTER_BOUND('',#15894,.T.) ;
#12722 = FACE_OUTER_BOUND('',#15895,.T.) ;
#12723 = FACE_OUTER_BOUND('',#15896,.T.) ;
#12724 = FACE_OUTER_BOUND('',#15897,.T.) ;
#12725 = FACE_OUTER_BOUND('',#15898,.T.) ;
#12726 = FACE_OUTER_BOUND('',#15899,.T.) ;
#12727 = FACE_OUTER_BOUND('',#15900,.T.) ;
#12728 = FACE_OUTER_BOUND('',#15901,.T.) ;
#12729 = FACE_OUTER_BOUND('',#15902,.T.) ;
#12730 = FACE_OUTER_BOUND('',#15903,.T.) ;
#12731 = FACE_OUTER_BOUND('',#15904,.T.) ;
#12732 = FACE_OUTER_BOUND('',#15905,.T.) ;
#12733 = FACE_OUTER_BOUND('',#15906,.T.) ;
#12734 = FACE_OUTER_BOUND('',#15907,.T.) ;
#12735 = FACE_OUTER_BOUND('',#15908,.T.) ;
#12736 = FACE_OUTER_BOUND('',#15909,.T.) ;
#12737 = FACE_OUTER_BOUND('',#15910,.T.) ;
#12738 = FACE_OUTER_BOUND('',#15911,.T.) ;
#12739 = FACE_OUTER_BOUND('',#15912,.T.) ;
#12740 = FACE_OUTER_BOUND('',#15913,.T.) ;
#12741 = FACE_OUTER_BOUND('',#15914,.T.) ;
#12742 = FACE_OUTER_BOUND('',#15915,.T.) ;
#12743 = FACE_OUTER_BOUND('',#15916,.T.) ;
#12744 = FACE_OUTER_BOUND('',#15917,.T.) ;
#12745 = FACE_OUTER_BOUND('',#15918,.T.) ;
#12746 = FACE_OUTER_BOUND('',#15919,.T.) ;
#12747 = FACE_OUTER_BOUND('',#15920,.T.) ;
#12748 = FACE_OUTER_BOUND('',#15921,.T.) ;
#12749 = FACE_OUTER_BOUND('',#15922,.T.) ;
#12750 = FACE_OUTER_BOUND('',#15923,.T.) ;
#12751 = FACE_OUTER_BOUND('',#15924,.T.) ;
#12752 = FACE_OUTER_BOUND('',#15925,.T.) ;
#12753 = FACE_OUTER_BOUND('',#15926,.T.) ;
#12754 = FACE_OUTER_BOUND('',#15927,.T.) ;
#12755 = FACE_OUTER_BOUND('',#15928,.T.) ;
#12756 = FACE_OUTER_BOUND('',#15929,.T.) ;
#12757 = FACE_OUTER_BOUND('',#15933,.T.) ;
#12758 = FACE_OUTER_BOUND('',#15934,.T.) ;
#12759 = FACE_OUTER_BOUND('',#15935,.T.) ;
#12760 = FACE_OUTER_BOUND('',#15936,.T.) ;
#12761 = FACE_OUTER_BOUND('',#15937,.T.) ;
#12762 = FACE_OUTER_BOUND('',#15938,.T.) ;
#12763 = FACE_OUTER_BOUND('',#15939,.T.) ;
#12764 = FACE_OUTER_BOUND('',#15940,.T.) ;
#12765 = FACE_OUTER_BOUND('',#15941,.T.) ;
#12766 = FACE_OUTER_BOUND('',#15942,.T.) ;
#12767 = FACE_OUTER_BOUND('',#15943,.T.) ;
#12768 = FACE_OUTER_BOUND('',#15944,.T.) ;
#12769 = FACE_OUTER_BOUND('',#15945,.T.) ;
#12770 = FACE_OUTER_BOUND('',#15946,.T.) ;
#12771 = FACE_OUTER_BOUND('',#15947,.T.) ;
#12772 = FACE_OUTER_BOUND('',#15948,.T.) ;
#12773 = FACE_OUTER_BOUND('',#15949,.T.) ;
#12774 = FACE_OUTER_BOUND('',#15950,.T.) ;
#12775 = FACE_OUTER_BOUND('',#15951,.T.) ;
#12776 = FACE_OUTER_BOUND('',#15952,.T.) ;
#12777 = FACE_OUTER_BOUND('',#15953,.T.) ;
#12778 = FACE_OUTER_BOUND('',#15954,.T.) ;
#12779 = FACE_OUTER_BOUND('',#15955,.T.) ;
#12780 = FACE_OUTER_BOUND('',#15956,.T.) ;
#12781 = FACE_OUTER_BOUND('',#15957,.T.) ;
#12782 = FACE_OUTER_BOUND('',#15958,.T.) ;
#12783 = FACE_OUTER_BOUND('',#15959,.T.) ;
#12784 = FACE_OUTER_BOUND('',#15960,.T.) ;
#12785 = FACE_OUTER_BOUND('',#15961,.T.) ;
#12786 = FACE_OUTER_BOUND('',#15962,.T.) ;
#12787 = FACE_OUTER_BOUND('',#15964,.T.) ;
#12788 = FACE_OUTER_BOUND('',#15965,.T.) ;
#12789 = FACE_OUTER_BOUND('',#15966,.T.) ;
#12790 = FACE_OUTER_BOUND('',#15967,.T.) ;
#12791 = FACE_OUTER_BOUND('',#15968,.T.) ;
#12792 = FACE_OUTER_BOUND('',#15969,.T.) ;
#12793 = FACE_OUTER_BOUND('',#15970,.T.) ;
#12794 = FACE_OUTER_BOUND('',#15971,.T.) ;
#12795 = FACE_OUTER_BOUND('',#15972,.T.) ;
#12796 = FACE_OUTER_BOUND('',#15974,.T.) ;
#12797 = FACE_OUTER_BOUND('',#15975,.T.) ;
#12798 = FACE_OUTER_BOUND('',#15977,.T.) ;
#12799 = FACE_OUTER_BOUND('',#15978,.T.) ;
#12800 = FACE_OUTER_BOUND('',#15979,.T.) ;
#12801 = FACE_OUTER_BOUND('',#15980,.T.) ;
#12802 = FACE_OUTER_BOUND('',#15981,.T.) ;
#12803 = FACE_OUTER_BOUND('',#15982,.T.) ;
#12804 = FACE_OUTER_BOUND('',#15983,.T.) ;
#12805 = FACE_OUTER_BOUND('',#15984,.T.) ;
#12806 = FACE_OUTER_BOUND('',#15985,.T.) ;
#12807 = FACE_OUTER_BOUND('',#15986,.T.) ;
#12808 = FACE_OUTER_BOUND('',#15987,.T.) ;
#12809 = FACE_OUTER_BOUND('',#15988,.T.) ;
#12810 = FACE_OUTER_BOUND('',#15989,.T.) ;
#12811 = FACE_OUTER_BOUND('',#15990,.T.) ;
#12812 = FACE_OUTER_BOUND('',#15991,.T.) ;
#12813 = FACE_OUTER_BOUND('',#15992,.T.) ;
#12814 = FACE_OUTER_BOUND('',#15993,.T.) ;
#12815 = FACE_OUTER_BOUND('',#15994,.T.) ;
#12816 = FACE_OUTER_BOUND('',#15995,.T.) ;
#12817 = FACE_OUTER_BOUND('',#15996,.T.) ;
#12818 = FACE_OUTER_BOUND('',#15997,.T.) ;
#12819 = FACE_OUTER_BOUND('',#15998,.T.) ;
#12820 = FACE_OUTER_BOUND('',#15999,.T.) ;
#12821 = FACE_OUTER_BOUND('',#16000,.T.) ;
#12822 = FACE_OUTER_BOUND('',#16001,.T.) ;
#12823 = FACE_OUTER_BOUND('',#16002,.T.) ;
#12824 = FACE_OUTER_BOUND('',#16003,.T.) ;
#12825 = FACE_OUTER_BOUND('',#16004,.T.) ;
#12826 = FACE_OUTER_BOUND('',#16005,.T.) ;
#12827 = FACE_OUTER_BOUND('',#16006,.T.) ;
#12828 = FACE_OUTER_BOUND('',#16007,.T.) ;
#12829 = FACE_OUTER_BOUND('',#16008,.T.) ;
#12830 = FACE_OUTER_BOUND('',#16009,.T.) ;
#12831 = FACE_OUTER_BOUND('',#16010,.T.) ;
#12832 = FACE_OUTER_BOUND('',#16011,.T.) ;
#12833 = FACE_OUTER_BOUND('',#16012,.T.) ;
#12834 = FACE_OUTER_BOUND('',#16013,.T.) ;
#12835 = FACE_OUTER_BOUND('',#16014,.T.) ;
#12836 = FACE_OUTER_BOUND('',#16015,.T.) ;
#12837 = FACE_OUTER_BOUND('',#16016,.T.) ;
#12838 = FACE_OUTER_BOUND('',#16017,.T.) ;
#12839 = FACE_OUTER_BOUND('',#16018,.T.) ;
#12840 = FACE_OUTER_BOUND('',#16019,.T.) ;
#12841 = FACE_OUTER_BOUND('',#16020,.T.) ;
#12842 = FACE_OUTER_BOUND('',#16021,.T.) ;
#12843 = FACE_OUTER_BOUND('',#16022,.T.) ;
#12844 = FACE_OUTER_BOUND('',#16023,.T.) ;
#12845 = FACE_OUTER_BOUND('',#16024,.T.) ;
#12846 = FACE_OUTER_BOUND('',#16025,.T.) ;
#12847 = FACE_OUTER_BOUND('',#16026,.T.) ;
#12848 = FACE_OUTER_BOUND('',#16027,.T.) ;
#12849 = FACE_OUTER_BOUND('',#16028,.T.) ;
#12850 = FACE_OUTER_BOUND('',#16029,.T.) ;
#12851 = FACE_OUTER_BOUND('',#16030,.T.) ;
#12852 = FACE_OUTER_BOUND('',#16031,.T.) ;
#12853 = FACE_OUTER_BOUND('',#16032,.T.) ;
#12854 = FACE_OUTER_BOUND('',#16033,.T.) ;
#12855 = FACE_OUTER_BOUND('',#16034,.T.) ;
#12856 = FACE_OUTER_BOUND('',#16035,.T.) ;
#12857 = FACE_OUTER_BOUND('',#16036,.T.) ;
#12858 = FACE_OUTER_BOUND('',#16037,.T.) ;
#12859 = FACE_OUTER_BOUND('',#16038,.T.) ;
#12860 = FACE_OUTER_BOUND('',#16039,.T.) ;
#12861 = FACE_OUTER_BOUND('',#16040,.T.) ;
#12862 = FACE_OUTER_BOUND('',#16041,.T.) ;
#12863 = FACE_OUTER_BOUND('',#16042,.T.) ;
#12864 = FACE_OUTER_BOUND('',#16043,.T.) ;
#12865 = FACE_OUTER_BOUND('',#16044,.T.) ;
#12866 = FACE_OUTER_BOUND('',#16045,.T.) ;
#12867 = FACE_OUTER_BOUND('',#16046,.T.) ;
#12868 = FACE_OUTER_BOUND('',#16047,.T.) ;
#12869 = FACE_OUTER_BOUND('',#16048,.T.) ;
#12870 = FACE_OUTER_BOUND('',#16049,.T.) ;
#12871 = FACE_OUTER_BOUND('',#16050,.T.) ;
#12872 = FACE_OUTER_BOUND('',#16051,.T.) ;
#12873 = FACE_OUTER_BOUND('',#16052,.T.) ;
#12874 = FACE_OUTER_BOUND('',#16053,.T.) ;
#12875 = FACE_OUTER_BOUND('',#16054,.T.) ;
#12876 = FACE_OUTER_BOUND('',#16055,.T.) ;
#12877 = FACE_OUTER_BOUND('',#16056,.T.) ;
#12878 = FACE_OUTER_BOUND('',#16057,.T.) ;
#12879 = FACE_OUTER_BOUND('',#16058,.T.) ;
#12880 = FACE_OUTER_BOUND('',#16059,.T.) ;
#12881 = FACE_OUTER_BOUND('',#16060,.T.) ;
#12882 = FACE_OUTER_BOUND('',#16061,.T.) ;
#12883 = FACE_OUTER_BOUND('',#16062,.T.) ;
#12884 = FACE_OUTER_BOUND('',#16063,.T.) ;
#12885 = FACE_OUTER_BOUND('',#16064,.T.) ;
#12886 = FACE_OUTER_BOUND('',#16065,.T.) ;
#12887 = FACE_OUTER_BOUND('',#16066,.T.) ;
#12888 = FACE_OUTER_BOUND('',#16067,.T.) ;
#12889 = FACE_OUTER_BOUND('',#16068,.T.) ;
#12890 = FACE_OUTER_BOUND('',#16069,.T.) ;
#12891 = FACE_OUTER_BOUND('',#16070,.T.) ;
#12892 = FACE_OUTER_BOUND('',#16071,.T.) ;
#12893 = FACE_OUTER_BOUND('',#16072,.T.) ;
#12894 = FACE_OUTER_BOUND('',#16073,.T.) ;
#12895 = FACE_OUTER_BOUND('',#16074,.T.) ;
#12896 = FACE_OUTER_BOUND('',#16075,.T.) ;
#12897 = FACE_OUTER_BOUND('',#16076,.T.) ;
#12898 = FACE_OUTER_BOUND('',#16077,.T.) ;
#12899 = FACE_OUTER_BOUND('',#16078,.T.) ;
#12900 = FACE_OUTER_BOUND('',#16079,.T.) ;
#12901 = FACE_OUTER_BOUND('',#16080,.T.) ;
#12902 = FACE_OUTER_BOUND('',#16081,.T.) ;
#12903 = FACE_OUTER_BOUND('',#16082,.T.) ;
#12904 = FACE_OUTER_BOUND('',#16083,.T.) ;
#12905 = FACE_OUTER_BOUND('',#16084,.T.) ;
#12906 = FACE_OUTER_BOUND('',#16085,.T.) ;
#12907 = FACE_OUTER_BOUND('',#16086,.T.) ;
#12908 = FACE_OUTER_BOUND('',#16087,.T.) ;
#12909 = FACE_OUTER_BOUND('',#16088,.T.) ;
#12910 = FACE_OUTER_BOUND('',#16089,.T.) ;
#12911 = FACE_OUTER_BOUND('',#16090,.T.) ;
#12912 = FACE_OUTER_BOUND('',#16091,.T.) ;
#12913 = FACE_OUTER_BOUND('',#16092,.T.) ;
#12914 = FACE_OUTER_BOUND('',#16093,.T.) ;
#12915 = FACE_OUTER_BOUND('',#16094,.T.) ;
#12916 = FACE_OUTER_BOUND('',#16095,.T.) ;
#12917 = FACE_OUTER_BOUND('',#16096,.T.) ;
#12918 = FACE_OUTER_BOUND('',#16097,.T.) ;
#12919 = FACE_OUTER_BOUND('',#16098,.T.) ;
#12920 = FACE_OUTER_BOUND('',#16099,.T.) ;
#12921 = FACE_OUTER_BOUND('',#16100,.T.) ;
#12922 = FACE_OUTER_BOUND('',#16101,.T.) ;
#12923 = FACE_OUTER_BOUND('',#16102,.T.) ;
#12924 = FACE_OUTER_BOUND('',#16103,.T.) ;
#12925 = FACE_OUTER_BOUND('',#16104,.T.) ;
#12926 = FACE_OUTER_BOUND('',#16105,.T.) ;
#12927 = FACE_OUTER_BOUND('',#16109,.T.) ;
#12928 = FACE_OUTER_BOUND('',#16110,.T.) ;
#12929 = FACE_OUTER_BOUND('',#16111,.T.) ;
#12930 = FACE_OUTER_BOUND('',#16112,.T.) ;
#12931 = FACE_OUTER_BOUND('',#16113,.T.) ;
#12932 = FACE_OUTER_BOUND('',#16114,.T.) ;
#12933 = FACE_OUTER_BOUND('',#16115,.T.) ;
#12934 = FACE_OUTER_BOUND('',#16116,.T.) ;
#12935 = FACE_OUTER_BOUND('',#16117,.T.) ;
#12936 = FACE_OUTER_BOUND('',#16118,.T.) ;
#12937 = FACE_OUTER_BOUND('',#16119,.T.) ;
#12938 = FACE_OUTER_BOUND('',#16120,.T.) ;
#12939 = FACE_OUTER_BOUND('',#16121,.T.) ;
#12940 = FACE_OUTER_BOUND('',#16122,.T.) ;
#12941 = FACE_OUTER_BOUND('',#16123,.T.) ;
#12942 = FACE_OUTER_BOUND('',#16124,.T.) ;
#12943 = FACE_OUTER_BOUND('',#16125,.T.) ;
#12944 = FACE_OUTER_BOUND('',#16126,.T.) ;
#12945 = FACE_OUTER_BOUND('',#16127,.T.) ;
#12946 = FACE_OUTER_BOUND('',#16128,.T.) ;
#12947 = FACE_OUTER_BOUND('',#16129,.T.) ;
#12948 = FACE_OUTER_BOUND('',#16130,.T.) ;
#12949 = FACE_OUTER_BOUND('',#16131,.T.) ;
#12950 = FACE_OUTER_BOUND('',#16132,.T.) ;
#12951 = FACE_OUTER_BOUND('',#16133,.T.) ;
#12952 = FACE_OUTER_BOUND('',#16134,.T.) ;
#12953 = FACE_OUTER_BOUND('',#16135,.T.) ;
#12954 = FACE_OUTER_BOUND('',#16136,.T.) ;
#12955 = FACE_OUTER_BOUND('',#16137,.T.) ;
#12956 = FACE_OUTER_BOUND('',#16138,.T.) ;
#12957 = FACE_OUTER_BOUND('',#16139,.T.) ;
#12958 = FACE_OUTER_BOUND('',#16140,.T.) ;
#12959 = FACE_OUTER_BOUND('',#16141,.T.) ;
#12960 = FACE_OUTER_BOUND('',#16142,.T.) ;
#12961 = FACE_OUTER_BOUND('',#16143,.T.) ;
#12962 = FACE_OUTER_BOUND('',#16144,.T.) ;
#12963 = FACE_OUTER_BOUND('',#16145,.T.) ;
#12964 = FACE_OUTER_BOUND('',#16146,.T.) ;
#12965 = FACE_OUTER_BOUND('',#16147,.T.) ;
#12966 = FACE_OUTER_BOUND('',#16148,.T.) ;
#12967 = FACE_OUTER_BOUND('',#16149,.T.) ;
#12968 = FACE_OUTER_BOUND('',#16150,.T.) ;
#12969 = FACE_OUTER_BOUND('',#16151,.T.) ;
#12970 = FACE_OUTER_BOUND('',#16152,.T.) ;
#12971 = FACE_OUTER_BOUND('',#16153,.T.) ;
#12972 = FACE_OUTER_BOUND('',#16154,.T.) ;
#12973 = FACE_OUTER_BOUND('',#16155,.T.) ;
#12974 = FACE_OUTER_BOUND('',#16156,.T.) ;
#12975 = FACE_OUTER_BOUND('',#16157,.T.) ;
#12976 = FACE_OUTER_BOUND('',#16158,.T.) ;
#12977 = FACE_OUTER_BOUND('',#16159,.T.) ;
#12978 = FACE_OUTER_BOUND('',#16160,.T.) ;
#12979 = FACE_OUTER_BOUND('',#16161,.T.) ;
#12980 = FACE_OUTER_BOUND('',#16162,.T.) ;
#12981 = FACE_OUTER_BOUND('',#16163,.T.) ;
#12982 = FACE_OUTER_BOUND('',#16164,.T.) ;
#12983 = FACE_OUTER_BOUND('',#16165,.T.) ;
#12984 = FACE_OUTER_BOUND('',#16166,.T.) ;
#12985 = FACE_OUTER_BOUND('',#16167,.T.) ;
#12986 = FACE_OUTER_BOUND('',#16168,.T.) ;
#12987 = FACE_OUTER_BOUND('',#16169,.T.) ;
#12988 = FACE_OUTER_BOUND('',#16170,.T.) ;
#12989 = FACE_OUTER_BOUND('',#16171,.T.) ;
#12990 = FACE_OUTER_BOUND('',#16172,.T.) ;
#12991 = FACE_OUTER_BOUND('',#16173,.T.) ;
#12992 = FACE_OUTER_BOUND('',#16174,.T.) ;
#12993 = FACE_OUTER_BOUND('',#16175,.T.) ;
#12994 = FACE_OUTER_BOUND('',#16176,.T.) ;
#12995 = FACE_OUTER_BOUND('',#16177,.T.) ;
#12996 = FACE_OUTER_BOUND('',#16178,.T.) ;
#12997 = FACE_OUTER_BOUND('',#16179,.T.) ;
#12998 = FACE_OUTER_BOUND('',#16180,.T.) ;
#12999 = FACE_OUTER_BOUND('',#16181,.T.) ;
#13000 = FACE_OUTER_BOUND('',#16182,.T.) ;
#13001 = FACE_OUTER_BOUND('',#16183,.T.) ;
#13002 = FACE_OUTER_BOUND('',#16184,.T.) ;
#13003 = FACE_OUTER_BOUND('',#16185,.T.) ;
#13004 = FACE_OUTER_BOUND('',#16186,.T.) ;
#13005 = FACE_OUTER_BOUND('',#16187,.T.) ;
#13006 = FACE_OUTER_BOUND('',#16188,.T.) ;
#13007 = FACE_OUTER_BOUND('',#16189,.T.) ;
#13008 = FACE_OUTER_BOUND('',#16190,.T.) ;
#13009 = FACE_OUTER_BOUND('',#16191,.T.) ;
#13010 = FACE_OUTER_BOUND('',#16192,.T.) ;
#13011 = FACE_OUTER_BOUND('',#16193,.T.) ;
#13012 = FACE_OUTER_BOUND('',#16194,.T.) ;
#13013 = FACE_OUTER_BOUND('',#16195,.T.) ;
#13014 = FACE_OUTER_BOUND('',#16196,.T.) ;
#13015 = FACE_OUTER_BOUND('',#16197,.T.) ;
#13016 = FACE_OUTER_BOUND('',#16198,.T.) ;
#13017 = FACE_OUTER_BOUND('',#16199,.T.) ;
#13018 = FACE_OUTER_BOUND('',#16200,.T.) ;
#13019 = FACE_OUTER_BOUND('',#16201,.T.) ;
#13020 = FACE_OUTER_BOUND('',#16202,.T.) ;
#13021 = FACE_OUTER_BOUND('',#16203,.T.) ;
#13022 = FACE_OUTER_BOUND('',#16204,.T.) ;
#13023 = FACE_OUTER_BOUND('',#16205,.T.) ;
#13024 = FACE_OUTER_BOUND('',#16206,.T.) ;
#13025 = FACE_OUTER_BOUND('',#16207,.T.) ;
#13026 = FACE_OUTER_BOUND('',#16208,.T.) ;
#13027 = FACE_OUTER_BOUND('',#16209,.T.) ;
#13028 = FACE_OUTER_BOUND('',#16210,.T.) ;
#13029 = FACE_OUTER_BOUND('',#16211,.T.) ;
#13030 = FACE_OUTER_BOUND('',#16212,.T.) ;
#13031 = FACE_OUTER_BOUND('',#16213,.T.) ;
#13032 = FACE_OUTER_BOUND('',#16214,.T.) ;
#13033 = FACE_OUTER_BOUND('',#16215,.T.) ;
#13034 = FACE_OUTER_BOUND('',#16216,.T.) ;
#13035 = FACE_OUTER_BOUND('',#16217,.T.) ;
#13036 = FACE_OUTER_BOUND('',#16218,.T.) ;
#13037 = FACE_OUTER_BOUND('',#16219,.T.) ;
#13038 = FACE_OUTER_BOUND('',#16220,.T.) ;
#13039 = FACE_OUTER_BOUND('',#16221,.T.) ;
#13040 = FACE_OUTER_BOUND('',#16222,.T.) ;
#13041 = FACE_OUTER_BOUND('',#16223,.T.) ;
#13042 = FACE_OUTER_BOUND('',#16224,.T.) ;
#13043 = FACE_OUTER_BOUND('',#16225,.T.) ;
#13044 = FACE_OUTER_BOUND('',#16226,.T.) ;
#13045 = FACE_OUTER_BOUND('',#16227,.T.) ;
#13046 = FACE_OUTER_BOUND('',#16228,.T.) ;
#13047 = FACE_OUTER_BOUND('',#16229,.T.) ;
#13048 = FACE_OUTER_BOUND('',#16230,.T.) ;
#13049 = FACE_OUTER_BOUND('',#16231,.T.) ;
#13050 = FACE_OUTER_BOUND('',#16232,.T.) ;
#13051 = FACE_OUTER_BOUND('',#16233,.T.) ;
#13052 = FACE_OUTER_BOUND('',#16234,.T.) ;
#13053 = FACE_OUTER_BOUND('',#16235,.T.) ;
#13054 = FACE_OUTER_BOUND('',#16236,.T.) ;
#13055 = FACE_OUTER_BOUND('',#16237,.T.) ;
#13056 = FACE_OUTER_BOUND('',#16238,.T.) ;
#13057 = FACE_OUTER_BOUND('',#16239,.T.) ;
#13058 = FACE_OUTER_BOUND('',#16240,.T.) ;
#13059 = FACE_OUTER_BOUND('',#16241,.T.) ;
#13060 = FACE_OUTER_BOUND('',#16242,.T.) ;
#13061 = FACE_OUTER_BOUND('',#16243,.T.) ;
#13062 = FACE_OUTER_BOUND('',#16244,.T.) ;
#13063 = FACE_OUTER_BOUND('',#16245,.T.) ;
#13064 = FACE_OUTER_BOUND('',#16246,.T.) ;
#13065 = FACE_OUTER_BOUND('',#16247,.T.) ;
#13066 = FACE_OUTER_BOUND('',#16248,.T.) ;
#13067 = FACE_OUTER_BOUND('',#16249,.T.) ;
#13068 = FACE_OUTER_BOUND('',#16250,.T.) ;
#13069 = FACE_OUTER_BOUND('',#16251,.T.) ;
#13070 = FACE_OUTER_BOUND('',#16252,.T.) ;
#13071 = FACE_OUTER_BOUND('',#16253,.T.) ;
#13072 = FACE_OUTER_BOUND('',#16254,.T.) ;
#13073 = FACE_OUTER_BOUND('',#16255,.T.) ;
#13074 = FACE_OUTER_BOUND('',#16256,.T.) ;
#13075 = FACE_OUTER_BOUND('',#16257,.T.) ;
#13076 = FACE_OUTER_BOUND('',#16258,.T.) ;
#13077 = FACE_OUTER_BOUND('',#16259,.T.) ;
#13078 = FACE_OUTER_BOUND('',#16260,.T.) ;
#13079 = FACE_OUTER_BOUND('',#16261,.T.) ;
#13080 = FACE_OUTER_BOUND('',#16263,.T.) ;
#13081 = FACE_OUTER_BOUND('',#16264,.T.) ;
#13082 = FACE_OUTER_BOUND('',#16265,.T.) ;
#13083 = FACE_OUTER_BOUND('',#16266,.T.) ;
#13084 = FACE_OUTER_BOUND('',#16267,.T.) ;
#13085 = FACE_OUTER_BOUND('',#16268,.T.) ;
#13086 = FACE_OUTER_BOUND('',#16269,.T.) ;
#13087 = FACE_OUTER_BOUND('',#16270,.T.) ;
#13088 = FACE_OUTER_BOUND('',#16271,.T.) ;
#13089 = FACE_OUTER_BOUND('',#16272,.T.) ;
#13090 = FACE_OUTER_BOUND('',#16273,.T.) ;
#13091 = FACE_OUTER_BOUND('',#16274,.T.) ;
#13092 = FACE_OUTER_BOUND('',#16275,.T.) ;
#13093 = FACE_OUTER_BOUND('',#16276,.T.) ;
#13094 = FACE_OUTER_BOUND('',#16277,.T.) ;
#13095 = FACE_OUTER_BOUND('',#16278,.T.) ;
#13096 = FACE_OUTER_BOUND('',#16279,.T.) ;
#13097 = FACE_OUTER_BOUND('',#16280,.T.) ;
#13098 = FACE_OUTER_BOUND('',#16281,.T.) ;
#13099 = FACE_OUTER_BOUND('',#16282,.T.) ;
#13100 = FACE_OUTER_BOUND('',#16283,.T.) ;
#13101 = FACE_OUTER_BOUND('',#16284,.T.) ;
#13102 = FACE_OUTER_BOUND('',#16285,.T.) ;
#13103 = FACE_OUTER_BOUND('',#16286,.T.) ;
#13104 = FACE_OUTER_BOUND('',#16287,.T.) ;
#13105 = FACE_OUTER_BOUND('',#16288,.T.) ;
#13106 = FACE_OUTER_BOUND('',#16289,.T.) ;
#13107 = FACE_OUTER_BOUND('',#16290,.T.) ;
#13108 = FACE_OUTER_BOUND('',#16291,.T.) ;
#13109 = FACE_OUTER_BOUND('',#16292,.T.) ;
#13110 = FACE_OUTER_BOUND('',#16293,.T.) ;
#13111 = FACE_OUTER_BOUND('',#16294,.T.) ;
#13112 = FACE_OUTER_BOUND('',#16295,.T.) ;
#13113 = FACE_OUTER_BOUND('',#16296,.T.) ;
#13114 = FACE_OUTER_BOUND('',#16297,.T.) ;
#13115 = FACE_OUTER_BOUND('',#16298,.T.) ;
#13116 = FACE_OUTER_BOUND('',#16299,.T.) ;
#13117 = FACE_OUTER_BOUND('',#16300,.T.) ;
#13118 = FACE_OUTER_BOUND('',#16301,.T.) ;
#13119 = FACE_OUTER_BOUND('',#16302,.T.) ;
#13120 = FACE_OUTER_BOUND('',#16303,.T.) ;
#13121 = FACE_OUTER_BOUND('',#16304,.T.) ;
#13122 = FACE_OUTER_BOUND('',#16305,.T.) ;
#13123 = FACE_OUTER_BOUND('',#16306,.T.) ;
#13124 = FACE_OUTER_BOUND('',#16307,.T.) ;
#13125 = FACE_OUTER_BOUND('',#16308,.T.) ;
#13126 = FACE_OUTER_BOUND('',#16309,.T.) ;
#13127 = FACE_OUTER_BOUND('',#16310,.T.) ;
#13128 = FACE_OUTER_BOUND('',#16311,.T.) ;
#13129 = FACE_OUTER_BOUND('',#16312,.T.) ;
#13130 = FACE_OUTER_BOUND('',#16313,.T.) ;
#13131 = FACE_OUTER_BOUND('',#16314,.T.) ;
#13132 = FACE_OUTER_BOUND('',#16315,.T.) ;
#13133 = FACE_OUTER_BOUND('',#16316,.T.) ;
#13134 = FACE_OUTER_BOUND('',#16317,.T.) ;
#13135 = FACE_OUTER_BOUND('',#16318,.T.) ;
#13136 = FACE_OUTER_BOUND('',#16319,.T.) ;
#13137 = FACE_OUTER_BOUND('',#16320,.T.) ;
#13138 = FACE_OUTER_BOUND('',#16321,.T.) ;
#13139 = FACE_OUTER_BOUND('',#16322,.T.) ;
#13140 = FACE_OUTER_BOUND('',#16323,.T.) ;
#13141 = FACE_OUTER_BOUND('',#16324,.T.) ;
#13142 = FACE_OUTER_BOUND('',#16325,.T.) ;
#13143 = FACE_OUTER_BOUND('',#16326,.T.) ;
#13144 = FACE_OUTER_BOUND('',#16327,.T.) ;
#13145 = FACE_OUTER_BOUND('',#16328,.T.) ;
#13146 = FACE_OUTER_BOUND('',#16329,.T.) ;
#13147 = FACE_OUTER_BOUND('',#16330,.T.) ;
#13148 = FACE_OUTER_BOUND('',#16331,.T.) ;
#13149 = FACE_OUTER_BOUND('',#16332,.T.) ;
#13150 = FACE_OUTER_BOUND('',#16333,.T.) ;
#13151 = FACE_OUTER_BOUND('',#16334,.T.) ;
#13152 = FACE_OUTER_BOUND('',#16335,.T.) ;
#13153 = FACE_OUTER_BOUND('',#16336,.T.) ;
#13154 = FACE_OUTER_BOUND('',#16337,.T.) ;
#13155 = FACE_OUTER_BOUND('',#16338,.T.) ;
#13156 = FACE_OUTER_BOUND('',#16339,.T.) ;
#13157 = FACE_OUTER_BOUND('',#16340,.T.) ;
#13158 = FACE_OUTER_BOUND('',#16341,.T.) ;
#13159 = FACE_OUTER_BOUND('',#16342,.T.) ;
#13160 = FACE_OUTER_BOUND('',#16343,.T.) ;
#13161 = FACE_OUTER_BOUND('',#16344,.T.) ;
#13162 = FACE_OUTER_BOUND('',#16345,.T.) ;
#13163 = FACE_OUTER_BOUND('',#16346,.T.) ;
#13164 = FACE_OUTER_BOUND('',#16347,.T.) ;
#13165 = FACE_OUTER_BOUND('',#16348,.T.) ;
#13166 = FACE_OUTER_BOUND('',#16349,.T.) ;
#13167 = FACE_OUTER_BOUND('',#16350,.T.) ;
#13168 = FACE_OUTER_BOUND('',#16351,.T.) ;
#13169 = FACE_OUTER_BOUND('',#16352,.T.) ;
#13170 = FACE_OUTER_BOUND('',#16353,.T.) ;
#13171 = FACE_OUTER_BOUND('',#16354,.T.) ;
#13172 = FACE_OUTER_BOUND('',#16355,.T.) ;
#13173 = FACE_OUTER_BOUND('',#16356,.T.) ;
#13174 = FACE_OUTER_BOUND('',#16357,.T.) ;
#13175 = FACE_OUTER_BOUND('',#16358,.T.) ;
#13176 = FACE_OUTER_BOUND('',#16359,.T.) ;
#13177 = FACE_OUTER_BOUND('',#16360,.T.) ;
#13178 = FACE_OUTER_BOUND('',#16361,.T.) ;
#13179 = FACE_OUTER_BOUND('',#16362,.T.) ;
#13180 = FACE_OUTER_BOUND('',#16363,.T.) ;
#13181 = FACE_OUTER_BOUND('',#16364,.T.) ;
#13182 = FACE_OUTER_BOUND('',#16365,.T.) ;
#13183 = FACE_OUTER_BOUND('',#16366,.T.) ;
#13184 = FACE_OUTER_BOUND('',#16367,.T.) ;
#13185 = FACE_OUTER_BOUND('',#16368,.T.) ;
#13186 = FACE_OUTER_BOUND('',#16369,.T.) ;
#13187 = FACE_OUTER_BOUND('',#16370,.T.) ;
#13188 = FACE_OUTER_BOUND('',#16371,.T.) ;
#13189 = FACE_OUTER_BOUND('',#16372,.T.) ;
#13190 = FACE_OUTER_BOUND('',#16373,.T.) ;
#13191 = FACE_OUTER_BOUND('',#16374,.T.) ;
#13192 = FACE_OUTER_BOUND('',#16375,.T.) ;
#13193 = FACE_OUTER_BOUND('',#16376,.T.) ;
#13194 = FACE_OUTER_BOUND('',#16377,.T.) ;
#13195 = FACE_OUTER_BOUND('',#16378,.T.) ;
#13196 = FACE_OUTER_BOUND('',#16379,.T.) ;
#13197 = FACE_OUTER_BOUND('',#16380,.T.) ;
#13198 = FACE_OUTER_BOUND('',#16381,.T.) ;
#13199 = FACE_OUTER_BOUND('',#16382,.T.) ;
#13200 = FACE_OUTER_BOUND('',#16383,.T.) ;
#13201 = FACE_OUTER_BOUND('',#16384,.T.) ;
#13202 = FACE_OUTER_BOUND('',#16385,.T.) ;
#13203 = FACE_OUTER_BOUND('',#16386,.T.) ;
#13204 = FACE_OUTER_BOUND('',#16387,.T.) ;
#13205 = FACE_OUTER_BOUND('',#16388,.T.) ;
#13206 = FACE_OUTER_BOUND('',#16389,.T.) ;
#13207 = FACE_OUTER_BOUND('',#16390,.T.) ;
#13208 = FACE_OUTER_BOUND('',#16391,.T.) ;
#13209 = FACE_OUTER_BOUND('',#16392,.T.) ;
#13210 = FACE_OUTER_BOUND('',#16393,.T.) ;
#13211 = FACE_OUTER_BOUND('',#16394,.T.) ;
#13212 = FACE_OUTER_BOUND('',#16395,.T.) ;
#13213 = FACE_OUTER_BOUND('',#16396,.T.) ;
#13214 = FACE_OUTER_BOUND('',#16397,.T.) ;
#13215 = FACE_OUTER_BOUND('',#16398,.T.) ;
#13216 = FACE_OUTER_BOUND('',#16399,.T.) ;
#13217 = FACE_OUTER_BOUND('',#16400,.T.) ;
#13218 = FACE_OUTER_BOUND('',#16401,.T.) ;
#13219 = FACE_OUTER_BOUND('',#16402,.T.) ;
#13220 = FACE_OUTER_BOUND('',#16403,.T.) ;
#13221 = FACE_OUTER_BOUND('',#16404,.T.) ;
#13222 = FACE_OUTER_BOUND('',#16405,.T.) ;
#13223 = FACE_OUTER_BOUND('',#16406,.T.) ;
#13224 = FACE_OUTER_BOUND('',#16407,.T.) ;
#13225 = FACE_OUTER_BOUND('',#16408,.T.) ;
#13226 = FACE_OUTER_BOUND('',#16409,.T.) ;
#13227 = FACE_OUTER_BOUND('',#16410,.T.) ;
#13228 = FACE_OUTER_BOUND('',#16412,.T.) ;
#13229 = FACE_OUTER_BOUND('',#16413,.T.) ;
#13230 = FACE_OUTER_BOUND('',#16414,.T.) ;
#13231 = FACE_OUTER_BOUND('',#16415,.T.) ;
#13232 = FACE_OUTER_BOUND('',#16416,.T.) ;
#13233 = FACE_OUTER_BOUND('',#16417,.T.) ;
#13234 = FACE_OUTER_BOUND('',#16418,.T.) ;
#13235 = FACE_OUTER_BOUND('',#16419,.T.) ;
#13236 = FACE_OUTER_BOUND('',#16421,.T.) ;
#13237 = FACE_OUTER_BOUND('',#16422,.T.) ;
#13238 = FACE_OUTER_BOUND('',#16424,.T.) ;
#13239 = FACE_OUTER_BOUND('',#16426,.T.) ;
#13240 = FACE_OUTER_BOUND('',#16428,.T.) ;
#13241 = FACE_OUTER_BOUND('',#16429,.T.) ;
#13242 = FACE_OUTER_BOUND('',#16430,.T.) ;
#13243 = FACE_OUTER_BOUND('',#16431,.T.) ;
#13244 = FACE_OUTER_BOUND('',#16432,.T.) ;
#13245 = FACE_OUTER_BOUND('',#16433,.T.) ;
#13246 = FACE_OUTER_BOUND('',#16434,.T.) ;
#13247 = FACE_OUTER_BOUND('',#16435,.T.) ;
#13248 = FACE_OUTER_BOUND('',#16436,.T.) ;
#13249 = FACE_OUTER_BOUND('',#16437,.T.) ;
#13250 = FACE_OUTER_BOUND('',#16438,.T.) ;
#13251 = FACE_OUTER_BOUND('',#16439,.T.) ;
#13252 = FACE_OUTER_BOUND('',#16440,.T.) ;
#13253 = FACE_OUTER_BOUND('',#16441,.T.) ;
#13254 = FACE_OUTER_BOUND('',#16442,.T.) ;
#13255 = FACE_OUTER_BOUND('',#16443,.T.) ;
#13256 = FACE_OUTER_BOUND('',#16444,.T.) ;
#13257 = FACE_OUTER_BOUND('',#16445,.T.) ;
#13258 = FACE_OUTER_BOUND('',#16446,.T.) ;
#13259 = FACE_OUTER_BOUND('',#16447,.T.) ;
#13260 = FACE_OUTER_BOUND('',#16448,.T.) ;
#13261 = FACE_OUTER_BOUND('',#16449,.T.) ;
#13262 = FACE_OUTER_BOUND('',#16450,.T.) ;
#13263 = FACE_OUTER_BOUND('',#16451,.T.) ;
#13264 = FACE_OUTER_BOUND('',#16452,.T.) ;
#13265 = FACE_OUTER_BOUND('',#16453,.T.) ;
#13266 = FACE_OUTER_BOUND('',#16454,.T.) ;
#13267 = FACE_OUTER_BOUND('',#16455,.T.) ;
#13268 = FACE_OUTER_BOUND('',#16456,.T.) ;
#13269 = FACE_OUTER_BOUND('',#16457,.T.) ;
#13270 = FACE_OUTER_BOUND('',#16458,.T.) ;
#13271 = FACE_OUTER_BOUND('',#16459,.T.) ;
#13272 = FACE_OUTER_BOUND('',#16460,.T.) ;
#13273 = FACE_OUTER_BOUND('',#16461,.T.) ;
#13274 = FACE_OUTER_BOUND('',#16462,.T.) ;
#13275 = FACE_OUTER_BOUND('',#16463,.T.) ;
#13276 = FACE_OUTER_BOUND('',#16464,.T.) ;
#13277 = FACE_OUTER_BOUND('',#16465,.T.) ;
#13278 = FACE_OUTER_BOUND('',#16466,.T.) ;
#13279 = FACE_OUTER_BOUND('',#16467,.T.) ;
#13280 = FACE_OUTER_BOUND('',#16468,.T.) ;
#13281 = FACE_OUTER_BOUND('',#16469,.T.) ;
#13282 = FACE_OUTER_BOUND('',#16470,.T.) ;
#13283 = FACE_OUTER_BOUND('',#16471,.T.) ;
#13284 = FACE_OUTER_BOUND('',#16472,.T.) ;
#13285 = FACE_OUTER_BOUND('',#16473,.T.) ;
#13286 = FACE_OUTER_BOUND('',#16474,.T.) ;
#13287 = FACE_OUTER_BOUND('',#16475,.T.) ;
#13288 = FACE_OUTER_BOUND('',#16476,.T.) ;
#13289 = FACE_OUTER_BOUND('',#16477,.T.) ;
#13290 = FACE_OUTER_BOUND('',#16478,.T.) ;
#13291 = FACE_OUTER_BOUND('',#16479,.T.) ;
#13292 = FACE_OUTER_BOUND('',#16480,.T.) ;
#13293 = FACE_OUTER_BOUND('',#16481,.T.) ;
#13294 = FACE_OUTER_BOUND('',#16482,.T.) ;
#13295 = FACE_OUTER_BOUND('',#16483,.T.) ;
#13296 = FACE_OUTER_BOUND('',#16484,.T.) ;
#13297 = FACE_OUTER_BOUND('',#16485,.T.) ;
#13298 = FACE_OUTER_BOUND('',#16486,.T.) ;
#13299 = FACE_OUTER_BOUND('',#16487,.T.) ;
#13300 = FACE_OUTER_BOUND('',#16488,.T.) ;
#13301 = FACE_OUTER_BOUND('',#16489,.T.) ;
#13302 = FACE_OUTER_BOUND('',#16490,.T.) ;
#13303 = FACE_OUTER_BOUND('',#16491,.T.) ;
#13304 = FACE_OUTER_BOUND('',#16492,.T.) ;
#13305 = FACE_OUTER_BOUND('',#16493,.T.) ;
#13306 = FACE_OUTER_BOUND('',#16494,.T.) ;
#13307 = FACE_OUTER_BOUND('',#16495,.T.) ;
#13308 = FACE_OUTER_BOUND('',#16496,.T.) ;
#13309 = FACE_OUTER_BOUND('',#16497,.T.) ;
#13310 = FACE_OUTER_BOUND('',#16498,.T.) ;
#13311 = FACE_OUTER_BOUND('',#16499,.T.) ;
#13312 = FACE_OUTER_BOUND('',#16500,.T.) ;
#13313 = FACE_OUTER_BOUND('',#16501,.T.) ;
#13314 = FACE_OUTER_BOUND('',#16502,.T.) ;
#13315 = FACE_OUTER_BOUND('',#16503,.T.) ;
#13316 = FACE_OUTER_BOUND('',#16504,.T.) ;
#13317 = FACE_OUTER_BOUND('',#16505,.T.) ;
#13318 = FACE_OUTER_BOUND('',#16506,.T.) ;
#13319 = FACE_OUTER_BOUND('',#16507,.T.) ;
#13320 = FACE_OUTER_BOUND('',#16508,.T.) ;
#13321 = FACE_OUTER_BOUND('',#16509,.T.) ;
#13322 = FACE_OUTER_BOUND('',#16510,.T.) ;
#13323 = FACE_OUTER_BOUND('',#16511,.T.) ;
#13324 = FACE_OUTER_BOUND('',#16512,.T.) ;
#13325 = FACE_OUTER_BOUND('',#16513,.T.) ;
#13326 = FACE_OUTER_BOUND('',#16514,.T.) ;
#13327 = FACE_OUTER_BOUND('',#16515,.T.) ;
#13328 = FACE_OUTER_BOUND('',#16516,.T.) ;
#13329 = FACE_OUTER_BOUND('',#16517,.T.) ;
#13330 = FACE_OUTER_BOUND('',#16518,.T.) ;
#13331 = FACE_OUTER_BOUND('',#16519,.T.) ;
#13332 = FACE_OUTER_BOUND('',#16520,.T.) ;
#13333 = FACE_OUTER_BOUND('',#16521,.T.) ;
#13334 = FACE_OUTER_BOUND('',#16522,.T.) ;
#13335 = FACE_OUTER_BOUND('',#16523,.T.) ;
#13336 = FACE_OUTER_BOUND('',#16524,.T.) ;
#13337 = FACE_OUTER_BOUND('',#16525,.T.) ;
#13338 = FACE_OUTER_BOUND('',#16526,.T.) ;
#13339 = FACE_OUTER_BOUND('',#16527,.T.) ;
#13340 = FACE_OUTER_BOUND('',#16528,.T.) ;
#13341 = FACE_OUTER_BOUND('',#16529,.T.) ;
#13342 = FACE_OUTER_BOUND('',#16530,.T.) ;
#13343 = FACE_OUTER_BOUND('',#16531,.T.) ;
#13344 = FACE_OUTER_BOUND('',#16532,.T.) ;
#13345 = FACE_OUTER_BOUND('',#16533,.T.) ;
#13346 = FACE_OUTER_BOUND('',#16534,.T.) ;
#13347 = FACE_OUTER_BOUND('',#16535,.T.) ;
#13348 = FACE_OUTER_BOUND('',#16536,.T.) ;
#13349 = FACE_OUTER_BOUND('',#16537,.T.) ;
#13350 = FACE_OUTER_BOUND('',#16538,.T.) ;
#13351 = FACE_OUTER_BOUND('',#16539,.T.) ;
#13352 = FACE_OUTER_BOUND('',#16540,.T.) ;
#13353 = FACE_OUTER_BOUND('',#16541,.T.) ;
#13354 = FACE_OUTER_BOUND('',#16542,.T.) ;
#13355 = FACE_OUTER_BOUND('',#16543,.T.) ;
#13356 = FACE_OUTER_BOUND('',#16544,.T.) ;
#13357 = FACE_OUTER_BOUND('',#16545,.T.) ;
#13358 = FACE_OUTER_BOUND('',#16546,.T.) ;
#13359 = FACE_OUTER_BOUND('',#16547,.T.) ;
#13360 = FACE_OUTER_BOUND('',#16548,.T.) ;
#13361 = FACE_OUTER_BOUND('',#16549,.T.) ;
#13362 = FACE_OUTER_BOUND('',#16550,.T.) ;
#13363 = FACE_OUTER_BOUND('',#16551,.T.) ;
#13364 = FACE_OUTER_BOUND('',#16552,.T.) ;
#13365 = FACE_OUTER_BOUND('',#16553,.T.) ;
#13366 = FACE_OUTER_BOUND('',#16554,.T.) ;
#13367 = FACE_OUTER_BOUND('',#16555,.T.) ;
#13368 = FACE_OUTER_BOUND('',#16556,.T.) ;
#13369 = FACE_OUTER_BOUND('',#16557,.T.) ;
#13370 = FACE_OUTER_BOUND('',#16558,.T.) ;
#13371 = FACE_OUTER_BOUND('',#16559,.T.) ;
#13372 = FACE_OUTER_BOUND('',#16560,.T.) ;
#13373 = FACE_OUTER_BOUND('',#16561,.T.) ;
#13374 = FACE_OUTER_BOUND('',#16562,.T.) ;
#13375 = FACE_OUTER_BOUND('',#16563,.T.) ;
#13376 = FACE_OUTER_BOUND('',#16564,.T.) ;
#13377 = FACE_OUTER_BOUND('',#16565,.T.) ;
#13378 = FACE_OUTER_BOUND('',#16566,.T.) ;
#13379 = FACE_OUTER_BOUND('',#16567,.T.) ;
#13380 = FACE_OUTER_BOUND('',#16568,.T.) ;
#13381 = FACE_OUTER_BOUND('',#16569,.T.) ;
#13382 = FACE_OUTER_BOUND('',#16570,.T.) ;
#13383 = FACE_OUTER_BOUND('',#16571,.T.) ;
#13384 = FACE_OUTER_BOUND('',#16572,.T.) ;
#13385 = FACE_OUTER_BOUND('',#16573,.T.) ;
#13386 = FACE_OUTER_BOUND('',#16574,.T.) ;
#13387 = FACE_OUTER_BOUND('',#16575,.T.) ;
#13388 = FACE_OUTER_BOUND('',#16576,.T.) ;
#13389 = FACE_OUTER_BOUND('',#16577,.T.) ;
#13390 = FACE_OUTER_BOUND('',#16578,.T.) ;
#13391 = FACE_OUTER_BOUND('',#16579,.T.) ;
#13392 = FACE_OUTER_BOUND('',#16580,.T.) ;
#13393 = FACE_OUTER_BOUND('',#16581,.T.) ;
#13394 = FACE_OUTER_BOUND('',#16582,.T.) ;
#13395 = FACE_OUTER_BOUND('',#16583,.T.) ;
#13396 = FACE_OUTER_BOUND('',#16584,.T.) ;
#13397 = FACE_OUTER_BOUND('',#16585,.T.) ;
#13398 = FACE_OUTER_BOUND('',#16586,.T.) ;
#13399 = FACE_OUTER_BOUND('',#16587,.T.) ;
#13400 = FACE_OUTER_BOUND('',#16588,.T.) ;
#13401 = FACE_OUTER_BOUND('',#16589,.T.) ;
#13402 = FACE_OUTER_BOUND('',#16590,.T.) ;
#13403 = FACE_OUTER_BOUND('',#16591,.T.) ;
#13404 = FACE_OUTER_BOUND('',#16592,.T.) ;
#13405 = FACE_OUTER_BOUND('',#16593,.T.) ;
#13406 = FACE_OUTER_BOUND('',#16594,.T.) ;
#13407 = FACE_OUTER_BOUND('',#16595,.T.) ;
#13408 = FACE_OUTER_BOUND('',#16596,.T.) ;
#13409 = FACE_OUTER_BOUND('',#16597,.T.) ;
#13410 = FACE_OUTER_BOUND('',#16598,.T.) ;
#13411 = FACE_OUTER_BOUND('',#16599,.T.) ;
#13412 = FACE_OUTER_BOUND('',#16600,.T.) ;
#13413 = FACE_OUTER_BOUND('',#16601,.T.) ;
#13414 = FACE_OUTER_BOUND('',#16602,.T.) ;
#13415 = FACE_OUTER_BOUND('',#16603,.T.) ;
#13416 = FACE_OUTER_BOUND('',#16604,.T.) ;
#13417 = FACE_OUTER_BOUND('',#16605,.T.) ;
#13418 = FACE_OUTER_BOUND('',#16606,.T.) ;
#13419 = FACE_OUTER_BOUND('',#16607,.T.) ;
#13420 = FACE_OUTER_BOUND('',#16608,.T.) ;
#13421 = FACE_OUTER_BOUND('',#16609,.T.) ;
#13422 = FACE_OUTER_BOUND('',#16610,.T.) ;
#13423 = FACE_OUTER_BOUND('',#16611,.T.) ;
#13424 = FACE_OUTER_BOUND('',#16612,.T.) ;
#13425 = FACE_OUTER_BOUND('',#16613,.T.) ;
#13426 = FACE_OUTER_BOUND('',#16614,.T.) ;
#13427 = FACE_OUTER_BOUND('',#16615,.T.) ;
#13428 = FACE_OUTER_BOUND('',#16616,.T.) ;
#13429 = FACE_OUTER_BOUND('',#16617,.T.) ;
#13430 = FACE_OUTER_BOUND('',#16618,.T.) ;
#13431 = FACE_OUTER_BOUND('',#16619,.T.) ;
#13432 = FACE_OUTER_BOUND('',#16620,.T.) ;
#13433 = FACE_OUTER_BOUND('',#16621,.T.) ;
#13434 = FACE_OUTER_BOUND('',#16622,.T.) ;
#13435 = FACE_OUTER_BOUND('',#16623,.T.) ;
#13436 = FACE_OUTER_BOUND('',#16624,.T.) ;
#13437 = FACE_OUTER_BOUND('',#16625,.T.) ;
#13438 = FACE_OUTER_BOUND('',#16626,.T.) ;
#13439 = FACE_OUTER_BOUND('',#16627,.T.) ;
#13440 = FACE_OUTER_BOUND('',#16628,.T.) ;
#13441 = FACE_OUTER_BOUND('',#16629,.T.) ;
#13442 = FACE_OUTER_BOUND('',#16630,.T.) ;
#13443 = FACE_OUTER_BOUND('',#16631,.T.) ;
#13444 = FACE_OUTER_BOUND('',#16632,.T.) ;
#13445 = FACE_OUTER_BOUND('',#16633,.T.) ;
#13446 = FACE_OUTER_BOUND('',#16634,.T.) ;
#13447 = FACE_OUTER_BOUND('',#16635,.T.) ;
#13448 = FACE_OUTER_BOUND('',#16636,.T.) ;
#13449 = FACE_OUTER_BOUND('',#16637,.T.) ;
#13450 = FACE_OUTER_BOUND('',#16638,.T.) ;
#13451 = FACE_OUTER_BOUND('',#16639,.T.) ;
#13452 = FACE_OUTER_BOUND('',#16640,.T.) ;
#13453 = FACE_OUTER_BOUND('',#16641,.T.) ;
#13454 = FACE_OUTER_BOUND('',#16642,.T.) ;
#13455 = FACE_OUTER_BOUND('',#16643,.T.) ;
#13456 = FACE_OUTER_BOUND('',#16644,.T.) ;
#13457 = FACE_OUTER_BOUND('',#16645,.T.) ;
#13458 = FACE_OUTER_BOUND('',#16646,.T.) ;
#13459 = FACE_OUTER_BOUND('',#16647,.T.) ;
#13460 = FACE_OUTER_BOUND('',#16648,.T.) ;
#13461 = FACE_OUTER_BOUND('',#16649,.T.) ;
#13462 = FACE_OUTER_BOUND('',#16650,.T.) ;
#13463 = FACE_OUTER_BOUND('',#16651,.T.) ;
#13464 = FACE_OUTER_BOUND('',#16652,.T.) ;
#13465 = FACE_OUTER_BOUND('',#16653,.T.) ;
#13466 = FACE_OUTER_BOUND('',#16654,.T.) ;
#13467 = FACE_OUTER_BOUND('',#16655,.T.) ;
#13468 = FACE_OUTER_BOUND('',#16656,.T.) ;
#13469 = FACE_OUTER_BOUND('',#16657,.T.) ;
#13470 = FACE_OUTER_BOUND('',#16658,.T.) ;
#13471 = FACE_OUTER_BOUND('',#16659,.T.) ;
#13472 = FACE_OUTER_BOUND('',#16660,.T.) ;
#13473 = FACE_OUTER_BOUND('',#16661,.T.) ;
#13474 = FACE_OUTER_BOUND('',#16662,.T.) ;
#13475 = FACE_OUTER_BOUND('',#16663,.T.) ;
#13476 = FACE_OUTER_BOUND('',#16664,.T.) ;
#13477 = FACE_OUTER_BOUND('',#16665,.T.) ;
#13478 = FACE_OUTER_BOUND('',#16666,.T.) ;
#13479 = FACE_OUTER_BOUND('',#16667,.T.) ;
#13480 = FACE_OUTER_BOUND('',#16668,.T.) ;
#13481 = FACE_OUTER_BOUND('',#16669,.T.) ;
#13482 = FACE_OUTER_BOUND('',#16670,.T.) ;
#13483 = FACE_OUTER_BOUND('',#16671,.T.) ;
#13484 = FACE_OUTER_BOUND('',#16672,.T.) ;
#13485 = FACE_OUTER_BOUND('',#16673,.T.) ;
#13486 = FACE_OUTER_BOUND('',#16674,.T.) ;
#13487 = FACE_OUTER_BOUND('',#16675,.T.) ;
#13488 = FACE_OUTER_BOUND('',#16676,.T.) ;
#13489 = FACE_OUTER_BOUND('',#16677,.T.) ;
#13490 = FACE_OUTER_BOUND('',#16678,.T.) ;
#13491 = FACE_OUTER_BOUND('',#16679,.T.) ;
#13492 = FACE_OUTER_BOUND('',#16680,.T.) ;
#13493 = FACE_OUTER_BOUND('',#16681,.T.) ;
#13494 = FACE_OUTER_BOUND('',#16682,.T.) ;
#13495 = FACE_OUTER_BOUND('',#16683,.T.) ;
#13496 = FACE_OUTER_BOUND('',#16684,.T.) ;
#13497 = FACE_OUTER_BOUND('',#16685,.T.) ;
#13498 = FACE_OUTER_BOUND('',#16686,.T.) ;
#13499 = FACE_OUTER_BOUND('',#16687,.T.) ;
#13500 = FACE_OUTER_BOUND('',#16688,.T.) ;
#13501 = FACE_OUTER_BOUND('',#16689,.T.) ;
#13502 = FACE_OUTER_BOUND('',#16690,.T.) ;
#13503 = FACE_OUTER_BOUND('',#16691,.T.) ;
#13504 = FACE_OUTER_BOUND('',#16692,.T.) ;
#13505 = FACE_OUTER_BOUND('',#16693,.T.) ;
#13506 = FACE_OUTER_BOUND('',#16694,.T.) ;
#13507 = FACE_OUTER_BOUND('',#16695,.T.) ;
#13508 = FACE_OUTER_BOUND('',#16696,.T.) ;
#13509 = FACE_OUTER_BOUND('',#16697,.T.) ;
#13510 = FACE_OUTER_BOUND('',#16698,.T.) ;
#13511 = FACE_OUTER_BOUND('',#16699,.T.) ;
#13512 = FACE_OUTER_BOUND('',#16700,.T.) ;
#13513 = FACE_OUTER_BOUND('',#16701,.T.) ;
#13514 = FACE_OUTER_BOUND('',#16702,.T.) ;
#13515 = FACE_OUTER_BOUND('',#16703,.T.) ;
#13516 = FACE_OUTER_BOUND('',#16704,.T.) ;
#13517 = FACE_OUTER_BOUND('',#16705,.T.) ;
#13518 = FACE_OUTER_BOUND('',#16706,.T.) ;
#13519 = FACE_OUTER_BOUND('',#16707,.T.) ;
#13520 = FACE_OUTER_BOUND('',#16708,.T.) ;
#13521 = FACE_OUTER_BOUND('',#16709,.T.) ;
#13522 = FACE_OUTER_BOUND('',#16710,.T.) ;
#13523 = FACE_OUTER_BOUND('',#16711,.T.) ;
#13524 = FACE_OUTER_BOUND('',#16712,.T.) ;
#13525 = FACE_OUTER_BOUND('',#16713,.T.) ;
#13526 = FACE_OUTER_BOUND('',#16714,.T.) ;
#13527 = FACE_OUTER_BOUND('',#16716,.T.) ;
#13528 = FACE_OUTER_BOUND('',#16717,.T.) ;
#13529 = FACE_OUTER_BOUND('',#16719,.T.) ;
#13530 = FACE_OUTER_BOUND('',#16721,.T.) ;
#13531 = FACE_OUTER_BOUND('',#16723,.T.) ;
#13532 = FACE_OUTER_BOUND('',#16724,.T.) ;
#13533 = FACE_OUTER_BOUND('',#16725,.T.) ;
#13534 = FACE_OUTER_BOUND('',#16726,.T.) ;
#13535 = FACE_OUTER_BOUND('',#16727,.T.) ;
#13536 = FACE_OUTER_BOUND('',#16728,.T.) ;
#13537 = FACE_OUTER_BOUND('',#16729,.T.) ;
#13538 = FACE_OUTER_BOUND('',#16730,.T.) ;
#13539 = FACE_OUTER_BOUND('',#16731,.T.) ;
#13540 = FACE_OUTER_BOUND('',#16732,.T.) ;
#13541 = FACE_OUTER_BOUND('',#16733,.T.) ;
#13542 = FACE_OUTER_BOUND('',#16734,.T.) ;
#13543 = FACE_OUTER_BOUND('',#16735,.T.) ;
#13544 = FACE_OUTER_BOUND('',#16736,.T.) ;
#13545 = FACE_OUTER_BOUND('',#16737,.T.) ;
#13546 = FACE_OUTER_BOUND('',#16738,.T.) ;
#13547 = FACE_OUTER_BOUND('',#16739,.T.) ;
#13548 = FACE_OUTER_BOUND('',#16740,.T.) ;
#13549 = FACE_OUTER_BOUND('',#16741,.T.) ;
#13550 = FACE_OUTER_BOUND('',#16742,.T.) ;
#13551 = FACE_OUTER_BOUND('',#16743,.T.) ;
#13552 = FACE_OUTER_BOUND('',#16744,.T.) ;
#13553 = FACE_OUTER_BOUND('',#16745,.T.) ;
#13554 = FACE_OUTER_BOUND('',#16746,.T.) ;
#13555 = FACE_OUTER_BOUND('',#16747,.T.) ;
#13556 = FACE_OUTER_BOUND('',#16748,.T.) ;
#13557 = FACE_OUTER_BOUND('',#16749,.T.) ;
#13558 = FACE_OUTER_BOUND('',#16750,.T.) ;
#13559 = FACE_OUTER_BOUND('',#16751,.T.) ;
#13560 = FACE_OUTER_BOUND('',#16752,.T.) ;
#13561 = FACE_OUTER_BOUND('',#16753,.T.) ;
#13562 = FACE_OUTER_BOUND('',#16754,.T.) ;
#13563 = FACE_OUTER_BOUND('',#16755,.T.) ;
#13564 = FACE_OUTER_BOUND('',#16756,.T.) ;
#13565 = FACE_OUTER_BOUND('',#16757,.T.) ;
#13566 = FACE_OUTER_BOUND('',#16758,.T.) ;
#13567 = FACE_OUTER_BOUND('',#16759,.T.) ;
#13568 = FACE_OUTER_BOUND('',#16760,.T.) ;
#13569 = FACE_OUTER_BOUND('',#16761,.T.) ;
#13570 = FACE_OUTER_BOUND('',#16762,.T.) ;
#13571 = FACE_OUTER_BOUND('',#16763,.T.) ;
#13572 = FACE_OUTER_BOUND('',#16764,.T.) ;
#13573 = FACE_OUTER_BOUND('',#16765,.T.) ;
#13574 = FACE_OUTER_BOUND('',#16766,.T.) ;
#13575 = FACE_OUTER_BOUND('',#16767,.T.) ;
#13576 = FACE_OUTER_BOUND('',#16768,.T.) ;
#13577 = FACE_OUTER_BOUND('',#16769,.T.) ;
#13578 = FACE_OUTER_BOUND('',#16770,.T.) ;
#13579 = FACE_OUTER_BOUND('',#16771,.T.) ;
#13580 = FACE_OUTER_BOUND('',#16772,.T.) ;
#13581 = FACE_OUTER_BOUND('',#16773,.T.) ;
#13582 = FACE_OUTER_BOUND('',#16774,.T.) ;
#13583 = FACE_OUTER_BOUND('',#16775,.T.) ;
#13584 = FACE_OUTER_BOUND('',#16776,.T.) ;
#13585 = FACE_OUTER_BOUND('',#16777,.T.) ;
#13586 = FACE_OUTER_BOUND('',#16778,.T.) ;
#13587 = FACE_OUTER_BOUND('',#16779,.T.) ;
#13588 = FACE_OUTER_BOUND('',#16780,.T.) ;
#13589 = FACE_OUTER_BOUND('',#16781,.T.) ;
#13590 = FACE_OUTER_BOUND('',#16782,.T.) ;
#13591 = FACE_OUTER_BOUND('',#16783,.T.) ;
#13592 = FACE_OUTER_BOUND('',#16784,.T.) ;
#13593 = FACE_OUTER_BOUND('',#16785,.T.) ;
#13594 = FACE_OUTER_BOUND('',#16786,.T.) ;
#13595 = FACE_OUTER_BOUND('',#16787,.T.) ;
#13596 = FACE_OUTER_BOUND('',#16788,.T.) ;
#13597 = FACE_OUTER_BOUND('',#16789,.T.) ;
#13598 = FACE_OUTER_BOUND('',#16790,.T.) ;
#13599 = FACE_OUTER_BOUND('',#16791,.T.) ;
#13600 = FACE_OUTER_BOUND('',#16792,.T.) ;
#13601 = FACE_OUTER_BOUND('',#16793,.T.) ;
#13602 = FACE_OUTER_BOUND('',#16794,.T.) ;
#13603 = FACE_OUTER_BOUND('',#16795,.T.) ;
#13604 = FACE_OUTER_BOUND('',#16796,.T.) ;
#13605 = FACE_OUTER_BOUND('',#16797,.T.) ;
#13606 = FACE_OUTER_BOUND('',#16798,.T.) ;
#13607 = FACE_OUTER_BOUND('',#16799,.T.) ;
#13608 = FACE_OUTER_BOUND('',#16800,.T.) ;
#13609 = FACE_OUTER_BOUND('',#16801,.T.) ;
#13610 = FACE_OUTER_BOUND('',#16802,.T.) ;
#13611 = FACE_OUTER_BOUND('',#16803,.T.) ;
#13612 = FACE_OUTER_BOUND('',#16804,.T.) ;
#13613 = FACE_OUTER_BOUND('',#16805,.T.) ;
#13614 = FACE_OUTER_BOUND('',#16806,.T.) ;
#13615 = FACE_OUTER_BOUND('',#16807,.T.) ;
#13616 = FACE_OUTER_BOUND('',#16808,.T.) ;
#13617 = FACE_OUTER_BOUND('',#16809,.T.) ;
#13618 = FACE_OUTER_BOUND('',#16810,.T.) ;
#13619 = FACE_OUTER_BOUND('',#16811,.T.) ;
#13620 = FACE_OUTER_BOUND('',#16812,.T.) ;
#13621 = FACE_OUTER_BOUND('',#16813,.T.) ;
#13622 = FACE_OUTER_BOUND('',#16814,.T.) ;
#13623 = FACE_OUTER_BOUND('',#16815,.T.) ;
#13624 = FACE_OUTER_BOUND('',#16816,.T.) ;
#13625 = FACE_OUTER_BOUND('',#16817,.T.) ;
#13626 = FACE_OUTER_BOUND('',#16818,.T.) ;
#13627 = FACE_OUTER_BOUND('',#16819,.T.) ;
#13628 = FACE_OUTER_BOUND('',#16820,.T.) ;
#13629 = FACE_OUTER_BOUND('',#16821,.T.) ;
#13630 = FACE_OUTER_BOUND('',#16822,.T.) ;
#13631 = FACE_OUTER_BOUND('',#16823,.T.) ;
#13632 = FACE_OUTER_BOUND('',#16824,.T.) ;
#13633 = FACE_OUTER_BOUND('',#16825,.T.) ;
#13634 = FACE_OUTER_BOUND('',#16826,.T.) ;
#13635 = FACE_OUTER_BOUND('',#16827,.T.) ;
#13636 = FACE_OUTER_BOUND('',#16828,.T.) ;
#13637 = FACE_OUTER_BOUND('',#16829,.T.) ;
#13638 = FACE_OUTER_BOUND('',#16830,.T.) ;
#13639 = FACE_OUTER_BOUND('',#16831,.T.) ;
#13640 = FACE_OUTER_BOUND('',#16832,.T.) ;
#13641 = FACE_OUTER_BOUND('',#16833,.T.) ;
#13642 = FACE_OUTER_BOUND('',#16834,.T.) ;
#13643 = FACE_OUTER_BOUND('',#16835,.T.) ;
#13644 = FACE_OUTER_BOUND('',#16836,.T.) ;
#13645 = FACE_OUTER_BOUND('',#16837,.T.) ;
#13646 = FACE_OUTER_BOUND('',#16838,.T.) ;
#13647 = FACE_OUTER_BOUND('',#16839,.T.) ;
#13648 = FACE_OUTER_BOUND('',#16840,.T.) ;
#13649 = FACE_OUTER_BOUND('',#16841,.T.) ;
#13650 = FACE_OUTER_BOUND('',#16842,.T.) ;
#13651 = FACE_OUTER_BOUND('',#16843,.T.) ;
#13652 = FACE_OUTER_BOUND('',#16844,.T.) ;
#13653 = FACE_OUTER_BOUND('',#16845,.T.) ;
#13654 = FACE_OUTER_BOUND('',#16846,.T.) ;
#13655 = FACE_OUTER_BOUND('',#16847,.T.) ;
#13656 = FACE_OUTER_BOUND('',#16848,.T.) ;
#13657 = FACE_OUTER_BOUND('',#16849,.T.) ;
#13658 = FACE_OUTER_BOUND('',#16850,.T.) ;
#13659 = FACE_OUTER_BOUND('',#16851,.T.) ;
#13660 = FACE_OUTER_BOUND('',#16852,.T.) ;
#13661 = FACE_OUTER_BOUND('',#16853,.T.) ;
#13662 = FACE_OUTER_BOUND('',#16854,.T.) ;
#13663 = FACE_OUTER_BOUND('',#16855,.T.) ;
#13664 = FACE_OUTER_BOUND('',#16856,.T.) ;
#13665 = FACE_OUTER_BOUND('',#16857,.T.) ;
#13666 = FACE_OUTER_BOUND('',#16858,.T.) ;
#13667 = FACE_OUTER_BOUND('',#16859,.T.) ;
#13668 = FACE_OUTER_BOUND('',#16860,.T.) ;
#13669 = FACE_OUTER_BOUND('',#16861,.T.) ;
#13670 = FACE_OUTER_BOUND('',#16862,.T.) ;
#13671 = FACE_OUTER_BOUND('',#16863,.T.) ;
#13672 = FACE_OUTER_BOUND('',#16864,.T.) ;
#13673 = FACE_OUTER_BOUND('',#16865,.T.) ;
#13674 = FACE_OUTER_BOUND('',#16866,.T.) ;
#13675 = FACE_OUTER_BOUND('',#16867,.T.) ;
#13676 = FACE_OUTER_BOUND('',#16868,.T.) ;
#13677 = FACE_OUTER_BOUND('',#16869,.T.) ;
#13678 = FACE_OUTER_BOUND('',#16870,.T.) ;
#13679 = FACE_OUTER_BOUND('',#16871,.T.) ;
#13680 = FACE_OUTER_BOUND('',#16872,.T.) ;
#13681 = FACE_OUTER_BOUND('',#16873,.T.) ;
#13682 = FACE_OUTER_BOUND('',#16874,.T.) ;
#13683 = FACE_OUTER_BOUND('',#16875,.T.) ;
#13684 = FACE_OUTER_BOUND('',#16876,.T.) ;
#13685 = FACE_OUTER_BOUND('',#16877,.T.) ;
#13686 = FACE_OUTER_BOUND('',#16878,.T.) ;
#13687 = FACE_OUTER_BOUND('',#16879,.T.) ;
#13688 = FACE_OUTER_BOUND('',#16880,.T.) ;
#13689 = FACE_OUTER_BOUND('',#16881,.T.) ;
#13690 = FACE_OUTER_BOUND('',#16882,.T.) ;
#13691 = FACE_OUTER_BOUND('',#16883,.T.) ;
#13692 = FACE_OUTER_BOUND('',#16884,.T.) ;
#13693 = FACE_OUTER_BOUND('',#16885,.T.) ;
#13694 = FACE_OUTER_BOUND('',#16886,.T.) ;
#13695 = FACE_OUTER_BOUND('',#16887,.T.) ;
#13696 = FACE_OUTER_BOUND('',#16888,.T.) ;
#13697 = FACE_OUTER_BOUND('',#16889,.T.) ;
#13698 = FACE_OUTER_BOUND('',#16890,.T.) ;
#13699 = FACE_OUTER_BOUND('',#16891,.T.) ;
#13700 = FACE_OUTER_BOUND('',#16892,.T.) ;
#13701 = FACE_OUTER_BOUND('',#16893,.T.) ;
#13702 = FACE_OUTER_BOUND('',#16894,.T.) ;
#13703 = FACE_OUTER_BOUND('',#16895,.T.) ;
#13704 = FACE_OUTER_BOUND('',#16896,.T.) ;
#13705 = FACE_OUTER_BOUND('',#16897,.T.) ;
#13706 = FACE_OUTER_BOUND('',#16898,.T.) ;
#13707 = FACE_OUTER_BOUND('',#16899,.T.) ;
#13708 = FACE_OUTER_BOUND('',#16900,.T.) ;
#13709 = FACE_OUTER_BOUND('',#16901,.T.) ;
#13710 = FACE_OUTER_BOUND('',#16902,.T.) ;
#13711 = FACE_OUTER_BOUND('',#16903,.T.) ;
#13712 = FACE_OUTER_BOUND('',#16904,.T.) ;
#13713 = FACE_OUTER_BOUND('',#16905,.T.) ;
#13714 = FACE_OUTER_BOUND('',#16906,.T.) ;
#13715 = FACE_OUTER_BOUND('',#16907,.T.) ;
#13716 = FACE_OUTER_BOUND('',#16908,.T.) ;
#13717 = FACE_OUTER_BOUND('',#16909,.T.) ;
#13718 = FACE_OUTER_BOUND('',#16910,.T.) ;
#13719 = FACE_OUTER_BOUND('',#16911,.T.) ;
#13720 = FACE_OUTER_BOUND('',#16912,.T.) ;
#13721 = FACE_OUTER_BOUND('',#16913,.T.) ;
#13722 = FACE_OUTER_BOUND('',#16914,.T.) ;
#13723 = FACE_OUTER_BOUND('',#16915,.T.) ;
#13724 = FACE_OUTER_BOUND('',#16916,.T.) ;
#13725 = FACE_OUTER_BOUND('',#16917,.T.) ;
#13726 = FACE_OUTER_BOUND('',#16918,.T.) ;
#13727 = FACE_OUTER_BOUND('',#16919,.T.) ;
#13728 = FACE_OUTER_BOUND('',#16920,.T.) ;
#13729 = FACE_OUTER_BOUND('',#16921,.T.) ;
#13730 = FACE_OUTER_BOUND('',#16922,.T.) ;
#13731 = FACE_OUTER_BOUND('',#16923,.T.) ;
#13732 = FACE_OUTER_BOUND('',#16924,.T.) ;
#13733 = FACE_OUTER_BOUND('',#16925,.T.) ;
#13734 = FACE_OUTER_BOUND('',#16926,.T.) ;
#13735 = FACE_OUTER_BOUND('',#16927,.T.) ;
#13736 = FACE_OUTER_BOUND('',#16928,.T.) ;
#13737 = FACE_OUTER_BOUND('',#16929,.T.) ;
#13738 = FACE_OUTER_BOUND('',#16930,.T.) ;
#13739 = FACE_OUTER_BOUND('',#16931,.T.) ;
#13740 = FACE_OUTER_BOUND('',#16932,.T.) ;
#13741 = FACE_OUTER_BOUND('',#16933,.T.) ;
#13742 = FACE_OUTER_BOUND('',#16934,.T.) ;
#13743 = FACE_OUTER_BOUND('',#16935,.T.) ;
#13744 = FACE_OUTER_BOUND('',#16936,.T.) ;
#13745 = FACE_OUTER_BOUND('',#16937,.T.) ;
#13746 = FACE_OUTER_BOUND('',#16938,.T.) ;
#13747 = FACE_OUTER_BOUND('',#16939,.T.) ;
#13748 = FACE_OUTER_BOUND('',#16940,.T.) ;
#13749 = FACE_OUTER_BOUND('',#16941,.T.) ;
#13750 = FACE_OUTER_BOUND('',#16942,.T.) ;
#13751 = FACE_OUTER_BOUND('',#16943,.T.) ;
#13752 = FACE_OUTER_BOUND('',#16944,.T.) ;
#13753 = FACE_OUTER_BOUND('',#16945,.T.) ;
#13754 = FACE_OUTER_BOUND('',#16946,.T.) ;
#13755 = FACE_OUTER_BOUND('',#16947,.T.) ;
#13756 = FACE_OUTER_BOUND('',#16948,.T.) ;
#13757 = FACE_OUTER_BOUND('',#16949,.T.) ;
#13758 = FACE_OUTER_BOUND('',#16950,.T.) ;
#13759 = FACE_OUTER_BOUND('',#16951,.T.) ;
#13760 = FACE_OUTER_BOUND('',#16952,.T.) ;
#13761 = FACE_OUTER_BOUND('',#16953,.T.) ;
#13762 = FACE_OUTER_BOUND('',#16954,.T.) ;
#13763 = FACE_OUTER_BOUND('',#16955,.T.) ;
#13764 = FACE_OUTER_BOUND('',#16956,.T.) ;
#13765 = FACE_OUTER_BOUND('',#16957,.T.) ;
#13766 = FACE_OUTER_BOUND('',#16958,.T.) ;
#13767 = FACE_OUTER_BOUND('',#16959,.T.) ;
#13768 = FACE_OUTER_BOUND('',#16960,.T.) ;
#13769 = FACE_OUTER_BOUND('',#16961,.T.) ;
#13770 = FACE_OUTER_BOUND('',#16962,.T.) ;
#13771 = FACE_OUTER_BOUND('',#16963,.T.) ;
#13772 = FACE_OUTER_BOUND('',#16964,.T.) ;
#13773 = FACE_OUTER_BOUND('',#16965,.T.) ;
#13774 = FACE_OUTER_BOUND('',#16966,.T.) ;
#13775 = FACE_OUTER_BOUND('',#16967,.T.) ;
#13776 = FACE_OUTER_BOUND('',#16968,.T.) ;
#13777 = FACE_OUTER_BOUND('',#16969,.T.) ;
#13778 = FACE_OUTER_BOUND('',#16970,.T.) ;
#13779 = FACE_OUTER_BOUND('',#16971,.T.) ;
#13780 = FACE_OUTER_BOUND('',#16972,.T.) ;
#13781 = FACE_OUTER_BOUND('',#16973,.T.) ;
#13782 = FACE_OUTER_BOUND('',#16974,.T.) ;
#13783 = FACE_OUTER_BOUND('',#16975,.T.) ;
#13784 = FACE_OUTER_BOUND('',#16976,.T.) ;
#13785 = FACE_OUTER_BOUND('',#16977,.T.) ;
#13786 = FACE_OUTER_BOUND('',#16978,.T.) ;
#13787 = FACE_OUTER_BOUND('',#16979,.T.) ;
#13788 = FACE_OUTER_BOUND('',#16980,.T.) ;
#13789 = FACE_OUTER_BOUND('',#16981,.T.) ;
#13790 = FACE_OUTER_BOUND('',#16982,.T.) ;
#13791 = FACE_OUTER_BOUND('',#16983,.T.) ;
#13792 = FACE_OUTER_BOUND('',#16984,.T.) ;
#13793 = FACE_OUTER_BOUND('',#16985,.T.) ;
#13794 = FACE_OUTER_BOUND('',#16986,.T.) ;
#13795 = FACE_OUTER_BOUND('',#16987,.T.) ;
#13796 = FACE_OUTER_BOUND('',#16988,.T.) ;
#13797 = FACE_OUTER_BOUND('',#16989,.T.) ;
#13798 = FACE_OUTER_BOUND('',#16990,.T.) ;
#13799 = FACE_OUTER_BOUND('',#16991,.T.) ;
#13800 = FACE_OUTER_BOUND('',#16992,.T.) ;
#13801 = FACE_OUTER_BOUND('',#16993,.T.) ;
#13802 = FACE_OUTER_BOUND('',#16994,.T.) ;
#13803 = FACE_OUTER_BOUND('',#16995,.T.) ;
#13804 = FACE_OUTER_BOUND('',#16996,.T.) ;
#13805 = FACE_OUTER_BOUND('',#16997,.T.) ;
#13806 = FACE_OUTER_BOUND('',#16998,.T.) ;
#13807 = FACE_OUTER_BOUND('',#16999,.T.) ;
#13808 = FACE_OUTER_BOUND('',#17000,.T.) ;
#13809 = FACE_OUTER_BOUND('',#17001,.T.) ;
#13810 = FACE_OUTER_BOUND('',#17002,.T.) ;
#13811 = FACE_OUTER_BOUND('',#17003,.T.) ;
#13812 = FACE_OUTER_BOUND('',#17004,.T.) ;
#13813 = FACE_OUTER_BOUND('',#17005,.T.) ;
#13814 = FACE_OUTER_BOUND('',#17006,.T.) ;
#13815 = FACE_OUTER_BOUND('',#17007,.T.) ;
#13816 = FACE_OUTER_BOUND('',#17008,.T.) ;
#13817 = FACE_OUTER_BOUND('',#17009,.T.) ;
#13818 = FACE_OUTER_BOUND('',#17010,.T.) ;
#13819 = FACE_OUTER_BOUND('',#17011,.T.) ;
#13820 = FACE_OUTER_BOUND('',#17012,.T.) ;
#13821 = FACE_OUTER_BOUND('',#17013,.T.) ;
#13822 = FACE_OUTER_BOUND('',#17014,.T.) ;
#13823 = FACE_OUTER_BOUND('',#17015,.T.) ;
#13824 = FACE_OUTER_BOUND('',#17016,.T.) ;
#13825 = FACE_OUTER_BOUND('',#17017,.T.) ;
#13826 = FACE_OUTER_BOUND('',#17018,.T.) ;
#13827 = FACE_OUTER_BOUND('',#17022,.T.) ;
#13828 = FACE_OUTER_BOUND('',#17023,.T.) ;
#13829 = FACE_OUTER_BOUND('',#17024,.T.) ;
#13830 = FACE_OUTER_BOUND('',#17025,.T.) ;
#13831 = FACE_OUTER_BOUND('',#17026,.T.) ;
#13832 = FACE_OUTER_BOUND('',#17027,.T.) ;
#13833 = FACE_OUTER_BOUND('',#17028,.T.) ;
#13834 = FACE_OUTER_BOUND('',#17029,.T.) ;
#13835 = FACE_OUTER_BOUND('',#17030,.T.) ;
#13836 = FACE_OUTER_BOUND('',#17031,.T.) ;
#13837 = FACE_OUTER_BOUND('',#17032,.T.) ;
#13838 = FACE_OUTER_BOUND('',#17033,.T.) ;
#13839 = EDGE_LOOP('',(#30994,#30995,#30996,#30997)) ;
#13840 = EDGE_LOOP('',(#30998,#30999,#31000,#31001,#31002,#31003,#31004,#31005,
#31006,#31007,#31008,#31009,#31010,#31011,#31012,#31013,#31014,#31015,#31016,
#31017,#31018,#31019,#31020,#31021,#31022,#31023,#31024,#31025,#31026,#31027,
#31028,#31029,#31030,#31031,#31032,#31033,#31034,#31035,#31036,#31037,#31038,
#31039,#31040,#31041,#31042,#31043,#31044,#31045,#31046,#31047,#31048,#31049,
#31050,#31051,#31052,#31053,#31054,#31055,#31056,#31057,#31058,#31059,#31060,
#31061,#31062,#31063,#31064,#31065,#31066,#31067,#31068,#31069,#31070,#31071,
#31072,#31073,#31074,#31075,#31076,#31077,#31078,#31079,#31080,#31081)) ;
#13841 = EDGE_LOOP('',(#31082)) ;
#13842 = EDGE_LOOP('',(#31083,#31084,#31085,#31086)) ;
#13843 = EDGE_LOOP('',(#31087,#31088,#31089,#31090)) ;
#13844 = EDGE_LOOP('',(#31091,#31092,#31093,#31094)) ;
#13845 = EDGE_LOOP('',(#31095,#31096,#31097,#31098)) ;
#13846 = EDGE_LOOP('',(#31099,#31100,#31101,#31102)) ;
#13847 = EDGE_LOOP('',(#31103,#31104,#31105,#31106)) ;
#13848 = EDGE_LOOP('',(#31107,#31108,#31109,#31110)) ;
#13849 = EDGE_LOOP('',(#31111,#31112,#31113,#31114)) ;
#13850 = EDGE_LOOP('',(#31115,#31116,#31117,#31118)) ;
#13851 = EDGE_LOOP('',(#31119,#31120,#31121,#31122)) ;
#13852 = EDGE_LOOP('',(#31123,#31124,#31125,#31126)) ;
#13853 = EDGE_LOOP('',(#31127,#31128,#31129,#31130)) ;
#13854 = EDGE_LOOP('',(#31131,#31132,#31133,#31134)) ;
#13855 = EDGE_LOOP('',(#31135,#31136,#31137,#31138)) ;
#13856 = EDGE_LOOP('',(#31139,#31140,#31141,#31142)) ;
#13857 = EDGE_LOOP('',(#31143,#31144,#31145,#31146)) ;
#13858 = EDGE_LOOP('',(#31147,#31148,#31149)) ;
#13859 = EDGE_LOOP('',(#31150,#31151,#31152)) ;
#13860 = EDGE_LOOP('',(#31153,#31154,#31155)) ;
#13861 = EDGE_LOOP('',(#31156,#31157,#31158)) ;
#13862 = EDGE_LOOP('',(#31159,#31160,#31161)) ;
#13863 = EDGE_LOOP('',(#31162,#31163,#31164)) ;
#13864 = EDGE_LOOP('',(#31165,#31166,#31167)) ;
#13865 = EDGE_LOOP('',(#31168,#31169,#31170)) ;
#13866 = EDGE_LOOP('',(#31171,#31172,#31173,#31174)) ;
#13867 = EDGE_LOOP('',(#31175,#31176,#31177,#31178)) ;
#13868 = EDGE_LOOP('',(#31179,#31180,#31181,#31182)) ;
#13869 = EDGE_LOOP('',(#31183,#31184,#31185,#31186)) ;
#13870 = EDGE_LOOP('',(#31187,#31188,#31189,#31190)) ;
#13871 = EDGE_LOOP('',(#31191,#31192,#31193,#31194)) ;
#13872 = EDGE_LOOP('',(#31195,#31196,#31197,#31198)) ;
#13873 = EDGE_LOOP('',(#31199,#31200,#31201,#31202)) ;
#13874 = EDGE_LOOP('',(#31203,#31204,#31205,#31206)) ;
#13875 = EDGE_LOOP('',(#31207,#31208,#31209,#31210)) ;
#13876 = EDGE_LOOP('',(#31211,#31212,#31213,#31214)) ;
#13877 = EDGE_LOOP('',(#31215,#31216,#31217,#31218)) ;
#13878 = EDGE_LOOP('',(#31219,#31220,#31221,#31222,#31223,#31224,#31225,#31226,
#31227,#31228,#31229,#31230,#31231,#31232,#31233,#31234)) ;
#13879 = EDGE_LOOP('',(#31235,#31236,#31237)) ;
#13880 = EDGE_LOOP('',(#31238,#31239,#31240)) ;
#13881 = EDGE_LOOP('',(#31241,#31242,#31243)) ;
#13882 = EDGE_LOOP('',(#31244,#31245,#31246,#31247)) ;
#13883 = EDGE_LOOP('',(#31248,#31249,#31250)) ;
#13884 = EDGE_LOOP('',(#31251,#31252,#31253)) ;
#13885 = EDGE_LOOP('',(#31254,#31255,#31256,#31257)) ;
#13886 = EDGE_LOOP('',(#31258,#31259,#31260)) ;
#13887 = EDGE_LOOP('',(#31261,#31262,#31263)) ;
#13888 = EDGE_LOOP('',(#31264,#31265,#31266,#31267)) ;
#13889 = EDGE_LOOP('',(#31268,#31269,#31270)) ;
#13890 = EDGE_LOOP('',(#31271,#31272,#31273)) ;
#13891 = EDGE_LOOP('',(#31274,#31275,#31276,#31277)) ;
#13892 = EDGE_LOOP('',(#31278,#31279,#31280)) ;
#13893 = EDGE_LOOP('',(#31281,#31282,#31283)) ;
#13894 = EDGE_LOOP('',(#31284,#31285,#31286,#31287)) ;
#13895 = EDGE_LOOP('',(#31288,#31289,#31290)) ;
#13896 = EDGE_LOOP('',(#31291,#31292,#31293)) ;
#13897 = EDGE_LOOP('',(#31294,#31295,#31296,#31297)) ;
#13898 = EDGE_LOOP('',(#31298,#31299,#31300)) ;
#13899 = EDGE_LOOP('',(#31301,#31302,#31303)) ;
#13900 = EDGE_LOOP('',(#31304,#31305,#31306,#31307)) ;
#13901 = EDGE_LOOP('',(#31308,#31309,#31310)) ;
#13902 = EDGE_LOOP('',(#31311,#31312,#31313)) ;
#13903 = EDGE_LOOP('',(#31314,#31315,#31316,#31317,#31318)) ;
#13904 = EDGE_LOOP('',(#31319,#31320,#31321)) ;
#13905 = EDGE_LOOP('',(#31322,#31323,#31324)) ;
#13906 = EDGE_LOOP('',(#31325,#31326,#31327,#31328)) ;
#13907 = EDGE_LOOP('',(#31329,#31330,#31331)) ;
#13908 = EDGE_LOOP('',(#31332,#31333,#31334)) ;
#13909 = EDGE_LOOP('',(#31335,#31336,#31337,#31338)) ;
#13910 = EDGE_LOOP('',(#31339,#31340,#31341)) ;
#13911 = EDGE_LOOP('',(#31342,#31343,#31344)) ;
#13912 = EDGE_LOOP('',(#31345,#31346,#31347,#31348)) ;
#13913 = EDGE_LOOP('',(#31349,#31350,#31351)) ;
#13914 = EDGE_LOOP('',(#31352,#31353,#31354)) ;
#13915 = EDGE_LOOP('',(#31355,#31356,#31357,#31358)) ;
#13916 = EDGE_LOOP('',(#31359,#31360,#31361)) ;
#13917 = EDGE_LOOP('',(#31362,#31363,#31364)) ;
#13918 = EDGE_LOOP('',(#31365,#31366,#31367,#31368)) ;
#13919 = EDGE_LOOP('',(#31369,#31370,#31371)) ;
#13920 = EDGE_LOOP('',(#31372,#31373,#31374)) ;
#13921 = EDGE_LOOP('',(#31375,#31376,#31377,#31378)) ;
#13922 = EDGE_LOOP('',(#31379,#31380,#31381)) ;
#13923 = EDGE_LOOP('',(#31382,#31383,#31384)) ;
#13924 = EDGE_LOOP('',(#31385,#31386,#31387,#31388)) ;
#13925 = EDGE_LOOP('',(#31389,#31390,#31391)) ;
#13926 = EDGE_LOOP('',(#31392,#31393,#31394)) ;
#13927 = EDGE_LOOP('',(#31395,#31396,#31397,#31398)) ;
#13928 = EDGE_LOOP('',(#31399,#31400,#31401)) ;
#13929 = EDGE_LOOP('',(#31402,#31403,#31404)) ;
#13930 = EDGE_LOOP('',(#31405,#31406,#31407,#31408)) ;
#13931 = EDGE_LOOP('',(#31409,#31410,#31411)) ;
#13932 = EDGE_LOOP('',(#31412,#31413,#31414)) ;
#13933 = EDGE_LOOP('',(#31415,#31416,#31417,#31418)) ;
#13934 = EDGE_LOOP('',(#31419,#31420,#31421)) ;
#13935 = EDGE_LOOP('',(#31422,#31423,#31424)) ;
#13936 = EDGE_LOOP('',(#31425,#31426,#31427,#31428)) ;
#13937 = EDGE_LOOP('',(#31429,#31430,#31431)) ;
#13938 = EDGE_LOOP('',(#31432,#31433,#31434,#31435)) ;
#13939 = EDGE_LOOP('',(#31436,#31437,#31438,#31439)) ;
#13940 = EDGE_LOOP('',(#31440,#31441,#31442,#31443)) ;
#13941 = EDGE_LOOP('',(#31444,#31445,#31446,#31447)) ;
#13942 = EDGE_LOOP('',(#31448,#31449,#31450,#31451)) ;
#13943 = EDGE_LOOP('',(#31452,#31453,#31454,#31455)) ;
#13944 = EDGE_LOOP('',(#31456,#31457,#31458,#31459,#31460,#31461)) ;
#13945 = EDGE_LOOP('',(#31462,#31463,#31464,#31465)) ;
#13946 = EDGE_LOOP('',(#31466,#31467,#31468,#31469)) ;
#13947 = EDGE_LOOP('',(#31470,#31471,#31472,#31473)) ;
#13948 = EDGE_LOOP('',(#31474,#31475,#31476,#31477,#31478,#31479)) ;
#13949 = EDGE_LOOP('',(#31480,#31481,#31482,#31483)) ;
#13950 = EDGE_LOOP('',(#31484,#31485,#31486,#31487,#31488,#31489)) ;
#13951 = EDGE_LOOP('',(#31490,#31491,#31492,#31493)) ;
#13952 = EDGE_LOOP('',(#31494,#31495,#31496,#31497)) ;
#13953 = EDGE_LOOP('',(#31498,#31499,#31500,#31501)) ;
#13954 = EDGE_LOOP('',(#31502,#31503,#31504,#31505)) ;
#13955 = EDGE_LOOP('',(#31506,#31507,#31508,#31509)) ;
#13956 = EDGE_LOOP('',(#31510,#31511,#31512,#31513,#31514,#31515)) ;
#13957 = EDGE_LOOP('',(#31516,#31517,#31518,#31519)) ;
#13958 = EDGE_LOOP('',(#31520,#31521,#31522,#31523,#31524,#31525)) ;
#13959 = EDGE_LOOP('',(#31526,#31527,#31528,#31529)) ;
#13960 = EDGE_LOOP('',(#31530,#31531,#31532,#31533)) ;
#13961 = EDGE_LOOP('',(#31534,#31535,#31536,#31537)) ;
#13962 = EDGE_LOOP('',(#31538,#31539,#31540,#31541)) ;
#13963 = EDGE_LOOP('',(#31542,#31543,#31544,#31545)) ;
#13964 = EDGE_LOOP('',(#31546,#31547,#31548,#31549,#31550,#31551)) ;
#13965 = EDGE_LOOP('',(#31552,#31553,#31554,#31555)) ;
#13966 = EDGE_LOOP('',(#31556,#31557,#31558,#31559,#31560,#31561)) ;
#13967 = EDGE_LOOP('',(#31562,#31563,#31564,#31565)) ;
#13968 = EDGE_LOOP('',(#31566,#31567,#31568,#31569)) ;
#13969 = EDGE_LOOP('',(#31570,#31571,#31572,#31573)) ;
#13970 = EDGE_LOOP('',(#31574,#31575,#31576,#31577)) ;
#13971 = EDGE_LOOP('',(#31578,#31579,#31580,#31581)) ;
#13972 = EDGE_LOOP('',(#31582,#31583,#31584,#31585,#31586,#31587)) ;
#13973 = EDGE_LOOP('',(#31588,#31589,#31590,#31591)) ;
#13974 = EDGE_LOOP('',(#31592,#31593,#31594,#31595,#31596,#31597)) ;
#13975 = EDGE_LOOP('',(#31598,#31599,#31600,#31601)) ;
#13976 = EDGE_LOOP('',(#31602,#31603,#31604,#31605)) ;
#13977 = EDGE_LOOP('',(#31606,#31607,#31608,#31609)) ;
#13978 = EDGE_LOOP('',(#31610,#31611,#31612,#31613)) ;
#13979 = EDGE_LOOP('',(#31614,#31615,#31616,#31617)) ;
#13980 = EDGE_LOOP('',(#31618,#31619,#31620,#31621,#31622,#31623)) ;
#13981 = EDGE_LOOP('',(#31624,#31625,#31626,#31627)) ;
#13982 = EDGE_LOOP('',(#31628,#31629,#31630,#31631,#31632,#31633)) ;
#13983 = EDGE_LOOP('',(#31634,#31635,#31636,#31637)) ;
#13984 = EDGE_LOOP('',(#31638,#31639,#31640,#31641)) ;
#13985 = EDGE_LOOP('',(#31642,#31643,#31644,#31645)) ;
#13986 = EDGE_LOOP('',(#31646,#31647,#31648,#31649)) ;
#13987 = EDGE_LOOP('',(#31650,#31651,#31652,#31653)) ;
#13988 = EDGE_LOOP('',(#31654,#31655,#31656,#31657,#31658,#31659)) ;
#13989 = EDGE_LOOP('',(#31660,#31661,#31662,#31663)) ;
#13990 = EDGE_LOOP('',(#31664,#31665,#31666,#31667,#31668,#31669,#31670)) ;
#13991 = EDGE_LOOP('',(#31671,#31672,#31673,#31674)) ;
#13992 = EDGE_LOOP('',(#31675,#31676,#31677,#31678)) ;
#13993 = EDGE_LOOP('',(#31679,#31680,#31681,#31682)) ;
#13994 = EDGE_LOOP('',(#31683,#31684,#31685,#31686)) ;
#13995 = EDGE_LOOP('',(#31687,#31688,#31689,#31690)) ;
#13996 = EDGE_LOOP('',(#31691,#31692,#31693,#31694,#31695,#31696)) ;
#13997 = EDGE_LOOP('',(#31697,#31698,#31699,#31700)) ;
#13998 = EDGE_LOOP('',(#31701,#31702,#31703,#31704,#31705,#31706)) ;
#13999 = EDGE_LOOP('',(#31707,#31708,#31709,#31710)) ;
#14000 = EDGE_LOOP('',(#31711,#31712,#31713,#31714)) ;
#14001 = EDGE_LOOP('',(#31715,#31716,#31717,#31718)) ;
#14002 = EDGE_LOOP('',(#31719,#31720,#31721,#31722)) ;
#14003 = EDGE_LOOP('',(#31723,#31724,#31725,#31726)) ;
#14004 = EDGE_LOOP('',(#31727,#31728,#31729,#31730,#31731,#31732)) ;
#14005 = EDGE_LOOP('',(#31733,#31734,#31735,#31736)) ;
#14006 = EDGE_LOOP('',(#31737,#31738,#31739,#31740,#31741,#31742)) ;
#14007 = EDGE_LOOP('',(#31743,#31744,#31745,#31746)) ;
#14008 = EDGE_LOOP('',(#31747,#31748,#31749,#31750)) ;
#14009 = EDGE_LOOP('',(#31751,#31752,#31753,#31754)) ;
#14010 = EDGE_LOOP('',(#31755,#31756,#31757,#31758)) ;
#14011 = EDGE_LOOP('',(#31759,#31760,#31761,#31762)) ;
#14012 = EDGE_LOOP('',(#31763,#31764,#31765,#31766,#31767,#31768)) ;
#14013 = EDGE_LOOP('',(#31769,#31770,#31771,#31772)) ;
#14014 = EDGE_LOOP('',(#31773,#31774,#31775,#31776,#31777,#31778)) ;
#14015 = EDGE_LOOP('',(#31779,#31780,#31781,#31782)) ;
#14016 = EDGE_LOOP('',(#31783,#31784,#31785,#31786)) ;
#14017 = EDGE_LOOP('',(#31787,#31788,#31789,#31790)) ;
#14018 = EDGE_LOOP('',(#31791,#31792,#31793,#31794,#31795,#31796)) ;
#14019 = EDGE_LOOP('',(#31797,#31798,#31799,#31800,#31801,#31802)) ;
#14020 = EDGE_LOOP('',(#31803,#31804,#31805,#31806,#31807,#31808)) ;
#14021 = EDGE_LOOP('',(#31809,#31810,#31811,#31812,#31813,#31814)) ;
#14022 = EDGE_LOOP('',(#31815,#31816,#31817,#31818,#31819,#31820)) ;
#14023 = EDGE_LOOP('',(#31821,#31822,#31823,#31824,#31825,#31826)) ;
#14024 = EDGE_LOOP('',(#31827,#31828,#31829,#31830,#31831,#31832)) ;
#14025 = EDGE_LOOP('',(#31833,#31834,#31835,#31836,#31837,#31838)) ;
#14026 = EDGE_LOOP('',(#31839,#31840,#31841,#31842,#31843,#31844)) ;
#14027 = EDGE_LOOP('',(#31845,#31846,#31847,#31848,#31849,#31850)) ;
#14028 = EDGE_LOOP('',(#31851,#31852,#31853,#31854,#31855,#31856)) ;
#14029 = EDGE_LOOP('',(#31857,#31858,#31859,#31860,#31861,#31862)) ;
#14030 = EDGE_LOOP('',(#31863,#31864,#31865,#31866,#31867,#31868)) ;
#14031 = EDGE_LOOP('',(#31869,#31870,#31871,#31872,#31873,#31874)) ;
#14032 = EDGE_LOOP('',(#31875,#31876,#31877,#31878,#31879,#31880)) ;
#14033 = EDGE_LOOP('',(#31881,#31882,#31883,#31884,#31885,#31886)) ;
#14034 = EDGE_LOOP('',(#31887,#31888,#31889,#31890,#31891,#31892)) ;
#14035 = EDGE_LOOP('',(#31893,#31894,#31895,#31896,#31897,#31898)) ;
#14036 = EDGE_LOOP('',(#31899,#31900,#31901,#31902,#31903,#31904)) ;
#14037 = EDGE_LOOP('',(#31905,#31906,#31907,#31908,#31909,#31910)) ;
#14038 = EDGE_LOOP('',(#31911,#31912,#31913,#31914,#31915,#31916)) ;
#14039 = EDGE_LOOP('',(#31917,#31918,#31919,#31920,#31921,#31922,#31923,#31924,
#31925,#31926,#31927,#31928,#31929,#31930,#31931,#31932,#31933,#31934,#31935,
#31936,#31937,#31938,#31939,#31940,#31941,#31942,#31943,#31944,#31945,#31946,
#31947,#31948,#31949,#31950,#31951,#31952,#31953,#31954,#31955,#31956,#31957,
#31958,#31959,#31960)) ;
#14040 = EDGE_LOOP('',(#31961,#31962,#31963,#31964)) ;
#14041 = EDGE_LOOP('',(#31965)) ;
#14042 = EDGE_LOOP('',(#31966,#31967,#31968,#31969,#31970,#31971,#31972,#31973,
#31974,#31975,#31976,#31977,#31978,#31979,#31980,#31981,#31982,#31983,#31984,
#31985,#31986,#31987,#31988,#31989)) ;
#14043 = EDGE_LOOP('',(#31990,#31991,#31992,#31993)) ;
#14044 = EDGE_LOOP('',(#31994,#31995,#31996,#31997)) ;
#14045 = EDGE_LOOP('',(#31998,#31999,#32000,#32001)) ;
#14046 = EDGE_LOOP('',(#32002,#32003,#32004,#32005)) ;
#14047 = EDGE_LOOP('',(#32006,#32007,#32008,#32009)) ;
#14048 = EDGE_LOOP('',(#32010,#32011,#32012,#32013)) ;
#14049 = EDGE_LOOP('',(#32014,#32015,#32016,#32017)) ;
#14050 = EDGE_LOOP('',(#32018,#32019,#32020,#32021)) ;
#14051 = EDGE_LOOP('',(#32022,#32023,#32024,#32025)) ;
#14052 = EDGE_LOOP('',(#32026,#32027,#32028,#32029)) ;
#14053 = EDGE_LOOP('',(#32030,#32031,#32032,#32033)) ;
#14054 = EDGE_LOOP('',(#32034,#32035,#32036,#32037)) ;
#14055 = EDGE_LOOP('',(#32038,#32039,#32040,#32041)) ;
#14056 = EDGE_LOOP('',(#32042,#32043,#32044,#32045)) ;
#14057 = EDGE_LOOP('',(#32046,#32047,#32048,#32049)) ;
#14058 = EDGE_LOOP('',(#32050,#32051,#32052,#32053)) ;
#14059 = EDGE_LOOP('',(#32054,#32055,#32056,#32057)) ;
#14060 = EDGE_LOOP('',(#32058,#32059,#32060,#32061)) ;
#14061 = EDGE_LOOP('',(#32062,#32063,#32064,#32065)) ;
#14062 = EDGE_LOOP('',(#32066,#32067,#32068,#32069)) ;
#14063 = EDGE_LOOP('',(#32070,#32071,#32072,#32073)) ;
#14064 = EDGE_LOOP('',(#32074,#32075,#32076,#32077)) ;
#14065 = EDGE_LOOP('',(#32078,#32079,#32080,#32081)) ;
#14066 = EDGE_LOOP('',(#32082,#32083,#32084,#32085)) ;
#14067 = EDGE_LOOP('',(#32086,#32087,#32088,#32089)) ;
#14068 = EDGE_LOOP('',(#32090,#32091,#32092,#32093)) ;
#14069 = EDGE_LOOP('',(#32094,#32095,#32096,#32097)) ;
#14070 = EDGE_LOOP('',(#32098,#32099,#32100,#32101)) ;
#14071 = EDGE_LOOP('',(#32102,#32103,#32104,#32105)) ;
#14072 = EDGE_LOOP('',(#32106,#32107,#32108,#32109)) ;
#14073 = EDGE_LOOP('',(#32110,#32111,#32112,#32113)) ;
#14074 = EDGE_LOOP('',(#32114,#32115,#32116,#32117)) ;
#14075 = EDGE_LOOP('',(#32118,#32119)) ;
#14076 = EDGE_LOOP('',(#32120,#32121)) ;
#14077 = EDGE_LOOP('',(#32122,#32123)) ;
#14078 = EDGE_LOOP('',(#32124,#32125)) ;
#14079 = EDGE_LOOP('',(#32126,#32127)) ;
#14080 = EDGE_LOOP('',(#32128,#32129)) ;
#14081 = EDGE_LOOP('',(#32130,#32131)) ;
#14082 = EDGE_LOOP('',(#32132,#32133)) ;
#14083 = EDGE_LOOP('',(#32134,#32135)) ;
#14084 = EDGE_LOOP('',(#32136,#32137)) ;
#14085 = EDGE_LOOP('',(#32138,#32139)) ;
#14086 = EDGE_LOOP('',(#32140,#32141)) ;
#14087 = EDGE_LOOP('',(#32142,#32143)) ;
#14088 = EDGE_LOOP('',(#32144,#32145)) ;
#14089 = EDGE_LOOP('',(#32146,#32147)) ;
#14090 = EDGE_LOOP('',(#32148,#32149)) ;
#14091 = EDGE_LOOP('',(#32150,#32151)) ;
#14092 = EDGE_LOOP('',(#32152,#32153)) ;
#14093 = EDGE_LOOP('',(#32154,#32155)) ;
#14094 = EDGE_LOOP('',(#32156,#32157)) ;
#14095 = EDGE_LOOP('',(#32158,#32159,#32160,#32161)) ;
#14096 = EDGE_LOOP('',(#32162,#32163,#32164,#32165)) ;
#14097 = EDGE_LOOP('',(#32166,#32167,#32168,#32169)) ;
#14098 = EDGE_LOOP('',(#32170,#32171,#32172,#32173)) ;
#14099 = EDGE_LOOP('',(#32174,#32175,#32176,#32177)) ;
#14100 = EDGE_LOOP('',(#32178,#32179,#32180,#32181)) ;
#14101 = EDGE_LOOP('',(#32182,#32183,#32184,#32185)) ;
#14102 = EDGE_LOOP('',(#32186,#32187,#32188,#32189)) ;
#14103 = EDGE_LOOP('',(#32190,#32191,#32192,#32193)) ;
#14104 = EDGE_LOOP('',(#32194,#32195,#32196,#32197)) ;
#14105 = EDGE_LOOP('',(#32198,#32199,#32200,#32201,#32202,#32203)) ;
#14106 = EDGE_LOOP('',(#32204,#32205,#32206,#32207)) ;
#14107 = EDGE_LOOP('',(#32208,#32209,#32210,#32211,#32212)) ;
#14108 = EDGE_LOOP('',(#32213,#32214,#32215,#32216)) ;
#14109 = EDGE_LOOP('',(#32217,#32218,#32219,#32220)) ;
#14110 = EDGE_LOOP('',(#32221,#32222,#32223,#32224)) ;
#14111 = EDGE_LOOP('',(#32225,#32226,#32227,#32228)) ;
#14112 = EDGE_LOOP('',(#32229,#32230,#32231,#32232)) ;
#14113 = EDGE_LOOP('',(#32233,#32234,#32235,#32236)) ;
#14114 = EDGE_LOOP('',(#32237,#32238,#32239,#32240)) ;
#14115 = EDGE_LOOP('',(#32241,#32242,#32243,#32244)) ;
#14116 = EDGE_LOOP('',(#32245,#32246,#32247,#32248)) ;
#14117 = EDGE_LOOP('',(#32249,#32250,#32251,#32252)) ;
#14118 = EDGE_LOOP('',(#32253,#32254,#32255,#32256)) ;
#14119 = EDGE_LOOP('',(#32257,#32258,#32259,#32260)) ;
#14120 = EDGE_LOOP('',(#32261,#32262,#32263,#32264,#32265,#32266,#32267,#32268,
#32269,#32270,#32271,#32272,#32273,#32274,#32275,#32276,#32277,#32278,#32279,
#32280)) ;
#14121 = EDGE_LOOP('',(#32281,#32282,#32283,#32284,#32285,#32286,#32287,#32288)) ;
#14122 = EDGE_LOOP('',(#32289,#32290,#32291,#32292,#32293,#32294,#32295,#32296,
#32297,#32298,#32299)) ;
#14123 = EDGE_LOOP('',(#32300)) ;
#14124 = EDGE_LOOP('',(#32301,#32302,#32303,#32304,#32305,#32306,#32307,#32308)) ;
#14125 = EDGE_LOOP('',(#32309,#32310,#32311,#32312)) ;
#14126 = EDGE_LOOP('',(#32313,#32314,#32315,#32316)) ;
#14127 = EDGE_LOOP('',(#32317,#32318,#32319,#32320)) ;
#14128 = EDGE_LOOP('',(#32321,#32322,#32323,#32324)) ;
#14129 = EDGE_LOOP('',(#32325,#32326,#32327,#32328)) ;
#14130 = EDGE_LOOP('',(#32329,#32330,#32331,#32332)) ;
#14131 = EDGE_LOOP('',(#32333,#32334,#32335,#32336)) ;
#14132 = EDGE_LOOP('',(#32337,#32338,#32339,#32340)) ;
#14133 = EDGE_LOOP('',(#32341,#32342,#32343,#32344)) ;
#14134 = EDGE_LOOP('',(#32345,#32346,#32347,#32348)) ;
#14135 = EDGE_LOOP('',(#32349,#32350,#32351,#32352)) ;
#14136 = EDGE_LOOP('',(#32353,#32354,#32355,#32356)) ;
#14137 = EDGE_LOOP('',(#32357,#32358,#32359,#32360)) ;
#14138 = EDGE_LOOP('',(#32361,#32362,#32363,#32364)) ;
#14139 = EDGE_LOOP('',(#32365,#32366,#32367,#32368)) ;
#14140 = EDGE_LOOP('',(#32369,#32370,#32371,#32372)) ;
#14141 = EDGE_LOOP('',(#32373,#32374,#32375,#32376)) ;
#14142 = EDGE_LOOP('',(#32377,#32378,#32379,#32380)) ;
#14143 = EDGE_LOOP('',(#32381,#32382,#32383,#32384)) ;
#14144 = EDGE_LOOP('',(#32385,#32386,#32387,#32388)) ;
#14145 = EDGE_LOOP('',(#32389,#32390,#32391,#32392)) ;
#14146 = EDGE_LOOP('',(#32393,#32394,#32395,#32396)) ;
#14147 = EDGE_LOOP('',(#32397,#32398,#32399,#32400)) ;
#14148 = EDGE_LOOP('',(#32401,#32402,#32403,#32404)) ;
#14149 = EDGE_LOOP('',(#32405,#32406,#32407,#32408)) ;
#14150 = EDGE_LOOP('',(#32409,#32410,#32411,#32412)) ;
#14151 = EDGE_LOOP('',(#32413,#32414,#32415,#32416)) ;
#14152 = EDGE_LOOP('',(#32417,#32418,#32419,#32420)) ;
#14153 = EDGE_LOOP('',(#32421,#32422,#32423,#32424)) ;
#14154 = EDGE_LOOP('',(#32425,#32426,#32427,#32428)) ;
#14155 = EDGE_LOOP('',(#32429,#32430,#32431,#32432)) ;
#14156 = EDGE_LOOP('',(#32433,#32434,#32435,#32436)) ;
#14157 = EDGE_LOOP('',(#32437,#32438,#32439,#32440)) ;
#14158 = EDGE_LOOP('',(#32441,#32442,#32443,#32444)) ;
#14159 = EDGE_LOOP('',(#32445,#32446,#32447,#32448)) ;
#14160 = EDGE_LOOP('',(#32449,#32450,#32451,#32452)) ;
#14161 = EDGE_LOOP('',(#32453,#32454,#32455,#32456)) ;
#14162 = EDGE_LOOP('',(#32457,#32458,#32459,#32460,#32461,#32462,#32463)) ;
#14163 = EDGE_LOOP('',(#32464,#32465,#32466,#32467,#32468,#32469,#32470)) ;
#14164 = EDGE_LOOP('',(#32471,#32472,#32473,#32474)) ;
#14165 = EDGE_LOOP('',(#32475,#32476,#32477,#32478)) ;
#14166 = EDGE_LOOP('',(#32479,#32480,#32481,#32482)) ;
#14167 = EDGE_LOOP('',(#32483,#32484,#32485,#32486)) ;
#14168 = EDGE_LOOP('',(#32487,#32488,#32489,#32490)) ;
#14169 = EDGE_LOOP('',(#32491,#32492,#32493,#32494)) ;
#14170 = EDGE_LOOP('',(#32495,#32496,#32497,#32498)) ;
#14171 = EDGE_LOOP('',(#32499,#32500,#32501)) ;
#14172 = EDGE_LOOP('',(#32502,#32503,#32504,#32505)) ;
#14173 = EDGE_LOOP('',(#32506,#32507,#32508,#32509)) ;
#14174 = EDGE_LOOP('',(#32510,#32511,#32512,#32513)) ;
#14175 = EDGE_LOOP('',(#32514,#32515,#32516,#32517,#32518)) ;
#14176 = EDGE_LOOP('',(#32519,#32520,#32521,#32522)) ;
#14177 = EDGE_LOOP('',(#32523,#32524,#32525,#32526)) ;
#14178 = EDGE_LOOP('',(#32527,#32528,#32529,#32530)) ;
#14179 = EDGE_LOOP('',(#32531,#32532,#32533,#32534)) ;
#14180 = EDGE_LOOP('',(#32535,#32536,#32537,#32538)) ;
#14181 = EDGE_LOOP('',(#32539,#32540,#32541,#32542)) ;
#14182 = EDGE_LOOP('',(#32543,#32544,#32545,#32546)) ;
#14183 = EDGE_LOOP('',(#32547,#32548,#32549,#32550)) ;
#14184 = EDGE_LOOP('',(#32551,#32552,#32553,#32554)) ;
#14185 = EDGE_LOOP('',(#32555,#32556,#32557,#32558)) ;
#14186 = EDGE_LOOP('',(#32559,#32560,#32561,#32562)) ;
#14187 = EDGE_LOOP('',(#32563,#32564,#32565,#32566)) ;
#14188 = EDGE_LOOP('',(#32567,#32568,#32569,#32570)) ;
#14189 = EDGE_LOOP('',(#32571,#32572,#32573,#32574)) ;
#14190 = EDGE_LOOP('',(#32575,#32576,#32577)) ;
#14191 = EDGE_LOOP('',(#32578,#32579,#32580,#32581,#32582,#32583,#32584,#32585,
#32586,#32587)) ;
#14192 = EDGE_LOOP('',(#32588,#32589,#32590,#32591)) ;
#14193 = EDGE_LOOP('',(#32592,#32593,#32594,#32595)) ;
#14194 = EDGE_LOOP('',(#32596,#32597,#32598,#32599,#32600)) ;
#14195 = EDGE_LOOP('',(#32601,#32602,#32603,#32604)) ;
#14196 = EDGE_LOOP('',(#32605,#32606,#32607,#32608)) ;
#14197 = EDGE_LOOP('',(#32609,#32610,#32611,#32612)) ;
#14198 = EDGE_LOOP('',(#32613,#32614,#32615,#32616)) ;
#14199 = EDGE_LOOP('',(#32617,#32618,#32619,#32620)) ;
#14200 = EDGE_LOOP('',(#32621,#32622,#32623,#32624)) ;
#14201 = EDGE_LOOP('',(#32625,#32626,#32627,#32628)) ;
#14202 = EDGE_LOOP('',(#32629,#32630,#32631,#32632)) ;
#14203 = EDGE_LOOP('',(#32633,#32634,#32635,#32636)) ;
#14204 = EDGE_LOOP('',(#32637,#32638,#32639,#32640,#32641,#32642,#32643,#32644)) ;
#14205 = EDGE_LOOP('',(#32645,#32646,#32647,#32648)) ;
#14206 = EDGE_LOOP('',(#32649,#32650,#32651,#32652)) ;
#14207 = EDGE_LOOP('',(#32653,#32654,#32655,#32656)) ;
#14208 = EDGE_LOOP('',(#32657,#32658,#32659,#32660)) ;
#14209 = EDGE_LOOP('',(#32661,#32662,#32663,#32664)) ;
#14210 = EDGE_LOOP('',(#32665,#32666,#32667,#32668)) ;
#14211 = EDGE_LOOP('',(#32669,#32670,#32671,#32672)) ;
#14212 = EDGE_LOOP('',(#32673,#32674,#32675,#32676)) ;
#14213 = EDGE_LOOP('',(#32677,#32678,#32679,#32680)) ;
#14214 = EDGE_LOOP('',(#32681,#32682,#32683,#32684)) ;
#14215 = EDGE_LOOP('',(#32685,#32686,#32687,#32688,#32689,#32690,#32691,#32692)) ;
#14216 = EDGE_LOOP('',(#32693,#32694,#32695)) ;
#14217 = EDGE_LOOP('',(#32696,#32697,#32698,#32699)) ;
#14218 = EDGE_LOOP('',(#32700,#32701,#32702,#32703)) ;
#14219 = EDGE_LOOP('',(#32704,#32705,#32706,#32707,#32708)) ;
#14220 = EDGE_LOOP('',(#32709,#32710,#32711,#32712)) ;
#14221 = EDGE_LOOP('',(#32713,#32714,#32715,#32716)) ;
#14222 = EDGE_LOOP('',(#32717,#32718,#32719,#32720)) ;
#14223 = EDGE_LOOP('',(#32721,#32722,#32723,#32724)) ;
#14224 = EDGE_LOOP('',(#32725,#32726,#32727,#32728)) ;
#14225 = EDGE_LOOP('',(#32729,#32730,#32731,#32732)) ;
#14226 = EDGE_LOOP('',(#32733,#32734,#32735,#32736,#32737,#32738)) ;
#14227 = EDGE_LOOP('',(#32739,#32740,#32741,#32742,#32743,#32744)) ;
#14228 = EDGE_LOOP('',(#32745,#32746,#32747,#32748)) ;
#14229 = EDGE_LOOP('',(#32749,#32750,#32751,#32752)) ;
#14230 = EDGE_LOOP('',(#32753,#32754,#32755,#32756)) ;
#14231 = EDGE_LOOP('',(#32757,#32758,#32759,#32760)) ;
#14232 = EDGE_LOOP('',(#32761,#32762,#32763,#32764)) ;
#14233 = EDGE_LOOP('',(#32765,#32766,#32767,#32768)) ;
#14234 = EDGE_LOOP('',(#32769,#32770,#32771,#32772)) ;
#14235 = EDGE_LOOP('',(#32773,#32774,#32775,#32776)) ;
#14236 = EDGE_LOOP('',(#32777,#32778,#32779,#32780)) ;
#14237 = EDGE_LOOP('',(#32781,#32782,#32783,#32784)) ;
#14238 = EDGE_LOOP('',(#32785,#32786,#32787,#32788,#32789,#32790,#32791,#32792,
#32793,#32794,#32795)) ;
#14239 = EDGE_LOOP('',(#32796,#32797,#32798,#32799,#32800,#32801,#32802,#32803)) ;
#14240 = EDGE_LOOP('',(#32804,#32805,#32806,#32807,#32808,#32809,#32810,#32811,
#32812,#32813)) ;
#14241 = EDGE_LOOP('',(#32814,#32815,#32816,#32817)) ;
#14242 = EDGE_LOOP('',(#32818,#32819,#32820,#32821,#32822,#32823)) ;
#14243 = EDGE_LOOP('',(#32824,#32825,#32826,#32827)) ;
#14244 = EDGE_LOOP('',(#32828,#32829,#32830)) ;
#14245 = EDGE_LOOP('',(#32831,#32832,#32833,#32834)) ;
#14246 = EDGE_LOOP('',(#32835,#32836,#32837,#32838)) ;
#14247 = EDGE_LOOP('',(#32839,#32840,#32841,#32842)) ;
#14248 = EDGE_LOOP('',(#32843,#32844,#32845)) ;
#14249 = EDGE_LOOP('',(#32846,#32847,#32848,#32849)) ;
#14250 = EDGE_LOOP('',(#32850,#32851,#32852)) ;
#14251 = EDGE_LOOP('',(#32853,#32854,#32855,#32856)) ;
#14252 = EDGE_LOOP('',(#32857,#32858,#32859,#32860)) ;
#14253 = EDGE_LOOP('',(#32861,#32862,#32863,#32864)) ;
#14254 = EDGE_LOOP('',(#32865,#32866,#32867,#32868,#32869)) ;
#14255 = EDGE_LOOP('',(#32870,#32871,#32872,#32873)) ;
#14256 = EDGE_LOOP('',(#32874,#32875,#32876,#32877)) ;
#14257 = EDGE_LOOP('',(#32878,#32879,#32880,#32881)) ;
#14258 = EDGE_LOOP('',(#32882,#32883,#32884,#32885)) ;
#14259 = EDGE_LOOP('',(#32886,#32887,#32888,#32889)) ;
#14260 = EDGE_LOOP('',(#32890,#32891,#32892,#32893)) ;
#14261 = EDGE_LOOP('',(#32894,#32895,#32896,#32897)) ;
#14262 = EDGE_LOOP('',(#32898,#32899,#32900,#32901)) ;
#14263 = EDGE_LOOP('',(#32902,#32903,#32904,#32905)) ;
#14264 = EDGE_LOOP('',(#32906,#32907,#32908,#32909)) ;
#14265 = EDGE_LOOP('',(#32910,#32911,#32912,#32913)) ;
#14266 = EDGE_LOOP('',(#32914,#32915,#32916,#32917)) ;
#14267 = EDGE_LOOP('',(#32918,#32919,#32920,#32921)) ;
#14268 = EDGE_LOOP('',(#32922,#32923,#32924,#32925)) ;
#14269 = EDGE_LOOP('',(#32926,#32927,#32928,#32929)) ;
#14270 = EDGE_LOOP('',(#32930,#32931,#32932,#32933)) ;
#14271 = EDGE_LOOP('',(#32934,#32935,#32936,#32937)) ;
#14272 = EDGE_LOOP('',(#32938,#32939,#32940,#32941)) ;
#14273 = EDGE_LOOP('',(#32942,#32943,#32944,#32945,#32946)) ;
#14274 = EDGE_LOOP('',(#32947,#32948,#32949,#32950)) ;
#14275 = EDGE_LOOP('',(#32951,#32952,#32953,#32954,#32955)) ;
#14276 = EDGE_LOOP('',(#32956,#32957,#32958,#32959)) ;
#14277 = EDGE_LOOP('',(#32960,#32961,#32962,#32963)) ;
#14278 = EDGE_LOOP('',(#32964,#32965,#32966,#32967)) ;
#14279 = EDGE_LOOP('',(#32968,#32969,#32970,#32971)) ;
#14280 = EDGE_LOOP('',(#32972,#32973,#32974,#32975)) ;
#14281 = EDGE_LOOP('',(#32976,#32977,#32978,#32979)) ;
#14282 = EDGE_LOOP('',(#32980,#32981,#32982,#32983)) ;
#14283 = EDGE_LOOP('',(#32984,#32985,#32986,#32987)) ;
#14284 = EDGE_LOOP('',(#32988,#32989,#32990,#32991)) ;
#14285 = EDGE_LOOP('',(#32992,#32993,#32994,#32995)) ;
#14286 = EDGE_LOOP('',(#32996,#32997,#32998,#32999)) ;
#14287 = EDGE_LOOP('',(#33000,#33001,#33002,#33003)) ;
#14288 = EDGE_LOOP('',(#33004,#33005,#33006,#33007)) ;
#14289 = EDGE_LOOP('',(#33008,#33009,#33010,#33011)) ;
#14290 = EDGE_LOOP('',(#33012,#33013,#33014,#33015,#33016,#33017)) ;
#14291 = EDGE_LOOP('',(#33018,#33019,#33020,#33021,#33022)) ;
#14292 = EDGE_LOOP('',(#33023,#33024,#33025,#33026)) ;
#14293 = EDGE_LOOP('',(#33027,#33028,#33029,#33030)) ;
#14294 = EDGE_LOOP('',(#33031,#33032,#33033,#33034)) ;
#14295 = EDGE_LOOP('',(#33035,#33036,#33037,#33038)) ;
#14296 = EDGE_LOOP('',(#33039,#33040,#33041,#33042)) ;
#14297 = EDGE_LOOP('',(#33043,#33044,#33045,#33046)) ;
#14298 = EDGE_LOOP('',(#33047,#33048,#33049,#33050)) ;
#14299 = EDGE_LOOP('',(#33051,#33052,#33053,#33054)) ;
#14300 = EDGE_LOOP('',(#33055,#33056,#33057,#33058)) ;
#14301 = EDGE_LOOP('',(#33059,#33060,#33061,#33062)) ;
#14302 = EDGE_LOOP('',(#33063,#33064,#33065,#33066)) ;
#14303 = EDGE_LOOP('',(#33067,#33068,#33069,#33070,#33071,#33072,#33073,#33074,
#33075,#33076,#33077,#33078,#33079,#33080)) ;
#14304 = EDGE_LOOP('',(#33081,#33082,#33083)) ;
#14305 = EDGE_LOOP('',(#33084)) ;
#14306 = EDGE_LOOP('',(#33085,#33086,#33087,#33088,#33089,#33090)) ;
#14307 = EDGE_LOOP('',(#33091,#33092,#33093,#33094,#33095)) ;
#14308 = EDGE_LOOP('',(#33096,#33097,#33098,#33099)) ;
#14309 = EDGE_LOOP('',(#33100,#33101,#33102,#33103)) ;
#14310 = EDGE_LOOP('',(#33104,#33105,#33106,#33107)) ;
#14311 = EDGE_LOOP('',(#33108,#33109,#33110,#33111)) ;
#14312 = EDGE_LOOP('',(#33112,#33113,#33114,#33115)) ;
#14313 = EDGE_LOOP('',(#33116,#33117,#33118,#33119)) ;
#14314 = EDGE_LOOP('',(#33120,#33121,#33122,#33123)) ;
#14315 = EDGE_LOOP('',(#33124,#33125,#33126,#33127)) ;
#14316 = EDGE_LOOP('',(#33128,#33129,#33130,#33131)) ;
#14317 = EDGE_LOOP('',(#33132,#33133,#33134,#33135)) ;
#14318 = EDGE_LOOP('',(#33136,#33137,#33138,#33139)) ;
#14319 = EDGE_LOOP('',(#33140,#33141,#33142,#33143)) ;
#14320 = EDGE_LOOP('',(#33144,#33145,#33146,#33147)) ;
#14321 = EDGE_LOOP('',(#33148,#33149,#33150,#33151,#33152,#33153,#33154,#33155,
#33156,#33157,#33158,#33159,#33160,#33161,#33162,#33163,#33164,#33165,#33166)) ;
#14322 = EDGE_LOOP('',(#33167,#33168,#33169,#33170,#33171,#33172,#33173,#33174)) ;
#14323 = EDGE_LOOP('',(#33175,#33176,#33177,#33178)) ;
#14324 = EDGE_LOOP('',(#33179,#33180,#33181,#33182)) ;
#14325 = EDGE_LOOP('',(#33183,#33184,#33185,#33186)) ;
#14326 = EDGE_LOOP('',(#33187,#33188,#33189,#33190)) ;
#14327 = EDGE_LOOP('',(#33191,#33192,#33193,#33194)) ;
#14328 = EDGE_LOOP('',(#33195,#33196,#33197,#33198)) ;
#14329 = EDGE_LOOP('',(#33199,#33200,#33201,#33202)) ;
#14330 = EDGE_LOOP('',(#33203,#33204,#33205,#33206)) ;
#14331 = EDGE_LOOP('',(#33207,#33208,#33209,#33210)) ;
#14332 = EDGE_LOOP('',(#33211,#33212,#33213,#33214)) ;
#14333 = EDGE_LOOP('',(#33215,#33216,#33217,#33218)) ;
#14334 = EDGE_LOOP('',(#33219,#33220,#33221,#33222)) ;
#14335 = EDGE_LOOP('',(#33223,#33224,#33225,#33226)) ;
#14336 = EDGE_LOOP('',(#33227,#33228,#33229,#33230)) ;
#14337 = EDGE_LOOP('',(#33231,#33232,#33233,#33234)) ;
#14338 = EDGE_LOOP('',(#33235,#33236,#33237,#33238)) ;
#14339 = EDGE_LOOP('',(#33239,#33240,#33241,#33242)) ;
#14340 = EDGE_LOOP('',(#33243,#33244,#33245,#33246)) ;
#14341 = EDGE_LOOP('',(#33247,#33248,#33249,#33250)) ;
#14342 = EDGE_LOOP('',(#33251,#33252,#33253,#33254)) ;
#14343 = EDGE_LOOP('',(#33255,#33256,#33257,#33258)) ;
#14344 = EDGE_LOOP('',(#33259,#33260,#33261,#33262)) ;
#14345 = EDGE_LOOP('',(#33263,#33264,#33265,#33266)) ;
#14346 = EDGE_LOOP('',(#33267,#33268,#33269,#33270)) ;
#14347 = EDGE_LOOP('',(#33271,#33272,#33273,#33274)) ;
#14348 = EDGE_LOOP('',(#33275,#33276,#33277,#33278)) ;
#14349 = EDGE_LOOP('',(#33279,#33280,#33281,#33282)) ;
#14350 = EDGE_LOOP('',(#33283,#33284,#33285,#33286)) ;
#14351 = EDGE_LOOP('',(#33287,#33288,#33289,#33290)) ;
#14352 = EDGE_LOOP('',(#33291,#33292,#33293,#33294)) ;
#14353 = EDGE_LOOP('',(#33295,#33296,#33297,#33298)) ;
#14354 = EDGE_LOOP('',(#33299,#33300,#33301,#33302)) ;
#14355 = EDGE_LOOP('',(#33303,#33304,#33305,#33306)) ;
#14356 = EDGE_LOOP('',(#33307,#33308,#33309,#33310)) ;
#14357 = EDGE_LOOP('',(#33311,#33312,#33313,#33314)) ;
#14358 = EDGE_LOOP('',(#33315,#33316,#33317,#33318)) ;
#14359 = EDGE_LOOP('',(#33319,#33320,#33321,#33322)) ;
#14360 = EDGE_LOOP('',(#33323,#33324,#33325,#33326,#33327,#33328,#33329,#33330)) ;
#14361 = EDGE_LOOP('',(#33331,#33332,#33333,#33334)) ;
#14362 = EDGE_LOOP('',(#33335,#33336,#33337,#33338)) ;
#14363 = EDGE_LOOP('',(#33339,#33340,#33341,#33342)) ;
#14364 = EDGE_LOOP('',(#33343,#33344,#33345,#33346)) ;
#14365 = EDGE_LOOP('',(#33347,#33348,#33349,#33350)) ;
#14366 = EDGE_LOOP('',(#33351,#33352,#33353)) ;
#14367 = EDGE_LOOP('',(#33354,#33355,#33356,#33357)) ;
#14368 = EDGE_LOOP('',(#33358,#33359,#33360,#33361)) ;
#14369 = EDGE_LOOP('',(#33362,#33363,#33364,#33365)) ;
#14370 = EDGE_LOOP('',(#33366,#33367,#33368,#33369)) ;
#14371 = EDGE_LOOP('',(#33370,#33371,#33372,#33373)) ;
#14372 = EDGE_LOOP('',(#33374,#33375,#33376,#33377)) ;
#14373 = EDGE_LOOP('',(#33378,#33379,#33380,#33381)) ;
#14374 = EDGE_LOOP('',(#33382,#33383,#33384,#33385)) ;
#14375 = EDGE_LOOP('',(#33386,#33387,#33388,#33389)) ;
#14376 = EDGE_LOOP('',(#33390,#33391,#33392,#33393)) ;
#14377 = EDGE_LOOP('',(#33394,#33395,#33396,#33397)) ;
#14378 = EDGE_LOOP('',(#33398,#33399,#33400,#33401)) ;
#14379 = EDGE_LOOP('',(#33402,#33403,#33404)) ;
#14380 = EDGE_LOOP('',(#33405,#33406,#33407,#33408)) ;
#14381 = EDGE_LOOP('',(#33409,#33410,#33411,#33412)) ;
#14382 = EDGE_LOOP('',(#33413,#33414,#33415,#33416)) ;
#14383 = EDGE_LOOP('',(#33417,#33418,#33419,#33420)) ;
#14384 = EDGE_LOOP('',(#33421,#33422,#33423,#33424)) ;
#14385 = EDGE_LOOP('',(#33425,#33426,#33427,#33428)) ;
#14386 = EDGE_LOOP('',(#33429,#33430,#33431,#33432)) ;
#14387 = EDGE_LOOP('',(#33433,#33434,#33435,#33436)) ;
#14388 = EDGE_LOOP('',(#33437,#33438,#33439,#33440)) ;
#14389 = EDGE_LOOP('',(#33441,#33442,#33443,#33444)) ;
#14390 = EDGE_LOOP('',(#33445,#33446,#33447,#33448)) ;
#14391 = EDGE_LOOP('',(#33449,#33450,#33451,#33452)) ;
#14392 = EDGE_LOOP('',(#33453,#33454,#33455,#33456)) ;
#14393 = EDGE_LOOP('',(#33457,#33458,#33459,#33460)) ;
#14394 = EDGE_LOOP('',(#33461,#33462,#33463,#33464)) ;
#14395 = EDGE_LOOP('',(#33465,#33466,#33467,#33468)) ;
#14396 = EDGE_LOOP('',(#33469,#33470,#33471,#33472)) ;
#14397 = EDGE_LOOP('',(#33473,#33474,#33475,#33476)) ;
#14398 = EDGE_LOOP('',(#33477,#33478,#33479,#33480)) ;
#14399 = EDGE_LOOP('',(#33481,#33482,#33483,#33484)) ;
#14400 = EDGE_LOOP('',(#33485,#33486,#33487,#33488)) ;
#14401 = EDGE_LOOP('',(#33489,#33490,#33491,#33492)) ;
#14402 = EDGE_LOOP('',(#33493,#33494,#33495,#33496)) ;
#14403 = EDGE_LOOP('',(#33497,#33498,#33499,#33500)) ;
#14404 = EDGE_LOOP('',(#33501,#33502,#33503,#33504)) ;
#14405 = EDGE_LOOP('',(#33505,#33506,#33507,#33508)) ;
#14406 = EDGE_LOOP('',(#33509,#33510,#33511,#33512)) ;
#14407 = EDGE_LOOP('',(#33513,#33514,#33515,#33516,#33517,#33518,#33519,#33520,
#33521,#33522,#33523,#33524,#33525,#33526,#33527,#33528,#33529,#33530,#33531,
#33532,#33533,#33534,#33535,#33536,#33537,#33538,#33539,#33540,#33541,#33542,
#33543,#33544,#33545,#33546,#33547,#33548,#33549,#33550,#33551,#33552,#33553,
#33554,#33555,#33556,#33557,#33558,#33559,#33560,#33561)) ;
#14408 = EDGE_LOOP('',(#33562,#33563,#33564)) ;
#14409 = EDGE_LOOP('',(#33565,#33566,#33567)) ;
#14410 = EDGE_LOOP('',(#33568,#33569,#33570,#33571,#33572,#33573,#33574,#33575,
#33576,#33577,#33578,#33579,#33580,#33581)) ;
#14411 = EDGE_LOOP('',(#33582,#33583,#33584,#33585,#33586,#33587,#33588,#33589,
#33590,#33591,#33592,#33593,#33594,#33595,#33596,#33597)) ;
#14412 = EDGE_LOOP('',(#33598,#33599,#33600,#33601,#33602,#33603,#33604,#33605,
#33606,#33607,#33608,#33609,#33610,#33611)) ;
#14413 = EDGE_LOOP('',(#33612,#33613,#33614,#33615,#33616,#33617,#33618,#33619,
#33620,#33621,#33622,#33623,#33624,#33625)) ;
#14414 = EDGE_LOOP('',(#33626,#33627,#33628,#33629,#33630,#33631,#33632,#33633,
#33634,#33635,#33636,#33637,#33638,#33639)) ;
#14415 = EDGE_LOOP('',(#33640)) ;
#14416 = EDGE_LOOP('',(#33641,#33642,#33643,#33644,#33645,#33646,#33647,#33648,
#33649,#33650,#33651,#33652,#33653,#33654,#33655)) ;
#14417 = EDGE_LOOP('',(#33656)) ;
#14418 = EDGE_LOOP('',(#33657)) ;
#14419 = EDGE_LOOP('',(#33658,#33659,#33660,#33661,#33662,#33663,#33664,#33665,
#33666,#33667,#33668,#33669,#33670,#33671)) ;
#14420 = EDGE_LOOP('',(#33672)) ;
#14421 = EDGE_LOOP('',(#33673)) ;
#14422 = EDGE_LOOP('',(#33674,#33675,#33676,#33677,#33678,#33679,#33680,#33681)) ;
#14423 = EDGE_LOOP('',(#33682,#33683,#33684,#33685,#33686,#33687,#33688,#33689,
#33690,#33691,#33692,#33693,#33694,#33695)) ;
#14424 = EDGE_LOOP('',(#33696,#33697,#33698,#33699)) ;
#14425 = EDGE_LOOP('',(#33700,#33701,#33702,#33703,#33704,#33705,#33706,#33707,
#33708,#33709,#33710,#33711,#33712,#33713,#33714,#33715,#33716,#33717,#33718)) ;
#14426 = EDGE_LOOP('',(#33719,#33720,#33721,#33722)) ;
#14427 = EDGE_LOOP('',(#33723,#33724,#33725,#33726)) ;
#14428 = EDGE_LOOP('',(#33727,#33728,#33729,#33730)) ;
#14429 = EDGE_LOOP('',(#33731,#33732,#33733,#33734)) ;
#14430 = EDGE_LOOP('',(#33735,#33736,#33737,#33738)) ;
#14431 = EDGE_LOOP('',(#33739,#33740,#33741,#33742)) ;
#14432 = EDGE_LOOP('',(#33743,#33744,#33745,#33746)) ;
#14433 = EDGE_LOOP('',(#33747,#33748,#33749,#33750)) ;
#14434 = EDGE_LOOP('',(#33751,#33752,#33753,#33754)) ;
#14435 = EDGE_LOOP('',(#33755,#33756,#33757,#33758)) ;
#14436 = EDGE_LOOP('',(#33759,#33760,#33761,#33762)) ;
#14437 = EDGE_LOOP('',(#33763,#33764,#33765,#33766)) ;
#14438 = EDGE_LOOP('',(#33767,#33768,#33769,#33770)) ;
#14439 = EDGE_LOOP('',(#33771,#33772,#33773,#33774)) ;
#14440 = EDGE_LOOP('',(#33775,#33776,#33777,#33778)) ;
#14441 = EDGE_LOOP('',(#33779,#33780,#33781,#33782)) ;
#14442 = EDGE_LOOP('',(#33783,#33784,#33785,#33786)) ;
#14443 = EDGE_LOOP('',(#33787,#33788,#33789,#33790)) ;
#14444 = EDGE_LOOP('',(#33791,#33792,#33793,#33794)) ;
#14445 = EDGE_LOOP('',(#33795,#33796,#33797,#33798,#33799)) ;
#14446 = EDGE_LOOP('',(#33800)) ;
#14447 = EDGE_LOOP('',(#33801)) ;
#14448 = EDGE_LOOP('',(#33802,#33803,#33804,#33805,#33806)) ;
#14449 = EDGE_LOOP('',(#33807,#33808,#33809,#33810)) ;
#14450 = EDGE_LOOP('',(#33811,#33812,#33813,#33814)) ;
#14451 = EDGE_LOOP('',(#33815,#33816,#33817,#33818)) ;
#14452 = EDGE_LOOP('',(#33819,#33820,#33821,#33822,#33823,#33824,#33825,#33826,
#33827,#33828,#33829,#33830,#33831,#33832,#33833,#33834,#33835,#33836,#33837,
#33838,#33839,#33840,#33841,#33842,#33843,#33844,#33845,#33846,#33847,#33848,
#33849,#33850,#33851,#33852,#33853,#33854,#33855,#33856,#33857,#33858,#33859,
#33860,#33861,#33862,#33863,#33864,#33865,#33866,#33867,#33868,#33869,#33870,
#33871,#33872,#33873,#33874,#33875)) ;
#14453 = EDGE_LOOP('',(#33876)) ;
#14454 = EDGE_LOOP('',(#33877,#33878,#33879,#33880,#33881,#33882,#33883,#33884,
#33885,#33886,#33887,#33888,#33889,#33890)) ;
#14455 = EDGE_LOOP('',(#33891)) ;
#14456 = EDGE_LOOP('',(#33892)) ;
#14457 = EDGE_LOOP('',(#33893,#33894,#33895,#33896,#33897,#33898,#33899,#33900,
#33901,#33902,#33903,#33904,#33905,#33906,#33907,#33908)) ;
#14458 = EDGE_LOOP('',(#33909)) ;
#14459 = EDGE_LOOP('',(#33910,#33911,#33912,#33913,#33914,#33915,#33916,#33917,
#33918,#33919,#33920,#33921,#33922,#33923)) ;
#14460 = EDGE_LOOP('',(#33924,#33925,#33926,#33927,#33928,#33929,#33930,#33931)) ;
#14461 = EDGE_LOOP('',(#33932,#33933,#33934,#33935,#33936,#33937,#33938,#33939,
#33940,#33941,#33942,#33943,#33944,#33945)) ;
#14462 = EDGE_LOOP('',(#33946,#33947,#33948,#33949,#33950,#33951,#33952,#33953,
#33954,#33955,#33956,#33957,#33958,#33959)) ;
#14463 = EDGE_LOOP('',(#33960,#33961,#33962,#33963,#33964,#33965,#33966,#33967,
#33968,#33969,#33970,#33971,#33972,#33973)) ;
#14464 = EDGE_LOOP('',(#33974,#33975,#33976,#33977,#33978,#33979,#33980,#33981,
#33982,#33983,#33984,#33985,#33986,#33987)) ;
#14465 = EDGE_LOOP('',(#33988)) ;
#14466 = EDGE_LOOP('',(#33989)) ;
#14467 = EDGE_LOOP('',(#33990,#33991,#33992,#33993)) ;
#14468 = EDGE_LOOP('',(#33994,#33995,#33996,#33997)) ;
#14469 = EDGE_LOOP('',(#33998,#33999,#34000,#34001)) ;
#14470 = EDGE_LOOP('',(#34002,#34003,#34004,#34005)) ;
#14471 = EDGE_LOOP('',(#34006,#34007,#34008,#34009)) ;
#14472 = EDGE_LOOP('',(#34010,#34011,#34012,#34013)) ;
#14473 = EDGE_LOOP('',(#34014,#34015,#34016,#34017)) ;
#14474 = EDGE_LOOP('',(#34018,#34019,#34020,#34021)) ;
#14475 = EDGE_LOOP('',(#34022,#34023,#34024,#34025)) ;
#14476 = EDGE_LOOP('',(#34026,#34027,#34028,#34029)) ;
#14477 = EDGE_LOOP('',(#34030,#34031,#34032,#34033)) ;
#14478 = EDGE_LOOP('',(#34034,#34035,#34036,#34037)) ;
#14479 = EDGE_LOOP('',(#34038,#34039,#34040,#34041)) ;
#14480 = EDGE_LOOP('',(#34042,#34043,#34044,#34045,#34046,#34047,#34048,#34049)) ;
#14481 = EDGE_LOOP('',(#34050,#34051,#34052,#34053)) ;
#14482 = EDGE_LOOP('',(#34054,#34055,#34056,#34057)) ;
#14483 = EDGE_LOOP('',(#34058,#34059,#34060,#34061)) ;
#14484 = EDGE_LOOP('',(#34062,#34063,#34064,#34065)) ;
#14485 = EDGE_LOOP('',(#34066,#34067,#34068,#34069)) ;
#14486 = EDGE_LOOP('',(#34070,#34071,#34072,#34073)) ;
#14487 = EDGE_LOOP('',(#34074,#34075,#34076,#34077)) ;
#14488 = EDGE_LOOP('',(#34078,#34079,#34080,#34081)) ;
#14489 = EDGE_LOOP('',(#34082,#34083,#34084,#34085)) ;
#14490 = EDGE_LOOP('',(#34086,#34087,#34088,#34089,#34090,#34091,#34092,#34093)) ;
#14491 = EDGE_LOOP('',(#34094,#34095,#34096,#34097)) ;
#14492 = EDGE_LOOP('',(#34098,#34099,#34100,#34101)) ;
#14493 = EDGE_LOOP('',(#34102,#34103,#34104,#34105,#34106)) ;
#14494 = EDGE_LOOP('',(#34107,#34108,#34109,#34110,#34111)) ;
#14495 = EDGE_LOOP('',(#34112)) ;
#14496 = EDGE_LOOP('',(#34113)) ;
#14497 = EDGE_LOOP('',(#34114,#34115,#34116,#34117,#34118)) ;
#14498 = EDGE_LOOP('',(#34119,#34120,#34121,#34122,#34123)) ;
#14499 = EDGE_LOOP('',(#34124,#34125,#34126,#34127,#34128)) ;
#14500 = EDGE_LOOP('',(#34129,#34130,#34131,#34132,#34133,#34134)) ;
#14501 = EDGE_LOOP('',(#34135,#34136,#34137,#34138,#34139,#34140)) ;
#14502 = EDGE_LOOP('',(#34141)) ;
#14503 = EDGE_LOOP('',(#34142,#34143,#34144,#34145,#34146)) ;
#14504 = EDGE_LOOP('',(#34147,#34148,#34149,#34150,#34151,#34152)) ;
#14505 = EDGE_LOOP('',(#34153)) ;
#14506 = EDGE_LOOP('',(#34154,#34155,#34156,#34157,#34158)) ;
#14507 = EDGE_LOOP('',(#34159,#34160,#34161,#34162,#34163,#34164)) ;
#14508 = EDGE_LOOP('',(#34165,#34166,#34167,#34168,#34169,#34170)) ;
#14509 = EDGE_LOOP('',(#34171)) ;
#14510 = EDGE_LOOP('',(#34172,#34173,#34174,#34175,#34176)) ;
#14511 = EDGE_LOOP('',(#34177,#34178,#34179,#34180,#34181,#34182)) ;
#14512 = EDGE_LOOP('',(#34183)) ;
#14513 = EDGE_LOOP('',(#34184,#34185,#34186,#34187)) ;
#14514 = EDGE_LOOP('',(#34188,#34189,#34190,#34191)) ;
#14515 = EDGE_LOOP('',(#34192,#34193,#34194,#34195)) ;
#14516 = EDGE_LOOP('',(#34196,#34197,#34198,#34199)) ;
#14517 = EDGE_LOOP('',(#34200,#34201,#34202,#34203)) ;
#14518 = EDGE_LOOP('',(#34204,#34205,#34206,#34207,#34208,#34209,#34210,#34211,
#34212,#34213,#34214,#34215,#34216,#34217,#34218,#34219,#34220,#34221,#34222,
#34223,#34224,#34225,#34226,#34227)) ;
#14519 = EDGE_LOOP('',(#34228,#34229,#34230,#34231)) ;
#14520 = EDGE_LOOP('',(#34232,#34233,#34234,#34235,#34236,#34237,#34238,#34239,
#34240,#34241,#34242,#34243,#34244,#34245,#34246,#34247,#34248,#34249,#34250,
#34251,#34252,#34253,#34254,#34255,#34256,#34257,#34258,#34259,#34260,#34261,
#34262)) ;
#14521 = EDGE_LOOP('',(#34263,#34264,#34265,#34266)) ;
#14522 = EDGE_LOOP('',(#34267,#34268,#34269,#34270)) ;
#14523 = EDGE_LOOP('',(#34271,#34272,#34273,#34274)) ;
#14524 = EDGE_LOOP('',(#34275,#34276,#34277,#34278)) ;
#14525 = EDGE_LOOP('',(#34279,#34280,#34281,#34282)) ;
#14526 = EDGE_LOOP('',(#34283,#34284,#34285,#34286)) ;
#14527 = EDGE_LOOP('',(#34287,#34288,#34289,#34290)) ;
#14528 = EDGE_LOOP('',(#34291,#34292,#34293,#34294)) ;
#14529 = EDGE_LOOP('',(#34295,#34296,#34297,#34298,#34299)) ;
#14530 = EDGE_LOOP('',(#34300,#34301,#34302,#34303)) ;
#14531 = EDGE_LOOP('',(#34304,#34305,#34306,#34307)) ;
#14532 = EDGE_LOOP('',(#34308,#34309,#34310,#34311,#34312)) ;
#14533 = EDGE_LOOP('',(#34313,#34314,#34315,#34316)) ;
#14534 = EDGE_LOOP('',(#34317,#34318,#34319,#34320,#34321)) ;
#14535 = EDGE_LOOP('',(#34322,#34323,#34324)) ;
#14536 = EDGE_LOOP('',(#34325,#34326,#34327,#34328)) ;
#14537 = EDGE_LOOP('',(#34329,#34330,#34331,#34332)) ;
#14538 = EDGE_LOOP('',(#34333,#34334,#34335)) ;
#14539 = EDGE_LOOP('',(#34336,#34337,#34338,#34339)) ;
#14540 = EDGE_LOOP('',(#34340,#34341,#34342,#34343)) ;
#14541 = EDGE_LOOP('',(#34344,#34345,#34346,#34347)) ;
#14542 = EDGE_LOOP('',(#34348,#34349,#34350,#34351)) ;
#14543 = EDGE_LOOP('',(#34352,#34353,#34354,#34355)) ;
#14544 = EDGE_LOOP('',(#34356,#34357,#34358,#34359)) ;
#14545 = EDGE_LOOP('',(#34360,#34361,#34362,#34363)) ;
#14546 = EDGE_LOOP('',(#34364,#34365,#34366,#34367)) ;
#14547 = EDGE_LOOP('',(#34368,#34369,#34370,#34371)) ;
#14548 = EDGE_LOOP('',(#34372,#34373,#34374,#34375)) ;
#14549 = EDGE_LOOP('',(#34376,#34377,#34378)) ;
#14550 = EDGE_LOOP('',(#34379,#34380,#34381,#34382)) ;
#14551 = EDGE_LOOP('',(#34383,#34384,#34385,#34386)) ;
#14552 = EDGE_LOOP('',(#34387,#34388,#34389,#34390)) ;
#14553 = EDGE_LOOP('',(#34391,#34392,#34393,#34394)) ;
#14554 = EDGE_LOOP('',(#34395,#34396,#34397,#34398)) ;
#14555 = EDGE_LOOP('',(#34399,#34400,#34401,#34402)) ;
#14556 = EDGE_LOOP('',(#34403,#34404,#34405,#34406)) ;
#14557 = EDGE_LOOP('',(#34407,#34408,#34409)) ;
#14558 = EDGE_LOOP('',(#34410,#34411,#34412,#34413)) ;
#14559 = EDGE_LOOP('',(#34414,#34415,#34416,#34417,#34418)) ;
#14560 = EDGE_LOOP('',(#34419,#34420,#34421)) ;
#14561 = EDGE_LOOP('',(#34422,#34423,#34424,#34425)) ;
#14562 = EDGE_LOOP('',(#34426,#34427,#34428,#34429)) ;
#14563 = EDGE_LOOP('',(#34430,#34431,#34432,#34433,#34434)) ;
#14564 = EDGE_LOOP('',(#34435,#34436,#34437,#34438)) ;
#14565 = EDGE_LOOP('',(#34439,#34440,#34441,#34442)) ;
#14566 = EDGE_LOOP('',(#34443,#34444,#34445,#34446)) ;
#14567 = EDGE_LOOP('',(#34447,#34448,#34449,#34450)) ;
#14568 = EDGE_LOOP('',(#34451,#34452,#34453,#34454)) ;
#14569 = EDGE_LOOP('',(#34455,#34456,#34457,#34458)) ;
#14570 = EDGE_LOOP('',(#34459,#34460,#34461,#34462)) ;
#14571 = EDGE_LOOP('',(#34463,#34464,#34465,#34466)) ;
#14572 = EDGE_LOOP('',(#34467,#34468,#34469,#34470)) ;
#14573 = EDGE_LOOP('',(#34471,#34472,#34473,#34474)) ;
#14574 = EDGE_LOOP('',(#34475,#34476,#34477,#34478)) ;
#14575 = EDGE_LOOP('',(#34479,#34480,#34481,#34482)) ;
#14576 = EDGE_LOOP('',(#34483,#34484,#34485,#34486)) ;
#14577 = EDGE_LOOP('',(#34487,#34488,#34489,#34490)) ;
#14578 = EDGE_LOOP('',(#34491,#34492,#34493,#34494)) ;
#14579 = EDGE_LOOP('',(#34495,#34496,#34497,#34498)) ;
#14580 = EDGE_LOOP('',(#34499,#34500,#34501,#34502)) ;
#14581 = EDGE_LOOP('',(#34503,#34504,#34505,#34506)) ;
#14582 = EDGE_LOOP('',(#34507,#34508,#34509,#34510)) ;
#14583 = EDGE_LOOP('',(#34511,#34512,#34513,#34514)) ;
#14584 = EDGE_LOOP('',(#34515,#34516,#34517,#34518)) ;
#14585 = EDGE_LOOP('',(#34519,#34520,#34521,#34522)) ;
#14586 = EDGE_LOOP('',(#34523,#34524,#34525,#34526)) ;
#14587 = EDGE_LOOP('',(#34527,#34528,#34529,#34530)) ;
#14588 = EDGE_LOOP('',(#34531,#34532,#34533,#34534)) ;
#14589 = EDGE_LOOP('',(#34535,#34536,#34537,#34538)) ;
#14590 = EDGE_LOOP('',(#34539,#34540,#34541,#34542)) ;
#14591 = EDGE_LOOP('',(#34543,#34544,#34545,#34546)) ;
#14592 = EDGE_LOOP('',(#34547,#34548,#34549,#34550)) ;
#14593 = EDGE_LOOP('',(#34551,#34552,#34553,#34554)) ;
#14594 = EDGE_LOOP('',(#34555,#34556,#34557,#34558)) ;
#14595 = EDGE_LOOP('',(#34559,#34560,#34561,#34562)) ;
#14596 = EDGE_LOOP('',(#34563,#34564,#34565,#34566)) ;
#14597 = EDGE_LOOP('',(#34567,#34568,#34569)) ;
#14598 = EDGE_LOOP('',(#34570,#34571,#34572)) ;
#14599 = EDGE_LOOP('',(#34573,#34574,#34575,#34576)) ;
#14600 = EDGE_LOOP('',(#34577,#34578,#34579,#34580)) ;
#14601 = EDGE_LOOP('',(#34581,#34582,#34583,#34584)) ;
#14602 = EDGE_LOOP('',(#34585,#34586,#34587,#34588)) ;
#14603 = EDGE_LOOP('',(#34589,#34590,#34591,#34592)) ;
#14604 = EDGE_LOOP('',(#34593,#34594,#34595,#34596)) ;
#14605 = EDGE_LOOP('',(#34597,#34598,#34599,#34600)) ;
#14606 = EDGE_LOOP('',(#34601,#34602,#34603,#34604)) ;
#14607 = EDGE_LOOP('',(#34605,#34606,#34607,#34608)) ;
#14608 = EDGE_LOOP('',(#34609,#34610,#34611,#34612)) ;
#14609 = EDGE_LOOP('',(#34613,#34614,#34615,#34616)) ;
#14610 = EDGE_LOOP('',(#34617,#34618,#34619,#34620)) ;
#14611 = EDGE_LOOP('',(#34621,#34622,#34623,#34624)) ;
#14612 = EDGE_LOOP('',(#34625,#34626,#34627,#34628)) ;
#14613 = EDGE_LOOP('',(#34629,#34630,#34631,#34632)) ;
#14614 = EDGE_LOOP('',(#34633,#34634,#34635,#34636)) ;
#14615 = EDGE_LOOP('',(#34637,#34638,#34639,#34640)) ;
#14616 = EDGE_LOOP('',(#34641,#34642,#34643,#34644)) ;
#14617 = EDGE_LOOP('',(#34645,#34646,#34647,#34648)) ;
#14618 = EDGE_LOOP('',(#34649,#34650,#34651,#34652)) ;
#14619 = EDGE_LOOP('',(#34653,#34654,#34655,#34656)) ;
#14620 = EDGE_LOOP('',(#34657,#34658,#34659)) ;
#14621 = EDGE_LOOP('',(#34660,#34661,#34662,#34663)) ;
#14622 = EDGE_LOOP('',(#34664,#34665,#34666)) ;
#14623 = EDGE_LOOP('',(#34667,#34668,#34669,#34670)) ;
#14624 = EDGE_LOOP('',(#34671,#34672,#34673,#34674)) ;
#14625 = EDGE_LOOP('',(#34675,#34676,#34677,#34678)) ;
#14626 = EDGE_LOOP('',(#34679,#34680,#34681,#34682)) ;
#14627 = EDGE_LOOP('',(#34683,#34684,#34685,#34686)) ;
#14628 = EDGE_LOOP('',(#34687,#34688,#34689,#34690)) ;
#14629 = EDGE_LOOP('',(#34691,#34692,#34693,#34694)) ;
#14630 = EDGE_LOOP('',(#34695,#34696,#34697,#34698)) ;
#14631 = EDGE_LOOP('',(#34699,#34700,#34701,#34702)) ;
#14632 = EDGE_LOOP('',(#34703,#34704,#34705)) ;
#14633 = EDGE_LOOP('',(#34706,#34707,#34708,#34709)) ;
#14634 = EDGE_LOOP('',(#34710,#34711,#34712,#34713)) ;
#14635 = EDGE_LOOP('',(#34714,#34715,#34716)) ;
#14636 = EDGE_LOOP('',(#34717,#34718,#34719,#34720)) ;
#14637 = EDGE_LOOP('',(#34721,#34722,#34723,#34724)) ;
#14638 = EDGE_LOOP('',(#34725,#34726,#34727,#34728)) ;
#14639 = EDGE_LOOP('',(#34729,#34730,#34731,#34732)) ;
#14640 = EDGE_LOOP('',(#34733,#34734,#34735,#34736)) ;
#14641 = EDGE_LOOP('',(#34737,#34738,#34739,#34740)) ;
#14642 = EDGE_LOOP('',(#34741,#34742,#34743,#34744)) ;
#14643 = EDGE_LOOP('',(#34745,#34746,#34747,#34748)) ;
#14644 = EDGE_LOOP('',(#34749,#34750,#34751,#34752)) ;
#14645 = EDGE_LOOP('',(#34753,#34754,#34755,#34756)) ;
#14646 = EDGE_LOOP('',(#34757,#34758,#34759,#34760)) ;
#14647 = EDGE_LOOP('',(#34761,#34762,#34763,#34764)) ;
#14648 = EDGE_LOOP('',(#34765,#34766,#34767,#34768)) ;
#14649 = EDGE_LOOP('',(#34769,#34770,#34771,#34772)) ;
#14650 = EDGE_LOOP('',(#34773,#34774,#34775,#34776)) ;
#14651 = EDGE_LOOP('',(#34777,#34778,#34779,#34780)) ;
#14652 = EDGE_LOOP('',(#34781,#34782,#34783)) ;
#14653 = EDGE_LOOP('',(#34784,#34785,#34786,#34787)) ;
#14654 = EDGE_LOOP('',(#34788,#34789,#34790,#34791)) ;
#14655 = EDGE_LOOP('',(#34792,#34793,#34794)) ;
#14656 = EDGE_LOOP('',(#34795,#34796,#34797,#34798)) ;
#14657 = EDGE_LOOP('',(#34799,#34800,#34801,#34802)) ;
#14658 = EDGE_LOOP('',(#34803,#34804,#34805,#34806)) ;
#14659 = EDGE_LOOP('',(#34807,#34808,#34809,#34810)) ;
#14660 = EDGE_LOOP('',(#34811,#34812,#34813,#34814)) ;
#14661 = EDGE_LOOP('',(#34815,#34816,#34817,#34818)) ;
#14662 = EDGE_LOOP('',(#34819,#34820,#34821,#34822)) ;
#14663 = EDGE_LOOP('',(#34823,#34824,#34825,#34826)) ;
#14664 = EDGE_LOOP('',(#34827,#34828,#34829,#34830)) ;
#14665 = EDGE_LOOP('',(#34831,#34832,#34833,#34834)) ;
#14666 = EDGE_LOOP('',(#34835,#34836,#34837,#34838)) ;
#14667 = EDGE_LOOP('',(#34839,#34840,#34841,#34842)) ;
#14668 = EDGE_LOOP('',(#34843,#34844,#34845)) ;
#14669 = EDGE_LOOP('',(#34846,#34847,#34848,#34849)) ;
#14670 = EDGE_LOOP('',(#34850,#34851,#34852,#34853)) ;
#14671 = EDGE_LOOP('',(#34854,#34855,#34856,#34857)) ;
#14672 = EDGE_LOOP('',(#34858,#34859,#34860,#34861)) ;
#14673 = EDGE_LOOP('',(#34862,#34863,#34864,#34865)) ;
#14674 = EDGE_LOOP('',(#34866,#34867,#34868,#34869)) ;
#14675 = EDGE_LOOP('',(#34870,#34871,#34872,#34873)) ;
#14676 = EDGE_LOOP('',(#34874,#34875,#34876,#34877)) ;
#14677 = EDGE_LOOP('',(#34878,#34879,#34880,#34881)) ;
#14678 = EDGE_LOOP('',(#34882,#34883,#34884,#34885)) ;
#14679 = EDGE_LOOP('',(#34886,#34887,#34888,#34889)) ;
#14680 = EDGE_LOOP('',(#34890,#34891,#34892,#34893)) ;
#14681 = EDGE_LOOP('',(#34894,#34895,#34896,#34897)) ;
#14682 = EDGE_LOOP('',(#34898,#34899,#34900,#34901)) ;
#14683 = EDGE_LOOP('',(#34902,#34903,#34904,#34905)) ;
#14684 = EDGE_LOOP('',(#34906,#34907,#34908,#34909)) ;
#14685 = EDGE_LOOP('',(#34910,#34911,#34912,#34913)) ;
#14686 = EDGE_LOOP('',(#34914,#34915,#34916,#34917)) ;
#14687 = EDGE_LOOP('',(#34918,#34919,#34920,#34921)) ;
#14688 = EDGE_LOOP('',(#34922,#34923,#34924,#34925)) ;
#14689 = EDGE_LOOP('',(#34926,#34927,#34928,#34929)) ;
#14690 = EDGE_LOOP('',(#34930,#34931,#34932,#34933)) ;
#14691 = EDGE_LOOP('',(#34934,#34935,#34936,#34937)) ;
#14692 = EDGE_LOOP('',(#34938,#34939,#34940,#34941)) ;
#14693 = EDGE_LOOP('',(#34942,#34943,#34944,#34945)) ;
#14694 = EDGE_LOOP('',(#34946,#34947,#34948,#34949)) ;
#14695 = EDGE_LOOP('',(#34950,#34951,#34952,#34953)) ;
#14696 = EDGE_LOOP('',(#34954,#34955,#34956,#34957)) ;
#14697 = EDGE_LOOP('',(#34958,#34959,#34960,#34961)) ;
#14698 = EDGE_LOOP('',(#34962,#34963,#34964,#34965)) ;
#14699 = EDGE_LOOP('',(#34966,#34967,#34968,#34969)) ;
#14700 = EDGE_LOOP('',(#34970,#34971,#34972,#34973)) ;
#14701 = EDGE_LOOP('',(#34974,#34975,#34976,#34977)) ;
#14702 = EDGE_LOOP('',(#34978,#34979,#34980,#34981)) ;
#14703 = EDGE_LOOP('',(#34982,#34983,#34984,#34985)) ;
#14704 = EDGE_LOOP('',(#34986,#34987,#34988,#34989)) ;
#14705 = EDGE_LOOP('',(#34990,#34991,#34992,#34993)) ;
#14706 = EDGE_LOOP('',(#34994,#34995,#34996,#34997)) ;
#14707 = EDGE_LOOP('',(#34998,#34999,#35000,#35001)) ;
#14708 = EDGE_LOOP('',(#35002,#35003,#35004,#35005)) ;
#14709 = EDGE_LOOP('',(#35006,#35007,#35008,#35009)) ;
#14710 = EDGE_LOOP('',(#35010,#35011,#35012,#35013)) ;
#14711 = EDGE_LOOP('',(#35014,#35015,#35016,#35017)) ;
#14712 = EDGE_LOOP('',(#35018,#35019,#35020,#35021)) ;
#14713 = EDGE_LOOP('',(#35022,#35023,#35024,#35025)) ;
#14714 = EDGE_LOOP('',(#35026,#35027,#35028)) ;
#14715 = EDGE_LOOP('',(#35029,#35030,#35031)) ;
#14716 = EDGE_LOOP('',(#35032,#35033,#35034,#35035)) ;
#14717 = EDGE_LOOP('',(#35036,#35037,#35038,#35039)) ;
#14718 = EDGE_LOOP('',(#35040,#35041,#35042,#35043)) ;
#14719 = EDGE_LOOP('',(#35044,#35045,#35046,#35047)) ;
#14720 = EDGE_LOOP('',(#35048,#35049,#35050,#35051)) ;
#14721 = EDGE_LOOP('',(#35052,#35053,#35054,#35055)) ;
#14722 = EDGE_LOOP('',(#35056,#35057,#35058,#35059)) ;
#14723 = EDGE_LOOP('',(#35060,#35061,#35062,#35063)) ;
#14724 = EDGE_LOOP('',(#35064,#35065,#35066,#35067)) ;
#14725 = EDGE_LOOP('',(#35068,#35069,#35070,#35071)) ;
#14726 = EDGE_LOOP('',(#35072,#35073,#35074,#35075)) ;
#14727 = EDGE_LOOP('',(#35076,#35077,#35078,#35079)) ;
#14728 = EDGE_LOOP('',(#35080,#35081,#35082,#35083)) ;
#14729 = EDGE_LOOP('',(#35084,#35085,#35086,#35087)) ;
#14730 = EDGE_LOOP('',(#35088,#35089,#35090,#35091)) ;
#14731 = EDGE_LOOP('',(#35092,#35093,#35094,#35095)) ;
#14732 = EDGE_LOOP('',(#35096,#35097,#35098,#35099)) ;
#14733 = EDGE_LOOP('',(#35100,#35101,#35102,#35103)) ;
#14734 = EDGE_LOOP('',(#35104,#35105,#35106,#35107)) ;
#14735 = EDGE_LOOP('',(#35108,#35109,#35110,#35111)) ;
#14736 = EDGE_LOOP('',(#35112,#35113,#35114,#35115)) ;
#14737 = EDGE_LOOP('',(#35116,#35117,#35118,#35119)) ;
#14738 = EDGE_LOOP('',(#35120,#35121,#35122)) ;
#14739 = EDGE_LOOP('',(#35123,#35124,#35125,#35126)) ;
#14740 = EDGE_LOOP('',(#35127,#35128,#35129,#35130)) ;
#14741 = EDGE_LOOP('',(#35131,#35132,#35133,#35134)) ;
#14742 = EDGE_LOOP('',(#35135,#35136,#35137,#35138)) ;
#14743 = EDGE_LOOP('',(#35139,#35140,#35141)) ;
#14744 = EDGE_LOOP('',(#35142,#35143,#35144,#35145)) ;
#14745 = EDGE_LOOP('',(#35146,#35147,#35148,#35149)) ;
#14746 = EDGE_LOOP('',(#35150,#35151,#35152,#35153)) ;
#14747 = EDGE_LOOP('',(#35154,#35155,#35156,#35157)) ;
#14748 = EDGE_LOOP('',(#35158,#35159,#35160,#35161)) ;
#14749 = EDGE_LOOP('',(#35162,#35163,#35164,#35165)) ;
#14750 = EDGE_LOOP('',(#35166,#35167,#35168,#35169)) ;
#14751 = EDGE_LOOP('',(#35170,#35171,#35172,#35173)) ;
#14752 = EDGE_LOOP('',(#35174,#35175,#35176,#35177)) ;
#14753 = EDGE_LOOP('',(#35178,#35179,#35180,#35181)) ;
#14754 = EDGE_LOOP('',(#35182,#35183,#35184,#35185)) ;
#14755 = EDGE_LOOP('',(#35186,#35187,#35188,#35189)) ;
#14756 = EDGE_LOOP('',(#35190,#35191,#35192,#35193)) ;
#14757 = EDGE_LOOP('',(#35194,#35195,#35196,#35197)) ;
#14758 = EDGE_LOOP('',(#35198,#35199,#35200,#35201)) ;
#14759 = EDGE_LOOP('',(#35202,#35203,#35204,#35205)) ;
#14760 = EDGE_LOOP('',(#35206,#35207,#35208,#35209)) ;
#14761 = EDGE_LOOP('',(#35210,#35211,#35212,#35213)) ;
#14762 = EDGE_LOOP('',(#35214,#35215,#35216,#35217)) ;
#14763 = EDGE_LOOP('',(#35218,#35219,#35220,#35221)) ;
#14764 = EDGE_LOOP('',(#35222,#35223,#35224,#35225)) ;
#14765 = EDGE_LOOP('',(#35226,#35227,#35228,#35229)) ;
#14766 = EDGE_LOOP('',(#35230,#35231,#35232,#35233)) ;
#14767 = EDGE_LOOP('',(#35234,#35235,#35236,#35237)) ;
#14768 = EDGE_LOOP('',(#35238,#35239,#35240,#35241)) ;
#14769 = EDGE_LOOP('',(#35242,#35243,#35244,#35245)) ;
#14770 = EDGE_LOOP('',(#35246,#35247,#35248,#35249)) ;
#14771 = EDGE_LOOP('',(#35250,#35251,#35252,#35253)) ;
#14772 = EDGE_LOOP('',(#35254,#35255,#35256,#35257)) ;
#14773 = EDGE_LOOP('',(#35258,#35259,#35260,#35261)) ;
#14774 = EDGE_LOOP('',(#35262,#35263,#35264,#35265)) ;
#14775 = EDGE_LOOP('',(#35266,#35267,#35268,#35269)) ;
#14776 = EDGE_LOOP('',(#35270,#35271,#35272,#35273)) ;
#14777 = EDGE_LOOP('',(#35274,#35275,#35276,#35277)) ;
#14778 = EDGE_LOOP('',(#35278,#35279,#35280,#35281)) ;
#14779 = EDGE_LOOP('',(#35282,#35283,#35284,#35285)) ;
#14780 = EDGE_LOOP('',(#35286,#35287,#35288,#35289)) ;
#14781 = EDGE_LOOP('',(#35290,#35291,#35292,#35293)) ;
#14782 = EDGE_LOOP('',(#35294,#35295,#35296,#35297)) ;
#14783 = EDGE_LOOP('',(#35298,#35299,#35300,#35301)) ;
#14784 = EDGE_LOOP('',(#35302,#35303,#35304,#35305)) ;
#14785 = EDGE_LOOP('',(#35306,#35307,#35308,#35309)) ;
#14786 = EDGE_LOOP('',(#35310,#35311,#35312,#35313)) ;
#14787 = EDGE_LOOP('',(#35314,#35315,#35316,#35317)) ;
#14788 = EDGE_LOOP('',(#35318,#35319,#35320,#35321)) ;
#14789 = EDGE_LOOP('',(#35322,#35323,#35324,#35325)) ;
#14790 = EDGE_LOOP('',(#35326,#35327,#35328,#35329)) ;
#14791 = EDGE_LOOP('',(#35330,#35331,#35332,#35333)) ;
#14792 = EDGE_LOOP('',(#35334,#35335,#35336,#35337)) ;
#14793 = EDGE_LOOP('',(#35338,#35339,#35340,#35341)) ;
#14794 = EDGE_LOOP('',(#35342,#35343,#35344,#35345)) ;
#14795 = EDGE_LOOP('',(#35346,#35347,#35348,#35349)) ;
#14796 = EDGE_LOOP('',(#35350,#35351,#35352,#35353)) ;
#14797 = EDGE_LOOP('',(#35354,#35355,#35356,#35357)) ;
#14798 = EDGE_LOOP('',(#35358,#35359,#35360,#35361)) ;
#14799 = EDGE_LOOP('',(#35362,#35363,#35364,#35365)) ;
#14800 = EDGE_LOOP('',(#35366,#35367,#35368,#35369)) ;
#14801 = EDGE_LOOP('',(#35370,#35371,#35372,#35373)) ;
#14802 = EDGE_LOOP('',(#35374,#35375,#35376,#35377)) ;
#14803 = EDGE_LOOP('',(#35378,#35379,#35380,#35381,#35382)) ;
#14804 = EDGE_LOOP('',(#35383,#35384,#35385,#35386)) ;
#14805 = EDGE_LOOP('',(#35387,#35388,#35389,#35390)) ;
#14806 = EDGE_LOOP('',(#35391,#35392,#35393,#35394)) ;
#14807 = EDGE_LOOP('',(#35395,#35396,#35397,#35398)) ;
#14808 = EDGE_LOOP('',(#35399,#35400,#35401,#35402)) ;
#14809 = EDGE_LOOP('',(#35403,#35404,#35405,#35406)) ;
#14810 = EDGE_LOOP('',(#35407,#35408,#35409,#35410)) ;
#14811 = EDGE_LOOP('',(#35411,#35412,#35413,#35414)) ;
#14812 = EDGE_LOOP('',(#35415,#35416,#35417,#35418)) ;
#14813 = EDGE_LOOP('',(#35419,#35420,#35421,#35422)) ;
#14814 = EDGE_LOOP('',(#35423,#35424,#35425,#35426)) ;
#14815 = EDGE_LOOP('',(#35427,#35428,#35429,#35430)) ;
#14816 = EDGE_LOOP('',(#35431,#35432,#35433,#35434)) ;
#14817 = EDGE_LOOP('',(#35435,#35436,#35437,#35438)) ;
#14818 = EDGE_LOOP('',(#35439,#35440,#35441,#35442)) ;
#14819 = EDGE_LOOP('',(#35443,#35444,#35445,#35446)) ;
#14820 = EDGE_LOOP('',(#35447,#35448,#35449,#35450)) ;
#14821 = EDGE_LOOP('',(#35451,#35452,#35453,#35454)) ;
#14822 = EDGE_LOOP('',(#35455,#35456,#35457,#35458)) ;
#14823 = EDGE_LOOP('',(#35459,#35460,#35461,#35462)) ;
#14824 = EDGE_LOOP('',(#35463,#35464,#35465,#35466)) ;
#14825 = EDGE_LOOP('',(#35467,#35468,#35469,#35470)) ;
#14826 = EDGE_LOOP('',(#35471,#35472,#35473,#35474)) ;
#14827 = EDGE_LOOP('',(#35475,#35476,#35477,#35478)) ;
#14828 = EDGE_LOOP('',(#35479,#35480,#35481,#35482)) ;
#14829 = EDGE_LOOP('',(#35483,#35484,#35485,#35486)) ;
#14830 = EDGE_LOOP('',(#35487,#35488,#35489)) ;
#14831 = EDGE_LOOP('',(#35490,#35491,#35492,#35493)) ;
#14832 = EDGE_LOOP('',(#35494,#35495,#35496,#35497)) ;
#14833 = EDGE_LOOP('',(#35498,#35499,#35500,#35501,#35502,#35503)) ;
#14834 = EDGE_LOOP('',(#35504,#35505,#35506,#35507)) ;
#14835 = EDGE_LOOP('',(#35508,#35509,#35510,#35511)) ;
#14836 = EDGE_LOOP('',(#35512,#35513,#35514)) ;
#14837 = EDGE_LOOP('',(#35515,#35516,#35517,#35518,#35519)) ;
#14838 = EDGE_LOOP('',(#35520,#35521,#35522,#35523)) ;
#14839 = EDGE_LOOP('',(#35524,#35525,#35526,#35527)) ;
#14840 = EDGE_LOOP('',(#35528,#35529,#35530,#35531)) ;
#14841 = EDGE_LOOP('',(#35532,#35533,#35534,#35535)) ;
#14842 = EDGE_LOOP('',(#35536,#35537,#35538,#35539)) ;
#14843 = EDGE_LOOP('',(#35540,#35541,#35542,#35543)) ;
#14844 = EDGE_LOOP('',(#35544,#35545,#35546,#35547)) ;
#14845 = EDGE_LOOP('',(#35548,#35549,#35550,#35551)) ;
#14846 = EDGE_LOOP('',(#35552,#35553,#35554,#35555)) ;
#14847 = EDGE_LOOP('',(#35556,#35557,#35558,#35559)) ;
#14848 = EDGE_LOOP('',(#35560,#35561,#35562,#35563)) ;
#14849 = EDGE_LOOP('',(#35564,#35565,#35566,#35567)) ;
#14850 = EDGE_LOOP('',(#35568,#35569,#35570,#35571)) ;
#14851 = EDGE_LOOP('',(#35572,#35573,#35574,#35575)) ;
#14852 = EDGE_LOOP('',(#35576,#35577,#35578,#35579)) ;
#14853 = EDGE_LOOP('',(#35580,#35581,#35582,#35583)) ;
#14854 = EDGE_LOOP('',(#35584,#35585,#35586,#35587)) ;
#14855 = EDGE_LOOP('',(#35588,#35589,#35590,#35591)) ;
#14856 = EDGE_LOOP('',(#35592,#35593,#35594,#35595)) ;
#14857 = EDGE_LOOP('',(#35596,#35597,#35598,#35599)) ;
#14858 = EDGE_LOOP('',(#35600,#35601,#35602,#35603)) ;
#14859 = EDGE_LOOP('',(#35604,#35605,#35606)) ;
#14860 = EDGE_LOOP('',(#35607,#35608,#35609,#35610)) ;
#14861 = EDGE_LOOP('',(#35611,#35612,#35613,#35614)) ;
#14862 = EDGE_LOOP('',(#35615,#35616,#35617,#35618)) ;
#14863 = EDGE_LOOP('',(#35619,#35620,#35621,#35622)) ;
#14864 = EDGE_LOOP('',(#35623,#35624,#35625,#35626)) ;
#14865 = EDGE_LOOP('',(#35627,#35628,#35629,#35630)) ;
#14866 = EDGE_LOOP('',(#35631,#35632,#35633,#35634)) ;
#14867 = EDGE_LOOP('',(#35635,#35636,#35637,#35638)) ;
#14868 = EDGE_LOOP('',(#35639,#35640,#35641,#35642)) ;
#14869 = EDGE_LOOP('',(#35643,#35644,#35645,#35646)) ;
#14870 = EDGE_LOOP('',(#35647,#35648,#35649)) ;
#14871 = EDGE_LOOP('',(#35650,#35651,#35652,#35653)) ;
#14872 = EDGE_LOOP('',(#35654,#35655,#35656,#35657)) ;
#14873 = EDGE_LOOP('',(#35658,#35659,#35660,#35661)) ;
#14874 = EDGE_LOOP('',(#35662,#35663,#35664,#35665)) ;
#14875 = EDGE_LOOP('',(#35666,#35667,#35668,#35669)) ;
#14876 = EDGE_LOOP('',(#35670,#35671,#35672,#35673)) ;
#14877 = EDGE_LOOP('',(#35674,#35675,#35676,#35677)) ;
#14878 = EDGE_LOOP('',(#35678,#35679,#35680,#35681)) ;
#14879 = EDGE_LOOP('',(#35682,#35683,#35684,#35685)) ;
#14880 = EDGE_LOOP('',(#35686,#35687,#35688,#35689)) ;
#14881 = EDGE_LOOP('',(#35690,#35691,#35692,#35693)) ;
#14882 = EDGE_LOOP('',(#35694,#35695,#35696,#35697)) ;
#14883 = EDGE_LOOP('',(#35698,#35699,#35700)) ;
#14884 = EDGE_LOOP('',(#35701,#35702,#35703,#35704,#35705)) ;
#14885 = EDGE_LOOP('',(#35706,#35707,#35708,#35709)) ;
#14886 = EDGE_LOOP('',(#35710,#35711,#35712,#35713)) ;
#14887 = EDGE_LOOP('',(#35714,#35715,#35716)) ;
#14888 = EDGE_LOOP('',(#35717,#35718,#35719,#35720)) ;
#14889 = EDGE_LOOP('',(#35721,#35722,#35723,#35724)) ;
#14890 = EDGE_LOOP('',(#35725,#35726,#35727,#35728)) ;
#14891 = EDGE_LOOP('',(#35729,#35730,#35731,#35732)) ;
#14892 = EDGE_LOOP('',(#35733,#35734,#35735,#35736)) ;
#14893 = EDGE_LOOP('',(#35737,#35738,#35739,#35740)) ;
#14894 = EDGE_LOOP('',(#35741,#35742,#35743,#35744)) ;
#14895 = EDGE_LOOP('',(#35745,#35746,#35747,#35748)) ;
#14896 = EDGE_LOOP('',(#35749,#35750,#35751,#35752)) ;
#14897 = EDGE_LOOP('',(#35753,#35754,#35755,#35756)) ;
#14898 = EDGE_LOOP('',(#35757,#35758,#35759,#35760)) ;
#14899 = EDGE_LOOP('',(#35761,#35762,#35763,#35764)) ;
#14900 = EDGE_LOOP('',(#35765,#35766,#35767,#35768)) ;
#14901 = EDGE_LOOP('',(#35769,#35770,#35771)) ;
#14902 = EDGE_LOOP('',(#35772,#35773,#35774,#35775)) ;
#14903 = EDGE_LOOP('',(#35776,#35777,#35778,#35779)) ;
#14904 = EDGE_LOOP('',(#35780,#35781,#35782,#35783,#35784,#35785)) ;
#14905 = EDGE_LOOP('',(#35786,#35787,#35788,#35789)) ;
#14906 = EDGE_LOOP('',(#35790,#35791,#35792,#35793)) ;
#14907 = EDGE_LOOP('',(#35794,#35795,#35796)) ;
#14908 = EDGE_LOOP('',(#35797,#35798,#35799,#35800,#35801,#35802,#35803)) ;
#14909 = EDGE_LOOP('',(#35804,#35805,#35806,#35807)) ;
#14910 = EDGE_LOOP('',(#35808,#35809,#35810,#35811)) ;
#14911 = EDGE_LOOP('',(#35812,#35813,#35814,#35815)) ;
#14912 = EDGE_LOOP('',(#35816,#35817,#35818,#35819)) ;
#14913 = EDGE_LOOP('',(#35820,#35821,#35822,#35823)) ;
#14914 = EDGE_LOOP('',(#35824,#35825,#35826,#35827)) ;
#14915 = EDGE_LOOP('',(#35828,#35829,#35830,#35831)) ;
#14916 = EDGE_LOOP('',(#35832,#35833,#35834,#35835)) ;
#14917 = EDGE_LOOP('',(#35836,#35837,#35838,#35839)) ;
#14918 = EDGE_LOOP('',(#35840,#35841,#35842,#35843)) ;
#14919 = EDGE_LOOP('',(#35844,#35845,#35846,#35847)) ;
#14920 = EDGE_LOOP('',(#35848,#35849,#35850,#35851)) ;
#14921 = EDGE_LOOP('',(#35852,#35853,#35854,#35855)) ;
#14922 = EDGE_LOOP('',(#35856,#35857,#35858,#35859)) ;
#14923 = EDGE_LOOP('',(#35860,#35861,#35862,#35863)) ;
#14924 = EDGE_LOOP('',(#35864,#35865,#35866,#35867)) ;
#14925 = EDGE_LOOP('',(#35868,#35869,#35870,#35871)) ;
#14926 = EDGE_LOOP('',(#35872,#35873,#35874,#35875)) ;
#14927 = EDGE_LOOP('',(#35876,#35877,#35878,#35879)) ;
#14928 = EDGE_LOOP('',(#35880,#35881,#35882,#35883)) ;
#14929 = EDGE_LOOP('',(#35884,#35885,#35886,#35887)) ;
#14930 = EDGE_LOOP('',(#35888,#35889,#35890,#35891)) ;
#14931 = EDGE_LOOP('',(#35892,#35893,#35894,#35895)) ;
#14932 = EDGE_LOOP('',(#35896,#35897,#35898,#35899)) ;
#14933 = EDGE_LOOP('',(#35900,#35901,#35902,#35903)) ;
#14934 = EDGE_LOOP('',(#35904,#35905,#35906,#35907)) ;
#14935 = EDGE_LOOP('',(#35908,#35909,#35910,#35911)) ;
#14936 = EDGE_LOOP('',(#35912,#35913,#35914,#35915)) ;
#14937 = EDGE_LOOP('',(#35916,#35917,#35918,#35919)) ;
#14938 = EDGE_LOOP('',(#35920,#35921,#35922,#35923)) ;
#14939 = EDGE_LOOP('',(#35924,#35925,#35926,#35927)) ;
#14940 = EDGE_LOOP('',(#35928,#35929,#35930,#35931)) ;
#14941 = EDGE_LOOP('',(#35932,#35933,#35934,#35935)) ;
#14942 = EDGE_LOOP('',(#35936,#35937,#35938,#35939)) ;
#14943 = EDGE_LOOP('',(#35940,#35941,#35942,#35943)) ;
#14944 = EDGE_LOOP('',(#35944,#35945,#35946,#35947)) ;
#14945 = EDGE_LOOP('',(#35948,#35949,#35950,#35951)) ;
#14946 = EDGE_LOOP('',(#35952,#35953,#35954,#35955)) ;
#14947 = EDGE_LOOP('',(#35956,#35957,#35958,#35959)) ;
#14948 = EDGE_LOOP('',(#35960,#35961,#35962,#35963)) ;
#14949 = EDGE_LOOP('',(#35964,#35965,#35966,#35967)) ;
#14950 = EDGE_LOOP('',(#35968,#35969,#35970,#35971)) ;
#14951 = EDGE_LOOP('',(#35972,#35973,#35974,#35975)) ;
#14952 = EDGE_LOOP('',(#35976,#35977,#35978,#35979)) ;
#14953 = EDGE_LOOP('',(#35980,#35981,#35982,#35983)) ;
#14954 = EDGE_LOOP('',(#35984,#35985,#35986,#35987)) ;
#14955 = EDGE_LOOP('',(#35988,#35989,#35990,#35991)) ;
#14956 = EDGE_LOOP('',(#35992,#35993,#35994,#35995)) ;
#14957 = EDGE_LOOP('',(#35996,#35997,#35998,#35999)) ;
#14958 = EDGE_LOOP('',(#36000,#36001,#36002,#36003,#36004)) ;
#14959 = EDGE_LOOP('',(#36005,#36006,#36007,#36008,#36009)) ;
#14960 = EDGE_LOOP('',(#36010,#36011,#36012,#36013)) ;
#14961 = EDGE_LOOP('',(#36014,#36015,#36016,#36017)) ;
#14962 = EDGE_LOOP('',(#36018,#36019,#36020)) ;
#14963 = EDGE_LOOP('',(#36021,#36022,#36023,#36024,#36025,#36026,#36027)) ;
#14964 = EDGE_LOOP('',(#36028,#36029,#36030,#36031,#36032,#36033)) ;
#14965 = EDGE_LOOP('',(#36034,#36035,#36036,#36037)) ;
#14966 = EDGE_LOOP('',(#36038,#36039,#36040,#36041)) ;
#14967 = EDGE_LOOP('',(#36042,#36043,#36044,#36045)) ;
#14968 = EDGE_LOOP('',(#36046,#36047,#36048)) ;
#14969 = EDGE_LOOP('',(#36049,#36050,#36051,#36052)) ;
#14970 = EDGE_LOOP('',(#36053,#36054,#36055,#36056)) ;
#14971 = EDGE_LOOP('',(#36057,#36058,#36059,#36060)) ;
#14972 = EDGE_LOOP('',(#36061,#36062,#36063,#36064)) ;
#14973 = EDGE_LOOP('',(#36065,#36066,#36067,#36068)) ;
#14974 = EDGE_LOOP('',(#36069,#36070,#36071,#36072)) ;
#14975 = EDGE_LOOP('',(#36073,#36074,#36075,#36076)) ;
#14976 = EDGE_LOOP('',(#36077,#36078,#36079,#36080)) ;
#14977 = EDGE_LOOP('',(#36081,#36082,#36083,#36084)) ;
#14978 = EDGE_LOOP('',(#36085,#36086,#36087,#36088)) ;
#14979 = EDGE_LOOP('',(#36089,#36090,#36091,#36092)) ;
#14980 = EDGE_LOOP('',(#36093,#36094,#36095,#36096)) ;
#14981 = EDGE_LOOP('',(#36097,#36098,#36099,#36100)) ;
#14982 = EDGE_LOOP('',(#36101,#36102,#36103,#36104,#36105,#36106)) ;
#14983 = EDGE_LOOP('',(#36107,#36108,#36109,#36110,#36111)) ;
#14984 = EDGE_LOOP('',(#36112,#36113,#36114,#36115,#36116)) ;
#14985 = EDGE_LOOP('',(#36117,#36118,#36119,#36120,#36121)) ;
#14986 = EDGE_LOOP('',(#36122,#36123,#36124,#36125)) ;
#14987 = EDGE_LOOP('',(#36126,#36127,#36128,#36129)) ;
#14988 = EDGE_LOOP('',(#36130,#36131,#36132,#36133)) ;
#14989 = EDGE_LOOP('',(#36134,#36135,#36136,#36137)) ;
#14990 = EDGE_LOOP('',(#36138,#36139,#36140,#36141)) ;
#14991 = EDGE_LOOP('',(#36142,#36143,#36144,#36145)) ;
#14992 = EDGE_LOOP('',(#36146,#36147,#36148,#36149)) ;
#14993 = EDGE_LOOP('',(#36150,#36151,#36152,#36153)) ;
#14994 = EDGE_LOOP('',(#36154,#36155,#36156,#36157)) ;
#14995 = EDGE_LOOP('',(#36158,#36159,#36160,#36161)) ;
#14996 = EDGE_LOOP('',(#36162,#36163,#36164,#36165)) ;
#14997 = EDGE_LOOP('',(#36166,#36167,#36168,#36169)) ;
#14998 = EDGE_LOOP('',(#36170,#36171,#36172,#36173)) ;
#14999 = EDGE_LOOP('',(#36174,#36175,#36176,#36177)) ;
#15000 = EDGE_LOOP('',(#36178,#36179,#36180,#36181)) ;
#15001 = EDGE_LOOP('',(#36182,#36183,#36184,#36185)) ;
#15002 = EDGE_LOOP('',(#36186,#36187,#36188,#36189)) ;
#15003 = EDGE_LOOP('',(#36190,#36191,#36192,#36193)) ;
#15004 = EDGE_LOOP('',(#36194,#36195,#36196,#36197)) ;
#15005 = EDGE_LOOP('',(#36198,#36199,#36200,#36201)) ;
#15006 = EDGE_LOOP('',(#36202,#36203,#36204,#36205)) ;
#15007 = EDGE_LOOP('',(#36206,#36207,#36208,#36209)) ;
#15008 = EDGE_LOOP('',(#36210,#36211,#36212,#36213)) ;
#15009 = EDGE_LOOP('',(#36214,#36215,#36216,#36217)) ;
#15010 = EDGE_LOOP('',(#36218,#36219,#36220,#36221)) ;
#15011 = EDGE_LOOP('',(#36222,#36223,#36224,#36225)) ;
#15012 = EDGE_LOOP('',(#36226,#36227,#36228,#36229)) ;
#15013 = EDGE_LOOP('',(#36230,#36231,#36232,#36233)) ;
#15014 = EDGE_LOOP('',(#36234,#36235,#36236,#36237)) ;
#15015 = EDGE_LOOP('',(#36238,#36239,#36240,#36241)) ;
#15016 = EDGE_LOOP('',(#36242)) ;
#15017 = EDGE_LOOP('',(#36243)) ;
#15018 = EDGE_LOOP('',(#36244,#36245,#36246,#36247,#36248)) ;
#15019 = EDGE_LOOP('',(#36249,#36250,#36251,#36252,#36253)) ;
#15020 = EDGE_LOOP('',(#36254,#36255,#36256,#36257,#36258)) ;
#15021 = EDGE_LOOP('',(#36259,#36260,#36261,#36262,#36263)) ;
#15022 = EDGE_LOOP('',(#36264,#36265,#36266,#36267,#36268)) ;
#15023 = EDGE_LOOP('',(#36269,#36270,#36271,#36272,#36273)) ;
#15024 = EDGE_LOOP('',(#36274)) ;
#15025 = EDGE_LOOP('',(#36275)) ;
#15026 = EDGE_LOOP('',(#36276,#36277,#36278,#36279)) ;
#15027 = EDGE_LOOP('',(#36280,#36281,#36282,#36283)) ;
#15028 = EDGE_LOOP('',(#36284,#36285,#36286,#36287,#36288)) ;
#15029 = EDGE_LOOP('',(#36289,#36290,#36291,#36292,#36293)) ;
#15030 = EDGE_LOOP('',(#36294,#36295,#36296,#36297)) ;
#15031 = EDGE_LOOP('',(#36298)) ;
#15032 = EDGE_LOOP('',(#36299)) ;
#15033 = EDGE_LOOP('',(#36300,#36301,#36302,#36303,#36304)) ;
#15034 = EDGE_LOOP('',(#36305,#36306,#36307,#36308,#36309)) ;
#15035 = EDGE_LOOP('',(#36310,#36311,#36312,#36313,#36314)) ;
#15036 = EDGE_LOOP('',(#36315,#36316,#36317,#36318,#36319)) ;
#15037 = EDGE_LOOP('',(#36320)) ;
#15038 = EDGE_LOOP('',(#36321)) ;
#15039 = EDGE_LOOP('',(#36322,#36323,#36324,#36325)) ;
#15040 = EDGE_LOOP('',(#36326,#36327,#36328,#36329)) ;
#15041 = EDGE_LOOP('',(#36330,#36331,#36332,#36333)) ;
#15042 = EDGE_LOOP('',(#36334,#36335,#36336,#36337)) ;
#15043 = EDGE_LOOP('',(#36338,#36339,#36340,#36341)) ;
#15044 = EDGE_LOOP('',(#36342,#36343,#36344,#36345)) ;
#15045 = EDGE_LOOP('',(#36346,#36347,#36348,#36349)) ;
#15046 = EDGE_LOOP('',(#36350,#36351,#36352,#36353)) ;
#15047 = EDGE_LOOP('',(#36354,#36355,#36356)) ;
#15048 = EDGE_LOOP('',(#36357,#36358,#36359,#36360,#36361)) ;
#15049 = EDGE_LOOP('',(#36362,#36363,#36364,#36365,#36366)) ;
#15050 = EDGE_LOOP('',(#36367,#36368,#36369,#36370,#36371)) ;
#15051 = EDGE_LOOP('',(#36372,#36373,#36374,#36375,#36376)) ;
#15052 = EDGE_LOOP('',(#36377,#36378,#36379,#36380)) ;
#15053 = EDGE_LOOP('',(#36381,#36382,#36383,#36384)) ;
#15054 = EDGE_LOOP('',(#36385,#36386,#36387,#36388)) ;
#15055 = EDGE_LOOP('',(#36389,#36390,#36391,#36392,#36393)) ;
#15056 = EDGE_LOOP('',(#36394,#36395,#36396,#36397,#36398,#36399,#36400)) ;
#15057 = EDGE_LOOP('',(#36401,#36402,#36403,#36404,#36405)) ;
#15058 = EDGE_LOOP('',(#36406,#36407,#36408,#36409)) ;
#15059 = EDGE_LOOP('',(#36410,#36411,#36412,#36413)) ;
#15060 = EDGE_LOOP('',(#36414,#36415,#36416,#36417)) ;
#15061 = EDGE_LOOP('',(#36418,#36419,#36420,#36421)) ;
#15062 = EDGE_LOOP('',(#36422,#36423,#36424,#36425)) ;
#15063 = EDGE_LOOP('',(#36426,#36427,#36428,#36429)) ;
#15064 = EDGE_LOOP('',(#36430,#36431,#36432,#36433)) ;
#15065 = EDGE_LOOP('',(#36434,#36435,#36436)) ;
#15066 = EDGE_LOOP('',(#36437,#36438,#36439,#36440)) ;
#15067 = EDGE_LOOP('',(#36441,#36442,#36443,#36444)) ;
#15068 = EDGE_LOOP('',(#36445,#36446,#36447)) ;
#15069 = EDGE_LOOP('',(#36448,#36449,#36450,#36451)) ;
#15070 = EDGE_LOOP('',(#36452,#36453,#36454,#36455)) ;
#15071 = EDGE_LOOP('',(#36456,#36457,#36458)) ;
#15072 = EDGE_LOOP('',(#36459,#36460,#36461,#36462)) ;
#15073 = EDGE_LOOP('',(#36463,#36464,#36465,#36466,#36467)) ;
#15074 = EDGE_LOOP('',(#36468,#36469,#36470,#36471)) ;
#15075 = EDGE_LOOP('',(#36472,#36473,#36474,#36475,#36476,#36477)) ;
#15076 = EDGE_LOOP('',(#36478,#36479,#36480,#36481,#36482)) ;
#15077 = EDGE_LOOP('',(#36483,#36484,#36485,#36486)) ;
#15078 = EDGE_LOOP('',(#36487,#36488,#36489,#36490,#36491)) ;
#15079 = EDGE_LOOP('',(#36492,#36493,#36494,#36495,#36496)) ;
#15080 = EDGE_LOOP('',(#36497,#36498,#36499,#36500)) ;
#15081 = EDGE_LOOP('',(#36501,#36502,#36503,#36504)) ;
#15082 = EDGE_LOOP('',(#36505,#36506,#36507,#36508,#36509,#36510,#36511)) ;
#15083 = EDGE_LOOP('',(#36512,#36513,#36514,#36515)) ;
#15084 = EDGE_LOOP('',(#36516,#36517,#36518,#36519,#36520,#36521)) ;
#15085 = EDGE_LOOP('',(#36522,#36523,#36524,#36525)) ;
#15086 = EDGE_LOOP('',(#36526,#36527,#36528,#36529)) ;
#15087 = EDGE_LOOP('',(#36530,#36531,#36532,#36533)) ;
#15088 = EDGE_LOOP('',(#36534,#36535,#36536,#36537,#36538,#36539)) ;
#15089 = EDGE_LOOP('',(#36540,#36541,#36542,#36543)) ;
#15090 = EDGE_LOOP('',(#36544,#36545,#36546,#36547,#36548)) ;
#15091 = EDGE_LOOP('',(#36549,#36550,#36551,#36552,#36553)) ;
#15092 = EDGE_LOOP('',(#36554,#36555,#36556,#36557,#36558)) ;
#15093 = EDGE_LOOP('',(#36559,#36560,#36561)) ;
#15094 = EDGE_LOOP('',(#36562,#36563,#36564)) ;
#15095 = EDGE_LOOP('',(#36565,#36566,#36567)) ;
#15096 = EDGE_LOOP('',(#36568,#36569,#36570)) ;
#15097 = EDGE_LOOP('',(#36571,#36572,#36573)) ;
#15098 = EDGE_LOOP('',(#36574,#36575,#36576)) ;
#15099 = EDGE_LOOP('',(#36577,#36578,#36579,#36580)) ;
#15100 = EDGE_LOOP('',(#36581,#36582,#36583,#36584)) ;
#15101 = EDGE_LOOP('',(#36585,#36586,#36587,#36588)) ;
#15102 = EDGE_LOOP('',(#36589,#36590,#36591,#36592)) ;
#15103 = EDGE_LOOP('',(#36593,#36594,#36595,#36596)) ;
#15104 = EDGE_LOOP('',(#36597,#36598,#36599)) ;
#15105 = EDGE_LOOP('',(#36600,#36601,#36602,#36603)) ;
#15106 = EDGE_LOOP('',(#36604,#36605,#36606,#36607)) ;
#15107 = EDGE_LOOP('',(#36608,#36609,#36610,#36611)) ;
#15108 = EDGE_LOOP('',(#36612,#36613,#36614)) ;
#15109 = EDGE_LOOP('',(#36615,#36616,#36617,#36618)) ;
#15110 = EDGE_LOOP('',(#36619,#36620,#36621,#36622)) ;
#15111 = EDGE_LOOP('',(#36623,#36624,#36625,#36626)) ;
#15112 = EDGE_LOOP('',(#36627,#36628,#36629,#36630)) ;
#15113 = EDGE_LOOP('',(#36631,#36632,#36633,#36634,#36635,#36636)) ;
#15114 = EDGE_LOOP('',(#36637,#36638,#36639,#36640)) ;
#15115 = EDGE_LOOP('',(#36641,#36642,#36643,#36644)) ;
#15116 = EDGE_LOOP('',(#36645,#36646,#36647,#36648)) ;
#15117 = EDGE_LOOP('',(#36649,#36650,#36651,#36652)) ;
#15118 = EDGE_LOOP('',(#36653,#36654,#36655,#36656,#36657,#36658,#36659)) ;
#15119 = EDGE_LOOP('',(#36660,#36661,#36662,#36663,#36664,#36665)) ;
#15120 = EDGE_LOOP('',(#36666,#36667,#36668,#36669)) ;
#15121 = EDGE_LOOP('',(#36670,#36671,#36672,#36673)) ;
#15122 = EDGE_LOOP('',(#36674,#36675,#36676,#36677)) ;
#15123 = EDGE_LOOP('',(#36678,#36679,#36680)) ;
#15124 = EDGE_LOOP('',(#36681,#36682,#36683)) ;
#15125 = EDGE_LOOP('',(#36684,#36685,#36686,#36687,#36688,#36689,#36690,#36691,
#36692,#36693,#36694,#36695,#36696,#36697,#36698,#36699,#36700,#36701,#36702,
#36703,#36704,#36705,#36706,#36707,#36708)) ;
#15126 = EDGE_LOOP('',(#36709,#36710,#36711,#36712)) ;
#15127 = EDGE_LOOP('',(#36713,#36714,#36715,#36716,#36717,#36718,#36719,#36720)) ;
#15128 = EDGE_LOOP('',(#36721,#36722,#36723,#36724,#36725,#36726,#36727,#36728)) ;
#15129 = EDGE_LOOP('',(#36729,#36730,#36731,#36732,#36733,#36734,#36735,#36736)) ;
#15130 = EDGE_LOOP('',(#36737,#36738,#36739,#36740,#36741,#36742,#36743,#36744)) ;
#15131 = EDGE_LOOP('',(#36745,#36746,#36747,#36748)) ;
#15132 = EDGE_LOOP('',(#36749,#36750,#36751,#36752)) ;
#15133 = EDGE_LOOP('',(#36753,#36754,#36755,#36756)) ;
#15134 = EDGE_LOOP('',(#36757,#36758,#36759,#36760,#36761,#36762,#36763,#36764,
#36765,#36766,#36767,#36768,#36769,#36770,#36771,#36772,#36773,#36774,#36775,
#36776,#36777,#36778,#36779,#36780,#36781)) ;
#15135 = EDGE_LOOP('',(#36782,#36783,#36784,#36785)) ;
#15136 = EDGE_LOOP('',(#36786,#36787,#36788,#36789)) ;
#15137 = EDGE_LOOP('',(#36790,#36791,#36792,#36793)) ;
#15138 = EDGE_LOOP('',(#36794,#36795,#36796,#36797)) ;
#15139 = EDGE_LOOP('',(#36798,#36799,#36800,#36801)) ;
#15140 = EDGE_LOOP('',(#36802,#36803,#36804,#36805)) ;
#15141 = EDGE_LOOP('',(#36806,#36807,#36808,#36809)) ;
#15142 = EDGE_LOOP('',(#36810,#36811,#36812,#36813)) ;
#15143 = EDGE_LOOP('',(#36814,#36815,#36816,#36817)) ;
#15144 = EDGE_LOOP('',(#36818,#36819,#36820,#36821)) ;
#15145 = EDGE_LOOP('',(#36822,#36823,#36824,#36825)) ;
#15146 = EDGE_LOOP('',(#36826,#36827,#36828,#36829)) ;
#15147 = EDGE_LOOP('',(#36830,#36831,#36832,#36833)) ;
#15148 = EDGE_LOOP('',(#36834,#36835,#36836,#36837)) ;
#15149 = EDGE_LOOP('',(#36838,#36839,#36840,#36841)) ;
#15150 = EDGE_LOOP('',(#36842,#36843,#36844,#36845)) ;
#15151 = EDGE_LOOP('',(#36846,#36847,#36848,#36849)) ;
#15152 = EDGE_LOOP('',(#36850,#36851,#36852,#36853)) ;
#15153 = EDGE_LOOP('',(#36854,#36855,#36856,#36857)) ;
#15154 = EDGE_LOOP('',(#36858,#36859,#36860,#36861)) ;
#15155 = EDGE_LOOP('',(#36862,#36863,#36864,#36865)) ;
#15156 = EDGE_LOOP('',(#36866,#36867,#36868,#36869)) ;
#15157 = EDGE_LOOP('',(#36870,#36871,#36872,#36873,#36874)) ;
#15158 = EDGE_LOOP('',(#36875,#36876,#36877,#36878)) ;
#15159 = EDGE_LOOP('',(#36879,#36880,#36881,#36882,#36883)) ;
#15160 = EDGE_LOOP('',(#36884,#36885,#36886,#36887)) ;
#15161 = EDGE_LOOP('',(#36888,#36889,#36890,#36891,#36892)) ;
#15162 = EDGE_LOOP('',(#36893,#36894,#36895,#36896,#36897)) ;
#15163 = EDGE_LOOP('',(#36898,#36899,#36900,#36901)) ;
#15164 = EDGE_LOOP('',(#36902,#36903,#36904,#36905)) ;
#15165 = EDGE_LOOP('',(#36906,#36907,#36908,#36909)) ;
#15166 = EDGE_LOOP('',(#36910,#36911,#36912,#36913,#36914)) ;
#15167 = EDGE_LOOP('',(#36915,#36916,#36917,#36918)) ;
#15168 = EDGE_LOOP('',(#36919,#36920,#36921,#36922)) ;
#15169 = EDGE_LOOP('',(#36923,#36924,#36925,#36926)) ;
#15170 = EDGE_LOOP('',(#36927,#36928,#36929,#36930)) ;
#15171 = EDGE_LOOP('',(#36931,#36932,#36933,#36934)) ;
#15172 = EDGE_LOOP('',(#36935,#36936,#36937,#36938)) ;
#15173 = EDGE_LOOP('',(#36939,#36940,#36941,#36942)) ;
#15174 = EDGE_LOOP('',(#36943,#36944,#36945,#36946,#36947)) ;
#15175 = EDGE_LOOP('',(#36948,#36949,#36950,#36951)) ;
#15176 = EDGE_LOOP('',(#36952,#36953,#36954,#36955)) ;
#15177 = EDGE_LOOP('',(#36956,#36957,#36958,#36959)) ;
#15178 = EDGE_LOOP('',(#36960,#36961,#36962,#36963,#36964)) ;
#15179 = EDGE_LOOP('',(#36965,#36966,#36967,#36968,#36969,#36970)) ;
#15180 = EDGE_LOOP('',(#36971,#36972,#36973,#36974)) ;
#15181 = EDGE_LOOP('',(#36975,#36976,#36977,#36978,#36979)) ;
#15182 = EDGE_LOOP('',(#36980,#36981,#36982,#36983)) ;
#15183 = EDGE_LOOP('',(#36984,#36985,#36986,#36987)) ;
#15184 = EDGE_LOOP('',(#36988,#36989,#36990,#36991,#36992,#36993)) ;
#15185 = EDGE_LOOP('',(#36994,#36995,#36996,#36997)) ;
#15186 = EDGE_LOOP('',(#36998,#36999,#37000,#37001)) ;
#15187 = EDGE_LOOP('',(#37002,#37003,#37004,#37005)) ;
#15188 = EDGE_LOOP('',(#37006,#37007,#37008,#37009)) ;
#15189 = EDGE_LOOP('',(#37010,#37011,#37012,#37013)) ;
#15190 = EDGE_LOOP('',(#37014,#37015,#37016,#37017)) ;
#15191 = EDGE_LOOP('',(#37018,#37019,#37020,#37021)) ;
#15192 = EDGE_LOOP('',(#37022,#37023,#37024,#37025)) ;
#15193 = EDGE_LOOP('',(#37026,#37027,#37028,#37029)) ;
#15194 = EDGE_LOOP('',(#37030,#37031,#37032,#37033)) ;
#15195 = EDGE_LOOP('',(#37034,#37035,#37036,#37037)) ;
#15196 = EDGE_LOOP('',(#37038,#37039,#37040,#37041)) ;
#15197 = EDGE_LOOP('',(#37042,#37043,#37044,#37045)) ;
#15198 = EDGE_LOOP('',(#37046,#37047,#37048,#37049)) ;
#15199 = EDGE_LOOP('',(#37050,#37051,#37052,#37053)) ;
#15200 = EDGE_LOOP('',(#37054,#37055,#37056,#37057)) ;
#15201 = EDGE_LOOP('',(#37058,#37059,#37060,#37061)) ;
#15202 = EDGE_LOOP('',(#37062,#37063,#37064,#37065)) ;
#15203 = EDGE_LOOP('',(#37066,#37067,#37068,#37069)) ;
#15204 = EDGE_LOOP('',(#37070,#37071,#37072,#37073)) ;
#15205 = EDGE_LOOP('',(#37074,#37075,#37076,#37077)) ;
#15206 = EDGE_LOOP('',(#37078,#37079,#37080,#37081)) ;
#15207 = EDGE_LOOP('',(#37082,#37083,#37084,#37085)) ;
#15208 = EDGE_LOOP('',(#37086,#37087,#37088,#37089)) ;
#15209 = EDGE_LOOP('',(#37090,#37091,#37092,#37093)) ;
#15210 = EDGE_LOOP('',(#37094,#37095,#37096,#37097)) ;
#15211 = EDGE_LOOP('',(#37098,#37099,#37100,#37101)) ;
#15212 = EDGE_LOOP('',(#37102,#37103,#37104,#37105)) ;
#15213 = EDGE_LOOP('',(#37106,#37107,#37108,#37109)) ;
#15214 = EDGE_LOOP('',(#37110,#37111,#37112,#37113)) ;
#15215 = EDGE_LOOP('',(#37114,#37115,#37116,#37117)) ;
#15216 = EDGE_LOOP('',(#37118,#37119,#37120,#37121)) ;
#15217 = EDGE_LOOP('',(#37122,#37123,#37124,#37125)) ;
#15218 = EDGE_LOOP('',(#37126,#37127,#37128,#37129)) ;
#15219 = EDGE_LOOP('',(#37130,#37131,#37132,#37133)) ;
#15220 = EDGE_LOOP('',(#37134,#37135,#37136,#37137)) ;
#15221 = EDGE_LOOP('',(#37138,#37139,#37140,#37141)) ;
#15222 = EDGE_LOOP('',(#37142,#37143,#37144,#37145)) ;
#15223 = EDGE_LOOP('',(#37146,#37147,#37148,#37149)) ;
#15224 = EDGE_LOOP('',(#37150,#37151,#37152,#37153)) ;
#15225 = EDGE_LOOP('',(#37154,#37155,#37156,#37157)) ;
#15226 = EDGE_LOOP('',(#37158,#37159,#37160,#37161)) ;
#15227 = EDGE_LOOP('',(#37162,#37163,#37164,#37165)) ;
#15228 = EDGE_LOOP('',(#37166,#37167,#37168,#37169)) ;
#15229 = EDGE_LOOP('',(#37170,#37171,#37172,#37173)) ;
#15230 = EDGE_LOOP('',(#37174,#37175,#37176,#37177)) ;
#15231 = EDGE_LOOP('',(#37178,#37179,#37180,#37181)) ;
#15232 = EDGE_LOOP('',(#37182,#37183,#37184,#37185)) ;
#15233 = EDGE_LOOP('',(#37186,#37187,#37188,#37189)) ;
#15234 = EDGE_LOOP('',(#37190,#37191,#37192,#37193)) ;
#15235 = EDGE_LOOP('',(#37194,#37195,#37196,#37197)) ;
#15236 = EDGE_LOOP('',(#37198,#37199,#37200,#37201,#37202,#37203)) ;
#15237 = EDGE_LOOP('',(#37204,#37205,#37206,#37207)) ;
#15238 = EDGE_LOOP('',(#37208,#37209,#37210,#37211)) ;
#15239 = EDGE_LOOP('',(#37212,#37213,#37214,#37215)) ;
#15240 = EDGE_LOOP('',(#37216,#37217,#37218,#37219)) ;
#15241 = EDGE_LOOP('',(#37220,#37221,#37222,#37223)) ;
#15242 = EDGE_LOOP('',(#37224,#37225,#37226,#37227,#37228,#37229)) ;
#15243 = EDGE_LOOP('',(#37230,#37231,#37232,#37233)) ;
#15244 = EDGE_LOOP('',(#37234,#37235,#37236,#37237)) ;
#15245 = EDGE_LOOP('',(#37238,#37239,#37240,#37241)) ;
#15246 = EDGE_LOOP('',(#37242,#37243,#37244,#37245)) ;
#15247 = EDGE_LOOP('',(#37246,#37247,#37248,#37249)) ;
#15248 = EDGE_LOOP('',(#37250,#37251,#37252,#37253)) ;
#15249 = EDGE_LOOP('',(#37254,#37255,#37256,#37257)) ;
#15250 = EDGE_LOOP('',(#37258,#37259,#37260,#37261)) ;
#15251 = EDGE_LOOP('',(#37262,#37263,#37264,#37265)) ;
#15252 = EDGE_LOOP('',(#37266,#37267,#37268,#37269)) ;
#15253 = EDGE_LOOP('',(#37270,#37271,#37272,#37273)) ;
#15254 = EDGE_LOOP('',(#37274,#37275,#37276,#37277,#37278,#37279)) ;
#15255 = EDGE_LOOP('',(#37280,#37281,#37282,#37283,#37284)) ;
#15256 = EDGE_LOOP('',(#37285,#37286,#37287,#37288,#37289)) ;
#15257 = EDGE_LOOP('',(#37290)) ;
#15258 = EDGE_LOOP('',(#37291)) ;
#15259 = EDGE_LOOP('',(#37292,#37293,#37294,#37295,#37296,#37297)) ;
#15260 = EDGE_LOOP('',(#37298,#37299,#37300,#37301,#37302)) ;
#15261 = EDGE_LOOP('',(#37303,#37304,#37305,#37306,#37307)) ;
#15262 = EDGE_LOOP('',(#37308)) ;
#15263 = EDGE_LOOP('',(#37309)) ;
#15264 = EDGE_LOOP('',(#37310,#37311,#37312,#37313)) ;
#15265 = EDGE_LOOP('',(#37314,#37315,#37316,#37317)) ;
#15266 = EDGE_LOOP('',(#37318)) ;
#15267 = EDGE_LOOP('',(#37319)) ;
#15268 = EDGE_LOOP('',(#37320,#37321,#37322,#37323)) ;
#15269 = EDGE_LOOP('',(#37324)) ;
#15270 = EDGE_LOOP('',(#37325)) ;
#15271 = EDGE_LOOP('',(#37326,#37327,#37328,#37329)) ;
#15272 = EDGE_LOOP('',(#37330,#37331,#37332)) ;
#15273 = EDGE_LOOP('',(#37333,#37334,#37335,#37336)) ;
#15274 = EDGE_LOOP('',(#37337,#37338,#37339)) ;
#15275 = EDGE_LOOP('',(#37340,#37341,#37342,#37343,#37344)) ;
#15276 = EDGE_LOOP('',(#37345,#37346,#37347,#37348)) ;
#15277 = EDGE_LOOP('',(#37349,#37350,#37351,#37352)) ;
#15278 = EDGE_LOOP('',(#37353,#37354,#37355)) ;
#15279 = EDGE_LOOP('',(#37356,#37357,#37358,#37359)) ;
#15280 = EDGE_LOOP('',(#37360,#37361,#37362,#37363)) ;
#15281 = EDGE_LOOP('',(#37364,#37365,#37366,#37367)) ;
#15282 = EDGE_LOOP('',(#37368,#37369,#37370)) ;
#15283 = EDGE_LOOP('',(#37371,#37372,#37373,#37374)) ;
#15284 = EDGE_LOOP('',(#37375,#37376,#37377)) ;
#15285 = EDGE_LOOP('',(#37378,#37379,#37380,#37381,#37382)) ;
#15286 = EDGE_LOOP('',(#37383,#37384,#37385,#37386)) ;
#15287 = EDGE_LOOP('',(#37387,#37388,#37389,#37390)) ;
#15288 = EDGE_LOOP('',(#37391,#37392,#37393,#37394)) ;
#15289 = EDGE_LOOP('',(#37395,#37396,#37397)) ;
#15290 = EDGE_LOOP('',(#37398,#37399,#37400,#37401)) ;
#15291 = EDGE_LOOP('',(#37402,#37403,#37404,#37405)) ;
#15292 = EDGE_LOOP('',(#37406,#37407,#37408)) ;
#15293 = EDGE_LOOP('',(#37409,#37410,#37411,#37412)) ;
#15294 = EDGE_LOOP('',(#37413,#37414,#37415,#37416)) ;
#15295 = EDGE_LOOP('',(#37417,#37418,#37419)) ;
#15296 = EDGE_LOOP('',(#37420,#37421,#37422,#37423,#37424)) ;
#15297 = EDGE_LOOP('',(#37425,#37426,#37427,#37428)) ;
#15298 = EDGE_LOOP('',(#37429,#37430,#37431,#37432)) ;
#15299 = EDGE_LOOP('',(#37433,#37434,#37435)) ;
#15300 = EDGE_LOOP('',(#37436,#37437,#37438,#37439)) ;
#15301 = EDGE_LOOP('',(#37440,#37441,#37442,#37443)) ;
#15302 = EDGE_LOOP('',(#37444,#37445,#37446,#37447)) ;
#15303 = EDGE_LOOP('',(#37448,#37449,#37450)) ;
#15304 = EDGE_LOOP('',(#37451,#37452,#37453,#37454)) ;
#15305 = EDGE_LOOP('',(#37455,#37456,#37457)) ;
#15306 = EDGE_LOOP('',(#37458,#37459,#37460,#37461,#37462)) ;
#15307 = EDGE_LOOP('',(#37463,#37464,#37465,#37466)) ;
#15308 = EDGE_LOOP('',(#37467,#37468,#37469,#37470)) ;
#15309 = EDGE_LOOP('',(#37471,#37472,#37473,#37474)) ;
#15310 = EDGE_LOOP('',(#37475,#37476,#37477)) ;
#15311 = EDGE_LOOP('',(#37478,#37479,#37480,#37481)) ;
#15312 = EDGE_LOOP('',(#37482,#37483,#37484,#37485)) ;
#15313 = EDGE_LOOP('',(#37486,#37487,#37488,#37489)) ;
#15314 = EDGE_LOOP('',(#37490,#37491,#37492,#37493)) ;
#15315 = EDGE_LOOP('',(#37494,#37495,#37496,#37497)) ;
#15316 = EDGE_LOOP('',(#37498,#37499,#37500,#37501)) ;
#15317 = EDGE_LOOP('',(#37502,#37503,#37504,#37505)) ;
#15318 = EDGE_LOOP('',(#37506,#37507,#37508,#37509)) ;
#15319 = EDGE_LOOP('',(#37510,#37511,#37512,#37513)) ;
#15320 = EDGE_LOOP('',(#37514,#37515,#37516,#37517)) ;
#15321 = EDGE_LOOP('',(#37518,#37519,#37520,#37521,#37522)) ;
#15322 = EDGE_LOOP('',(#37523,#37524,#37525,#37526)) ;
#15323 = EDGE_LOOP('',(#37527,#37528,#37529,#37530,#37531)) ;
#15324 = EDGE_LOOP('',(#37532,#37533,#37534,#37535)) ;
#15325 = EDGE_LOOP('',(#37536,#37537,#37538,#37539)) ;
#15326 = EDGE_LOOP('',(#37540,#37541,#37542,#37543)) ;
#15327 = EDGE_LOOP('',(#37544,#37545,#37546,#37547,#37548)) ;
#15328 = EDGE_LOOP('',(#37549,#37550,#37551,#37552)) ;
#15329 = EDGE_LOOP('',(#37553,#37554,#37555,#37556,#37557)) ;
#15330 = EDGE_LOOP('',(#37558)) ;
#15331 = EDGE_LOOP('',(#37559,#37560,#37561,#37562,#37563,#37564,#37565,#37566,
#37567,#37568,#37569,#37570,#37571,#37572,#37573,#37574,#37575,#37576,#37577,
#37578)) ;
#15332 = EDGE_LOOP('',(#37579,#37580,#37581,#37582,#37583)) ;
#15333 = EDGE_LOOP('',(#37584,#37585,#37586,#37587)) ;
#15334 = EDGE_LOOP('',(#37588,#37589,#37590,#37591)) ;
#15335 = EDGE_LOOP('',(#37592,#37593,#37594,#37595,#37596)) ;
#15336 = EDGE_LOOP('',(#37597,#37598,#37599,#37600,#37601)) ;
#15337 = EDGE_LOOP('',(#37602,#37603,#37604,#37605)) ;
#15338 = EDGE_LOOP('',(#37606,#37607,#37608,#37609,#37610)) ;
#15339 = EDGE_LOOP('',(#37611,#37612,#37613,#37614)) ;
#15340 = EDGE_LOOP('',(#37615,#37616,#37617,#37618)) ;
#15341 = EDGE_LOOP('',(#37619,#37620,#37621,#37622)) ;
#15342 = EDGE_LOOP('',(#37623,#37624,#37625,#37626)) ;
#15343 = EDGE_LOOP('',(#37627,#37628,#37629,#37630)) ;
#15344 = EDGE_LOOP('',(#37631,#37632,#37633,#37634,#37635,#37636,#37637,#37638,
#37639,#37640,#37641,#37642)) ;
#15345 = EDGE_LOOP('',(#37643,#37644,#37645,#37646)) ;
#15346 = EDGE_LOOP('',(#37647,#37648,#37649,#37650,#37651)) ;
#15347 = EDGE_LOOP('',(#37652,#37653,#37654,#37655,#37656)) ;
#15348 = EDGE_LOOP('',(#37657)) ;
#15349 = EDGE_LOOP('',(#37658,#37659,#37660,#37661)) ;
#15350 = EDGE_LOOP('',(#37662,#37663,#37664)) ;
#15351 = EDGE_LOOP('',(#37665,#37666,#37667)) ;
#15352 = EDGE_LOOP('',(#37668,#37669,#37670)) ;
#15353 = EDGE_LOOP('',(#37671,#37672,#37673,#37674)) ;
#15354 = EDGE_LOOP('',(#37675,#37676,#37677,#37678)) ;
#15355 = EDGE_LOOP('',(#37679,#37680,#37681)) ;
#15356 = EDGE_LOOP('',(#37682,#37683,#37684)) ;
#15357 = EDGE_LOOP('',(#37685,#37686,#37687,#37688)) ;
#15358 = EDGE_LOOP('',(#37689,#37690,#37691,#37692)) ;
#15359 = EDGE_LOOP('',(#37693,#37694,#37695,#37696)) ;
#15360 = EDGE_LOOP('',(#37697,#37698,#37699,#37700)) ;
#15361 = EDGE_LOOP('',(#37701,#37702,#37703,#37704)) ;
#15362 = EDGE_LOOP('',(#37705,#37706,#37707,#37708)) ;
#15363 = EDGE_LOOP('',(#37709,#37710,#37711,#37712)) ;
#15364 = EDGE_LOOP('',(#37713,#37714,#37715,#37716)) ;
#15365 = EDGE_LOOP('',(#37717,#37718,#37719,#37720)) ;
#15366 = EDGE_LOOP('',(#37721,#37722,#37723,#37724)) ;
#15367 = EDGE_LOOP('',(#37725,#37726,#37727,#37728)) ;
#15368 = EDGE_LOOP('',(#37729,#37730,#37731,#37732)) ;
#15369 = EDGE_LOOP('',(#37733,#37734,#37735,#37736)) ;
#15370 = EDGE_LOOP('',(#37737,#37738,#37739,#37740,#37741)) ;
#15371 = EDGE_LOOP('',(#37742,#37743,#37744,#37745,#37746)) ;
#15372 = EDGE_LOOP('',(#37747,#37748,#37749,#37750,#37751,#37752)) ;
#15373 = EDGE_LOOP('',(#37753)) ;
#15374 = EDGE_LOOP('',(#37754,#37755,#37756,#37757)) ;
#15375 = EDGE_LOOP('',(#37758,#37759,#37760,#37761)) ;
#15376 = EDGE_LOOP('',(#37762,#37763,#37764,#37765)) ;
#15377 = EDGE_LOOP('',(#37766,#37767,#37768,#37769)) ;
#15378 = EDGE_LOOP('',(#37770,#37771,#37772,#37773)) ;
#15379 = EDGE_LOOP('',(#37774,#37775,#37776,#37777)) ;
#15380 = EDGE_LOOP('',(#37778,#37779,#37780,#37781)) ;
#15381 = EDGE_LOOP('',(#37782,#37783,#37784,#37785)) ;
#15382 = EDGE_LOOP('',(#37786,#37787,#37788,#37789)) ;
#15383 = EDGE_LOOP('',(#37790,#37791,#37792,#37793)) ;
#15384 = EDGE_LOOP('',(#37794,#37795,#37796,#37797)) ;
#15385 = EDGE_LOOP('',(#37798,#37799,#37800,#37801)) ;
#15386 = EDGE_LOOP('',(#37802,#37803,#37804,#37805)) ;
#15387 = EDGE_LOOP('',(#37806,#37807,#37808,#37809)) ;
#15388 = EDGE_LOOP('',(#37810,#37811,#37812,#37813)) ;
#15389 = EDGE_LOOP('',(#37814,#37815,#37816,#37817)) ;
#15390 = EDGE_LOOP('',(#37818,#37819,#37820,#37821)) ;
#15391 = EDGE_LOOP('',(#37822,#37823,#37824,#37825)) ;
#15392 = EDGE_LOOP('',(#37826)) ;
#15393 = EDGE_LOOP('',(#37827,#37828,#37829,#37830,#37831,#37832,#37833,#37834,
#37835,#37836,#37837,#37838)) ;
#15394 = EDGE_LOOP('',(#37839,#37840,#37841,#37842)) ;
#15395 = EDGE_LOOP('',(#37843,#37844,#37845,#37846)) ;
#15396 = EDGE_LOOP('',(#37847,#37848,#37849,#37850)) ;
#15397 = EDGE_LOOP('',(#37851,#37852,#37853,#37854)) ;
#15398 = EDGE_LOOP('',(#37855,#37856,#37857,#37858)) ;
#15399 = EDGE_LOOP('',(#37859,#37860,#37861,#37862)) ;
#15400 = EDGE_LOOP('',(#37863,#37864,#37865,#37866)) ;
#15401 = EDGE_LOOP('',(#37867,#37868,#37869,#37870)) ;
#15402 = EDGE_LOOP('',(#37871,#37872,#37873,#37874)) ;
#15403 = EDGE_LOOP('',(#37875,#37876,#37877,#37878)) ;
#15404 = EDGE_LOOP('',(#37879,#37880,#37881,#37882)) ;
#15405 = EDGE_LOOP('',(#37883,#37884,#37885,#37886)) ;
#15406 = EDGE_LOOP('',(#37887,#37888,#37889,#37890)) ;
#15407 = EDGE_LOOP('',(#37891,#37892,#37893,#37894)) ;
#15408 = EDGE_LOOP('',(#37895,#37896,#37897,#37898)) ;
#15409 = EDGE_LOOP('',(#37899,#37900,#37901,#37902,#37903,#37904,#37905,#37906,
#37907,#37908,#37909,#37910)) ;
#15410 = EDGE_LOOP('',(#37911,#37912,#37913,#37914,#37915)) ;
#15411 = EDGE_LOOP('',(#37916,#37917,#37918,#37919)) ;
#15412 = EDGE_LOOP('',(#37920,#37921,#37922,#37923)) ;
#15413 = EDGE_LOOP('',(#37924,#37925,#37926,#37927)) ;
#15414 = EDGE_LOOP('',(#37928,#37929,#37930,#37931)) ;
#15415 = EDGE_LOOP('',(#37932,#37933,#37934,#37935)) ;
#15416 = EDGE_LOOP('',(#37936,#37937,#37938,#37939)) ;
#15417 = EDGE_LOOP('',(#37940,#37941,#37942,#37943)) ;
#15418 = EDGE_LOOP('',(#37944,#37945,#37946,#37947)) ;
#15419 = EDGE_LOOP('',(#37948,#37949,#37950,#37951)) ;
#15420 = EDGE_LOOP('',(#37952,#37953,#37954,#37955)) ;
#15421 = EDGE_LOOP('',(#37956,#37957,#37958,#37959)) ;
#15422 = EDGE_LOOP('',(#37960,#37961,#37962,#37963)) ;
#15423 = EDGE_LOOP('',(#37964,#37965,#37966,#37967)) ;
#15424 = EDGE_LOOP('',(#37968,#37969,#37970,#37971)) ;
#15425 = EDGE_LOOP('',(#37972,#37973,#37974,#37975)) ;
#15426 = EDGE_LOOP('',(#37976,#37977,#37978,#37979)) ;
#15427 = EDGE_LOOP('',(#37980,#37981,#37982,#37983)) ;
#15428 = EDGE_LOOP('',(#37984,#37985,#37986,#37987)) ;
#15429 = EDGE_LOOP('',(#37988,#37989,#37990,#37991)) ;
#15430 = EDGE_LOOP('',(#37992,#37993,#37994,#37995)) ;
#15431 = EDGE_LOOP('',(#37996,#37997,#37998,#37999)) ;
#15432 = EDGE_LOOP('',(#38000,#38001,#38002,#38003,#38004,#38005,#38006,#38007,
#38008,#38009,#38010,#38011)) ;
#15433 = EDGE_LOOP('',(#38012,#38013,#38014,#38015,#38016)) ;
#15434 = EDGE_LOOP('',(#38017,#38018,#38019,#38020,#38021,#38022)) ;
#15435 = EDGE_LOOP('',(#38023)) ;
#15436 = EDGE_LOOP('',(#38024,#38025,#38026,#38027)) ;
#15437 = EDGE_LOOP('',(#38028,#38029,#38030,#38031)) ;
#15438 = EDGE_LOOP('',(#38032,#38033,#38034,#38035)) ;
#15439 = EDGE_LOOP('',(#38036,#38037,#38038,#38039)) ;
#15440 = EDGE_LOOP('',(#38040,#38041,#38042,#38043)) ;
#15441 = EDGE_LOOP('',(#38044,#38045,#38046,#38047)) ;
#15442 = EDGE_LOOP('',(#38048,#38049,#38050,#38051)) ;
#15443 = EDGE_LOOP('',(#38052,#38053,#38054,#38055)) ;
#15444 = EDGE_LOOP('',(#38056,#38057,#38058,#38059)) ;
#15445 = EDGE_LOOP('',(#38060,#38061,#38062,#38063)) ;
#15446 = EDGE_LOOP('',(#38064,#38065,#38066,#38067)) ;
#15447 = EDGE_LOOP('',(#38068,#38069,#38070,#38071)) ;
#15448 = EDGE_LOOP('',(#38072,#38073,#38074,#38075)) ;
#15449 = EDGE_LOOP('',(#38076,#38077,#38078,#38079)) ;
#15450 = EDGE_LOOP('',(#38080,#38081,#38082,#38083)) ;
#15451 = EDGE_LOOP('',(#38084)) ;
#15452 = EDGE_LOOP('',(#38085,#38086,#38087,#38088,#38089,#38090,#38091,#38092,
#38093,#38094,#38095,#38096)) ;
#15453 = EDGE_LOOP('',(#38097,#38098,#38099,#38100,#38101)) ;
#15454 = EDGE_LOOP('',(#38102,#38103,#38104,#38105)) ;
#15455 = EDGE_LOOP('',(#38106,#38107,#38108,#38109)) ;
#15456 = EDGE_LOOP('',(#38110,#38111,#38112,#38113)) ;
#15457 = EDGE_LOOP('',(#38114,#38115,#38116,#38117)) ;
#15458 = EDGE_LOOP('',(#38118,#38119,#38120,#38121)) ;
#15459 = EDGE_LOOP('',(#38122,#38123,#38124,#38125)) ;
#15460 = EDGE_LOOP('',(#38126,#38127,#38128,#38129)) ;
#15461 = EDGE_LOOP('',(#38130,#38131,#38132,#38133)) ;
#15462 = EDGE_LOOP('',(#38134,#38135,#38136,#38137)) ;
#15463 = EDGE_LOOP('',(#38138,#38139,#38140,#38141)) ;
#15464 = EDGE_LOOP('',(#38142,#38143,#38144,#38145)) ;
#15465 = EDGE_LOOP('',(#38146,#38147,#38148,#38149)) ;
#15466 = EDGE_LOOP('',(#38150,#38151,#38152,#38153)) ;
#15467 = EDGE_LOOP('',(#38154,#38155,#38156,#38157)) ;
#15468 = EDGE_LOOP('',(#38158,#38159,#38160,#38161)) ;
#15469 = EDGE_LOOP('',(#38162,#38163,#38164,#38165)) ;
#15470 = EDGE_LOOP('',(#38166,#38167,#38168,#38169)) ;
#15471 = EDGE_LOOP('',(#38170,#38171,#38172,#38173)) ;
#15472 = EDGE_LOOP('',(#38174,#38175,#38176,#38177)) ;
#15473 = EDGE_LOOP('',(#38178,#38179,#38180,#38181)) ;
#15474 = EDGE_LOOP('',(#38182,#38183,#38184,#38185)) ;
#15475 = EDGE_LOOP('',(#38186,#38187,#38188,#38189,#38190,#38191,#38192,#38193,
#38194,#38195,#38196,#38197)) ;
#15476 = EDGE_LOOP('',(#38198,#38199,#38200,#38201,#38202)) ;
#15477 = EDGE_LOOP('',(#38203,#38204,#38205,#38206,#38207,#38208)) ;
#15478 = EDGE_LOOP('',(#38209)) ;
#15479 = EDGE_LOOP('',(#38210,#38211,#38212,#38213)) ;
#15480 = EDGE_LOOP('',(#38214,#38215,#38216,#38217)) ;
#15481 = EDGE_LOOP('',(#38218,#38219,#38220,#38221)) ;
#15482 = EDGE_LOOP('',(#38222,#38223,#38224,#38225)) ;
#15483 = EDGE_LOOP('',(#38226,#38227,#38228,#38229)) ;
#15484 = EDGE_LOOP('',(#38230,#38231,#38232,#38233)) ;
#15485 = EDGE_LOOP('',(#38234,#38235,#38236,#38237)) ;
#15486 = EDGE_LOOP('',(#38238,#38239,#38240,#38241)) ;
#15487 = EDGE_LOOP('',(#38242,#38243,#38244,#38245)) ;
#15488 = EDGE_LOOP('',(#38246,#38247,#38248,#38249)) ;
#15489 = EDGE_LOOP('',(#38250,#38251,#38252,#38253)) ;
#15490 = EDGE_LOOP('',(#38254,#38255,#38256,#38257)) ;
#15491 = EDGE_LOOP('',(#38258,#38259,#38260,#38261)) ;
#15492 = EDGE_LOOP('',(#38262,#38263,#38264,#38265)) ;
#15493 = EDGE_LOOP('',(#38266,#38267,#38268,#38269)) ;
#15494 = EDGE_LOOP('',(#38270)) ;
#15495 = EDGE_LOOP('',(#38271,#38272,#38273,#38274,#38275,#38276,#38277,#38278,
#38279,#38280,#38281,#38282)) ;
#15496 = EDGE_LOOP('',(#38283,#38284,#38285,#38286,#38287)) ;
#15497 = EDGE_LOOP('',(#38288,#38289,#38290,#38291)) ;
#15498 = EDGE_LOOP('',(#38292,#38293,#38294,#38295)) ;
#15499 = EDGE_LOOP('',(#38296,#38297,#38298,#38299)) ;
#15500 = EDGE_LOOP('',(#38300,#38301,#38302)) ;
#15501 = EDGE_LOOP('',(#38303,#38304,#38305)) ;
#15502 = EDGE_LOOP('',(#38306,#38307,#38308,#38309)) ;
#15503 = EDGE_LOOP('',(#38310,#38311,#38312)) ;
#15504 = EDGE_LOOP('',(#38313,#38314,#38315,#38316)) ;
#15505 = EDGE_LOOP('',(#38317,#38318,#38319,#38320)) ;
#15506 = EDGE_LOOP('',(#38321,#38322,#38323,#38324)) ;
#15507 = EDGE_LOOP('',(#38325,#38326,#38327,#38328)) ;
#15508 = EDGE_LOOP('',(#38329,#38330,#38331,#38332)) ;
#15509 = EDGE_LOOP('',(#38333,#38334,#38335)) ;
#15510 = EDGE_LOOP('',(#38336,#38337,#38338,#38339)) ;
#15511 = EDGE_LOOP('',(#38340,#38341,#38342,#38343)) ;
#15512 = EDGE_LOOP('',(#38344,#38345,#38346,#38347)) ;
#15513 = EDGE_LOOP('',(#38348,#38349,#38350,#38351)) ;
#15514 = EDGE_LOOP('',(#38352,#38353,#38354,#38355)) ;
#15515 = EDGE_LOOP('',(#38356,#38357,#38358,#38359)) ;
#15516 = EDGE_LOOP('',(#38360,#38361,#38362,#38363)) ;
#15517 = EDGE_LOOP('',(#38364,#38365,#38366,#38367)) ;
#15518 = EDGE_LOOP('',(#38368,#38369,#38370,#38371)) ;
#15519 = EDGE_LOOP('',(#38372,#38373,#38374,#38375)) ;
#15520 = EDGE_LOOP('',(#38376,#38377,#38378,#38379)) ;
#15521 = EDGE_LOOP('',(#38380,#38381,#38382,#38383)) ;
#15522 = EDGE_LOOP('',(#38384,#38385,#38386,#38387)) ;
#15523 = EDGE_LOOP('',(#38388,#38389,#38390,#38391)) ;
#15524 = EDGE_LOOP('',(#38392,#38393,#38394,#38395)) ;
#15525 = EDGE_LOOP('',(#38396,#38397,#38398)) ;
#15526 = EDGE_LOOP('',(#38399,#38400,#38401)) ;
#15527 = EDGE_LOOP('',(#38402,#38403,#38404,#38405)) ;
#15528 = EDGE_LOOP('',(#38406,#38407,#38408,#38409)) ;
#15529 = EDGE_LOOP('',(#38410,#38411,#38412)) ;
#15530 = EDGE_LOOP('',(#38413,#38414,#38415,#38416)) ;
#15531 = EDGE_LOOP('',(#38417,#38418,#38419,#38420,#38421)) ;
#15532 = EDGE_LOOP('',(#38422,#38423,#38424,#38425)) ;
#15533 = EDGE_LOOP('',(#38426,#38427,#38428,#38429)) ;
#15534 = EDGE_LOOP('',(#38430,#38431,#38432,#38433)) ;
#15535 = EDGE_LOOP('',(#38434,#38435,#38436,#38437)) ;
#15536 = EDGE_LOOP('',(#38438,#38439,#38440,#38441,#38442,#38443,#38444)) ;
#15537 = EDGE_LOOP('',(#38445,#38446,#38447,#38448)) ;
#15538 = EDGE_LOOP('',(#38449,#38450,#38451,#38452)) ;
#15539 = EDGE_LOOP('',(#38453,#38454,#38455,#38456,#38457,#38458,#38459,#38460)) ;
#15540 = EDGE_LOOP('',(#38461,#38462,#38463,#38464,#38465)) ;
#15541 = EDGE_LOOP('',(#38466,#38467,#38468,#38469)) ;
#15542 = EDGE_LOOP('',(#38470,#38471,#38472,#38473)) ;
#15543 = EDGE_LOOP('',(#38474,#38475,#38476,#38477)) ;
#15544 = EDGE_LOOP('',(#38478,#38479,#38480,#38481,#38482)) ;
#15545 = EDGE_LOOP('',(#38483,#38484,#38485,#38486)) ;
#15546 = EDGE_LOOP('',(#38487,#38488,#38489,#38490)) ;
#15547 = EDGE_LOOP('',(#38491,#38492,#38493,#38494)) ;
#15548 = EDGE_LOOP('',(#38495,#38496,#38497,#38498)) ;
#15549 = EDGE_LOOP('',(#38499,#38500,#38501,#38502)) ;
#15550 = EDGE_LOOP('',(#38503,#38504,#38505,#38506)) ;
#15551 = EDGE_LOOP('',(#38507,#38508,#38509,#38510)) ;
#15552 = EDGE_LOOP('',(#38511,#38512,#38513,#38514)) ;
#15553 = EDGE_LOOP('',(#38515,#38516,#38517,#38518)) ;
#15554 = EDGE_LOOP('',(#38519,#38520,#38521,#38522)) ;
#15555 = EDGE_LOOP('',(#38523,#38524,#38525,#38526)) ;
#15556 = EDGE_LOOP('',(#38527,#38528,#38529,#38530)) ;
#15557 = EDGE_LOOP('',(#38531,#38532,#38533,#38534)) ;
#15558 = EDGE_LOOP('',(#38535,#38536,#38537,#38538)) ;
#15559 = EDGE_LOOP('',(#38539,#38540,#38541,#38542)) ;
#15560 = EDGE_LOOP('',(#38543,#38544,#38545,#38546)) ;
#15561 = EDGE_LOOP('',(#38547,#38548,#38549,#38550)) ;
#15562 = EDGE_LOOP('',(#38551,#38552,#38553,#38554)) ;
#15563 = EDGE_LOOP('',(#38555,#38556,#38557,#38558)) ;
#15564 = EDGE_LOOP('',(#38559,#38560,#38561,#38562)) ;
#15565 = EDGE_LOOP('',(#38563,#38564,#38565,#38566)) ;
#15566 = EDGE_LOOP('',(#38567,#38568,#38569,#38570)) ;
#15567 = EDGE_LOOP('',(#38571,#38572,#38573,#38574)) ;
#15568 = EDGE_LOOP('',(#38575,#38576,#38577,#38578)) ;
#15569 = EDGE_LOOP('',(#38579,#38580,#38581,#38582)) ;
#15570 = EDGE_LOOP('',(#38583,#38584,#38585,#38586)) ;
#15571 = EDGE_LOOP('',(#38587,#38588,#38589,#38590)) ;
#15572 = EDGE_LOOP('',(#38591,#38592,#38593,#38594)) ;
#15573 = EDGE_LOOP('',(#38595,#38596,#38597,#38598)) ;
#15574 = EDGE_LOOP('',(#38599,#38600,#38601,#38602,#38603,#38604,#38605,#38606,
#38607,#38608,#38609,#38610,#38611,#38612,#38613,#38614,#38615,#38616,#38617)) ;
#15575 = EDGE_LOOP('',(#38618,#38619,#38620,#38621,#38622,#38623,#38624,#38625)) ;
#15576 = EDGE_LOOP('',(#38626,#38627,#38628,#38629,#38630,#38631,#38632,#38633,
#38634,#38635,#38636,#38637,#38638,#38639,#38640,#38641,#38642,#38643)) ;
#15577 = EDGE_LOOP('',(#38644,#38645,#38646,#38647)) ;
#15578 = EDGE_LOOP('',(#38648,#38649,#38650,#38651,#38652,#38653,#38654,#38655,
#38656,#38657,#38658,#38659,#38660,#38661,#38662,#38663,#38664,#38665,#38666)) ;
#15579 = EDGE_LOOP('',(#38667,#38668,#38669,#38670)) ;
#15580 = EDGE_LOOP('',(#38671,#38672,#38673,#38674)) ;
#15581 = EDGE_LOOP('',(#38675,#38676,#38677,#38678)) ;
#15582 = EDGE_LOOP('',(#38679,#38680,#38681,#38682)) ;
#15583 = EDGE_LOOP('',(#38683,#38684,#38685,#38686)) ;
#15584 = EDGE_LOOP('',(#38687,#38688,#38689,#38690,#38691)) ;
#15585 = EDGE_LOOP('',(#38692,#38693,#38694,#38695,#38696)) ;
#15586 = EDGE_LOOP('',(#38697,#38698,#38699,#38700,#38701,#38702,#38703)) ;
#15587 = EDGE_LOOP('',(#38704,#38705,#38706,#38707)) ;
#15588 = EDGE_LOOP('',(#38708,#38709,#38710,#38711,#38712)) ;
#15589 = EDGE_LOOP('',(#38713,#38714,#38715,#38716,#38717,#38718,#38719)) ;
#15590 = EDGE_LOOP('',(#38720,#38721,#38722,#38723)) ;
#15591 = EDGE_LOOP('',(#38724,#38725,#38726,#38727)) ;
#15592 = EDGE_LOOP('',(#38728,#38729,#38730,#38731)) ;
#15593 = EDGE_LOOP('',(#38732,#38733,#38734,#38735)) ;
#15594 = EDGE_LOOP('',(#38736,#38737,#38738,#38739,#38740)) ;
#15595 = EDGE_LOOP('',(#38741,#38742,#38743,#38744)) ;
#15596 = EDGE_LOOP('',(#38745,#38746,#38747,#38748,#38749)) ;
#15597 = EDGE_LOOP('',(#38750,#38751,#38752,#38753)) ;
#15598 = EDGE_LOOP('',(#38754,#38755,#38756)) ;
#15599 = EDGE_LOOP('',(#38757,#38758,#38759,#38760,#38761,#38762,#38763,#38764,
#38765,#38766,#38767,#38768,#38769,#38770,#38771,#38772,#38773)) ;
#15600 = EDGE_LOOP('',(#38774,#38775,#38776,#38777,#38778)) ;
#15601 = EDGE_LOOP('',(#38779,#38780,#38781,#38782)) ;
#15602 = EDGE_LOOP('',(#38783,#38784,#38785,#38786)) ;
#15603 = EDGE_LOOP('',(#38787,#38788,#38789)) ;
#15604 = EDGE_LOOP('',(#38790,#38791,#38792,#38793,#38794)) ;
#15605 = EDGE_LOOP('',(#38795,#38796,#38797,#38798,#38799)) ;
#15606 = EDGE_LOOP('',(#38800,#38801,#38802,#38803,#38804)) ;
#15607 = EDGE_LOOP('',(#38805,#38806,#38807,#38808,#38809)) ;
#15608 = EDGE_LOOP('',(#38810,#38811,#38812,#38813)) ;
#15609 = EDGE_LOOP('',(#38814,#38815,#38816,#38817)) ;
#15610 = EDGE_LOOP('',(#38818,#38819,#38820,#38821,#38822)) ;
#15611 = EDGE_LOOP('',(#38823,#38824,#38825,#38826,#38827,#38828,#38829,#38830,
#38831,#38832,#38833,#38834,#38835,#38836,#38837,#38838)) ;
#15612 = EDGE_LOOP('',(#38839,#38840,#38841,#38842,#38843)) ;
#15613 = EDGE_LOOP('',(#38844,#38845,#38846,#38847,#38848)) ;
#15614 = EDGE_LOOP('',(#38849,#38850,#38851)) ;
#15615 = EDGE_LOOP('',(#38852,#38853,#38854,#38855)) ;
#15616 = EDGE_LOOP('',(#38856,#38857,#38858,#38859,#38860,#38861)) ;
#15617 = EDGE_LOOP('',(#38862,#38863,#38864,#38865,#38866,#38867,#38868,#38869,
#38870)) ;
#15618 = EDGE_LOOP('',(#38871,#38872,#38873,#38874)) ;
#15619 = EDGE_LOOP('',(#38875,#38876,#38877,#38878,#38879)) ;
#15620 = EDGE_LOOP('',(#38880,#38881,#38882,#38883)) ;
#15621 = EDGE_LOOP('',(#38884,#38885,#38886,#38887)) ;
#15622 = EDGE_LOOP('',(#38888,#38889,#38890,#38891,#38892,#38893)) ;
#15623 = EDGE_LOOP('',(#38894,#38895,#38896,#38897)) ;
#15624 = EDGE_LOOP('',(#38898,#38899,#38900,#38901)) ;
#15625 = EDGE_LOOP('',(#38902,#38903,#38904,#38905,#38906)) ;
#15626 = EDGE_LOOP('',(#38907,#38908,#38909,#38910)) ;
#15627 = EDGE_LOOP('',(#38911,#38912,#38913,#38914,#38915,#38916,#38917,#38918,
#38919)) ;
#15628 = EDGE_LOOP('',(#38920,#38921,#38922,#38923)) ;
#15629 = EDGE_LOOP('',(#38924,#38925,#38926,#38927)) ;
#15630 = EDGE_LOOP('',(#38928,#38929,#38930,#38931)) ;
#15631 = EDGE_LOOP('',(#38932,#38933,#38934,#38935,#38936,#38937,#38938)) ;
#15632 = EDGE_LOOP('',(#38939,#38940,#38941,#38942)) ;
#15633 = EDGE_LOOP('',(#38943,#38944,#38945,#38946,#38947)) ;
#15634 = EDGE_LOOP('',(#38948,#38949,#38950,#38951)) ;
#15635 = EDGE_LOOP('',(#38952,#38953,#38954,#38955)) ;
#15636 = EDGE_LOOP('',(#38956,#38957,#38958,#38959)) ;
#15637 = EDGE_LOOP('',(#38960,#38961,#38962,#38963)) ;
#15638 = EDGE_LOOP('',(#38964,#38965,#38966,#38967)) ;
#15639 = EDGE_LOOP('',(#38968,#38969,#38970,#38971)) ;
#15640 = EDGE_LOOP('',(#38972,#38973,#38974,#38975)) ;
#15641 = EDGE_LOOP('',(#38976,#38977,#38978,#38979,#38980,#38981)) ;
#15642 = EDGE_LOOP('',(#38982,#38983,#38984,#38985,#38986,#38987,#38988,#38989,
#38990)) ;
#15643 = EDGE_LOOP('',(#38991,#38992,#38993,#38994)) ;
#15644 = EDGE_LOOP('',(#38995,#38996,#38997,#38998,#38999,#39000,#39001,#39002)) ;
#15645 = EDGE_LOOP('',(#39003,#39004,#39005,#39006,#39007)) ;
#15646 = EDGE_LOOP('',(#39008,#39009,#39010)) ;
#15647 = EDGE_LOOP('',(#39011,#39012,#39013,#39014)) ;
#15648 = EDGE_LOOP('',(#39015,#39016,#39017,#39018)) ;
#15649 = EDGE_LOOP('',(#39019,#39020,#39021,#39022)) ;
#15650 = EDGE_LOOP('',(#39023,#39024,#39025,#39026)) ;
#15651 = EDGE_LOOP('',(#39027,#39028,#39029,#39030)) ;
#15652 = EDGE_LOOP('',(#39031,#39032,#39033,#39034)) ;
#15653 = EDGE_LOOP('',(#39035,#39036,#39037,#39038)) ;
#15654 = EDGE_LOOP('',(#39039,#39040,#39041,#39042)) ;
#15655 = EDGE_LOOP('',(#39043,#39044,#39045,#39046)) ;
#15656 = EDGE_LOOP('',(#39047,#39048,#39049,#39050)) ;
#15657 = EDGE_LOOP('',(#39051,#39052,#39053,#39054,#39055,#39056,#39057,#39058,
#39059,#39060,#39061,#39062,#39063,#39064,#39065,#39066,#39067,#39068)) ;
#15658 = EDGE_LOOP('',(#39069,#39070,#39071,#39072)) ;
#15659 = EDGE_LOOP('',(#39073,#39074,#39075,#39076,#39077)) ;
#15660 = EDGE_LOOP('',(#39078,#39079,#39080,#39081,#39082)) ;
#15661 = EDGE_LOOP('',(#39083,#39084,#39085,#39086)) ;
#15662 = EDGE_LOOP('',(#39087,#39088,#39089,#39090,#39091)) ;
#15663 = EDGE_LOOP('',(#39092,#39093,#39094,#39095)) ;
#15664 = EDGE_LOOP('',(#39096,#39097,#39098,#39099)) ;
#15665 = EDGE_LOOP('',(#39100,#39101,#39102,#39103,#39104,#39105,#39106)) ;
#15666 = EDGE_LOOP('',(#39107,#39108,#39109,#39110)) ;
#15667 = EDGE_LOOP('',(#39111,#39112,#39113,#39114)) ;
#15668 = EDGE_LOOP('',(#39115,#39116,#39117,#39118)) ;
#15669 = EDGE_LOOP('',(#39119,#39120,#39121,#39122)) ;
#15670 = EDGE_LOOP('',(#39123,#39124,#39125,#39126)) ;
#15671 = EDGE_LOOP('',(#39127,#39128,#39129,#39130)) ;
#15672 = EDGE_LOOP('',(#39131,#39132,#39133,#39134)) ;
#15673 = EDGE_LOOP('',(#39135,#39136,#39137,#39138,#39139)) ;
#15674 = EDGE_LOOP('',(#39140,#39141,#39142,#39143)) ;
#15675 = EDGE_LOOP('',(#39144,#39145,#39146,#39147)) ;
#15676 = EDGE_LOOP('',(#39148,#39149,#39150,#39151)) ;
#15677 = EDGE_LOOP('',(#39152,#39153,#39154,#39155)) ;
#15678 = EDGE_LOOP('',(#39156,#39157,#39158,#39159)) ;
#15679 = EDGE_LOOP('',(#39160,#39161,#39162,#39163)) ;
#15680 = EDGE_LOOP('',(#39164,#39165,#39166,#39167)) ;
#15681 = EDGE_LOOP('',(#39168,#39169,#39170,#39171)) ;
#15682 = EDGE_LOOP('',(#39172,#39173,#39174,#39175,#39176,#39177,#39178,#39179,
#39180)) ;
#15683 = EDGE_LOOP('',(#39181,#39182,#39183,#39184)) ;
#15684 = EDGE_LOOP('',(#39185,#39186,#39187,#39188,#39189,#39190)) ;
#15685 = EDGE_LOOP('',(#39191,#39192,#39193,#39194)) ;
#15686 = EDGE_LOOP('',(#39195,#39196,#39197,#39198)) ;
#15687 = EDGE_LOOP('',(#39199,#39200,#39201,#39202,#39203)) ;
#15688 = EDGE_LOOP('',(#39204,#39205,#39206,#39207)) ;
#15689 = EDGE_LOOP('',(#39208,#39209,#39210,#39211)) ;
#15690 = EDGE_LOOP('',(#39212,#39213,#39214,#39215)) ;
#15691 = EDGE_LOOP('',(#39216,#39217,#39218,#39219)) ;
#15692 = EDGE_LOOP('',(#39220,#39221,#39222,#39223)) ;
#15693 = EDGE_LOOP('',(#39224,#39225,#39226,#39227,#39228,#39229,#39230)) ;
#15694 = EDGE_LOOP('',(#39231,#39232,#39233,#39234,#39235,#39236,#39237,#39238,
#39239)) ;
#15695 = EDGE_LOOP('',(#39240,#39241,#39242)) ;
#15696 = EDGE_LOOP('',(#39243,#39244,#39245,#39246,#39247,#39248)) ;
#15697 = EDGE_LOOP('',(#39249,#39250,#39251,#39252)) ;
#15698 = EDGE_LOOP('',(#39253,#39254,#39255,#39256)) ;
#15699 = EDGE_LOOP('',(#39257,#39258,#39259,#39260)) ;
#15700 = EDGE_LOOP('',(#39261,#39262,#39263,#39264)) ;
#15701 = EDGE_LOOP('',(#39265,#39266,#39267,#39268)) ;
#15702 = EDGE_LOOP('',(#39269,#39270,#39271,#39272)) ;
#15703 = EDGE_LOOP('',(#39273,#39274,#39275,#39276,#39277,#39278,#39279,#39280)) ;
#15704 = EDGE_LOOP('',(#39281,#39282,#39283)) ;
#15705 = EDGE_LOOP('',(#39284,#39285,#39286,#39287)) ;
#15706 = EDGE_LOOP('',(#39288,#39289,#39290,#39291)) ;
#15707 = EDGE_LOOP('',(#39292,#39293,#39294,#39295,#39296,#39297)) ;
#15708 = EDGE_LOOP('',(#39298,#39299,#39300,#39301,#39302)) ;
#15709 = EDGE_LOOP('',(#39303,#39304,#39305,#39306)) ;
#15710 = EDGE_LOOP('',(#39307,#39308,#39309)) ;
#15711 = EDGE_LOOP('',(#39310,#39311,#39312,#39313)) ;
#15712 = EDGE_LOOP('',(#39314,#39315,#39316,#39317)) ;
#15713 = EDGE_LOOP('',(#39318,#39319,#39320,#39321)) ;
#15714 = EDGE_LOOP('',(#39322,#39323,#39324,#39325)) ;
#15715 = EDGE_LOOP('',(#39326,#39327,#39328,#39329)) ;
#15716 = EDGE_LOOP('',(#39330,#39331,#39332,#39333)) ;
#15717 = EDGE_LOOP('',(#39334,#39335,#39336,#39337,#39338,#39339,#39340,#39341,
#39342,#39343,#39344,#39345,#39346,#39347,#39348,#39349,#39350,#39351,#39352,
#39353,#39354,#39355,#39356,#39357,#39358,#39359,#39360,#39361,#39362,#39363,
#39364,#39365,#39366,#39367,#39368,#39369,#39370,#39371,#39372,#39373,#39374,
#39375,#39376,#39377,#39378,#39379,#39380,#39381,#39382,#39383,#39384,#39385,
#39386,#39387,#39388,#39389,#39390,#39391,#39392,#39393,#39394,#39395,#39396,
#39397,#39398,#39399,#39400,#39401,#39402,#39403,#39404,#39405,#39406,#39407,
#39408,#39409,#39410,#39411,#39412,#39413,#39414,#39415,#39416,#39417,#39418,
#39419,#39420,#39421,#39422,#39423,#39424,#39425,#39426,#39427,#39428,#39429,
#39430,#39431,#39432,#39433,#39434,#39435,#39436,#39437,#39438,#39439,#39440,
#39441,#39442,#39443,#39444)) ;
#15718 = EDGE_LOOP('',(#39445,#39446,#39447,#39448,#39449,#39450,#39451,#39452)) ;
#15719 = EDGE_LOOP('',(#39453)) ;
#15720 = EDGE_LOOP('',(#39454,#39455,#39456,#39457,#39458,#39459,#39460,#39461,
#39462,#39463,#39464,#39465,#39466,#39467)) ;
#15721 = EDGE_LOOP('',(#39468)) ;
#15722 = EDGE_LOOP('',(#39469,#39470,#39471,#39472,#39473,#39474,#39475,#39476,
#39477,#39478,#39479,#39480)) ;
#15723 = EDGE_LOOP('',(#39481,#39482,#39483,#39484,#39485,#39486,#39487,#39488,
#39489,#39490,#39491,#39492,#39493,#39494,#39495)) ;
#15724 = EDGE_LOOP('',(#39496,#39497,#39498,#39499,#39500,#39501,#39502,#39503,
#39504,#39505,#39506,#39507,#39508,#39509)) ;
#15725 = EDGE_LOOP('',(#39510,#39511,#39512,#39513)) ;
#15726 = EDGE_LOOP('',(#39514,#39515,#39516,#39517)) ;
#15727 = EDGE_LOOP('',(#39518,#39519,#39520,#39521,#39522)) ;
#15728 = EDGE_LOOP('',(#39523,#39524,#39525,#39526)) ;
#15729 = EDGE_LOOP('',(#39527,#39528,#39529,#39530)) ;
#15730 = EDGE_LOOP('',(#39531,#39532,#39533,#39534)) ;
#15731 = EDGE_LOOP('',(#39535,#39536,#39537,#39538)) ;
#15732 = EDGE_LOOP('',(#39539,#39540,#39541,#39542,#39543,#39544,#39545)) ;
#15733 = EDGE_LOOP('',(#39546,#39547,#39548,#39549,#39550,#39551,#39552,#39553)) ;
#15734 = EDGE_LOOP('',(#39554,#39555,#39556,#39557,#39558,#39559)) ;
#15735 = EDGE_LOOP('',(#39560,#39561,#39562)) ;
#15736 = EDGE_LOOP('',(#39563,#39564,#39565,#39566)) ;
#15737 = EDGE_LOOP('',(#39567,#39568,#39569,#39570)) ;
#15738 = EDGE_LOOP('',(#39571,#39572,#39573,#39574)) ;
#15739 = EDGE_LOOP('',(#39575,#39576,#39577,#39578)) ;
#15740 = EDGE_LOOP('',(#39579,#39580,#39581,#39582)) ;
#15741 = EDGE_LOOP('',(#39583,#39584,#39585,#39586)) ;
#15742 = EDGE_LOOP('',(#39587,#39588,#39589,#39590)) ;
#15743 = EDGE_LOOP('',(#39591,#39592,#39593,#39594)) ;
#15744 = EDGE_LOOP('',(#39595,#39596,#39597,#39598)) ;
#15745 = EDGE_LOOP('',(#39599,#39600,#39601,#39602,#39603)) ;
#15746 = EDGE_LOOP('',(#39604,#39605,#39606,#39607)) ;
#15747 = EDGE_LOOP('',(#39608,#39609,#39610,#39611)) ;
#15748 = EDGE_LOOP('',(#39612,#39613,#39614,#39615)) ;
#15749 = EDGE_LOOP('',(#39616,#39617,#39618,#39619)) ;
#15750 = EDGE_LOOP('',(#39620,#39621,#39622,#39623)) ;
#15751 = EDGE_LOOP('',(#39624,#39625,#39626,#39627)) ;
#15752 = EDGE_LOOP('',(#39628,#39629,#39630,#39631)) ;
#15753 = EDGE_LOOP('',(#39632,#39633,#39634,#39635)) ;
#15754 = EDGE_LOOP('',(#39636,#39637,#39638,#39639)) ;
#15755 = EDGE_LOOP('',(#39640,#39641,#39642,#39643,#39644,#39645,#39646,#39647,
#39648,#39649,#39650,#39651,#39652,#39653,#39654,#39655,#39656,#39657)) ;
#15756 = EDGE_LOOP('',(#39658,#39659,#39660,#39661,#39662,#39663)) ;
#15757 = EDGE_LOOP('',(#39664,#39665,#39666,#39667)) ;
#15758 = EDGE_LOOP('',(#39668,#39669,#39670,#39671)) ;
#15759 = EDGE_LOOP('',(#39672,#39673,#39674,#39675)) ;
#15760 = EDGE_LOOP('',(#39676,#39677,#39678,#39679,#39680,#39681,#39682,#39683,
#39684,#39685,#39686,#39687,#39688)) ;
#15761 = EDGE_LOOP('',(#39689,#39690,#39691,#39692)) ;
#15762 = EDGE_LOOP('',(#39693,#39694,#39695,#39696)) ;
#15763 = EDGE_LOOP('',(#39697,#39698,#39699,#39700)) ;
#15764 = EDGE_LOOP('',(#39701,#39702,#39703,#39704,#39705,#39706)) ;
#15765 = EDGE_LOOP('',(#39707,#39708,#39709,#39710)) ;
#15766 = EDGE_LOOP('',(#39711,#39712,#39713,#39714)) ;
#15767 = EDGE_LOOP('',(#39715,#39716,#39717,#39718)) ;
#15768 = EDGE_LOOP('',(#39719,#39720,#39721,#39722)) ;
#15769 = EDGE_LOOP('',(#39723,#39724,#39725,#39726)) ;
#15770 = EDGE_LOOP('',(#39727,#39728,#39729,#39730)) ;
#15771 = EDGE_LOOP('',(#39731,#39732,#39733,#39734)) ;
#15772 = EDGE_LOOP('',(#39735,#39736,#39737,#39738)) ;
#15773 = EDGE_LOOP('',(#39739,#39740,#39741,#39742)) ;
#15774 = EDGE_LOOP('',(#39743,#39744,#39745,#39746)) ;
#15775 = EDGE_LOOP('',(#39747,#39748,#39749,#39750)) ;
#15776 = EDGE_LOOP('',(#39751,#39752,#39753,#39754)) ;
#15777 = EDGE_LOOP('',(#39755,#39756,#39757,#39758)) ;
#15778 = EDGE_LOOP('',(#39759,#39760,#39761,#39762)) ;
#15779 = EDGE_LOOP('',(#39763,#39764,#39765,#39766)) ;
#15780 = EDGE_LOOP('',(#39767,#39768,#39769,#39770)) ;
#15781 = EDGE_LOOP('',(#39771,#39772,#39773,#39774)) ;
#15782 = EDGE_LOOP('',(#39775,#39776,#39777,#39778)) ;
#15783 = EDGE_LOOP('',(#39779,#39780,#39781,#39782)) ;
#15784 = EDGE_LOOP('',(#39783,#39784,#39785,#39786)) ;
#15785 = EDGE_LOOP('',(#39787,#39788,#39789,#39790)) ;
#15786 = EDGE_LOOP('',(#39791,#39792,#39793,#39794)) ;
#15787 = EDGE_LOOP('',(#39795,#39796,#39797,#39798)) ;
#15788 = EDGE_LOOP('',(#39799,#39800,#39801,#39802)) ;
#15789 = EDGE_LOOP('',(#39803,#39804,#39805,#39806)) ;
#15790 = EDGE_LOOP('',(#39807,#39808,#39809,#39810)) ;
#15791 = EDGE_LOOP('',(#39811,#39812,#39813,#39814)) ;
#15792 = EDGE_LOOP('',(#39815,#39816,#39817,#39818)) ;
#15793 = EDGE_LOOP('',(#39819,#39820,#39821,#39822)) ;
#15794 = EDGE_LOOP('',(#39823,#39824,#39825,#39826)) ;
#15795 = EDGE_LOOP('',(#39827,#39828,#39829,#39830)) ;
#15796 = EDGE_LOOP('',(#39831,#39832,#39833,#39834)) ;
#15797 = EDGE_LOOP('',(#39835,#39836,#39837,#39838,#39839,#39840,#39841)) ;
#15798 = EDGE_LOOP('',(#39842,#39843,#39844,#39845,#39846,#39847,#39848)) ;
#15799 = EDGE_LOOP('',(#39849,#39850,#39851,#39852,#39853)) ;
#15800 = EDGE_LOOP('',(#39854,#39855,#39856,#39857)) ;
#15801 = EDGE_LOOP('',(#39858,#39859,#39860,#39861)) ;
#15802 = EDGE_LOOP('',(#39862,#39863,#39864,#39865)) ;
#15803 = EDGE_LOOP('',(#39866,#39867,#39868,#39869,#39870)) ;
#15804 = EDGE_LOOP('',(#39871,#39872,#39873,#39874,#39875,#39876,#39877,#39878,
#39879,#39880)) ;
#15805 = EDGE_LOOP('',(#39881,#39882,#39883,#39884)) ;
#15806 = EDGE_LOOP('',(#39885,#39886,#39887,#39888,#39889,#39890,#39891,#39892,
#39893,#39894)) ;
#15807 = EDGE_LOOP('',(#39895,#39896,#39897,#39898,#39899)) ;
#15808 = EDGE_LOOP('',(#39900,#39901,#39902,#39903,#39904,#39905,#39906,#39907)) ;
#15809 = EDGE_LOOP('',(#39908,#39909,#39910,#39911)) ;
#15810 = EDGE_LOOP('',(#39912,#39913,#39914,#39915)) ;
#15811 = EDGE_LOOP('',(#39916,#39917,#39918,#39919)) ;
#15812 = EDGE_LOOP('',(#39920,#39921,#39922,#39923)) ;
#15813 = EDGE_LOOP('',(#39924,#39925,#39926,#39927)) ;
#15814 = EDGE_LOOP('',(#39928,#39929,#39930,#39931)) ;
#15815 = EDGE_LOOP('',(#39932,#39933,#39934,#39935)) ;
#15816 = EDGE_LOOP('',(#39936,#39937,#39938,#39939)) ;
#15817 = EDGE_LOOP('',(#39940,#39941,#39942,#39943)) ;
#15818 = EDGE_LOOP('',(#39944,#39945,#39946,#39947)) ;
#15819 = EDGE_LOOP('',(#39948,#39949,#39950,#39951)) ;
#15820 = EDGE_LOOP('',(#39952,#39953,#39954,#39955)) ;
#15821 = EDGE_LOOP('',(#39956,#39957,#39958,#39959)) ;
#15822 = EDGE_LOOP('',(#39960,#39961,#39962,#39963)) ;
#15823 = EDGE_LOOP('',(#39964,#39965,#39966,#39967)) ;
#15824 = EDGE_LOOP('',(#39968,#39969,#39970,#39971,#39972,#39973,#39974,#39975,
#39976,#39977,#39978,#39979,#39980,#39981,#39982,#39983,#39984)) ;
#15825 = EDGE_LOOP('',(#39985,#39986,#39987,#39988)) ;
#15826 = EDGE_LOOP('',(#39989,#39990,#39991,#39992,#39993,#39994,#39995,#39996,
#39997,#39998,#39999,#40000,#40001)) ;
#15827 = EDGE_LOOP('',(#40002,#40003,#40004,#40005)) ;
#15828 = EDGE_LOOP('',(#40006,#40007,#40008,#40009,#40010)) ;
#15829 = EDGE_LOOP('',(#40011,#40012,#40013,#40014)) ;
#15830 = EDGE_LOOP('',(#40015,#40016,#40017,#40018)) ;
#15831 = EDGE_LOOP('',(#40019,#40020,#40021,#40022)) ;
#15832 = EDGE_LOOP('',(#40023,#40024,#40025,#40026)) ;
#15833 = EDGE_LOOP('',(#40027,#40028,#40029,#40030)) ;
#15834 = EDGE_LOOP('',(#40031,#40032,#40033,#40034)) ;
#15835 = EDGE_LOOP('',(#40035,#40036,#40037,#40038)) ;
#15836 = EDGE_LOOP('',(#40039,#40040,#40041,#40042)) ;
#15837 = EDGE_LOOP('',(#40043,#40044,#40045,#40046)) ;
#15838 = EDGE_LOOP('',(#40047,#40048,#40049,#40050)) ;
#15839 = EDGE_LOOP('',(#40051,#40052,#40053,#40054)) ;
#15840 = EDGE_LOOP('',(#40055,#40056,#40057,#40058)) ;
#15841 = EDGE_LOOP('',(#40059,#40060,#40061,#40062)) ;
#15842 = EDGE_LOOP('',(#40063,#40064,#40065,#40066)) ;
#15843 = EDGE_LOOP('',(#40067,#40068,#40069,#40070)) ;
#15844 = EDGE_LOOP('',(#40071,#40072,#40073,#40074)) ;
#15845 = EDGE_LOOP('',(#40075,#40076,#40077,#40078)) ;
#15846 = EDGE_LOOP('',(#40079,#40080,#40081,#40082)) ;
#15847 = EDGE_LOOP('',(#40083,#40084,#40085,#40086)) ;
#15848 = EDGE_LOOP('',(#40087,#40088,#40089,#40090)) ;
#15849 = EDGE_LOOP('',(#40091,#40092,#40093,#40094)) ;
#15850 = EDGE_LOOP('',(#40095,#40096,#40097,#40098)) ;
#15851 = EDGE_LOOP('',(#40099,#40100,#40101,#40102)) ;
#15852 = EDGE_LOOP('',(#40103,#40104,#40105,#40106)) ;
#15853 = EDGE_LOOP('',(#40107,#40108,#40109,#40110)) ;
#15854 = EDGE_LOOP('',(#40111,#40112,#40113,#40114)) ;
#15855 = EDGE_LOOP('',(#40115,#40116,#40117,#40118)) ;
#15856 = EDGE_LOOP('',(#40119,#40120,#40121,#40122)) ;
#15857 = EDGE_LOOP('',(#40123,#40124,#40125,#40126)) ;
#15858 = EDGE_LOOP('',(#40127,#40128,#40129,#40130)) ;
#15859 = EDGE_LOOP('',(#40131,#40132,#40133,#40134)) ;
#15860 = EDGE_LOOP('',(#40135,#40136,#40137,#40138)) ;
#15861 = EDGE_LOOP('',(#40139,#40140,#40141,#40142)) ;
#15862 = EDGE_LOOP('',(#40143,#40144,#40145,#40146)) ;
#15863 = EDGE_LOOP('',(#40147,#40148,#40149,#40150,#40151)) ;
#15864 = EDGE_LOOP('',(#40152,#40153,#40154,#40155)) ;
#15865 = EDGE_LOOP('',(#40156,#40157,#40158,#40159)) ;
#15866 = EDGE_LOOP('',(#40160,#40161,#40162,#40163)) ;
#15867 = EDGE_LOOP('',(#40164,#40165,#40166,#40167)) ;
#15868 = EDGE_LOOP('',(#40168,#40169,#40170,#40171)) ;
#15869 = EDGE_LOOP('',(#40172,#40173,#40174,#40175)) ;
#15870 = EDGE_LOOP('',(#40176,#40177,#40178,#40179)) ;
#15871 = EDGE_LOOP('',(#40180,#40181,#40182,#40183)) ;
#15872 = EDGE_LOOP('',(#40184,#40185,#40186,#40187)) ;
#15873 = EDGE_LOOP('',(#40188,#40189,#40190,#40191)) ;
#15874 = EDGE_LOOP('',(#40192,#40193,#40194,#40195)) ;
#15875 = EDGE_LOOP('',(#40196,#40197,#40198,#40199)) ;
#15876 = EDGE_LOOP('',(#40200,#40201,#40202,#40203)) ;
#15877 = EDGE_LOOP('',(#40204,#40205,#40206,#40207)) ;
#15878 = EDGE_LOOP('',(#40208,#40209,#40210,#40211)) ;
#15879 = EDGE_LOOP('',(#40212,#40213,#40214,#40215)) ;
#15880 = EDGE_LOOP('',(#40216,#40217,#40218,#40219)) ;
#15881 = EDGE_LOOP('',(#40220,#40221,#40222,#40223)) ;
#15882 = EDGE_LOOP('',(#40224,#40225,#40226,#40227,#40228)) ;
#15883 = EDGE_LOOP('',(#40229,#40230,#40231,#40232,#40233)) ;
#15884 = EDGE_LOOP('',(#40234,#40235,#40236,#40237)) ;
#15885 = EDGE_LOOP('',(#40238,#40239,#40240,#40241,#40242,#40243,#40244,#40245,
#40246,#40247,#40248,#40249,#40250,#40251,#40252,#40253,#40254,#40255,#40256,
#40257,#40258,#40259)) ;
#15886 = EDGE_LOOP('',(#40260,#40261,#40262,#40263,#40264,#40265,#40266)) ;
#15887 = EDGE_LOOP('',(#40267,#40268,#40269,#40270,#40271,#40272,#40273)) ;
#15888 = EDGE_LOOP('',(#40274,#40275,#40276,#40277)) ;
#15889 = EDGE_LOOP('',(#40278,#40279,#40280,#40281,#40282)) ;
#15890 = EDGE_LOOP('',(#40283,#40284,#40285,#40286,#40287,#40288,#40289)) ;
#15891 = EDGE_LOOP('',(#40290)) ;
#15892 = EDGE_LOOP('',(#40291,#40292,#40293,#40294)) ;
#15893 = EDGE_LOOP('',(#40295,#40296,#40297,#40298,#40299,#40300,#40301,#40302,
#40303,#40304)) ;
#15894 = EDGE_LOOP('',(#40305,#40306,#40307,#40308,#40309)) ;
#15895 = EDGE_LOOP('',(#40310,#40311,#40312,#40313)) ;
#15896 = EDGE_LOOP('',(#40314,#40315,#40316,#40317)) ;
#15897 = EDGE_LOOP('',(#40318,#40319,#40320,#40321)) ;
#15898 = EDGE_LOOP('',(#40322,#40323,#40324,#40325)) ;
#15899 = EDGE_LOOP('',(#40326,#40327,#40328,#40329)) ;
#15900 = EDGE_LOOP('',(#40330,#40331,#40332,#40333)) ;
#15901 = EDGE_LOOP('',(#40334,#40335,#40336,#40337)) ;
#15902 = EDGE_LOOP('',(#40338,#40339,#40340,#40341)) ;
#15903 = EDGE_LOOP('',(#40342,#40343,#40344,#40345)) ;
#15904 = EDGE_LOOP('',(#40346,#40347,#40348,#40349)) ;
#15905 = EDGE_LOOP('',(#40350,#40351,#40352,#40353)) ;
#15906 = EDGE_LOOP('',(#40354,#40355,#40356,#40357)) ;
#15907 = EDGE_LOOP('',(#40358,#40359,#40360,#40361,#40362,#40363)) ;
#15908 = EDGE_LOOP('',(#40364,#40365,#40366)) ;
#15909 = EDGE_LOOP('',(#40367,#40368,#40369,#40370,#40371,#40372,#40373,#40374)) ;
#15910 = EDGE_LOOP('',(#40375,#40376,#40377,#40378,#40379,#40380,#40381,#40382,
#40383,#40384,#40385)) ;
#15911 = EDGE_LOOP('',(#40386,#40387,#40388,#40389,#40390,#40391,#40392)) ;
#15912 = EDGE_LOOP('',(#40393,#40394,#40395,#40396)) ;
#15913 = EDGE_LOOP('',(#40397,#40398,#40399,#40400,#40401,#40402,#40403)) ;
#15914 = EDGE_LOOP('',(#40404,#40405,#40406,#40407,#40408,#40409,#40410,#40411,
#40412,#40413)) ;
#15915 = EDGE_LOOP('',(#40414,#40415,#40416,#40417)) ;
#15916 = EDGE_LOOP('',(#40418,#40419,#40420,#40421,#40422,#40423,#40424,#40425)) ;
#15917 = EDGE_LOOP('',(#40426,#40427,#40428,#40429,#40430)) ;
#15918 = EDGE_LOOP('',(#40431,#40432,#40433,#40434)) ;
#15919 = EDGE_LOOP('',(#40435,#40436,#40437,#40438)) ;
#15920 = EDGE_LOOP('',(#40439,#40440,#40441,#40442)) ;
#15921 = EDGE_LOOP('',(#40443,#40444,#40445,#40446)) ;
#15922 = EDGE_LOOP('',(#40447,#40448,#40449,#40450)) ;
#15923 = EDGE_LOOP('',(#40451,#40452,#40453,#40454,#40455,#40456)) ;
#15924 = EDGE_LOOP('',(#40457,#40458,#40459,#40460,#40461,#40462,#40463,#40464,
#40465)) ;
#15925 = EDGE_LOOP('',(#40466,#40467,#40468,#40469,#40470,#40471,#40472,#40473)) ;
#15926 = EDGE_LOOP('',(#40474,#40475,#40476,#40477)) ;
#15927 = EDGE_LOOP('',(#40478,#40479,#40480,#40481)) ;
#15928 = EDGE_LOOP('',(#40482,#40483,#40484,#40485)) ;
#15929 = EDGE_LOOP('',(#40486,#40487,#40488,#40489,#40490,#40491,#40492,#40493,
#40494,#40495)) ;
#15930 = EDGE_LOOP('',(#40496,#40497,#40498,#40499,#40500,#40501,#40502,#40503,
#40504,#40505,#40506)) ;
#15931 = EDGE_LOOP('',(#40507,#40508,#40509,#40510,#40511,#40512,#40513,#40514,
#40515,#40516,#40517)) ;
#15932 = EDGE_LOOP('',(#40518,#40519,#40520,#40521)) ;
#15933 = EDGE_LOOP('',(#40522,#40523,#40524,#40525,#40526,#40527)) ;
#15934 = EDGE_LOOP('',(#40528,#40529,#40530,#40531,#40532,#40533)) ;
#15935 = EDGE_LOOP('',(#40534,#40535,#40536,#40537,#40538)) ;
#15936 = EDGE_LOOP('',(#40539,#40540,#40541,#40542,#40543,#40544)) ;
#15937 = EDGE_LOOP('',(#40545,#40546,#40547,#40548,#40549)) ;
#15938 = EDGE_LOOP('',(#40550,#40551,#40552,#40553,#40554)) ;
#15939 = EDGE_LOOP('',(#40555,#40556,#40557,#40558)) ;
#15940 = EDGE_LOOP('',(#40559,#40560,#40561,#40562,#40563)) ;
#15941 = EDGE_LOOP('',(#40564,#40565,#40566,#40567,#40568)) ;
#15942 = EDGE_LOOP('',(#40569,#40570,#40571,#40572)) ;
#15943 = EDGE_LOOP('',(#40573,#40574,#40575,#40576)) ;
#15944 = EDGE_LOOP('',(#40577,#40578,#40579,#40580,#40581,#40582,#40583,#40584,
#40585,#40586)) ;
#15945 = EDGE_LOOP('',(#40587,#40588,#40589,#40590,#40591,#40592,#40593,#40594)) ;
#15946 = EDGE_LOOP('',(#40595,#40596,#40597,#40598)) ;
#15947 = EDGE_LOOP('',(#40599,#40600,#40601,#40602)) ;
#15948 = EDGE_LOOP('',(#40603,#40604,#40605,#40606,#40607,#40608,#40609,#40610,
#40611,#40612,#40613,#40614)) ;
#15949 = EDGE_LOOP('',(#40615,#40616,#40617,#40618,#40619,#40620,#40621,#40622)) ;
#15950 = EDGE_LOOP('',(#40623,#40624,#40625,#40626)) ;
#15951 = EDGE_LOOP('',(#40627,#40628,#40629,#40630,#40631)) ;
#15952 = EDGE_LOOP('',(#40632,#40633,#40634,#40635)) ;
#15953 = EDGE_LOOP('',(#40636,#40637,#40638,#40639,#40640,#40641)) ;
#15954 = EDGE_LOOP('',(#40642,#40643,#40644,#40645)) ;
#15955 = EDGE_LOOP('',(#40646,#40647,#40648,#40649)) ;
#15956 = EDGE_LOOP('',(#40650,#40651,#40652,#40653,#40654)) ;
#15957 = EDGE_LOOP('',(#40655,#40656,#40657,#40658)) ;
#15958 = EDGE_LOOP('',(#40659,#40660,#40661,#40662)) ;
#15959 = EDGE_LOOP('',(#40663,#40664,#40665,#40666)) ;
#15960 = EDGE_LOOP('',(#40667,#40668,#40669,#40670)) ;
#15961 = EDGE_LOOP('',(#40671,#40672,#40673,#40674)) ;
#15962 = EDGE_LOOP('',(#40675,#40676,#40677,#40678,#40679,#40680,#40681,#40682,
#40683,#40684,#40685,#40686,#40687,#40688,#40689,#40690)) ;
#15963 = EDGE_LOOP('',(#40691,#40692,#40693,#40694)) ;
#15964 = EDGE_LOOP('',(#40695,#40696,#40697,#40698)) ;
#15965 = EDGE_LOOP('',(#40699,#40700,#40701,#40702)) ;
#15966 = EDGE_LOOP('',(#40703,#40704,#40705,#40706)) ;
#15967 = EDGE_LOOP('',(#40707,#40708,#40709,#40710)) ;
#15968 = EDGE_LOOP('',(#40711,#40712,#40713,#40714,#40715)) ;
#15969 = EDGE_LOOP('',(#40716,#40717,#40718,#40719)) ;
#15970 = EDGE_LOOP('',(#40720,#40721,#40722,#40723)) ;
#15971 = EDGE_LOOP('',(#40724,#40725,#40726,#40727)) ;
#15972 = EDGE_LOOP('',(#40728,#40729,#40730,#40731,#40732)) ;
#15973 = EDGE_LOOP('',(#40733,#40734,#40735,#40736,#40737,#40738)) ;
#15974 = EDGE_LOOP('',(#40739,#40740,#40741,#40742)) ;
#15975 = EDGE_LOOP('',(#40743,#40744,#40745,#40746,#40747)) ;
#15976 = EDGE_LOOP('',(#40748,#40749,#40750,#40751,#40752,#40753)) ;
#15977 = EDGE_LOOP('',(#40754,#40755,#40756,#40757,#40758,#40759,#40760,#40761)) ;
#15978 = EDGE_LOOP('',(#40762,#40763,#40764,#40765)) ;
#15979 = EDGE_LOOP('',(#40766,#40767,#40768,#40769)) ;
#15980 = EDGE_LOOP('',(#40770,#40771,#40772,#40773)) ;
#15981 = EDGE_LOOP('',(#40774,#40775,#40776,#40777)) ;
#15982 = EDGE_LOOP('',(#40778,#40779,#40780,#40781)) ;
#15983 = EDGE_LOOP('',(#40782,#40783,#40784,#40785)) ;
#15984 = EDGE_LOOP('',(#40786,#40787,#40788,#40789)) ;
#15985 = EDGE_LOOP('',(#40790,#40791,#40792,#40793)) ;
#15986 = EDGE_LOOP('',(#40794,#40795,#40796,#40797)) ;
#15987 = EDGE_LOOP('',(#40798,#40799,#40800,#40801)) ;
#15988 = EDGE_LOOP('',(#40802,#40803,#40804,#40805)) ;
#15989 = EDGE_LOOP('',(#40806,#40807,#40808,#40809,#40810,#40811,#40812)) ;
#15990 = EDGE_LOOP('',(#40813,#40814,#40815,#40816)) ;
#15991 = EDGE_LOOP('',(#40817,#40818,#40819,#40820)) ;
#15992 = EDGE_LOOP('',(#40821,#40822,#40823,#40824)) ;
#15993 = EDGE_LOOP('',(#40825,#40826,#40827,#40828)) ;
#15994 = EDGE_LOOP('',(#40829,#40830,#40831,#40832)) ;
#15995 = EDGE_LOOP('',(#40833,#40834,#40835,#40836)) ;
#15996 = EDGE_LOOP('',(#40837,#40838,#40839,#40840)) ;
#15997 = EDGE_LOOP('',(#40841,#40842,#40843,#40844)) ;
#15998 = EDGE_LOOP('',(#40845,#40846,#40847,#40848)) ;
#15999 = EDGE_LOOP('',(#40849,#40850,#40851,#40852)) ;
#16000 = EDGE_LOOP('',(#40853,#40854,#40855,#40856)) ;
#16001 = EDGE_LOOP('',(#40857,#40858,#40859,#40860,#40861,#40862,#40863)) ;
#16002 = EDGE_LOOP('',(#40864,#40865,#40866,#40867)) ;
#16003 = EDGE_LOOP('',(#40868,#40869,#40870,#40871)) ;
#16004 = EDGE_LOOP('',(#40872,#40873,#40874,#40875)) ;
#16005 = EDGE_LOOP('',(#40876,#40877,#40878,#40879)) ;
#16006 = EDGE_LOOP('',(#40880,#40881,#40882,#40883)) ;
#16007 = EDGE_LOOP('',(#40884,#40885,#40886,#40887)) ;
#16008 = EDGE_LOOP('',(#40888,#40889,#40890,#40891)) ;
#16009 = EDGE_LOOP('',(#40892,#40893,#40894,#40895)) ;
#16010 = EDGE_LOOP('',(#40896,#40897,#40898,#40899)) ;
#16011 = EDGE_LOOP('',(#40900,#40901,#40902,#40903)) ;
#16012 = EDGE_LOOP('',(#40904,#40905,#40906,#40907)) ;
#16013 = EDGE_LOOP('',(#40908,#40909,#40910,#40911,#40912,#40913,#40914)) ;
#16014 = EDGE_LOOP('',(#40915,#40916,#40917,#40918)) ;
#16015 = EDGE_LOOP('',(#40919,#40920,#40921,#40922)) ;
#16016 = EDGE_LOOP('',(#40923,#40924,#40925,#40926)) ;
#16017 = EDGE_LOOP('',(#40927,#40928,#40929,#40930)) ;
#16018 = EDGE_LOOP('',(#40931,#40932,#40933,#40934)) ;
#16019 = EDGE_LOOP('',(#40935,#40936,#40937,#40938)) ;
#16020 = EDGE_LOOP('',(#40939,#40940,#40941,#40942)) ;
#16021 = EDGE_LOOP('',(#40943,#40944,#40945,#40946)) ;
#16022 = EDGE_LOOP('',(#40947,#40948,#40949,#40950)) ;
#16023 = EDGE_LOOP('',(#40951,#40952,#40953,#40954)) ;
#16024 = EDGE_LOOP('',(#40955,#40956,#40957,#40958)) ;
#16025 = EDGE_LOOP('',(#40959,#40960,#40961,#40962)) ;
#16026 = EDGE_LOOP('',(#40963,#40964,#40965,#40966)) ;
#16027 = EDGE_LOOP('',(#40967,#40968,#40969,#40970)) ;
#16028 = EDGE_LOOP('',(#40971,#40972,#40973,#40974)) ;
#16029 = EDGE_LOOP('',(#40975,#40976,#40977,#40978)) ;
#16030 = EDGE_LOOP('',(#40979,#40980,#40981,#40982)) ;
#16031 = EDGE_LOOP('',(#40983,#40984,#40985,#40986)) ;
#16032 = EDGE_LOOP('',(#40987,#40988,#40989,#40990,#40991,#40992,#40993)) ;
#16033 = EDGE_LOOP('',(#40994,#40995,#40996,#40997)) ;
#16034 = EDGE_LOOP('',(#40998,#40999,#41000,#41001)) ;
#16035 = EDGE_LOOP('',(#41002,#41003,#41004,#41005)) ;
#16036 = EDGE_LOOP('',(#41006,#41007,#41008,#41009)) ;
#16037 = EDGE_LOOP('',(#41010,#41011,#41012,#41013)) ;
#16038 = EDGE_LOOP('',(#41014,#41015,#41016,#41017)) ;
#16039 = EDGE_LOOP('',(#41018,#41019,#41020,#41021)) ;
#16040 = EDGE_LOOP('',(#41022,#41023,#41024,#41025)) ;
#16041 = EDGE_LOOP('',(#41026,#41027,#41028,#41029)) ;
#16042 = EDGE_LOOP('',(#41030,#41031,#41032,#41033)) ;
#16043 = EDGE_LOOP('',(#41034,#41035,#41036,#41037)) ;
#16044 = EDGE_LOOP('',(#41038,#41039,#41040,#41041)) ;
#16045 = EDGE_LOOP('',(#41042,#41043,#41044,#41045)) ;
#16046 = EDGE_LOOP('',(#41046,#41047,#41048,#41049)) ;
#16047 = EDGE_LOOP('',(#41050,#41051,#41052,#41053)) ;
#16048 = EDGE_LOOP('',(#41054,#41055,#41056,#41057)) ;
#16049 = EDGE_LOOP('',(#41058,#41059,#41060,#41061)) ;
#16050 = EDGE_LOOP('',(#41062,#41063,#41064,#41065)) ;
#16051 = EDGE_LOOP('',(#41066,#41067,#41068,#41069)) ;
#16052 = EDGE_LOOP('',(#41070,#41071,#41072,#41073)) ;
#16053 = EDGE_LOOP('',(#41074,#41075,#41076,#41077)) ;
#16054 = EDGE_LOOP('',(#41078,#41079,#41080,#41081)) ;
#16055 = EDGE_LOOP('',(#41082,#41083,#41084,#41085)) ;
#16056 = EDGE_LOOP('',(#41086,#41087,#41088,#41089)) ;
#16057 = EDGE_LOOP('',(#41090,#41091,#41092,#41093,#41094,#41095,#41096,#41097,
#41098,#41099,#41100)) ;
#16058 = EDGE_LOOP('',(#41101,#41102,#41103,#41104)) ;
#16059 = EDGE_LOOP('',(#41105,#41106,#41107,#41108)) ;
#16060 = EDGE_LOOP('',(#41109,#41110,#41111,#41112)) ;
#16061 = EDGE_LOOP('',(#41113,#41114,#41115,#41116)) ;
#16062 = EDGE_LOOP('',(#41117,#41118,#41119,#41120)) ;
#16063 = EDGE_LOOP('',(#41121,#41122,#41123,#41124)) ;
#16064 = EDGE_LOOP('',(#41125,#41126,#41127,#41128)) ;
#16065 = EDGE_LOOP('',(#41129,#41130,#41131,#41132)) ;
#16066 = EDGE_LOOP('',(#41133,#41134,#41135,#41136)) ;
#16067 = EDGE_LOOP('',(#41137,#41138,#41139,#41140)) ;
#16068 = EDGE_LOOP('',(#41141,#41142,#41143,#41144)) ;
#16069 = EDGE_LOOP('',(#41145,#41146,#41147,#41148)) ;
#16070 = EDGE_LOOP('',(#41149,#41150,#41151,#41152)) ;
#16071 = EDGE_LOOP('',(#41153,#41154,#41155,#41156)) ;
#16072 = EDGE_LOOP('',(#41157,#41158,#41159,#41160)) ;
#16073 = EDGE_LOOP('',(#41161,#41162,#41163,#41164)) ;
#16074 = EDGE_LOOP('',(#41165,#41166,#41167,#41168)) ;
#16075 = EDGE_LOOP('',(#41169,#41170,#41171,#41172,#41173,#41174,#41175,#41176,
#41177,#41178,#41179)) ;
#16076 = EDGE_LOOP('',(#41180,#41181,#41182,#41183)) ;
#16077 = EDGE_LOOP('',(#41184,#41185,#41186,#41187)) ;
#16078 = EDGE_LOOP('',(#41188,#41189,#41190,#41191)) ;
#16079 = EDGE_LOOP('',(#41192,#41193,#41194,#41195)) ;
#16080 = EDGE_LOOP('',(#41196,#41197,#41198,#41199)) ;
#16081 = EDGE_LOOP('',(#41200,#41201,#41202,#41203)) ;
#16082 = EDGE_LOOP('',(#41204,#41205,#41206,#41207)) ;
#16083 = EDGE_LOOP('',(#41208,#41209,#41210,#41211)) ;
#16084 = EDGE_LOOP('',(#41212,#41213,#41214,#41215)) ;
#16085 = EDGE_LOOP('',(#41216,#41217,#41218,#41219)) ;
#16086 = EDGE_LOOP('',(#41220,#41221,#41222,#41223)) ;
#16087 = EDGE_LOOP('',(#41224,#41225,#41226,#41227)) ;
#16088 = EDGE_LOOP('',(#41228,#41229,#41230,#41231)) ;
#16089 = EDGE_LOOP('',(#41232,#41233,#41234,#41235)) ;
#16090 = EDGE_LOOP('',(#41236,#41237,#41238,#41239)) ;
#16091 = EDGE_LOOP('',(#41240,#41241,#41242,#41243)) ;
#16092 = EDGE_LOOP('',(#41244,#41245,#41246,#41247)) ;
#16093 = EDGE_LOOP('',(#41248,#41249,#41250,#41251)) ;
#16094 = EDGE_LOOP('',(#41252,#41253,#41254,#41255)) ;
#16095 = EDGE_LOOP('',(#41256,#41257,#41258,#41259)) ;
#16096 = EDGE_LOOP('',(#41260,#41261,#41262,#41263)) ;
#16097 = EDGE_LOOP('',(#41264,#41265,#41266,#41267)) ;
#16098 = EDGE_LOOP('',(#41268,#41269,#41270,#41271)) ;
#16099 = EDGE_LOOP('',(#41272,#41273,#41274,#41275)) ;
#16100 = EDGE_LOOP('',(#41276,#41277,#41278,#41279)) ;
#16101 = EDGE_LOOP('',(#41280,#41281,#41282,#41283)) ;
#16102 = EDGE_LOOP('',(#41284,#41285,#41286,#41287)) ;
#16103 = EDGE_LOOP('',(#41288,#41289,#41290,#41291)) ;
#16104 = EDGE_LOOP('',(#41292,#41293,#41294,#41295)) ;
#16105 = EDGE_LOOP('',(#41296,#41297,#41298,#41299,#41300,#41301,#41302,#41303,
#41304,#41305,#41306,#41307,#41308)) ;
#16106 = EDGE_LOOP('',(#41309,#41310,#41311,#41312)) ;
#16107 = EDGE_LOOP('',(#41313,#41314,#41315,#41316,#41317,#41318,#41319)) ;
#16108 = EDGE_LOOP('',(#41320,#41321,#41322,#41323,#41324,#41325,#41326)) ;
#16109 = EDGE_LOOP('',(#41327,#41328,#41329,#41330)) ;
#16110 = EDGE_LOOP('',(#41331,#41332,#41333,#41334)) ;
#16111 = EDGE_LOOP('',(#41335,#41336,#41337,#41338)) ;
#16112 = EDGE_LOOP('',(#41339,#41340,#41341,#41342)) ;
#16113 = EDGE_LOOP('',(#41343,#41344,#41345,#41346)) ;
#16114 = EDGE_LOOP('',(#41347,#41348,#41349,#41350)) ;
#16115 = EDGE_LOOP('',(#41351,#41352,#41353,#41354)) ;
#16116 = EDGE_LOOP('',(#41355,#41356,#41357,#41358)) ;
#16117 = EDGE_LOOP('',(#41359,#41360,#41361,#41362)) ;
#16118 = EDGE_LOOP('',(#41363,#41364,#41365,#41366)) ;
#16119 = EDGE_LOOP('',(#41367,#41368,#41369,#41370)) ;
#16120 = EDGE_LOOP('',(#41371,#41372,#41373,#41374)) ;
#16121 = EDGE_LOOP('',(#41375,#41376,#41377,#41378)) ;
#16122 = EDGE_LOOP('',(#41379,#41380,#41381,#41382)) ;
#16123 = EDGE_LOOP('',(#41383,#41384,#41385,#41386)) ;
#16124 = EDGE_LOOP('',(#41387,#41388,#41389,#41390)) ;
#16125 = EDGE_LOOP('',(#41391,#41392,#41393,#41394)) ;
#16126 = EDGE_LOOP('',(#41395,#41396,#41397,#41398)) ;
#16127 = EDGE_LOOP('',(#41399,#41400,#41401,#41402)) ;
#16128 = EDGE_LOOP('',(#41403,#41404,#41405,#41406)) ;
#16129 = EDGE_LOOP('',(#41407,#41408,#41409,#41410)) ;
#16130 = EDGE_LOOP('',(#41411,#41412,#41413,#41414)) ;
#16131 = EDGE_LOOP('',(#41415,#41416,#41417,#41418)) ;
#16132 = EDGE_LOOP('',(#41419,#41420,#41421,#41422)) ;
#16133 = EDGE_LOOP('',(#41423,#41424,#41425,#41426)) ;
#16134 = EDGE_LOOP('',(#41427,#41428,#41429,#41430)) ;
#16135 = EDGE_LOOP('',(#41431,#41432,#41433,#41434)) ;
#16136 = EDGE_LOOP('',(#41435,#41436,#41437,#41438)) ;
#16137 = EDGE_LOOP('',(#41439,#41440,#41441,#41442)) ;
#16138 = EDGE_LOOP('',(#41443,#41444,#41445,#41446)) ;
#16139 = EDGE_LOOP('',(#41447,#41448,#41449,#41450)) ;
#16140 = EDGE_LOOP('',(#41451,#41452,#41453,#41454)) ;
#16141 = EDGE_LOOP('',(#41455,#41456,#41457,#41458)) ;
#16142 = EDGE_LOOP('',(#41459,#41460,#41461,#41462)) ;
#16143 = EDGE_LOOP('',(#41463,#41464,#41465,#41466)) ;
#16144 = EDGE_LOOP('',(#41467,#41468,#41469,#41470)) ;
#16145 = EDGE_LOOP('',(#41471,#41472,#41473,#41474)) ;
#16146 = EDGE_LOOP('',(#41475,#41476,#41477,#41478)) ;
#16147 = EDGE_LOOP('',(#41479,#41480,#41481,#41482)) ;
#16148 = EDGE_LOOP('',(#41483,#41484,#41485,#41486)) ;
#16149 = EDGE_LOOP('',(#41487,#41488,#41489,#41490)) ;
#16150 = EDGE_LOOP('',(#41491,#41492,#41493,#41494)) ;
#16151 = EDGE_LOOP('',(#41495,#41496,#41497,#41498)) ;
#16152 = EDGE_LOOP('',(#41499,#41500,#41501,#41502)) ;
#16153 = EDGE_LOOP('',(#41503,#41504,#41505,#41506)) ;
#16154 = EDGE_LOOP('',(#41507,#41508,#41509,#41510)) ;
#16155 = EDGE_LOOP('',(#41511,#41512,#41513,#41514)) ;
#16156 = EDGE_LOOP('',(#41515,#41516,#41517,#41518)) ;
#16157 = EDGE_LOOP('',(#41519,#41520,#41521,#41522,#41523,#41524)) ;
#16158 = EDGE_LOOP('',(#41525,#41526,#41527,#41528)) ;
#16159 = EDGE_LOOP('',(#41529,#41530,#41531,#41532)) ;
#16160 = EDGE_LOOP('',(#41533,#41534,#41535,#41536)) ;
#16161 = EDGE_LOOP('',(#41537,#41538,#41539,#41540)) ;
#16162 = EDGE_LOOP('',(#41541,#41542,#41543,#41544)) ;
#16163 = EDGE_LOOP('',(#41545,#41546,#41547,#41548,#41549)) ;
#16164 = EDGE_LOOP('',(#41550,#41551,#41552,#41553,#41554,#41555,#41556,#41557,
#41558,#41559,#41560)) ;
#16165 = EDGE_LOOP('',(#41561,#41562,#41563,#41564,#41565)) ;
#16166 = EDGE_LOOP('',(#41566,#41567,#41568,#41569)) ;
#16167 = EDGE_LOOP('',(#41570,#41571,#41572,#41573)) ;
#16168 = EDGE_LOOP('',(#41574,#41575,#41576,#41577)) ;
#16169 = EDGE_LOOP('',(#41578,#41579,#41580,#41581)) ;
#16170 = EDGE_LOOP('',(#41582,#41583,#41584,#41585)) ;
#16171 = EDGE_LOOP('',(#41586,#41587,#41588,#41589)) ;
#16172 = EDGE_LOOP('',(#41590,#41591,#41592,#41593,#41594,#41595,#41596,#41597,
#41598,#41599,#41600,#41601,#41602,#41603,#41604,#41605,#41606)) ;
#16173 = EDGE_LOOP('',(#41607,#41608,#41609,#41610)) ;
#16174 = EDGE_LOOP('',(#41611,#41612,#41613,#41614,#41615)) ;
#16175 = EDGE_LOOP('',(#41616,#41617,#41618,#41619)) ;
#16176 = EDGE_LOOP('',(#41620,#41621,#41622,#41623)) ;
#16177 = EDGE_LOOP('',(#41624,#41625,#41626,#41627,#41628)) ;
#16178 = EDGE_LOOP('',(#41629,#41630,#41631,#41632)) ;
#16179 = EDGE_LOOP('',(#41633,#41634,#41635,#41636)) ;
#16180 = EDGE_LOOP('',(#41637,#41638,#41639,#41640)) ;
#16181 = EDGE_LOOP('',(#41641,#41642,#41643,#41644)) ;
#16182 = EDGE_LOOP('',(#41645,#41646,#41647,#41648)) ;
#16183 = EDGE_LOOP('',(#41649,#41650,#41651,#41652)) ;
#16184 = EDGE_LOOP('',(#41653,#41654,#41655,#41656,#41657)) ;
#16185 = EDGE_LOOP('',(#41658,#41659,#41660,#41661,#41662)) ;
#16186 = EDGE_LOOP('',(#41663,#41664,#41665,#41666)) ;
#16187 = EDGE_LOOP('',(#41667,#41668,#41669,#41670,#41671)) ;
#16188 = EDGE_LOOP('',(#41672,#41673,#41674,#41675,#41676,#41677,#41678,#41679)) ;
#16189 = EDGE_LOOP('',(#41680,#41681,#41682,#41683,#41684)) ;
#16190 = EDGE_LOOP('',(#41685,#41686,#41687,#41688,#41689)) ;
#16191 = EDGE_LOOP('',(#41690,#41691,#41692,#41693,#41694,#41695,#41696,#41697,
#41698,#41699,#41700,#41701,#41702,#41703,#41704)) ;
#16192 = EDGE_LOOP('',(#41705,#41706,#41707,#41708,#41709)) ;
#16193 = EDGE_LOOP('',(#41710,#41711,#41712,#41713)) ;
#16194 = EDGE_LOOP('',(#41714,#41715,#41716,#41717)) ;
#16195 = EDGE_LOOP('',(#41718,#41719,#41720,#41721)) ;
#16196 = EDGE_LOOP('',(#41722,#41723,#41724,#41725)) ;
#16197 = EDGE_LOOP('',(#41726,#41727,#41728,#41729)) ;
#16198 = EDGE_LOOP('',(#41730,#41731,#41732,#41733)) ;
#16199 = EDGE_LOOP('',(#41734,#41735,#41736,#41737)) ;
#16200 = EDGE_LOOP('',(#41738,#41739,#41740)) ;
#16201 = EDGE_LOOP('',(#41741,#41742,#41743,#41744)) ;
#16202 = EDGE_LOOP('',(#41745,#41746,#41747)) ;
#16203 = EDGE_LOOP('',(#41748,#41749,#41750,#41751)) ;
#16204 = EDGE_LOOP('',(#41752,#41753,#41754,#41755)) ;
#16205 = EDGE_LOOP('',(#41756,#41757,#41758,#41759,#41760)) ;
#16206 = EDGE_LOOP('',(#41761,#41762,#41763,#41764)) ;
#16207 = EDGE_LOOP('',(#41765,#41766,#41767,#41768)) ;
#16208 = EDGE_LOOP('',(#41769,#41770,#41771,#41772)) ;
#16209 = EDGE_LOOP('',(#41773,#41774,#41775,#41776)) ;
#16210 = EDGE_LOOP('',(#41777,#41778,#41779)) ;
#16211 = EDGE_LOOP('',(#41780,#41781,#41782,#41783)) ;
#16212 = EDGE_LOOP('',(#41784,#41785,#41786,#41787)) ;
#16213 = EDGE_LOOP('',(#41788,#41789,#41790,#41791)) ;
#16214 = EDGE_LOOP('',(#41792,#41793,#41794,#41795)) ;
#16215 = EDGE_LOOP('',(#41796,#41797,#41798,#41799)) ;
#16216 = EDGE_LOOP('',(#41800,#41801,#41802,#41803)) ;
#16217 = EDGE_LOOP('',(#41804,#41805,#41806,#41807)) ;
#16218 = EDGE_LOOP('',(#41808,#41809,#41810,#41811)) ;
#16219 = EDGE_LOOP('',(#41812,#41813,#41814,#41815)) ;
#16220 = EDGE_LOOP('',(#41816,#41817,#41818,#41819)) ;
#16221 = EDGE_LOOP('',(#41820,#41821,#41822,#41823)) ;
#16222 = EDGE_LOOP('',(#41824,#41825,#41826,#41827)) ;
#16223 = EDGE_LOOP('',(#41828,#41829,#41830,#41831)) ;
#16224 = EDGE_LOOP('',(#41832,#41833,#41834,#41835)) ;
#16225 = EDGE_LOOP('',(#41836,#41837,#41838,#41839)) ;
#16226 = EDGE_LOOP('',(#41840,#41841,#41842,#41843)) ;
#16227 = EDGE_LOOP('',(#41844,#41845,#41846,#41847)) ;
#16228 = EDGE_LOOP('',(#41848,#41849,#41850,#41851,#41852)) ;
#16229 = EDGE_LOOP('',(#41853,#41854,#41855,#41856)) ;
#16230 = EDGE_LOOP('',(#41857,#41858,#41859,#41860)) ;
#16231 = EDGE_LOOP('',(#41861,#41862,#41863,#41864)) ;
#16232 = EDGE_LOOP('',(#41865,#41866,#41867,#41868,#41869)) ;
#16233 = EDGE_LOOP('',(#41870,#41871,#41872,#41873)) ;
#16234 = EDGE_LOOP('',(#41874,#41875,#41876,#41877)) ;
#16235 = EDGE_LOOP('',(#41878,#41879,#41880,#41881)) ;
#16236 = EDGE_LOOP('',(#41882,#41883,#41884,#41885)) ;
#16237 = EDGE_LOOP('',(#41886,#41887,#41888,#41889)) ;
#16238 = EDGE_LOOP('',(#41890,#41891,#41892,#41893)) ;
#16239 = EDGE_LOOP('',(#41894,#41895,#41896,#41897)) ;
#16240 = EDGE_LOOP('',(#41898,#41899,#41900,#41901)) ;
#16241 = EDGE_LOOP('',(#41902,#41903,#41904,#41905)) ;
#16242 = EDGE_LOOP('',(#41906,#41907,#41908,#41909,#41910)) ;
#16243 = EDGE_LOOP('',(#41911,#41912,#41913,#41914)) ;
#16244 = EDGE_LOOP('',(#41915,#41916,#41917,#41918,#41919)) ;
#16245 = EDGE_LOOP('',(#41920,#41921,#41922,#41923)) ;
#16246 = EDGE_LOOP('',(#41924,#41925,#41926,#41927)) ;
#16247 = EDGE_LOOP('',(#41928,#41929,#41930,#41931)) ;
#16248 = EDGE_LOOP('',(#41932,#41933,#41934,#41935)) ;
#16249 = EDGE_LOOP('',(#41936,#41937,#41938,#41939)) ;
#16250 = EDGE_LOOP('',(#41940,#41941,#41942,#41943)) ;
#16251 = EDGE_LOOP('',(#41944,#41945,#41946,#41947)) ;
#16252 = EDGE_LOOP('',(#41948,#41949,#41950,#41951)) ;
#16253 = EDGE_LOOP('',(#41952,#41953,#41954,#41955)) ;
#16254 = EDGE_LOOP('',(#41956,#41957,#41958,#41959)) ;
#16255 = EDGE_LOOP('',(#41960,#41961,#41962,#41963)) ;
#16256 = EDGE_LOOP('',(#41964,#41965,#41966,#41967)) ;
#16257 = EDGE_LOOP('',(#41968,#41969,#41970,#41971)) ;
#16258 = EDGE_LOOP('',(#41972,#41973,#41974,#41975)) ;
#16259 = EDGE_LOOP('',(#41976,#41977,#41978,#41979)) ;
#16260 = EDGE_LOOP('',(#41980,#41981,#41982,#41983)) ;
#16261 = EDGE_LOOP('',(#41984,#41985,#41986,#41987)) ;
#16262 = EDGE_LOOP('',(#41988)) ;
#16263 = EDGE_LOOP('',(#41989,#41990,#41991,#41992)) ;
#16264 = EDGE_LOOP('',(#41993,#41994,#41995,#41996)) ;
#16265 = EDGE_LOOP('',(#41997,#41998,#41999,#42000)) ;
#16266 = EDGE_LOOP('',(#42001,#42002,#42003,#42004)) ;
#16267 = EDGE_LOOP('',(#42005,#42006,#42007,#42008)) ;
#16268 = EDGE_LOOP('',(#42009,#42010,#42011,#42012)) ;
#16269 = EDGE_LOOP('',(#42013,#42014,#42015,#42016)) ;
#16270 = EDGE_LOOP('',(#42017,#42018,#42019,#42020)) ;
#16271 = EDGE_LOOP('',(#42021,#42022,#42023,#42024)) ;
#16272 = EDGE_LOOP('',(#42025,#42026,#42027,#42028)) ;
#16273 = EDGE_LOOP('',(#42029,#42030,#42031,#42032)) ;
#16274 = EDGE_LOOP('',(#42033,#42034,#42035,#42036)) ;
#16275 = EDGE_LOOP('',(#42037,#42038,#42039,#42040)) ;
#16276 = EDGE_LOOP('',(#42041,#42042,#42043,#42044)) ;
#16277 = EDGE_LOOP('',(#42045,#42046,#42047,#42048)) ;
#16278 = EDGE_LOOP('',(#42049,#42050,#42051,#42052)) ;
#16279 = EDGE_LOOP('',(#42053,#42054,#42055,#42056)) ;
#16280 = EDGE_LOOP('',(#42057,#42058,#42059,#42060)) ;
#16281 = EDGE_LOOP('',(#42061,#42062,#42063,#42064)) ;
#16282 = EDGE_LOOP('',(#42065,#42066,#42067,#42068)) ;
#16283 = EDGE_LOOP('',(#42069,#42070,#42071,#42072)) ;
#16284 = EDGE_LOOP('',(#42073,#42074,#42075,#42076)) ;
#16285 = EDGE_LOOP('',(#42077,#42078,#42079,#42080)) ;
#16286 = EDGE_LOOP('',(#42081,#42082,#42083,#42084)) ;
#16287 = EDGE_LOOP('',(#42085,#42086,#42087,#42088)) ;
#16288 = EDGE_LOOP('',(#42089,#42090,#42091,#42092)) ;
#16289 = EDGE_LOOP('',(#42093,#42094,#42095,#42096)) ;
#16290 = EDGE_LOOP('',(#42097,#42098,#42099,#42100)) ;
#16291 = EDGE_LOOP('',(#42101,#42102,#42103,#42104,#42105,#42106)) ;
#16292 = EDGE_LOOP('',(#42107,#42108,#42109,#42110)) ;
#16293 = EDGE_LOOP('',(#42111,#42112,#42113,#42114)) ;
#16294 = EDGE_LOOP('',(#42115,#42116,#42117,#42118)) ;
#16295 = EDGE_LOOP('',(#42119,#42120,#42121,#42122)) ;
#16296 = EDGE_LOOP('',(#42123,#42124,#42125,#42126)) ;
#16297 = EDGE_LOOP('',(#42127,#42128,#42129,#42130)) ;
#16298 = EDGE_LOOP('',(#42131,#42132,#42133,#42134)) ;
#16299 = EDGE_LOOP('',(#42135,#42136,#42137,#42138)) ;
#16300 = EDGE_LOOP('',(#42139,#42140,#42141,#42142)) ;
#16301 = EDGE_LOOP('',(#42143,#42144,#42145,#42146)) ;
#16302 = EDGE_LOOP('',(#42147,#42148,#42149,#42150)) ;
#16303 = EDGE_LOOP('',(#42151,#42152,#42153,#42154)) ;
#16304 = EDGE_LOOP('',(#42155,#42156,#42157,#42158)) ;
#16305 = EDGE_LOOP('',(#42159,#42160,#42161,#42162)) ;
#16306 = EDGE_LOOP('',(#42163,#42164,#42165,#42166)) ;
#16307 = EDGE_LOOP('',(#42167,#42168,#42169,#42170)) ;
#16308 = EDGE_LOOP('',(#42171,#42172,#42173,#42174)) ;
#16309 = EDGE_LOOP('',(#42175,#42176,#42177,#42178,#42179,#42180,#42181,#42182,
#42183,#42184,#42185,#42186,#42187,#42188)) ;
#16310 = EDGE_LOOP('',(#42189,#42190,#42191,#42192)) ;
#16311 = EDGE_LOOP('',(#42193,#42194,#42195,#42196)) ;
#16312 = EDGE_LOOP('',(#42197,#42198,#42199,#42200)) ;
#16313 = EDGE_LOOP('',(#42201,#42202,#42203,#42204)) ;
#16314 = EDGE_LOOP('',(#42205,#42206,#42207,#42208)) ;
#16315 = EDGE_LOOP('',(#42209,#42210,#42211,#42212)) ;
#16316 = EDGE_LOOP('',(#42213,#42214,#42215,#42216,#42217,#42218,#42219,#42220,
#42221,#42222,#42223,#42224)) ;
#16317 = EDGE_LOOP('',(#42225,#42226,#42227,#42228)) ;
#16318 = EDGE_LOOP('',(#42229,#42230,#42231,#42232)) ;
#16319 = EDGE_LOOP('',(#42233,#42234,#42235,#42236)) ;
#16320 = EDGE_LOOP('',(#42237,#42238,#42239,#42240)) ;
#16321 = EDGE_LOOP('',(#42241,#42242,#42243,#42244)) ;
#16322 = EDGE_LOOP('',(#42245,#42246,#42247,#42248)) ;
#16323 = EDGE_LOOP('',(#42249,#42250,#42251,#42252)) ;
#16324 = EDGE_LOOP('',(#42253,#42254,#42255,#42256,#42257,#42258,#42259,#42260,
#42261,#42262,#42263,#42264,#42265,#42266,#42267)) ;
#16325 = EDGE_LOOP('',(#42268,#42269,#42270,#42271)) ;
#16326 = EDGE_LOOP('',(#42272,#42273,#42274,#42275)) ;
#16327 = EDGE_LOOP('',(#42276,#42277,#42278,#42279)) ;
#16328 = EDGE_LOOP('',(#42280,#42281,#42282,#42283)) ;
#16329 = EDGE_LOOP('',(#42284,#42285,#42286,#42287)) ;
#16330 = EDGE_LOOP('',(#42288,#42289,#42290,#42291)) ;
#16331 = EDGE_LOOP('',(#42292,#42293,#42294,#42295)) ;
#16332 = EDGE_LOOP('',(#42296,#42297,#42298,#42299,#42300,#42301,#42302,#42303,
#42304,#42305,#42306,#42307,#42308,#42309)) ;
#16333 = EDGE_LOOP('',(#42310,#42311,#42312,#42313)) ;
#16334 = EDGE_LOOP('',(#42314,#42315,#42316,#42317)) ;
#16335 = EDGE_LOOP('',(#42318,#42319,#42320,#42321)) ;
#16336 = EDGE_LOOP('',(#42322,#42323,#42324,#42325)) ;
#16337 = EDGE_LOOP('',(#42326,#42327,#42328,#42329)) ;
#16338 = EDGE_LOOP('',(#42330,#42331,#42332,#42333)) ;
#16339 = EDGE_LOOP('',(#42334,#42335,#42336,#42337)) ;
#16340 = EDGE_LOOP('',(#42338,#42339,#42340,#42341,#42342,#42343,#42344,#42345,
#42346,#42347,#42348,#42349,#42350,#42351)) ;
#16341 = EDGE_LOOP('',(#42352,#42353,#42354,#42355)) ;
#16342 = EDGE_LOOP('',(#42356,#42357,#42358,#42359)) ;
#16343 = EDGE_LOOP('',(#42360,#42361,#42362,#42363)) ;
#16344 = EDGE_LOOP('',(#42364,#42365,#42366,#42367)) ;
#16345 = EDGE_LOOP('',(#42368,#42369,#42370,#42371)) ;
#16346 = EDGE_LOOP('',(#42372,#42373,#42374,#42375)) ;
#16347 = EDGE_LOOP('',(#42376,#42377,#42378,#42379,#42380,#42381,#42382,#42383,
#42384,#42385,#42386,#42387)) ;
#16348 = EDGE_LOOP('',(#42388)) ;
#16349 = EDGE_LOOP('',(#42389,#42390,#42391,#42392)) ;
#16350 = EDGE_LOOP('',(#42393,#42394,#42395,#42396)) ;
#16351 = EDGE_LOOP('',(#42397)) ;
#16352 = EDGE_LOOP('',(#42398,#42399,#42400,#42401)) ;
#16353 = EDGE_LOOP('',(#42402,#42403,#42404,#42405,#42406,#42407)) ;
#16354 = EDGE_LOOP('',(#42408,#42409,#42410,#42411)) ;
#16355 = EDGE_LOOP('',(#42412,#42413,#42414,#42415,#42416)) ;
#16356 = EDGE_LOOP('',(#42417,#42418,#42419,#42420)) ;
#16357 = EDGE_LOOP('',(#42421,#42422,#42423,#42424)) ;
#16358 = EDGE_LOOP('',(#42425,#42426,#42427,#42428)) ;
#16359 = EDGE_LOOP('',(#42429,#42430,#42431,#42432)) ;
#16360 = EDGE_LOOP('',(#42433,#42434,#42435,#42436)) ;
#16361 = EDGE_LOOP('',(#42437,#42438,#42439,#42440,#42441,#42442,#42443)) ;
#16362 = EDGE_LOOP('',(#42444,#42445,#42446,#42447)) ;
#16363 = EDGE_LOOP('',(#42448,#42449,#42450,#42451,#42452,#42453,#42454,#42455,
#42456,#42457,#42458,#42459,#42460)) ;
#16364 = EDGE_LOOP('',(#42461,#42462,#42463,#42464)) ;
#16365 = EDGE_LOOP('',(#42465,#42466,#42467,#42468)) ;
#16366 = EDGE_LOOP('',(#42469,#42470,#42471,#42472,#42473,#42474,#42475,#42476,
#42477)) ;
#16367 = EDGE_LOOP('',(#42478,#42479,#42480,#42481)) ;
#16368 = EDGE_LOOP('',(#42482,#42483,#42484,#42485)) ;
#16369 = EDGE_LOOP('',(#42486,#42487,#42488,#42489,#42490)) ;
#16370 = EDGE_LOOP('',(#42491,#42492,#42493,#42494)) ;
#16371 = EDGE_LOOP('',(#42495,#42496,#42497,#42498)) ;
#16372 = EDGE_LOOP('',(#42499,#42500,#42501,#42502,#42503)) ;
#16373 = EDGE_LOOP('',(#42504,#42505,#42506,#42507,#42508,#42509)) ;
#16374 = EDGE_LOOP('',(#42510,#42511,#42512,#42513)) ;
#16375 = EDGE_LOOP('',(#42514,#42515,#42516,#42517,#42518,#42519,#42520,#42521)) ;
#16376 = EDGE_LOOP('',(#42522,#42523,#42524,#42525,#42526,#42527)) ;
#16377 = EDGE_LOOP('',(#42528,#42529,#42530,#42531,#42532)) ;
#16378 = EDGE_LOOP('',(#42533,#42534,#42535,#42536)) ;
#16379 = EDGE_LOOP('',(#42537,#42538,#42539,#42540)) ;
#16380 = EDGE_LOOP('',(#42541,#42542,#42543,#42544)) ;
#16381 = EDGE_LOOP('',(#42545,#42546,#42547,#42548)) ;
#16382 = EDGE_LOOP('',(#42549,#42550,#42551,#42552,#42553,#42554,#42555,#42556,
#42557,#42558,#42559,#42560)) ;
#16383 = EDGE_LOOP('',(#42561,#42562,#42563,#42564)) ;
#16384 = EDGE_LOOP('',(#42565,#42566,#42567,#42568)) ;
#16385 = EDGE_LOOP('',(#42569,#42570,#42571,#42572,#42573,#42574,#42575,#42576)) ;
#16386 = EDGE_LOOP('',(#42577,#42578,#42579,#42580,#42581,#42582,#42583,#42584)) ;
#16387 = EDGE_LOOP('',(#42585,#42586,#42587,#42588,#42589)) ;
#16388 = EDGE_LOOP('',(#42590,#42591,#42592,#42593)) ;
#16389 = EDGE_LOOP('',(#42594,#42595,#42596,#42597,#42598,#42599,#42600,#42601,
#42602,#42603)) ;
#16390 = EDGE_LOOP('',(#42604,#42605,#42606,#42607)) ;
#16391 = EDGE_LOOP('',(#42608,#42609,#42610,#42611)) ;
#16392 = EDGE_LOOP('',(#42612,#42613,#42614,#42615)) ;
#16393 = EDGE_LOOP('',(#42616,#42617,#42618,#42619)) ;
#16394 = EDGE_LOOP('',(#42620,#42621,#42622,#42623)) ;
#16395 = EDGE_LOOP('',(#42624,#42625,#42626,#42627)) ;
#16396 = EDGE_LOOP('',(#42628,#42629,#42630,#42631)) ;
#16397 = EDGE_LOOP('',(#42632,#42633,#42634,#42635)) ;
#16398 = EDGE_LOOP('',(#42636,#42637,#42638,#42639,#42640,#42641,#42642,#42643)) ;
#16399 = EDGE_LOOP('',(#42644,#42645,#42646,#42647,#42648,#42649,#42650,#42651)) ;
#16400 = EDGE_LOOP('',(#42652,#42653,#42654,#42655)) ;
#16401 = EDGE_LOOP('',(#42656,#42657,#42658,#42659,#42660,#42661,#42662,#42663)) ;
#16402 = EDGE_LOOP('',(#42664,#42665,#42666,#42667,#42668,#42669)) ;
#16403 = EDGE_LOOP('',(#42670,#42671,#42672,#42673)) ;
#16404 = EDGE_LOOP('',(#42674,#42675,#42676,#42677)) ;
#16405 = EDGE_LOOP('',(#42678,#42679,#42680,#42681)) ;
#16406 = EDGE_LOOP('',(#42682,#42683,#42684,#42685)) ;
#16407 = EDGE_LOOP('',(#42686,#42687,#42688,#42689)) ;
#16408 = EDGE_LOOP('',(#42690,#42691,#42692,#42693,#42694,#42695)) ;
#16409 = EDGE_LOOP('',(#42696,#42697,#42698,#42699,#42700,#42701)) ;
#16410 = EDGE_LOOP('',(#42702,#42703,#42704,#42705,#42706,#42707,#42708,#42709,
#42710,#42711,#42712,#42713,#42714)) ;
#16411 = EDGE_LOOP('',(#42715)) ;
#16412 = EDGE_LOOP('',(#42716,#42717,#42718,#42719,#42720)) ;
#16413 = EDGE_LOOP('',(#42721,#42722,#42723,#42724,#42725)) ;
#16414 = EDGE_LOOP('',(#42726,#42727,#42728,#42729,#42730,#42731,#42732,#42733,
#42734,#42735,#42736,#42737,#42738,#42739,#42740,#42741,#42742)) ;
#16415 = EDGE_LOOP('',(#42743,#42744,#42745,#42746,#42747,#42748,#42749,#42750,
#42751,#42752,#42753,#42754,#42755,#42756,#42757)) ;
#16416 = EDGE_LOOP('',(#42758,#42759,#42760,#42761,#42762)) ;
#16417 = EDGE_LOOP('',(#42763)) ;
#16418 = EDGE_LOOP('',(#42764,#42765,#42766,#42767)) ;
#16419 = EDGE_LOOP('',(#42768)) ;
#16420 = EDGE_LOOP('',(#42769)) ;
#16421 = EDGE_LOOP('',(#42770,#42771,#42772,#42773)) ;
#16422 = EDGE_LOOP('',(#42774)) ;
#16423 = EDGE_LOOP('',(#42775)) ;
#16424 = EDGE_LOOP('',(#42776)) ;
#16425 = EDGE_LOOP('',(#42777)) ;
#16426 = EDGE_LOOP('',(#42778)) ;
#16427 = EDGE_LOOP('',(#42779)) ;
#16428 = EDGE_LOOP('',(#42780,#42781,#42782,#42783,#42784)) ;
#16429 = EDGE_LOOP('',(#42785,#42786,#42787,#42788,#42789)) ;
#16430 = EDGE_LOOP('',(#42790,#42791,#42792,#42793)) ;
#16431 = EDGE_LOOP('',(#42794,#42795,#42796,#42797)) ;
#16432 = EDGE_LOOP('',(#42798,#42799,#42800,#42801)) ;
#16433 = EDGE_LOOP('',(#42802,#42803,#42804,#42805)) ;
#16434 = EDGE_LOOP('',(#42806,#42807,#42808,#42809)) ;
#16435 = EDGE_LOOP('',(#42810,#42811,#42812,#42813)) ;
#16436 = EDGE_LOOP('',(#42814,#42815,#42816,#42817)) ;
#16437 = EDGE_LOOP('',(#42818,#42819,#42820,#42821)) ;
#16438 = EDGE_LOOP('',(#42822,#42823,#42824,#42825)) ;
#16439 = EDGE_LOOP('',(#42826,#42827,#42828,#42829)) ;
#16440 = EDGE_LOOP('',(#42830,#42831,#42832,#42833)) ;
#16441 = EDGE_LOOP('',(#42834,#42835,#42836,#42837)) ;
#16442 = EDGE_LOOP('',(#42838,#42839,#42840,#42841)) ;
#16443 = EDGE_LOOP('',(#42842,#42843,#42844,#42845)) ;
#16444 = EDGE_LOOP('',(#42846,#42847,#42848,#42849)) ;
#16445 = EDGE_LOOP('',(#42850,#42851,#42852,#42853)) ;
#16446 = EDGE_LOOP('',(#42854,#42855,#42856,#42857)) ;
#16447 = EDGE_LOOP('',(#42858,#42859,#42860,#42861)) ;
#16448 = EDGE_LOOP('',(#42862,#42863,#42864,#42865)) ;
#16449 = EDGE_LOOP('',(#42866,#42867,#42868,#42869)) ;
#16450 = EDGE_LOOP('',(#42870,#42871,#42872,#42873)) ;
#16451 = EDGE_LOOP('',(#42874,#42875,#42876,#42877)) ;
#16452 = EDGE_LOOP('',(#42878,#42879,#42880,#42881)) ;
#16453 = EDGE_LOOP('',(#42882,#42883,#42884,#42885)) ;
#16454 = EDGE_LOOP('',(#42886,#42887,#42888,#42889)) ;
#16455 = EDGE_LOOP('',(#42890,#42891,#42892,#42893)) ;
#16456 = EDGE_LOOP('',(#42894,#42895,#42896,#42897)) ;
#16457 = EDGE_LOOP('',(#42898,#42899,#42900,#42901)) ;
#16458 = EDGE_LOOP('',(#42902,#42903,#42904,#42905)) ;
#16459 = EDGE_LOOP('',(#42906,#42907,#42908,#42909)) ;
#16460 = EDGE_LOOP('',(#42910,#42911,#42912,#42913)) ;
#16461 = EDGE_LOOP('',(#42914,#42915,#42916,#42917)) ;
#16462 = EDGE_LOOP('',(#42918,#42919,#42920,#42921)) ;
#16463 = EDGE_LOOP('',(#42922,#42923,#42924,#42925)) ;
#16464 = EDGE_LOOP('',(#42926,#42927,#42928,#42929)) ;
#16465 = EDGE_LOOP('',(#42930,#42931,#42932,#42933)) ;
#16466 = EDGE_LOOP('',(#42934,#42935,#42936,#42937)) ;
#16467 = EDGE_LOOP('',(#42938,#42939,#42940,#42941)) ;
#16468 = EDGE_LOOP('',(#42942,#42943,#42944,#42945)) ;
#16469 = EDGE_LOOP('',(#42946,#42947,#42948,#42949)) ;
#16470 = EDGE_LOOP('',(#42950,#42951,#42952,#42953)) ;
#16471 = EDGE_LOOP('',(#42954,#42955,#42956,#42957)) ;
#16472 = EDGE_LOOP('',(#42958,#42959,#42960,#42961)) ;
#16473 = EDGE_LOOP('',(#42962,#42963,#42964,#42965)) ;
#16474 = EDGE_LOOP('',(#42966,#42967,#42968,#42969)) ;
#16475 = EDGE_LOOP('',(#42970,#42971,#42972,#42973)) ;
#16476 = EDGE_LOOP('',(#42974,#42975,#42976,#42977)) ;
#16477 = EDGE_LOOP('',(#42978,#42979,#42980,#42981)) ;
#16478 = EDGE_LOOP('',(#42982,#42983,#42984,#42985)) ;
#16479 = EDGE_LOOP('',(#42986,#42987,#42988,#42989)) ;
#16480 = EDGE_LOOP('',(#42990,#42991,#42992,#42993)) ;
#16481 = EDGE_LOOP('',(#42994,#42995,#42996,#42997)) ;
#16482 = EDGE_LOOP('',(#42998,#42999,#43000,#43001)) ;
#16483 = EDGE_LOOP('',(#43002,#43003,#43004,#43005)) ;
#16484 = EDGE_LOOP('',(#43006,#43007,#43008,#43009)) ;
#16485 = EDGE_LOOP('',(#43010,#43011,#43012,#43013)) ;
#16486 = EDGE_LOOP('',(#43014,#43015,#43016,#43017)) ;
#16487 = EDGE_LOOP('',(#43018,#43019,#43020,#43021)) ;
#16488 = EDGE_LOOP('',(#43022,#43023,#43024,#43025)) ;
#16489 = EDGE_LOOP('',(#43026,#43027,#43028,#43029)) ;
#16490 = EDGE_LOOP('',(#43030,#43031,#43032,#43033)) ;
#16491 = EDGE_LOOP('',(#43034,#43035,#43036,#43037)) ;
#16492 = EDGE_LOOP('',(#43038,#43039,#43040,#43041)) ;
#16493 = EDGE_LOOP('',(#43042,#43043,#43044,#43045)) ;
#16494 = EDGE_LOOP('',(#43046,#43047,#43048,#43049)) ;
#16495 = EDGE_LOOP('',(#43050,#43051,#43052,#43053)) ;
#16496 = EDGE_LOOP('',(#43054,#43055,#43056,#43057)) ;
#16497 = EDGE_LOOP('',(#43058,#43059,#43060,#43061)) ;
#16498 = EDGE_LOOP('',(#43062,#43063,#43064,#43065)) ;
#16499 = EDGE_LOOP('',(#43066,#43067,#43068,#43069)) ;
#16500 = EDGE_LOOP('',(#43070,#43071,#43072,#43073)) ;
#16501 = EDGE_LOOP('',(#43074,#43075,#43076,#43077)) ;
#16502 = EDGE_LOOP('',(#43078,#43079,#43080,#43081)) ;
#16503 = EDGE_LOOP('',(#43082,#43083,#43084,#43085)) ;
#16504 = EDGE_LOOP('',(#43086,#43087,#43088,#43089)) ;
#16505 = EDGE_LOOP('',(#43090,#43091,#43092,#43093)) ;
#16506 = EDGE_LOOP('',(#43094,#43095,#43096,#43097)) ;
#16507 = EDGE_LOOP('',(#43098,#43099,#43100,#43101)) ;
#16508 = EDGE_LOOP('',(#43102,#43103,#43104,#43105)) ;
#16509 = EDGE_LOOP('',(#43106,#43107,#43108,#43109)) ;
#16510 = EDGE_LOOP('',(#43110,#43111,#43112,#43113)) ;
#16511 = EDGE_LOOP('',(#43114,#43115,#43116,#43117)) ;
#16512 = EDGE_LOOP('',(#43118,#43119,#43120,#43121)) ;
#16513 = EDGE_LOOP('',(#43122,#43123,#43124,#43125)) ;
#16514 = EDGE_LOOP('',(#43126,#43127,#43128,#43129)) ;
#16515 = EDGE_LOOP('',(#43130,#43131,#43132,#43133)) ;
#16516 = EDGE_LOOP('',(#43134,#43135,#43136,#43137)) ;
#16517 = EDGE_LOOP('',(#43138,#43139,#43140,#43141)) ;
#16518 = EDGE_LOOP('',(#43142,#43143,#43144,#43145)) ;
#16519 = EDGE_LOOP('',(#43146,#43147,#43148,#43149)) ;
#16520 = EDGE_LOOP('',(#43150,#43151,#43152,#43153)) ;
#16521 = EDGE_LOOP('',(#43154,#43155,#43156,#43157)) ;
#16522 = EDGE_LOOP('',(#43158,#43159,#43160,#43161)) ;
#16523 = EDGE_LOOP('',(#43162,#43163,#43164,#43165)) ;
#16524 = EDGE_LOOP('',(#43166,#43167,#43168,#43169)) ;
#16525 = EDGE_LOOP('',(#43170,#43171,#43172,#43173)) ;
#16526 = EDGE_LOOP('',(#43174,#43175,#43176,#43177)) ;
#16527 = EDGE_LOOP('',(#43178,#43179,#43180,#43181)) ;
#16528 = EDGE_LOOP('',(#43182,#43183,#43184,#43185)) ;
#16529 = EDGE_LOOP('',(#43186,#43187,#43188,#43189)) ;
#16530 = EDGE_LOOP('',(#43190,#43191,#43192,#43193)) ;
#16531 = EDGE_LOOP('',(#43194,#43195,#43196,#43197)) ;
#16532 = EDGE_LOOP('',(#43198,#43199,#43200,#43201)) ;
#16533 = EDGE_LOOP('',(#43202,#43203,#43204,#43205)) ;
#16534 = EDGE_LOOP('',(#43206,#43207,#43208,#43209)) ;
#16535 = EDGE_LOOP('',(#43210,#43211,#43212,#43213)) ;
#16536 = EDGE_LOOP('',(#43214,#43215,#43216,#43217)) ;
#16537 = EDGE_LOOP('',(#43218,#43219,#43220,#43221)) ;
#16538 = EDGE_LOOP('',(#43222,#43223,#43224,#43225)) ;
#16539 = EDGE_LOOP('',(#43226,#43227,#43228,#43229)) ;
#16540 = EDGE_LOOP('',(#43230,#43231,#43232,#43233)) ;
#16541 = EDGE_LOOP('',(#43234,#43235,#43236,#43237)) ;
#16542 = EDGE_LOOP('',(#43238,#43239,#43240,#43241)) ;
#16543 = EDGE_LOOP('',(#43242,#43243,#43244,#43245)) ;
#16544 = EDGE_LOOP('',(#43246,#43247,#43248,#43249)) ;
#16545 = EDGE_LOOP('',(#43250,#43251,#43252,#43253)) ;
#16546 = EDGE_LOOP('',(#43254,#43255,#43256,#43257)) ;
#16547 = EDGE_LOOP('',(#43258,#43259,#43260,#43261)) ;
#16548 = EDGE_LOOP('',(#43262,#43263,#43264,#43265)) ;
#16549 = EDGE_LOOP('',(#43266,#43267,#43268,#43269)) ;
#16550 = EDGE_LOOP('',(#43270,#43271,#43272,#43273)) ;
#16551 = EDGE_LOOP('',(#43274,#43275,#43276,#43277)) ;
#16552 = EDGE_LOOP('',(#43278,#43279,#43280,#43281)) ;
#16553 = EDGE_LOOP('',(#43282,#43283,#43284,#43285)) ;
#16554 = EDGE_LOOP('',(#43286,#43287,#43288,#43289)) ;
#16555 = EDGE_LOOP('',(#43290,#43291,#43292,#43293)) ;
#16556 = EDGE_LOOP('',(#43294,#43295,#43296,#43297)) ;
#16557 = EDGE_LOOP('',(#43298,#43299,#43300,#43301)) ;
#16558 = EDGE_LOOP('',(#43302,#43303,#43304,#43305)) ;
#16559 = EDGE_LOOP('',(#43306,#43307,#43308,#43309)) ;
#16560 = EDGE_LOOP('',(#43310,#43311,#43312,#43313)) ;
#16561 = EDGE_LOOP('',(#43314,#43315,#43316,#43317)) ;
#16562 = EDGE_LOOP('',(#43318,#43319,#43320,#43321)) ;
#16563 = EDGE_LOOP('',(#43322,#43323,#43324,#43325)) ;
#16564 = EDGE_LOOP('',(#43326,#43327,#43328,#43329)) ;
#16565 = EDGE_LOOP('',(#43330,#43331,#43332,#43333)) ;
#16566 = EDGE_LOOP('',(#43334,#43335,#43336,#43337)) ;
#16567 = EDGE_LOOP('',(#43338,#43339,#43340,#43341)) ;
#16568 = EDGE_LOOP('',(#43342,#43343,#43344,#43345,#43346)) ;
#16569 = EDGE_LOOP('',(#43347,#43348,#43349,#43350,#43351,#43352,#43353,#43354,
#43355,#43356,#43357,#43358,#43359,#43360,#43361,#43362,#43363,#43364,#43365,
#43366,#43367,#43368,#43369,#43370,#43371,#43372,#43373,#43374,#43375,#43376,
#43377,#43378,#43379,#43380,#43381,#43382,#43383,#43384,#43385,#43386,#43387,
#43388,#43389,#43390,#43391)) ;
#16570 = EDGE_LOOP('',(#43392,#43393,#43394,#43395)) ;
#16571 = EDGE_LOOP('',(#43396,#43397,#43398,#43399,#43400,#43401,#43402,#43403,
#43404,#43405,#43406,#43407,#43408,#43409,#43410,#43411,#43412,#43413,#43414,
#43415,#43416,#43417,#43418,#43419,#43420,#43421,#43422,#43423,#43424,#43425,
#43426,#43427,#43428,#43429,#43430,#43431,#43432,#43433,#43434,#43435,#43436,
#43437,#43438,#43439,#43440)) ;
#16572 = EDGE_LOOP('',(#43441,#43442,#43443,#43444)) ;
#16573 = EDGE_LOOP('',(#43445,#43446,#43447,#43448)) ;
#16574 = EDGE_LOOP('',(#43449,#43450,#43451,#43452)) ;
#16575 = EDGE_LOOP('',(#43453,#43454,#43455,#43456)) ;
#16576 = EDGE_LOOP('',(#43457,#43458,#43459,#43460)) ;
#16577 = EDGE_LOOP('',(#43461,#43462,#43463,#43464)) ;
#16578 = EDGE_LOOP('',(#43465,#43466,#43467,#43468)) ;
#16579 = EDGE_LOOP('',(#43469,#43470,#43471,#43472)) ;
#16580 = EDGE_LOOP('',(#43473,#43474,#43475,#43476)) ;
#16581 = EDGE_LOOP('',(#43477,#43478,#43479,#43480)) ;
#16582 = EDGE_LOOP('',(#43481,#43482,#43483,#43484)) ;
#16583 = EDGE_LOOP('',(#43485,#43486,#43487,#43488)) ;
#16584 = EDGE_LOOP('',(#43489,#43490,#43491,#43492)) ;
#16585 = EDGE_LOOP('',(#43493,#43494,#43495,#43496)) ;
#16586 = EDGE_LOOP('',(#43497,#43498,#43499,#43500)) ;
#16587 = EDGE_LOOP('',(#43501,#43502,#43503,#43504)) ;
#16588 = EDGE_LOOP('',(#43505,#43506,#43507,#43508)) ;
#16589 = EDGE_LOOP('',(#43509,#43510,#43511,#43512)) ;
#16590 = EDGE_LOOP('',(#43513,#43514,#43515,#43516)) ;
#16591 = EDGE_LOOP('',(#43517,#43518,#43519,#43520,#43521)) ;
#16592 = EDGE_LOOP('',(#43522,#43523,#43524,#43525)) ;
#16593 = EDGE_LOOP('',(#43526,#43527,#43528,#43529)) ;
#16594 = EDGE_LOOP('',(#43530,#43531,#43532,#43533)) ;
#16595 = EDGE_LOOP('',(#43534,#43535,#43536,#43537)) ;
#16596 = EDGE_LOOP('',(#43538,#43539,#43540,#43541)) ;
#16597 = EDGE_LOOP('',(#43542,#43543,#43544,#43545)) ;
#16598 = EDGE_LOOP('',(#43546,#43547,#43548,#43549)) ;
#16599 = EDGE_LOOP('',(#43550,#43551,#43552,#43553)) ;
#16600 = EDGE_LOOP('',(#43554,#43555,#43556,#43557)) ;
#16601 = EDGE_LOOP('',(#43558,#43559,#43560,#43561)) ;
#16602 = EDGE_LOOP('',(#43562,#43563,#43564,#43565)) ;
#16603 = EDGE_LOOP('',(#43566,#43567,#43568,#43569)) ;
#16604 = EDGE_LOOP('',(#43570,#43571,#43572,#43573)) ;
#16605 = EDGE_LOOP('',(#43574,#43575,#43576,#43577)) ;
#16606 = EDGE_LOOP('',(#43578,#43579,#43580,#43581)) ;
#16607 = EDGE_LOOP('',(#43582,#43583,#43584,#43585)) ;
#16608 = EDGE_LOOP('',(#43586,#43587,#43588,#43589)) ;
#16609 = EDGE_LOOP('',(#43590,#43591,#43592,#43593)) ;
#16610 = EDGE_LOOP('',(#43594,#43595,#43596,#43597)) ;
#16611 = EDGE_LOOP('',(#43598,#43599,#43600,#43601)) ;
#16612 = EDGE_LOOP('',(#43602,#43603,#43604,#43605)) ;
#16613 = EDGE_LOOP('',(#43606,#43607,#43608,#43609)) ;
#16614 = EDGE_LOOP('',(#43610,#43611,#43612,#43613)) ;
#16615 = EDGE_LOOP('',(#43614,#43615,#43616,#43617)) ;
#16616 = EDGE_LOOP('',(#43618,#43619,#43620,#43621)) ;
#16617 = EDGE_LOOP('',(#43622,#43623,#43624,#43625)) ;
#16618 = EDGE_LOOP('',(#43626,#43627,#43628,#43629)) ;
#16619 = EDGE_LOOP('',(#43630,#43631,#43632,#43633)) ;
#16620 = EDGE_LOOP('',(#43634,#43635,#43636,#43637)) ;
#16621 = EDGE_LOOP('',(#43638,#43639,#43640,#43641)) ;
#16622 = EDGE_LOOP('',(#43642,#43643,#43644,#43645)) ;
#16623 = EDGE_LOOP('',(#43646,#43647,#43648,#43649)) ;
#16624 = EDGE_LOOP('',(#43650,#43651,#43652,#43653)) ;
#16625 = EDGE_LOOP('',(#43654,#43655,#43656,#43657)) ;
#16626 = EDGE_LOOP('',(#43658,#43659,#43660,#43661)) ;
#16627 = EDGE_LOOP('',(#43662,#43663,#43664,#43665)) ;
#16628 = EDGE_LOOP('',(#43666,#43667,#43668,#43669)) ;
#16629 = EDGE_LOOP('',(#43670,#43671,#43672,#43673)) ;
#16630 = EDGE_LOOP('',(#43674,#43675,#43676,#43677)) ;
#16631 = EDGE_LOOP('',(#43678,#43679,#43680,#43681)) ;
#16632 = EDGE_LOOP('',(#43682,#43683,#43684,#43685)) ;
#16633 = EDGE_LOOP('',(#43686,#43687,#43688,#43689)) ;
#16634 = EDGE_LOOP('',(#43690,#43691,#43692,#43693)) ;
#16635 = EDGE_LOOP('',(#43694,#43695,#43696,#43697)) ;
#16636 = EDGE_LOOP('',(#43698,#43699,#43700,#43701)) ;
#16637 = EDGE_LOOP('',(#43702,#43703,#43704,#43705)) ;
#16638 = EDGE_LOOP('',(#43706,#43707,#43708,#43709)) ;
#16639 = EDGE_LOOP('',(#43710,#43711,#43712,#43713)) ;
#16640 = EDGE_LOOP('',(#43714,#43715,#43716,#43717)) ;
#16641 = EDGE_LOOP('',(#43718,#43719,#43720,#43721)) ;
#16642 = EDGE_LOOP('',(#43722,#43723,#43724,#43725)) ;
#16643 = EDGE_LOOP('',(#43726,#43727,#43728,#43729)) ;
#16644 = EDGE_LOOP('',(#43730,#43731,#43732,#43733)) ;
#16645 = EDGE_LOOP('',(#43734,#43735,#43736,#43737)) ;
#16646 = EDGE_LOOP('',(#43738,#43739,#43740,#43741)) ;
#16647 = EDGE_LOOP('',(#43742,#43743,#43744,#43745)) ;
#16648 = EDGE_LOOP('',(#43746,#43747,#43748,#43749)) ;
#16649 = EDGE_LOOP('',(#43750,#43751,#43752,#43753)) ;
#16650 = EDGE_LOOP('',(#43754,#43755,#43756,#43757)) ;
#16651 = EDGE_LOOP('',(#43758,#43759,#43760,#43761)) ;
#16652 = EDGE_LOOP('',(#43762,#43763,#43764,#43765)) ;
#16653 = EDGE_LOOP('',(#43766,#43767,#43768,#43769)) ;
#16654 = EDGE_LOOP('',(#43770,#43771,#43772,#43773)) ;
#16655 = EDGE_LOOP('',(#43774,#43775,#43776,#43777)) ;
#16656 = EDGE_LOOP('',(#43778,#43779,#43780,#43781)) ;
#16657 = EDGE_LOOP('',(#43782,#43783,#43784,#43785)) ;
#16658 = EDGE_LOOP('',(#43786,#43787,#43788,#43789)) ;
#16659 = EDGE_LOOP('',(#43790,#43791,#43792,#43793)) ;
#16660 = EDGE_LOOP('',(#43794,#43795,#43796,#43797)) ;
#16661 = EDGE_LOOP('',(#43798,#43799,#43800,#43801)) ;
#16662 = EDGE_LOOP('',(#43802,#43803,#43804,#43805)) ;
#16663 = EDGE_LOOP('',(#43806,#43807,#43808,#43809)) ;
#16664 = EDGE_LOOP('',(#43810,#43811,#43812,#43813)) ;
#16665 = EDGE_LOOP('',(#43814,#43815,#43816,#43817)) ;
#16666 = EDGE_LOOP('',(#43818,#43819,#43820,#43821)) ;
#16667 = EDGE_LOOP('',(#43822,#43823,#43824,#43825)) ;
#16668 = EDGE_LOOP('',(#43826,#43827,#43828,#43829)) ;
#16669 = EDGE_LOOP('',(#43830,#43831,#43832,#43833)) ;
#16670 = EDGE_LOOP('',(#43834,#43835,#43836,#43837)) ;
#16671 = EDGE_LOOP('',(#43838,#43839,#43840,#43841)) ;
#16672 = EDGE_LOOP('',(#43842,#43843,#43844,#43845)) ;
#16673 = EDGE_LOOP('',(#43846,#43847,#43848,#43849)) ;
#16674 = EDGE_LOOP('',(#43850,#43851,#43852,#43853)) ;
#16675 = EDGE_LOOP('',(#43854,#43855,#43856,#43857)) ;
#16676 = EDGE_LOOP('',(#43858,#43859,#43860,#43861)) ;
#16677 = EDGE_LOOP('',(#43862,#43863,#43864,#43865)) ;
#16678 = EDGE_LOOP('',(#43866,#43867,#43868,#43869)) ;
#16679 = EDGE_LOOP('',(#43870,#43871,#43872,#43873)) ;
#16680 = EDGE_LOOP('',(#43874,#43875,#43876,#43877)) ;
#16681 = EDGE_LOOP('',(#43878,#43879,#43880,#43881)) ;
#16682 = EDGE_LOOP('',(#43882,#43883,#43884,#43885)) ;
#16683 = EDGE_LOOP('',(#43886,#43887,#43888,#43889)) ;
#16684 = EDGE_LOOP('',(#43890,#43891,#43892,#43893)) ;
#16685 = EDGE_LOOP('',(#43894,#43895,#43896,#43897)) ;
#16686 = EDGE_LOOP('',(#43898,#43899,#43900,#43901)) ;
#16687 = EDGE_LOOP('',(#43902,#43903,#43904,#43905)) ;
#16688 = EDGE_LOOP('',(#43906,#43907,#43908,#43909)) ;
#16689 = EDGE_LOOP('',(#43910,#43911,#43912,#43913)) ;
#16690 = EDGE_LOOP('',(#43914,#43915,#43916,#43917)) ;
#16691 = EDGE_LOOP('',(#43918,#43919,#43920,#43921)) ;
#16692 = EDGE_LOOP('',(#43922,#43923,#43924,#43925)) ;
#16693 = EDGE_LOOP('',(#43926,#43927,#43928,#43929)) ;
#16694 = EDGE_LOOP('',(#43930,#43931,#43932,#43933)) ;
#16695 = EDGE_LOOP('',(#43934,#43935,#43936,#43937)) ;
#16696 = EDGE_LOOP('',(#43938,#43939,#43940,#43941)) ;
#16697 = EDGE_LOOP('',(#43942,#43943,#43944,#43945)) ;
#16698 = EDGE_LOOP('',(#43946,#43947,#43948,#43949)) ;
#16699 = EDGE_LOOP('',(#43950,#43951,#43952,#43953)) ;
#16700 = EDGE_LOOP('',(#43954,#43955,#43956,#43957)) ;
#16701 = EDGE_LOOP('',(#43958,#43959,#43960,#43961)) ;
#16702 = EDGE_LOOP('',(#43962,#43963,#43964,#43965)) ;
#16703 = EDGE_LOOP('',(#43966,#43967,#43968,#43969)) ;
#16704 = EDGE_LOOP('',(#43970,#43971,#43972,#43973)) ;
#16705 = EDGE_LOOP('',(#43974,#43975,#43976,#43977)) ;
#16706 = EDGE_LOOP('',(#43978,#43979,#43980,#43981)) ;
#16707 = EDGE_LOOP('',(#43982,#43983,#43984,#43985)) ;
#16708 = EDGE_LOOP('',(#43986,#43987,#43988,#43989)) ;
#16709 = EDGE_LOOP('',(#43990,#43991,#43992,#43993)) ;
#16710 = EDGE_LOOP('',(#43994,#43995,#43996,#43997)) ;
#16711 = EDGE_LOOP('',(#43998,#43999,#44000,#44001)) ;
#16712 = EDGE_LOOP('',(#44002,#44003,#44004,#44005)) ;
#16713 = EDGE_LOOP('',(#44006,#44007,#44008,#44009)) ;
#16714 = EDGE_LOOP('',(#44010)) ;
#16715 = EDGE_LOOP('',(#44011)) ;
#16716 = EDGE_LOOP('',(#44012,#44013,#44014,#44015)) ;
#16717 = EDGE_LOOP('',(#44016)) ;
#16718 = EDGE_LOOP('',(#44017)) ;
#16719 = EDGE_LOOP('',(#44018)) ;
#16720 = EDGE_LOOP('',(#44019)) ;
#16721 = EDGE_LOOP('',(#44020)) ;
#16722 = EDGE_LOOP('',(#44021)) ;
#16723 = EDGE_LOOP('',(#44022,#44023,#44024,#44025,#44026)) ;
#16724 = EDGE_LOOP('',(#44027,#44028,#44029,#44030,#44031)) ;
#16725 = EDGE_LOOP('',(#44032,#44033,#44034,#44035)) ;
#16726 = EDGE_LOOP('',(#44036,#44037,#44038,#44039)) ;
#16727 = EDGE_LOOP('',(#44040,#44041,#44042,#44043)) ;
#16728 = EDGE_LOOP('',(#44044,#44045,#44046,#44047)) ;
#16729 = EDGE_LOOP('',(#44048,#44049,#44050,#44051)) ;
#16730 = EDGE_LOOP('',(#44052,#44053,#44054,#44055)) ;
#16731 = EDGE_LOOP('',(#44056,#44057,#44058,#44059)) ;
#16732 = EDGE_LOOP('',(#44060,#44061,#44062,#44063)) ;
#16733 = EDGE_LOOP('',(#44064,#44065,#44066,#44067)) ;
#16734 = EDGE_LOOP('',(#44068,#44069,#44070,#44071)) ;
#16735 = EDGE_LOOP('',(#44072,#44073,#44074,#44075)) ;
#16736 = EDGE_LOOP('',(#44076,#44077,#44078,#44079)) ;
#16737 = EDGE_LOOP('',(#44080,#44081,#44082,#44083)) ;
#16738 = EDGE_LOOP('',(#44084,#44085,#44086,#44087)) ;
#16739 = EDGE_LOOP('',(#44088,#44089,#44090,#44091)) ;
#16740 = EDGE_LOOP('',(#44092,#44093,#44094,#44095)) ;
#16741 = EDGE_LOOP('',(#44096,#44097,#44098,#44099)) ;
#16742 = EDGE_LOOP('',(#44100,#44101,#44102,#44103)) ;
#16743 = EDGE_LOOP('',(#44104,#44105,#44106,#44107)) ;
#16744 = EDGE_LOOP('',(#44108,#44109,#44110,#44111)) ;
#16745 = EDGE_LOOP('',(#44112,#44113,#44114,#44115)) ;
#16746 = EDGE_LOOP('',(#44116,#44117,#44118,#44119)) ;
#16747 = EDGE_LOOP('',(#44120,#44121,#44122,#44123)) ;
#16748 = EDGE_LOOP('',(#44124,#44125,#44126,#44127)) ;
#16749 = EDGE_LOOP('',(#44128,#44129,#44130,#44131)) ;
#16750 = EDGE_LOOP('',(#44132,#44133,#44134,#44135)) ;
#16751 = EDGE_LOOP('',(#44136,#44137,#44138,#44139)) ;
#16752 = EDGE_LOOP('',(#44140,#44141,#44142,#44143)) ;
#16753 = EDGE_LOOP('',(#44144,#44145,#44146,#44147)) ;
#16754 = EDGE_LOOP('',(#44148,#44149,#44150,#44151)) ;
#16755 = EDGE_LOOP('',(#44152,#44153,#44154,#44155)) ;
#16756 = EDGE_LOOP('',(#44156,#44157,#44158,#44159)) ;
#16757 = EDGE_LOOP('',(#44160,#44161,#44162,#44163)) ;
#16758 = EDGE_LOOP('',(#44164,#44165,#44166,#44167)) ;
#16759 = EDGE_LOOP('',(#44168,#44169,#44170,#44171)) ;
#16760 = EDGE_LOOP('',(#44172,#44173,#44174,#44175)) ;
#16761 = EDGE_LOOP('',(#44176,#44177,#44178,#44179)) ;
#16762 = EDGE_LOOP('',(#44180,#44181,#44182,#44183)) ;
#16763 = EDGE_LOOP('',(#44184,#44185,#44186,#44187)) ;
#16764 = EDGE_LOOP('',(#44188,#44189,#44190,#44191)) ;
#16765 = EDGE_LOOP('',(#44192,#44193,#44194,#44195)) ;
#16766 = EDGE_LOOP('',(#44196,#44197,#44198,#44199)) ;
#16767 = EDGE_LOOP('',(#44200,#44201,#44202,#44203)) ;
#16768 = EDGE_LOOP('',(#44204,#44205,#44206,#44207)) ;
#16769 = EDGE_LOOP('',(#44208,#44209,#44210,#44211)) ;
#16770 = EDGE_LOOP('',(#44212,#44213,#44214,#44215)) ;
#16771 = EDGE_LOOP('',(#44216,#44217,#44218,#44219)) ;
#16772 = EDGE_LOOP('',(#44220,#44221,#44222,#44223)) ;
#16773 = EDGE_LOOP('',(#44224,#44225,#44226,#44227)) ;
#16774 = EDGE_LOOP('',(#44228,#44229,#44230,#44231)) ;
#16775 = EDGE_LOOP('',(#44232,#44233,#44234,#44235)) ;
#16776 = EDGE_LOOP('',(#44236,#44237,#44238,#44239)) ;
#16777 = EDGE_LOOP('',(#44240,#44241,#44242,#44243)) ;
#16778 = EDGE_LOOP('',(#44244,#44245,#44246,#44247)) ;
#16779 = EDGE_LOOP('',(#44248,#44249,#44250,#44251)) ;
#16780 = EDGE_LOOP('',(#44252,#44253,#44254,#44255)) ;
#16781 = EDGE_LOOP('',(#44256,#44257,#44258,#44259)) ;
#16782 = EDGE_LOOP('',(#44260,#44261,#44262,#44263)) ;
#16783 = EDGE_LOOP('',(#44264,#44265,#44266,#44267)) ;
#16784 = EDGE_LOOP('',(#44268,#44269,#44270,#44271)) ;
#16785 = EDGE_LOOP('',(#44272,#44273,#44274,#44275)) ;
#16786 = EDGE_LOOP('',(#44276,#44277,#44278,#44279)) ;
#16787 = EDGE_LOOP('',(#44280,#44281,#44282,#44283)) ;
#16788 = EDGE_LOOP('',(#44284,#44285,#44286,#44287)) ;
#16789 = EDGE_LOOP('',(#44288,#44289,#44290,#44291)) ;
#16790 = EDGE_LOOP('',(#44292,#44293,#44294,#44295)) ;
#16791 = EDGE_LOOP('',(#44296,#44297,#44298,#44299)) ;
#16792 = EDGE_LOOP('',(#44300,#44301,#44302,#44303)) ;
#16793 = EDGE_LOOP('',(#44304,#44305,#44306,#44307)) ;
#16794 = EDGE_LOOP('',(#44308,#44309,#44310,#44311)) ;
#16795 = EDGE_LOOP('',(#44312,#44313,#44314,#44315)) ;
#16796 = EDGE_LOOP('',(#44316,#44317,#44318,#44319)) ;
#16797 = EDGE_LOOP('',(#44320,#44321,#44322,#44323)) ;
#16798 = EDGE_LOOP('',(#44324,#44325,#44326,#44327)) ;
#16799 = EDGE_LOOP('',(#44328,#44329,#44330,#44331)) ;
#16800 = EDGE_LOOP('',(#44332,#44333,#44334,#44335)) ;
#16801 = EDGE_LOOP('',(#44336,#44337,#44338,#44339)) ;
#16802 = EDGE_LOOP('',(#44340,#44341,#44342,#44343)) ;
#16803 = EDGE_LOOP('',(#44344,#44345,#44346,#44347)) ;
#16804 = EDGE_LOOP('',(#44348,#44349,#44350,#44351)) ;
#16805 = EDGE_LOOP('',(#44352,#44353,#44354,#44355)) ;
#16806 = EDGE_LOOP('',(#44356,#44357,#44358,#44359)) ;
#16807 = EDGE_LOOP('',(#44360,#44361,#44362,#44363)) ;
#16808 = EDGE_LOOP('',(#44364,#44365,#44366,#44367)) ;
#16809 = EDGE_LOOP('',(#44368,#44369,#44370,#44371)) ;
#16810 = EDGE_LOOP('',(#44372,#44373,#44374,#44375)) ;
#16811 = EDGE_LOOP('',(#44376,#44377,#44378,#44379)) ;
#16812 = EDGE_LOOP('',(#44380,#44381,#44382,#44383)) ;
#16813 = EDGE_LOOP('',(#44384,#44385,#44386,#44387)) ;
#16814 = EDGE_LOOP('',(#44388,#44389,#44390,#44391)) ;
#16815 = EDGE_LOOP('',(#44392,#44393,#44394,#44395)) ;
#16816 = EDGE_LOOP('',(#44396,#44397,#44398,#44399)) ;
#16817 = EDGE_LOOP('',(#44400,#44401,#44402,#44403)) ;
#16818 = EDGE_LOOP('',(#44404,#44405,#44406,#44407)) ;
#16819 = EDGE_LOOP('',(#44408,#44409,#44410,#44411)) ;
#16820 = EDGE_LOOP('',(#44412,#44413,#44414,#44415)) ;
#16821 = EDGE_LOOP('',(#44416,#44417,#44418,#44419)) ;
#16822 = EDGE_LOOP('',(#44420,#44421,#44422,#44423)) ;
#16823 = EDGE_LOOP('',(#44424,#44425,#44426,#44427)) ;
#16824 = EDGE_LOOP('',(#44428,#44429,#44430,#44431)) ;
#16825 = EDGE_LOOP('',(#44432,#44433,#44434,#44435)) ;
#16826 = EDGE_LOOP('',(#44436,#44437,#44438,#44439)) ;
#16827 = EDGE_LOOP('',(#44440,#44441,#44442,#44443)) ;
#16828 = EDGE_LOOP('',(#44444,#44445,#44446,#44447)) ;
#16829 = EDGE_LOOP('',(#44448,#44449,#44450,#44451)) ;
#16830 = EDGE_LOOP('',(#44452,#44453,#44454,#44455)) ;
#16831 = EDGE_LOOP('',(#44456,#44457,#44458,#44459)) ;
#16832 = EDGE_LOOP('',(#44460,#44461,#44462,#44463)) ;
#16833 = EDGE_LOOP('',(#44464,#44465,#44466,#44467)) ;
#16834 = EDGE_LOOP('',(#44468,#44469,#44470,#44471)) ;
#16835 = EDGE_LOOP('',(#44472,#44473,#44474,#44475)) ;
#16836 = EDGE_LOOP('',(#44476,#44477,#44478,#44479)) ;
#16837 = EDGE_LOOP('',(#44480,#44481,#44482,#44483)) ;
#16838 = EDGE_LOOP('',(#44484,#44485,#44486,#44487)) ;
#16839 = EDGE_LOOP('',(#44488,#44489,#44490,#44491)) ;
#16840 = EDGE_LOOP('',(#44492,#44493,#44494,#44495)) ;
#16841 = EDGE_LOOP('',(#44496,#44497,#44498,#44499)) ;
#16842 = EDGE_LOOP('',(#44500,#44501,#44502,#44503)) ;
#16843 = EDGE_LOOP('',(#44504,#44505,#44506,#44507)) ;
#16844 = EDGE_LOOP('',(#44508,#44509,#44510,#44511)) ;
#16845 = EDGE_LOOP('',(#44512,#44513,#44514,#44515)) ;
#16846 = EDGE_LOOP('',(#44516,#44517,#44518,#44519)) ;
#16847 = EDGE_LOOP('',(#44520,#44521,#44522,#44523)) ;
#16848 = EDGE_LOOP('',(#44524,#44525,#44526,#44527)) ;
#16849 = EDGE_LOOP('',(#44528,#44529,#44530,#44531)) ;
#16850 = EDGE_LOOP('',(#44532,#44533,#44534,#44535)) ;
#16851 = EDGE_LOOP('',(#44536,#44537,#44538,#44539)) ;
#16852 = EDGE_LOOP('',(#44540,#44541,#44542,#44543)) ;
#16853 = EDGE_LOOP('',(#44544,#44545,#44546,#44547)) ;
#16854 = EDGE_LOOP('',(#44548,#44549,#44550,#44551)) ;
#16855 = EDGE_LOOP('',(#44552,#44553,#44554,#44555)) ;
#16856 = EDGE_LOOP('',(#44556,#44557,#44558,#44559)) ;
#16857 = EDGE_LOOP('',(#44560,#44561,#44562,#44563)) ;
#16858 = EDGE_LOOP('',(#44564,#44565,#44566,#44567)) ;
#16859 = EDGE_LOOP('',(#44568,#44569,#44570,#44571)) ;
#16860 = EDGE_LOOP('',(#44572,#44573,#44574,#44575)) ;
#16861 = EDGE_LOOP('',(#44576,#44577,#44578,#44579)) ;
#16862 = EDGE_LOOP('',(#44580,#44581,#44582,#44583)) ;
#16863 = EDGE_LOOP('',(#44584,#44585,#44586,#44587,#44588)) ;
#16864 = EDGE_LOOP('',(#44589,#44590,#44591,#44592,#44593,#44594,#44595,#44596,
#44597,#44598,#44599,#44600,#44601,#44602,#44603,#44604,#44605,#44606,#44607,
#44608,#44609,#44610,#44611,#44612,#44613,#44614,#44615,#44616,#44617,#44618,
#44619,#44620,#44621,#44622,#44623,#44624,#44625,#44626,#44627,#44628,#44629,
#44630,#44631,#44632,#44633)) ;
#16865 = EDGE_LOOP('',(#44634,#44635,#44636,#44637)) ;
#16866 = EDGE_LOOP('',(#44638,#44639,#44640,#44641,#44642,#44643,#44644,#44645,
#44646,#44647,#44648,#44649,#44650,#44651,#44652,#44653,#44654,#44655,#44656,
#44657,#44658,#44659,#44660,#44661,#44662,#44663,#44664,#44665,#44666,#44667,
#44668,#44669,#44670,#44671,#44672,#44673,#44674,#44675,#44676,#44677,#44678,
#44679,#44680,#44681,#44682)) ;
#16867 = EDGE_LOOP('',(#44683,#44684,#44685,#44686)) ;
#16868 = EDGE_LOOP('',(#44687,#44688,#44689,#44690)) ;
#16869 = EDGE_LOOP('',(#44691,#44692,#44693,#44694)) ;
#16870 = EDGE_LOOP('',(#44695,#44696,#44697,#44698)) ;
#16871 = EDGE_LOOP('',(#44699,#44700,#44701,#44702)) ;
#16872 = EDGE_LOOP('',(#44703,#44704,#44705,#44706)) ;
#16873 = EDGE_LOOP('',(#44707,#44708,#44709,#44710)) ;
#16874 = EDGE_LOOP('',(#44711,#44712,#44713,#44714)) ;
#16875 = EDGE_LOOP('',(#44715,#44716,#44717,#44718)) ;
#16876 = EDGE_LOOP('',(#44719,#44720,#44721,#44722)) ;
#16877 = EDGE_LOOP('',(#44723,#44724,#44725,#44726)) ;
#16878 = EDGE_LOOP('',(#44727,#44728,#44729,#44730)) ;
#16879 = EDGE_LOOP('',(#44731,#44732,#44733,#44734)) ;
#16880 = EDGE_LOOP('',(#44735,#44736,#44737,#44738)) ;
#16881 = EDGE_LOOP('',(#44739,#44740,#44741,#44742)) ;
#16882 = EDGE_LOOP('',(#44743,#44744,#44745,#44746)) ;
#16883 = EDGE_LOOP('',(#44747,#44748,#44749,#44750)) ;
#16884 = EDGE_LOOP('',(#44751,#44752,#44753,#44754)) ;
#16885 = EDGE_LOOP('',(#44755,#44756,#44757,#44758)) ;
#16886 = EDGE_LOOP('',(#44759,#44760,#44761,#44762,#44763)) ;
#16887 = EDGE_LOOP('',(#44764,#44765,#44766,#44767)) ;
#16888 = EDGE_LOOP('',(#44768,#44769,#44770,#44771)) ;
#16889 = EDGE_LOOP('',(#44772,#44773,#44774,#44775)) ;
#16890 = EDGE_LOOP('',(#44776,#44777,#44778,#44779)) ;
#16891 = EDGE_LOOP('',(#44780,#44781,#44782,#44783)) ;
#16892 = EDGE_LOOP('',(#44784,#44785,#44786,#44787)) ;
#16893 = EDGE_LOOP('',(#44788,#44789,#44790,#44791)) ;
#16894 = EDGE_LOOP('',(#44792,#44793,#44794,#44795)) ;
#16895 = EDGE_LOOP('',(#44796,#44797,#44798,#44799)) ;
#16896 = EDGE_LOOP('',(#44800,#44801,#44802,#44803)) ;
#16897 = EDGE_LOOP('',(#44804,#44805,#44806,#44807)) ;
#16898 = EDGE_LOOP('',(#44808,#44809,#44810,#44811)) ;
#16899 = EDGE_LOOP('',(#44812,#44813,#44814,#44815)) ;
#16900 = EDGE_LOOP('',(#44816,#44817,#44818,#44819)) ;
#16901 = EDGE_LOOP('',(#44820,#44821,#44822,#44823)) ;
#16902 = EDGE_LOOP('',(#44824,#44825,#44826,#44827)) ;
#16903 = EDGE_LOOP('',(#44828,#44829,#44830,#44831)) ;
#16904 = EDGE_LOOP('',(#44832,#44833,#44834,#44835)) ;
#16905 = EDGE_LOOP('',(#44836,#44837,#44838,#44839)) ;
#16906 = EDGE_LOOP('',(#44840,#44841,#44842,#44843)) ;
#16907 = EDGE_LOOP('',(#44844,#44845,#44846,#44847)) ;
#16908 = EDGE_LOOP('',(#44848,#44849,#44850,#44851)) ;
#16909 = EDGE_LOOP('',(#44852,#44853,#44854,#44855)) ;
#16910 = EDGE_LOOP('',(#44856,#44857,#44858,#44859)) ;
#16911 = EDGE_LOOP('',(#44860,#44861,#44862,#44863)) ;
#16912 = EDGE_LOOP('',(#44864,#44865,#44866,#44867)) ;
#16913 = EDGE_LOOP('',(#44868,#44869,#44870,#44871)) ;
#16914 = EDGE_LOOP('',(#44872,#44873,#44874,#44875)) ;
#16915 = EDGE_LOOP('',(#44876,#44877,#44878,#44879)) ;
#16916 = EDGE_LOOP('',(#44880,#44881,#44882,#44883)) ;
#16917 = EDGE_LOOP('',(#44884,#44885,#44886,#44887)) ;
#16918 = EDGE_LOOP('',(#44888,#44889,#44890,#44891)) ;
#16919 = EDGE_LOOP('',(#44892,#44893,#44894,#44895)) ;
#16920 = EDGE_LOOP('',(#44896,#44897,#44898,#44899)) ;
#16921 = EDGE_LOOP('',(#44900,#44901,#44902,#44903)) ;
#16922 = EDGE_LOOP('',(#44904,#44905,#44906,#44907)) ;
#16923 = EDGE_LOOP('',(#44908,#44909,#44910,#44911)) ;
#16924 = EDGE_LOOP('',(#44912,#44913,#44914,#44915)) ;
#16925 = EDGE_LOOP('',(#44916,#44917,#44918,#44919)) ;
#16926 = EDGE_LOOP('',(#44920,#44921,#44922,#44923)) ;
#16927 = EDGE_LOOP('',(#44924,#44925,#44926,#44927)) ;
#16928 = EDGE_LOOP('',(#44928,#44929,#44930,#44931)) ;
#16929 = EDGE_LOOP('',(#44932,#44933,#44934,#44935)) ;
#16930 = EDGE_LOOP('',(#44936,#44937,#44938,#44939)) ;
#16931 = EDGE_LOOP('',(#44940,#44941,#44942,#44943)) ;
#16932 = EDGE_LOOP('',(#44944,#44945,#44946,#44947)) ;
#16933 = EDGE_LOOP('',(#44948,#44949,#44950,#44951)) ;
#16934 = EDGE_LOOP('',(#44952,#44953,#44954,#44955)) ;
#16935 = EDGE_LOOP('',(#44956,#44957,#44958,#44959)) ;
#16936 = EDGE_LOOP('',(#44960,#44961,#44962,#44963)) ;
#16937 = EDGE_LOOP('',(#44964,#44965,#44966,#44967)) ;
#16938 = EDGE_LOOP('',(#44968,#44969,#44970,#44971)) ;
#16939 = EDGE_LOOP('',(#44972,#44973,#44974,#44975)) ;
#16940 = EDGE_LOOP('',(#44976,#44977,#44978,#44979)) ;
#16941 = EDGE_LOOP('',(#44980,#44981,#44982,#44983)) ;
#16942 = EDGE_LOOP('',(#44984,#44985,#44986,#44987)) ;
#16943 = EDGE_LOOP('',(#44988,#44989,#44990,#44991)) ;
#16944 = EDGE_LOOP('',(#44992,#44993,#44994,#44995)) ;
#16945 = EDGE_LOOP('',(#44996,#44997,#44998,#44999)) ;
#16946 = EDGE_LOOP('',(#45000,#45001,#45002,#45003)) ;
#16947 = EDGE_LOOP('',(#45004,#45005,#45006,#45007)) ;
#16948 = EDGE_LOOP('',(#45008,#45009,#45010,#45011)) ;
#16949 = EDGE_LOOP('',(#45012,#45013,#45014,#45015)) ;
#16950 = EDGE_LOOP('',(#45016,#45017,#45018,#45019)) ;
#16951 = EDGE_LOOP('',(#45020,#45021,#45022,#45023)) ;
#16952 = EDGE_LOOP('',(#45024,#45025,#45026,#45027)) ;
#16953 = EDGE_LOOP('',(#45028,#45029,#45030,#45031)) ;
#16954 = EDGE_LOOP('',(#45032,#45033,#45034,#45035)) ;
#16955 = EDGE_LOOP('',(#45036,#45037,#45038,#45039)) ;
#16956 = EDGE_LOOP('',(#45040,#45041,#45042,#45043)) ;
#16957 = EDGE_LOOP('',(#45044,#45045,#45046,#45047)) ;
#16958 = EDGE_LOOP('',(#45048,#45049,#45050,#45051)) ;
#16959 = EDGE_LOOP('',(#45052,#45053,#45054,#45055)) ;
#16960 = EDGE_LOOP('',(#45056,#45057,#45058,#45059)) ;
#16961 = EDGE_LOOP('',(#45060,#45061,#45062,#45063)) ;
#16962 = EDGE_LOOP('',(#45064,#45065,#45066,#45067)) ;
#16963 = EDGE_LOOP('',(#45068,#45069,#45070,#45071)) ;
#16964 = EDGE_LOOP('',(#45072,#45073,#45074,#45075)) ;
#16965 = EDGE_LOOP('',(#45076,#45077,#45078,#45079)) ;
#16966 = EDGE_LOOP('',(#45080,#45081,#45082,#45083)) ;
#16967 = EDGE_LOOP('',(#45084,#45085,#45086,#45087)) ;
#16968 = EDGE_LOOP('',(#45088,#45089,#45090,#45091)) ;
#16969 = EDGE_LOOP('',(#45092,#45093,#45094,#45095)) ;
#16970 = EDGE_LOOP('',(#45096,#45097,#45098,#45099)) ;
#16971 = EDGE_LOOP('',(#45100,#45101,#45102,#45103)) ;
#16972 = EDGE_LOOP('',(#45104,#45105,#45106,#45107)) ;
#16973 = EDGE_LOOP('',(#45108,#45109,#45110,#45111)) ;
#16974 = EDGE_LOOP('',(#45112,#45113,#45114,#45115)) ;
#16975 = EDGE_LOOP('',(#45116,#45117,#45118,#45119)) ;
#16976 = EDGE_LOOP('',(#45120,#45121,#45122,#45123)) ;
#16977 = EDGE_LOOP('',(#45124,#45125,#45126,#45127)) ;
#16978 = EDGE_LOOP('',(#45128,#45129,#45130,#45131)) ;
#16979 = EDGE_LOOP('',(#45132,#45133,#45134,#45135)) ;
#16980 = EDGE_LOOP('',(#45136,#45137,#45138,#45139)) ;
#16981 = EDGE_LOOP('',(#45140,#45141,#45142,#45143)) ;
#16982 = EDGE_LOOP('',(#45144,#45145,#45146,#45147)) ;
#16983 = EDGE_LOOP('',(#45148,#45149,#45150,#45151)) ;
#16984 = EDGE_LOOP('',(#45152,#45153,#45154,#45155)) ;
#16985 = EDGE_LOOP('',(#45156,#45157,#45158,#45159)) ;
#16986 = EDGE_LOOP('',(#45160,#45161,#45162,#45163)) ;
#16987 = EDGE_LOOP('',(#45164,#45165,#45166,#45167)) ;
#16988 = EDGE_LOOP('',(#45168,#45169,#45170,#45171)) ;
#16989 = EDGE_LOOP('',(#45172,#45173,#45174,#45175)) ;
#16990 = EDGE_LOOP('',(#45176,#45177,#45178,#45179)) ;
#16991 = EDGE_LOOP('',(#45180,#45181,#45182,#45183)) ;
#16992 = EDGE_LOOP('',(#45184,#45185,#45186,#45187)) ;
#16993 = EDGE_LOOP('',(#45188,#45189,#45190,#45191)) ;
#16994 = EDGE_LOOP('',(#45192,#45193,#45194,#45195)) ;
#16995 = EDGE_LOOP('',(#45196,#45197,#45198,#45199)) ;
#16996 = EDGE_LOOP('',(#45200,#45201,#45202,#45203)) ;
#16997 = EDGE_LOOP('',(#45204,#45205,#45206,#45207)) ;
#16998 = EDGE_LOOP('',(#45208,#45209,#45210,#45211)) ;
#16999 = EDGE_LOOP('',(#45212,#45213,#45214,#45215)) ;
#17000 = EDGE_LOOP('',(#45216,#45217,#45218,#45219)) ;
#17001 = EDGE_LOOP('',(#45220,#45221,#45222,#45223)) ;
#17002 = EDGE_LOOP('',(#45224,#45225,#45226,#45227)) ;
#17003 = EDGE_LOOP('',(#45228,#45229,#45230,#45231)) ;
#17004 = EDGE_LOOP('',(#45232,#45233,#45234,#45235)) ;
#17005 = EDGE_LOOP('',(#45236,#45237,#45238,#45239)) ;
#17006 = EDGE_LOOP('',(#45240,#45241,#45242,#45243)) ;
#17007 = EDGE_LOOP('',(#45244,#45245,#45246,#45247)) ;
#17008 = EDGE_LOOP('',(#45248,#45249,#45250,#45251)) ;
#17009 = EDGE_LOOP('',(#45252,#45253,#45254,#45255)) ;
#17010 = EDGE_LOOP('',(#45256,#45257,#45258,#45259,#45260,#45261)) ;
#17011 = EDGE_LOOP('',(#45262,#45263,#45264,#45265,#45266,#45267)) ;
#17012 = EDGE_LOOP('',(#45268,#45269,#45270,#45271)) ;
#17013 = EDGE_LOOP('',(#45272,#45273,#45274,#45275,#45276)) ;
#17014 = EDGE_LOOP('',(#45277,#45278,#45279,#45280)) ;
#17015 = EDGE_LOOP('',(#45281,#45282,#45283,#45284,#45285)) ;
#17016 = EDGE_LOOP('',(#45286,#45287,#45288,#45289)) ;
#17017 = EDGE_LOOP('',(#45290,#45291,#45292,#45293,#45294)) ;
#17018 = EDGE_LOOP('',(#45295)) ;
#17019 = EDGE_LOOP('',(#45296,#45297,#45298,#45299,#45300,#45301,#45302,#45303,
#45304,#45305,#45306,#45307,#45308,#45309)) ;
#17020 = EDGE_LOOP('',(#45310,#45311,#45312,#45313,#45314,#45315,#45316,#45317,
#45318,#45319,#45320,#45321,#45322,#45323,#45324,#45325,#45326,#45327)) ;
#17021 = EDGE_LOOP('',(#45328)) ;
#17022 = EDGE_LOOP('',(#45329,#45330,#45331,#45332,#45333)) ;
#17023 = EDGE_LOOP('',(#45334,#45335,#45336,#45337,#45338)) ;
#17024 = EDGE_LOOP('',(#45339,#45340,#45341,#45342,#45343)) ;
#17025 = EDGE_LOOP('',(#45344,#45345,#45346,#45347,#45348,#45349,#45350,#45351,
#45352,#45353,#45354,#45355,#45356,#45357,#45358,#45359,#45360)) ;
#17026 = EDGE_LOOP('',(#45361,#45362,#45363,#45364,#45365)) ;
#17027 = EDGE_LOOP('',(#45366,#45367,#45368,#45369,#45370,#45371,#45372,#45373,
#45374,#45375,#45376,#45377,#45378,#45379,#45380,#45381)) ;
#17028 = EDGE_LOOP('',(#45382,#45383,#45384,#45385,#45386)) ;
#17029 = EDGE_LOOP('',(#45387,#45388,#45389,#45390,#45391,#45392,#45393,#45394,
#45395,#45396,#45397,#45398,#45399,#45400,#45401,#45402,#45403,#45404,#45405,
#45406,#45407)) ;
#17030 = EDGE_LOOP('',(#45408,#45409,#45410,#45411)) ;
#17031 = EDGE_LOOP('',(#45412,#45413,#45414,#45415,#45416,#45417,#45418,#45419,
#45420,#45421,#45422,#45423,#45424,#45425,#45426,#45427,#45428,#45429)) ;
#17032 = EDGE_LOOP('',(#45430)) ;
#17033 = EDGE_LOOP('',(#45431)) ;
#17034 = CIRCLE('',#49313,5.8) ;
#17035 = CIRCLE('',#49314,0.2) ;
#17036 = CIRCLE('',#49315,6.) ;
#17037 = CIRCLE('',#49317,6.) ;
#17038 = CIRCLE('',#49318,6.) ;
#17039 = CIRCLE('',#49319,6.) ;
#17040 = CIRCLE('',#49320,6.) ;
#17041 = CIRCLE('',#49321,6.) ;
#17042 = CIRCLE('',#49322,6.) ;
#17043 = CIRCLE('',#49323,6.) ;
#17044 = CIRCLE('',#49324,6.) ;
#17045 = CIRCLE('',#49325,6.) ;
#17046 = CIRCLE('',#49326,6.) ;
#17047 = CIRCLE('',#49327,6.) ;
#17048 = CIRCLE('',#49328,6.) ;
#17049 = CIRCLE('',#49329,6.) ;
#17050 = CIRCLE('',#49330,6.) ;
#17051 = CIRCLE('',#49331,6.) ;
#17052 = CIRCLE('',#49332,6.) ;
#17053 = CIRCLE('',#49333,6.) ;
#17054 = CIRCLE('',#49334,6.) ;
#17055 = CIRCLE('',#49335,6.) ;
#17056 = CIRCLE('',#49336,6.) ;
#17057 = CIRCLE('',#49337,6.) ;
#17058 = CIRCLE('',#49338,6.) ;
#17059 = CIRCLE('',#49339,6.) ;
#17060 = CIRCLE('',#49340,6.) ;
#17061 = CIRCLE('',#49341,6.) ;
#17062 = CIRCLE('',#49342,6.) ;
#17063 = CIRCLE('',#49343,6.) ;
#17064 = CIRCLE('',#49344,6.) ;
#17065 = CIRCLE('',#49345,6.) ;
#17066 = CIRCLE('',#49346,6.) ;
#17067 = CIRCLE('',#49347,6.) ;
#17068 = CIRCLE('',#49348,6.) ;
#17069 = CIRCLE('',#49349,6.) ;
#17070 = CIRCLE('',#49350,6.) ;
#17071 = CIRCLE('',#49351,6.) ;
#17072 = CIRCLE('',#49352,6.) ;
#17073 = CIRCLE('',#49353,6.) ;
#17074 = CIRCLE('',#49354,6.) ;
#17075 = CIRCLE('',#49355,6.) ;
#17076 = CIRCLE('',#49356,6.) ;
#17077 = CIRCLE('',#49357,6.) ;
#17078 = CIRCLE('',#49360,0.199999999999987) ;
#17079 = CIRCLE('',#49361,0.2) ;
#17080 = CIRCLE('',#49363,0.199999999999996) ;
#17081 = CIRCLE('',#49364,0.2) ;
#17082 = CIRCLE('',#49366,0.2) ;
#17083 = CIRCLE('',#49367,0.95) ;
#17084 = CIRCLE('',#49368,1.15) ;
#17085 = CIRCLE('',#49370,0.2) ;
#17086 = CIRCLE('',#49372,0.199999999999996) ;
#17087 = CIRCLE('',#49373,0.2) ;
#17088 = CIRCLE('',#49375,0.199999999999996) ;
#17089 = CIRCLE('',#49376,0.2) ;
#17090 = CIRCLE('',#49378,0.2) ;
#17091 = CIRCLE('',#49379,0.95) ;
#17092 = CIRCLE('',#49380,1.15) ;
#17093 = CIRCLE('',#49382,0.2) ;
#17094 = CIRCLE('',#49384,0.199999999999996) ;
#17095 = CIRCLE('',#49385,0.2) ;
#17096 = CIRCLE('',#49387,0.200000000000005) ;
#17097 = CIRCLE('',#49388,0.2) ;
#17098 = CIRCLE('',#49390,0.2) ;
#17099 = CIRCLE('',#49391,0.95) ;
#17100 = CIRCLE('',#49392,1.15) ;
#17101 = CIRCLE('',#49394,0.2) ;
#17102 = CIRCLE('',#49396,0.199999999999996) ;
#17103 = CIRCLE('',#49397,0.2) ;
#17104 = CIRCLE('',#49399,0.200000000000031) ;
#17105 = CIRCLE('',#49400,1.15) ;
#17106 = CIRCLE('',#49401,0.2) ;
#17107 = CIRCLE('',#49402,0.95) ;
#17108 = CIRCLE('',#49404,0.2) ;
#17109 = CIRCLE('',#49406,0.199999999999996) ;
#17110 = CIRCLE('',#49408,0.199999999999995) ;
#17111 = CIRCLE('',#49410,0.199999999999995) ;
#17112 = CIRCLE('',#49412,0.199999999999995) ;
#17113 = CIRCLE('',#49414,0.200000000000001) ;
#17114 = CIRCLE('',#49416,0.199999999999988) ;
#17115 = CIRCLE('',#49418,0.199999999999995) ;
#17116 = CIRCLE('',#49420,0.200000000000001) ;
#17117 = CIRCLE('',#49422,0.199999999999995) ;
#17118 = CIRCLE('',#49425,0.199999999999996) ;
#17119 = CIRCLE('',#49428,0.199999999999996) ;
#17120 = CIRCLE('',#49431,0.95) ;
#17121 = CIRCLE('',#49434,0.199999999999996) ;
#17122 = CIRCLE('',#49437,0.199999999999996) ;
#17123 = CIRCLE('',#49440,0.95) ;
#17124 = CIRCLE('',#49443,0.199999999999995) ;
#17125 = CIRCLE('',#49444,0.199999999999992) ;
#17126 = CIRCLE('',#49445,0.199999999999994) ;
#17127 = CIRCLE('',#49447,0.199999999999988) ;
#17128 = CIRCLE('',#49448,0.199999999999996) ;
#17129 = CIRCLE('',#49449,0.199999999999999) ;
#17130 = CIRCLE('',#49451,0.199999999999999) ;
#17131 = CIRCLE('',#49452,0.199999999999982) ;
#17132 = CIRCLE('',#49453,0.2) ;
#17133 = CIRCLE('',#49455,5.969599660801) ;
#17134 = CIRCLE('',#49457,0.200000000000008) ;
#17135 = CIRCLE('',#49458,0.19999999999999) ;
#17136 = CIRCLE('',#49459,0.200000000000008) ;
#17137 = CIRCLE('',#49461,0.199999999999994) ;
#17138 = CIRCLE('',#49462,0.199999999999987) ;
#17139 = CIRCLE('',#49463,0.199999999999998) ;
#17140 = CIRCLE('',#49465,0.20000000000001) ;
#17141 = CIRCLE('',#49466,0.199999999999985) ;
#17142 = CIRCLE('',#49467,0.2) ;
#17143 = CIRCLE('',#49469,0.200000000000011) ;
#17144 = CIRCLE('',#49470,0.199999999999991) ;
#17145 = CIRCLE('',#49471,0.200000000000002) ;
#17146 = CIRCLE('',#49473,5.96959966080102) ;
#17147 = CIRCLE('',#49475,0.199999999999997) ;
#17148 = CIRCLE('',#49476,0.199999999999996) ;
#17149 = CIRCLE('',#49477,0.200000000000025) ;
#17150 = CIRCLE('',#49479,0.200000000000012) ;
#17151 = CIRCLE('',#49480,0.199999999999987) ;
#17152 = CIRCLE('',#49481,0.199999999999999) ;
#17153 = CIRCLE('',#49483,0.20000000000003) ;
#17154 = CIRCLE('',#49484,0.200000000000018) ;
#17155 = CIRCLE('',#49485,0.200000000000015) ;
#17156 = CIRCLE('',#49487,0.19999999999999) ;
#17157 = CIRCLE('',#49488,0.200000000000018) ;
#17158 = CIRCLE('',#49489,0.200000000000003) ;
#17159 = CIRCLE('',#49491,5.96959966080103) ;
#17160 = CIRCLE('',#49493,0.200000000000015) ;
#17161 = CIRCLE('',#49494,0.200000000000001) ;
#17162 = CIRCLE('',#49495,0.200000000000003) ;
#17163 = CIRCLE('',#49497,0.200000000000041) ;
#17164 = CIRCLE('',#49498,0.199999999999999) ;
#17165 = CIRCLE('',#49499,0.200000000000003) ;
#17166 = CIRCLE('',#49501,0.199999999999998) ;
#17167 = CIRCLE('',#49502,0.200000000000007) ;
#17168 = CIRCLE('',#49503,0.200000000000005) ;
#17169 = CIRCLE('',#49505,0.199999999999993) ;
#17170 = CIRCLE('',#49506,0.200000000000012) ;
#17171 = CIRCLE('',#49507,0.199999999999966) ;
#17172 = CIRCLE('',#49509,5.96959966080102) ;
#17173 = CIRCLE('',#49511,0.200000000000011) ;
#17174 = CIRCLE('',#49512,0.200000000000011) ;
#17175 = CIRCLE('',#49513,0.200000000000004) ;
#17176 = CIRCLE('',#49515,0.200000000000011) ;
#17177 = CIRCLE('',#49516,0.199999999999993) ;
#17178 = CIRCLE('',#49517,0.199999999999993) ;
#17179 = CIRCLE('',#49519,0.199999999999991) ;
#17180 = CIRCLE('',#49520,0.200000000000016) ;
#17181 = CIRCLE('',#49521,0.199999999999994) ;
#17182 = CIRCLE('',#49523,0.199999999999997) ;
#17183 = CIRCLE('',#49524,0.200000000000006) ;
#17184 = CIRCLE('',#49525,0.199999999999972) ;
#17185 = CIRCLE('',#49527,5.96959966080102) ;
#17186 = CIRCLE('',#49529,0.200000000000025) ;
#17187 = CIRCLE('',#49530,0.199999999999982) ;
#17188 = CIRCLE('',#49531,0.200000000000005) ;
#17189 = CIRCLE('',#49533,0.200000000000004) ;
#17190 = CIRCLE('',#49534,0.199999999999997) ;
#17191 = CIRCLE('',#49535,0.200000000000013) ;
#17192 = CIRCLE('',#49537,0.199999999999988) ;
#17193 = CIRCLE('',#49538,0.199999999999999) ;
#17194 = CIRCLE('',#49539,0.200000000000008) ;
#17195 = CIRCLE('',#49541,0.199999999999983) ;
#17196 = CIRCLE('',#49542,0.200000000000023) ;
#17197 = CIRCLE('',#49543,0.199999999999958) ;
#17198 = CIRCLE('',#49545,5.96959966080103) ;
#17199 = CIRCLE('',#49547,0.199999999999977) ;
#17200 = CIRCLE('',#49548,0.199999999999992) ;
#17201 = CIRCLE('',#49549,0.200000000000011) ;
#17202 = CIRCLE('',#49551,0.200000000000011) ;
#17203 = CIRCLE('',#49552,0.199999999999988) ;
#17204 = CIRCLE('',#49553,0.200000000000004) ;
#17205 = CIRCLE('',#49555,0.200000000000011) ;
#17206 = CIRCLE('',#49556,0.199999999999997) ;
#17207 = CIRCLE('',#49557,0.200000000000003) ;
#17208 = CIRCLE('',#49559,0.200000000000004) ;
#17209 = CIRCLE('',#49560,0.200000000000027) ;
#17210 = CIRCLE('',#49561,0.200000000000023) ;
#17211 = CIRCLE('',#49563,5.96959966080103) ;
#17212 = CIRCLE('',#49565,0.200000000000041) ;
#17213 = CIRCLE('',#49566,0.199999999999997) ;
#17214 = CIRCLE('',#49567,0.200000000000006) ;
#17215 = CIRCLE('',#49569,0.199999999999987) ;
#17216 = CIRCLE('',#49570,0.199999999999974) ;
#17217 = CIRCLE('',#49571,0.200000000000003) ;
#17218 = CIRCLE('',#49573,0.19999999999999) ;
#17219 = CIRCLE('',#49574,0.200000000000024) ;
#17220 = CIRCLE('',#49575,0.199999999999975) ;
#17221 = CIRCLE('',#49577,0.199999999999998) ;
#17222 = CIRCLE('',#49578,0.199999999999994) ;
#17223 = CIRCLE('',#49579,0.199999999999988) ;
#17224 = CIRCLE('',#49581,5.96959966080101) ;
#17225 = CIRCLE('',#49583,0.199999999999973) ;
#17226 = CIRCLE('',#49584,0.199999999999997) ;
#17227 = CIRCLE('',#49585,0.200000000000006) ;
#17228 = CIRCLE('',#49587,0.200000000000005) ;
#17229 = CIRCLE('',#49588,0.199999999999995) ;
#17230 = CIRCLE('',#49589,0.199999999999988) ;
#17231 = CIRCLE('',#49591,0.199999999999998) ;
#17232 = CIRCLE('',#49592,0.200000000000031) ;
#17233 = CIRCLE('',#49593,0.199999999999995) ;
#17234 = CIRCLE('',#49595,0.20000000000001) ;
#17235 = CIRCLE('',#49596,0.199999999999985) ;
#17236 = CIRCLE('',#49597,0.200000000000003) ;
#17237 = CIRCLE('',#49599,5.96959966080101) ;
#17238 = CIRCLE('',#49601,0.199999999999984) ;
#17239 = CIRCLE('',#49602,0.199999999999994) ;
#17240 = CIRCLE('',#49603,0.199999999999998) ;
#17241 = CIRCLE('',#49605,0.200000000000008) ;
#17242 = CIRCLE('',#49606,0.199999999999995) ;
#17243 = CIRCLE('',#49607,0.199999999999974) ;
#17244 = CIRCLE('',#49609,0.199999999999963) ;
#17245 = CIRCLE('',#49610,0.199999999999986) ;
#17246 = CIRCLE('',#49611,0.199999999999991) ;
#17247 = CIRCLE('',#49613,0.199999999999988) ;
#17248 = CIRCLE('',#49614,0.199999999999968) ;
#17249 = CIRCLE('',#49615,0.199999999999999) ;
#17250 = CIRCLE('',#49617,5.96959966080098) ;
#17251 = CIRCLE('',#49619,0.199999999999995) ;
#17252 = CIRCLE('',#49620,0.199999999999996) ;
#17253 = CIRCLE('',#49621,0.199999999999998) ;
#17254 = CIRCLE('',#49623,5.96959966080099) ;
#17255 = CIRCLE('',#49628,5.8) ;
#17256 = CIRCLE('',#49631,5.96959966080104) ;
#17257 = CIRCLE('',#49634,5.8) ;
#17258 = CIRCLE('',#49637,5.8) ;
#17259 = CIRCLE('',#49641,5.96959966080103) ;
#17260 = CIRCLE('',#49644,5.8) ;
#17261 = CIRCLE('',#49647,5.8) ;
#17262 = CIRCLE('',#49651,5.96959966080101) ;
#17263 = CIRCLE('',#49654,5.8) ;
#17264 = CIRCLE('',#49657,5.8) ;
#17265 = CIRCLE('',#49661,5.96959966080102) ;
#17266 = CIRCLE('',#49664,5.8) ;
#17267 = CIRCLE('',#49667,5.8) ;
#17268 = CIRCLE('',#49671,5.96959966080103) ;
#17269 = CIRCLE('',#49674,5.8) ;
#17270 = CIRCLE('',#49677,5.8) ;
#17271 = CIRCLE('',#49681,5.96959966080102) ;
#17272 = CIRCLE('',#49684,5.8) ;
#17273 = CIRCLE('',#49687,5.8) ;
#17274 = CIRCLE('',#49691,5.96959966080101) ;
#17275 = CIRCLE('',#49694,5.8) ;
#17276 = CIRCLE('',#49697,5.8) ;
#17277 = CIRCLE('',#49701,5.96959966080101) ;
#17278 = CIRCLE('',#49704,5.8) ;
#17279 = CIRCLE('',#49707,5.8) ;
#17280 = CIRCLE('',#49711,5.96959966080104) ;
#17281 = CIRCLE('',#49714,5.8) ;
#17282 = CIRCLE('',#49717,5.8) ;
#17283 = CIRCLE('',#49721,5.8) ;
#17284 = CIRCLE('',#49723,0.599999999999996) ;
#17285 = CIRCLE('',#49725,0.599999999999996) ;
#17286 = CIRCLE('',#49727,0.599999999999996) ;
#17287 = CIRCLE('',#49729,0.599999999999996) ;
#17288 = CIRCLE('',#49731,0.599999999999996) ;
#17289 = CIRCLE('',#49733,0.599999999999996) ;
#17290 = CIRCLE('',#49735,0.599999999999996) ;
#17291 = CIRCLE('',#49737,0.599999999999996) ;
#17292 = CIRCLE('',#49739,0.599999999999996) ;
#17293 = CIRCLE('',#49741,0.599999999999996) ;
#17294 = CIRCLE('',#49743,0.599999999999996) ;
#17295 = CIRCLE('',#49745,0.599999999999996) ;
#17296 = CIRCLE('',#49747,0.599999999999996) ;
#17297 = CIRCLE('',#49749,0.599999999999996) ;
#17298 = CIRCLE('',#49751,0.599999999999996) ;
#17299 = CIRCLE('',#49753,0.599999999999996) ;
#17300 = CIRCLE('',#49755,0.599999999999996) ;
#17301 = CIRCLE('',#49757,0.599999999999996) ;
#17302 = CIRCLE('',#49759,0.599999999999996) ;
#17303 = CIRCLE('',#49761,0.599999999999996) ;
#17304 = CIRCLE('',#49763,5.3087501324996) ;
#17305 = CIRCLE('',#49765,0.200000000000005) ;
#17306 = CIRCLE('',#49766,0.75) ;
#17307 = CIRCLE('',#49767,0.2) ;
#17308 = CIRCLE('',#49769,5.13915047169858) ;
#17309 = CIRCLE('',#49770,0.399999999999992) ;
#17310 = CIRCLE('',#49771,0.399999999999992) ;
#17311 = CIRCLE('',#49772,0.75) ;
#17312 = CIRCLE('',#49773,0.399999999999992) ;
#17313 = CIRCLE('',#49774,0.399999999999992) ;
#17314 = CIRCLE('',#49775,0.75) ;
#17315 = CIRCLE('',#49776,0.399999999999992) ;
#17316 = CIRCLE('',#49777,0.399999999999983) ;
#17317 = CIRCLE('',#49778,0.75) ;
#17318 = CIRCLE('',#49779,0.399999999999992) ;
#17319 = CIRCLE('',#49780,0.399999999999992) ;
#17320 = CIRCLE('',#49782,0.199999999999996) ;
#17321 = CIRCLE('',#49785,0.199999999999996) ;
#17322 = CIRCLE('',#49786,0.2) ;
#17323 = CIRCLE('',#49788,0.199999999999996) ;
#17324 = CIRCLE('',#49790,0.200000000000031) ;
#17325 = CIRCLE('',#49791,0.2) ;
#17326 = CIRCLE('',#49792,0.95) ;
#17327 = CIRCLE('',#49795,0.199999999999996) ;
#17328 = CIRCLE('',#49798,0.200000000000005) ;
#17329 = CIRCLE('',#49799,0.2) ;
#17330 = CIRCLE('',#49800,0.95) ;
#17331 = CIRCLE('',#49803,0.199999999999996) ;
#17332 = CIRCLE('',#49805,0.2) ;
#17333 = CIRCLE('',#49807,0.2) ;
#17334 = CIRCLE('',#49809,0.199999999999996) ;
#17335 = CIRCLE('',#49810,0.2) ;
#17336 = CIRCLE('',#49813,0.2) ;
#17337 = CIRCLE('',#49814,0.199999999999996) ;
#17338 = CIRCLE('',#49818,0.2) ;
#17339 = CIRCLE('',#49820,0.199999999999996) ;
#17340 = CIRCLE('',#49821,0.2) ;
#17341 = CIRCLE('',#49824,0.199999999999996) ;
#17342 = CIRCLE('',#49825,0.199999999999996) ;
#17343 = CIRCLE('',#49826,0.2) ;
#17344 = CIRCLE('',#49830,0.199999999999996) ;
#17345 = CIRCLE('',#49831,0.199999999999996) ;
#17346 = CIRCLE('',#49832,0.2) ;
#17347 = CIRCLE('',#49835,0.199999999999996) ;
#17348 = CIRCLE('',#49836,0.2) ;
#17349 = CIRCLE('',#49867,0.119999999999978) ;
#17350 = CIRCLE('',#49868,0.119999999999985) ;
#17351 = CIRCLE('',#49869,0.420453920364715) ;
#17352 = CIRCLE('',#49870,0.12) ;
#17353 = CIRCLE('',#49871,0.300324228815928) ;
#17354 = CIRCLE('',#49873,0.119999999999985) ;
#17355 = CIRCLE('',#49875,0.12000000000001) ;
#17356 = CIRCLE('',#49878,0.120000000000005) ;
#17357 = CIRCLE('',#49880,0.120000000000011) ;
#17358 = CIRCLE('',#49881,0.12) ;
#17359 = CIRCLE('',#49882,0.120000000000005) ;
#17360 = CIRCLE('',#49884,0.120000000000005) ;
#17361 = CIRCLE('',#49886,0.120000000000023) ;
#17362 = CIRCLE('',#49888,0.120000000000006) ;
#17363 = CIRCLE('',#49889,0.12000000000004) ;
#17364 = CIRCLE('',#49891,0.120000000000005) ;
#17365 = CIRCLE('',#49897,3.48) ;
#17366 = CIRCLE('',#49898,8.88713010990353) ;
#17367 = CIRCLE('',#49902,33.1299448717372) ;
#17368 = CIRCLE('',#49906,33.6004676577322) ;
#17369 = CIRCLE('',#49907,3.48) ;
#17370 = CIRCLE('',#49914,9.12754474878259) ;
#17371 = CIRCLE('',#49915,3.48) ;
#17372 = CIRCLE('',#49916,2.12) ;
#17373 = CIRCLE('',#49918,0.12) ;
#17374 = CIRCLE('',#49919,0.120000000000005) ;
#17375 = CIRCLE('',#49921,0.119999999999995) ;
#17376 = CIRCLE('',#49922,0.120000000000007) ;
#17377 = CIRCLE('',#49923,0.119999999999985) ;
#17378 = CIRCLE('',#49925,0.119999999999985) ;
#17379 = CIRCLE('',#49926,0.11999999999998) ;
#17380 = CIRCLE('',#49927,0.120000000000006) ;
#17381 = CIRCLE('',#49931,0.12) ;
#17382 = CIRCLE('',#49932,2.) ;
#17383 = CIRCLE('',#49934,2.) ;
#17384 = CIRCLE('',#49939,3.6) ;
#17385 = CIRCLE('',#49941,0.12) ;
#17386 = CIRCLE('',#49942,33.4983398799233) ;
#17387 = CIRCLE('',#49943,0.12) ;
#17388 = CIRCLE('',#49945,0.12) ;
#17389 = CIRCLE('',#49947,0.12) ;
#17390 = CIRCLE('',#49948,0.12) ;
#17391 = CIRCLE('',#49949,0.12) ;
#17392 = CIRCLE('',#49951,0.12) ;
#17393 = CIRCLE('',#49952,0.12) ;
#17394 = CIRCLE('',#49954,0.12) ;
#17395 = CIRCLE('',#49955,0.12) ;
#17396 = CIRCLE('',#49956,33.2502644468207) ;
#17397 = CIRCLE('',#49957,0.12) ;
#17398 = CIRCLE('',#49959,0.12) ;
#17399 = CIRCLE('',#49961,0.12) ;
#17400 = CIRCLE('',#49963,0.12) ;
#17401 = CIRCLE('',#49964,9.00722646272021) ;
#17402 = CIRCLE('',#49969,3.6) ;
#17403 = CIRCLE('',#49971,33.2502644469926) ;
#17404 = CIRCLE('',#49979,3.6) ;
#17405 = CIRCLE('',#49982,3.6) ;
#17406 = CIRCLE('',#49983,0.119999999999985) ;
#17407 = CIRCLE('',#49984,0.12) ;
#17408 = CIRCLE('',#49986,0.120000000000048) ;
#17409 = CIRCLE('',#49987,0.119999999999985) ;
#17410 = CIRCLE('',#49988,0.12) ;
#17411 = CIRCLE('',#49989,0.119999999999999) ;
#17412 = CIRCLE('',#49990,0.12) ;
#17413 = CIRCLE('',#49992,0.119999999999985) ;
#17414 = CIRCLE('',#49993,0.119999999999999) ;
#17415 = CIRCLE('',#49994,0.119999999999999) ;
#17416 = CIRCLE('',#49995,0.12) ;
#17417 = CIRCLE('',#49996,0.120000000000005) ;
#17418 = CIRCLE('',#49998,0.12) ;
#17419 = CIRCLE('',#50005,0.119999999999992) ;
#17420 = CIRCLE('',#50006,0.120000000000003) ;
#17421 = CIRCLE('',#50010,0.12) ;
#17422 = CIRCLE('',#50012,0.12) ;
#17423 = CIRCLE('',#50013,9.00744547576183) ;
#17424 = CIRCLE('',#50014,8.88734620275781) ;
#17425 = CIRCLE('',#50018,0.120000000000011) ;
#17426 = CIRCLE('',#50019,9.00744547576355) ;
#17427 = CIRCLE('',#50020,0.120000000000005) ;
#17428 = CIRCLE('',#50024,3.6) ;
#17429 = CIRCLE('',#50028,0.11999999999999) ;
#17430 = CIRCLE('',#50029,0.120000000000005) ;
#17431 = CIRCLE('',#50030,0.120000000000003) ;
#17432 = CIRCLE('',#50032,0.119999999999969) ;
#17433 = CIRCLE('',#50035,0.120000000000005) ;
#17434 = CIRCLE('',#50036,0.120000000000038) ;
#17435 = CIRCLE('',#50038,0.119999999999997) ;
#17436 = CIRCLE('',#50039,0.119999999999985) ;
#17437 = CIRCLE('',#50042,0.120000000000006) ;
#17438 = CIRCLE('',#50043,0.12) ;
#17439 = CIRCLE('',#50044,0.120000000000007) ;
#17440 = CIRCLE('',#50045,0.120000000000005) ;
#17441 = CIRCLE('',#50048,0.120000000000005) ;
#17442 = CIRCLE('',#50049,0.119999999999998) ;
#17443 = CIRCLE('',#50050,0.120000000000008) ;
#17444 = CIRCLE('',#50051,0.119999999999969) ;
#17445 = CIRCLE('',#50057,0.120000000000005) ;
#17446 = CIRCLE('',#50058,0.120000000000007) ;
#17447 = CIRCLE('',#50059,0.12) ;
#17448 = CIRCLE('',#50060,0.119999999999989) ;
#17449 = CIRCLE('',#50062,0.12) ;
#17450 = CIRCLE('',#50064,0.120000000000005) ;
#17451 = CIRCLE('',#50065,0.12) ;
#17452 = CIRCLE('',#50066,0.11999999999999) ;
#17453 = CIRCLE('',#50067,0.120000000000005) ;
#17454 = CIRCLE('',#50068,0.120000000000005) ;
#17455 = CIRCLE('',#50070,0.12) ;
#17456 = CIRCLE('',#50072,0.12) ;
#17457 = CIRCLE('',#50075,0.12) ;
#17458 = CIRCLE('',#50076,0.12) ;
#17459 = CIRCLE('',#50078,0.120000000000005) ;
#17460 = CIRCLE('',#50079,0.12) ;
#17461 = CIRCLE('',#50080,0.120000000000002) ;
#17462 = CIRCLE('',#50082,0.120000000000005) ;
#17463 = CIRCLE('',#50085,0.120000000000005) ;
#17464 = CIRCLE('',#50086,0.119999999999998) ;
#17465 = CIRCLE('',#50092,33.129944871325) ;
#17466 = CIRCLE('',#50096,0.120000000000005) ;
#17467 = CIRCLE('',#50097,0.12) ;
#17468 = CIRCLE('',#50099,0.120000000000001) ;
#17469 = CIRCLE('',#50100,0.120000000000005) ;
#17470 = CIRCLE('',#50101,0.12) ;
#17471 = CIRCLE('',#50102,0.12) ;
#17472 = CIRCLE('',#50104,0.12) ;
#17473 = CIRCLE('',#50105,0.119999999999996) ;
#17474 = CIRCLE('',#50106,0.12) ;
#17475 = CIRCLE('',#50108,0.120000000000005) ;
#17476 = CIRCLE('',#50109,0.12) ;
#17477 = CIRCLE('',#50110,0.12) ;
#17478 = CIRCLE('',#50112,0.119999999999996) ;
#17479 = CIRCLE('',#50113,0.12) ;
#17480 = CIRCLE('',#50114,0.119999999999985) ;
#17481 = CIRCLE('',#50115,0.119999999999985) ;
#17482 = CIRCLE('',#50116,0.12) ;
#17483 = CIRCLE('',#50118,0.120000000000003) ;
#17484 = CIRCLE('',#50119,0.120000000000021) ;
#17485 = CIRCLE('',#50120,0.120000000000021) ;
#17486 = CIRCLE('',#50121,0.12) ;
#17487 = CIRCLE('',#50131,33.4983398800573) ;
#17488 = CIRCLE('',#50132,0.120000000000003) ;
#17489 = CIRCLE('',#50137,0.119999999999997) ;
#17490 = CIRCLE('',#50138,0.119999999999985) ;
#17491 = CIRCLE('',#50139,0.119999999999985) ;
#17492 = CIRCLE('',#50140,0.12) ;
#17493 = CIRCLE('',#50141,0.12) ;
#17494 = CIRCLE('',#50142,0.12) ;
#17495 = CIRCLE('',#50143,0.12) ;
#17496 = CIRCLE('',#50144,0.12) ;
#17497 = CIRCLE('',#50145,0.12) ;
#17498 = CIRCLE('',#50148,0.12) ;
#17499 = CIRCLE('',#50149,0.12) ;
#17500 = CIRCLE('',#50150,0.12) ;
#17501 = CIRCLE('',#50151,0.12) ;
#17502 = CIRCLE('',#50152,0.12) ;
#17503 = CIRCLE('',#50160,3.6) ;
#17504 = CIRCLE('',#50179,0.119999488241585) ;
#17505 = CIRCLE('',#50181,0.120001966232961) ;
#17506 = CIRCLE('',#50232,0.120002766430327) ;
#17507 = CIRCLE('',#50242,0.119999998071627) ;
#17508 = CIRCLE('',#50252,2.6) ;
#17509 = CIRCLE('',#50253,2.6) ;
#17510 = CIRCLE('',#50256,0.5) ;
#17511 = CIRCLE('',#50257,0.5) ;
#17512 = CIRCLE('',#50258,0.200000000000031) ;
#17513 = CIRCLE('',#50259,0.199999999999996) ;
#17514 = CIRCLE('',#50260,0.5) ;
#17515 = CIRCLE('',#50261,0.7) ;
#17516 = CIRCLE('',#50262,3.9) ;
#17517 = CIRCLE('',#50263,3.9) ;
#17518 = CIRCLE('',#50264,3.9) ;
#17519 = CIRCLE('',#50265,0.7) ;
#17520 = CIRCLE('',#50266,0.5) ;
#17521 = CIRCLE('',#50267,0.500000000000023) ;
#17522 = CIRCLE('',#50268,2.59999999999999) ;
#17523 = CIRCLE('',#50269,2.59999999999996) ;
#17524 = CIRCLE('',#50270,0.500000000000005) ;
#17525 = CIRCLE('',#50271,0.5) ;
#17526 = CIRCLE('',#50272,0.7) ;
#17527 = CIRCLE('',#50273,0.200000000000031) ;
#17528 = CIRCLE('',#50274,0.199999999999996) ;
#17529 = CIRCLE('',#50275,0.200000000000031) ;
#17530 = CIRCLE('',#50276,0.200000000000031) ;
#17531 = CIRCLE('',#50277,0.199999999999996) ;
#17532 = CIRCLE('',#50278,0.199999999999996) ;
#17533 = CIRCLE('',#50279,0.200000000000031) ;
#17534 = CIRCLE('',#50280,0.199999999999969) ;
#17535 = CIRCLE('',#50281,0.199999999999978) ;
#17536 = CIRCLE('',#50282,0.199999999999969) ;
#17537 = CIRCLE('',#50283,0.200000000000031) ;
#17538 = CIRCLE('',#50284,0.199999999999996) ;
#17539 = CIRCLE('',#50285,0.200000000000031) ;
#17540 = CIRCLE('',#50286,0.200000000000031) ;
#17541 = CIRCLE('',#50287,0.199999999999996) ;
#17542 = CIRCLE('',#50288,0.199999999999996) ;
#17543 = CIRCLE('',#50289,0.200000000000031) ;
#17544 = CIRCLE('',#50290,0.199999999999996) ;
#17545 = CIRCLE('',#50291,0.2) ;
#17546 = CIRCLE('',#50292,0.200000000000031) ;
#17547 = CIRCLE('',#50293,0.199999999999996) ;
#17548 = CIRCLE('',#50294,0.199999999999996) ;
#17549 = CIRCLE('',#50295,0.200000000000031) ;
#17550 = CIRCLE('',#50296,0.199999999999996) ;
#17551 = CIRCLE('',#50297,0.200000000000001) ;
#17552 = CIRCLE('',#50298,0.199999999999996) ;
#17553 = CIRCLE('',#50299,0.199999999999969) ;
#17554 = CIRCLE('',#50300,0.200000000000031) ;
#17555 = CIRCLE('',#50301,2.6) ;
#17556 = CIRCLE('',#50302,0.200000000000031) ;
#17557 = CIRCLE('',#50303,0.199999999999929) ;
#17558 = CIRCLE('',#50304,0.199999999999973) ;
#17559 = CIRCLE('',#50305,0.199999999999966) ;
#17560 = CIRCLE('',#50306,0.200000000000031) ;
#17561 = CIRCLE('',#50307,4.06491106406736) ;
#17562 = CIRCLE('',#50308,4.06491106406735) ;
#17563 = CIRCLE('',#50309,0.199999999999957) ;
#17564 = CIRCLE('',#50310,0.199999999999969) ;
#17565 = CIRCLE('',#50311,0.199999999999969) ;
#17566 = CIRCLE('',#50312,0.199999999999996) ;
#17567 = CIRCLE('',#50313,4.06491106406736) ;
#17568 = CIRCLE('',#50314,2.1) ;
#17569 = CIRCLE('',#50315,0.200000000000031) ;
#17570 = CIRCLE('',#50316,0.199999999999996) ;
#17571 = CIRCLE('',#50317,0.200000000000031) ;
#17572 = CIRCLE('',#50318,0.199999999999996) ;
#17573 = CIRCLE('',#50319,0.200000000000031) ;
#17574 = CIRCLE('',#50320,0.199999999999996) ;
#17575 = CIRCLE('',#50321,0.200000000000031) ;
#17576 = CIRCLE('',#50322,0.200000000000031) ;
#17577 = CIRCLE('',#50323,0.199999999999996) ;
#17578 = CIRCLE('',#50324,0.199999999999996) ;
#17579 = CIRCLE('',#50350,2.) ;
#17580 = CIRCLE('',#50351,0.1) ;
#17581 = CIRCLE('',#50352,2.1) ;
#17582 = CIRCLE('',#50353,2.) ;
#17583 = CIRCLE('',#50355,2.89999999999999) ;
#17584 = CIRCLE('',#50357,2.) ;
#17585 = CIRCLE('',#50359,2.99999999999999) ;
#17586 = CIRCLE('',#50360,0.1) ;
#17587 = CIRCLE('',#50362,2.99999999999999) ;
#17588 = CIRCLE('',#50364,3.09999999999999) ;
#17589 = CIRCLE('',#50365,0.1) ;
#17590 = CIRCLE('',#50367,0.2) ;
#17591 = CIRCLE('',#50368,0.2) ;
#17592 = CIRCLE('',#50369,0.2) ;
#17593 = CIRCLE('',#50370,0.2) ;
#17594 = CIRCLE('',#50375,0.7) ;
#17595 = CIRCLE('',#50376,0.5) ;
#17596 = CIRCLE('',#50377,0.500000000000005) ;
#17597 = CIRCLE('',#50378,2.59999999999996) ;
#17598 = CIRCLE('',#50379,2.59999999999999) ;
#17599 = CIRCLE('',#50380,0.500000000000023) ;
#17600 = CIRCLE('',#50381,0.5) ;
#17601 = CIRCLE('',#50382,0.7) ;
#17602 = CIRCLE('',#50383,3.9) ;
#17603 = CIRCLE('',#50384,3.9) ;
#17604 = CIRCLE('',#50385,3.9) ;
#17605 = CIRCLE('',#50386,0.7) ;
#17606 = CIRCLE('',#50387,0.5) ;
#17607 = CIRCLE('',#50388,0.5) ;
#17608 = CIRCLE('',#50389,0.5) ;
#17609 = CIRCLE('',#50390,4.) ;
#17610 = CIRCLE('',#50391,0.2) ;
#17611 = CIRCLE('',#50392,0.2) ;
#17612 = CIRCLE('',#50393,0.2) ;
#17613 = CIRCLE('',#50394,0.2) ;
#17614 = CIRCLE('',#50395,0.2) ;
#17615 = CIRCLE('',#50396,0.2) ;
#17616 = CIRCLE('',#50397,2.6) ;
#17617 = CIRCLE('',#50398,2.5) ;
#17618 = CIRCLE('',#50399,0.200000000000067) ;
#17619 = CIRCLE('',#50400,0.2) ;
#17620 = CIRCLE('',#50401,0.2) ;
#17621 = CIRCLE('',#50402,0.2) ;
#17622 = CIRCLE('',#50403,0.2) ;
#17623 = CIRCLE('',#50404,0.199999999999996) ;
#17624 = CIRCLE('',#50405,2.) ;
#17625 = CIRCLE('',#50406,0.1) ;
#17626 = CIRCLE('',#50407,0.1) ;
#17627 = CIRCLE('',#50408,0.1) ;
#17628 = CIRCLE('',#50409,0.1) ;
#17629 = CIRCLE('',#50410,0.1) ;
#17630 = CIRCLE('',#50411,0.1) ;
#17631 = CIRCLE('',#50412,0.199999999999991) ;
#17632 = CIRCLE('',#50413,0.200000000000031) ;
#17633 = CIRCLE('',#50414,0.199999999999996) ;
#17634 = CIRCLE('',#50415,0.200000000000031) ;
#17635 = CIRCLE('',#50416,0.2) ;
#17636 = CIRCLE('',#50417,0.2) ;
#17637 = CIRCLE('',#50418,0.2) ;
#17638 = CIRCLE('',#50419,0.2) ;
#17639 = CIRCLE('',#50420,0.2) ;
#17640 = CIRCLE('',#50421,0.200000000000067) ;
#17641 = CIRCLE('',#50422,0.2) ;
#17642 = CIRCLE('',#50423,0.2) ;
#17643 = CIRCLE('',#50424,0.2) ;
#17644 = CIRCLE('',#50425,0.2) ;
#17645 = CIRCLE('',#50426,0.2) ;
#17646 = CIRCLE('',#50427,0.2) ;
#17647 = CIRCLE('',#50428,0.2) ;
#17648 = CIRCLE('',#50429,0.2) ;
#17649 = CIRCLE('',#50430,0.2) ;
#17650 = CIRCLE('',#50431,0.2) ;
#17651 = CIRCLE('',#50432,0.2) ;
#17652 = CIRCLE('',#50433,0.2) ;
#17653 = CIRCLE('',#50434,0.2) ;
#17654 = CIRCLE('',#50435,0.2) ;
#17655 = CIRCLE('',#50437,0.0999999999999934) ;
#17656 = CIRCLE('',#50438,0.399999999999996) ;
#17657 = CIRCLE('',#50439,0.1) ;
#17658 = CIRCLE('',#50440,0.5) ;
#17659 = CIRCLE('',#50442,0.100000000000002) ;
#17660 = CIRCLE('',#50444,0.100000000000005) ;
#17661 = CIRCLE('',#50445,1.9) ;
#17662 = CIRCLE('',#50446,2.) ;
#17663 = CIRCLE('',#50448,0.0999999999999979) ;
#17664 = CIRCLE('',#50450,0.0999999999999979) ;
#17665 = CIRCLE('',#50451,1.9) ;
#17666 = CIRCLE('',#50452,2.) ;
#17667 = CIRCLE('',#50454,0.100000000000002) ;
#17668 = CIRCLE('',#50456,0.100000000000007) ;
#17669 = CIRCLE('',#50457,2.7) ;
#17670 = CIRCLE('',#50458,2.6) ;
#17671 = CIRCLE('',#50460,0.0999999999999979) ;
#17672 = CIRCLE('',#50462,0.0999999999999979) ;
#17673 = CIRCLE('',#50463,1.9) ;
#17674 = CIRCLE('',#50464,2.) ;
#17675 = CIRCLE('',#50466,0.0999999999999956) ;
#17676 = CIRCLE('',#50468,0.0999999999999979) ;
#17677 = CIRCLE('',#50469,1.9) ;
#17678 = CIRCLE('',#50470,2.) ;
#17679 = CIRCLE('',#50472,0.0999999999999979) ;
#17680 = CIRCLE('',#50474,0.5) ;
#17681 = CIRCLE('',#50475,0.1) ;
#17682 = CIRCLE('',#50476,0.400000000000027) ;
#17683 = CIRCLE('',#50478,1.1) ;
#17684 = CIRCLE('',#50480,2.) ;
#17685 = CIRCLE('',#50483,2.) ;
#17686 = CIRCLE('',#50486,2.6) ;
#17687 = CIRCLE('',#50489,2.) ;
#17688 = CIRCLE('',#50492,2.) ;
#17689 = CIRCLE('',#50494,1.1) ;
#17690 = CIRCLE('',#50496,1.) ;
#17691 = CIRCLE('',#50497,3.) ;
#17692 = CIRCLE('',#50499,3.) ;
#17693 = CIRCLE('',#50501,0.12) ;
#17694 = CIRCLE('',#50502,2.88) ;
#17695 = CIRCLE('',#50504,2.12) ;
#17696 = CIRCLE('',#50506,2.) ;
#17697 = CIRCLE('',#50507,0.12) ;
#17698 = CIRCLE('',#50508,2.) ;
#17699 = CIRCLE('',#50510,2.) ;
#17700 = CIRCLE('',#50512,1.97000000000001) ;
#17701 = CIRCLE('',#50513,0.12) ;
#17702 = CIRCLE('',#50514,1.85) ;
#17703 = CIRCLE('',#50515,1.85) ;
#17704 = CIRCLE('',#50517,1.85) ;
#17705 = CIRCLE('',#50518,1.85) ;
#17706 = CIRCLE('',#50523,1.97000000000001) ;
#17707 = CIRCLE('',#50524,0.12) ;
#17708 = CIRCLE('',#50527,1.97) ;
#17709 = CIRCLE('',#50528,0.12) ;
#17710 = CIRCLE('',#50529,1.85) ;
#17711 = CIRCLE('',#50530,1.85) ;
#17712 = CIRCLE('',#50532,1.85) ;
#17713 = CIRCLE('',#50533,1.85) ;
#17714 = CIRCLE('',#50538,1.97) ;
#17715 = CIRCLE('',#50539,0.12) ;
#17716 = CIRCLE('',#50542,0.100000000000002) ;
#17717 = CIRCLE('',#50543,1.9) ;
#17718 = CIRCLE('',#50544,0.100000000000016) ;
#17719 = CIRCLE('',#50546,0.100000000000051) ;
#17720 = CIRCLE('',#50548,0.100000000000016) ;
#17721 = CIRCLE('',#50549,2.7) ;
#17722 = CIRCLE('',#50551,0.100000000000051) ;
#17723 = CIRCLE('',#50553,0.100000000000016) ;
#17724 = CIRCLE('',#50554,1.9) ;
#17725 = CIRCLE('',#50556,1.9) ;
#17726 = CIRCLE('',#50557,1.9) ;
#17727 = CIRCLE('',#50559,0.100000000000016) ;
#17728 = CIRCLE('',#50567,0.100000000000016) ;
#17729 = CIRCLE('',#50569,0.4) ;
#17730 = CIRCLE('',#50570,0.400000000000023) ;
#17731 = CIRCLE('',#50572,0.399999999999998) ;
#17732 = CIRCLE('',#50574,0.399999999999988) ;
#17733 = CIRCLE('',#50575,0.4) ;
#17734 = CIRCLE('',#50578,0.0999999999999979) ;
#17735 = CIRCLE('',#50580,0.100000000000016) ;
#17736 = CIRCLE('',#50581,0.1) ;
#17737 = CIRCLE('',#50582,0.100000000000002) ;
#17738 = CIRCLE('',#50584,0.0999999999999801) ;
#17739 = CIRCLE('',#50586,0.0999999999999785) ;
#17740 = CIRCLE('',#50587,0.1) ;
#17741 = CIRCLE('',#50589,0.1) ;
#17742 = CIRCLE('',#50593,0.0999999999999979) ;
#17743 = CIRCLE('',#50594,0.100000000000016) ;
#17744 = CIRCLE('',#50595,0.0999999999999979) ;
#17745 = CIRCLE('',#50597,0.0999999999999979) ;
#17746 = CIRCLE('',#50599,0.1) ;
#17747 = CIRCLE('',#50600,0.100000000000016) ;
#17748 = CIRCLE('',#50602,0.0999999999999979) ;
#17749 = CIRCLE('',#50603,0.0999999999999973) ;
#17750 = CIRCLE('',#50604,0.0999999999999973) ;
#17751 = CIRCLE('',#50607,0.100000000000016) ;
#17752 = CIRCLE('',#50608,0.0999999999999979) ;
#17753 = CIRCLE('',#50609,0.0999999999999934) ;
#17754 = CIRCLE('',#50611,0.100000000000016) ;
#17755 = CIRCLE('',#50612,0.0999999999999934) ;
#17756 = CIRCLE('',#50613,0.0999999999999979) ;
#17757 = CIRCLE('',#50617,0.100000000000016) ;
#17758 = CIRCLE('',#50618,0.1) ;
#17759 = CIRCLE('',#50619,0.2) ;
#17760 = CIRCLE('',#50622,0.0999999999999801) ;
#17761 = CIRCLE('',#50624,0.1) ;
#17762 = CIRCLE('',#50625,0.2) ;
#17763 = CIRCLE('',#50627,0.0999999999999979) ;
#17764 = CIRCLE('',#50629,0.0999999999999973) ;
#17765 = CIRCLE('',#50630,0.0999999999999973) ;
#17766 = CIRCLE('',#50632,0.100000000000016) ;
#17767 = CIRCLE('',#50635,0.100000000000016) ;
#17768 = CIRCLE('',#50637,0.0999999999999973) ;
#17769 = CIRCLE('',#50640,0.0999999999999979) ;
#17770 = CIRCLE('',#50641,0.1) ;
#17771 = CIRCLE('',#50642,0.2) ;
#17772 = CIRCLE('',#50644,0.0999999999999979) ;
#17773 = CIRCLE('',#50650,0.0999999999999979) ;
#17774 = CIRCLE('',#50654,0.100000000000007) ;
#17775 = CIRCLE('',#50656,0.1) ;
#17776 = CIRCLE('',#50657,0.2) ;
#17777 = CIRCLE('',#50662,0.100000000000016) ;
#17778 = CIRCLE('',#50663,0.1) ;
#17779 = CIRCLE('',#50665,0.100000000000026) ;
#17780 = CIRCLE('',#50666,0.1) ;
#17781 = CIRCLE('',#50668,0.0999999999999973) ;
#17782 = CIRCLE('',#50670,0.100000000000002) ;
#17783 = CIRCLE('',#50671,0.1) ;
#17784 = CIRCLE('',#50673,0.0999999999999934) ;
#17785 = CIRCLE('',#50675,0.1) ;
#17786 = CIRCLE('',#50677,0.1) ;
#17787 = CIRCLE('',#50680,0.100000000000016) ;
#17788 = CIRCLE('',#50683,0.0999999999999753) ;
#17789 = CIRCLE('',#50686,0.0999999999999979) ;
#17790 = CIRCLE('',#50689,0.099999999999991) ;
#17791 = CIRCLE('',#50692,0.100000000000016) ;
#17792 = CIRCLE('',#50695,0.0999999999999979) ;
#17793 = CIRCLE('',#50696,0.100000000000016) ;
#17794 = CIRCLE('',#50698,0.0999999999999934) ;
#17795 = CIRCLE('',#50699,0.1) ;
#17796 = CIRCLE('',#50701,0.0999999999999934) ;
#17797 = CIRCLE('',#50703,0.0999999999999934) ;
#17798 = CIRCLE('',#50704,0.1) ;
#17799 = CIRCLE('',#50706,0.0999999999999979) ;
#17800 = CIRCLE('',#50708,0.0999999999999934) ;
#17801 = CIRCLE('',#50709,0.1) ;
#17802 = CIRCLE('',#50711,0.0999999999999934) ;
#17803 = CIRCLE('',#50713,0.0999999999999934) ;
#17804 = CIRCLE('',#50714,0.1) ;
#17805 = CIRCLE('',#50716,0.0999999999999979) ;
#17806 = CIRCLE('',#50718,0.0999999999999934) ;
#17807 = CIRCLE('',#50719,0.0999999999999979) ;
#17808 = CIRCLE('',#50721,0.0999999999999934) ;
#17809 = CIRCLE('',#50722,0.1) ;
#17810 = CIRCLE('',#50724,0.0999999999999979) ;
#17811 = CIRCLE('',#50726,0.0999999999999934) ;
#17812 = CIRCLE('',#50727,0.1) ;
#17813 = CIRCLE('',#50729,0.0999999999999934) ;
#17814 = CIRCLE('',#50731,0.0999999999999973) ;
#17815 = CIRCLE('',#50733,0.100000000000004) ;
#17816 = CIRCLE('',#50735,0.100000000000016) ;
#17817 = CIRCLE('',#50738,0.0999999999999979) ;
#17818 = CIRCLE('',#50741,0.100000000000016) ;
#17819 = CIRCLE('',#50744,0.0999999999999979) ;
#17820 = CIRCLE('',#50747,0.100000000000016) ;
#17821 = CIRCLE('',#50748,0.0999999999999979) ;
#17822 = CIRCLE('',#50749,0.0999999999999934) ;
#17823 = CIRCLE('',#50751,0.100000000000051) ;
#17824 = CIRCLE('',#50752,0.100000000000002) ;
#17825 = CIRCLE('',#50753,0.0999999999999979) ;
#17826 = CIRCLE('',#50755,0.100000000000016) ;
#17827 = CIRCLE('',#50757,0.100000000000029) ;
#17828 = CIRCLE('',#50758,0.1) ;
#17829 = CIRCLE('',#50760,0.099999999999991) ;
#17830 = CIRCLE('',#50762,0.100000000000007) ;
#17831 = CIRCLE('',#50763,0.1) ;
#17832 = CIRCLE('',#50765,0.100000000000007) ;
#17833 = CIRCLE('',#50767,0.100000000000022) ;
#17834 = CIRCLE('',#50768,0.1) ;
#17835 = CIRCLE('',#50770,0.099999999999991) ;
#17836 = CIRCLE('',#50772,0.0999999999999801) ;
#17837 = CIRCLE('',#50773,0.1) ;
#17838 = CIRCLE('',#50776,0.1) ;
#17839 = CIRCLE('',#50778,0.0999999999999979) ;
#17840 = CIRCLE('',#50782,0.100000000000016) ;
#17841 = CIRCLE('',#50786,0.1) ;
#17842 = CIRCLE('',#50789,0.0999999999999979) ;
#17843 = CIRCLE('',#50790,0.100000000000016) ;
#17844 = CIRCLE('',#50791,0.1) ;
#17845 = CIRCLE('',#50793,0.0999999999999979) ;
#17846 = CIRCLE('',#50795,0.0999999999999979) ;
#17847 = CIRCLE('',#50796,0.0999999999999979) ;
#17848 = CIRCLE('',#50798,0.0999999999999979) ;
#17849 = CIRCLE('',#50799,0.1) ;
#17850 = CIRCLE('',#50801,0.0999999999999979) ;
#17851 = CIRCLE('',#50803,0.0999999999999979) ;
#17852 = CIRCLE('',#50804,0.1) ;
#17853 = CIRCLE('',#50806,0.0999999999999979) ;
#17854 = CIRCLE('',#50808,0.0999999999999973) ;
#17855 = CIRCLE('',#50810,0.0999999999999979) ;
#17856 = CIRCLE('',#50811,0.100000000000016) ;
#17857 = CIRCLE('',#50813,0.1) ;
#17858 = CIRCLE('',#50814,0.100000000000051) ;
#17859 = CIRCLE('',#50816,0.100000000000004) ;
#17860 = CIRCLE('',#50819,0.0999999999999979) ;
#17861 = CIRCLE('',#50822,0.100000000000016) ;
#17862 = CIRCLE('',#50825,0.0999999999999979) ;
#17863 = CIRCLE('',#50828,0.100000000000016) ;
#17864 = CIRCLE('',#50831,0.0999999999999979) ;
#17865 = CIRCLE('',#50832,0.100000000000016) ;
#17866 = CIRCLE('',#50833,0.1) ;
#17867 = CIRCLE('',#50835,0.0999999999999979) ;
#17868 = CIRCLE('',#50837,0.0999999999999979) ;
#17869 = CIRCLE('',#50838,0.0999999999999979) ;
#17870 = CIRCLE('',#50840,0.0999999999999979) ;
#17871 = CIRCLE('',#50841,0.1) ;
#17872 = CIRCLE('',#50843,0.0999999999999979) ;
#17873 = CIRCLE('',#50845,0.0999999999999979) ;
#17874 = CIRCLE('',#50846,0.1) ;
#17875 = CIRCLE('',#50848,0.0999999999999979) ;
#17876 = CIRCLE('',#50850,0.0999999999999973) ;
#17877 = CIRCLE('',#50852,0.0999999999999979) ;
#17878 = CIRCLE('',#50853,0.100000000000016) ;
#17879 = CIRCLE('',#50855,0.1) ;
#17880 = CIRCLE('',#50856,0.100000000000051) ;
#17881 = CIRCLE('',#50858,0.0999999999999973) ;
#17882 = CIRCLE('',#50861,0.0999999999999979) ;
#17883 = CIRCLE('',#50864,0.100000000000016) ;
#17884 = CIRCLE('',#50867,0.0999999999999979) ;
#17885 = CIRCLE('',#50870,0.100000000000016) ;
#17886 = CIRCLE('',#50873,0.100000000000002) ;
#17887 = CIRCLE('',#50875,0.100000000000002) ;
#17888 = CIRCLE('',#50876,0.100000000000016) ;
#17889 = CIRCLE('',#50878,0.1) ;
#17890 = CIRCLE('',#50879,0.100000000000051) ;
#17891 = CIRCLE('',#50884,0.100000000000016) ;
#17892 = CIRCLE('',#50885,0.1) ;
#17893 = CIRCLE('',#50888,0.100000000000016) ;
#17894 = CIRCLE('',#50890,0.100000000000022) ;
#17895 = CIRCLE('',#50891,0.1) ;
#17896 = CIRCLE('',#50893,0.0999999999999785) ;
#17897 = CIRCLE('',#50895,0.100000000000007) ;
#17898 = CIRCLE('',#50896,0.1) ;
#17899 = CIRCLE('',#50898,0.0999999999999979) ;
#17900 = CIRCLE('',#50900,0.0999999999999973) ;
#17901 = CIRCLE('',#50901,0.1) ;
#17902 = CIRCLE('',#50903,0.099999999999991) ;
#17903 = CIRCLE('',#50905,0.0999999999999801) ;
#17904 = CIRCLE('',#50906,0.1) ;
#17905 = CIRCLE('',#50910,0.0999999999999722) ;
#17906 = CIRCLE('',#50913,0.0999999999999979) ;
#17907 = CIRCLE('',#50916,0.099999999999991) ;
#17908 = CIRCLE('',#50919,0.100000000000016) ;
#17909 = CIRCLE('',#50923,0.100000000000016) ;
#17910 = CIRCLE('',#50924,0.100000000000016) ;
#17911 = CIRCLE('',#50925,0.1) ;
#17912 = CIRCLE('',#50928,0.0999999999999979) ;
#17913 = CIRCLE('',#50929,0.0999999999999934) ;
#17914 = CIRCLE('',#50932,0.100000000000016) ;
#17915 = CIRCLE('',#50933,0.0999999999999979) ;
#17916 = CIRCLE('',#50934,0.0999999999999979) ;
#17917 = CIRCLE('',#50936,0.0999999999999979) ;
#17918 = CIRCLE('',#50937,0.100000000000016) ;
#17919 = CIRCLE('',#50938,0.0999999999999979) ;
#17920 = CIRCLE('',#50943,0.100000000000051) ;
#17921 = CIRCLE('',#50944,0.0999999999999979) ;
#17922 = CIRCLE('',#50945,0.0999999999999979) ;
#17923 = CIRCLE('',#50953,0.0999999999999801) ;
#17924 = CIRCLE('',#50954,0.1) ;
#17925 = CIRCLE('',#50955,0.100000000000051) ;
#17926 = CIRCLE('',#50957,0.100000000000016) ;
#17927 = CIRCLE('',#50958,0.100000000000016) ;
#17928 = CIRCLE('',#50959,0.1) ;
#17929 = CIRCLE('',#50962,0.0999999999999979) ;
#17930 = CIRCLE('',#50963,0.0999999999999979) ;
#17931 = CIRCLE('',#50965,0.100000000000016) ;
#17932 = CIRCLE('',#50966,0.0999999999999979) ;
#17933 = CIRCLE('',#50969,0.0999999999999979) ;
#17934 = CIRCLE('',#50970,0.100000000000016) ;
#17935 = CIRCLE('',#50972,0.0999999999999979) ;
#17936 = CIRCLE('',#50973,0.0999999999999979) ;
#17937 = CIRCLE('',#50976,0.0999999999999979) ;
#17938 = CIRCLE('',#50977,0.100000000000016) ;
#17939 = CIRCLE('',#50978,0.0999999999999979) ;
#17940 = CIRCLE('',#50980,0.100000000000016) ;
#17941 = CIRCLE('',#50981,0.0999999999999979) ;
#17942 = CIRCLE('',#50982,0.0999999999999979) ;
#17943 = CIRCLE('',#50986,0.100000000000016) ;
#17944 = CIRCLE('',#50987,0.0999999999999979) ;
#17945 = CIRCLE('',#50988,0.0999999999999979) ;
#17946 = CIRCLE('',#50990,0.0999999999999979) ;
#17947 = CIRCLE('',#50991,0.100000000000016) ;
#17948 = CIRCLE('',#50992,0.0999999999999979) ;
#17949 = CIRCLE('',#51005,0.0999999999999801) ;
#17950 = CIRCLE('',#51006,0.1) ;
#17951 = CIRCLE('',#51007,0.100000000000051) ;
#17952 = CIRCLE('',#51009,0.100000000000016) ;
#17953 = CIRCLE('',#51010,0.100000000000016) ;
#17954 = CIRCLE('',#51011,0.1) ;
#17955 = CIRCLE('',#51014,0.0999999999999979) ;
#17956 = CIRCLE('',#51015,0.0999999999999979) ;
#17957 = CIRCLE('',#51017,0.0999999999999979) ;
#17958 = CIRCLE('',#51018,0.100000000000016) ;
#17959 = CIRCLE('',#51021,0.100000000000016) ;
#17960 = CIRCLE('',#51022,0.0999999999999979) ;
#17961 = CIRCLE('',#51025,0.0999999999999979) ;
#17962 = CIRCLE('',#51026,0.100000000000016) ;
#17963 = CIRCLE('',#51027,0.0999999999999979) ;
#17964 = CIRCLE('',#51029,0.0999999999999979) ;
#17965 = CIRCLE('',#51030,0.0999999999999979) ;
#17966 = CIRCLE('',#51033,0.100000000000016) ;
#17967 = CIRCLE('',#51034,0.0999999999999979) ;
#17968 = CIRCLE('',#51035,0.0999999999999979) ;
#17969 = CIRCLE('',#51037,0.100000000000016) ;
#17970 = CIRCLE('',#51038,0.0999999999999979) ;
#17971 = CIRCLE('',#51039,0.0999999999999979) ;
#17972 = CIRCLE('',#51043,0.0999999999999979) ;
#17973 = CIRCLE('',#51044,0.100000000000016) ;
#17974 = CIRCLE('',#51045,0.0999999999999979) ;
#17975 = CIRCLE('',#51057,0.100000000000016) ;
#17976 = CIRCLE('',#51058,0.0999999999999979) ;
#17977 = CIRCLE('',#51059,0.0999999999999979) ;
#17978 = CIRCLE('',#51061,0.0999999999999979) ;
#17979 = CIRCLE('',#51062,0.100000000000016) ;
#17980 = CIRCLE('',#51063,0.0999999999999979) ;
#17981 = CIRCLE('',#51065,0.100000000000051) ;
#17982 = CIRCLE('',#51066,0.0999999999999979) ;
#17983 = CIRCLE('',#51068,0.0999999999999979) ;
#17984 = CIRCLE('',#51069,1.2) ;
#17985 = CIRCLE('',#51071,0.0999999999999934) ;
#17986 = CIRCLE('',#51073,0.0999999999999801) ;
#17987 = CIRCLE('',#51074,0.6) ;
#17988 = CIRCLE('',#51076,0.100000000000016) ;
#17989 = CIRCLE('',#51078,0.100000000000002) ;
#17990 = CIRCLE('',#51079,0.6) ;
#17991 = CIRCLE('',#51083,0.100000000000016) ;
#17992 = CIRCLE('',#51085,0.100000000000016) ;
#17993 = CIRCLE('',#51087,0.100000000000002) ;
#17994 = CIRCLE('',#51088,1.2) ;
#17995 = CIRCLE('',#51090,0.100000000000002) ;
#17996 = CIRCLE('',#51092,0.100000000000002) ;
#17997 = CIRCLE('',#51093,0.6) ;
#17998 = CIRCLE('',#51095,0.100000000000002) ;
#17999 = CIRCLE('',#51097,0.100000000000002) ;
#18000 = CIRCLE('',#51098,0.6) ;
#18001 = CIRCLE('',#51100,0.100000000000002) ;
#18002 = CIRCLE('',#51102,0.100000000000002) ;
#18003 = CIRCLE('',#51103,0.600000000000005) ;
#18004 = CIRCLE('',#51105,0.100000000000002) ;
#18005 = CIRCLE('',#51106,2.49999999999996) ;
#18006 = CIRCLE('',#51108,0.0999999999999979) ;
#18007 = CIRCLE('',#51110,0.100000000000002) ;
#18008 = CIRCLE('',#51111,2.49999999999999) ;
#18009 = CIRCLE('',#51113,0.100000000000002) ;
#18010 = CIRCLE('',#51114,0.600000000000023) ;
#18011 = CIRCLE('',#51116,0.100000000000002) ;
#18012 = CIRCLE('',#51118,0.100000000000002) ;
#18013 = CIRCLE('',#51119,0.6) ;
#18014 = CIRCLE('',#51121,0.100000000000002) ;
#18015 = CIRCLE('',#51123,0.100000000000002) ;
#18016 = CIRCLE('',#51124,0.6) ;
#18017 = CIRCLE('',#51126,0.100000000000002) ;
#18018 = CIRCLE('',#51128,0.100000000000002) ;
#18019 = CIRCLE('',#51129,4.) ;
#18020 = CIRCLE('',#51131,0.0999999999999934) ;
#18021 = CIRCLE('',#51133,0.0999999999999979) ;
#18022 = CIRCLE('',#51134,4.) ;
#18023 = CIRCLE('',#51136,0.0999999999999979) ;
#18024 = CIRCLE('',#51138,0.0999999999999979) ;
#18025 = CIRCLE('',#51139,4.) ;
#18026 = CIRCLE('',#51141,0.0999999999999979) ;
#18027 = CIRCLE('',#51143,0.0999999999999979) ;
#18028 = CIRCLE('',#51144,0.6) ;
#18029 = CIRCLE('',#51146,0.100000000000002) ;
#18030 = CIRCLE('',#51148,0.100000000000002) ;
#18031 = CIRCLE('',#51149,0.6) ;
#18032 = CIRCLE('',#51152,0.1000000000003) ;
#18033 = CIRCLE('',#51153,0.1) ;
#18034 = CIRCLE('',#51154,0.2) ;
#18035 = CIRCLE('',#51158,0.0999999999999801) ;
#18036 = CIRCLE('',#51160,0.1) ;
#18037 = CIRCLE('',#51161,0.2) ;
#18038 = CIRCLE('',#51167,0.6) ;
#18039 = CIRCLE('',#51170,0.600000000000005) ;
#18040 = CIRCLE('',#51172,2.49999999999996) ;
#18041 = CIRCLE('',#51175,2.49999999999999) ;
#18042 = CIRCLE('',#51177,0.600000000000023) ;
#18043 = CIRCLE('',#51180,0.6) ;
#18044 = CIRCLE('',#51183,0.6) ;
#18045 = CIRCLE('',#51186,4.) ;
#18046 = CIRCLE('',#51189,4.) ;
#18047 = CIRCLE('',#51192,4.) ;
#18048 = CIRCLE('',#51195,0.6) ;
#18049 = CIRCLE('',#51198,0.6) ;
#18050 = CIRCLE('',#51201,0.099999999999989) ;
#18051 = CIRCLE('',#51203,0.1) ;
#18052 = CIRCLE('',#51204,0.0999999999999979) ;
#18053 = CIRCLE('',#51206,0.100000000000002) ;
#18054 = CIRCLE('',#51207,0.9) ;
#18055 = CIRCLE('',#51208,1.) ;
#18056 = CIRCLE('',#51212,1.) ;
#18057 = CIRCLE('',#51215,0.1) ;
#18058 = CIRCLE('',#51217,0.100000000000016) ;
#18059 = CIRCLE('',#51219,0.100000000000016) ;
#18060 = CIRCLE('',#51220,0.9) ;
#18061 = CIRCLE('',#51225,0.100000000000016) ;
#18062 = CIRCLE('',#51226,0.0999999999999979) ;
#18063 = CIRCLE('',#51227,0.100000000000002) ;
#18064 = CIRCLE('',#51229,0.100000000000016) ;
#18065 = CIRCLE('',#51230,0.0999999999999934) ;
#18066 = CIRCLE('',#51231,0.0999999999999785) ;
#18067 = CIRCLE('',#51234,0.0999999999999847) ;
#18068 = CIRCLE('',#51235,0.0999999999999979) ;
#18069 = CIRCLE('',#51236,0.0999999999999979) ;
#18070 = CIRCLE('',#51239,0.0999999999999979) ;
#18071 = CIRCLE('',#51240,0.100000000000002) ;
#18072 = CIRCLE('',#51241,0.0999999999999847) ;
#18073 = CIRCLE('',#51244,0.099999999999991) ;
#18074 = CIRCLE('',#51245,0.0999999999999934) ;
#18075 = CIRCLE('',#51246,0.100000000000016) ;
#18076 = CIRCLE('',#51249,0.0999999999999979) ;
#18077 = CIRCLE('',#51250,0.100000000000016) ;
#18078 = CIRCLE('',#51251,0.0999999999999979) ;
#18079 = CIRCLE('',#51264,0.0999999999999979) ;
#18080 = CIRCLE('',#51265,0.0999999999999979) ;
#18081 = CIRCLE('',#51266,0.100000000000016) ;
#18082 = CIRCLE('',#51268,0.100000000000016) ;
#18083 = CIRCLE('',#51269,0.0999999999999979) ;
#18084 = CIRCLE('',#51270,0.100000000000002) ;
#18085 = CIRCLE('',#51274,0.100000000000016) ;
#18086 = CIRCLE('',#51275,0.0999999999999979) ;
#18087 = CIRCLE('',#51276,0.100000000000002) ;
#18088 = CIRCLE('',#51278,0.0999999999999979) ;
#18089 = CIRCLE('',#51279,0.0999999999999979) ;
#18090 = CIRCLE('',#51282,0.100000000000016) ;
#18091 = CIRCLE('',#51283,0.0999999999999979) ;
#18092 = CIRCLE('',#51284,0.0999999999999979) ;
#18093 = CIRCLE('',#51287,0.100000000000016) ;
#18094 = CIRCLE('',#51288,0.100000000000002) ;
#18095 = CIRCLE('',#51291,0.100000000000002) ;
#18096 = CIRCLE('',#51292,0.100000000000016) ;
#18097 = CIRCLE('',#51294,0.0999999999999979) ;
#18098 = CIRCLE('',#51295,0.0999999999999979) ;
#18099 = CIRCLE('',#51306,0.1) ;
#18100 = CIRCLE('',#51307,0.100000000000016) ;
#18101 = CIRCLE('',#51309,0.100000000000016) ;
#18102 = CIRCLE('',#51310,1.) ;
#18103 = CIRCLE('',#51311,0.9) ;
#18104 = CIRCLE('',#51315,0.1) ;
#18105 = CIRCLE('',#51316,0.0999999999999979) ;
#18106 = CIRCLE('',#51318,0.100000000000002) ;
#18107 = CIRCLE('',#51319,0.900000000000001) ;
#18108 = CIRCLE('',#51320,1.) ;
#18109 = CIRCLE('',#51325,0.0999999999999979) ;
#18110 = CIRCLE('',#51326,0.0999999999999785) ;
#18111 = CIRCLE('',#51329,0.0999999999999979) ;
#18112 = CIRCLE('',#51330,0.0999999999999979) ;
#18113 = CIRCLE('',#51333,0.0999999999999934) ;
#18114 = CIRCLE('',#51334,0.099999999999991) ;
#18115 = CIRCLE('',#51337,0.0999999999999979) ;
#18116 = CIRCLE('',#51338,0.100000000000016) ;
#18117 = CIRCLE('',#51342,0.1) ;
#18118 = CIRCLE('',#51343,0.0999999999999979) ;
#18119 = CIRCLE('',#51345,0.100000000000007) ;
#18120 = CIRCLE('',#51346,0.9) ;
#18121 = CIRCLE('',#51347,1.) ;
#18122 = CIRCLE('',#51351,1.) ;
#18123 = CIRCLE('',#51354,0.1) ;
#18124 = CIRCLE('',#51356,0.100000000000016) ;
#18125 = CIRCLE('',#51358,0.100000000000016) ;
#18126 = CIRCLE('',#51359,0.9) ;
#18127 = CIRCLE('',#51364,0.0999999999999847) ;
#18128 = CIRCLE('',#51365,0.0999999999999979) ;
#18129 = CIRCLE('',#51366,0.100000000000016) ;
#18130 = CIRCLE('',#51368,0.0999999999999979) ;
#18131 = CIRCLE('',#51369,0.100000000000002) ;
#18132 = CIRCLE('',#51370,0.099999999999991) ;
#18133 = CIRCLE('',#51372,0.0999999999999847) ;
#18134 = CIRCLE('',#51373,0.0999999999999934) ;
#18135 = CIRCLE('',#51374,0.0999999999999979) ;
#18136 = CIRCLE('',#51376,0.100000000000016) ;
#18137 = CIRCLE('',#51377,0.0999999999999934) ;
#18138 = CIRCLE('',#51378,0.0999999999999847) ;
#18139 = CIRCLE('',#51400,0.0999999999999979) ;
#18140 = CIRCLE('',#51401,0.100000000000016) ;
#18141 = CIRCLE('',#51402,0.0999999999999979) ;
#18142 = CIRCLE('',#51404,0.0999999999999979) ;
#18143 = CIRCLE('',#51405,0.0999999999999934) ;
#18144 = CIRCLE('',#51406,0.100000000000016) ;
#18145 = CIRCLE('',#51408,0.100000000000016) ;
#18146 = CIRCLE('',#51409,0.0999999999999979) ;
#18147 = CIRCLE('',#51410,0.0999999999999979) ;
#18148 = CIRCLE('',#51412,0.0999999999999979) ;
#18149 = CIRCLE('',#51413,0.0999999999999934) ;
#18150 = CIRCLE('',#51414,0.100000000000016) ;
#18151 = CIRCLE('',#51416,0.0999999999999979) ;
#18152 = CIRCLE('',#51417,0.100000000000016) ;
#18153 = CIRCLE('',#51418,0.0999999999999934) ;
#18154 = CIRCLE('',#51420,0.100000000000016) ;
#18155 = CIRCLE('',#51421,0.0999999999999934) ;
#18156 = CIRCLE('',#51422,0.0999999999999979) ;
#18157 = CIRCLE('',#51424,0.0999999999999979) ;
#18158 = CIRCLE('',#51425,0.100000000000016) ;
#18159 = CIRCLE('',#51426,0.0999999999999979) ;
#18160 = CIRCLE('',#51429,0.0999999999999934) ;
#18161 = CIRCLE('',#51430,0.0999999999999979) ;
#18162 = CIRCLE('',#51431,0.100000000000016) ;
#18163 = CIRCLE('',#51448,0.1) ;
#18164 = CIRCLE('',#51449,2.5) ;
#18165 = CIRCLE('',#51451,2.5) ;
#18166 = CIRCLE('',#51452,2.5) ;
#18167 = CIRCLE('',#51454,0.1) ;
#18168 = CIRCLE('',#51456,0.1) ;
#18169 = CIRCLE('',#51457,0.100000000000016) ;
#18170 = CIRCLE('',#51459,0.100000000000016) ;
#18171 = CIRCLE('',#51460,1.) ;
#18172 = CIRCLE('',#51461,0.900000000000001) ;
#18173 = CIRCLE('',#51466,0.1) ;
#18174 = CIRCLE('',#51469,0.0999999999999979) ;
#18175 = CIRCLE('',#51471,0.0999999999999934) ;
#18176 = CIRCLE('',#51472,0.9) ;
#18177 = CIRCLE('',#51473,1.) ;
#18178 = CIRCLE('',#51478,0.100000000000002) ;
#18179 = CIRCLE('',#51479,0.099999999999991) ;
#18180 = CIRCLE('',#51483,0.0999999999999979) ;
#18181 = CIRCLE('',#51484,0.0999999999999979) ;
#18182 = CIRCLE('',#51487,0.0999999999999979) ;
#18183 = CIRCLE('',#51488,0.0999999999999847) ;
#18184 = CIRCLE('',#51491,0.0999999999999979) ;
#18185 = CIRCLE('',#51492,0.100000000000016) ;
#18186 = CIRCLE('',#51495,0.100000000000002) ;
#18187 = CIRCLE('',#51496,0.0999999999999979) ;
#18188 = CIRCLE('',#51501,0.1) ;
#18189 = CIRCLE('',#51502,2.5) ;
#18190 = CIRCLE('',#51503,2.5) ;
#18191 = CIRCLE('',#51506,0.1) ;
#18192 = CIRCLE('',#51507,2.) ;
#18193 = CIRCLE('',#51508,2.) ;
#18194 = CIRCLE('',#51511,0.0999999999999979) ;
#18195 = CIRCLE('',#51513,0.0999999999999847) ;
#18196 = CIRCLE('',#51514,0.6) ;
#18197 = CIRCLE('',#51516,0.0999999999999847) ;
#18198 = CIRCLE('',#51518,0.100000000000016) ;
#18199 = CIRCLE('',#51520,0.0999999999999979) ;
#18200 = CIRCLE('',#51522,0.0999999999999938) ;
#18201 = CIRCLE('',#51524,0.0999999999999979) ;
#18202 = CIRCLE('',#51526,0.099999999999989) ;
#18203 = CIRCLE('',#51528,0.100000000000029) ;
#18204 = CIRCLE('',#51530,0.0999999999999979) ;
#18205 = CIRCLE('',#51532,0.0999999999999979) ;
#18206 = CIRCLE('',#51534,0.0999999999999847) ;
#18207 = CIRCLE('',#51536,0.0999999999999847) ;
#18208 = CIRCLE('',#51538,0.099999999999989) ;
#18209 = CIRCLE('',#51540,0.0999999999999979) ;
#18210 = CIRCLE('',#51542,0.100000000000006) ;
#18211 = CIRCLE('',#51544,0.100000000000006) ;
#18212 = CIRCLE('',#51546,0.100000000000022) ;
#18213 = CIRCLE('',#51548,0.1) ;
#18214 = CIRCLE('',#51550,0.100000000000007) ;
#18215 = CIRCLE('',#51552,0.0999999999999979) ;
#18216 = CIRCLE('',#51554,0.0999999999999801) ;
#18217 = CIRCLE('',#51556,0.0999999999999801) ;
#18218 = CIRCLE('',#51560,0.100000000000002) ;
#18219 = CIRCLE('',#51561,0.6) ;
#18220 = CIRCLE('',#51563,0.0999999999999934) ;
#18221 = CIRCLE('',#51565,0.0999999999999979) ;
#18222 = CIRCLE('',#51566,0.6) ;
#18223 = CIRCLE('',#51569,0.2) ;
#18224 = CIRCLE('',#51570,2.2) ;
#18225 = CIRCLE('',#51572,2.6) ;
#18226 = CIRCLE('',#51574,2.8) ;
#18227 = CIRCLE('',#51575,0.2) ;
#18228 = CIRCLE('',#51576,2.8) ;
#18229 = CIRCLE('',#51578,2.8) ;
#18230 = CIRCLE('',#51580,0.2) ;
#18231 = CIRCLE('',#51581,2.80637980653322) ;
#18232 = CIRCLE('',#51582,2.80637980653322) ;
#18233 = CIRCLE('',#51584,2.8) ;
#18234 = CIRCLE('',#51585,0.2) ;
#18235 = CIRCLE('',#51586,2.80637980653322) ;
#18236 = CIRCLE('',#51587,2.80637980653322) ;
#18237 = CIRCLE('',#51589,2.8) ;
#18238 = CIRCLE('',#51590,2.8) ;
#18239 = CIRCLE('',#51592,0.2) ;
#18240 = CIRCLE('',#51593,2.6) ;
#18241 = CIRCLE('',#51595,2.2) ;
#18242 = CIRCLE('',#51597,2.) ;
#18243 = CIRCLE('',#51598,0.2) ;
#18244 = CIRCLE('',#51600,2.) ;
#18245 = CIRCLE('',#51602,2.79999999999999) ;
#18246 = CIRCLE('',#51603,0.2) ;
#18247 = CIRCLE('',#51604,2.80637980653321) ;
#18248 = CIRCLE('',#51605,2.80637980653321) ;
#18249 = CIRCLE('',#51607,2.79999999999999) ;
#18250 = CIRCLE('',#51608,2.79999999999999) ;
#18251 = CIRCLE('',#51610,0.2) ;
#18252 = CIRCLE('',#51611,2.2) ;
#18253 = CIRCLE('',#51613,2.59999999999999) ;
#18254 = CIRCLE('',#51615,0.2) ;
#18255 = CIRCLE('',#51617,1.3) ;
#18256 = CIRCLE('',#51619,1.3) ;
#18257 = CIRCLE('',#51621,1.3) ;
#18258 = CIRCLE('',#51633,0.499999999999998) ;
#18259 = CIRCLE('',#51638,0.500000000000007) ;
#18260 = CIRCLE('',#51643,0.499999999999998) ;
#18261 = CIRCLE('',#51646,0.500000000000007) ;
#18262 = CIRCLE('',#51648,1.2) ;
#18263 = CIRCLE('',#51649,1.20000000000002) ;
#18264 = CIRCLE('',#51652,1.20000000000002) ;
#18265 = CIRCLE('',#51653,1.19999999999999) ;
#18266 = CIRCLE('',#51658,1.2) ;
#18267 = CIRCLE('',#51659,1.20000000000002) ;
#18268 = CIRCLE('',#51662,1.20000000000002) ;
#18269 = CIRCLE('',#51663,1.2) ;
#18270 = CIRCLE('',#51668,0.499999999999994) ;
#18271 = CIRCLE('',#51670,0.499999999999998) ;
#18272 = CIRCLE('',#51678,0.499999999999994) ;
#18273 = CIRCLE('',#51680,0.499999999999989) ;
#18274 = CIRCLE('',#51718,0.0999999999999979) ;
#18275 = CIRCLE('',#51719,0.100000000000016) ;
#18276 = CIRCLE('',#51720,0.0999999999999979) ;
#18277 = CIRCLE('',#51724,0.1) ;
#18278 = CIRCLE('',#51736,0.100000000000016) ;
#18279 = CIRCLE('',#51738,0.100000000000007) ;
#18280 = CIRCLE('',#51739,0.100000000000016) ;
#18281 = CIRCLE('',#51741,0.0999999999999979) ;
#18282 = CIRCLE('',#51743,0.0999999999999973) ;
#18283 = CIRCLE('',#51745,0.0999999999999973) ;
#18284 = CIRCLE('',#51747,3.1) ;
#18285 = CIRCLE('',#51748,0.1) ;
#18286 = CIRCLE('',#51749,0.4) ;
#18287 = CIRCLE('',#51750,0.4) ;
#18288 = CIRCLE('',#51751,0.4) ;
#18289 = CIRCLE('',#51752,2.4) ;
#18290 = CIRCLE('',#51753,1.55266329058736) ;
#18291 = CIRCLE('',#51754,1.55266329058736) ;
#18292 = CIRCLE('',#51756,0.0999999999999979) ;
#18293 = CIRCLE('',#51759,0.100000000000007) ;
#18294 = CIRCLE('',#51761,2.4) ;
#18295 = CIRCLE('',#51762,0.4) ;
#18296 = CIRCLE('',#51763,0.4) ;
#18297 = CIRCLE('',#51764,0.4) ;
#18298 = CIRCLE('',#51765,0.1) ;
#18299 = CIRCLE('',#51766,3.1) ;
#18300 = CIRCLE('',#51767,1.45266329058736) ;
#18301 = CIRCLE('',#51768,1.45266329058736) ;
#18302 = CIRCLE('',#51770,0.1) ;
#18303 = CIRCLE('',#51773,0.1) ;
#18304 = CIRCLE('',#51777,0.0999999999999979) ;
#18305 = CIRCLE('',#51778,0.0999999999999979) ;
#18306 = CIRCLE('',#51779,0.5) ;
#18307 = CIRCLE('',#51781,0.0999999999999979) ;
#18308 = CIRCLE('',#51782,0.5) ;
#18309 = CIRCLE('',#51783,0.0999999999999984) ;
#18310 = CIRCLE('',#51787,0.0999999999999979) ;
#18311 = CIRCLE('',#51789,0.0999999999999979) ;
#18312 = CIRCLE('',#51791,0.0999999999999984) ;
#18313 = CIRCLE('',#51792,0.0999999999999979) ;
#18314 = CIRCLE('',#51793,0.5) ;
#18315 = CIRCLE('',#51795,0.5) ;
#18316 = CIRCLE('',#51796,0.0999999999999801) ;
#18317 = CIRCLE('',#51801,0.0999999999999984) ;
#18318 = CIRCLE('',#51802,0.0999999999999979) ;
#18319 = CIRCLE('',#51803,0.5) ;
#18320 = CIRCLE('',#51805,0.0999999999999979) ;
#18321 = CIRCLE('',#51806,0.5) ;
#18322 = CIRCLE('',#51809,0.0999999999999979) ;
#18323 = CIRCLE('',#51812,0.100000000000012) ;
#18324 = CIRCLE('',#51813,0.199999999999978) ;
#18325 = CIRCLE('',#51819,0.199999999999996) ;
#18326 = CIRCLE('',#51828,0.0999999999999979) ;
#18327 = CIRCLE('',#51829,0.0999999999999801) ;
#18328 = CIRCLE('',#51830,0.2) ;
#18329 = CIRCLE('',#51831,0.2) ;
#18330 = CIRCLE('',#51836,0.0999999999999979) ;
#18331 = CIRCLE('',#51837,0.0999999999999979) ;
#18332 = CIRCLE('',#51839,0.0999999999999979) ;
#18333 = CIRCLE('',#51840,1.45266329058736) ;
#18334 = CIRCLE('',#51842,0.0999999999999979) ;
#18335 = CIRCLE('',#51844,1.45266329058736) ;
#18336 = CIRCLE('',#51848,3.) ;
#18337 = CIRCLE('',#51851,3.) ;
#18338 = CIRCLE('',#51868,0.300000000000002) ;
#18339 = CIRCLE('',#51869,1.19999999999999) ;
#18340 = CIRCLE('',#51870,0.899999999999993) ;
#18341 = CIRCLE('',#51872,0.300000000000002) ;
#18342 = CIRCLE('',#51874,1.19999999999999) ;
#18343 = CIRCLE('',#51875,0.899999999999993) ;
#18344 = CIRCLE('',#51878,0.300000000000002) ;
#18345 = CIRCLE('',#51879,1.19999999999999) ;
#18346 = CIRCLE('',#51880,0.899999999999993) ;
#18347 = CIRCLE('',#51882,0.300000000000002) ;
#18348 = CIRCLE('',#51884,1.19999999999999) ;
#18349 = CIRCLE('',#51885,0.899999999999993) ;
#18350 = CIRCLE('',#51888,0.300000000000002) ;
#18351 = CIRCLE('',#51889,1.19999999999999) ;
#18352 = CIRCLE('',#51890,0.899999999999993) ;
#18353 = CIRCLE('',#51892,0.300000000000002) ;
#18354 = CIRCLE('',#51894,1.19999999999999) ;
#18355 = CIRCLE('',#51895,0.899999999999993) ;
#18356 = CIRCLE('',#51898,0.300000000000002) ;
#18357 = CIRCLE('',#51899,1.19999999999999) ;
#18358 = CIRCLE('',#51900,0.899999999999993) ;
#18359 = CIRCLE('',#51902,0.300000000000002) ;
#18360 = CIRCLE('',#51904,1.19999999999999) ;
#18361 = CIRCLE('',#51905,0.899999999999993) ;
#18362 = CIRCLE('',#51908,0.300000000000002) ;
#18363 = CIRCLE('',#51909,1.19999999999999) ;
#18364 = CIRCLE('',#51910,0.899999999999993) ;
#18365 = CIRCLE('',#51912,0.300000000000002) ;
#18366 = CIRCLE('',#51914,1.19999999999999) ;
#18367 = CIRCLE('',#51915,0.899999999999993) ;
#18368 = CIRCLE('',#51918,0.300000000000002) ;
#18369 = CIRCLE('',#51919,1.19999999999999) ;
#18370 = CIRCLE('',#51920,0.899999999999993) ;
#18371 = CIRCLE('',#51922,0.300000000000002) ;
#18372 = CIRCLE('',#51924,1.19999999999999) ;
#18373 = CIRCLE('',#51925,0.899999999999993) ;
#18374 = CIRCLE('',#51928,0.300000000000002) ;
#18375 = CIRCLE('',#51929,1.19999999999999) ;
#18376 = CIRCLE('',#51930,0.899999999999993) ;
#18377 = CIRCLE('',#51932,0.300000000000002) ;
#18378 = CIRCLE('',#51934,1.19999999999999) ;
#18379 = CIRCLE('',#51935,0.899999999999993) ;
#18380 = CIRCLE('',#51938,0.300000000000002) ;
#18381 = CIRCLE('',#51939,1.19999999999999) ;
#18382 = CIRCLE('',#51940,0.899999999999993) ;
#18383 = CIRCLE('',#51942,0.300000000000002) ;
#18384 = CIRCLE('',#51944,1.19999999999999) ;
#18385 = CIRCLE('',#51945,0.899999999999993) ;
#18386 = CIRCLE('',#51983,2.) ;
#18387 = CIRCLE('',#51984,0.45) ;
#18388 = CIRCLE('',#51985,2.4) ;
#18389 = CIRCLE('',#51986,2.4) ;
#18390 = CIRCLE('',#51987,2.) ;
#18391 = CIRCLE('',#51989,2.) ;
#18392 = CIRCLE('',#51991,2.4) ;
#18393 = CIRCLE('',#51995,2.49999999999999) ;
#18394 = CIRCLE('',#51996,0.45) ;
#18395 = CIRCLE('',#51997,2.69999999999999) ;
#18396 = CIRCLE('',#51998,2.69999999999999) ;
#18397 = CIRCLE('',#51999,2.49999999999999) ;
#18398 = CIRCLE('',#52001,2.49999999999999) ;
#18399 = CIRCLE('',#52003,2.69999999999999) ;
#18400 = CIRCLE('',#52007,2.5) ;
#18401 = CIRCLE('',#52008,0.45) ;
#18402 = CIRCLE('',#52009,2.95) ;
#18403 = CIRCLE('',#52011,2.5) ;
#18404 = CIRCLE('',#52013,3.) ;
#18405 = CIRCLE('',#52015,3.) ;
#18406 = CIRCLE('',#52019,0.120000000000005) ;
#18407 = CIRCLE('',#52020,0.120000000000005) ;
#18408 = CIRCLE('',#52021,0.12) ;
#18409 = CIRCLE('',#52022,0.240000000000009) ;
#18410 = CIRCLE('',#52023,0.119999999999969) ;
#18411 = CIRCLE('',#52028,0.120000000000005) ;
#18412 = CIRCLE('',#52029,0.120000000000005) ;
#18413 = CIRCLE('',#52030,0.12) ;
#18414 = CIRCLE('',#52031,0.120000000000022) ;
#18415 = CIRCLE('',#52038,0.120000000000005) ;
#18416 = CIRCLE('',#52039,0.120000000000005) ;
#18417 = CIRCLE('',#52040,0.12) ;
#18418 = CIRCLE('',#52041,0.240000000000009) ;
#18419 = CIRCLE('',#52042,0.119999999999987) ;
#18420 = CIRCLE('',#52048,0.120000000000005) ;
#18421 = CIRCLE('',#52049,0.120000000000005) ;
#18422 = CIRCLE('',#52050,0.12) ;
#18423 = CIRCLE('',#52051,0.240000000000009) ;
#18424 = CIRCLE('',#52052,0.119999999999969) ;
#18425 = CIRCLE('',#52057,0.120000000000005) ;
#18426 = CIRCLE('',#52058,0.120000000000005) ;
#18427 = CIRCLE('',#52059,0.12) ;
#18428 = CIRCLE('',#52060,0.120000000000005) ;
#18429 = CIRCLE('',#52068,0.120000000000005) ;
#18430 = CIRCLE('',#52069,0.120000000000005) ;
#18431 = CIRCLE('',#52070,0.12) ;
#18432 = CIRCLE('',#52071,0.240000000000009) ;
#18433 = CIRCLE('',#52072,0.119999999999987) ;
#18434 = CIRCLE('',#52077,0.120000000000005) ;
#18435 = CIRCLE('',#52078,0.120000000000005) ;
#18436 = CIRCLE('',#52079,0.12) ;
#18437 = CIRCLE('',#52080,0.240000000000009) ;
#18438 = CIRCLE('',#52081,0.119999999999987) ;
#18439 = CIRCLE('',#52087,0.120000000000005) ;
#18440 = CIRCLE('',#52088,0.120000000000005) ;
#18441 = CIRCLE('',#52089,0.12) ;
#18442 = CIRCLE('',#52090,0.120000000000005) ;
#18443 = CIRCLE('',#52097,0.120000000000005) ;
#18444 = CIRCLE('',#52098,0.120000000000005) ;
#18445 = CIRCLE('',#52099,0.12) ;
#18446 = CIRCLE('',#52100,0.240000000000009) ;
#18447 = CIRCLE('',#52101,0.119999999999969) ;
#18448 = CIRCLE('',#52107,0.120000000000005) ;
#18449 = CIRCLE('',#52108,0.119999999999996) ;
#18450 = CIRCLE('',#52109,0.12) ;
#18451 = CIRCLE('',#52110,0.239999999999991) ;
#18452 = CIRCLE('',#52111,0.119999999999987) ;
#18453 = CIRCLE('',#52116,0.120000000000005) ;
#18454 = CIRCLE('',#52117,0.120000000000005) ;
#18455 = CIRCLE('',#52118,0.12) ;
#18456 = CIRCLE('',#52119,0.120000000000022) ;
#18457 = CIRCLE('',#52127,0.119999999999996) ;
#18458 = CIRCLE('',#52128,0.120000000000005) ;
#18459 = CIRCLE('',#52129,0.12) ;
#18460 = CIRCLE('',#52130,0.240000000000009) ;
#18461 = CIRCLE('',#52131,0.119999999999969) ;
#18462 = CIRCLE('',#52154,1.74999999999999) ;
#18463 = CIRCLE('',#52169,0.25) ;
#18464 = CIRCLE('',#52170,1.99999999999999) ;
#18465 = CIRCLE('',#52172,1.99999999999999) ;
#18466 = CIRCLE('',#52173,1.99999999999999) ;
#18467 = CIRCLE('',#52175,1.74999999999999) ;
#18468 = CIRCLE('',#52176,0.25) ;
#18469 = CIRCLE('',#52181,0.100000000000016) ;
#18470 = CIRCLE('',#52182,0.0999999999999979) ;
#18471 = CIRCLE('',#52183,0.0999999999999979) ;
#18472 = CIRCLE('',#52185,0.0999999999999979) ;
#18473 = CIRCLE('',#52186,0.100000000000016) ;
#18474 = CIRCLE('',#52187,0.0999999999999979) ;
#18475 = CIRCLE('',#52189,0.0999999999999979) ;
#18476 = CIRCLE('',#52190,0.100000000000016) ;
#18477 = CIRCLE('',#52191,0.0999999999999979) ;
#18478 = CIRCLE('',#52196,0.100000000000016) ;
#18479 = CIRCLE('',#52197,0.0999999999999979) ;
#18480 = CIRCLE('',#52198,0.0999999999999979) ;
#18481 = CIRCLE('',#52200,0.0999999999999979) ;
#18482 = CIRCLE('',#52201,0.0999999999999979) ;
#18483 = CIRCLE('',#52202,0.100000000000051) ;
#18484 = CIRCLE('',#52206,0.1) ;
#18485 = CIRCLE('',#52221,1.9) ;
#18486 = CIRCLE('',#52222,0.1) ;
#18487 = CIRCLE('',#52223,2.) ;
#18488 = CIRCLE('',#52224,2.) ;
#18489 = CIRCLE('',#52226,2.) ;
#18490 = CIRCLE('',#52227,2.) ;
#18491 = CIRCLE('',#52260,1.8) ;
#18492 = CIRCLE('',#52290,0.2) ;
#18493 = CIRCLE('',#52327,2.39999999999999) ;
#18494 = CIRCLE('',#52328,0.1) ;
#18495 = CIRCLE('',#52329,2.49999999999999) ;
#18496 = CIRCLE('',#52330,2.49999999999999) ;
#18497 = CIRCLE('',#52332,2.49999999999999) ;
#18498 = CIRCLE('',#52333,2.49999999999999) ;
#18499 = CIRCLE('',#52363,2.29999999999999) ;
#18500 = CIRCLE('',#52365,0.2) ;
#18501 = CIRCLE('',#52402,2.4) ;
#18502 = CIRCLE('',#52403,0.1) ;
#18503 = CIRCLE('',#52404,2.5) ;
#18504 = CIRCLE('',#52405,2.5) ;
#18505 = CIRCLE('',#52407,2.5) ;
#18506 = CIRCLE('',#52408,2.5) ;
#18507 = CIRCLE('',#52438,2.3) ;
#18508 = CIRCLE('',#52440,0.2) ;
#18509 = CIRCLE('',#52446,0.0499999999999901) ;
#18510 = CIRCLE('',#52447,0.0499999999999989) ;
#18511 = CIRCLE('',#52448,0.0499999999999989) ;
#18512 = CIRCLE('',#52450,0.0499999999999989) ;
#18513 = CIRCLE('',#52451,0.0499999999999989) ;
#18514 = CIRCLE('',#52452,0.0500000000000149) ;
#18515 = CIRCLE('',#52455,0.0499999999999989) ;
#18516 = CIRCLE('',#52456,0.0499999999999901) ;
#18517 = CIRCLE('',#52457,0.0499999999999945) ;
#18518 = CIRCLE('',#52460,0.0499999999999989) ;
#18519 = CIRCLE('',#52461,0.0500000000000034) ;
#18520 = CIRCLE('',#52462,0.0999999999999979) ;
#18521 = CIRCLE('',#52463,0.0499999999999901) ;
#18522 = CIRCLE('',#52465,0.0499999999999989) ;
#18523 = CIRCLE('',#52467,0.0499999999999989) ;
#18524 = CIRCLE('',#52471,0.0500000000000005) ;
#18525 = CIRCLE('',#52472,0.0499999999999945) ;
#18526 = CIRCLE('',#52473,0.0499999999999989) ;
#18527 = CIRCLE('',#52477,0.0999999999999801) ;
#18528 = CIRCLE('',#52478,0.0499999999999989) ;
#18529 = CIRCLE('',#52479,0.0499999999999901) ;
#18530 = CIRCLE('',#52480,0.0500000000000034) ;
#18531 = CIRCLE('',#52482,0.0500000000000077) ;
#18532 = CIRCLE('',#52484,0.0500000000000034) ;
#18533 = CIRCLE('',#52497,0.0499999999999989) ;
#18534 = CIRCLE('',#52498,0.0499999999999989) ;
#18535 = CIRCLE('',#52499,0.0499999999999901) ;
#18536 = CIRCLE('',#52501,0.0499999999999901) ;
#18537 = CIRCLE('',#52502,0.0499999999999989) ;
#18538 = CIRCLE('',#52503,0.0499999999999989) ;
#18539 = CIRCLE('',#52508,0.0499999999999989) ;
#18540 = CIRCLE('',#52509,0.0499999999999989) ;
#18541 = CIRCLE('',#52510,0.0500000000000243) ;
#18542 = CIRCLE('',#52513,0.05) ;
#18543 = CIRCLE('',#52517,0.05) ;
#18544 = CIRCLE('',#52519,0.05) ;
#18545 = CIRCLE('',#52527,0.499999999999998) ;
#18546 = CIRCLE('',#52528,0.500000000000009) ;
#18547 = CIRCLE('',#52529,0.500000000000009) ;
#18548 = CIRCLE('',#52530,0.499999999999998) ;
#18549 = CIRCLE('',#52531,0.499999999999998) ;
#18550 = CIRCLE('',#52545,6.15) ;
#18551 = CIRCLE('',#52546,1.1) ;
#18552 = CIRCLE('',#52547,0.500000000000129) ;
#18553 = CIRCLE('',#52548,0.700000000000129) ;
#18554 = CIRCLE('',#52549,0.9) ;
#18555 = CIRCLE('',#52550,4.09999999999997) ;
#18556 = CIRCLE('',#52551,1.40000000000004) ;
#18557 = CIRCLE('',#52552,3.79999999999997) ;
#18558 = CIRCLE('',#52553,3.79999999999982) ;
#18559 = CIRCLE('',#52554,1.9) ;
#18560 = CIRCLE('',#52558,0.240000000000009) ;
#18561 = CIRCLE('',#52559,0.24) ;
#18562 = CIRCLE('',#52560,0.48) ;
#18563 = CIRCLE('',#52562,0.240000000000009) ;
#18564 = CIRCLE('',#52563,0.239999999999991) ;
#18565 = CIRCLE('',#52564,0.16) ;
#18566 = CIRCLE('',#52565,0.4) ;
#18567 = CIRCLE('',#52567,0.239999999999991) ;
#18568 = CIRCLE('',#52568,1.53630687649659) ;
#18569 = CIRCLE('',#52571,0.4) ;
#18570 = CIRCLE('',#52574,0.24) ;
#18571 = CIRCLE('',#52577,0.239999999999991) ;
#18572 = CIRCLE('',#52578,0.239999999999974) ;
#18573 = CIRCLE('',#52579,0.16) ;
#18574 = CIRCLE('',#52580,0.4) ;
#18575 = CIRCLE('',#52582,0.240000000000009) ;
#18576 = CIRCLE('',#52584,0.24) ;
#18577 = CIRCLE('',#52585,0.48) ;
#18578 = CIRCLE('',#52588,0.4) ;
#18579 = CIRCLE('',#52597,0.24) ;
#18580 = CIRCLE('',#52603,0.24) ;
#18581 = CIRCLE('',#52604,0.239999999999998) ;
#18582 = CIRCLE('',#52608,0.299999999999998) ;
#18583 = CIRCLE('',#52610,0.45) ;
#18584 = CIRCLE('',#52612,0.0999999999999979) ;
#18585 = CIRCLE('',#52613,0.240000000000002) ;
#18586 = CIRCLE('',#52619,0.24) ;
#18587 = CIRCLE('',#52620,0.24) ;
#18588 = CIRCLE('',#52624,0.300000000000031) ;
#18589 = CIRCLE('',#52625,0.299999999999996) ;
#18590 = CIRCLE('',#52626,1.4) ;
#18591 = CIRCLE('',#52630,0.0999999999999446) ;
#18592 = CIRCLE('',#52633,0.100000000000002) ;
#18593 = CIRCLE('',#52635,0.24) ;
#18594 = CIRCLE('',#52637,0.24) ;
#18595 = CIRCLE('',#52643,0.1) ;
#18596 = CIRCLE('',#52645,0.0999999999999979) ;
#18597 = CIRCLE('',#52649,0.199999999999984) ;
#18598 = CIRCLE('',#52651,0.200000000000005) ;
#18599 = CIRCLE('',#52657,0.199999999999996) ;
#18600 = CIRCLE('',#52660,0.0999999999999934) ;
#18601 = CIRCLE('',#52661,0.24) ;
#18602 = CIRCLE('',#52662,0.0999999999999894) ;
#18603 = CIRCLE('',#52663,0.14) ;
#18604 = CIRCLE('',#52666,0.0999999999999979) ;
#18605 = CIRCLE('',#52670,0.1) ;
#18606 = CIRCLE('',#52671,0.14) ;
#18607 = CIRCLE('',#52672,0.0999999999999979) ;
#18608 = CIRCLE('',#52673,0.24) ;
#18609 = CIRCLE('',#52676,0.1) ;
#18610 = CIRCLE('',#52678,0.2) ;
#18611 = CIRCLE('',#52679,0.099999999999838) ;
#18612 = CIRCLE('',#52680,0.3) ;
#18613 = CIRCLE('',#52682,0.299999999999998) ;
#18614 = CIRCLE('',#52683,0.75) ;
#18615 = CIRCLE('',#52686,0.3) ;
#18616 = CIRCLE('',#52687,0.1) ;
#18617 = CIRCLE('',#52688,0.2) ;
#18618 = CIRCLE('',#52690,0.300000000000002) ;
#18619 = CIRCLE('',#52692,0.300000000000011) ;
#18620 = CIRCLE('',#52693,0.75) ;
#18621 = CIRCLE('',#52694,0.45) ;
#18622 = CIRCLE('',#52698,0.0999999999999801) ;
#18623 = CIRCLE('',#52701,0.800000000000003) ;
#18624 = CIRCLE('',#52704,0.100000000000016) ;
#18625 = CIRCLE('',#52705,0.0999999999999979) ;
#18626 = CIRCLE('',#52706,0.0999999999999979) ;
#18627 = CIRCLE('',#52710,3.99999999999997) ;
#18628 = CIRCLE('',#52711,0.0999999999999801) ;
#18629 = CIRCLE('',#52712,4.09999999999997) ;
#18630 = CIRCLE('',#52714,0.100000000000016) ;
#18631 = CIRCLE('',#52716,0.0999999999999977) ;
#18632 = CIRCLE('',#52717,0.9) ;
#18633 = CIRCLE('',#52718,1.) ;
#18634 = CIRCLE('',#52720,0.0999999999999973) ;
#18635 = CIRCLE('',#52721,0.700000000000129) ;
#18636 = CIRCLE('',#52722,0.600000000000129) ;
#18637 = CIRCLE('',#52724,0.0999999999999847) ;
#18638 = CIRCLE('',#52726,0.0999999999999979) ;
#18639 = CIRCLE('',#52727,0.500000000000129) ;
#18640 = CIRCLE('',#52728,0.600000000000129) ;
#18641 = CIRCLE('',#52731,0.0999999999999979) ;
#18642 = CIRCLE('',#52733,0.2) ;
#18643 = CIRCLE('',#52734,0.1) ;
#18644 = CIRCLE('',#52736,0.100000000000051) ;
#18645 = CIRCLE('',#52737,0.0999999999999979) ;
#18646 = CIRCLE('',#52738,4.49999999999997) ;
#18647 = CIRCLE('',#52739,2.9) ;
#18648 = CIRCLE('',#52740,0.1) ;
#18649 = CIRCLE('',#52742,0.1) ;
#18650 = CIRCLE('',#52745,0.1) ;
#18651 = CIRCLE('',#52746,0.100000000000013) ;
#18652 = CIRCLE('',#52749,1.50000000000013) ;
#18653 = CIRCLE('',#52750,1.50000000000013) ;
#18654 = CIRCLE('',#52752,0.0999999999999979) ;
#18655 = CIRCLE('',#52755,0.200000000000002) ;
#18656 = CIRCLE('',#52756,0.100000000000002) ;
#18657 = CIRCLE('',#52757,0.1) ;
#18658 = CIRCLE('',#52758,0.100000000000096) ;
#18659 = CIRCLE('',#52760,0.0999999999999801) ;
#18660 = CIRCLE('',#52762,0.700000000000003) ;
#18661 = CIRCLE('',#52764,0.1) ;
#18662 = CIRCLE('',#52765,0.0999999999999957) ;
#18663 = CIRCLE('',#52766,0.100000000000004) ;
#18664 = CIRCLE('',#52770,0.0999999999999941) ;
#18665 = CIRCLE('',#52775,3.89999999999997) ;
#18666 = CIRCLE('',#52776,0.100000000000022) ;
#18667 = CIRCLE('',#52778,0.0999999999999856) ;
#18668 = CIRCLE('',#52780,0.099999999999989) ;
#18669 = CIRCLE('',#52781,3.89999999999982) ;
#18670 = CIRCLE('',#52783,0.0999999999999979) ;
#18671 = CIRCLE('',#52785,0.10000000000006) ;
#18672 = CIRCLE('',#52786,0.75) ;
#18673 = CIRCLE('',#52787,0.65) ;
#18674 = CIRCLE('',#52789,0.0999999999999979) ;
#18675 = CIRCLE('',#52791,0.75) ;
#18676 = CIRCLE('',#52792,0.65) ;
#18677 = CIRCLE('',#52794,0.700000000000003) ;
#18678 = CIRCLE('',#52797,3.89999999999982) ;
#18679 = CIRCLE('',#52800,3.89999999999997) ;
#18680 = CIRCLE('',#52802,0.100000000000027) ;
#18681 = CIRCLE('',#52803,0.0999999999999976) ;
#18682 = CIRCLE('',#52804,0.0999999999999801) ;
#18683 = CIRCLE('',#52808,0.100000000000016) ;
#18684 = CIRCLE('',#52809,0.100000000000014) ;
#18685 = CIRCLE('',#52812,0.100000000000001) ;
#18686 = CIRCLE('',#52823,0.100000000000016) ;
#18687 = CIRCLE('',#52827,2.) ;
#18688 = CIRCLE('',#52832,2.) ;
#18689 = CIRCLE('',#52835,0.0999999999999801) ;
#18690 = CIRCLE('',#52839,0.0999999999999973) ;
#18691 = CIRCLE('',#52840,0.2) ;
#18692 = CIRCLE('',#52841,0.1) ;
#18693 = CIRCLE('',#52845,0.1) ;
#18694 = CIRCLE('',#52847,0.0999999999999979) ;
#18695 = CIRCLE('',#52849,0.0999999999999847) ;
#18696 = CIRCLE('',#52850,0.0999999999999979) ;
#18697 = CIRCLE('',#52851,0.0999999999999979) ;
#18698 = CIRCLE('',#52855,0.0999999999999979) ;
#18699 = CIRCLE('',#52856,0.0999999999999979) ;
#18700 = CIRCLE('',#52857,0.199999999999978) ;
#18701 = CIRCLE('',#52858,0.0999999999999847) ;
#18702 = CIRCLE('',#52863,1.) ;
#18703 = CIRCLE('',#52864,4.06491106406736) ;
#18704 = CIRCLE('',#52865,4.05) ;
#18705 = CIRCLE('',#52866,0.200000000000031) ;
#18706 = CIRCLE('',#52867,0.199999999999996) ;
#18707 = CIRCLE('',#52868,0.199999999999996) ;
#18708 = CIRCLE('',#52869,0.200000000000001) ;
#18709 = CIRCLE('',#52870,4.05) ;
#18710 = CIRCLE('',#52871,4.06491106406736) ;
#18711 = CIRCLE('',#52872,1.) ;
#18712 = CIRCLE('',#52873,1.) ;
#18713 = CIRCLE('',#52874,4.06491106406736) ;
#18714 = CIRCLE('',#52875,4.05) ;
#18715 = CIRCLE('',#52876,4.06491106406736) ;
#18716 = CIRCLE('',#52877,1.) ;
#18717 = CIRCLE('',#52878,1.60000000000004) ;
#18718 = CIRCLE('',#52879,2.99999999999998) ;
#18719 = CIRCLE('',#52880,3.6) ;
#18720 = CIRCLE('',#52881,3.6) ;
#18721 = CIRCLE('',#52882,4.09999999999997) ;
#18722 = CIRCLE('',#52883,3.) ;
#18723 = CIRCLE('',#52884,4.49999999999997) ;
#18724 = CIRCLE('',#52885,0.199999999999996) ;
#18725 = CIRCLE('',#52886,0.199999999999996) ;
#18726 = CIRCLE('',#52887,0.199999999999996) ;
#18727 = CIRCLE('',#52888,0.199999999999996) ;
#18728 = CIRCLE('',#52889,0.200000000000031) ;
#18729 = CIRCLE('',#52890,4.49999999999997) ;
#18730 = CIRCLE('',#52891,0.100000000000016) ;
#18731 = CIRCLE('',#52892,0.100000000000004) ;
#18732 = CIRCLE('',#52893,0.0999999999999979) ;
#18733 = CIRCLE('',#52894,0.0999999999999973) ;
#18734 = CIRCLE('',#52895,1.1) ;
#18735 = CIRCLE('',#52896,0.100000000000106) ;
#18736 = CIRCLE('',#52897,0.3999999999999) ;
#18737 = CIRCLE('',#52898,0.400000000000114) ;
#18738 = CIRCLE('',#52899,0.100000000000016) ;
#18739 = CIRCLE('',#52900,0.500000000000025) ;
#18740 = CIRCLE('',#52901,0.199999999999996) ;
#18741 = CIRCLE('',#52902,0.200000000000031) ;
#18742 = CIRCLE('',#52903,0.2) ;
#18743 = CIRCLE('',#52904,0.200000000000031) ;
#18744 = CIRCLE('',#52905,2.6) ;
#18745 = CIRCLE('',#52906,0.199999999999996) ;
#18746 = CIRCLE('',#52907,0.199999999999996) ;
#18747 = CIRCLE('',#52908,0.199999999999996) ;
#18748 = CIRCLE('',#52909,0.199999999999996) ;
#18749 = CIRCLE('',#52910,0.199999999999996) ;
#18750 = CIRCLE('',#52911,0.199999999999996) ;
#18751 = CIRCLE('',#52912,2.49999999999999) ;
#18752 = CIRCLE('',#52913,0.199999999999996) ;
#18753 = CIRCLE('',#52914,0.199999999999995) ;
#18754 = CIRCLE('',#52915,0.199999999999996) ;
#18755 = CIRCLE('',#52916,0.199999999999995) ;
#18756 = CIRCLE('',#52917,0.199999999999996) ;
#18757 = CIRCLE('',#52918,0.199999999999996) ;
#18758 = CIRCLE('',#52919,0.200000000000031) ;
#18759 = CIRCLE('',#52920,0.199999999999996) ;
#18760 = CIRCLE('',#52921,0.199999999999996) ;
#18761 = CIRCLE('',#52922,0.199999999999996) ;
#18762 = CIRCLE('',#52923,0.199999999999996) ;
#18763 = CIRCLE('',#52924,0.199999999999996) ;
#18764 = CIRCLE('',#52925,0.199999999999996) ;
#18765 = CIRCLE('',#52926,0.199999999999996) ;
#18766 = CIRCLE('',#52928,0.10000000000001) ;
#18767 = CIRCLE('',#52929,0.0999999999999845) ;
#18768 = CIRCLE('',#52932,2.9) ;
#18769 = CIRCLE('',#52934,0.0999999999999979) ;
#18770 = CIRCLE('',#52935,3.99999999999997) ;
#18771 = CIRCLE('',#52937,0.1) ;
#18772 = CIRCLE('',#52940,3.99999999999997) ;
#18773 = CIRCLE('',#52944,0.0999999999999801) ;
#18774 = CIRCLE('',#52945,0.0999999999999979) ;
#18775 = CIRCLE('',#52946,0.0999999999999848) ;
#18776 = CIRCLE('',#52948,0.0999999999999979) ;
#18777 = CIRCLE('',#52950,0.0999999999999979) ;
#18778 = CIRCLE('',#52951,0.599999999999915) ;
#18779 = CIRCLE('',#52952,0.699999999999915) ;
#18780 = CIRCLE('',#52954,0.0999999999999979) ;
#18781 = CIRCLE('',#52956,0.0999999999999979) ;
#18782 = CIRCLE('',#52957,1.) ;
#18783 = CIRCLE('',#52958,0.9) ;
#18784 = CIRCLE('',#52961,0.100000000000016) ;
#18785 = CIRCLE('',#52963,0.0999999999999984) ;
#18786 = CIRCLE('',#52964,0.600000000000114) ;
#18787 = CIRCLE('',#52965,0.500000000000114) ;
#18788 = CIRCLE('',#52968,0.0999999999999979) ;
#18789 = CIRCLE('',#52970,0.0999999999999984) ;
#18790 = CIRCLE('',#52972,0.999999999999996) ;
#18791 = CIRCLE('',#52973,0.100000000000022) ;
#18792 = CIRCLE('',#52974,0.100000000000008) ;
#18793 = CIRCLE('',#52975,0.200000000000106) ;
#18794 = CIRCLE('',#52977,0.0999999999999848) ;
#18795 = CIRCLE('',#52979,0.0999999999999979) ;
#18796 = CIRCLE('',#52980,0.499999999999901) ;
#18797 = CIRCLE('',#52984,0.100000000000162) ;
#18798 = CIRCLE('',#52986,0.0999999999999801) ;
#18799 = CIRCLE('',#52987,0.500000000000114) ;
#18800 = CIRCLE('',#52989,0.0999999999999801) ;
#18801 = CIRCLE('',#52991,0.500000000000025) ;
#18802 = CIRCLE('',#52995,0.599999999999915) ;
#18803 = CIRCLE('',#52998,1.) ;
#18804 = CIRCLE('',#53000,0.85) ;
#18805 = CIRCLE('',#53001,0.65) ;
#18806 = CIRCLE('',#53002,0.6) ;
#18807 = CIRCLE('',#53009,0.999999999999996) ;
#18808 = CIRCLE('',#53011,0.0999999999999979) ;
#18809 = CIRCLE('',#53012,0.0999999999999915) ;
#18810 = CIRCLE('',#53014,0.1) ;
#18811 = CIRCLE('',#53016,0.0999999999999979) ;
#18812 = CIRCLE('',#53017,0.0999999999999979) ;
#18813 = CIRCLE('',#53018,0.199999999999996) ;
#18814 = CIRCLE('',#53019,0.100000000000016) ;
#18815 = CIRCLE('',#53021,0.0999999999999979) ;
#18816 = CIRCLE('',#53023,0.6) ;
#18817 = CIRCLE('',#53024,0.5) ;
#18818 = CIRCLE('',#53026,0.200000000000031) ;
#18819 = CIRCLE('',#53027,0.0999999999999979) ;
#18820 = CIRCLE('',#53028,0.100000000000016) ;
#18821 = CIRCLE('',#53029,0.0999999999999979) ;
#18822 = CIRCLE('',#53030,0.100000000000005) ;
#18823 = CIRCLE('',#53031,0.100000000000016) ;
#18824 = CIRCLE('',#53033,0.0999999999999979) ;
#18825 = CIRCLE('',#53034,0.5) ;
#18826 = CIRCLE('',#53035,0.6) ;
#18827 = CIRCLE('',#53038,0.0999999999999915) ;
#18828 = CIRCLE('',#53039,0.0999999999999926) ;
#18829 = CIRCLE('',#53040,0.0999999999999879) ;
#18830 = CIRCLE('',#53044,0.1) ;
#18831 = CIRCLE('',#53046,0.1) ;
#18832 = CIRCLE('',#53047,0.199999999999996) ;
#18833 = CIRCLE('',#53049,0.1) ;
#18834 = CIRCLE('',#53051,0.1) ;
#18835 = CIRCLE('',#53052,0.200000000000031) ;
#18836 = CIRCLE('',#53055,0.1) ;
#18837 = CIRCLE('',#53057,0.100000000000016) ;
#18838 = CIRCLE('',#53059,0.100000000000007) ;
#18839 = CIRCLE('',#53060,0.3) ;
#18840 = CIRCLE('',#53061,0.4) ;
#18841 = CIRCLE('',#53063,0.0999999999999623) ;
#18842 = CIRCLE('',#53065,0.100000000000016) ;
#18843 = CIRCLE('',#53066,0.300000000000031) ;
#18844 = CIRCLE('',#53067,0.200000000000031) ;
#18845 = CIRCLE('',#53069,0.100000000000016) ;
#18846 = CIRCLE('',#53071,0.100000000000002) ;
#18847 = CIRCLE('',#53072,0.3) ;
#18848 = CIRCLE('',#53073,0.2) ;
#18849 = CIRCLE('',#53075,0.0999999999999979) ;
#18850 = CIRCLE('',#53077,0.0999999999999801) ;
#18851 = CIRCLE('',#53078,0.3) ;
#18852 = CIRCLE('',#53079,0.4) ;
#18853 = CIRCLE('',#53082,0.100000000000016) ;
#18854 = CIRCLE('',#53083,0.100000000000009) ;
#18855 = CIRCLE('',#53086,0.1) ;
#18856 = CIRCLE('',#53088,0.5) ;
#18857 = CIRCLE('',#53091,0.4) ;
#18858 = CIRCLE('',#53096,0.4) ;
#18859 = CIRCLE('',#53102,0.4) ;
#18860 = CIRCLE('',#53104,0.1) ;
#18861 = CIRCLE('',#53105,0.1) ;
#18862 = CIRCLE('',#53108,0.1) ;
#18863 = CIRCLE('',#53109,0.1) ;
#18864 = CIRCLE('',#53111,0.199999999999996) ;
#18865 = CIRCLE('',#53112,0.100000000000016) ;
#18866 = CIRCLE('',#53113,0.0999999999999979) ;
#18867 = CIRCLE('',#53114,0.0999999999999979) ;
#18868 = CIRCLE('',#53116,0.100000000000051) ;
#18869 = CIRCLE('',#53117,0.0999999999999979) ;
#18870 = CIRCLE('',#53118,0.200000000000067) ;
#18871 = CIRCLE('',#53119,0.0999999999999979) ;
#18872 = CIRCLE('',#53122,0.0999999999999979) ;
#18873 = CIRCLE('',#53123,0.1) ;
#18874 = CIRCLE('',#53125,0.0999999999999979) ;
#18875 = CIRCLE('',#53126,0.500000000000007) ;
#18876 = CIRCLE('',#53127,0.400000000000007) ;
#18877 = CIRCLE('',#53130,0.1) ;
#18878 = CIRCLE('',#53132,0.1) ;
#18879 = CIRCLE('',#53134,0.0999999999999979) ;
#18880 = CIRCLE('',#53136,0.0999999999999979) ;
#18881 = CIRCLE('',#53137,0.500000000000007) ;
#18882 = CIRCLE('',#53138,0.400000000000007) ;
#18883 = CIRCLE('',#53140,0.1) ;
#18884 = CIRCLE('',#53142,0.500000000000007) ;
#18885 = CIRCLE('',#53144,0.3) ;
#18886 = CIRCLE('',#53145,0.4) ;
#18887 = CIRCLE('',#53146,0.6) ;
#18888 = CIRCLE('',#53147,0.65) ;
#18889 = CIRCLE('',#53149,0.500000000000007) ;
#18890 = CIRCLE('',#53152,0.0999999999999979) ;
#18891 = CIRCLE('',#53154,0.0999999999999979) ;
#18892 = CIRCLE('',#53158,0.10000000000001) ;
#18893 = CIRCLE('',#53159,0.699999999999915) ;
#18894 = CIRCLE('',#53161,0.0999999999999847) ;
#18895 = CIRCLE('',#53163,0.0999999999999979) ;
#18896 = CIRCLE('',#53164,0.9) ;
#18897 = CIRCLE('',#53166,0.0999999999999979) ;
#18898 = CIRCLE('',#53168,0.0999999999999801) ;
#18899 = CIRCLE('',#53169,0.5) ;
#18900 = CIRCLE('',#53171,0.0999999999999979) ;
#18901 = CIRCLE('',#53173,0.0999999999999446) ;
#18902 = CIRCLE('',#53174,0.75) ;
#18903 = CIRCLE('',#53176,0.0999999999999979) ;
#18904 = CIRCLE('',#53178,0.0999999999999091) ;
#18905 = CIRCLE('',#53179,0.75) ;
#18906 = CIRCLE('',#53181,0.0999999999999979) ;
#18907 = CIRCLE('',#53182,0.0999999999999984) ;
#18908 = CIRCLE('',#53185,0.0999999999999984) ;
#18909 = CIRCLE('',#53186,0.100000000000022) ;
#18910 = CIRCLE('',#53188,0.0999999999999918) ;
#18911 = CIRCLE('',#53190,0.100000000000001) ;
#18912 = CIRCLE('',#53192,0.0999999999999979) ;
#18913 = CIRCLE('',#53194,0.0999999999999801) ;
#18914 = CIRCLE('',#53196,0.0999999999999973) ;
#18915 = CIRCLE('',#53197,0.600000000000129) ;
#18916 = CIRCLE('',#53199,0.0999999999999973) ;
#18917 = CIRCLE('',#53201,0.10000000000002) ;
#18918 = CIRCLE('',#53202,0.600000000000129) ;
#18919 = CIRCLE('',#53204,0.0999999999999801) ;
#18920 = CIRCLE('',#53205,1.) ;
#18921 = CIRCLE('',#53207,0.100000000000016) ;
#18922 = CIRCLE('',#53209,0.0999999999999979) ;
#18923 = CIRCLE('',#53211,0.0999999999999979) ;
#18924 = CIRCLE('',#53213,1.50000000000004) ;
#18925 = CIRCLE('',#53216,1.50000000000004) ;
#18926 = CIRCLE('',#53223,0.100000000000264) ;
#18927 = CIRCLE('',#53227,0.0999999999999979) ;
#18928 = CIRCLE('',#53229,0.0999999999999934) ;
#18929 = CIRCLE('',#53230,1.5) ;
#18930 = CIRCLE('',#53233,0.0999999999999979) ;
#18931 = CIRCLE('',#53234,0.400000000000007) ;
#18932 = CIRCLE('',#53236,0.0999999999999979) ;
#18933 = CIRCLE('',#53238,0.100000000000002) ;
#18934 = CIRCLE('',#53239,0.75) ;
#18935 = CIRCLE('',#53241,0.0999999999999979) ;
#18936 = CIRCLE('',#53243,0.100000000000007) ;
#18937 = CIRCLE('',#53245,0.0999999999999934) ;
#18938 = CIRCLE('',#53247,0.100000000000016) ;
#18939 = CIRCLE('',#53248,0.5) ;
#18940 = CIRCLE('',#53252,0.1) ;
#18941 = CIRCLE('',#53253,0.0999999999999979) ;
#18942 = CIRCLE('',#53255,0.0999999999999979) ;
#18943 = CIRCLE('',#53256,0.500000000000043) ;
#18944 = CIRCLE('',#53257,0.400000000000043) ;
#18945 = CIRCLE('',#53259,0.0999999999999979) ;
#18946 = CIRCLE('',#53261,0.0999999999999979) ;
#18947 = CIRCLE('',#53262,0.400000000000007) ;
#18948 = CIRCLE('',#53264,0.0999999999999979) ;
#18949 = CIRCLE('',#53266,0.0999999999999801) ;
#18950 = CIRCLE('',#53267,0.4) ;
#18951 = CIRCLE('',#53273,0.5) ;
#18952 = CIRCLE('',#53274,4.56491106406736) ;
#18953 = CIRCLE('',#53275,4.55) ;
#18954 = CIRCLE('',#53277,0.500000000000009) ;
#18955 = CIRCLE('',#53282,2.) ;
#18956 = CIRCLE('',#53284,0.4) ;
#18957 = CIRCLE('',#53288,0.100000000000016) ;
#18958 = CIRCLE('',#53290,0.100000000000003) ;
#18959 = CIRCLE('',#53292,0.0999999999999979) ;
#18960 = CIRCLE('',#53294,0.100000000000007) ;
#18961 = CIRCLE('',#53296,0.0999999999999981) ;
#18962 = CIRCLE('',#53297,0.0999999999999979) ;
#18963 = CIRCLE('',#53299,0.099999999999989) ;
#18964 = CIRCLE('',#53300,0.75) ;
#18965 = CIRCLE('',#53301,0.65) ;
#18966 = CIRCLE('',#53304,0.1) ;
#18967 = CIRCLE('',#53307,0.1) ;
#18968 = CIRCLE('',#53309,0.0999999999999979) ;
#18969 = CIRCLE('',#53310,0.100000000000003) ;
#18970 = CIRCLE('',#53313,0.4) ;
#18971 = CIRCLE('',#53319,0.515810020027939) ;
#18972 = CIRCLE('',#53330,0.200000000000009) ;
#18973 = CIRCLE('',#53332,0.200000000000046) ;
#18974 = CIRCLE('',#53333,0.200000000000015) ;
#18975 = CIRCLE('',#53335,0.199999999999996) ;
#18976 = CIRCLE('',#53336,0.19999999999999) ;
#18977 = CIRCLE('',#53342,0.199999999999979) ;
#18978 = CIRCLE('',#53345,0.200000000000007) ;
#18979 = CIRCLE('',#53346,0.199999999999997) ;
#18980 = CIRCLE('',#53351,6.15) ;
#18981 = CIRCLE('',#53352,6.15) ;
#18982 = CIRCLE('',#53353,0.799999999999972) ;
#18983 = CIRCLE('',#53354,0.199999999999963) ;
#18984 = CIRCLE('',#53355,0.199999999999963) ;
#18985 = CIRCLE('',#53356,0.799999999999972) ;
#18986 = CIRCLE('',#53362,0.2) ;
#18987 = CIRCLE('',#53364,0.199999999999978) ;
#18988 = CIRCLE('',#53369,0.200000000000008) ;
#18989 = CIRCLE('',#53370,0.2) ;
#18990 = CIRCLE('',#53378,6.15) ;
#18991 = CIRCLE('',#53386,3.6) ;
#18992 = CIRCLE('',#53389,3.6) ;
#18993 = CIRCLE('',#53390,3.6) ;
#18994 = CIRCLE('',#53392,3.6) ;
#18995 = CIRCLE('',#53397,3.79999999999997) ;
#18996 = CIRCLE('',#53398,1.40000000000004) ;
#18997 = CIRCLE('',#53400,0.0999999999999979) ;
#18998 = CIRCLE('',#53403,0.0999999999999928) ;
#18999 = CIRCLE('',#53505,0.1) ;
#19000 = CIRCLE('',#53507,0.1) ;
#19001 = CIRCLE('',#53508,0.699999999999972) ;
#19002 = CIRCLE('',#53509,0.599999999999972) ;
#19003 = CIRCLE('',#53515,0.1) ;
#19004 = CIRCLE('',#53517,0.1) ;
#19005 = CIRCLE('',#53518,0.299999999999963) ;
#19006 = CIRCLE('',#53519,0.399999999999963) ;
#19007 = CIRCLE('',#53527,0.299999999999963) ;
#19008 = CIRCLE('',#53537,0.1) ;
#19009 = CIRCLE('',#53539,0.1) ;
#19010 = CIRCLE('',#53540,0.699999999999972) ;
#19011 = CIRCLE('',#53541,0.599999999999972) ;
#19012 = CIRCLE('',#53547,0.1) ;
#19013 = CIRCLE('',#53549,0.1) ;
#19014 = CIRCLE('',#53550,0.299999999999963) ;
#19015 = CIRCLE('',#53551,0.399999999999963) ;
#19016 = CIRCLE('',#53560,0.299999999999963) ;
#19017 = CIRCLE('',#53604,4.56491106406736) ;
#19018 = CIRCLE('',#53605,4.55) ;
#19019 = CIRCLE('',#53606,4.55) ;
#19020 = CIRCLE('',#53607,4.56491106406736) ;
#19021 = CIRCLE('',#53608,0.5) ;
#19022 = CIRCLE('',#53643,0.0999999999999801) ;
#19023 = CIRCLE('',#53654,0.100000000000005) ;
#19024 = CIRCLE('',#53655,0.1) ;
#19025 = CIRCLE('',#53657,0.0999999999999979) ;
#19026 = CIRCLE('',#53660,0.0999999999999745) ;
#19027 = CIRCLE('',#53661,0.699999999999972) ;
#19028 = CIRCLE('',#53663,0.1) ;
#19029 = CIRCLE('',#53672,0.099999999999989) ;
#19030 = CIRCLE('',#53683,0.0999999999999745) ;
#19031 = CIRCLE('',#53684,0.699999999999972) ;
#19032 = CIRCLE('',#53687,0.100000000000005) ;
#19033 = CIRCLE('',#53689,0.100000000000007) ;
#19034 = CIRCLE('',#53704,4.55) ;
#19035 = CIRCLE('',#53705,4.56491106406736) ;
#19036 = CIRCLE('',#53708,2.99999999999998) ;
#19037 = CIRCLE('',#53711,1.60000000000004) ;
#19038 = CIRCLE('',#53716,0.500000000000043) ;
#19039 = CIRCLE('',#53718,0.500000000000043) ;
#19040 = CIRCLE('',#53729,1.5) ;
#19041 = CIRCLE('',#53734,0.399999999999992) ;
#19042 = CIRCLE('',#53741,0.4) ;
#19043 = CIRCLE('',#53752,0.499999999999998) ;
#19044 = CIRCLE('',#53753,0.500000000000009) ;
#19045 = CIRCLE('',#53754,0.499999999999997) ;
#19046 = CIRCLE('',#53756,4.06491106406736) ;
#19047 = CIRCLE('',#53757,0.499999999999998) ;
#19048 = CIRCLE('',#53759,0.499999999999998) ;
#19049 = CIRCLE('',#53760,0.499999999999998) ;
#19050 = CIRCLE('',#53762,0.499999999999998) ;
#19051 = CIRCLE('',#53763,4.05) ;
#19052 = CIRCLE('',#53767,0.499999999999998) ;
#19053 = CIRCLE('',#53768,0.499999999999992) ;
#19054 = CIRCLE('',#53769,0.500000000000009) ;
#19055 = CIRCLE('',#53773,4.06491106406736) ;
#19056 = CIRCLE('',#53774,0.499999999999998) ;
#19057 = CIRCLE('',#53775,0.500000000000018) ;
#19058 = CIRCLE('',#53776,0.500000000000019) ;
#19059 = CIRCLE('',#53778,0.499999999999998) ;
#19060 = CIRCLE('',#53780,4.05) ;
#19061 = CIRCLE('',#53782,0.499999999999998) ;
#19062 = CIRCLE('',#53783,0.499999999999998) ;
#19063 = CIRCLE('',#53785,0.499999999999998) ;
#19064 = CIRCLE('',#53786,4.05) ;
#19065 = CIRCLE('',#53788,0.50000000000001) ;
#19066 = CIRCLE('',#53789,0.500000000000019) ;
#19067 = CIRCLE('',#53791,0.499999999999998) ;
#19068 = CIRCLE('',#53793,4.05) ;
#19069 = CIRCLE('',#53796,0.499999999999998) ;
#19070 = CIRCLE('',#53797,0.499999999999989) ;
#19071 = CIRCLE('',#53799,4.06491106406736) ;
#19072 = CIRCLE('',#53800,1.) ;
#19073 = CIRCLE('',#53803,0.499999999999998) ;
#19074 = CIRCLE('',#53804,0.499999999999998) ;
#19075 = CIRCLE('',#53806,4.06491106406736) ;
#19076 = CIRCLE('',#53809,0.500000000000012) ;
#19077 = CIRCLE('',#53812,1.) ;
#19078 = CIRCLE('',#53813,0.500000000000009) ;
#19079 = CIRCLE('',#53819,0.500000000000009) ;
#19080 = CIRCLE('',#53820,0.500000000000009) ;
#19081 = CIRCLE('',#53831,0.500000000000043) ;
#19082 = CIRCLE('',#53836,0.200000000000031) ;
#19083 = CIRCLE('',#53840,0.199999999999996) ;
#19084 = CIRCLE('',#53843,0.199999999999996) ;
#19085 = CIRCLE('',#53849,2.) ;
#19086 = CIRCLE('',#53852,2.6) ;
#19087 = CIRCLE('',#53855,0.200000000000001) ;
#19088 = CIRCLE('',#53858,0.199999999999996) ;
#19089 = CIRCLE('',#53861,0.199999999999996) ;
#19090 = CIRCLE('',#53864,0.199999999999996) ;
#19091 = CIRCLE('',#53868,0.199999999999996) ;
#19092 = CIRCLE('',#53871,2.49999999999999) ;
#19093 = CIRCLE('',#53874,0.199999999999995) ;
#19094 = CIRCLE('',#53877,0.199999999999996) ;
#19095 = CIRCLE('',#53880,0.199999999999996) ;
#19096 = CIRCLE('',#53883,0.199999999999996) ;
#19097 = CIRCLE('',#53888,0.100000000000016) ;
#19098 = CIRCLE('',#53891,0.0999999999999979) ;
#19099 = CIRCLE('',#53894,0.100000000000051) ;
#19100 = CIRCLE('',#53896,0.199999999999996) ;
#19101 = CIRCLE('',#53899,0.199999999999996) ;
#19102 = CIRCLE('',#53903,0.199999999999996) ;
#19103 = CIRCLE('',#53906,0.199999999999996) ;
#19104 = CIRCLE('',#53910,0.199999999999996) ;
#19105 = CIRCLE('',#53913,0.199999999999996) ;
#19106 = CIRCLE('',#53919,0.199999999999995) ;
#19107 = CIRCLE('',#53922,0.199999999999996) ;
#19108 = CIRCLE('',#53927,0.199999999999996) ;
#19109 = CIRCLE('',#53930,0.200000000000031) ;
#19110 = CIRCLE('',#53934,0.199999999999996) ;
#19111 = CIRCLE('',#53941,0.200000000000031) ;
#19112 = CIRCLE('',#53943,4.05) ;
#19113 = CIRCLE('',#53945,0.199999999999996) ;
#19114 = CIRCLE('',#53949,0.199999999999996) ;
#19115 = CIRCLE('',#53952,0.199999999999996) ;
#19116 = CIRCLE('',#53956,0.0999999999999973) ;
#19117 = CIRCLE('',#53959,0.0999999999999979) ;
#19118 = CIRCLE('',#53962,0.100000000000004) ;
#19119 = CIRCLE('',#53967,0.199999999999996) ;
#19120 = CIRCLE('',#53982,4.49999999999997) ;
#19121 = CIRCLE('',#53983,0.199999999999996) ;
#19122 = CIRCLE('',#54029,1.67775) ;
#19123 = CIRCLE('',#54034,1.9635) ;
#19124 = CIRCLE('',#54035,1.9635) ;
#19125 = CIRCLE('',#54036,1.9635) ;
#19126 = CIRCLE('',#54038,1.67775) ;
#19127 = CIRCLE('',#54044,3.) ;
#19128 = CIRCLE('',#54045,1.) ;
#19129 = CIRCLE('',#54046,3.96824583655185) ;
#19130 = CIRCLE('',#54049,4.) ;
#19131 = CIRCLE('',#54050,1.) ;
#19132 = CIRCLE('',#54051,3.) ;
#19133 = CIRCLE('',#54054,2.) ;
#19134 = CIRCLE('',#54056,2.) ;
#19135 = CIRCLE('',#54058,4.95) ;
#19136 = CIRCLE('',#54059,5.1) ;
#19137 = CIRCLE('',#54062,0.350000000000003) ;
#19138 = CIRCLE('',#54063,0.500000000000003) ;
#19139 = CIRCLE('',#54066,4.95) ;
#19140 = CIRCLE('',#54067,5.1) ;
#19141 = CIRCLE('',#54070,0.350000000000003) ;
#19142 = CIRCLE('',#54071,0.500000000000003) ;
#19143 = CIRCLE('',#54074,4.95) ;
#19144 = CIRCLE('',#54075,5.1) ;
#19145 = CIRCLE('',#54078,0.350000000000003) ;
#19146 = CIRCLE('',#54079,0.500000000000003) ;
#19147 = CIRCLE('',#54082,4.95) ;
#19148 = CIRCLE('',#54083,5.1) ;
#19149 = CIRCLE('',#54086,0.350000000000003) ;
#19150 = CIRCLE('',#54087,0.500000000000003) ;
#19151 = CIRCLE('',#54090,4.95) ;
#19152 = CIRCLE('',#54091,5.1) ;
#19153 = CIRCLE('',#54094,0.350000000000003) ;
#19154 = CIRCLE('',#54095,0.500000000000003) ;
#19155 = CIRCLE('',#54098,4.95) ;
#19156 = CIRCLE('',#54099,5.1) ;
#19157 = CIRCLE('',#54102,0.350000000000003) ;
#19158 = CIRCLE('',#54103,0.500000000000003) ;
#19159 = CIRCLE('',#54106,4.95) ;
#19160 = CIRCLE('',#54107,5.1) ;
#19161 = CIRCLE('',#54110,0.350000000000003) ;
#19162 = CIRCLE('',#54111,0.500000000000003) ;
#19163 = CIRCLE('',#54114,4.95) ;
#19164 = CIRCLE('',#54115,5.1) ;
#19165 = CIRCLE('',#54118,0.350000000000003) ;
#19166 = CIRCLE('',#54119,0.500000000000003) ;
#19167 = CIRCLE('',#54122,4.95) ;
#19168 = CIRCLE('',#54123,5.1) ;
#19169 = CIRCLE('',#54126,0.350000000000003) ;
#19170 = CIRCLE('',#54127,0.500000000000003) ;
#19171 = CIRCLE('',#54130,4.95) ;
#19172 = CIRCLE('',#54131,5.1) ;
#19173 = CIRCLE('',#54134,0.350000000000003) ;
#19174 = CIRCLE('',#54135,0.500000000000003) ;
#19175 = CIRCLE('',#54138,4.95) ;
#19176 = CIRCLE('',#54139,5.1) ;
#19177 = CIRCLE('',#54142,0.500000000000003) ;
#19178 = CIRCLE('',#54143,0.350000000000003) ;
#19179 = CIRCLE('',#54146,5.1) ;
#19180 = CIRCLE('',#54147,4.95) ;
#19181 = CIRCLE('',#54150,0.500000000000003) ;
#19182 = CIRCLE('',#54151,0.350000000000003) ;
#19183 = CIRCLE('',#54154,5.1) ;
#19184 = CIRCLE('',#54155,4.95) ;
#19185 = CIRCLE('',#54158,0.500000000000003) ;
#19186 = CIRCLE('',#54159,0.350000000000003) ;
#19187 = CIRCLE('',#54162,5.1) ;
#19188 = CIRCLE('',#54163,4.95) ;
#19189 = CIRCLE('',#54166,0.500000000000003) ;
#19190 = CIRCLE('',#54167,0.350000000000003) ;
#19191 = CIRCLE('',#54170,5.1) ;
#19192 = CIRCLE('',#54171,4.95) ;
#19193 = CIRCLE('',#54174,0.500000000000003) ;
#19194 = CIRCLE('',#54175,0.350000000000003) ;
#19195 = CIRCLE('',#54178,5.1) ;
#19196 = CIRCLE('',#54179,4.95) ;
#19197 = CIRCLE('',#54182,0.500000000000003) ;
#19198 = CIRCLE('',#54183,0.350000000000003) ;
#19199 = CIRCLE('',#54186,5.1) ;
#19200 = CIRCLE('',#54187,4.95) ;
#19201 = CIRCLE('',#54190,0.500000000000003) ;
#19202 = CIRCLE('',#54191,0.350000000000003) ;
#19203 = CIRCLE('',#54194,5.1) ;
#19204 = CIRCLE('',#54195,4.95) ;
#19205 = CIRCLE('',#54198,0.500000000000003) ;
#19206 = CIRCLE('',#54199,0.350000000000003) ;
#19207 = CIRCLE('',#54202,5.1) ;
#19208 = CIRCLE('',#54203,4.95) ;
#19209 = CIRCLE('',#54206,0.500000000000003) ;
#19210 = CIRCLE('',#54207,0.350000000000003) ;
#19211 = CIRCLE('',#54210,5.1) ;
#19212 = CIRCLE('',#54211,4.95) ;
#19213 = CIRCLE('',#54214,0.500000000000003) ;
#19214 = CIRCLE('',#54215,0.350000000000003) ;
#19215 = CIRCLE('',#54219,0.500000000000003) ;
#19216 = CIRCLE('',#54222,5.1) ;
#19217 = CIRCLE('',#54225,0.500000000000003) ;
#19218 = CIRCLE('',#54228,5.1) ;
#19219 = CIRCLE('',#54231,0.500000000000003) ;
#19220 = CIRCLE('',#54234,5.1) ;
#19221 = CIRCLE('',#54237,0.500000000000003) ;
#19222 = CIRCLE('',#54240,5.1) ;
#19223 = CIRCLE('',#54243,0.500000000000003) ;
#19224 = CIRCLE('',#54246,5.1) ;
#19225 = CIRCLE('',#54249,0.500000000000003) ;
#19226 = CIRCLE('',#54252,5.1) ;
#19227 = CIRCLE('',#54255,0.500000000000003) ;
#19228 = CIRCLE('',#54258,5.1) ;
#19229 = CIRCLE('',#54261,0.500000000000003) ;
#19230 = CIRCLE('',#54264,5.1) ;
#19231 = CIRCLE('',#54267,0.500000000000003) ;
#19232 = CIRCLE('',#54270,5.1) ;
#19233 = CIRCLE('',#54273,0.500000000000003) ;
#19234 = CIRCLE('',#54276,5.1) ;
#19235 = CIRCLE('',#54278,4.95) ;
#19236 = CIRCLE('',#54280,4.95) ;
#19237 = CIRCLE('',#54282,4.95) ;
#19238 = CIRCLE('',#54284,4.95) ;
#19239 = CIRCLE('',#54286,4.95) ;
#19240 = CIRCLE('',#54288,4.95) ;
#19241 = CIRCLE('',#54290,4.95) ;
#19242 = CIRCLE('',#54292,4.95) ;
#19243 = CIRCLE('',#54294,4.95) ;
#19244 = CIRCLE('',#54296,4.95) ;
#19245 = CIRCLE('',#54298,4.95) ;
#19246 = CIRCLE('',#54300,4.95) ;
#19247 = CIRCLE('',#54302,4.95) ;
#19248 = CIRCLE('',#54304,4.95) ;
#19249 = CIRCLE('',#54306,4.95) ;
#19250 = CIRCLE('',#54308,4.95) ;
#19251 = CIRCLE('',#54310,4.95) ;
#19252 = CIRCLE('',#54312,4.95) ;
#19253 = CIRCLE('',#54314,4.95) ;
#19254 = CIRCLE('',#54315,4.95) ;
#19255 = CIRCLE('',#54317,0.15) ;
#19256 = CIRCLE('',#54318,4.95) ;
#19257 = CIRCLE('',#54321,0.15) ;
#19258 = CIRCLE('',#54322,4.95) ;
#19259 = CIRCLE('',#54323,4.95) ;
#19260 = CIRCLE('',#54324,4.95) ;
#19261 = CIRCLE('',#54325,4.95) ;
#19262 = CIRCLE('',#54326,4.95) ;
#19263 = CIRCLE('',#54327,4.95) ;
#19264 = CIRCLE('',#54328,4.95) ;
#19265 = CIRCLE('',#54329,4.95) ;
#19266 = CIRCLE('',#54330,4.95) ;
#19267 = CIRCLE('',#54331,4.95) ;
#19268 = CIRCLE('',#54332,4.95) ;
#19269 = CIRCLE('',#54333,4.95) ;
#19270 = CIRCLE('',#54334,4.95) ;
#19271 = CIRCLE('',#54335,4.95) ;
#19272 = CIRCLE('',#54336,4.95) ;
#19273 = CIRCLE('',#54337,4.95) ;
#19274 = CIRCLE('',#54338,4.95) ;
#19275 = CIRCLE('',#54339,4.95) ;
#19276 = CIRCLE('',#54340,4.95) ;
#19277 = CIRCLE('',#54341,4.95) ;
#19278 = CIRCLE('',#54342,4.95) ;
#19279 = CIRCLE('',#54343,4.95) ;
#19280 = CIRCLE('',#54344,4.95) ;
#19281 = CIRCLE('',#54345,4.95) ;
#19282 = CIRCLE('',#54346,4.95) ;
#19283 = CIRCLE('',#54347,4.95) ;
#19284 = CIRCLE('',#54348,4.95) ;
#19285 = CIRCLE('',#54349,4.95) ;
#19286 = CIRCLE('',#54350,4.95) ;
#19287 = CIRCLE('',#54351,4.95) ;
#19288 = CIRCLE('',#54352,4.95) ;
#19289 = CIRCLE('',#54353,4.95) ;
#19290 = CIRCLE('',#54354,4.95) ;
#19291 = CIRCLE('',#54355,4.95) ;
#19292 = CIRCLE('',#54356,4.95) ;
#19293 = CIRCLE('',#54357,4.95) ;
#19294 = CIRCLE('',#54358,4.95) ;
#19295 = CIRCLE('',#54359,4.95) ;
#19296 = CIRCLE('',#54360,4.95) ;
#19297 = CIRCLE('',#54361,4.95) ;
#19298 = CIRCLE('',#54362,4.95) ;
#19299 = CIRCLE('',#54364,0.350000000000003) ;
#19300 = CIRCLE('',#54366,0.350000000000003) ;
#19301 = CIRCLE('',#54368,0.350000000000003) ;
#19302 = CIRCLE('',#54370,0.350000000000003) ;
#19303 = CIRCLE('',#54372,0.350000000000003) ;
#19304 = CIRCLE('',#54374,0.350000000000003) ;
#19305 = CIRCLE('',#54376,0.350000000000003) ;
#19306 = CIRCLE('',#54378,0.350000000000003) ;
#19307 = CIRCLE('',#54380,0.350000000000003) ;
#19308 = CIRCLE('',#54382,0.350000000000003) ;
#19309 = CIRCLE('',#54384,0.350000000000003) ;
#19310 = CIRCLE('',#54386,0.350000000000003) ;
#19311 = CIRCLE('',#54388,0.350000000000003) ;
#19312 = CIRCLE('',#54390,0.350000000000003) ;
#19313 = CIRCLE('',#54392,0.350000000000003) ;
#19314 = CIRCLE('',#54394,0.350000000000003) ;
#19315 = CIRCLE('',#54396,0.350000000000003) ;
#19316 = CIRCLE('',#54398,0.350000000000003) ;
#19317 = CIRCLE('',#54400,0.350000000000003) ;
#19318 = CIRCLE('',#54402,0.350000000000003) ;
#19319 = CIRCLE('',#54404,5.1) ;
#19320 = CIRCLE('',#54449,5.1) ;
#19321 = CIRCLE('',#54452,0.500000000000003) ;
#19322 = CIRCLE('',#54455,5.1) ;
#19323 = CIRCLE('',#54458,0.500000000000003) ;
#19324 = CIRCLE('',#54461,5.1) ;
#19325 = CIRCLE('',#54464,0.500000000000003) ;
#19326 = CIRCLE('',#54467,5.1) ;
#19327 = CIRCLE('',#54470,0.500000000000003) ;
#19328 = CIRCLE('',#54473,5.1) ;
#19329 = CIRCLE('',#54476,0.500000000000003) ;
#19330 = CIRCLE('',#54479,5.1) ;
#19331 = CIRCLE('',#54482,0.500000000000003) ;
#19332 = CIRCLE('',#54485,5.1) ;
#19333 = CIRCLE('',#54488,0.500000000000003) ;
#19334 = CIRCLE('',#54491,5.1) ;
#19335 = CIRCLE('',#54494,0.500000000000003) ;
#19336 = CIRCLE('',#54497,5.1) ;
#19337 = CIRCLE('',#54500,0.500000000000003) ;
#19338 = CIRCLE('',#54502,0.500000000000003) ;
#19339 = CIRCLE('',#54546,3.) ;
#19340 = CIRCLE('',#54547,1.) ;
#19341 = CIRCLE('',#54548,3.96824583655185) ;
#19342 = CIRCLE('',#54551,4.) ;
#19343 = CIRCLE('',#54552,1.) ;
#19344 = CIRCLE('',#54553,3.) ;
#19345 = CIRCLE('',#54556,2.) ;
#19346 = CIRCLE('',#54558,2.) ;
#19347 = CIRCLE('',#54560,4.95) ;
#19348 = CIRCLE('',#54561,5.1) ;
#19349 = CIRCLE('',#54564,0.350000000000003) ;
#19350 = CIRCLE('',#54565,0.500000000000003) ;
#19351 = CIRCLE('',#54568,4.95) ;
#19352 = CIRCLE('',#54569,5.1) ;
#19353 = CIRCLE('',#54572,0.350000000000003) ;
#19354 = CIRCLE('',#54573,0.500000000000003) ;
#19355 = CIRCLE('',#54576,4.95) ;
#19356 = CIRCLE('',#54577,5.1) ;
#19357 = CIRCLE('',#54580,0.350000000000003) ;
#19358 = CIRCLE('',#54581,0.500000000000003) ;
#19359 = CIRCLE('',#54584,4.95) ;
#19360 = CIRCLE('',#54585,5.1) ;
#19361 = CIRCLE('',#54588,0.350000000000003) ;
#19362 = CIRCLE('',#54589,0.500000000000003) ;
#19363 = CIRCLE('',#54592,4.95) ;
#19364 = CIRCLE('',#54593,5.1) ;
#19365 = CIRCLE('',#54596,0.350000000000003) ;
#19366 = CIRCLE('',#54597,0.500000000000003) ;
#19367 = CIRCLE('',#54600,4.95) ;
#19368 = CIRCLE('',#54601,5.1) ;
#19369 = CIRCLE('',#54604,0.350000000000003) ;
#19370 = CIRCLE('',#54605,0.500000000000003) ;
#19371 = CIRCLE('',#54608,4.95) ;
#19372 = CIRCLE('',#54609,5.1) ;
#19373 = CIRCLE('',#54612,0.350000000000003) ;
#19374 = CIRCLE('',#54613,0.500000000000003) ;
#19375 = CIRCLE('',#54616,4.95) ;
#19376 = CIRCLE('',#54617,5.1) ;
#19377 = CIRCLE('',#54620,0.350000000000003) ;
#19378 = CIRCLE('',#54621,0.500000000000003) ;
#19379 = CIRCLE('',#54624,4.95) ;
#19380 = CIRCLE('',#54625,5.1) ;
#19381 = CIRCLE('',#54628,0.350000000000003) ;
#19382 = CIRCLE('',#54629,0.500000000000003) ;
#19383 = CIRCLE('',#54632,4.95) ;
#19384 = CIRCLE('',#54633,5.1) ;
#19385 = CIRCLE('',#54636,0.350000000000003) ;
#19386 = CIRCLE('',#54637,0.500000000000003) ;
#19387 = CIRCLE('',#54640,4.95) ;
#19388 = CIRCLE('',#54641,5.1) ;
#19389 = CIRCLE('',#54644,0.500000000000003) ;
#19390 = CIRCLE('',#54645,0.350000000000003) ;
#19391 = CIRCLE('',#54648,5.1) ;
#19392 = CIRCLE('',#54649,4.95) ;
#19393 = CIRCLE('',#54652,0.500000000000003) ;
#19394 = CIRCLE('',#54653,0.350000000000003) ;
#19395 = CIRCLE('',#54656,5.1) ;
#19396 = CIRCLE('',#54657,4.95) ;
#19397 = CIRCLE('',#54660,0.500000000000003) ;
#19398 = CIRCLE('',#54661,0.350000000000003) ;
#19399 = CIRCLE('',#54664,5.1) ;
#19400 = CIRCLE('',#54665,4.95) ;
#19401 = CIRCLE('',#54668,0.500000000000003) ;
#19402 = CIRCLE('',#54669,0.350000000000003) ;
#19403 = CIRCLE('',#54672,5.1) ;
#19404 = CIRCLE('',#54673,4.95) ;
#19405 = CIRCLE('',#54676,0.500000000000003) ;
#19406 = CIRCLE('',#54677,0.350000000000003) ;
#19407 = CIRCLE('',#54680,5.1) ;
#19408 = CIRCLE('',#54681,4.95) ;
#19409 = CIRCLE('',#54684,0.500000000000003) ;
#19410 = CIRCLE('',#54685,0.350000000000003) ;
#19411 = CIRCLE('',#54688,5.1) ;
#19412 = CIRCLE('',#54689,4.95) ;
#19413 = CIRCLE('',#54692,0.500000000000003) ;
#19414 = CIRCLE('',#54693,0.350000000000003) ;
#19415 = CIRCLE('',#54696,5.1) ;
#19416 = CIRCLE('',#54697,4.95) ;
#19417 = CIRCLE('',#54700,0.500000000000003) ;
#19418 = CIRCLE('',#54701,0.350000000000003) ;
#19419 = CIRCLE('',#54704,5.1) ;
#19420 = CIRCLE('',#54705,4.95) ;
#19421 = CIRCLE('',#54708,0.500000000000003) ;
#19422 = CIRCLE('',#54709,0.350000000000003) ;
#19423 = CIRCLE('',#54712,5.1) ;
#19424 = CIRCLE('',#54713,4.95) ;
#19425 = CIRCLE('',#54716,0.500000000000003) ;
#19426 = CIRCLE('',#54717,0.350000000000003) ;
#19427 = CIRCLE('',#54721,0.500000000000003) ;
#19428 = CIRCLE('',#54724,5.1) ;
#19429 = CIRCLE('',#54727,0.500000000000003) ;
#19430 = CIRCLE('',#54730,5.1) ;
#19431 = CIRCLE('',#54733,0.500000000000003) ;
#19432 = CIRCLE('',#54736,5.1) ;
#19433 = CIRCLE('',#54739,0.500000000000003) ;
#19434 = CIRCLE('',#54742,5.1) ;
#19435 = CIRCLE('',#54745,0.500000000000003) ;
#19436 = CIRCLE('',#54748,5.1) ;
#19437 = CIRCLE('',#54751,0.500000000000003) ;
#19438 = CIRCLE('',#54754,5.1) ;
#19439 = CIRCLE('',#54757,0.500000000000003) ;
#19440 = CIRCLE('',#54760,5.1) ;
#19441 = CIRCLE('',#54763,0.500000000000003) ;
#19442 = CIRCLE('',#54766,5.1) ;
#19443 = CIRCLE('',#54769,0.500000000000003) ;
#19444 = CIRCLE('',#54772,5.1) ;
#19445 = CIRCLE('',#54775,0.500000000000003) ;
#19446 = CIRCLE('',#54778,5.1) ;
#19447 = CIRCLE('',#54780,4.95) ;
#19448 = CIRCLE('',#54782,4.95) ;
#19449 = CIRCLE('',#54784,4.95) ;
#19450 = CIRCLE('',#54786,4.95) ;
#19451 = CIRCLE('',#54788,4.95) ;
#19452 = CIRCLE('',#54790,4.95) ;
#19453 = CIRCLE('',#54792,4.95) ;
#19454 = CIRCLE('',#54794,4.95) ;
#19455 = CIRCLE('',#54796,4.95) ;
#19456 = CIRCLE('',#54798,4.95) ;
#19457 = CIRCLE('',#54800,4.95) ;
#19458 = CIRCLE('',#54802,4.95) ;
#19459 = CIRCLE('',#54804,4.95) ;
#19460 = CIRCLE('',#54806,4.95) ;
#19461 = CIRCLE('',#54808,4.95) ;
#19462 = CIRCLE('',#54810,4.95) ;
#19463 = CIRCLE('',#54812,4.95) ;
#19464 = CIRCLE('',#54814,4.95) ;
#19465 = CIRCLE('',#54816,4.95) ;
#19466 = CIRCLE('',#54817,4.95) ;
#19467 = CIRCLE('',#54819,0.15) ;
#19468 = CIRCLE('',#54820,4.95) ;
#19469 = CIRCLE('',#54823,0.15) ;
#19470 = CIRCLE('',#54824,4.95) ;
#19471 = CIRCLE('',#54825,4.95) ;
#19472 = CIRCLE('',#54826,4.95) ;
#19473 = CIRCLE('',#54827,4.95) ;
#19474 = CIRCLE('',#54828,4.95) ;
#19475 = CIRCLE('',#54829,4.95) ;
#19476 = CIRCLE('',#54830,4.95) ;
#19477 = CIRCLE('',#54831,4.95) ;
#19478 = CIRCLE('',#54832,4.95) ;
#19479 = CIRCLE('',#54833,4.95) ;
#19480 = CIRCLE('',#54834,4.95) ;
#19481 = CIRCLE('',#54835,4.95) ;
#19482 = CIRCLE('',#54836,4.95) ;
#19483 = CIRCLE('',#54837,4.95) ;
#19484 = CIRCLE('',#54838,4.95) ;
#19485 = CIRCLE('',#54839,4.95) ;
#19486 = CIRCLE('',#54840,4.95) ;
#19487 = CIRCLE('',#54841,4.95) ;
#19488 = CIRCLE('',#54842,4.95) ;
#19489 = CIRCLE('',#54843,4.95) ;
#19490 = CIRCLE('',#54844,4.95) ;
#19491 = CIRCLE('',#54845,4.95) ;
#19492 = CIRCLE('',#54846,4.95) ;
#19493 = CIRCLE('',#54847,4.95) ;
#19494 = CIRCLE('',#54848,4.95) ;
#19495 = CIRCLE('',#54849,4.95) ;
#19496 = CIRCLE('',#54850,4.95) ;
#19497 = CIRCLE('',#54851,4.95) ;
#19498 = CIRCLE('',#54852,4.95) ;
#19499 = CIRCLE('',#54853,4.95) ;
#19500 = CIRCLE('',#54854,4.95) ;
#19501 = CIRCLE('',#54855,4.95) ;
#19502 = CIRCLE('',#54856,4.95) ;
#19503 = CIRCLE('',#54857,4.95) ;
#19504 = CIRCLE('',#54858,4.95) ;
#19505 = CIRCLE('',#54859,4.95) ;
#19506 = CIRCLE('',#54860,4.95) ;
#19507 = CIRCLE('',#54861,4.95) ;
#19508 = CIRCLE('',#54862,4.95) ;
#19509 = CIRCLE('',#54863,4.95) ;
#19510 = CIRCLE('',#54864,4.95) ;
#19511 = CIRCLE('',#54866,0.350000000000003) ;
#19512 = CIRCLE('',#54868,0.350000000000003) ;
#19513 = CIRCLE('',#54870,0.350000000000003) ;
#19514 = CIRCLE('',#54872,0.350000000000003) ;
#19515 = CIRCLE('',#54874,0.350000000000003) ;
#19516 = CIRCLE('',#54876,0.350000000000003) ;
#19517 = CIRCLE('',#54878,0.350000000000003) ;
#19518 = CIRCLE('',#54880,0.350000000000003) ;
#19519 = CIRCLE('',#54882,0.350000000000003) ;
#19520 = CIRCLE('',#54884,0.350000000000003) ;
#19521 = CIRCLE('',#54886,0.350000000000003) ;
#19522 = CIRCLE('',#54888,0.350000000000003) ;
#19523 = CIRCLE('',#54890,0.350000000000003) ;
#19524 = CIRCLE('',#54892,0.350000000000003) ;
#19525 = CIRCLE('',#54894,0.350000000000003) ;
#19526 = CIRCLE('',#54896,0.350000000000003) ;
#19527 = CIRCLE('',#54898,0.350000000000003) ;
#19528 = CIRCLE('',#54900,0.350000000000003) ;
#19529 = CIRCLE('',#54902,0.350000000000003) ;
#19530 = CIRCLE('',#54904,0.350000000000003) ;
#19531 = CIRCLE('',#54906,5.1) ;
#19532 = CIRCLE('',#54951,5.1) ;
#19533 = CIRCLE('',#54954,0.500000000000003) ;
#19534 = CIRCLE('',#54957,5.1) ;
#19535 = CIRCLE('',#54960,0.500000000000003) ;
#19536 = CIRCLE('',#54963,5.1) ;
#19537 = CIRCLE('',#54966,0.500000000000003) ;
#19538 = CIRCLE('',#54969,5.1) ;
#19539 = CIRCLE('',#54972,0.500000000000003) ;
#19540 = CIRCLE('',#54975,5.1) ;
#19541 = CIRCLE('',#54978,0.500000000000003) ;
#19542 = CIRCLE('',#54981,5.1) ;
#19543 = CIRCLE('',#54984,0.500000000000003) ;
#19544 = CIRCLE('',#54987,5.1) ;
#19545 = CIRCLE('',#54990,0.500000000000003) ;
#19546 = CIRCLE('',#54993,5.1) ;
#19547 = CIRCLE('',#54996,0.500000000000003) ;
#19548 = CIRCLE('',#54999,5.1) ;
#19549 = CIRCLE('',#55002,0.500000000000003) ;
#19550 = CIRCLE('',#55004,0.500000000000003) ;
#19551 = CIRCLE('',#55048,1.67774999999999) ;
#19552 = CIRCLE('',#55053,1.67774999999999) ;
#19553 = CIRCLE('',#55060,1.9635) ;
#19554 = CIRCLE('',#55061,1.9635) ;
#19555 = CIRCLE('',#55062,1.9635) ;
#19556 = CIRCLE('',#55063,1.9635) ;
#19557 = CIRCLE('',#55064,1.9635) ;
#19558 = CIRCLE('',#55065,1.9635) ;
#19559 = CIRCLE('',#55067,1.67774999999999) ;
#19560 = CIRCLE('',#55069,1.67774999999999) ;
#19561 = VERTEX_POINT('',#69888) ;
#19562 = VERTEX_POINT('',#69890) ;
#19563 = VERTEX_POINT('',#69894) ;
#19564 = VERTEX_POINT('',#69896) ;
#19565 = VERTEX_POINT('',#69898) ;
#19566 = VERTEX_POINT('',#69900) ;
#19567 = VERTEX_POINT('',#69902) ;
#19568 = VERTEX_POINT('',#69904) ;
#19569 = VERTEX_POINT('',#69906) ;
#19570 = VERTEX_POINT('',#69908) ;
#19571 = VERTEX_POINT('',#69910) ;
#19572 = VERTEX_POINT('',#69912) ;
#19573 = VERTEX_POINT('',#69914) ;
#19574 = VERTEX_POINT('',#69916) ;
#19575 = VERTEX_POINT('',#69918) ;
#19576 = VERTEX_POINT('',#69920) ;
#19577 = VERTEX_POINT('',#69922) ;
#19578 = VERTEX_POINT('',#69924) ;
#19579 = VERTEX_POINT('',#69926) ;
#19580 = VERTEX_POINT('',#69928) ;
#19581 = VERTEX_POINT('',#69930) ;
#19582 = VERTEX_POINT('',#69932) ;
#19583 = VERTEX_POINT('',#69934) ;
#19584 = VERTEX_POINT('',#69936) ;
#19585 = VERTEX_POINT('',#69938) ;
#19586 = VERTEX_POINT('',#69940) ;
#19587 = VERTEX_POINT('',#69942) ;
#19588 = VERTEX_POINT('',#69944) ;
#19589 = VERTEX_POINT('',#69946) ;
#19590 = VERTEX_POINT('',#69948) ;
#19591 = VERTEX_POINT('',#69950) ;
#19592 = VERTEX_POINT('',#69952) ;
#19593 = VERTEX_POINT('',#69954) ;
#19594 = VERTEX_POINT('',#69956) ;
#19595 = VERTEX_POINT('',#69958) ;
#19596 = VERTEX_POINT('',#69960) ;
#19597 = VERTEX_POINT('',#69962) ;
#19598 = VERTEX_POINT('',#69964) ;
#19599 = VERTEX_POINT('',#69966) ;
#19600 = VERTEX_POINT('',#69968) ;
#19601 = VERTEX_POINT('',#69970) ;
#19602 = VERTEX_POINT('',#69972) ;
#19603 = VERTEX_POINT('',#69974) ;
#19604 = VERTEX_POINT('',#69976) ;
#19605 = VERTEX_POINT('',#69978) ;
#19606 = VERTEX_POINT('',#69980) ;
#19607 = VERTEX_POINT('',#69982) ;
#19608 = VERTEX_POINT('',#69984) ;
#19609 = VERTEX_POINT('',#69986) ;
#19610 = VERTEX_POINT('',#69988) ;
#19611 = VERTEX_POINT('',#69990) ;
#19612 = VERTEX_POINT('',#69992) ;
#19613 = VERTEX_POINT('',#69994) ;
#19614 = VERTEX_POINT('',#69996) ;
#19615 = VERTEX_POINT('',#69998) ;
#19616 = VERTEX_POINT('',#70000) ;
#19617 = VERTEX_POINT('',#70002) ;
#19618 = VERTEX_POINT('',#70004) ;
#19619 = VERTEX_POINT('',#70006) ;
#19620 = VERTEX_POINT('',#70008) ;
#19621 = VERTEX_POINT('',#70010) ;
#19622 = VERTEX_POINT('',#70012) ;
#19623 = VERTEX_POINT('',#70014) ;
#19624 = VERTEX_POINT('',#70016) ;
#19625 = VERTEX_POINT('',#70018) ;
#19626 = VERTEX_POINT('',#70020) ;
#19627 = VERTEX_POINT('',#70022) ;
#19628 = VERTEX_POINT('',#70024) ;
#19629 = VERTEX_POINT('',#70026) ;
#19630 = VERTEX_POINT('',#70028) ;
#19631 = VERTEX_POINT('',#70030) ;
#19632 = VERTEX_POINT('',#70032) ;
#19633 = VERTEX_POINT('',#70034) ;
#19634 = VERTEX_POINT('',#70036) ;
#19635 = VERTEX_POINT('',#70038) ;
#19636 = VERTEX_POINT('',#70040) ;
#19637 = VERTEX_POINT('',#70042) ;
#19638 = VERTEX_POINT('',#70044) ;
#19639 = VERTEX_POINT('',#70046) ;
#19640 = VERTEX_POINT('',#70048) ;
#19641 = VERTEX_POINT('',#70050) ;
#19642 = VERTEX_POINT('',#70052) ;
#19643 = VERTEX_POINT('',#70054) ;
#19644 = VERTEX_POINT('',#70059) ;
#19645 = VERTEX_POINT('',#70060) ;
#19646 = VERTEX_POINT('',#70062) ;
#19647 = VERTEX_POINT('',#70064) ;
#19648 = VERTEX_POINT('',#70068) ;
#19649 = VERTEX_POINT('',#70069) ;
#19650 = VERTEX_POINT('',#70071) ;
#19651 = VERTEX_POINT('',#70073) ;
#19652 = VERTEX_POINT('',#70077) ;
#19653 = VERTEX_POINT('',#70078) ;
#19654 = VERTEX_POINT('',#70083) ;
#19655 = VERTEX_POINT('',#70088) ;
#19656 = VERTEX_POINT('',#70089) ;
#19657 = VERTEX_POINT('',#70092) ;
#19658 = VERTEX_POINT('',#70096) ;
#19659 = VERTEX_POINT('',#70097) ;
#19660 = VERTEX_POINT('',#70099) ;
#19661 = VERTEX_POINT('',#70101) ;
#19662 = VERTEX_POINT('',#70105) ;
#19663 = VERTEX_POINT('',#70106) ;
#19664 = VERTEX_POINT('',#70111) ;
#19665 = VERTEX_POINT('',#70116) ;
#19666 = VERTEX_POINT('',#70117) ;
#19667 = VERTEX_POINT('',#70120) ;
#19668 = VERTEX_POINT('',#70124) ;
#19669 = VERTEX_POINT('',#70125) ;
#19670 = VERTEX_POINT('',#70127) ;
#19671 = VERTEX_POINT('',#70129) ;
#19672 = VERTEX_POINT('',#70133) ;
#19673 = VERTEX_POINT('',#70134) ;
#19674 = VERTEX_POINT('',#70139) ;
#19675 = VERTEX_POINT('',#70144) ;
#19676 = VERTEX_POINT('',#70145) ;
#19677 = VERTEX_POINT('',#70148) ;
#19678 = VERTEX_POINT('',#70152) ;
#19679 = VERTEX_POINT('',#70153) ;
#19680 = VERTEX_POINT('',#70155) ;
#19681 = VERTEX_POINT('',#70157) ;
#19682 = VERTEX_POINT('',#70161) ;
#19683 = VERTEX_POINT('',#70166) ;
#19684 = VERTEX_POINT('',#70187) ;
#19685 = VERTEX_POINT('',#70189) ;
#19686 = VERTEX_POINT('',#70193) ;
#19687 = VERTEX_POINT('',#70197) ;
#19688 = VERTEX_POINT('',#70201) ;
#19689 = VERTEX_POINT('',#70205) ;
#19690 = VERTEX_POINT('',#70209) ;
#19691 = VERTEX_POINT('',#70213) ;
#19692 = VERTEX_POINT('',#70217) ;
#19693 = VERTEX_POINT('',#70221) ;
#19694 = VERTEX_POINT('',#70225) ;
#19695 = VERTEX_POINT('',#70229) ;
#19696 = VERTEX_POINT('',#70233) ;
#19697 = VERTEX_POINT('',#70238) ;
#19698 = VERTEX_POINT('',#70240) ;
#19699 = VERTEX_POINT('',#70244) ;
#19700 = VERTEX_POINT('',#70246) ;
#19701 = VERTEX_POINT('',#70250) ;
#19702 = VERTEX_POINT('',#70252) ;
#19703 = VERTEX_POINT('',#70258) ;
#19704 = VERTEX_POINT('',#70260) ;
#19705 = VERTEX_POINT('',#70264) ;
#19706 = VERTEX_POINT('',#70266) ;
#19707 = VERTEX_POINT('',#70536) ;
#19708 = VERTEX_POINT('',#70538) ;
#19709 = VERTEX_POINT('',#70542) ;
#19710 = VERTEX_POINT('',#70544) ;
#19711 = VERTEX_POINT('',#70550) ;
#19712 = VERTEX_POINT('',#70552) ;
#19713 = VERTEX_POINT('',#70556) ;
#19714 = VERTEX_POINT('',#70558) ;
#19715 = VERTEX_POINT('',#70755) ;
#19716 = VERTEX_POINT('',#70757) ;
#19717 = VERTEX_POINT('',#70761) ;
#19718 = VERTEX_POINT('',#70763) ;
#19719 = VERTEX_POINT('',#70769) ;
#19720 = VERTEX_POINT('',#70771) ;
#19721 = VERTEX_POINT('',#70775) ;
#19722 = VERTEX_POINT('',#70777) ;
#19723 = VERTEX_POINT('',#70974) ;
#19724 = VERTEX_POINT('',#70976) ;
#19725 = VERTEX_POINT('',#70980) ;
#19726 = VERTEX_POINT('',#70982) ;
#19727 = VERTEX_POINT('',#70988) ;
#19728 = VERTEX_POINT('',#70990) ;
#19729 = VERTEX_POINT('',#70994) ;
#19730 = VERTEX_POINT('',#70996) ;
#19731 = VERTEX_POINT('',#71074) ;
#19732 = VERTEX_POINT('',#71198) ;
#19733 = VERTEX_POINT('',#71200) ;
#19734 = VERTEX_POINT('',#71204) ;
#19735 = VERTEX_POINT('',#71206) ;
#19736 = VERTEX_POINT('',#71212) ;
#19737 = VERTEX_POINT('',#71214) ;
#19738 = VERTEX_POINT('',#71218) ;
#19739 = VERTEX_POINT('',#71220) ;
#19740 = VERTEX_POINT('',#71426) ;
#19741 = VERTEX_POINT('',#71428) ;
#19742 = VERTEX_POINT('',#71432) ;
#19743 = VERTEX_POINT('',#71434) ;
#19744 = VERTEX_POINT('',#71440) ;
#19745 = VERTEX_POINT('',#71442) ;
#19746 = VERTEX_POINT('',#71446) ;
#19747 = VERTEX_POINT('',#71448) ;
#19748 = VERTEX_POINT('',#71645) ;
#19749 = VERTEX_POINT('',#71647) ;
#19750 = VERTEX_POINT('',#71651) ;
#19751 = VERTEX_POINT('',#71653) ;
#19752 = VERTEX_POINT('',#71659) ;
#19753 = VERTEX_POINT('',#71661) ;
#19754 = VERTEX_POINT('',#71665) ;
#19755 = VERTEX_POINT('',#71667) ;
#19756 = VERTEX_POINT('',#71864) ;
#19757 = VERTEX_POINT('',#71866) ;
#19758 = VERTEX_POINT('',#71870) ;
#19759 = VERTEX_POINT('',#71872) ;
#19760 = VERTEX_POINT('',#71878) ;
#19761 = VERTEX_POINT('',#71880) ;
#19762 = VERTEX_POINT('',#71884) ;
#19763 = VERTEX_POINT('',#71886) ;
#19764 = VERTEX_POINT('',#72071) ;
#19765 = VERTEX_POINT('',#72073) ;
#19766 = VERTEX_POINT('',#72077) ;
#19767 = VERTEX_POINT('',#72079) ;
#19768 = VERTEX_POINT('',#72085) ;
#19769 = VERTEX_POINT('',#72087) ;
#19770 = VERTEX_POINT('',#72091) ;
#19771 = VERTEX_POINT('',#72093) ;
#19772 = VERTEX_POINT('',#72202) ;
#19773 = VERTEX_POINT('',#72204) ;
#19774 = VERTEX_POINT('',#72208) ;
#19775 = VERTEX_POINT('',#72210) ;
#19776 = VERTEX_POINT('',#72216) ;
#19777 = VERTEX_POINT('',#72218) ;
#19778 = VERTEX_POINT('',#72402) ;
#19779 = VERTEX_POINT('',#72419) ;
#19780 = VERTEX_POINT('',#72630) ;
#19781 = VERTEX_POINT('',#72645) ;
#19782 = VERTEX_POINT('',#72652) ;
#19783 = VERTEX_POINT('',#72661) ;
#19784 = VERTEX_POINT('',#72680) ;
#19785 = VERTEX_POINT('',#72697) ;
#19786 = VERTEX_POINT('',#72704) ;
#19787 = VERTEX_POINT('',#72713) ;
#19788 = VERTEX_POINT('',#72728) ;
#19789 = VERTEX_POINT('',#72735) ;
#19790 = VERTEX_POINT('',#72940) ;
#19791 = VERTEX_POINT('',#72955) ;
#19792 = VERTEX_POINT('',#72974) ;
#19793 = VERTEX_POINT('',#72991) ;
#19794 = VERTEX_POINT('',#72998) ;
#19795 = VERTEX_POINT('',#73007) ;
#19796 = VERTEX_POINT('',#73022) ;
#19797 = VERTEX_POINT('',#73029) ;
#19798 = VERTEX_POINT('',#73231) ;
#19799 = VERTEX_POINT('',#73246) ;
#19800 = VERTEX_POINT('',#73265) ;
#19801 = VERTEX_POINT('',#73282) ;
#19802 = VERTEX_POINT('',#73289) ;
#19803 = VERTEX_POINT('',#73298) ;
#19804 = VERTEX_POINT('',#73313) ;
#19805 = VERTEX_POINT('',#73320) ;
#19806 = VERTEX_POINT('',#73434) ;
#19807 = VERTEX_POINT('',#73449) ;
#19808 = VERTEX_POINT('',#73468) ;
#19809 = VERTEX_POINT('',#73485) ;
#19810 = VERTEX_POINT('',#73492) ;
#19811 = VERTEX_POINT('',#73501) ;
#19812 = VERTEX_POINT('',#73516) ;
#19813 = VERTEX_POINT('',#73523) ;
#19814 = VERTEX_POINT('',#73710) ;
#19815 = VERTEX_POINT('',#73725) ;
#19816 = VERTEX_POINT('',#73744) ;
#19817 = VERTEX_POINT('',#73761) ;
#19818 = VERTEX_POINT('',#73768) ;
#19819 = VERTEX_POINT('',#73777) ;
#19820 = VERTEX_POINT('',#73792) ;
#19821 = VERTEX_POINT('',#73799) ;
#19822 = VERTEX_POINT('',#74001) ;
#19823 = VERTEX_POINT('',#74016) ;
#19824 = VERTEX_POINT('',#74035) ;
#19825 = VERTEX_POINT('',#74052) ;
#19826 = VERTEX_POINT('',#74059) ;
#19827 = VERTEX_POINT('',#74068) ;
#19828 = VERTEX_POINT('',#74083) ;
#19829 = VERTEX_POINT('',#74090) ;
#19830 = VERTEX_POINT('',#74295) ;
#19831 = VERTEX_POINT('',#74310) ;
#19832 = VERTEX_POINT('',#74329) ;
#19833 = VERTEX_POINT('',#74346) ;
#19834 = VERTEX_POINT('',#74353) ;
#19835 = VERTEX_POINT('',#74362) ;
#19836 = VERTEX_POINT('',#74377) ;
#19837 = VERTEX_POINT('',#74384) ;
#19838 = VERTEX_POINT('',#74571) ;
#19839 = VERTEX_POINT('',#74586) ;
#19840 = VERTEX_POINT('',#74605) ;
#19841 = VERTEX_POINT('',#74622) ;
#19842 = VERTEX_POINT('',#74629) ;
#19843 = VERTEX_POINT('',#74638) ;
#19844 = VERTEX_POINT('',#74653) ;
#19845 = VERTEX_POINT('',#74660) ;
#19846 = VERTEX_POINT('',#74774) ;
#19847 = VERTEX_POINT('',#74789) ;
#19848 = VERTEX_POINT('',#74808) ;
#19849 = VERTEX_POINT('',#74825) ;
#19850 = VERTEX_POINT('',#74832) ;
#19851 = VERTEX_POINT('',#74841) ;
#19852 = VERTEX_POINT('',#74856) ;
#19853 = VERTEX_POINT('',#74863) ;
#19854 = VERTEX_POINT('',#75053) ;
#19855 = VERTEX_POINT('',#75068) ;
#19856 = VERTEX_POINT('',#75085) ;
#19857 = VERTEX_POINT('',#75092) ;
#19858 = VERTEX_POINT('',#75141) ;
#19859 = VERTEX_POINT('',#75145) ;
#19860 = VERTEX_POINT('',#75147) ;
#19861 = VERTEX_POINT('',#75151) ;
#19862 = VERTEX_POINT('',#75153) ;
#19863 = VERTEX_POINT('',#75155) ;
#19864 = VERTEX_POINT('',#75157) ;
#19865 = VERTEX_POINT('',#75159) ;
#19866 = VERTEX_POINT('',#75161) ;
#19867 = VERTEX_POINT('',#75163) ;
#19868 = VERTEX_POINT('',#75165) ;
#19869 = VERTEX_POINT('',#75167) ;
#19870 = VERTEX_POINT('',#75169) ;
#19871 = VERTEX_POINT('',#75171) ;
#19872 = VERTEX_POINT('',#75173) ;
#19873 = VERTEX_POINT('',#75175) ;
#19874 = VERTEX_POINT('',#75177) ;
#19875 = VERTEX_POINT('',#75179) ;
#19876 = VERTEX_POINT('',#75181) ;
#19877 = VERTEX_POINT('',#75183) ;
#19878 = VERTEX_POINT('',#75185) ;
#19879 = VERTEX_POINT('',#75187) ;
#19880 = VERTEX_POINT('',#75189) ;
#19881 = VERTEX_POINT('',#75191) ;
#19882 = VERTEX_POINT('',#75193) ;
#19883 = VERTEX_POINT('',#75195) ;
#19884 = VERTEX_POINT('',#75199) ;
#19885 = VERTEX_POINT('',#75210) ;
#19886 = VERTEX_POINT('',#75212) ;
#19887 = VERTEX_POINT('',#75219) ;
#19888 = VERTEX_POINT('',#75226) ;
#19889 = VERTEX_POINT('',#75249) ;
#19890 = VERTEX_POINT('',#75255) ;
#19891 = VERTEX_POINT('',#75257) ;
#19892 = VERTEX_POINT('',#75266) ;
#19893 = VERTEX_POINT('',#75268) ;
#19894 = VERTEX_POINT('',#75274) ;
#19895 = VERTEX_POINT('',#75336) ;
#19896 = VERTEX_POINT('',#75337) ;
#19897 = VERTEX_POINT('',#75339) ;
#19898 = VERTEX_POINT('',#75344) ;
#19899 = VERTEX_POINT('',#75377) ;
#19900 = VERTEX_POINT('',#75378) ;
#19901 = VERTEX_POINT('',#75380) ;
#19902 = VERTEX_POINT('',#75382) ;
#19903 = VERTEX_POINT('',#75386) ;
#19904 = VERTEX_POINT('',#75387) ;
#19905 = VERTEX_POINT('',#75426) ;
#19906 = VERTEX_POINT('',#75427) ;
#19907 = VERTEX_POINT('',#75499) ;
#19908 = VERTEX_POINT('',#75501) ;
#19909 = VERTEX_POINT('',#75514) ;
#19910 = VERTEX_POINT('',#75537) ;
#19911 = VERTEX_POINT('',#75560) ;
#19912 = VERTEX_POINT('',#75562) ;
#19913 = VERTEX_POINT('',#75585) ;
#19914 = VERTEX_POINT('',#75586) ;
#19915 = VERTEX_POINT('',#75588) ;
#19916 = VERTEX_POINT('',#75593) ;
#19917 = VERTEX_POINT('',#75629) ;
#19918 = VERTEX_POINT('',#75636) ;
#19919 = VERTEX_POINT('',#75645) ;
#19920 = VERTEX_POINT('',#75646) ;
#19921 = VERTEX_POINT('',#75670) ;
#19922 = VERTEX_POINT('',#75672) ;
#19923 = VERTEX_POINT('',#75695) ;
#19924 = VERTEX_POINT('',#75696) ;
#19925 = VERTEX_POINT('',#75736) ;
#19926 = VERTEX_POINT('',#75743) ;
#19927 = VERTEX_POINT('',#75752) ;
#19928 = VERTEX_POINT('',#75753) ;
#19929 = VERTEX_POINT('',#75787) ;
#19930 = VERTEX_POINT('',#75789) ;
#19931 = VERTEX_POINT('',#75793) ;
#19932 = VERTEX_POINT('',#75810) ;
#19933 = VERTEX_POINT('',#75827) ;
#19934 = VERTEX_POINT('',#75834) ;
#19935 = VERTEX_POINT('',#75835) ;
#19936 = VERTEX_POINT('',#75837) ;
#19937 = VERTEX_POINT('',#75839) ;
#19938 = VERTEX_POINT('',#75841) ;
#19939 = VERTEX_POINT('',#75843) ;
#19940 = VERTEX_POINT('',#75845) ;
#19941 = VERTEX_POINT('',#75847) ;
#19942 = VERTEX_POINT('',#75849) ;
#19943 = VERTEX_POINT('',#75851) ;
#19944 = VERTEX_POINT('',#75853) ;
#19945 = VERTEX_POINT('',#75859) ;
#19946 = VERTEX_POINT('',#75861) ;
#19947 = VERTEX_POINT('',#75863) ;
#19948 = VERTEX_POINT('',#75871) ;
#19949 = VERTEX_POINT('',#75877) ;
#19950 = VERTEX_POINT('',#75883) ;
#19951 = VERTEX_POINT('',#75885) ;
#19952 = VERTEX_POINT('',#75887) ;
#19953 = VERTEX_POINT('',#75889) ;
#19954 = VERTEX_POINT('',#75892) ;
#19955 = VERTEX_POINT('',#75893) ;
#19956 = VERTEX_POINT('',#75895) ;
#19957 = VERTEX_POINT('',#75897) ;
#19958 = VERTEX_POINT('',#75899) ;
#19959 = VERTEX_POINT('',#75906) ;
#19960 = VERTEX_POINT('',#75908) ;
#19961 = VERTEX_POINT('',#75914) ;
#19962 = VERTEX_POINT('',#75922) ;
#19963 = VERTEX_POINT('',#75923) ;
#19964 = VERTEX_POINT('',#75930) ;
#19965 = VERTEX_POINT('',#75932) ;
#19966 = VERTEX_POINT('',#75934) ;
#19967 = VERTEX_POINT('',#75942) ;
#19968 = VERTEX_POINT('',#75944) ;
#19969 = VERTEX_POINT('',#75950) ;
#19970 = VERTEX_POINT('',#75952) ;
#19971 = VERTEX_POINT('',#75954) ;
#19972 = VERTEX_POINT('',#75956) ;
#19973 = VERTEX_POINT('',#75959) ;
#19974 = VERTEX_POINT('',#75962) ;
#19975 = VERTEX_POINT('',#75964) ;
#19976 = VERTEX_POINT('',#75987) ;
#19977 = VERTEX_POINT('',#76010) ;
#19978 = VERTEX_POINT('',#76046) ;
#19979 = VERTEX_POINT('',#76055) ;
#19980 = VERTEX_POINT('',#76083) ;
#19981 = VERTEX_POINT('',#76110) ;
#19982 = VERTEX_POINT('',#76164) ;
#19983 = VERTEX_POINT('',#76166) ;
#19984 = VERTEX_POINT('',#76182) ;
#19985 = VERTEX_POINT('',#76196) ;
#19986 = VERTEX_POINT('',#76200) ;
#19987 = VERTEX_POINT('',#76204) ;
#19988 = VERTEX_POINT('',#76208) ;
#19989 = VERTEX_POINT('',#76212) ;
#19990 = VERTEX_POINT('',#76214) ;
#19991 = VERTEX_POINT('',#76218) ;
#19992 = VERTEX_POINT('',#76237) ;
#19993 = VERTEX_POINT('',#76273) ;
#19994 = VERTEX_POINT('',#76296) ;
#19995 = VERTEX_POINT('',#76319) ;
#19996 = VERTEX_POINT('',#76347) ;
#19997 = VERTEX_POINT('',#76383) ;
#19998 = VERTEX_POINT('',#76430) ;
#19999 = VERTEX_POINT('',#76440) ;
#20000 = VERTEX_POINT('',#76463) ;
#20001 = VERTEX_POINT('',#76491) ;
#20002 = VERTEX_POINT('',#76523) ;
#20003 = VERTEX_POINT('',#76546) ;
#20004 = VERTEX_POINT('',#76569) ;
#20005 = VERTEX_POINT('',#76592) ;
#20006 = VERTEX_POINT('',#76615) ;
#20007 = VERTEX_POINT('',#76619) ;
#20008 = VERTEX_POINT('',#76623) ;
#20009 = VERTEX_POINT('',#76672) ;
#20010 = VERTEX_POINT('',#76674) ;
#20011 = VERTEX_POINT('',#76682) ;
#20012 = VERTEX_POINT('',#76705) ;
#20013 = VERTEX_POINT('',#76720) ;
#20014 = VERTEX_POINT('',#76722) ;
#20015 = VERTEX_POINT('',#76725) ;
#20016 = VERTEX_POINT('',#76758) ;
#20017 = VERTEX_POINT('',#76769) ;
#20018 = VERTEX_POINT('',#76778) ;
#20019 = VERTEX_POINT('',#76782) ;
#20020 = VERTEX_POINT('',#76786) ;
#20021 = VERTEX_POINT('',#76790) ;
#20022 = VERTEX_POINT('',#76794) ;
#20023 = VERTEX_POINT('',#76809) ;
#20024 = VERTEX_POINT('',#76850) ;
#20025 = VERTEX_POINT('',#76852) ;
#20026 = VERTEX_POINT('',#76860) ;
#20027 = VERTEX_POINT('',#76861) ;
#20028 = VERTEX_POINT('',#76863) ;
#20029 = VERTEX_POINT('',#76913) ;
#20030 = VERTEX_POINT('',#76915) ;
#20031 = VERTEX_POINT('',#76924) ;
#20032 = VERTEX_POINT('',#76925) ;
#20033 = VERTEX_POINT('',#76927) ;
#20034 = VERTEX_POINT('',#76929) ;
#20035 = VERTEX_POINT('',#76966) ;
#20036 = VERTEX_POINT('',#76967) ;
#20037 = VERTEX_POINT('',#76969) ;
#20038 = VERTEX_POINT('',#76971) ;
#20039 = VERTEX_POINT('',#77036) ;
#20040 = VERTEX_POINT('',#77037) ;
#20041 = VERTEX_POINT('',#77074) ;
#20042 = VERTEX_POINT('',#77118) ;
#20043 = VERTEX_POINT('',#77120) ;
#20044 = VERTEX_POINT('',#77143) ;
#20045 = VERTEX_POINT('',#77144) ;
#20046 = VERTEX_POINT('',#77149) ;
#20047 = VERTEX_POINT('',#77150) ;
#20048 = VERTEX_POINT('',#77185) ;
#20049 = VERTEX_POINT('',#77208) ;
#20050 = VERTEX_POINT('',#77233) ;
#20051 = VERTEX_POINT('',#77248) ;
#20052 = VERTEX_POINT('',#77250) ;
#20053 = VERTEX_POINT('',#77272) ;
#20054 = VERTEX_POINT('',#77274) ;
#20055 = VERTEX_POINT('',#77303) ;
#20056 = VERTEX_POINT('',#77305) ;
#20057 = VERTEX_POINT('',#77332) ;
#20058 = VERTEX_POINT('',#77355) ;
#20059 = VERTEX_POINT('',#77359) ;
#20060 = VERTEX_POINT('',#77392) ;
#20061 = VERTEX_POINT('',#77393) ;
#20062 = VERTEX_POINT('',#77427) ;
#20063 = VERTEX_POINT('',#77429) ;
#20064 = VERTEX_POINT('',#77460) ;
#20065 = VERTEX_POINT('',#77461) ;
#20066 = VERTEX_POINT('',#77507) ;
#20067 = VERTEX_POINT('',#77508) ;
#20068 = VERTEX_POINT('',#77510) ;
#20069 = VERTEX_POINT('',#77517) ;
#20070 = VERTEX_POINT('',#77549) ;
#20071 = VERTEX_POINT('',#77575) ;
#20072 = VERTEX_POINT('',#77579) ;
#20073 = VERTEX_POINT('',#77617) ;
#20074 = VERTEX_POINT('',#77646) ;
#20075 = VERTEX_POINT('',#77672) ;
#20076 = VERTEX_POINT('',#77673) ;
#20077 = VERTEX_POINT('',#77710) ;
#20078 = VERTEX_POINT('',#77711) ;
#20079 = VERTEX_POINT('',#77713) ;
#20080 = VERTEX_POINT('',#77741) ;
#20081 = VERTEX_POINT('',#77742) ;
#20082 = VERTEX_POINT('',#77744) ;
#20083 = VERTEX_POINT('',#77746) ;
#20084 = VERTEX_POINT('',#77764) ;
#20085 = VERTEX_POINT('',#77765) ;
#20086 = VERTEX_POINT('',#77767) ;
#20087 = VERTEX_POINT('',#77769) ;
#20088 = VERTEX_POINT('',#77771) ;
#20089 = VERTEX_POINT('',#77797) ;
#20090 = VERTEX_POINT('',#77802) ;
#20091 = VERTEX_POINT('',#77831) ;
#20092 = VERTEX_POINT('',#77833) ;
#20093 = VERTEX_POINT('',#77837) ;
#20094 = VERTEX_POINT('',#77838) ;
#20095 = VERTEX_POINT('',#77877) ;
#20096 = VERTEX_POINT('',#77885) ;
#20097 = VERTEX_POINT('',#77957) ;
#20098 = VERTEX_POINT('',#77958) ;
#20099 = VERTEX_POINT('',#77960) ;
#20100 = VERTEX_POINT('',#77967) ;
#20101 = VERTEX_POINT('',#77969) ;
#20102 = VERTEX_POINT('',#77977) ;
#20103 = VERTEX_POINT('',#78020) ;
#20104 = VERTEX_POINT('',#78025) ;
#20105 = VERTEX_POINT('',#78051) ;
#20106 = VERTEX_POINT('',#78053) ;
#20107 = VERTEX_POINT('',#78057) ;
#20108 = VERTEX_POINT('',#78058) ;
#20109 = VERTEX_POINT('',#78092) ;
#20110 = VERTEX_POINT('',#78099) ;
#20111 = VERTEX_POINT('',#78180) ;
#20112 = VERTEX_POINT('',#78181) ;
#20113 = VERTEX_POINT('',#78183) ;
#20114 = VERTEX_POINT('',#78185) ;
#20115 = VERTEX_POINT('',#78191) ;
#20116 = VERTEX_POINT('',#78197) ;
#20117 = VERTEX_POINT('',#78203) ;
#20118 = VERTEX_POINT('',#78211) ;
#20119 = VERTEX_POINT('',#78213) ;
#20120 = VERTEX_POINT('',#78215) ;
#20121 = VERTEX_POINT('',#78221) ;
#20122 = VERTEX_POINT('',#78224) ;
#20123 = VERTEX_POINT('',#78225) ;
#20124 = VERTEX_POINT('',#78233) ;
#20125 = VERTEX_POINT('',#78238) ;
#20126 = VERTEX_POINT('',#78244) ;
#20127 = VERTEX_POINT('',#78246) ;
#20128 = VERTEX_POINT('',#78254) ;
#20129 = VERTEX_POINT('',#78259) ;
#20130 = VERTEX_POINT('',#78303) ;
#20131 = VERTEX_POINT('',#78305) ;
#20132 = VERTEX_POINT('',#78315) ;
#20133 = VERTEX_POINT('',#78316) ;
#20134 = VERTEX_POINT('',#78318) ;
#20135 = VERTEX_POINT('',#78362) ;
#20136 = VERTEX_POINT('',#78364) ;
#20137 = VERTEX_POINT('',#78392) ;
#20138 = VERTEX_POINT('',#78394) ;
#20139 = VERTEX_POINT('',#78402) ;
#20140 = VERTEX_POINT('',#78403) ;
#20141 = VERTEX_POINT('',#78405) ;
#20142 = VERTEX_POINT('',#78419) ;
#20143 = VERTEX_POINT('',#78420) ;
#20144 = VERTEX_POINT('',#78422) ;
#20145 = VERTEX_POINT('',#78488) ;
#20146 = VERTEX_POINT('',#78490) ;
#20147 = VERTEX_POINT('',#78500) ;
#20148 = VERTEX_POINT('',#78501) ;
#20149 = VERTEX_POINT('',#78503) ;
#20150 = VERTEX_POINT('',#78505) ;
#20151 = VERTEX_POINT('',#78676) ;
#20152 = VERTEX_POINT('',#78677) ;
#20153 = VERTEX_POINT('',#78690) ;
#20154 = VERTEX_POINT('',#78692) ;
#20155 = VERTEX_POINT('',#78767) ;
#20156 = VERTEX_POINT('',#78772) ;
#20157 = VERTEX_POINT('',#78897) ;
#20158 = VERTEX_POINT('',#78901) ;
#20159 = VERTEX_POINT('',#78939) ;
#20160 = VERTEX_POINT('',#78973) ;
#20161 = VERTEX_POINT('',#79101) ;
#20162 = VERTEX_POINT('',#79248) ;
#20163 = VERTEX_POINT('',#79249) ;
#20164 = VERTEX_POINT('',#79260) ;
#20165 = VERTEX_POINT('',#79275) ;
#20166 = VERTEX_POINT('',#79364) ;
#20167 = VERTEX_POINT('',#79365) ;
#20168 = VERTEX_POINT('',#79372) ;
#20169 = VERTEX_POINT('',#79398) ;
#20170 = VERTEX_POINT('',#79471) ;
#20171 = VERTEX_POINT('',#79482) ;
#20172 = VERTEX_POINT('',#79542) ;
#20173 = VERTEX_POINT('',#79544) ;
#20174 = VERTEX_POINT('',#79548) ;
#20175 = VERTEX_POINT('',#79550) ;
#20176 = VERTEX_POINT('',#79606) ;
#20177 = VERTEX_POINT('',#79613) ;
#20178 = VERTEX_POINT('',#79727) ;
#20179 = VERTEX_POINT('',#79729) ;
#20180 = VERTEX_POINT('',#79733) ;
#20181 = VERTEX_POINT('',#79737) ;
#20182 = VERTEX_POINT('',#79750) ;
#20183 = VERTEX_POINT('',#79759) ;
#20184 = VERTEX_POINT('',#79760) ;
#20185 = VERTEX_POINT('',#79762) ;
#20186 = VERTEX_POINT('',#79771) ;
#20187 = VERTEX_POINT('',#79782) ;
#20188 = VERTEX_POINT('',#79793) ;
#20189 = VERTEX_POINT('',#79802) ;
#20190 = VERTEX_POINT('',#79804) ;
#20191 = VERTEX_POINT('',#79806) ;
#20192 = VERTEX_POINT('',#79808) ;
#20193 = VERTEX_POINT('',#79815) ;
#20194 = VERTEX_POINT('',#79824) ;
#20195 = VERTEX_POINT('',#79833) ;
#20196 = VERTEX_POINT('',#79842) ;
#20197 = VERTEX_POINT('',#79849) ;
#20198 = VERTEX_POINT('',#79858) ;
#20199 = VERTEX_POINT('',#79865) ;
#20200 = VERTEX_POINT('',#79867) ;
#20201 = VERTEX_POINT('',#79869) ;
#20202 = VERTEX_POINT('',#79873) ;
#20203 = VERTEX_POINT('',#79875) ;
#20204 = VERTEX_POINT('',#79900) ;
#20205 = VERTEX_POINT('',#79904) ;
#20206 = VERTEX_POINT('',#79968) ;
#20207 = VERTEX_POINT('',#80059) ;
#20208 = VERTEX_POINT('',#80149) ;
#20209 = VERTEX_POINT('',#80150) ;
#20210 = VERTEX_POINT('',#80222) ;
#20211 = VERTEX_POINT('',#80264) ;
#20212 = VERTEX_POINT('',#80265) ;
#20213 = VERTEX_POINT('',#80332) ;
#20214 = VERTEX_POINT('',#80336) ;
#20215 = VERTEX_POINT('',#80340) ;
#20216 = VERTEX_POINT('',#80385) ;
#20217 = VERTEX_POINT('',#80458) ;
#20218 = VERTEX_POINT('',#80573) ;
#20219 = VERTEX_POINT('',#80667) ;
#20220 = VERTEX_POINT('',#80728) ;
#20221 = VERTEX_POINT('',#80840) ;
#20222 = VERTEX_POINT('',#80842) ;
#20223 = VERTEX_POINT('',#80860) ;
#20224 = VERTEX_POINT('',#80869) ;
#20225 = VERTEX_POINT('',#80873) ;
#20226 = VERTEX_POINT('',#80877) ;
#20227 = VERTEX_POINT('',#80890) ;
#20228 = VERTEX_POINT('',#80908) ;
#20229 = VERTEX_POINT('',#80926) ;
#20230 = VERTEX_POINT('',#80972) ;
#20231 = VERTEX_POINT('',#80981) ;
#20232 = VERTEX_POINT('',#81024) ;
#20233 = VERTEX_POINT('',#81025) ;
#20234 = VERTEX_POINT('',#81048) ;
#20235 = VERTEX_POINT('',#81072) ;
#20236 = VERTEX_POINT('',#81089) ;
#20237 = VERTEX_POINT('',#81093) ;
#20238 = VERTEX_POINT('',#81094) ;
#20239 = VERTEX_POINT('',#81161) ;
#20240 = VERTEX_POINT('',#81205) ;
#20241 = VERTEX_POINT('',#81283) ;
#20242 = VERTEX_POINT('',#81336) ;
#20243 = VERTEX_POINT('',#81518) ;
#20244 = VERTEX_POINT('',#81519) ;
#20245 = VERTEX_POINT('',#81521) ;
#20246 = VERTEX_POINT('',#81523) ;
#20247 = VERTEX_POINT('',#81527) ;
#20248 = VERTEX_POINT('',#81529) ;
#20249 = VERTEX_POINT('',#81536) ;
#20250 = VERTEX_POINT('',#81538) ;
#20251 = VERTEX_POINT('',#81542) ;
#20252 = VERTEX_POINT('',#81547) ;
#20253 = VERTEX_POINT('',#81548) ;
#20254 = VERTEX_POINT('',#81550) ;
#20255 = VERTEX_POINT('',#81552) ;
#20256 = VERTEX_POINT('',#81556) ;
#20257 = VERTEX_POINT('',#81558) ;
#20258 = VERTEX_POINT('',#81562) ;
#20259 = VERTEX_POINT('',#81564) ;
#20260 = VERTEX_POINT('',#81571) ;
#20261 = VERTEX_POINT('',#81573) ;
#20262 = VERTEX_POINT('',#81577) ;
#20263 = VERTEX_POINT('',#81582) ;
#20264 = VERTEX_POINT('',#81583) ;
#20265 = VERTEX_POINT('',#81585) ;
#20266 = VERTEX_POINT('',#81587) ;
#20267 = VERTEX_POINT('',#81591) ;
#20268 = VERTEX_POINT('',#81593) ;
#20269 = VERTEX_POINT('',#81600) ;
#20270 = VERTEX_POINT('',#81602) ;
#20271 = VERTEX_POINT('',#81606) ;
#20272 = VERTEX_POINT('',#81611) ;
#20273 = VERTEX_POINT('',#81612) ;
#20274 = VERTEX_POINT('',#81685) ;
#20275 = VERTEX_POINT('',#81770) ;
#20276 = VERTEX_POINT('',#81792) ;
#20277 = VERTEX_POINT('',#81794) ;
#20278 = VERTEX_POINT('',#81837) ;
#20279 = VERTEX_POINT('',#81846) ;
#20280 = VERTEX_POINT('',#81917) ;
#20281 = VERTEX_POINT('',#81928) ;
#20282 = VERTEX_POINT('',#82019) ;
#20283 = VERTEX_POINT('',#82030) ;
#20284 = VERTEX_POINT('',#82121) ;
#20285 = VERTEX_POINT('',#82132) ;
#20286 = VERTEX_POINT('',#82193) ;
#20287 = VERTEX_POINT('',#82202) ;
#20288 = VERTEX_POINT('',#82251) ;
#20289 = VERTEX_POINT('',#82253) ;
#20290 = VERTEX_POINT('',#82255) ;
#20291 = VERTEX_POINT('',#82259) ;
#20292 = VERTEX_POINT('',#82261) ;
#20293 = VERTEX_POINT('',#82265) ;
#20294 = VERTEX_POINT('',#82267) ;
#20295 = VERTEX_POINT('',#82303) ;
#20296 = VERTEX_POINT('',#82305) ;
#20297 = VERTEX_POINT('',#82358) ;
#20298 = VERTEX_POINT('',#82426) ;
#20299 = VERTEX_POINT('',#82555) ;
#20300 = VERTEX_POINT('',#82556) ;
#20301 = VERTEX_POINT('',#82558) ;
#20302 = VERTEX_POINT('',#82560) ;
#20303 = VERTEX_POINT('',#82562) ;
#20304 = VERTEX_POINT('',#82564) ;
#20305 = VERTEX_POINT('',#82566) ;
#20306 = VERTEX_POINT('',#82568) ;
#20307 = VERTEX_POINT('',#82570) ;
#20308 = VERTEX_POINT('',#82572) ;
#20309 = VERTEX_POINT('',#82575) ;
#20310 = VERTEX_POINT('',#82577) ;
#20311 = VERTEX_POINT('',#82579) ;
#20312 = VERTEX_POINT('',#82581) ;
#20313 = VERTEX_POINT('',#82583) ;
#20314 = VERTEX_POINT('',#82585) ;
#20315 = VERTEX_POINT('',#82587) ;
#20316 = VERTEX_POINT('',#82589) ;
#20317 = VERTEX_POINT('',#82591) ;
#20318 = VERTEX_POINT('',#82593) ;
#20319 = VERTEX_POINT('',#82595) ;
#20320 = VERTEX_POINT('',#82597) ;
#20321 = VERTEX_POINT('',#82599) ;
#20322 = VERTEX_POINT('',#82601) ;
#20323 = VERTEX_POINT('',#82603) ;
#20324 = VERTEX_POINT('',#82605) ;
#20325 = VERTEX_POINT('',#82607) ;
#20326 = VERTEX_POINT('',#82609) ;
#20327 = VERTEX_POINT('',#82611) ;
#20328 = VERTEX_POINT('',#82613) ;
#20329 = VERTEX_POINT('',#82615) ;
#20330 = VERTEX_POINT('',#82617) ;
#20331 = VERTEX_POINT('',#82619) ;
#20332 = VERTEX_POINT('',#82621) ;
#20333 = VERTEX_POINT('',#82623) ;
#20334 = VERTEX_POINT('',#82625) ;
#20335 = VERTEX_POINT('',#82627) ;
#20336 = VERTEX_POINT('',#82629) ;
#20337 = VERTEX_POINT('',#82631) ;
#20338 = VERTEX_POINT('',#82633) ;
#20339 = VERTEX_POINT('',#82635) ;
#20340 = VERTEX_POINT('',#82637) ;
#20341 = VERTEX_POINT('',#82639) ;
#20342 = VERTEX_POINT('',#82641) ;
#20343 = VERTEX_POINT('',#82643) ;
#20344 = VERTEX_POINT('',#82645) ;
#20345 = VERTEX_POINT('',#82647) ;
#20346 = VERTEX_POINT('',#82649) ;
#20347 = VERTEX_POINT('',#82652) ;
#20348 = VERTEX_POINT('',#82653) ;
#20349 = VERTEX_POINT('',#82655) ;
#20350 = VERTEX_POINT('',#82658) ;
#20351 = VERTEX_POINT('',#82659) ;
#20352 = VERTEX_POINT('',#82661) ;
#20353 = VERTEX_POINT('',#82664) ;
#20354 = VERTEX_POINT('',#82665) ;
#20355 = VERTEX_POINT('',#82667) ;
#20356 = VERTEX_POINT('',#82669) ;
#20357 = VERTEX_POINT('',#82671) ;
#20358 = VERTEX_POINT('',#82673) ;
#20359 = VERTEX_POINT('',#82675) ;
#20360 = VERTEX_POINT('',#82677) ;
#20361 = VERTEX_POINT('',#82679) ;
#20362 = VERTEX_POINT('',#82681) ;
#20363 = VERTEX_POINT('',#82683) ;
#20364 = VERTEX_POINT('',#82685) ;
#20365 = VERTEX_POINT('',#82687) ;
#20366 = VERTEX_POINT('',#82689) ;
#20367 = VERTEX_POINT('',#82692) ;
#20368 = VERTEX_POINT('',#82693) ;
#20369 = VERTEX_POINT('',#82695) ;
#20370 = VERTEX_POINT('',#82697) ;
#20371 = VERTEX_POINT('',#82699) ;
#20372 = VERTEX_POINT('',#82701) ;
#20373 = VERTEX_POINT('',#82703) ;
#20374 = VERTEX_POINT('',#82705) ;
#20375 = VERTEX_POINT('',#82707) ;
#20376 = VERTEX_POINT('',#82709) ;
#20377 = VERTEX_POINT('',#82711) ;
#20378 = VERTEX_POINT('',#82713) ;
#20379 = VERTEX_POINT('',#82715) ;
#20380 = VERTEX_POINT('',#82717) ;
#20381 = VERTEX_POINT('',#82719) ;
#20382 = VERTEX_POINT('',#82721) ;
#20383 = VERTEX_POINT('',#82724) ;
#20384 = VERTEX_POINT('',#82725) ;
#20385 = VERTEX_POINT('',#82727) ;
#20386 = VERTEX_POINT('',#82729) ;
#20387 = VERTEX_POINT('',#82731) ;
#20388 = VERTEX_POINT('',#82733) ;
#20389 = VERTEX_POINT('',#82735) ;
#20390 = VERTEX_POINT('',#82737) ;
#20391 = VERTEX_POINT('',#82739) ;
#20392 = VERTEX_POINT('',#82741) ;
#20393 = VERTEX_POINT('',#82743) ;
#20394 = VERTEX_POINT('',#82745) ;
#20395 = VERTEX_POINT('',#82747) ;
#20396 = VERTEX_POINT('',#82749) ;
#20397 = VERTEX_POINT('',#82752) ;
#20398 = VERTEX_POINT('',#82753) ;
#20399 = VERTEX_POINT('',#82755) ;
#20400 = VERTEX_POINT('',#82757) ;
#20401 = VERTEX_POINT('',#82759) ;
#20402 = VERTEX_POINT('',#82761) ;
#20403 = VERTEX_POINT('',#82763) ;
#20404 = VERTEX_POINT('',#82765) ;
#20405 = VERTEX_POINT('',#82767) ;
#20406 = VERTEX_POINT('',#82769) ;
#20407 = VERTEX_POINT('',#82771) ;
#20408 = VERTEX_POINT('',#82773) ;
#20409 = VERTEX_POINT('',#82775) ;
#20410 = VERTEX_POINT('',#82777) ;
#20411 = VERTEX_POINT('',#82780) ;
#20412 = VERTEX_POINT('',#82781) ;
#20413 = VERTEX_POINT('',#82783) ;
#20414 = VERTEX_POINT('',#82785) ;
#20415 = VERTEX_POINT('',#82787) ;
#20416 = VERTEX_POINT('',#82789) ;
#20417 = VERTEX_POINT('',#82791) ;
#20418 = VERTEX_POINT('',#82793) ;
#20419 = VERTEX_POINT('',#82795) ;
#20420 = VERTEX_POINT('',#82797) ;
#20421 = VERTEX_POINT('',#82799) ;
#20422 = VERTEX_POINT('',#82801) ;
#20423 = VERTEX_POINT('',#82803) ;
#20424 = VERTEX_POINT('',#82805) ;
#20425 = VERTEX_POINT('',#82808) ;
#20426 = VERTEX_POINT('',#82810) ;
#20427 = VERTEX_POINT('',#82811) ;
#20428 = VERTEX_POINT('',#82813) ;
#20429 = VERTEX_POINT('',#82815) ;
#20430 = VERTEX_POINT('',#82817) ;
#20431 = VERTEX_POINT('',#82819) ;
#20432 = VERTEX_POINT('',#82821) ;
#20433 = VERTEX_POINT('',#82823) ;
#20434 = VERTEX_POINT('',#82825) ;
#20435 = VERTEX_POINT('',#82827) ;
#20436 = VERTEX_POINT('',#82829) ;
#20437 = VERTEX_POINT('',#82831) ;
#20438 = VERTEX_POINT('',#82833) ;
#20439 = VERTEX_POINT('',#82835) ;
#20440 = VERTEX_POINT('',#82837) ;
#20441 = VERTEX_POINT('',#82840) ;
#20442 = VERTEX_POINT('',#82842) ;
#20443 = VERTEX_POINT('',#82844) ;
#20444 = VERTEX_POINT('',#82845) ;
#20445 = VERTEX_POINT('',#82847) ;
#20446 = VERTEX_POINT('',#82849) ;
#20447 = VERTEX_POINT('',#82851) ;
#20448 = VERTEX_POINT('',#82853) ;
#20449 = VERTEX_POINT('',#82855) ;
#20450 = VERTEX_POINT('',#82857) ;
#20451 = VERTEX_POINT('',#82859) ;
#20452 = VERTEX_POINT('',#82861) ;
#20453 = VERTEX_POINT('',#82863) ;
#20454 = VERTEX_POINT('',#82865) ;
#20455 = VERTEX_POINT('',#82867) ;
#20456 = VERTEX_POINT('',#82869) ;
#20457 = VERTEX_POINT('',#82872) ;
#20458 = VERTEX_POINT('',#82874) ;
#20459 = VERTEX_POINT('',#82876) ;
#20460 = VERTEX_POINT('',#82877) ;
#20461 = VERTEX_POINT('',#82879) ;
#20462 = VERTEX_POINT('',#82881) ;
#20463 = VERTEX_POINT('',#82883) ;
#20464 = VERTEX_POINT('',#82885) ;
#20465 = VERTEX_POINT('',#82887) ;
#20466 = VERTEX_POINT('',#82889) ;
#20467 = VERTEX_POINT('',#82892) ;
#20468 = VERTEX_POINT('',#82893) ;
#20469 = VERTEX_POINT('',#82895) ;
#20470 = VERTEX_POINT('',#82897) ;
#20471 = VERTEX_POINT('',#82899) ;
#20472 = VERTEX_POINT('',#82901) ;
#20473 = VERTEX_POINT('',#82903) ;
#20474 = VERTEX_POINT('',#82905) ;
#20475 = VERTEX_POINT('',#82907) ;
#20476 = VERTEX_POINT('',#82909) ;
#20477 = VERTEX_POINT('',#82911) ;
#20478 = VERTEX_POINT('',#82913) ;
#20479 = VERTEX_POINT('',#82915) ;
#20480 = VERTEX_POINT('',#82917) ;
#20481 = VERTEX_POINT('',#82920) ;
#20482 = VERTEX_POINT('',#82921) ;
#20483 = VERTEX_POINT('',#82923) ;
#20484 = VERTEX_POINT('',#82925) ;
#20485 = VERTEX_POINT('',#82942) ;
#20486 = VERTEX_POINT('',#83012) ;
#20487 = VERTEX_POINT('',#83013) ;
#20488 = VERTEX_POINT('',#83015) ;
#20489 = VERTEX_POINT('',#83020) ;
#20490 = VERTEX_POINT('',#83023) ;
#20491 = VERTEX_POINT('',#83027) ;
#20492 = VERTEX_POINT('',#83031) ;
#20493 = VERTEX_POINT('',#83035) ;
#20494 = VERTEX_POINT('',#83039) ;
#20495 = VERTEX_POINT('',#83040) ;
#20496 = VERTEX_POINT('',#83042) ;
#20497 = VERTEX_POINT('',#83044) ;
#20498 = VERTEX_POINT('',#83046) ;
#20499 = VERTEX_POINT('',#83048) ;
#20500 = VERTEX_POINT('',#83050) ;
#20501 = VERTEX_POINT('',#83052) ;
#20502 = VERTEX_POINT('',#83054) ;
#20503 = VERTEX_POINT('',#83056) ;
#20504 = VERTEX_POINT('',#83058) ;
#20505 = VERTEX_POINT('',#83060) ;
#20506 = VERTEX_POINT('',#83062) ;
#20507 = VERTEX_POINT('',#83064) ;
#20508 = VERTEX_POINT('',#83066) ;
#20509 = VERTEX_POINT('',#83068) ;
#20510 = VERTEX_POINT('',#83070) ;
#20511 = VERTEX_POINT('',#83072) ;
#20512 = VERTEX_POINT('',#83074) ;
#20513 = VERTEX_POINT('',#83076) ;
#20514 = VERTEX_POINT('',#83078) ;
#20515 = VERTEX_POINT('',#83080) ;
#20516 = VERTEX_POINT('',#83082) ;
#20517 = VERTEX_POINT('',#83084) ;
#20518 = VERTEX_POINT('',#83086) ;
#20519 = VERTEX_POINT('',#83088) ;
#20520 = VERTEX_POINT('',#83090) ;
#20521 = VERTEX_POINT('',#83092) ;
#20522 = VERTEX_POINT('',#83094) ;
#20523 = VERTEX_POINT('',#83096) ;
#20524 = VERTEX_POINT('',#83098) ;
#20525 = VERTEX_POINT('',#83100) ;
#20526 = VERTEX_POINT('',#83102) ;
#20527 = VERTEX_POINT('',#83104) ;
#20528 = VERTEX_POINT('',#83106) ;
#20529 = VERTEX_POINT('',#83108) ;
#20530 = VERTEX_POINT('',#83110) ;
#20531 = VERTEX_POINT('',#83112) ;
#20532 = VERTEX_POINT('',#83114) ;
#20533 = VERTEX_POINT('',#83116) ;
#20534 = VERTEX_POINT('',#83118) ;
#20535 = VERTEX_POINT('',#83120) ;
#20536 = VERTEX_POINT('',#83122) ;
#20537 = VERTEX_POINT('',#83124) ;
#20538 = VERTEX_POINT('',#83126) ;
#20539 = VERTEX_POINT('',#83128) ;
#20540 = VERTEX_POINT('',#83130) ;
#20541 = VERTEX_POINT('',#83132) ;
#20542 = VERTEX_POINT('',#83134) ;
#20543 = VERTEX_POINT('',#83136) ;
#20544 = VERTEX_POINT('',#83138) ;
#20545 = VERTEX_POINT('',#83145) ;
#20546 = VERTEX_POINT('',#83147) ;
#20547 = VERTEX_POINT('',#83154) ;
#20548 = VERTEX_POINT('',#83156) ;
#20549 = VERTEX_POINT('',#83158) ;
#20550 = VERTEX_POINT('',#83160) ;
#20551 = VERTEX_POINT('',#83163) ;
#20552 = VERTEX_POINT('',#83165) ;
#20553 = VERTEX_POINT('',#83166) ;
#20554 = VERTEX_POINT('',#83168) ;
#20555 = VERTEX_POINT('',#83170) ;
#20556 = VERTEX_POINT('',#83172) ;
#20557 = VERTEX_POINT('',#83174) ;
#20558 = VERTEX_POINT('',#83176) ;
#20559 = VERTEX_POINT('',#83178) ;
#20560 = VERTEX_POINT('',#83180) ;
#20561 = VERTEX_POINT('',#83182) ;
#20562 = VERTEX_POINT('',#83184) ;
#20563 = VERTEX_POINT('',#83186) ;
#20564 = VERTEX_POINT('',#83188) ;
#20565 = VERTEX_POINT('',#83190) ;
#20566 = VERTEX_POINT('',#83193) ;
#20567 = VERTEX_POINT('',#83195) ;
#20568 = VERTEX_POINT('',#83197) ;
#20569 = VERTEX_POINT('',#83198) ;
#20570 = VERTEX_POINT('',#83200) ;
#20571 = VERTEX_POINT('',#83202) ;
#20572 = VERTEX_POINT('',#83204) ;
#20573 = VERTEX_POINT('',#83206) ;
#20574 = VERTEX_POINT('',#83208) ;
#20575 = VERTEX_POINT('',#83210) ;
#20576 = VERTEX_POINT('',#83212) ;
#20577 = VERTEX_POINT('',#83214) ;
#20578 = VERTEX_POINT('',#83216) ;
#20579 = VERTEX_POINT('',#83218) ;
#20580 = VERTEX_POINT('',#83220) ;
#20581 = VERTEX_POINT('',#83222) ;
#20582 = VERTEX_POINT('',#83224) ;
#20583 = VERTEX_POINT('',#83226) ;
#20584 = VERTEX_POINT('',#83229) ;
#20585 = VERTEX_POINT('',#83231) ;
#20586 = VERTEX_POINT('',#83232) ;
#20587 = VERTEX_POINT('',#83234) ;
#20588 = VERTEX_POINT('',#83236) ;
#20589 = VERTEX_POINT('',#83238) ;
#20590 = VERTEX_POINT('',#83240) ;
#20591 = VERTEX_POINT('',#83242) ;
#20592 = VERTEX_POINT('',#83244) ;
#20593 = VERTEX_POINT('',#83246) ;
#20594 = VERTEX_POINT('',#83248) ;
#20595 = VERTEX_POINT('',#83250) ;
#20596 = VERTEX_POINT('',#83252) ;
#20597 = VERTEX_POINT('',#83254) ;
#20598 = VERTEX_POINT('',#83256) ;
#20599 = VERTEX_POINT('',#83259) ;
#20600 = VERTEX_POINT('',#83260) ;
#20601 = VERTEX_POINT('',#83262) ;
#20602 = VERTEX_POINT('',#83264) ;
#20603 = VERTEX_POINT('',#83266) ;
#20604 = VERTEX_POINT('',#83268) ;
#20605 = VERTEX_POINT('',#83270) ;
#20606 = VERTEX_POINT('',#83272) ;
#20607 = VERTEX_POINT('',#83275) ;
#20608 = VERTEX_POINT('',#83276) ;
#20609 = VERTEX_POINT('',#83278) ;
#20610 = VERTEX_POINT('',#83280) ;
#20611 = VERTEX_POINT('',#83282) ;
#20612 = VERTEX_POINT('',#83289) ;
#20613 = VERTEX_POINT('',#83291) ;
#20614 = VERTEX_POINT('',#83293) ;
#20615 = VERTEX_POINT('',#83295) ;
#20616 = VERTEX_POINT('',#83297) ;
#20617 = VERTEX_POINT('',#83299) ;
#20618 = VERTEX_POINT('',#83301) ;
#20619 = VERTEX_POINT('',#83303) ;
#20620 = VERTEX_POINT('',#83305) ;
#20621 = VERTEX_POINT('',#83313) ;
#20622 = VERTEX_POINT('',#83314) ;
#20623 = VERTEX_POINT('',#83316) ;
#20624 = VERTEX_POINT('',#83323) ;
#20625 = VERTEX_POINT('',#83325) ;
#20626 = VERTEX_POINT('',#83327) ;
#20627 = VERTEX_POINT('',#83329) ;
#20628 = VERTEX_POINT('',#83331) ;
#20629 = VERTEX_POINT('',#83333) ;
#20630 = VERTEX_POINT('',#83335) ;
#20631 = VERTEX_POINT('',#83337) ;
#20632 = VERTEX_POINT('',#83339) ;
#20633 = VERTEX_POINT('',#83341) ;
#20634 = VERTEX_POINT('',#83343) ;
#20635 = VERTEX_POINT('',#83351) ;
#20636 = VERTEX_POINT('',#83352) ;
#20637 = VERTEX_POINT('',#83354) ;
#20638 = VERTEX_POINT('',#83356) ;
#20639 = VERTEX_POINT('',#83358) ;
#20640 = VERTEX_POINT('',#83360) ;
#20641 = VERTEX_POINT('',#83362) ;
#20642 = VERTEX_POINT('',#83364) ;
#20643 = VERTEX_POINT('',#83366) ;
#20644 = VERTEX_POINT('',#83368) ;
#20645 = VERTEX_POINT('',#83370) ;
#20646 = VERTEX_POINT('',#83372) ;
#20647 = VERTEX_POINT('',#83374) ;
#20648 = VERTEX_POINT('',#83376) ;
#20649 = VERTEX_POINT('',#83379) ;
#20650 = VERTEX_POINT('',#83380) ;
#20651 = VERTEX_POINT('',#83382) ;
#20652 = VERTEX_POINT('',#83384) ;
#20653 = VERTEX_POINT('',#83386) ;
#20654 = VERTEX_POINT('',#83388) ;
#20655 = VERTEX_POINT('',#83390) ;
#20656 = VERTEX_POINT('',#83392) ;
#20657 = VERTEX_POINT('',#83394) ;
#20658 = VERTEX_POINT('',#83396) ;
#20659 = VERTEX_POINT('',#83398) ;
#20660 = VERTEX_POINT('',#83400) ;
#20661 = VERTEX_POINT('',#83402) ;
#20662 = VERTEX_POINT('',#83404) ;
#20663 = VERTEX_POINT('',#83407) ;
#20664 = VERTEX_POINT('',#83427) ;
#20665 = VERTEX_POINT('',#83428) ;
#20666 = VERTEX_POINT('',#83431) ;
#20667 = VERTEX_POINT('',#83435) ;
#20668 = VERTEX_POINT('',#83436) ;
#20669 = VERTEX_POINT('',#83441) ;
#20670 = VERTEX_POINT('',#83442) ;
#20671 = VERTEX_POINT('',#83447) ;
#20672 = VERTEX_POINT('',#83448) ;
#20673 = VERTEX_POINT('',#83453) ;
#20674 = VERTEX_POINT('',#83454) ;
#20675 = VERTEX_POINT('',#83459) ;
#20676 = VERTEX_POINT('',#83460) ;
#20677 = VERTEX_POINT('',#83465) ;
#20678 = VERTEX_POINT('',#83466) ;
#20679 = VERTEX_POINT('',#83471) ;
#20680 = VERTEX_POINT('',#83472) ;
#20681 = VERTEX_POINT('',#83477) ;
#20682 = VERTEX_POINT('',#83478) ;
#20683 = VERTEX_POINT('',#83483) ;
#20684 = VERTEX_POINT('',#83484) ;
#20685 = VERTEX_POINT('',#83489) ;
#20686 = VERTEX_POINT('',#83490) ;
#20687 = VERTEX_POINT('',#83495) ;
#20688 = VERTEX_POINT('',#83496) ;
#20689 = VERTEX_POINT('',#83501) ;
#20690 = VERTEX_POINT('',#83506) ;
#20691 = VERTEX_POINT('',#83508) ;
#20692 = VERTEX_POINT('',#83510) ;
#20693 = VERTEX_POINT('',#83512) ;
#20694 = VERTEX_POINT('',#83514) ;
#20695 = VERTEX_POINT('',#83518) ;
#20696 = VERTEX_POINT('',#83522) ;
#20697 = VERTEX_POINT('',#83526) ;
#20698 = VERTEX_POINT('',#83530) ;
#20699 = VERTEX_POINT('',#83534) ;
#20700 = VERTEX_POINT('',#83538) ;
#20701 = VERTEX_POINT('',#83542) ;
#20702 = VERTEX_POINT('',#83546) ;
#20703 = VERTEX_POINT('',#83550) ;
#20704 = VERTEX_POINT('',#83554) ;
#20705 = VERTEX_POINT('',#83556) ;
#20706 = VERTEX_POINT('',#83558) ;
#20707 = VERTEX_POINT('',#83560) ;
#20708 = VERTEX_POINT('',#83564) ;
#20709 = VERTEX_POINT('',#83568) ;
#20710 = VERTEX_POINT('',#83661) ;
#20711 = VERTEX_POINT('',#83667) ;
#20712 = VERTEX_POINT('',#83688) ;
#20713 = VERTEX_POINT('',#83692) ;
#20714 = VERTEX_POINT('',#83695) ;
#20715 = VERTEX_POINT('',#83696) ;
#20716 = VERTEX_POINT('',#83701) ;
#20717 = VERTEX_POINT('',#83705) ;
#20718 = VERTEX_POINT('',#83707) ;
#20719 = VERTEX_POINT('',#83709) ;
#20720 = VERTEX_POINT('',#83713) ;
#20721 = VERTEX_POINT('',#83715) ;
#20722 = VERTEX_POINT('',#83719) ;
#20723 = VERTEX_POINT('',#83720) ;
#20724 = VERTEX_POINT('',#83722) ;
#20725 = VERTEX_POINT('',#83724) ;
#20726 = VERTEX_POINT('',#83726) ;
#20727 = VERTEX_POINT('',#83728) ;
#20728 = VERTEX_POINT('',#83732) ;
#20729 = VERTEX_POINT('',#83736) ;
#20730 = VERTEX_POINT('',#83737) ;
#20731 = VERTEX_POINT('',#83744) ;
#20732 = VERTEX_POINT('',#83746) ;
#20733 = VERTEX_POINT('',#83754) ;
#20734 = VERTEX_POINT('',#83756) ;
#20735 = VERTEX_POINT('',#83758) ;
#20736 = VERTEX_POINT('',#83762) ;
#20737 = VERTEX_POINT('',#83764) ;
#20738 = VERTEX_POINT('',#83768) ;
#20739 = VERTEX_POINT('',#83769) ;
#20740 = VERTEX_POINT('',#83771) ;
#20741 = VERTEX_POINT('',#83773) ;
#20742 = VERTEX_POINT('',#83775) ;
#20743 = VERTEX_POINT('',#83777) ;
#20744 = VERTEX_POINT('',#83781) ;
#20745 = VERTEX_POINT('',#83785) ;
#20746 = VERTEX_POINT('',#83786) ;
#20747 = VERTEX_POINT('',#83792) ;
#20748 = VERTEX_POINT('',#83794) ;
#20749 = VERTEX_POINT('',#83803) ;
#20750 = VERTEX_POINT('',#83805) ;
#20751 = VERTEX_POINT('',#83809) ;
#20752 = VERTEX_POINT('',#83813) ;
#20753 = VERTEX_POINT('',#83817) ;
#20754 = VERTEX_POINT('',#83821) ;
#20755 = VERTEX_POINT('',#83825) ;
#20756 = VERTEX_POINT('',#83827) ;
#20757 = VERTEX_POINT('',#83829) ;
#20758 = VERTEX_POINT('',#83831) ;
#20759 = VERTEX_POINT('',#83833) ;
#20760 = VERTEX_POINT('',#83845) ;
#20761 = VERTEX_POINT('',#83856) ;
#20762 = VERTEX_POINT('',#83858) ;
#20763 = VERTEX_POINT('',#83860) ;
#20764 = VERTEX_POINT('',#83872) ;
#20765 = VERTEX_POINT('',#83883) ;
#20766 = VERTEX_POINT('',#83885) ;
#20767 = VERTEX_POINT('',#83887) ;
#20768 = VERTEX_POINT('',#83889) ;
#20769 = VERTEX_POINT('',#83895) ;
#20770 = VERTEX_POINT('',#83897) ;
#20771 = VERTEX_POINT('',#83917) ;
#20772 = VERTEX_POINT('',#83936) ;
#20773 = VERTEX_POINT('',#83939) ;
#20774 = VERTEX_POINT('',#83941) ;
#20775 = VERTEX_POINT('',#83961) ;
#20776 = VERTEX_POINT('',#83980) ;
#20777 = VERTEX_POINT('',#83982) ;
#20778 = VERTEX_POINT('',#83984) ;
#20779 = VERTEX_POINT('',#83986) ;
#20780 = VERTEX_POINT('',#83991) ;
#20781 = VERTEX_POINT('',#83993) ;
#20782 = VERTEX_POINT('',#84037) ;
#20783 = VERTEX_POINT('',#84060) ;
#20784 = VERTEX_POINT('',#84082) ;
#20785 = VERTEX_POINT('',#84120) ;
#20786 = VERTEX_POINT('',#84122) ;
#20787 = VERTEX_POINT('',#84126) ;
#20788 = VERTEX_POINT('',#84130) ;
#20789 = VERTEX_POINT('',#84134) ;
#20790 = VERTEX_POINT('',#84157) ;
#20791 = VERTEX_POINT('',#84159) ;
#20792 = VERTEX_POINT('',#84163) ;
#20793 = VERTEX_POINT('',#84167) ;
#20794 = VERTEX_POINT('',#84171) ;
#20795 = VERTEX_POINT('',#84172) ;
#20796 = VERTEX_POINT('',#84180) ;
#20797 = VERTEX_POINT('',#84182) ;
#20798 = VERTEX_POINT('',#84186) ;
#20799 = VERTEX_POINT('',#84187) ;
#20800 = VERTEX_POINT('',#84196) ;
#20801 = VERTEX_POINT('',#84197) ;
#20802 = VERTEX_POINT('',#84205) ;
#20803 = VERTEX_POINT('',#84206) ;
#20804 = VERTEX_POINT('',#84214) ;
#20805 = VERTEX_POINT('',#84218) ;
#20806 = VERTEX_POINT('',#84222) ;
#20807 = VERTEX_POINT('',#84228) ;
#20808 = VERTEX_POINT('',#84232) ;
#20809 = VERTEX_POINT('',#84234) ;
#20810 = VERTEX_POINT('',#84240) ;
#20811 = VERTEX_POINT('',#84241) ;
#20812 = VERTEX_POINT('',#84246) ;
#20813 = VERTEX_POINT('',#84247) ;
#20814 = VERTEX_POINT('',#84274) ;
#20815 = VERTEX_POINT('',#84299) ;
#20816 = VERTEX_POINT('',#84300) ;
#20817 = VERTEX_POINT('',#84305) ;
#20818 = VERTEX_POINT('',#84306) ;
#20819 = VERTEX_POINT('',#84314) ;
#20820 = VERTEX_POINT('',#84320) ;
#20821 = VERTEX_POINT('',#84322) ;
#20822 = VERTEX_POINT('',#84326) ;
#20823 = VERTEX_POINT('',#84330) ;
#20824 = VERTEX_POINT('',#84334) ;
#20825 = VERTEX_POINT('',#84338) ;
#20826 = VERTEX_POINT('',#84344) ;
#20827 = VERTEX_POINT('',#84348) ;
#20828 = VERTEX_POINT('',#84350) ;
#20829 = VERTEX_POINT('',#84354) ;
#20830 = VERTEX_POINT('',#84358) ;
#20831 = VERTEX_POINT('',#84362) ;
#20832 = VERTEX_POINT('',#84366) ;
#20833 = VERTEX_POINT('',#84370) ;
#20834 = VERTEX_POINT('',#84374) ;
#20835 = VERTEX_POINT('',#84378) ;
#20836 = VERTEX_POINT('',#84382) ;
#20837 = VERTEX_POINT('',#84386) ;
#20838 = VERTEX_POINT('',#84390) ;
#20839 = VERTEX_POINT('',#84394) ;
#20840 = VERTEX_POINT('',#84396) ;
#20841 = VERTEX_POINT('',#84400) ;
#20842 = VERTEX_POINT('',#84404) ;
#20843 = VERTEX_POINT('',#84408) ;
#20844 = VERTEX_POINT('',#84412) ;
#20845 = VERTEX_POINT('',#84416) ;
#20846 = VERTEX_POINT('',#84420) ;
#20847 = VERTEX_POINT('',#84424) ;
#20848 = VERTEX_POINT('',#84428) ;
#20849 = VERTEX_POINT('',#84432) ;
#20850 = VERTEX_POINT('',#84434) ;
#20851 = VERTEX_POINT('',#84438) ;
#20852 = VERTEX_POINT('',#84442) ;
#20853 = VERTEX_POINT('',#84446) ;
#20854 = VERTEX_POINT('',#84450) ;
#20855 = VERTEX_POINT('',#84458) ;
#20856 = VERTEX_POINT('',#84460) ;
#20857 = VERTEX_POINT('',#84464) ;
#20858 = VERTEX_POINT('',#84468) ;
#20859 = VERTEX_POINT('',#84472) ;
#20860 = VERTEX_POINT('',#84476) ;
#20861 = VERTEX_POINT('',#84480) ;
#20862 = VERTEX_POINT('',#84484) ;
#20863 = VERTEX_POINT('',#84488) ;
#20864 = VERTEX_POINT('',#84492) ;
#20865 = VERTEX_POINT('',#84494) ;
#20866 = VERTEX_POINT('',#84498) ;
#20867 = VERTEX_POINT('',#84499) ;
#20868 = VERTEX_POINT('',#84504) ;
#20869 = VERTEX_POINT('',#84508) ;
#20870 = VERTEX_POINT('',#84512) ;
#20871 = VERTEX_POINT('',#84516) ;
#20872 = VERTEX_POINT('',#84520) ;
#20873 = VERTEX_POINT('',#84524) ;
#20874 = VERTEX_POINT('',#84528) ;
#20875 = VERTEX_POINT('',#84532) ;
#20876 = VERTEX_POINT('',#84538) ;
#20877 = VERTEX_POINT('',#84542) ;
#20878 = VERTEX_POINT('',#84543) ;
#20879 = VERTEX_POINT('',#84570) ;
#20880 = VERTEX_POINT('',#84571) ;
#20881 = VERTEX_POINT('',#84598) ;
#20882 = VERTEX_POINT('',#84602) ;
#20883 = VERTEX_POINT('',#84606) ;
#20884 = VERTEX_POINT('',#84608) ;
#20885 = VERTEX_POINT('',#84612) ;
#20886 = VERTEX_POINT('',#84616) ;
#20887 = VERTEX_POINT('',#84618) ;
#20888 = VERTEX_POINT('',#84622) ;
#20889 = VERTEX_POINT('',#84626) ;
#20890 = VERTEX_POINT('',#84630) ;
#20891 = VERTEX_POINT('',#84634) ;
#20892 = VERTEX_POINT('',#84640) ;
#20893 = VERTEX_POINT('',#84642) ;
#20894 = VERTEX_POINT('',#84646) ;
#20895 = VERTEX_POINT('',#84652) ;
#20896 = VERTEX_POINT('',#84654) ;
#20897 = VERTEX_POINT('',#84658) ;
#20898 = VERTEX_POINT('',#84662) ;
#20899 = VERTEX_POINT('',#84666) ;
#20900 = VERTEX_POINT('',#84670) ;
#20901 = VERTEX_POINT('',#84674) ;
#20902 = VERTEX_POINT('',#84678) ;
#20903 = VERTEX_POINT('',#84682) ;
#20904 = VERTEX_POINT('',#84686) ;
#20905 = VERTEX_POINT('',#84690) ;
#20906 = VERTEX_POINT('',#84692) ;
#20907 = VERTEX_POINT('',#84696) ;
#20908 = VERTEX_POINT('',#84700) ;
#20909 = VERTEX_POINT('',#84702) ;
#20910 = VERTEX_POINT('',#84706) ;
#20911 = VERTEX_POINT('',#84710) ;
#20912 = VERTEX_POINT('',#84714) ;
#20913 = VERTEX_POINT('',#84718) ;
#20914 = VERTEX_POINT('',#84724) ;
#20915 = VERTEX_POINT('',#84726) ;
#20916 = VERTEX_POINT('',#84730) ;
#20917 = VERTEX_POINT('',#84736) ;
#20918 = VERTEX_POINT('',#84738) ;
#20919 = VERTEX_POINT('',#84742) ;
#20920 = VERTEX_POINT('',#84746) ;
#20921 = VERTEX_POINT('',#84750) ;
#20922 = VERTEX_POINT('',#84754) ;
#20923 = VERTEX_POINT('',#84758) ;
#20924 = VERTEX_POINT('',#84762) ;
#20925 = VERTEX_POINT('',#84766) ;
#20926 = VERTEX_POINT('',#84770) ;
#20927 = VERTEX_POINT('',#84776) ;
#20928 = VERTEX_POINT('',#84781) ;
#20929 = VERTEX_POINT('',#84790) ;
#20930 = VERTEX_POINT('',#84795) ;
#20931 = VERTEX_POINT('',#84799) ;
#20932 = VERTEX_POINT('',#84803) ;
#20933 = VERTEX_POINT('',#84807) ;
#20934 = VERTEX_POINT('',#84811) ;
#20935 = VERTEX_POINT('',#84815) ;
#20936 = VERTEX_POINT('',#84819) ;
#20937 = VERTEX_POINT('',#84823) ;
#20938 = VERTEX_POINT('',#84829) ;
#20939 = VERTEX_POINT('',#84833) ;
#20940 = VERTEX_POINT('',#84837) ;
#20941 = VERTEX_POINT('',#84841) ;
#20942 = VERTEX_POINT('',#84845) ;
#20943 = VERTEX_POINT('',#84849) ;
#20944 = VERTEX_POINT('',#84853) ;
#20945 = VERTEX_POINT('',#84857) ;
#20946 = VERTEX_POINT('',#84865) ;
#20947 = VERTEX_POINT('',#84867) ;
#20948 = VERTEX_POINT('',#84871) ;
#20949 = VERTEX_POINT('',#84873) ;
#20950 = VERTEX_POINT('',#84875) ;
#20951 = VERTEX_POINT('',#84879) ;
#20952 = VERTEX_POINT('',#84886) ;
#20953 = VERTEX_POINT('',#84890) ;
#20954 = VERTEX_POINT('',#84900) ;
#20955 = VERTEX_POINT('',#84915) ;
#20956 = VERTEX_POINT('',#84917) ;
#20957 = VERTEX_POINT('',#84921) ;
#20958 = VERTEX_POINT('',#84923) ;
#20959 = VERTEX_POINT('',#84928) ;
#20960 = VERTEX_POINT('',#84930) ;
#20961 = VERTEX_POINT('',#84948) ;
#20962 = VERTEX_POINT('',#84954) ;
#20963 = VERTEX_POINT('',#84962) ;
#20964 = VERTEX_POINT('',#84966) ;
#20965 = VERTEX_POINT('',#84988) ;
#20966 = VERTEX_POINT('',#84990) ;
#20967 = VERTEX_POINT('',#84994) ;
#20968 = VERTEX_POINT('',#84996) ;
#20969 = VERTEX_POINT('',#85001) ;
#20970 = VERTEX_POINT('',#85003) ;
#20971 = VERTEX_POINT('',#85018) ;
#20972 = VERTEX_POINT('',#85028) ;
#20973 = VERTEX_POINT('',#85033) ;
#20974 = VERTEX_POINT('',#85040) ;
#20975 = VERTEX_POINT('',#85061) ;
#20976 = VERTEX_POINT('',#85063) ;
#20977 = VERTEX_POINT('',#85067) ;
#20978 = VERTEX_POINT('',#85069) ;
#20979 = VERTEX_POINT('',#85081) ;
#20980 = VERTEX_POINT('',#85085) ;
#20981 = VERTEX_POINT('',#85089) ;
#20982 = VERTEX_POINT('',#85105) ;
#20983 = VERTEX_POINT('',#85109) ;
#20984 = VERTEX_POINT('',#85113) ;
#20985 = VERTEX_POINT('',#85117) ;
#20986 = VERTEX_POINT('',#85121) ;
#20987 = VERTEX_POINT('',#85125) ;
#20988 = VERTEX_POINT('',#85129) ;
#20989 = VERTEX_POINT('',#85133) ;
#20990 = VERTEX_POINT('',#85137) ;
#20991 = VERTEX_POINT('',#85141) ;
#20992 = VERTEX_POINT('',#85145) ;
#20993 = VERTEX_POINT('',#85149) ;
#20994 = VERTEX_POINT('',#85153) ;
#20995 = VERTEX_POINT('',#85157) ;
#20996 = VERTEX_POINT('',#85161) ;
#20997 = VERTEX_POINT('',#85165) ;
#20998 = VERTEX_POINT('',#85169) ;
#20999 = VERTEX_POINT('',#85173) ;
#21000 = VERTEX_POINT('',#85177) ;
#21001 = VERTEX_POINT('',#85181) ;
#21002 = VERTEX_POINT('',#85185) ;
#21003 = VERTEX_POINT('',#85189) ;
#21004 = VERTEX_POINT('',#85193) ;
#21005 = VERTEX_POINT('',#85199) ;
#21006 = VERTEX_POINT('',#85200) ;
#21007 = VERTEX_POINT('',#85210) ;
#21008 = VERTEX_POINT('',#85211) ;
#21009 = VERTEX_POINT('',#85219) ;
#21010 = VERTEX_POINT('',#85223) ;
#21011 = VERTEX_POINT('',#85225) ;
#21012 = VERTEX_POINT('',#85229) ;
#21013 = VERTEX_POINT('',#85233) ;
#21014 = VERTEX_POINT('',#85237) ;
#21015 = VERTEX_POINT('',#85241) ;
#21016 = VERTEX_POINT('',#85245) ;
#21017 = VERTEX_POINT('',#85249) ;
#21018 = VERTEX_POINT('',#85253) ;
#21019 = VERTEX_POINT('',#85257) ;
#21020 = VERTEX_POINT('',#85261) ;
#21021 = VERTEX_POINT('',#85265) ;
#21022 = VERTEX_POINT('',#85269) ;
#21023 = VERTEX_POINT('',#85273) ;
#21024 = VERTEX_POINT('',#85277) ;
#21025 = VERTEX_POINT('',#85281) ;
#21026 = VERTEX_POINT('',#85285) ;
#21027 = VERTEX_POINT('',#85289) ;
#21028 = VERTEX_POINT('',#85293) ;
#21029 = VERTEX_POINT('',#85297) ;
#21030 = VERTEX_POINT('',#85301) ;
#21031 = VERTEX_POINT('',#85305) ;
#21032 = VERTEX_POINT('',#85309) ;
#21033 = VERTEX_POINT('',#85317) ;
#21034 = VERTEX_POINT('',#85318) ;
#21035 = VERTEX_POINT('',#85320) ;
#21036 = VERTEX_POINT('',#85322) ;
#21037 = VERTEX_POINT('',#85326) ;
#21038 = VERTEX_POINT('',#85333) ;
#21039 = VERTEX_POINT('',#85337) ;
#21040 = VERTEX_POINT('',#85341) ;
#21041 = VERTEX_POINT('',#85343) ;
#21042 = VERTEX_POINT('',#85345) ;
#21043 = VERTEX_POINT('',#85349) ;
#21044 = VERTEX_POINT('',#85353) ;
#21045 = VERTEX_POINT('',#85362) ;
#21046 = VERTEX_POINT('',#85364) ;
#21047 = VERTEX_POINT('',#85368) ;
#21048 = VERTEX_POINT('',#85369) ;
#21049 = VERTEX_POINT('',#85376) ;
#21050 = VERTEX_POINT('',#85377) ;
#21051 = VERTEX_POINT('',#85384) ;
#21052 = VERTEX_POINT('',#85385) ;
#21053 = VERTEX_POINT('',#85392) ;
#21054 = VERTEX_POINT('',#85393) ;
#21055 = VERTEX_POINT('',#85400) ;
#21056 = VERTEX_POINT('',#85402) ;
#21057 = VERTEX_POINT('',#85432) ;
#21058 = VERTEX_POINT('',#85434) ;
#21059 = VERTEX_POINT('',#85438) ;
#21060 = VERTEX_POINT('',#85440) ;
#21061 = VERTEX_POINT('',#85449) ;
#21062 = VERTEX_POINT('',#85451) ;
#21063 = VERTEX_POINT('',#85460) ;
#21064 = VERTEX_POINT('',#85492) ;
#21065 = VERTEX_POINT('',#85493) ;
#21066 = VERTEX_POINT('',#85495) ;
#21067 = VERTEX_POINT('',#85497) ;
#21068 = VERTEX_POINT('',#85506) ;
#21069 = VERTEX_POINT('',#85510) ;
#21070 = VERTEX_POINT('',#85511) ;
#21071 = VERTEX_POINT('',#85513) ;
#21072 = VERTEX_POINT('',#85515) ;
#21073 = VERTEX_POINT('',#85545) ;
#21074 = VERTEX_POINT('',#85546) ;
#21075 = VERTEX_POINT('',#85548) ;
#21076 = VERTEX_POINT('',#85550) ;
#21077 = VERTEX_POINT('',#85560) ;
#21078 = VERTEX_POINT('',#85564) ;
#21079 = VERTEX_POINT('',#85568) ;
#21080 = VERTEX_POINT('',#85570) ;
#21081 = VERTEX_POINT('',#85572) ;
#21082 = VERTEX_POINT('',#85576) ;
#21083 = VERTEX_POINT('',#85580) ;
#21084 = VERTEX_POINT('',#85589) ;
#21085 = VERTEX_POINT('',#85590) ;
#21086 = VERTEX_POINT('',#85595) ;
#21087 = VERTEX_POINT('',#85596) ;
#21088 = VERTEX_POINT('',#85601) ;
#21089 = VERTEX_POINT('',#85602) ;
#21090 = VERTEX_POINT('',#85607) ;
#21091 = VERTEX_POINT('',#85608) ;
#21092 = VERTEX_POINT('',#85649) ;
#21093 = VERTEX_POINT('',#85651) ;
#21094 = VERTEX_POINT('',#85655) ;
#21095 = VERTEX_POINT('',#85656) ;
#21096 = VERTEX_POINT('',#85661) ;
#21097 = VERTEX_POINT('',#85663) ;
#21098 = VERTEX_POINT('',#85667) ;
#21099 = VERTEX_POINT('',#85668) ;
#21100 = VERTEX_POINT('',#85673) ;
#21101 = VERTEX_POINT('',#85675) ;
#21102 = VERTEX_POINT('',#85679) ;
#21103 = VERTEX_POINT('',#85680) ;
#21104 = VERTEX_POINT('',#85685) ;
#21105 = VERTEX_POINT('',#85687) ;
#21106 = VERTEX_POINT('',#85693) ;
#21107 = VERTEX_POINT('',#85694) ;
#21108 = VERTEX_POINT('',#85729) ;
#21109 = VERTEX_POINT('',#85733) ;
#21110 = VERTEX_POINT('',#85735) ;
#21111 = VERTEX_POINT('',#85741) ;
#21112 = VERTEX_POINT('',#85742) ;
#21113 = VERTEX_POINT('',#85744) ;
#21114 = VERTEX_POINT('',#85746) ;
#21115 = VERTEX_POINT('',#85756) ;
#21116 = VERTEX_POINT('',#85760) ;
#21117 = VERTEX_POINT('',#85762) ;
#21118 = VERTEX_POINT('',#85764) ;
#21119 = VERTEX_POINT('',#85768) ;
#21120 = VERTEX_POINT('',#85772) ;
#21121 = VERTEX_POINT('',#85776) ;
#21122 = VERTEX_POINT('',#85808) ;
#21123 = VERTEX_POINT('',#85810) ;
#21124 = VERTEX_POINT('',#85816) ;
#21125 = VERTEX_POINT('',#85818) ;
#21126 = VERTEX_POINT('',#85873) ;
#21127 = VERTEX_POINT('',#85877) ;
#21128 = VERTEX_POINT('',#85881) ;
#21129 = VERTEX_POINT('',#85887) ;
#21130 = VERTEX_POINT('',#85891) ;
#21131 = VERTEX_POINT('',#85894) ;
#21132 = VERTEX_POINT('',#85895) ;
#21133 = VERTEX_POINT('',#85900) ;
#21134 = VERTEX_POINT('',#85904) ;
#21135 = VERTEX_POINT('',#85906) ;
#21136 = VERTEX_POINT('',#85910) ;
#21137 = VERTEX_POINT('',#85912) ;
#21138 = VERTEX_POINT('',#85914) ;
#21139 = VERTEX_POINT('',#85918) ;
#21140 = VERTEX_POINT('',#85920) ;
#21141 = VERTEX_POINT('',#85924) ;
#21142 = VERTEX_POINT('',#85928) ;
#21143 = VERTEX_POINT('',#85931) ;
#21144 = VERTEX_POINT('',#85935) ;
#21145 = VERTEX_POINT('',#85939) ;
#21146 = VERTEX_POINT('',#85941) ;
#21147 = VERTEX_POINT('',#85943) ;
#21148 = VERTEX_POINT('',#85947) ;
#21149 = VERTEX_POINT('',#85949) ;
#21150 = VERTEX_POINT('',#85953) ;
#21151 = VERTEX_POINT('',#85957) ;
#21152 = VERTEX_POINT('',#86010) ;
#21153 = VERTEX_POINT('',#86038) ;
#21154 = VERTEX_POINT('',#86039) ;
#21155 = VERTEX_POINT('',#86042) ;
#21156 = VERTEX_POINT('',#86071) ;
#21157 = VERTEX_POINT('',#86074) ;
#21158 = VERTEX_POINT('',#86076) ;
#21159 = VERTEX_POINT('',#86104) ;
#21160 = VERTEX_POINT('',#86105) ;
#21161 = VERTEX_POINT('',#86110) ;
#21162 = VERTEX_POINT('',#86172) ;
#21163 = VERTEX_POINT('',#86179) ;
#21164 = VERTEX_POINT('',#86241) ;
#21165 = VERTEX_POINT('',#86248) ;
#21166 = VERTEX_POINT('',#86252) ;
#21167 = VERTEX_POINT('',#86260) ;
#21168 = VERTEX_POINT('',#86268) ;
#21169 = VERTEX_POINT('',#86276) ;
#21170 = VERTEX_POINT('',#86544) ;
#21171 = VERTEX_POINT('',#86545) ;
#21172 = VERTEX_POINT('',#86547) ;
#21173 = VERTEX_POINT('',#86549) ;
#21174 = VERTEX_POINT('',#86553) ;
#21175 = VERTEX_POINT('',#86555) ;
#21176 = VERTEX_POINT('',#86559) ;
#21177 = VERTEX_POINT('',#86561) ;
#21178 = VERTEX_POINT('',#86565) ;
#21179 = VERTEX_POINT('',#86566) ;
#21180 = VERTEX_POINT('',#86568) ;
#21181 = VERTEX_POINT('',#86572) ;
#21182 = VERTEX_POINT('',#86573) ;
#21183 = VERTEX_POINT('',#86578) ;
#21184 = VERTEX_POINT('',#86579) ;
#21185 = VERTEX_POINT('',#86587) ;
#21186 = VERTEX_POINT('',#86589) ;
#21187 = VERTEX_POINT('',#86593) ;
#21188 = VERTEX_POINT('',#86598) ;
#21189 = VERTEX_POINT('',#86602) ;
#21190 = VERTEX_POINT('',#86613) ;
#21191 = VERTEX_POINT('',#86614) ;
#21192 = VERTEX_POINT('',#86625) ;
#21193 = VERTEX_POINT('',#86627) ;
#21194 = VERTEX_POINT('',#86631) ;
#21195 = VERTEX_POINT('',#86633) ;
#21196 = VERTEX_POINT('',#86635) ;
#21197 = VERTEX_POINT('',#86639) ;
#21198 = VERTEX_POINT('',#86640) ;
#21199 = VERTEX_POINT('',#86651) ;
#21200 = VERTEX_POINT('',#86660) ;
#21201 = VERTEX_POINT('',#86662) ;
#21202 = VERTEX_POINT('',#86664) ;
#21203 = VERTEX_POINT('',#86666) ;
#21204 = VERTEX_POINT('',#86668) ;
#21205 = VERTEX_POINT('',#86670) ;
#21206 = VERTEX_POINT('',#86672) ;
#21207 = VERTEX_POINT('',#86674) ;
#21208 = VERTEX_POINT('',#86676) ;
#21209 = VERTEX_POINT('',#86678) ;
#21210 = VERTEX_POINT('',#86680) ;
#21211 = VERTEX_POINT('',#86682) ;
#21212 = VERTEX_POINT('',#86684) ;
#21213 = VERTEX_POINT('',#86686) ;
#21214 = VERTEX_POINT('',#86688) ;
#21215 = VERTEX_POINT('',#86690) ;
#21216 = VERTEX_POINT('',#86692) ;
#21217 = VERTEX_POINT('',#86694) ;
#21218 = VERTEX_POINT('',#86696) ;
#21219 = VERTEX_POINT('',#86698) ;
#21220 = VERTEX_POINT('',#86700) ;
#21221 = VERTEX_POINT('',#86702) ;
#21222 = VERTEX_POINT('',#86704) ;
#21223 = VERTEX_POINT('',#86707) ;
#21224 = VERTEX_POINT('',#86708) ;
#21225 = VERTEX_POINT('',#86710) ;
#21226 = VERTEX_POINT('',#86712) ;
#21227 = VERTEX_POINT('',#86715) ;
#21228 = VERTEX_POINT('',#86716) ;
#21229 = VERTEX_POINT('',#86727) ;
#21230 = VERTEX_POINT('',#86729) ;
#21231 = VERTEX_POINT('',#86740) ;
#21232 = VERTEX_POINT('',#86742) ;
#21233 = VERTEX_POINT('',#86753) ;
#21234 = VERTEX_POINT('',#86755) ;
#21235 = VERTEX_POINT('',#86767) ;
#21236 = VERTEX_POINT('',#86768) ;
#21237 = VERTEX_POINT('',#86770) ;
#21238 = VERTEX_POINT('',#86781) ;
#21239 = VERTEX_POINT('',#86783) ;
#21240 = VERTEX_POINT('',#86794) ;
#21241 = VERTEX_POINT('',#86796) ;
#21242 = VERTEX_POINT('',#86807) ;
#21243 = VERTEX_POINT('',#86819) ;
#21244 = VERTEX_POINT('',#86820) ;
#21245 = VERTEX_POINT('',#86822) ;
#21246 = VERTEX_POINT('',#86833) ;
#21247 = VERTEX_POINT('',#86835) ;
#21248 = VERTEX_POINT('',#86846) ;
#21249 = VERTEX_POINT('',#86848) ;
#21250 = VERTEX_POINT('',#86859) ;
#21251 = VERTEX_POINT('',#86871) ;
#21252 = VERTEX_POINT('',#86872) ;
#21253 = VERTEX_POINT('',#86874) ;
#21254 = VERTEX_POINT('',#86885) ;
#21255 = VERTEX_POINT('',#86887) ;
#21256 = VERTEX_POINT('',#86898) ;
#21257 = VERTEX_POINT('',#86900) ;
#21258 = VERTEX_POINT('',#86911) ;
#21259 = VERTEX_POINT('',#86924) ;
#21260 = VERTEX_POINT('',#86928) ;
#21261 = VERTEX_POINT('',#86932) ;
#21262 = VERTEX_POINT('',#86936) ;
#21263 = VERTEX_POINT('',#86938) ;
#21264 = VERTEX_POINT('',#86940) ;
#21265 = VERTEX_POINT('',#86942) ;
#21266 = VERTEX_POINT('',#86944) ;
#21267 = VERTEX_POINT('',#86946) ;
#21268 = VERTEX_POINT('',#86948) ;
#21269 = VERTEX_POINT('',#86950) ;
#21270 = VERTEX_POINT('',#86952) ;
#21271 = VERTEX_POINT('',#86954) ;
#21272 = VERTEX_POINT('',#86956) ;
#21273 = VERTEX_POINT('',#86958) ;
#21274 = VERTEX_POINT('',#86960) ;
#21275 = VERTEX_POINT('',#86962) ;
#21276 = VERTEX_POINT('',#86964) ;
#21277 = VERTEX_POINT('',#86966) ;
#21278 = VERTEX_POINT('',#86968) ;
#21279 = VERTEX_POINT('',#86970) ;
#21280 = VERTEX_POINT('',#86972) ;
#21281 = VERTEX_POINT('',#86974) ;
#21282 = VERTEX_POINT('',#86976) ;
#21283 = VERTEX_POINT('',#86978) ;
#21284 = VERTEX_POINT('',#86981) ;
#21285 = VERTEX_POINT('',#86982) ;
#21286 = VERTEX_POINT('',#86984) ;
#21287 = VERTEX_POINT('',#86986) ;
#21288 = VERTEX_POINT('',#86989) ;
#21289 = VERTEX_POINT('',#86990) ;
#21290 = VERTEX_POINT('',#86992) ;
#21291 = VERTEX_POINT('',#86994) ;
#21292 = VERTEX_POINT('',#86998) ;
#21293 = VERTEX_POINT('',#87000) ;
#21294 = VERTEX_POINT('',#87004) ;
#21295 = VERTEX_POINT('',#87006) ;
#21296 = VERTEX_POINT('',#87013) ;
#21297 = VERTEX_POINT('',#87015) ;
#21298 = VERTEX_POINT('',#87019) ;
#21299 = VERTEX_POINT('',#87021) ;
#21300 = VERTEX_POINT('',#87028) ;
#21301 = VERTEX_POINT('',#87030) ;
#21302 = VERTEX_POINT('',#87036) ;
#21303 = VERTEX_POINT('',#87040) ;
#21304 = VERTEX_POINT('',#87042) ;
#21305 = VERTEX_POINT('',#87046) ;
#21306 = VERTEX_POINT('',#87056) ;
#21307 = VERTEX_POINT('',#87061) ;
#21308 = VERTEX_POINT('',#87067) ;
#21309 = VERTEX_POINT('',#87071) ;
#21310 = VERTEX_POINT('',#87101) ;
#21311 = VERTEX_POINT('',#87102) ;
#21312 = VERTEX_POINT('',#87104) ;
#21313 = VERTEX_POINT('',#87107) ;
#21314 = VERTEX_POINT('',#87111) ;
#21315 = VERTEX_POINT('',#87113) ;
#21316 = VERTEX_POINT('',#87141) ;
#21317 = VERTEX_POINT('',#87144) ;
#21318 = VERTEX_POINT('',#87148) ;
#21319 = VERTEX_POINT('',#87150) ;
#21320 = VERTEX_POINT('',#87156) ;
#21321 = VERTEX_POINT('',#87168) ;
#21322 = VERTEX_POINT('',#87187) ;
#21323 = VERTEX_POINT('',#87189) ;
#21324 = VERTEX_POINT('',#87193) ;
#21325 = VERTEX_POINT('',#87197) ;
#21326 = VERTEX_POINT('',#87208) ;
#21327 = VERTEX_POINT('',#87215) ;
#21328 = VERTEX_POINT('',#87222) ;
#21329 = VERTEX_POINT('',#87224) ;
#21330 = VERTEX_POINT('',#87244) ;
#21331 = VERTEX_POINT('',#87253) ;
#21332 = VERTEX_POINT('',#87263) ;
#21333 = VERTEX_POINT('',#87264) ;
#21334 = VERTEX_POINT('',#87269) ;
#21335 = VERTEX_POINT('',#87270) ;
#21336 = VERTEX_POINT('',#87279) ;
#21337 = VERTEX_POINT('',#87280) ;
#21338 = VERTEX_POINT('',#87285) ;
#21339 = VERTEX_POINT('',#87286) ;
#21340 = VERTEX_POINT('',#87295) ;
#21341 = VERTEX_POINT('',#87296) ;
#21342 = VERTEX_POINT('',#87301) ;
#21343 = VERTEX_POINT('',#87302) ;
#21344 = VERTEX_POINT('',#87311) ;
#21345 = VERTEX_POINT('',#87312) ;
#21346 = VERTEX_POINT('',#87317) ;
#21347 = VERTEX_POINT('',#87318) ;
#21348 = VERTEX_POINT('',#87327) ;
#21349 = VERTEX_POINT('',#87328) ;
#21350 = VERTEX_POINT('',#87333) ;
#21351 = VERTEX_POINT('',#87334) ;
#21352 = VERTEX_POINT('',#87343) ;
#21353 = VERTEX_POINT('',#87344) ;
#21354 = VERTEX_POINT('',#87349) ;
#21355 = VERTEX_POINT('',#87350) ;
#21356 = VERTEX_POINT('',#87359) ;
#21357 = VERTEX_POINT('',#87360) ;
#21358 = VERTEX_POINT('',#87365) ;
#21359 = VERTEX_POINT('',#87366) ;
#21360 = VERTEX_POINT('',#87375) ;
#21361 = VERTEX_POINT('',#87376) ;
#21362 = VERTEX_POINT('',#87381) ;
#21363 = VERTEX_POINT('',#87382) ;
#21364 = VERTEX_POINT('',#87411) ;
#21365 = VERTEX_POINT('',#87412) ;
#21366 = VERTEX_POINT('',#87414) ;
#21367 = VERTEX_POINT('',#87416) ;
#21368 = VERTEX_POINT('',#87447) ;
#21369 = VERTEX_POINT('',#87448) ;
#21370 = VERTEX_POINT('',#87450) ;
#21371 = VERTEX_POINT('',#87452) ;
#21372 = VERTEX_POINT('',#87456) ;
#21373 = VERTEX_POINT('',#87458) ;
#21374 = VERTEX_POINT('',#87462) ;
#21375 = VERTEX_POINT('',#87464) ;
#21376 = VERTEX_POINT('',#87474) ;
#21377 = VERTEX_POINT('',#87475) ;
#21378 = VERTEX_POINT('',#87477) ;
#21379 = VERTEX_POINT('',#87479) ;
#21380 = VERTEX_POINT('',#87484) ;
#21381 = VERTEX_POINT('',#87488) ;
#21382 = VERTEX_POINT('',#87494) ;
#21383 = VERTEX_POINT('',#87495) ;
#21384 = VERTEX_POINT('',#87497) ;
#21385 = VERTEX_POINT('',#87499) ;
#21386 = VERTEX_POINT('',#87504) ;
#21387 = VERTEX_POINT('',#87508) ;
#21388 = VERTEX_POINT('',#87514) ;
#21389 = VERTEX_POINT('',#87516) ;
#21390 = VERTEX_POINT('',#87520) ;
#21391 = VERTEX_POINT('',#87524) ;
#21392 = VERTEX_POINT('',#87527) ;
#21393 = VERTEX_POINT('',#87533) ;
#21394 = VERTEX_POINT('',#87534) ;
#21395 = VERTEX_POINT('',#87536) ;
#21396 = VERTEX_POINT('',#87538) ;
#21397 = VERTEX_POINT('',#87561) ;
#21398 = VERTEX_POINT('',#87562) ;
#21399 = VERTEX_POINT('',#87564) ;
#21400 = VERTEX_POINT('',#87571) ;
#21401 = VERTEX_POINT('',#87572) ;
#21402 = VERTEX_POINT('',#87574) ;
#21403 = VERTEX_POINT('',#87602) ;
#21404 = VERTEX_POINT('',#87603) ;
#21405 = VERTEX_POINT('',#87605) ;
#21406 = VERTEX_POINT('',#87607) ;
#21407 = VERTEX_POINT('',#87609) ;
#21408 = VERTEX_POINT('',#87616) ;
#21409 = VERTEX_POINT('',#87617) ;
#21410 = VERTEX_POINT('',#87619) ;
#21411 = VERTEX_POINT('',#87621) ;
#21412 = VERTEX_POINT('',#87644) ;
#21413 = VERTEX_POINT('',#87645) ;
#21414 = VERTEX_POINT('',#87647) ;
#21415 = VERTEX_POINT('',#87657) ;
#21416 = VERTEX_POINT('',#87658) ;
#21417 = VERTEX_POINT('',#87660) ;
#21418 = VERTEX_POINT('',#87662) ;
#21419 = VERTEX_POINT('',#87685) ;
#21420 = VERTEX_POINT('',#87686) ;
#21421 = VERTEX_POINT('',#87688) ;
#21422 = VERTEX_POINT('',#87695) ;
#21423 = VERTEX_POINT('',#87696) ;
#21424 = VERTEX_POINT('',#87698) ;
#21425 = VERTEX_POINT('',#87726) ;
#21426 = VERTEX_POINT('',#87727) ;
#21427 = VERTEX_POINT('',#87729) ;
#21428 = VERTEX_POINT('',#87731) ;
#21429 = VERTEX_POINT('',#87733) ;
#21430 = VERTEX_POINT('',#87743) ;
#21431 = VERTEX_POINT('',#87744) ;
#21432 = VERTEX_POINT('',#87746) ;
#21433 = VERTEX_POINT('',#87748) ;
#21434 = VERTEX_POINT('',#87771) ;
#21435 = VERTEX_POINT('',#87772) ;
#21436 = VERTEX_POINT('',#87774) ;
#21437 = VERTEX_POINT('',#87781) ;
#21438 = VERTEX_POINT('',#87782) ;
#21439 = VERTEX_POINT('',#87784) ;
#21440 = VERTEX_POINT('',#87786) ;
#21441 = VERTEX_POINT('',#87809) ;
#21442 = VERTEX_POINT('',#87810) ;
#21443 = VERTEX_POINT('',#87812) ;
#21444 = VERTEX_POINT('',#87822) ;
#21445 = VERTEX_POINT('',#87823) ;
#21446 = VERTEX_POINT('',#87825) ;
#21447 = VERTEX_POINT('',#87853) ;
#21448 = VERTEX_POINT('',#87854) ;
#21449 = VERTEX_POINT('',#87856) ;
#21450 = VERTEX_POINT('',#87858) ;
#21451 = VERTEX_POINT('',#87860) ;
#21452 = VERTEX_POINT('',#87867) ;
#21453 = VERTEX_POINT('',#87868) ;
#21454 = VERTEX_POINT('',#87870) ;
#21455 = VERTEX_POINT('',#87872) ;
#21456 = VERTEX_POINT('',#87895) ;
#21457 = VERTEX_POINT('',#87896) ;
#21458 = VERTEX_POINT('',#87898) ;
#21459 = VERTEX_POINT('',#87908) ;
#21460 = VERTEX_POINT('',#87909) ;
#21461 = VERTEX_POINT('',#87911) ;
#21462 = VERTEX_POINT('',#87913) ;
#21463 = VERTEX_POINT('',#87936) ;
#21464 = VERTEX_POINT('',#87937) ;
#21465 = VERTEX_POINT('',#87939) ;
#21466 = VERTEX_POINT('',#87946) ;
#21467 = VERTEX_POINT('',#87947) ;
#21468 = VERTEX_POINT('',#87949) ;
#21469 = VERTEX_POINT('',#87977) ;
#21470 = VERTEX_POINT('',#87978) ;
#21471 = VERTEX_POINT('',#87980) ;
#21472 = VERTEX_POINT('',#87982) ;
#21473 = VERTEX_POINT('',#87984) ;
#21474 = VERTEX_POINT('',#87994) ;
#21475 = VERTEX_POINT('',#87995) ;
#21476 = VERTEX_POINT('',#87997) ;
#21477 = VERTEX_POINT('',#87999) ;
#21478 = VERTEX_POINT('',#88022) ;
#21479 = VERTEX_POINT('',#88023) ;
#21480 = VERTEX_POINT('',#88025) ;
#21481 = VERTEX_POINT('',#88075) ;
#21482 = VERTEX_POINT('',#88104) ;
#21483 = VERTEX_POINT('',#88108) ;
#21484 = VERTEX_POINT('',#88110) ;
#21485 = VERTEX_POINT('',#88114) ;
#21486 = VERTEX_POINT('',#88121) ;
#21487 = VERTEX_POINT('',#88122) ;
#21488 = VERTEX_POINT('',#88124) ;
#21489 = VERTEX_POINT('',#88128) ;
#21490 = VERTEX_POINT('',#88129) ;
#21491 = VERTEX_POINT('',#88131) ;
#21492 = VERTEX_POINT('',#88135) ;
#21493 = VERTEX_POINT('',#88136) ;
#21494 = VERTEX_POINT('',#88138) ;
#21495 = VERTEX_POINT('',#88142) ;
#21496 = VERTEX_POINT('',#88144) ;
#21497 = VERTEX_POINT('',#88151) ;
#21498 = VERTEX_POINT('',#88152) ;
#21499 = VERTEX_POINT('',#88154) ;
#21500 = VERTEX_POINT('',#88158) ;
#21501 = VERTEX_POINT('',#88159) ;
#21502 = VERTEX_POINT('',#88161) ;
#21503 = VERTEX_POINT('',#88171) ;
#21504 = VERTEX_POINT('',#88172) ;
#21505 = VERTEX_POINT('',#88180) ;
#21506 = VERTEX_POINT('',#88182) ;
#21507 = VERTEX_POINT('',#88204) ;
#21508 = VERTEX_POINT('',#88206) ;
#21509 = VERTEX_POINT('',#88208) ;
#21510 = VERTEX_POINT('',#88212) ;
#21511 = VERTEX_POINT('',#88214) ;
#21512 = VERTEX_POINT('',#88219) ;
#21513 = VERTEX_POINT('',#88220) ;
#21514 = VERTEX_POINT('',#88222) ;
#21515 = VERTEX_POINT('',#88224) ;
#21516 = VERTEX_POINT('',#88228) ;
#21517 = VERTEX_POINT('',#88230) ;
#21518 = VERTEX_POINT('',#88234) ;
#21519 = VERTEX_POINT('',#88236) ;
#21520 = VERTEX_POINT('',#88240) ;
#21521 = VERTEX_POINT('',#88242) ;
#21522 = VERTEX_POINT('',#88246) ;
#21523 = VERTEX_POINT('',#88248) ;
#21524 = VERTEX_POINT('',#88252) ;
#21525 = VERTEX_POINT('',#88253) ;
#21526 = VERTEX_POINT('',#88255) ;
#21527 = VERTEX_POINT('',#88257) ;
#21528 = VERTEX_POINT('',#88261) ;
#21529 = VERTEX_POINT('',#88263) ;
#21530 = VERTEX_POINT('',#88270) ;
#21531 = VERTEX_POINT('',#88272) ;
#21532 = VERTEX_POINT('',#88276) ;
#21533 = VERTEX_POINT('',#88278) ;
#21534 = VERTEX_POINT('',#88282) ;
#21535 = VERTEX_POINT('',#88284) ;
#21536 = VERTEX_POINT('',#88291) ;
#21537 = VERTEX_POINT('',#88293) ;
#21538 = VERTEX_POINT('',#88297) ;
#21539 = VERTEX_POINT('',#88301) ;
#21540 = VERTEX_POINT('',#88305) ;
#21541 = VERTEX_POINT('',#88309) ;
#21542 = VERTEX_POINT('',#88313) ;
#21543 = VERTEX_POINT('',#88317) ;
#21544 = VERTEX_POINT('',#88320) ;
#21545 = VERTEX_POINT('',#88321) ;
#21546 = VERTEX_POINT('',#88323) ;
#21547 = VERTEX_POINT('',#88325) ;
#21548 = VERTEX_POINT('',#88329) ;
#21549 = VERTEX_POINT('',#88331) ;
#21550 = VERTEX_POINT('',#88335) ;
#21551 = VERTEX_POINT('',#88337) ;
#21552 = VERTEX_POINT('',#88341) ;
#21553 = VERTEX_POINT('',#88346) ;
#21554 = VERTEX_POINT('',#88350) ;
#21555 = VERTEX_POINT('',#88354) ;
#21556 = VERTEX_POINT('',#88358) ;
#21557 = VERTEX_POINT('',#88362) ;
#21558 = VERTEX_POINT('',#88366) ;
#21559 = VERTEX_POINT('',#88370) ;
#21560 = VERTEX_POINT('',#88372) ;
#21561 = VERTEX_POINT('',#88394) ;
#21562 = VERTEX_POINT('',#88395) ;
#21563 = VERTEX_POINT('',#88397) ;
#21564 = VERTEX_POINT('',#88399) ;
#21565 = VERTEX_POINT('',#88403) ;
#21566 = VERTEX_POINT('',#88405) ;
#21567 = VERTEX_POINT('',#88409) ;
#21568 = VERTEX_POINT('',#88411) ;
#21569 = VERTEX_POINT('',#88415) ;
#21570 = VERTEX_POINT('',#88417) ;
#21571 = VERTEX_POINT('',#88421) ;
#21572 = VERTEX_POINT('',#88423) ;
#21573 = VERTEX_POINT('',#88427) ;
#21574 = VERTEX_POINT('',#88429) ;
#21575 = VERTEX_POINT('',#88433) ;
#21576 = VERTEX_POINT('',#88435) ;
#21577 = VERTEX_POINT('',#88439) ;
#21578 = VERTEX_POINT('',#88441) ;
#21579 = VERTEX_POINT('',#88445) ;
#21580 = VERTEX_POINT('',#88447) ;
#21581 = VERTEX_POINT('',#88451) ;
#21582 = VERTEX_POINT('',#88453) ;
#21583 = VERTEX_POINT('',#88457) ;
#21584 = VERTEX_POINT('',#88459) ;
#21585 = VERTEX_POINT('',#88466) ;
#21586 = VERTEX_POINT('',#88468) ;
#21587 = VERTEX_POINT('',#88472) ;
#21588 = VERTEX_POINT('',#88476) ;
#21589 = VERTEX_POINT('',#88480) ;
#21590 = VERTEX_POINT('',#88484) ;
#21591 = VERTEX_POINT('',#88488) ;
#21592 = VERTEX_POINT('',#88493) ;
#21593 = VERTEX_POINT('',#88495) ;
#21594 = VERTEX_POINT('',#88497) ;
#21595 = VERTEX_POINT('',#88501) ;
#21596 = VERTEX_POINT('',#88503) ;
#21597 = VERTEX_POINT('',#88508) ;
#21598 = VERTEX_POINT('',#88509) ;
#21599 = VERTEX_POINT('',#88514) ;
#21600 = VERTEX_POINT('',#88518) ;
#21601 = VERTEX_POINT('',#88522) ;
#21602 = VERTEX_POINT('',#88526) ;
#21603 = VERTEX_POINT('',#88528) ;
#21604 = VERTEX_POINT('',#88532) ;
#21605 = VERTEX_POINT('',#88533) ;
#21606 = VERTEX_POINT('',#88535) ;
#21607 = VERTEX_POINT('',#88537) ;
#21608 = VERTEX_POINT('',#88541) ;
#21609 = VERTEX_POINT('',#88543) ;
#21610 = VERTEX_POINT('',#88550) ;
#21611 = VERTEX_POINT('',#88552) ;
#21612 = VERTEX_POINT('',#88557) ;
#21613 = VERTEX_POINT('',#88561) ;
#21614 = VERTEX_POINT('',#88573) ;
#21615 = VERTEX_POINT('',#88584) ;
#21616 = VERTEX_POINT('',#88585) ;
#21617 = VERTEX_POINT('',#88587) ;
#21618 = VERTEX_POINT('',#88589) ;
#21619 = VERTEX_POINT('',#88593) ;
#21620 = VERTEX_POINT('',#88595) ;
#21621 = VERTEX_POINT('',#88599) ;
#21622 = VERTEX_POINT('',#88601) ;
#21623 = VERTEX_POINT('',#88605) ;
#21624 = VERTEX_POINT('',#88607) ;
#21625 = VERTEX_POINT('',#88611) ;
#21626 = VERTEX_POINT('',#88613) ;
#21627 = VERTEX_POINT('',#88617) ;
#21628 = VERTEX_POINT('',#88619) ;
#21629 = VERTEX_POINT('',#88623) ;
#21630 = VERTEX_POINT('',#88625) ;
#21631 = VERTEX_POINT('',#88629) ;
#21632 = VERTEX_POINT('',#88631) ;
#21633 = VERTEX_POINT('',#88635) ;
#21634 = VERTEX_POINT('',#88637) ;
#21635 = VERTEX_POINT('',#88641) ;
#21636 = VERTEX_POINT('',#88643) ;
#21637 = VERTEX_POINT('',#88647) ;
#21638 = VERTEX_POINT('',#88649) ;
#21639 = VERTEX_POINT('',#88656) ;
#21640 = VERTEX_POINT('',#88658) ;
#21641 = VERTEX_POINT('',#88662) ;
#21642 = VERTEX_POINT('',#88666) ;
#21643 = VERTEX_POINT('',#88670) ;
#21644 = VERTEX_POINT('',#88674) ;
#21645 = VERTEX_POINT('',#88678) ;
#21646 = VERTEX_POINT('',#88683) ;
#21647 = VERTEX_POINT('',#88685) ;
#21648 = VERTEX_POINT('',#88687) ;
#21649 = VERTEX_POINT('',#88691) ;
#21650 = VERTEX_POINT('',#88693) ;
#21651 = VERTEX_POINT('',#88698) ;
#21652 = VERTEX_POINT('',#88699) ;
#21653 = VERTEX_POINT('',#88704) ;
#21654 = VERTEX_POINT('',#88708) ;
#21655 = VERTEX_POINT('',#88712) ;
#21656 = VERTEX_POINT('',#88716) ;
#21657 = VERTEX_POINT('',#88718) ;
#21658 = VERTEX_POINT('',#88722) ;
#21659 = VERTEX_POINT('',#88723) ;
#21660 = VERTEX_POINT('',#88725) ;
#21661 = VERTEX_POINT('',#88727) ;
#21662 = VERTEX_POINT('',#88731) ;
#21663 = VERTEX_POINT('',#88733) ;
#21664 = VERTEX_POINT('',#88740) ;
#21665 = VERTEX_POINT('',#88742) ;
#21666 = VERTEX_POINT('',#88747) ;
#21667 = VERTEX_POINT('',#88751) ;
#21668 = VERTEX_POINT('',#88763) ;
#21669 = VERTEX_POINT('',#88774) ;
#21670 = VERTEX_POINT('',#88775) ;
#21671 = VERTEX_POINT('',#88777) ;
#21672 = VERTEX_POINT('',#88781) ;
#21673 = VERTEX_POINT('',#88782) ;
#21674 = VERTEX_POINT('',#88784) ;
#21675 = VERTEX_POINT('',#88791) ;
#21676 = VERTEX_POINT('',#88792) ;
#21677 = VERTEX_POINT('',#88794) ;
#21678 = VERTEX_POINT('',#88801) ;
#21679 = VERTEX_POINT('',#88802) ;
#21680 = VERTEX_POINT('',#88804) ;
#21681 = VERTEX_POINT('',#88806) ;
#21682 = VERTEX_POINT('',#88839) ;
#21683 = VERTEX_POINT('',#88840) ;
#21684 = VERTEX_POINT('',#88842) ;
#21685 = VERTEX_POINT('',#88844) ;
#21686 = VERTEX_POINT('',#88854) ;
#21687 = VERTEX_POINT('',#88855) ;
#21688 = VERTEX_POINT('',#88857) ;
#21689 = VERTEX_POINT('',#88867) ;
#21690 = VERTEX_POINT('',#88868) ;
#21691 = VERTEX_POINT('',#88870) ;
#21692 = VERTEX_POINT('',#88872) ;
#21693 = VERTEX_POINT('',#88900) ;
#21694 = VERTEX_POINT('',#88901) ;
#21695 = VERTEX_POINT('',#88903) ;
#21696 = VERTEX_POINT('',#88905) ;
#21697 = VERTEX_POINT('',#88932) ;
#21698 = VERTEX_POINT('',#88933) ;
#21699 = VERTEX_POINT('',#88935) ;
#21700 = VERTEX_POINT('',#88939) ;
#21701 = VERTEX_POINT('',#88940) ;
#21702 = VERTEX_POINT('',#88942) ;
#21703 = VERTEX_POINT('',#88949) ;
#21704 = VERTEX_POINT('',#88951) ;
#21705 = VERTEX_POINT('',#88955) ;
#21706 = VERTEX_POINT('',#88956) ;
#21707 = VERTEX_POINT('',#88958) ;
#21708 = VERTEX_POINT('',#88965) ;
#21709 = VERTEX_POINT('',#88970) ;
#21710 = VERTEX_POINT('',#88971) ;
#21711 = VERTEX_POINT('',#88976) ;
#21712 = VERTEX_POINT('',#88977) ;
#21713 = VERTEX_POINT('',#88982) ;
#21714 = VERTEX_POINT('',#88983) ;
#21715 = VERTEX_POINT('',#88990) ;
#21716 = VERTEX_POINT('',#89078) ;
#21717 = VERTEX_POINT('',#89079) ;
#21718 = VERTEX_POINT('',#89093) ;
#21719 = VERTEX_POINT('',#89100) ;
#21720 = VERTEX_POINT('',#89244) ;
#21721 = VERTEX_POINT('',#89258) ;
#21722 = VERTEX_POINT('',#89405) ;
#21723 = VERTEX_POINT('',#89412) ;
#21724 = VERTEX_POINT('',#89456) ;
#21725 = VERTEX_POINT('',#89624) ;
#21726 = VERTEX_POINT('',#89636) ;
#21727 = VERTEX_POINT('',#89804) ;
#21728 = VERTEX_POINT('',#89811) ;
#21729 = VERTEX_POINT('',#89875) ;
#21730 = VERTEX_POINT('',#89876) ;
#21731 = VERTEX_POINT('',#89878) ;
#21732 = VERTEX_POINT('',#89880) ;
#21733 = VERTEX_POINT('',#89893) ;
#21734 = VERTEX_POINT('',#89899) ;
#21735 = VERTEX_POINT('',#89916) ;
#21736 = VERTEX_POINT('',#89922) ;
#21737 = VERTEX_POINT('',#89939) ;
#21738 = VERTEX_POINT('',#89945) ;
#21739 = VERTEX_POINT('',#89962) ;
#21740 = VERTEX_POINT('',#89968) ;
#21741 = VERTEX_POINT('',#89985) ;
#21742 = VERTEX_POINT('',#89991) ;
#21743 = VERTEX_POINT('',#89999) ;
#21744 = VERTEX_POINT('',#90001) ;
#21745 = VERTEX_POINT('',#90008) ;
#21746 = VERTEX_POINT('',#90009) ;
#21747 = VERTEX_POINT('',#90011) ;
#21748 = VERTEX_POINT('',#90013) ;
#21749 = VERTEX_POINT('',#90017) ;
#21750 = VERTEX_POINT('',#90019) ;
#21751 = VERTEX_POINT('',#90032) ;
#21752 = VERTEX_POINT('',#90038) ;
#21753 = VERTEX_POINT('',#90055) ;
#21754 = VERTEX_POINT('',#90061) ;
#21755 = VERTEX_POINT('',#90078) ;
#21756 = VERTEX_POINT('',#90084) ;
#21757 = VERTEX_POINT('',#90101) ;
#21758 = VERTEX_POINT('',#90107) ;
#21759 = VERTEX_POINT('',#90115) ;
#21760 = VERTEX_POINT('',#90117) ;
#21761 = VERTEX_POINT('',#90121) ;
#21762 = VERTEX_POINT('',#90123) ;
#21763 = VERTEX_POINT('',#90127) ;
#21764 = VERTEX_POINT('',#90129) ;
#21765 = VERTEX_POINT('',#90142) ;
#21766 = VERTEX_POINT('',#90148) ;
#21767 = VERTEX_POINT('',#90165) ;
#21768 = VERTEX_POINT('',#90171) ;
#21769 = VERTEX_POINT('',#90188) ;
#21770 = VERTEX_POINT('',#90194) ;
#21771 = VERTEX_POINT('',#90211) ;
#21772 = VERTEX_POINT('',#90217) ;
#21773 = VERTEX_POINT('',#90234) ;
#21774 = VERTEX_POINT('',#90240) ;
#21775 = VERTEX_POINT('',#90257) ;
#21776 = VERTEX_POINT('',#90263) ;
#21777 = VERTEX_POINT('',#90280) ;
#21778 = VERTEX_POINT('',#90286) ;
#21779 = VERTEX_POINT('',#90294) ;
#21780 = VERTEX_POINT('',#90296) ;
#21781 = VERTEX_POINT('',#90300) ;
#21782 = VERTEX_POINT('',#90302) ;
#21783 = VERTEX_POINT('',#90310) ;
#21784 = VERTEX_POINT('',#90311) ;
#21785 = VERTEX_POINT('',#90313) ;
#21786 = VERTEX_POINT('',#90315) ;
#21787 = VERTEX_POINT('',#90317) ;
#21788 = VERTEX_POINT('',#90319) ;
#21789 = VERTEX_POINT('',#90321) ;
#21790 = VERTEX_POINT('',#90323) ;
#21791 = VERTEX_POINT('',#90325) ;
#21792 = VERTEX_POINT('',#90327) ;
#21793 = VERTEX_POINT('',#90329) ;
#21794 = VERTEX_POINT('',#90331) ;
#21795 = VERTEX_POINT('',#90333) ;
#21796 = VERTEX_POINT('',#90335) ;
#21797 = VERTEX_POINT('',#90337) ;
#21798 = VERTEX_POINT('',#90339) ;
#21799 = VERTEX_POINT('',#90341) ;
#21800 = VERTEX_POINT('',#90343) ;
#21801 = VERTEX_POINT('',#90346) ;
#21802 = VERTEX_POINT('',#90347) ;
#21803 = VERTEX_POINT('',#90349) ;
#21804 = VERTEX_POINT('',#90351) ;
#21805 = VERTEX_POINT('',#90362) ;
#21806 = VERTEX_POINT('',#90363) ;
#21807 = VERTEX_POINT('',#90365) ;
#21808 = VERTEX_POINT('',#90367) ;
#21809 = VERTEX_POINT('',#90382) ;
#21810 = VERTEX_POINT('',#90389) ;
#21811 = VERTEX_POINT('',#90398) ;
#21812 = VERTEX_POINT('',#90399) ;
#21813 = VERTEX_POINT('',#90401) ;
#21814 = VERTEX_POINT('',#90403) ;
#21815 = VERTEX_POINT('',#90414) ;
#21816 = VERTEX_POINT('',#90415) ;
#21817 = VERTEX_POINT('',#90428) ;
#21818 = VERTEX_POINT('',#90429) ;
#21819 = VERTEX_POINT('',#90434) ;
#21820 = VERTEX_POINT('',#90435) ;
#21821 = VERTEX_POINT('',#90437) ;
#21822 = VERTEX_POINT('',#90464) ;
#21823 = VERTEX_POINT('',#90465) ;
#21824 = VERTEX_POINT('',#90494) ;
#21825 = VERTEX_POINT('',#90508) ;
#21826 = VERTEX_POINT('',#90510) ;
#21827 = VERTEX_POINT('',#90512) ;
#21828 = VERTEX_POINT('',#90514) ;
#21829 = VERTEX_POINT('',#90518) ;
#21830 = VERTEX_POINT('',#90522) ;
#21831 = VERTEX_POINT('',#90550) ;
#21832 = VERTEX_POINT('',#90551) ;
#21833 = VERTEX_POINT('',#90558) ;
#21834 = VERTEX_POINT('',#90560) ;
#21835 = VERTEX_POINT('',#90562) ;
#21836 = VERTEX_POINT('',#90564) ;
#21837 = VERTEX_POINT('',#90578) ;
#21838 = VERTEX_POINT('',#90592) ;
#21839 = VERTEX_POINT('',#90593) ;
#21840 = VERTEX_POINT('',#90606) ;
#21841 = VERTEX_POINT('',#90607) ;
#21842 = VERTEX_POINT('',#90612) ;
#21843 = VERTEX_POINT('',#90613) ;
#21844 = VERTEX_POINT('',#90618) ;
#21845 = VERTEX_POINT('',#90619) ;
#21846 = VERTEX_POINT('',#90629) ;
#21847 = VERTEX_POINT('',#90631) ;
#21848 = VERTEX_POINT('',#90635) ;
#21849 = VERTEX_POINT('',#90639) ;
#21850 = VERTEX_POINT('',#90708) ;
#21851 = VERTEX_POINT('',#90710) ;
#21852 = VERTEX_POINT('',#90723) ;
#21853 = VERTEX_POINT('',#90756) ;
#21854 = VERTEX_POINT('',#90763) ;
#21855 = VERTEX_POINT('',#90772) ;
#21856 = VERTEX_POINT('',#90774) ;
#21857 = VERTEX_POINT('',#90776) ;
#21858 = VERTEX_POINT('',#90782) ;
#21859 = VERTEX_POINT('',#90784) ;
#21860 = VERTEX_POINT('',#90786) ;
#21861 = VERTEX_POINT('',#90788) ;
#21862 = VERTEX_POINT('',#90790) ;
#21863 = VERTEX_POINT('',#90792) ;
#21864 = VERTEX_POINT('',#90794) ;
#21865 = VERTEX_POINT('',#90796) ;
#21866 = VERTEX_POINT('',#90824) ;
#21867 = VERTEX_POINT('',#90825) ;
#21868 = VERTEX_POINT('',#90827) ;
#21869 = VERTEX_POINT('',#90829) ;
#21870 = VERTEX_POINT('',#90831) ;
#21871 = VERTEX_POINT('',#90835) ;
#21872 = VERTEX_POINT('',#90836) ;
#21873 = VERTEX_POINT('',#90860) ;
#21874 = VERTEX_POINT('',#90861) ;
#21875 = VERTEX_POINT('',#90889) ;
#21876 = VERTEX_POINT('',#90903) ;
#21877 = VERTEX_POINT('',#90905) ;
#21878 = VERTEX_POINT('',#90909) ;
#21879 = VERTEX_POINT('',#90911) ;
#21880 = VERTEX_POINT('',#90915) ;
#21881 = VERTEX_POINT('',#90943) ;
#21882 = VERTEX_POINT('',#90944) ;
#21883 = VERTEX_POINT('',#90946) ;
#21884 = VERTEX_POINT('',#90948) ;
#21885 = VERTEX_POINT('',#90950) ;
#21886 = VERTEX_POINT('',#90954) ;
#21887 = VERTEX_POINT('',#90955) ;
#21888 = VERTEX_POINT('',#90979) ;
#21889 = VERTEX_POINT('',#90980) ;
#21890 = VERTEX_POINT('',#91008) ;
#21891 = VERTEX_POINT('',#91019) ;
#21892 = VERTEX_POINT('',#91031) ;
#21893 = VERTEX_POINT('',#91033) ;
#21894 = VERTEX_POINT('',#91035) ;
#21895 = VERTEX_POINT('',#91037) ;
#21896 = VERTEX_POINT('',#91039) ;
#21897 = VERTEX_POINT('',#91041) ;
#21898 = VERTEX_POINT('',#91044) ;
#21899 = VERTEX_POINT('',#91046) ;
#21900 = VERTEX_POINT('',#91048) ;
#21901 = VERTEX_POINT('',#91050) ;
#21902 = VERTEX_POINT('',#91054) ;
#21903 = VERTEX_POINT('',#91058) ;
#21904 = VERTEX_POINT('',#91060) ;
#21905 = VERTEX_POINT('',#91083) ;
#21906 = VERTEX_POINT('',#91084) ;
#21907 = VERTEX_POINT('',#91086) ;
#21908 = VERTEX_POINT('',#91090) ;
#21909 = VERTEX_POINT('',#91092) ;
#21910 = VERTEX_POINT('',#91096) ;
#21911 = VERTEX_POINT('',#91098) ;
#21912 = VERTEX_POINT('',#91109) ;
#21913 = VERTEX_POINT('',#91111) ;
#21914 = VERTEX_POINT('',#91115) ;
#21915 = VERTEX_POINT('',#91117) ;
#21916 = VERTEX_POINT('',#91119) ;
#21917 = VERTEX_POINT('',#91121) ;
#21918 = VERTEX_POINT('',#91123) ;
#21919 = VERTEX_POINT('',#91125) ;
#21920 = VERTEX_POINT('',#91127) ;
#21921 = VERTEX_POINT('',#91133) ;
#21922 = VERTEX_POINT('',#91137) ;
#21923 = VERTEX_POINT('',#91141) ;
#21924 = VERTEX_POINT('',#91143) ;
#21925 = VERTEX_POINT('',#91147) ;
#21926 = VERTEX_POINT('',#91180) ;
#21927 = VERTEX_POINT('',#91181) ;
#21928 = VERTEX_POINT('',#91183) ;
#21929 = VERTEX_POINT('',#91185) ;
#21930 = VERTEX_POINT('',#91192) ;
#21931 = VERTEX_POINT('',#91194) ;
#21932 = VERTEX_POINT('',#91196) ;
#21933 = VERTEX_POINT('',#91200) ;
#21934 = VERTEX_POINT('',#91204) ;
#21935 = VERTEX_POINT('',#91206) ;
#21936 = VERTEX_POINT('',#91208) ;
#21937 = VERTEX_POINT('',#91210) ;
#21938 = VERTEX_POINT('',#91214) ;
#21939 = VERTEX_POINT('',#91216) ;
#21940 = VERTEX_POINT('',#91218) ;
#21941 = VERTEX_POINT('',#91224) ;
#21942 = VERTEX_POINT('',#91226) ;
#21943 = VERTEX_POINT('',#91230) ;
#21944 = VERTEX_POINT('',#91232) ;
#21945 = VERTEX_POINT('',#91234) ;
#21946 = VERTEX_POINT('',#91238) ;
#21947 = VERTEX_POINT('',#91240) ;
#21948 = VERTEX_POINT('',#91246) ;
#21949 = VERTEX_POINT('',#91250) ;
#21950 = VERTEX_POINT('',#91252) ;
#21951 = VERTEX_POINT('',#91256) ;
#21952 = VERTEX_POINT('',#91262) ;
#21953 = VERTEX_POINT('',#91264) ;
#21954 = VERTEX_POINT('',#91268) ;
#21955 = VERTEX_POINT('',#91269) ;
#21956 = VERTEX_POINT('',#91274) ;
#21957 = VERTEX_POINT('',#91281) ;
#21958 = VERTEX_POINT('',#91283) ;
#21959 = VERTEX_POINT('',#91285) ;
#21960 = VERTEX_POINT('',#91287) ;
#21961 = VERTEX_POINT('',#91289) ;
#21962 = VERTEX_POINT('',#91293) ;
#21963 = VERTEX_POINT('',#91297) ;
#21964 = VERTEX_POINT('',#91299) ;
#21965 = VERTEX_POINT('',#91301) ;
#21966 = VERTEX_POINT('',#91303) ;
#21967 = VERTEX_POINT('',#91305) ;
#21968 = VERTEX_POINT('',#91309) ;
#21969 = VERTEX_POINT('',#91320) ;
#21970 = VERTEX_POINT('',#91321) ;
#21971 = VERTEX_POINT('',#91323) ;
#21972 = VERTEX_POINT('',#91327) ;
#21973 = VERTEX_POINT('',#91328) ;
#21974 = VERTEX_POINT('',#91333) ;
#21975 = VERTEX_POINT('',#91334) ;
#21976 = VERTEX_POINT('',#91351) ;
#21977 = VERTEX_POINT('',#91353) ;
#21978 = VERTEX_POINT('',#91357) ;
#21979 = VERTEX_POINT('',#91358) ;
#21980 = VERTEX_POINT('',#91363) ;
#21981 = VERTEX_POINT('',#91364) ;
#21982 = VERTEX_POINT('',#91369) ;
#21983 = VERTEX_POINT('',#91370) ;
#21984 = VERTEX_POINT('',#91375) ;
#21985 = VERTEX_POINT('',#91376) ;
#21986 = VERTEX_POINT('',#91381) ;
#21987 = VERTEX_POINT('',#91382) ;
#21988 = VERTEX_POINT('',#91390) ;
#21989 = VERTEX_POINT('',#91391) ;
#21990 = VERTEX_POINT('',#91396) ;
#21991 = VERTEX_POINT('',#91397) ;
#21992 = VERTEX_POINT('',#91407) ;
#21993 = VERTEX_POINT('',#91409) ;
#21994 = VERTEX_POINT('',#91411) ;
#21995 = VERTEX_POINT('',#91413) ;
#21996 = VERTEX_POINT('',#91415) ;
#21997 = VERTEX_POINT('',#91417) ;
#21998 = VERTEX_POINT('',#91419) ;
#21999 = VERTEX_POINT('',#91421) ;
#22000 = VERTEX_POINT('',#91423) ;
#22001 = VERTEX_POINT('',#91427) ;
#22002 = VERTEX_POINT('',#91431) ;
#22003 = VERTEX_POINT('',#91435) ;
#22004 = VERTEX_POINT('',#91436) ;
#22005 = VERTEX_POINT('',#91438) ;
#22006 = VERTEX_POINT('',#91440) ;
#22007 = VERTEX_POINT('',#91442) ;
#22008 = VERTEX_POINT('',#91487) ;
#22009 = VERTEX_POINT('',#91488) ;
#22010 = VERTEX_POINT('',#91513) ;
#22011 = VERTEX_POINT('',#91515) ;
#22012 = VERTEX_POINT('',#91519) ;
#22013 = VERTEX_POINT('',#91521) ;
#22014 = VERTEX_POINT('',#91554) ;
#22015 = VERTEX_POINT('',#91561) ;
#22016 = VERTEX_POINT('',#91573) ;
#22017 = VERTEX_POINT('',#91575) ;
#22018 = VERTEX_POINT('',#91579) ;
#22019 = VERTEX_POINT('',#91580) ;
#22020 = VERTEX_POINT('',#91583) ;
#22021 = VERTEX_POINT('',#91587) ;
#22022 = VERTEX_POINT('',#91593) ;
#22023 = VERTEX_POINT('',#91616) ;
#22024 = VERTEX_POINT('',#91621) ;
#22025 = VERTEX_POINT('',#91647) ;
#22026 = VERTEX_POINT('',#91648) ;
#22027 = VERTEX_POINT('',#91653) ;
#22028 = VERTEX_POINT('',#91654) ;
#22029 = VERTEX_POINT('',#91683) ;
#22030 = VERTEX_POINT('',#91684) ;
#22031 = VERTEX_POINT('',#91696) ;
#22032 = VERTEX_POINT('',#91705) ;
#22033 = VERTEX_POINT('',#91707) ;
#22034 = VERTEX_POINT('',#91711) ;
#22035 = VERTEX_POINT('',#91715) ;
#22036 = VERTEX_POINT('',#91719) ;
#22037 = VERTEX_POINT('',#91723) ;
#22038 = VERTEX_POINT('',#91724) ;
#22039 = VERTEX_POINT('',#91729) ;
#22040 = VERTEX_POINT('',#91730) ;
#22041 = VERTEX_POINT('',#91738) ;
#22042 = VERTEX_POINT('',#91742) ;
#22043 = VERTEX_POINT('',#91746) ;
#22044 = VERTEX_POINT('',#91750) ;
#22045 = VERTEX_POINT('',#91752) ;
#22046 = VERTEX_POINT('',#91754) ;
#22047 = VERTEX_POINT('',#91758) ;
#22048 = VERTEX_POINT('',#91762) ;
#22049 = VERTEX_POINT('',#91789) ;
#22050 = VERTEX_POINT('',#91790) ;
#22051 = VERTEX_POINT('',#91792) ;
#22052 = VERTEX_POINT('',#91812) ;
#22053 = VERTEX_POINT('',#91820) ;
#22054 = VERTEX_POINT('',#91851) ;
#22055 = VERTEX_POINT('',#91852) ;
#22056 = VERTEX_POINT('',#91857) ;
#22057 = VERTEX_POINT('',#91858) ;
#22058 = VERTEX_POINT('',#91882) ;
#22059 = VERTEX_POINT('',#91883) ;
#22060 = VERTEX_POINT('',#91907) ;
#22061 = VERTEX_POINT('',#91908) ;
#22062 = VERTEX_POINT('',#91928) ;
#22063 = VERTEX_POINT('',#91930) ;
#22064 = VERTEX_POINT('',#91943) ;
#22065 = VERTEX_POINT('',#91945) ;
#22066 = VERTEX_POINT('',#91950) ;
#22067 = VERTEX_POINT('',#91954) ;
#22068 = VERTEX_POINT('',#91956) ;
#22069 = VERTEX_POINT('',#91958) ;
#22070 = VERTEX_POINT('',#91960) ;
#22071 = VERTEX_POINT('',#91969) ;
#22072 = VERTEX_POINT('',#91975) ;
#22073 = VERTEX_POINT('',#91979) ;
#22074 = VERTEX_POINT('',#91981) ;
#22075 = VERTEX_POINT('',#91998) ;
#22076 = VERTEX_POINT('',#92015) ;
#22077 = VERTEX_POINT('',#92021) ;
#22078 = VERTEX_POINT('',#92023) ;
#22079 = VERTEX_POINT('',#92027) ;
#22080 = VERTEX_POINT('',#92051) ;
#22081 = VERTEX_POINT('',#92052) ;
#22082 = VERTEX_POINT('',#92054) ;
#22083 = VERTEX_POINT('',#92058) ;
#22084 = VERTEX_POINT('',#92059) ;
#22085 = VERTEX_POINT('',#92064) ;
#22086 = VERTEX_POINT('',#92065) ;
#22087 = VERTEX_POINT('',#92091) ;
#22088 = VERTEX_POINT('',#92093) ;
#22089 = VERTEX_POINT('',#92095) ;
#22090 = VERTEX_POINT('',#92097) ;
#22091 = VERTEX_POINT('',#92101) ;
#22092 = VERTEX_POINT('',#92105) ;
#22093 = VERTEX_POINT('',#92107) ;
#22094 = VERTEX_POINT('',#92111) ;
#22095 = VERTEX_POINT('',#92112) ;
#22096 = VERTEX_POINT('',#92114) ;
#22097 = VERTEX_POINT('',#92124) ;
#22098 = VERTEX_POINT('',#92125) ;
#22099 = VERTEX_POINT('',#92127) ;
#22100 = VERTEX_POINT('',#92129) ;
#22101 = VERTEX_POINT('',#92142) ;
#22102 = VERTEX_POINT('',#92144) ;
#22103 = VERTEX_POINT('',#92146) ;
#22104 = VERTEX_POINT('',#92148) ;
#22105 = VERTEX_POINT('',#92150) ;
#22106 = VERTEX_POINT('',#92152) ;
#22107 = VERTEX_POINT('',#92154) ;
#22108 = VERTEX_POINT('',#92156) ;
#22109 = VERTEX_POINT('',#92158) ;
#22110 = VERTEX_POINT('',#92160) ;
#22111 = VERTEX_POINT('',#92162) ;
#22112 = VERTEX_POINT('',#92164) ;
#22113 = VERTEX_POINT('',#92166) ;
#22114 = VERTEX_POINT('',#92168) ;
#22115 = VERTEX_POINT('',#92170) ;
#22116 = VERTEX_POINT('',#92172) ;
#22117 = VERTEX_POINT('',#92174) ;
#22118 = VERTEX_POINT('',#92176) ;
#22119 = VERTEX_POINT('',#92178) ;
#22120 = VERTEX_POINT('',#92180) ;
#22121 = VERTEX_POINT('',#92182) ;
#22122 = VERTEX_POINT('',#92184) ;
#22123 = VERTEX_POINT('',#92186) ;
#22124 = VERTEX_POINT('',#92188) ;
#22125 = VERTEX_POINT('',#92190) ;
#22126 = VERTEX_POINT('',#92192) ;
#22127 = VERTEX_POINT('',#92194) ;
#22128 = VERTEX_POINT('',#92196) ;
#22129 = VERTEX_POINT('',#92198) ;
#22130 = VERTEX_POINT('',#92200) ;
#22131 = VERTEX_POINT('',#92202) ;
#22132 = VERTEX_POINT('',#92204) ;
#22133 = VERTEX_POINT('',#92206) ;
#22134 = VERTEX_POINT('',#92208) ;
#22135 = VERTEX_POINT('',#92210) ;
#22136 = VERTEX_POINT('',#92212) ;
#22137 = VERTEX_POINT('',#92214) ;
#22138 = VERTEX_POINT('',#92216) ;
#22139 = VERTEX_POINT('',#92218) ;
#22140 = VERTEX_POINT('',#92220) ;
#22141 = VERTEX_POINT('',#92222) ;
#22142 = VERTEX_POINT('',#92224) ;
#22143 = VERTEX_POINT('',#92226) ;
#22144 = VERTEX_POINT('',#92233) ;
#22145 = VERTEX_POINT('',#92235) ;
#22146 = VERTEX_POINT('',#92242) ;
#22147 = VERTEX_POINT('',#92244) ;
#22148 = VERTEX_POINT('',#92246) ;
#22149 = VERTEX_POINT('',#92248) ;
#22150 = VERTEX_POINT('',#92250) ;
#22151 = VERTEX_POINT('',#92252) ;
#22152 = VERTEX_POINT('',#92254) ;
#22153 = VERTEX_POINT('',#92256) ;
#22154 = VERTEX_POINT('',#92258) ;
#22155 = VERTEX_POINT('',#92260) ;
#22156 = VERTEX_POINT('',#92262) ;
#22157 = VERTEX_POINT('',#92264) ;
#22158 = VERTEX_POINT('',#92266) ;
#22159 = VERTEX_POINT('',#92275) ;
#22160 = VERTEX_POINT('',#92277) ;
#22161 = VERTEX_POINT('',#92279) ;
#22162 = VERTEX_POINT('',#92281) ;
#22163 = VERTEX_POINT('',#92283) ;
#22164 = VERTEX_POINT('',#92285) ;
#22165 = VERTEX_POINT('',#92287) ;
#22166 = VERTEX_POINT('',#92289) ;
#22167 = VERTEX_POINT('',#92291) ;
#22168 = VERTEX_POINT('',#92293) ;
#22169 = VERTEX_POINT('',#92295) ;
#22170 = VERTEX_POINT('',#92297) ;
#22171 = VERTEX_POINT('',#92299) ;
#22172 = VERTEX_POINT('',#92301) ;
#22173 = VERTEX_POINT('',#92303) ;
#22174 = VERTEX_POINT('',#92305) ;
#22175 = VERTEX_POINT('',#92307) ;
#22176 = VERTEX_POINT('',#92309) ;
#22177 = VERTEX_POINT('',#92311) ;
#22178 = VERTEX_POINT('',#92313) ;
#22179 = VERTEX_POINT('',#92315) ;
#22180 = VERTEX_POINT('',#92317) ;
#22181 = VERTEX_POINT('',#92319) ;
#22182 = VERTEX_POINT('',#92321) ;
#22183 = VERTEX_POINT('',#92323) ;
#22184 = VERTEX_POINT('',#92325) ;
#22185 = VERTEX_POINT('',#92327) ;
#22186 = VERTEX_POINT('',#92329) ;
#22187 = VERTEX_POINT('',#92331) ;
#22188 = VERTEX_POINT('',#92333) ;
#22189 = VERTEX_POINT('',#92336) ;
#22190 = VERTEX_POINT('',#92338) ;
#22191 = VERTEX_POINT('',#92340) ;
#22192 = VERTEX_POINT('',#92342) ;
#22193 = VERTEX_POINT('',#92344) ;
#22194 = VERTEX_POINT('',#92346) ;
#22195 = VERTEX_POINT('',#92348) ;
#22196 = VERTEX_POINT('',#92350) ;
#22197 = VERTEX_POINT('',#92352) ;
#22198 = VERTEX_POINT('',#92354) ;
#22199 = VERTEX_POINT('',#92356) ;
#22200 = VERTEX_POINT('',#92359) ;
#22201 = VERTEX_POINT('',#92360) ;
#22202 = VERTEX_POINT('',#92362) ;
#22203 = VERTEX_POINT('',#92364) ;
#22204 = VERTEX_POINT('',#92366) ;
#22205 = VERTEX_POINT('',#92368) ;
#22206 = VERTEX_POINT('',#92370) ;
#22207 = VERTEX_POINT('',#92372) ;
#22208 = VERTEX_POINT('',#92375) ;
#22209 = VERTEX_POINT('',#92377) ;
#22210 = VERTEX_POINT('',#92378) ;
#22211 = VERTEX_POINT('',#92380) ;
#22212 = VERTEX_POINT('',#92382) ;
#22213 = VERTEX_POINT('',#92384) ;
#22214 = VERTEX_POINT('',#92386) ;
#22215 = VERTEX_POINT('',#92388) ;
#22216 = VERTEX_POINT('',#92390) ;
#22217 = VERTEX_POINT('',#92392) ;
#22218 = VERTEX_POINT('',#92394) ;
#22219 = VERTEX_POINT('',#92396) ;
#22220 = VERTEX_POINT('',#92398) ;
#22221 = VERTEX_POINT('',#92400) ;
#22222 = VERTEX_POINT('',#92402) ;
#22223 = VERTEX_POINT('',#92405) ;
#22224 = VERTEX_POINT('',#92407) ;
#22225 = VERTEX_POINT('',#92408) ;
#22226 = VERTEX_POINT('',#92410) ;
#22227 = VERTEX_POINT('',#92417) ;
#22228 = VERTEX_POINT('',#92419) ;
#22229 = VERTEX_POINT('',#92421) ;
#22230 = VERTEX_POINT('',#92423) ;
#22231 = VERTEX_POINT('',#92425) ;
#22232 = VERTEX_POINT('',#92427) ;
#22233 = VERTEX_POINT('',#92429) ;
#22234 = VERTEX_POINT('',#92431) ;
#22235 = VERTEX_POINT('',#92433) ;
#22236 = VERTEX_POINT('',#92441) ;
#22237 = VERTEX_POINT('',#92442) ;
#22238 = VERTEX_POINT('',#92450) ;
#22239 = VERTEX_POINT('',#92452) ;
#22240 = VERTEX_POINT('',#92454) ;
#22241 = VERTEX_POINT('',#92456) ;
#22242 = VERTEX_POINT('',#92458) ;
#22243 = VERTEX_POINT('',#92460) ;
#22244 = VERTEX_POINT('',#92462) ;
#22245 = VERTEX_POINT('',#92464) ;
#22246 = VERTEX_POINT('',#92466) ;
#22247 = VERTEX_POINT('',#92468) ;
#22248 = VERTEX_POINT('',#92471) ;
#22249 = VERTEX_POINT('',#92472) ;
#22250 = VERTEX_POINT('',#92474) ;
#22251 = VERTEX_POINT('',#92476) ;
#22252 = VERTEX_POINT('',#92478) ;
#22253 = VERTEX_POINT('',#92480) ;
#22254 = VERTEX_POINT('',#92482) ;
#22255 = VERTEX_POINT('',#92484) ;
#22256 = VERTEX_POINT('',#92486) ;
#22257 = VERTEX_POINT('',#92488) ;
#22258 = VERTEX_POINT('',#92490) ;
#22259 = VERTEX_POINT('',#92492) ;
#22260 = VERTEX_POINT('',#92494) ;
#22261 = VERTEX_POINT('',#92496) ;
#22262 = VERTEX_POINT('',#92556) ;
#22263 = VERTEX_POINT('',#92557) ;
#22264 = VERTEX_POINT('',#92566) ;
#22265 = VERTEX_POINT('',#92581) ;
#22266 = VERTEX_POINT('',#92603) ;
#22267 = VERTEX_POINT('',#92607) ;
#22268 = VERTEX_POINT('',#92613) ;
#22269 = VERTEX_POINT('',#92615) ;
#22270 = VERTEX_POINT('',#92619) ;
#22271 = VERTEX_POINT('',#92622) ;
#22272 = VERTEX_POINT('',#92627) ;
#22273 = VERTEX_POINT('',#92629) ;
#22274 = VERTEX_POINT('',#92633) ;
#22275 = VERTEX_POINT('',#92634) ;
#22276 = VERTEX_POINT('',#92636) ;
#22277 = VERTEX_POINT('',#92640) ;
#22278 = VERTEX_POINT('',#92642) ;
#22279 = VERTEX_POINT('',#92646) ;
#22280 = VERTEX_POINT('',#92647) ;
#22281 = VERTEX_POINT('',#92652) ;
#22282 = VERTEX_POINT('',#92653) ;
#22283 = VERTEX_POINT('',#92658) ;
#22284 = VERTEX_POINT('',#92659) ;
#22285 = VERTEX_POINT('',#92667) ;
#22286 = VERTEX_POINT('',#92668) ;
#22287 = VERTEX_POINT('',#92683) ;
#22288 = VERTEX_POINT('',#92685) ;
#22289 = VERTEX_POINT('',#92689) ;
#22290 = VERTEX_POINT('',#92690) ;
#22291 = VERTEX_POINT('',#92746) ;
#22292 = VERTEX_POINT('',#92748) ;
#22293 = VERTEX_POINT('',#92750) ;
#22294 = VERTEX_POINT('',#92754) ;
#22295 = VERTEX_POINT('',#92766) ;
#22296 = VERTEX_POINT('',#92770) ;
#22297 = VERTEX_POINT('',#92774) ;
#22298 = VERTEX_POINT('',#92783) ;
#22299 = VERTEX_POINT('',#92787) ;
#22300 = VERTEX_POINT('',#92791) ;
#22301 = VERTEX_POINT('',#92809) ;
#22302 = VERTEX_POINT('',#92840) ;
#22303 = VERTEX_POINT('',#92842) ;
#22304 = VERTEX_POINT('',#92846) ;
#22305 = VERTEX_POINT('',#92848) ;
#22306 = VERTEX_POINT('',#92850) ;
#22307 = VERTEX_POINT('',#92854) ;
#22308 = VERTEX_POINT('',#92858) ;
#22309 = VERTEX_POINT('',#92862) ;
#22310 = VERTEX_POINT('',#92866) ;
#22311 = VERTEX_POINT('',#92868) ;
#22312 = VERTEX_POINT('',#92870) ;
#22313 = VERTEX_POINT('',#92872) ;
#22314 = VERTEX_POINT('',#92874) ;
#22315 = VERTEX_POINT('',#92876) ;
#22316 = VERTEX_POINT('',#92878) ;
#22317 = VERTEX_POINT('',#92882) ;
#22318 = VERTEX_POINT('',#92886) ;
#22319 = VERTEX_POINT('',#92890) ;
#22320 = VERTEX_POINT('',#92894) ;
#22321 = VERTEX_POINT('',#92896) ;
#22322 = VERTEX_POINT('',#92932) ;
#22323 = VERTEX_POINT('',#92933) ;
#22324 = VERTEX_POINT('',#92935) ;
#22325 = VERTEX_POINT('',#92961) ;
#22326 = VERTEX_POINT('',#92970) ;
#22327 = VERTEX_POINT('',#92971) ;
#22328 = VERTEX_POINT('',#92976) ;
#22329 = VERTEX_POINT('',#92977) ;
#22330 = VERTEX_POINT('',#92979) ;
#22331 = VERTEX_POINT('',#92981) ;
#22332 = VERTEX_POINT('',#92985) ;
#22333 = VERTEX_POINT('',#92986) ;
#22334 = VERTEX_POINT('',#92994) ;
#22335 = VERTEX_POINT('',#92995) ;
#22336 = VERTEX_POINT('',#92997) ;
#22337 = VERTEX_POINT('',#92999) ;
#22338 = VERTEX_POINT('',#93032) ;
#22339 = VERTEX_POINT('',#93033) ;
#22340 = VERTEX_POINT('',#93059) ;
#22341 = VERTEX_POINT('',#93061) ;
#22342 = VERTEX_POINT('',#93070) ;
#22343 = VERTEX_POINT('',#93071) ;
#22344 = VERTEX_POINT('',#93079) ;
#22345 = VERTEX_POINT('',#93080) ;
#22346 = VERTEX_POINT('',#93109) ;
#22347 = VERTEX_POINT('',#93141) ;
#22348 = VERTEX_POINT('',#93147) ;
#22349 = VERTEX_POINT('',#93148) ;
#22350 = VERTEX_POINT('',#93153) ;
#22351 = VERTEX_POINT('',#93157) ;
#22352 = VERTEX_POINT('',#93161) ;
#22353 = VERTEX_POINT('',#93167) ;
#22354 = VERTEX_POINT('',#93168) ;
#22355 = VERTEX_POINT('',#93173) ;
#22356 = VERTEX_POINT('',#93174) ;
#22357 = VERTEX_POINT('',#93179) ;
#22358 = VERTEX_POINT('',#93180) ;
#22359 = VERTEX_POINT('',#93185) ;
#22360 = VERTEX_POINT('',#93186) ;
#22361 = VERTEX_POINT('',#93191) ;
#22362 = VERTEX_POINT('',#93192) ;
#22363 = VERTEX_POINT('',#93197) ;
#22364 = VERTEX_POINT('',#93198) ;
#22365 = VERTEX_POINT('',#93203) ;
#22366 = VERTEX_POINT('',#93204) ;
#22367 = VERTEX_POINT('',#93209) ;
#22368 = VERTEX_POINT('',#93210) ;
#22369 = VERTEX_POINT('',#93215) ;
#22370 = VERTEX_POINT('',#93216) ;
#22371 = VERTEX_POINT('',#93224) ;
#22372 = VERTEX_POINT('',#93225) ;
#22373 = VERTEX_POINT('',#93254) ;
#22374 = VERTEX_POINT('',#93288) ;
#22375 = VERTEX_POINT('',#93289) ;
#22376 = VERTEX_POINT('',#93294) ;
#22377 = VERTEX_POINT('',#93298) ;
#22378 = VERTEX_POINT('',#93305) ;
#22379 = VERTEX_POINT('',#93307) ;
#22380 = VERTEX_POINT('',#93318) ;
#22381 = VERTEX_POINT('',#93320) ;
#22382 = VERTEX_POINT('',#93325) ;
#22383 = VERTEX_POINT('',#93331) ;
#22384 = VERTEX_POINT('',#93338) ;
#22385 = VERTEX_POINT('',#93342) ;
#22386 = VERTEX_POINT('',#93343) ;
#22387 = VERTEX_POINT('',#93345) ;
#22388 = VERTEX_POINT('',#93347) ;
#22389 = VERTEX_POINT('',#93351) ;
#22390 = VERTEX_POINT('',#93353) ;
#22391 = VERTEX_POINT('',#93357) ;
#22392 = VERTEX_POINT('',#93359) ;
#22393 = VERTEX_POINT('',#93363) ;
#22394 = VERTEX_POINT('',#93364) ;
#22395 = VERTEX_POINT('',#93366) ;
#22396 = VERTEX_POINT('',#93368) ;
#22397 = VERTEX_POINT('',#93372) ;
#22398 = VERTEX_POINT('',#93373) ;
#22399 = VERTEX_POINT('',#93375) ;
#22400 = VERTEX_POINT('',#93377) ;
#22401 = VERTEX_POINT('',#93384) ;
#22402 = VERTEX_POINT('',#93385) ;
#22403 = VERTEX_POINT('',#93387) ;
#22404 = VERTEX_POINT('',#93389) ;
#22405 = VERTEX_POINT('',#93393) ;
#22406 = VERTEX_POINT('',#93394) ;
#22407 = VERTEX_POINT('',#93402) ;
#22408 = VERTEX_POINT('',#93403) ;
#22409 = VERTEX_POINT('',#93408) ;
#22410 = VERTEX_POINT('',#93409) ;
#22411 = VERTEX_POINT('',#93414) ;
#22412 = VERTEX_POINT('',#93415) ;
#22413 = VERTEX_POINT('',#93420) ;
#22414 = VERTEX_POINT('',#93421) ;
#22415 = VERTEX_POINT('',#93426) ;
#22416 = VERTEX_POINT('',#93427) ;
#22417 = VERTEX_POINT('',#93432) ;
#22418 = VERTEX_POINT('',#93434) ;
#22419 = VERTEX_POINT('',#93438) ;
#22420 = VERTEX_POINT('',#93440) ;
#22421 = VERTEX_POINT('',#93442) ;
#22422 = VERTEX_POINT('',#93444) ;
#22423 = VERTEX_POINT('',#93446) ;
#22424 = VERTEX_POINT('',#93448) ;
#22425 = VERTEX_POINT('',#93450) ;
#22426 = VERTEX_POINT('',#93452) ;
#22427 = VERTEX_POINT('',#93454) ;
#22428 = VERTEX_POINT('',#93456) ;
#22429 = VERTEX_POINT('',#93460) ;
#22430 = VERTEX_POINT('',#93464) ;
#22431 = VERTEX_POINT('',#93466) ;
#22432 = VERTEX_POINT('',#93468) ;
#22433 = VERTEX_POINT('',#93470) ;
#22434 = VERTEX_POINT('',#93476) ;
#22435 = VERTEX_POINT('',#93478) ;
#22436 = VERTEX_POINT('',#93516) ;
#22437 = VERTEX_POINT('',#93522) ;
#22438 = VERTEX_POINT('',#93526) ;
#22439 = VERTEX_POINT('',#93530) ;
#22440 = VERTEX_POINT('',#93534) ;
#22441 = VERTEX_POINT('',#93538) ;
#22442 = VERTEX_POINT('',#93542) ;
#22443 = VERTEX_POINT('',#93546) ;
#22444 = VERTEX_POINT('',#93550) ;
#22445 = VERTEX_POINT('',#93554) ;
#22446 = VERTEX_POINT('',#93558) ;
#22447 = VERTEX_POINT('',#93585) ;
#22448 = VERTEX_POINT('',#93589) ;
#22449 = VERTEX_POINT('',#93620) ;
#22450 = VERTEX_POINT('',#93651) ;
#22451 = VERTEX_POINT('',#93688) ;
#22452 = VERTEX_POINT('',#93692) ;
#22453 = VERTEX_POINT('',#93696) ;
#22454 = VERTEX_POINT('',#93700) ;
#22455 = VERTEX_POINT('',#93713) ;
#22456 = VERTEX_POINT('',#93728) ;
#22457 = VERTEX_POINT('',#93734) ;
#22458 = VERTEX_POINT('',#93738) ;
#22459 = VERTEX_POINT('',#93744) ;
#22460 = VERTEX_POINT('',#93748) ;
#22461 = VERTEX_POINT('',#93759) ;
#22462 = VERTEX_POINT('',#93763) ;
#22463 = VERTEX_POINT('',#93767) ;
#22464 = VERTEX_POINT('',#93771) ;
#22465 = VERTEX_POINT('',#93772) ;
#22466 = VERTEX_POINT('',#93774) ;
#22467 = VERTEX_POINT('',#93776) ;
#22468 = VERTEX_POINT('',#93780) ;
#22469 = VERTEX_POINT('',#93785) ;
#22470 = VERTEX_POINT('',#93789) ;
#22471 = VERTEX_POINT('',#93793) ;
#22472 = VERTEX_POINT('',#93797) ;
#22473 = VERTEX_POINT('',#93807) ;
#22474 = VERTEX_POINT('',#93809) ;
#22475 = VERTEX_POINT('',#93811) ;
#22476 = VERTEX_POINT('',#93813) ;
#22477 = VERTEX_POINT('',#93815) ;
#22478 = VERTEX_POINT('',#93818) ;
#22479 = VERTEX_POINT('',#93819) ;
#22480 = VERTEX_POINT('',#93843) ;
#22481 = VERTEX_POINT('',#93845) ;
#22482 = VERTEX_POINT('',#93857) ;
#22483 = VERTEX_POINT('',#93859) ;
#22484 = VERTEX_POINT('',#93861) ;
#22485 = VERTEX_POINT('',#93864) ;
#22486 = VERTEX_POINT('',#93865) ;
#22487 = VERTEX_POINT('',#93867) ;
#22488 = VERTEX_POINT('',#93869) ;
#22489 = VERTEX_POINT('',#93871) ;
#22490 = VERTEX_POINT('',#93888) ;
#22491 = VERTEX_POINT('',#93890) ;
#22492 = VERTEX_POINT('',#93904) ;
#22493 = VERTEX_POINT('',#93908) ;
#22494 = VERTEX_POINT('',#93910) ;
#22495 = VERTEX_POINT('',#93914) ;
#22496 = VERTEX_POINT('',#93917) ;
#22497 = VERTEX_POINT('',#93920) ;
#22498 = VERTEX_POINT('',#93923) ;
#22499 = VERTEX_POINT('',#93927) ;
#22500 = VERTEX_POINT('',#93929) ;
#22501 = VERTEX_POINT('',#93931) ;
#22502 = VERTEX_POINT('',#93967) ;
#22503 = VERTEX_POINT('',#93968) ;
#22504 = VERTEX_POINT('',#93970) ;
#22505 = VERTEX_POINT('',#93972) ;
#22506 = VERTEX_POINT('',#94005) ;
#22507 = VERTEX_POINT('',#94006) ;
#22508 = VERTEX_POINT('',#94008) ;
#22509 = VERTEX_POINT('',#94010) ;
#22510 = VERTEX_POINT('',#94014) ;
#22511 = VERTEX_POINT('',#94016) ;
#22512 = VERTEX_POINT('',#94044) ;
#22513 = VERTEX_POINT('',#94045) ;
#22514 = VERTEX_POINT('',#94081) ;
#22515 = VERTEX_POINT('',#94082) ;
#22516 = VERTEX_POINT('',#94090) ;
#22517 = VERTEX_POINT('',#94091) ;
#22518 = VERTEX_POINT('',#94099) ;
#22519 = VERTEX_POINT('',#94100) ;
#22520 = VERTEX_POINT('',#94105) ;
#22521 = VERTEX_POINT('',#94129) ;
#22522 = VERTEX_POINT('',#94157) ;
#22523 = VERTEX_POINT('',#94159) ;
#22524 = VERTEX_POINT('',#94167) ;
#22525 = VERTEX_POINT('',#94169) ;
#22526 = VERTEX_POINT('',#94173) ;
#22527 = VERTEX_POINT('',#94175) ;
#22528 = VERTEX_POINT('',#94177) ;
#22529 = VERTEX_POINT('',#94193) ;
#22530 = VERTEX_POINT('',#94194) ;
#22531 = VERTEX_POINT('',#94199) ;
#22532 = VERTEX_POINT('',#94201) ;
#22533 = VERTEX_POINT('',#94203) ;
#22534 = VERTEX_POINT('',#94208) ;
#22535 = VERTEX_POINT('',#94210) ;
#22536 = VERTEX_POINT('',#94212) ;
#22537 = VERTEX_POINT('',#94216) ;
#22538 = VERTEX_POINT('',#94242) ;
#22539 = VERTEX_POINT('',#94315) ;
#22540 = VERTEX_POINT('',#94373) ;
#22541 = VERTEX_POINT('',#94411) ;
#22542 = VERTEX_POINT('',#94432) ;
#22543 = VERTEX_POINT('',#94437) ;
#22544 = VERTEX_POINT('',#94439) ;
#22545 = VERTEX_POINT('',#94444) ;
#22546 = VERTEX_POINT('',#94446) ;
#22547 = VERTEX_POINT('',#94478) ;
#22548 = VERTEX_POINT('',#94482) ;
#22549 = VERTEX_POINT('',#94483) ;
#22550 = VERTEX_POINT('',#94515) ;
#22551 = VERTEX_POINT('',#94539) ;
#22552 = VERTEX_POINT('',#94560) ;
#22553 = VERTEX_POINT('',#94562) ;
#22554 = VERTEX_POINT('',#94564) ;
#22555 = VERTEX_POINT('',#94566) ;
#22556 = VERTEX_POINT('',#94568) ;
#22557 = VERTEX_POINT('',#94571) ;
#22558 = VERTEX_POINT('',#94574) ;
#22559 = VERTEX_POINT('',#94575) ;
#22560 = VERTEX_POINT('',#94577) ;
#22561 = VERTEX_POINT('',#94579) ;
#22562 = VERTEX_POINT('',#94581) ;
#22563 = VERTEX_POINT('',#94583) ;
#22564 = VERTEX_POINT('',#94585) ;
#22565 = VERTEX_POINT('',#94587) ;
#22566 = VERTEX_POINT('',#94589) ;
#22567 = VERTEX_POINT('',#94591) ;
#22568 = VERTEX_POINT('',#94593) ;
#22569 = VERTEX_POINT('',#94596) ;
#22570 = VERTEX_POINT('',#94597) ;
#22571 = VERTEX_POINT('',#94599) ;
#22572 = VERTEX_POINT('',#94601) ;
#22573 = VERTEX_POINT('',#94603) ;
#22574 = VERTEX_POINT('',#94605) ;
#22575 = VERTEX_POINT('',#94607) ;
#22576 = VERTEX_POINT('',#94609) ;
#22577 = VERTEX_POINT('',#94611) ;
#22578 = VERTEX_POINT('',#94613) ;
#22579 = VERTEX_POINT('',#94615) ;
#22580 = VERTEX_POINT('',#94618) ;
#22581 = VERTEX_POINT('',#94619) ;
#22582 = VERTEX_POINT('',#94621) ;
#22583 = VERTEX_POINT('',#94623) ;
#22584 = VERTEX_POINT('',#94630) ;
#22585 = VERTEX_POINT('',#94667) ;
#22586 = VERTEX_POINT('',#94671) ;
#22587 = VERTEX_POINT('',#94684) ;
#22588 = VERTEX_POINT('',#94733) ;
#22589 = VERTEX_POINT('',#94776) ;
#22590 = VERTEX_POINT('',#94782) ;
#22591 = VERTEX_POINT('',#94786) ;
#22592 = VERTEX_POINT('',#94793) ;
#22593 = VERTEX_POINT('',#94804) ;
#22594 = VERTEX_POINT('',#94806) ;
#22595 = VERTEX_POINT('',#94809) ;
#22596 = VERTEX_POINT('',#94831) ;
#22597 = VERTEX_POINT('',#94832) ;
#22598 = VERTEX_POINT('',#94834) ;
#22599 = VERTEX_POINT('',#94836) ;
#22600 = VERTEX_POINT('',#94841) ;
#22601 = VERTEX_POINT('',#94845) ;
#22602 = VERTEX_POINT('',#94847) ;
#22603 = VERTEX_POINT('',#94888) ;
#22604 = VERTEX_POINT('',#94890) ;
#22605 = VERTEX_POINT('',#94894) ;
#22606 = VERTEX_POINT('',#94898) ;
#22607 = VERTEX_POINT('',#94902) ;
#22608 = VERTEX_POINT('',#94908) ;
#22609 = VERTEX_POINT('',#94910) ;
#22610 = VERTEX_POINT('',#94912) ;
#22611 = VERTEX_POINT('',#94914) ;
#22612 = VERTEX_POINT('',#94917) ;
#22613 = VERTEX_POINT('',#94931) ;
#22614 = VERTEX_POINT('',#94933) ;
#22615 = VERTEX_POINT('',#94937) ;
#22616 = VERTEX_POINT('',#94939) ;
#22617 = VERTEX_POINT('',#94953) ;
#22618 = VERTEX_POINT('',#94954) ;
#22619 = VERTEX_POINT('',#94956) ;
#22620 = VERTEX_POINT('',#94971) ;
#22621 = VERTEX_POINT('',#95024) ;
#22622 = VERTEX_POINT('',#95035) ;
#22623 = VERTEX_POINT('',#95157) ;
#22624 = VERTEX_POINT('',#95159) ;
#22625 = VERTEX_POINT('',#95230) ;
#22626 = VERTEX_POINT('',#95242) ;
#22627 = VERTEX_POINT('',#95269) ;
#22628 = VERTEX_POINT('',#95271) ;
#22629 = VERTEX_POINT('',#95275) ;
#22630 = VERTEX_POINT('',#95277) ;
#22631 = VERTEX_POINT('',#95284) ;
#22632 = VERTEX_POINT('',#95286) ;
#22633 = VERTEX_POINT('',#95290) ;
#22634 = VERTEX_POINT('',#95294) ;
#22635 = VERTEX_POINT('',#95298) ;
#22636 = VERTEX_POINT('',#95382) ;
#22637 = VERTEX_POINT('',#95383) ;
#22638 = VERTEX_POINT('',#95400) ;
#22639 = VERTEX_POINT('',#95415) ;
#22640 = VERTEX_POINT('',#95537) ;
#22641 = VERTEX_POINT('',#95539) ;
#22642 = VERTEX_POINT('',#95543) ;
#22643 = VERTEX_POINT('',#95545) ;
#22644 = VERTEX_POINT('',#95549) ;
#22645 = VERTEX_POINT('',#95551) ;
#22646 = VERTEX_POINT('',#95555) ;
#22647 = VERTEX_POINT('',#95557) ;
#22648 = VERTEX_POINT('',#95638) ;
#22649 = VERTEX_POINT('',#95754) ;
#22650 = VERTEX_POINT('',#95786) ;
#22651 = VERTEX_POINT('',#95788) ;
#22652 = VERTEX_POINT('',#95811) ;
#22653 = VERTEX_POINT('',#95965) ;
#22654 = VERTEX_POINT('',#95988) ;
#22655 = VERTEX_POINT('',#96077) ;
#22656 = VERTEX_POINT('',#96078) ;
#22657 = VERTEX_POINT('',#96080) ;
#22658 = VERTEX_POINT('',#96082) ;
#22659 = VERTEX_POINT('',#96086) ;
#22660 = VERTEX_POINT('',#96088) ;
#22661 = VERTEX_POINT('',#96092) ;
#22662 = VERTEX_POINT('',#96094) ;
#22663 = VERTEX_POINT('',#96098) ;
#22664 = VERTEX_POINT('',#96100) ;
#22665 = VERTEX_POINT('',#96104) ;
#22666 = VERTEX_POINT('',#96106) ;
#22667 = VERTEX_POINT('',#96110) ;
#22668 = VERTEX_POINT('',#96112) ;
#22669 = VERTEX_POINT('',#96119) ;
#22670 = VERTEX_POINT('',#96121) ;
#22671 = VERTEX_POINT('',#96125) ;
#22672 = VERTEX_POINT('',#96129) ;
#22673 = VERTEX_POINT('',#96133) ;
#22674 = VERTEX_POINT('',#96138) ;
#22675 = VERTEX_POINT('',#96139) ;
#22676 = VERTEX_POINT('',#96141) ;
#22677 = VERTEX_POINT('',#96143) ;
#22678 = VERTEX_POINT('',#96147) ;
#22679 = VERTEX_POINT('',#96149) ;
#22680 = VERTEX_POINT('',#96153) ;
#22681 = VERTEX_POINT('',#96155) ;
#22682 = VERTEX_POINT('',#96162) ;
#22683 = VERTEX_POINT('',#96164) ;
#22684 = VERTEX_POINT('',#96168) ;
#22685 = VERTEX_POINT('',#96173) ;
#22686 = VERTEX_POINT('',#96174) ;
#22687 = VERTEX_POINT('',#96176) ;
#22688 = VERTEX_POINT('',#96178) ;
#22689 = VERTEX_POINT('',#96182) ;
#22690 = VERTEX_POINT('',#96184) ;
#22691 = VERTEX_POINT('',#96188) ;
#22692 = VERTEX_POINT('',#96190) ;
#22693 = VERTEX_POINT('',#96194) ;
#22694 = VERTEX_POINT('',#96196) ;
#22695 = VERTEX_POINT('',#96200) ;
#22696 = VERTEX_POINT('',#96202) ;
#22697 = VERTEX_POINT('',#96206) ;
#22698 = VERTEX_POINT('',#96208) ;
#22699 = VERTEX_POINT('',#96215) ;
#22700 = VERTEX_POINT('',#96217) ;
#22701 = VERTEX_POINT('',#96221) ;
#22702 = VERTEX_POINT('',#96225) ;
#22703 = VERTEX_POINT('',#96229) ;
#22704 = VERTEX_POINT('',#96234) ;
#22705 = VERTEX_POINT('',#96235) ;
#22706 = VERTEX_POINT('',#96237) ;
#22707 = VERTEX_POINT('',#96239) ;
#22708 = VERTEX_POINT('',#96243) ;
#22709 = VERTEX_POINT('',#96245) ;
#22710 = VERTEX_POINT('',#96249) ;
#22711 = VERTEX_POINT('',#96251) ;
#22712 = VERTEX_POINT('',#96258) ;
#22713 = VERTEX_POINT('',#96260) ;
#22714 = VERTEX_POINT('',#96264) ;
#22715 = VERTEX_POINT('',#96269) ;
#22716 = VERTEX_POINT('',#96270) ;
#22717 = VERTEX_POINT('',#96272) ;
#22718 = VERTEX_POINT('',#96274) ;
#22719 = VERTEX_POINT('',#96278) ;
#22720 = VERTEX_POINT('',#96280) ;
#22721 = VERTEX_POINT('',#96284) ;
#22722 = VERTEX_POINT('',#96286) ;
#22723 = VERTEX_POINT('',#96290) ;
#22724 = VERTEX_POINT('',#96291) ;
#22725 = VERTEX_POINT('',#96296) ;
#22726 = VERTEX_POINT('',#96298) ;
#22727 = VERTEX_POINT('',#96302) ;
#22728 = VERTEX_POINT('',#96304) ;
#22729 = VERTEX_POINT('',#96308) ;
#22730 = VERTEX_POINT('',#96310) ;
#22731 = VERTEX_POINT('',#96314) ;
#22732 = VERTEX_POINT('',#96315) ;
#22733 = VERTEX_POINT('',#96320) ;
#22734 = VERTEX_POINT('',#96322) ;
#22735 = VERTEX_POINT('',#96326) ;
#22736 = VERTEX_POINT('',#96328) ;
#22737 = VERTEX_POINT('',#96335) ;
#22738 = VERTEX_POINT('',#96337) ;
#22739 = VERTEX_POINT('',#96341) ;
#22740 = VERTEX_POINT('',#96345) ;
#22741 = VERTEX_POINT('',#96349) ;
#22742 = VERTEX_POINT('',#96353) ;
#22743 = VERTEX_POINT('',#96357) ;
#22744 = VERTEX_POINT('',#96362) ;
#22745 = VERTEX_POINT('',#96363) ;
#22746 = VERTEX_POINT('',#96365) ;
#22747 = VERTEX_POINT('',#96367) ;
#22748 = VERTEX_POINT('',#96371) ;
#22749 = VERTEX_POINT('',#96373) ;
#22750 = VERTEX_POINT('',#96377) ;
#22751 = VERTEX_POINT('',#96378) ;
#22752 = VERTEX_POINT('',#96383) ;
#22753 = VERTEX_POINT('',#96385) ;
#22754 = VERTEX_POINT('',#96389) ;
#22755 = VERTEX_POINT('',#96391) ;
#22756 = VERTEX_POINT('',#96395) ;
#22757 = VERTEX_POINT('',#96397) ;
#22758 = VERTEX_POINT('',#96401) ;
#22759 = VERTEX_POINT('',#96402) ;
#22760 = VERTEX_POINT('',#96407) ;
#22761 = VERTEX_POINT('',#96409) ;
#22762 = VERTEX_POINT('',#96413) ;
#22763 = VERTEX_POINT('',#96415) ;
#22764 = VERTEX_POINT('',#96419) ;
#22765 = VERTEX_POINT('',#96421) ;
#22766 = VERTEX_POINT('',#96428) ;
#22767 = VERTEX_POINT('',#96430) ;
#22768 = VERTEX_POINT('',#96434) ;
#22769 = VERTEX_POINT('',#96438) ;
#22770 = VERTEX_POINT('',#96442) ;
#22771 = VERTEX_POINT('',#96446) ;
#22772 = VERTEX_POINT('',#96450) ;
#22773 = VERTEX_POINT('',#96606) ;
#22774 = VERTEX_POINT('',#96758) ;
#22775 = VERTEX_POINT('',#97051) ;
#22776 = VERTEX_POINT('',#97053) ;
#22777 = VERTEX_POINT('',#97193) ;
#22778 = VERTEX_POINT('',#97194) ;
#22779 = VERTEX_POINT('',#97197) ;
#22780 = VERTEX_POINT('',#97201) ;
#22781 = VERTEX_POINT('',#97203) ;
#22782 = VERTEX_POINT('',#97207) ;
#22783 = VERTEX_POINT('',#97211) ;
#22784 = VERTEX_POINT('',#97215) ;
#22785 = VERTEX_POINT('',#97219) ;
#22786 = VERTEX_POINT('',#97231) ;
#22787 = VERTEX_POINT('',#97232) ;
#22788 = VERTEX_POINT('',#97234) ;
#22789 = VERTEX_POINT('',#97236) ;
#22790 = VERTEX_POINT('',#97239) ;
#22791 = VERTEX_POINT('',#97241) ;
#22792 = VERTEX_POINT('',#97243) ;
#22793 = VERTEX_POINT('',#97246) ;
#22794 = VERTEX_POINT('',#97296) ;
#22795 = VERTEX_POINT('',#97299) ;
#22796 = VERTEX_POINT('',#97300) ;
#22797 = VERTEX_POINT('',#97302) ;
#22798 = VERTEX_POINT('',#97304) ;
#22799 = VERTEX_POINT('',#97307) ;
#22800 = VERTEX_POINT('',#97308) ;
#22801 = VERTEX_POINT('',#97310) ;
#22802 = VERTEX_POINT('',#97312) ;
#22803 = VERTEX_POINT('',#97314) ;
#22804 = VERTEX_POINT('',#97316) ;
#22805 = VERTEX_POINT('',#97318) ;
#22806 = VERTEX_POINT('',#97327) ;
#22807 = VERTEX_POINT('',#97335) ;
#22808 = VERTEX_POINT('',#97337) ;
#22809 = VERTEX_POINT('',#97361) ;
#22810 = VERTEX_POINT('',#97369) ;
#22811 = VERTEX_POINT('',#97370) ;
#22812 = VERTEX_POINT('',#97390) ;
#22813 = VERTEX_POINT('',#97394) ;
#22814 = VERTEX_POINT('',#97406) ;
#22815 = VERTEX_POINT('',#97408) ;
#22816 = VERTEX_POINT('',#97412) ;
#22817 = VERTEX_POINT('',#97425) ;
#22818 = VERTEX_POINT('',#97453) ;
#22819 = VERTEX_POINT('',#97457) ;
#22820 = VERTEX_POINT('',#97459) ;
#22821 = VERTEX_POINT('',#97461) ;
#22822 = VERTEX_POINT('',#97463) ;
#22823 = VERTEX_POINT('',#97465) ;
#22824 = VERTEX_POINT('',#97471) ;
#22825 = VERTEX_POINT('',#97475) ;
#22826 = VERTEX_POINT('',#97479) ;
#22827 = VERTEX_POINT('',#97483) ;
#22828 = VERTEX_POINT('',#97487) ;
#22829 = VERTEX_POINT('',#97491) ;
#22830 = VERTEX_POINT('',#97495) ;
#22831 = VERTEX_POINT('',#97499) ;
#22832 = VERTEX_POINT('',#97503) ;
#22833 = VERTEX_POINT('',#97510) ;
#22834 = VERTEX_POINT('',#97512) ;
#22835 = VERTEX_POINT('',#97516) ;
#22836 = VERTEX_POINT('',#97520) ;
#22837 = VERTEX_POINT('',#97528) ;
#22838 = VERTEX_POINT('',#97530) ;
#22839 = VERTEX_POINT('',#97534) ;
#22840 = VERTEX_POINT('',#97536) ;
#22841 = VERTEX_POINT('',#97545) ;
#22842 = VERTEX_POINT('',#97558) ;
#22843 = VERTEX_POINT('',#97572) ;
#22844 = VERTEX_POINT('',#97589) ;
#22845 = VERTEX_POINT('',#97593) ;
#22846 = VERTEX_POINT('',#97595) ;
#22847 = VERTEX_POINT('',#97599) ;
#22848 = VERTEX_POINT('',#97718) ;
#22849 = VERTEX_POINT('',#97719) ;
#22850 = VERTEX_POINT('',#97731) ;
#22851 = VERTEX_POINT('',#97738) ;
#22852 = VERTEX_POINT('',#97761) ;
#22853 = VERTEX_POINT('',#97767) ;
#22854 = VERTEX_POINT('',#97768) ;
#22855 = VERTEX_POINT('',#97807) ;
#22856 = VERTEX_POINT('',#97809) ;
#22857 = VERTEX_POINT('',#97816) ;
#22858 = VERTEX_POINT('',#97817) ;
#22859 = VERTEX_POINT('',#97889) ;
#22860 = VERTEX_POINT('',#97890) ;
#22861 = VERTEX_POINT('',#97898) ;
#22862 = VERTEX_POINT('',#97923) ;
#22863 = VERTEX_POINT('',#97925) ;
#22864 = VERTEX_POINT('',#97932) ;
#22865 = VERTEX_POINT('',#97933) ;
#22866 = VERTEX_POINT('',#97986) ;
#22867 = VERTEX_POINT('',#97988) ;
#22868 = VERTEX_POINT('',#98006) ;
#22869 = VERTEX_POINT('',#98008) ;
#22870 = VERTEX_POINT('',#98014) ;
#22871 = VERTEX_POINT('',#98015) ;
#22872 = VERTEX_POINT('',#98017) ;
#22873 = VERTEX_POINT('',#98019) ;
#22874 = VERTEX_POINT('',#98074) ;
#22875 = VERTEX_POINT('',#98075) ;
#22876 = VERTEX_POINT('',#98080) ;
#22877 = VERTEX_POINT('',#98081) ;
#22878 = VERTEX_POINT('',#98086) ;
#22879 = VERTEX_POINT('',#98088) ;
#22880 = VERTEX_POINT('',#98111) ;
#22881 = VERTEX_POINT('',#98112) ;
#22882 = VERTEX_POINT('',#98139) ;
#22883 = VERTEX_POINT('',#98141) ;
#22884 = VERTEX_POINT('',#98145) ;
#22885 = VERTEX_POINT('',#98149) ;
#22886 = VERTEX_POINT('',#98153) ;
#22887 = VERTEX_POINT('',#98157) ;
#22888 = VERTEX_POINT('',#98161) ;
#22889 = VERTEX_POINT('',#98165) ;
#22890 = VERTEX_POINT('',#98169) ;
#22891 = VERTEX_POINT('',#98173) ;
#22892 = VERTEX_POINT('',#98188) ;
#22893 = VERTEX_POINT('',#98197) ;
#22894 = VERTEX_POINT('',#98222) ;
#22895 = VERTEX_POINT('',#98226) ;
#22896 = VERTEX_POINT('',#98230) ;
#22897 = VERTEX_POINT('',#98232) ;
#22898 = VERTEX_POINT('',#98236) ;
#22899 = VERTEX_POINT('',#98240) ;
#22900 = VERTEX_POINT('',#98244) ;
#22901 = VERTEX_POINT('',#98248) ;
#22902 = VERTEX_POINT('',#98252) ;
#22903 = VERTEX_POINT('',#98253) ;
#22904 = VERTEX_POINT('',#98258) ;
#22905 = VERTEX_POINT('',#98262) ;
#22906 = VERTEX_POINT('',#98266) ;
#22907 = VERTEX_POINT('',#98270) ;
#22908 = VERTEX_POINT('',#98274) ;
#22909 = VERTEX_POINT('',#98278) ;
#22910 = VERTEX_POINT('',#98282) ;
#22911 = VERTEX_POINT('',#98286) ;
#22912 = VERTEX_POINT('',#98287) ;
#22913 = VERTEX_POINT('',#98292) ;
#22914 = VERTEX_POINT('',#98296) ;
#22915 = VERTEX_POINT('',#98300) ;
#22916 = VERTEX_POINT('',#98304) ;
#22917 = VERTEX_POINT('',#98319) ;
#22918 = VERTEX_POINT('',#98328) ;
#22919 = VERTEX_POINT('',#98329) ;
#22920 = VERTEX_POINT('',#98334) ;
#22921 = VERTEX_POINT('',#98338) ;
#22922 = VERTEX_POINT('',#98342) ;
#22923 = VERTEX_POINT('',#98348) ;
#22924 = VERTEX_POINT('',#98352) ;
#22925 = VERTEX_POINT('',#98353) ;
#22926 = VERTEX_POINT('',#98358) ;
#22927 = VERTEX_POINT('',#98363) ;
#22928 = VERTEX_POINT('',#98367) ;
#22929 = VERTEX_POINT('',#98373) ;
#22930 = VERTEX_POINT('',#98374) ;
#22931 = VERTEX_POINT('',#98379) ;
#22932 = VERTEX_POINT('',#98383) ;
#22933 = VERTEX_POINT('',#98387) ;
#22934 = VERTEX_POINT('',#98391) ;
#22935 = VERTEX_POINT('',#98395) ;
#22936 = VERTEX_POINT('',#98399) ;
#22937 = VERTEX_POINT('',#98403) ;
#22938 = VERTEX_POINT('',#98407) ;
#22939 = VERTEX_POINT('',#98411) ;
#22940 = VERTEX_POINT('',#98415) ;
#22941 = VERTEX_POINT('',#98419) ;
#22942 = VERTEX_POINT('',#98423) ;
#22943 = VERTEX_POINT('',#98430) ;
#22944 = VERTEX_POINT('',#98445) ;
#22945 = VERTEX_POINT('',#98454) ;
#22946 = VERTEX_POINT('',#98458) ;
#22947 = VERTEX_POINT('',#98462) ;
#22948 = VERTEX_POINT('',#98480) ;
#22949 = VERTEX_POINT('',#98489) ;
#22950 = VERTEX_POINT('',#98493) ;
#22951 = VERTEX_POINT('',#98497) ;
#22952 = VERTEX_POINT('',#98501) ;
#22953 = VERTEX_POINT('',#98505) ;
#22954 = VERTEX_POINT('',#98512) ;
#22955 = VERTEX_POINT('',#98516) ;
#22956 = VERTEX_POINT('',#98520) ;
#22957 = VERTEX_POINT('',#98524) ;
#22958 = VERTEX_POINT('',#98528) ;
#22959 = VERTEX_POINT('',#98532) ;
#22960 = VERTEX_POINT('',#98536) ;
#22961 = VERTEX_POINT('',#98540) ;
#22962 = VERTEX_POINT('',#98544) ;
#22963 = VERTEX_POINT('',#98548) ;
#22964 = VERTEX_POINT('',#98552) ;
#22965 = VERTEX_POINT('',#98556) ;
#22966 = VERTEX_POINT('',#98560) ;
#22967 = VERTEX_POINT('',#98564) ;
#22968 = VERTEX_POINT('',#98571) ;
#22969 = VERTEX_POINT('',#98575) ;
#22970 = VERTEX_POINT('',#98579) ;
#22971 = VERTEX_POINT('',#98583) ;
#22972 = VERTEX_POINT('',#98587) ;
#22973 = VERTEX_POINT('',#98595) ;
#22974 = VERTEX_POINT('',#98599) ;
#22975 = VERTEX_POINT('',#98627) ;
#22976 = VERTEX_POINT('',#98674) ;
#22977 = VERTEX_POINT('',#98675) ;
#22978 = VERTEX_POINT('',#98677) ;
#22979 = VERTEX_POINT('',#98679) ;
#22980 = VERTEX_POINT('',#98683) ;
#22981 = VERTEX_POINT('',#98685) ;
#22982 = VERTEX_POINT('',#98689) ;
#22983 = VERTEX_POINT('',#98691) ;
#22984 = VERTEX_POINT('',#98695) ;
#22985 = VERTEX_POINT('',#98697) ;
#22986 = VERTEX_POINT('',#98701) ;
#22987 = VERTEX_POINT('',#98703) ;
#22988 = VERTEX_POINT('',#98707) ;
#22989 = VERTEX_POINT('',#98709) ;
#22990 = VERTEX_POINT('',#98713) ;
#22991 = VERTEX_POINT('',#98715) ;
#22992 = VERTEX_POINT('',#98723) ;
#22993 = VERTEX_POINT('',#98724) ;
#22994 = VERTEX_POINT('',#98726) ;
#22995 = VERTEX_POINT('',#98728) ;
#22996 = VERTEX_POINT('',#98732) ;
#22997 = VERTEX_POINT('',#98735) ;
#22998 = VERTEX_POINT('',#98739) ;
#22999 = VERTEX_POINT('',#98741) ;
#23000 = VERTEX_POINT('',#98751) ;
#23001 = VERTEX_POINT('',#98752) ;
#23002 = VERTEX_POINT('',#98754) ;
#23003 = VERTEX_POINT('',#98835) ;
#23004 = VERTEX_POINT('',#98888) ;
#23005 = VERTEX_POINT('',#98889) ;
#23006 = VERTEX_POINT('',#99176) ;
#23007 = VERTEX_POINT('',#99177) ;
#23008 = VERTEX_POINT('',#99179) ;
#23009 = VERTEX_POINT('',#99238) ;
#23010 = VERTEX_POINT('',#99299) ;
#23011 = VERTEX_POINT('',#99300) ;
#23012 = VERTEX_POINT('',#99302) ;
#23013 = VERTEX_POINT('',#99427) ;
#23014 = VERTEX_POINT('',#99535) ;
#23015 = VERTEX_POINT('',#99536) ;
#23016 = VERTEX_POINT('',#99538) ;
#23017 = VERTEX_POINT('',#99547) ;
#23018 = VERTEX_POINT('',#99741) ;
#23019 = VERTEX_POINT('',#99935) ;
#23020 = VERTEX_POINT('',#100132) ;
#23021 = VERTEX_POINT('',#100194) ;
#23022 = VERTEX_POINT('',#100196) ;
#23023 = VERTEX_POINT('',#100202) ;
#23024 = VERTEX_POINT('',#100396) ;
#23025 = VERTEX_POINT('',#100593) ;
#23026 = VERTEX_POINT('',#100787) ;
#23027 = VERTEX_POINT('',#100949) ;
#23028 = VERTEX_POINT('',#100952) ;
#23029 = VERTEX_POINT('',#101049) ;
#23030 = VERTEX_POINT('',#101051) ;
#23031 = VERTEX_POINT('',#101227) ;
#23032 = VERTEX_POINT('',#101444) ;
#23033 = VERTEX_POINT('',#101747) ;
#23034 = VERTEX_POINT('',#101749) ;
#23035 = VERTEX_POINT('',#101753) ;
#23036 = VERTEX_POINT('',#101771) ;
#23037 = VERTEX_POINT('',#101773) ;
#23038 = VERTEX_POINT('',#101777) ;
#23039 = VERTEX_POINT('',#101795) ;
#23040 = VERTEX_POINT('',#101798) ;
#23041 = VERTEX_POINT('',#101880) ;
#23042 = VERTEX_POINT('',#101886) ;
#23043 = VERTEX_POINT('',#101987) ;
#23044 = VERTEX_POINT('',#101993) ;
#23045 = VERTEX_POINT('',#102015) ;
#23046 = VERTEX_POINT('',#102016) ;
#23047 = VERTEX_POINT('',#102018) ;
#23048 = VERTEX_POINT('',#102033) ;
#23049 = VERTEX_POINT('',#102050) ;
#23050 = VERTEX_POINT('',#102052) ;
#23051 = VERTEX_POINT('',#102071) ;
#23052 = VERTEX_POINT('',#102073) ;
#23053 = VERTEX_POINT('',#102092) ;
#23054 = VERTEX_POINT('',#102094) ;
#23055 = VERTEX_POINT('',#102111) ;
#23056 = VERTEX_POINT('',#102113) ;
#23057 = VERTEX_POINT('',#102130) ;
#23058 = VERTEX_POINT('',#102132) ;
#23059 = VERTEX_POINT('',#102151) ;
#23060 = VERTEX_POINT('',#102153) ;
#23061 = VERTEX_POINT('',#102172) ;
#23062 = VERTEX_POINT('',#102174) ;
#23063 = VERTEX_POINT('',#102191) ;
#23064 = VERTEX_POINT('',#102193) ;
#23065 = VERTEX_POINT('',#102210) ;
#23066 = VERTEX_POINT('',#102212) ;
#23067 = VERTEX_POINT('',#102231) ;
#23068 = VERTEX_POINT('',#102233) ;
#23069 = VERTEX_POINT('',#102252) ;
#23070 = VERTEX_POINT('',#102254) ;
#23071 = VERTEX_POINT('',#102271) ;
#23072 = VERTEX_POINT('',#102273) ;
#23073 = VERTEX_POINT('',#102290) ;
#23074 = VERTEX_POINT('',#102292) ;
#23075 = VERTEX_POINT('',#102311) ;
#23076 = VERTEX_POINT('',#102313) ;
#23077 = VERTEX_POINT('',#102332) ;
#23078 = VERTEX_POINT('',#102334) ;
#23079 = VERTEX_POINT('',#102351) ;
#23080 = VERTEX_POINT('',#102353) ;
#23081 = VERTEX_POINT('',#102370) ;
#23082 = VERTEX_POINT('',#102372) ;
#23083 = VERTEX_POINT('',#102391) ;
#23084 = VERTEX_POINT('',#102393) ;
#23085 = VERTEX_POINT('',#102412) ;
#23086 = VERTEX_POINT('',#102414) ;
#23087 = VERTEX_POINT('',#102431) ;
#23088 = VERTEX_POINT('',#102433) ;
#23089 = VERTEX_POINT('',#102450) ;
#23090 = VERTEX_POINT('',#102452) ;
#23091 = VERTEX_POINT('',#102471) ;
#23092 = VERTEX_POINT('',#102473) ;
#23093 = VERTEX_POINT('',#102492) ;
#23094 = VERTEX_POINT('',#102494) ;
#23095 = VERTEX_POINT('',#102511) ;
#23096 = VERTEX_POINT('',#102513) ;
#23097 = VERTEX_POINT('',#102530) ;
#23098 = VERTEX_POINT('',#102532) ;
#23099 = VERTEX_POINT('',#102551) ;
#23100 = VERTEX_POINT('',#102553) ;
#23101 = VERTEX_POINT('',#102572) ;
#23102 = VERTEX_POINT('',#102574) ;
#23103 = VERTEX_POINT('',#102591) ;
#23104 = VERTEX_POINT('',#102593) ;
#23105 = VERTEX_POINT('',#102610) ;
#23106 = VERTEX_POINT('',#102612) ;
#23107 = VERTEX_POINT('',#102631) ;
#23108 = VERTEX_POINT('',#102633) ;
#23109 = VERTEX_POINT('',#102652) ;
#23110 = VERTEX_POINT('',#102654) ;
#23111 = VERTEX_POINT('',#102671) ;
#23112 = VERTEX_POINT('',#102673) ;
#23113 = VERTEX_POINT('',#102690) ;
#23114 = VERTEX_POINT('',#102692) ;
#23115 = VERTEX_POINT('',#102711) ;
#23116 = VERTEX_POINT('',#102713) ;
#23117 = VERTEX_POINT('',#102732) ;
#23118 = VERTEX_POINT('',#102734) ;
#23119 = VERTEX_POINT('',#102751) ;
#23120 = VERTEX_POINT('',#102753) ;
#23121 = VERTEX_POINT('',#102770) ;
#23122 = VERTEX_POINT('',#102772) ;
#23123 = VERTEX_POINT('',#102791) ;
#23124 = VERTEX_POINT('',#102793) ;
#23125 = VERTEX_POINT('',#102812) ;
#23126 = VERTEX_POINT('',#102814) ;
#23127 = VERTEX_POINT('',#102831) ;
#23128 = VERTEX_POINT('',#102833) ;
#23129 = VERTEX_POINT('',#102850) ;
#23130 = VERTEX_POINT('',#102852) ;
#23131 = VERTEX_POINT('',#102871) ;
#23132 = VERTEX_POINT('',#102873) ;
#23133 = VERTEX_POINT('',#102892) ;
#23134 = VERTEX_POINT('',#102894) ;
#23135 = VERTEX_POINT('',#102911) ;
#23136 = VERTEX_POINT('',#102913) ;
#23137 = VERTEX_POINT('',#102930) ;
#23138 = VERTEX_POINT('',#102932) ;
#23139 = VERTEX_POINT('',#102951) ;
#23140 = VERTEX_POINT('',#102953) ;
#23141 = VERTEX_POINT('',#102972) ;
#23142 = VERTEX_POINT('',#102974) ;
#23143 = VERTEX_POINT('',#102991) ;
#23144 = VERTEX_POINT('',#102993) ;
#23145 = VERTEX_POINT('',#103010) ;
#23146 = VERTEX_POINT('',#103012) ;
#23147 = VERTEX_POINT('',#103031) ;
#23148 = VERTEX_POINT('',#103033) ;
#23149 = VERTEX_POINT('',#103052) ;
#23150 = VERTEX_POINT('',#103054) ;
#23151 = VERTEX_POINT('',#103071) ;
#23152 = VERTEX_POINT('',#103073) ;
#23153 = VERTEX_POINT('',#103090) ;
#23154 = VERTEX_POINT('',#103092) ;
#23155 = VERTEX_POINT('',#103111) ;
#23156 = VERTEX_POINT('',#103113) ;
#23157 = VERTEX_POINT('',#103132) ;
#23158 = VERTEX_POINT('',#103134) ;
#23159 = VERTEX_POINT('',#103151) ;
#23160 = VERTEX_POINT('',#103153) ;
#23161 = VERTEX_POINT('',#103170) ;
#23162 = VERTEX_POINT('',#103172) ;
#23163 = VERTEX_POINT('',#103191) ;
#23164 = VERTEX_POINT('',#103193) ;
#23165 = VERTEX_POINT('',#103212) ;
#23166 = VERTEX_POINT('',#103214) ;
#23167 = VERTEX_POINT('',#103231) ;
#23168 = VERTEX_POINT('',#103233) ;
#23169 = VERTEX_POINT('',#103250) ;
#23170 = VERTEX_POINT('',#103252) ;
#23171 = VERTEX_POINT('',#103271) ;
#23172 = VERTEX_POINT('',#103273) ;
#23173 = VERTEX_POINT('',#103292) ;
#23174 = VERTEX_POINT('',#103294) ;
#23175 = VERTEX_POINT('',#103311) ;
#23176 = VERTEX_POINT('',#103313) ;
#23177 = VERTEX_POINT('',#103330) ;
#23178 = VERTEX_POINT('',#103332) ;
#23179 = VERTEX_POINT('',#103351) ;
#23180 = VERTEX_POINT('',#103353) ;
#23181 = VERTEX_POINT('',#103372) ;
#23182 = VERTEX_POINT('',#103374) ;
#23183 = VERTEX_POINT('',#103391) ;
#23184 = VERTEX_POINT('',#103393) ;
#23185 = VERTEX_POINT('',#103410) ;
#23186 = VERTEX_POINT('',#103412) ;
#23187 = VERTEX_POINT('',#103431) ;
#23188 = VERTEX_POINT('',#103433) ;
#23189 = VERTEX_POINT('',#103452) ;
#23190 = VERTEX_POINT('',#103454) ;
#23191 = VERTEX_POINT('',#103471) ;
#23192 = VERTEX_POINT('',#103473) ;
#23193 = VERTEX_POINT('',#103490) ;
#23194 = VERTEX_POINT('',#103492) ;
#23195 = VERTEX_POINT('',#103511) ;
#23196 = VERTEX_POINT('',#103513) ;
#23197 = VERTEX_POINT('',#103532) ;
#23198 = VERTEX_POINT('',#103534) ;
#23199 = VERTEX_POINT('',#103551) ;
#23200 = VERTEX_POINT('',#103553) ;
#23201 = VERTEX_POINT('',#103570) ;
#23202 = VERTEX_POINT('',#103572) ;
#23203 = VERTEX_POINT('',#103591) ;
#23204 = VERTEX_POINT('',#103593) ;
#23205 = VERTEX_POINT('',#103615) ;
#23206 = VERTEX_POINT('',#103617) ;
#23207 = VERTEX_POINT('',#103621) ;
#23208 = VERTEX_POINT('',#103625) ;
#23209 = VERTEX_POINT('',#103629) ;
#23210 = VERTEX_POINT('',#103633) ;
#23211 = VERTEX_POINT('',#103637) ;
#23212 = VERTEX_POINT('',#103641) ;
#23213 = VERTEX_POINT('',#103645) ;
#23214 = VERTEX_POINT('',#103649) ;
#23215 = VERTEX_POINT('',#103653) ;
#23216 = VERTEX_POINT('',#103657) ;
#23217 = VERTEX_POINT('',#103661) ;
#23218 = VERTEX_POINT('',#103665) ;
#23219 = VERTEX_POINT('',#103669) ;
#23220 = VERTEX_POINT('',#103673) ;
#23221 = VERTEX_POINT('',#103677) ;
#23222 = VERTEX_POINT('',#103681) ;
#23223 = VERTEX_POINT('',#103685) ;
#23224 = VERTEX_POINT('',#103689) ;
#23225 = VERTEX_POINT('',#103693) ;
#23226 = VERTEX_POINT('',#103697) ;
#23227 = VERTEX_POINT('',#103701) ;
#23228 = VERTEX_POINT('',#103705) ;
#23229 = VERTEX_POINT('',#103709) ;
#23230 = VERTEX_POINT('',#103713) ;
#23231 = VERTEX_POINT('',#103717) ;
#23232 = VERTEX_POINT('',#103721) ;
#23233 = VERTEX_POINT('',#103725) ;
#23234 = VERTEX_POINT('',#103729) ;
#23235 = VERTEX_POINT('',#103733) ;
#23236 = VERTEX_POINT('',#103737) ;
#23237 = VERTEX_POINT('',#103741) ;
#23238 = VERTEX_POINT('',#103745) ;
#23239 = VERTEX_POINT('',#103749) ;
#23240 = VERTEX_POINT('',#103753) ;
#23241 = VERTEX_POINT('',#103757) ;
#23242 = VERTEX_POINT('',#103761) ;
#23243 = VERTEX_POINT('',#103765) ;
#23244 = VERTEX_POINT('',#103769) ;
#23245 = VERTEX_POINT('',#103773) ;
#23246 = VERTEX_POINT('',#103813) ;
#23247 = VERTEX_POINT('',#103821) ;
#23248 = VERTEX_POINT('',#103823) ;
#23249 = VERTEX_POINT('',#103825) ;
#23250 = VERTEX_POINT('',#103827) ;
#23251 = VERTEX_POINT('',#103829) ;
#23252 = VERTEX_POINT('',#103831) ;
#23253 = VERTEX_POINT('',#103833) ;
#23254 = VERTEX_POINT('',#103835) ;
#23255 = VERTEX_POINT('',#103837) ;
#23256 = VERTEX_POINT('',#103839) ;
#23257 = VERTEX_POINT('',#103841) ;
#23258 = VERTEX_POINT('',#103843) ;
#23259 = VERTEX_POINT('',#103845) ;
#23260 = VERTEX_POINT('',#103847) ;
#23261 = VERTEX_POINT('',#103849) ;
#23262 = VERTEX_POINT('',#103851) ;
#23263 = VERTEX_POINT('',#103853) ;
#23264 = VERTEX_POINT('',#103855) ;
#23265 = VERTEX_POINT('',#103857) ;
#23266 = VERTEX_POINT('',#103859) ;
#23267 = VERTEX_POINT('',#103861) ;
#23268 = VERTEX_POINT('',#103863) ;
#23269 = VERTEX_POINT('',#103865) ;
#23270 = VERTEX_POINT('',#103867) ;
#23271 = VERTEX_POINT('',#103869) ;
#23272 = VERTEX_POINT('',#103871) ;
#23273 = VERTEX_POINT('',#103873) ;
#23274 = VERTEX_POINT('',#103875) ;
#23275 = VERTEX_POINT('',#103877) ;
#23276 = VERTEX_POINT('',#103879) ;
#23277 = VERTEX_POINT('',#103881) ;
#23278 = VERTEX_POINT('',#103883) ;
#23279 = VERTEX_POINT('',#103885) ;
#23280 = VERTEX_POINT('',#103887) ;
#23281 = VERTEX_POINT('',#103889) ;
#23282 = VERTEX_POINT('',#103891) ;
#23283 = VERTEX_POINT('',#103893) ;
#23284 = VERTEX_POINT('',#103895) ;
#23285 = VERTEX_POINT('',#103897) ;
#23286 = VERTEX_POINT('',#103899) ;
#23287 = VERTEX_POINT('',#103901) ;
#23288 = VERTEX_POINT('',#103905) ;
#23289 = VERTEX_POINT('',#103907) ;
#23290 = VERTEX_POINT('',#103911) ;
#23291 = VERTEX_POINT('',#103913) ;
#23292 = VERTEX_POINT('',#103917) ;
#23293 = VERTEX_POINT('',#103919) ;
#23294 = VERTEX_POINT('',#103923) ;
#23295 = VERTEX_POINT('',#103925) ;
#23296 = VERTEX_POINT('',#103929) ;
#23297 = VERTEX_POINT('',#103931) ;
#23298 = VERTEX_POINT('',#103935) ;
#23299 = VERTEX_POINT('',#103937) ;
#23300 = VERTEX_POINT('',#103941) ;
#23301 = VERTEX_POINT('',#103943) ;
#23302 = VERTEX_POINT('',#103947) ;
#23303 = VERTEX_POINT('',#103949) ;
#23304 = VERTEX_POINT('',#103953) ;
#23305 = VERTEX_POINT('',#103955) ;
#23306 = VERTEX_POINT('',#103959) ;
#23307 = VERTEX_POINT('',#103961) ;
#23308 = VERTEX_POINT('',#103965) ;
#23309 = VERTEX_POINT('',#103967) ;
#23310 = VERTEX_POINT('',#103971) ;
#23311 = VERTEX_POINT('',#103973) ;
#23312 = VERTEX_POINT('',#103977) ;
#23313 = VERTEX_POINT('',#103979) ;
#23314 = VERTEX_POINT('',#103983) ;
#23315 = VERTEX_POINT('',#103985) ;
#23316 = VERTEX_POINT('',#103989) ;
#23317 = VERTEX_POINT('',#103991) ;
#23318 = VERTEX_POINT('',#103995) ;
#23319 = VERTEX_POINT('',#103997) ;
#23320 = VERTEX_POINT('',#104001) ;
#23321 = VERTEX_POINT('',#104003) ;
#23322 = VERTEX_POINT('',#104007) ;
#23323 = VERTEX_POINT('',#104009) ;
#23324 = VERTEX_POINT('',#104013) ;
#23325 = VERTEX_POINT('',#104015) ;
#23326 = VERTEX_POINT('',#104019) ;
#23327 = VERTEX_POINT('',#104021) ;
#23328 = VERTEX_POINT('',#104025) ;
#23329 = VERTEX_POINT('',#104040) ;
#23330 = VERTEX_POINT('',#104057) ;
#23331 = VERTEX_POINT('',#104076) ;
#23332 = VERTEX_POINT('',#104109) ;
#23333 = VERTEX_POINT('',#104160) ;
#23334 = VERTEX_POINT('',#104161) ;
#23335 = VERTEX_POINT('',#104257) ;
#23336 = VERTEX_POINT('',#104258) ;
#23337 = VERTEX_POINT('',#104354) ;
#23338 = VERTEX_POINT('',#104355) ;
#23339 = VERTEX_POINT('',#104451) ;
#23340 = VERTEX_POINT('',#104452) ;
#23341 = VERTEX_POINT('',#104548) ;
#23342 = VERTEX_POINT('',#104549) ;
#23343 = VERTEX_POINT('',#104645) ;
#23344 = VERTEX_POINT('',#104646) ;
#23345 = VERTEX_POINT('',#104742) ;
#23346 = VERTEX_POINT('',#104743) ;
#23347 = VERTEX_POINT('',#104839) ;
#23348 = VERTEX_POINT('',#104840) ;
#23349 = VERTEX_POINT('',#105032) ;
#23350 = VERTEX_POINT('',#105049) ;
#23351 = VERTEX_POINT('',#105071) ;
#23352 = VERTEX_POINT('',#105088) ;
#23353 = VERTEX_POINT('',#105110) ;
#23354 = VERTEX_POINT('',#105127) ;
#23355 = VERTEX_POINT('',#105149) ;
#23356 = VERTEX_POINT('',#105166) ;
#23357 = VERTEX_POINT('',#105188) ;
#23358 = VERTEX_POINT('',#105205) ;
#23359 = VERTEX_POINT('',#105227) ;
#23360 = VERTEX_POINT('',#105244) ;
#23361 = VERTEX_POINT('',#105266) ;
#23362 = VERTEX_POINT('',#105283) ;
#23363 = VERTEX_POINT('',#105305) ;
#23364 = VERTEX_POINT('',#105322) ;
#23365 = VERTEX_POINT('',#105344) ;
#23366 = VERTEX_POINT('',#105361) ;
#23367 = VERTEX_POINT('',#105466) ;
#23368 = VERTEX_POINT('',#105468) ;
#23369 = VERTEX_POINT('',#105472) ;
#23370 = VERTEX_POINT('',#105491) ;
#23371 = VERTEX_POINT('',#105493) ;
#23372 = VERTEX_POINT('',#105497) ;
#23373 = VERTEX_POINT('',#105516) ;
#23374 = VERTEX_POINT('',#105519) ;
#23375 = VERTEX_POINT('',#105606) ;
#23376 = VERTEX_POINT('',#105612) ;
#23377 = VERTEX_POINT('',#105719) ;
#23378 = VERTEX_POINT('',#105725) ;
#23379 = VERTEX_POINT('',#105748) ;
#23380 = VERTEX_POINT('',#105749) ;
#23381 = VERTEX_POINT('',#105751) ;
#23382 = VERTEX_POINT('',#105766) ;
#23383 = VERTEX_POINT('',#105783) ;
#23384 = VERTEX_POINT('',#105785) ;
#23385 = VERTEX_POINT('',#105804) ;
#23386 = VERTEX_POINT('',#105806) ;
#23387 = VERTEX_POINT('',#105825) ;
#23388 = VERTEX_POINT('',#105827) ;
#23389 = VERTEX_POINT('',#105844) ;
#23390 = VERTEX_POINT('',#105846) ;
#23391 = VERTEX_POINT('',#105863) ;
#23392 = VERTEX_POINT('',#105865) ;
#23393 = VERTEX_POINT('',#105884) ;
#23394 = VERTEX_POINT('',#105886) ;
#23395 = VERTEX_POINT('',#105905) ;
#23396 = VERTEX_POINT('',#105907) ;
#23397 = VERTEX_POINT('',#105924) ;
#23398 = VERTEX_POINT('',#105926) ;
#23399 = VERTEX_POINT('',#105943) ;
#23400 = VERTEX_POINT('',#105945) ;
#23401 = VERTEX_POINT('',#105964) ;
#23402 = VERTEX_POINT('',#105966) ;
#23403 = VERTEX_POINT('',#105985) ;
#23404 = VERTEX_POINT('',#105987) ;
#23405 = VERTEX_POINT('',#106004) ;
#23406 = VERTEX_POINT('',#106006) ;
#23407 = VERTEX_POINT('',#106023) ;
#23408 = VERTEX_POINT('',#106025) ;
#23409 = VERTEX_POINT('',#106044) ;
#23410 = VERTEX_POINT('',#106046) ;
#23411 = VERTEX_POINT('',#106065) ;
#23412 = VERTEX_POINT('',#106067) ;
#23413 = VERTEX_POINT('',#106084) ;
#23414 = VERTEX_POINT('',#106086) ;
#23415 = VERTEX_POINT('',#106103) ;
#23416 = VERTEX_POINT('',#106105) ;
#23417 = VERTEX_POINT('',#106124) ;
#23418 = VERTEX_POINT('',#106126) ;
#23419 = VERTEX_POINT('',#106145) ;
#23420 = VERTEX_POINT('',#106147) ;
#23421 = VERTEX_POINT('',#106164) ;
#23422 = VERTEX_POINT('',#106166) ;
#23423 = VERTEX_POINT('',#106183) ;
#23424 = VERTEX_POINT('',#106185) ;
#23425 = VERTEX_POINT('',#106204) ;
#23426 = VERTEX_POINT('',#106206) ;
#23427 = VERTEX_POINT('',#106225) ;
#23428 = VERTEX_POINT('',#106227) ;
#23429 = VERTEX_POINT('',#106244) ;
#23430 = VERTEX_POINT('',#106246) ;
#23431 = VERTEX_POINT('',#106263) ;
#23432 = VERTEX_POINT('',#106265) ;
#23433 = VERTEX_POINT('',#106284) ;
#23434 = VERTEX_POINT('',#106286) ;
#23435 = VERTEX_POINT('',#106305) ;
#23436 = VERTEX_POINT('',#106307) ;
#23437 = VERTEX_POINT('',#106324) ;
#23438 = VERTEX_POINT('',#106326) ;
#23439 = VERTEX_POINT('',#106343) ;
#23440 = VERTEX_POINT('',#106345) ;
#23441 = VERTEX_POINT('',#106364) ;
#23442 = VERTEX_POINT('',#106366) ;
#23443 = VERTEX_POINT('',#106385) ;
#23444 = VERTEX_POINT('',#106387) ;
#23445 = VERTEX_POINT('',#106404) ;
#23446 = VERTEX_POINT('',#106406) ;
#23447 = VERTEX_POINT('',#106423) ;
#23448 = VERTEX_POINT('',#106425) ;
#23449 = VERTEX_POINT('',#106444) ;
#23450 = VERTEX_POINT('',#106446) ;
#23451 = VERTEX_POINT('',#106465) ;
#23452 = VERTEX_POINT('',#106467) ;
#23453 = VERTEX_POINT('',#106484) ;
#23454 = VERTEX_POINT('',#106486) ;
#23455 = VERTEX_POINT('',#106503) ;
#23456 = VERTEX_POINT('',#106505) ;
#23457 = VERTEX_POINT('',#106524) ;
#23458 = VERTEX_POINT('',#106526) ;
#23459 = VERTEX_POINT('',#106545) ;
#23460 = VERTEX_POINT('',#106547) ;
#23461 = VERTEX_POINT('',#106564) ;
#23462 = VERTEX_POINT('',#106566) ;
#23463 = VERTEX_POINT('',#106583) ;
#23464 = VERTEX_POINT('',#106585) ;
#23465 = VERTEX_POINT('',#106604) ;
#23466 = VERTEX_POINT('',#106606) ;
#23467 = VERTEX_POINT('',#106625) ;
#23468 = VERTEX_POINT('',#106627) ;
#23469 = VERTEX_POINT('',#106644) ;
#23470 = VERTEX_POINT('',#106646) ;
#23471 = VERTEX_POINT('',#106663) ;
#23472 = VERTEX_POINT('',#106665) ;
#23473 = VERTEX_POINT('',#106684) ;
#23474 = VERTEX_POINT('',#106686) ;
#23475 = VERTEX_POINT('',#106705) ;
#23476 = VERTEX_POINT('',#106707) ;
#23477 = VERTEX_POINT('',#106724) ;
#23478 = VERTEX_POINT('',#106726) ;
#23479 = VERTEX_POINT('',#106743) ;
#23480 = VERTEX_POINT('',#106745) ;
#23481 = VERTEX_POINT('',#106764) ;
#23482 = VERTEX_POINT('',#106766) ;
#23483 = VERTEX_POINT('',#106785) ;
#23484 = VERTEX_POINT('',#106787) ;
#23485 = VERTEX_POINT('',#106804) ;
#23486 = VERTEX_POINT('',#106806) ;
#23487 = VERTEX_POINT('',#106823) ;
#23488 = VERTEX_POINT('',#106825) ;
#23489 = VERTEX_POINT('',#106844) ;
#23490 = VERTEX_POINT('',#106846) ;
#23491 = VERTEX_POINT('',#106865) ;
#23492 = VERTEX_POINT('',#106867) ;
#23493 = VERTEX_POINT('',#106884) ;
#23494 = VERTEX_POINT('',#106886) ;
#23495 = VERTEX_POINT('',#106903) ;
#23496 = VERTEX_POINT('',#106905) ;
#23497 = VERTEX_POINT('',#106924) ;
#23498 = VERTEX_POINT('',#106926) ;
#23499 = VERTEX_POINT('',#106945) ;
#23500 = VERTEX_POINT('',#106947) ;
#23501 = VERTEX_POINT('',#106964) ;
#23502 = VERTEX_POINT('',#106966) ;
#23503 = VERTEX_POINT('',#106983) ;
#23504 = VERTEX_POINT('',#106985) ;
#23505 = VERTEX_POINT('',#107004) ;
#23506 = VERTEX_POINT('',#107006) ;
#23507 = VERTEX_POINT('',#107025) ;
#23508 = VERTEX_POINT('',#107027) ;
#23509 = VERTEX_POINT('',#107044) ;
#23510 = VERTEX_POINT('',#107046) ;
#23511 = VERTEX_POINT('',#107063) ;
#23512 = VERTEX_POINT('',#107065) ;
#23513 = VERTEX_POINT('',#107084) ;
#23514 = VERTEX_POINT('',#107086) ;
#23515 = VERTEX_POINT('',#107105) ;
#23516 = VERTEX_POINT('',#107107) ;
#23517 = VERTEX_POINT('',#107124) ;
#23518 = VERTEX_POINT('',#107126) ;
#23519 = VERTEX_POINT('',#107143) ;
#23520 = VERTEX_POINT('',#107145) ;
#23521 = VERTEX_POINT('',#107164) ;
#23522 = VERTEX_POINT('',#107166) ;
#23523 = VERTEX_POINT('',#107185) ;
#23524 = VERTEX_POINT('',#107187) ;
#23525 = VERTEX_POINT('',#107204) ;
#23526 = VERTEX_POINT('',#107206) ;
#23527 = VERTEX_POINT('',#107223) ;
#23528 = VERTEX_POINT('',#107225) ;
#23529 = VERTEX_POINT('',#107244) ;
#23530 = VERTEX_POINT('',#107246) ;
#23531 = VERTEX_POINT('',#107265) ;
#23532 = VERTEX_POINT('',#107267) ;
#23533 = VERTEX_POINT('',#107284) ;
#23534 = VERTEX_POINT('',#107286) ;
#23535 = VERTEX_POINT('',#107303) ;
#23536 = VERTEX_POINT('',#107305) ;
#23537 = VERTEX_POINT('',#107324) ;
#23538 = VERTEX_POINT('',#107326) ;
#23539 = VERTEX_POINT('',#107348) ;
#23540 = VERTEX_POINT('',#107350) ;
#23541 = VERTEX_POINT('',#107354) ;
#23542 = VERTEX_POINT('',#107358) ;
#23543 = VERTEX_POINT('',#107362) ;
#23544 = VERTEX_POINT('',#107366) ;
#23545 = VERTEX_POINT('',#107370) ;
#23546 = VERTEX_POINT('',#107374) ;
#23547 = VERTEX_POINT('',#107378) ;
#23548 = VERTEX_POINT('',#107382) ;
#23549 = VERTEX_POINT('',#107386) ;
#23550 = VERTEX_POINT('',#107390) ;
#23551 = VERTEX_POINT('',#107394) ;
#23552 = VERTEX_POINT('',#107398) ;
#23553 = VERTEX_POINT('',#107402) ;
#23554 = VERTEX_POINT('',#107406) ;
#23555 = VERTEX_POINT('',#107410) ;
#23556 = VERTEX_POINT('',#107414) ;
#23557 = VERTEX_POINT('',#107418) ;
#23558 = VERTEX_POINT('',#107422) ;
#23559 = VERTEX_POINT('',#107426) ;
#23560 = VERTEX_POINT('',#107430) ;
#23561 = VERTEX_POINT('',#107434) ;
#23562 = VERTEX_POINT('',#107438) ;
#23563 = VERTEX_POINT('',#107442) ;
#23564 = VERTEX_POINT('',#107446) ;
#23565 = VERTEX_POINT('',#107450) ;
#23566 = VERTEX_POINT('',#107454) ;
#23567 = VERTEX_POINT('',#107458) ;
#23568 = VERTEX_POINT('',#107462) ;
#23569 = VERTEX_POINT('',#107466) ;
#23570 = VERTEX_POINT('',#107470) ;
#23571 = VERTEX_POINT('',#107474) ;
#23572 = VERTEX_POINT('',#107478) ;
#23573 = VERTEX_POINT('',#107482) ;
#23574 = VERTEX_POINT('',#107486) ;
#23575 = VERTEX_POINT('',#107490) ;
#23576 = VERTEX_POINT('',#107494) ;
#23577 = VERTEX_POINT('',#107498) ;
#23578 = VERTEX_POINT('',#107502) ;
#23579 = VERTEX_POINT('',#107506) ;
#23580 = VERTEX_POINT('',#107546) ;
#23581 = VERTEX_POINT('',#107554) ;
#23582 = VERTEX_POINT('',#107556) ;
#23583 = VERTEX_POINT('',#107558) ;
#23584 = VERTEX_POINT('',#107560) ;
#23585 = VERTEX_POINT('',#107562) ;
#23586 = VERTEX_POINT('',#107564) ;
#23587 = VERTEX_POINT('',#107566) ;
#23588 = VERTEX_POINT('',#107568) ;
#23589 = VERTEX_POINT('',#107570) ;
#23590 = VERTEX_POINT('',#107572) ;
#23591 = VERTEX_POINT('',#107574) ;
#23592 = VERTEX_POINT('',#107576) ;
#23593 = VERTEX_POINT('',#107578) ;
#23594 = VERTEX_POINT('',#107580) ;
#23595 = VERTEX_POINT('',#107582) ;
#23596 = VERTEX_POINT('',#107584) ;
#23597 = VERTEX_POINT('',#107586) ;
#23598 = VERTEX_POINT('',#107588) ;
#23599 = VERTEX_POINT('',#107590) ;
#23600 = VERTEX_POINT('',#107592) ;
#23601 = VERTEX_POINT('',#107594) ;
#23602 = VERTEX_POINT('',#107596) ;
#23603 = VERTEX_POINT('',#107598) ;
#23604 = VERTEX_POINT('',#107600) ;
#23605 = VERTEX_POINT('',#107602) ;
#23606 = VERTEX_POINT('',#107604) ;
#23607 = VERTEX_POINT('',#107606) ;
#23608 = VERTEX_POINT('',#107608) ;
#23609 = VERTEX_POINT('',#107610) ;
#23610 = VERTEX_POINT('',#107612) ;
#23611 = VERTEX_POINT('',#107614) ;
#23612 = VERTEX_POINT('',#107616) ;
#23613 = VERTEX_POINT('',#107618) ;
#23614 = VERTEX_POINT('',#107620) ;
#23615 = VERTEX_POINT('',#107622) ;
#23616 = VERTEX_POINT('',#107624) ;
#23617 = VERTEX_POINT('',#107626) ;
#23618 = VERTEX_POINT('',#107628) ;
#23619 = VERTEX_POINT('',#107630) ;
#23620 = VERTEX_POINT('',#107632) ;
#23621 = VERTEX_POINT('',#107634) ;
#23622 = VERTEX_POINT('',#107638) ;
#23623 = VERTEX_POINT('',#107640) ;
#23624 = VERTEX_POINT('',#107644) ;
#23625 = VERTEX_POINT('',#107646) ;
#23626 = VERTEX_POINT('',#107650) ;
#23627 = VERTEX_POINT('',#107652) ;
#23628 = VERTEX_POINT('',#107656) ;
#23629 = VERTEX_POINT('',#107658) ;
#23630 = VERTEX_POINT('',#107662) ;
#23631 = VERTEX_POINT('',#107664) ;
#23632 = VERTEX_POINT('',#107668) ;
#23633 = VERTEX_POINT('',#107670) ;
#23634 = VERTEX_POINT('',#107674) ;
#23635 = VERTEX_POINT('',#107676) ;
#23636 = VERTEX_POINT('',#107680) ;
#23637 = VERTEX_POINT('',#107682) ;
#23638 = VERTEX_POINT('',#107686) ;
#23639 = VERTEX_POINT('',#107688) ;
#23640 = VERTEX_POINT('',#107692) ;
#23641 = VERTEX_POINT('',#107694) ;
#23642 = VERTEX_POINT('',#107698) ;
#23643 = VERTEX_POINT('',#107700) ;
#23644 = VERTEX_POINT('',#107704) ;
#23645 = VERTEX_POINT('',#107706) ;
#23646 = VERTEX_POINT('',#107710) ;
#23647 = VERTEX_POINT('',#107712) ;
#23648 = VERTEX_POINT('',#107716) ;
#23649 = VERTEX_POINT('',#107718) ;
#23650 = VERTEX_POINT('',#107722) ;
#23651 = VERTEX_POINT('',#107724) ;
#23652 = VERTEX_POINT('',#107728) ;
#23653 = VERTEX_POINT('',#107730) ;
#23654 = VERTEX_POINT('',#107734) ;
#23655 = VERTEX_POINT('',#107736) ;
#23656 = VERTEX_POINT('',#107740) ;
#23657 = VERTEX_POINT('',#107742) ;
#23658 = VERTEX_POINT('',#107746) ;
#23659 = VERTEX_POINT('',#107748) ;
#23660 = VERTEX_POINT('',#107752) ;
#23661 = VERTEX_POINT('',#107754) ;
#23662 = VERTEX_POINT('',#107758) ;
#23663 = VERTEX_POINT('',#107773) ;
#23664 = VERTEX_POINT('',#107790) ;
#23665 = VERTEX_POINT('',#107809) ;
#23666 = VERTEX_POINT('',#107842) ;
#23667 = VERTEX_POINT('',#107893) ;
#23668 = VERTEX_POINT('',#107894) ;
#23669 = VERTEX_POINT('',#107990) ;
#23670 = VERTEX_POINT('',#107991) ;
#23671 = VERTEX_POINT('',#108087) ;
#23672 = VERTEX_POINT('',#108088) ;
#23673 = VERTEX_POINT('',#108184) ;
#23674 = VERTEX_POINT('',#108185) ;
#23675 = VERTEX_POINT('',#108281) ;
#23676 = VERTEX_POINT('',#108282) ;
#23677 = VERTEX_POINT('',#108378) ;
#23678 = VERTEX_POINT('',#108379) ;
#23679 = VERTEX_POINT('',#108475) ;
#23680 = VERTEX_POINT('',#108476) ;
#23681 = VERTEX_POINT('',#108572) ;
#23682 = VERTEX_POINT('',#108573) ;
#23683 = VERTEX_POINT('',#108765) ;
#23684 = VERTEX_POINT('',#108782) ;
#23685 = VERTEX_POINT('',#108804) ;
#23686 = VERTEX_POINT('',#108821) ;
#23687 = VERTEX_POINT('',#108843) ;
#23688 = VERTEX_POINT('',#108860) ;
#23689 = VERTEX_POINT('',#108882) ;
#23690 = VERTEX_POINT('',#108899) ;
#23691 = VERTEX_POINT('',#108921) ;
#23692 = VERTEX_POINT('',#108938) ;
#23693 = VERTEX_POINT('',#108960) ;
#23694 = VERTEX_POINT('',#108977) ;
#23695 = VERTEX_POINT('',#108999) ;
#23696 = VERTEX_POINT('',#109016) ;
#23697 = VERTEX_POINT('',#109038) ;
#23698 = VERTEX_POINT('',#109055) ;
#23699 = VERTEX_POINT('',#109077) ;
#23700 = VERTEX_POINT('',#109094) ;
#23701 = VERTEX_POINT('',#109199) ;
#23702 = VERTEX_POINT('',#109200) ;
#23703 = VERTEX_POINT('',#109202) ;
#23704 = VERTEX_POINT('',#109283) ;
#23705 = VERTEX_POINT('',#109334) ;
#23706 = VERTEX_POINT('',#109335) ;
#23707 = VERTEX_POINT('',#109622) ;
#23708 = VERTEX_POINT('',#109623) ;
#23709 = VERTEX_POINT('',#109625) ;
#23710 = VERTEX_POINT('',#109688) ;
#23711 = VERTEX_POINT('',#109745) ;
#23712 = VERTEX_POINT('',#109746) ;
#23713 = VERTEX_POINT('',#109748) ;
#23714 = VERTEX_POINT('',#109873) ;
#23715 = VERTEX_POINT('',#109981) ;
#23716 = VERTEX_POINT('',#109982) ;
#23717 = VERTEX_POINT('',#109984) ;
#23718 = VERTEX_POINT('',#110079) ;
#23719 = VERTEX_POINT('',#110142) ;
#23720 = VERTEX_POINT('',#110143) ;
#23721 = VERTEX_POINT('',#110145) ;
#23722 = VERTEX_POINT('',#110477) ;
#23723 = VERTEX_POINT('',#110478) ;
#23724 = VERTEX_POINT('',#110811) ;
#23725 = VERTEX_POINT('',#110812) ;
#23726 = VERTEX_POINT('',#110814) ;
#23727 = VERTEX_POINT('',#111142) ;
#23728 = VERTEX_POINT('',#111143) ;
#23729 = VERTEX_POINT('',#111470) ;
#23730 = VERTEX_POINT('',#111471) ;
#23731 = VERTEX_POINT('',#111473) ;
#23732 = VERTEX_POINT('',#111810) ;
#23733 = VERTEX_POINT('',#111812) ;
#23734 = VERTEX_POINT('',#111813) ;
#23735 = VERTEX_POINT('',#111815) ;
#23736 = VERTEX_POINT('',#111824) ;
#23737 = VERTEX_POINT('',#112018) ;
#23738 = VERTEX_POINT('',#112212) ;
#23739 = VERTEX_POINT('',#112409) ;
#23740 = VERTEX_POINT('',#112471) ;
#23741 = VERTEX_POINT('',#112476) ;
#23742 = VERTEX_POINT('',#112478) ;
#23743 = VERTEX_POINT('',#112484) ;
#23744 = VERTEX_POINT('',#112678) ;
#23745 = VERTEX_POINT('',#112875) ;
#23746 = VERTEX_POINT('',#113069) ;
#23747 = VERTEX_POINT('',#113231) ;
#23748 = VERTEX_POINT('',#113232) ;
#23749 = VERTEX_POINT('',#113234) ;
#23750 = VERTEX_POINT('',#113243) ;
#23751 = VERTEX_POINT('',#113434) ;
#23752 = VERTEX_POINT('',#113625) ;
#23753 = VERTEX_POINT('',#113816) ;
#23754 = VERTEX_POINT('',#114010) ;
#23755 = VERTEX_POINT('',#114201) ;
#23756 = VERTEX_POINT('',#114263) ;
#23757 = VERTEX_POINT('',#114268) ;
#23758 = VERTEX_POINT('',#114270) ;
#23759 = VERTEX_POINT('',#114276) ;
#23760 = VERTEX_POINT('',#114467) ;
#23761 = VERTEX_POINT('',#114658) ;
#23762 = VERTEX_POINT('',#114849) ;
#23763 = VERTEX_POINT('',#115040) ;
#23764 = VERTEX_POINT('',#115231) ;
#23765 = VERTEX_POINT('',#115393) ;
#23766 = VERTEX_POINT('',#115396) ;
#23767 = VERTEX_POINT('',#115505) ;
#23768 = VERTEX_POINT('',#115507) ;
#23769 = VERTEX_POINT('',#115598) ;
#23770 = VERTEX_POINT('',#115695) ;
#23771 = VERTEX_POINT('',#115697) ;
#23772 = VERTEX_POINT('',#115873) ;
#23773 = VERTEX_POINT('',#116090) ;
#23774 = VERTEX_POINT('',#116482) ;
#23775 = EDGE_CURVE('',#19561,#19561,#17034,.T.) ;
#23776 = EDGE_CURVE('',#19561,#19562,#17035,.T.) ;
#23777 = EDGE_CURVE('',#19562,#19562,#17036,.T.) ;
#23778 = EDGE_CURVE('',#19562,#19563,#3032,.T.) ;
#23779 = EDGE_CURVE('',#19564,#19563,#17037,.T.) ;
#23780 = EDGE_CURVE('',#19565,#19564,#3033,.T.) ;
#23781 = EDGE_CURVE('',#19566,#19565,#17038,.T.) ;
#23782 = EDGE_CURVE('',#19567,#19566,#3034,.T.) ;
#23783 = EDGE_CURVE('',#19568,#19567,#17039,.T.) ;
#23784 = EDGE_CURVE('',#19569,#19568,#3035,.T.) ;
#23785 = EDGE_CURVE('',#19570,#19569,#17040,.T.) ;
#23786 = EDGE_CURVE('',#19571,#19570,#3036,.T.) ;
#23787 = EDGE_CURVE('',#19572,#19571,#17041,.T.) ;
#23788 = EDGE_CURVE('',#19573,#19572,#3037,.T.) ;
#23789 = EDGE_CURVE('',#19574,#19573,#17042,.T.) ;
#23790 = EDGE_CURVE('',#19575,#19574,#3038,.T.) ;
#23791 = EDGE_CURVE('',#19576,#19575,#17043,.T.) ;
#23792 = EDGE_CURVE('',#19577,#19576,#3039,.T.) ;
#23793 = EDGE_CURVE('',#19578,#19577,#17044,.T.) ;
#23794 = EDGE_CURVE('',#19579,#19578,#3040,.T.) ;
#23795 = EDGE_CURVE('',#19580,#19579,#17045,.T.) ;
#23796 = EDGE_CURVE('',#19581,#19580,#3041,.T.) ;
#23797 = EDGE_CURVE('',#19582,#19581,#17046,.T.) ;
#23798 = EDGE_CURVE('',#19583,#19582,#3042,.T.) ;
#23799 = EDGE_CURVE('',#19584,#19583,#17047,.T.) ;
#23800 = EDGE_CURVE('',#19585,#19584,#3043,.T.) ;
#23801 = EDGE_CURVE('',#19586,#19585,#17048,.T.) ;
#23802 = EDGE_CURVE('',#19587,#19586,#3044,.T.) ;
#23803 = EDGE_CURVE('',#19588,#19587,#17049,.T.) ;
#23804 = EDGE_CURVE('',#19589,#19588,#3045,.T.) ;
#23805 = EDGE_CURVE('',#19590,#19589,#17050,.T.) ;
#23806 = EDGE_CURVE('',#19591,#19590,#3046,.T.) ;
#23807 = EDGE_CURVE('',#19592,#19591,#17051,.T.) ;
#23808 = EDGE_CURVE('',#19593,#19592,#3047,.T.) ;
#23809 = EDGE_CURVE('',#19594,#19593,#17052,.T.) ;
#23810 = EDGE_CURVE('',#19595,#19594,#3048,.T.) ;
#23811 = EDGE_CURVE('',#19596,#19595,#17053,.T.) ;
#23812 = EDGE_CURVE('',#19597,#19596,#3049,.T.) ;
#23813 = EDGE_CURVE('',#19598,#19597,#17054,.T.) ;
#23814 = EDGE_CURVE('',#19599,#19598,#3050,.T.) ;
#23815 = EDGE_CURVE('',#19600,#19599,#17055,.T.) ;
#23816 = EDGE_CURVE('',#19601,#19600,#3051,.T.) ;
#23817 = EDGE_CURVE('',#19602,#19601,#17056,.T.) ;
#23818 = EDGE_CURVE('',#19603,#19602,#3052,.T.) ;
#23819 = EDGE_CURVE('',#19604,#19603,#17057,.T.) ;
#23820 = EDGE_CURVE('',#19605,#19604,#3053,.T.) ;
#23821 = EDGE_CURVE('',#19606,#19605,#17058,.T.) ;
#23822 = EDGE_CURVE('',#19607,#19606,#3054,.T.) ;
#23823 = EDGE_CURVE('',#19608,#19607,#17059,.T.) ;
#23824 = EDGE_CURVE('',#19609,#19608,#3055,.T.) ;
#23825 = EDGE_CURVE('',#19610,#19609,#17060,.T.) ;
#23826 = EDGE_CURVE('',#19611,#19610,#3056,.T.) ;
#23827 = EDGE_CURVE('',#19612,#19611,#17061,.T.) ;
#23828 = EDGE_CURVE('',#19613,#19612,#3057,.T.) ;
#23829 = EDGE_CURVE('',#19614,#19613,#17062,.T.) ;
#23830 = EDGE_CURVE('',#19615,#19614,#3058,.T.) ;
#23831 = EDGE_CURVE('',#19616,#19615,#17063,.T.) ;
#23832 = EDGE_CURVE('',#19617,#19616,#3059,.T.) ;
#23833 = EDGE_CURVE('',#19618,#19617,#17064,.T.) ;
#23834 = EDGE_CURVE('',#19619,#19618,#3060,.T.) ;
#23835 = EDGE_CURVE('',#19620,#19619,#17065,.T.) ;
#23836 = EDGE_CURVE('',#19621,#19620,#3061,.T.) ;
#23837 = EDGE_CURVE('',#19622,#19621,#17066,.T.) ;
#23838 = EDGE_CURVE('',#19623,#19622,#3062,.T.) ;
#23839 = EDGE_CURVE('',#19624,#19623,#17067,.T.) ;
#23840 = EDGE_CURVE('',#19625,#19624,#3063,.T.) ;
#23841 = EDGE_CURVE('',#19626,#19625,#17068,.T.) ;
#23842 = EDGE_CURVE('',#19627,#19626,#3064,.T.) ;
#23843 = EDGE_CURVE('',#19628,#19627,#17069,.T.) ;
#23844 = EDGE_CURVE('',#19629,#19628,#3065,.T.) ;
#23845 = EDGE_CURVE('',#19630,#19629,#17070,.T.) ;
#23846 = EDGE_CURVE('',#19631,#19630,#3066,.T.) ;
#23847 = EDGE_CURVE('',#19632,#19631,#17071,.T.) ;
#23848 = EDGE_CURVE('',#19633,#19632,#3067,.T.) ;
#23849 = EDGE_CURVE('',#19634,#19633,#17072,.T.) ;
#23850 = EDGE_CURVE('',#19635,#19634,#3068,.T.) ;
#23851 = EDGE_CURVE('',#19636,#19635,#17073,.T.) ;
#23852 = EDGE_CURVE('',#19637,#19636,#3069,.T.) ;
#23853 = EDGE_CURVE('',#19638,#19637,#17074,.T.) ;
#23854 = EDGE_CURVE('',#19639,#19638,#3070,.T.) ;
#23855 = EDGE_CURVE('',#19640,#19639,#17075,.T.) ;
#23856 = EDGE_CURVE('',#19641,#19640,#3071,.T.) ;
#23857 = EDGE_CURVE('',#19642,#19641,#17076,.T.) ;
#23858 = EDGE_CURVE('',#19643,#19642,#3072,.T.) ;
#23859 = EDGE_CURVE('',#19563,#19643,#17077,.T.) ;
#23860 = EDGE_CURVE('',#19644,#19645,#17078,.T.) ;
#23861 = EDGE_CURVE('',#19645,#19646,#3073,.T.) ;
#23862 = EDGE_CURVE('',#19646,#19647,#17079,.T.) ;
#23863 = EDGE_CURVE('',#19647,#19644,#3074,.T.) ;
#23864 = EDGE_CURVE('',#19648,#19649,#17080,.T.) ;
#23865 = EDGE_CURVE('',#19649,#19650,#3075,.T.) ;
#23866 = EDGE_CURVE('',#19650,#19651,#17081,.T.) ;
#23867 = EDGE_CURVE('',#19651,#19648,#3076,.T.) ;
#23868 = EDGE_CURVE('',#19652,#19653,#17082,.T.) ;
#23869 = EDGE_CURVE('',#19653,#19651,#17083,.T.) ;
#23870 = EDGE_CURVE('',#19650,#19652,#17084,.T.) ;
#23871 = EDGE_CURVE('',#19645,#19654,#17085,.T.) ;
#23872 = EDGE_CURVE('',#19654,#19653,#3077,.T.) ;
#23873 = EDGE_CURVE('',#19652,#19645,#3078,.T.) ;
#23874 = EDGE_CURVE('',#19655,#19656,#17086,.T.) ;
#23875 = EDGE_CURVE('',#19656,#19649,#3079,.T.) ;
#23876 = EDGE_CURVE('',#19649,#19657,#17087,.T.) ;
#23877 = EDGE_CURVE('',#19657,#19655,#3080,.T.) ;
#23878 = EDGE_CURVE('',#19658,#19659,#17088,.T.) ;
#23879 = EDGE_CURVE('',#19659,#19660,#3081,.T.) ;
#23880 = EDGE_CURVE('',#19660,#19661,#17089,.T.) ;
#23881 = EDGE_CURVE('',#19661,#19658,#3082,.T.) ;
#23882 = EDGE_CURVE('',#19662,#19663,#17090,.T.) ;
#23883 = EDGE_CURVE('',#19663,#19661,#17091,.T.) ;
#23884 = EDGE_CURVE('',#19660,#19662,#17092,.T.) ;
#23885 = EDGE_CURVE('',#19656,#19664,#17093,.T.) ;
#23886 = EDGE_CURVE('',#19664,#19663,#3083,.T.) ;
#23887 = EDGE_CURVE('',#19662,#19656,#3084,.T.) ;
#23888 = EDGE_CURVE('',#19665,#19666,#17094,.T.) ;
#23889 = EDGE_CURVE('',#19666,#19659,#3085,.T.) ;
#23890 = EDGE_CURVE('',#19659,#19667,#17095,.T.) ;
#23891 = EDGE_CURVE('',#19667,#19665,#3086,.T.) ;
#23892 = EDGE_CURVE('',#19668,#19669,#17096,.T.) ;
#23893 = EDGE_CURVE('',#19669,#19670,#3087,.T.) ;
#23894 = EDGE_CURVE('',#19670,#19671,#17097,.T.) ;
#23895 = EDGE_CURVE('',#19671,#19668,#3088,.T.) ;
#23896 = EDGE_CURVE('',#19672,#19673,#17098,.T.) ;
#23897 = EDGE_CURVE('',#19673,#19671,#17099,.T.) ;
#23898 = EDGE_CURVE('',#19670,#19672,#17100,.T.) ;
#23899 = EDGE_CURVE('',#19666,#19674,#17101,.T.) ;
#23900 = EDGE_CURVE('',#19674,#19673,#3089,.T.) ;
#23901 = EDGE_CURVE('',#19672,#19666,#3090,.T.) ;
#23902 = EDGE_CURVE('',#19675,#19676,#17102,.T.) ;
#23903 = EDGE_CURVE('',#19676,#19669,#3091,.T.) ;
#23904 = EDGE_CURVE('',#19669,#19677,#17103,.T.) ;
#23905 = EDGE_CURVE('',#19677,#19675,#3092,.T.) ;
#23906 = EDGE_CURVE('',#19678,#19679,#17104,.T.) ;
#23907 = EDGE_CURVE('',#19679,#19680,#17105,.T.) ;
#23908 = EDGE_CURVE('',#19680,#19681,#17106,.T.) ;
#23909 = EDGE_CURVE('',#19681,#19678,#17107,.T.) ;
#23910 = EDGE_CURVE('',#19676,#19682,#17108,.T.) ;
#23911 = EDGE_CURVE('',#19682,#19681,#3093,.T.) ;
#23912 = EDGE_CURVE('',#19680,#19676,#3094,.T.) ;
#23913 = EDGE_CURVE('',#19683,#19646,#17109,.T.) ;
#23914 = EDGE_CURVE('',#19646,#19679,#3095,.T.) ;
#23915 = EDGE_CURVE('',#19678,#19683,#3096,.T.) ;
#23916 = EDGE_CURVE('',#19675,#19682,#17110,.T.) ;
#23917 = EDGE_CURVE('',#19668,#19677,#17111,.T.) ;
#23918 = EDGE_CURVE('',#19665,#19674,#17112,.T.) ;
#23919 = EDGE_CURVE('',#19658,#19667,#17113,.T.) ;
#23920 = EDGE_CURVE('',#19655,#19664,#17114,.T.) ;
#23921 = EDGE_CURVE('',#19648,#19657,#17115,.T.) ;
#23922 = EDGE_CURVE('',#19644,#19654,#17116,.T.) ;
#23923 = EDGE_CURVE('',#19683,#19647,#17117,.T.) ;
#23924 = EDGE_CURVE('',#19684,#19664,#3097,.T.) ;
#23925 = EDGE_CURVE('',#19685,#19684,#3098,.T.) ;
#23926 = EDGE_CURVE('',#19663,#19685,#3099,.T.) ;
#23927 = EDGE_CURVE('',#19655,#19686,#3100,.T.) ;
#23928 = EDGE_CURVE('',#19686,#19684,#17118,.F.) ;
#23929 = EDGE_CURVE('',#19687,#19657,#3101,.T.) ;
#23930 = EDGE_CURVE('',#19686,#19687,#3102,.T.) ;
#23931 = EDGE_CURVE('',#19648,#19688,#3103,.T.) ;
#23932 = EDGE_CURVE('',#19688,#19687,#17119,.F.) ;
#23933 = EDGE_CURVE('',#19689,#19651,#3104,.T.) ;
#23934 = EDGE_CURVE('',#19688,#19689,#3105,.T.) ;
#23935 = EDGE_CURVE('',#19653,#19690,#3106,.T.) ;
#23936 = EDGE_CURVE('',#19689,#19690,#17120,.T.) ;
#23937 = EDGE_CURVE('',#19691,#19654,#3107,.T.) ;
#23938 = EDGE_CURVE('',#19690,#19691,#3108,.T.) ;
#23939 = EDGE_CURVE('',#19644,#19692,#3109,.T.) ;
#23940 = EDGE_CURVE('',#19692,#19691,#17121,.F.) ;
#23941 = EDGE_CURVE('',#19693,#19647,#3110,.T.) ;
#23942 = EDGE_CURVE('',#19692,#19693,#3111,.T.) ;
#23943 = EDGE_CURVE('',#19683,#19694,#3112,.T.) ;
#23944 = EDGE_CURVE('',#19694,#19693,#17122,.F.) ;
#23945 = EDGE_CURVE('',#19695,#19678,#3113,.T.) ;
#23946 = EDGE_CURVE('',#19694,#19695,#3114,.T.) ;
#23947 = EDGE_CURVE('',#19681,#19696,#3115,.T.) ;
#23948 = EDGE_CURVE('',#19695,#19696,#17123,.T.) ;
#23949 = EDGE_CURVE('',#19697,#19629,#17124,.F.) ;
#23950 = EDGE_CURVE('',#19698,#19697,#17125,.F.) ;
#23951 = EDGE_CURVE('',#19629,#19698,#17126,.F.) ;
#23952 = EDGE_CURVE('',#19626,#19699,#17127,.F.) ;
#23953 = EDGE_CURVE('',#19700,#19626,#17128,.F.) ;
#23954 = EDGE_CURVE('',#19699,#19700,#17129,.F.) ;
#23955 = EDGE_CURVE('',#19630,#19701,#17130,.F.) ;
#23956 = EDGE_CURVE('',#19702,#19630,#17131,.F.) ;
#23957 = EDGE_CURVE('',#19701,#19702,#17132,.F.) ;
#23958 = EDGE_CURVE('',#19698,#19702,#17133,.T.) ;
#23959 = EDGE_CURVE('',#19703,#19625,#17134,.F.) ;
#23960 = EDGE_CURVE('',#19704,#19703,#17135,.F.) ;
#23961 = EDGE_CURVE('',#19625,#19704,#17136,.F.) ;
#23962 = EDGE_CURVE('',#19705,#19633,#17137,.F.) ;
#23963 = EDGE_CURVE('',#19706,#19705,#17138,.F.) ;
#23964 = EDGE_CURVE('',#19633,#19706,#17139,.F.) ;
#23965 = EDGE_CURVE('',#19702,#19706,#774,.T.) ;
#23966 = EDGE_CURVE('',#19705,#19701,#775,.T.) ;
#23967 = EDGE_CURVE('',#19622,#19707,#17140,.F.) ;
#23968 = EDGE_CURVE('',#19708,#19622,#17141,.F.) ;
#23969 = EDGE_CURVE('',#19707,#19708,#17142,.F.) ;
#23970 = EDGE_CURVE('',#19634,#19709,#17143,.F.) ;
#23971 = EDGE_CURVE('',#19710,#19634,#17144,.F.) ;
#23972 = EDGE_CURVE('',#19709,#19710,#17145,.F.) ;
#23973 = EDGE_CURVE('',#19706,#19710,#17146,.T.) ;
#23974 = EDGE_CURVE('',#19711,#19621,#17147,.F.) ;
#23975 = EDGE_CURVE('',#19712,#19711,#17148,.F.) ;
#23976 = EDGE_CURVE('',#19621,#19712,#17149,.F.) ;
#23977 = EDGE_CURVE('',#19713,#19637,#17150,.F.) ;
#23978 = EDGE_CURVE('',#19714,#19713,#17151,.F.) ;
#23979 = EDGE_CURVE('',#19637,#19714,#17152,.F.) ;
#23980 = EDGE_CURVE('',#19710,#19714,#776,.T.) ;
#23981 = EDGE_CURVE('',#19713,#19709,#777,.T.) ;
#23982 = EDGE_CURVE('',#19618,#19715,#17153,.F.) ;
#23983 = EDGE_CURVE('',#19716,#19618,#17154,.F.) ;
#23984 = EDGE_CURVE('',#19715,#19716,#17155,.F.) ;
#23985 = EDGE_CURVE('',#19638,#19717,#17156,.F.) ;
#23986 = EDGE_CURVE('',#19718,#19638,#17157,.F.) ;
#23987 = EDGE_CURVE('',#19717,#19718,#17158,.F.) ;
#23988 = EDGE_CURVE('',#19714,#19718,#17159,.T.) ;
#23989 = EDGE_CURVE('',#19719,#19617,#17160,.F.) ;
#23990 = EDGE_CURVE('',#19720,#19719,#17161,.F.) ;
#23991 = EDGE_CURVE('',#19617,#19720,#17162,.F.) ;
#23992 = EDGE_CURVE('',#19721,#19641,#17163,.F.) ;
#23993 = EDGE_CURVE('',#19722,#19721,#17164,.F.) ;
#23994 = EDGE_CURVE('',#19641,#19722,#17165,.F.) ;
#23995 = EDGE_CURVE('',#19718,#19722,#778,.T.) ;
#23996 = EDGE_CURVE('',#19721,#19717,#779,.T.) ;
#23997 = EDGE_CURVE('',#19614,#19723,#17166,.F.) ;
#23998 = EDGE_CURVE('',#19724,#19614,#17167,.F.) ;
#23999 = EDGE_CURVE('',#19723,#19724,#17168,.F.) ;
#24000 = EDGE_CURVE('',#19642,#19725,#17169,.F.) ;
#24001 = EDGE_CURVE('',#19726,#19642,#17170,.F.) ;
#24002 = EDGE_CURVE('',#19725,#19726,#17171,.F.) ;
#24003 = EDGE_CURVE('',#19722,#19726,#17172,.T.) ;
#24004 = EDGE_CURVE('',#19727,#19613,#17173,.F.) ;
#24005 = EDGE_CURVE('',#19728,#19727,#17174,.F.) ;
#24006 = EDGE_CURVE('',#19613,#19728,#17175,.F.) ;
#24007 = EDGE_CURVE('',#19729,#19565,#17176,.F.) ;
#24008 = EDGE_CURVE('',#19730,#19729,#17177,.F.) ;
#24009 = EDGE_CURVE('',#19565,#19730,#17178,.F.) ;
#24010 = EDGE_CURVE('',#19726,#19731,#780,.T.) ;
#24011 = EDGE_CURVE('',#19731,#19730,#781,.T.) ;
#24012 = EDGE_CURVE('',#19729,#19725,#782,.T.) ;
#24013 = EDGE_CURVE('',#19610,#19732,#17179,.F.) ;
#24014 = EDGE_CURVE('',#19733,#19610,#17180,.F.) ;
#24015 = EDGE_CURVE('',#19732,#19733,#17181,.F.) ;
#24016 = EDGE_CURVE('',#19566,#19734,#17182,.F.) ;
#24017 = EDGE_CURVE('',#19735,#19566,#17183,.F.) ;
#24018 = EDGE_CURVE('',#19734,#19735,#17184,.F.) ;
#24019 = EDGE_CURVE('',#19730,#19735,#17185,.T.) ;
#24020 = EDGE_CURVE('',#19736,#19609,#17186,.F.) ;
#24021 = EDGE_CURVE('',#19737,#19736,#17187,.F.) ;
#24022 = EDGE_CURVE('',#19609,#19737,#17188,.F.) ;
#24023 = EDGE_CURVE('',#19738,#19569,#17189,.F.) ;
#24024 = EDGE_CURVE('',#19739,#19738,#17190,.F.) ;
#24025 = EDGE_CURVE('',#19569,#19739,#17191,.F.) ;
#24026 = EDGE_CURVE('',#19735,#19739,#783,.T.) ;
#24027 = EDGE_CURVE('',#19738,#19734,#784,.T.) ;
#24028 = EDGE_CURVE('',#19606,#19740,#17192,.F.) ;
#24029 = EDGE_CURVE('',#19741,#19606,#17193,.F.) ;
#24030 = EDGE_CURVE('',#19740,#19741,#17194,.F.) ;
#24031 = EDGE_CURVE('',#19570,#19742,#17195,.F.) ;
#24032 = EDGE_CURVE('',#19743,#19570,#17196,.F.) ;
#24033 = EDGE_CURVE('',#19742,#19743,#17197,.F.) ;
#24034 = EDGE_CURVE('',#19739,#19743,#17198,.T.) ;
#24035 = EDGE_CURVE('',#19744,#19605,#17199,.F.) ;
#24036 = EDGE_CURVE('',#19745,#19744,#17200,.F.) ;
#24037 = EDGE_CURVE('',#19605,#19745,#17201,.F.) ;
#24038 = EDGE_CURVE('',#19746,#19573,#17202,.F.) ;
#24039 = EDGE_CURVE('',#19747,#19746,#17203,.F.) ;
#24040 = EDGE_CURVE('',#19573,#19747,#17204,.F.) ;
#24041 = EDGE_CURVE('',#19743,#19747,#785,.T.) ;
#24042 = EDGE_CURVE('',#19746,#19742,#786,.T.) ;
#24043 = EDGE_CURVE('',#19602,#19748,#17205,.F.) ;
#24044 = EDGE_CURVE('',#19749,#19602,#17206,.F.) ;
#24045 = EDGE_CURVE('',#19748,#19749,#17207,.F.) ;
#24046 = EDGE_CURVE('',#19574,#19750,#17208,.F.) ;
#24047 = EDGE_CURVE('',#19751,#19574,#17209,.F.) ;
#24048 = EDGE_CURVE('',#19750,#19751,#17210,.F.) ;
#24049 = EDGE_CURVE('',#19747,#19751,#17211,.T.) ;
#24050 = EDGE_CURVE('',#19752,#19601,#17212,.F.) ;
#24051 = EDGE_CURVE('',#19753,#19752,#17213,.F.) ;
#24052 = EDGE_CURVE('',#19601,#19753,#17214,.F.) ;
#24053 = EDGE_CURVE('',#19754,#19577,#17215,.F.) ;
#24054 = EDGE_CURVE('',#19755,#19754,#17216,.F.) ;
#24055 = EDGE_CURVE('',#19577,#19755,#17217,.F.) ;
#24056 = EDGE_CURVE('',#19751,#19755,#787,.T.) ;
#24057 = EDGE_CURVE('',#19754,#19750,#788,.T.) ;
#24058 = EDGE_CURVE('',#19598,#19756,#17218,.F.) ;
#24059 = EDGE_CURVE('',#19757,#19598,#17219,.F.) ;
#24060 = EDGE_CURVE('',#19756,#19757,#17220,.F.) ;
#24061 = EDGE_CURVE('',#19578,#19758,#17221,.F.) ;
#24062 = EDGE_CURVE('',#19759,#19578,#17222,.F.) ;
#24063 = EDGE_CURVE('',#19758,#19759,#17223,.F.) ;
#24064 = EDGE_CURVE('',#19755,#19759,#17224,.T.) ;
#24065 = EDGE_CURVE('',#19760,#19597,#17225,.F.) ;
#24066 = EDGE_CURVE('',#19761,#19760,#17226,.F.) ;
#24067 = EDGE_CURVE('',#19597,#19761,#17227,.F.) ;
#24068 = EDGE_CURVE('',#19762,#19581,#17228,.F.) ;
#24069 = EDGE_CURVE('',#19763,#19762,#17229,.F.) ;
#24070 = EDGE_CURVE('',#19581,#19763,#17230,.F.) ;
#24071 = EDGE_CURVE('',#19759,#19763,#789,.T.) ;
#24072 = EDGE_CURVE('',#19762,#19758,#790,.T.) ;
#24073 = EDGE_CURVE('',#19594,#19764,#17231,.F.) ;
#24074 = EDGE_CURVE('',#19765,#19594,#17232,.F.) ;
#24075 = EDGE_CURVE('',#19764,#19765,#17233,.F.) ;
#24076 = EDGE_CURVE('',#19582,#19766,#17234,.F.) ;
#24077 = EDGE_CURVE('',#19767,#19582,#17235,.F.) ;
#24078 = EDGE_CURVE('',#19766,#19767,#17236,.F.) ;
#24079 = EDGE_CURVE('',#19763,#19767,#17237,.T.) ;
#24080 = EDGE_CURVE('',#19768,#19593,#17238,.F.) ;
#24081 = EDGE_CURVE('',#19769,#19768,#17239,.F.) ;
#24082 = EDGE_CURVE('',#19593,#19769,#17240,.F.) ;
#24083 = EDGE_CURVE('',#19770,#19585,#17241,.F.) ;
#24084 = EDGE_CURVE('',#19771,#19770,#17242,.F.) ;
#24085 = EDGE_CURVE('',#19585,#19771,#17243,.F.) ;
#24086 = EDGE_CURVE('',#19767,#19771,#791,.T.) ;
#24087 = EDGE_CURVE('',#19770,#19766,#792,.T.) ;
#24088 = EDGE_CURVE('',#19590,#19772,#17244,.F.) ;
#24089 = EDGE_CURVE('',#19773,#19590,#17245,.F.) ;
#24090 = EDGE_CURVE('',#19772,#19773,#17246,.F.) ;
#24091 = EDGE_CURVE('',#19586,#19774,#17247,.F.) ;
#24092 = EDGE_CURVE('',#19775,#19586,#17248,.F.) ;
#24093 = EDGE_CURVE('',#19774,#19775,#17249,.F.) ;
#24094 = EDGE_CURVE('',#19771,#19775,#17250,.T.) ;
#24095 = EDGE_CURVE('',#19776,#19589,#17251,.F.) ;
#24096 = EDGE_CURVE('',#19777,#19776,#17252,.F.) ;
#24097 = EDGE_CURVE('',#19589,#19777,#17253,.F.) ;
#24098 = EDGE_CURVE('',#19775,#19777,#793,.T.) ;
#24099 = EDGE_CURVE('',#19776,#19774,#794,.T.) ;
#24100 = EDGE_CURVE('',#19777,#19773,#17254,.T.) ;
#24101 = EDGE_CURVE('',#19778,#19776,#3116,.T.) ;
#24102 = EDGE_CURVE('',#19588,#19778,#795,.T.) ;
#24103 = EDGE_CURVE('',#19774,#19779,#3117,.T.) ;
#24104 = EDGE_CURVE('',#19779,#19587,#796,.T.) ;
#24105 = EDGE_CURVE('',#19773,#19769,#797,.T.) ;
#24106 = EDGE_CURVE('',#19768,#19772,#798,.T.) ;
#24107 = EDGE_CURVE('',#19772,#19780,#3118,.T.) ;
#24108 = EDGE_CURVE('',#19780,#19591,#799,.T.) ;
#24109 = EDGE_CURVE('',#19779,#19781,#800,.T.) ;
#24110 = EDGE_CURVE('',#19781,#19782,#17255,.T.) ;
#24111 = EDGE_CURVE('',#19782,#19778,#801,.T.) ;
#24112 = EDGE_CURVE('',#19783,#19770,#3119,.T.) ;
#24113 = EDGE_CURVE('',#19584,#19783,#802,.T.) ;
#24114 = EDGE_CURVE('',#19769,#19765,#17256,.T.) ;
#24115 = EDGE_CURVE('',#19784,#19768,#3120,.T.) ;
#24116 = EDGE_CURVE('',#19592,#19784,#803,.T.) ;
#24117 = EDGE_CURVE('',#19780,#19785,#804,.T.) ;
#24118 = EDGE_CURVE('',#19785,#19786,#17257,.T.) ;
#24119 = EDGE_CURVE('',#19786,#19784,#805,.T.) ;
#24120 = EDGE_CURVE('',#19766,#19787,#3121,.T.) ;
#24121 = EDGE_CURVE('',#19787,#19583,#806,.T.) ;
#24122 = EDGE_CURVE('',#19787,#19788,#807,.T.) ;
#24123 = EDGE_CURVE('',#19788,#19789,#17258,.T.) ;
#24124 = EDGE_CURVE('',#19789,#19783,#808,.T.) ;
#24125 = EDGE_CURVE('',#19765,#19761,#809,.T.) ;
#24126 = EDGE_CURVE('',#19760,#19764,#810,.T.) ;
#24127 = EDGE_CURVE('',#19764,#19790,#3122,.T.) ;
#24128 = EDGE_CURVE('',#19790,#19595,#811,.T.) ;
#24129 = EDGE_CURVE('',#19791,#19762,#3123,.T.) ;
#24130 = EDGE_CURVE('',#19580,#19791,#812,.T.) ;
#24131 = EDGE_CURVE('',#19761,#19757,#17259,.T.) ;
#24132 = EDGE_CURVE('',#19792,#19760,#3124,.T.) ;
#24133 = EDGE_CURVE('',#19596,#19792,#813,.T.) ;
#24134 = EDGE_CURVE('',#19790,#19793,#814,.T.) ;
#24135 = EDGE_CURVE('',#19793,#19794,#17260,.T.) ;
#24136 = EDGE_CURVE('',#19794,#19792,#815,.T.) ;
#24137 = EDGE_CURVE('',#19758,#19795,#3125,.T.) ;
#24138 = EDGE_CURVE('',#19795,#19579,#816,.T.) ;
#24139 = EDGE_CURVE('',#19795,#19796,#817,.T.) ;
#24140 = EDGE_CURVE('',#19796,#19797,#17261,.T.) ;
#24141 = EDGE_CURVE('',#19797,#19791,#818,.T.) ;
#24142 = EDGE_CURVE('',#19757,#19753,#819,.T.) ;
#24143 = EDGE_CURVE('',#19752,#19756,#820,.T.) ;
#24144 = EDGE_CURVE('',#19756,#19798,#3126,.T.) ;
#24145 = EDGE_CURVE('',#19798,#19599,#821,.T.) ;
#24146 = EDGE_CURVE('',#19799,#19754,#3127,.T.) ;
#24147 = EDGE_CURVE('',#19576,#19799,#822,.T.) ;
#24148 = EDGE_CURVE('',#19753,#19749,#17262,.T.) ;
#24149 = EDGE_CURVE('',#19800,#19752,#3128,.T.) ;
#24150 = EDGE_CURVE('',#19600,#19800,#823,.T.) ;
#24151 = EDGE_CURVE('',#19798,#19801,#824,.T.) ;
#24152 = EDGE_CURVE('',#19801,#19802,#17263,.T.) ;
#24153 = EDGE_CURVE('',#19802,#19800,#825,.T.) ;
#24154 = EDGE_CURVE('',#19750,#19803,#3129,.T.) ;
#24155 = EDGE_CURVE('',#19803,#19575,#826,.T.) ;
#24156 = EDGE_CURVE('',#19803,#19804,#827,.T.) ;
#24157 = EDGE_CURVE('',#19804,#19805,#17264,.T.) ;
#24158 = EDGE_CURVE('',#19805,#19799,#828,.T.) ;
#24159 = EDGE_CURVE('',#19749,#19745,#829,.T.) ;
#24160 = EDGE_CURVE('',#19744,#19748,#830,.T.) ;
#24161 = EDGE_CURVE('',#19748,#19806,#3130,.T.) ;
#24162 = EDGE_CURVE('',#19806,#19603,#831,.T.) ;
#24163 = EDGE_CURVE('',#19807,#19746,#3131,.T.) ;
#24164 = EDGE_CURVE('',#19572,#19807,#832,.T.) ;
#24165 = EDGE_CURVE('',#19745,#19741,#17265,.T.) ;
#24166 = EDGE_CURVE('',#19808,#19744,#3132,.T.) ;
#24167 = EDGE_CURVE('',#19604,#19808,#833,.T.) ;
#24168 = EDGE_CURVE('',#19806,#19809,#834,.T.) ;
#24169 = EDGE_CURVE('',#19809,#19810,#17266,.T.) ;
#24170 = EDGE_CURVE('',#19810,#19808,#835,.T.) ;
#24171 = EDGE_CURVE('',#19742,#19811,#3133,.T.) ;
#24172 = EDGE_CURVE('',#19811,#19571,#836,.T.) ;
#24173 = EDGE_CURVE('',#19811,#19812,#837,.T.) ;
#24174 = EDGE_CURVE('',#19812,#19813,#17267,.T.) ;
#24175 = EDGE_CURVE('',#19813,#19807,#838,.T.) ;
#24176 = EDGE_CURVE('',#19741,#19737,#839,.T.) ;
#24177 = EDGE_CURVE('',#19736,#19740,#840,.T.) ;
#24178 = EDGE_CURVE('',#19740,#19814,#3134,.T.) ;
#24179 = EDGE_CURVE('',#19814,#19607,#841,.T.) ;
#24180 = EDGE_CURVE('',#19815,#19738,#3135,.T.) ;
#24181 = EDGE_CURVE('',#19568,#19815,#842,.T.) ;
#24182 = EDGE_CURVE('',#19737,#19733,#17268,.T.) ;
#24183 = EDGE_CURVE('',#19816,#19736,#3136,.T.) ;
#24184 = EDGE_CURVE('',#19608,#19816,#843,.T.) ;
#24185 = EDGE_CURVE('',#19814,#19817,#844,.T.) ;
#24186 = EDGE_CURVE('',#19817,#19818,#17269,.T.) ;
#24187 = EDGE_CURVE('',#19818,#19816,#845,.T.) ;
#24188 = EDGE_CURVE('',#19734,#19819,#3137,.T.) ;
#24189 = EDGE_CURVE('',#19819,#19567,#846,.T.) ;
#24190 = EDGE_CURVE('',#19819,#19820,#847,.T.) ;
#24191 = EDGE_CURVE('',#19820,#19821,#17270,.T.) ;
#24192 = EDGE_CURVE('',#19821,#19815,#848,.T.) ;
#24193 = EDGE_CURVE('',#19733,#19728,#849,.T.) ;
#24194 = EDGE_CURVE('',#19727,#19732,#850,.T.) ;
#24195 = EDGE_CURVE('',#19732,#19822,#3138,.T.) ;
#24196 = EDGE_CURVE('',#19822,#19611,#851,.T.) ;
#24197 = EDGE_CURVE('',#19823,#19729,#3139,.T.) ;
#24198 = EDGE_CURVE('',#19564,#19823,#852,.T.) ;
#24199 = EDGE_CURVE('',#19728,#19724,#17271,.T.) ;
#24200 = EDGE_CURVE('',#19824,#19727,#3140,.T.) ;
#24201 = EDGE_CURVE('',#19612,#19824,#853,.T.) ;
#24202 = EDGE_CURVE('',#19822,#19825,#854,.T.) ;
#24203 = EDGE_CURVE('',#19825,#19826,#17272,.T.) ;
#24204 = EDGE_CURVE('',#19826,#19824,#855,.T.) ;
#24205 = EDGE_CURVE('',#19725,#19827,#3141,.T.) ;
#24206 = EDGE_CURVE('',#19827,#19643,#856,.T.) ;
#24207 = EDGE_CURVE('',#19827,#19828,#857,.T.) ;
#24208 = EDGE_CURVE('',#19828,#19829,#17273,.T.) ;
#24209 = EDGE_CURVE('',#19829,#19823,#858,.T.) ;
#24210 = EDGE_CURVE('',#19724,#19720,#859,.T.) ;
#24211 = EDGE_CURVE('',#19719,#19723,#860,.T.) ;
#24212 = EDGE_CURVE('',#19723,#19830,#3142,.T.) ;
#24213 = EDGE_CURVE('',#19830,#19615,#861,.T.) ;
#24214 = EDGE_CURVE('',#19831,#19721,#3143,.T.) ;
#24215 = EDGE_CURVE('',#19640,#19831,#862,.T.) ;
#24216 = EDGE_CURVE('',#19720,#19716,#17274,.T.) ;
#24217 = EDGE_CURVE('',#19832,#19719,#3144,.T.) ;
#24218 = EDGE_CURVE('',#19616,#19832,#863,.T.) ;
#24219 = EDGE_CURVE('',#19830,#19833,#864,.T.) ;
#24220 = EDGE_CURVE('',#19833,#19834,#17275,.T.) ;
#24221 = EDGE_CURVE('',#19834,#19832,#865,.T.) ;
#24222 = EDGE_CURVE('',#19717,#19835,#3145,.T.) ;
#24223 = EDGE_CURVE('',#19835,#19639,#866,.T.) ;
#24224 = EDGE_CURVE('',#19835,#19836,#867,.T.) ;
#24225 = EDGE_CURVE('',#19836,#19837,#17276,.T.) ;
#24226 = EDGE_CURVE('',#19837,#19831,#868,.T.) ;
#24227 = EDGE_CURVE('',#19716,#19712,#869,.T.) ;
#24228 = EDGE_CURVE('',#19711,#19715,#870,.T.) ;
#24229 = EDGE_CURVE('',#19715,#19838,#3146,.T.) ;
#24230 = EDGE_CURVE('',#19838,#19619,#871,.T.) ;
#24231 = EDGE_CURVE('',#19839,#19713,#3147,.T.) ;
#24232 = EDGE_CURVE('',#19636,#19839,#872,.T.) ;
#24233 = EDGE_CURVE('',#19712,#19708,#17277,.T.) ;
#24234 = EDGE_CURVE('',#19840,#19711,#3148,.T.) ;
#24235 = EDGE_CURVE('',#19620,#19840,#873,.T.) ;
#24236 = EDGE_CURVE('',#19838,#19841,#874,.T.) ;
#24237 = EDGE_CURVE('',#19841,#19842,#17278,.T.) ;
#24238 = EDGE_CURVE('',#19842,#19840,#875,.T.) ;
#24239 = EDGE_CURVE('',#19709,#19843,#3149,.T.) ;
#24240 = EDGE_CURVE('',#19843,#19635,#876,.T.) ;
#24241 = EDGE_CURVE('',#19843,#19844,#877,.T.) ;
#24242 = EDGE_CURVE('',#19844,#19845,#17279,.T.) ;
#24243 = EDGE_CURVE('',#19845,#19839,#878,.T.) ;
#24244 = EDGE_CURVE('',#19708,#19704,#879,.T.) ;
#24245 = EDGE_CURVE('',#19703,#19707,#880,.T.) ;
#24246 = EDGE_CURVE('',#19707,#19846,#3150,.T.) ;
#24247 = EDGE_CURVE('',#19846,#19623,#881,.T.) ;
#24248 = EDGE_CURVE('',#19847,#19705,#3151,.T.) ;
#24249 = EDGE_CURVE('',#19632,#19847,#882,.T.) ;
#24250 = EDGE_CURVE('',#19704,#19700,#17280,.T.) ;
#24251 = EDGE_CURVE('',#19848,#19703,#3152,.T.) ;
#24252 = EDGE_CURVE('',#19624,#19848,#883,.T.) ;
#24253 = EDGE_CURVE('',#19846,#19849,#884,.T.) ;
#24254 = EDGE_CURVE('',#19849,#19850,#17281,.T.) ;
#24255 = EDGE_CURVE('',#19850,#19848,#885,.T.) ;
#24256 = EDGE_CURVE('',#19701,#19851,#3153,.T.) ;
#24257 = EDGE_CURVE('',#19851,#19631,#886,.T.) ;
#24258 = EDGE_CURVE('',#19851,#19852,#887,.T.) ;
#24259 = EDGE_CURVE('',#19852,#19853,#17282,.T.) ;
#24260 = EDGE_CURVE('',#19853,#19847,#888,.T.) ;
#24261 = EDGE_CURVE('',#19700,#19698,#889,.T.) ;
#24262 = EDGE_CURVE('',#19697,#19699,#890,.T.) ;
#24263 = EDGE_CURVE('',#19699,#19854,#3154,.T.) ;
#24264 = EDGE_CURVE('',#19854,#19627,#891,.T.) ;
#24265 = EDGE_CURVE('',#19855,#19697,#3155,.T.) ;
#24266 = EDGE_CURVE('',#19628,#19855,#892,.T.) ;
#24267 = EDGE_CURVE('',#19854,#19856,#893,.T.) ;
#24268 = EDGE_CURVE('',#19856,#19857,#17283,.T.) ;
#24269 = EDGE_CURVE('',#19857,#19855,#894,.T.) ;
#24270 = EDGE_CURVE('',#19852,#19853,#17284,.T.) ;
#24271 = EDGE_CURVE('',#19844,#19845,#17285,.T.) ;
#24272 = EDGE_CURVE('',#19836,#19837,#17286,.T.) ;
#24273 = EDGE_CURVE('',#19828,#19829,#17287,.T.) ;
#24274 = EDGE_CURVE('',#19820,#19821,#17288,.T.) ;
#24275 = EDGE_CURVE('',#19812,#19813,#17289,.T.) ;
#24276 = EDGE_CURVE('',#19804,#19805,#17290,.T.) ;
#24277 = EDGE_CURVE('',#19796,#19797,#17291,.T.) ;
#24278 = EDGE_CURVE('',#19788,#19789,#17292,.T.) ;
#24279 = EDGE_CURVE('',#19781,#19782,#17293,.T.) ;
#24280 = EDGE_CURVE('',#19785,#19786,#17294,.T.) ;
#24281 = EDGE_CURVE('',#19793,#19794,#17295,.T.) ;
#24282 = EDGE_CURVE('',#19801,#19802,#17296,.T.) ;
#24283 = EDGE_CURVE('',#19809,#19810,#17297,.T.) ;
#24284 = EDGE_CURVE('',#19817,#19818,#17298,.T.) ;
#24285 = EDGE_CURVE('',#19825,#19826,#17299,.T.) ;
#24286 = EDGE_CURVE('',#19833,#19834,#17300,.T.) ;
#24287 = EDGE_CURVE('',#19841,#19842,#17301,.T.) ;
#24288 = EDGE_CURVE('',#19849,#19850,#17302,.T.) ;
#24289 = EDGE_CURVE('',#19856,#19857,#17303,.T.) ;
#24290 = EDGE_CURVE('',#19731,#19858,#3156,.T.) ;
#24291 = EDGE_CURVE('',#19858,#19858,#17304,.T.) ;
#24292 = EDGE_CURVE('',#19696,#19859,#17305,.T.) ;
#24293 = EDGE_CURVE('',#19859,#19860,#17306,.T.) ;
#24294 = EDGE_CURVE('',#19860,#19695,#17307,.T.) ;
#24295 = EDGE_CURVE('',#19861,#19861,#17308,.T.) ;
#24296 = EDGE_CURVE('',#19862,#19859,#3157,.T.) ;
#24297 = EDGE_CURVE('',#19863,#19862,#17309,.T.) ;
#24298 = EDGE_CURVE('',#19864,#19863,#3158,.T.) ;
#24299 = EDGE_CURVE('',#19865,#19864,#17310,.T.) ;
#24300 = EDGE_CURVE('',#19866,#19865,#3159,.T.) ;
#24301 = EDGE_CURVE('',#19867,#19866,#17311,.T.) ;
#24302 = EDGE_CURVE('',#19868,#19867,#3160,.T.) ;
#24303 = EDGE_CURVE('',#19869,#19868,#17312,.T.) ;
#24304 = EDGE_CURVE('',#19870,#19869,#3161,.T.) ;
#24305 = EDGE_CURVE('',#19871,#19870,#17313,.T.) ;
#24306 = EDGE_CURVE('',#19872,#19871,#3162,.T.) ;
#24307 = EDGE_CURVE('',#19873,#19872,#17314,.T.) ;
#24308 = EDGE_CURVE('',#19874,#19873,#3163,.T.) ;
#24309 = EDGE_CURVE('',#19875,#19874,#17315,.T.) ;
#24310 = EDGE_CURVE('',#19876,#19875,#3164,.T.) ;
#24311 = EDGE_CURVE('',#19877,#19876,#17316,.T.) ;
#24312 = EDGE_CURVE('',#19878,#19877,#3165,.T.) ;
#24313 = EDGE_CURVE('',#19879,#19878,#17317,.T.) ;
#24314 = EDGE_CURVE('',#19880,#19879,#3166,.T.) ;
#24315 = EDGE_CURVE('',#19881,#19880,#17318,.T.) ;
#24316 = EDGE_CURVE('',#19882,#19881,#3167,.T.) ;
#24317 = EDGE_CURVE('',#19883,#19882,#17319,.T.) ;
#24318 = EDGE_CURVE('',#19860,#19883,#3168,.T.) ;
#24319 = EDGE_CURVE('',#19696,#19884,#3169,.T.) ;
#24320 = EDGE_CURVE('',#19884,#19862,#17320,.T.) ;
#24321 = EDGE_CURVE('',#19884,#19682,#3170,.T.) ;
#24322 = EDGE_CURVE('',#19690,#19879,#17321,.T.) ;
#24323 = EDGE_CURVE('',#19878,#19689,#17322,.T.) ;
#24324 = EDGE_CURVE('',#19691,#19880,#17323,.T.) ;
#24325 = EDGE_CURVE('',#19885,#19867,#17324,.T.) ;
#24326 = EDGE_CURVE('',#19866,#19886,#17325,.T.) ;
#24327 = EDGE_CURVE('',#19886,#19885,#17326,.T.) ;
#24328 = EDGE_CURVE('',#19673,#19885,#3171,.T.) ;
#24329 = EDGE_CURVE('',#19886,#19671,#3172,.T.) ;
#24330 = EDGE_CURVE('',#19885,#19887,#3173,.T.) ;
#24331 = EDGE_CURVE('',#19887,#19868,#17327,.T.) ;
#24332 = EDGE_CURVE('',#19887,#19674,#3174,.T.) ;
#24333 = EDGE_CURVE('',#19685,#19873,#17328,.T.) ;
#24334 = EDGE_CURVE('',#19872,#19888,#17329,.T.) ;
#24335 = EDGE_CURVE('',#19888,#19685,#17330,.T.) ;
#24336 = EDGE_CURVE('',#19888,#19661,#3175,.T.) ;
#24337 = EDGE_CURVE('',#19684,#19874,#17331,.T.) ;
#24338 = EDGE_CURVE('',#19858,#19861,#17332,.T.) ;
#24339 = EDGE_CURVE('',#19881,#19692,#17333,.T.) ;
#24340 = EDGE_CURVE('',#19693,#19882,#17334,.T.) ;
#24341 = EDGE_CURVE('',#19883,#19694,#17335,.T.) ;
#24342 = EDGE_CURVE('',#19877,#19688,#17336,.T.) ;
#24343 = EDGE_CURVE('',#19687,#19876,#17337,.T.) ;
#24344 = EDGE_CURVE('',#19875,#19686,#17338,.T.) ;
#24345 = EDGE_CURVE('',#19889,#19884,#17339,.F.) ;
#24346 = EDGE_CURVE('',#19863,#19889,#17340,.T.) ;
#24347 = EDGE_CURVE('',#19675,#19889,#3176,.T.) ;
#24348 = EDGE_CURVE('',#19890,#19864,#17341,.T.) ;
#24349 = EDGE_CURVE('',#19891,#19890,#17342,.F.) ;
#24350 = EDGE_CURVE('',#19865,#19891,#17343,.T.) ;
#24351 = EDGE_CURVE('',#19889,#19890,#3177,.T.) ;
#24352 = EDGE_CURVE('',#19668,#19891,#3178,.T.) ;
#24353 = EDGE_CURVE('',#19890,#19677,#3179,.T.) ;
#24354 = EDGE_CURVE('',#19892,#19870,#17344,.T.) ;
#24355 = EDGE_CURVE('',#19893,#19892,#17345,.F.) ;
#24356 = EDGE_CURVE('',#19871,#19893,#17346,.T.) ;
#24357 = EDGE_CURVE('',#19891,#19886,#3180,.T.) ;
#24358 = EDGE_CURVE('',#19894,#19887,#17347,.F.) ;
#24359 = EDGE_CURVE('',#19869,#19894,#17348,.T.) ;
#24360 = EDGE_CURVE('',#19665,#19894,#3181,.T.) ;
#24361 = EDGE_CURVE('',#19894,#19892,#3182,.T.) ;
#24362 = EDGE_CURVE('',#19658,#19893,#3183,.T.) ;
#24363 = EDGE_CURVE('',#19892,#19667,#3184,.T.) ;
#24364 = EDGE_CURVE('',#19893,#19888,#3185,.T.) ;
#24365 = EDGE_CURVE('',#19895,#19896,#17349,.T.) ;
#24366 = EDGE_CURVE('',#19896,#19897,#895,.T.) ;
#24367 = EDGE_CURVE('',#19897,#19898,#896,.T.) ;
#24368 = EDGE_CURVE('',#19898,#19895,#897,.T.) ;
#24369 = EDGE_CURVE('',#19899,#19900,#17350,.T.) ;
#24370 = EDGE_CURVE('',#19900,#19901,#17351,.T.) ;
#24371 = EDGE_CURVE('',#19901,#19902,#17352,.T.) ;
#24372 = EDGE_CURVE('',#19902,#19899,#17353,.T.) ;
#24373 = EDGE_CURVE('',#19903,#19904,#17354,.T.) ;
#24374 = EDGE_CURVE('',#19904,#19900,#3186,.T.) ;
#24375 = EDGE_CURVE('',#19899,#19903,#3187,.T.) ;
#24376 = EDGE_CURVE('',#19905,#19906,#898,.T.) ;
#24377 = EDGE_CURVE('',#19906,#19904,#899,.T.) ;
#24378 = EDGE_CURVE('',#19903,#19905,#900,.T.) ;
#24379 = EDGE_CURVE('',#19901,#19896,#901,.T.) ;
#24380 = EDGE_CURVE('',#19895,#19902,#902,.T.) ;
#24381 = EDGE_CURVE('',#19907,#19899,#3188,.T.) ;
#24382 = EDGE_CURVE('',#19908,#19907,#3189,.T.) ;
#24383 = EDGE_CURVE('',#19903,#19908,#3190,.T.) ;
#24384 = EDGE_CURVE('',#19898,#19909,#3191,.T.) ;
#24385 = EDGE_CURVE('',#19907,#19909,#903,.T.) ;
#24386 = EDGE_CURVE('',#19910,#19896,#17355,.T.) ;
#24387 = EDGE_CURVE('',#19910,#19898,#103,.T.) ;
#24388 = EDGE_CURVE('',#19901,#19911,#104,.T.) ;
#24389 = EDGE_CURVE('',#19912,#19911,#17356,.T.) ;
#24390 = EDGE_CURVE('',#19912,#19910,#105,.T.) ;
#24391 = EDGE_CURVE('',#19913,#19914,#17357,.T.) ;
#24392 = EDGE_CURVE('',#19914,#19915,#904,.T.) ;
#24393 = EDGE_CURVE('',#19915,#19916,#17358,.T.) ;
#24394 = EDGE_CURVE('',#19916,#19913,#905,.T.) ;
#24395 = EDGE_CURVE('',#19913,#19917,#906,.T.) ;
#24396 = EDGE_CURVE('',#19917,#19918,#17359,.T.) ;
#24397 = EDGE_CURVE('',#19918,#19914,#907,.T.) ;
#24398 = EDGE_CURVE('',#19919,#19920,#17360,.T.) ;
#24399 = EDGE_CURVE('',#19920,#19918,#3192,.T.) ;
#24400 = EDGE_CURVE('',#19917,#19919,#3193,.T.) ;
#24401 = EDGE_CURVE('',#19919,#19921,#106,.T.) ;
#24402 = EDGE_CURVE('',#19921,#19922,#17361,.T.) ;
#24403 = EDGE_CURVE('',#19922,#19920,#107,.T.) ;
#24404 = EDGE_CURVE('',#19923,#19924,#17362,.T.) ;
#24405 = EDGE_CURVE('',#19924,#19922,#908,.T.) ;
#24406 = EDGE_CURVE('',#19921,#19923,#909,.T.) ;
#24407 = EDGE_CURVE('',#19923,#19925,#910,.T.) ;
#24408 = EDGE_CURVE('',#19925,#19926,#17363,.T.) ;
#24409 = EDGE_CURVE('',#19926,#19924,#911,.T.) ;
#24410 = EDGE_CURVE('',#19927,#19928,#17364,.T.) ;
#24411 = EDGE_CURVE('',#19928,#19926,#3194,.T.) ;
#24412 = EDGE_CURVE('',#19925,#19927,#3195,.T.) ;
#24413 = EDGE_CURVE('',#19927,#19916,#108,.T.) ;
#24414 = EDGE_CURVE('',#19915,#19928,#109,.T.) ;
#24415 = EDGE_CURVE('',#19919,#19929,#3196,.T.) ;
#24416 = EDGE_CURVE('',#19930,#19929,#110,.T.) ;
#24417 = EDGE_CURVE('',#19930,#19921,#3197,.T.) ;
#24418 = EDGE_CURVE('',#19931,#19917,#3198,.T.) ;
#24419 = EDGE_CURVE('',#19929,#19931,#3199,.T.) ;
#24420 = EDGE_CURVE('',#19913,#19932,#3200,.T.) ;
#24421 = EDGE_CURVE('',#19931,#19932,#912,.T.) ;
#24422 = EDGE_CURVE('',#19933,#19916,#3201,.T.) ;
#24423 = EDGE_CURVE('',#19932,#19933,#913,.T.) ;
#24424 = EDGE_CURVE('',#19934,#19935,#3202,.T.) ;
#24425 = EDGE_CURVE('',#19936,#19934,#17365,.T.) ;
#24426 = EDGE_CURVE('',#19937,#19936,#3203,.T.) ;
#24427 = EDGE_CURVE('',#19938,#19937,#3204,.T.) ;
#24428 = EDGE_CURVE('',#19939,#19938,#17366,.T.) ;
#24429 = EDGE_CURVE('',#19940,#19939,#111,.T.) ;
#24430 = EDGE_CURVE('',#19941,#19940,#112,.T.) ;
#24431 = EDGE_CURVE('',#19942,#19941,#113,.T.) ;
#24432 = EDGE_CURVE('',#19943,#19942,#17367,.T.) ;
#24433 = EDGE_CURVE('',#19944,#19943,#914,.T.) ;
#24434 = EDGE_CURVE('',#19945,#19944,#114,.T.) ;
#24435 = EDGE_CURVE('',#19946,#19945,#3205,.T.) ;
#24436 = EDGE_CURVE('',#19947,#19946,#915,.T.) ;
#24437 = EDGE_CURVE('',#19948,#19947,#916,.T.) ;
#24438 = EDGE_CURVE('',#19949,#19948,#917,.T.) ;
#24439 = EDGE_CURVE('',#19950,#19949,#115,.T.) ;
#24440 = EDGE_CURVE('',#19951,#19950,#116,.T.) ;
#24441 = EDGE_CURVE('',#19952,#19951,#17368,.T.) ;
#24442 = EDGE_CURVE('',#19953,#19952,#3206,.T.) ;
#24443 = EDGE_CURVE('',#19935,#19953,#17369,.T.) ;
#24444 = EDGE_CURVE('',#19954,#19955,#3207,.T.) ;
#24445 = EDGE_CURVE('',#19956,#19954,#117,.T.) ;
#24446 = EDGE_CURVE('',#19957,#19956,#118,.T.) ;
#24447 = EDGE_CURVE('',#19958,#19957,#918,.T.) ;
#24448 = EDGE_CURVE('',#19959,#19958,#3208,.T.) ;
#24449 = EDGE_CURVE('',#19960,#19959,#919,.T.) ;
#24450 = EDGE_CURVE('',#19961,#19960,#119,.T.) ;
#24451 = EDGE_CURVE('',#19955,#19961,#920,.T.) ;
#24452 = EDGE_CURVE('',#19962,#19963,#921,.T.) ;
#24453 = EDGE_CURVE('',#19964,#19962,#120,.T.) ;
#24454 = EDGE_CURVE('',#19965,#19964,#121,.T.) ;
#24455 = EDGE_CURVE('',#19966,#19965,#922,.T.) ;
#24456 = EDGE_CURVE('',#19967,#19966,#3209,.T.) ;
#24457 = EDGE_CURVE('',#19968,#19967,#923,.T.) ;
#24458 = EDGE_CURVE('',#19969,#19968,#122,.T.) ;
#24459 = EDGE_CURVE('',#19970,#19969,#17370,.T.) ;
#24460 = EDGE_CURVE('',#19971,#19970,#3210,.T.) ;
#24461 = EDGE_CURVE('',#19972,#19971,#17371,.T.) ;
#24462 = EDGE_CURVE('',#19963,#19972,#3211,.T.) ;
#24463 = EDGE_CURVE('',#19973,#19973,#17372,.T.) ;
#24464 = EDGE_CURVE('',#19955,#19974,#17373,.T.) ;
#24465 = EDGE_CURVE('',#19974,#19975,#3212,.T.) ;
#24466 = EDGE_CURVE('',#19975,#19954,#17374,.T.) ;
#24467 = EDGE_CURVE('',#19975,#19976,#123,.T.) ;
#24468 = EDGE_CURVE('',#19976,#19956,#17375,.T.) ;
#24469 = EDGE_CURVE('',#19977,#19957,#17376,.T.) ;
#24470 = EDGE_CURVE('',#19976,#19977,#924,.T.) ;
#24471 = EDGE_CURVE('',#19977,#19978,#925,.T.) ;
#24472 = EDGE_CURVE('',#19978,#19958,#17377,.T.) ;
#24473 = EDGE_CURVE('',#19979,#19959,#17378,.T.) ;
#24474 = EDGE_CURVE('',#19978,#19979,#3213,.T.) ;
#24475 = EDGE_CURVE('',#19979,#19980,#926,.T.) ;
#24476 = EDGE_CURVE('',#19980,#19960,#17379,.T.) ;
#24477 = EDGE_CURVE('',#19981,#19961,#17380,.T.) ;
#24478 = EDGE_CURVE('',#19980,#19981,#927,.T.) ;
#24479 = EDGE_CURVE('',#19981,#19974,#928,.T.) ;
#24480 = EDGE_CURVE('',#19977,#19982,#3214,.T.) ;
#24481 = EDGE_CURVE('',#19983,#19982,#929,.T.) ;
#24482 = EDGE_CURVE('',#19983,#19978,#3215,.T.) ;
#24483 = EDGE_CURVE('',#19984,#19976,#3216,.T.) ;
#24484 = EDGE_CURVE('',#19982,#19984,#930,.T.) ;
#24485 = EDGE_CURVE('',#19975,#19985,#3217,.T.) ;
#24486 = EDGE_CURVE('',#19984,#19985,#124,.T.) ;
#24487 = EDGE_CURVE('',#19986,#19974,#3218,.T.) ;
#24488 = EDGE_CURVE('',#19985,#19986,#3219,.T.) ;
#24489 = EDGE_CURVE('',#19973,#19987,#17381,.T.) ;
#24490 = EDGE_CURVE('',#19987,#19987,#17382,.T.) ;
#24491 = EDGE_CURVE('',#19988,#19988,#17383,.T.) ;
#24492 = EDGE_CURVE('',#19988,#19987,#3220,.T.) ;
#24493 = EDGE_CURVE('',#19935,#19989,#125,.T.) ;
#24494 = EDGE_CURVE('',#19989,#19990,#3221,.T.) ;
#24495 = EDGE_CURVE('',#19934,#19990,#126,.T.) ;
#24496 = EDGE_CURVE('',#19953,#19991,#931,.T.) ;
#24497 = EDGE_CURVE('',#19991,#19989,#17384,.T.) ;
#24498 = EDGE_CURVE('',#19952,#19992,#932,.T.) ;
#24499 = EDGE_CURVE('',#19992,#19991,#3222,.T.) ;
#24500 = EDGE_CURVE('',#19951,#19993,#17385,.T.) ;
#24501 = EDGE_CURVE('',#19993,#19992,#17386,.T.) ;
#24502 = EDGE_CURVE('',#19950,#19994,#17387,.T.) ;
#24503 = EDGE_CURVE('',#19994,#19993,#127,.T.) ;
#24504 = EDGE_CURVE('',#19949,#19995,#17388,.T.) ;
#24505 = EDGE_CURVE('',#19995,#19994,#128,.T.) ;
#24506 = EDGE_CURVE('',#19948,#19996,#17389,.T.) ;
#24507 = EDGE_CURVE('',#19996,#19995,#933,.T.) ;
#24508 = EDGE_CURVE('',#19947,#19997,#17390,.T.) ;
#24509 = EDGE_CURVE('',#19997,#19996,#934,.T.) ;
#24510 = EDGE_CURVE('',#19946,#19998,#17391,.T.) ;
#24511 = EDGE_CURVE('',#19998,#19997,#935,.T.) ;
#24512 = EDGE_CURVE('',#19945,#19999,#17392,.T.) ;
#24513 = EDGE_CURVE('',#19999,#19998,#3223,.T.) ;
#24514 = EDGE_CURVE('',#19944,#20000,#17393,.T.) ;
#24515 = EDGE_CURVE('',#20000,#19999,#129,.T.) ;
#24516 = EDGE_CURVE('',#19943,#20001,#17394,.T.) ;
#24517 = EDGE_CURVE('',#20001,#20000,#936,.T.) ;
#24518 = EDGE_CURVE('',#19942,#20002,#17395,.T.) ;
#24519 = EDGE_CURVE('',#20002,#20001,#17396,.T.) ;
#24520 = EDGE_CURVE('',#19941,#20003,#17397,.T.) ;
#24521 = EDGE_CURVE('',#20003,#20002,#130,.T.) ;
#24522 = EDGE_CURVE('',#19940,#20004,#17398,.T.) ;
#24523 = EDGE_CURVE('',#20004,#20003,#131,.T.) ;
#24524 = EDGE_CURVE('',#19939,#20005,#17399,.T.) ;
#24525 = EDGE_CURVE('',#20005,#20004,#132,.T.) ;
#24526 = EDGE_CURVE('',#19938,#20006,#17400,.T.) ;
#24527 = EDGE_CURVE('',#20006,#20005,#17401,.T.) ;
#24528 = EDGE_CURVE('',#20007,#20006,#3224,.T.) ;
#24529 = EDGE_CURVE('',#19937,#20007,#133,.T.) ;
#24530 = EDGE_CURVE('',#20008,#20007,#3225,.T.) ;
#24531 = EDGE_CURVE('',#19936,#20008,#937,.T.) ;
#24532 = EDGE_CURVE('',#19990,#20008,#17402,.T.) ;
#24533 = EDGE_CURVE('',#20001,#20009,#3226,.T.) ;
#24534 = EDGE_CURVE('',#20010,#20009,#938,.T.) ;
#24535 = EDGE_CURVE('',#20000,#20010,#3227,.T.) ;
#24536 = EDGE_CURVE('',#20011,#20002,#3228,.T.) ;
#24537 = EDGE_CURVE('',#20009,#20011,#17403,.T.) ;
#24538 = EDGE_CURVE('',#20012,#20003,#3229,.T.) ;
#24539 = EDGE_CURVE('',#20011,#20012,#134,.T.) ;
#24540 = EDGE_CURVE('',#20013,#20004,#3230,.T.) ;
#24541 = EDGE_CURVE('',#20014,#20013,#135,.T.) ;
#24542 = EDGE_CURVE('',#19905,#20014,#3231,.T.) ;
#24543 = EDGE_CURVE('',#20015,#19905,#3232,.T.) ;
#24544 = EDGE_CURVE('',#20012,#20015,#136,.T.) ;
#24545 = EDGE_CURVE('',#20016,#20005,#3233,.T.) ;
#24546 = EDGE_CURVE('',#20016,#19906,#137,.T.) ;
#24547 = EDGE_CURVE('',#20006,#20017,#3234,.T.) ;
#24548 = EDGE_CURVE('',#20017,#20016,#939,.T.) ;
#24549 = EDGE_CURVE('',#20018,#20007,#3235,.T.) ;
#24550 = EDGE_CURVE('',#20018,#20017,#3236,.T.) ;
#24551 = EDGE_CURVE('',#20019,#20008,#3237,.T.) ;
#24552 = EDGE_CURVE('',#20019,#20018,#3238,.T.) ;
#24553 = EDGE_CURVE('',#20020,#19990,#3239,.T.) ;
#24554 = EDGE_CURVE('',#20020,#20019,#17404,.T.) ;
#24555 = EDGE_CURVE('',#20021,#19989,#3240,.T.) ;
#24556 = EDGE_CURVE('',#20021,#20020,#3241,.T.) ;
#24557 = EDGE_CURVE('',#19971,#20022,#940,.T.) ;
#24558 = EDGE_CURVE('',#20022,#20023,#17405,.T.) ;
#24559 = EDGE_CURVE('',#19972,#20023,#941,.T.) ;
#24560 = EDGE_CURVE('',#20024,#19967,#17406,.T.) ;
#24561 = EDGE_CURVE('',#20025,#20024,#942,.F.) ;
#24562 = EDGE_CURVE('',#19968,#20025,#17407,.T.) ;
#24563 = EDGE_CURVE('',#20026,#20027,#17408,.F.) ;
#24564 = EDGE_CURVE('',#20028,#20026,#17409,.F.) ;
#24565 = EDGE_CURVE('',#20027,#20028,#17410,.F.) ;
#24566 = EDGE_CURVE('',#20024,#20028,#3242,.T.) ;
#24567 = EDGE_CURVE('',#20026,#20025,#3243,.T.) ;
#24568 = EDGE_CURVE('',#20029,#19965,#17411,.T.) ;
#24569 = EDGE_CURVE('',#20030,#20029,#943,.F.) ;
#24570 = EDGE_CURVE('',#19966,#20030,#17412,.T.) ;
#24571 = EDGE_CURVE('',#20031,#20032,#17413,.F.) ;
#24572 = EDGE_CURVE('',#20033,#20031,#17414,.F.) ;
#24573 = EDGE_CURVE('',#20034,#20033,#17415,.F.) ;
#24574 = EDGE_CURVE('',#20032,#20034,#17416,.F.) ;
#24575 = EDGE_CURVE('',#20029,#20034,#3244,.T.) ;
#24576 = EDGE_CURVE('',#20031,#20030,#3245,.T.) ;
#24577 = EDGE_CURVE('',#20035,#20036,#17417,.T.) ;
#24578 = EDGE_CURVE('',#20036,#20037,#138,.T.) ;
#24579 = EDGE_CURVE('',#20037,#20038,#17418,.T.) ;
#24580 = EDGE_CURVE('',#20038,#20035,#139,.T.) ;
#24581 = EDGE_CURVE('',#20034,#20038,#140,.T.) ;
#24582 = EDGE_CURVE('',#20037,#20032,#141,.T.) ;
#24583 = EDGE_CURVE('',#20028,#20031,#3246,.T.) ;
#24584 = EDGE_CURVE('',#20032,#20027,#3247,.T.) ;
#24585 = EDGE_CURVE('',#20030,#20024,#3248,.T.) ;
#24586 = EDGE_CURVE('',#20039,#20040,#142,.T.) ;
#24587 = EDGE_CURVE('',#20040,#19962,#17419,.T.) ;
#24588 = EDGE_CURVE('',#19963,#20039,#944,.T.) ;
#24589 = EDGE_CURVE('',#20041,#19964,#17420,.T.) ;
#24590 = EDGE_CURVE('',#20040,#20041,#143,.T.) ;
#24591 = EDGE_CURVE('',#20041,#20029,#144,.T.) ;
#24592 = EDGE_CURVE('',#20027,#20042,#145,.T.) ;
#24593 = EDGE_CURVE('',#20042,#20043,#17421,.T.) ;
#24594 = EDGE_CURVE('',#20043,#20026,#146,.T.) ;
#24595 = EDGE_CURVE('',#20044,#20045,#17422,.T.) ;
#24596 = EDGE_CURVE('',#20045,#20043,#17423,.T.) ;
#24597 = EDGE_CURVE('',#20042,#20044,#17424,.T.) ;
#24598 = EDGE_CURVE('',#20046,#20047,#945,.T.) ;
#24599 = EDGE_CURVE('',#20046,#20045,#3249,.T.) ;
#24600 = EDGE_CURVE('',#20044,#20047,#3250,.T.) ;
#24601 = EDGE_CURVE('',#20023,#20039,#3251,.T.) ;
#24602 = EDGE_CURVE('',#20025,#20048,#147,.T.) ;
#24603 = EDGE_CURVE('',#20048,#19969,#17425,.T.) ;
#24604 = EDGE_CURVE('',#20048,#20049,#17426,.T.) ;
#24605 = EDGE_CURVE('',#20049,#19970,#17427,.T.) ;
#24606 = EDGE_CURVE('',#20049,#20022,#3252,.T.) ;
#24607 = EDGE_CURVE('',#20035,#20050,#946,.T.) ;
#24608 = EDGE_CURVE('',#20050,#20036,#148,.T.) ;
#24609 = EDGE_CURVE('',#20050,#20051,#3253,.T.) ;
#24610 = EDGE_CURVE('',#20052,#20051,#3254,.T.) ;
#24611 = EDGE_CURVE('',#20047,#20052,#17428,.T.) ;
#24612 = EDGE_CURVE('',#20038,#20041,#3255,.T.) ;
#24613 = EDGE_CURVE('',#20035,#20040,#3256,.T.) ;
#24614 = EDGE_CURVE('',#20053,#20039,#3257,.T.) ;
#24615 = EDGE_CURVE('',#20053,#20054,#149,.T.) ;
#24616 = EDGE_CURVE('',#20054,#20035,#3258,.T.) ;
#24617 = EDGE_CURVE('',#19982,#20055,#17429,.T.) ;
#24618 = EDGE_CURVE('',#20055,#20056,#947,.T.) ;
#24619 = EDGE_CURVE('',#20056,#19983,#17430,.T.) ;
#24620 = EDGE_CURVE('',#19984,#20057,#17431,.T.) ;
#24621 = EDGE_CURVE('',#20057,#20055,#150,.T.) ;
#24622 = EDGE_CURVE('',#19985,#20058,#17432,.T.) ;
#24623 = EDGE_CURVE('',#20058,#20057,#151,.T.) ;
#24624 = EDGE_CURVE('',#19986,#20059,#17433,.T.) ;
#24625 = EDGE_CURVE('',#20059,#20058,#3259,.T.) ;
#24626 = EDGE_CURVE('',#20060,#20061,#17434,.T.) ;
#24627 = EDGE_CURVE('',#20061,#20059,#948,.T.) ;
#24628 = EDGE_CURVE('',#19986,#20060,#949,.T.) ;
#24629 = EDGE_CURVE('',#20060,#20062,#152,.T.) ;
#24630 = EDGE_CURVE('',#20062,#20063,#17435,.T.) ;
#24631 = EDGE_CURVE('',#20063,#20061,#950,.T.) ;
#24632 = EDGE_CURVE('',#20064,#20065,#17436,.T.) ;
#24633 = EDGE_CURVE('',#20065,#20063,#951,.T.) ;
#24634 = EDGE_CURVE('',#20062,#20064,#952,.T.) ;
#24635 = EDGE_CURVE('',#20064,#19983,#3260,.T.) ;
#24636 = EDGE_CURVE('',#20056,#20065,#3261,.T.) ;
#24637 = EDGE_CURVE('',#20066,#20067,#17437,.T.) ;
#24638 = EDGE_CURVE('',#20067,#20068,#953,.T.) ;
#24639 = EDGE_CURVE('',#20068,#20069,#17438,.T.) ;
#24640 = EDGE_CURVE('',#20069,#20066,#954,.T.) ;
#24641 = EDGE_CURVE('',#20066,#19930,#955,.T.) ;
#24642 = EDGE_CURVE('',#19930,#20070,#17439,.T.) ;
#24643 = EDGE_CURVE('',#20070,#20067,#956,.T.) ;
#24644 = EDGE_CURVE('',#19929,#20071,#17440,.T.) ;
#24645 = EDGE_CURVE('',#20071,#20070,#153,.T.) ;
#24646 = EDGE_CURVE('',#19931,#20072,#17441,.T.) ;
#24647 = EDGE_CURVE('',#20072,#20071,#3262,.T.) ;
#24648 = EDGE_CURVE('',#19932,#20073,#17442,.T.) ;
#24649 = EDGE_CURVE('',#20073,#20072,#957,.T.) ;
#24650 = EDGE_CURVE('',#19933,#20074,#17443,.T.) ;
#24651 = EDGE_CURVE('',#20074,#20073,#958,.T.) ;
#24652 = EDGE_CURVE('',#20075,#20076,#17444,.T.) ;
#24653 = EDGE_CURVE('',#20076,#20074,#154,.T.) ;
#24654 = EDGE_CURVE('',#19933,#20075,#155,.T.) ;
#24655 = EDGE_CURVE('',#20075,#20069,#3263,.T.) ;
#24656 = EDGE_CURVE('',#20068,#20076,#3264,.T.) ;
#24657 = EDGE_CURVE('',#19923,#20066,#3265,.T.) ;
#24658 = EDGE_CURVE('',#20069,#19925,#3266,.T.) ;
#24659 = EDGE_CURVE('',#20077,#20078,#17445,.F.) ;
#24660 = EDGE_CURVE('',#20079,#20077,#17446,.F.) ;
#24661 = EDGE_CURVE('',#20078,#20079,#17447,.F.) ;
#24662 = EDGE_CURVE('',#20080,#20081,#17448,.T.) ;
#24663 = EDGE_CURVE('',#20082,#20080,#156,.F.) ;
#24664 = EDGE_CURVE('',#20083,#20082,#17449,.T.) ;
#24665 = EDGE_CURVE('',#20083,#20081,#959,.T.) ;
#24666 = EDGE_CURVE('',#20080,#20079,#3267,.T.) ;
#24667 = EDGE_CURVE('',#20077,#20082,#3268,.T.) ;
#24668 = EDGE_CURVE('',#20084,#20085,#17450,.F.) ;
#24669 = EDGE_CURVE('',#20086,#20084,#17451,.F.) ;
#24670 = EDGE_CURVE('',#20087,#20086,#17452,.F.) ;
#24671 = EDGE_CURVE('',#20088,#20087,#17453,.F.) ;
#24672 = EDGE_CURVE('',#20085,#20088,#17454,.F.) ;
#24673 = EDGE_CURVE('',#20084,#20077,#3269,.T.) ;
#24674 = EDGE_CURVE('',#20078,#20086,#3270,.T.) ;
#24675 = EDGE_CURVE('',#20086,#20089,#960,.T.) ;
#24676 = EDGE_CURVE('',#20089,#20090,#17455,.T.) ;
#24677 = EDGE_CURVE('',#20090,#20087,#961,.T.) ;
#24678 = EDGE_CURVE('',#20089,#20091,#157,.T.) ;
#24679 = EDGE_CURVE('',#20091,#20092,#17456,.T.) ;
#24680 = EDGE_CURVE('',#20092,#20090,#158,.T.) ;
#24681 = EDGE_CURVE('',#20093,#20094,#17457,.T.) ;
#24682 = EDGE_CURVE('',#20094,#20092,#3271,.T.) ;
#24683 = EDGE_CURVE('',#20091,#20093,#3272,.T.) ;
#24684 = EDGE_CURVE('',#20093,#20095,#962,.T.) ;
#24685 = EDGE_CURVE('',#20095,#20096,#17458,.T.) ;
#24686 = EDGE_CURVE('',#20096,#20094,#963,.T.) ;
#24687 = EDGE_CURVE('',#20079,#20096,#964,.T.) ;
#24688 = EDGE_CURVE('',#20095,#20078,#965,.T.) ;
#24689 = EDGE_CURVE('',#20097,#20098,#159,.T.) ;
#24690 = EDGE_CURVE('',#20098,#20099,#966,.T.) ;
#24691 = EDGE_CURVE('',#20100,#20099,#17459,.T.) ;
#24692 = EDGE_CURVE('',#20101,#20100,#967,.F.) ;
#24693 = EDGE_CURVE('',#20102,#20101,#17460,.T.) ;
#24694 = EDGE_CURVE('',#20102,#20097,#968,.T.) ;
#24695 = EDGE_CURVE('',#20087,#20101,#3273,.T.) ;
#24696 = EDGE_CURVE('',#20100,#20084,#3274,.T.) ;
#24697 = EDGE_CURVE('',#20101,#20103,#969,.T.) ;
#24698 = EDGE_CURVE('',#20103,#20104,#17461,.T.) ;
#24699 = EDGE_CURVE('',#20104,#20102,#970,.T.) ;
#24700 = EDGE_CURVE('',#20103,#20105,#160,.T.) ;
#24701 = EDGE_CURVE('',#20105,#20106,#17462,.T.) ;
#24702 = EDGE_CURVE('',#20106,#20104,#161,.T.) ;
#24703 = EDGE_CURVE('',#20107,#20108,#17463,.T.) ;
#24704 = EDGE_CURVE('',#20108,#20106,#3275,.T.) ;
#24705 = EDGE_CURVE('',#20105,#20107,#3276,.T.) ;
#24706 = EDGE_CURVE('',#20107,#20109,#971,.T.) ;
#24707 = EDGE_CURVE('',#20109,#20110,#17464,.T.) ;
#24708 = EDGE_CURVE('',#20110,#20108,#972,.T.) ;
#24709 = EDGE_CURVE('',#20081,#20110,#973,.T.) ;
#24710 = EDGE_CURVE('',#20109,#20080,#974,.T.) ;
#24711 = EDGE_CURVE('',#20099,#20083,#3277,.T.) ;
#24712 = EDGE_CURVE('',#20082,#20100,#3278,.T.) ;
#24713 = EDGE_CURVE('',#20107,#20094,#3279,.T.) ;
#24714 = EDGE_CURVE('',#20096,#20109,#3280,.T.) ;
#24715 = EDGE_CURVE('',#20103,#20090,#3281,.T.) ;
#24716 = EDGE_CURVE('',#20092,#20105,#3282,.T.) ;
#24717 = EDGE_CURVE('',#20111,#20112,#162,.T.) ;
#24718 = EDGE_CURVE('',#20113,#20111,#3283,.T.) ;
#24719 = EDGE_CURVE('',#20114,#20113,#975,.T.) ;
#24720 = EDGE_CURVE('',#20115,#20114,#976,.T.) ;
#24721 = EDGE_CURVE('',#20116,#20115,#977,.T.) ;
#24722 = EDGE_CURVE('',#20117,#20116,#978,.T.) ;
#24723 = EDGE_CURVE('',#20118,#20117,#3284,.T.) ;
#24724 = EDGE_CURVE('',#20119,#20118,#163,.T.) ;
#24725 = EDGE_CURVE('',#20120,#20119,#979,.T.) ;
#24726 = EDGE_CURVE('',#20121,#20120,#17465,.T.) ;
#24727 = EDGE_CURVE('',#20112,#20121,#164,.T.) ;
#24728 = EDGE_CURVE('',#20122,#20123,#980,.T.) ;
#24729 = EDGE_CURVE('',#20124,#20122,#981,.T.) ;
#24730 = EDGE_CURVE('',#20125,#20124,#982,.T.) ;
#24731 = EDGE_CURVE('',#20126,#20125,#3285,.T.) ;
#24732 = EDGE_CURVE('',#20127,#20126,#983,.T.) ;
#24733 = EDGE_CURVE('',#20128,#20127,#984,.T.) ;
#24734 = EDGE_CURVE('',#20129,#20128,#985,.T.) ;
#24735 = EDGE_CURVE('',#20123,#20129,#3286,.T.) ;
#24736 = EDGE_CURVE('',#20130,#20126,#17466,.T.) ;
#24737 = EDGE_CURVE('',#20131,#20130,#986,.F.) ;
#24738 = EDGE_CURVE('',#20127,#20131,#17467,.T.) ;
#24739 = EDGE_CURVE('',#20132,#20133,#17468,.F.) ;
#24740 = EDGE_CURVE('',#20134,#20132,#17469,.F.) ;
#24741 = EDGE_CURVE('',#20133,#20134,#17470,.F.) ;
#24742 = EDGE_CURVE('',#20130,#20134,#3287,.T.) ;
#24743 = EDGE_CURVE('',#20132,#20131,#3288,.T.) ;
#24744 = EDGE_CURVE('',#20135,#20124,#17471,.T.) ;
#24745 = EDGE_CURVE('',#20136,#20135,#165,.F.) ;
#24746 = EDGE_CURVE('',#20125,#20136,#17472,.T.) ;
#24747 = EDGE_CURVE('',#20137,#20128,#17473,.T.) ;
#24748 = EDGE_CURVE('',#20138,#20137,#987,.F.) ;
#24749 = EDGE_CURVE('',#20129,#20138,#17474,.T.) ;
#24750 = EDGE_CURVE('',#20139,#20140,#17475,.F.) ;
#24751 = EDGE_CURVE('',#20141,#20139,#17476,.F.) ;
#24752 = EDGE_CURVE('',#20140,#20141,#17477,.F.) ;
#24753 = EDGE_CURVE('',#20135,#20141,#3289,.T.) ;
#24754 = EDGE_CURVE('',#20139,#20136,#3290,.T.) ;
#24755 = EDGE_CURVE('',#20142,#20143,#17478,.F.) ;
#24756 = EDGE_CURVE('',#20144,#20142,#17479,.F.) ;
#24757 = EDGE_CURVE('',#20143,#20144,#17480,.F.) ;
#24758 = EDGE_CURVE('',#20142,#20132,#988,.T.) ;
#24759 = EDGE_CURVE('',#20133,#20144,#989,.T.) ;
#24760 = EDGE_CURVE('',#20145,#20123,#17481,.T.) ;
#24761 = EDGE_CURVE('',#20146,#20145,#990,.F.) ;
#24762 = EDGE_CURVE('',#20122,#20146,#17482,.T.) ;
#24763 = EDGE_CURVE('',#20147,#20148,#17483,.F.) ;
#24764 = EDGE_CURVE('',#20149,#20147,#17484,.F.) ;
#24765 = EDGE_CURVE('',#20150,#20149,#17485,.F.) ;
#24766 = EDGE_CURVE('',#20148,#20150,#17486,.F.) ;
#24767 = EDGE_CURVE('',#20145,#20150,#3291,.T.) ;
#24768 = EDGE_CURVE('',#20147,#20146,#3292,.T.) ;
#24769 = EDGE_CURVE('',#20150,#20143,#3293,.T.) ;
#24770 = EDGE_CURVE('',#20144,#20148,#3294,.T.) ;
#24771 = EDGE_CURVE('',#20141,#20147,#991,.T.) ;
#24772 = EDGE_CURVE('',#20148,#20140,#166,.T.) ;
#24773 = EDGE_CURVE('',#20146,#20135,#167,.T.) ;
#24774 = EDGE_CURVE('',#20138,#20145,#3295,.T.) ;
#24775 = EDGE_CURVE('',#20143,#20138,#3296,.T.) ;
#24776 = EDGE_CURVE('',#20137,#20142,#3297,.T.) ;
#24777 = EDGE_CURVE('',#20134,#20139,#3298,.T.) ;
#24778 = EDGE_CURVE('',#20140,#20133,#3299,.T.) ;
#24779 = EDGE_CURVE('',#20131,#20137,#992,.T.) ;
#24780 = EDGE_CURVE('',#20136,#20130,#3300,.T.) ;
#24781 = EDGE_CURVE('',#20151,#20152,#993,.T.) ;
#24782 = EDGE_CURVE('',#20152,#20153,#17487,.T.) ;
#24783 = EDGE_CURVE('',#20153,#20154,#17488,.T.) ;
#24784 = EDGE_CURVE('',#20154,#20151,#994,.T.) ;
#24785 = EDGE_CURVE('',#19911,#20154,#168,.T.) ;
#24786 = EDGE_CURVE('',#20153,#19912,#169,.T.) ;
#24787 = EDGE_CURVE('',#19910,#19995,#3301,.T.) ;
#24788 = EDGE_CURVE('',#19912,#19994,#3302,.T.) ;
#24789 = EDGE_CURVE('',#20153,#19993,#3303,.T.) ;
#24790 = EDGE_CURVE('',#20152,#19992,#3304,.T.) ;
#24791 = EDGE_CURVE('',#20155,#20151,#3305,.T.) ;
#24792 = EDGE_CURVE('',#20155,#19991,#3306,.T.) ;
#24793 = EDGE_CURVE('',#20015,#20111,#17489,.F.) ;
#24794 = EDGE_CURVE('',#20156,#20015,#17490,.F.) ;
#24795 = EDGE_CURVE('',#19908,#20156,#17491,.F.) ;
#24796 = EDGE_CURVE('',#20111,#19908,#17492,.F.) ;
#24797 = EDGE_CURVE('',#20112,#20012,#17493,.T.) ;
#24798 = EDGE_CURVE('',#20121,#20011,#17494,.T.) ;
#24799 = EDGE_CURVE('',#20120,#20009,#17495,.T.) ;
#24800 = EDGE_CURVE('',#20119,#20010,#17496,.T.) ;
#24801 = EDGE_CURVE('',#20118,#20157,#17497,.T.) ;
#24802 = EDGE_CURVE('',#20157,#20010,#170,.T.) ;
#24803 = EDGE_CURVE('',#20117,#20158,#17498,.T.) ;
#24804 = EDGE_CURVE('',#20158,#20157,#3307,.T.) ;
#24805 = EDGE_CURVE('',#20116,#20159,#17499,.T.) ;
#24806 = EDGE_CURVE('',#20159,#20158,#995,.T.) ;
#24807 = EDGE_CURVE('',#20115,#20160,#17500,.T.) ;
#24808 = EDGE_CURVE('',#20160,#20159,#996,.T.) ;
#24809 = EDGE_CURVE('',#20114,#19909,#17501,.T.) ;
#24810 = EDGE_CURVE('',#19909,#20160,#997,.T.) ;
#24811 = EDGE_CURVE('',#20113,#19907,#17502,.T.) ;
#24812 = EDGE_CURVE('',#20157,#19999,#3308,.T.) ;
#24813 = EDGE_CURVE('',#19998,#20158,#3309,.T.) ;
#24814 = EDGE_CURVE('',#20159,#19997,#3310,.T.) ;
#24815 = EDGE_CURVE('',#20160,#19996,#3311,.T.) ;
#24816 = EDGE_CURVE('',#20054,#20161,#3312,.T.) ;
#24817 = EDGE_CURVE('',#20051,#20161,#3313,.T.) ;
#24818 = EDGE_CURVE('',#20048,#20043,#3314,.T.) ;
#24819 = EDGE_CURVE('',#20045,#20049,#3315,.T.) ;
#24820 = EDGE_CURVE('',#19979,#20064,#3316,.T.) ;
#24821 = EDGE_CURVE('',#20062,#19980,#3317,.T.) ;
#24822 = EDGE_CURVE('',#19981,#20060,#3318,.T.) ;
#24823 = EDGE_CURVE('',#19927,#20075,#3319,.T.) ;
#24824 = EDGE_CURVE('',#20046,#20022,#3320,.T.) ;
#24825 = EDGE_CURVE('',#20155,#20021,#17503,.T.) ;
#24826 = EDGE_CURVE('',#20053,#20161,#3321,.T.) ;
#24827 = EDGE_CURVE('',#20052,#20023,#3322,.T.) ;
#24828 = EDGE_CURVE('',#20162,#20163,#998,.T.) ;
#24829 = EDGE_CURVE('',#20163,#20164,#999,.T.) ;
#24830 = EDGE_CURVE('',#20164,#20165,#1000,.T.) ;
#24831 = EDGE_CURVE('',#20162,#20165,#1001,.T.) ;
#24832 = EDGE_CURVE('',#20166,#20167,#1002,.T.) ;
#24833 = EDGE_CURVE('',#20167,#20168,#1003,.T.) ;
#24834 = EDGE_CURVE('',#20168,#20169,#1004,.T.) ;
#24835 = EDGE_CURVE('',#20169,#20166,#1005,.T.) ;
#24836 = EDGE_CURVE('',#20163,#20170,#1006,.T.) ;
#24837 = EDGE_CURVE('',#20170,#20171,#1007,.T.) ;
#24838 = EDGE_CURVE('',#20171,#20164,#1008,.T.) ;
#24839 = EDGE_CURVE('',#20170,#20172,#3323,.T.) ;
#24840 = EDGE_CURVE('',#20172,#20173,#171,.T.) ;
#24841 = EDGE_CURVE('',#20173,#20171,#3324,.T.) ;
#24842 = EDGE_CURVE('',#20174,#20173,#3325,.T.) ;
#24843 = EDGE_CURVE('',#20172,#20175,#3326,.T.) ;
#24844 = EDGE_CURVE('',#20175,#20174,#172,.T.) ;
#24845 = EDGE_CURVE('',#20167,#20174,#3327,.T.) ;
#24846 = EDGE_CURVE('',#20175,#20168,#3328,.T.) ;
#24847 = EDGE_CURVE('',#20176,#20166,#1009,.T.) ;
#24848 = EDGE_CURVE('',#20169,#20177,#1010,.T.) ;
#24849 = EDGE_CURVE('',#20177,#20176,#1011,.T.) ;
#24850 = EDGE_CURVE('',#20165,#20176,#1012,.T.) ;
#24851 = EDGE_CURVE('',#20177,#20162,#1013,.T.) ;
#24852 = EDGE_CURVE('',#20178,#20173,#3329,.T.) ;
#24853 = EDGE_CURVE('',#20179,#20178,#3330,.T.) ;
#24854 = EDGE_CURVE('',#20179,#20171,#3331,.T.) ;
#24855 = EDGE_CURVE('',#20180,#20174,#3332,.T.) ;
#24856 = EDGE_CURVE('',#20178,#20180,#3333,.T.) ;
#24857 = EDGE_CURVE('',#20181,#20167,#3334,.T.) ;
#24858 = EDGE_CURVE('',#20180,#20181,#3335,.T.) ;
#24859 = EDGE_CURVE('',#20182,#20166,#3336,.T.) ;
#24860 = EDGE_CURVE('',#20181,#20182,#1014,.T.) ;
#24861 = EDGE_CURVE('',#20183,#20184,#3337,.T.) ;
#24862 = EDGE_CURVE('',#20185,#20183,#1015,.T.) ;
#24863 = EDGE_CURVE('',#20186,#20185,#1016,.T.) ;
#24864 = EDGE_CURVE('',#20187,#20186,#1017,.T.) ;
#24865 = EDGE_CURVE('',#20188,#20187,#1018,.T.) ;
#24866 = EDGE_CURVE('',#20189,#20188,#3338,.T.) ;
#24867 = EDGE_CURVE('',#20190,#20189,#3339,.T.) ;
#24868 = EDGE_CURVE('',#20191,#20190,#3340,.T.) ;
#24869 = EDGE_CURVE('',#20192,#20191,#1019,.T.) ;
#24870 = EDGE_CURVE('',#20193,#20192,#1020,.T.) ;
#24871 = EDGE_CURVE('',#20194,#20193,#1021,.T.) ;
#24872 = EDGE_CURVE('',#20195,#20194,#1022,.T.) ;
#24873 = EDGE_CURVE('',#20196,#20195,#1023,.T.) ;
#24874 = EDGE_CURVE('',#20197,#20196,#1024,.T.) ;
#24875 = EDGE_CURVE('',#20198,#20197,#1025,.T.) ;
#24876 = EDGE_CURVE('',#20199,#20198,#3341,.T.) ;
#24877 = EDGE_CURVE('',#20200,#20199,#3342,.T.) ;
#24878 = EDGE_CURVE('',#20201,#20200,#3343,.T.) ;
#24879 = EDGE_CURVE('',#20184,#20201,#3344,.T.) ;
#24880 = EDGE_CURVE('',#20190,#20202,#173,.T.) ;
#24881 = EDGE_CURVE('',#20202,#20203,#3345,.T.) ;
#24882 = EDGE_CURVE('',#20191,#20203,#1026,.T.) ;
#24883 = EDGE_CURVE('',#20189,#20204,#174,.T.) ;
#24884 = EDGE_CURVE('',#20204,#20202,#3346,.T.) ;
#24885 = EDGE_CURVE('',#20188,#20205,#1027,.T.) ;
#24886 = EDGE_CURVE('',#20205,#20204,#3347,.T.) ;
#24887 = EDGE_CURVE('',#20187,#20206,#1028,.T.) ;
#24888 = EDGE_CURVE('',#20206,#20205,#1029,.T.) ;
#24889 = EDGE_CURVE('',#20186,#20207,#1030,.T.) ;
#24890 = EDGE_CURVE('',#20207,#20206,#1031,.T.) ;
#24891 = EDGE_CURVE('',#20208,#20209,#1032,.T.) ;
#24892 = EDGE_CURVE('',#20209,#20198,#17504,.T.) ;
#24893 = EDGE_CURVE('',#20197,#20208,#1033,.T.) ;
#24894 = EDGE_CURVE('',#20185,#20210,#1034,.T.) ;
#24895 = EDGE_CURVE('',#20210,#20207,#1035,.T.) ;
#24896 = EDGE_CURVE('',#20211,#20212,#3348,.T.) ;
#24897 = EDGE_CURVE('',#20212,#20183,#17505,.T.) ;
#24898 = EDGE_CURVE('',#20184,#20211,#175,.T.) ;
#24899 = EDGE_CURVE('',#20212,#20210,#1036,.T.) ;
#24900 = EDGE_CURVE('',#20201,#20213,#176,.T.) ;
#24901 = EDGE_CURVE('',#20213,#20211,#3349,.T.) ;
#24902 = EDGE_CURVE('',#20214,#20213,#3350,.T.) ;
#24903 = EDGE_CURVE('',#20200,#20214,#177,.T.) ;
#24904 = EDGE_CURVE('',#20215,#20214,#3351,.T.) ;
#24905 = EDGE_CURVE('',#20199,#20215,#178,.T.) ;
#24906 = EDGE_CURVE('',#20209,#20215,#3352,.T.) ;
#24907 = EDGE_CURVE('',#20216,#20208,#1037,.T.) ;
#24908 = EDGE_CURVE('',#20196,#20216,#1038,.T.) ;
#24909 = EDGE_CURVE('',#20217,#20216,#1039,.T.) ;
#24910 = EDGE_CURVE('',#20195,#20217,#1040,.T.) ;
#24911 = EDGE_CURVE('',#20218,#20217,#1041,.T.) ;
#24912 = EDGE_CURVE('',#20194,#20218,#1042,.T.) ;
#24913 = EDGE_CURVE('',#20219,#20218,#1043,.T.) ;
#24914 = EDGE_CURVE('',#20193,#20219,#1044,.T.) ;
#24915 = EDGE_CURVE('',#20220,#20219,#1045,.T.) ;
#24916 = EDGE_CURVE('',#20192,#20220,#1046,.T.) ;
#24917 = EDGE_CURVE('',#20203,#20220,#1047,.T.) ;
#24918 = EDGE_CURVE('',#20221,#20220,#3353,.T.) ;
#24919 = EDGE_CURVE('',#20222,#20221,#1048,.T.) ;
#24920 = EDGE_CURVE('',#20222,#20219,#3354,.T.) ;
#24921 = EDGE_CURVE('',#20223,#20203,#3355,.T.) ;
#24922 = EDGE_CURVE('',#20221,#20223,#1049,.T.) ;
#24923 = EDGE_CURVE('',#20224,#20202,#3356,.T.) ;
#24924 = EDGE_CURVE('',#20223,#20224,#3357,.T.) ;
#24925 = EDGE_CURVE('',#20225,#20204,#3358,.T.) ;
#24926 = EDGE_CURVE('',#20224,#20225,#3359,.T.) ;
#24927 = EDGE_CURVE('',#20226,#20205,#3360,.T.) ;
#24928 = EDGE_CURVE('',#20225,#20226,#3361,.T.) ;
#24929 = EDGE_CURVE('',#20227,#20206,#3362,.T.) ;
#24930 = EDGE_CURVE('',#20226,#20227,#1050,.T.) ;
#24931 = EDGE_CURVE('',#20228,#20207,#3363,.T.) ;
#24932 = EDGE_CURVE('',#20227,#20228,#1051,.T.) ;
#24933 = EDGE_CURVE('',#20229,#20210,#3364,.T.) ;
#24934 = EDGE_CURVE('',#20228,#20229,#1052,.T.) ;
#24935 = EDGE_CURVE('',#20230,#20212,#3365,.T.) ;
#24936 = EDGE_CURVE('',#20229,#20230,#1053,.T.) ;
#24937 = EDGE_CURVE('',#20231,#20211,#3366,.T.) ;
#24938 = EDGE_CURVE('',#20230,#20231,#3367,.T.) ;
#24939 = EDGE_CURVE('',#20232,#20233,#1054,.T.) ;
#24940 = EDGE_CURVE('',#20233,#20182,#1055,.T.) ;
#24941 = EDGE_CURVE('',#20182,#20234,#1056,.T.) ;
#24942 = EDGE_CURVE('',#20232,#20234,#1057,.T.) ;
#24943 = EDGE_CURVE('',#20181,#20235,#1058,.T.) ;
#24944 = EDGE_CURVE('',#20235,#20236,#3368,.T.) ;
#24945 = EDGE_CURVE('',#20236,#20180,#179,.T.) ;
#24946 = EDGE_CURVE('',#20237,#20238,#3369,.T.) ;
#24947 = EDGE_CURVE('',#20238,#20179,#1059,.T.) ;
#24948 = EDGE_CURVE('',#20178,#20237,#180,.T.) ;
#24949 = EDGE_CURVE('',#20239,#20179,#1060,.T.) ;
#24950 = EDGE_CURVE('',#20238,#20240,#1061,.T.) ;
#24951 = EDGE_CURVE('',#20240,#20239,#1062,.T.) ;
#24952 = EDGE_CURVE('',#20236,#20237,#3370,.T.) ;
#24953 = EDGE_CURVE('',#20241,#20239,#1063,.T.) ;
#24954 = EDGE_CURVE('',#20240,#20242,#1064,.T.) ;
#24955 = EDGE_CURVE('',#20242,#20241,#1065,.T.) ;
#24956 = EDGE_CURVE('',#20234,#20241,#1066,.T.) ;
#24957 = EDGE_CURVE('',#20242,#20232,#1067,.T.) ;
#24958 = EDGE_CURVE('',#20233,#20235,#1068,.T.) ;
#24959 = EDGE_CURVE('',#20243,#20244,#3371,.T.) ;
#24960 = EDGE_CURVE('',#20244,#20245,#181,.T.) ;
#24961 = EDGE_CURVE('',#20245,#20246,#3372,.T.) ;
#24962 = EDGE_CURVE('',#20243,#20246,#182,.T.) ;
#24963 = EDGE_CURVE('',#20247,#20245,#3373,.T.) ;
#24964 = EDGE_CURVE('',#20244,#20248,#3374,.T.) ;
#24965 = EDGE_CURVE('',#20248,#20247,#183,.T.) ;
#24966 = EDGE_CURVE('',#20246,#20247,#3375,.T.) ;
#24967 = EDGE_CURVE('',#20248,#20243,#3376,.T.) ;
#24968 = EDGE_CURVE('',#20249,#20246,#3377,.T.) ;
#24969 = EDGE_CURVE('',#20250,#20249,#3378,.T.) ;
#24970 = EDGE_CURVE('',#20250,#20247,#3379,.T.) ;
#24971 = EDGE_CURVE('',#20251,#20245,#3380,.T.) ;
#24972 = EDGE_CURVE('',#20249,#20251,#3381,.T.) ;
#24973 = EDGE_CURVE('',#20252,#20253,#3382,.T.) ;
#24974 = EDGE_CURVE('',#20253,#20254,#184,.T.) ;
#24975 = EDGE_CURVE('',#20254,#20255,#3383,.T.) ;
#24976 = EDGE_CURVE('',#20252,#20255,#185,.T.) ;
#24977 = EDGE_CURVE('',#20256,#20254,#3384,.T.) ;
#24978 = EDGE_CURVE('',#20253,#20257,#3385,.T.) ;
#24979 = EDGE_CURVE('',#20257,#20256,#186,.T.) ;
#24980 = EDGE_CURVE('',#20258,#20256,#3386,.T.) ;
#24981 = EDGE_CURVE('',#20257,#20259,#3387,.T.) ;
#24982 = EDGE_CURVE('',#20259,#20258,#187,.T.) ;
#24983 = EDGE_CURVE('',#20255,#20258,#3388,.T.) ;
#24984 = EDGE_CURVE('',#20259,#20252,#3389,.T.) ;
#24985 = EDGE_CURVE('',#20260,#20255,#3390,.T.) ;
#24986 = EDGE_CURVE('',#20261,#20260,#3391,.T.) ;
#24987 = EDGE_CURVE('',#20261,#20258,#3392,.T.) ;
#24988 = EDGE_CURVE('',#20262,#20254,#3393,.T.) ;
#24989 = EDGE_CURVE('',#20260,#20262,#3394,.T.) ;
#24990 = EDGE_CURVE('',#20263,#20264,#3395,.T.) ;
#24991 = EDGE_CURVE('',#20264,#20265,#188,.T.) ;
#24992 = EDGE_CURVE('',#20265,#20266,#3396,.T.) ;
#24993 = EDGE_CURVE('',#20263,#20266,#189,.T.) ;
#24994 = EDGE_CURVE('',#20267,#20265,#3397,.T.) ;
#24995 = EDGE_CURVE('',#20264,#20268,#3398,.T.) ;
#24996 = EDGE_CURVE('',#20268,#20267,#190,.T.) ;
#24997 = EDGE_CURVE('',#20266,#20267,#3399,.T.) ;
#24998 = EDGE_CURVE('',#20268,#20263,#3400,.T.) ;
#24999 = EDGE_CURVE('',#20269,#20266,#3401,.T.) ;
#25000 = EDGE_CURVE('',#20270,#20269,#3402,.T.) ;
#25001 = EDGE_CURVE('',#20270,#20267,#3403,.T.) ;
#25002 = EDGE_CURVE('',#20271,#20265,#3404,.T.) ;
#25003 = EDGE_CURVE('',#20269,#20271,#3405,.T.) ;
#25004 = EDGE_CURVE('',#20272,#20273,#3406,.T.) ;
#25005 = EDGE_CURVE('',#20273,#20223,#1069,.T.) ;
#25006 = EDGE_CURVE('',#20272,#20224,#191,.T.) ;
#25007 = EDGE_CURVE('',#20273,#20274,#1070,.T.) ;
#25008 = EDGE_CURVE('',#20274,#20221,#1071,.T.) ;
#25009 = EDGE_CURVE('',#20274,#20275,#1072,.T.) ;
#25010 = EDGE_CURVE('',#20275,#20222,#1073,.T.) ;
#25011 = EDGE_CURVE('',#20226,#20276,#17506,.T.) ;
#25012 = EDGE_CURVE('',#20276,#20277,#3407,.T.) ;
#25013 = EDGE_CURVE('',#20277,#20225,#192,.T.) ;
#25014 = EDGE_CURVE('',#20275,#20278,#1074,.T.) ;
#25015 = EDGE_CURVE('',#20278,#20279,#1075,.T.) ;
#25016 = EDGE_CURVE('',#20279,#20222,#1076,.T.) ;
#25017 = EDGE_CURVE('',#20278,#20280,#1077,.T.) ;
#25018 = EDGE_CURVE('',#20280,#20281,#1078,.T.) ;
#25019 = EDGE_CURVE('',#20281,#20279,#1079,.T.) ;
#25020 = EDGE_CURVE('',#20280,#20282,#1080,.T.) ;
#25021 = EDGE_CURVE('',#20282,#20283,#1081,.T.) ;
#25022 = EDGE_CURVE('',#20283,#20281,#1082,.T.) ;
#25023 = EDGE_CURVE('',#20282,#20284,#1083,.T.) ;
#25024 = EDGE_CURVE('',#20284,#20285,#1084,.T.) ;
#25025 = EDGE_CURVE('',#20285,#20283,#1085,.T.) ;
#25026 = EDGE_CURVE('',#20284,#20286,#1086,.T.) ;
#25027 = EDGE_CURVE('',#20286,#20287,#1087,.T.) ;
#25028 = EDGE_CURVE('',#20287,#20285,#1088,.T.) ;
#25029 = EDGE_CURVE('',#20231,#20288,#3408,.T.) ;
#25030 = EDGE_CURVE('',#20288,#20289,#193,.T.) ;
#25031 = EDGE_CURVE('',#20289,#20290,#3409,.T.) ;
#25032 = EDGE_CURVE('',#20290,#20231,#194,.T.) ;
#25033 = EDGE_CURVE('',#20286,#20291,#3410,.T.) ;
#25034 = EDGE_CURVE('',#20291,#20292,#195,.T.) ;
#25035 = EDGE_CURVE('',#20292,#20287,#3411,.T.) ;
#25036 = EDGE_CURVE('',#20291,#20293,#3412,.T.) ;
#25037 = EDGE_CURVE('',#20293,#20294,#196,.T.) ;
#25038 = EDGE_CURVE('',#20294,#20292,#3413,.T.) ;
#25039 = EDGE_CURVE('',#20288,#20294,#3414,.T.) ;
#25040 = EDGE_CURVE('',#20293,#20289,#3415,.T.) ;
#25041 = EDGE_CURVE('',#20230,#20295,#17507,.T.) ;
#25042 = EDGE_CURVE('',#20295,#20296,#1089,.T.) ;
#25043 = EDGE_CURVE('',#20296,#20229,#1090,.T.) ;
#25044 = EDGE_CURVE('',#20290,#20295,#3416,.T.) ;
#25045 = EDGE_CURVE('',#20296,#20297,#1091,.T.) ;
#25046 = EDGE_CURVE('',#20297,#20228,#1092,.T.) ;
#25047 = EDGE_CURVE('',#20297,#20298,#1093,.T.) ;
#25048 = EDGE_CURVE('',#20298,#20227,#1094,.T.) ;
#25049 = EDGE_CURVE('',#20298,#20276,#1095,.T.) ;
#25050 = EDGE_CURVE('',#20277,#20272,#3417,.T.) ;
#25051 = EDGE_CURVE('',#20279,#20218,#3418,.T.) ;
#25052 = EDGE_CURVE('',#20281,#20217,#3419,.T.) ;
#25053 = EDGE_CURVE('',#20283,#20216,#3420,.T.) ;
#25054 = EDGE_CURVE('',#20285,#20208,#3421,.T.) ;
#25055 = EDGE_CURVE('',#20287,#20209,#3422,.T.) ;
#25056 = EDGE_CURVE('',#20292,#20215,#3423,.T.) ;
#25057 = EDGE_CURVE('',#20294,#20214,#3424,.T.) ;
#25058 = EDGE_CURVE('',#20288,#20213,#3425,.T.) ;
#25059 = EDGE_CURVE('',#20299,#20300,#3426,.T.) ;
#25060 = EDGE_CURVE('',#20301,#20299,#3427,.T.) ;
#25061 = EDGE_CURVE('',#20302,#20301,#3428,.T.) ;
#25062 = EDGE_CURVE('',#20303,#20302,#197,.T.) ;
#25063 = EDGE_CURVE('',#20304,#20303,#3429,.T.) ;
#25064 = EDGE_CURVE('',#20305,#20304,#198,.T.) ;
#25065 = EDGE_CURVE('',#20306,#20305,#3430,.T.) ;
#25066 = EDGE_CURVE('',#20307,#20306,#3431,.T.) ;
#25067 = EDGE_CURVE('',#20308,#20307,#17508,.T.) ;
#25068 = EDGE_CURVE('',#20307,#20308,#17509,.T.) ;
#25069 = EDGE_CURVE('',#20309,#20307,#3432,.T.) ;
#25070 = EDGE_CURVE('',#20310,#20309,#3433,.T.) ;
#25071 = EDGE_CURVE('',#20311,#20310,#199,.T.) ;
#25072 = EDGE_CURVE('',#20312,#20311,#3434,.T.) ;
#25073 = EDGE_CURVE('',#20313,#20312,#200,.T.) ;
#25074 = EDGE_CURVE('',#20314,#20313,#3435,.T.) ;
#25075 = EDGE_CURVE('',#20315,#20314,#3436,.T.) ;
#25076 = EDGE_CURVE('',#20316,#20315,#3437,.T.) ;
#25077 = EDGE_CURVE('',#20317,#20316,#17510,.T.) ;
#25078 = EDGE_CURVE('',#20318,#20317,#3438,.T.) ;
#25079 = EDGE_CURVE('',#20319,#20318,#17511,.T.) ;
#25080 = EDGE_CURVE('',#20320,#20319,#3439,.T.) ;
#25081 = EDGE_CURVE('',#20321,#20320,#17512,.T.) ;
#25082 = EDGE_CURVE('',#20322,#20321,#3440,.T.) ;
#25083 = EDGE_CURVE('',#20323,#20322,#17513,.T.) ;
#25084 = EDGE_CURVE('',#20324,#20323,#3441,.T.) ;
#25085 = EDGE_CURVE('',#20325,#20324,#17514,.T.) ;
#25086 = EDGE_CURVE('',#20326,#20325,#3442,.T.) ;
#25087 = EDGE_CURVE('',#20327,#20326,#17515,.T.) ;
#25088 = EDGE_CURVE('',#20328,#20327,#3443,.T.) ;
#25089 = EDGE_CURVE('',#20329,#20328,#17516,.T.) ;
#25090 = EDGE_CURVE('',#20330,#20329,#3444,.T.) ;
#25091 = EDGE_CURVE('',#20331,#20330,#17517,.T.) ;
#25092 = EDGE_CURVE('',#20332,#20331,#3445,.T.) ;
#25093 = EDGE_CURVE('',#20333,#20332,#17518,.T.) ;
#25094 = EDGE_CURVE('',#20334,#20333,#3446,.T.) ;
#25095 = EDGE_CURVE('',#20335,#20334,#17519,.T.) ;
#25096 = EDGE_CURVE('',#20336,#20335,#3447,.T.) ;
#25097 = EDGE_CURVE('',#20337,#20336,#17520,.T.) ;
#25098 = EDGE_CURVE('',#20338,#20337,#3448,.T.) ;
#25099 = EDGE_CURVE('',#20339,#20338,#17521,.T.) ;
#25100 = EDGE_CURVE('',#20340,#20339,#17522,.T.) ;
#25101 = EDGE_CURVE('',#20341,#20340,#3449,.T.) ;
#25102 = EDGE_CURVE('',#20342,#20341,#17523,.T.) ;
#25103 = EDGE_CURVE('',#20343,#20342,#17524,.T.) ;
#25104 = EDGE_CURVE('',#20344,#20343,#3450,.T.) ;
#25105 = EDGE_CURVE('',#20345,#20344,#17525,.T.) ;
#25106 = EDGE_CURVE('',#20346,#20345,#3451,.T.) ;
#25107 = EDGE_CURVE('',#20300,#20346,#17526,.T.) ;
#25108 = EDGE_CURVE('',#20347,#20348,#3452,.T.) ;
#25109 = EDGE_CURVE('',#20349,#20347,#3453,.T.) ;
#25110 = EDGE_CURVE('',#20348,#20349,#3454,.T.) ;
#25111 = EDGE_CURVE('',#20350,#20351,#3455,.T.) ;
#25112 = EDGE_CURVE('',#20352,#20350,#3456,.T.) ;
#25113 = EDGE_CURVE('',#20351,#20352,#3457,.T.) ;
#25114 = EDGE_CURVE('',#20353,#20354,#17527,.T.) ;
#25115 = EDGE_CURVE('',#20355,#20353,#3458,.T.) ;
#25116 = EDGE_CURVE('',#20356,#20355,#17528,.T.) ;
#25117 = EDGE_CURVE('',#20357,#20356,#3459,.T.) ;
#25118 = EDGE_CURVE('',#20358,#20357,#17529,.T.) ;
#25119 = EDGE_CURVE('',#20359,#20358,#3460,.T.) ;
#25120 = EDGE_CURVE('',#20360,#20359,#3461,.T.) ;
#25121 = EDGE_CURVE('',#20361,#20360,#17530,.T.) ;
#25122 = EDGE_CURVE('',#20362,#20361,#3462,.T.) ;
#25123 = EDGE_CURVE('',#20363,#20362,#17531,.T.) ;
#25124 = EDGE_CURVE('',#20364,#20363,#3463,.T.) ;
#25125 = EDGE_CURVE('',#20365,#20364,#3464,.T.) ;
#25126 = EDGE_CURVE('',#20366,#20365,#17532,.T.) ;
#25127 = EDGE_CURVE('',#20354,#20366,#3465,.T.) ;
#25128 = EDGE_CURVE('',#20367,#20368,#3466,.T.) ;
#25129 = EDGE_CURVE('',#20369,#20368,#3467,.T.) ;
#25130 = EDGE_CURVE('',#20370,#20369,#3468,.T.) ;
#25131 = EDGE_CURVE('',#20371,#20370,#3469,.T.) ;
#25132 = EDGE_CURVE('',#20371,#20372,#3470,.T.) ;
#25133 = EDGE_CURVE('',#20373,#20372,#17533,.T.) ;
#25134 = EDGE_CURVE('',#20374,#20373,#3471,.T.) ;
#25135 = EDGE_CURVE('',#20375,#20374,#17534,.T.) ;
#25136 = EDGE_CURVE('',#20376,#20375,#3472,.T.) ;
#25137 = EDGE_CURVE('',#20377,#20376,#17535,.T.) ;
#25138 = EDGE_CURVE('',#20378,#20377,#3473,.T.) ;
#25139 = EDGE_CURVE('',#20379,#20378,#17536,.T.) ;
#25140 = EDGE_CURVE('',#20380,#20379,#3474,.T.) ;
#25141 = EDGE_CURVE('',#20381,#20380,#17537,.T.) ;
#25142 = EDGE_CURVE('',#20382,#20381,#3475,.T.) ;
#25143 = EDGE_CURVE('',#20367,#20382,#17538,.T.) ;
#25144 = EDGE_CURVE('',#20383,#20384,#17539,.T.) ;
#25145 = EDGE_CURVE('',#20385,#20383,#3476,.T.) ;
#25146 = EDGE_CURVE('',#20386,#20385,#3477,.T.) ;
#25147 = EDGE_CURVE('',#20387,#20386,#17540,.T.) ;
#25148 = EDGE_CURVE('',#20388,#20387,#3478,.T.) ;
#25149 = EDGE_CURVE('',#20389,#20388,#17541,.T.) ;
#25150 = EDGE_CURVE('',#20390,#20389,#3479,.T.) ;
#25151 = EDGE_CURVE('',#20391,#20390,#3480,.T.) ;
#25152 = EDGE_CURVE('',#20392,#20391,#17542,.T.) ;
#25153 = EDGE_CURVE('',#20393,#20392,#3481,.T.) ;
#25154 = EDGE_CURVE('',#20394,#20393,#17543,.T.) ;
#25155 = EDGE_CURVE('',#20395,#20394,#3482,.T.) ;
#25156 = EDGE_CURVE('',#20396,#20395,#17544,.T.) ;
#25157 = EDGE_CURVE('',#20384,#20396,#3483,.T.) ;
#25158 = EDGE_CURVE('',#20397,#20398,#17545,.T.) ;
#25159 = EDGE_CURVE('',#20399,#20397,#3484,.T.) ;
#25160 = EDGE_CURVE('',#20400,#20399,#3485,.T.) ;
#25161 = EDGE_CURVE('',#20401,#20400,#17546,.T.) ;
#25162 = EDGE_CURVE('',#20402,#20401,#3486,.T.) ;
#25163 = EDGE_CURVE('',#20403,#20402,#17547,.T.) ;
#25164 = EDGE_CURVE('',#20404,#20403,#3487,.T.) ;
#25165 = EDGE_CURVE('',#20405,#20404,#3488,.T.) ;
#25166 = EDGE_CURVE('',#20406,#20405,#17548,.T.) ;
#25167 = EDGE_CURVE('',#20407,#20406,#3489,.T.) ;
#25168 = EDGE_CURVE('',#20408,#20407,#17549,.T.) ;
#25169 = EDGE_CURVE('',#20409,#20408,#3490,.T.) ;
#25170 = EDGE_CURVE('',#20410,#20409,#17550,.T.) ;
#25171 = EDGE_CURVE('',#20398,#20410,#3491,.T.) ;
#25172 = EDGE_CURVE('',#20411,#20412,#3492,.T.) ;
#25173 = EDGE_CURVE('',#20413,#20412,#3493,.T.) ;
#25174 = EDGE_CURVE('',#20414,#20413,#3494,.T.) ;
#25175 = EDGE_CURVE('',#20415,#20414,#3495,.T.) ;
#25176 = EDGE_CURVE('',#20415,#20416,#3496,.T.) ;
#25177 = EDGE_CURVE('',#20417,#20416,#3497,.T.) ;
#25178 = EDGE_CURVE('',#20418,#20417,#17551,.T.) ;
#25179 = EDGE_CURVE('',#20419,#20418,#3498,.T.) ;
#25180 = EDGE_CURVE('',#20420,#20419,#17552,.T.) ;
#25181 = EDGE_CURVE('',#20421,#20420,#3499,.T.) ;
#25182 = EDGE_CURVE('',#20422,#20421,#17553,.T.) ;
#25183 = EDGE_CURVE('',#20423,#20422,#3500,.T.) ;
#25184 = EDGE_CURVE('',#20424,#20423,#17554,.T.) ;
#25185 = EDGE_CURVE('',#20411,#20424,#3501,.T.) ;
#25186 = EDGE_CURVE('',#20425,#20425,#17555,.T.) ;
#25187 = EDGE_CURVE('',#20426,#20427,#3502,.T.) ;
#25188 = EDGE_CURVE('',#20428,#20427,#17556,.T.) ;
#25189 = EDGE_CURVE('',#20429,#20428,#3503,.T.) ;
#25190 = EDGE_CURVE('',#20430,#20429,#17557,.T.) ;
#25191 = EDGE_CURVE('',#20431,#20430,#3504,.T.) ;
#25192 = EDGE_CURVE('',#20432,#20431,#17558,.T.) ;
#25193 = EDGE_CURVE('',#20433,#20432,#3505,.T.) ;
#25194 = EDGE_CURVE('',#20434,#20433,#17559,.T.) ;
#25195 = EDGE_CURVE('',#20435,#20434,#3506,.T.) ;
#25196 = EDGE_CURVE('',#20436,#20435,#17560,.T.) ;
#25197 = EDGE_CURVE('',#20437,#20436,#3507,.T.) ;
#25198 = EDGE_CURVE('',#20437,#20438,#3508,.T.) ;
#25199 = EDGE_CURVE('',#20439,#20438,#3509,.T.) ;
#25200 = EDGE_CURVE('',#20440,#20439,#3510,.T.) ;
#25201 = EDGE_CURVE('',#20426,#20440,#3511,.T.) ;
#25202 = EDGE_CURVE('',#20441,#20441,#17561,.T.) ;
#25203 = EDGE_CURVE('',#20442,#20442,#17562,.T.) ;
#25204 = EDGE_CURVE('',#20443,#20444,#3512,.T.) ;
#25205 = EDGE_CURVE('',#20443,#20445,#3513,.T.) ;
#25206 = EDGE_CURVE('',#20446,#20445,#3514,.T.) ;
#25207 = EDGE_CURVE('',#20447,#20446,#17563,.T.) ;
#25208 = EDGE_CURVE('',#20448,#20447,#3515,.T.) ;
#25209 = EDGE_CURVE('',#20449,#20448,#17564,.T.) ;
#25210 = EDGE_CURVE('',#20450,#20449,#3516,.T.) ;
#25211 = EDGE_CURVE('',#20451,#20450,#17565,.T.) ;
#25212 = EDGE_CURVE('',#20452,#20451,#3517,.T.) ;
#25213 = EDGE_CURVE('',#20453,#20452,#17566,.T.) ;
#25214 = EDGE_CURVE('',#20454,#20453,#3518,.T.) ;
#25215 = EDGE_CURVE('',#20454,#20455,#3519,.T.) ;
#25216 = EDGE_CURVE('',#20456,#20455,#3520,.T.) ;
#25217 = EDGE_CURVE('',#20444,#20456,#3521,.T.) ;
#25218 = EDGE_CURVE('',#20457,#20457,#17567,.T.) ;
#25219 = EDGE_CURVE('',#20458,#20458,#17568,.T.) ;
#25220 = EDGE_CURVE('',#20459,#20460,#17569,.T.) ;
#25221 = EDGE_CURVE('',#20461,#20459,#3522,.T.) ;
#25222 = EDGE_CURVE('',#20462,#20461,#17570,.T.) ;
#25223 = EDGE_CURVE('',#20463,#20462,#3523,.T.) ;
#25224 = EDGE_CURVE('',#20464,#20463,#17571,.T.) ;
#25225 = EDGE_CURVE('',#20465,#20464,#3524,.T.) ;
#25226 = EDGE_CURVE('',#20466,#20465,#17572,.T.) ;
#25227 = EDGE_CURVE('',#20460,#20466,#3525,.T.) ;
#25228 = EDGE_CURVE('',#20467,#20468,#17573,.T.) ;
#25229 = EDGE_CURVE('',#20469,#20467,#3526,.T.) ;
#25230 = EDGE_CURVE('',#20470,#20469,#17574,.T.) ;
#25231 = EDGE_CURVE('',#20471,#20470,#3527,.T.) ;
#25232 = EDGE_CURVE('',#20472,#20471,#17575,.T.) ;
#25233 = EDGE_CURVE('',#20473,#20472,#3528,.T.) ;
#25234 = EDGE_CURVE('',#20474,#20473,#3529,.T.) ;
#25235 = EDGE_CURVE('',#20475,#20474,#17576,.T.) ;
#25236 = EDGE_CURVE('',#20476,#20475,#3530,.T.) ;
#25237 = EDGE_CURVE('',#20477,#20476,#17577,.T.) ;
#25238 = EDGE_CURVE('',#20478,#20477,#3531,.T.) ;
#25239 = EDGE_CURVE('',#20479,#20478,#3532,.T.) ;
#25240 = EDGE_CURVE('',#20480,#20479,#17578,.T.) ;
#25241 = EDGE_CURVE('',#20468,#20480,#3533,.T.) ;
#25242 = EDGE_CURVE('',#20481,#20482,#3534,.T.) ;
#25243 = EDGE_CURVE('',#20483,#20481,#3535,.T.) ;
#25244 = EDGE_CURVE('',#20484,#20483,#3536,.T.) ;
#25245 = EDGE_CURVE('',#20482,#20484,#3537,.T.) ;
#25246 = EDGE_CURVE('',#20348,#20249,#201,.T.) ;
#25247 = EDGE_CURVE('',#20251,#20347,#202,.T.) ;
#25248 = EDGE_CURVE('',#20349,#20250,#203,.T.) ;
#25249 = EDGE_CURVE('',#20251,#20250,#3538,.T.) ;
#25250 = EDGE_CURVE('',#20482,#20260,#204,.T.) ;
#25251 = EDGE_CURVE('',#20262,#20481,#205,.T.) ;
#25252 = EDGE_CURVE('',#20484,#20261,#206,.T.) ;
#25253 = EDGE_CURVE('',#20485,#20261,#3539,.T.) ;
#25254 = EDGE_CURVE('',#20483,#20485,#207,.T.) ;
#25255 = EDGE_CURVE('',#20262,#20485,#3540,.T.) ;
#25256 = EDGE_CURVE('',#20485,#20256,#3541,.T.) ;
#25257 = EDGE_CURVE('',#20351,#20269,#208,.T.) ;
#25258 = EDGE_CURVE('',#20271,#20350,#209,.T.) ;
#25259 = EDGE_CURVE('',#20352,#20270,#210,.T.) ;
#25260 = EDGE_CURVE('',#20271,#20270,#3542,.T.) ;
#25261 = EDGE_CURVE('',#20239,#20164,#3543,.T.) ;
#25262 = EDGE_CURVE('',#20241,#20165,#3544,.T.) ;
#25263 = EDGE_CURVE('',#20234,#20176,#3545,.T.) ;
#25264 = EDGE_CURVE('',#20486,#20487,#17579,.T.) ;
#25265 = EDGE_CURVE('',#20487,#20488,#17580,.T.) ;
#25266 = EDGE_CURVE('',#20488,#20488,#17581,.T.) ;
#25267 = EDGE_CURVE('',#20487,#20486,#17582,.T.) ;
#25268 = EDGE_CURVE('',#20489,#20489,#17583,.T.) ;
#25269 = EDGE_CURVE('',#20486,#20490,#3546,.T.) ;
#25270 = EDGE_CURVE('',#20490,#20490,#17584,.T.) ;
#25271 = EDGE_CURVE('',#20491,#20491,#17585,.T.) ;
#25272 = EDGE_CURVE('',#20491,#20489,#17586,.T.) ;
#25273 = EDGE_CURVE('',#20492,#20492,#17587,.T.) ;
#25274 = EDGE_CURVE('',#20492,#20491,#3547,.T.) ;
#25275 = EDGE_CURVE('',#20493,#20493,#17588,.T.) ;
#25276 = EDGE_CURVE('',#20493,#20492,#17589,.T.) ;
#25277 = EDGE_CURVE('',#20494,#20495,#3548,.T.) ;
#25278 = EDGE_CURVE('',#20496,#20494,#17590,.T.) ;
#25279 = EDGE_CURVE('',#20497,#20496,#3549,.T.) ;
#25280 = EDGE_CURVE('',#20498,#20497,#3550,.T.) ;
#25281 = EDGE_CURVE('',#20498,#20499,#3551,.T.) ;
#25282 = EDGE_CURVE('',#20499,#20500,#3552,.T.) ;
#25283 = EDGE_CURVE('',#20501,#20500,#3553,.T.) ;
#25284 = EDGE_CURVE('',#20502,#20501,#17591,.T.) ;
#25285 = EDGE_CURVE('',#20503,#20502,#3554,.T.) ;
#25286 = EDGE_CURVE('',#20504,#20503,#17592,.T.) ;
#25287 = EDGE_CURVE('',#20505,#20504,#3555,.T.) ;
#25288 = EDGE_CURVE('',#20506,#20505,#17593,.T.) ;
#25289 = EDGE_CURVE('',#20507,#20506,#3556,.T.) ;
#25290 = EDGE_CURVE('',#20508,#20507,#3557,.T.) ;
#25291 = EDGE_CURVE('',#20508,#20509,#211,.T.) ;
#25292 = EDGE_CURVE('',#20510,#20509,#3558,.F.) ;
#25293 = EDGE_CURVE('',#20510,#20511,#212,.T.) ;
#25294 = EDGE_CURVE('',#20512,#20511,#3559,.F.) ;
#25295 = EDGE_CURVE('',#20513,#20512,#3560,.T.) ;
#25296 = EDGE_CURVE('',#20514,#20513,#3561,.T.) ;
#25297 = EDGE_CURVE('',#20514,#20515,#213,.T.) ;
#25298 = EDGE_CURVE('',#20516,#20515,#3562,.F.) ;
#25299 = EDGE_CURVE('',#20516,#20517,#214,.T.) ;
#25300 = EDGE_CURVE('',#20518,#20517,#3563,.T.) ;
#25301 = EDGE_CURVE('',#20519,#20518,#3564,.T.) ;
#25302 = EDGE_CURVE('',#20520,#20519,#17594,.T.) ;
#25303 = EDGE_CURVE('',#20521,#20520,#3565,.T.) ;
#25304 = EDGE_CURVE('',#20522,#20521,#17595,.T.) ;
#25305 = EDGE_CURVE('',#20523,#20522,#3566,.T.) ;
#25306 = EDGE_CURVE('',#20524,#20523,#17596,.T.) ;
#25307 = EDGE_CURVE('',#20525,#20524,#17597,.T.) ;
#25308 = EDGE_CURVE('',#20526,#20525,#3567,.T.) ;
#25309 = EDGE_CURVE('',#20527,#20526,#17598,.T.) ;
#25310 = EDGE_CURVE('',#20528,#20527,#17599,.T.) ;
#25311 = EDGE_CURVE('',#20529,#20528,#3568,.T.) ;
#25312 = EDGE_CURVE('',#20530,#20529,#17600,.T.) ;
#25313 = EDGE_CURVE('',#20531,#20530,#3569,.T.) ;
#25314 = EDGE_CURVE('',#20532,#20531,#17601,.T.) ;
#25315 = EDGE_CURVE('',#20533,#20532,#3570,.T.) ;
#25316 = EDGE_CURVE('',#20534,#20533,#17602,.T.) ;
#25317 = EDGE_CURVE('',#20535,#20534,#3571,.T.) ;
#25318 = EDGE_CURVE('',#20536,#20535,#17603,.T.) ;
#25319 = EDGE_CURVE('',#20537,#20536,#3572,.T.) ;
#25320 = EDGE_CURVE('',#20538,#20537,#17604,.T.) ;
#25321 = EDGE_CURVE('',#20539,#20538,#3573,.T.) ;
#25322 = EDGE_CURVE('',#20540,#20539,#17605,.T.) ;
#25323 = EDGE_CURVE('',#20541,#20540,#3574,.T.) ;
#25324 = EDGE_CURVE('',#20542,#20541,#17606,.T.) ;
#25325 = EDGE_CURVE('',#20543,#20542,#3575,.T.) ;
#25326 = EDGE_CURVE('',#20544,#20543,#1096,.T.) ;
#25327 = EDGE_CURVE('',#20544,#20545,#3576,.T.) ;
#25328 = EDGE_CURVE('',#20546,#20545,#1097,.T.) ;
#25329 = EDGE_CURVE('',#20547,#20546,#3577,.T.) ;
#25330 = EDGE_CURVE('',#20548,#20547,#17607,.T.) ;
#25331 = EDGE_CURVE('',#20549,#20548,#3578,.T.) ;
#25332 = EDGE_CURVE('',#20550,#20549,#17608,.T.) ;
#25333 = EDGE_CURVE('',#20495,#20550,#3579,.T.) ;
#25334 = EDGE_CURVE('',#20551,#20551,#17609,.T.) ;
#25335 = EDGE_CURVE('',#20552,#20553,#3580,.T.) ;
#25336 = EDGE_CURVE('',#20554,#20552,#3581,.T.) ;
#25337 = EDGE_CURVE('',#20555,#20554,#17610,.T.) ;
#25338 = EDGE_CURVE('',#20556,#20555,#3582,.T.) ;
#25339 = EDGE_CURVE('',#20557,#20556,#17611,.T.) ;
#25340 = EDGE_CURVE('',#20558,#20557,#3583,.T.) ;
#25341 = EDGE_CURVE('',#20559,#20558,#3584,.T.) ;
#25342 = EDGE_CURVE('',#20560,#20559,#17612,.T.) ;
#25343 = EDGE_CURVE('',#20561,#20560,#3585,.T.) ;
#25344 = EDGE_CURVE('',#20562,#20561,#17613,.T.) ;
#25345 = EDGE_CURVE('',#20563,#20562,#3586,.T.) ;
#25346 = EDGE_CURVE('',#20564,#20563,#17614,.T.) ;
#25347 = EDGE_CURVE('',#20565,#20564,#3587,.T.) ;
#25348 = EDGE_CURVE('',#20553,#20565,#17615,.T.) ;
#25349 = EDGE_CURVE('',#20566,#20566,#17616,.T.) ;
#25350 = EDGE_CURVE('',#20567,#20567,#17617,.T.) ;
#25351 = EDGE_CURVE('',#20568,#20569,#3588,.T.) ;
#25352 = EDGE_CURVE('',#20570,#20568,#3589,.T.) ;
#25353 = EDGE_CURVE('',#20571,#20570,#17618,.T.) ;
#25354 = EDGE_CURVE('',#20572,#20571,#3590,.T.) ;
#25355 = EDGE_CURVE('',#20573,#20572,#17619,.T.) ;
#25356 = EDGE_CURVE('',#20574,#20573,#3591,.T.) ;
#25357 = EDGE_CURVE('',#20575,#20574,#17620,.T.) ;
#25358 = EDGE_CURVE('',#20576,#20575,#3592,.T.) ;
#25359 = EDGE_CURVE('',#20577,#20576,#17621,.T.) ;
#25360 = EDGE_CURVE('',#20578,#20577,#3593,.T.) ;
#25361 = EDGE_CURVE('',#20579,#20578,#17622,.T.) ;
#25362 = EDGE_CURVE('',#20580,#20579,#3594,.T.) ;
#25363 = EDGE_CURVE('',#20581,#20580,#17623,.T.) ;
#25364 = EDGE_CURVE('',#20582,#20581,#3595,.T.) ;
#25365 = EDGE_CURVE('',#20583,#20582,#3596,.T.) ;
#25366 = EDGE_CURVE('',#20583,#20569,#3597,.T.) ;
#25367 = EDGE_CURVE('',#20584,#20584,#17624,.T.) ;
#25368 = EDGE_CURVE('',#20585,#20586,#3598,.T.) ;
#25369 = EDGE_CURVE('',#20587,#20586,#17625,.T.) ;
#25370 = EDGE_CURVE('',#20588,#20587,#3599,.T.) ;
#25371 = EDGE_CURVE('',#20589,#20588,#17626,.T.) ;
#25372 = EDGE_CURVE('',#20589,#20590,#3600,.T.) ;
#25373 = EDGE_CURVE('',#20591,#20590,#17627,.T.) ;
#25374 = EDGE_CURVE('',#20592,#20591,#3601,.T.) ;
#25375 = EDGE_CURVE('',#20593,#20592,#17628,.T.) ;
#25376 = EDGE_CURVE('',#20593,#20594,#3602,.T.) ;
#25377 = EDGE_CURVE('',#20595,#20594,#17629,.T.) ;
#25378 = EDGE_CURVE('',#20595,#20596,#3603,.T.) ;
#25379 = EDGE_CURVE('',#20596,#20597,#3604,.T.) ;
#25380 = EDGE_CURVE('',#20597,#20598,#3605,.T.) ;
#25381 = EDGE_CURVE('',#20585,#20598,#17630,.T.) ;
#25382 = EDGE_CURVE('',#20599,#20600,#17631,.T.) ;
#25383 = EDGE_CURVE('',#20601,#20599,#3606,.T.) ;
#25384 = EDGE_CURVE('',#20602,#20601,#17632,.T.) ;
#25385 = EDGE_CURVE('',#20603,#20602,#3607,.T.) ;
#25386 = EDGE_CURVE('',#20604,#20603,#17633,.T.) ;
#25387 = EDGE_CURVE('',#20605,#20604,#3608,.T.) ;
#25388 = EDGE_CURVE('',#20606,#20605,#17634,.T.) ;
#25389 = EDGE_CURVE('',#20600,#20606,#3609,.T.) ;
#25390 = EDGE_CURVE('',#20607,#20608,#3610,.T.) ;
#25391 = EDGE_CURVE('',#20608,#20609,#3611,.T.) ;
#25392 = EDGE_CURVE('',#20609,#20610,#3612,.T.) ;
#25393 = EDGE_CURVE('',#20611,#20610,#1098,.T.) ;
#25394 = EDGE_CURVE('',#20612,#20611,#3613,.T.) ;
#25395 = EDGE_CURVE('',#20613,#20612,#17635,.T.) ;
#25396 = EDGE_CURVE('',#20614,#20613,#3614,.T.) ;
#25397 = EDGE_CURVE('',#20615,#20614,#17636,.T.) ;
#25398 = EDGE_CURVE('',#20616,#20615,#3615,.T.) ;
#25399 = EDGE_CURVE('',#20617,#20616,#17637,.T.) ;
#25400 = EDGE_CURVE('',#20618,#20617,#3616,.T.) ;
#25401 = EDGE_CURVE('',#20619,#20618,#17638,.T.) ;
#25402 = EDGE_CURVE('',#20620,#20619,#3617,.T.) ;
#25403 = EDGE_CURVE('',#20607,#20620,#1099,.T.) ;
#25404 = EDGE_CURVE('',#20621,#20622,#3618,.T.) ;
#25405 = EDGE_CURVE('',#20623,#20622,#1100,.T.) ;
#25406 = EDGE_CURVE('',#20624,#20623,#3619,.T.) ;
#25407 = EDGE_CURVE('',#20625,#20624,#3620,.T.) ;
#25408 = EDGE_CURVE('',#20626,#20625,#17639,.T.) ;
#25409 = EDGE_CURVE('',#20627,#20626,#3621,.T.) ;
#25410 = EDGE_CURVE('',#20628,#20627,#17640,.T.) ;
#25411 = EDGE_CURVE('',#20629,#20628,#3622,.T.) ;
#25412 = EDGE_CURVE('',#20630,#20629,#17641,.T.) ;
#25413 = EDGE_CURVE('',#20631,#20630,#3623,.T.) ;
#25414 = EDGE_CURVE('',#20632,#20631,#17642,.T.) ;
#25415 = EDGE_CURVE('',#20633,#20632,#3624,.T.) ;
#25416 = EDGE_CURVE('',#20634,#20633,#3625,.T.) ;
#25417 = EDGE_CURVE('',#20621,#20634,#1101,.T.) ;
#25418 = EDGE_CURVE('',#20635,#20636,#17643,.T.) ;
#25419 = EDGE_CURVE('',#20637,#20635,#3626,.T.) ;
#25420 = EDGE_CURVE('',#20638,#20637,#17644,.T.) ;
#25421 = EDGE_CURVE('',#20639,#20638,#3627,.T.) ;
#25422 = EDGE_CURVE('',#20640,#20639,#17645,.T.) ;
#25423 = EDGE_CURVE('',#20641,#20640,#3628,.T.) ;
#25424 = EDGE_CURVE('',#20642,#20641,#17646,.T.) ;
#25425 = EDGE_CURVE('',#20643,#20642,#3629,.T.) ;
#25426 = EDGE_CURVE('',#20644,#20643,#3630,.T.) ;
#25427 = EDGE_CURVE('',#20645,#20644,#17647,.T.) ;
#25428 = EDGE_CURVE('',#20646,#20645,#3631,.T.) ;
#25429 = EDGE_CURVE('',#20647,#20646,#17648,.T.) ;
#25430 = EDGE_CURVE('',#20648,#20647,#3632,.T.) ;
#25431 = EDGE_CURVE('',#20636,#20648,#3633,.T.) ;
#25432 = EDGE_CURVE('',#20649,#20650,#17649,.T.) ;
#25433 = EDGE_CURVE('',#20651,#20649,#3634,.T.) ;
#25434 = EDGE_CURVE('',#20652,#20651,#17650,.T.) ;
#25435 = EDGE_CURVE('',#20653,#20652,#3635,.T.) ;
#25436 = EDGE_CURVE('',#20654,#20653,#17651,.T.) ;
#25437 = EDGE_CURVE('',#20655,#20654,#3636,.T.) ;
#25438 = EDGE_CURVE('',#20656,#20655,#17652,.T.) ;
#25439 = EDGE_CURVE('',#20657,#20656,#3637,.T.) ;
#25440 = EDGE_CURVE('',#20658,#20657,#3638,.T.) ;
#25441 = EDGE_CURVE('',#20659,#20658,#17653,.T.) ;
#25442 = EDGE_CURVE('',#20660,#20659,#3639,.T.) ;
#25443 = EDGE_CURVE('',#20661,#20660,#17654,.T.) ;
#25444 = EDGE_CURVE('',#20662,#20661,#3640,.T.) ;
#25445 = EDGE_CURVE('',#20650,#20662,#3641,.T.) ;
#25446 = EDGE_CURVE('',#20663,#20663,#1102,.T.) ;
#25447 = EDGE_CURVE('',#20664,#20665,#17655,.T.) ;
#25448 = EDGE_CURVE('',#20495,#20665,#17656,.T.) ;
#25449 = EDGE_CURVE('',#20495,#20666,#17657,.T.) ;
#25450 = EDGE_CURVE('',#20666,#20664,#17658,.T.) ;
#25451 = EDGE_CURVE('',#20667,#20668,#17659,.T.) ;
#25452 = EDGE_CURVE('',#20668,#20665,#3642,.T.) ;
#25453 = EDGE_CURVE('',#20664,#20667,#3643,.T.) ;
#25454 = EDGE_CURVE('',#20669,#20670,#17660,.T.) ;
#25455 = EDGE_CURVE('',#20670,#20668,#17661,.T.) ;
#25456 = EDGE_CURVE('',#20667,#20669,#17662,.T.) ;
#25457 = EDGE_CURVE('',#20671,#20672,#17663,.T.) ;
#25458 = EDGE_CURVE('',#20672,#20670,#3644,.T.) ;
#25459 = EDGE_CURVE('',#20669,#20671,#3645,.T.) ;
#25460 = EDGE_CURVE('',#20673,#20674,#17664,.T.) ;
#25461 = EDGE_CURVE('',#20674,#20672,#17665,.T.) ;
#25462 = EDGE_CURVE('',#20671,#20673,#17666,.T.) ;
#25463 = EDGE_CURVE('',#20675,#20676,#17667,.T.) ;
#25464 = EDGE_CURVE('',#20676,#20674,#3646,.T.) ;
#25465 = EDGE_CURVE('',#20673,#20675,#3647,.T.) ;
#25466 = EDGE_CURVE('',#20677,#20678,#17668,.T.) ;
#25467 = EDGE_CURVE('',#20678,#20676,#17669,.T.) ;
#25468 = EDGE_CURVE('',#20675,#20677,#17670,.T.) ;
#25469 = EDGE_CURVE('',#20679,#20680,#17671,.T.) ;
#25470 = EDGE_CURVE('',#20680,#20678,#3648,.T.) ;
#25471 = EDGE_CURVE('',#20677,#20679,#3649,.T.) ;
#25472 = EDGE_CURVE('',#20681,#20682,#17672,.T.) ;
#25473 = EDGE_CURVE('',#20682,#20680,#17673,.T.) ;
#25474 = EDGE_CURVE('',#20679,#20681,#17674,.T.) ;
#25475 = EDGE_CURVE('',#20683,#20684,#17675,.T.) ;
#25476 = EDGE_CURVE('',#20684,#20682,#3650,.T.) ;
#25477 = EDGE_CURVE('',#20681,#20683,#3651,.T.) ;
#25478 = EDGE_CURVE('',#20685,#20686,#17676,.T.) ;
#25479 = EDGE_CURVE('',#20686,#20684,#17677,.T.) ;
#25480 = EDGE_CURVE('',#20683,#20685,#17678,.T.) ;
#25481 = EDGE_CURVE('',#20687,#20688,#17679,.T.) ;
#25482 = EDGE_CURVE('',#20688,#20686,#3652,.T.) ;
#25483 = EDGE_CURVE('',#20685,#20687,#3653,.T.) ;
#25484 = EDGE_CURVE('',#20687,#20689,#17680,.T.) ;
#25485 = EDGE_CURVE('',#20689,#20518,#17681,.T.) ;
#25486 = EDGE_CURVE('',#20688,#20518,#17682,.T.) ;
#25487 = EDGE_CURVE('',#20690,#20685,#3654,.T.) ;
#25488 = EDGE_CURVE('',#20691,#20690,#3655,.T.) ;
#25489 = EDGE_CURVE('',#20692,#20691,#17683,.T.) ;
#25490 = EDGE_CURVE('',#20693,#20692,#3656,.T.) ;
#25491 = EDGE_CURVE('',#20694,#20693,#3657,.T.) ;
#25492 = EDGE_CURVE('',#20689,#20694,#3658,.T.) ;
#25493 = EDGE_CURVE('',#20683,#20695,#3659,.T.) ;
#25494 = EDGE_CURVE('',#20690,#20695,#17684,.T.) ;
#25495 = EDGE_CURVE('',#20696,#20681,#3660,.T.) ;
#25496 = EDGE_CURVE('',#20695,#20696,#3661,.T.) ;
#25497 = EDGE_CURVE('',#20679,#20697,#3662,.T.) ;
#25498 = EDGE_CURVE('',#20696,#20697,#17685,.T.) ;
#25499 = EDGE_CURVE('',#20677,#20698,#3663,.T.) ;
#25500 = EDGE_CURVE('',#20697,#20698,#3664,.T.) ;
#25501 = EDGE_CURVE('',#20675,#20699,#3665,.T.) ;
#25502 = EDGE_CURVE('',#20698,#20699,#17686,.T.) ;
#25503 = EDGE_CURVE('',#20700,#20673,#3666,.T.) ;
#25504 = EDGE_CURVE('',#20699,#20700,#3667,.T.) ;
#25505 = EDGE_CURVE('',#20671,#20701,#3668,.T.) ;
#25506 = EDGE_CURVE('',#20700,#20701,#17687,.T.) ;
#25507 = EDGE_CURVE('',#20702,#20669,#3669,.T.) ;
#25508 = EDGE_CURVE('',#20701,#20702,#3670,.T.) ;
#25509 = EDGE_CURVE('',#20667,#20703,#3671,.T.) ;
#25510 = EDGE_CURVE('',#20702,#20703,#17688,.T.) ;
#25511 = EDGE_CURVE('',#20704,#20666,#3672,.T.) ;
#25512 = EDGE_CURVE('',#20705,#20704,#3673,.T.) ;
#25513 = EDGE_CURVE('',#20706,#20705,#3674,.T.) ;
#25514 = EDGE_CURVE('',#20707,#20706,#17689,.T.) ;
#25515 = EDGE_CURVE('',#20703,#20707,#3675,.T.) ;
#25516 = EDGE_CURVE('',#20551,#20708,#17690,.T.) ;
#25517 = EDGE_CURVE('',#20708,#20708,#17691,.T.) ;
#25518 = EDGE_CURVE('',#20708,#20709,#3676,.T.) ;
#25519 = EDGE_CURVE('',#20709,#20709,#17692,.T.) ;
#25520 = EDGE_CURVE('',#20663,#20710,#1103,.T.) ;
#25521 = EDGE_CURVE('',#20710,#20711,#1104,.T.) ;
#25522 = EDGE_CURVE('',#20711,#20710,#3677,.T.) ;
#25523 = EDGE_CURVE('',#20711,#20712,#17693,.T.) ;
#25524 = EDGE_CURVE('',#20712,#20712,#17694,.T.) ;
#25525 = EDGE_CURVE('',#20713,#20713,#17695,.T.) ;
#25526 = EDGE_CURVE('',#20714,#20715,#17696,.T.) ;
#25527 = EDGE_CURVE('',#20715,#20713,#17697,.T.) ;
#25528 = EDGE_CURVE('',#20715,#20714,#17698,.T.) ;
#25529 = EDGE_CURVE('',#20714,#20716,#3678,.T.) ;
#25530 = EDGE_CURVE('',#20716,#20716,#17699,.T.) ;
#25531 = EDGE_CURVE('',#20717,#20717,#17700,.T.) ;
#25532 = EDGE_CURVE('',#20717,#20718,#17701,.T.) ;
#25533 = EDGE_CURVE('',#20718,#20719,#17702,.T.) ;
#25534 = EDGE_CURVE('',#20719,#20718,#17703,.T.) ;
#25535 = EDGE_CURVE('',#20719,#20720,#3679,.T.) ;
#25536 = EDGE_CURVE('',#20721,#20720,#17704,.T.) ;
#25537 = EDGE_CURVE('',#20720,#20721,#17705,.T.) ;
#25538 = EDGE_CURVE('',#20722,#20723,#3680,.T.) ;
#25539 = EDGE_CURVE('',#20724,#20722,#3681,.T.) ;
#25540 = EDGE_CURVE('',#20725,#20724,#215,.T.) ;
#25541 = EDGE_CURVE('',#20725,#20726,#3682,.T.) ;
#25542 = EDGE_CURVE('',#20727,#20726,#216,.T.) ;
#25543 = EDGE_CURVE('',#20723,#20727,#3683,.T.) ;
#25544 = EDGE_CURVE('',#20728,#20728,#17706,.T.) ;
#25545 = EDGE_CURVE('',#20728,#20721,#17707,.T.) ;
#25546 = EDGE_CURVE('',#20729,#20730,#1105,.T.) ;
#25547 = EDGE_CURVE('',#20730,#20516,#3684,.T.) ;
#25548 = EDGE_CURVE('',#20515,#20731,#3685,.T.) ;
#25549 = EDGE_CURVE('',#20731,#20732,#1106,.T.) ;
#25550 = EDGE_CURVE('',#20729,#20732,#3686,.T.) ;
#25551 = EDGE_CURVE('',#20733,#20733,#17708,.T.) ;
#25552 = EDGE_CURVE('',#20733,#20734,#17709,.T.) ;
#25553 = EDGE_CURVE('',#20734,#20735,#17710,.T.) ;
#25554 = EDGE_CURVE('',#20735,#20734,#17711,.T.) ;
#25555 = EDGE_CURVE('',#20735,#20736,#3687,.T.) ;
#25556 = EDGE_CURVE('',#20737,#20736,#17712,.T.) ;
#25557 = EDGE_CURVE('',#20736,#20737,#17713,.T.) ;
#25558 = EDGE_CURVE('',#20738,#20739,#3688,.T.) ;
#25559 = EDGE_CURVE('',#20740,#20738,#3689,.T.) ;
#25560 = EDGE_CURVE('',#20741,#20740,#217,.T.) ;
#25561 = EDGE_CURVE('',#20741,#20742,#3690,.T.) ;
#25562 = EDGE_CURVE('',#20743,#20742,#218,.T.) ;
#25563 = EDGE_CURVE('',#20739,#20743,#3691,.T.) ;
#25564 = EDGE_CURVE('',#20744,#20744,#17714,.T.) ;
#25565 = EDGE_CURVE('',#20744,#20737,#17715,.T.) ;
#25566 = EDGE_CURVE('',#20745,#20746,#1107,.T.) ;
#25567 = EDGE_CURVE('',#20747,#20746,#3692,.T.) ;
#25568 = EDGE_CURVE('',#20747,#20748,#1108,.T.) ;
#25569 = EDGE_CURVE('',#20748,#20510,#3693,.T.) ;
#25570 = EDGE_CURVE('',#20509,#20745,#3694,.T.) ;
#25571 = EDGE_CURVE('',#20701,#20749,#17716,.T.) ;
#25572 = EDGE_CURVE('',#20749,#20750,#17717,.T.) ;
#25573 = EDGE_CURVE('',#20750,#20700,#17718,.T.) ;
#25574 = EDGE_CURVE('',#20751,#20699,#17719,.T.) ;
#25575 = EDGE_CURVE('',#20750,#20751,#3695,.T.) ;
#25576 = EDGE_CURVE('',#20752,#20698,#17720,.T.) ;
#25577 = EDGE_CURVE('',#20751,#20752,#17721,.T.) ;
#25578 = EDGE_CURVE('',#20753,#20697,#17722,.T.) ;
#25579 = EDGE_CURVE('',#20752,#20753,#3696,.T.) ;
#25580 = EDGE_CURVE('',#20754,#20696,#17723,.T.) ;
#25581 = EDGE_CURVE('',#20753,#20754,#17724,.T.) ;
#25582 = EDGE_CURVE('',#20755,#20749,#3697,.T.) ;
#25583 = EDGE_CURVE('',#20756,#20755,#17725,.T.) ;
#25584 = EDGE_CURVE('',#20757,#20756,#3698,.T.) ;
#25585 = EDGE_CURVE('',#20758,#20757,#3699,.T.) ;
#25586 = EDGE_CURVE('',#20759,#20758,#3700,.T.) ;
#25587 = EDGE_CURVE('',#20742,#20759,#1109,.T.) ;
#25588 = EDGE_CURVE('',#20760,#20741,#1110,.T.) ;
#25589 = EDGE_CURVE('',#20761,#20760,#3701,.T.) ;
#25590 = EDGE_CURVE('',#20762,#20761,#3702,.T.) ;
#25591 = EDGE_CURVE('',#20763,#20762,#3703,.T.) ;
#25592 = EDGE_CURVE('',#20726,#20763,#1111,.T.) ;
#25593 = EDGE_CURVE('',#20764,#20725,#1112,.T.) ;
#25594 = EDGE_CURVE('',#20765,#20764,#3704,.T.) ;
#25595 = EDGE_CURVE('',#20766,#20765,#3705,.T.) ;
#25596 = EDGE_CURVE('',#20767,#20766,#3706,.T.) ;
#25597 = EDGE_CURVE('',#20768,#20767,#17726,.T.) ;
#25598 = EDGE_CURVE('',#20754,#20768,#3707,.T.) ;
#25599 = EDGE_CURVE('',#20755,#20702,#17727,.T.) ;
#25600 = EDGE_CURVE('',#20769,#20688,#3708,.T.) ;
#25601 = EDGE_CURVE('',#20770,#20769,#219,.T.) ;
#25602 = EDGE_CURVE('',#20770,#20729,#1113,.T.) ;
#25603 = EDGE_CURVE('',#20732,#20771,#1114,.T.) ;
#25604 = EDGE_CURVE('',#20772,#20771,#220,.T.) ;
#25605 = EDGE_CURVE('',#20513,#20772,#3709,.T.) ;
#25606 = EDGE_CURVE('',#20512,#20773,#3710,.T.) ;
#25607 = EDGE_CURVE('',#20774,#20773,#221,.T.) ;
#25608 = EDGE_CURVE('',#20774,#20747,#1115,.T.) ;
#25609 = EDGE_CURVE('',#20746,#20775,#1116,.T.) ;
#25610 = EDGE_CURVE('',#20776,#20775,#222,.T.) ;
#25611 = EDGE_CURVE('',#20777,#20776,#3711,.T.) ;
#25612 = EDGE_CURVE('',#20778,#20777,#223,.T.) ;
#25613 = EDGE_CURVE('',#20779,#20778,#1117,.T.) ;
#25614 = EDGE_CURVE('',#20780,#20779,#3712,.T.) ;
#25615 = EDGE_CURVE('',#20781,#20780,#1118,.T.) ;
#25616 = EDGE_CURVE('',#20665,#20781,#3713,.T.) ;
#25617 = EDGE_CURVE('',#20768,#20695,#17728,.T.) ;
#25618 = EDGE_CURVE('',#20508,#20776,#1119,.T.) ;
#25619 = EDGE_CURVE('',#20507,#20777,#17729,.T.) ;
#25620 = EDGE_CURVE('',#20782,#20778,#17730,.T.) ;
#25621 = EDGE_CURVE('',#20507,#20782,#224,.T.) ;
#25622 = EDGE_CURVE('',#20783,#20779,#17731,.T.) ;
#25623 = EDGE_CURVE('',#20782,#20783,#1120,.T.) ;
#25624 = EDGE_CURVE('',#20784,#20780,#17732,.T.) ;
#25625 = EDGE_CURVE('',#20783,#20784,#3714,.T.) ;
#25626 = EDGE_CURVE('',#20494,#20781,#17733,.T.) ;
#25627 = EDGE_CURVE('',#20784,#20494,#1121,.T.) ;
#25628 = EDGE_CURVE('',#20550,#20704,#17734,.T.) ;
#25629 = EDGE_CURVE('',#20785,#20784,#17735,.T.) ;
#25630 = EDGE_CURVE('',#20785,#20786,#17736,.T.) ;
#25631 = EDGE_CURVE('',#20786,#20496,#17737,.T.) ;
#25632 = EDGE_CURVE('',#20787,#20783,#17738,.T.) ;
#25633 = EDGE_CURVE('',#20787,#20785,#3715,.T.) ;
#25634 = EDGE_CURVE('',#20788,#20782,#17739,.T.) ;
#25635 = EDGE_CURVE('',#20788,#20787,#17740,.T.) ;
#25636 = EDGE_CURVE('',#20789,#20506,#17741,.T.) ;
#25637 = EDGE_CURVE('',#20789,#20788,#3716,.T.) ;
#25638 = EDGE_CURVE('',#20769,#20517,#1122,.T.) ;
#25639 = EDGE_CURVE('',#20770,#20730,#1123,.T.) ;
#25640 = EDGE_CURVE('',#20399,#20790,#17742,.F.) ;
#25641 = EDGE_CURVE('',#20791,#20399,#17743,.F.) ;
#25642 = EDGE_CURVE('',#20790,#20791,#17744,.F.) ;
#25643 = EDGE_CURVE('',#20397,#20792,#17745,.T.) ;
#25644 = EDGE_CURVE('',#20792,#20791,#3717,.T.) ;
#25645 = EDGE_CURVE('',#20398,#20793,#17746,.T.) ;
#25646 = EDGE_CURVE('',#20792,#20793,#17747,.T.) ;
#25647 = EDGE_CURVE('',#20794,#20795,#17748,.T.) ;
#25648 = EDGE_CURVE('',#20795,#20624,#17749,.T.) ;
#25649 = EDGE_CURVE('',#20624,#20794,#17750,.T.) ;
#25650 = EDGE_CURVE('',#20794,#20790,#3718,.T.) ;
#25651 = EDGE_CURVE('',#20791,#20795,#3719,.T.) ;
#25652 = EDGE_CURVE('',#20796,#20402,#17751,.T.) ;
#25653 = EDGE_CURVE('',#20797,#20796,#17752,.F.) ;
#25654 = EDGE_CURVE('',#20403,#20797,#17753,.T.) ;
#25655 = EDGE_CURVE('',#20798,#20799,#17754,.F.) ;
#25656 = EDGE_CURVE('',#20401,#20798,#17755,.T.) ;
#25657 = EDGE_CURVE('',#20799,#20400,#17756,.T.) ;
#25658 = EDGE_CURVE('',#20798,#20796,#3720,.T.) ;
#25659 = EDGE_CURVE('',#20790,#20799,#3721,.T.) ;
#25660 = EDGE_CURVE('',#20800,#20801,#17757,.T.) ;
#25661 = EDGE_CURVE('',#20801,#20623,#17758,.T.) ;
#25662 = EDGE_CURVE('',#20622,#20800,#17759,.T.) ;
#25663 = EDGE_CURVE('',#20799,#20801,#3722,.T.) ;
#25664 = EDGE_CURVE('',#20800,#20798,#3723,.T.) ;
#25665 = EDGE_CURVE('',#20802,#20803,#17760,.T.) ;
#25666 = EDGE_CURVE('',#20803,#20797,#3724,.T.) ;
#25667 = EDGE_CURVE('',#20796,#20802,#3725,.T.) ;
#25668 = EDGE_CURVE('',#20634,#20803,#17761,.T.) ;
#25669 = EDGE_CURVE('',#20802,#20621,#17762,.T.) ;
#25670 = EDGE_CURVE('',#20804,#20404,#17763,.T.) ;
#25671 = EDGE_CURVE('',#20797,#20804,#3726,.T.) ;
#25672 = EDGE_CURVE('',#20804,#20805,#17764,.T.) ;
#25673 = EDGE_CURVE('',#20805,#20404,#17765,.T.) ;
#25674 = EDGE_CURVE('',#20795,#20806,#3727,.T.) ;
#25675 = EDGE_CURVE('',#20806,#20625,#17766,.T.) ;
#25676 = EDGE_CURVE('',#20806,#20792,#3728,.T.) ;
#25677 = EDGE_CURVE('',#20805,#20807,#3729,.T.) ;
#25678 = EDGE_CURVE('',#20807,#20405,#17767,.T.) ;
#25679 = EDGE_CURVE('',#20804,#20808,#3730,.T.) ;
#25680 = EDGE_CURVE('',#20809,#20808,#17768,.T.) ;
#25681 = EDGE_CURVE('',#20809,#20805,#3731,.T.) ;
#25682 = EDGE_CURVE('',#20808,#20803,#3732,.T.) ;
#25683 = EDGE_CURVE('',#20810,#20811,#17769,.T.) ;
#25684 = EDGE_CURVE('',#20811,#20611,#17770,.T.) ;
#25685 = EDGE_CURVE('',#20610,#20810,#17771,.T.) ;
#25686 = EDGE_CURVE('',#20812,#20813,#17772,.T.) ;
#25687 = EDGE_CURVE('',#20813,#20811,#3733,.T.) ;
#25688 = EDGE_CURVE('',#20810,#20812,#3734,.T.) ;
#25689 = EDGE_CURVE('',#20812,#20454,#225,.T.) ;
#25690 = EDGE_CURVE('',#20454,#20813,#226,.T.) ;
#25691 = EDGE_CURVE('',#20812,#20814,#3735,.T.) ;
#25692 = EDGE_CURVE('',#20455,#20814,#227,.F.) ;
#25693 = EDGE_CURVE('',#20609,#20814,#3736,.T.) ;
#25694 = EDGE_CURVE('',#20815,#20816,#17773,.T.) ;
#25695 = EDGE_CURVE('',#20816,#20445,#228,.T.) ;
#25696 = EDGE_CURVE('',#20445,#20815,#229,.T.) ;
#25697 = EDGE_CURVE('',#20817,#20818,#17774,.T.) ;
#25698 = EDGE_CURVE('',#20818,#20816,#3737,.T.) ;
#25699 = EDGE_CURVE('',#20815,#20817,#3738,.T.) ;
#25700 = EDGE_CURVE('',#20620,#20818,#17775,.T.) ;
#25701 = EDGE_CURVE('',#20817,#20607,#17776,.T.) ;
#25702 = EDGE_CURVE('',#20819,#20815,#3739,.T.) ;
#25703 = EDGE_CURVE('',#20819,#20608,#3740,.T.) ;
#25704 = EDGE_CURVE('',#20443,#20819,#230,.T.) ;
#25705 = EDGE_CURVE('',#20820,#20501,#17777,.T.) ;
#25706 = EDGE_CURVE('',#20500,#20821,#17778,.F.) ;
#25707 = EDGE_CURVE('',#20821,#20820,#3741,.T.) ;
#25708 = EDGE_CURVE('',#20822,#20502,#17779,.T.) ;
#25709 = EDGE_CURVE('',#20820,#20822,#17780,.T.) ;
#25710 = EDGE_CURVE('',#20823,#20503,#17781,.T.) ;
#25711 = EDGE_CURVE('',#20822,#20823,#3742,.T.) ;
#25712 = EDGE_CURVE('',#20824,#20504,#17782,.T.) ;
#25713 = EDGE_CURVE('',#20823,#20824,#17783,.T.) ;
#25714 = EDGE_CURVE('',#20825,#20505,#17784,.T.) ;
#25715 = EDGE_CURVE('',#20824,#20825,#3743,.T.) ;
#25716 = EDGE_CURVE('',#20825,#20789,#17785,.T.) ;
#25717 = EDGE_CURVE('',#20497,#20826,#17786,.T.) ;
#25718 = EDGE_CURVE('',#20786,#20826,#3744,.T.) ;
#25719 = EDGE_CURVE('',#20827,#20786,#3745,.T.) ;
#25720 = EDGE_CURVE('',#20828,#20827,#3746,.T.) ;
#25721 = EDGE_CURVE('',#20828,#20826,#3747,.T.) ;
#25722 = EDGE_CURVE('',#20785,#20829,#3748,.T.) ;
#25723 = EDGE_CURVE('',#20829,#20827,#17787,.F.) ;
#25724 = EDGE_CURVE('',#20830,#20787,#3749,.T.) ;
#25725 = EDGE_CURVE('',#20829,#20830,#3750,.T.) ;
#25726 = EDGE_CURVE('',#20788,#20831,#3751,.T.) ;
#25727 = EDGE_CURVE('',#20831,#20830,#17788,.F.) ;
#25728 = EDGE_CURVE('',#20832,#20789,#3752,.T.) ;
#25729 = EDGE_CURVE('',#20831,#20832,#3753,.T.) ;
#25730 = EDGE_CURVE('',#20825,#20833,#3754,.T.) ;
#25731 = EDGE_CURVE('',#20833,#20832,#17789,.F.) ;
#25732 = EDGE_CURVE('',#20834,#20824,#3755,.T.) ;
#25733 = EDGE_CURVE('',#20833,#20834,#3756,.T.) ;
#25734 = EDGE_CURVE('',#20823,#20835,#3757,.T.) ;
#25735 = EDGE_CURVE('',#20835,#20834,#17790,.F.) ;
#25736 = EDGE_CURVE('',#20836,#20822,#3758,.T.) ;
#25737 = EDGE_CURVE('',#20835,#20836,#3759,.T.) ;
#25738 = EDGE_CURVE('',#20820,#20837,#3760,.T.) ;
#25739 = EDGE_CURVE('',#20837,#20836,#17791,.F.) ;
#25740 = EDGE_CURVE('',#20821,#20838,#3761,.T.) ;
#25741 = EDGE_CURVE('',#20837,#20838,#3762,.T.) ;
#25742 = EDGE_CURVE('',#20553,#20839,#17792,.T.) ;
#25743 = EDGE_CURVE('',#20839,#20840,#3763,.T.) ;
#25744 = EDGE_CURVE('',#20840,#20552,#17793,.T.) ;
#25745 = EDGE_CURVE('',#20565,#20841,#17794,.T.) ;
#25746 = EDGE_CURVE('',#20841,#20839,#17795,.T.) ;
#25747 = EDGE_CURVE('',#20564,#20842,#17796,.T.) ;
#25748 = EDGE_CURVE('',#20842,#20841,#3764,.T.) ;
#25749 = EDGE_CURVE('',#20563,#20843,#17797,.T.) ;
#25750 = EDGE_CURVE('',#20843,#20842,#17798,.T.) ;
#25751 = EDGE_CURVE('',#20562,#20844,#17799,.T.) ;
#25752 = EDGE_CURVE('',#20844,#20843,#3765,.T.) ;
#25753 = EDGE_CURVE('',#20561,#20845,#17800,.T.) ;
#25754 = EDGE_CURVE('',#20845,#20844,#17801,.T.) ;
#25755 = EDGE_CURVE('',#20560,#20846,#17802,.T.) ;
#25756 = EDGE_CURVE('',#20846,#20845,#3766,.T.) ;
#25757 = EDGE_CURVE('',#20559,#20847,#17803,.T.) ;
#25758 = EDGE_CURVE('',#20847,#20846,#17804,.T.) ;
#25759 = EDGE_CURVE('',#20558,#20848,#17805,.T.) ;
#25760 = EDGE_CURVE('',#20848,#20847,#3767,.T.) ;
#25761 = EDGE_CURVE('',#20557,#20849,#17806,.T.) ;
#25762 = EDGE_CURVE('',#20849,#20850,#3768,.T.) ;
#25763 = EDGE_CURVE('',#20850,#20558,#17807,.T.) ;
#25764 = EDGE_CURVE('',#20556,#20851,#17808,.T.) ;
#25765 = EDGE_CURVE('',#20851,#20849,#17809,.T.) ;
#25766 = EDGE_CURVE('',#20555,#20852,#17810,.T.) ;
#25767 = EDGE_CURVE('',#20852,#20851,#3769,.T.) ;
#25768 = EDGE_CURVE('',#20554,#20853,#17811,.T.) ;
#25769 = EDGE_CURVE('',#20853,#20852,#17812,.T.) ;
#25770 = EDGE_CURVE('',#20552,#20854,#17813,.T.) ;
#25771 = EDGE_CURVE('',#20854,#20853,#3770,.T.) ;
#25772 = EDGE_CURVE('',#20850,#20848,#17814,.T.) ;
#25773 = EDGE_CURVE('',#20840,#20854,#17815,.T.) ;
#25774 = EDGE_CURVE('',#20843,#20855,#3771,.T.) ;
#25775 = EDGE_CURVE('',#20855,#20856,#17816,.F.) ;
#25776 = EDGE_CURVE('',#20856,#20842,#3772,.T.) ;
#25777 = EDGE_CURVE('',#20857,#20844,#3773,.T.) ;
#25778 = EDGE_CURVE('',#20855,#20857,#3774,.T.) ;
#25779 = EDGE_CURVE('',#20845,#20858,#3775,.T.) ;
#25780 = EDGE_CURVE('',#20858,#20857,#17817,.F.) ;
#25781 = EDGE_CURVE('',#20859,#20846,#3776,.T.) ;
#25782 = EDGE_CURVE('',#20858,#20859,#3777,.T.) ;
#25783 = EDGE_CURVE('',#20847,#20860,#3778,.T.) ;
#25784 = EDGE_CURVE('',#20860,#20859,#17818,.F.) ;
#25785 = EDGE_CURVE('',#20861,#20848,#3779,.T.) ;
#25786 = EDGE_CURVE('',#20860,#20861,#3780,.T.) ;
#25787 = EDGE_CURVE('',#20850,#20862,#3781,.T.) ;
#25788 = EDGE_CURVE('',#20862,#20861,#17819,.F.) ;
#25789 = EDGE_CURVE('',#20863,#20849,#3782,.T.) ;
#25790 = EDGE_CURVE('',#20862,#20863,#3783,.T.) ;
#25791 = EDGE_CURVE('',#20864,#20580,#17820,.T.) ;
#25792 = EDGE_CURVE('',#20865,#20864,#17821,.F.) ;
#25793 = EDGE_CURVE('',#20581,#20865,#17822,.T.) ;
#25794 = EDGE_CURVE('',#20866,#20867,#17823,.F.) ;
#25795 = EDGE_CURVE('',#20571,#20866,#17824,.T.) ;
#25796 = EDGE_CURVE('',#20867,#20570,#17825,.T.) ;
#25797 = EDGE_CURVE('',#20868,#20572,#17826,.T.) ;
#25798 = EDGE_CURVE('',#20866,#20868,#3784,.T.) ;
#25799 = EDGE_CURVE('',#20869,#20573,#17827,.T.) ;
#25800 = EDGE_CURVE('',#20868,#20869,#17828,.T.) ;
#25801 = EDGE_CURVE('',#20870,#20574,#17829,.T.) ;
#25802 = EDGE_CURVE('',#20869,#20870,#3785,.T.) ;
#25803 = EDGE_CURVE('',#20871,#20575,#17830,.T.) ;
#25804 = EDGE_CURVE('',#20870,#20871,#17831,.T.) ;
#25805 = EDGE_CURVE('',#20872,#20576,#17832,.T.) ;
#25806 = EDGE_CURVE('',#20871,#20872,#3786,.T.) ;
#25807 = EDGE_CURVE('',#20873,#20577,#17833,.T.) ;
#25808 = EDGE_CURVE('',#20872,#20873,#17834,.T.) ;
#25809 = EDGE_CURVE('',#20874,#20578,#17835,.T.) ;
#25810 = EDGE_CURVE('',#20873,#20874,#3787,.T.) ;
#25811 = EDGE_CURVE('',#20875,#20579,#17836,.T.) ;
#25812 = EDGE_CURVE('',#20874,#20875,#17837,.T.) ;
#25813 = EDGE_CURVE('',#20875,#20864,#3788,.T.) ;
#25814 = EDGE_CURVE('',#20568,#20876,#17838,.F.) ;
#25815 = EDGE_CURVE('',#20876,#20867,#3789,.T.) ;
#25816 = EDGE_CURVE('',#20877,#20878,#17839,.T.) ;
#25817 = EDGE_CURVE('',#20878,#20866,#3790,.T.) ;
#25818 = EDGE_CURVE('',#20867,#20877,#3791,.T.) ;
#25819 = EDGE_CURVE('',#20877,#20411,#231,.T.) ;
#25820 = EDGE_CURVE('',#20411,#20878,#232,.T.) ;
#25821 = EDGE_CURVE('',#20879,#20880,#17840,.T.) ;
#25822 = EDGE_CURVE('',#20880,#20865,#3792,.T.) ;
#25823 = EDGE_CURVE('',#20864,#20879,#3793,.T.) ;
#25824 = EDGE_CURVE('',#20879,#20416,#233,.T.) ;
#25825 = EDGE_CURVE('',#20416,#20880,#234,.T.) ;
#25826 = EDGE_CURVE('',#20582,#20881,#17841,.T.) ;
#25827 = EDGE_CURVE('',#20865,#20881,#3794,.T.) ;
#25828 = EDGE_CURVE('',#20876,#20882,#3795,.T.) ;
#25829 = EDGE_CURVE('',#20877,#20882,#3796,.T.) ;
#25830 = EDGE_CURVE('',#20650,#20883,#17842,.T.) ;
#25831 = EDGE_CURVE('',#20883,#20884,#17843,.T.) ;
#25832 = EDGE_CURVE('',#20884,#20649,#17844,.T.) ;
#25833 = EDGE_CURVE('',#20662,#20885,#17845,.T.) ;
#25834 = EDGE_CURVE('',#20885,#20883,#3797,.T.) ;
#25835 = EDGE_CURVE('',#20661,#20886,#17846,.T.) ;
#25836 = EDGE_CURVE('',#20886,#20887,#3798,.T.) ;
#25837 = EDGE_CURVE('',#20887,#20662,#17847,.T.) ;
#25838 = EDGE_CURVE('',#20660,#20888,#17848,.T.) ;
#25839 = EDGE_CURVE('',#20888,#20886,#17849,.T.) ;
#25840 = EDGE_CURVE('',#20659,#20889,#17850,.T.) ;
#25841 = EDGE_CURVE('',#20889,#20888,#3799,.T.) ;
#25842 = EDGE_CURVE('',#20658,#20890,#17851,.T.) ;
#25843 = EDGE_CURVE('',#20890,#20889,#17852,.T.) ;
#25844 = EDGE_CURVE('',#20657,#20891,#17853,.T.) ;
#25845 = EDGE_CURVE('',#20891,#20890,#3800,.T.) ;
#25846 = EDGE_CURVE('',#20887,#20885,#17854,.T.) ;
#25847 = EDGE_CURVE('',#20656,#20892,#17855,.T.) ;
#25848 = EDGE_CURVE('',#20892,#20893,#3801,.T.) ;
#25849 = EDGE_CURVE('',#20893,#20657,#17856,.T.) ;
#25850 = EDGE_CURVE('',#20655,#20894,#17857,.T.) ;
#25851 = EDGE_CURVE('',#20892,#20894,#17858,.T.) ;
#25852 = EDGE_CURVE('',#20893,#20891,#17859,.T.) ;
#25853 = EDGE_CURVE('',#20895,#20885,#3802,.T.) ;
#25854 = EDGE_CURVE('',#20896,#20895,#3803,.T.) ;
#25855 = EDGE_CURVE('',#20883,#20896,#3804,.T.) ;
#25856 = EDGE_CURVE('',#20887,#20897,#3805,.T.) ;
#25857 = EDGE_CURVE('',#20897,#20895,#17860,.F.) ;
#25858 = EDGE_CURVE('',#20898,#20886,#3806,.T.) ;
#25859 = EDGE_CURVE('',#20897,#20898,#3807,.T.) ;
#25860 = EDGE_CURVE('',#20888,#20899,#3808,.T.) ;
#25861 = EDGE_CURVE('',#20899,#20898,#17861,.F.) ;
#25862 = EDGE_CURVE('',#20900,#20889,#3809,.T.) ;
#25863 = EDGE_CURVE('',#20899,#20900,#3810,.T.) ;
#25864 = EDGE_CURVE('',#20890,#20901,#3811,.T.) ;
#25865 = EDGE_CURVE('',#20901,#20900,#17862,.F.) ;
#25866 = EDGE_CURVE('',#20902,#20891,#3812,.T.) ;
#25867 = EDGE_CURVE('',#20901,#20902,#3813,.T.) ;
#25868 = EDGE_CURVE('',#20893,#20903,#3814,.T.) ;
#25869 = EDGE_CURVE('',#20903,#20902,#17863,.F.) ;
#25870 = EDGE_CURVE('',#20904,#20892,#3815,.T.) ;
#25871 = EDGE_CURVE('',#20903,#20904,#3816,.T.) ;
#25872 = EDGE_CURVE('',#20636,#20905,#17864,.T.) ;
#25873 = EDGE_CURVE('',#20905,#20906,#17865,.T.) ;
#25874 = EDGE_CURVE('',#20906,#20635,#17866,.T.) ;
#25875 = EDGE_CURVE('',#20648,#20907,#17867,.T.) ;
#25876 = EDGE_CURVE('',#20907,#20905,#3817,.T.) ;
#25877 = EDGE_CURVE('',#20647,#20908,#17868,.T.) ;
#25878 = EDGE_CURVE('',#20908,#20909,#3818,.T.) ;
#25879 = EDGE_CURVE('',#20909,#20648,#17869,.T.) ;
#25880 = EDGE_CURVE('',#20646,#20910,#17870,.T.) ;
#25881 = EDGE_CURVE('',#20910,#20908,#17871,.T.) ;
#25882 = EDGE_CURVE('',#20645,#20911,#17872,.T.) ;
#25883 = EDGE_CURVE('',#20911,#20910,#3819,.T.) ;
#25884 = EDGE_CURVE('',#20644,#20912,#17873,.T.) ;
#25885 = EDGE_CURVE('',#20912,#20911,#17874,.T.) ;
#25886 = EDGE_CURVE('',#20643,#20913,#17875,.T.) ;
#25887 = EDGE_CURVE('',#20913,#20912,#3820,.T.) ;
#25888 = EDGE_CURVE('',#20909,#20907,#17876,.T.) ;
#25889 = EDGE_CURVE('',#20642,#20914,#17877,.T.) ;
#25890 = EDGE_CURVE('',#20914,#20915,#3821,.T.) ;
#25891 = EDGE_CURVE('',#20915,#20643,#17878,.T.) ;
#25892 = EDGE_CURVE('',#20641,#20916,#17879,.T.) ;
#25893 = EDGE_CURVE('',#20914,#20916,#17880,.T.) ;
#25894 = EDGE_CURVE('',#20915,#20913,#17881,.T.) ;
#25895 = EDGE_CURVE('',#20917,#20907,#3822,.T.) ;
#25896 = EDGE_CURVE('',#20918,#20917,#3823,.T.) ;
#25897 = EDGE_CURVE('',#20905,#20918,#3824,.T.) ;
#25898 = EDGE_CURVE('',#20909,#20919,#3825,.T.) ;
#25899 = EDGE_CURVE('',#20919,#20917,#17882,.F.) ;
#25900 = EDGE_CURVE('',#20920,#20908,#3826,.T.) ;
#25901 = EDGE_CURVE('',#20919,#20920,#3827,.T.) ;
#25902 = EDGE_CURVE('',#20910,#20921,#3828,.T.) ;
#25903 = EDGE_CURVE('',#20921,#20920,#17883,.F.) ;
#25904 = EDGE_CURVE('',#20922,#20911,#3829,.T.) ;
#25905 = EDGE_CURVE('',#20921,#20922,#3830,.T.) ;
#25906 = EDGE_CURVE('',#20912,#20923,#3831,.T.) ;
#25907 = EDGE_CURVE('',#20923,#20922,#17884,.F.) ;
#25908 = EDGE_CURVE('',#20924,#20913,#3832,.T.) ;
#25909 = EDGE_CURVE('',#20923,#20924,#3833,.T.) ;
#25910 = EDGE_CURVE('',#20915,#20925,#3834,.T.) ;
#25911 = EDGE_CURVE('',#20925,#20924,#17885,.F.) ;
#25912 = EDGE_CURVE('',#20926,#20914,#3835,.T.) ;
#25913 = EDGE_CURVE('',#20925,#20926,#3836,.T.) ;
#25914 = EDGE_CURVE('',#20633,#20808,#17886,.T.) ;
#25915 = EDGE_CURVE('',#20632,#20927,#17887,.T.) ;
#25916 = EDGE_CURVE('',#20927,#20809,#3837,.T.) ;
#25917 = EDGE_CURVE('',#20809,#20633,#17888,.T.) ;
#25918 = EDGE_CURVE('',#20631,#20928,#17889,.T.) ;
#25919 = EDGE_CURVE('',#20927,#20928,#17890,.T.) ;
#25920 = EDGE_CURVE('',#20807,#20927,#3838,.T.) ;
#25921 = EDGE_CURVE('',#20801,#20794,#3839,.T.) ;
#25922 = EDGE_CURVE('',#20806,#20929,#17891,.T.) ;
#25923 = EDGE_CURVE('',#20929,#20626,#17892,.T.) ;
#25924 = EDGE_CURVE('',#20811,#20930,#3840,.T.) ;
#25925 = EDGE_CURVE('',#20930,#20612,#17893,.T.) ;
#25926 = EDGE_CURVE('',#20931,#20613,#17894,.T.) ;
#25927 = EDGE_CURVE('',#20930,#20931,#17895,.T.) ;
#25928 = EDGE_CURVE('',#20932,#20614,#17896,.T.) ;
#25929 = EDGE_CURVE('',#20931,#20932,#3841,.T.) ;
#25930 = EDGE_CURVE('',#20933,#20615,#17897,.T.) ;
#25931 = EDGE_CURVE('',#20932,#20933,#17898,.T.) ;
#25932 = EDGE_CURVE('',#20934,#20616,#17899,.T.) ;
#25933 = EDGE_CURVE('',#20933,#20934,#3842,.T.) ;
#25934 = EDGE_CURVE('',#20935,#20617,#17900,.T.) ;
#25935 = EDGE_CURVE('',#20934,#20935,#17901,.T.) ;
#25936 = EDGE_CURVE('',#20936,#20618,#17902,.T.) ;
#25937 = EDGE_CURVE('',#20935,#20936,#3843,.T.) ;
#25938 = EDGE_CURVE('',#20937,#20619,#17903,.T.) ;
#25939 = EDGE_CURVE('',#20936,#20937,#17904,.T.) ;
#25940 = EDGE_CURVE('',#20937,#20818,#3844,.T.) ;
#25941 = EDGE_CURVE('',#20938,#20937,#3845,.T.) ;
#25942 = EDGE_CURVE('',#20816,#20938,#3846,.T.) ;
#25943 = EDGE_CURVE('',#20936,#20939,#3847,.T.) ;
#25944 = EDGE_CURVE('',#20939,#20938,#17905,.F.) ;
#25945 = EDGE_CURVE('',#20940,#20935,#3848,.T.) ;
#25946 = EDGE_CURVE('',#20939,#20940,#3849,.T.) ;
#25947 = EDGE_CURVE('',#20934,#20941,#3850,.T.) ;
#25948 = EDGE_CURVE('',#20941,#20940,#17906,.F.) ;
#25949 = EDGE_CURVE('',#20942,#20933,#3851,.T.) ;
#25950 = EDGE_CURVE('',#20941,#20942,#3852,.T.) ;
#25951 = EDGE_CURVE('',#20932,#20943,#3853,.T.) ;
#25952 = EDGE_CURVE('',#20943,#20942,#17907,.F.) ;
#25953 = EDGE_CURVE('',#20944,#20931,#3854,.T.) ;
#25954 = EDGE_CURVE('',#20943,#20944,#3855,.T.) ;
#25955 = EDGE_CURVE('',#20930,#20945,#3856,.T.) ;
#25956 = EDGE_CURVE('',#20945,#20944,#17908,.F.) ;
#25957 = EDGE_CURVE('',#20945,#20813,#3857,.T.) ;
#25958 = EDGE_CURVE('',#20793,#20929,#3858,.T.) ;
#25959 = EDGE_CURVE('',#20946,#20629,#17909,.T.) ;
#25960 = EDGE_CURVE('',#20946,#20947,#17910,.T.) ;
#25961 = EDGE_CURVE('',#20947,#20630,#17911,.T.) ;
#25962 = EDGE_CURVE('',#20948,#20946,#3859,.T.) ;
#25963 = EDGE_CURVE('',#20949,#20948,#3860,.T.) ;
#25964 = EDGE_CURVE('',#20950,#20949,#3861,.T.) ;
#25965 = EDGE_CURVE('',#20946,#20950,#3862,.T.) ;
#25966 = EDGE_CURVE('',#20951,#20807,#17912,.F.) ;
#25967 = EDGE_CURVE('',#20406,#20951,#17913,.T.) ;
#25968 = EDGE_CURVE('',#20928,#20951,#3863,.T.) ;
#25969 = EDGE_CURVE('',#20949,#20409,#17914,.T.) ;
#25970 = EDGE_CURVE('',#20952,#20949,#17915,.F.) ;
#25971 = EDGE_CURVE('',#20410,#20952,#17916,.T.) ;
#25972 = EDGE_CURVE('',#20953,#20407,#17917,.T.) ;
#25973 = EDGE_CURVE('',#20950,#20953,#17918,.F.) ;
#25974 = EDGE_CURVE('',#20408,#20950,#17919,.T.) ;
#25975 = EDGE_CURVE('',#20951,#20953,#3864,.T.) ;
#25976 = EDGE_CURVE('',#20953,#20947,#3865,.T.) ;
#25977 = EDGE_CURVE('',#20948,#20954,#17920,.F.) ;
#25978 = EDGE_CURVE('',#20628,#20948,#17921,.T.) ;
#25979 = EDGE_CURVE('',#20954,#20627,#17922,.T.) ;
#25980 = EDGE_CURVE('',#20929,#20954,#3866,.T.) ;
#25981 = EDGE_CURVE('',#20954,#20952,#3867,.T.) ;
#25982 = EDGE_CURVE('',#20952,#20793,#3868,.T.) ;
#25983 = EDGE_CURVE('',#20947,#20928,#3869,.T.) ;
#25984 = EDGE_CURVE('',#20955,#20652,#17923,.T.) ;
#25985 = EDGE_CURVE('',#20651,#20956,#17924,.T.) ;
#25986 = EDGE_CURVE('',#20955,#20956,#17925,.T.) ;
#25987 = EDGE_CURVE('',#20957,#20653,#17926,.T.) ;
#25988 = EDGE_CURVE('',#20957,#20958,#17927,.T.) ;
#25989 = EDGE_CURVE('',#20958,#20654,#17928,.T.) ;
#25990 = EDGE_CURVE('',#20955,#20957,#3870,.T.) ;
#25991 = EDGE_CURVE('',#20959,#20955,#3871,.T.) ;
#25992 = EDGE_CURVE('',#20960,#20959,#3872,.T.) ;
#25993 = EDGE_CURVE('',#20957,#20960,#3873,.T.) ;
#25994 = EDGE_CURVE('',#20361,#20899,#17929,.T.) ;
#25995 = EDGE_CURVE('',#20898,#20360,#17930,.T.) ;
#25996 = EDGE_CURVE('',#20900,#20362,#17931,.T.) ;
#25997 = EDGE_CURVE('',#20363,#20901,#17932,.T.) ;
#25998 = EDGE_CURVE('',#20359,#20897,#17933,.F.) ;
#25999 = EDGE_CURVE('',#20895,#20359,#17934,.F.) ;
#26000 = EDGE_CURVE('',#20364,#20903,#17935,.F.) ;
#26001 = EDGE_CURVE('',#20902,#20364,#17936,.F.) ;
#26002 = EDGE_CURVE('',#20961,#20357,#17937,.T.) ;
#26003 = EDGE_CURVE('',#20896,#20961,#17938,.F.) ;
#26004 = EDGE_CURVE('',#20358,#20896,#17939,.T.) ;
#26005 = EDGE_CURVE('',#20904,#20365,#17940,.T.) ;
#26006 = EDGE_CURVE('',#20962,#20904,#17941,.F.) ;
#26007 = EDGE_CURVE('',#20366,#20962,#17942,.T.) ;
#26008 = EDGE_CURVE('',#20894,#20962,#3874,.T.) ;
#26009 = EDGE_CURVE('',#20959,#20355,#17943,.T.) ;
#26010 = EDGE_CURVE('',#20963,#20959,#17944,.F.) ;
#26011 = EDGE_CURVE('',#20356,#20963,#17945,.T.) ;
#26012 = EDGE_CURVE('',#20964,#20354,#17946,.T.) ;
#26013 = EDGE_CURVE('',#20960,#20964,#17947,.F.) ;
#26014 = EDGE_CURVE('',#20353,#20960,#17948,.T.) ;
#26015 = EDGE_CURVE('',#20962,#20964,#3875,.T.) ;
#26016 = EDGE_CURVE('',#20964,#20958,#3876,.T.) ;
#26017 = EDGE_CURVE('',#20956,#20963,#3877,.T.) ;
#26018 = EDGE_CURVE('',#20963,#20961,#3878,.T.) ;
#26019 = EDGE_CURVE('',#20961,#20884,#3879,.T.) ;
#26020 = EDGE_CURVE('',#20958,#20894,#3880,.T.) ;
#26021 = EDGE_CURVE('',#20965,#20638,#17949,.T.) ;
#26022 = EDGE_CURVE('',#20637,#20966,#17950,.T.) ;
#26023 = EDGE_CURVE('',#20965,#20966,#17951,.T.) ;
#26024 = EDGE_CURVE('',#20967,#20639,#17952,.T.) ;
#26025 = EDGE_CURVE('',#20967,#20968,#17953,.T.) ;
#26026 = EDGE_CURVE('',#20968,#20640,#17954,.T.) ;
#26027 = EDGE_CURVE('',#20965,#20967,#3881,.T.) ;
#26028 = EDGE_CURVE('',#20969,#20965,#3882,.T.) ;
#26029 = EDGE_CURVE('',#20970,#20969,#3883,.T.) ;
#26030 = EDGE_CURVE('',#20967,#20970,#3884,.T.) ;
#26031 = EDGE_CURVE('',#20920,#20474,#17955,.T.) ;
#26032 = EDGE_CURVE('',#20475,#20921,#17956,.T.) ;
#26033 = EDGE_CURVE('',#20473,#20919,#17957,.F.) ;
#26034 = EDGE_CURVE('',#20917,#20473,#17958,.F.) ;
#26035 = EDGE_CURVE('',#20922,#20476,#17959,.T.) ;
#26036 = EDGE_CURVE('',#20477,#20923,#17960,.T.) ;
#26037 = EDGE_CURVE('',#20971,#20471,#17961,.T.) ;
#26038 = EDGE_CURVE('',#20918,#20971,#17962,.F.) ;
#26039 = EDGE_CURVE('',#20472,#20918,#17963,.T.) ;
#26040 = EDGE_CURVE('',#20478,#20925,#17964,.F.) ;
#26041 = EDGE_CURVE('',#20924,#20478,#17965,.F.) ;
#26042 = EDGE_CURVE('',#20969,#20469,#17966,.T.) ;
#26043 = EDGE_CURVE('',#20972,#20969,#17967,.F.) ;
#26044 = EDGE_CURVE('',#20470,#20972,#17968,.T.) ;
#26045 = EDGE_CURVE('',#20926,#20479,#17969,.T.) ;
#26046 = EDGE_CURVE('',#20973,#20926,#17970,.F.) ;
#26047 = EDGE_CURVE('',#20480,#20973,#17971,.T.) ;
#26048 = EDGE_CURVE('',#20916,#20973,#3885,.T.) ;
#26049 = EDGE_CURVE('',#20974,#20468,#17972,.T.) ;
#26050 = EDGE_CURVE('',#20970,#20974,#17973,.F.) ;
#26051 = EDGE_CURVE('',#20467,#20970,#17974,.T.) ;
#26052 = EDGE_CURVE('',#20973,#20974,#3886,.T.) ;
#26053 = EDGE_CURVE('',#20974,#20968,#3887,.T.) ;
#26054 = EDGE_CURVE('',#20966,#20972,#3888,.T.) ;
#26055 = EDGE_CURVE('',#20972,#20971,#3889,.T.) ;
#26056 = EDGE_CURVE('',#20971,#20906,#3890,.T.) ;
#26057 = EDGE_CURVE('',#20968,#20916,#3891,.T.) ;
#26058 = EDGE_CURVE('',#20975,#20322,#17975,.T.) ;
#26059 = EDGE_CURVE('',#20976,#20975,#17976,.F.) ;
#26060 = EDGE_CURVE('',#20323,#20976,#17977,.T.) ;
#26061 = EDGE_CURVE('',#20977,#20320,#17978,.T.) ;
#26062 = EDGE_CURVE('',#20978,#20977,#17979,.F.) ;
#26063 = EDGE_CURVE('',#20321,#20978,#17980,.T.) ;
#26064 = EDGE_CURVE('',#20756,#20703,#17981,.T.) ;
#26065 = EDGE_CURVE('',#20707,#20757,#17982,.T.) ;
#26066 = EDGE_CURVE('',#20706,#20315,#17983,.T.) ;
#26067 = EDGE_CURVE('',#20315,#20757,#17984,.T.) ;
#26068 = EDGE_CURVE('',#20705,#20316,#17985,.T.) ;
#26069 = EDGE_CURVE('',#20979,#20317,#17986,.T.) ;
#26070 = EDGE_CURVE('',#20705,#20979,#17987,.T.) ;
#26071 = EDGE_CURVE('',#20980,#20318,#17988,.T.) ;
#26072 = EDGE_CURVE('',#20979,#20980,#3892,.T.) ;
#26073 = EDGE_CURVE('',#20981,#20319,#17989,.T.) ;
#26074 = EDGE_CURVE('',#20980,#20981,#17990,.T.) ;
#26075 = EDGE_CURVE('',#20981,#20977,#3893,.T.) ;
#26076 = EDGE_CURVE('',#20767,#20690,#17991,.T.) ;
#26077 = EDGE_CURVE('',#20766,#20691,#17992,.T.) ;
#26078 = EDGE_CURVE('',#20299,#20692,#17993,.T.) ;
#26079 = EDGE_CURVE('',#20766,#20299,#17994,.T.) ;
#26080 = EDGE_CURVE('',#20300,#20693,#17995,.T.) ;
#26081 = EDGE_CURVE('',#20346,#20982,#17996,.T.) ;
#26082 = EDGE_CURVE('',#20982,#20693,#17997,.T.) ;
#26083 = EDGE_CURVE('',#20345,#20983,#17998,.T.) ;
#26084 = EDGE_CURVE('',#20983,#20982,#3894,.T.) ;
#26085 = EDGE_CURVE('',#20344,#20984,#17999,.T.) ;
#26086 = EDGE_CURVE('',#20984,#20983,#18000,.T.) ;
#26087 = EDGE_CURVE('',#20343,#20985,#18001,.T.) ;
#26088 = EDGE_CURVE('',#20985,#20984,#3895,.T.) ;
#26089 = EDGE_CURVE('',#20342,#20986,#18002,.T.) ;
#26090 = EDGE_CURVE('',#20986,#20985,#18003,.T.) ;
#26091 = EDGE_CURVE('',#20341,#20987,#18004,.T.) ;
#26092 = EDGE_CURVE('',#20987,#20986,#18005,.T.) ;
#26093 = EDGE_CURVE('',#20340,#20988,#18006,.T.) ;
#26094 = EDGE_CURVE('',#20988,#20987,#3896,.T.) ;
#26095 = EDGE_CURVE('',#20339,#20989,#18007,.T.) ;
#26096 = EDGE_CURVE('',#20989,#20988,#18008,.T.) ;
#26097 = EDGE_CURVE('',#20338,#20990,#18009,.T.) ;
#26098 = EDGE_CURVE('',#20990,#20989,#18010,.T.) ;
#26099 = EDGE_CURVE('',#20337,#20991,#18011,.T.) ;
#26100 = EDGE_CURVE('',#20991,#20990,#3897,.T.) ;
#26101 = EDGE_CURVE('',#20336,#20992,#18012,.T.) ;
#26102 = EDGE_CURVE('',#20992,#20991,#18013,.T.) ;
#26103 = EDGE_CURVE('',#20335,#20993,#18014,.T.) ;
#26104 = EDGE_CURVE('',#20993,#20992,#3898,.T.) ;
#26105 = EDGE_CURVE('',#20334,#20994,#18015,.T.) ;
#26106 = EDGE_CURVE('',#20994,#20993,#18016,.T.) ;
#26107 = EDGE_CURVE('',#20333,#20995,#18017,.T.) ;
#26108 = EDGE_CURVE('',#20995,#20994,#3899,.T.) ;
#26109 = EDGE_CURVE('',#20332,#20996,#18018,.T.) ;
#26110 = EDGE_CURVE('',#20996,#20995,#18019,.T.) ;
#26111 = EDGE_CURVE('',#20331,#20997,#18020,.T.) ;
#26112 = EDGE_CURVE('',#20997,#20996,#3900,.T.) ;
#26113 = EDGE_CURVE('',#20330,#20998,#18021,.T.) ;
#26114 = EDGE_CURVE('',#20998,#20997,#18022,.T.) ;
#26115 = EDGE_CURVE('',#20329,#20999,#18023,.T.) ;
#26116 = EDGE_CURVE('',#20999,#20998,#3901,.T.) ;
#26117 = EDGE_CURVE('',#20328,#21000,#18024,.T.) ;
#26118 = EDGE_CURVE('',#21000,#20999,#18025,.T.) ;
#26119 = EDGE_CURVE('',#20327,#21001,#18026,.T.) ;
#26120 = EDGE_CURVE('',#21001,#21000,#3902,.T.) ;
#26121 = EDGE_CURVE('',#20326,#21002,#18027,.T.) ;
#26122 = EDGE_CURVE('',#21002,#21001,#18028,.T.) ;
#26123 = EDGE_CURVE('',#20325,#21003,#18029,.T.) ;
#26124 = EDGE_CURVE('',#21003,#21002,#3903,.T.) ;
#26125 = EDGE_CURVE('',#20324,#21004,#18030,.T.) ;
#26126 = EDGE_CURVE('',#21004,#21003,#18031,.T.) ;
#26127 = EDGE_CURVE('',#20976,#21004,#3904,.T.) ;
#26128 = EDGE_CURVE('',#21005,#21006,#18032,.T.) ;
#26129 = EDGE_CURVE('',#21006,#20546,#18033,.T.) ;
#26130 = EDGE_CURVE('',#20545,#21005,#18034,.T.) ;
#26131 = EDGE_CURVE('',#20977,#21006,#3905,.T.) ;
#26132 = EDGE_CURVE('',#21005,#20978,#3906,.T.) ;
#26133 = EDGE_CURVE('',#20978,#20975,#3907,.T.) ;
#26134 = EDGE_CURVE('',#21007,#21008,#18035,.T.) ;
#26135 = EDGE_CURVE('',#21008,#20976,#3908,.T.) ;
#26136 = EDGE_CURVE('',#20975,#21007,#3909,.T.) ;
#26137 = EDGE_CURVE('',#20543,#21008,#18036,.T.) ;
#26138 = EDGE_CURVE('',#21007,#20544,#18037,.T.) ;
#26139 = EDGE_CURVE('',#21009,#20765,#235,.T.) ;
#26140 = EDGE_CURVE('',#20301,#21009,#236,.T.) ;
#26141 = EDGE_CURVE('',#21010,#20983,#3910,.T.) ;
#26142 = EDGE_CURVE('',#21011,#21010,#3911,.T.) ;
#26143 = EDGE_CURVE('',#20982,#21011,#3912,.T.) ;
#26144 = EDGE_CURVE('',#20984,#21012,#3913,.T.) ;
#26145 = EDGE_CURVE('',#21010,#21012,#18038,.T.) ;
#26146 = EDGE_CURVE('',#21013,#20985,#3914,.T.) ;
#26147 = EDGE_CURVE('',#21012,#21013,#3915,.T.) ;
#26148 = EDGE_CURVE('',#20986,#21014,#3916,.T.) ;
#26149 = EDGE_CURVE('',#21013,#21014,#18039,.T.) ;
#26150 = EDGE_CURVE('',#21015,#20987,#3917,.T.) ;
#26151 = EDGE_CURVE('',#21014,#21015,#18040,.T.) ;
#26152 = EDGE_CURVE('',#21016,#20988,#3918,.T.) ;
#26153 = EDGE_CURVE('',#21015,#21016,#3919,.T.) ;
#26154 = EDGE_CURVE('',#21017,#20989,#3920,.T.) ;
#26155 = EDGE_CURVE('',#21016,#21017,#18041,.T.) ;
#26156 = EDGE_CURVE('',#20990,#21018,#3921,.T.) ;
#26157 = EDGE_CURVE('',#21017,#21018,#18042,.T.) ;
#26158 = EDGE_CURVE('',#21019,#20991,#3922,.T.) ;
#26159 = EDGE_CURVE('',#21018,#21019,#3923,.T.) ;
#26160 = EDGE_CURVE('',#20992,#21020,#3924,.T.) ;
#26161 = EDGE_CURVE('',#21019,#21020,#18043,.T.) ;
#26162 = EDGE_CURVE('',#21021,#20993,#3925,.T.) ;
#26163 = EDGE_CURVE('',#21020,#21021,#3926,.T.) ;
#26164 = EDGE_CURVE('',#20994,#21022,#3927,.T.) ;
#26165 = EDGE_CURVE('',#21021,#21022,#18044,.T.) ;
#26166 = EDGE_CURVE('',#21023,#20995,#3928,.T.) ;
#26167 = EDGE_CURVE('',#21022,#21023,#3929,.T.) ;
#26168 = EDGE_CURVE('',#21024,#20996,#3930,.T.) ;
#26169 = EDGE_CURVE('',#21023,#21024,#18045,.T.) ;
#26170 = EDGE_CURVE('',#21025,#20997,#3931,.T.) ;
#26171 = EDGE_CURVE('',#21024,#21025,#3932,.T.) ;
#26172 = EDGE_CURVE('',#20998,#21026,#3933,.T.) ;
#26173 = EDGE_CURVE('',#21025,#21026,#18046,.T.) ;
#26174 = EDGE_CURVE('',#21027,#20999,#3934,.T.) ;
#26175 = EDGE_CURVE('',#21026,#21027,#3935,.T.) ;
#26176 = EDGE_CURVE('',#21000,#21028,#3936,.T.) ;
#26177 = EDGE_CURVE('',#21027,#21028,#18047,.T.) ;
#26178 = EDGE_CURVE('',#21029,#21001,#3937,.T.) ;
#26179 = EDGE_CURVE('',#21028,#21029,#3938,.T.) ;
#26180 = EDGE_CURVE('',#21002,#21030,#3939,.T.) ;
#26181 = EDGE_CURVE('',#21029,#21030,#18048,.T.) ;
#26182 = EDGE_CURVE('',#21031,#21003,#3940,.T.) ;
#26183 = EDGE_CURVE('',#21030,#21031,#3941,.T.) ;
#26184 = EDGE_CURVE('',#21004,#21032,#3942,.T.) ;
#26185 = EDGE_CURVE('',#21031,#21032,#18049,.T.) ;
#26186 = EDGE_CURVE('',#21032,#21008,#3943,.T.) ;
#26187 = EDGE_CURVE('',#21032,#20542,#18050,.T.) ;
#26188 = EDGE_CURVE('',#21033,#21034,#18051,.T.) ;
#26189 = EDGE_CURVE('',#21034,#21035,#3944,.T.) ;
#26190 = EDGE_CURVE('',#21035,#21036,#18052,.T.) ;
#26191 = EDGE_CURVE('',#21036,#21033,#3945,.T.) ;
#26192 = EDGE_CURVE('',#20369,#21037,#18053,.T.) ;
#26193 = EDGE_CURVE('',#21037,#21036,#18054,.T.) ;
#26194 = EDGE_CURVE('',#21035,#20369,#18055,.T.) ;
#26195 = EDGE_CURVE('',#20368,#21037,#237,.F.) ;
#26196 = EDGE_CURVE('',#21035,#21038,#3946,.T.) ;
#26197 = EDGE_CURVE('',#20370,#21038,#18056,.T.) ;
#26198 = EDGE_CURVE('',#21039,#21034,#3947,.T.) ;
#26199 = EDGE_CURVE('',#21038,#21039,#3948,.T.) ;
#26200 = EDGE_CURVE('',#21033,#21040,#3949,.T.) ;
#26201 = EDGE_CURVE('',#21040,#21041,#3950,.T.) ;
#26202 = EDGE_CURVE('',#21041,#21042,#3951,.T.) ;
#26203 = EDGE_CURVE('',#21039,#21042,#18057,.T.) ;
#26204 = EDGE_CURVE('',#21042,#21043,#3952,.T.) ;
#26205 = EDGE_CURVE('',#21043,#21038,#18058,.T.) ;
#26206 = EDGE_CURVE('',#21044,#20370,#18059,.T.) ;
#26207 = EDGE_CURVE('',#21043,#21044,#18060,.T.) ;
#26208 = EDGE_CURVE('',#20371,#21044,#238,.T.) ;
#26209 = EDGE_CURVE('',#21041,#20596,#3953,.T.) ;
#26210 = EDGE_CURVE('',#21044,#20596,#3954,.T.) ;
#26211 = EDGE_CURVE('',#21045,#20382,#18061,.T.) ;
#26212 = EDGE_CURVE('',#21046,#21045,#18062,.F.) ;
#26213 = EDGE_CURVE('',#20367,#21046,#18063,.T.) ;
#26214 = EDGE_CURVE('',#21047,#21048,#18064,.F.) ;
#26215 = EDGE_CURVE('',#20381,#21047,#18065,.T.) ;
#26216 = EDGE_CURVE('',#21048,#20380,#18066,.T.) ;
#26217 = EDGE_CURVE('',#21047,#21045,#3955,.T.) ;
#26218 = EDGE_CURVE('',#21049,#21050,#18067,.F.) ;
#26219 = EDGE_CURVE('',#20379,#21049,#18068,.T.) ;
#26220 = EDGE_CURVE('',#21050,#20378,#18069,.T.) ;
#26221 = EDGE_CURVE('',#21049,#21048,#3956,.T.) ;
#26222 = EDGE_CURVE('',#21051,#21052,#18070,.F.) ;
#26223 = EDGE_CURVE('',#20377,#21051,#18071,.T.) ;
#26224 = EDGE_CURVE('',#21052,#20376,#18072,.T.) ;
#26225 = EDGE_CURVE('',#21051,#21050,#3957,.T.) ;
#26226 = EDGE_CURVE('',#21053,#21054,#18073,.F.) ;
#26227 = EDGE_CURVE('',#20375,#21053,#18074,.T.) ;
#26228 = EDGE_CURVE('',#21054,#20374,#18075,.T.) ;
#26229 = EDGE_CURVE('',#21053,#21052,#3958,.T.) ;
#26230 = EDGE_CURVE('',#21055,#20372,#18076,.T.) ;
#26231 = EDGE_CURVE('',#21056,#21055,#18077,.F.) ;
#26232 = EDGE_CURVE('',#20373,#21056,#18078,.T.) ;
#26233 = EDGE_CURVE('',#21044,#21055,#3959,.T.) ;
#26234 = EDGE_CURVE('',#20594,#21056,#3960,.T.) ;
#26235 = EDGE_CURVE('',#21055,#20595,#3961,.T.) ;
#26236 = EDGE_CURVE('',#21056,#21054,#3962,.T.) ;
#26237 = EDGE_CURVE('',#20592,#21053,#3963,.T.) ;
#26238 = EDGE_CURVE('',#21054,#20593,#3964,.T.) ;
#26239 = EDGE_CURVE('',#20590,#21051,#3965,.T.) ;
#26240 = EDGE_CURVE('',#21052,#20591,#3966,.T.) ;
#26241 = EDGE_CURVE('',#20588,#21049,#3967,.T.) ;
#26242 = EDGE_CURVE('',#21050,#20589,#3968,.T.) ;
#26243 = EDGE_CURVE('',#20586,#21047,#3969,.T.) ;
#26244 = EDGE_CURVE('',#21048,#20587,#3970,.T.) ;
#26245 = EDGE_CURVE('',#20598,#21046,#3971,.T.) ;
#26246 = EDGE_CURVE('',#21045,#20585,#3972,.T.) ;
#26247 = EDGE_CURVE('',#21046,#21037,#3973,.T.) ;
#26248 = EDGE_CURVE('',#20390,#21057,#18079,.F.) ;
#26249 = EDGE_CURVE('',#21058,#20390,#18080,.F.) ;
#26250 = EDGE_CURVE('',#21057,#21058,#18081,.F.) ;
#26251 = EDGE_CURVE('',#21059,#20391,#18082,.T.) ;
#26252 = EDGE_CURVE('',#21060,#21059,#18083,.F.) ;
#26253 = EDGE_CURVE('',#20392,#21060,#18084,.T.) ;
#26254 = EDGE_CURVE('',#21057,#21059,#3974,.T.) ;
#26255 = EDGE_CURVE('',#20841,#21060,#3975,.T.) ;
#26256 = EDGE_CURVE('',#21059,#20839,#3976,.T.) ;
#26257 = EDGE_CURVE('',#21061,#20388,#18085,.T.) ;
#26258 = EDGE_CURVE('',#21062,#21061,#18086,.F.) ;
#26259 = EDGE_CURVE('',#20389,#21062,#18087,.T.) ;
#26260 = EDGE_CURVE('',#20856,#20393,#18088,.T.) ;
#26261 = EDGE_CURVE('',#20394,#20855,#18089,.T.) ;
#26262 = EDGE_CURVE('',#21060,#20856,#3977,.T.) ;
#26263 = EDGE_CURVE('',#21063,#20863,#18090,.F.) ;
#26264 = EDGE_CURVE('',#20387,#21063,#18091,.T.) ;
#26265 = EDGE_CURVE('',#20863,#20386,#18092,.T.) ;
#26266 = EDGE_CURVE('',#21063,#21061,#3978,.T.) ;
#26267 = EDGE_CURVE('',#20857,#20395,#18093,.T.) ;
#26268 = EDGE_CURVE('',#20396,#20858,#18094,.T.) ;
#26269 = EDGE_CURVE('',#20385,#20862,#18095,.F.) ;
#26270 = EDGE_CURVE('',#20861,#20385,#18096,.F.) ;
#26271 = EDGE_CURVE('',#20859,#20384,#18097,.T.) ;
#26272 = EDGE_CURVE('',#20383,#20860,#18098,.T.) ;
#26273 = EDGE_CURVE('',#20851,#21063,#3979,.T.) ;
#26274 = EDGE_CURVE('',#20853,#21062,#3980,.T.) ;
#26275 = EDGE_CURVE('',#21061,#20852,#3981,.T.) ;
#26276 = EDGE_CURVE('',#21062,#21058,#3982,.T.) ;
#26277 = EDGE_CURVE('',#20840,#21057,#3983,.T.) ;
#26278 = EDGE_CURVE('',#21058,#20854,#3984,.T.) ;
#26279 = EDGE_CURVE('',#21064,#21065,#18099,.T.) ;
#26280 = EDGE_CURVE('',#21065,#21066,#3985,.T.) ;
#26281 = EDGE_CURVE('',#21066,#21067,#18100,.T.) ;
#26282 = EDGE_CURVE('',#21067,#21064,#3986,.T.) ;
#26283 = EDGE_CURVE('',#20819,#20444,#18101,.T.) ;
#26284 = EDGE_CURVE('',#20444,#21067,#18102,.T.) ;
#26285 = EDGE_CURVE('',#21066,#20819,#18103,.T.) ;
#26286 = EDGE_CURVE('',#21068,#21065,#3987,.T.) ;
#26287 = EDGE_CURVE('',#21068,#20608,#3988,.T.) ;
#26288 = EDGE_CURVE('',#21069,#21070,#18104,.T.) ;
#26289 = EDGE_CURVE('',#21070,#21071,#3989,.T.) ;
#26290 = EDGE_CURVE('',#21071,#21072,#18105,.T.) ;
#26291 = EDGE_CURVE('',#21072,#21069,#3990,.T.) ;
#26292 = EDGE_CURVE('',#20456,#20814,#18106,.T.) ;
#26293 = EDGE_CURVE('',#20814,#21072,#18107,.T.) ;
#26294 = EDGE_CURVE('',#21071,#20456,#18108,.T.) ;
#26295 = EDGE_CURVE('',#21071,#21067,#3991,.T.) ;
#26296 = EDGE_CURVE('',#21064,#21070,#3992,.T.) ;
#26297 = EDGE_CURVE('',#20453,#20945,#18109,.T.) ;
#26298 = EDGE_CURVE('',#20944,#20452,#18110,.T.) ;
#26299 = EDGE_CURVE('',#20451,#20943,#18111,.T.) ;
#26300 = EDGE_CURVE('',#20942,#20450,#18112,.T.) ;
#26301 = EDGE_CURVE('',#20449,#20941,#18113,.T.) ;
#26302 = EDGE_CURVE('',#20940,#20448,#18114,.T.) ;
#26303 = EDGE_CURVE('',#20447,#20939,#18115,.T.) ;
#26304 = EDGE_CURVE('',#20938,#20446,#18116,.T.) ;
#26305 = EDGE_CURVE('',#21073,#21074,#18117,.T.) ;
#26306 = EDGE_CURVE('',#21074,#21075,#3993,.T.) ;
#26307 = EDGE_CURVE('',#21075,#21076,#18118,.T.) ;
#26308 = EDGE_CURVE('',#21076,#21073,#3994,.T.) ;
#26309 = EDGE_CURVE('',#20413,#20882,#18119,.T.) ;
#26310 = EDGE_CURVE('',#20882,#21076,#18120,.T.) ;
#26311 = EDGE_CURVE('',#21075,#20413,#18121,.T.) ;
#26312 = EDGE_CURVE('',#20412,#20882,#239,.F.) ;
#26313 = EDGE_CURVE('',#21075,#21077,#3995,.T.) ;
#26314 = EDGE_CURVE('',#20414,#21077,#18122,.T.) ;
#26315 = EDGE_CURVE('',#21078,#21074,#3996,.T.) ;
#26316 = EDGE_CURVE('',#21077,#21078,#3997,.T.) ;
#26317 = EDGE_CURVE('',#21073,#21079,#3998,.T.) ;
#26318 = EDGE_CURVE('',#21079,#21080,#3999,.T.) ;
#26319 = EDGE_CURVE('',#21080,#21081,#4000,.T.) ;
#26320 = EDGE_CURVE('',#21078,#21081,#18123,.T.) ;
#26321 = EDGE_CURVE('',#21081,#21082,#4001,.T.) ;
#26322 = EDGE_CURVE('',#21082,#21077,#18124,.T.) ;
#26323 = EDGE_CURVE('',#21083,#20414,#18125,.T.) ;
#26324 = EDGE_CURVE('',#21082,#21083,#18126,.T.) ;
#26325 = EDGE_CURVE('',#20415,#21083,#240,.T.) ;
#26326 = EDGE_CURVE('',#21080,#20583,#4002,.T.) ;
#26327 = EDGE_CURVE('',#21083,#20881,#4003,.T.) ;
#26328 = EDGE_CURVE('',#21084,#21085,#18127,.F.) ;
#26329 = EDGE_CURVE('',#20418,#21084,#18128,.T.) ;
#26330 = EDGE_CURVE('',#21085,#20417,#18129,.T.) ;
#26331 = EDGE_CURVE('',#21086,#21087,#18130,.F.) ;
#26332 = EDGE_CURVE('',#20420,#21086,#18131,.T.) ;
#26333 = EDGE_CURVE('',#21087,#20419,#18132,.T.) ;
#26334 = EDGE_CURVE('',#21088,#21089,#18133,.F.) ;
#26335 = EDGE_CURVE('',#20422,#21088,#18134,.T.) ;
#26336 = EDGE_CURVE('',#21089,#20421,#18135,.T.) ;
#26337 = EDGE_CURVE('',#21090,#21091,#18136,.F.) ;
#26338 = EDGE_CURVE('',#20424,#21090,#18137,.T.) ;
#26339 = EDGE_CURVE('',#21091,#20423,#18138,.T.) ;
#26340 = EDGE_CURVE('',#21090,#20878,#4004,.T.) ;
#26341 = EDGE_CURVE('',#21088,#21091,#4005,.T.) ;
#26342 = EDGE_CURVE('',#20868,#21090,#4006,.T.) ;
#26343 = EDGE_CURVE('',#21091,#20869,#4007,.T.) ;
#26344 = EDGE_CURVE('',#21086,#21089,#4008,.T.) ;
#26345 = EDGE_CURVE('',#20870,#21088,#4009,.T.) ;
#26346 = EDGE_CURVE('',#21089,#20871,#4010,.T.) ;
#26347 = EDGE_CURVE('',#21084,#21087,#4011,.T.) ;
#26348 = EDGE_CURVE('',#20872,#21086,#4012,.T.) ;
#26349 = EDGE_CURVE('',#21087,#20873,#4013,.T.) ;
#26350 = EDGE_CURVE('',#20879,#21085,#4014,.T.) ;
#26351 = EDGE_CURVE('',#20874,#21084,#4015,.T.) ;
#26352 = EDGE_CURVE('',#21085,#20875,#4016,.T.) ;
#26353 = EDGE_CURVE('',#21083,#20880,#4017,.T.) ;
#26354 = EDGE_CURVE('',#20884,#20956,#4018,.T.) ;
#26355 = EDGE_CURVE('',#20906,#20966,#4019,.T.) ;
#26356 = EDGE_CURVE('',#21092,#20463,#18139,.T.) ;
#26357 = EDGE_CURVE('',#21093,#21092,#18140,.F.) ;
#26358 = EDGE_CURVE('',#20464,#21093,#18141,.T.) ;
#26359 = EDGE_CURVE('',#21094,#21095,#18142,.F.) ;
#26360 = EDGE_CURVE('',#20604,#21094,#18143,.T.) ;
#26361 = EDGE_CURVE('',#21095,#20603,#18144,.T.) ;
#26362 = EDGE_CURVE('',#21096,#20461,#18145,.T.) ;
#26363 = EDGE_CURVE('',#21097,#21096,#18146,.F.) ;
#26364 = EDGE_CURVE('',#20462,#21097,#18147,.T.) ;
#26365 = EDGE_CURVE('',#21098,#21099,#18148,.F.) ;
#26366 = EDGE_CURVE('',#20466,#21098,#18149,.T.) ;
#26367 = EDGE_CURVE('',#21099,#20465,#18150,.T.) ;
#26368 = EDGE_CURVE('',#21100,#20601,#18151,.T.) ;
#26369 = EDGE_CURVE('',#21101,#21100,#18152,.F.) ;
#26370 = EDGE_CURVE('',#20602,#21101,#18153,.T.) ;
#26371 = EDGE_CURVE('',#21102,#21103,#18154,.F.) ;
#26372 = EDGE_CURVE('',#20606,#21102,#18155,.T.) ;
#26373 = EDGE_CURVE('',#21103,#20605,#18156,.T.) ;
#26374 = EDGE_CURVE('',#21104,#20460,#18157,.T.) ;
#26375 = EDGE_CURVE('',#21105,#21104,#18158,.F.) ;
#26376 = EDGE_CURVE('',#20459,#21105,#18159,.T.) ;
#26377 = EDGE_CURVE('',#21098,#21104,#4020,.T.) ;
#26378 = EDGE_CURVE('',#21106,#21107,#18160,.F.) ;
#26379 = EDGE_CURVE('',#20599,#21106,#18161,.T.) ;
#26380 = EDGE_CURVE('',#21107,#20600,#18162,.T.) ;
#26381 = EDGE_CURVE('',#21106,#21100,#4021,.T.) ;
#26382 = EDGE_CURVE('',#21102,#21107,#4022,.T.) ;
#26383 = EDGE_CURVE('',#21104,#21106,#4023,.T.) ;
#26384 = EDGE_CURVE('',#21107,#21105,#4024,.T.) ;
#26385 = EDGE_CURVE('',#21105,#21096,#4025,.T.) ;
#26386 = EDGE_CURVE('',#21094,#21103,#4026,.T.) ;
#26387 = EDGE_CURVE('',#21096,#21102,#4027,.T.) ;
#26388 = EDGE_CURVE('',#21103,#21097,#4028,.T.) ;
#26389 = EDGE_CURVE('',#21099,#21101,#4029,.T.) ;
#26390 = EDGE_CURVE('',#21100,#21098,#4030,.T.) ;
#26391 = EDGE_CURVE('',#21101,#21095,#4031,.T.) ;
#26392 = EDGE_CURVE('',#21093,#21099,#4032,.T.) ;
#26393 = EDGE_CURVE('',#21097,#21092,#4033,.T.) ;
#26394 = EDGE_CURVE('',#21092,#21094,#4034,.T.) ;
#26395 = EDGE_CURVE('',#21095,#21093,#4035,.T.) ;
#26396 = EDGE_CURVE('',#20566,#21108,#18163,.T.) ;
#26397 = EDGE_CURVE('',#21108,#21108,#18164,.T.) ;
#26398 = EDGE_CURVE('',#21108,#21109,#4036,.T.) ;
#26399 = EDGE_CURVE('',#21110,#21109,#18165,.T.) ;
#26400 = EDGE_CURVE('',#21109,#21110,#18166,.T.) ;
#26401 = EDGE_CURVE('',#20425,#21110,#18167,.T.) ;
#26402 = EDGE_CURVE('',#21111,#21112,#18168,.T.) ;
#26403 = EDGE_CURVE('',#21112,#21113,#4037,.T.) ;
#26404 = EDGE_CURVE('',#21113,#21114,#18169,.T.) ;
#26405 = EDGE_CURVE('',#21114,#21111,#4038,.T.) ;
#26406 = EDGE_CURVE('',#20828,#20440,#18170,.T.) ;
#26407 = EDGE_CURVE('',#20440,#21114,#18171,.T.) ;
#26408 = EDGE_CURVE('',#21113,#20828,#18172,.T.) ;
#26409 = EDGE_CURVE('',#20426,#20828,#241,.T.) ;
#26410 = EDGE_CURVE('',#21115,#21112,#4039,.T.) ;
#26411 = EDGE_CURVE('',#21115,#20498,#4040,.T.) ;
#26412 = EDGE_CURVE('',#21111,#21116,#4041,.T.) ;
#26413 = EDGE_CURVE('',#21117,#21116,#18173,.T.) ;
#26414 = EDGE_CURVE('',#21117,#21118,#4042,.T.) ;
#26415 = EDGE_CURVE('',#21118,#21115,#4043,.T.) ;
#26416 = EDGE_CURVE('',#21119,#21114,#4044,.T.) ;
#26417 = EDGE_CURVE('',#21116,#21119,#4045,.T.) ;
#26418 = EDGE_CURVE('',#21119,#21120,#18174,.T.) ;
#26419 = EDGE_CURVE('',#21120,#21117,#4046,.T.) ;
#26420 = EDGE_CURVE('',#20439,#21121,#18175,.T.) ;
#26421 = EDGE_CURVE('',#21121,#21120,#18176,.T.) ;
#26422 = EDGE_CURVE('',#21119,#20439,#18177,.T.) ;
#26423 = EDGE_CURVE('',#20438,#21121,#242,.F.) ;
#26424 = EDGE_CURVE('',#20436,#20837,#18178,.T.) ;
#26425 = EDGE_CURVE('',#20836,#20435,#18179,.T.) ;
#26426 = EDGE_CURVE('',#20838,#20437,#243,.T.) ;
#26427 = EDGE_CURVE('',#20434,#20835,#18180,.T.) ;
#26428 = EDGE_CURVE('',#20834,#20433,#18181,.T.) ;
#26429 = EDGE_CURVE('',#20432,#20833,#18182,.T.) ;
#26430 = EDGE_CURVE('',#20832,#20431,#18183,.T.) ;
#26431 = EDGE_CURVE('',#20430,#20831,#18184,.T.) ;
#26432 = EDGE_CURVE('',#20830,#20429,#18185,.T.) ;
#26433 = EDGE_CURVE('',#20428,#20829,#18186,.T.) ;
#26434 = EDGE_CURVE('',#20827,#20427,#18187,.T.) ;
#26435 = EDGE_CURVE('',#20838,#21121,#4047,.T.) ;
#26436 = EDGE_CURVE('',#20308,#21122,#18188,.T.) ;
#26437 = EDGE_CURVE('',#21122,#21123,#18189,.T.) ;
#26438 = EDGE_CURVE('',#21123,#21122,#18190,.T.) ;
#26439 = EDGE_CURVE('',#20567,#21123,#4048,.T.) ;
#26440 = EDGE_CURVE('',#20458,#21124,#18191,.T.) ;
#26441 = EDGE_CURVE('',#21124,#21125,#18192,.T.) ;
#26442 = EDGE_CURVE('',#21125,#21124,#18193,.T.) ;
#26443 = EDGE_CURVE('',#20584,#21125,#4049,.T.) ;
#26444 = EDGE_CURVE('',#20694,#20519,#18194,.T.) ;
#26445 = EDGE_CURVE('',#21011,#20520,#18195,.T.) ;
#26446 = EDGE_CURVE('',#20694,#21011,#18196,.T.) ;
#26447 = EDGE_CURVE('',#21010,#20521,#18197,.T.) ;
#26448 = EDGE_CURVE('',#21012,#20522,#18198,.T.) ;
#26449 = EDGE_CURVE('',#21013,#20523,#18199,.T.) ;
#26450 = EDGE_CURVE('',#21014,#20524,#18200,.T.) ;
#26451 = EDGE_CURVE('',#21015,#20525,#18201,.T.) ;
#26452 = EDGE_CURVE('',#21016,#20526,#18202,.T.) ;
#26453 = EDGE_CURVE('',#21017,#20527,#18203,.T.) ;
#26454 = EDGE_CURVE('',#21018,#20528,#18204,.T.) ;
#26455 = EDGE_CURVE('',#21019,#20529,#18205,.T.) ;
#26456 = EDGE_CURVE('',#21020,#20530,#18206,.T.) ;
#26457 = EDGE_CURVE('',#21021,#20531,#18207,.T.) ;
#26458 = EDGE_CURVE('',#21022,#20532,#18208,.T.) ;
#26459 = EDGE_CURVE('',#21023,#20533,#18209,.T.) ;
#26460 = EDGE_CURVE('',#21024,#20534,#18210,.T.) ;
#26461 = EDGE_CURVE('',#21025,#20535,#18211,.T.) ;
#26462 = EDGE_CURVE('',#21026,#20536,#18212,.T.) ;
#26463 = EDGE_CURVE('',#21027,#20537,#18213,.T.) ;
#26464 = EDGE_CURVE('',#21028,#20538,#18214,.T.) ;
#26465 = EDGE_CURVE('',#21029,#20539,#18215,.T.) ;
#26466 = EDGE_CURVE('',#21030,#20540,#18216,.T.) ;
#26467 = EDGE_CURVE('',#21031,#20541,#18217,.T.) ;
#26468 = EDGE_CURVE('',#20549,#21126,#18218,.T.) ;
#26469 = EDGE_CURVE('',#21126,#20704,#18219,.T.) ;
#26470 = EDGE_CURVE('',#20548,#21127,#18220,.T.) ;
#26471 = EDGE_CURVE('',#21127,#21126,#4050,.T.) ;
#26472 = EDGE_CURVE('',#20547,#21128,#18221,.T.) ;
#26473 = EDGE_CURVE('',#21128,#21127,#18222,.T.) ;
#26474 = EDGE_CURVE('',#21006,#21128,#4051,.T.) ;
#26475 = EDGE_CURVE('',#20716,#21129,#18223,.T.) ;
#26476 = EDGE_CURVE('',#21129,#21129,#18224,.T.) ;
#26477 = EDGE_CURVE('',#21130,#21130,#18225,.T.) ;
#26478 = EDGE_CURVE('',#21131,#21132,#18226,.T.) ;
#26479 = EDGE_CURVE('',#21132,#21130,#18227,.T.) ;
#26480 = EDGE_CURVE('',#21132,#21131,#18228,.T.) ;
#26481 = EDGE_CURVE('',#21133,#21133,#18229,.T.) ;
#26482 = EDGE_CURVE('',#21133,#21131,#4052,.T.) ;
#26483 = EDGE_CURVE('',#21133,#21134,#18230,.T.) ;
#26484 = EDGE_CURVE('',#21134,#21135,#18231,.T.) ;
#26485 = EDGE_CURVE('',#21135,#21134,#18232,.T.) ;
#26486 = EDGE_CURVE('',#21136,#21136,#18233,.T.) ;
#26487 = EDGE_CURVE('',#21136,#21137,#18234,.T.) ;
#26488 = EDGE_CURVE('',#21137,#21138,#18235,.T.) ;
#26489 = EDGE_CURVE('',#21138,#21137,#18236,.T.) ;
#26490 = EDGE_CURVE('',#21136,#21139,#4053,.T.) ;
#26491 = EDGE_CURVE('',#21140,#21139,#18237,.T.) ;
#26492 = EDGE_CURVE('',#21139,#21140,#18238,.T.) ;
#26493 = EDGE_CURVE('',#21140,#21141,#18239,.T.) ;
#26494 = EDGE_CURVE('',#21141,#21141,#18240,.T.) ;
#26495 = EDGE_CURVE('',#21142,#21142,#18241,.T.) ;
#26496 = EDGE_CURVE('',#21143,#21143,#18242,.T.) ;
#26497 = EDGE_CURVE('',#21143,#21142,#18243,.T.) ;
#26498 = EDGE_CURVE('',#21144,#21144,#18244,.F.) ;
#26499 = EDGE_CURVE('',#21144,#21143,#4054,.T.) ;
#26500 = EDGE_CURVE('',#21145,#21145,#18245,.T.) ;
#26501 = EDGE_CURVE('',#21145,#21146,#18246,.T.) ;
#26502 = EDGE_CURVE('',#21146,#21147,#18247,.T.) ;
#26503 = EDGE_CURVE('',#21147,#21146,#18248,.T.) ;
#26504 = EDGE_CURVE('',#21145,#21148,#4055,.T.) ;
#26505 = EDGE_CURVE('',#21149,#21148,#18249,.T.) ;
#26506 = EDGE_CURVE('',#21148,#21149,#18250,.T.) ;
#26507 = EDGE_CURVE('',#20490,#21150,#18251,.T.) ;
#26508 = EDGE_CURVE('',#21150,#21150,#18252,.T.) ;
#26509 = EDGE_CURVE('',#21151,#21151,#18253,.T.) ;
#26510 = EDGE_CURVE('',#21149,#21151,#18254,.T.) ;
#26511 = EDGE_CURVE('',#21135,#20441,#18255,.T.) ;
#26512 = EDGE_CURVE('',#21138,#20457,#18256,.T.) ;
#26513 = EDGE_CURVE('',#21147,#20442,#18257,.T.) ;
#26514 = EDGE_CURVE('',#20980,#21127,#4056,.T.) ;
#26515 = EDGE_CURVE('',#21128,#20981,#4057,.T.) ;
#26516 = EDGE_CURVE('',#21126,#20979,#4058,.T.) ;
#26517 = EDGE_CURVE('',#20758,#20314,#244,.T.) ;
#26518 = EDGE_CURVE('',#20314,#21152,#245,.T.) ;
#26519 = EDGE_CURVE('',#21152,#20758,#18258,.T.) ;
#26520 = EDGE_CURVE('',#21153,#21154,#246,.T.) ;
#26521 = EDGE_CURVE('',#21154,#20309,#247,.T.) ;
#26522 = EDGE_CURVE('',#20309,#21155,#248,.T.) ;
#26523 = EDGE_CURVE('',#21155,#20761,#249,.T.) ;
#26524 = EDGE_CURVE('',#20761,#21153,#18259,.T.) ;
#26525 = EDGE_CURVE('',#20762,#21156,#250,.T.) ;
#26526 = EDGE_CURVE('',#21156,#20306,#251,.T.) ;
#26527 = EDGE_CURVE('',#20306,#21157,#252,.T.) ;
#26528 = EDGE_CURVE('',#21157,#21158,#253,.T.) ;
#26529 = EDGE_CURVE('',#21158,#20762,#18260,.T.) ;
#26530 = EDGE_CURVE('',#21159,#21160,#254,.T.) ;
#26531 = EDGE_CURVE('',#21160,#20301,#255,.T.) ;
#26532 = EDGE_CURVE('',#20765,#21159,#18261,.T.) ;
#26533 = EDGE_CURVE('',#21159,#21161,#4059,.T.) ;
#26534 = EDGE_CURVE('',#21161,#20302,#18262,.T.) ;
#26535 = EDGE_CURVE('',#20722,#20303,#18263,.T.) ;
#26536 = EDGE_CURVE('',#21161,#20722,#256,.T.) ;
#26537 = EDGE_CURVE('',#20723,#20304,#18264,.T.) ;
#26538 = EDGE_CURVE('',#21162,#20305,#18265,.T.) ;
#26539 = EDGE_CURVE('',#20723,#21162,#257,.T.) ;
#26540 = EDGE_CURVE('',#21162,#21158,#4060,.T.) ;
#26541 = EDGE_CURVE('',#21153,#21163,#4061,.T.) ;
#26542 = EDGE_CURVE('',#21163,#20310,#18266,.T.) ;
#26543 = EDGE_CURVE('',#20738,#20311,#18267,.T.) ;
#26544 = EDGE_CURVE('',#21163,#20738,#258,.T.) ;
#26545 = EDGE_CURVE('',#20739,#20312,#18268,.T.) ;
#26546 = EDGE_CURVE('',#21164,#20313,#18269,.T.) ;
#26547 = EDGE_CURVE('',#20739,#21164,#259,.T.) ;
#26548 = EDGE_CURVE('',#21164,#21152,#4062,.T.) ;
#26549 = EDGE_CURVE('',#20743,#21165,#18270,.T.) ;
#26550 = EDGE_CURVE('',#21165,#21164,#4063,.T.) ;
#26551 = EDGE_CURVE('',#21163,#21166,#4064,.T.) ;
#26552 = EDGE_CURVE('',#21166,#20740,#18271,.T.) ;
#26553 = EDGE_CURVE('',#21166,#21153,#4065,.T.) ;
#26554 = EDGE_CURVE('',#21166,#20760,#260,.T.) ;
#26555 = EDGE_CURVE('',#21158,#21167,#4066,.T.) ;
#26556 = EDGE_CURVE('',#20763,#21167,#261,.T.) ;
#26557 = EDGE_CURVE('',#21167,#21162,#4067,.T.) ;
#26558 = EDGE_CURVE('',#20727,#21167,#18272,.T.) ;
#26559 = EDGE_CURVE('',#21161,#21168,#4068,.T.) ;
#26560 = EDGE_CURVE('',#21168,#20724,#18273,.T.) ;
#26561 = EDGE_CURVE('',#21168,#21159,#4069,.T.) ;
#26562 = EDGE_CURVE('',#21168,#20764,#262,.T.) ;
#26563 = EDGE_CURVE('',#21169,#20609,#4070,.T.) ;
#26564 = EDGE_CURVE('',#21069,#21169,#4071,.T.) ;
#26565 = EDGE_CURVE('',#21169,#21068,#4072,.T.) ;
#26566 = EDGE_CURVE('',#20499,#21121,#4073,.T.) ;
#26567 = EDGE_CURVE('',#21118,#20499,#4074,.T.) ;
#26568 = EDGE_CURVE('',#20597,#21037,#4075,.T.) ;
#26569 = EDGE_CURVE('',#21040,#20597,#4076,.T.) ;
#26570 = EDGE_CURVE('',#21079,#20569,#4077,.T.) ;
#26571 = EDGE_CURVE('',#20745,#20775,#1124,.T.) ;
#26572 = EDGE_CURVE('',#20731,#20771,#1125,.T.) ;
#26573 = EDGE_CURVE('',#20772,#20514,#4078,.T.) ;
#26574 = EDGE_CURVE('',#20511,#20773,#4079,.T.) ;
#26575 = EDGE_CURVE('',#20774,#20748,#1126,.T.) ;
#26576 = EDGE_CURVE('',#20759,#21165,#263,.T.) ;
#26577 = EDGE_CURVE('',#21152,#21165,#4080,.T.) ;
#26578 = EDGE_CURVE('',#21170,#21171,#4081,.T.) ;
#26579 = EDGE_CURVE('',#21171,#21172,#264,.T.) ;
#26580 = EDGE_CURVE('',#21172,#21173,#4082,.T.) ;
#26581 = EDGE_CURVE('',#21173,#21170,#265,.T.) ;
#26582 = EDGE_CURVE('',#21173,#21174,#4083,.T.) ;
#26583 = EDGE_CURVE('',#21174,#21175,#266,.T.) ;
#26584 = EDGE_CURVE('',#21175,#21170,#4084,.T.) ;
#26585 = EDGE_CURVE('',#21174,#21176,#4085,.T.) ;
#26586 = EDGE_CURVE('',#21176,#21177,#267,.T.) ;
#26587 = EDGE_CURVE('',#21177,#21175,#4086,.T.) ;
#26588 = EDGE_CURVE('',#21178,#21179,#18274,.F.) ;
#26589 = EDGE_CURVE('',#21180,#21178,#18275,.F.) ;
#26590 = EDGE_CURVE('',#21179,#21180,#18276,.F.) ;
#26591 = EDGE_CURVE('',#21181,#21182,#268,.T.) ;
#26592 = EDGE_CURVE('',#21182,#21180,#4087,.T.) ;
#26593 = EDGE_CURVE('',#21178,#21181,#4088,.T.) ;
#26594 = EDGE_CURVE('',#21183,#21184,#18277,.T.) ;
#26595 = EDGE_CURVE('',#21184,#21179,#4089,.T.) ;
#26596 = EDGE_CURVE('',#21180,#21183,#4090,.T.) ;
#26597 = EDGE_CURVE('',#21176,#21178,#4091,.T.) ;
#26598 = EDGE_CURVE('',#21179,#21177,#4092,.T.) ;
#26599 = EDGE_CURVE('',#21170,#21185,#4093,.T.) ;
#26600 = EDGE_CURVE('',#21186,#21185,#4094,.T.) ;
#26601 = EDGE_CURVE('',#21171,#21186,#4095,.T.) ;
#26602 = EDGE_CURVE('',#21187,#21186,#4096,.T.) ;
#26603 = EDGE_CURVE('',#21182,#21187,#4097,.T.) ;
#26604 = EDGE_CURVE('',#21172,#21181,#4098,.T.) ;
#26605 = EDGE_CURVE('',#21175,#21188,#4099,.T.) ;
#26606 = EDGE_CURVE('',#21185,#21188,#4100,.T.) ;
#26607 = EDGE_CURVE('',#21177,#21189,#4101,.T.) ;
#26608 = EDGE_CURVE('',#21188,#21189,#4102,.T.) ;
#26609 = EDGE_CURVE('',#21189,#21184,#4103,.T.) ;
#26610 = EDGE_CURVE('',#21183,#21187,#4104,.T.) ;
#26611 = EDGE_CURVE('',#21190,#21191,#1127,.T.) ;
#26612 = EDGE_CURVE('',#21191,#21192,#4105,.T.) ;
#26613 = EDGE_CURVE('',#21192,#21193,#18278,.T.) ;
#26614 = EDGE_CURVE('',#21193,#21190,#4106,.T.) ;
#26615 = EDGE_CURVE('',#21194,#21192,#18279,.T.) ;
#26616 = EDGE_CURVE('',#21192,#21195,#4107,.T.) ;
#26617 = EDGE_CURVE('',#21195,#21196,#18280,.T.) ;
#26618 = EDGE_CURVE('',#21196,#21194,#4108,.T.) ;
#26619 = EDGE_CURVE('',#21197,#21198,#1128,.T.) ;
#26620 = EDGE_CURVE('',#21198,#21199,#4109,.T.) ;
#26621 = EDGE_CURVE('',#21199,#21195,#18281,.T.) ;
#26622 = EDGE_CURVE('',#21195,#21197,#4110,.T.) ;
#26623 = EDGE_CURVE('',#21199,#21196,#18282,.T.) ;
#26624 = EDGE_CURVE('',#21194,#21193,#18283,.T.) ;
#26625 = EDGE_CURVE('',#21200,#21193,#4111,.T.) ;
#26626 = EDGE_CURVE('',#21201,#21200,#18284,.T.) ;
#26627 = EDGE_CURVE('',#21202,#21201,#4112,.T.) ;
#26628 = EDGE_CURVE('',#21203,#21202,#4113,.T.) ;
#26629 = EDGE_CURVE('',#21204,#21203,#4114,.T.) ;
#26630 = EDGE_CURVE('',#21205,#21204,#4115,.T.) ;
#26631 = EDGE_CURVE('',#21206,#21205,#4116,.T.) ;
#26632 = EDGE_CURVE('',#21207,#21206,#18285,.T.) ;
#26633 = EDGE_CURVE('',#21208,#21207,#4117,.T.) ;
#26634 = EDGE_CURVE('',#21209,#21208,#18286,.T.) ;
#26635 = EDGE_CURVE('',#21210,#21209,#4118,.T.) ;
#26636 = EDGE_CURVE('',#21211,#21210,#18287,.T.) ;
#26637 = EDGE_CURVE('',#21212,#21211,#4119,.T.) ;
#26638 = EDGE_CURVE('',#21213,#21212,#18288,.T.) ;
#26639 = EDGE_CURVE('',#21214,#21213,#4120,.T.) ;
#26640 = EDGE_CURVE('',#21215,#21214,#4121,.T.) ;
#26641 = EDGE_CURVE('',#21216,#21215,#4122,.T.) ;
#26642 = EDGE_CURVE('',#21217,#21216,#4123,.T.) ;
#26643 = EDGE_CURVE('',#21218,#21217,#4124,.T.) ;
#26644 = EDGE_CURVE('',#21219,#21218,#4125,.T.) ;
#26645 = EDGE_CURVE('',#21220,#21219,#4126,.T.) ;
#26646 = EDGE_CURVE('',#21221,#21220,#4127,.T.) ;
#26647 = EDGE_CURVE('',#21221,#21222,#4128,.T.) ;
#26648 = EDGE_CURVE('',#21222,#21190,#18289,.T.) ;
#26649 = EDGE_CURVE('',#21223,#21224,#4129,.T.) ;
#26650 = EDGE_CURVE('',#21225,#21223,#18290,.T.) ;
#26651 = EDGE_CURVE('',#21226,#21225,#4130,.T.) ;
#26652 = EDGE_CURVE('',#21224,#21226,#18291,.T.) ;
#26653 = EDGE_CURVE('',#21227,#21228,#1129,.F.) ;
#26654 = EDGE_CURVE('',#21229,#21227,#4131,.T.) ;
#26655 = EDGE_CURVE('',#21230,#21229,#1130,.F.) ;
#26656 = EDGE_CURVE('',#21231,#21230,#4132,.T.) ;
#26657 = EDGE_CURVE('',#21232,#21231,#1131,.F.) ;
#26658 = EDGE_CURVE('',#21233,#21232,#4133,.T.) ;
#26659 = EDGE_CURVE('',#21234,#21233,#1132,.F.) ;
#26660 = EDGE_CURVE('',#21228,#21234,#4134,.T.) ;
#26661 = EDGE_CURVE('',#21235,#21236,#4135,.T.) ;
#26662 = EDGE_CURVE('',#21237,#21236,#1133,.F.) ;
#26663 = EDGE_CURVE('',#21237,#21238,#4136,.T.) ;
#26664 = EDGE_CURVE('',#21239,#21238,#1134,.F.) ;
#26665 = EDGE_CURVE('',#21239,#21240,#4137,.T.) ;
#26666 = EDGE_CURVE('',#21241,#21240,#1135,.F.) ;
#26667 = EDGE_CURVE('',#21241,#21242,#4138,.T.) ;
#26668 = EDGE_CURVE('',#21235,#21242,#1136,.F.) ;
#26669 = EDGE_CURVE('',#21243,#21244,#4139,.T.) ;
#26670 = EDGE_CURVE('',#21245,#21244,#1137,.F.) ;
#26671 = EDGE_CURVE('',#21245,#21246,#4140,.T.) ;
#26672 = EDGE_CURVE('',#21247,#21246,#1138,.F.) ;
#26673 = EDGE_CURVE('',#21247,#21248,#4141,.T.) ;
#26674 = EDGE_CURVE('',#21249,#21248,#1139,.F.) ;
#26675 = EDGE_CURVE('',#21249,#21250,#4142,.T.) ;
#26676 = EDGE_CURVE('',#21243,#21250,#1140,.F.) ;
#26677 = EDGE_CURVE('',#21251,#21252,#4143,.T.) ;
#26678 = EDGE_CURVE('',#21253,#21252,#1141,.F.) ;
#26679 = EDGE_CURVE('',#21253,#21254,#4144,.T.) ;
#26680 = EDGE_CURVE('',#21255,#21254,#1142,.F.) ;
#26681 = EDGE_CURVE('',#21255,#21256,#4145,.T.) ;
#26682 = EDGE_CURVE('',#21257,#21256,#1143,.F.) ;
#26683 = EDGE_CURVE('',#21257,#21258,#4146,.T.) ;
#26684 = EDGE_CURVE('',#21251,#21258,#1144,.F.) ;
#26685 = EDGE_CURVE('',#21194,#21259,#4147,.T.) ;
#26686 = EDGE_CURVE('',#21200,#21259,#18292,.T.) ;
#26687 = EDGE_CURVE('',#21260,#21196,#4148,.T.) ;
#26688 = EDGE_CURVE('',#21259,#21260,#4149,.T.) ;
#26689 = EDGE_CURVE('',#21199,#21261,#4150,.T.) ;
#26690 = EDGE_CURVE('',#21260,#21261,#18293,.T.) ;
#26691 = EDGE_CURVE('',#21198,#21262,#18294,.T.) ;
#26692 = EDGE_CURVE('',#21262,#21263,#4151,.T.) ;
#26693 = EDGE_CURVE('',#21263,#21264,#4152,.T.) ;
#26694 = EDGE_CURVE('',#21264,#21265,#4153,.T.) ;
#26695 = EDGE_CURVE('',#21265,#21266,#4154,.T.) ;
#26696 = EDGE_CURVE('',#21266,#21267,#4155,.T.) ;
#26697 = EDGE_CURVE('',#21267,#21268,#4156,.T.) ;
#26698 = EDGE_CURVE('',#21268,#21269,#4157,.T.) ;
#26699 = EDGE_CURVE('',#21270,#21269,#4158,.T.) ;
#26700 = EDGE_CURVE('',#21271,#21270,#4159,.T.) ;
#26701 = EDGE_CURVE('',#21272,#21271,#18295,.T.) ;
#26702 = EDGE_CURVE('',#21273,#21272,#4160,.T.) ;
#26703 = EDGE_CURVE('',#21274,#21273,#18296,.T.) ;
#26704 = EDGE_CURVE('',#21275,#21274,#4161,.T.) ;
#26705 = EDGE_CURVE('',#21276,#21275,#18297,.T.) ;
#26706 = EDGE_CURVE('',#21277,#21276,#4162,.T.) ;
#26707 = EDGE_CURVE('',#21278,#21277,#18298,.T.) ;
#26708 = EDGE_CURVE('',#21279,#21278,#4163,.T.) ;
#26709 = EDGE_CURVE('',#21280,#21279,#4164,.T.) ;
#26710 = EDGE_CURVE('',#21281,#21280,#4165,.T.) ;
#26711 = EDGE_CURVE('',#21281,#21282,#4166,.T.) ;
#26712 = EDGE_CURVE('',#21282,#21283,#4167,.T.) ;
#26713 = EDGE_CURVE('',#21261,#21283,#18299,.T.) ;
#26714 = EDGE_CURVE('',#21284,#21285,#18300,.T.) ;
#26715 = EDGE_CURVE('',#21285,#21286,#4168,.T.) ;
#26716 = EDGE_CURVE('',#21286,#21287,#18301,.T.) ;
#26717 = EDGE_CURVE('',#21287,#21284,#4169,.T.) ;
#26718 = EDGE_CURVE('',#21288,#21289,#4170,.T.) ;
#26719 = EDGE_CURVE('',#21289,#21290,#4171,.T.) ;
#26720 = EDGE_CURVE('',#21290,#21291,#4172,.T.) ;
#26721 = EDGE_CURVE('',#21291,#21288,#4173,.T.) ;
#26722 = EDGE_CURVE('',#21269,#21292,#18302,.T.) ;
#26723 = EDGE_CURVE('',#21292,#21293,#4174,.T.) ;
#26724 = EDGE_CURVE('',#21293,#21270,#269,.F.) ;
#26725 = EDGE_CURVE('',#21294,#21215,#18303,.T.) ;
#26726 = EDGE_CURVE('',#21214,#21295,#270,.F.) ;
#26727 = EDGE_CURVE('',#21295,#21294,#4175,.T.) ;
#26728 = EDGE_CURVE('',#21294,#21292,#4176,.T.) ;
#26729 = EDGE_CURVE('',#21295,#21293,#4177,.T.) ;
#26730 = EDGE_CURVE('',#21296,#21274,#18304,.T.) ;
#26731 = EDGE_CURVE('',#21273,#21297,#18305,.T.) ;
#26732 = EDGE_CURVE('',#21297,#21296,#18306,.T.) ;
#26733 = EDGE_CURVE('',#21210,#21298,#18307,.T.) ;
#26734 = EDGE_CURVE('',#21298,#21299,#18308,.T.) ;
#26735 = EDGE_CURVE('',#21299,#21211,#18309,.T.) ;
#26736 = EDGE_CURVE('',#21298,#21296,#4178,.T.) ;
#26737 = EDGE_CURVE('',#21297,#21299,#4179,.T.) ;
#26738 = EDGE_CURVE('',#21300,#21298,#4180,.T.) ;
#26739 = EDGE_CURVE('',#21301,#21300,#4181,.T.) ;
#26740 = EDGE_CURVE('',#21296,#21301,#4182,.T.) ;
#26741 = EDGE_CURVE('',#21300,#21209,#18310,.T.) ;
#26742 = EDGE_CURVE('',#21299,#21302,#4183,.T.) ;
#26743 = EDGE_CURVE('',#21212,#21302,#18311,.T.) ;
#26744 = EDGE_CURVE('',#21303,#21272,#18312,.T.) ;
#26745 = EDGE_CURVE('',#21271,#21304,#18313,.T.) ;
#26746 = EDGE_CURVE('',#21304,#21303,#18314,.T.) ;
#26747 = EDGE_CURVE('',#21302,#21305,#18315,.T.) ;
#26748 = EDGE_CURVE('',#21305,#21213,#18316,.T.) ;
#26749 = EDGE_CURVE('',#21302,#21303,#4184,.T.) ;
#26750 = EDGE_CURVE('',#21304,#21305,#4185,.T.) ;
#26751 = EDGE_CURVE('',#21303,#21297,#4186,.T.) ;
#26752 = EDGE_CURVE('',#21306,#21276,#18317,.T.) ;
#26753 = EDGE_CURVE('',#21275,#21301,#18318,.T.) ;
#26754 = EDGE_CURVE('',#21301,#21306,#18319,.T.) ;
#26755 = EDGE_CURVE('',#21208,#21307,#18320,.T.) ;
#26756 = EDGE_CURVE('',#21307,#21300,#18321,.T.) ;
#26757 = EDGE_CURVE('',#21307,#21306,#4187,.T.) ;
#26758 = EDGE_CURVE('',#21306,#21308,#4188,.T.) ;
#26759 = EDGE_CURVE('',#21277,#21308,#18322,.T.) ;
#26760 = EDGE_CURVE('',#21309,#21307,#4189,.T.) ;
#26761 = EDGE_CURVE('',#21308,#21309,#4190,.T.) ;
#26762 = EDGE_CURVE('',#21309,#21207,#18323,.T.) ;
#26763 = EDGE_CURVE('',#21310,#21311,#18324,.T.) ;
#26764 = EDGE_CURVE('',#21311,#21312,#271,.T.) ;
#26765 = EDGE_CURVE('',#21312,#21205,#272,.T.) ;
#26766 = EDGE_CURVE('',#21205,#21313,#273,.T.) ;
#26767 = EDGE_CURVE('',#21313,#21310,#274,.T.) ;
#26768 = EDGE_CURVE('',#21310,#21314,#4191,.T.) ;
#26769 = EDGE_CURVE('',#21314,#21315,#18325,.T.) ;
#26770 = EDGE_CURVE('',#21315,#21311,#4192,.T.) ;
#26771 = EDGE_CURVE('',#21314,#21316,#275,.T.) ;
#26772 = EDGE_CURVE('',#21316,#21279,#276,.T.) ;
#26773 = EDGE_CURVE('',#21279,#21317,#277,.T.) ;
#26774 = EDGE_CURVE('',#21317,#21315,#278,.T.) ;
#26775 = EDGE_CURVE('',#21318,#21310,#4193,.T.) ;
#26776 = EDGE_CURVE('',#21318,#21319,#4194,.T.) ;
#26777 = EDGE_CURVE('',#21314,#21319,#4195,.T.) ;
#26778 = EDGE_CURVE('',#21204,#21318,#279,.T.) ;
#26779 = EDGE_CURVE('',#21311,#21320,#4196,.T.) ;
#26780 = EDGE_CURVE('',#21206,#21320,#18326,.T.) ;
#26781 = EDGE_CURVE('',#21321,#21278,#18327,.T.) ;
#26782 = EDGE_CURVE('',#21308,#21321,#18328,.T.) ;
#26783 = EDGE_CURVE('',#21320,#21309,#18329,.T.) ;
#26784 = EDGE_CURVE('',#21320,#21321,#4197,.T.) ;
#26785 = EDGE_CURVE('',#21321,#21315,#4198,.T.) ;
#26786 = EDGE_CURVE('',#21322,#21223,#18330,.T.) ;
#26787 = EDGE_CURVE('',#21224,#21323,#18331,.T.) ;
#26788 = EDGE_CURVE('',#21323,#21322,#4199,.T.) ;
#26789 = EDGE_CURVE('',#21226,#21324,#18332,.T.) ;
#26790 = EDGE_CURVE('',#21324,#21323,#18333,.T.) ;
#26791 = EDGE_CURVE('',#21225,#21325,#18334,.T.) ;
#26792 = EDGE_CURVE('',#21325,#21324,#4200,.T.) ;
#26793 = EDGE_CURVE('',#21322,#21325,#18335,.T.) ;
#26794 = EDGE_CURVE('',#21322,#21285,#4201,.T.) ;
#26795 = EDGE_CURVE('',#21325,#21284,#4202,.T.) ;
#26796 = EDGE_CURVE('',#21323,#21286,#4203,.T.) ;
#26797 = EDGE_CURVE('',#21326,#21201,#1145,.T.) ;
#26798 = EDGE_CURVE('',#21259,#21327,#18336,.T.) ;
#26799 = EDGE_CURVE('',#21327,#21326,#1146,.T.) ;
#26800 = EDGE_CURVE('',#21327,#21328,#4204,.T.) ;
#26801 = EDGE_CURVE('',#21329,#21328,#1147,.T.) ;
#26802 = EDGE_CURVE('',#21326,#21329,#4205,.T.) ;
#26803 = EDGE_CURVE('',#21328,#21260,#18337,.T.) ;
#26804 = EDGE_CURVE('',#21191,#21197,#4206,.T.) ;
#26805 = EDGE_CURVE('',#21283,#21329,#1148,.T.) ;
#26806 = EDGE_CURVE('',#21202,#21282,#4207,.T.) ;
#26807 = EDGE_CURVE('',#21319,#21330,#4208,.T.) ;
#26808 = EDGE_CURVE('',#21330,#21281,#280,.T.) ;
#26809 = EDGE_CURVE('',#21280,#21319,#281,.T.) ;
#26810 = EDGE_CURVE('',#21293,#21304,#4209,.T.) ;
#26811 = EDGE_CURVE('',#21331,#21330,#4210,.T.) ;
#26812 = EDGE_CURVE('',#21203,#21331,#282,.T.) ;
#26813 = EDGE_CURVE('',#21331,#21318,#4211,.T.) ;
#26814 = EDGE_CURVE('',#21305,#21295,#4212,.T.) ;
#26815 = EDGE_CURVE('',#21332,#21333,#18338,.T.) ;
#26816 = EDGE_CURVE('',#21333,#21255,#18339,.T.) ;
#26817 = EDGE_CURVE('',#21254,#21332,#18340,.T.) ;
#26818 = EDGE_CURVE('',#21334,#21335,#18341,.T.) ;
#26819 = EDGE_CURVE('',#21335,#21333,#4213,.T.) ;
#26820 = EDGE_CURVE('',#21332,#21334,#4214,.T.) ;
#26821 = EDGE_CURVE('',#21252,#21335,#18342,.T.) ;
#26822 = EDGE_CURVE('',#21334,#21253,#18343,.T.) ;
#26823 = EDGE_CURVE('',#21336,#21337,#18344,.T.) ;
#26824 = EDGE_CURVE('',#21337,#21251,#18345,.T.) ;
#26825 = EDGE_CURVE('',#21258,#21336,#18346,.T.) ;
#26826 = EDGE_CURVE('',#21338,#21339,#18347,.T.) ;
#26827 = EDGE_CURVE('',#21339,#21337,#4215,.T.) ;
#26828 = EDGE_CURVE('',#21336,#21338,#4216,.T.) ;
#26829 = EDGE_CURVE('',#21256,#21339,#18348,.T.) ;
#26830 = EDGE_CURVE('',#21338,#21257,#18349,.T.) ;
#26831 = EDGE_CURVE('',#21340,#21341,#18350,.T.) ;
#26832 = EDGE_CURVE('',#21341,#21235,#18351,.T.) ;
#26833 = EDGE_CURVE('',#21242,#21340,#18352,.T.) ;
#26834 = EDGE_CURVE('',#21342,#21343,#18353,.T.) ;
#26835 = EDGE_CURVE('',#21343,#21341,#4217,.T.) ;
#26836 = EDGE_CURVE('',#21340,#21342,#4218,.T.) ;
#26837 = EDGE_CURVE('',#21240,#21343,#18354,.T.) ;
#26838 = EDGE_CURVE('',#21342,#21241,#18355,.T.) ;
#26839 = EDGE_CURVE('',#21344,#21345,#18356,.T.) ;
#26840 = EDGE_CURVE('',#21345,#21239,#18357,.T.) ;
#26841 = EDGE_CURVE('',#21238,#21344,#18358,.T.) ;
#26842 = EDGE_CURVE('',#21346,#21347,#18359,.T.) ;
#26843 = EDGE_CURVE('',#21347,#21345,#4219,.T.) ;
#26844 = EDGE_CURVE('',#21344,#21346,#4220,.T.) ;
#26845 = EDGE_CURVE('',#21236,#21347,#18360,.T.) ;
#26846 = EDGE_CURVE('',#21346,#21237,#18361,.T.) ;
#26847 = EDGE_CURVE('',#21348,#21349,#18362,.T.) ;
#26848 = EDGE_CURVE('',#21349,#21243,#18363,.T.) ;
#26849 = EDGE_CURVE('',#21250,#21348,#18364,.T.) ;
#26850 = EDGE_CURVE('',#21350,#21351,#18365,.T.) ;
#26851 = EDGE_CURVE('',#21351,#21349,#4221,.T.) ;
#26852 = EDGE_CURVE('',#21348,#21350,#4222,.T.) ;
#26853 = EDGE_CURVE('',#21248,#21351,#18366,.T.) ;
#26854 = EDGE_CURVE('',#21350,#21249,#18367,.T.) ;
#26855 = EDGE_CURVE('',#21352,#21353,#18368,.T.) ;
#26856 = EDGE_CURVE('',#21353,#21247,#18369,.T.) ;
#26857 = EDGE_CURVE('',#21246,#21352,#18370,.T.) ;
#26858 = EDGE_CURVE('',#21354,#21355,#18371,.T.) ;
#26859 = EDGE_CURVE('',#21355,#21353,#4223,.T.) ;
#26860 = EDGE_CURVE('',#21352,#21354,#4224,.T.) ;
#26861 = EDGE_CURVE('',#21244,#21355,#18372,.T.) ;
#26862 = EDGE_CURVE('',#21354,#21245,#18373,.T.) ;
#26863 = EDGE_CURVE('',#21356,#21357,#18374,.T.) ;
#26864 = EDGE_CURVE('',#21357,#21227,#18375,.T.) ;
#26865 = EDGE_CURVE('',#21228,#21356,#18376,.T.) ;
#26866 = EDGE_CURVE('',#21358,#21359,#18377,.T.) ;
#26867 = EDGE_CURVE('',#21359,#21357,#4225,.T.) ;
#26868 = EDGE_CURVE('',#21356,#21358,#4226,.T.) ;
#26869 = EDGE_CURVE('',#21233,#21359,#18378,.T.) ;
#26870 = EDGE_CURVE('',#21358,#21234,#18379,.T.) ;
#26871 = EDGE_CURVE('',#21360,#21361,#18380,.T.) ;
#26872 = EDGE_CURVE('',#21361,#21232,#18381,.T.) ;
#26873 = EDGE_CURVE('',#21231,#21360,#18382,.T.) ;
#26874 = EDGE_CURVE('',#21362,#21363,#18383,.T.) ;
#26875 = EDGE_CURVE('',#21363,#21361,#4227,.T.) ;
#26876 = EDGE_CURVE('',#21360,#21362,#4228,.T.) ;
#26877 = EDGE_CURVE('',#21229,#21363,#18384,.T.) ;
#26878 = EDGE_CURVE('',#21362,#21230,#18385,.T.) ;
#26879 = EDGE_CURVE('',#21361,#21359,#4229,.T.) ;
#26880 = EDGE_CURVE('',#21357,#21363,#4230,.T.) ;
#26881 = EDGE_CURVE('',#21353,#21351,#4231,.T.) ;
#26882 = EDGE_CURVE('',#21349,#21355,#4232,.T.) ;
#26883 = EDGE_CURVE('',#21341,#21347,#4233,.T.) ;
#26884 = EDGE_CURVE('',#21345,#21343,#4234,.T.) ;
#26885 = EDGE_CURVE('',#21333,#21339,#4235,.T.) ;
#26886 = EDGE_CURVE('',#21337,#21335,#4236,.T.) ;
#26887 = EDGE_CURVE('',#21364,#21365,#4237,.T.) ;
#26888 = EDGE_CURVE('',#21366,#21364,#4238,.T.) ;
#26889 = EDGE_CURVE('',#21367,#21366,#4239,.T.) ;
#26890 = EDGE_CURVE('',#21365,#21367,#4240,.T.) ;
#26891 = EDGE_CURVE('',#21367,#21290,#4241,.T.) ;
#26892 = EDGE_CURVE('',#21365,#21289,#4242,.T.) ;
#26893 = EDGE_CURVE('',#21366,#21291,#4243,.T.) ;
#26894 = EDGE_CURVE('',#21262,#21222,#4244,.T.) ;
#26895 = EDGE_CURVE('',#21221,#21263,#4245,.T.) ;
#26896 = EDGE_CURVE('',#21324,#21287,#4246,.T.) ;
#26897 = EDGE_CURVE('',#21364,#21288,#4247,.T.) ;
#26898 = EDGE_CURVE('',#21216,#21268,#4248,.T.) ;
#26899 = EDGE_CURVE('',#21217,#21267,#4249,.T.) ;
#26900 = EDGE_CURVE('',#21218,#21266,#4250,.T.) ;
#26901 = EDGE_CURVE('',#21219,#21265,#4251,.T.) ;
#26902 = EDGE_CURVE('',#21220,#21264,#4252,.T.) ;
#26903 = EDGE_CURVE('',#21368,#21369,#4253,.T.) ;
#26904 = EDGE_CURVE('',#21369,#21370,#4254,.T.) ;
#26905 = EDGE_CURVE('',#21371,#21370,#4255,.T.) ;
#26906 = EDGE_CURVE('',#21368,#21371,#4256,.T.) ;
#26907 = EDGE_CURVE('',#21372,#21368,#4257,.T.) ;
#26908 = EDGE_CURVE('',#21373,#21371,#4258,.T.) ;
#26909 = EDGE_CURVE('',#21372,#21373,#4259,.T.) ;
#26910 = EDGE_CURVE('',#21374,#21372,#4260,.T.) ;
#26911 = EDGE_CURVE('',#21375,#21373,#4261,.T.) ;
#26912 = EDGE_CURVE('',#21374,#21375,#4262,.T.) ;
#26913 = EDGE_CURVE('',#21369,#21374,#4263,.T.) ;
#26914 = EDGE_CURVE('',#21370,#21375,#4264,.T.) ;
#26915 = EDGE_CURVE('',#21376,#21377,#18386,.T.) ;
#26916 = EDGE_CURVE('',#21377,#21378,#18387,.T.) ;
#26917 = EDGE_CURVE('',#21379,#21378,#18388,.T.) ;
#26918 = EDGE_CURVE('',#21378,#21379,#18389,.T.) ;
#26919 = EDGE_CURVE('',#21377,#21376,#18390,.T.) ;
#26920 = EDGE_CURVE('',#21376,#21380,#4265,.T.) ;
#26921 = EDGE_CURVE('',#21380,#21380,#18391,.T.) ;
#26922 = EDGE_CURVE('',#21381,#21381,#18392,.T.) ;
#26923 = EDGE_CURVE('',#21381,#21379,#4266,.T.) ;
#26924 = EDGE_CURVE('',#21382,#21383,#18393,.T.) ;
#26925 = EDGE_CURVE('',#21383,#21384,#18394,.T.) ;
#26926 = EDGE_CURVE('',#21385,#21384,#18395,.T.) ;
#26927 = EDGE_CURVE('',#21384,#21385,#18396,.T.) ;
#26928 = EDGE_CURVE('',#21383,#21382,#18397,.T.) ;
#26929 = EDGE_CURVE('',#21382,#21386,#4267,.T.) ;
#26930 = EDGE_CURVE('',#21386,#21386,#18398,.T.) ;
#26931 = EDGE_CURVE('',#21387,#21387,#18399,.T.) ;
#26932 = EDGE_CURVE('',#21387,#21385,#4268,.T.) ;
#26933 = EDGE_CURVE('',#21388,#21388,#18400,.T.) ;
#26934 = EDGE_CURVE('',#21388,#21389,#18401,.T.) ;
#26935 = EDGE_CURVE('',#21389,#21389,#18402,.T.) ;
#26936 = EDGE_CURVE('',#21388,#21390,#4269,.T.) ;
#26937 = EDGE_CURVE('',#21390,#21390,#18403,.T.) ;
#26938 = EDGE_CURVE('',#21391,#21391,#18404,.T.) ;
#26939 = EDGE_CURVE('',#21392,#21392,#18405,.T.) ;
#26940 = EDGE_CURVE('',#21392,#21391,#4270,.T.) ;
#26941 = EDGE_CURVE('',#21393,#21394,#18406,.T.) ;
#26942 = EDGE_CURVE('',#21395,#21393,#18407,.F.) ;
#26943 = EDGE_CURVE('',#21396,#21395,#18408,.T.) ;
#26944 = EDGE_CURVE('',#21396,#21394,#18409,.T.) ;
#26945 = EDGE_CURVE('',#21397,#21398,#18410,.T.) ;
#26946 = EDGE_CURVE('',#21398,#21399,#283,.T.) ;
#26947 = EDGE_CURVE('',#21399,#21397,#284,.T.) ;
#26948 = EDGE_CURVE('',#21397,#21395,#4271,.T.) ;
#26949 = EDGE_CURVE('',#21393,#21398,#4272,.T.) ;
#26950 = EDGE_CURVE('',#21400,#21401,#18411,.F.) ;
#26951 = EDGE_CURVE('',#21402,#21400,#18412,.F.) ;
#26952 = EDGE_CURVE('',#21401,#21402,#18413,.F.) ;
#26953 = EDGE_CURVE('',#21403,#21404,#18414,.T.) ;
#26954 = EDGE_CURVE('',#21404,#21405,#285,.T.) ;
#26955 = EDGE_CURVE('',#21405,#21406,#286,.T.) ;
#26956 = EDGE_CURVE('',#21406,#21407,#287,.T.) ;
#26957 = EDGE_CURVE('',#21407,#21403,#288,.T.) ;
#26958 = EDGE_CURVE('',#21403,#21402,#4273,.T.) ;
#26959 = EDGE_CURVE('',#21400,#21404,#4274,.T.) ;
#26960 = EDGE_CURVE('',#21408,#21409,#18415,.T.) ;
#26961 = EDGE_CURVE('',#21410,#21408,#18416,.F.) ;
#26962 = EDGE_CURVE('',#21411,#21410,#18417,.T.) ;
#26963 = EDGE_CURVE('',#21411,#21409,#18418,.T.) ;
#26964 = EDGE_CURVE('',#21412,#21413,#18419,.T.) ;
#26965 = EDGE_CURVE('',#21413,#21414,#289,.T.) ;
#26966 = EDGE_CURVE('',#21414,#21412,#290,.T.) ;
#26967 = EDGE_CURVE('',#21412,#21410,#4275,.T.) ;
#26968 = EDGE_CURVE('',#21408,#21413,#4276,.T.) ;
#26969 = EDGE_CURVE('',#21394,#21411,#4277,.T.) ;
#26970 = EDGE_CURVE('',#21410,#21393,#4278,.T.) ;
#26971 = EDGE_CURVE('',#21415,#21416,#18420,.T.) ;
#26972 = EDGE_CURVE('',#21417,#21415,#18421,.F.) ;
#26973 = EDGE_CURVE('',#21418,#21417,#18422,.T.) ;
#26974 = EDGE_CURVE('',#21418,#21416,#18423,.T.) ;
#26975 = EDGE_CURVE('',#21419,#21420,#18424,.T.) ;
#26976 = EDGE_CURVE('',#21420,#21421,#291,.T.) ;
#26977 = EDGE_CURVE('',#21421,#21419,#292,.T.) ;
#26978 = EDGE_CURVE('',#21419,#21417,#4279,.T.) ;
#26979 = EDGE_CURVE('',#21415,#21420,#4280,.T.) ;
#26980 = EDGE_CURVE('',#21422,#21423,#18425,.F.) ;
#26981 = EDGE_CURVE('',#21424,#21422,#18426,.F.) ;
#26982 = EDGE_CURVE('',#21423,#21424,#18427,.F.) ;
#26983 = EDGE_CURVE('',#21425,#21426,#18428,.T.) ;
#26984 = EDGE_CURVE('',#21426,#21427,#293,.T.) ;
#26985 = EDGE_CURVE('',#21427,#21428,#294,.T.) ;
#26986 = EDGE_CURVE('',#21428,#21429,#295,.T.) ;
#26987 = EDGE_CURVE('',#21429,#21425,#296,.T.) ;
#26988 = EDGE_CURVE('',#21425,#21424,#4281,.T.) ;
#26989 = EDGE_CURVE('',#21422,#21426,#4282,.T.) ;
#26990 = EDGE_CURVE('',#21409,#21423,#4283,.T.) ;
#26991 = EDGE_CURVE('',#21424,#21408,#4284,.T.) ;
#26992 = EDGE_CURVE('',#21430,#21431,#18429,.T.) ;
#26993 = EDGE_CURVE('',#21432,#21430,#18430,.F.) ;
#26994 = EDGE_CURVE('',#21433,#21432,#18431,.T.) ;
#26995 = EDGE_CURVE('',#21433,#21431,#18432,.T.) ;
#26996 = EDGE_CURVE('',#21434,#21435,#18433,.T.) ;
#26997 = EDGE_CURVE('',#21435,#21436,#297,.T.) ;
#26998 = EDGE_CURVE('',#21436,#21434,#298,.T.) ;
#26999 = EDGE_CURVE('',#21434,#21432,#4285,.T.) ;
#27000 = EDGE_CURVE('',#21430,#21435,#4286,.T.) ;
#27001 = EDGE_CURVE('',#21437,#21438,#18434,.T.) ;
#27002 = EDGE_CURVE('',#21439,#21437,#18435,.F.) ;
#27003 = EDGE_CURVE('',#21440,#21439,#18436,.T.) ;
#27004 = EDGE_CURVE('',#21440,#21438,#18437,.T.) ;
#27005 = EDGE_CURVE('',#21441,#21442,#18438,.T.) ;
#27006 = EDGE_CURVE('',#21442,#21443,#299,.T.) ;
#27007 = EDGE_CURVE('',#21443,#21441,#300,.T.) ;
#27008 = EDGE_CURVE('',#21441,#21439,#4287,.T.) ;
#27009 = EDGE_CURVE('',#21437,#21442,#4288,.T.) ;
#27010 = EDGE_CURVE('',#21423,#21440,#4289,.T.) ;
#27011 = EDGE_CURVE('',#21439,#21422,#4290,.T.) ;
#27012 = EDGE_CURVE('',#21444,#21445,#18439,.F.) ;
#27013 = EDGE_CURVE('',#21446,#21444,#18440,.F.) ;
#27014 = EDGE_CURVE('',#21445,#21446,#18441,.F.) ;
#27015 = EDGE_CURVE('',#21447,#21448,#18442,.T.) ;
#27016 = EDGE_CURVE('',#21448,#21449,#301,.T.) ;
#27017 = EDGE_CURVE('',#21449,#21450,#302,.T.) ;
#27018 = EDGE_CURVE('',#21450,#21451,#303,.T.) ;
#27019 = EDGE_CURVE('',#21451,#21447,#304,.T.) ;
#27020 = EDGE_CURVE('',#21447,#21446,#4291,.T.) ;
#27021 = EDGE_CURVE('',#21444,#21448,#4292,.T.) ;
#27022 = EDGE_CURVE('',#21452,#21453,#18443,.T.) ;
#27023 = EDGE_CURVE('',#21454,#21452,#18444,.F.) ;
#27024 = EDGE_CURVE('',#21455,#21454,#18445,.T.) ;
#27025 = EDGE_CURVE('',#21455,#21453,#18446,.T.) ;
#27026 = EDGE_CURVE('',#21456,#21457,#18447,.T.) ;
#27027 = EDGE_CURVE('',#21457,#21458,#305,.T.) ;
#27028 = EDGE_CURVE('',#21458,#21456,#306,.T.) ;
#27029 = EDGE_CURVE('',#21456,#21454,#4293,.T.) ;
#27030 = EDGE_CURVE('',#21452,#21457,#4294,.T.) ;
#27031 = EDGE_CURVE('',#21438,#21455,#4295,.T.) ;
#27032 = EDGE_CURVE('',#21454,#21437,#4296,.T.) ;
#27033 = EDGE_CURVE('',#21459,#21460,#18448,.T.) ;
#27034 = EDGE_CURVE('',#21461,#21459,#18449,.F.) ;
#27035 = EDGE_CURVE('',#21462,#21461,#18450,.T.) ;
#27036 = EDGE_CURVE('',#21462,#21460,#18451,.T.) ;
#27037 = EDGE_CURVE('',#21463,#21464,#18452,.T.) ;
#27038 = EDGE_CURVE('',#21464,#21465,#307,.T.) ;
#27039 = EDGE_CURVE('',#21465,#21463,#308,.T.) ;
#27040 = EDGE_CURVE('',#21463,#21461,#4297,.T.) ;
#27041 = EDGE_CURVE('',#21459,#21464,#4298,.T.) ;
#27042 = EDGE_CURVE('',#21466,#21467,#18453,.F.) ;
#27043 = EDGE_CURVE('',#21468,#21466,#18454,.F.) ;
#27044 = EDGE_CURVE('',#21467,#21468,#18455,.F.) ;
#27045 = EDGE_CURVE('',#21469,#21470,#18456,.T.) ;
#27046 = EDGE_CURVE('',#21470,#21471,#309,.T.) ;
#27047 = EDGE_CURVE('',#21471,#21472,#310,.T.) ;
#27048 = EDGE_CURVE('',#21472,#21473,#311,.T.) ;
#27049 = EDGE_CURVE('',#21473,#21469,#312,.T.) ;
#27050 = EDGE_CURVE('',#21469,#21468,#4299,.T.) ;
#27051 = EDGE_CURVE('',#21466,#21470,#4300,.T.) ;
#27052 = EDGE_CURVE('',#21453,#21467,#4301,.T.) ;
#27053 = EDGE_CURVE('',#21468,#21452,#4302,.T.) ;
#27054 = EDGE_CURVE('',#21474,#21475,#18457,.T.) ;
#27055 = EDGE_CURVE('',#21476,#21474,#18458,.F.) ;
#27056 = EDGE_CURVE('',#21477,#21476,#18459,.T.) ;
#27057 = EDGE_CURVE('',#21477,#21475,#18460,.T.) ;
#27058 = EDGE_CURVE('',#21478,#21479,#18461,.T.) ;
#27059 = EDGE_CURVE('',#21479,#21480,#313,.T.) ;
#27060 = EDGE_CURVE('',#21480,#21478,#314,.T.) ;
#27061 = EDGE_CURVE('',#21478,#21476,#4303,.T.) ;
#27062 = EDGE_CURVE('',#21474,#21479,#4304,.T.) ;
#27063 = EDGE_CURVE('',#21467,#21477,#4305,.T.) ;
#27064 = EDGE_CURVE('',#21476,#21466,#4306,.T.) ;
#27065 = EDGE_CURVE('',#21475,#21462,#4307,.T.) ;
#27066 = EDGE_CURVE('',#21461,#21474,#4308,.T.) ;
#27067 = EDGE_CURVE('',#21460,#21445,#4309,.T.) ;
#27068 = EDGE_CURVE('',#21446,#21459,#4310,.T.) ;
#27069 = EDGE_CURVE('',#21445,#21433,#4311,.T.) ;
#27070 = EDGE_CURVE('',#21432,#21444,#4312,.T.) ;
#27071 = EDGE_CURVE('',#21431,#21418,#4313,.T.) ;
#27072 = EDGE_CURVE('',#21417,#21430,#4314,.T.) ;
#27073 = EDGE_CURVE('',#21416,#21401,#4315,.T.) ;
#27074 = EDGE_CURVE('',#21402,#21415,#4316,.T.) ;
#27075 = EDGE_CURVE('',#21401,#21396,#4317,.T.) ;
#27076 = EDGE_CURVE('',#21395,#21400,#4318,.T.) ;
#27077 = EDGE_CURVE('',#21398,#21412,#4319,.T.) ;
#27078 = EDGE_CURVE('',#21413,#21425,#4320,.T.) ;
#27079 = EDGE_CURVE('',#21428,#21414,#4321,.T.) ;
#27080 = EDGE_CURVE('',#21426,#21441,#4322,.T.) ;
#27081 = EDGE_CURVE('',#21443,#21428,#4323,.T.) ;
#27082 = EDGE_CURVE('',#21442,#21456,#4324,.T.) ;
#27083 = EDGE_CURVE('',#21458,#21443,#4325,.T.) ;
#27084 = EDGE_CURVE('',#21457,#21469,#4326,.T.) ;
#27085 = EDGE_CURVE('',#21472,#21458,#4327,.T.) ;
#27086 = EDGE_CURVE('',#21470,#21478,#4328,.T.) ;
#27087 = EDGE_CURVE('',#21480,#21472,#4329,.T.) ;
#27088 = EDGE_CURVE('',#21481,#21481,#18462,.T.) ;
#27089 = EDGE_CURVE('',#21450,#21465,#4330,.T.) ;
#27090 = EDGE_CURVE('',#21464,#21447,#4331,.T.) ;
#27091 = EDGE_CURVE('',#21465,#21480,#4332,.T.) ;
#27092 = EDGE_CURVE('',#21479,#21463,#4333,.T.) ;
#27093 = EDGE_CURVE('',#21414,#21399,#4334,.T.) ;
#27094 = EDGE_CURVE('',#21399,#21406,#4335,.T.) ;
#27095 = EDGE_CURVE('',#21404,#21397,#4336,.T.) ;
#27096 = EDGE_CURVE('',#21406,#21421,#4337,.T.) ;
#27097 = EDGE_CURVE('',#21420,#21403,#4338,.T.) ;
#27098 = EDGE_CURVE('',#21421,#21436,#4339,.T.) ;
#27099 = EDGE_CURVE('',#21435,#21419,#4340,.T.) ;
#27100 = EDGE_CURVE('',#21436,#21450,#4341,.T.) ;
#27101 = EDGE_CURVE('',#21448,#21434,#4342,.T.) ;
#27102 = EDGE_CURVE('',#21481,#21482,#18463,.T.) ;
#27103 = EDGE_CURVE('',#21482,#21482,#18464,.T.) ;
#27104 = EDGE_CURVE('',#21482,#21483,#4343,.T.) ;
#27105 = EDGE_CURVE('',#21484,#21483,#18465,.T.) ;
#27106 = EDGE_CURVE('',#21483,#21484,#18466,.T.) ;
#27107 = EDGE_CURVE('',#21485,#21485,#18467,.T.) ;
#27108 = EDGE_CURVE('',#21485,#21484,#18468,.T.) ;
#27109 = EDGE_CURVE('',#21486,#21487,#18469,.F.) ;
#27110 = EDGE_CURVE('',#21488,#21486,#18470,.F.) ;
#27111 = EDGE_CURVE('',#21487,#21488,#18471,.F.) ;
#27112 = EDGE_CURVE('',#21489,#21490,#18472,.F.) ;
#27113 = EDGE_CURVE('',#21491,#21489,#18473,.F.) ;
#27114 = EDGE_CURVE('',#21490,#21491,#18474,.F.) ;
#27115 = EDGE_CURVE('',#21492,#21493,#18475,.F.) ;
#27116 = EDGE_CURVE('',#21494,#21492,#18476,.F.) ;
#27117 = EDGE_CURVE('',#21493,#21494,#18477,.F.) ;
#27118 = EDGE_CURVE('',#21495,#21494,#4344,.T.) ;
#27119 = EDGE_CURVE('',#21492,#21496,#4345,.T.) ;
#27120 = EDGE_CURVE('',#21496,#21495,#315,.T.) ;
#27121 = EDGE_CURVE('',#21489,#21493,#4346,.T.) ;
#27122 = EDGE_CURVE('',#21494,#21491,#4347,.T.) ;
#27123 = EDGE_CURVE('',#21497,#21498,#18478,.F.) ;
#27124 = EDGE_CURVE('',#21499,#21497,#18479,.F.) ;
#27125 = EDGE_CURVE('',#21498,#21499,#18480,.F.) ;
#27126 = EDGE_CURVE('',#21500,#21501,#18481,.F.) ;
#27127 = EDGE_CURVE('',#21502,#21500,#18482,.F.) ;
#27128 = EDGE_CURVE('',#21501,#21502,#18483,.F.) ;
#27129 = EDGE_CURVE('',#21500,#21492,#4348,.T.) ;
#27130 = EDGE_CURVE('',#21493,#21502,#4349,.T.) ;
#27131 = EDGE_CURVE('',#21497,#21501,#4350,.T.) ;
#27132 = EDGE_CURVE('',#21502,#21499,#4351,.T.) ;
#27133 = EDGE_CURVE('',#21503,#21504,#18484,.T.) ;
#27134 = EDGE_CURVE('',#21504,#21500,#4352,.T.) ;
#27135 = EDGE_CURVE('',#21501,#21503,#4353,.T.) ;
#27136 = EDGE_CURVE('',#21490,#21498,#4354,.T.) ;
#27137 = EDGE_CURVE('',#21499,#21489,#4355,.T.) ;
#27138 = EDGE_CURVE('',#21505,#21497,#4356,.T.) ;
#27139 = EDGE_CURVE('',#21498,#21506,#4357,.T.) ;
#27140 = EDGE_CURVE('',#21506,#21505,#316,.T.) ;
#27141 = EDGE_CURVE('',#21487,#21490,#4358,.T.) ;
#27142 = EDGE_CURVE('',#21491,#21486,#4359,.T.) ;
#27143 = EDGE_CURVE('',#21506,#21487,#4360,.T.) ;
#27144 = EDGE_CURVE('',#21488,#21505,#4361,.T.) ;
#27145 = EDGE_CURVE('',#21496,#21488,#4362,.T.) ;
#27146 = EDGE_CURVE('',#21486,#21495,#4363,.T.) ;
#27147 = EDGE_CURVE('',#21496,#21504,#4364,.T.) ;
#27148 = EDGE_CURVE('',#21503,#21505,#4365,.T.) ;
#27149 = EDGE_CURVE('',#21507,#21507,#18485,.T.) ;
#27150 = EDGE_CURVE('',#21507,#21508,#18486,.T.) ;
#27151 = EDGE_CURVE('',#21508,#21509,#18487,.T.) ;
#27152 = EDGE_CURVE('',#21509,#21508,#18488,.T.) ;
#27153 = EDGE_CURVE('',#21509,#21510,#4366,.T.) ;
#27154 = EDGE_CURVE('',#21511,#21510,#18489,.T.) ;
#27155 = EDGE_CURVE('',#21510,#21511,#18490,.T.) ;
#27156 = EDGE_CURVE('',#21512,#21513,#4367,.T.) ;
#27157 = EDGE_CURVE('',#21513,#21514,#317,.T.) ;
#27158 = EDGE_CURVE('',#21514,#21515,#4368,.T.) ;
#27159 = EDGE_CURVE('',#21512,#21515,#318,.T.) ;
#27160 = EDGE_CURVE('',#21513,#21516,#4369,.T.) ;
#27161 = EDGE_CURVE('',#21516,#21517,#319,.T.) ;
#27162 = EDGE_CURVE('',#21517,#21514,#4370,.T.) ;
#27163 = EDGE_CURVE('',#21516,#21518,#4371,.T.) ;
#27164 = EDGE_CURVE('',#21518,#21519,#320,.T.) ;
#27165 = EDGE_CURVE('',#21519,#21517,#4372,.T.) ;
#27166 = EDGE_CURVE('',#21518,#21520,#4373,.T.) ;
#27167 = EDGE_CURVE('',#21520,#21521,#321,.T.) ;
#27168 = EDGE_CURVE('',#21521,#21519,#4374,.T.) ;
#27169 = EDGE_CURVE('',#21520,#21522,#4375,.T.) ;
#27170 = EDGE_CURVE('',#21522,#21523,#322,.T.) ;
#27171 = EDGE_CURVE('',#21523,#21521,#4376,.T.) ;
#27172 = EDGE_CURVE('',#21524,#21525,#4377,.T.) ;
#27173 = EDGE_CURVE('',#21525,#21526,#323,.T.) ;
#27174 = EDGE_CURVE('',#21526,#21527,#4378,.T.) ;
#27175 = EDGE_CURVE('',#21527,#21524,#324,.T.) ;
#27176 = EDGE_CURVE('',#21528,#21526,#4379,.T.) ;
#27177 = EDGE_CURVE('',#21525,#21529,#4380,.T.) ;
#27178 = EDGE_CURVE('',#21529,#21528,#325,.T.) ;
#27179 = EDGE_CURVE('',#21522,#21524,#4381,.T.) ;
#27180 = EDGE_CURVE('',#21527,#21523,#4382,.T.) ;
#27181 = EDGE_CURVE('',#21530,#21528,#4383,.T.) ;
#27182 = EDGE_CURVE('',#21529,#21531,#4384,.T.) ;
#27183 = EDGE_CURVE('',#21531,#21530,#326,.T.) ;
#27184 = EDGE_CURVE('',#21532,#21530,#4385,.T.) ;
#27185 = EDGE_CURVE('',#21531,#21533,#4386,.T.) ;
#27186 = EDGE_CURVE('',#21533,#21532,#327,.T.) ;
#27187 = EDGE_CURVE('',#21534,#21532,#4387,.T.) ;
#27188 = EDGE_CURVE('',#21533,#21535,#4388,.T.) ;
#27189 = EDGE_CURVE('',#21535,#21534,#328,.T.) ;
#27190 = EDGE_CURVE('',#21515,#21534,#4389,.T.) ;
#27191 = EDGE_CURVE('',#21535,#21512,#4390,.T.) ;
#27192 = EDGE_CURVE('',#21517,#21536,#4391,.T.) ;
#27193 = EDGE_CURVE('',#21537,#21536,#4392,.T.) ;
#27194 = EDGE_CURVE('',#21514,#21537,#4393,.T.) ;
#27195 = EDGE_CURVE('',#21519,#21538,#4394,.T.) ;
#27196 = EDGE_CURVE('',#21536,#21538,#4395,.T.) ;
#27197 = EDGE_CURVE('',#21521,#21539,#4396,.T.) ;
#27198 = EDGE_CURVE('',#21538,#21539,#4397,.T.) ;
#27199 = EDGE_CURVE('',#21523,#21540,#4398,.T.) ;
#27200 = EDGE_CURVE('',#21539,#21540,#4399,.T.) ;
#27201 = EDGE_CURVE('',#21527,#21541,#4400,.T.) ;
#27202 = EDGE_CURVE('',#21540,#21541,#4401,.T.) ;
#27203 = EDGE_CURVE('',#21526,#21542,#4402,.T.) ;
#27204 = EDGE_CURVE('',#21541,#21542,#4403,.T.) ;
#27205 = EDGE_CURVE('',#21543,#21543,#18491,.T.) ;
#27206 = EDGE_CURVE('',#21544,#21545,#4404,.T.) ;
#27207 = EDGE_CURVE('',#21545,#21546,#329,.T.) ;
#27208 = EDGE_CURVE('',#21546,#21547,#4405,.T.) ;
#27209 = EDGE_CURVE('',#21544,#21547,#330,.T.) ;
#27210 = EDGE_CURVE('',#21545,#21548,#4406,.T.) ;
#27211 = EDGE_CURVE('',#21548,#21549,#331,.T.) ;
#27212 = EDGE_CURVE('',#21549,#21546,#4407,.T.) ;
#27213 = EDGE_CURVE('',#21548,#21550,#4408,.T.) ;
#27214 = EDGE_CURVE('',#21550,#21551,#332,.T.) ;
#27215 = EDGE_CURVE('',#21551,#21549,#4409,.T.) ;
#27216 = EDGE_CURVE('',#21550,#21552,#4410,.T.) ;
#27217 = EDGE_CURVE('',#21552,#21542,#333,.T.) ;
#27218 = EDGE_CURVE('',#21542,#21551,#4411,.T.) ;
#27219 = EDGE_CURVE('',#21552,#21553,#4412,.T.) ;
#27220 = EDGE_CURVE('',#21553,#21541,#334,.T.) ;
#27221 = EDGE_CURVE('',#21553,#21554,#4413,.T.) ;
#27222 = EDGE_CURVE('',#21554,#21540,#335,.T.) ;
#27223 = EDGE_CURVE('',#21554,#21555,#4414,.T.) ;
#27224 = EDGE_CURVE('',#21555,#21539,#336,.T.) ;
#27225 = EDGE_CURVE('',#21555,#21556,#4415,.T.) ;
#27226 = EDGE_CURVE('',#21556,#21538,#337,.T.) ;
#27227 = EDGE_CURVE('',#21556,#21557,#4416,.T.) ;
#27228 = EDGE_CURVE('',#21557,#21536,#338,.T.) ;
#27229 = EDGE_CURVE('',#21557,#21558,#4417,.T.) ;
#27230 = EDGE_CURVE('',#21558,#21537,#339,.T.) ;
#27231 = EDGE_CURVE('',#21559,#21537,#4418,.T.) ;
#27232 = EDGE_CURVE('',#21558,#21560,#4419,.T.) ;
#27233 = EDGE_CURVE('',#21560,#21559,#340,.T.) ;
#27234 = EDGE_CURVE('',#21547,#21559,#4420,.T.) ;
#27235 = EDGE_CURVE('',#21560,#21544,#4421,.T.) ;
#27236 = EDGE_CURVE('',#21515,#21559,#4422,.T.) ;
#27237 = EDGE_CURVE('',#21534,#21547,#4423,.T.) ;
#27238 = EDGE_CURVE('',#21532,#21546,#4424,.T.) ;
#27239 = EDGE_CURVE('',#21511,#21543,#18492,.T.) ;
#27240 = EDGE_CURVE('',#21530,#21549,#4425,.T.) ;
#27241 = EDGE_CURVE('',#21528,#21551,#4426,.T.) ;
#27242 = EDGE_CURVE('',#21561,#21562,#4427,.T.) ;
#27243 = EDGE_CURVE('',#21562,#21563,#341,.T.) ;
#27244 = EDGE_CURVE('',#21563,#21564,#4428,.T.) ;
#27245 = EDGE_CURVE('',#21561,#21564,#342,.T.) ;
#27246 = EDGE_CURVE('',#21562,#21565,#4429,.T.) ;
#27247 = EDGE_CURVE('',#21565,#21566,#343,.T.) ;
#27248 = EDGE_CURVE('',#21566,#21563,#4430,.T.) ;
#27249 = EDGE_CURVE('',#21565,#21567,#4431,.T.) ;
#27250 = EDGE_CURVE('',#21567,#21568,#344,.T.) ;
#27251 = EDGE_CURVE('',#21568,#21566,#4432,.T.) ;
#27252 = EDGE_CURVE('',#21567,#21569,#4433,.T.) ;
#27253 = EDGE_CURVE('',#21569,#21570,#345,.T.) ;
#27254 = EDGE_CURVE('',#21570,#21568,#4434,.T.) ;
#27255 = EDGE_CURVE('',#21569,#21571,#4435,.T.) ;
#27256 = EDGE_CURVE('',#21571,#21572,#346,.T.) ;
#27257 = EDGE_CURVE('',#21572,#21570,#4436,.T.) ;
#27258 = EDGE_CURVE('',#21573,#21572,#4437,.T.) ;
#27259 = EDGE_CURVE('',#21571,#21574,#4438,.T.) ;
#27260 = EDGE_CURVE('',#21574,#21573,#347,.T.) ;
#27261 = EDGE_CURVE('',#21575,#21573,#4439,.T.) ;
#27262 = EDGE_CURVE('',#21574,#21576,#4440,.T.) ;
#27263 = EDGE_CURVE('',#21576,#21575,#348,.T.) ;
#27264 = EDGE_CURVE('',#21577,#21575,#4441,.T.) ;
#27265 = EDGE_CURVE('',#21576,#21578,#4442,.T.) ;
#27266 = EDGE_CURVE('',#21578,#21577,#349,.T.) ;
#27267 = EDGE_CURVE('',#21579,#21577,#4443,.T.) ;
#27268 = EDGE_CURVE('',#21578,#21580,#4444,.T.) ;
#27269 = EDGE_CURVE('',#21580,#21579,#350,.T.) ;
#27270 = EDGE_CURVE('',#21581,#21579,#4445,.T.) ;
#27271 = EDGE_CURVE('',#21580,#21582,#4446,.T.) ;
#27272 = EDGE_CURVE('',#21582,#21581,#351,.T.) ;
#27273 = EDGE_CURVE('',#21583,#21581,#4447,.T.) ;
#27274 = EDGE_CURVE('',#21582,#21584,#4448,.T.) ;
#27275 = EDGE_CURVE('',#21584,#21583,#352,.T.) ;
#27276 = EDGE_CURVE('',#21564,#21583,#4449,.T.) ;
#27277 = EDGE_CURVE('',#21584,#21561,#4450,.T.) ;
#27278 = EDGE_CURVE('',#21585,#21577,#4451,.T.) ;
#27279 = EDGE_CURVE('',#21586,#21585,#4452,.T.) ;
#27280 = EDGE_CURVE('',#21586,#21575,#4453,.T.) ;
#27281 = EDGE_CURVE('',#21587,#21579,#4454,.T.) ;
#27282 = EDGE_CURVE('',#21585,#21587,#4455,.T.) ;
#27283 = EDGE_CURVE('',#21588,#21581,#4456,.T.) ;
#27284 = EDGE_CURVE('',#21587,#21588,#4457,.T.) ;
#27285 = EDGE_CURVE('',#21589,#21583,#4458,.T.) ;
#27286 = EDGE_CURVE('',#21588,#21589,#4459,.T.) ;
#27287 = EDGE_CURVE('',#21590,#21564,#4460,.T.) ;
#27288 = EDGE_CURVE('',#21589,#21590,#4461,.T.) ;
#27289 = EDGE_CURVE('',#21591,#21563,#4462,.T.) ;
#27290 = EDGE_CURVE('',#21590,#21591,#4463,.T.) ;
#27291 = EDGE_CURVE('',#21592,#21592,#18493,.T.) ;
#27292 = EDGE_CURVE('',#21592,#21593,#18494,.T.) ;
#27293 = EDGE_CURVE('',#21593,#21594,#18495,.T.) ;
#27294 = EDGE_CURVE('',#21594,#21593,#18496,.T.) ;
#27295 = EDGE_CURVE('',#21594,#21595,#4464,.T.) ;
#27296 = EDGE_CURVE('',#21596,#21595,#18497,.T.) ;
#27297 = EDGE_CURVE('',#21595,#21596,#18498,.T.) ;
#27298 = EDGE_CURVE('',#21597,#21598,#4465,.T.) ;
#27299 = EDGE_CURVE('',#21598,#21588,#353,.T.) ;
#27300 = EDGE_CURVE('',#21597,#21589,#354,.T.) ;
#27301 = EDGE_CURVE('',#21598,#21599,#4466,.T.) ;
#27302 = EDGE_CURVE('',#21599,#21587,#355,.T.) ;
#27303 = EDGE_CURVE('',#21599,#21600,#4467,.T.) ;
#27304 = EDGE_CURVE('',#21600,#21585,#356,.T.) ;
#27305 = EDGE_CURVE('',#21600,#21601,#4468,.T.) ;
#27306 = EDGE_CURVE('',#21601,#21586,#357,.T.) ;
#27307 = EDGE_CURVE('',#21601,#21602,#4469,.T.) ;
#27308 = EDGE_CURVE('',#21602,#21603,#358,.T.) ;
#27309 = EDGE_CURVE('',#21603,#21586,#4470,.T.) ;
#27310 = EDGE_CURVE('',#21604,#21605,#4471,.T.) ;
#27311 = EDGE_CURVE('',#21605,#21606,#359,.T.) ;
#27312 = EDGE_CURVE('',#21606,#21607,#4472,.T.) ;
#27313 = EDGE_CURVE('',#21607,#21604,#360,.T.) ;
#27314 = EDGE_CURVE('',#21608,#21606,#4473,.T.) ;
#27315 = EDGE_CURVE('',#21605,#21609,#4474,.T.) ;
#27316 = EDGE_CURVE('',#21609,#21608,#361,.T.) ;
#27317 = EDGE_CURVE('',#21602,#21604,#4475,.T.) ;
#27318 = EDGE_CURVE('',#21607,#21603,#4476,.T.) ;
#27319 = EDGE_CURVE('',#21610,#21608,#4477,.T.) ;
#27320 = EDGE_CURVE('',#21609,#21611,#4478,.T.) ;
#27321 = EDGE_CURVE('',#21611,#21610,#362,.T.) ;
#27322 = EDGE_CURVE('',#21591,#21610,#4479,.T.) ;
#27323 = EDGE_CURVE('',#21611,#21612,#4480,.T.) ;
#27324 = EDGE_CURVE('',#21612,#21591,#363,.T.) ;
#27325 = EDGE_CURVE('',#21612,#21613,#4481,.T.) ;
#27326 = EDGE_CURVE('',#21613,#21590,#364,.T.) ;
#27327 = EDGE_CURVE('',#21613,#21597,#4482,.T.) ;
#27328 = EDGE_CURVE('',#21603,#21573,#4483,.T.) ;
#27329 = EDGE_CURVE('',#21607,#21572,#4484,.T.) ;
#27330 = EDGE_CURVE('',#21606,#21570,#4485,.T.) ;
#27331 = EDGE_CURVE('',#21614,#21614,#18499,.T.) ;
#27332 = EDGE_CURVE('',#21596,#21614,#18500,.T.) ;
#27333 = EDGE_CURVE('',#21610,#21566,#4486,.T.) ;
#27334 = EDGE_CURVE('',#21608,#21568,#4487,.T.) ;
#27335 = EDGE_CURVE('',#21615,#21616,#4488,.T.) ;
#27336 = EDGE_CURVE('',#21616,#21617,#365,.T.) ;
#27337 = EDGE_CURVE('',#21617,#21618,#4489,.T.) ;
#27338 = EDGE_CURVE('',#21615,#21618,#366,.T.) ;
#27339 = EDGE_CURVE('',#21616,#21619,#4490,.T.) ;
#27340 = EDGE_CURVE('',#21619,#21620,#367,.T.) ;
#27341 = EDGE_CURVE('',#21620,#21617,#4491,.T.) ;
#27342 = EDGE_CURVE('',#21619,#21621,#4492,.T.) ;
#27343 = EDGE_CURVE('',#21621,#21622,#368,.T.) ;
#27344 = EDGE_CURVE('',#21622,#21620,#4493,.T.) ;
#27345 = EDGE_CURVE('',#21621,#21623,#4494,.T.) ;
#27346 = EDGE_CURVE('',#21623,#21624,#369,.T.) ;
#27347 = EDGE_CURVE('',#21624,#21622,#4495,.T.) ;
#27348 = EDGE_CURVE('',#21623,#21625,#4496,.T.) ;
#27349 = EDGE_CURVE('',#21625,#21626,#370,.T.) ;
#27350 = EDGE_CURVE('',#21626,#21624,#4497,.T.) ;
#27351 = EDGE_CURVE('',#21627,#21626,#4498,.T.) ;
#27352 = EDGE_CURVE('',#21625,#21628,#4499,.T.) ;
#27353 = EDGE_CURVE('',#21628,#21627,#371,.T.) ;
#27354 = EDGE_CURVE('',#21629,#21627,#4500,.T.) ;
#27355 = EDGE_CURVE('',#21628,#21630,#4501,.T.) ;
#27356 = EDGE_CURVE('',#21630,#21629,#372,.T.) ;
#27357 = EDGE_CURVE('',#21631,#21629,#4502,.T.) ;
#27358 = EDGE_CURVE('',#21630,#21632,#4503,.T.) ;
#27359 = EDGE_CURVE('',#21632,#21631,#373,.T.) ;
#27360 = EDGE_CURVE('',#21633,#21631,#4504,.T.) ;
#27361 = EDGE_CURVE('',#21632,#21634,#4505,.T.) ;
#27362 = EDGE_CURVE('',#21634,#21633,#374,.T.) ;
#27363 = EDGE_CURVE('',#21635,#21633,#4506,.T.) ;
#27364 = EDGE_CURVE('',#21634,#21636,#4507,.T.) ;
#27365 = EDGE_CURVE('',#21636,#21635,#375,.T.) ;
#27366 = EDGE_CURVE('',#21637,#21635,#4508,.T.) ;
#27367 = EDGE_CURVE('',#21636,#21638,#4509,.T.) ;
#27368 = EDGE_CURVE('',#21638,#21637,#376,.T.) ;
#27369 = EDGE_CURVE('',#21618,#21637,#4510,.T.) ;
#27370 = EDGE_CURVE('',#21638,#21615,#4511,.T.) ;
#27371 = EDGE_CURVE('',#21639,#21631,#4512,.T.) ;
#27372 = EDGE_CURVE('',#21640,#21639,#4513,.T.) ;
#27373 = EDGE_CURVE('',#21640,#21629,#4514,.T.) ;
#27374 = EDGE_CURVE('',#21641,#21633,#4515,.T.) ;
#27375 = EDGE_CURVE('',#21639,#21641,#4516,.T.) ;
#27376 = EDGE_CURVE('',#21642,#21635,#4517,.T.) ;
#27377 = EDGE_CURVE('',#21641,#21642,#4518,.T.) ;
#27378 = EDGE_CURVE('',#21643,#21637,#4519,.T.) ;
#27379 = EDGE_CURVE('',#21642,#21643,#4520,.T.) ;
#27380 = EDGE_CURVE('',#21644,#21618,#4521,.T.) ;
#27381 = EDGE_CURVE('',#21643,#21644,#4522,.T.) ;
#27382 = EDGE_CURVE('',#21645,#21617,#4523,.T.) ;
#27383 = EDGE_CURVE('',#21644,#21645,#4524,.T.) ;
#27384 = EDGE_CURVE('',#21646,#21646,#18501,.T.) ;
#27385 = EDGE_CURVE('',#21646,#21647,#18502,.T.) ;
#27386 = EDGE_CURVE('',#21647,#21648,#18503,.T.) ;
#27387 = EDGE_CURVE('',#21648,#21647,#18504,.T.) ;
#27388 = EDGE_CURVE('',#21648,#21649,#4525,.T.) ;
#27389 = EDGE_CURVE('',#21650,#21649,#18505,.T.) ;
#27390 = EDGE_CURVE('',#21649,#21650,#18506,.T.) ;
#27391 = EDGE_CURVE('',#21651,#21652,#4526,.T.) ;
#27392 = EDGE_CURVE('',#21652,#21642,#377,.T.) ;
#27393 = EDGE_CURVE('',#21651,#21643,#378,.T.) ;
#27394 = EDGE_CURVE('',#21652,#21653,#4527,.T.) ;
#27395 = EDGE_CURVE('',#21653,#21641,#379,.T.) ;
#27396 = EDGE_CURVE('',#21653,#21654,#4528,.T.) ;
#27397 = EDGE_CURVE('',#21654,#21639,#380,.T.) ;
#27398 = EDGE_CURVE('',#21654,#21655,#4529,.T.) ;
#27399 = EDGE_CURVE('',#21655,#21640,#381,.T.) ;
#27400 = EDGE_CURVE('',#21655,#21656,#4530,.T.) ;
#27401 = EDGE_CURVE('',#21656,#21657,#382,.T.) ;
#27402 = EDGE_CURVE('',#21657,#21640,#4531,.T.) ;
#27403 = EDGE_CURVE('',#21658,#21659,#4532,.T.) ;
#27404 = EDGE_CURVE('',#21659,#21660,#383,.T.) ;
#27405 = EDGE_CURVE('',#21660,#21661,#4533,.T.) ;
#27406 = EDGE_CURVE('',#21661,#21658,#384,.T.) ;
#27407 = EDGE_CURVE('',#21662,#21660,#4534,.T.) ;
#27408 = EDGE_CURVE('',#21659,#21663,#4535,.T.) ;
#27409 = EDGE_CURVE('',#21663,#21662,#385,.T.) ;
#27410 = EDGE_CURVE('',#21656,#21658,#4536,.T.) ;
#27411 = EDGE_CURVE('',#21661,#21657,#4537,.T.) ;
#27412 = EDGE_CURVE('',#21664,#21662,#4538,.T.) ;
#27413 = EDGE_CURVE('',#21663,#21665,#4539,.T.) ;
#27414 = EDGE_CURVE('',#21665,#21664,#386,.T.) ;
#27415 = EDGE_CURVE('',#21645,#21664,#4540,.T.) ;
#27416 = EDGE_CURVE('',#21665,#21666,#4541,.T.) ;
#27417 = EDGE_CURVE('',#21666,#21645,#387,.T.) ;
#27418 = EDGE_CURVE('',#21666,#21667,#4542,.T.) ;
#27419 = EDGE_CURVE('',#21667,#21644,#388,.T.) ;
#27420 = EDGE_CURVE('',#21667,#21651,#4543,.T.) ;
#27421 = EDGE_CURVE('',#21657,#21627,#4544,.T.) ;
#27422 = EDGE_CURVE('',#21661,#21626,#4545,.T.) ;
#27423 = EDGE_CURVE('',#21660,#21624,#4546,.T.) ;
#27424 = EDGE_CURVE('',#21668,#21668,#18507,.T.) ;
#27425 = EDGE_CURVE('',#21650,#21668,#18508,.T.) ;
#27426 = EDGE_CURVE('',#21664,#21620,#4547,.T.) ;
#27427 = EDGE_CURVE('',#21662,#21622,#4548,.T.) ;
#27428 = EDGE_CURVE('',#21669,#21670,#18509,.F.) ;
#27429 = EDGE_CURVE('',#21671,#21669,#18510,.F.) ;
#27430 = EDGE_CURVE('',#21670,#21671,#18511,.F.) ;
#27431 = EDGE_CURVE('',#21672,#21673,#18512,.F.) ;
#27432 = EDGE_CURVE('',#21674,#21672,#18513,.F.) ;
#27433 = EDGE_CURVE('',#21673,#21674,#18514,.F.) ;
#27434 = EDGE_CURVE('',#21672,#21670,#4549,.T.) ;
#27435 = EDGE_CURVE('',#21671,#21674,#4550,.T.) ;
#27436 = EDGE_CURVE('',#21675,#21676,#18515,.F.) ;
#27437 = EDGE_CURVE('',#21677,#21675,#18516,.F.) ;
#27438 = EDGE_CURVE('',#21676,#21677,#18517,.F.) ;
#27439 = EDGE_CURVE('',#21669,#21677,#4551,.T.) ;
#27440 = EDGE_CURVE('',#21675,#21671,#4552,.T.) ;
#27441 = EDGE_CURVE('',#21678,#21679,#18518,.F.) ;
#27442 = EDGE_CURVE('',#21680,#21678,#18519,.T.) ;
#27443 = EDGE_CURVE('',#21680,#21681,#18520,.T.) ;
#27444 = EDGE_CURVE('',#21679,#21681,#18521,.T.) ;
#27445 = EDGE_CURVE('',#21682,#21683,#389,.T.) ;
#27446 = EDGE_CURVE('',#21684,#21683,#18522,.T.) ;
#27447 = EDGE_CURVE('',#21685,#21684,#390,.F.) ;
#27448 = EDGE_CURVE('',#21682,#21685,#18523,.T.) ;
#27449 = EDGE_CURVE('',#21683,#21680,#4553,.T.) ;
#27450 = EDGE_CURVE('',#21678,#21684,#4554,.T.) ;
#27451 = EDGE_CURVE('',#21673,#21685,#4555,.T.) ;
#27452 = EDGE_CURVE('',#21684,#21672,#4556,.T.) ;
#27453 = EDGE_CURVE('',#21686,#21687,#18524,.F.) ;
#27454 = EDGE_CURVE('',#21688,#21686,#18525,.F.) ;
#27455 = EDGE_CURVE('',#21687,#21688,#18526,.F.) ;
#27456 = EDGE_CURVE('',#21674,#21688,#4557,.T.) ;
#27457 = EDGE_CURVE('',#21686,#21673,#4558,.T.) ;
#27458 = EDGE_CURVE('',#21676,#21687,#4559,.T.) ;
#27459 = EDGE_CURVE('',#21688,#21675,#4560,.T.) ;
#27460 = EDGE_CURVE('',#21689,#21690,#18527,.T.) ;
#27461 = EDGE_CURVE('',#21691,#21690,#18528,.T.) ;
#27462 = EDGE_CURVE('',#21692,#21691,#18529,.F.) ;
#27463 = EDGE_CURVE('',#21689,#21692,#18530,.T.) ;
#27464 = EDGE_CURVE('',#21693,#21694,#391,.T.) ;
#27465 = EDGE_CURVE('',#21695,#21694,#18531,.T.) ;
#27466 = EDGE_CURVE('',#21696,#21695,#392,.F.) ;
#27467 = EDGE_CURVE('',#21693,#21696,#18532,.T.) ;
#27468 = EDGE_CURVE('',#21690,#21693,#4561,.T.) ;
#27469 = EDGE_CURVE('',#21696,#21691,#4562,.T.) ;
#27470 = EDGE_CURVE('',#21685,#21695,#4563,.T.) ;
#27471 = EDGE_CURVE('',#21694,#21682,#4564,.T.) ;
#27472 = EDGE_CURVE('',#21695,#21686,#4565,.T.) ;
#27473 = EDGE_CURVE('',#21687,#21696,#4566,.T.) ;
#27474 = EDGE_CURVE('',#21691,#21676,#4567,.T.) ;
#27475 = EDGE_CURVE('',#21677,#21692,#4568,.T.) ;
#27476 = EDGE_CURVE('',#21681,#21689,#4569,.T.) ;
#27477 = EDGE_CURVE('',#21692,#21679,#4570,.T.) ;
#27478 = EDGE_CURVE('',#21679,#21669,#4571,.T.) ;
#27479 = EDGE_CURVE('',#21670,#21678,#4572,.T.) ;
#27480 = EDGE_CURVE('',#21697,#21698,#18533,.F.) ;
#27481 = EDGE_CURVE('',#21699,#21697,#18534,.F.) ;
#27482 = EDGE_CURVE('',#21698,#21699,#18535,.F.) ;
#27483 = EDGE_CURVE('',#21700,#21701,#18536,.F.) ;
#27484 = EDGE_CURVE('',#21702,#21700,#18537,.F.) ;
#27485 = EDGE_CURVE('',#21701,#21702,#18538,.F.) ;
#27486 = EDGE_CURVE('',#21700,#21698,#4573,.T.) ;
#27487 = EDGE_CURVE('',#21699,#21702,#4574,.T.) ;
#27488 = EDGE_CURVE('',#21703,#21699,#4575,.T.) ;
#27489 = EDGE_CURVE('',#21697,#21704,#4576,.T.) ;
#27490 = EDGE_CURVE('',#21704,#21703,#393,.T.) ;
#27491 = EDGE_CURVE('',#21705,#21706,#18539,.F.) ;
#27492 = EDGE_CURVE('',#21707,#21705,#18540,.F.) ;
#27493 = EDGE_CURVE('',#21706,#21707,#18541,.F.) ;
#27494 = EDGE_CURVE('',#21705,#21701,#4577,.T.) ;
#27495 = EDGE_CURVE('',#21702,#21707,#4578,.T.) ;
#27496 = EDGE_CURVE('',#21708,#21706,#4579,.T.) ;
#27497 = EDGE_CURVE('',#21707,#21703,#4580,.T.) ;
#27498 = EDGE_CURVE('',#21704,#21708,#18542,.T.) ;
#27499 = EDGE_CURVE('',#21709,#21710,#394,.T.) ;
#27500 = EDGE_CURVE('',#21710,#21705,#4581,.T.) ;
#27501 = EDGE_CURVE('',#21706,#21709,#4582,.T.) ;
#27502 = EDGE_CURVE('',#21711,#21712,#18543,.T.) ;
#27503 = EDGE_CURVE('',#21712,#21700,#4583,.T.) ;
#27504 = EDGE_CURVE('',#21701,#21711,#4584,.T.) ;
#27505 = EDGE_CURVE('',#21713,#21714,#18544,.T.) ;
#27506 = EDGE_CURVE('',#21714,#21697,#4585,.T.) ;
#27507 = EDGE_CURVE('',#21698,#21713,#4586,.T.) ;
#27508 = EDGE_CURVE('',#21711,#21710,#4587,.T.) ;
#27509 = EDGE_CURVE('',#21715,#21709,#4588,.T.) ;
#27510 = EDGE_CURVE('',#21715,#21714,#4589,.T.) ;
#27511 = EDGE_CURVE('',#21713,#21712,#4590,.T.) ;
#27512 = EDGE_CURVE('',#21708,#21715,#4591,.T.) ;
#27513 = EDGE_CURVE('',#21716,#21717,#1149,.T.) ;
#27514 = EDGE_CURVE('',#21716,#21718,#1150,.T.) ;
#27515 = EDGE_CURVE('',#21718,#21719,#1151,.T.) ;
#27516 = EDGE_CURVE('',#21717,#21719,#18545,.T.) ;
#27517 = EDGE_CURVE('',#21716,#21720,#1152,.T.) ;
#27518 = EDGE_CURVE('',#21721,#21720,#18546,.T.) ;
#27519 = EDGE_CURVE('',#21721,#21718,#1153,.T.) ;
#27520 = EDGE_CURVE('',#21716,#21722,#1154,.T.) ;
#27521 = EDGE_CURVE('',#21722,#21723,#1155,.T.) ;
#27522 = EDGE_CURVE('',#21723,#21724,#1156,.T.) ;
#27523 = EDGE_CURVE('',#21720,#21724,#18547,.T.) ;
#27524 = EDGE_CURVE('',#21716,#21725,#1157,.T.) ;
#27525 = EDGE_CURVE('',#21726,#21725,#18548,.T.) ;
#27526 = EDGE_CURVE('',#21726,#21722,#1158,.T.) ;
#27527 = EDGE_CURVE('',#21716,#21727,#1159,.T.) ;
#27528 = EDGE_CURVE('',#21727,#21728,#1160,.T.) ;
#27529 = EDGE_CURVE('',#21725,#21728,#18549,.T.) ;
#27530 = EDGE_CURVE('',#21729,#21730,#4592,.T.) ;
#27531 = EDGE_CURVE('',#21729,#21731,#4593,.T.) ;
#27532 = EDGE_CURVE('',#21731,#21732,#4594,.T.) ;
#27533 = EDGE_CURVE('',#21730,#21732,#4595,.T.) ;
#27534 = EDGE_CURVE('',#21733,#21729,#1161,.T.) ;
#27535 = EDGE_CURVE('',#21733,#21734,#4596,.T.) ;
#27536 = EDGE_CURVE('',#21734,#21731,#1162,.T.) ;
#27537 = EDGE_CURVE('',#21735,#21733,#1163,.T.) ;
#27538 = EDGE_CURVE('',#21735,#21736,#4597,.T.) ;
#27539 = EDGE_CURVE('',#21736,#21734,#1164,.T.) ;
#27540 = EDGE_CURVE('',#21737,#21735,#1165,.T.) ;
#27541 = EDGE_CURVE('',#21737,#21738,#4598,.T.) ;
#27542 = EDGE_CURVE('',#21738,#21736,#1166,.T.) ;
#27543 = EDGE_CURVE('',#21739,#21737,#1167,.T.) ;
#27544 = EDGE_CURVE('',#21739,#21740,#4599,.T.) ;
#27545 = EDGE_CURVE('',#21740,#21738,#1168,.T.) ;
#27546 = EDGE_CURVE('',#21741,#21739,#1169,.T.) ;
#27547 = EDGE_CURVE('',#21741,#21742,#4600,.T.) ;
#27548 = EDGE_CURVE('',#21742,#21740,#1170,.T.) ;
#27549 = EDGE_CURVE('',#21743,#21741,#4601,.T.) ;
#27550 = EDGE_CURVE('',#21743,#21744,#4602,.T.) ;
#27551 = EDGE_CURVE('',#21744,#21742,#4603,.T.) ;
#27552 = EDGE_CURVE('',#21730,#21743,#4604,.T.) ;
#27553 = EDGE_CURVE('',#21732,#21744,#4605,.T.) ;
#27554 = EDGE_CURVE('',#21745,#21746,#4606,.T.) ;
#27555 = EDGE_CURVE('',#21745,#21747,#4607,.T.) ;
#27556 = EDGE_CURVE('',#21747,#21748,#4608,.T.) ;
#27557 = EDGE_CURVE('',#21746,#21748,#4609,.T.) ;
#27558 = EDGE_CURVE('',#21749,#21745,#4610,.T.) ;
#27559 = EDGE_CURVE('',#21749,#21750,#4611,.T.) ;
#27560 = EDGE_CURVE('',#21750,#21747,#4612,.T.) ;
#27561 = EDGE_CURVE('',#21751,#21749,#1171,.T.) ;
#27562 = EDGE_CURVE('',#21751,#21752,#4613,.T.) ;
#27563 = EDGE_CURVE('',#21752,#21750,#1172,.T.) ;
#27564 = EDGE_CURVE('',#21753,#21751,#1173,.T.) ;
#27565 = EDGE_CURVE('',#21753,#21754,#4614,.T.) ;
#27566 = EDGE_CURVE('',#21754,#21752,#1174,.T.) ;
#27567 = EDGE_CURVE('',#21755,#21753,#1175,.T.) ;
#27568 = EDGE_CURVE('',#21755,#21756,#4615,.T.) ;
#27569 = EDGE_CURVE('',#21756,#21754,#1176,.T.) ;
#27570 = EDGE_CURVE('',#21757,#21755,#1177,.T.) ;
#27571 = EDGE_CURVE('',#21757,#21758,#4616,.T.) ;
#27572 = EDGE_CURVE('',#21758,#21756,#1178,.T.) ;
#27573 = EDGE_CURVE('',#21759,#21757,#4617,.T.) ;
#27574 = EDGE_CURVE('',#21759,#21760,#4618,.T.) ;
#27575 = EDGE_CURVE('',#21760,#21758,#4619,.T.) ;
#27576 = EDGE_CURVE('',#21761,#21759,#4620,.T.) ;
#27577 = EDGE_CURVE('',#21761,#21762,#4621,.T.) ;
#27578 = EDGE_CURVE('',#21762,#21760,#4622,.T.) ;
#27579 = EDGE_CURVE('',#21763,#21761,#4623,.T.) ;
#27580 = EDGE_CURVE('',#21763,#21764,#4624,.T.) ;
#27581 = EDGE_CURVE('',#21764,#21762,#4625,.T.) ;
#27582 = EDGE_CURVE('',#21765,#21763,#1179,.T.) ;
#27583 = EDGE_CURVE('',#21765,#21766,#4626,.T.) ;
#27584 = EDGE_CURVE('',#21766,#21764,#1180,.T.) ;
#27585 = EDGE_CURVE('',#21767,#21765,#1181,.T.) ;
#27586 = EDGE_CURVE('',#21767,#21768,#4627,.T.) ;
#27587 = EDGE_CURVE('',#21768,#21766,#1182,.T.) ;
#27588 = EDGE_CURVE('',#21769,#21767,#1183,.T.) ;
#27589 = EDGE_CURVE('',#21769,#21770,#4628,.T.) ;
#27590 = EDGE_CURVE('',#21770,#21768,#1184,.T.) ;
#27591 = EDGE_CURVE('',#21771,#21769,#1185,.T.) ;
#27592 = EDGE_CURVE('',#21771,#21772,#4629,.T.) ;
#27593 = EDGE_CURVE('',#21772,#21770,#1186,.T.) ;
#27594 = EDGE_CURVE('',#21773,#21771,#1187,.T.) ;
#27595 = EDGE_CURVE('',#21773,#21774,#4630,.T.) ;
#27596 = EDGE_CURVE('',#21774,#21772,#1188,.T.) ;
#27597 = EDGE_CURVE('',#21775,#21773,#1189,.T.) ;
#27598 = EDGE_CURVE('',#21775,#21776,#4631,.T.) ;
#27599 = EDGE_CURVE('',#21776,#21774,#1190,.T.) ;
#27600 = EDGE_CURVE('',#21777,#21775,#1191,.T.) ;
#27601 = EDGE_CURVE('',#21777,#21778,#4632,.T.) ;
#27602 = EDGE_CURVE('',#21778,#21776,#1192,.T.) ;
#27603 = EDGE_CURVE('',#21779,#21777,#4633,.T.) ;
#27604 = EDGE_CURVE('',#21779,#21780,#4634,.T.) ;
#27605 = EDGE_CURVE('',#21780,#21778,#4635,.T.) ;
#27606 = EDGE_CURVE('',#21781,#21779,#4636,.T.) ;
#27607 = EDGE_CURVE('',#21781,#21782,#4637,.T.) ;
#27608 = EDGE_CURVE('',#21782,#21780,#4638,.T.) ;
#27609 = EDGE_CURVE('',#21746,#21781,#4639,.T.) ;
#27610 = EDGE_CURVE('',#21748,#21782,#4640,.T.) ;
#27611 = EDGE_CURVE('',#21783,#21784,#4641,.T.) ;
#27612 = EDGE_CURVE('',#21785,#21783,#4642,.T.) ;
#27613 = EDGE_CURVE('',#21785,#21786,#18550,.T.) ;
#27614 = EDGE_CURVE('',#21787,#21786,#4643,.T.) ;
#27615 = EDGE_CURVE('',#21788,#21787,#18551,.T.) ;
#27616 = EDGE_CURVE('',#21789,#21788,#4644,.T.) ;
#27617 = EDGE_CURVE('',#21790,#21789,#18552,.T.) ;
#27618 = EDGE_CURVE('',#21791,#21790,#4645,.T.) ;
#27619 = EDGE_CURVE('',#21792,#21791,#18553,.T.) ;
#27620 = EDGE_CURVE('',#21793,#21792,#18554,.T.) ;
#27621 = EDGE_CURVE('',#21794,#21793,#4646,.T.) ;
#27622 = EDGE_CURVE('',#21795,#21794,#18555,.T.) ;
#27623 = EDGE_CURVE('',#21796,#21795,#4647,.T.) ;
#27624 = EDGE_CURVE('',#21797,#21796,#18556,.T.) ;
#27625 = EDGE_CURVE('',#21798,#21797,#4648,.T.) ;
#27626 = EDGE_CURVE('',#21799,#21798,#18557,.T.) ;
#27627 = EDGE_CURVE('',#21800,#21799,#4649,.T.) ;
#27628 = EDGE_CURVE('',#21784,#21800,#18558,.T.) ;
#27629 = EDGE_CURVE('',#21801,#21802,#4650,.T.) ;
#27630 = EDGE_CURVE('',#21803,#21801,#18559,.T.) ;
#27631 = EDGE_CURVE('',#21804,#21803,#4651,.T.) ;
#27632 = EDGE_CURVE('',#21802,#21804,#4652,.T.) ;
#27633 = EDGE_CURVE('',#21805,#21806,#395,.T.) ;
#27634 = EDGE_CURVE('',#21805,#21807,#4653,.T.) ;
#27635 = EDGE_CURVE('',#21807,#21808,#396,.T.) ;
#27636 = EDGE_CURVE('',#21808,#21806,#4654,.T.) ;
#27637 = EDGE_CURVE('',#21808,#21809,#1193,.T.) ;
#27638 = EDGE_CURVE('',#21809,#21810,#4655,.T.) ;
#27639 = EDGE_CURVE('',#21810,#21806,#1194,.T.) ;
#27640 = EDGE_CURVE('',#21811,#21812,#18560,.T.) ;
#27641 = EDGE_CURVE('',#21812,#21813,#18561,.T.) ;
#27642 = EDGE_CURVE('',#21813,#21814,#1195,.F.) ;
#27643 = EDGE_CURVE('',#21814,#21811,#18562,.T.) ;
#27644 = EDGE_CURVE('',#21815,#21816,#18563,.T.) ;
#27645 = EDGE_CURVE('',#21816,#21812,#4656,.T.) ;
#27646 = EDGE_CURVE('',#21811,#21815,#4657,.T.) ;
#27647 = EDGE_CURVE('',#21817,#21818,#18564,.T.) ;
#27648 = EDGE_CURVE('',#21818,#21816,#18565,.T.) ;
#27649 = EDGE_CURVE('',#21815,#21817,#18566,.T.) ;
#27650 = EDGE_CURVE('',#21819,#21820,#18567,.T.) ;
#27651 = EDGE_CURVE('',#21820,#21821,#1196,.T.) ;
#27652 = EDGE_CURVE('',#21821,#21818,#4658,.T.) ;
#27653 = EDGE_CURVE('',#21817,#21819,#4659,.T.) ;
#27654 = EDGE_CURVE('',#21822,#21823,#1197,.T.) ;
#27655 = EDGE_CURVE('',#21824,#21822,#1198,.F.) ;
#27656 = EDGE_CURVE('',#21820,#21824,#1199,.F.) ;
#27657 = EDGE_CURVE('',#21819,#21823,#18568,.T.) ;
#27658 = EDGE_CURVE('',#21825,#21817,#4660,.T.) ;
#27659 = EDGE_CURVE('',#21826,#21825,#4661,.T.) ;
#27660 = EDGE_CURVE('',#21827,#21826,#4662,.T.) ;
#27661 = EDGE_CURVE('',#21828,#21827,#4663,.T.) ;
#27662 = EDGE_CURVE('',#21828,#21823,#4664,.T.) ;
#27663 = EDGE_CURVE('',#21815,#21829,#4665,.T.) ;
#27664 = EDGE_CURVE('',#21829,#21825,#18569,.T.) ;
#27665 = EDGE_CURVE('',#21830,#21814,#4666,.F.) ;
#27666 = EDGE_CURVE('',#21829,#21830,#4667,.F.) ;
#27667 = EDGE_CURVE('',#21831,#21832,#1200,.T.) ;
#27668 = EDGE_CURVE('',#21831,#21833,#397,.T.) ;
#27669 = EDGE_CURVE('',#21833,#21834,#18570,.T.) ;
#27670 = EDGE_CURVE('',#21834,#21835,#398,.T.) ;
#27671 = EDGE_CURVE('',#21835,#21836,#1201,.T.) ;
#27672 = EDGE_CURVE('',#21836,#21837,#1202,.T.) ;
#27673 = EDGE_CURVE('',#21837,#21832,#1203,.T.) ;
#27674 = EDGE_CURVE('',#21838,#21839,#18571,.T.) ;
#27675 = EDGE_CURVE('',#21839,#21834,#4668,.T.) ;
#27676 = EDGE_CURVE('',#21833,#21838,#4669,.T.) ;
#27677 = EDGE_CURVE('',#21840,#21841,#18572,.T.) ;
#27678 = EDGE_CURVE('',#21841,#21839,#18573,.T.) ;
#27679 = EDGE_CURVE('',#21838,#21840,#18574,.T.) ;
#27680 = EDGE_CURVE('',#21842,#21843,#18575,.T.) ;
#27681 = EDGE_CURVE('',#21843,#21841,#4670,.T.) ;
#27682 = EDGE_CURVE('',#21840,#21842,#4671,.T.) ;
#27683 = EDGE_CURVE('',#21844,#21845,#1204,.F.) ;
#27684 = EDGE_CURVE('',#21845,#21843,#18576,.T.) ;
#27685 = EDGE_CURVE('',#21842,#21844,#18577,.T.) ;
#27686 = EDGE_CURVE('',#21846,#21840,#4672,.T.) ;
#27687 = EDGE_CURVE('',#21847,#21846,#4673,.F.) ;
#27688 = EDGE_CURVE('',#21844,#21847,#4674,.F.) ;
#27689 = EDGE_CURVE('',#21838,#21848,#4675,.T.) ;
#27690 = EDGE_CURVE('',#21848,#21846,#18578,.T.) ;
#27691 = EDGE_CURVE('',#21849,#21831,#4676,.T.) ;
#27692 = EDGE_CURVE('',#21848,#21849,#4677,.T.) ;
#27693 = EDGE_CURVE('',#21832,#21850,#4678,.T.) ;
#27694 = EDGE_CURVE('',#21851,#21850,#1205,.T.) ;
#27695 = EDGE_CURVE('',#21851,#21852,#1206,.T.) ;
#27696 = EDGE_CURVE('',#21852,#21832,#399,.F.) ;
#27697 = EDGE_CURVE('',#21837,#21850,#4679,.T.) ;
#27698 = EDGE_CURVE('',#21853,#21836,#1207,.T.) ;
#27699 = EDGE_CURVE('',#21853,#21854,#1208,.T.) ;
#27700 = EDGE_CURVE('',#21855,#21854,#400,.T.) ;
#27701 = EDGE_CURVE('',#21856,#21855,#4680,.T.) ;
#27702 = EDGE_CURVE('',#21857,#21856,#1209,.T.) ;
#27703 = EDGE_CURVE('',#21858,#21857,#401,.T.) ;
#27704 = EDGE_CURVE('',#21859,#21858,#4681,.T.) ;
#27705 = EDGE_CURVE('',#21860,#21859,#4682,.T.) ;
#27706 = EDGE_CURVE('',#21861,#21860,#4683,.T.) ;
#27707 = EDGE_CURVE('',#21862,#21861,#4684,.T.) ;
#27708 = EDGE_CURVE('',#21863,#21862,#402,.T.) ;
#27709 = EDGE_CURVE('',#21864,#21863,#4685,.T.) ;
#27710 = EDGE_CURVE('',#21865,#21864,#403,.T.) ;
#27711 = EDGE_CURVE('',#21851,#21865,#4686,.T.) ;
#27712 = EDGE_CURVE('',#21866,#21867,#18579,.T.) ;
#27713 = EDGE_CURVE('',#21867,#21868,#404,.T.) ;
#27714 = EDGE_CURVE('',#21868,#21869,#405,.T.) ;
#27715 = EDGE_CURVE('',#21869,#21870,#406,.T.) ;
#27716 = EDGE_CURVE('',#21870,#21866,#407,.T.) ;
#27717 = EDGE_CURVE('',#21871,#21872,#18580,.T.) ;
#27718 = EDGE_CURVE('',#21872,#21867,#4687,.T.) ;
#27719 = EDGE_CURVE('',#21866,#21871,#4688,.T.) ;
#27720 = EDGE_CURVE('',#21873,#21874,#18581,.T.) ;
#27721 = EDGE_CURVE('',#21874,#21872,#408,.T.) ;
#27722 = EDGE_CURVE('',#21871,#21873,#409,.T.) ;
#27723 = EDGE_CURVE('',#21873,#21875,#1210,.T.) ;
#27724 = EDGE_CURVE('',#21875,#21874,#1211,.T.) ;
#27725 = EDGE_CURVE('',#21871,#21876,#4689,.T.) ;
#27726 = EDGE_CURVE('',#21876,#21877,#18582,.T.) ;
#27727 = EDGE_CURVE('',#21877,#21875,#4690,.T.) ;
#27728 = EDGE_CURVE('',#21878,#21866,#4691,.T.) ;
#27729 = EDGE_CURVE('',#21879,#21878,#4692,.T.) ;
#27730 = EDGE_CURVE('',#21876,#21879,#18583,.T.) ;
#27731 = EDGE_CURVE('',#21869,#21880,#4693,.T.) ;
#27732 = EDGE_CURVE('',#21878,#21880,#18584,.T.) ;
#27733 = EDGE_CURVE('',#21881,#21882,#18585,.T.) ;
#27734 = EDGE_CURVE('',#21882,#21883,#410,.T.) ;
#27735 = EDGE_CURVE('',#21883,#21884,#411,.T.) ;
#27736 = EDGE_CURVE('',#21884,#21885,#412,.T.) ;
#27737 = EDGE_CURVE('',#21885,#21881,#413,.T.) ;
#27738 = EDGE_CURVE('',#21886,#21887,#18586,.T.) ;
#27739 = EDGE_CURVE('',#21887,#21882,#4694,.T.) ;
#27740 = EDGE_CURVE('',#21881,#21886,#4695,.T.) ;
#27741 = EDGE_CURVE('',#21888,#21889,#18587,.T.) ;
#27742 = EDGE_CURVE('',#21889,#21887,#414,.T.) ;
#27743 = EDGE_CURVE('',#21886,#21888,#415,.T.) ;
#27744 = EDGE_CURVE('',#21888,#21890,#1212,.T.) ;
#27745 = EDGE_CURVE('',#21890,#21860,#1213,.T.) ;
#27746 = EDGE_CURVE('',#21860,#21891,#1214,.T.) ;
#27747 = EDGE_CURVE('',#21891,#21889,#1215,.T.) ;
#27748 = EDGE_CURVE('',#21892,#21874,#4696,.T.) ;
#27749 = EDGE_CURVE('',#21893,#21892,#4697,.T.) ;
#27750 = EDGE_CURVE('',#21894,#21893,#18588,.T.) ;
#27751 = EDGE_CURVE('',#21895,#21894,#4698,.T.) ;
#27752 = EDGE_CURVE('',#21896,#21895,#18589,.T.) ;
#27753 = EDGE_CURVE('',#21897,#21896,#4699,.T.) ;
#27754 = EDGE_CURVE('',#21888,#21897,#4700,.T.) ;
#27755 = EDGE_CURVE('',#21898,#21881,#4701,.T.) ;
#27756 = EDGE_CURVE('',#21899,#21898,#4702,.T.) ;
#27757 = EDGE_CURVE('',#21900,#21899,#18590,.T.) ;
#27758 = EDGE_CURVE('',#21901,#21900,#4703,.T.) ;
#27759 = EDGE_CURVE('',#21867,#21901,#4704,.T.) ;
#27760 = EDGE_CURVE('',#21884,#21902,#4705,.T.) ;
#27761 = EDGE_CURVE('',#21902,#21898,#416,.T.) ;
#27762 = EDGE_CURVE('',#21882,#21903,#4706,.T.) ;
#27763 = EDGE_CURVE('',#21904,#21903,#18591,.T.) ;
#27764 = EDGE_CURVE('',#21904,#21884,#4707,.T.) ;
#27765 = EDGE_CURVE('',#21905,#21906,#417,.T.) ;
#27766 = EDGE_CURVE('',#21906,#21907,#418,.T.) ;
#27767 = EDGE_CURVE('',#21907,#21905,#18592,.T.) ;
#27768 = EDGE_CURVE('',#21906,#21908,#4708,.T.) ;
#27769 = EDGE_CURVE('',#21908,#21909,#18593,.T.) ;
#27770 = EDGE_CURVE('',#21909,#21907,#4709,.T.) ;
#27771 = EDGE_CURVE('',#21905,#21910,#4710,.T.) ;
#27772 = EDGE_CURVE('',#21910,#21911,#1216,.T.) ;
#27773 = EDGE_CURVE('',#21911,#21912,#4711,.T.) ;
#27774 = EDGE_CURVE('',#21912,#21913,#18594,.T.) ;
#27775 = EDGE_CURVE('',#21913,#21906,#4712,.T.) ;
#27776 = EDGE_CURVE('',#21908,#21914,#4713,.T.) ;
#27777 = EDGE_CURVE('',#21915,#21914,#4714,.T.) ;
#27778 = EDGE_CURVE('',#21916,#21915,#4715,.T.) ;
#27779 = EDGE_CURVE('',#21917,#21916,#4716,.T.) ;
#27780 = EDGE_CURVE('',#21918,#21917,#419,.T.) ;
#27781 = EDGE_CURVE('',#21919,#21918,#4717,.T.) ;
#27782 = EDGE_CURVE('',#21920,#21919,#420,.T.) ;
#27783 = EDGE_CURVE('',#21909,#21920,#4718,.T.) ;
#27784 = EDGE_CURVE('',#21914,#21913,#4719,.T.) ;
#27785 = EDGE_CURVE('',#21912,#21921,#18595,.T.) ;
#27786 = EDGE_CURVE('',#21915,#21921,#4720,.T.) ;
#27787 = EDGE_CURVE('',#21911,#21922,#18596,.T.) ;
#27788 = EDGE_CURVE('',#21922,#21921,#4721,.T.) ;
#27789 = EDGE_CURVE('',#21812,#21923,#4722,.T.) ;
#27790 = EDGE_CURVE('',#21924,#21923,#421,.T.) ;
#27791 = EDGE_CURVE('',#21924,#21813,#4723,.T.) ;
#27792 = EDGE_CURVE('',#21925,#21821,#1217,.F.) ;
#27793 = EDGE_CURVE('',#21923,#21925,#4724,.T.) ;
#27794 = EDGE_CURVE('',#21926,#21927,#18597,.T.) ;
#27795 = EDGE_CURVE('',#21927,#21928,#422,.T.) ;
#27796 = EDGE_CURVE('',#21928,#21929,#18598,.T.) ;
#27797 = EDGE_CURVE('',#21929,#21926,#423,.T.) ;
#27798 = EDGE_CURVE('',#21845,#21928,#4725,.T.) ;
#27799 = EDGE_CURVE('',#21927,#21843,#4726,.T.) ;
#27800 = EDGE_CURVE('',#21930,#21929,#4727,.T.) ;
#27801 = EDGE_CURVE('',#21931,#21930,#424,.T.) ;
#27802 = EDGE_CURVE('',#21932,#21931,#4728,.T.) ;
#27803 = EDGE_CURVE('',#21926,#21932,#4729,.T.) ;
#27804 = EDGE_CURVE('',#21928,#21933,#4730,.T.) ;
#27805 = EDGE_CURVE('',#21933,#21930,#18599,.T.) ;
#27806 = EDGE_CURVE('',#21847,#21934,#4731,.T.) ;
#27807 = EDGE_CURVE('',#21934,#21935,#4732,.T.) ;
#27808 = EDGE_CURVE('',#21935,#21936,#4733,.T.) ;
#27809 = EDGE_CURVE('',#21937,#21936,#4734,.T.) ;
#27810 = EDGE_CURVE('',#21933,#21937,#4735,.T.) ;
#27811 = EDGE_CURVE('',#21938,#21892,#18600,.T.) ;
#27812 = EDGE_CURVE('',#21892,#21939,#18601,.T.) ;
#27813 = EDGE_CURVE('',#21939,#21940,#18602,.T.) ;
#27814 = EDGE_CURVE('',#21940,#21938,#18603,.T.) ;
#27815 = EDGE_CURVE('',#21875,#21939,#4736,.T.) ;
#27816 = EDGE_CURVE('',#21939,#21941,#4737,.T.) ;
#27817 = EDGE_CURVE('',#21942,#21941,#18604,.T.) ;
#27818 = EDGE_CURVE('',#21942,#21940,#4738,.T.) ;
#27819 = EDGE_CURVE('',#21943,#21877,#4739,.T.) ;
#27820 = EDGE_CURVE('',#21944,#21943,#4740,.T.) ;
#27821 = EDGE_CURVE('',#21945,#21944,#4741,.T.) ;
#27822 = EDGE_CURVE('',#21941,#21945,#425,.T.) ;
#27823 = EDGE_CURVE('',#21897,#21946,#18605,.T.) ;
#27824 = EDGE_CURVE('',#21946,#21947,#18606,.T.) ;
#27825 = EDGE_CURVE('',#21947,#21861,#18607,.T.) ;
#27826 = EDGE_CURVE('',#21861,#21897,#18608,.T.) ;
#27827 = EDGE_CURVE('',#21896,#21948,#18609,.T.) ;
#27828 = EDGE_CURVE('',#21948,#21946,#4742,.T.) ;
#27829 = EDGE_CURVE('',#21880,#21949,#18610,.T.) ;
#27830 = EDGE_CURVE('',#21949,#21950,#18611,.T.) ;
#27831 = EDGE_CURVE('',#21950,#21878,#18612,.T.) ;
#27832 = EDGE_CURVE('',#21879,#21951,#18613,.T.) ;
#27833 = EDGE_CURVE('',#21951,#21877,#18614,.T.) ;
#27834 = EDGE_CURVE('',#21950,#21951,#4743,.T.) ;
#27835 = EDGE_CURVE('',#21903,#21952,#18615,.T.) ;
#27836 = EDGE_CURVE('',#21952,#21953,#18616,.T.) ;
#27837 = EDGE_CURVE('',#21953,#21904,#18617,.T.) ;
#27838 = EDGE_CURVE('',#21954,#21955,#18618,.T.) ;
#27839 = EDGE_CURVE('',#21955,#21952,#4744,.T.) ;
#27840 = EDGE_CURVE('',#21903,#21954,#4745,.T.) ;
#27841 = EDGE_CURVE('',#21956,#21859,#18619,.T.) ;
#27842 = EDGE_CURVE('',#21859,#21955,#18620,.T.) ;
#27843 = EDGE_CURVE('',#21954,#21956,#18621,.T.) ;
#27844 = EDGE_CURVE('',#21956,#21887,#4746,.T.) ;
#27845 = EDGE_CURVE('',#21957,#21953,#4747,.T.) ;
#27846 = EDGE_CURVE('',#21958,#21957,#4748,.T.) ;
#27847 = EDGE_CURVE('',#21958,#21959,#4749,.T.) ;
#27848 = EDGE_CURVE('',#21959,#21960,#4750,.T.) ;
#27849 = EDGE_CURVE('',#21961,#21960,#4751,.T.) ;
#27850 = EDGE_CURVE('',#21961,#21902,#4752,.T.) ;
#27851 = EDGE_CURVE('',#21952,#21962,#4753,.T.) ;
#27852 = EDGE_CURVE('',#21957,#21962,#18622,.T.) ;
#27853 = EDGE_CURVE('',#21963,#21955,#4754,.T.) ;
#27854 = EDGE_CURVE('',#21964,#21963,#426,.T.) ;
#27855 = EDGE_CURVE('',#21965,#21964,#4755,.T.) ;
#27856 = EDGE_CURVE('',#21966,#21965,#4756,.T.) ;
#27857 = EDGE_CURVE('',#21967,#21966,#4757,.T.) ;
#27858 = EDGE_CURVE('',#21962,#21967,#18623,.T.) ;
#27859 = EDGE_CURVE('',#21968,#21858,#1218,.T.) ;
#27860 = EDGE_CURVE('',#21963,#21968,#1219,.T.) ;
#27861 = EDGE_CURVE('',#21969,#21970,#18624,.F.) ;
#27862 = EDGE_CURVE('',#21971,#21969,#18625,.F.) ;
#27863 = EDGE_CURVE('',#21970,#21971,#18626,.F.) ;
#27864 = EDGE_CURVE('',#21972,#21973,#427,.T.) ;
#27865 = EDGE_CURVE('',#21973,#21971,#4758,.T.) ;
#27866 = EDGE_CURVE('',#21969,#21972,#4759,.T.) ;
#27867 = EDGE_CURVE('',#21974,#21975,#1220,.T.) ;
#27868 = EDGE_CURVE('',#21975,#21976,#18627,.T.) ;
#27869 = EDGE_CURVE('',#21976,#21977,#18628,.T.) ;
#27870 = EDGE_CURVE('',#21977,#21974,#18629,.T.) ;
#27871 = EDGE_CURVE('',#21978,#21979,#18630,.T.) ;
#27872 = EDGE_CURVE('',#21979,#21977,#4760,.T.) ;
#27873 = EDGE_CURVE('',#21976,#21978,#4761,.T.) ;
#27874 = EDGE_CURVE('',#21980,#21981,#18631,.T.) ;
#27875 = EDGE_CURVE('',#21981,#21979,#18632,.T.) ;
#27876 = EDGE_CURVE('',#21978,#21980,#18633,.T.) ;
#27877 = EDGE_CURVE('',#21982,#21983,#18634,.T.) ;
#27878 = EDGE_CURVE('',#21983,#21981,#18635,.T.) ;
#27879 = EDGE_CURVE('',#21980,#21982,#18636,.T.) ;
#27880 = EDGE_CURVE('',#21984,#21985,#18637,.T.) ;
#27881 = EDGE_CURVE('',#21985,#21983,#4762,.T.) ;
#27882 = EDGE_CURVE('',#21982,#21984,#4763,.T.) ;
#27883 = EDGE_CURVE('',#21986,#21987,#18638,.T.) ;
#27884 = EDGE_CURVE('',#21987,#21985,#18639,.T.) ;
#27885 = EDGE_CURVE('',#21984,#21986,#18640,.T.) ;
#27886 = EDGE_CURVE('',#21971,#21987,#4764,.T.) ;
#27887 = EDGE_CURVE('',#21986,#21970,#4765,.T.) ;
#27888 = EDGE_CURVE('',#21988,#21989,#18641,.T.) ;
#27889 = EDGE_CURVE('',#21989,#21969,#4766,.T.) ;
#27890 = EDGE_CURVE('',#21970,#21988,#4767,.T.) ;
#27891 = EDGE_CURVE('',#21990,#21991,#1221,.F.) ;
#27892 = EDGE_CURVE('',#21991,#21989,#18642,.T.) ;
#27893 = EDGE_CURVE('',#21988,#21990,#18643,.T.) ;
#27894 = EDGE_CURVE('',#21992,#21973,#4768,.T.) ;
#27895 = EDGE_CURVE('',#21992,#21993,#18644,.T.) ;
#27896 = EDGE_CURVE('',#21994,#21993,#4769,.T.) ;
#27897 = EDGE_CURVE('',#21994,#21995,#18645,.T.) ;
#27898 = EDGE_CURVE('',#21996,#21995,#4770,.T.) ;
#27899 = EDGE_CURVE('',#21997,#21996,#4771,.T.) ;
#27900 = EDGE_CURVE('',#21997,#21998,#4772,.T.) ;
#27901 = EDGE_CURVE('',#21999,#21998,#18646,.T.) ;
#27902 = EDGE_CURVE('',#21999,#22000,#18647,.F.) ;
#27903 = EDGE_CURVE('',#21974,#22000,#18648,.T.) ;
#27904 = EDGE_CURVE('',#21972,#22001,#4773,.T.) ;
#27905 = EDGE_CURVE('',#22001,#21992,#18649,.T.) ;
#27906 = EDGE_CURVE('',#22002,#21991,#4774,.T.) ;
#27907 = EDGE_CURVE('',#21972,#22002,#4775,.T.) ;
#27908 = EDGE_CURVE('',#22003,#22004,#18650,.T.) ;
#27909 = EDGE_CURVE('',#22003,#22005,#4776,.T.) ;
#27910 = EDGE_CURVE('',#22005,#22006,#18651,.T.) ;
#27911 = EDGE_CURVE('',#22006,#22007,#4777,.T.) ;
#27912 = EDGE_CURVE('',#22004,#22007,#428,.T.) ;
#27913 = EDGE_CURVE('',#22008,#22009,#1222,.T.) ;
#27914 = EDGE_CURVE('',#22009,#22006,#1223,.T.) ;
#27915 = EDGE_CURVE('',#22005,#22008,#1224,.T.) ;
#27916 = EDGE_CURVE('',#22010,#22003,#18652,.T.) ;
#27917 = EDGE_CURVE('',#22011,#22010,#4778,.T.) ;
#27918 = EDGE_CURVE('',#22011,#22008,#18653,.T.) ;
#27919 = EDGE_CURVE('',#21988,#22012,#4779,.T.) ;
#27920 = EDGE_CURVE('',#22012,#22013,#18654,.T.) ;
#27921 = EDGE_CURVE('',#22013,#21990,#4780,.T.) ;
#27922 = EDGE_CURVE('',#22012,#22014,#1225,.T.) ;
#27923 = EDGE_CURVE('',#22014,#22015,#1226,.T.) ;
#27924 = EDGE_CURVE('',#22015,#22013,#1227,.T.) ;
#27925 = EDGE_CURVE('',#21986,#22016,#4781,.T.) ;
#27926 = EDGE_CURVE('',#22017,#22016,#4782,.T.) ;
#27927 = EDGE_CURVE('',#22014,#22017,#4783,.T.) ;
#27928 = EDGE_CURVE('',#22018,#22019,#18655,.T.) ;
#27929 = EDGE_CURVE('',#21966,#22019,#18656,.T.) ;
#27930 = EDGE_CURVE('',#22020,#21966,#18657,.F.) ;
#27931 = EDGE_CURVE('',#22018,#22020,#18658,.T.) ;
#27932 = EDGE_CURVE('',#22021,#21967,#18659,.T.) ;
#27933 = EDGE_CURVE('',#22019,#22021,#4784,.T.) ;
#27934 = EDGE_CURVE('',#22021,#21957,#18660,.T.) ;
#27935 = EDGE_CURVE('',#21965,#22022,#18661,.T.) ;
#27936 = EDGE_CURVE('',#22022,#22020,#4785,.T.) ;
#27937 = EDGE_CURVE('',#21965,#22023,#1228,.T.) ;
#27938 = EDGE_CURVE('',#22023,#22024,#18662,.T.) ;
#27939 = EDGE_CURVE('',#22024,#22022,#1229,.T.) ;
#27940 = EDGE_CURVE('',#22025,#22026,#18663,.T.) ;
#27941 = EDGE_CURVE('',#22026,#22024,#429,.T.) ;
#27942 = EDGE_CURVE('',#22023,#22025,#430,.T.) ;
#27943 = EDGE_CURVE('',#22027,#22028,#18664,.T.) ;
#27944 = EDGE_CURVE('',#22028,#22026,#4786,.T.) ;
#27945 = EDGE_CURVE('',#22025,#22027,#4787,.T.) ;
#27946 = EDGE_CURVE('',#22029,#22030,#1230,.T.) ;
#27947 = EDGE_CURVE('',#22030,#22028,#431,.T.) ;
#27948 = EDGE_CURVE('',#22027,#22031,#432,.T.) ;
#27949 = EDGE_CURVE('',#22031,#22029,#1231,.T.) ;
#27950 = EDGE_CURVE('',#21798,#22032,#433,.T.) ;
#27951 = EDGE_CURVE('',#22032,#22033,#18665,.T.) ;
#27952 = EDGE_CURVE('',#22033,#21799,#18666,.T.) ;
#27953 = EDGE_CURVE('',#22034,#21800,#18667,.T.) ;
#27954 = EDGE_CURVE('',#22033,#22034,#4788,.T.) ;
#27955 = EDGE_CURVE('',#22035,#21784,#18668,.T.) ;
#27956 = EDGE_CURVE('',#22034,#22035,#18669,.T.) ;
#27957 = EDGE_CURVE('',#22036,#21783,#18670,.T.) ;
#27958 = EDGE_CURVE('',#22035,#22036,#4789,.T.) ;
#27959 = EDGE_CURVE('',#22037,#22038,#18671,.T.) ;
#27960 = EDGE_CURVE('',#22038,#21783,#18672,.T.) ;
#27961 = EDGE_CURVE('',#22036,#22037,#18673,.T.) ;
#27962 = EDGE_CURVE('',#22039,#22040,#18674,.T.) ;
#27963 = EDGE_CURVE('',#22040,#22038,#4790,.T.) ;
#27964 = EDGE_CURVE('',#22037,#22039,#4791,.T.) ;
#27965 = EDGE_CURVE('',#22020,#22040,#18675,.T.) ;
#27966 = EDGE_CURVE('',#22039,#22018,#18676,.T.) ;
#27967 = EDGE_CURVE('',#22041,#22021,#4792,.T.) ;
#27968 = EDGE_CURVE('',#21958,#22041,#18677,.T.) ;
#27969 = EDGE_CURVE('',#22042,#22035,#4793,.T.) ;
#27970 = EDGE_CURVE('',#22042,#22041,#4794,.T.) ;
#27971 = EDGE_CURVE('',#22043,#22034,#4795,.T.) ;
#27972 = EDGE_CURVE('',#22043,#22042,#18678,.T.) ;
#27973 = EDGE_CURVE('',#22044,#22033,#4796,.T.) ;
#27974 = EDGE_CURVE('',#22045,#22044,#4797,.T.) ;
#27975 = EDGE_CURVE('',#22046,#22045,#4798,.T.) ;
#27976 = EDGE_CURVE('',#22046,#22043,#4799,.T.) ;
#27977 = EDGE_CURVE('',#22047,#22032,#4800,.T.) ;
#27978 = EDGE_CURVE('',#22044,#22047,#18679,.T.) ;
#27979 = EDGE_CURVE('',#22048,#21797,#18680,.T.) ;
#27980 = EDGE_CURVE('',#22048,#22032,#4801,.T.) ;
#27981 = EDGE_CURVE('',#22049,#22050,#18681,.T.) ;
#27982 = EDGE_CURVE('',#22050,#22051,#1232,.T.) ;
#27983 = EDGE_CURVE('',#22051,#22052,#1233,.T.) ;
#27984 = EDGE_CURVE('',#22052,#22053,#1234,.T.) ;
#27985 = EDGE_CURVE('',#22053,#22049,#1235,.T.) ;
#27986 = EDGE_CURVE('',#22054,#22055,#18682,.T.) ;
#27987 = EDGE_CURVE('',#22055,#22050,#434,.T.) ;
#27988 = EDGE_CURVE('',#22049,#22054,#435,.T.) ;
#27989 = EDGE_CURVE('',#22056,#22057,#18683,.T.) ;
#27990 = EDGE_CURVE('',#22057,#22055,#4802,.T.) ;
#27991 = EDGE_CURVE('',#22054,#22056,#4803,.T.) ;
#27992 = EDGE_CURVE('',#22058,#22059,#18684,.T.) ;
#27993 = EDGE_CURVE('',#22059,#22057,#436,.T.) ;
#27994 = EDGE_CURVE('',#22056,#22058,#437,.T.) ;
#27995 = EDGE_CURVE('',#22060,#22061,#18685,.T.) ;
#27996 = EDGE_CURVE('',#22061,#22059,#438,.T.) ;
#27997 = EDGE_CURVE('',#22058,#22060,#439,.T.) ;
#27998 = EDGE_CURVE('',#22060,#22062,#440,.T.) ;
#27999 = EDGE_CURVE('',#22062,#22063,#1236,.T.) ;
#28000 = EDGE_CURVE('',#22063,#22061,#441,.T.) ;
#28001 = EDGE_CURVE('',#22056,#22064,#4804,.T.) ;
#28002 = EDGE_CURVE('',#22065,#22064,#1237,.T.) ;
#28003 = EDGE_CURVE('',#22066,#22065,#442,.T.) ;
#28004 = EDGE_CURVE('',#22066,#22062,#4805,.T.) ;
#28005 = EDGE_CURVE('',#22067,#22059,#4806,.T.) ;
#28006 = EDGE_CURVE('',#22068,#22067,#4807,.T.) ;
#28007 = EDGE_CURVE('',#22068,#22069,#4808,.T.) ;
#28008 = EDGE_CURVE('',#22070,#22069,#1238,.F.) ;
#28009 = EDGE_CURVE('',#22071,#22070,#4809,.T.) ;
#28010 = EDGE_CURVE('',#22050,#22071,#443,.T.) ;
#28011 = EDGE_CURVE('',#22064,#22054,#4810,.T.) ;
#28012 = EDGE_CURVE('',#22052,#22072,#4811,.T.) ;
#28013 = EDGE_CURVE('',#22064,#22072,#18686,.T.) ;
#28014 = EDGE_CURVE('',#21802,#22073,#444,.T.) ;
#28015 = EDGE_CURVE('',#22073,#22074,#4812,.T.) ;
#28016 = EDGE_CURVE('',#22074,#21801,#1239,.T.) ;
#28017 = EDGE_CURVE('',#22074,#22075,#18687,.T.) ;
#28018 = EDGE_CURVE('',#22075,#21803,#1240,.T.) ;
#28019 = EDGE_CURVE('',#22075,#22076,#4813,.T.) ;
#28020 = EDGE_CURVE('',#22076,#21804,#445,.T.) ;
#28021 = EDGE_CURVE('',#22076,#22073,#4814,.T.) ;
#28022 = EDGE_CURVE('',#22077,#22074,#4815,.T.) ;
#28023 = EDGE_CURVE('',#22078,#22077,#18688,.T.) ;
#28024 = EDGE_CURVE('',#22078,#22075,#4816,.T.) ;
#28025 = EDGE_CURVE('',#22073,#22079,#4817,.T.) ;
#28026 = EDGE_CURVE('',#22077,#22079,#4818,.T.) ;
#28027 = EDGE_CURVE('',#22080,#22081,#18689,.T.) ;
#28028 = EDGE_CURVE('',#22081,#22082,#446,.T.) ;
#28029 = EDGE_CURVE('',#22082,#22080,#447,.T.) ;
#28030 = EDGE_CURVE('',#22083,#22084,#18690,.T.) ;
#28031 = EDGE_CURVE('',#22084,#22081,#18691,.T.) ;
#28032 = EDGE_CURVE('',#22080,#22083,#18692,.T.) ;
#28033 = EDGE_CURVE('',#22085,#22086,#1241,.T.) ;
#28034 = EDGE_CURVE('',#22086,#22084,#4819,.T.) ;
#28035 = EDGE_CURVE('',#22083,#22085,#4820,.T.) ;
#28036 = EDGE_CURVE('',#22087,#22083,#4821,.T.) ;
#28037 = EDGE_CURVE('',#22087,#22088,#4822,.T.) ;
#28038 = EDGE_CURVE('',#22088,#22089,#4823,.T.) ;
#28039 = EDGE_CURVE('',#22089,#22090,#4824,.T.) ;
#28040 = EDGE_CURVE('',#22090,#22085,#4825,.T.) ;
#28041 = EDGE_CURVE('',#22082,#22091,#4826,.T.) ;
#28042 = EDGE_CURVE('',#22091,#22087,#18693,.T.) ;
#28043 = EDGE_CURVE('',#22081,#22092,#4827,.T.) ;
#28044 = EDGE_CURVE('',#22093,#22092,#18694,.T.) ;
#28045 = EDGE_CURVE('',#22093,#22082,#4828,.T.) ;
#28046 = EDGE_CURVE('',#22094,#22095,#18695,.F.) ;
#28047 = EDGE_CURVE('',#22096,#22094,#18696,.F.) ;
#28048 = EDGE_CURVE('',#22095,#22096,#18697,.F.) ;
#28049 = EDGE_CURVE('',#21917,#22096,#4829,.T.) ;
#28050 = EDGE_CURVE('',#22094,#21918,#4830,.T.) ;
#28051 = EDGE_CURVE('',#22007,#22095,#4831,.T.) ;
#28052 = EDGE_CURVE('',#22096,#22004,#4832,.T.) ;
#28053 = EDGE_CURVE('',#22097,#22098,#18698,.F.) ;
#28054 = EDGE_CURVE('',#22099,#22097,#18699,.T.) ;
#28055 = EDGE_CURVE('',#22099,#22100,#18700,.T.) ;
#28056 = EDGE_CURVE('',#22098,#22100,#18701,.T.) ;
#28057 = EDGE_CURVE('',#22009,#22099,#4833,.T.) ;
#28058 = EDGE_CURVE('',#22097,#22006,#4834,.T.) ;
#28059 = EDGE_CURVE('',#21919,#22098,#4835,.T.) ;
#28060 = EDGE_CURVE('',#22100,#21920,#4836,.T.) ;
#28061 = EDGE_CURVE('',#22095,#22097,#4837,.T.) ;
#28062 = EDGE_CURVE('',#22098,#22094,#4838,.T.) ;
#28063 = EDGE_CURVE('',#22101,#21916,#4839,.T.) ;
#28064 = EDGE_CURVE('',#22102,#22101,#18702,.T.) ;
#28065 = EDGE_CURVE('',#22103,#22102,#4840,.T.) ;
#28066 = EDGE_CURVE('',#22103,#22104,#18703,.T.) ;
#28067 = EDGE_CURVE('',#22104,#22105,#4841,.T.) ;
#28068 = EDGE_CURVE('',#22105,#22106,#18704,.T.) ;
#28069 = EDGE_CURVE('',#22107,#22106,#4842,.T.) ;
#28070 = EDGE_CURVE('',#22108,#22107,#18705,.T.) ;
#28071 = EDGE_CURVE('',#22109,#22108,#4843,.T.) ;
#28072 = EDGE_CURVE('',#22110,#22109,#4844,.T.) ;
#28073 = EDGE_CURVE('',#22111,#22110,#4845,.T.) ;
#28074 = EDGE_CURVE('',#22112,#22111,#4846,.T.) ;
#28075 = EDGE_CURVE('',#22113,#22112,#4847,.T.) ;
#28076 = EDGE_CURVE('',#22114,#22113,#18706,.T.) ;
#28077 = EDGE_CURVE('',#22115,#22114,#4848,.T.) ;
#28078 = EDGE_CURVE('',#22116,#22115,#18707,.T.) ;
#28079 = EDGE_CURVE('',#22117,#22116,#4849,.T.) ;
#28080 = EDGE_CURVE('',#22118,#22117,#18708,.T.) ;
#28081 = EDGE_CURVE('',#22119,#22118,#4850,.T.) ;
#28082 = EDGE_CURVE('',#22119,#22120,#18709,.T.) ;
#28083 = EDGE_CURVE('',#22120,#22121,#4851,.T.) ;
#28084 = EDGE_CURVE('',#22121,#22122,#18710,.T.) ;
#28085 = EDGE_CURVE('',#22122,#22123,#4852,.T.) ;
#28086 = EDGE_CURVE('',#22124,#22123,#18711,.T.) ;
#28087 = EDGE_CURVE('',#22125,#22124,#4853,.T.) ;
#28088 = EDGE_CURVE('',#22126,#22125,#4854,.T.) ;
#28089 = EDGE_CURVE('',#22127,#22126,#4855,.T.) ;
#28090 = EDGE_CURVE('',#22128,#22127,#18712,.T.) ;
#28091 = EDGE_CURVE('',#22129,#22128,#4856,.T.) ;
#28092 = EDGE_CURVE('',#22129,#22130,#18713,.T.) ;
#28093 = EDGE_CURVE('',#22130,#22131,#4857,.T.) ;
#28094 = EDGE_CURVE('',#22131,#22132,#18714,.T.) ;
#28095 = EDGE_CURVE('',#22132,#22133,#4858,.T.) ;
#28096 = EDGE_CURVE('',#22133,#22134,#18715,.T.) ;
#28097 = EDGE_CURVE('',#22134,#22135,#4859,.T.) ;
#28098 = EDGE_CURVE('',#22136,#22135,#18716,.T.) ;
#28099 = EDGE_CURVE('',#22137,#22136,#4860,.T.) ;
#28100 = EDGE_CURVE('',#22137,#22138,#4861,.T.) ;
#28101 = EDGE_CURVE('',#22138,#22139,#4862,.T.) ;
#28102 = EDGE_CURVE('',#22139,#22140,#4863,.T.) ;
#28103 = EDGE_CURVE('',#22140,#22141,#4864,.T.) ;
#28104 = EDGE_CURVE('',#22141,#22142,#4865,.T.) ;
#28105 = EDGE_CURVE('',#22142,#22143,#1242,.T.) ;
#28106 = EDGE_CURVE('',#22144,#22143,#4866,.T.) ;
#28107 = EDGE_CURVE('',#22144,#22145,#1243,.T.) ;
#28108 = EDGE_CURVE('',#22145,#22146,#4867,.T.) ;
#28109 = EDGE_CURVE('',#22146,#22147,#4868,.T.) ;
#28110 = EDGE_CURVE('',#22147,#22148,#4869,.T.) ;
#28111 = EDGE_CURVE('',#22148,#22149,#18717,.T.) ;
#28112 = EDGE_CURVE('',#22149,#22150,#4870,.T.) ;
#28113 = EDGE_CURVE('',#22150,#22151,#18718,.T.) ;
#28114 = EDGE_CURVE('',#22151,#22152,#4871,.T.) ;
#28115 = EDGE_CURVE('',#22152,#22153,#4872,.T.) ;
#28116 = EDGE_CURVE('',#22153,#22154,#18719,.T.) ;
#28117 = EDGE_CURVE('',#22154,#22155,#4873,.T.) ;
#28118 = EDGE_CURVE('',#22156,#22155,#4874,.T.) ;
#28119 = EDGE_CURVE('',#22156,#22157,#18720,.T.) ;
#28120 = EDGE_CURVE('',#22157,#22158,#4875,.T.) ;
#28121 = EDGE_CURVE('',#22158,#22090,#1244,.T.) ;
#28122 = EDGE_CURVE('',#22089,#22159,#4876,.T.) ;
#28123 = EDGE_CURVE('',#22160,#22159,#4877,.F.) ;
#28124 = EDGE_CURVE('',#22161,#22160,#4878,.T.) ;
#28125 = EDGE_CURVE('',#22162,#22161,#18721,.T.) ;
#28126 = EDGE_CURVE('',#22163,#22162,#18722,.T.) ;
#28127 = EDGE_CURVE('',#22164,#22163,#18723,.T.) ;
#28128 = EDGE_CURVE('',#22164,#22165,#18724,.T.) ;
#28129 = EDGE_CURVE('',#22166,#22165,#4879,.T.) ;
#28130 = EDGE_CURVE('',#22166,#22167,#18725,.T.) ;
#28131 = EDGE_CURVE('',#22168,#22167,#4880,.T.) ;
#28132 = EDGE_CURVE('',#22169,#22168,#4881,.T.) ;
#28133 = EDGE_CURVE('',#22169,#22170,#18726,.T.) ;
#28134 = EDGE_CURVE('',#22171,#22170,#4882,.T.) ;
#28135 = EDGE_CURVE('',#22171,#22172,#18727,.T.) ;
#28136 = EDGE_CURVE('',#22173,#22172,#4883,.T.) ;
#28137 = EDGE_CURVE('',#22174,#22173,#4884,.T.) ;
#28138 = EDGE_CURVE('',#22174,#22175,#18728,.T.) ;
#28139 = EDGE_CURVE('',#22176,#22175,#4885,.T.) ;
#28140 = EDGE_CURVE('',#22176,#22177,#18729,.T.) ;
#28141 = EDGE_CURVE('',#22177,#22178,#4886,.T.) ;
#28142 = EDGE_CURVE('',#22178,#22179,#4887,.T.) ;
#28143 = EDGE_CURVE('',#22180,#22179,#4888,.T.) ;
#28144 = EDGE_CURVE('',#22181,#22180,#18730,.T.) ;
#28145 = EDGE_CURVE('',#22182,#22181,#4889,.T.) ;
#28146 = EDGE_CURVE('',#22183,#22182,#18731,.T.) ;
#28147 = EDGE_CURVE('',#22184,#22183,#4890,.T.) ;
#28148 = EDGE_CURVE('',#22185,#22184,#18732,.T.) ;
#28149 = EDGE_CURVE('',#22186,#22185,#4891,.T.) ;
#28150 = EDGE_CURVE('',#22187,#22186,#18733,.T.) ;
#28151 = EDGE_CURVE('',#22188,#22187,#4892,.T.) ;
#28152 = EDGE_CURVE('',#22188,#22002,#4893,.T.) ;
#28153 = EDGE_CURVE('',#22189,#22013,#18734,.T.) ;
#28154 = EDGE_CURVE('',#22190,#22189,#18735,.T.) ;
#28155 = EDGE_CURVE('',#22191,#22190,#4894,.T.) ;
#28156 = EDGE_CURVE('',#22192,#22191,#18736,.T.) ;
#28157 = EDGE_CURVE('',#22193,#22192,#4895,.T.) ;
#28158 = EDGE_CURVE('',#22194,#22193,#4896,.T.) ;
#28159 = EDGE_CURVE('',#22195,#22194,#18737,.T.) ;
#28160 = EDGE_CURVE('',#22196,#22195,#4897,.T.) ;
#28161 = EDGE_CURVE('',#22197,#22196,#18738,.T.) ;
#28162 = EDGE_CURVE('',#22197,#22198,#18739,.T.) ;
#28163 = EDGE_CURVE('',#22198,#22199,#4898,.T.) ;
#28164 = EDGE_CURVE('',#22199,#22010,#4899,.T.) ;
#28165 = EDGE_CURVE('',#22200,#22201,#18740,.T.) ;
#28166 = EDGE_CURVE('',#22202,#22200,#4900,.T.) ;
#28167 = EDGE_CURVE('',#22203,#22202,#18741,.T.) ;
#28168 = EDGE_CURVE('',#22204,#22203,#4901,.T.) ;
#28169 = EDGE_CURVE('',#22205,#22204,#18742,.T.) ;
#28170 = EDGE_CURVE('',#22206,#22205,#4902,.T.) ;
#28171 = EDGE_CURVE('',#22207,#22206,#18743,.T.) ;
#28172 = EDGE_CURVE('',#22201,#22207,#4903,.T.) ;
#28173 = EDGE_CURVE('',#22208,#22208,#18744,.T.) ;
#28174 = EDGE_CURVE('',#22209,#22210,#18745,.T.) ;
#28175 = EDGE_CURVE('',#22211,#22209,#4904,.T.) ;
#28176 = EDGE_CURVE('',#22212,#22211,#18746,.T.) ;
#28177 = EDGE_CURVE('',#22213,#22212,#4905,.T.) ;
#28178 = EDGE_CURVE('',#22214,#22213,#4906,.T.) ;
#28179 = EDGE_CURVE('',#22215,#22214,#18747,.T.) ;
#28180 = EDGE_CURVE('',#22216,#22215,#4907,.T.) ;
#28181 = EDGE_CURVE('',#22217,#22216,#18748,.T.) ;
#28182 = EDGE_CURVE('',#22218,#22217,#4908,.T.) ;
#28183 = EDGE_CURVE('',#22219,#22218,#18749,.T.) ;
#28184 = EDGE_CURVE('',#22220,#22219,#4909,.T.) ;
#28185 = EDGE_CURVE('',#22221,#22220,#18750,.T.) ;
#28186 = EDGE_CURVE('',#22222,#22221,#4910,.T.) ;
#28187 = EDGE_CURVE('',#22210,#22222,#4911,.T.) ;
#28188 = EDGE_CURVE('',#22223,#22223,#18751,.T.) ;
#28189 = EDGE_CURVE('',#22224,#22225,#4912,.T.) ;
#28190 = EDGE_CURVE('',#22226,#22224,#1245,.T.) ;
#28191 = EDGE_CURVE('',#22227,#22226,#4913,.T.) ;
#28192 = EDGE_CURVE('',#22228,#22227,#18752,.T.) ;
#28193 = EDGE_CURVE('',#22229,#22228,#4914,.T.) ;
#28194 = EDGE_CURVE('',#22230,#22229,#18753,.T.) ;
#28195 = EDGE_CURVE('',#22231,#22230,#4915,.T.) ;
#28196 = EDGE_CURVE('',#22232,#22231,#18754,.T.) ;
#28197 = EDGE_CURVE('',#22233,#22232,#4916,.T.) ;
#28198 = EDGE_CURVE('',#22234,#22233,#18755,.T.) ;
#28199 = EDGE_CURVE('',#22235,#22234,#4917,.T.) ;
#28200 = EDGE_CURVE('',#22225,#22235,#1246,.T.) ;
#28201 = EDGE_CURVE('',#22236,#22237,#1247,.T.) ;
#28202 = EDGE_CURVE('',#21809,#22236,#4918,.T.) ;
#28203 = EDGE_CURVE('',#22238,#21807,#4919,.T.) ;
#28204 = EDGE_CURVE('',#22239,#22238,#4920,.T.) ;
#28205 = EDGE_CURVE('',#22240,#22239,#18756,.T.) ;
#28206 = EDGE_CURVE('',#22241,#22240,#4921,.T.) ;
#28207 = EDGE_CURVE('',#22242,#22241,#18757,.T.) ;
#28208 = EDGE_CURVE('',#22243,#22242,#4922,.T.) ;
#28209 = EDGE_CURVE('',#22244,#22243,#18758,.T.) ;
#28210 = EDGE_CURVE('',#22245,#22244,#4923,.T.) ;
#28211 = EDGE_CURVE('',#22246,#22245,#18759,.T.) ;
#28212 = EDGE_CURVE('',#22247,#22246,#4924,.T.) ;
#28213 = EDGE_CURVE('',#22237,#22247,#4925,.T.) ;
#28214 = EDGE_CURVE('',#22248,#22249,#18760,.T.) ;
#28215 = EDGE_CURVE('',#22250,#22248,#4926,.T.) ;
#28216 = EDGE_CURVE('',#22251,#22250,#18761,.T.) ;
#28217 = EDGE_CURVE('',#22252,#22251,#4927,.T.) ;
#28218 = EDGE_CURVE('',#22253,#22252,#4928,.T.) ;
#28219 = EDGE_CURVE('',#22254,#22253,#18762,.T.) ;
#28220 = EDGE_CURVE('',#22255,#22254,#4929,.T.) ;
#28221 = EDGE_CURVE('',#22256,#22255,#18763,.T.) ;
#28222 = EDGE_CURVE('',#22257,#22256,#4930,.T.) ;
#28223 = EDGE_CURVE('',#22258,#22257,#18764,.T.) ;
#28224 = EDGE_CURVE('',#22259,#22258,#4931,.T.) ;
#28225 = EDGE_CURVE('',#22260,#22259,#18765,.T.) ;
#28226 = EDGE_CURVE('',#22261,#22260,#4932,.T.) ;
#28227 = EDGE_CURVE('',#22249,#22261,#4933,.T.) ;
#28228 = EDGE_CURVE('',#22262,#22263,#1248,.T.) ;
#28229 = EDGE_CURVE('',#22264,#22263,#18766,.T.) ;
#28230 = EDGE_CURVE('',#22162,#22264,#1249,.F.) ;
#28231 = EDGE_CURVE('',#22262,#22162,#18767,.T.) ;
#28232 = EDGE_CURVE('',#22000,#22264,#4934,.T.) ;
#28233 = EDGE_CURVE('',#22263,#21975,#4935,.T.) ;
#28234 = EDGE_CURVE('',#22265,#22163,#1250,.T.) ;
#28235 = EDGE_CURVE('',#22264,#22265,#18768,.T.) ;
#28236 = EDGE_CURVE('',#22161,#22266,#18769,.T.) ;
#28237 = EDGE_CURVE('',#22266,#22262,#18770,.T.) ;
#28238 = EDGE_CURVE('',#22160,#22267,#18771,.F.) ;
#28239 = EDGE_CURVE('',#22267,#22266,#4936,.T.) ;
#28240 = EDGE_CURVE('',#22265,#21999,#4937,.T.) ;
#28241 = EDGE_CURVE('',#22266,#22268,#4938,.T.) ;
#28242 = EDGE_CURVE('',#22269,#22268,#18772,.T.) ;
#28243 = EDGE_CURVE('',#21976,#22269,#4939,.T.) ;
#28244 = EDGE_CURVE('',#22270,#22267,#4940,.T.) ;
#28245 = EDGE_CURVE('',#22270,#22091,#4941,.T.) ;
#28246 = EDGE_CURVE('',#22093,#22271,#4942,.T.) ;
#28247 = EDGE_CURVE('',#22268,#22271,#4943,.T.) ;
#28248 = EDGE_CURVE('',#22001,#22188,#4944,.T.) ;
#28249 = EDGE_CURVE('',#22187,#22272,#4945,.T.) ;
#28250 = EDGE_CURVE('',#22272,#22273,#4946,.T.) ;
#28251 = EDGE_CURVE('',#21992,#22273,#4947,.T.) ;
#28252 = EDGE_CURVE('',#22274,#22275,#18773,.F.) ;
#28253 = EDGE_CURVE('',#22276,#22274,#18774,.F.) ;
#28254 = EDGE_CURVE('',#22275,#22276,#18775,.F.) ;
#28255 = EDGE_CURVE('',#21907,#22277,#4948,.T.) ;
#28256 = EDGE_CURVE('',#22277,#22278,#18776,.T.) ;
#28257 = EDGE_CURVE('',#22278,#21905,#4949,.T.) ;
#28258 = EDGE_CURVE('',#22279,#22280,#18777,.T.) ;
#28259 = EDGE_CURVE('',#22280,#22278,#18778,.T.) ;
#28260 = EDGE_CURVE('',#22277,#22279,#18779,.T.) ;
#28261 = EDGE_CURVE('',#22281,#22282,#18780,.T.) ;
#28262 = EDGE_CURVE('',#22282,#22280,#4950,.T.) ;
#28263 = EDGE_CURVE('',#22279,#22281,#4951,.T.) ;
#28264 = EDGE_CURVE('',#22283,#22284,#18781,.T.) ;
#28265 = EDGE_CURVE('',#22284,#22282,#18782,.T.) ;
#28266 = EDGE_CURVE('',#22281,#22283,#18783,.T.) ;
#28267 = EDGE_CURVE('',#22274,#22284,#4952,.T.) ;
#28268 = EDGE_CURVE('',#22283,#22276,#4953,.T.) ;
#28269 = EDGE_CURVE('',#22285,#22286,#1251,.T.) ;
#28270 = EDGE_CURVE('',#22286,#22287,#4954,.T.) ;
#28271 = EDGE_CURVE('',#22287,#22288,#18784,.T.) ;
#28272 = EDGE_CURVE('',#22288,#22285,#4955,.T.) ;
#28273 = EDGE_CURVE('',#22289,#22290,#18785,.T.) ;
#28274 = EDGE_CURVE('',#22290,#22288,#18786,.T.) ;
#28275 = EDGE_CURVE('',#22287,#22289,#18787,.T.) ;
#28276 = EDGE_CURVE('',#22276,#22290,#4956,.T.) ;
#28277 = EDGE_CURVE('',#22289,#22275,#4957,.T.) ;
#28278 = EDGE_CURVE('',#22193,#22291,#448,.F.) ;
#28279 = EDGE_CURVE('',#22292,#22193,#18788,.T.) ;
#28280 = EDGE_CURVE('',#22292,#22293,#449,.T.) ;
#28281 = EDGE_CURVE('',#22291,#22293,#18789,.T.) ;
#28282 = EDGE_CURVE('',#22014,#22294,#18790,.T.) ;
#28283 = EDGE_CURVE('',#22294,#22189,#18791,.T.) ;
#28284 = EDGE_CURVE('',#22295,#22190,#18792,.T.) ;
#28285 = EDGE_CURVE('',#22294,#22295,#18793,.T.) ;
#28286 = EDGE_CURVE('',#22296,#22191,#18794,.T.) ;
#28287 = EDGE_CURVE('',#22295,#22296,#4958,.T.) ;
#28288 = EDGE_CURVE('',#22297,#22192,#18795,.T.) ;
#28289 = EDGE_CURVE('',#22296,#22297,#18796,.T.) ;
#28290 = EDGE_CURVE('',#22297,#22292,#4959,.T.) ;
#28291 = EDGE_CURVE('',#22293,#22274,#4960,.T.) ;
#28292 = EDGE_CURVE('',#22275,#22291,#4961,.T.) ;
#28293 = EDGE_CURVE('',#22298,#22194,#18797,.T.) ;
#28294 = EDGE_CURVE('',#22291,#22298,#4962,.T.) ;
#28295 = EDGE_CURVE('',#22299,#22195,#18798,.T.) ;
#28296 = EDGE_CURVE('',#22298,#22299,#18799,.T.) ;
#28297 = EDGE_CURVE('',#22300,#22196,#18800,.T.) ;
#28298 = EDGE_CURVE('',#22299,#22300,#4963,.T.) ;
#28299 = EDGE_CURVE('',#22197,#22301,#1252,.F.) ;
#28300 = EDGE_CURVE('',#22301,#22300,#1253,.F.) ;
#28301 = EDGE_CURVE('',#22011,#22302,#4964,.T.) ;
#28302 = EDGE_CURVE('',#22302,#22303,#4965,.T.) ;
#28303 = EDGE_CURVE('',#22303,#22285,#18801,.T.) ;
#28304 = EDGE_CURVE('',#22278,#22304,#4966,.T.) ;
#28305 = EDGE_CURVE('',#22305,#22304,#4967,.T.) ;
#28306 = EDGE_CURVE('',#22306,#22305,#4968,.T.) ;
#28307 = EDGE_CURVE('',#21910,#22306,#450,.T.) ;
#28308 = EDGE_CURVE('',#22280,#22307,#4969,.T.) ;
#28309 = EDGE_CURVE('',#22304,#22307,#18802,.T.) ;
#28310 = EDGE_CURVE('',#22308,#22282,#4970,.T.) ;
#28311 = EDGE_CURVE('',#22307,#22308,#4971,.T.) ;
#28312 = EDGE_CURVE('',#22284,#22309,#4972,.T.) ;
#28313 = EDGE_CURVE('',#22308,#22309,#18803,.T.) ;
#28314 = EDGE_CURVE('',#22297,#22310,#4973,.T.) ;
#28315 = EDGE_CURVE('',#22311,#22310,#4974,.T.) ;
#28316 = EDGE_CURVE('',#22312,#22311,#18804,.T.) ;
#28317 = EDGE_CURVE('',#22313,#22312,#4975,.T.) ;
#28318 = EDGE_CURVE('',#22314,#22313,#18805,.T.) ;
#28319 = EDGE_CURVE('',#22315,#22314,#4976,.T.) ;
#28320 = EDGE_CURVE('',#22316,#22315,#18806,.T.) ;
#28321 = EDGE_CURVE('',#22309,#22316,#4977,.T.) ;
#28322 = EDGE_CURVE('',#22296,#22317,#4978,.T.) ;
#28323 = EDGE_CURVE('',#22310,#22317,#451,.T.) ;
#28324 = EDGE_CURVE('',#22295,#22318,#4979,.T.) ;
#28325 = EDGE_CURVE('',#22317,#22318,#4980,.T.) ;
#28326 = EDGE_CURVE('',#22319,#22294,#4981,.T.) ;
#28327 = EDGE_CURVE('',#22318,#22319,#452,.T.) ;
#28328 = EDGE_CURVE('',#22320,#22017,#18807,.T.) ;
#28329 = EDGE_CURVE('',#22321,#22320,#1254,.T.) ;
#28330 = EDGE_CURVE('',#22319,#22321,#453,.T.) ;
#28331 = EDGE_CURVE('',#22322,#22323,#18808,.T.) ;
#28332 = EDGE_CURVE('',#22324,#22322,#1255,.F.) ;
#28333 = EDGE_CURVE('',#22325,#22324,#18809,.T.) ;
#28334 = EDGE_CURVE('',#22325,#22323,#1256,.T.) ;
#28335 = EDGE_CURVE('',#22326,#22327,#18810,.T.) ;
#28336 = EDGE_CURVE('',#22326,#22324,#4982,.T.) ;
#28337 = EDGE_CURVE('',#22322,#22327,#4983,.T.) ;
#28338 = EDGE_CURVE('',#22328,#22329,#18811,.F.) ;
#28339 = EDGE_CURVE('',#22330,#22328,#18812,.T.) ;
#28340 = EDGE_CURVE('',#22330,#22331,#18813,.T.) ;
#28341 = EDGE_CURVE('',#22329,#22331,#18814,.T.) ;
#28342 = EDGE_CURVE('',#22332,#22333,#18815,.T.) ;
#28343 = EDGE_CURVE('',#22333,#22330,#4984,.T.) ;
#28344 = EDGE_CURVE('',#22328,#22332,#4985,.T.) ;
#28345 = EDGE_CURVE('',#22332,#22322,#18816,.T.) ;
#28346 = EDGE_CURVE('',#22323,#22333,#18817,.T.) ;
#28347 = EDGE_CURVE('',#22334,#22335,#18818,.T.) ;
#28348 = EDGE_CURVE('',#22336,#22335,#18819,.T.) ;
#28349 = EDGE_CURVE('',#22337,#22336,#18820,.F.) ;
#28350 = EDGE_CURVE('',#22334,#22337,#18821,.T.) ;
#28351 = EDGE_CURVE('',#22338,#22339,#1257,.F.) ;
#28352 = EDGE_CURVE('',#22340,#22338,#18822,.T.) ;
#28353 = EDGE_CURVE('',#22340,#22341,#1258,.T.) ;
#28354 = EDGE_CURVE('',#22339,#22341,#18823,.T.) ;
#28355 = EDGE_CURVE('',#22342,#22343,#18824,.T.) ;
#28356 = EDGE_CURVE('',#22343,#22340,#18825,.T.) ;
#28357 = EDGE_CURVE('',#22338,#22342,#18826,.T.) ;
#28358 = EDGE_CURVE('',#22335,#22343,#4986,.T.) ;
#28359 = EDGE_CURVE('',#22342,#22336,#4987,.T.) ;
#28360 = EDGE_CURVE('',#22344,#22345,#18827,.T.) ;
#28361 = EDGE_CURVE('',#22345,#22339,#4988,.T.) ;
#28362 = EDGE_CURVE('',#22341,#22344,#4989,.T.) ;
#28363 = EDGE_CURVE('',#21863,#22346,#18828,.T.) ;
#28364 = EDGE_CURVE('',#22346,#22345,#1259,.T.) ;
#28365 = EDGE_CURVE('',#22344,#21863,#1260,.T.) ;
#28366 = EDGE_CURVE('',#21862,#22347,#18829,.T.) ;
#28367 = EDGE_CURVE('',#22347,#22346,#454,.T.) ;
#28368 = EDGE_CURVE('',#21947,#22347,#4990,.T.) ;
#28369 = EDGE_CURVE('',#22348,#22349,#18830,.T.) ;
#28370 = EDGE_CURVE('',#22348,#22338,#4991,.T.) ;
#28371 = EDGE_CURVE('',#22339,#22349,#4992,.T.) ;
#28372 = EDGE_CURVE('',#21895,#22350,#18831,.T.) ;
#28373 = EDGE_CURVE('',#22350,#21948,#18832,.T.) ;
#28374 = EDGE_CURVE('',#21894,#22351,#18833,.T.) ;
#28375 = EDGE_CURVE('',#22351,#22350,#4993,.T.) ;
#28376 = EDGE_CURVE('',#21893,#22352,#18834,.T.) ;
#28377 = EDGE_CURVE('',#22352,#22351,#18835,.T.) ;
#28378 = EDGE_CURVE('',#21938,#22352,#4994,.T.) ;
#28379 = EDGE_CURVE('',#22353,#22354,#18836,.T.) ;
#28380 = EDGE_CURVE('',#22353,#22337,#4995,.T.) ;
#28381 = EDGE_CURVE('',#22336,#22354,#4996,.T.) ;
#28382 = EDGE_CURVE('',#22355,#22356,#18837,.T.) ;
#28383 = EDGE_CURVE('',#22356,#22334,#4997,.T.) ;
#28384 = EDGE_CURVE('',#22337,#22355,#4998,.T.) ;
#28385 = EDGE_CURVE('',#22357,#22358,#18838,.T.) ;
#28386 = EDGE_CURVE('',#22358,#22356,#18839,.T.) ;
#28387 = EDGE_CURVE('',#22355,#22357,#18840,.T.) ;
#28388 = EDGE_CURVE('',#22359,#22360,#18841,.T.) ;
#28389 = EDGE_CURVE('',#22360,#22358,#4999,.T.) ;
#28390 = EDGE_CURVE('',#22357,#22359,#5000,.T.) ;
#28391 = EDGE_CURVE('',#22361,#22362,#18842,.T.) ;
#28392 = EDGE_CURVE('',#22362,#22360,#18843,.T.) ;
#28393 = EDGE_CURVE('',#22359,#22361,#18844,.T.) ;
#28394 = EDGE_CURVE('',#22363,#22364,#18845,.T.) ;
#28395 = EDGE_CURVE('',#22364,#22362,#5001,.T.) ;
#28396 = EDGE_CURVE('',#22361,#22363,#5002,.T.) ;
#28397 = EDGE_CURVE('',#22365,#22366,#18846,.T.) ;
#28398 = EDGE_CURVE('',#22366,#22364,#18847,.T.) ;
#28399 = EDGE_CURVE('',#22363,#22365,#18848,.T.) ;
#28400 = EDGE_CURVE('',#22367,#22368,#18849,.T.) ;
#28401 = EDGE_CURVE('',#22368,#22366,#5003,.T.) ;
#28402 = EDGE_CURVE('',#22365,#22367,#5004,.T.) ;
#28403 = EDGE_CURVE('',#22369,#22370,#18850,.T.) ;
#28404 = EDGE_CURVE('',#22370,#22368,#18851,.T.) ;
#28405 = EDGE_CURVE('',#22367,#22369,#18852,.T.) ;
#28406 = EDGE_CURVE('',#22331,#22370,#5005,.T.) ;
#28407 = EDGE_CURVE('',#22369,#22329,#5006,.T.) ;
#28408 = EDGE_CURVE('',#22371,#22372,#18853,.T.) ;
#28409 = EDGE_CURVE('',#22372,#22325,#5007,.T.) ;
#28410 = EDGE_CURVE('',#22324,#22371,#5008,.T.) ;
#28411 = EDGE_CURVE('',#22371,#22373,#1261,.T.) ;
#28412 = EDGE_CURVE('',#22373,#21945,#18854,.T.) ;
#28413 = EDGE_CURVE('',#21945,#22372,#1262,.T.) ;
#28414 = EDGE_CURVE('',#22373,#21942,#455,.T.) ;
#28415 = EDGE_CURVE('',#22374,#22375,#18855,.T.) ;
#28416 = EDGE_CURVE('',#22374,#22328,#5009,.T.) ;
#28417 = EDGE_CURVE('',#22329,#22375,#5010,.T.) ;
#28418 = EDGE_CURVE('',#22376,#21944,#18856,.T.) ;
#28419 = EDGE_CURVE('',#22376,#22333,#5011,.T.) ;
#28420 = EDGE_CURVE('',#22343,#22377,#5012,.T.) ;
#28421 = EDGE_CURVE('',#22377,#21864,#1263,.F.) ;
#28422 = EDGE_CURVE('',#22347,#22378,#5013,.T.) ;
#28423 = EDGE_CURVE('',#22378,#22379,#18857,.F.) ;
#28424 = EDGE_CURVE('',#22379,#22345,#5014,.T.) ;
#28425 = EDGE_CURVE('',#22200,#22350,#5015,.T.) ;
#28426 = EDGE_CURVE('',#22201,#21948,#5016,.T.) ;
#28427 = EDGE_CURVE('',#22202,#22351,#5017,.T.) ;
#28428 = EDGE_CURVE('',#22203,#22352,#5018,.T.) ;
#28429 = EDGE_CURVE('',#22371,#22380,#5019,.T.) ;
#28430 = EDGE_CURVE('',#22380,#22381,#18858,.F.) ;
#28431 = EDGE_CURVE('',#22381,#21942,#5020,.T.) ;
#28432 = EDGE_CURVE('',#22207,#22359,#5021,.T.) ;
#28433 = EDGE_CURVE('',#22382,#22357,#5022,.T.) ;
#28434 = EDGE_CURVE('',#22382,#22378,#5023,.T.) ;
#28435 = EDGE_CURVE('',#22326,#22380,#5024,.T.) ;
#28436 = EDGE_CURVE('',#22381,#22383,#5025,.T.) ;
#28437 = EDGE_CURVE('',#22367,#22383,#5026,.T.) ;
#28438 = EDGE_CURVE('',#22204,#22365,#5027,.T.) ;
#28439 = EDGE_CURVE('',#22374,#22327,#5028,.T.) ;
#28440 = EDGE_CURVE('',#22384,#22375,#5029,.T.) ;
#28441 = EDGE_CURVE('',#22383,#22384,#18859,.F.) ;
#28442 = EDGE_CURVE('',#22385,#22386,#18860,.F.) ;
#28443 = EDGE_CURVE('',#22386,#22387,#5030,.T.) ;
#28444 = EDGE_CURVE('',#22387,#22388,#18861,.F.) ;
#28445 = EDGE_CURVE('',#22388,#22385,#5031,.T.) ;
#28446 = EDGE_CURVE('',#22389,#22386,#5032,.T.) ;
#28447 = EDGE_CURVE('',#22390,#22389,#5033,.T.) ;
#28448 = EDGE_CURVE('',#22387,#22390,#5034,.T.) ;
#28449 = EDGE_CURVE('',#22391,#22390,#18862,.F.) ;
#28450 = EDGE_CURVE('',#22389,#22392,#18863,.F.) ;
#28451 = EDGE_CURVE('',#22392,#22391,#5035,.T.) ;
#28452 = EDGE_CURVE('',#22393,#22394,#18864,.T.) ;
#28453 = EDGE_CURVE('',#22395,#22394,#18865,.T.) ;
#28454 = EDGE_CURVE('',#22396,#22395,#18866,.F.) ;
#28455 = EDGE_CURVE('',#22393,#22396,#18867,.T.) ;
#28456 = EDGE_CURVE('',#22397,#22398,#18868,.F.) ;
#28457 = EDGE_CURVE('',#22399,#22397,#18869,.T.) ;
#28458 = EDGE_CURVE('',#22399,#22400,#18870,.T.) ;
#28459 = EDGE_CURVE('',#22398,#22400,#18871,.T.) ;
#28460 = EDGE_CURVE('',#22394,#22399,#5036,.T.) ;
#28461 = EDGE_CURVE('',#22397,#22395,#5037,.T.) ;
#28462 = EDGE_CURVE('',#22401,#22402,#18872,.T.) ;
#28463 = EDGE_CURVE('',#22402,#22403,#5038,.T.) ;
#28464 = EDGE_CURVE('',#22403,#22404,#18873,.F.) ;
#28465 = EDGE_CURVE('',#22404,#22401,#5039,.T.) ;
#28466 = EDGE_CURVE('',#22405,#22406,#18874,.T.) ;
#28467 = EDGE_CURVE('',#22406,#22402,#18875,.T.) ;
#28468 = EDGE_CURVE('',#22401,#22405,#18876,.T.) ;
#28469 = EDGE_CURVE('',#22400,#22406,#5040,.T.) ;
#28470 = EDGE_CURVE('',#22405,#22398,#5041,.T.) ;
#28471 = EDGE_CURVE('',#22407,#22408,#18877,.T.) ;
#28472 = EDGE_CURVE('',#22407,#22397,#5042,.T.) ;
#28473 = EDGE_CURVE('',#22398,#22408,#5043,.T.) ;
#28474 = EDGE_CURVE('',#22409,#22410,#18878,.T.) ;
#28475 = EDGE_CURVE('',#22409,#22396,#5044,.T.) ;
#28476 = EDGE_CURVE('',#22395,#22410,#5045,.T.) ;
#28477 = EDGE_CURVE('',#22411,#22412,#18879,.T.) ;
#28478 = EDGE_CURVE('',#22412,#22393,#5046,.T.) ;
#28479 = EDGE_CURVE('',#22396,#22411,#5047,.T.) ;
#28480 = EDGE_CURVE('',#22413,#22414,#18880,.T.) ;
#28481 = EDGE_CURVE('',#22414,#22412,#18881,.T.) ;
#28482 = EDGE_CURVE('',#22411,#22413,#18882,.T.) ;
#28483 = EDGE_CURVE('',#22415,#22416,#18883,.F.) ;
#28484 = EDGE_CURVE('',#22416,#22414,#5048,.T.) ;
#28485 = EDGE_CURVE('',#22413,#22415,#5049,.T.) ;
#28486 = EDGE_CURVE('',#22406,#22417,#5050,.T.) ;
#28487 = EDGE_CURVE('',#22418,#22417,#18884,.T.) ;
#28488 = EDGE_CURVE('',#22402,#22418,#5051,.T.) ;
#28489 = EDGE_CURVE('',#22419,#22412,#5052,.T.) ;
#28490 = EDGE_CURVE('',#22420,#22419,#5053,.T.) ;
#28491 = EDGE_CURVE('',#22421,#22420,#18885,.T.) ;
#28492 = EDGE_CURVE('',#22422,#22421,#5054,.T.) ;
#28493 = EDGE_CURVE('',#22423,#22422,#5055,.T.) ;
#28494 = EDGE_CURVE('',#22424,#22423,#18886,.T.) ;
#28495 = EDGE_CURVE('',#22425,#22424,#5056,.T.) ;
#28496 = EDGE_CURVE('',#22426,#22425,#18887,.T.) ;
#28497 = EDGE_CURVE('',#22427,#22426,#5057,.T.) ;
#28498 = EDGE_CURVE('',#22428,#22427,#18888,.T.) ;
#28499 = EDGE_CURVE('',#22417,#22428,#5058,.T.) ;
#28500 = EDGE_CURVE('',#22429,#22414,#5059,.T.) ;
#28501 = EDGE_CURVE('',#22419,#22429,#18889,.T.) ;
#28502 = EDGE_CURVE('',#22430,#21869,#5060,.T.) ;
#28503 = EDGE_CURVE('',#22430,#22431,#5061,.T.) ;
#28504 = EDGE_CURVE('',#22432,#22431,#5062,.T.) ;
#28505 = EDGE_CURVE('',#22433,#22432,#5063,.T.) ;
#28506 = EDGE_CURVE('',#22429,#22433,#5064,.T.) ;
#28507 = EDGE_CURVE('',#22416,#22403,#5065,.T.) ;
#28508 = EDGE_CURVE('',#21949,#22418,#5066,.T.) ;
#28509 = EDGE_CURVE('',#22304,#22434,#18890,.T.) ;
#28510 = EDGE_CURVE('',#22434,#22435,#5067,.T.) ;
#28511 = EDGE_CURVE('',#22435,#22305,#456,.T.) ;
#28512 = EDGE_CURVE('',#22306,#22436,#18891,.T.) ;
#28513 = EDGE_CURVE('',#22436,#21922,#457,.T.) ;
#28514 = EDGE_CURVE('',#22435,#22436,#5068,.T.) ;
#28515 = EDGE_CURVE('',#22307,#22437,#18892,.T.) ;
#28516 = EDGE_CURVE('',#22437,#22434,#18893,.T.) ;
#28517 = EDGE_CURVE('',#22308,#22438,#18894,.T.) ;
#28518 = EDGE_CURVE('',#22438,#22437,#5069,.T.) ;
#28519 = EDGE_CURVE('',#22309,#22439,#18895,.T.) ;
#28520 = EDGE_CURVE('',#22439,#22438,#18896,.T.) ;
#28521 = EDGE_CURVE('',#22316,#22440,#18897,.T.) ;
#28522 = EDGE_CURVE('',#22440,#22439,#5070,.T.) ;
#28523 = EDGE_CURVE('',#22315,#22441,#18898,.T.) ;
#28524 = EDGE_CURVE('',#22441,#22440,#18899,.T.) ;
#28525 = EDGE_CURVE('',#22314,#22442,#18900,.T.) ;
#28526 = EDGE_CURVE('',#22442,#22441,#5071,.T.) ;
#28527 = EDGE_CURVE('',#22313,#22443,#18901,.T.) ;
#28528 = EDGE_CURVE('',#22443,#22442,#18902,.T.) ;
#28529 = EDGE_CURVE('',#22312,#22444,#18903,.T.) ;
#28530 = EDGE_CURVE('',#22444,#22443,#5072,.T.) ;
#28531 = EDGE_CURVE('',#22311,#22445,#18904,.T.) ;
#28532 = EDGE_CURVE('',#22445,#22444,#18905,.T.) ;
#28533 = EDGE_CURVE('',#22310,#22446,#18906,.T.) ;
#28534 = EDGE_CURVE('',#22446,#22445,#5073,.T.) ;
#28535 = EDGE_CURVE('',#22317,#22447,#18907,.T.) ;
#28536 = EDGE_CURVE('',#22447,#22446,#458,.T.) ;
#28537 = EDGE_CURVE('',#22318,#22448,#18908,.T.) ;
#28538 = EDGE_CURVE('',#22448,#22447,#5074,.T.) ;
#28539 = EDGE_CURVE('',#22319,#22449,#18909,.T.) ;
#28540 = EDGE_CURVE('',#22449,#22448,#459,.T.) ;
#28541 = EDGE_CURVE('',#22321,#22450,#18910,.T.) ;
#28542 = EDGE_CURVE('',#22450,#22449,#460,.T.) ;
#28543 = EDGE_CURVE('',#22320,#21787,#18911,.T.) ;
#28544 = EDGE_CURVE('',#21787,#22450,#1264,.T.) ;
#28545 = EDGE_CURVE('',#22017,#21788,#18912,.T.) ;
#28546 = EDGE_CURVE('',#22016,#21789,#18913,.T.) ;
#28547 = EDGE_CURVE('',#22451,#21790,#18914,.T.) ;
#28548 = EDGE_CURVE('',#22016,#22451,#18915,.T.) ;
#28549 = EDGE_CURVE('',#22452,#21791,#18916,.T.) ;
#28550 = EDGE_CURVE('',#22451,#22452,#5075,.T.) ;
#28551 = EDGE_CURVE('',#22453,#21792,#18917,.T.) ;
#28552 = EDGE_CURVE('',#22452,#22453,#18918,.T.) ;
#28553 = EDGE_CURVE('',#22454,#21793,#18919,.T.) ;
#28554 = EDGE_CURVE('',#22453,#22454,#18920,.T.) ;
#28555 = EDGE_CURVE('',#22269,#21794,#18921,.T.) ;
#28556 = EDGE_CURVE('',#22454,#22269,#5076,.T.) ;
#28557 = EDGE_CURVE('',#22268,#21795,#18922,.T.) ;
#28558 = EDGE_CURVE('',#22271,#21796,#18923,.T.) ;
#28559 = EDGE_CURVE('',#22271,#22048,#18924,.T.) ;
#28560 = EDGE_CURVE('',#22455,#22048,#5077,.T.) ;
#28561 = EDGE_CURVE('',#22047,#22455,#5078,.T.) ;
#28562 = EDGE_CURVE('',#22455,#22093,#18925,.T.) ;
#28563 = EDGE_CURVE('',#21978,#22454,#5079,.T.) ;
#28564 = EDGE_CURVE('',#22453,#21980,#5080,.T.) ;
#28565 = EDGE_CURVE('',#21982,#22452,#5081,.T.) ;
#28566 = EDGE_CURVE('',#21984,#22451,#5082,.T.) ;
#28567 = EDGE_CURVE('',#22418,#22456,#18926,.T.) ;
#28568 = EDGE_CURVE('',#22456,#21950,#5083,.T.) ;
#28569 = EDGE_CURVE('',#21901,#22430,#461,.T.) ;
#28570 = EDGE_CURVE('',#21902,#22457,#5084,.T.) ;
#28571 = EDGE_CURVE('',#22457,#21899,#18927,.T.) ;
#28572 = EDGE_CURVE('',#22458,#21900,#18928,.T.) ;
#28573 = EDGE_CURVE('',#22457,#22458,#18929,.T.) ;
#28574 = EDGE_CURVE('',#22458,#22430,#5085,.T.) ;
#28575 = EDGE_CURVE('',#22417,#22459,#18930,.T.) ;
#28576 = EDGE_CURVE('',#22459,#22456,#18931,.T.) ;
#28577 = EDGE_CURVE('',#22428,#22460,#18932,.T.) ;
#28578 = EDGE_CURVE('',#22460,#22459,#5086,.T.) ;
#28579 = EDGE_CURVE('',#22427,#21943,#18933,.T.) ;
#28580 = EDGE_CURVE('',#21943,#22460,#18934,.T.) ;
#28581 = EDGE_CURVE('',#22426,#21944,#18935,.T.) ;
#28582 = EDGE_CURVE('',#22425,#22376,#18936,.T.) ;
#28583 = EDGE_CURVE('',#22424,#22461,#18937,.T.) ;
#28584 = EDGE_CURVE('',#22461,#22376,#5087,.T.) ;
#28585 = EDGE_CURVE('',#22423,#22462,#18938,.T.) ;
#28586 = EDGE_CURVE('',#22462,#22461,#18939,.T.) ;
#28587 = EDGE_CURVE('',#22463,#22462,#5088,.T.) ;
#28588 = EDGE_CURVE('',#22422,#22463,#462,.T.) ;
#28589 = EDGE_CURVE('',#22464,#22465,#18940,.T.) ;
#28590 = EDGE_CURVE('',#22465,#22466,#5089,.T.) ;
#28591 = EDGE_CURVE('',#22466,#22467,#18941,.T.) ;
#28592 = EDGE_CURVE('',#22467,#22464,#5090,.T.) ;
#28593 = EDGE_CURVE('',#22468,#22433,#18942,.T.) ;
#28594 = EDGE_CURVE('',#22433,#22467,#18943,.T.) ;
#28595 = EDGE_CURVE('',#22466,#22468,#18944,.T.) ;
#28596 = EDGE_CURVE('',#22469,#22429,#18945,.T.) ;
#28597 = EDGE_CURVE('',#22468,#22469,#5091,.T.) ;
#28598 = EDGE_CURVE('',#22470,#22419,#18946,.T.) ;
#28599 = EDGE_CURVE('',#22469,#22470,#18947,.T.) ;
#28600 = EDGE_CURVE('',#22471,#22420,#18948,.T.) ;
#28601 = EDGE_CURVE('',#22470,#22471,#5092,.T.) ;
#28602 = EDGE_CURVE('',#22472,#22421,#18949,.T.) ;
#28603 = EDGE_CURVE('',#22471,#22472,#18950,.T.) ;
#28604 = EDGE_CURVE('',#22472,#22463,#5093,.T.) ;
#28605 = EDGE_CURVE('',#21951,#22460,#5094,.T.) ;
#28606 = EDGE_CURVE('',#22473,#22461,#5095,.T.) ;
#28607 = EDGE_CURVE('',#22474,#22473,#18951,.T.) ;
#28608 = EDGE_CURVE('',#22475,#22474,#5096,.T.) ;
#28609 = EDGE_CURVE('',#22476,#22475,#18952,.T.) ;
#28610 = EDGE_CURVE('',#22477,#22476,#5097,.T.) ;
#28611 = EDGE_CURVE('',#22377,#22477,#18953,.T.) ;
#28612 = EDGE_CURVE('',#22478,#22479,#1265,.T.) ;
#28613 = EDGE_CURVE('',#22480,#22478,#5098,.T.) ;
#28614 = EDGE_CURVE('',#22481,#22480,#1266,.T.) ;
#28615 = EDGE_CURVE('',#22482,#22481,#5099,.T.) ;
#28616 = EDGE_CURVE('',#22483,#22482,#5100,.T.) ;
#28617 = EDGE_CURVE('',#22484,#22483,#5101,.T.) ;
#28618 = EDGE_CURVE('',#22479,#22484,#5102,.T.) ;
#28619 = EDGE_CURVE('',#22485,#22486,#5103,.T.) ;
#28620 = EDGE_CURVE('',#22487,#22485,#5104,.T.) ;
#28621 = EDGE_CURVE('',#22488,#22487,#5105,.T.) ;
#28622 = EDGE_CURVE('',#22489,#22488,#1267,.T.) ;
#28623 = EDGE_CURVE('',#22490,#22489,#5106,.T.) ;
#28624 = EDGE_CURVE('',#22491,#22490,#1268,.T.) ;
#28625 = EDGE_CURVE('',#22486,#22491,#5107,.T.) ;
#28626 = EDGE_CURVE('',#22462,#22492,#5108,.T.) ;
#28627 = EDGE_CURVE('',#22492,#22473,#18954,.F.) ;
#28628 = EDGE_CURVE('',#22463,#22493,#5109,.T.) ;
#28629 = EDGE_CURVE('',#22494,#22493,#5110,.T.) ;
#28630 = EDGE_CURVE('',#22492,#22494,#463,.T.) ;
#28631 = EDGE_CURVE('',#22495,#22472,#5111,.T.) ;
#28632 = EDGE_CURVE('',#22495,#22138,#5112,.T.) ;
#28633 = EDGE_CURVE('',#22496,#22137,#5113,.T.) ;
#28634 = EDGE_CURVE('',#22493,#22496,#464,.T.) ;
#28635 = EDGE_CURVE('',#22497,#22497,#18955,.T.) ;
#28636 = EDGE_CURVE('',#22471,#22498,#5114,.T.) ;
#28637 = EDGE_CURVE('',#22498,#22495,#18956,.T.) ;
#28638 = EDGE_CURVE('',#22465,#22499,#5115,.T.) ;
#28639 = EDGE_CURVE('',#22499,#22500,#5116,.T.) ;
#28640 = EDGE_CURVE('',#22501,#22500,#5117,.T.) ;
#28641 = EDGE_CURVE('',#22498,#22501,#5118,.T.) ;
#28642 = EDGE_CURVE('',#22464,#22142,#5119,.T.) ;
#28643 = EDGE_CURVE('',#22499,#22141,#5120,.T.) ;
#28644 = EDGE_CURVE('',#22502,#22503,#465,.T.) ;
#28645 = EDGE_CURVE('',#22504,#22503,#18957,.T.) ;
#28646 = EDGE_CURVE('',#22505,#22504,#466,.F.) ;
#28647 = EDGE_CURVE('',#22502,#22505,#18958,.T.) ;
#28648 = EDGE_CURVE('',#22506,#22507,#467,.T.) ;
#28649 = EDGE_CURVE('',#22508,#22507,#18959,.T.) ;
#28650 = EDGE_CURVE('',#22509,#22508,#468,.F.) ;
#28651 = EDGE_CURVE('',#22506,#22509,#18960,.T.) ;
#28652 = EDGE_CURVE('',#22030,#22510,#5121,.T.) ;
#28653 = EDGE_CURVE('',#22510,#22511,#18961,.T.) ;
#28654 = EDGE_CURVE('',#22511,#22028,#5122,.T.) ;
#28655 = EDGE_CURVE('',#22512,#22513,#18962,.T.) ;
#28656 = EDGE_CURVE('',#22513,#22511,#1269,.T.) ;
#28657 = EDGE_CURVE('',#22510,#22512,#1270,.T.) ;
#28658 = EDGE_CURVE('',#22514,#22515,#18963,.T.) ;
#28659 = EDGE_CURVE('',#22515,#22513,#18964,.T.) ;
#28660 = EDGE_CURVE('',#22512,#22514,#18965,.T.) ;
#28661 = EDGE_CURVE('',#22507,#22515,#5123,.T.) ;
#28662 = EDGE_CURVE('',#22514,#22508,#5124,.T.) ;
#28663 = EDGE_CURVE('',#22516,#22517,#18966,.T.) ;
#28664 = EDGE_CURVE('',#22516,#22509,#5125,.T.) ;
#28665 = EDGE_CURVE('',#22508,#22517,#5126,.T.) ;
#28666 = EDGE_CURVE('',#22503,#22506,#5127,.T.) ;
#28667 = EDGE_CURVE('',#22509,#22504,#5128,.T.) ;
#28668 = EDGE_CURVE('',#22518,#22519,#18967,.T.) ;
#28669 = EDGE_CURVE('',#22518,#22505,#5129,.T.) ;
#28670 = EDGE_CURVE('',#22504,#22519,#5130,.T.) ;
#28671 = EDGE_CURVE('',#22066,#22520,#18968,.T.) ;
#28672 = EDGE_CURVE('',#22520,#22502,#5131,.T.) ;
#28673 = EDGE_CURVE('',#22505,#22066,#5132,.T.) ;
#28674 = EDGE_CURVE('',#22065,#22521,#18969,.T.) ;
#28675 = EDGE_CURVE('',#22521,#22520,#469,.T.) ;
#28676 = EDGE_CURVE('',#22072,#22521,#1271,.T.) ;
#28677 = EDGE_CURVE('',#22029,#22522,#5133,.F.) ;
#28678 = EDGE_CURVE('',#22522,#22523,#18970,.F.) ;
#28679 = EDGE_CURVE('',#22523,#22512,#5134,.T.) ;
#28680 = EDGE_CURVE('',#22026,#22511,#5135,.T.) ;
#28681 = EDGE_CURVE('',#22515,#22040,#5136,.T.) ;
#28682 = EDGE_CURVE('',#22524,#22521,#5137,.T.) ;
#28683 = EDGE_CURVE('',#22524,#22525,#470,.T.) ;
#28684 = EDGE_CURVE('',#22038,#22525,#5138,.T.) ;
#28685 = EDGE_CURVE('',#22052,#22526,#18971,.T.) ;
#28686 = EDGE_CURVE('',#22527,#22526,#471,.T.) ;
#28687 = EDGE_CURVE('',#22527,#22528,#5139,.T.) ;
#28688 = EDGE_CURVE('',#22528,#22524,#1272,.T.) ;
#28689 = EDGE_CURVE('',#22529,#22530,#5140,.T.) ;
#28690 = EDGE_CURVE('',#22530,#22068,#472,.F.) ;
#28691 = EDGE_CURVE('',#22067,#22529,#473,.T.) ;
#28692 = EDGE_CURVE('',#22061,#22531,#5141,.T.) ;
#28693 = EDGE_CURVE('',#22531,#22532,#474,.T.) ;
#28694 = EDGE_CURVE('',#22532,#22533,#5142,.T.) ;
#28695 = EDGE_CURVE('',#22533,#22529,#475,.T.) ;
#28696 = EDGE_CURVE('',#22530,#21924,#5143,.F.) ;
#28697 = EDGE_CURVE('',#22534,#22533,#5144,.T.) ;
#28698 = EDGE_CURVE('',#22534,#22535,#5145,.T.) ;
#28699 = EDGE_CURVE('',#22536,#22535,#5146,.F.) ;
#28700 = EDGE_CURVE('',#22536,#21830,#5147,.T.) ;
#28701 = EDGE_CURVE('',#22532,#22537,#5148,.T.) ;
#28702 = EDGE_CURVE('',#22534,#22537,#5149,.T.) ;
#28703 = EDGE_CURVE('',#22537,#22518,#5150,.T.) ;
#28704 = EDGE_CURVE('',#22063,#22531,#5151,.T.) ;
#28705 = EDGE_CURVE('',#21835,#22538,#1273,.T.) ;
#28706 = EDGE_CURVE('',#21854,#22538,#18972,.T.) ;
#28707 = EDGE_CURVE('',#21931,#21856,#18973,.T.) ;
#28708 = EDGE_CURVE('',#21855,#21932,#18974,.T.) ;
#28709 = EDGE_CURVE('',#22538,#21932,#476,.T.) ;
#28710 = EDGE_CURVE('',#22539,#21857,#18975,.T.) ;
#28711 = EDGE_CURVE('',#21931,#22539,#1274,.T.) ;
#28712 = EDGE_CURVE('',#22540,#21858,#18976,.T.) ;
#28713 = EDGE_CURVE('',#22539,#22540,#477,.T.) ;
#28714 = EDGE_CURVE('',#22541,#21968,#1275,.T.) ;
#28715 = EDGE_CURVE('',#22540,#22541,#1276,.T.) ;
#28716 = EDGE_CURVE('',#21834,#21927,#5152,.T.) ;
#28717 = EDGE_CURVE('',#21865,#22542,#1277,.F.) ;
#28718 = EDGE_CURVE('',#22542,#22543,#5153,.T.) ;
#28719 = EDGE_CURVE('',#22543,#22544,#1278,.F.) ;
#28720 = EDGE_CURVE('',#22544,#22545,#5154,.T.) ;
#28721 = EDGE_CURVE('',#22546,#22545,#478,.T.) ;
#28722 = EDGE_CURVE('',#21832,#22546,#5155,.T.) ;
#28723 = EDGE_CURVE('',#22546,#21822,#479,.T.) ;
#28724 = EDGE_CURVE('',#22545,#22547,#18977,.T.) ;
#28725 = EDGE_CURVE('',#22547,#21925,#480,.T.) ;
#28726 = EDGE_CURVE('',#22548,#22549,#18978,.T.) ;
#28727 = EDGE_CURVE('',#22549,#22547,#5156,.T.) ;
#28728 = EDGE_CURVE('',#22545,#22548,#5157,.T.) ;
#28729 = EDGE_CURVE('',#22550,#22069,#18979,.T.) ;
#28730 = EDGE_CURVE('',#22069,#22549,#481,.T.) ;
#28731 = EDGE_CURVE('',#22548,#22550,#482,.T.) ;
#28732 = EDGE_CURVE('',#22550,#22551,#483,.T.) ;
#28733 = EDGE_CURVE('',#22551,#22070,#1279,.F.) ;
#28734 = EDGE_CURVE('',#22552,#22444,#5158,.T.) ;
#28735 = EDGE_CURVE('',#22552,#22553,#18980,.T.) ;
#28736 = EDGE_CURVE('',#22553,#22554,#5159,.T.) ;
#28737 = EDGE_CURVE('',#22554,#22555,#5160,.T.) ;
#28738 = EDGE_CURVE('',#22555,#22556,#5161,.T.) ;
#28739 = EDGE_CURVE('',#22556,#22528,#18981,.T.) ;
#28740 = EDGE_CURVE('',#22557,#22527,#5162,.T.) ;
#28741 = EDGE_CURVE('',#22443,#22557,#5163,.T.) ;
#28742 = EDGE_CURVE('',#22558,#22559,#5164,.T.) ;
#28743 = EDGE_CURVE('',#22560,#22558,#18982,.T.) ;
#28744 = EDGE_CURVE('',#22561,#22560,#5165,.T.) ;
#28745 = EDGE_CURVE('',#22562,#22561,#5166,.T.) ;
#28746 = EDGE_CURVE('',#22563,#22562,#5167,.T.) ;
#28747 = EDGE_CURVE('',#22564,#22563,#18983,.T.) ;
#28748 = EDGE_CURVE('',#22565,#22564,#5168,.T.) ;
#28749 = EDGE_CURVE('',#22566,#22565,#5169,.T.) ;
#28750 = EDGE_CURVE('',#22567,#22566,#5170,.T.) ;
#28751 = EDGE_CURVE('',#22568,#22567,#5171,.T.) ;
#28752 = EDGE_CURVE('',#22559,#22568,#5172,.T.) ;
#28753 = EDGE_CURVE('',#22569,#22570,#5173,.T.) ;
#28754 = EDGE_CURVE('',#22571,#22570,#5174,.T.) ;
#28755 = EDGE_CURVE('',#22572,#22571,#18984,.T.) ;
#28756 = EDGE_CURVE('',#22573,#22572,#5175,.T.) ;
#28757 = EDGE_CURVE('',#22574,#22573,#5176,.T.) ;
#28758 = EDGE_CURVE('',#22575,#22574,#5177,.T.) ;
#28759 = EDGE_CURVE('',#22576,#22575,#5178,.T.) ;
#28760 = EDGE_CURVE('',#22577,#22576,#5179,.T.) ;
#28761 = EDGE_CURVE('',#22578,#22577,#5180,.T.) ;
#28762 = EDGE_CURVE('',#22579,#22578,#18985,.T.) ;
#28763 = EDGE_CURVE('',#22569,#22579,#5181,.T.) ;
#28764 = EDGE_CURVE('',#22580,#22581,#5182,.T.) ;
#28765 = EDGE_CURVE('',#22582,#22580,#5183,.T.) ;
#28766 = EDGE_CURVE('',#22583,#22582,#5184,.T.) ;
#28767 = EDGE_CURVE('',#22581,#22583,#5185,.T.) ;
#28768 = EDGE_CURVE('',#22551,#22557,#484,.T.) ;
#28769 = EDGE_CURVE('',#22548,#22442,#5186,.T.) ;
#28770 = EDGE_CURVE('',#22584,#22544,#485,.T.) ;
#28771 = EDGE_CURVE('',#22441,#22584,#5187,.T.) ;
#28772 = EDGE_CURVE('',#22527,#22071,#18986,.T.) ;
#28773 = EDGE_CURVE('',#22585,#21933,#486,.F.) ;
#28774 = EDGE_CURVE('',#22539,#22585,#18987,.T.) ;
#28775 = EDGE_CURVE('',#22585,#22586,#5188,.T.) ;
#28776 = EDGE_CURVE('',#22586,#22541,#1280,.T.) ;
#28777 = EDGE_CURVE('',#21937,#22587,#487,.F.) ;
#28778 = EDGE_CURVE('',#22587,#22585,#5189,.T.) ;
#28779 = EDGE_CURVE('',#22588,#22586,#5190,.T.) ;
#28780 = EDGE_CURVE('',#22588,#21963,#18988,.T.) ;
#28781 = EDGE_CURVE('',#21964,#22589,#18989,.F.) ;
#28782 = EDGE_CURVE('',#22589,#22588,#5191,.F.) ;
#28783 = EDGE_CURVE('',#22589,#22023,#5192,.T.) ;
#28784 = EDGE_CURVE('',#22590,#22587,#5193,.T.) ;
#28785 = EDGE_CURVE('',#22031,#22590,#488,.T.) ;
#28786 = EDGE_CURVE('',#22591,#21828,#5194,.F.) ;
#28787 = EDGE_CURVE('',#22591,#21849,#5195,.F.) ;
#28788 = EDGE_CURVE('',#21826,#22536,#5196,.T.) ;
#28789 = EDGE_CURVE('',#21827,#22535,#5197,.T.) ;
#28790 = EDGE_CURVE('',#21786,#22592,#1281,.T.) ;
#28791 = EDGE_CURVE('',#22592,#22450,#5198,.T.) ;
#28792 = EDGE_CURVE('',#22525,#21785,#1282,.T.) ;
#28793 = EDGE_CURVE('',#22556,#22593,#5199,.T.) ;
#28794 = EDGE_CURVE('',#22593,#22594,#18990,.T.) ;
#28795 = EDGE_CURVE('',#22553,#22594,#5200,.T.) ;
#28796 = EDGE_CURVE('',#22595,#22552,#1283,.T.) ;
#28797 = EDGE_CURVE('',#22592,#22595,#489,.T.) ;
#28798 = EDGE_CURVE('',#22445,#22595,#5201,.T.) ;
#28799 = EDGE_CURVE('',#22517,#22523,#5202,.T.) ;
#28800 = EDGE_CURVE('',#22596,#22597,#5203,.T.) ;
#28801 = EDGE_CURVE('',#22598,#22596,#5204,.T.) ;
#28802 = EDGE_CURVE('',#22599,#22598,#5205,.T.) ;
#28803 = EDGE_CURVE('',#22599,#22153,#5206,.T.) ;
#28804 = EDGE_CURVE('',#22597,#22152,#5207,.T.) ;
#28805 = EDGE_CURVE('',#22600,#22599,#18991,.T.) ;
#28806 = EDGE_CURVE('',#22154,#22600,#5208,.T.) ;
#28807 = EDGE_CURVE('',#22601,#22157,#5209,.T.) ;
#28808 = EDGE_CURVE('',#22601,#22602,#5210,.T.) ;
#28809 = EDGE_CURVE('',#22602,#22158,#5211,.T.) ;
#28810 = EDGE_CURVE('',#22602,#22086,#1284,.T.) ;
#28811 = EDGE_CURVE('',#22603,#22596,#18992,.T.) ;
#28812 = EDGE_CURVE('',#22604,#22603,#5212,.T.) ;
#28813 = EDGE_CURVE('',#22598,#22604,#18993,.T.) ;
#28814 = EDGE_CURVE('',#22605,#22156,#5213,.T.) ;
#28815 = EDGE_CURVE('',#22601,#22605,#18994,.T.) ;
#28816 = EDGE_CURVE('',#22606,#22151,#5214,.T.) ;
#28817 = EDGE_CURVE('',#22606,#22597,#5215,.T.) ;
#28818 = EDGE_CURVE('',#22155,#22607,#5216,.T.) ;
#28819 = EDGE_CURVE('',#22607,#22605,#5217,.F.) ;
#28820 = EDGE_CURVE('',#22600,#22607,#5218,.F.) ;
#28821 = EDGE_CURVE('',#22608,#22604,#5219,.F.) ;
#28822 = EDGE_CURVE('',#22609,#22608,#5220,.T.) ;
#28823 = EDGE_CURVE('',#22610,#22609,#18995,.T.) ;
#28824 = EDGE_CURVE('',#22611,#22610,#5221,.T.) ;
#28825 = EDGE_CURVE('',#22092,#22611,#18996,.T.) ;
#28826 = EDGE_CURVE('',#22079,#22612,#5222,.T.) ;
#28827 = EDGE_CURVE('',#22612,#22078,#5223,.T.) ;
#28828 = EDGE_CURVE('',#22609,#22044,#18997,.T.) ;
#28829 = EDGE_CURVE('',#22047,#22610,#490,.T.) ;
#28830 = EDGE_CURVE('',#22455,#22611,#18998,.T.) ;
#28831 = EDGE_CURVE('',#22608,#22045,#491,.F.) ;
#28832 = EDGE_CURVE('',#22046,#22603,#5224,.T.) ;
#28833 = EDGE_CURVE('',#22613,#22388,#5225,.T.) ;
#28834 = EDGE_CURVE('',#22614,#22613,#5226,.T.) ;
#28835 = EDGE_CURVE('',#22385,#22614,#5227,.T.) ;
#28836 = EDGE_CURVE('',#22615,#22392,#5228,.T.) ;
#28837 = EDGE_CURVE('',#22616,#22615,#5229,.T.) ;
#28838 = EDGE_CURVE('',#22391,#22616,#5230,.T.) ;
#28839 = EDGE_CURVE('',#22616,#22613,#5231,.T.) ;
#28840 = EDGE_CURVE('',#22614,#22615,#5232,.T.) ;
#28841 = EDGE_CURVE('',#22409,#22415,#5233,.T.) ;
#28842 = EDGE_CURVE('',#22407,#22410,#5234,.T.) ;
#28843 = EDGE_CURVE('',#22404,#22408,#5235,.T.) ;
#28844 = EDGE_CURVE('',#22617,#22618,#5236,.T.) ;
#28845 = EDGE_CURVE('',#22618,#22619,#1285,.T.) ;
#28846 = EDGE_CURVE('',#22619,#22620,#5237,.T.) ;
#28847 = EDGE_CURVE('',#22617,#22620,#492,.T.) ;
#28848 = EDGE_CURVE('',#22618,#22621,#1286,.T.) ;
#28849 = EDGE_CURVE('',#22621,#22622,#1287,.T.) ;
#28850 = EDGE_CURVE('',#22622,#22619,#1288,.T.) ;
#28851 = EDGE_CURVE('',#22621,#22623,#5238,.T.) ;
#28852 = EDGE_CURVE('',#22623,#22624,#1289,.T.) ;
#28853 = EDGE_CURVE('',#22624,#22622,#5239,.T.) ;
#28854 = EDGE_CURVE('',#22625,#22624,#1290,.T.) ;
#28855 = EDGE_CURVE('',#22623,#22626,#1291,.T.) ;
#28856 = EDGE_CURVE('',#22626,#22625,#1292,.T.) ;
#28857 = EDGE_CURVE('',#22627,#22625,#5240,.T.) ;
#28858 = EDGE_CURVE('',#22626,#22628,#5241,.T.) ;
#28859 = EDGE_CURVE('',#22628,#22627,#493,.T.) ;
#28860 = EDGE_CURVE('',#22629,#22627,#5242,.T.) ;
#28861 = EDGE_CURVE('',#22628,#22630,#5243,.T.) ;
#28862 = EDGE_CURVE('',#22630,#22629,#494,.T.) ;
#28863 = EDGE_CURVE('',#22620,#22629,#5244,.T.) ;
#28864 = EDGE_CURVE('',#22630,#22617,#5245,.T.) ;
#28865 = EDGE_CURVE('',#22631,#22627,#5246,.T.) ;
#28866 = EDGE_CURVE('',#22632,#22631,#5247,.T.) ;
#28867 = EDGE_CURVE('',#22632,#22625,#5248,.T.) ;
#28868 = EDGE_CURVE('',#22633,#22629,#5249,.T.) ;
#28869 = EDGE_CURVE('',#22631,#22633,#5250,.T.) ;
#28870 = EDGE_CURVE('',#22634,#22620,#5251,.T.) ;
#28871 = EDGE_CURVE('',#22633,#22634,#5252,.T.) ;
#28872 = EDGE_CURVE('',#22635,#22619,#5253,.T.) ;
#28873 = EDGE_CURVE('',#22634,#22635,#5254,.T.) ;
#28874 = EDGE_CURVE('',#22636,#22637,#1293,.T.) ;
#28875 = EDGE_CURVE('',#22637,#22638,#1294,.T.) ;
#28876 = EDGE_CURVE('',#22638,#22639,#1295,.T.) ;
#28877 = EDGE_CURVE('',#22636,#22639,#1296,.T.) ;
#28878 = EDGE_CURVE('',#22637,#22640,#5255,.T.) ;
#28879 = EDGE_CURVE('',#22640,#22641,#495,.T.) ;
#28880 = EDGE_CURVE('',#22641,#22638,#5256,.T.) ;
#28881 = EDGE_CURVE('',#22640,#22642,#5257,.T.) ;
#28882 = EDGE_CURVE('',#22642,#22643,#496,.T.) ;
#28883 = EDGE_CURVE('',#22643,#22641,#5258,.T.) ;
#28884 = EDGE_CURVE('',#22644,#22643,#5259,.T.) ;
#28885 = EDGE_CURVE('',#22642,#22645,#5260,.T.) ;
#28886 = EDGE_CURVE('',#22645,#22644,#497,.T.) ;
#28887 = EDGE_CURVE('',#22646,#22644,#5261,.T.) ;
#28888 = EDGE_CURVE('',#22645,#22647,#5262,.T.) ;
#28889 = EDGE_CURVE('',#22647,#22646,#1297,.T.) ;
#28890 = EDGE_CURVE('',#22648,#22646,#1298,.T.) ;
#28891 = EDGE_CURVE('',#22647,#22649,#1299,.T.) ;
#28892 = EDGE_CURVE('',#22649,#22648,#1300,.T.) ;
#28893 = EDGE_CURVE('',#22639,#22648,#5263,.T.) ;
#28894 = EDGE_CURVE('',#22649,#22636,#5264,.T.) ;
#28895 = EDGE_CURVE('',#22650,#22646,#5265,.T.) ;
#28896 = EDGE_CURVE('',#22651,#22650,#5266,.T.) ;
#28897 = EDGE_CURVE('',#22651,#22644,#5267,.T.) ;
#28898 = EDGE_CURVE('',#22652,#22648,#5268,.T.) ;
#28899 = EDGE_CURVE('',#22650,#22652,#1301,.T.) ;
#28900 = EDGE_CURVE('',#22653,#22639,#5269,.T.) ;
#28901 = EDGE_CURVE('',#22652,#22653,#5270,.T.) ;
#28902 = EDGE_CURVE('',#22654,#22638,#5271,.T.) ;
#28903 = EDGE_CURVE('',#22653,#22654,#1302,.T.) ;
#28904 = EDGE_CURVE('',#22655,#22656,#5272,.T.) ;
#28905 = EDGE_CURVE('',#22656,#22657,#498,.T.) ;
#28906 = EDGE_CURVE('',#22657,#22658,#5273,.T.) ;
#28907 = EDGE_CURVE('',#22655,#22658,#499,.T.) ;
#28908 = EDGE_CURVE('',#22656,#22659,#5274,.T.) ;
#28909 = EDGE_CURVE('',#22659,#22660,#500,.T.) ;
#28910 = EDGE_CURVE('',#22660,#22657,#5275,.T.) ;
#28911 = EDGE_CURVE('',#22659,#22661,#5276,.T.) ;
#28912 = EDGE_CURVE('',#22661,#22662,#501,.T.) ;
#28913 = EDGE_CURVE('',#22662,#22660,#5277,.T.) ;
#28914 = EDGE_CURVE('',#22663,#22662,#5278,.T.) ;
#28915 = EDGE_CURVE('',#22661,#22664,#5279,.T.) ;
#28916 = EDGE_CURVE('',#22664,#22663,#502,.T.) ;
#28917 = EDGE_CURVE('',#22665,#22663,#5280,.T.) ;
#28918 = EDGE_CURVE('',#22664,#22666,#5281,.T.) ;
#28919 = EDGE_CURVE('',#22666,#22665,#503,.T.) ;
#28920 = EDGE_CURVE('',#22667,#22665,#5282,.T.) ;
#28921 = EDGE_CURVE('',#22666,#22668,#5283,.T.) ;
#28922 = EDGE_CURVE('',#22668,#22667,#504,.T.) ;
#28923 = EDGE_CURVE('',#22658,#22667,#5284,.T.) ;
#28924 = EDGE_CURVE('',#22668,#22655,#5285,.T.) ;
#28925 = EDGE_CURVE('',#22669,#22665,#5286,.T.) ;
#28926 = EDGE_CURVE('',#22670,#22669,#5287,.T.) ;
#28927 = EDGE_CURVE('',#22670,#22663,#5288,.T.) ;
#28928 = EDGE_CURVE('',#22671,#22667,#5289,.T.) ;
#28929 = EDGE_CURVE('',#22669,#22671,#5290,.T.) ;
#28930 = EDGE_CURVE('',#22672,#22658,#5291,.T.) ;
#28931 = EDGE_CURVE('',#22671,#22672,#5292,.T.) ;
#28932 = EDGE_CURVE('',#22673,#22657,#5293,.T.) ;
#28933 = EDGE_CURVE('',#22672,#22673,#5294,.T.) ;
#28934 = EDGE_CURVE('',#22674,#22675,#5295,.T.) ;
#28935 = EDGE_CURVE('',#22675,#22676,#505,.T.) ;
#28936 = EDGE_CURVE('',#22676,#22677,#5296,.T.) ;
#28937 = EDGE_CURVE('',#22674,#22677,#506,.T.) ;
#28938 = EDGE_CURVE('',#22678,#22676,#5297,.T.) ;
#28939 = EDGE_CURVE('',#22675,#22679,#5298,.T.) ;
#28940 = EDGE_CURVE('',#22679,#22678,#507,.T.) ;
#28941 = EDGE_CURVE('',#22680,#22678,#5299,.T.) ;
#28942 = EDGE_CURVE('',#22679,#22681,#5300,.T.) ;
#28943 = EDGE_CURVE('',#22681,#22680,#508,.T.) ;
#28944 = EDGE_CURVE('',#22677,#22680,#5301,.T.) ;
#28945 = EDGE_CURVE('',#22681,#22674,#5302,.T.) ;
#28946 = EDGE_CURVE('',#22682,#22677,#5303,.T.) ;
#28947 = EDGE_CURVE('',#22683,#22682,#5304,.T.) ;
#28948 = EDGE_CURVE('',#22683,#22680,#5305,.T.) ;
#28949 = EDGE_CURVE('',#22684,#22676,#5306,.T.) ;
#28950 = EDGE_CURVE('',#22682,#22684,#5307,.T.) ;
#28951 = EDGE_CURVE('',#22685,#22686,#5308,.T.) ;
#28952 = EDGE_CURVE('',#22686,#22687,#509,.T.) ;
#28953 = EDGE_CURVE('',#22687,#22688,#5309,.T.) ;
#28954 = EDGE_CURVE('',#22685,#22688,#510,.T.) ;
#28955 = EDGE_CURVE('',#22686,#22689,#5310,.T.) ;
#28956 = EDGE_CURVE('',#22689,#22690,#511,.T.) ;
#28957 = EDGE_CURVE('',#22690,#22687,#5311,.T.) ;
#28958 = EDGE_CURVE('',#22689,#22691,#5312,.T.) ;
#28959 = EDGE_CURVE('',#22691,#22692,#512,.T.) ;
#28960 = EDGE_CURVE('',#22692,#22690,#5313,.T.) ;
#28961 = EDGE_CURVE('',#22693,#22692,#5314,.T.) ;
#28962 = EDGE_CURVE('',#22691,#22694,#5315,.T.) ;
#28963 = EDGE_CURVE('',#22694,#22693,#513,.T.) ;
#28964 = EDGE_CURVE('',#22695,#22693,#5316,.T.) ;
#28965 = EDGE_CURVE('',#22694,#22696,#5317,.T.) ;
#28966 = EDGE_CURVE('',#22696,#22695,#514,.T.) ;
#28967 = EDGE_CURVE('',#22697,#22695,#5318,.T.) ;
#28968 = EDGE_CURVE('',#22696,#22698,#5319,.T.) ;
#28969 = EDGE_CURVE('',#22698,#22697,#515,.T.) ;
#28970 = EDGE_CURVE('',#22688,#22697,#5320,.T.) ;
#28971 = EDGE_CURVE('',#22698,#22685,#5321,.T.) ;
#28972 = EDGE_CURVE('',#22699,#22695,#5322,.T.) ;
#28973 = EDGE_CURVE('',#22700,#22699,#5323,.T.) ;
#28974 = EDGE_CURVE('',#22700,#22693,#5324,.T.) ;
#28975 = EDGE_CURVE('',#22701,#22697,#5325,.T.) ;
#28976 = EDGE_CURVE('',#22699,#22701,#5326,.T.) ;
#28977 = EDGE_CURVE('',#22702,#22688,#5327,.T.) ;
#28978 = EDGE_CURVE('',#22701,#22702,#5328,.T.) ;
#28979 = EDGE_CURVE('',#22703,#22687,#5329,.T.) ;
#28980 = EDGE_CURVE('',#22702,#22703,#5330,.T.) ;
#28981 = EDGE_CURVE('',#22704,#22705,#5331,.T.) ;
#28982 = EDGE_CURVE('',#22705,#22706,#516,.T.) ;
#28983 = EDGE_CURVE('',#22706,#22707,#5332,.T.) ;
#28984 = EDGE_CURVE('',#22704,#22707,#517,.T.) ;
#28985 = EDGE_CURVE('',#22708,#22706,#5333,.T.) ;
#28986 = EDGE_CURVE('',#22705,#22709,#5334,.T.) ;
#28987 = EDGE_CURVE('',#22709,#22708,#518,.T.) ;
#28988 = EDGE_CURVE('',#22710,#22708,#5335,.T.) ;
#28989 = EDGE_CURVE('',#22709,#22711,#5336,.T.) ;
#28990 = EDGE_CURVE('',#22711,#22710,#519,.T.) ;
#28991 = EDGE_CURVE('',#22707,#22710,#5337,.T.) ;
#28992 = EDGE_CURVE('',#22711,#22704,#5338,.T.) ;
#28993 = EDGE_CURVE('',#22712,#22707,#5339,.T.) ;
#28994 = EDGE_CURVE('',#22713,#22712,#5340,.T.) ;
#28995 = EDGE_CURVE('',#22713,#22710,#5341,.T.) ;
#28996 = EDGE_CURVE('',#22714,#22706,#5342,.T.) ;
#28997 = EDGE_CURVE('',#22712,#22714,#5343,.T.) ;
#28998 = EDGE_CURVE('',#22715,#22716,#5344,.T.) ;
#28999 = EDGE_CURVE('',#22716,#22717,#520,.T.) ;
#29000 = EDGE_CURVE('',#22717,#22718,#5345,.T.) ;
#29001 = EDGE_CURVE('',#22715,#22718,#521,.T.) ;
#29002 = EDGE_CURVE('',#22716,#22719,#5346,.T.) ;
#29003 = EDGE_CURVE('',#22719,#22720,#522,.T.) ;
#29004 = EDGE_CURVE('',#22720,#22717,#5347,.T.) ;
#29005 = EDGE_CURVE('',#22719,#22721,#5348,.T.) ;
#29006 = EDGE_CURVE('',#22721,#22722,#18999,.T.) ;
#29007 = EDGE_CURVE('',#22722,#22720,#5349,.T.) ;
#29008 = EDGE_CURVE('',#22723,#22724,#19000,.T.) ;
#29009 = EDGE_CURVE('',#22724,#22722,#19001,.T.) ;
#29010 = EDGE_CURVE('',#22721,#22723,#19002,.T.) ;
#29011 = EDGE_CURVE('',#22725,#22724,#5350,.T.) ;
#29012 = EDGE_CURVE('',#22723,#22726,#5351,.T.) ;
#29013 = EDGE_CURVE('',#22726,#22725,#523,.T.) ;
#29014 = EDGE_CURVE('',#22727,#22725,#5352,.T.) ;
#29015 = EDGE_CURVE('',#22726,#22728,#5353,.T.) ;
#29016 = EDGE_CURVE('',#22728,#22727,#524,.T.) ;
#29017 = EDGE_CURVE('',#22728,#22729,#5354,.T.) ;
#29018 = EDGE_CURVE('',#22729,#22730,#19003,.T.) ;
#29019 = EDGE_CURVE('',#22730,#22727,#5355,.T.) ;
#29020 = EDGE_CURVE('',#22731,#22732,#19004,.T.) ;
#29021 = EDGE_CURVE('',#22732,#22730,#19005,.T.) ;
#29022 = EDGE_CURVE('',#22729,#22731,#19006,.T.) ;
#29023 = EDGE_CURVE('',#22733,#22732,#5356,.T.) ;
#29024 = EDGE_CURVE('',#22731,#22734,#5357,.T.) ;
#29025 = EDGE_CURVE('',#22734,#22733,#525,.T.) ;
#29026 = EDGE_CURVE('',#22735,#22733,#5358,.T.) ;
#29027 = EDGE_CURVE('',#22734,#22736,#5359,.T.) ;
#29028 = EDGE_CURVE('',#22736,#22735,#526,.T.) ;
#29029 = EDGE_CURVE('',#22718,#22735,#5360,.T.) ;
#29030 = EDGE_CURVE('',#22736,#22715,#5361,.T.) ;
#29031 = EDGE_CURVE('',#22737,#22730,#5362,.T.) ;
#29032 = EDGE_CURVE('',#22738,#22737,#5363,.T.) ;
#29033 = EDGE_CURVE('',#22738,#22727,#5364,.T.) ;
#29034 = EDGE_CURVE('',#22739,#22732,#5365,.T.) ;
#29035 = EDGE_CURVE('',#22737,#22739,#19007,.T.) ;
#29036 = EDGE_CURVE('',#22740,#22733,#5366,.T.) ;
#29037 = EDGE_CURVE('',#22739,#22740,#5367,.T.) ;
#29038 = EDGE_CURVE('',#22741,#22735,#5368,.T.) ;
#29039 = EDGE_CURVE('',#22740,#22741,#5369,.T.) ;
#29040 = EDGE_CURVE('',#22742,#22718,#5370,.T.) ;
#29041 = EDGE_CURVE('',#22741,#22742,#5371,.T.) ;
#29042 = EDGE_CURVE('',#22743,#22717,#5372,.T.) ;
#29043 = EDGE_CURVE('',#22742,#22743,#5373,.T.) ;
#29044 = EDGE_CURVE('',#22744,#22745,#5374,.T.) ;
#29045 = EDGE_CURVE('',#22745,#22746,#527,.T.) ;
#29046 = EDGE_CURVE('',#22746,#22747,#5375,.T.) ;
#29047 = EDGE_CURVE('',#22744,#22747,#528,.T.) ;
#29048 = EDGE_CURVE('',#22745,#22748,#5376,.T.) ;
#29049 = EDGE_CURVE('',#22748,#22749,#19008,.T.) ;
#29050 = EDGE_CURVE('',#22749,#22746,#5377,.T.) ;
#29051 = EDGE_CURVE('',#22750,#22751,#19009,.T.) ;
#29052 = EDGE_CURVE('',#22751,#22749,#19010,.T.) ;
#29053 = EDGE_CURVE('',#22748,#22750,#19011,.T.) ;
#29054 = EDGE_CURVE('',#22752,#22751,#5378,.T.) ;
#29055 = EDGE_CURVE('',#22750,#22753,#5379,.T.) ;
#29056 = EDGE_CURVE('',#22753,#22752,#529,.T.) ;
#29057 = EDGE_CURVE('',#22753,#22754,#5380,.T.) ;
#29058 = EDGE_CURVE('',#22754,#22755,#530,.T.) ;
#29059 = EDGE_CURVE('',#22755,#22752,#5381,.T.) ;
#29060 = EDGE_CURVE('',#22754,#22756,#5382,.T.) ;
#29061 = EDGE_CURVE('',#22756,#22757,#19012,.T.) ;
#29062 = EDGE_CURVE('',#22757,#22755,#5383,.T.) ;
#29063 = EDGE_CURVE('',#22758,#22759,#19013,.T.) ;
#29064 = EDGE_CURVE('',#22759,#22757,#19014,.T.) ;
#29065 = EDGE_CURVE('',#22756,#22758,#19015,.T.) ;
#29066 = EDGE_CURVE('',#22760,#22759,#5384,.T.) ;
#29067 = EDGE_CURVE('',#22758,#22761,#5385,.T.) ;
#29068 = EDGE_CURVE('',#22761,#22760,#531,.T.) ;
#29069 = EDGE_CURVE('',#22762,#22760,#5386,.T.) ;
#29070 = EDGE_CURVE('',#22761,#22763,#5387,.T.) ;
#29071 = EDGE_CURVE('',#22763,#22762,#532,.T.) ;
#29072 = EDGE_CURVE('',#22764,#22762,#5388,.T.) ;
#29073 = EDGE_CURVE('',#22763,#22765,#5389,.T.) ;
#29074 = EDGE_CURVE('',#22765,#22764,#533,.T.) ;
#29075 = EDGE_CURVE('',#22747,#22764,#5390,.T.) ;
#29076 = EDGE_CURVE('',#22765,#22744,#5391,.T.) ;
#29077 = EDGE_CURVE('',#22766,#22759,#5392,.T.) ;
#29078 = EDGE_CURVE('',#22767,#22766,#19016,.T.) ;
#29079 = EDGE_CURVE('',#22767,#22757,#5393,.T.) ;
#29080 = EDGE_CURVE('',#22768,#22760,#5394,.T.) ;
#29081 = EDGE_CURVE('',#22766,#22768,#5395,.T.) ;
#29082 = EDGE_CURVE('',#22769,#22762,#5396,.T.) ;
#29083 = EDGE_CURVE('',#22768,#22769,#5397,.T.) ;
#29084 = EDGE_CURVE('',#22770,#22764,#5398,.T.) ;
#29085 = EDGE_CURVE('',#22769,#22770,#5399,.T.) ;
#29086 = EDGE_CURVE('',#22771,#22747,#5400,.T.) ;
#29087 = EDGE_CURVE('',#22770,#22771,#5401,.T.) ;
#29088 = EDGE_CURVE('',#22772,#22746,#5402,.T.) ;
#29089 = EDGE_CURVE('',#22771,#22772,#5403,.T.) ;
#29090 = EDGE_CURVE('',#22479,#22635,#1303,.T.) ;
#29091 = EDGE_CURVE('',#22635,#22773,#1304,.T.) ;
#29092 = EDGE_CURVE('',#22478,#22773,#1305,.T.) ;
#29093 = EDGE_CURVE('',#22773,#22774,#5404,.T.) ;
#29094 = EDGE_CURVE('',#22774,#22480,#1306,.T.) ;
#29095 = EDGE_CURVE('',#22484,#22634,#534,.T.) ;
#29096 = EDGE_CURVE('',#22483,#22633,#535,.T.) ;
#29097 = EDGE_CURVE('',#22482,#22631,#536,.T.) ;
#29098 = EDGE_CURVE('',#22481,#22632,#1307,.T.) ;
#29099 = EDGE_CURVE('',#22774,#22632,#1308,.T.) ;
#29100 = EDGE_CURVE('',#22774,#22624,#5405,.T.) ;
#29101 = EDGE_CURVE('',#22773,#22622,#5406,.T.) ;
#29102 = EDGE_CURVE('',#22488,#22650,#1309,.T.) ;
#29103 = EDGE_CURVE('',#22489,#22652,#1310,.T.) ;
#29104 = EDGE_CURVE('',#22487,#22651,#537,.T.) ;
#29105 = EDGE_CURVE('',#22486,#22775,#538,.T.) ;
#29106 = EDGE_CURVE('',#22775,#22776,#5407,.T.) ;
#29107 = EDGE_CURVE('',#22776,#22485,#539,.T.) ;
#29108 = EDGE_CURVE('',#22654,#22775,#5408,.T.) ;
#29109 = EDGE_CURVE('',#22491,#22654,#1311,.T.) ;
#29110 = EDGE_CURVE('',#22776,#22651,#5409,.T.) ;
#29111 = EDGE_CURVE('',#22490,#22653,#1312,.T.) ;
#29112 = EDGE_CURVE('',#22776,#22643,#5410,.T.) ;
#29113 = EDGE_CURVE('',#22775,#22641,#5411,.T.) ;
#29114 = EDGE_CURVE('',#22777,#22778,#5412,.T.) ;
#29115 = EDGE_CURVE('',#22778,#22673,#540,.T.) ;
#29116 = EDGE_CURVE('',#22673,#22779,#5413,.T.) ;
#29117 = EDGE_CURVE('',#22777,#22779,#541,.T.) ;
#29118 = EDGE_CURVE('',#22779,#22780,#5414,.T.) ;
#29119 = EDGE_CURVE('',#22780,#22781,#542,.T.) ;
#29120 = EDGE_CURVE('',#22781,#22777,#5415,.T.) ;
#29121 = EDGE_CURVE('',#22778,#22782,#5416,.T.) ;
#29122 = EDGE_CURVE('',#22782,#22672,#543,.T.) ;
#29123 = EDGE_CURVE('',#22782,#22783,#5417,.T.) ;
#29124 = EDGE_CURVE('',#22783,#22671,#544,.T.) ;
#29125 = EDGE_CURVE('',#22783,#22784,#5418,.T.) ;
#29126 = EDGE_CURVE('',#22784,#22669,#545,.T.) ;
#29127 = EDGE_CURVE('',#22784,#22785,#5419,.T.) ;
#29128 = EDGE_CURVE('',#22785,#22670,#546,.T.) ;
#29129 = EDGE_CURVE('',#22780,#22670,#5420,.T.) ;
#29130 = EDGE_CURVE('',#22785,#22781,#5421,.T.) ;
#29131 = EDGE_CURVE('',#22780,#22662,#5422,.T.) ;
#29132 = EDGE_CURVE('',#22779,#22660,#5423,.T.) ;
#29133 = EDGE_CURVE('',#22786,#22787,#5424,.T.) ;
#29134 = EDGE_CURVE('',#22788,#22786,#19017,.T.) ;
#29135 = EDGE_CURVE('',#22789,#22788,#5425,.T.) ;
#29136 = EDGE_CURVE('',#22543,#22789,#19018,.T.) ;
#29137 = EDGE_CURVE('',#22790,#22542,#19019,.T.) ;
#29138 = EDGE_CURVE('',#22791,#22790,#5426,.T.) ;
#29139 = EDGE_CURVE('',#22792,#22791,#19020,.T.) ;
#29140 = EDGE_CURVE('',#21728,#22792,#5427,.T.) ;
#29141 = EDGE_CURVE('',#22793,#21727,#1313,.T.) ;
#29142 = EDGE_CURVE('',#22794,#22793,#5428,.T.) ;
#29143 = EDGE_CURVE('',#22787,#22794,#19021,.T.) ;
#29144 = EDGE_CURVE('',#22795,#22796,#5429,.T.) ;
#29145 = EDGE_CURVE('',#22797,#22795,#5430,.T.) ;
#29146 = EDGE_CURVE('',#22798,#22797,#5431,.T.) ;
#29147 = EDGE_CURVE('',#22796,#22798,#5432,.T.) ;
#29148 = EDGE_CURVE('',#22799,#22800,#5433,.T.) ;
#29149 = EDGE_CURVE('',#22801,#22799,#5434,.T.) ;
#29150 = EDGE_CURVE('',#22802,#22801,#5435,.T.) ;
#29151 = EDGE_CURVE('',#22803,#22802,#5436,.T.) ;
#29152 = EDGE_CURVE('',#22804,#22803,#5437,.T.) ;
#29153 = EDGE_CURVE('',#22805,#22804,#5438,.T.) ;
#29154 = EDGE_CURVE('',#22800,#22805,#5439,.T.) ;
#29155 = EDGE_CURVE('',#22796,#22682,#547,.T.) ;
#29156 = EDGE_CURVE('',#22684,#22795,#548,.T.) ;
#29157 = EDGE_CURVE('',#22798,#22683,#549,.T.) ;
#29158 = EDGE_CURVE('',#22806,#22683,#5440,.T.) ;
#29159 = EDGE_CURVE('',#22797,#22806,#550,.T.) ;
#29160 = EDGE_CURVE('',#22684,#22806,#5441,.T.) ;
#29161 = EDGE_CURVE('',#22806,#22678,#5442,.T.) ;
#29162 = EDGE_CURVE('',#22800,#22807,#551,.T.) ;
#29163 = EDGE_CURVE('',#22807,#22808,#5443,.T.) ;
#29164 = EDGE_CURVE('',#22808,#22799,#552,.T.) ;
#29165 = EDGE_CURVE('',#22805,#22703,#553,.T.) ;
#29166 = EDGE_CURVE('',#22703,#22807,#5444,.T.) ;
#29167 = EDGE_CURVE('',#22804,#22702,#554,.T.) ;
#29168 = EDGE_CURVE('',#22803,#22701,#555,.T.) ;
#29169 = EDGE_CURVE('',#22802,#22699,#556,.T.) ;
#29170 = EDGE_CURVE('',#22801,#22700,#557,.T.) ;
#29171 = EDGE_CURVE('',#22808,#22700,#5445,.T.) ;
#29172 = EDGE_CURVE('',#22808,#22692,#5446,.T.) ;
#29173 = EDGE_CURVE('',#22807,#22690,#5447,.T.) ;
#29174 = EDGE_CURVE('',#22581,#22713,#558,.T.) ;
#29175 = EDGE_CURVE('',#22580,#22712,#559,.T.) ;
#29176 = EDGE_CURVE('',#22583,#22809,#560,.T.) ;
#29177 = EDGE_CURVE('',#22809,#22713,#5448,.T.) ;
#29178 = EDGE_CURVE('',#22714,#22582,#561,.T.) ;
#29179 = EDGE_CURVE('',#22714,#22809,#5449,.T.) ;
#29180 = EDGE_CURVE('',#22810,#22811,#5450,.T.) ;
#29181 = EDGE_CURVE('',#22811,#22578,#19022,.T.) ;
#29182 = EDGE_CURVE('',#22577,#22810,#562,.T.) ;
#29183 = EDGE_CURVE('',#22576,#22743,#563,.T.) ;
#29184 = EDGE_CURVE('',#22743,#22810,#5451,.T.) ;
#29185 = EDGE_CURVE('',#22575,#22742,#564,.T.) ;
#29186 = EDGE_CURVE('',#22574,#22741,#565,.T.) ;
#29187 = EDGE_CURVE('',#22573,#22740,#566,.T.) ;
#29188 = EDGE_CURVE('',#22737,#22571,#19023,.T.) ;
#29189 = EDGE_CURVE('',#22570,#22738,#19024,.F.) ;
#29190 = EDGE_CURVE('',#22739,#22572,#19025,.T.) ;
#29191 = EDGE_CURVE('',#22812,#22579,#19026,.T.) ;
#29192 = EDGE_CURVE('',#22811,#22812,#19027,.T.) ;
#29193 = EDGE_CURVE('',#22813,#22569,#19028,.F.) ;
#29194 = EDGE_CURVE('',#22812,#22813,#5452,.T.) ;
#29195 = EDGE_CURVE('',#22813,#22725,#5453,.T.) ;
#29196 = EDGE_CURVE('',#22812,#22724,#5454,.T.) ;
#29197 = EDGE_CURVE('',#22811,#22722,#5455,.T.) ;
#29198 = EDGE_CURVE('',#22810,#22720,#5456,.T.) ;
#29199 = EDGE_CURVE('',#22561,#22814,#567,.T.) ;
#29200 = EDGE_CURVE('',#22814,#22815,#5457,.T.) ;
#29201 = EDGE_CURVE('',#22815,#22562,#568,.T.) ;
#29202 = EDGE_CURVE('',#22772,#22816,#5458,.T.) ;
#29203 = EDGE_CURVE('',#22816,#22558,#19029,.T.) ;
#29204 = EDGE_CURVE('',#22559,#22772,#569,.T.) ;
#29205 = EDGE_CURVE('',#22568,#22771,#570,.T.) ;
#29206 = EDGE_CURVE('',#22567,#22770,#571,.T.) ;
#29207 = EDGE_CURVE('',#22566,#22769,#572,.T.) ;
#29208 = EDGE_CURVE('',#22565,#22768,#573,.T.) ;
#29209 = EDGE_CURVE('',#22817,#22560,#19030,.T.) ;
#29210 = EDGE_CURVE('',#22816,#22817,#19031,.T.) ;
#29211 = EDGE_CURVE('',#22817,#22814,#5459,.T.) ;
#29212 = EDGE_CURVE('',#22815,#22767,#5460,.T.) ;
#29213 = EDGE_CURVE('',#22767,#22563,#19032,.T.) ;
#29214 = EDGE_CURVE('',#22766,#22564,#19033,.T.) ;
#29215 = EDGE_CURVE('',#22815,#22755,#5461,.T.) ;
#29216 = EDGE_CURVE('',#22814,#22752,#5462,.T.) ;
#29217 = EDGE_CURVE('',#22817,#22751,#5463,.T.) ;
#29218 = EDGE_CURVE('',#22816,#22749,#5464,.T.) ;
#29219 = EDGE_CURVE('',#22809,#22708,#5465,.T.) ;
#29220 = EDGE_CURVE('',#22270,#22818,#5466,.F.) ;
#29221 = EDGE_CURVE('',#22818,#22088,#5467,.T.) ;
#29222 = EDGE_CURVE('',#22819,#22440,#5468,.T.) ;
#29223 = EDGE_CURVE('',#22820,#22819,#19034,.T.) ;
#29224 = EDGE_CURVE('',#22821,#22820,#5469,.T.) ;
#29225 = EDGE_CURVE('',#22822,#22821,#19035,.T.) ;
#29226 = EDGE_CURVE('',#22823,#22822,#5470,.T.) ;
#29227 = EDGE_CURVE('',#22435,#22823,#5471,.T.) ;
#29228 = EDGE_CURVE('',#22501,#22139,#5472,.T.) ;
#29229 = EDGE_CURVE('',#22824,#22150,#5473,.T.) ;
#29230 = EDGE_CURVE('',#22606,#22824,#19036,.T.) ;
#29231 = EDGE_CURVE('',#22825,#22149,#5474,.T.) ;
#29232 = EDGE_CURVE('',#22825,#22824,#5475,.T.) ;
#29233 = EDGE_CURVE('',#22826,#22148,#5476,.T.) ;
#29234 = EDGE_CURVE('',#22826,#22825,#19037,.T.) ;
#29235 = EDGE_CURVE('',#22827,#22147,#5477,.T.) ;
#29236 = EDGE_CURVE('',#22827,#22826,#5478,.T.) ;
#29237 = EDGE_CURVE('',#22828,#22146,#5479,.T.) ;
#29238 = EDGE_CURVE('',#22828,#22827,#5480,.T.) ;
#29239 = EDGE_CURVE('',#22829,#22145,#5481,.T.) ;
#29240 = EDGE_CURVE('',#22828,#22829,#5482,.T.) ;
#29241 = EDGE_CURVE('',#22830,#22829,#5483,.T.) ;
#29242 = EDGE_CURVE('',#21959,#22830,#19038,.T.) ;
#29243 = EDGE_CURVE('',#22830,#22831,#5484,.T.) ;
#29244 = EDGE_CURVE('',#21960,#22831,#19039,.T.) ;
#29245 = EDGE_CURVE('',#22145,#22832,#5485,.T.) ;
#29246 = EDGE_CURVE('',#22831,#22832,#5486,.T.) ;
#29247 = EDGE_CURVE('',#22500,#22140,#5487,.T.) ;
#29248 = EDGE_CURVE('',#22467,#22833,#5488,.T.) ;
#29249 = EDGE_CURVE('',#22834,#22833,#5489,.T.) ;
#29250 = EDGE_CURVE('',#22142,#22834,#5490,.T.) ;
#29251 = EDGE_CURVE('',#22594,#22835,#5491,.T.) ;
#29252 = EDGE_CURVE('',#22554,#22835,#5492,.T.) ;
#29253 = EDGE_CURVE('',#22835,#22836,#5493,.T.) ;
#29254 = EDGE_CURVE('',#22555,#22836,#5494,.T.) ;
#29255 = EDGE_CURVE('',#22836,#22593,#5495,.T.) ;
#29256 = EDGE_CURVE('',#22431,#21961,#5496,.T.) ;
#29257 = EDGE_CURVE('',#22431,#22837,#5497,.T.) ;
#29258 = EDGE_CURVE('',#22838,#22837,#5498,.T.) ;
#29259 = EDGE_CURVE('',#21961,#22838,#5499,.T.) ;
#29260 = EDGE_CURVE('',#22457,#22839,#5500,.T.) ;
#29261 = EDGE_CURVE('',#22840,#22839,#19040,.T.) ;
#29262 = EDGE_CURVE('',#22458,#22840,#5501,.T.) ;
#29263 = EDGE_CURVE('',#22837,#22840,#5502,.T.) ;
#29264 = EDGE_CURVE('',#22839,#22838,#5503,.T.) ;
#29265 = EDGE_CURVE('',#22590,#22841,#5504,.T.) ;
#29266 = EDGE_CURVE('',#22522,#22841,#19041,.T.) ;
#29267 = EDGE_CURVE('',#21934,#21849,#5505,.T.) ;
#29268 = EDGE_CURVE('',#22841,#21936,#5506,.T.) ;
#29269 = EDGE_CURVE('',#22591,#21935,#5507,.F.) ;
#29270 = EDGE_CURVE('',#22519,#22516,#5508,.T.) ;
#29271 = EDGE_CURVE('',#22355,#22842,#5509,.T.) ;
#29272 = EDGE_CURVE('',#22842,#22382,#19042,.F.) ;
#29273 = EDGE_CURVE('',#22353,#22842,#5510,.T.) ;
#29274 = EDGE_CURVE('',#22384,#22369,#5511,.T.) ;
#29275 = EDGE_CURVE('',#22612,#22076,#5512,.T.) ;
#29276 = EDGE_CURVE('',#22822,#22843,#1314,.T.) ;
#29277 = EDGE_CURVE('',#22843,#22844,#5513,.T.) ;
#29278 = EDGE_CURVE('',#22844,#22823,#574,.T.) ;
#29279 = EDGE_CURVE('',#22794,#22845,#19043,.F.) ;
#29280 = EDGE_CURVE('',#22846,#22794,#19044,.F.) ;
#29281 = EDGE_CURVE('',#22845,#22846,#19045,.F.) ;
#29282 = EDGE_CURVE('',#22821,#22847,#1315,.T.) ;
#29283 = EDGE_CURVE('',#22847,#22843,#19046,.T.) ;
#29284 = EDGE_CURVE('',#22793,#21717,#19047,.T.) ;
#29285 = EDGE_CURVE('',#21719,#22846,#5514,.T.) ;
#29286 = EDGE_CURVE('',#22848,#22849,#1316,.T.) ;
#29287 = EDGE_CURVE('',#22819,#22849,#19048,.T.) ;
#29288 = EDGE_CURVE('',#22584,#22819,#1317,.F.) ;
#29289 = EDGE_CURVE('',#22848,#22584,#19049,.T.) ;
#29290 = EDGE_CURVE('',#22850,#22820,#19050,.T.) ;
#29291 = EDGE_CURVE('',#22849,#22850,#19051,.T.) ;
#29292 = EDGE_CURVE('',#22850,#22847,#5515,.T.) ;
#29293 = EDGE_CURVE('',#22473,#22851,#19052,.F.) ;
#29294 = EDGE_CURVE('',#22851,#22492,#19053,.F.) ;
#29295 = EDGE_CURVE('',#22494,#22852,#19054,.T.) ;
#29296 = EDGE_CURVE('',#22852,#22851,#575,.T.) ;
#29297 = EDGE_CURVE('',#22496,#22852,#5516,.T.) ;
#29298 = EDGE_CURVE('',#22853,#22854,#19055,.T.) ;
#29299 = EDGE_CURVE('',#22854,#22792,#19056,.T.) ;
#29300 = EDGE_CURVE('',#22791,#22853,#1318,.T.) ;
#29301 = EDGE_CURVE('',#22855,#22543,#19057,.T.) ;
#29302 = EDGE_CURVE('',#22855,#22856,#1319,.T.) ;
#29303 = EDGE_CURVE('',#22544,#22856,#19058,.T.) ;
#29304 = EDGE_CURVE('',#22857,#22858,#5517,.T.) ;
#29305 = EDGE_CURVE('',#22858,#22789,#19059,.T.) ;
#29306 = EDGE_CURVE('',#22788,#22857,#1320,.T.) ;
#29307 = EDGE_CURVE('',#22858,#22855,#19060,.T.) ;
#29308 = EDGE_CURVE('',#22856,#22848,#576,.T.) ;
#29309 = EDGE_CURVE('',#22859,#22860,#1321,.T.) ;
#29310 = EDGE_CURVE('',#22542,#22860,#19061,.T.) ;
#29311 = EDGE_CURVE('',#22859,#21865,#19062,.T.) ;
#29312 = EDGE_CURVE('',#22861,#22790,#19063,.T.) ;
#29313 = EDGE_CURVE('',#22860,#22861,#19064,.T.) ;
#29314 = EDGE_CURVE('',#22861,#22853,#5518,.T.) ;
#29315 = EDGE_CURVE('',#22862,#22377,#19065,.T.) ;
#29316 = EDGE_CURVE('',#22862,#22863,#1322,.T.) ;
#29317 = EDGE_CURVE('',#21864,#22863,#19066,.T.) ;
#29318 = EDGE_CURVE('',#22864,#22865,#5519,.T.) ;
#29319 = EDGE_CURVE('',#22865,#22477,#19067,.T.) ;
#29320 = EDGE_CURVE('',#22476,#22864,#1323,.T.) ;
#29321 = EDGE_CURVE('',#22865,#22862,#19068,.T.) ;
#29322 = EDGE_CURVE('',#22863,#22859,#577,.T.) ;
#29323 = EDGE_CURVE('',#22474,#22866,#19069,.T.) ;
#29324 = EDGE_CURVE('',#22866,#22867,#5520,.T.) ;
#29325 = EDGE_CURVE('',#22867,#22475,#19070,.T.) ;
#29326 = EDGE_CURVE('',#22867,#22864,#19071,.T.) ;
#29327 = EDGE_CURVE('',#22851,#22866,#19072,.T.) ;
#29328 = EDGE_CURVE('',#22854,#21726,#5521,.T.) ;
#29329 = EDGE_CURVE('',#22787,#22868,#19073,.T.) ;
#29330 = EDGE_CURVE('',#22868,#22869,#5522,.T.) ;
#29331 = EDGE_CURVE('',#22869,#22786,#19074,.T.) ;
#29332 = EDGE_CURVE('',#22869,#22857,#19075,.T.) ;
#29333 = EDGE_CURVE('',#22870,#22871,#578,.T.) ;
#29334 = EDGE_CURVE('',#22871,#22872,#5523,.T.) ;
#29335 = EDGE_CURVE('',#22872,#22873,#19076,.T.) ;
#29336 = EDGE_CURVE('',#22873,#22870,#5524,.T.) ;
#29337 = EDGE_CURVE('',#21724,#22873,#579,.T.) ;
#29338 = EDGE_CURVE('',#22872,#21721,#580,.T.) ;
#29339 = EDGE_CURVE('',#22845,#22868,#19077,.T.) ;
#29340 = EDGE_CURVE('',#22874,#22875,#19078,.T.) ;
#29341 = EDGE_CURVE('',#22875,#22845,#581,.T.) ;
#29342 = EDGE_CURVE('',#22846,#22874,#582,.T.) ;
#29343 = EDGE_CURVE('',#22876,#22877,#583,.T.) ;
#29344 = EDGE_CURVE('',#22877,#22875,#5525,.T.) ;
#29345 = EDGE_CURVE('',#22874,#22876,#5526,.T.) ;
#29346 = EDGE_CURVE('',#22436,#22878,#5527,.T.) ;
#29347 = EDGE_CURVE('',#22878,#22879,#19079,.T.) ;
#29348 = EDGE_CURVE('',#22879,#21922,#5528,.T.) ;
#29349 = EDGE_CURVE('',#22880,#22881,#19080,.T.) ;
#29350 = EDGE_CURVE('',#22881,#22879,#584,.T.) ;
#29351 = EDGE_CURVE('',#22878,#22880,#585,.T.) ;
#29352 = EDGE_CURVE('',#22844,#22881,#5529,.T.) ;
#29353 = EDGE_CURVE('',#22880,#22823,#5530,.T.) ;
#29354 = EDGE_CURVE('',#22133,#22864,#5531,.T.) ;
#29355 = EDGE_CURVE('',#22132,#22865,#5532,.T.) ;
#29356 = EDGE_CURVE('',#22134,#22867,#5533,.T.) ;
#29357 = EDGE_CURVE('',#22135,#22866,#5534,.T.) ;
#29358 = EDGE_CURVE('',#22852,#22136,#5535,.T.) ;
#29359 = EDGE_CURVE('',#22833,#22432,#19081,.T.) ;
#29360 = EDGE_CURVE('',#22853,#22130,#5536,.T.) ;
#29361 = EDGE_CURVE('',#22129,#22854,#5537,.T.) ;
#29362 = EDGE_CURVE('',#22122,#22869,#5538,.T.) ;
#29363 = EDGE_CURVE('',#22121,#22857,#5539,.T.) ;
#29364 = EDGE_CURVE('',#22882,#22176,#5540,.T.) ;
#29365 = EDGE_CURVE('',#22175,#22883,#5541,.T.) ;
#29366 = EDGE_CURVE('',#22883,#22882,#5542,.T.) ;
#29367 = EDGE_CURVE('',#22884,#22883,#19082,.T.) ;
#29368 = EDGE_CURVE('',#22174,#22884,#5543,.T.) ;
#29369 = EDGE_CURVE('',#22885,#22884,#5544,.T.) ;
#29370 = EDGE_CURVE('',#22173,#22885,#5545,.T.) ;
#29371 = EDGE_CURVE('',#22886,#22885,#5546,.T.) ;
#29372 = EDGE_CURVE('',#22172,#22886,#5547,.T.) ;
#29373 = EDGE_CURVE('',#22887,#22886,#19083,.T.) ;
#29374 = EDGE_CURVE('',#22171,#22887,#5548,.T.) ;
#29375 = EDGE_CURVE('',#22888,#22887,#5549,.T.) ;
#29376 = EDGE_CURVE('',#22170,#22888,#5550,.T.) ;
#29377 = EDGE_CURVE('',#22889,#22888,#19084,.T.) ;
#29378 = EDGE_CURVE('',#22169,#22889,#5551,.T.) ;
#29379 = EDGE_CURVE('',#22890,#22889,#5552,.T.) ;
#29380 = EDGE_CURVE('',#22168,#22890,#5553,.T.) ;
#29381 = EDGE_CURVE('',#22891,#22890,#5554,.T.) ;
#29382 = EDGE_CURVE('',#22167,#22891,#5555,.T.) ;
#29383 = EDGE_CURVE('',#22144,#22892,#5556,.T.) ;
#29384 = EDGE_CURVE('',#22832,#22892,#1324,.T.) ;
#29385 = EDGE_CURVE('',#22143,#22893,#5557,.T.) ;
#29386 = EDGE_CURVE('',#22892,#22893,#5558,.T.) ;
#29387 = EDGE_CURVE('',#22893,#22834,#1325,.T.) ;
#29388 = EDGE_CURVE('',#22206,#22361,#5559,.T.) ;
#29389 = EDGE_CURVE('',#22205,#22363,#5560,.T.) ;
#29390 = EDGE_CURVE('',#22894,#22894,#19085,.T.) ;
#29391 = EDGE_CURVE('',#22208,#22895,#5561,.T.) ;
#29392 = EDGE_CURVE('',#22895,#22895,#19086,.T.) ;
#29393 = EDGE_CURVE('',#22896,#22119,#5562,.T.) ;
#29394 = EDGE_CURVE('',#22118,#22897,#5563,.T.) ;
#29395 = EDGE_CURVE('',#22897,#22896,#5564,.T.) ;
#29396 = EDGE_CURVE('',#22898,#22897,#19087,.T.) ;
#29397 = EDGE_CURVE('',#22117,#22898,#5565,.T.) ;
#29398 = EDGE_CURVE('',#22899,#22898,#5566,.T.) ;
#29399 = EDGE_CURVE('',#22116,#22899,#5567,.T.) ;
#29400 = EDGE_CURVE('',#22900,#22899,#19088,.T.) ;
#29401 = EDGE_CURVE('',#22115,#22900,#5568,.T.) ;
#29402 = EDGE_CURVE('',#22901,#22900,#5569,.T.) ;
#29403 = EDGE_CURVE('',#22114,#22901,#5570,.T.) ;
#29404 = EDGE_CURVE('',#22902,#22903,#19089,.T.) ;
#29405 = EDGE_CURVE('',#22217,#22903,#5571,.T.) ;
#29406 = EDGE_CURVE('',#22216,#22902,#5572,.T.) ;
#29407 = EDGE_CURVE('',#22904,#22902,#5573,.T.) ;
#29408 = EDGE_CURVE('',#22215,#22904,#5574,.T.) ;
#29409 = EDGE_CURVE('',#22905,#22904,#19090,.T.) ;
#29410 = EDGE_CURVE('',#22214,#22905,#5575,.T.) ;
#29411 = EDGE_CURVE('',#22906,#22905,#5576,.T.) ;
#29412 = EDGE_CURVE('',#22213,#22906,#5577,.T.) ;
#29413 = EDGE_CURVE('',#22907,#22906,#5578,.T.) ;
#29414 = EDGE_CURVE('',#22212,#22907,#5579,.T.) ;
#29415 = EDGE_CURVE('',#22908,#22907,#19091,.T.) ;
#29416 = EDGE_CURVE('',#22211,#22908,#5580,.T.) ;
#29417 = EDGE_CURVE('',#22909,#22908,#5581,.T.) ;
#29418 = EDGE_CURVE('',#22209,#22909,#5582,.T.) ;
#29419 = EDGE_CURVE('',#22223,#22910,#5583,.T.) ;
#29420 = EDGE_CURVE('',#22910,#22910,#19092,.T.) ;
#29421 = EDGE_CURVE('',#22911,#22912,#5584,.T.) ;
#29422 = EDGE_CURVE('',#22231,#22912,#5585,.T.) ;
#29423 = EDGE_CURVE('',#22230,#22911,#5586,.T.) ;
#29424 = EDGE_CURVE('',#22913,#22911,#19093,.T.) ;
#29425 = EDGE_CURVE('',#22229,#22913,#5587,.T.) ;
#29426 = EDGE_CURVE('',#22914,#22913,#5588,.T.) ;
#29427 = EDGE_CURVE('',#22228,#22914,#5589,.T.) ;
#29428 = EDGE_CURVE('',#22915,#22914,#19094,.T.) ;
#29429 = EDGE_CURVE('',#22227,#22915,#5590,.T.) ;
#29430 = EDGE_CURVE('',#22916,#22915,#5591,.T.) ;
#29431 = EDGE_CURVE('',#22226,#22916,#5592,.T.) ;
#29432 = EDGE_CURVE('',#22917,#22916,#1326,.T.) ;
#29433 = EDGE_CURVE('',#22224,#22917,#5593,.T.) ;
#29434 = EDGE_CURVE('',#22918,#22919,#19095,.T.) ;
#29435 = EDGE_CURVE('',#22242,#22919,#5594,.T.) ;
#29436 = EDGE_CURVE('',#22241,#22918,#5595,.T.) ;
#29437 = EDGE_CURVE('',#22920,#22918,#5596,.T.) ;
#29438 = EDGE_CURVE('',#22240,#22920,#5597,.T.) ;
#29439 = EDGE_CURVE('',#22921,#22920,#19096,.T.) ;
#29440 = EDGE_CURVE('',#22239,#22921,#5598,.T.) ;
#29441 = EDGE_CURVE('',#22922,#22921,#5599,.T.) ;
#29442 = EDGE_CURVE('',#22238,#22922,#5600,.T.) ;
#29443 = EDGE_CURVE('',#21805,#22922,#5601,.T.) ;
#29444 = EDGE_CURVE('',#22923,#21810,#5602,.T.) ;
#29445 = EDGE_CURVE('',#22236,#22923,#5603,.T.) ;
#29446 = EDGE_CURVE('',#22924,#22925,#19097,.T.) ;
#29447 = EDGE_CURVE('',#22181,#22925,#5604,.T.) ;
#29448 = EDGE_CURVE('',#22180,#22924,#5605,.T.) ;
#29449 = EDGE_CURVE('',#22926,#22924,#5606,.T.) ;
#29450 = EDGE_CURVE('',#21996,#22179,#5607,.T.) ;
#29451 = EDGE_CURVE('',#21995,#22926,#5608,.T.) ;
#29452 = EDGE_CURVE('',#22927,#22926,#19098,.T.) ;
#29453 = EDGE_CURVE('',#21994,#22927,#5609,.T.) ;
#29454 = EDGE_CURVE('',#22928,#22927,#5610,.T.) ;
#29455 = EDGE_CURVE('',#21993,#22928,#5611,.T.) ;
#29456 = EDGE_CURVE('',#22273,#22928,#19099,.T.) ;
#29457 = EDGE_CURVE('',#22929,#22930,#19100,.T.) ;
#29458 = EDGE_CURVE('',#22256,#22930,#5612,.T.) ;
#29459 = EDGE_CURVE('',#22255,#22929,#5613,.T.) ;
#29460 = EDGE_CURVE('',#22931,#22929,#5614,.T.) ;
#29461 = EDGE_CURVE('',#22254,#22931,#5615,.T.) ;
#29462 = EDGE_CURVE('',#22932,#22931,#19101,.T.) ;
#29463 = EDGE_CURVE('',#22253,#22932,#5616,.T.) ;
#29464 = EDGE_CURVE('',#22933,#22932,#5617,.T.) ;
#29465 = EDGE_CURVE('',#22252,#22933,#5618,.T.) ;
#29466 = EDGE_CURVE('',#22934,#22933,#5619,.T.) ;
#29467 = EDGE_CURVE('',#22251,#22934,#5620,.T.) ;
#29468 = EDGE_CURVE('',#22935,#22934,#19102,.T.) ;
#29469 = EDGE_CURVE('',#22250,#22935,#5621,.T.) ;
#29470 = EDGE_CURVE('',#22936,#22935,#5622,.T.) ;
#29471 = EDGE_CURVE('',#22248,#22936,#5623,.T.) ;
#29472 = EDGE_CURVE('',#22937,#22936,#19103,.T.) ;
#29473 = EDGE_CURVE('',#22249,#22937,#5624,.T.) ;
#29474 = EDGE_CURVE('',#22938,#22937,#5625,.T.) ;
#29475 = EDGE_CURVE('',#22261,#22938,#5626,.T.) ;
#29476 = EDGE_CURVE('',#22939,#22938,#5627,.T.) ;
#29477 = EDGE_CURVE('',#22260,#22939,#5628,.T.) ;
#29478 = EDGE_CURVE('',#22940,#22939,#19104,.T.) ;
#29479 = EDGE_CURVE('',#22259,#22940,#5629,.T.) ;
#29480 = EDGE_CURVE('',#22941,#22940,#5630,.T.) ;
#29481 = EDGE_CURVE('',#22258,#22941,#5631,.T.) ;
#29482 = EDGE_CURVE('',#22942,#22941,#19105,.T.) ;
#29483 = EDGE_CURVE('',#22257,#22942,#5632,.T.) ;
#29484 = EDGE_CURVE('',#22930,#22942,#5633,.T.) ;
#29485 = EDGE_CURVE('',#22943,#22917,#5634,.T.) ;
#29486 = EDGE_CURVE('',#22225,#22943,#5635,.T.) ;
#29487 = EDGE_CURVE('',#22944,#22943,#1327,.T.) ;
#29488 = EDGE_CURVE('',#22235,#22944,#5636,.T.) ;
#29489 = EDGE_CURVE('',#22945,#22944,#5637,.T.) ;
#29490 = EDGE_CURVE('',#22234,#22945,#5638,.T.) ;
#29491 = EDGE_CURVE('',#22946,#22945,#19106,.T.) ;
#29492 = EDGE_CURVE('',#22233,#22946,#5639,.T.) ;
#29493 = EDGE_CURVE('',#22947,#22946,#5640,.T.) ;
#29494 = EDGE_CURVE('',#22232,#22947,#5641,.T.) ;
#29495 = EDGE_CURVE('',#22912,#22947,#19107,.T.) ;
#29496 = EDGE_CURVE('',#22948,#22923,#1328,.T.) ;
#29497 = EDGE_CURVE('',#22237,#22948,#5642,.T.) ;
#29498 = EDGE_CURVE('',#22949,#22948,#5643,.T.) ;
#29499 = EDGE_CURVE('',#22247,#22949,#5644,.T.) ;
#29500 = EDGE_CURVE('',#22950,#22949,#5645,.T.) ;
#29501 = EDGE_CURVE('',#22246,#22950,#5646,.T.) ;
#29502 = EDGE_CURVE('',#22951,#22950,#19108,.T.) ;
#29503 = EDGE_CURVE('',#22245,#22951,#5647,.T.) ;
#29504 = EDGE_CURVE('',#22952,#22951,#5648,.T.) ;
#29505 = EDGE_CURVE('',#22244,#22952,#5649,.T.) ;
#29506 = EDGE_CURVE('',#22953,#22952,#19109,.T.) ;
#29507 = EDGE_CURVE('',#22243,#22953,#5650,.T.) ;
#29508 = EDGE_CURVE('',#22919,#22953,#5651,.T.) ;
#29509 = EDGE_CURVE('',#22954,#22901,#19110,.T.) ;
#29510 = EDGE_CURVE('',#22113,#22954,#5652,.T.) ;
#29511 = EDGE_CURVE('',#22955,#22954,#5653,.T.) ;
#29512 = EDGE_CURVE('',#22112,#22955,#5654,.T.) ;
#29513 = EDGE_CURVE('',#22956,#22955,#5655,.T.) ;
#29514 = EDGE_CURVE('',#22111,#22956,#5656,.T.) ;
#29515 = EDGE_CURVE('',#22957,#22956,#5657,.T.) ;
#29516 = EDGE_CURVE('',#22110,#22957,#5658,.T.) ;
#29517 = EDGE_CURVE('',#22958,#22957,#5659,.T.) ;
#29518 = EDGE_CURVE('',#22109,#22958,#5660,.T.) ;
#29519 = EDGE_CURVE('',#22959,#22958,#5661,.T.) ;
#29520 = EDGE_CURVE('',#22108,#22959,#5662,.T.) ;
#29521 = EDGE_CURVE('',#22960,#22959,#19111,.T.) ;
#29522 = EDGE_CURVE('',#22107,#22960,#5663,.T.) ;
#29523 = EDGE_CURVE('',#22961,#22896,#19112,.T.) ;
#29524 = EDGE_CURVE('',#22961,#22960,#5664,.T.) ;
#29525 = EDGE_CURVE('',#22962,#22909,#19113,.T.) ;
#29526 = EDGE_CURVE('',#22210,#22962,#5665,.T.) ;
#29527 = EDGE_CURVE('',#22963,#22962,#5666,.T.) ;
#29528 = EDGE_CURVE('',#22222,#22963,#5667,.T.) ;
#29529 = EDGE_CURVE('',#22964,#22963,#5668,.T.) ;
#29530 = EDGE_CURVE('',#22221,#22964,#5669,.T.) ;
#29531 = EDGE_CURVE('',#22965,#22964,#19114,.T.) ;
#29532 = EDGE_CURVE('',#22220,#22965,#5670,.T.) ;
#29533 = EDGE_CURVE('',#22966,#22965,#5671,.T.) ;
#29534 = EDGE_CURVE('',#22219,#22966,#5672,.T.) ;
#29535 = EDGE_CURVE('',#22967,#22966,#19115,.T.) ;
#29536 = EDGE_CURVE('',#22218,#22967,#5673,.T.) ;
#29537 = EDGE_CURVE('',#22903,#22967,#5674,.T.) ;
#29538 = EDGE_CURVE('',#22968,#22272,#19116,.T.) ;
#29539 = EDGE_CURVE('',#22186,#22968,#5675,.T.) ;
#29540 = EDGE_CURVE('',#22969,#22968,#5676,.T.) ;
#29541 = EDGE_CURVE('',#22185,#22969,#5677,.T.) ;
#29542 = EDGE_CURVE('',#22970,#22969,#19117,.T.) ;
#29543 = EDGE_CURVE('',#22184,#22970,#5678,.T.) ;
#29544 = EDGE_CURVE('',#22971,#22970,#5679,.T.) ;
#29545 = EDGE_CURVE('',#22183,#22971,#5680,.T.) ;
#29546 = EDGE_CURVE('',#22972,#22971,#19118,.T.) ;
#29547 = EDGE_CURVE('',#22182,#22972,#5681,.T.) ;
#29548 = EDGE_CURVE('',#22925,#22972,#5682,.T.) ;
#29549 = EDGE_CURVE('',#22973,#22891,#19119,.T.) ;
#29550 = EDGE_CURVE('',#22166,#22973,#5683,.T.) ;
#29551 = EDGE_CURVE('',#22974,#22973,#5684,.T.) ;
#29552 = EDGE_CURVE('',#22165,#22974,#5685,.T.) ;
#29553 = EDGE_CURVE('',#22127,#22873,#5686,.T.) ;
#29554 = EDGE_CURVE('',#22126,#22870,#5687,.T.) ;
#29555 = EDGE_CURVE('',#22877,#22125,#5688,.T.) ;
#29556 = EDGE_CURVE('',#22871,#22876,#5689,.T.) ;
#29557 = EDGE_CURVE('',#22875,#22124,#5690,.T.) ;
#29558 = EDGE_CURVE('',#22103,#22843,#5691,.T.) ;
#29559 = EDGE_CURVE('',#22881,#22102,#5692,.T.) ;
#29560 = EDGE_CURVE('',#22302,#22199,#5693,.T.) ;
#29561 = EDGE_CURVE('',#22289,#22298,#5694,.T.) ;
#29562 = EDGE_CURVE('',#22287,#22299,#5695,.T.) ;
#29563 = EDGE_CURVE('',#22286,#22300,#5696,.T.) ;
#29564 = EDGE_CURVE('',#22303,#22198,#5697,.T.) ;
#29565 = EDGE_CURVE('',#22975,#22882,#19120,.T.) ;
#29566 = EDGE_CURVE('',#22975,#22974,#19121,.T.) ;
#29567 = EDGE_CURVE('',#22164,#22975,#5698,.T.) ;
#29568 = EDGE_CURVE('',#21998,#22177,#5699,.T.) ;
#29569 = EDGE_CURVE('',#21997,#22178,#5700,.T.) ;
#29570 = EDGE_CURVE('',#22159,#22818,#5701,.T.) ;
#29571 = EDGE_CURVE('',#22123,#22868,#5702,.T.) ;
#29572 = EDGE_CURVE('',#22101,#22879,#5703,.T.) ;
#29573 = EDGE_CURVE('',#21723,#22128,#5704,.T.) ;
#29574 = EDGE_CURVE('',#22497,#22894,#5705,.T.) ;
#29575 = EDGE_CURVE('',#22106,#22961,#5706,.T.) ;
#29576 = EDGE_CURVE('',#22847,#22104,#5707,.T.) ;
#29577 = EDGE_CURVE('',#22120,#22858,#5708,.T.) ;
#29578 = EDGE_CURVE('',#22105,#22850,#5709,.T.) ;
#29579 = EDGE_CURVE('',#22131,#22861,#5710,.T.) ;
#29580 = EDGE_CURVE('',#22379,#22349,#5711,.T.) ;
#29581 = EDGE_CURVE('',#22348,#22354,#5712,.T.) ;
#29582 = EDGE_CURVE('',#22976,#22977,#5713,.T.) ;
#29583 = EDGE_CURVE('',#22978,#22977,#5714,.T.) ;
#29584 = EDGE_CURVE('',#22979,#22978,#5715,.T.) ;
#29585 = EDGE_CURVE('',#22976,#22979,#5716,.T.) ;
#29586 = EDGE_CURVE('',#22980,#22976,#5717,.T.) ;
#29587 = EDGE_CURVE('',#22981,#22979,#5718,.T.) ;
#29588 = EDGE_CURVE('',#22980,#22981,#5719,.T.) ;
#29589 = EDGE_CURVE('',#22982,#22980,#5720,.T.) ;
#29590 = EDGE_CURVE('',#22983,#22981,#5721,.T.) ;
#29591 = EDGE_CURVE('',#22982,#22983,#5722,.T.) ;
#29592 = EDGE_CURVE('',#22984,#22982,#5723,.T.) ;
#29593 = EDGE_CURVE('',#22985,#22983,#5724,.T.) ;
#29594 = EDGE_CURVE('',#22984,#22985,#5725,.T.) ;
#29595 = EDGE_CURVE('',#22986,#22984,#5726,.T.) ;
#29596 = EDGE_CURVE('',#22987,#22985,#5727,.T.) ;
#29597 = EDGE_CURVE('',#22986,#22987,#5728,.T.) ;
#29598 = EDGE_CURVE('',#22988,#22986,#5729,.T.) ;
#29599 = EDGE_CURVE('',#22989,#22987,#5730,.T.) ;
#29600 = EDGE_CURVE('',#22988,#22989,#5731,.T.) ;
#29601 = EDGE_CURVE('',#22990,#22988,#5732,.T.) ;
#29602 = EDGE_CURVE('',#22991,#22989,#5733,.T.) ;
#29603 = EDGE_CURVE('',#22990,#22991,#5734,.T.) ;
#29604 = EDGE_CURVE('',#22991,#22978,#5735,.T.) ;
#29605 = EDGE_CURVE('',#22977,#22990,#5736,.T.) ;
#29606 = EDGE_CURVE('',#22992,#22993,#5737,.T.) ;
#29607 = EDGE_CURVE('',#22993,#22994,#5738,.T.) ;
#29608 = EDGE_CURVE('',#22995,#22994,#5739,.T.) ;
#29609 = EDGE_CURVE('',#22992,#22995,#5740,.T.) ;
#29610 = EDGE_CURVE('',#22996,#22990,#5741,.T.) ;
#29611 = EDGE_CURVE('',#22996,#22992,#5742,.T.) ;
#29612 = EDGE_CURVE('',#22997,#22995,#5743,.T.) ;
#29613 = EDGE_CURVE('',#22991,#22997,#5744,.T.) ;
#29614 = EDGE_CURVE('',#22998,#22996,#5745,.T.) ;
#29615 = EDGE_CURVE('',#22999,#22997,#5746,.T.) ;
#29616 = EDGE_CURVE('',#22998,#22999,#5747,.T.) ;
#29617 = EDGE_CURVE('',#22993,#22998,#5748,.T.) ;
#29618 = EDGE_CURVE('',#22994,#22999,#5749,.T.) ;
#29619 = EDGE_CURVE('',#23000,#23001,#5750,.T.) ;
#29620 = EDGE_CURVE('',#23002,#23000,#1329,.F.) ;
#29621 = EDGE_CURVE('',#23003,#23002,#19122,.T.) ;
#29622 = EDGE_CURVE('',#23003,#23001,#1330,.T.) ;
#29623 = EDGE_CURVE('',#23004,#23005,#5751,.T.) ;
#29624 = EDGE_CURVE('',#23000,#23004,#1331,.F.) ;
#29625 = EDGE_CURVE('',#23001,#23005,#1332,.T.) ;
#29626 = EDGE_CURVE('',#23006,#23007,#5752,.T.) ;
#29627 = EDGE_CURVE('',#23008,#23006,#1333,.T.) ;
#29628 = EDGE_CURVE('',#23004,#23008,#1334,.F.) ;
#29629 = EDGE_CURVE('',#23005,#23009,#1335,.T.) ;
#29630 = EDGE_CURVE('',#23009,#23007,#1336,.T.) ;
#29631 = EDGE_CURVE('',#23010,#23011,#5753,.T.) ;
#29632 = EDGE_CURVE('',#23012,#23010,#1337,.T.) ;
#29633 = EDGE_CURVE('',#23006,#23012,#1338,.T.) ;
#29634 = EDGE_CURVE('',#23007,#23013,#1339,.T.) ;
#29635 = EDGE_CURVE('',#23013,#23011,#1340,.F.) ;
#29636 = EDGE_CURVE('',#23014,#23015,#19123,.T.) ;
#29637 = EDGE_CURVE('',#23015,#23016,#1341,.T.) ;
#29638 = EDGE_CURVE('',#23016,#23017,#1342,.T.) ;
#29639 = EDGE_CURVE('',#23017,#23018,#1343,.T.) ;
#29640 = EDGE_CURVE('',#23018,#23019,#1344,.T.) ;
#29641 = EDGE_CURVE('',#23019,#23020,#1345,.T.) ;
#29642 = EDGE_CURVE('',#23021,#23020,#19124,.F.) ;
#29643 = EDGE_CURVE('',#23021,#23022,#1346,.T.) ;
#29644 = EDGE_CURVE('',#23022,#23023,#1347,.T.) ;
#29645 = EDGE_CURVE('',#23023,#23024,#1348,.T.) ;
#29646 = EDGE_CURVE('',#23024,#23025,#1349,.T.) ;
#29647 = EDGE_CURVE('',#23025,#23026,#1350,.T.) ;
#29648 = EDGE_CURVE('',#23026,#23014,#1351,.T.) ;
#29649 = EDGE_CURVE('',#23027,#23027,#19125,.T.) ;
#29650 = EDGE_CURVE('',#23011,#23028,#1352,.F.) ;
#29651 = EDGE_CURVE('',#23029,#23028,#19126,.T.) ;
#29652 = EDGE_CURVE('',#23030,#23029,#1353,.T.) ;
#29653 = EDGE_CURVE('',#23010,#23030,#1354,.T.) ;
#29654 = EDGE_CURVE('',#23014,#23029,#1355,.T.) ;
#29655 = EDGE_CURVE('',#23028,#23031,#1356,.T.) ;
#29656 = EDGE_CURVE('',#23031,#23015,#1357,.T.) ;
#29657 = EDGE_CURVE('',#23032,#23021,#1358,.T.) ;
#29658 = EDGE_CURVE('',#23032,#23002,#1359,.T.) ;
#29659 = EDGE_CURVE('',#23020,#23003,#1360,.T.) ;
#29660 = EDGE_CURVE('',#23033,#23033,#19127,.T.) ;
#29661 = EDGE_CURVE('',#23033,#23034,#19128,.T.) ;
#29662 = EDGE_CURVE('',#23034,#23034,#19129,.T.) ;
#29663 = EDGE_CURVE('',#23035,#23035,#1361,.T.) ;
#29664 = EDGE_CURVE('',#23036,#23036,#19130,.T.) ;
#29665 = EDGE_CURVE('',#23036,#23037,#19131,.T.) ;
#29666 = EDGE_CURVE('',#23037,#23037,#19132,.T.) ;
#29667 = EDGE_CURVE('',#23038,#23038,#1362,.T.) ;
#29668 = EDGE_CURVE('',#23039,#23039,#19133,.T.) ;
#29669 = EDGE_CURVE('',#23040,#23040,#19134,.T.) ;
#29670 = EDGE_CURVE('',#23035,#23041,#1363,.T.) ;
#29671 = EDGE_CURVE('',#23041,#23042,#1364,.T.) ;
#29672 = EDGE_CURVE('',#23042,#23041,#1365,.T.) ;
#29673 = EDGE_CURVE('',#23038,#23043,#1366,.T.) ;
#29674 = EDGE_CURVE('',#23043,#23044,#1367,.T.) ;
#29675 = EDGE_CURVE('',#23044,#23043,#1368,.T.) ;
#29676 = EDGE_CURVE('',#23045,#23046,#19135,.T.) ;
#29677 = EDGE_CURVE('',#23045,#23047,#1369,.T.) ;
#29678 = EDGE_CURVE('',#23047,#23048,#19136,.T.) ;
#29679 = EDGE_CURVE('',#23046,#23048,#1370,.T.) ;
#29680 = EDGE_CURVE('',#23045,#23049,#5754,.T.) ;
#29681 = EDGE_CURVE('',#23049,#23050,#1371,.T.) ;
#29682 = EDGE_CURVE('',#23050,#23047,#5755,.T.) ;
#29683 = EDGE_CURVE('',#23049,#23051,#19137,.T.) ;
#29684 = EDGE_CURVE('',#23051,#23052,#1372,.T.) ;
#29685 = EDGE_CURVE('',#23052,#23050,#19138,.T.) ;
#29686 = EDGE_CURVE('',#23051,#23053,#5756,.T.) ;
#29687 = EDGE_CURVE('',#23053,#23054,#1373,.T.) ;
#29688 = EDGE_CURVE('',#23054,#23052,#5757,.T.) ;
#29689 = EDGE_CURVE('',#23055,#23053,#19139,.T.) ;
#29690 = EDGE_CURVE('',#23055,#23056,#1374,.T.) ;
#29691 = EDGE_CURVE('',#23056,#23054,#19140,.T.) ;
#29692 = EDGE_CURVE('',#23055,#23057,#5758,.T.) ;
#29693 = EDGE_CURVE('',#23057,#23058,#1375,.T.) ;
#29694 = EDGE_CURVE('',#23058,#23056,#5759,.T.) ;
#29695 = EDGE_CURVE('',#23057,#23059,#19141,.T.) ;
#29696 = EDGE_CURVE('',#23059,#23060,#1376,.T.) ;
#29697 = EDGE_CURVE('',#23060,#23058,#19142,.T.) ;
#29698 = EDGE_CURVE('',#23059,#23061,#5760,.T.) ;
#29699 = EDGE_CURVE('',#23061,#23062,#1377,.T.) ;
#29700 = EDGE_CURVE('',#23062,#23060,#5761,.T.) ;
#29701 = EDGE_CURVE('',#23063,#23061,#19143,.T.) ;
#29702 = EDGE_CURVE('',#23063,#23064,#1378,.T.) ;
#29703 = EDGE_CURVE('',#23064,#23062,#19144,.T.) ;
#29704 = EDGE_CURVE('',#23063,#23065,#5762,.T.) ;
#29705 = EDGE_CURVE('',#23065,#23066,#1379,.T.) ;
#29706 = EDGE_CURVE('',#23066,#23064,#5763,.T.) ;
#29707 = EDGE_CURVE('',#23065,#23067,#19145,.T.) ;
#29708 = EDGE_CURVE('',#23067,#23068,#1380,.T.) ;
#29709 = EDGE_CURVE('',#23068,#23066,#19146,.T.) ;
#29710 = EDGE_CURVE('',#23067,#23069,#5764,.T.) ;
#29711 = EDGE_CURVE('',#23069,#23070,#1381,.T.) ;
#29712 = EDGE_CURVE('',#23070,#23068,#5765,.T.) ;
#29713 = EDGE_CURVE('',#23071,#23069,#19147,.T.) ;
#29714 = EDGE_CURVE('',#23071,#23072,#1382,.T.) ;
#29715 = EDGE_CURVE('',#23072,#23070,#19148,.T.) ;
#29716 = EDGE_CURVE('',#23071,#23073,#5766,.T.) ;
#29717 = EDGE_CURVE('',#23073,#23074,#1383,.T.) ;
#29718 = EDGE_CURVE('',#23074,#23072,#5767,.T.) ;
#29719 = EDGE_CURVE('',#23073,#23075,#19149,.T.) ;
#29720 = EDGE_CURVE('',#23075,#23076,#1384,.T.) ;
#29721 = EDGE_CURVE('',#23076,#23074,#19150,.T.) ;
#29722 = EDGE_CURVE('',#23075,#23077,#5768,.T.) ;
#29723 = EDGE_CURVE('',#23077,#23078,#1385,.T.) ;
#29724 = EDGE_CURVE('',#23078,#23076,#5769,.T.) ;
#29725 = EDGE_CURVE('',#23079,#23077,#19151,.T.) ;
#29726 = EDGE_CURVE('',#23079,#23080,#1386,.T.) ;
#29727 = EDGE_CURVE('',#23080,#23078,#19152,.T.) ;
#29728 = EDGE_CURVE('',#23079,#23081,#5770,.T.) ;
#29729 = EDGE_CURVE('',#23081,#23082,#1387,.T.) ;
#29730 = EDGE_CURVE('',#23082,#23080,#5771,.T.) ;
#29731 = EDGE_CURVE('',#23081,#23083,#19153,.T.) ;
#29732 = EDGE_CURVE('',#23083,#23084,#1388,.T.) ;
#29733 = EDGE_CURVE('',#23084,#23082,#19154,.T.) ;
#29734 = EDGE_CURVE('',#23083,#23085,#5772,.T.) ;
#29735 = EDGE_CURVE('',#23085,#23086,#1389,.T.) ;
#29736 = EDGE_CURVE('',#23086,#23084,#5773,.T.) ;
#29737 = EDGE_CURVE('',#23087,#23085,#19155,.T.) ;
#29738 = EDGE_CURVE('',#23087,#23088,#1390,.T.) ;
#29739 = EDGE_CURVE('',#23088,#23086,#19156,.T.) ;
#29740 = EDGE_CURVE('',#23087,#23089,#5774,.T.) ;
#29741 = EDGE_CURVE('',#23089,#23090,#1391,.T.) ;
#29742 = EDGE_CURVE('',#23090,#23088,#5775,.T.) ;
#29743 = EDGE_CURVE('',#23089,#23091,#19157,.T.) ;
#29744 = EDGE_CURVE('',#23091,#23092,#1392,.T.) ;
#29745 = EDGE_CURVE('',#23092,#23090,#19158,.T.) ;
#29746 = EDGE_CURVE('',#23091,#23093,#5776,.T.) ;
#29747 = EDGE_CURVE('',#23093,#23094,#1393,.T.) ;
#29748 = EDGE_CURVE('',#23094,#23092,#5777,.T.) ;
#29749 = EDGE_CURVE('',#23095,#23093,#19159,.T.) ;
#29750 = EDGE_CURVE('',#23095,#23096,#1394,.T.) ;
#29751 = EDGE_CURVE('',#23096,#23094,#19160,.T.) ;
#29752 = EDGE_CURVE('',#23095,#23097,#5778,.T.) ;
#29753 = EDGE_CURVE('',#23097,#23098,#1395,.T.) ;
#29754 = EDGE_CURVE('',#23098,#23096,#5779,.T.) ;
#29755 = EDGE_CURVE('',#23097,#23099,#19161,.T.) ;
#29756 = EDGE_CURVE('',#23099,#23100,#1396,.T.) ;
#29757 = EDGE_CURVE('',#23100,#23098,#19162,.T.) ;
#29758 = EDGE_CURVE('',#23099,#23101,#5780,.T.) ;
#29759 = EDGE_CURVE('',#23101,#23102,#1397,.T.) ;
#29760 = EDGE_CURVE('',#23102,#23100,#5781,.T.) ;
#29761 = EDGE_CURVE('',#23103,#23101,#19163,.T.) ;
#29762 = EDGE_CURVE('',#23103,#23104,#1398,.T.) ;
#29763 = EDGE_CURVE('',#23104,#23102,#19164,.T.) ;
#29764 = EDGE_CURVE('',#23103,#23105,#5782,.T.) ;
#29765 = EDGE_CURVE('',#23105,#23106,#1399,.T.) ;
#29766 = EDGE_CURVE('',#23106,#23104,#5783,.T.) ;
#29767 = EDGE_CURVE('',#23105,#23107,#19165,.T.) ;
#29768 = EDGE_CURVE('',#23107,#23108,#1400,.T.) ;
#29769 = EDGE_CURVE('',#23108,#23106,#19166,.T.) ;
#29770 = EDGE_CURVE('',#23107,#23109,#5784,.T.) ;
#29771 = EDGE_CURVE('',#23109,#23110,#1401,.T.) ;
#29772 = EDGE_CURVE('',#23110,#23108,#5785,.T.) ;
#29773 = EDGE_CURVE('',#23111,#23109,#19167,.T.) ;
#29774 = EDGE_CURVE('',#23111,#23112,#1402,.T.) ;
#29775 = EDGE_CURVE('',#23112,#23110,#19168,.T.) ;
#29776 = EDGE_CURVE('',#23111,#23113,#5786,.T.) ;
#29777 = EDGE_CURVE('',#23113,#23114,#1403,.T.) ;
#29778 = EDGE_CURVE('',#23114,#23112,#5787,.T.) ;
#29779 = EDGE_CURVE('',#23113,#23115,#19169,.T.) ;
#29780 = EDGE_CURVE('',#23115,#23116,#1404,.T.) ;
#29781 = EDGE_CURVE('',#23116,#23114,#19170,.T.) ;
#29782 = EDGE_CURVE('',#23115,#23117,#5788,.T.) ;
#29783 = EDGE_CURVE('',#23117,#23118,#1405,.T.) ;
#29784 = EDGE_CURVE('',#23118,#23116,#5789,.T.) ;
#29785 = EDGE_CURVE('',#23119,#23117,#19171,.T.) ;
#29786 = EDGE_CURVE('',#23119,#23120,#1406,.T.) ;
#29787 = EDGE_CURVE('',#23120,#23118,#19172,.T.) ;
#29788 = EDGE_CURVE('',#23119,#23121,#5790,.T.) ;
#29789 = EDGE_CURVE('',#23121,#23122,#1407,.T.) ;
#29790 = EDGE_CURVE('',#23122,#23120,#5791,.T.) ;
#29791 = EDGE_CURVE('',#23121,#23123,#19173,.T.) ;
#29792 = EDGE_CURVE('',#23123,#23124,#1408,.T.) ;
#29793 = EDGE_CURVE('',#23124,#23122,#19174,.T.) ;
#29794 = EDGE_CURVE('',#23123,#23125,#5792,.T.) ;
#29795 = EDGE_CURVE('',#23125,#23126,#1409,.T.) ;
#29796 = EDGE_CURVE('',#23126,#23124,#5793,.T.) ;
#29797 = EDGE_CURVE('',#23127,#23125,#19175,.T.) ;
#29798 = EDGE_CURVE('',#23127,#23128,#1410,.T.) ;
#29799 = EDGE_CURVE('',#23128,#23126,#19176,.T.) ;
#29800 = EDGE_CURVE('',#23129,#23128,#5794,.T.) ;
#29801 = EDGE_CURVE('',#23127,#23130,#5795,.T.) ;
#29802 = EDGE_CURVE('',#23130,#23129,#1411,.T.) ;
#29803 = EDGE_CURVE('',#23131,#23129,#19177,.T.) ;
#29804 = EDGE_CURVE('',#23130,#23132,#19178,.T.) ;
#29805 = EDGE_CURVE('',#23132,#23131,#1412,.T.) ;
#29806 = EDGE_CURVE('',#23133,#23131,#5796,.T.) ;
#29807 = EDGE_CURVE('',#23132,#23134,#5797,.T.) ;
#29808 = EDGE_CURVE('',#23134,#23133,#1413,.T.) ;
#29809 = EDGE_CURVE('',#23135,#23133,#19179,.T.) ;
#29810 = EDGE_CURVE('',#23136,#23134,#19180,.T.) ;
#29811 = EDGE_CURVE('',#23136,#23135,#1414,.T.) ;
#29812 = EDGE_CURVE('',#23137,#23135,#5798,.T.) ;
#29813 = EDGE_CURVE('',#23136,#23138,#5799,.T.) ;
#29814 = EDGE_CURVE('',#23138,#23137,#1415,.T.) ;
#29815 = EDGE_CURVE('',#23139,#23137,#19181,.T.) ;
#29816 = EDGE_CURVE('',#23138,#23140,#19182,.T.) ;
#29817 = EDGE_CURVE('',#23140,#23139,#1416,.T.) ;
#29818 = EDGE_CURVE('',#23141,#23139,#5800,.T.) ;
#29819 = EDGE_CURVE('',#23140,#23142,#5801,.T.) ;
#29820 = EDGE_CURVE('',#23142,#23141,#1417,.T.) ;
#29821 = EDGE_CURVE('',#23143,#23141,#19183,.T.) ;
#29822 = EDGE_CURVE('',#23144,#23142,#19184,.T.) ;
#29823 = EDGE_CURVE('',#23144,#23143,#1418,.T.) ;
#29824 = EDGE_CURVE('',#23145,#23143,#5802,.T.) ;
#29825 = EDGE_CURVE('',#23144,#23146,#5803,.T.) ;
#29826 = EDGE_CURVE('',#23146,#23145,#1419,.T.) ;
#29827 = EDGE_CURVE('',#23147,#23145,#19185,.T.) ;
#29828 = EDGE_CURVE('',#23146,#23148,#19186,.T.) ;
#29829 = EDGE_CURVE('',#23148,#23147,#1420,.T.) ;
#29830 = EDGE_CURVE('',#23149,#23147,#5804,.T.) ;
#29831 = EDGE_CURVE('',#23148,#23150,#5805,.T.) ;
#29832 = EDGE_CURVE('',#23150,#23149,#1421,.T.) ;
#29833 = EDGE_CURVE('',#23151,#23149,#19187,.T.) ;
#29834 = EDGE_CURVE('',#23152,#23150,#19188,.T.) ;
#29835 = EDGE_CURVE('',#23152,#23151,#1422,.T.) ;
#29836 = EDGE_CURVE('',#23153,#23151,#5806,.T.) ;
#29837 = EDGE_CURVE('',#23152,#23154,#5807,.T.) ;
#29838 = EDGE_CURVE('',#23154,#23153,#1423,.T.) ;
#29839 = EDGE_CURVE('',#23155,#23153,#19189,.T.) ;
#29840 = EDGE_CURVE('',#23154,#23156,#19190,.T.) ;
#29841 = EDGE_CURVE('',#23156,#23155,#1424,.T.) ;
#29842 = EDGE_CURVE('',#23157,#23155,#5808,.T.) ;
#29843 = EDGE_CURVE('',#23156,#23158,#5809,.T.) ;
#29844 = EDGE_CURVE('',#23158,#23157,#1425,.T.) ;
#29845 = EDGE_CURVE('',#23159,#23157,#19191,.T.) ;
#29846 = EDGE_CURVE('',#23160,#23158,#19192,.T.) ;
#29847 = EDGE_CURVE('',#23160,#23159,#1426,.T.) ;
#29848 = EDGE_CURVE('',#23161,#23159,#5810,.T.) ;
#29849 = EDGE_CURVE('',#23160,#23162,#5811,.T.) ;
#29850 = EDGE_CURVE('',#23162,#23161,#1427,.T.) ;
#29851 = EDGE_CURVE('',#23163,#23161,#19193,.T.) ;
#29852 = EDGE_CURVE('',#23162,#23164,#19194,.T.) ;
#29853 = EDGE_CURVE('',#23164,#23163,#1428,.T.) ;
#29854 = EDGE_CURVE('',#23165,#23163,#5812,.T.) ;
#29855 = EDGE_CURVE('',#23164,#23166,#5813,.T.) ;
#29856 = EDGE_CURVE('',#23166,#23165,#1429,.T.) ;
#29857 = EDGE_CURVE('',#23167,#23165,#19195,.T.) ;
#29858 = EDGE_CURVE('',#23168,#23166,#19196,.T.) ;
#29859 = EDGE_CURVE('',#23168,#23167,#1430,.T.) ;
#29860 = EDGE_CURVE('',#23169,#23167,#5814,.T.) ;
#29861 = EDGE_CURVE('',#23168,#23170,#5815,.T.) ;
#29862 = EDGE_CURVE('',#23170,#23169,#1431,.T.) ;
#29863 = EDGE_CURVE('',#23171,#23169,#19197,.T.) ;
#29864 = EDGE_CURVE('',#23170,#23172,#19198,.T.) ;
#29865 = EDGE_CURVE('',#23172,#23171,#1432,.T.) ;
#29866 = EDGE_CURVE('',#23173,#23171,#5816,.T.) ;
#29867 = EDGE_CURVE('',#23172,#23174,#5817,.T.) ;
#29868 = EDGE_CURVE('',#23174,#23173,#1433,.T.) ;
#29869 = EDGE_CURVE('',#23175,#23173,#19199,.T.) ;
#29870 = EDGE_CURVE('',#23176,#23174,#19200,.T.) ;
#29871 = EDGE_CURVE('',#23176,#23175,#1434,.T.) ;
#29872 = EDGE_CURVE('',#23177,#23175,#5818,.T.) ;
#29873 = EDGE_CURVE('',#23176,#23178,#5819,.T.) ;
#29874 = EDGE_CURVE('',#23178,#23177,#1435,.T.) ;
#29875 = EDGE_CURVE('',#23179,#23177,#19201,.T.) ;
#29876 = EDGE_CURVE('',#23178,#23180,#19202,.T.) ;
#29877 = EDGE_CURVE('',#23180,#23179,#1436,.T.) ;
#29878 = EDGE_CURVE('',#23181,#23179,#5820,.T.) ;
#29879 = EDGE_CURVE('',#23180,#23182,#5821,.T.) ;
#29880 = EDGE_CURVE('',#23182,#23181,#1437,.T.) ;
#29881 = EDGE_CURVE('',#23183,#23181,#19203,.T.) ;
#29882 = EDGE_CURVE('',#23184,#23182,#19204,.T.) ;
#29883 = EDGE_CURVE('',#23184,#23183,#1438,.T.) ;
#29884 = EDGE_CURVE('',#23185,#23183,#5822,.T.) ;
#29885 = EDGE_CURVE('',#23184,#23186,#5823,.T.) ;
#29886 = EDGE_CURVE('',#23186,#23185,#1439,.T.) ;
#29887 = EDGE_CURVE('',#23187,#23185,#19205,.T.) ;
#29888 = EDGE_CURVE('',#23186,#23188,#19206,.T.) ;
#29889 = EDGE_CURVE('',#23188,#23187,#1440,.T.) ;
#29890 = EDGE_CURVE('',#23189,#23187,#5824,.T.) ;
#29891 = EDGE_CURVE('',#23188,#23190,#5825,.T.) ;
#29892 = EDGE_CURVE('',#23190,#23189,#1441,.T.) ;
#29893 = EDGE_CURVE('',#23191,#23189,#19207,.T.) ;
#29894 = EDGE_CURVE('',#23192,#23190,#19208,.T.) ;
#29895 = EDGE_CURVE('',#23192,#23191,#1442,.T.) ;
#29896 = EDGE_CURVE('',#23193,#23191,#5826,.T.) ;
#29897 = EDGE_CURVE('',#23192,#23194,#5827,.T.) ;
#29898 = EDGE_CURVE('',#23194,#23193,#1443,.T.) ;
#29899 = EDGE_CURVE('',#23195,#23193,#19209,.T.) ;
#29900 = EDGE_CURVE('',#23194,#23196,#19210,.T.) ;
#29901 = EDGE_CURVE('',#23196,#23195,#1444,.T.) ;
#29902 = EDGE_CURVE('',#23197,#23195,#5828,.T.) ;
#29903 = EDGE_CURVE('',#23196,#23198,#5829,.T.) ;
#29904 = EDGE_CURVE('',#23198,#23197,#1445,.T.) ;
#29905 = EDGE_CURVE('',#23199,#23197,#19211,.T.) ;
#29906 = EDGE_CURVE('',#23200,#23198,#19212,.T.) ;
#29907 = EDGE_CURVE('',#23200,#23199,#1446,.T.) ;
#29908 = EDGE_CURVE('',#23201,#23199,#5830,.T.) ;
#29909 = EDGE_CURVE('',#23200,#23202,#5831,.T.) ;
#29910 = EDGE_CURVE('',#23202,#23201,#1447,.T.) ;
#29911 = EDGE_CURVE('',#23203,#23201,#19213,.T.) ;
#29912 = EDGE_CURVE('',#23202,#23204,#19214,.T.) ;
#29913 = EDGE_CURVE('',#23204,#23203,#1448,.T.) ;
#29914 = EDGE_CURVE('',#23048,#23203,#5832,.T.) ;
#29915 = EDGE_CURVE('',#23204,#23046,#5833,.T.) ;
#29916 = EDGE_CURVE('',#23205,#23129,#5834,.T.) ;
#29917 = EDGE_CURVE('',#23206,#23205,#5835,.T.) ;
#29918 = EDGE_CURVE('',#23128,#23206,#5836,.T.) ;
#29919 = EDGE_CURVE('',#23207,#23131,#5837,.T.) ;
#29920 = EDGE_CURVE('',#23205,#23207,#19215,.T.) ;
#29921 = EDGE_CURVE('',#23208,#23133,#5838,.T.) ;
#29922 = EDGE_CURVE('',#23207,#23208,#5839,.T.) ;
#29923 = EDGE_CURVE('',#23135,#23209,#5840,.T.) ;
#29924 = EDGE_CURVE('',#23208,#23209,#19216,.T.) ;
#29925 = EDGE_CURVE('',#23210,#23137,#5841,.T.) ;
#29926 = EDGE_CURVE('',#23209,#23210,#5842,.T.) ;
#29927 = EDGE_CURVE('',#23211,#23139,#5843,.T.) ;
#29928 = EDGE_CURVE('',#23210,#23211,#19217,.T.) ;
#29929 = EDGE_CURVE('',#23212,#23141,#5844,.T.) ;
#29930 = EDGE_CURVE('',#23211,#23212,#5845,.T.) ;
#29931 = EDGE_CURVE('',#23143,#23213,#5846,.T.) ;
#29932 = EDGE_CURVE('',#23212,#23213,#19218,.T.) ;
#29933 = EDGE_CURVE('',#23214,#23145,#5847,.T.) ;
#29934 = EDGE_CURVE('',#23213,#23214,#5848,.T.) ;
#29935 = EDGE_CURVE('',#23215,#23147,#5849,.T.) ;
#29936 = EDGE_CURVE('',#23214,#23215,#19219,.T.) ;
#29937 = EDGE_CURVE('',#23216,#23149,#5850,.T.) ;
#29938 = EDGE_CURVE('',#23215,#23216,#5851,.T.) ;
#29939 = EDGE_CURVE('',#23151,#23217,#5852,.T.) ;
#29940 = EDGE_CURVE('',#23216,#23217,#19220,.T.) ;
#29941 = EDGE_CURVE('',#23218,#23153,#5853,.T.) ;
#29942 = EDGE_CURVE('',#23217,#23218,#5854,.T.) ;
#29943 = EDGE_CURVE('',#23219,#23155,#5855,.T.) ;
#29944 = EDGE_CURVE('',#23218,#23219,#19221,.T.) ;
#29945 = EDGE_CURVE('',#23220,#23157,#5856,.T.) ;
#29946 = EDGE_CURVE('',#23219,#23220,#5857,.T.) ;
#29947 = EDGE_CURVE('',#23159,#23221,#5858,.T.) ;
#29948 = EDGE_CURVE('',#23220,#23221,#19222,.T.) ;
#29949 = EDGE_CURVE('',#23222,#23161,#5859,.T.) ;
#29950 = EDGE_CURVE('',#23221,#23222,#5860,.T.) ;
#29951 = EDGE_CURVE('',#23223,#23163,#5861,.T.) ;
#29952 = EDGE_CURVE('',#23222,#23223,#19223,.T.) ;
#29953 = EDGE_CURVE('',#23224,#23165,#5862,.T.) ;
#29954 = EDGE_CURVE('',#23223,#23224,#5863,.T.) ;
#29955 = EDGE_CURVE('',#23167,#23225,#5864,.T.) ;
#29956 = EDGE_CURVE('',#23224,#23225,#19224,.T.) ;
#29957 = EDGE_CURVE('',#23226,#23169,#5865,.T.) ;
#29958 = EDGE_CURVE('',#23225,#23226,#5866,.T.) ;
#29959 = EDGE_CURVE('',#23227,#23171,#5867,.T.) ;
#29960 = EDGE_CURVE('',#23226,#23227,#19225,.T.) ;
#29961 = EDGE_CURVE('',#23228,#23173,#5868,.T.) ;
#29962 = EDGE_CURVE('',#23227,#23228,#5869,.T.) ;
#29963 = EDGE_CURVE('',#23175,#23229,#5870,.T.) ;
#29964 = EDGE_CURVE('',#23228,#23229,#19226,.T.) ;
#29965 = EDGE_CURVE('',#23230,#23177,#5871,.T.) ;
#29966 = EDGE_CURVE('',#23229,#23230,#5872,.T.) ;
#29967 = EDGE_CURVE('',#23231,#23179,#5873,.T.) ;
#29968 = EDGE_CURVE('',#23230,#23231,#19227,.T.) ;
#29969 = EDGE_CURVE('',#23232,#23181,#5874,.T.) ;
#29970 = EDGE_CURVE('',#23231,#23232,#5875,.T.) ;
#29971 = EDGE_CURVE('',#23183,#23233,#5876,.T.) ;
#29972 = EDGE_CURVE('',#23232,#23233,#19228,.T.) ;
#29973 = EDGE_CURVE('',#23234,#23185,#5877,.T.) ;
#29974 = EDGE_CURVE('',#23233,#23234,#5878,.T.) ;
#29975 = EDGE_CURVE('',#23235,#23187,#5879,.T.) ;
#29976 = EDGE_CURVE('',#23234,#23235,#19229,.T.) ;
#29977 = EDGE_CURVE('',#23236,#23189,#5880,.T.) ;
#29978 = EDGE_CURVE('',#23235,#23236,#5881,.T.) ;
#29979 = EDGE_CURVE('',#23191,#23237,#5882,.T.) ;
#29980 = EDGE_CURVE('',#23236,#23237,#19230,.T.) ;
#29981 = EDGE_CURVE('',#23238,#23193,#5883,.T.) ;
#29982 = EDGE_CURVE('',#23237,#23238,#5884,.T.) ;
#29983 = EDGE_CURVE('',#23239,#23195,#5885,.T.) ;
#29984 = EDGE_CURVE('',#23238,#23239,#19231,.T.) ;
#29985 = EDGE_CURVE('',#23240,#23197,#5886,.T.) ;
#29986 = EDGE_CURVE('',#23239,#23240,#5887,.T.) ;
#29987 = EDGE_CURVE('',#23199,#23241,#5888,.T.) ;
#29988 = EDGE_CURVE('',#23240,#23241,#19232,.T.) ;
#29989 = EDGE_CURVE('',#23242,#23201,#5889,.T.) ;
#29990 = EDGE_CURVE('',#23241,#23242,#5890,.T.) ;
#29991 = EDGE_CURVE('',#23243,#23203,#5891,.T.) ;
#29992 = EDGE_CURVE('',#23242,#23243,#19233,.T.) ;
#29993 = EDGE_CURVE('',#23244,#23048,#5892,.T.) ;
#29994 = EDGE_CURVE('',#23243,#23244,#5893,.T.) ;
#29995 = EDGE_CURVE('',#23047,#23245,#5894,.T.) ;
#29996 = EDGE_CURVE('',#23244,#23245,#19234,.T.) ;
#29997 = EDGE_CURVE('',#23134,#23127,#19235,.T.) ;
#29998 = EDGE_CURVE('',#23142,#23136,#19236,.T.) ;
#29999 = EDGE_CURVE('',#23125,#23119,#19237,.T.) ;
#30000 = EDGE_CURVE('',#23150,#23144,#19238,.T.) ;
#30001 = EDGE_CURVE('',#23117,#23111,#19239,.T.) ;
#30002 = EDGE_CURVE('',#23158,#23152,#19240,.T.) ;
#30003 = EDGE_CURVE('',#23109,#23103,#19241,.T.) ;
#30004 = EDGE_CURVE('',#23166,#23160,#19242,.T.) ;
#30005 = EDGE_CURVE('',#23101,#23095,#19243,.T.) ;
#30006 = EDGE_CURVE('',#23174,#23168,#19244,.T.) ;
#30007 = EDGE_CURVE('',#23093,#23087,#19245,.T.) ;
#30008 = EDGE_CURVE('',#23182,#23176,#19246,.T.) ;
#30009 = EDGE_CURVE('',#23085,#23079,#19247,.T.) ;
#30010 = EDGE_CURVE('',#23190,#23184,#19248,.T.) ;
#30011 = EDGE_CURVE('',#23077,#23071,#19249,.T.) ;
#30012 = EDGE_CURVE('',#23198,#23192,#19250,.T.) ;
#30013 = EDGE_CURVE('',#23069,#23063,#19251,.T.) ;
#30014 = EDGE_CURVE('',#23046,#23200,#19252,.T.) ;
#30015 = EDGE_CURVE('',#23246,#23055,#19253,.T.) ;
#30016 = EDGE_CURVE('',#23061,#23246,#19254,.T.) ;
#30017 = EDGE_CURVE('',#23042,#23246,#19255,.T.) ;
#30018 = EDGE_CURVE('',#23053,#23045,#19256,.T.) ;
#30019 = EDGE_CURVE('',#23044,#23247,#19257,.T.) ;
#30020 = EDGE_CURVE('',#23247,#23248,#19258,.T.) ;
#30021 = EDGE_CURVE('',#23249,#23248,#19259,.T.) ;
#30022 = EDGE_CURVE('',#23249,#23250,#19260,.T.) ;
#30023 = EDGE_CURVE('',#23251,#23250,#19261,.T.) ;
#30024 = EDGE_CURVE('',#23251,#23252,#19262,.T.) ;
#30025 = EDGE_CURVE('',#23253,#23252,#19263,.T.) ;
#30026 = EDGE_CURVE('',#23253,#23254,#19264,.T.) ;
#30027 = EDGE_CURVE('',#23255,#23254,#19265,.T.) ;
#30028 = EDGE_CURVE('',#23255,#23256,#19266,.T.) ;
#30029 = EDGE_CURVE('',#23257,#23256,#19267,.T.) ;
#30030 = EDGE_CURVE('',#23257,#23258,#19268,.T.) ;
#30031 = EDGE_CURVE('',#23259,#23258,#19269,.T.) ;
#30032 = EDGE_CURVE('',#23259,#23260,#19270,.T.) ;
#30033 = EDGE_CURVE('',#23261,#23260,#19271,.T.) ;
#30034 = EDGE_CURVE('',#23261,#23262,#19272,.T.) ;
#30035 = EDGE_CURVE('',#23263,#23262,#19273,.T.) ;
#30036 = EDGE_CURVE('',#23263,#23264,#19274,.T.) ;
#30037 = EDGE_CURVE('',#23265,#23264,#19275,.T.) ;
#30038 = EDGE_CURVE('',#23265,#23266,#19276,.T.) ;
#30039 = EDGE_CURVE('',#23267,#23266,#19277,.T.) ;
#30040 = EDGE_CURVE('',#23267,#23268,#19278,.T.) ;
#30041 = EDGE_CURVE('',#23269,#23268,#19279,.T.) ;
#30042 = EDGE_CURVE('',#23269,#23270,#19280,.T.) ;
#30043 = EDGE_CURVE('',#23271,#23270,#19281,.T.) ;
#30044 = EDGE_CURVE('',#23271,#23272,#19282,.T.) ;
#30045 = EDGE_CURVE('',#23273,#23272,#19283,.T.) ;
#30046 = EDGE_CURVE('',#23273,#23274,#19284,.T.) ;
#30047 = EDGE_CURVE('',#23275,#23274,#19285,.T.) ;
#30048 = EDGE_CURVE('',#23275,#23276,#19286,.T.) ;
#30049 = EDGE_CURVE('',#23277,#23276,#19287,.T.) ;
#30050 = EDGE_CURVE('',#23277,#23278,#19288,.T.) ;
#30051 = EDGE_CURVE('',#23279,#23278,#19289,.T.) ;
#30052 = EDGE_CURVE('',#23279,#23280,#19290,.T.) ;
#30053 = EDGE_CURVE('',#23281,#23280,#19291,.T.) ;
#30054 = EDGE_CURVE('',#23281,#23282,#19292,.T.) ;
#30055 = EDGE_CURVE('',#23283,#23282,#19293,.T.) ;
#30056 = EDGE_CURVE('',#23283,#23284,#19294,.T.) ;
#30057 = EDGE_CURVE('',#23285,#23284,#19295,.T.) ;
#30058 = EDGE_CURVE('',#23285,#23286,#19296,.T.) ;
#30059 = EDGE_CURVE('',#23287,#23286,#19297,.T.) ;
#30060 = EDGE_CURVE('',#23287,#23247,#19298,.T.) ;
#30061 = EDGE_CURVE('',#23288,#23285,#5895,.T.) ;
#30062 = EDGE_CURVE('',#23289,#23288,#19299,.T.) ;
#30063 = EDGE_CURVE('',#23286,#23289,#5896,.T.) ;
#30064 = EDGE_CURVE('',#23290,#23283,#5897,.T.) ;
#30065 = EDGE_CURVE('',#23291,#23290,#19300,.T.) ;
#30066 = EDGE_CURVE('',#23284,#23291,#5898,.T.) ;
#30067 = EDGE_CURVE('',#23292,#23281,#5899,.T.) ;
#30068 = EDGE_CURVE('',#23293,#23292,#19301,.T.) ;
#30069 = EDGE_CURVE('',#23282,#23293,#5900,.T.) ;
#30070 = EDGE_CURVE('',#23294,#23279,#5901,.T.) ;
#30071 = EDGE_CURVE('',#23295,#23294,#19302,.T.) ;
#30072 = EDGE_CURVE('',#23280,#23295,#5902,.T.) ;
#30073 = EDGE_CURVE('',#23296,#23277,#5903,.T.) ;
#30074 = EDGE_CURVE('',#23297,#23296,#19303,.T.) ;
#30075 = EDGE_CURVE('',#23278,#23297,#5904,.T.) ;
#30076 = EDGE_CURVE('',#23298,#23275,#5905,.T.) ;
#30077 = EDGE_CURVE('',#23299,#23298,#19304,.T.) ;
#30078 = EDGE_CURVE('',#23276,#23299,#5906,.T.) ;
#30079 = EDGE_CURVE('',#23300,#23273,#5907,.T.) ;
#30080 = EDGE_CURVE('',#23301,#23300,#19305,.T.) ;
#30081 = EDGE_CURVE('',#23274,#23301,#5908,.T.) ;
#30082 = EDGE_CURVE('',#23302,#23271,#5909,.T.) ;
#30083 = EDGE_CURVE('',#23303,#23302,#19306,.T.) ;
#30084 = EDGE_CURVE('',#23272,#23303,#5910,.T.) ;
#30085 = EDGE_CURVE('',#23304,#23269,#5911,.T.) ;
#30086 = EDGE_CURVE('',#23305,#23304,#19307,.T.) ;
#30087 = EDGE_CURVE('',#23270,#23305,#5912,.T.) ;
#30088 = EDGE_CURVE('',#23306,#23267,#5913,.T.) ;
#30089 = EDGE_CURVE('',#23307,#23306,#19308,.T.) ;
#30090 = EDGE_CURVE('',#23268,#23307,#5914,.T.) ;
#30091 = EDGE_CURVE('',#23308,#23265,#5915,.T.) ;
#30092 = EDGE_CURVE('',#23309,#23308,#19309,.T.) ;
#30093 = EDGE_CURVE('',#23266,#23309,#5916,.T.) ;
#30094 = EDGE_CURVE('',#23310,#23263,#5917,.T.) ;
#30095 = EDGE_CURVE('',#23311,#23310,#19310,.T.) ;
#30096 = EDGE_CURVE('',#23264,#23311,#5918,.T.) ;
#30097 = EDGE_CURVE('',#23312,#23261,#5919,.T.) ;
#30098 = EDGE_CURVE('',#23313,#23312,#19311,.T.) ;
#30099 = EDGE_CURVE('',#23262,#23313,#5920,.T.) ;
#30100 = EDGE_CURVE('',#23314,#23259,#5921,.T.) ;
#30101 = EDGE_CURVE('',#23315,#23314,#19312,.T.) ;
#30102 = EDGE_CURVE('',#23260,#23315,#5922,.T.) ;
#30103 = EDGE_CURVE('',#23316,#23257,#5923,.T.) ;
#30104 = EDGE_CURVE('',#23317,#23316,#19313,.T.) ;
#30105 = EDGE_CURVE('',#23258,#23317,#5924,.T.) ;
#30106 = EDGE_CURVE('',#23318,#23255,#5925,.T.) ;
#30107 = EDGE_CURVE('',#23319,#23318,#19314,.T.) ;
#30108 = EDGE_CURVE('',#23256,#23319,#5926,.T.) ;
#30109 = EDGE_CURVE('',#23320,#23253,#5927,.T.) ;
#30110 = EDGE_CURVE('',#23321,#23320,#19315,.T.) ;
#30111 = EDGE_CURVE('',#23254,#23321,#5928,.T.) ;
#30112 = EDGE_CURVE('',#23322,#23251,#5929,.T.) ;
#30113 = EDGE_CURVE('',#23323,#23322,#19316,.T.) ;
#30114 = EDGE_CURVE('',#23252,#23323,#5930,.T.) ;
#30115 = EDGE_CURVE('',#23324,#23249,#5931,.T.) ;
#30116 = EDGE_CURVE('',#23325,#23324,#19317,.T.) ;
#30117 = EDGE_CURVE('',#23250,#23325,#5932,.T.) ;
#30118 = EDGE_CURVE('',#23326,#23287,#5933,.T.) ;
#30119 = EDGE_CURVE('',#23327,#23326,#19318,.T.) ;
#30120 = EDGE_CURVE('',#23248,#23327,#5934,.T.) ;
#30121 = EDGE_CURVE('',#23266,#23328,#1449,.T.) ;
#30122 = EDGE_CURVE('',#23328,#23329,#19319,.T.) ;
#30123 = EDGE_CURVE('',#23267,#23329,#1450,.T.) ;
#30124 = EDGE_CURVE('',#23309,#23330,#1451,.T.) ;
#30125 = EDGE_CURVE('',#23330,#23328,#5935,.T.) ;
#30126 = EDGE_CURVE('',#23329,#23331,#5936,.T.) ;
#30127 = EDGE_CURVE('',#23331,#23306,#1452,.T.) ;
#30128 = EDGE_CURVE('',#23265,#23245,#1453,.T.) ;
#30129 = EDGE_CURVE('',#23245,#23332,#5937,.T.) ;
#30130 = EDGE_CURVE('',#23332,#23308,#1454,.T.) ;
#30131 = EDGE_CURVE('',#23264,#23244,#1455,.T.) ;
#30132 = EDGE_CURVE('',#23311,#23243,#1456,.T.) ;
#30133 = EDGE_CURVE('',#23333,#23334,#5938,.T.) ;
#30134 = EDGE_CURVE('',#23334,#23304,#1457,.T.) ;
#30135 = EDGE_CURVE('',#23269,#23333,#1458,.T.) ;
#30136 = EDGE_CURVE('',#23263,#23241,#1459,.T.) ;
#30137 = EDGE_CURVE('',#23242,#23310,#1460,.T.) ;
#30138 = EDGE_CURVE('',#23262,#23240,#1461,.T.) ;
#30139 = EDGE_CURVE('',#23313,#23239,#1462,.T.) ;
#30140 = EDGE_CURVE('',#23335,#23336,#5939,.T.) ;
#30141 = EDGE_CURVE('',#23336,#23302,#1463,.T.) ;
#30142 = EDGE_CURVE('',#23271,#23335,#1464,.T.) ;
#30143 = EDGE_CURVE('',#23261,#23237,#1465,.T.) ;
#30144 = EDGE_CURVE('',#23238,#23312,#1466,.T.) ;
#30145 = EDGE_CURVE('',#23260,#23236,#1467,.T.) ;
#30146 = EDGE_CURVE('',#23315,#23235,#1468,.T.) ;
#30147 = EDGE_CURVE('',#23337,#23338,#5940,.T.) ;
#30148 = EDGE_CURVE('',#23338,#23300,#1469,.T.) ;
#30149 = EDGE_CURVE('',#23273,#23337,#1470,.T.) ;
#30150 = EDGE_CURVE('',#23259,#23233,#1471,.T.) ;
#30151 = EDGE_CURVE('',#23234,#23314,#1472,.T.) ;
#30152 = EDGE_CURVE('',#23258,#23232,#1473,.T.) ;
#30153 = EDGE_CURVE('',#23317,#23231,#1474,.T.) ;
#30154 = EDGE_CURVE('',#23339,#23340,#5941,.T.) ;
#30155 = EDGE_CURVE('',#23340,#23298,#1475,.T.) ;
#30156 = EDGE_CURVE('',#23275,#23339,#1476,.T.) ;
#30157 = EDGE_CURVE('',#23257,#23229,#1477,.T.) ;
#30158 = EDGE_CURVE('',#23230,#23316,#1478,.T.) ;
#30159 = EDGE_CURVE('',#23256,#23228,#1479,.T.) ;
#30160 = EDGE_CURVE('',#23319,#23227,#1480,.T.) ;
#30161 = EDGE_CURVE('',#23341,#23342,#5942,.T.) ;
#30162 = EDGE_CURVE('',#23342,#23296,#1481,.T.) ;
#30163 = EDGE_CURVE('',#23277,#23341,#1482,.T.) ;
#30164 = EDGE_CURVE('',#23255,#23225,#1483,.T.) ;
#30165 = EDGE_CURVE('',#23226,#23318,#1484,.T.) ;
#30166 = EDGE_CURVE('',#23254,#23224,#1485,.T.) ;
#30167 = EDGE_CURVE('',#23321,#23223,#1486,.T.) ;
#30168 = EDGE_CURVE('',#23343,#23344,#5943,.T.) ;
#30169 = EDGE_CURVE('',#23344,#23294,#1487,.T.) ;
#30170 = EDGE_CURVE('',#23279,#23343,#1488,.T.) ;
#30171 = EDGE_CURVE('',#23253,#23221,#1489,.T.) ;
#30172 = EDGE_CURVE('',#23222,#23320,#1490,.T.) ;
#30173 = EDGE_CURVE('',#23252,#23220,#1491,.T.) ;
#30174 = EDGE_CURVE('',#23323,#23219,#1492,.T.) ;
#30175 = EDGE_CURVE('',#23345,#23346,#5944,.T.) ;
#30176 = EDGE_CURVE('',#23346,#23292,#1493,.T.) ;
#30177 = EDGE_CURVE('',#23281,#23345,#1494,.T.) ;
#30178 = EDGE_CURVE('',#23251,#23217,#1495,.T.) ;
#30179 = EDGE_CURVE('',#23218,#23322,#1496,.T.) ;
#30180 = EDGE_CURVE('',#23250,#23216,#1497,.T.) ;
#30181 = EDGE_CURVE('',#23325,#23215,#1498,.T.) ;
#30182 = EDGE_CURVE('',#23347,#23348,#5945,.T.) ;
#30183 = EDGE_CURVE('',#23348,#23290,#1499,.T.) ;
#30184 = EDGE_CURVE('',#23283,#23347,#1500,.T.) ;
#30185 = EDGE_CURVE('',#23249,#23213,#1501,.T.) ;
#30186 = EDGE_CURVE('',#23214,#23324,#1502,.T.) ;
#30187 = EDGE_CURVE('',#23248,#23212,#1503,.T.) ;
#30188 = EDGE_CURVE('',#23327,#23211,#1504,.T.) ;
#30189 = EDGE_CURVE('',#23205,#23288,#1505,.T.) ;
#30190 = EDGE_CURVE('',#23285,#23206,#1506,.T.) ;
#30191 = EDGE_CURVE('',#23287,#23209,#1507,.T.) ;
#30192 = EDGE_CURVE('',#23210,#23326,#1508,.T.) ;
#30193 = EDGE_CURVE('',#23286,#23208,#1509,.T.) ;
#30194 = EDGE_CURVE('',#23289,#23207,#1510,.T.) ;
#30195 = EDGE_CURVE('',#23349,#23206,#19320,.T.) ;
#30196 = EDGE_CURVE('',#23284,#23349,#1511,.T.) ;
#30197 = EDGE_CURVE('',#23350,#23349,#5946,.T.) ;
#30198 = EDGE_CURVE('',#23291,#23350,#1512,.T.) ;
#30199 = EDGE_CURVE('',#23348,#23350,#19321,.T.) ;
#30200 = EDGE_CURVE('',#23351,#23347,#19322,.T.) ;
#30201 = EDGE_CURVE('',#23282,#23351,#1513,.T.) ;
#30202 = EDGE_CURVE('',#23352,#23351,#5947,.T.) ;
#30203 = EDGE_CURVE('',#23293,#23352,#1514,.T.) ;
#30204 = EDGE_CURVE('',#23346,#23352,#19323,.T.) ;
#30205 = EDGE_CURVE('',#23353,#23345,#19324,.T.) ;
#30206 = EDGE_CURVE('',#23280,#23353,#1515,.T.) ;
#30207 = EDGE_CURVE('',#23354,#23353,#5948,.T.) ;
#30208 = EDGE_CURVE('',#23295,#23354,#1516,.T.) ;
#30209 = EDGE_CURVE('',#23344,#23354,#19325,.T.) ;
#30210 = EDGE_CURVE('',#23355,#23343,#19326,.T.) ;
#30211 = EDGE_CURVE('',#23278,#23355,#1517,.T.) ;
#30212 = EDGE_CURVE('',#23356,#23355,#5949,.T.) ;
#30213 = EDGE_CURVE('',#23297,#23356,#1518,.T.) ;
#30214 = EDGE_CURVE('',#23342,#23356,#19327,.T.) ;
#30215 = EDGE_CURVE('',#23357,#23341,#19328,.T.) ;
#30216 = EDGE_CURVE('',#23276,#23357,#1519,.T.) ;
#30217 = EDGE_CURVE('',#23358,#23357,#5950,.T.) ;
#30218 = EDGE_CURVE('',#23299,#23358,#1520,.T.) ;
#30219 = EDGE_CURVE('',#23340,#23358,#19329,.T.) ;
#30220 = EDGE_CURVE('',#23359,#23339,#19330,.T.) ;
#30221 = EDGE_CURVE('',#23274,#23359,#1521,.T.) ;
#30222 = EDGE_CURVE('',#23360,#23359,#5951,.T.) ;
#30223 = EDGE_CURVE('',#23301,#23360,#1522,.T.) ;
#30224 = EDGE_CURVE('',#23338,#23360,#19331,.T.) ;
#30225 = EDGE_CURVE('',#23361,#23337,#19332,.T.) ;
#30226 = EDGE_CURVE('',#23272,#23361,#1523,.T.) ;
#30227 = EDGE_CURVE('',#23362,#23361,#5952,.T.) ;
#30228 = EDGE_CURVE('',#23303,#23362,#1524,.T.) ;
#30229 = EDGE_CURVE('',#23336,#23362,#19333,.T.) ;
#30230 = EDGE_CURVE('',#23363,#23335,#19334,.T.) ;
#30231 = EDGE_CURVE('',#23270,#23363,#1525,.T.) ;
#30232 = EDGE_CURVE('',#23364,#23363,#5953,.T.) ;
#30233 = EDGE_CURVE('',#23305,#23364,#1526,.T.) ;
#30234 = EDGE_CURVE('',#23334,#23364,#19335,.T.) ;
#30235 = EDGE_CURVE('',#23365,#23333,#19336,.T.) ;
#30236 = EDGE_CURVE('',#23268,#23365,#1527,.T.) ;
#30237 = EDGE_CURVE('',#23366,#23365,#5954,.T.) ;
#30238 = EDGE_CURVE('',#23307,#23366,#1528,.T.) ;
#30239 = EDGE_CURVE('',#23331,#23366,#19337,.T.) ;
#30240 = EDGE_CURVE('',#23332,#23330,#19338,.T.) ;
#30241 = EDGE_CURVE('',#23056,#23329,#5955,.T.) ;
#30242 = EDGE_CURVE('',#23328,#23054,#5956,.T.) ;
#30243 = EDGE_CURVE('',#23330,#23052,#5957,.T.) ;
#30244 = EDGE_CURVE('',#23332,#23050,#5958,.T.) ;
#30245 = EDGE_CURVE('',#23349,#23126,#5959,.T.) ;
#30246 = EDGE_CURVE('',#23350,#23124,#5960,.T.) ;
#30247 = EDGE_CURVE('',#23348,#23122,#5961,.T.) ;
#30248 = EDGE_CURVE('',#23120,#23347,#5962,.T.) ;
#30249 = EDGE_CURVE('',#23351,#23118,#5963,.T.) ;
#30250 = EDGE_CURVE('',#23352,#23116,#5964,.T.) ;
#30251 = EDGE_CURVE('',#23346,#23114,#5965,.T.) ;
#30252 = EDGE_CURVE('',#23112,#23345,#5966,.T.) ;
#30253 = EDGE_CURVE('',#23353,#23110,#5967,.T.) ;
#30254 = EDGE_CURVE('',#23354,#23108,#5968,.T.) ;
#30255 = EDGE_CURVE('',#23344,#23106,#5969,.T.) ;
#30256 = EDGE_CURVE('',#23104,#23343,#5970,.T.) ;
#30257 = EDGE_CURVE('',#23355,#23102,#5971,.T.) ;
#30258 = EDGE_CURVE('',#23356,#23100,#5972,.T.) ;
#30259 = EDGE_CURVE('',#23342,#23098,#5973,.T.) ;
#30260 = EDGE_CURVE('',#23096,#23341,#5974,.T.) ;
#30261 = EDGE_CURVE('',#23357,#23094,#5975,.T.) ;
#30262 = EDGE_CURVE('',#23358,#23092,#5976,.T.) ;
#30263 = EDGE_CURVE('',#23340,#23090,#5977,.T.) ;
#30264 = EDGE_CURVE('',#23088,#23339,#5978,.T.) ;
#30265 = EDGE_CURVE('',#23359,#23086,#5979,.T.) ;
#30266 = EDGE_CURVE('',#23360,#23084,#5980,.T.) ;
#30267 = EDGE_CURVE('',#23338,#23082,#5981,.T.) ;
#30268 = EDGE_CURVE('',#23080,#23337,#5982,.T.) ;
#30269 = EDGE_CURVE('',#23361,#23078,#5983,.T.) ;
#30270 = EDGE_CURVE('',#23362,#23076,#5984,.T.) ;
#30271 = EDGE_CURVE('',#23336,#23074,#5985,.T.) ;
#30272 = EDGE_CURVE('',#23072,#23335,#5986,.T.) ;
#30273 = EDGE_CURVE('',#23363,#23070,#5987,.T.) ;
#30274 = EDGE_CURVE('',#23364,#23068,#5988,.T.) ;
#30275 = EDGE_CURVE('',#23334,#23066,#5989,.T.) ;
#30276 = EDGE_CURVE('',#23064,#23333,#5990,.T.) ;
#30277 = EDGE_CURVE('',#23365,#23062,#5991,.T.) ;
#30278 = EDGE_CURVE('',#23366,#23060,#5992,.T.) ;
#30279 = EDGE_CURVE('',#23331,#23058,#5993,.T.) ;
#30280 = EDGE_CURVE('',#23039,#23040,#5994,.T.) ;
#30281 = EDGE_CURVE('',#23367,#23367,#19339,.T.) ;
#30282 = EDGE_CURVE('',#23367,#23368,#19340,.T.) ;
#30283 = EDGE_CURVE('',#23368,#23368,#19341,.T.) ;
#30284 = EDGE_CURVE('',#23369,#23369,#1529,.T.) ;
#30285 = EDGE_CURVE('',#23370,#23370,#19342,.T.) ;
#30286 = EDGE_CURVE('',#23370,#23371,#19343,.T.) ;
#30287 = EDGE_CURVE('',#23371,#23371,#19344,.T.) ;
#30288 = EDGE_CURVE('',#23372,#23372,#1530,.T.) ;
#30289 = EDGE_CURVE('',#23373,#23373,#19345,.T.) ;
#30290 = EDGE_CURVE('',#23374,#23374,#19346,.T.) ;
#30291 = EDGE_CURVE('',#23369,#23375,#1531,.T.) ;
#30292 = EDGE_CURVE('',#23375,#23376,#1532,.T.) ;
#30293 = EDGE_CURVE('',#23376,#23375,#1533,.T.) ;
#30294 = EDGE_CURVE('',#23372,#23377,#1534,.T.) ;
#30295 = EDGE_CURVE('',#23377,#23378,#1535,.T.) ;
#30296 = EDGE_CURVE('',#23378,#23377,#1536,.T.) ;
#30297 = EDGE_CURVE('',#23379,#23380,#19347,.T.) ;
#30298 = EDGE_CURVE('',#23379,#23381,#1537,.T.) ;
#30299 = EDGE_CURVE('',#23381,#23382,#19348,.T.) ;
#30300 = EDGE_CURVE('',#23380,#23382,#1538,.T.) ;
#30301 = EDGE_CURVE('',#23379,#23383,#5995,.T.) ;
#30302 = EDGE_CURVE('',#23383,#23384,#1539,.T.) ;
#30303 = EDGE_CURVE('',#23384,#23381,#5996,.T.) ;
#30304 = EDGE_CURVE('',#23383,#23385,#19349,.T.) ;
#30305 = EDGE_CURVE('',#23385,#23386,#1540,.T.) ;
#30306 = EDGE_CURVE('',#23386,#23384,#19350,.T.) ;
#30307 = EDGE_CURVE('',#23385,#23387,#5997,.T.) ;
#30308 = EDGE_CURVE('',#23387,#23388,#1541,.T.) ;
#30309 = EDGE_CURVE('',#23388,#23386,#5998,.T.) ;
#30310 = EDGE_CURVE('',#23389,#23387,#19351,.T.) ;
#30311 = EDGE_CURVE('',#23389,#23390,#1542,.T.) ;
#30312 = EDGE_CURVE('',#23390,#23388,#19352,.T.) ;
#30313 = EDGE_CURVE('',#23389,#23391,#5999,.T.) ;
#30314 = EDGE_CURVE('',#23391,#23392,#1543,.T.) ;
#30315 = EDGE_CURVE('',#23392,#23390,#6000,.T.) ;
#30316 = EDGE_CURVE('',#23391,#23393,#19353,.T.) ;
#30317 = EDGE_CURVE('',#23393,#23394,#1544,.T.) ;
#30318 = EDGE_CURVE('',#23394,#23392,#19354,.T.) ;
#30319 = EDGE_CURVE('',#23393,#23395,#6001,.T.) ;
#30320 = EDGE_CURVE('',#23395,#23396,#1545,.T.) ;
#30321 = EDGE_CURVE('',#23396,#23394,#6002,.T.) ;
#30322 = EDGE_CURVE('',#23397,#23395,#19355,.T.) ;
#30323 = EDGE_CURVE('',#23397,#23398,#1546,.T.) ;
#30324 = EDGE_CURVE('',#23398,#23396,#19356,.T.) ;
#30325 = EDGE_CURVE('',#23397,#23399,#6003,.T.) ;
#30326 = EDGE_CURVE('',#23399,#23400,#1547,.T.) ;
#30327 = EDGE_CURVE('',#23400,#23398,#6004,.T.) ;
#30328 = EDGE_CURVE('',#23399,#23401,#19357,.T.) ;
#30329 = EDGE_CURVE('',#23401,#23402,#1548,.T.) ;
#30330 = EDGE_CURVE('',#23402,#23400,#19358,.T.) ;
#30331 = EDGE_CURVE('',#23401,#23403,#6005,.T.) ;
#30332 = EDGE_CURVE('',#23403,#23404,#1549,.T.) ;
#30333 = EDGE_CURVE('',#23404,#23402,#6006,.T.) ;
#30334 = EDGE_CURVE('',#23405,#23403,#19359,.T.) ;
#30335 = EDGE_CURVE('',#23405,#23406,#1550,.T.) ;
#30336 = EDGE_CURVE('',#23406,#23404,#19360,.T.) ;
#30337 = EDGE_CURVE('',#23405,#23407,#6007,.T.) ;
#30338 = EDGE_CURVE('',#23407,#23408,#1551,.T.) ;
#30339 = EDGE_CURVE('',#23408,#23406,#6008,.T.) ;
#30340 = EDGE_CURVE('',#23407,#23409,#19361,.T.) ;
#30341 = EDGE_CURVE('',#23409,#23410,#1552,.T.) ;
#30342 = EDGE_CURVE('',#23410,#23408,#19362,.T.) ;
#30343 = EDGE_CURVE('',#23409,#23411,#6009,.T.) ;
#30344 = EDGE_CURVE('',#23411,#23412,#1553,.T.) ;
#30345 = EDGE_CURVE('',#23412,#23410,#6010,.T.) ;
#30346 = EDGE_CURVE('',#23413,#23411,#19363,.T.) ;
#30347 = EDGE_CURVE('',#23413,#23414,#1554,.T.) ;
#30348 = EDGE_CURVE('',#23414,#23412,#19364,.T.) ;
#30349 = EDGE_CURVE('',#23413,#23415,#6011,.T.) ;
#30350 = EDGE_CURVE('',#23415,#23416,#1555,.T.) ;
#30351 = EDGE_CURVE('',#23416,#23414,#6012,.T.) ;
#30352 = EDGE_CURVE('',#23415,#23417,#19365,.T.) ;
#30353 = EDGE_CURVE('',#23417,#23418,#1556,.T.) ;
#30354 = EDGE_CURVE('',#23418,#23416,#19366,.T.) ;
#30355 = EDGE_CURVE('',#23417,#23419,#6013,.T.) ;
#30356 = EDGE_CURVE('',#23419,#23420,#1557,.T.) ;
#30357 = EDGE_CURVE('',#23420,#23418,#6014,.T.) ;
#30358 = EDGE_CURVE('',#23421,#23419,#19367,.T.) ;
#30359 = EDGE_CURVE('',#23421,#23422,#1558,.T.) ;
#30360 = EDGE_CURVE('',#23422,#23420,#19368,.T.) ;
#30361 = EDGE_CURVE('',#23421,#23423,#6015,.T.) ;
#30362 = EDGE_CURVE('',#23423,#23424,#1559,.T.) ;
#30363 = EDGE_CURVE('',#23424,#23422,#6016,.T.) ;
#30364 = EDGE_CURVE('',#23423,#23425,#19369,.T.) ;
#30365 = EDGE_CURVE('',#23425,#23426,#1560,.T.) ;
#30366 = EDGE_CURVE('',#23426,#23424,#19370,.T.) ;
#30367 = EDGE_CURVE('',#23425,#23427,#6017,.T.) ;
#30368 = EDGE_CURVE('',#23427,#23428,#1561,.T.) ;
#30369 = EDGE_CURVE('',#23428,#23426,#6018,.T.) ;
#30370 = EDGE_CURVE('',#23429,#23427,#19371,.T.) ;
#30371 = EDGE_CURVE('',#23429,#23430,#1562,.T.) ;
#30372 = EDGE_CURVE('',#23430,#23428,#19372,.T.) ;
#30373 = EDGE_CURVE('',#23429,#23431,#6019,.T.) ;
#30374 = EDGE_CURVE('',#23431,#23432,#1563,.T.) ;
#30375 = EDGE_CURVE('',#23432,#23430,#6020,.T.) ;
#30376 = EDGE_CURVE('',#23431,#23433,#19373,.T.) ;
#30377 = EDGE_CURVE('',#23433,#23434,#1564,.T.) ;
#30378 = EDGE_CURVE('',#23434,#23432,#19374,.T.) ;
#30379 = EDGE_CURVE('',#23433,#23435,#6021,.T.) ;
#30380 = EDGE_CURVE('',#23435,#23436,#1565,.T.) ;
#30381 = EDGE_CURVE('',#23436,#23434,#6022,.T.) ;
#30382 = EDGE_CURVE('',#23437,#23435,#19375,.T.) ;
#30383 = EDGE_CURVE('',#23437,#23438,#1566,.T.) ;
#30384 = EDGE_CURVE('',#23438,#23436,#19376,.T.) ;
#30385 = EDGE_CURVE('',#23437,#23439,#6023,.T.) ;
#30386 = EDGE_CURVE('',#23439,#23440,#1567,.T.) ;
#30387 = EDGE_CURVE('',#23440,#23438,#6024,.T.) ;
#30388 = EDGE_CURVE('',#23439,#23441,#19377,.T.) ;
#30389 = EDGE_CURVE('',#23441,#23442,#1568,.T.) ;
#30390 = EDGE_CURVE('',#23442,#23440,#19378,.T.) ;
#30391 = EDGE_CURVE('',#23441,#23443,#6025,.T.) ;
#30392 = EDGE_CURVE('',#23443,#23444,#1569,.T.) ;
#30393 = EDGE_CURVE('',#23444,#23442,#6026,.T.) ;
#30394 = EDGE_CURVE('',#23445,#23443,#19379,.T.) ;
#30395 = EDGE_CURVE('',#23445,#23446,#1570,.T.) ;
#30396 = EDGE_CURVE('',#23446,#23444,#19380,.T.) ;
#30397 = EDGE_CURVE('',#23445,#23447,#6027,.T.) ;
#30398 = EDGE_CURVE('',#23447,#23448,#1571,.T.) ;
#30399 = EDGE_CURVE('',#23448,#23446,#6028,.T.) ;
#30400 = EDGE_CURVE('',#23447,#23449,#19381,.T.) ;
#30401 = EDGE_CURVE('',#23449,#23450,#1572,.T.) ;
#30402 = EDGE_CURVE('',#23450,#23448,#19382,.T.) ;
#30403 = EDGE_CURVE('',#23449,#23451,#6029,.T.) ;
#30404 = EDGE_CURVE('',#23451,#23452,#1573,.T.) ;
#30405 = EDGE_CURVE('',#23452,#23450,#6030,.T.) ;
#30406 = EDGE_CURVE('',#23453,#23451,#19383,.T.) ;
#30407 = EDGE_CURVE('',#23453,#23454,#1574,.T.) ;
#30408 = EDGE_CURVE('',#23454,#23452,#19384,.T.) ;
#30409 = EDGE_CURVE('',#23453,#23455,#6031,.T.) ;
#30410 = EDGE_CURVE('',#23455,#23456,#1575,.T.) ;
#30411 = EDGE_CURVE('',#23456,#23454,#6032,.T.) ;
#30412 = EDGE_CURVE('',#23455,#23457,#19385,.T.) ;
#30413 = EDGE_CURVE('',#23457,#23458,#1576,.T.) ;
#30414 = EDGE_CURVE('',#23458,#23456,#19386,.T.) ;
#30415 = EDGE_CURVE('',#23457,#23459,#6033,.T.) ;
#30416 = EDGE_CURVE('',#23459,#23460,#1577,.T.) ;
#30417 = EDGE_CURVE('',#23460,#23458,#6034,.T.) ;
#30418 = EDGE_CURVE('',#23461,#23459,#19387,.T.) ;
#30419 = EDGE_CURVE('',#23461,#23462,#1578,.T.) ;
#30420 = EDGE_CURVE('',#23462,#23460,#19388,.T.) ;
#30421 = EDGE_CURVE('',#23463,#23462,#6035,.T.) ;
#30422 = EDGE_CURVE('',#23461,#23464,#6036,.T.) ;
#30423 = EDGE_CURVE('',#23464,#23463,#1579,.T.) ;
#30424 = EDGE_CURVE('',#23465,#23463,#19389,.T.) ;
#30425 = EDGE_CURVE('',#23464,#23466,#19390,.T.) ;
#30426 = EDGE_CURVE('',#23466,#23465,#1580,.T.) ;
#30427 = EDGE_CURVE('',#23467,#23465,#6037,.T.) ;
#30428 = EDGE_CURVE('',#23466,#23468,#6038,.T.) ;
#30429 = EDGE_CURVE('',#23468,#23467,#1581,.T.) ;
#30430 = EDGE_CURVE('',#23469,#23467,#19391,.T.) ;
#30431 = EDGE_CURVE('',#23470,#23468,#19392,.T.) ;
#30432 = EDGE_CURVE('',#23470,#23469,#1582,.T.) ;
#30433 = EDGE_CURVE('',#23471,#23469,#6039,.T.) ;
#30434 = EDGE_CURVE('',#23470,#23472,#6040,.T.) ;
#30435 = EDGE_CURVE('',#23472,#23471,#1583,.T.) ;
#30436 = EDGE_CURVE('',#23473,#23471,#19393,.T.) ;
#30437 = EDGE_CURVE('',#23472,#23474,#19394,.T.) ;
#30438 = EDGE_CURVE('',#23474,#23473,#1584,.T.) ;
#30439 = EDGE_CURVE('',#23475,#23473,#6041,.T.) ;
#30440 = EDGE_CURVE('',#23474,#23476,#6042,.T.) ;
#30441 = EDGE_CURVE('',#23476,#23475,#1585,.T.) ;
#30442 = EDGE_CURVE('',#23477,#23475,#19395,.T.) ;
#30443 = EDGE_CURVE('',#23478,#23476,#19396,.T.) ;
#30444 = EDGE_CURVE('',#23478,#23477,#1586,.T.) ;
#30445 = EDGE_CURVE('',#23479,#23477,#6043,.T.) ;
#30446 = EDGE_CURVE('',#23478,#23480,#6044,.T.) ;
#30447 = EDGE_CURVE('',#23480,#23479,#1587,.T.) ;
#30448 = EDGE_CURVE('',#23481,#23479,#19397,.T.) ;
#30449 = EDGE_CURVE('',#23480,#23482,#19398,.T.) ;
#30450 = EDGE_CURVE('',#23482,#23481,#1588,.T.) ;
#30451 = EDGE_CURVE('',#23483,#23481,#6045,.T.) ;
#30452 = EDGE_CURVE('',#23482,#23484,#6046,.T.) ;
#30453 = EDGE_CURVE('',#23484,#23483,#1589,.T.) ;
#30454 = EDGE_CURVE('',#23485,#23483,#19399,.T.) ;
#30455 = EDGE_CURVE('',#23486,#23484,#19400,.T.) ;
#30456 = EDGE_CURVE('',#23486,#23485,#1590,.T.) ;
#30457 = EDGE_CURVE('',#23487,#23485,#6047,.T.) ;
#30458 = EDGE_CURVE('',#23486,#23488,#6048,.T.) ;
#30459 = EDGE_CURVE('',#23488,#23487,#1591,.T.) ;
#30460 = EDGE_CURVE('',#23489,#23487,#19401,.T.) ;
#30461 = EDGE_CURVE('',#23488,#23490,#19402,.T.) ;
#30462 = EDGE_CURVE('',#23490,#23489,#1592,.T.) ;
#30463 = EDGE_CURVE('',#23491,#23489,#6049,.T.) ;
#30464 = EDGE_CURVE('',#23490,#23492,#6050,.T.) ;
#30465 = EDGE_CURVE('',#23492,#23491,#1593,.T.) ;
#30466 = EDGE_CURVE('',#23493,#23491,#19403,.T.) ;
#30467 = EDGE_CURVE('',#23494,#23492,#19404,.T.) ;
#30468 = EDGE_CURVE('',#23494,#23493,#1594,.T.) ;
#30469 = EDGE_CURVE('',#23495,#23493,#6051,.T.) ;
#30470 = EDGE_CURVE('',#23494,#23496,#6052,.T.) ;
#30471 = EDGE_CURVE('',#23496,#23495,#1595,.T.) ;
#30472 = EDGE_CURVE('',#23497,#23495,#19405,.T.) ;
#30473 = EDGE_CURVE('',#23496,#23498,#19406,.T.) ;
#30474 = EDGE_CURVE('',#23498,#23497,#1596,.T.) ;
#30475 = EDGE_CURVE('',#23499,#23497,#6053,.T.) ;
#30476 = EDGE_CURVE('',#23498,#23500,#6054,.T.) ;
#30477 = EDGE_CURVE('',#23500,#23499,#1597,.T.) ;
#30478 = EDGE_CURVE('',#23501,#23499,#19407,.T.) ;
#30479 = EDGE_CURVE('',#23502,#23500,#19408,.T.) ;
#30480 = EDGE_CURVE('',#23502,#23501,#1598,.T.) ;
#30481 = EDGE_CURVE('',#23503,#23501,#6055,.T.) ;
#30482 = EDGE_CURVE('',#23502,#23504,#6056,.T.) ;
#30483 = EDGE_CURVE('',#23504,#23503,#1599,.T.) ;
#30484 = EDGE_CURVE('',#23505,#23503,#19409,.T.) ;
#30485 = EDGE_CURVE('',#23504,#23506,#19410,.T.) ;
#30486 = EDGE_CURVE('',#23506,#23505,#1600,.T.) ;
#30487 = EDGE_CURVE('',#23507,#23505,#6057,.T.) ;
#30488 = EDGE_CURVE('',#23506,#23508,#6058,.T.) ;
#30489 = EDGE_CURVE('',#23508,#23507,#1601,.T.) ;
#30490 = EDGE_CURVE('',#23509,#23507,#19411,.T.) ;
#30491 = EDGE_CURVE('',#23510,#23508,#19412,.T.) ;
#30492 = EDGE_CURVE('',#23510,#23509,#1602,.T.) ;
#30493 = EDGE_CURVE('',#23511,#23509,#6059,.T.) ;
#30494 = EDGE_CURVE('',#23510,#23512,#6060,.T.) ;
#30495 = EDGE_CURVE('',#23512,#23511,#1603,.T.) ;
#30496 = EDGE_CURVE('',#23513,#23511,#19413,.T.) ;
#30497 = EDGE_CURVE('',#23512,#23514,#19414,.T.) ;
#30498 = EDGE_CURVE('',#23514,#23513,#1604,.T.) ;
#30499 = EDGE_CURVE('',#23515,#23513,#6061,.T.) ;
#30500 = EDGE_CURVE('',#23514,#23516,#6062,.T.) ;
#30501 = EDGE_CURVE('',#23516,#23515,#1605,.T.) ;
#30502 = EDGE_CURVE('',#23517,#23515,#19415,.T.) ;
#30503 = EDGE_CURVE('',#23518,#23516,#19416,.T.) ;
#30504 = EDGE_CURVE('',#23518,#23517,#1606,.T.) ;
#30505 = EDGE_CURVE('',#23519,#23517,#6063,.T.) ;
#30506 = EDGE_CURVE('',#23518,#23520,#6064,.T.) ;
#30507 = EDGE_CURVE('',#23520,#23519,#1607,.T.) ;
#30508 = EDGE_CURVE('',#23521,#23519,#19417,.T.) ;
#30509 = EDGE_CURVE('',#23520,#23522,#19418,.T.) ;
#30510 = EDGE_CURVE('',#23522,#23521,#1608,.T.) ;
#30511 = EDGE_CURVE('',#23523,#23521,#6065,.T.) ;
#30512 = EDGE_CURVE('',#23522,#23524,#6066,.T.) ;
#30513 = EDGE_CURVE('',#23524,#23523,#1609,.T.) ;
#30514 = EDGE_CURVE('',#23525,#23523,#19419,.T.) ;
#30515 = EDGE_CURVE('',#23526,#23524,#19420,.T.) ;
#30516 = EDGE_CURVE('',#23526,#23525,#1610,.T.) ;
#30517 = EDGE_CURVE('',#23527,#23525,#6067,.T.) ;
#30518 = EDGE_CURVE('',#23526,#23528,#6068,.T.) ;
#30519 = EDGE_CURVE('',#23528,#23527,#1611,.T.) ;
#30520 = EDGE_CURVE('',#23529,#23527,#19421,.T.) ;
#30521 = EDGE_CURVE('',#23528,#23530,#19422,.T.) ;
#30522 = EDGE_CURVE('',#23530,#23529,#1612,.T.) ;
#30523 = EDGE_CURVE('',#23531,#23529,#6069,.T.) ;
#30524 = EDGE_CURVE('',#23530,#23532,#6070,.T.) ;
#30525 = EDGE_CURVE('',#23532,#23531,#1613,.T.) ;
#30526 = EDGE_CURVE('',#23533,#23531,#19423,.T.) ;
#30527 = EDGE_CURVE('',#23534,#23532,#19424,.T.) ;
#30528 = EDGE_CURVE('',#23534,#23533,#1614,.T.) ;
#30529 = EDGE_CURVE('',#23535,#23533,#6071,.T.) ;
#30530 = EDGE_CURVE('',#23534,#23536,#6072,.T.) ;
#30531 = EDGE_CURVE('',#23536,#23535,#1615,.T.) ;
#30532 = EDGE_CURVE('',#23537,#23535,#19425,.T.) ;
#30533 = EDGE_CURVE('',#23536,#23538,#19426,.T.) ;
#30534 = EDGE_CURVE('',#23538,#23537,#1616,.T.) ;
#30535 = EDGE_CURVE('',#23382,#23537,#6073,.T.) ;
#30536 = EDGE_CURVE('',#23538,#23380,#6074,.T.) ;
#30537 = EDGE_CURVE('',#23539,#23463,#6075,.T.) ;
#30538 = EDGE_CURVE('',#23540,#23539,#6076,.T.) ;
#30539 = EDGE_CURVE('',#23462,#23540,#6077,.T.) ;
#30540 = EDGE_CURVE('',#23541,#23465,#6078,.T.) ;
#30541 = EDGE_CURVE('',#23539,#23541,#19427,.T.) ;
#30542 = EDGE_CURVE('',#23542,#23467,#6079,.T.) ;
#30543 = EDGE_CURVE('',#23541,#23542,#6080,.T.) ;
#30544 = EDGE_CURVE('',#23469,#23543,#6081,.T.) ;
#30545 = EDGE_CURVE('',#23542,#23543,#19428,.T.) ;
#30546 = EDGE_CURVE('',#23544,#23471,#6082,.T.) ;
#30547 = EDGE_CURVE('',#23543,#23544,#6083,.T.) ;
#30548 = EDGE_CURVE('',#23545,#23473,#6084,.T.) ;
#30549 = EDGE_CURVE('',#23544,#23545,#19429,.T.) ;
#30550 = EDGE_CURVE('',#23546,#23475,#6085,.T.) ;
#30551 = EDGE_CURVE('',#23545,#23546,#6086,.T.) ;
#30552 = EDGE_CURVE('',#23477,#23547,#6087,.T.) ;
#30553 = EDGE_CURVE('',#23546,#23547,#19430,.T.) ;
#30554 = EDGE_CURVE('',#23548,#23479,#6088,.T.) ;
#30555 = EDGE_CURVE('',#23547,#23548,#6089,.T.) ;
#30556 = EDGE_CURVE('',#23549,#23481,#6090,.T.) ;
#30557 = EDGE_CURVE('',#23548,#23549,#19431,.T.) ;
#30558 = EDGE_CURVE('',#23550,#23483,#6091,.T.) ;
#30559 = EDGE_CURVE('',#23549,#23550,#6092,.T.) ;
#30560 = EDGE_CURVE('',#23485,#23551,#6093,.T.) ;
#30561 = EDGE_CURVE('',#23550,#23551,#19432,.T.) ;
#30562 = EDGE_CURVE('',#23552,#23487,#6094,.T.) ;
#30563 = EDGE_CURVE('',#23551,#23552,#6095,.T.) ;
#30564 = EDGE_CURVE('',#23553,#23489,#6096,.T.) ;
#30565 = EDGE_CURVE('',#23552,#23553,#19433,.T.) ;
#30566 = EDGE_CURVE('',#23554,#23491,#6097,.T.) ;
#30567 = EDGE_CURVE('',#23553,#23554,#6098,.T.) ;
#30568 = EDGE_CURVE('',#23493,#23555,#6099,.T.) ;
#30569 = EDGE_CURVE('',#23554,#23555,#19434,.T.) ;
#30570 = EDGE_CURVE('',#23556,#23495,#6100,.T.) ;
#30571 = EDGE_CURVE('',#23555,#23556,#6101,.T.) ;
#30572 = EDGE_CURVE('',#23557,#23497,#6102,.T.) ;
#30573 = EDGE_CURVE('',#23556,#23557,#19435,.T.) ;
#30574 = EDGE_CURVE('',#23558,#23499,#6103,.T.) ;
#30575 = EDGE_CURVE('',#23557,#23558,#6104,.T.) ;
#30576 = EDGE_CURVE('',#23501,#23559,#6105,.T.) ;
#30577 = EDGE_CURVE('',#23558,#23559,#19436,.T.) ;
#30578 = EDGE_CURVE('',#23560,#23503,#6106,.T.) ;
#30579 = EDGE_CURVE('',#23559,#23560,#6107,.T.) ;
#30580 = EDGE_CURVE('',#23561,#23505,#6108,.T.) ;
#30581 = EDGE_CURVE('',#23560,#23561,#19437,.T.) ;
#30582 = EDGE_CURVE('',#23562,#23507,#6109,.T.) ;
#30583 = EDGE_CURVE('',#23561,#23562,#6110,.T.) ;
#30584 = EDGE_CURVE('',#23509,#23563,#6111,.T.) ;
#30585 = EDGE_CURVE('',#23562,#23563,#19438,.T.) ;
#30586 = EDGE_CURVE('',#23564,#23511,#6112,.T.) ;
#30587 = EDGE_CURVE('',#23563,#23564,#6113,.T.) ;
#30588 = EDGE_CURVE('',#23565,#23513,#6114,.T.) ;
#30589 = EDGE_CURVE('',#23564,#23565,#19439,.T.) ;
#30590 = EDGE_CURVE('',#23566,#23515,#6115,.T.) ;
#30591 = EDGE_CURVE('',#23565,#23566,#6116,.T.) ;
#30592 = EDGE_CURVE('',#23517,#23567,#6117,.T.) ;
#30593 = EDGE_CURVE('',#23566,#23567,#19440,.T.) ;
#30594 = EDGE_CURVE('',#23568,#23519,#6118,.T.) ;
#30595 = EDGE_CURVE('',#23567,#23568,#6119,.T.) ;
#30596 = EDGE_CURVE('',#23569,#23521,#6120,.T.) ;
#30597 = EDGE_CURVE('',#23568,#23569,#19441,.T.) ;
#30598 = EDGE_CURVE('',#23570,#23523,#6121,.T.) ;
#30599 = EDGE_CURVE('',#23569,#23570,#6122,.T.) ;
#30600 = EDGE_CURVE('',#23525,#23571,#6123,.T.) ;
#30601 = EDGE_CURVE('',#23570,#23571,#19442,.T.) ;
#30602 = EDGE_CURVE('',#23572,#23527,#6124,.T.) ;
#30603 = EDGE_CURVE('',#23571,#23572,#6125,.T.) ;
#30604 = EDGE_CURVE('',#23573,#23529,#6126,.T.) ;
#30605 = EDGE_CURVE('',#23572,#23573,#19443,.T.) ;
#30606 = EDGE_CURVE('',#23574,#23531,#6127,.T.) ;
#30607 = EDGE_CURVE('',#23573,#23574,#6128,.T.) ;
#30608 = EDGE_CURVE('',#23533,#23575,#6129,.T.) ;
#30609 = EDGE_CURVE('',#23574,#23575,#19444,.T.) ;
#30610 = EDGE_CURVE('',#23576,#23535,#6130,.T.) ;
#30611 = EDGE_CURVE('',#23575,#23576,#6131,.T.) ;
#30612 = EDGE_CURVE('',#23577,#23537,#6132,.T.) ;
#30613 = EDGE_CURVE('',#23576,#23577,#19445,.T.) ;
#30614 = EDGE_CURVE('',#23578,#23382,#6133,.T.) ;
#30615 = EDGE_CURVE('',#23577,#23578,#6134,.T.) ;
#30616 = EDGE_CURVE('',#23381,#23579,#6135,.T.) ;
#30617 = EDGE_CURVE('',#23578,#23579,#19446,.T.) ;
#30618 = EDGE_CURVE('',#23468,#23461,#19447,.T.) ;
#30619 = EDGE_CURVE('',#23476,#23470,#19448,.T.) ;
#30620 = EDGE_CURVE('',#23459,#23453,#19449,.T.) ;
#30621 = EDGE_CURVE('',#23484,#23478,#19450,.T.) ;
#30622 = EDGE_CURVE('',#23451,#23445,#19451,.T.) ;
#30623 = EDGE_CURVE('',#23492,#23486,#19452,.T.) ;
#30624 = EDGE_CURVE('',#23443,#23437,#19453,.T.) ;
#30625 = EDGE_CURVE('',#23500,#23494,#19454,.T.) ;
#30626 = EDGE_CURVE('',#23435,#23429,#19455,.T.) ;
#30627 = EDGE_CURVE('',#23508,#23502,#19456,.T.) ;
#30628 = EDGE_CURVE('',#23427,#23421,#19457,.T.) ;
#30629 = EDGE_CURVE('',#23516,#23510,#19458,.T.) ;
#30630 = EDGE_CURVE('',#23419,#23413,#19459,.T.) ;
#30631 = EDGE_CURVE('',#23524,#23518,#19460,.T.) ;
#30632 = EDGE_CURVE('',#23411,#23405,#19461,.T.) ;
#30633 = EDGE_CURVE('',#23532,#23526,#19462,.T.) ;
#30634 = EDGE_CURVE('',#23403,#23397,#19463,.T.) ;
#30635 = EDGE_CURVE('',#23380,#23534,#19464,.T.) ;
#30636 = EDGE_CURVE('',#23580,#23389,#19465,.T.) ;
#30637 = EDGE_CURVE('',#23395,#23580,#19466,.T.) ;
#30638 = EDGE_CURVE('',#23376,#23580,#19467,.T.) ;
#30639 = EDGE_CURVE('',#23387,#23379,#19468,.T.) ;
#30640 = EDGE_CURVE('',#23378,#23581,#19469,.T.) ;
#30641 = EDGE_CURVE('',#23581,#23582,#19470,.T.) ;
#30642 = EDGE_CURVE('',#23583,#23582,#19471,.T.) ;
#30643 = EDGE_CURVE('',#23583,#23584,#19472,.T.) ;
#30644 = EDGE_CURVE('',#23585,#23584,#19473,.T.) ;
#30645 = EDGE_CURVE('',#23585,#23586,#19474,.T.) ;
#30646 = EDGE_CURVE('',#23587,#23586,#19475,.T.) ;
#30647 = EDGE_CURVE('',#23587,#23588,#19476,.T.) ;
#30648 = EDGE_CURVE('',#23589,#23588,#19477,.T.) ;
#30649 = EDGE_CURVE('',#23589,#23590,#19478,.T.) ;
#30650 = EDGE_CURVE('',#23591,#23590,#19479,.T.) ;
#30651 = EDGE_CURVE('',#23591,#23592,#19480,.T.) ;
#30652 = EDGE_CURVE('',#23593,#23592,#19481,.T.) ;
#30653 = EDGE_CURVE('',#23593,#23594,#19482,.T.) ;
#30654 = EDGE_CURVE('',#23595,#23594,#19483,.T.) ;
#30655 = EDGE_CURVE('',#23595,#23596,#19484,.T.) ;
#30656 = EDGE_CURVE('',#23597,#23596,#19485,.T.) ;
#30657 = EDGE_CURVE('',#23597,#23598,#19486,.T.) ;
#30658 = EDGE_CURVE('',#23599,#23598,#19487,.T.) ;
#30659 = EDGE_CURVE('',#23599,#23600,#19488,.T.) ;
#30660 = EDGE_CURVE('',#23601,#23600,#19489,.T.) ;
#30661 = EDGE_CURVE('',#23601,#23602,#19490,.T.) ;
#30662 = EDGE_CURVE('',#23603,#23602,#19491,.T.) ;
#30663 = EDGE_CURVE('',#23603,#23604,#19492,.T.) ;
#30664 = EDGE_CURVE('',#23605,#23604,#19493,.T.) ;
#30665 = EDGE_CURVE('',#23605,#23606,#19494,.T.) ;
#30666 = EDGE_CURVE('',#23607,#23606,#19495,.T.) ;
#30667 = EDGE_CURVE('',#23607,#23608,#19496,.T.) ;
#30668 = EDGE_CURVE('',#23609,#23608,#19497,.T.) ;
#30669 = EDGE_CURVE('',#23609,#23610,#19498,.T.) ;
#30670 = EDGE_CURVE('',#23611,#23610,#19499,.T.) ;
#30671 = EDGE_CURVE('',#23611,#23612,#19500,.T.) ;
#30672 = EDGE_CURVE('',#23613,#23612,#19501,.T.) ;
#30673 = EDGE_CURVE('',#23613,#23614,#19502,.T.) ;
#30674 = EDGE_CURVE('',#23615,#23614,#19503,.T.) ;
#30675 = EDGE_CURVE('',#23615,#23616,#19504,.T.) ;
#30676 = EDGE_CURVE('',#23617,#23616,#19505,.T.) ;
#30677 = EDGE_CURVE('',#23617,#23618,#19506,.T.) ;
#30678 = EDGE_CURVE('',#23619,#23618,#19507,.T.) ;
#30679 = EDGE_CURVE('',#23619,#23620,#19508,.T.) ;
#30680 = EDGE_CURVE('',#23621,#23620,#19509,.T.) ;
#30681 = EDGE_CURVE('',#23621,#23581,#19510,.T.) ;
#30682 = EDGE_CURVE('',#23622,#23619,#6136,.T.) ;
#30683 = EDGE_CURVE('',#23623,#23622,#19511,.T.) ;
#30684 = EDGE_CURVE('',#23620,#23623,#6137,.T.) ;
#30685 = EDGE_CURVE('',#23624,#23617,#6138,.T.) ;
#30686 = EDGE_CURVE('',#23625,#23624,#19512,.T.) ;
#30687 = EDGE_CURVE('',#23618,#23625,#6139,.T.) ;
#30688 = EDGE_CURVE('',#23626,#23615,#6140,.T.) ;
#30689 = EDGE_CURVE('',#23627,#23626,#19513,.T.) ;
#30690 = EDGE_CURVE('',#23616,#23627,#6141,.T.) ;
#30691 = EDGE_CURVE('',#23628,#23613,#6142,.T.) ;
#30692 = EDGE_CURVE('',#23629,#23628,#19514,.T.) ;
#30693 = EDGE_CURVE('',#23614,#23629,#6143,.T.) ;
#30694 = EDGE_CURVE('',#23630,#23611,#6144,.T.) ;
#30695 = EDGE_CURVE('',#23631,#23630,#19515,.T.) ;
#30696 = EDGE_CURVE('',#23612,#23631,#6145,.T.) ;
#30697 = EDGE_CURVE('',#23632,#23609,#6146,.T.) ;
#30698 = EDGE_CURVE('',#23633,#23632,#19516,.T.) ;
#30699 = EDGE_CURVE('',#23610,#23633,#6147,.T.) ;
#30700 = EDGE_CURVE('',#23634,#23607,#6148,.T.) ;
#30701 = EDGE_CURVE('',#23635,#23634,#19517,.T.) ;
#30702 = EDGE_CURVE('',#23608,#23635,#6149,.T.) ;
#30703 = EDGE_CURVE('',#23636,#23605,#6150,.T.) ;
#30704 = EDGE_CURVE('',#23637,#23636,#19518,.T.) ;
#30705 = EDGE_CURVE('',#23606,#23637,#6151,.T.) ;
#30706 = EDGE_CURVE('',#23638,#23603,#6152,.T.) ;
#30707 = EDGE_CURVE('',#23639,#23638,#19519,.T.) ;
#30708 = EDGE_CURVE('',#23604,#23639,#6153,.T.) ;
#30709 = EDGE_CURVE('',#23640,#23601,#6154,.T.) ;
#30710 = EDGE_CURVE('',#23641,#23640,#19520,.T.) ;
#30711 = EDGE_CURVE('',#23602,#23641,#6155,.T.) ;
#30712 = EDGE_CURVE('',#23642,#23599,#6156,.T.) ;
#30713 = EDGE_CURVE('',#23643,#23642,#19521,.T.) ;
#30714 = EDGE_CURVE('',#23600,#23643,#6157,.T.) ;
#30715 = EDGE_CURVE('',#23644,#23597,#6158,.T.) ;
#30716 = EDGE_CURVE('',#23645,#23644,#19522,.T.) ;
#30717 = EDGE_CURVE('',#23598,#23645,#6159,.T.) ;
#30718 = EDGE_CURVE('',#23646,#23595,#6160,.T.) ;
#30719 = EDGE_CURVE('',#23647,#23646,#19523,.T.) ;
#30720 = EDGE_CURVE('',#23596,#23647,#6161,.T.) ;
#30721 = EDGE_CURVE('',#23648,#23593,#6162,.T.) ;
#30722 = EDGE_CURVE('',#23649,#23648,#19524,.T.) ;
#30723 = EDGE_CURVE('',#23594,#23649,#6163,.T.) ;
#30724 = EDGE_CURVE('',#23650,#23591,#6164,.T.) ;
#30725 = EDGE_CURVE('',#23651,#23650,#19525,.T.) ;
#30726 = EDGE_CURVE('',#23592,#23651,#6165,.T.) ;
#30727 = EDGE_CURVE('',#23652,#23589,#6166,.T.) ;
#30728 = EDGE_CURVE('',#23653,#23652,#19526,.T.) ;
#30729 = EDGE_CURVE('',#23590,#23653,#6167,.T.) ;
#30730 = EDGE_CURVE('',#23654,#23587,#6168,.T.) ;
#30731 = EDGE_CURVE('',#23655,#23654,#19527,.T.) ;
#30732 = EDGE_CURVE('',#23588,#23655,#6169,.T.) ;
#30733 = EDGE_CURVE('',#23656,#23585,#6170,.T.) ;
#30734 = EDGE_CURVE('',#23657,#23656,#19528,.T.) ;
#30735 = EDGE_CURVE('',#23586,#23657,#6171,.T.) ;
#30736 = EDGE_CURVE('',#23658,#23583,#6172,.T.) ;
#30737 = EDGE_CURVE('',#23659,#23658,#19529,.T.) ;
#30738 = EDGE_CURVE('',#23584,#23659,#6173,.T.) ;
#30739 = EDGE_CURVE('',#23660,#23621,#6174,.T.) ;
#30740 = EDGE_CURVE('',#23661,#23660,#19530,.T.) ;
#30741 = EDGE_CURVE('',#23582,#23661,#6175,.T.) ;
#30742 = EDGE_CURVE('',#23600,#23662,#1617,.T.) ;
#30743 = EDGE_CURVE('',#23662,#23663,#19531,.T.) ;
#30744 = EDGE_CURVE('',#23601,#23663,#1618,.T.) ;
#30745 = EDGE_CURVE('',#23643,#23664,#1619,.T.) ;
#30746 = EDGE_CURVE('',#23664,#23662,#6176,.T.) ;
#30747 = EDGE_CURVE('',#23663,#23665,#6177,.T.) ;
#30748 = EDGE_CURVE('',#23665,#23640,#1620,.T.) ;
#30749 = EDGE_CURVE('',#23599,#23579,#1621,.T.) ;
#30750 = EDGE_CURVE('',#23579,#23666,#6178,.T.) ;
#30751 = EDGE_CURVE('',#23666,#23642,#1622,.T.) ;
#30752 = EDGE_CURVE('',#23598,#23578,#1623,.T.) ;
#30753 = EDGE_CURVE('',#23645,#23577,#1624,.T.) ;
#30754 = EDGE_CURVE('',#23667,#23668,#6179,.T.) ;
#30755 = EDGE_CURVE('',#23668,#23638,#1625,.T.) ;
#30756 = EDGE_CURVE('',#23603,#23667,#1626,.T.) ;
#30757 = EDGE_CURVE('',#23597,#23575,#1627,.T.) ;
#30758 = EDGE_CURVE('',#23576,#23644,#1628,.T.) ;
#30759 = EDGE_CURVE('',#23596,#23574,#1629,.T.) ;
#30760 = EDGE_CURVE('',#23647,#23573,#1630,.T.) ;
#30761 = EDGE_CURVE('',#23669,#23670,#6180,.T.) ;
#30762 = EDGE_CURVE('',#23670,#23636,#1631,.T.) ;
#30763 = EDGE_CURVE('',#23605,#23669,#1632,.T.) ;
#30764 = EDGE_CURVE('',#23595,#23571,#1633,.T.) ;
#30765 = EDGE_CURVE('',#23572,#23646,#1634,.T.) ;
#30766 = EDGE_CURVE('',#23594,#23570,#1635,.T.) ;
#30767 = EDGE_CURVE('',#23649,#23569,#1636,.T.) ;
#30768 = EDGE_CURVE('',#23671,#23672,#6181,.T.) ;
#30769 = EDGE_CURVE('',#23672,#23634,#1637,.T.) ;
#30770 = EDGE_CURVE('',#23607,#23671,#1638,.T.) ;
#30771 = EDGE_CURVE('',#23593,#23567,#1639,.T.) ;
#30772 = EDGE_CURVE('',#23568,#23648,#1640,.T.) ;
#30773 = EDGE_CURVE('',#23592,#23566,#1641,.T.) ;
#30774 = EDGE_CURVE('',#23651,#23565,#1642,.T.) ;
#30775 = EDGE_CURVE('',#23673,#23674,#6182,.T.) ;
#30776 = EDGE_CURVE('',#23674,#23632,#1643,.T.) ;
#30777 = EDGE_CURVE('',#23609,#23673,#1644,.T.) ;
#30778 = EDGE_CURVE('',#23591,#23563,#1645,.T.) ;
#30779 = EDGE_CURVE('',#23564,#23650,#1646,.T.) ;
#30780 = EDGE_CURVE('',#23590,#23562,#1647,.T.) ;
#30781 = EDGE_CURVE('',#23653,#23561,#1648,.T.) ;
#30782 = EDGE_CURVE('',#23675,#23676,#6183,.T.) ;
#30783 = EDGE_CURVE('',#23676,#23630,#1649,.T.) ;
#30784 = EDGE_CURVE('',#23611,#23675,#1650,.T.) ;
#30785 = EDGE_CURVE('',#23589,#23559,#1651,.T.) ;
#30786 = EDGE_CURVE('',#23560,#23652,#1652,.T.) ;
#30787 = EDGE_CURVE('',#23588,#23558,#1653,.T.) ;
#30788 = EDGE_CURVE('',#23655,#23557,#1654,.T.) ;
#30789 = EDGE_CURVE('',#23677,#23678,#6184,.T.) ;
#30790 = EDGE_CURVE('',#23678,#23628,#1655,.T.) ;
#30791 = EDGE_CURVE('',#23613,#23677,#1656,.T.) ;
#30792 = EDGE_CURVE('',#23587,#23555,#1657,.T.) ;
#30793 = EDGE_CURVE('',#23556,#23654,#1658,.T.) ;
#30794 = EDGE_CURVE('',#23586,#23554,#1659,.T.) ;
#30795 = EDGE_CURVE('',#23657,#23553,#1660,.T.) ;
#30796 = EDGE_CURVE('',#23679,#23680,#6185,.T.) ;
#30797 = EDGE_CURVE('',#23680,#23626,#1661,.T.) ;
#30798 = EDGE_CURVE('',#23615,#23679,#1662,.T.) ;
#30799 = EDGE_CURVE('',#23585,#23551,#1663,.T.) ;
#30800 = EDGE_CURVE('',#23552,#23656,#1664,.T.) ;
#30801 = EDGE_CURVE('',#23584,#23550,#1665,.T.) ;
#30802 = EDGE_CURVE('',#23659,#23549,#1666,.T.) ;
#30803 = EDGE_CURVE('',#23681,#23682,#6186,.T.) ;
#30804 = EDGE_CURVE('',#23682,#23624,#1667,.T.) ;
#30805 = EDGE_CURVE('',#23617,#23681,#1668,.T.) ;
#30806 = EDGE_CURVE('',#23583,#23547,#1669,.T.) ;
#30807 = EDGE_CURVE('',#23548,#23658,#1670,.T.) ;
#30808 = EDGE_CURVE('',#23582,#23546,#1671,.T.) ;
#30809 = EDGE_CURVE('',#23661,#23545,#1672,.T.) ;
#30810 = EDGE_CURVE('',#23539,#23622,#1673,.T.) ;
#30811 = EDGE_CURVE('',#23619,#23540,#1674,.T.) ;
#30812 = EDGE_CURVE('',#23621,#23543,#1675,.T.) ;
#30813 = EDGE_CURVE('',#23544,#23660,#1676,.T.) ;
#30814 = EDGE_CURVE('',#23620,#23542,#1677,.T.) ;
#30815 = EDGE_CURVE('',#23623,#23541,#1678,.T.) ;
#30816 = EDGE_CURVE('',#23683,#23540,#19532,.T.) ;
#30817 = EDGE_CURVE('',#23618,#23683,#1679,.T.) ;
#30818 = EDGE_CURVE('',#23684,#23683,#6187,.T.) ;
#30819 = EDGE_CURVE('',#23625,#23684,#1680,.T.) ;
#30820 = EDGE_CURVE('',#23682,#23684,#19533,.T.) ;
#30821 = EDGE_CURVE('',#23685,#23681,#19534,.T.) ;
#30822 = EDGE_CURVE('',#23616,#23685,#1681,.T.) ;
#30823 = EDGE_CURVE('',#23686,#23685,#6188,.T.) ;
#30824 = EDGE_CURVE('',#23627,#23686,#1682,.T.) ;
#30825 = EDGE_CURVE('',#23680,#23686,#19535,.T.) ;
#30826 = EDGE_CURVE('',#23687,#23679,#19536,.T.) ;
#30827 = EDGE_CURVE('',#23614,#23687,#1683,.T.) ;
#30828 = EDGE_CURVE('',#23688,#23687,#6189,.T.) ;
#30829 = EDGE_CURVE('',#23629,#23688,#1684,.T.) ;
#30830 = EDGE_CURVE('',#23678,#23688,#19537,.T.) ;
#30831 = EDGE_CURVE('',#23689,#23677,#19538,.T.) ;
#30832 = EDGE_CURVE('',#23612,#23689,#1685,.T.) ;
#30833 = EDGE_CURVE('',#23690,#23689,#6190,.T.) ;
#30834 = EDGE_CURVE('',#23631,#23690,#1686,.T.) ;
#30835 = EDGE_CURVE('',#23676,#23690,#19539,.T.) ;
#30836 = EDGE_CURVE('',#23691,#23675,#19540,.T.) ;
#30837 = EDGE_CURVE('',#23610,#23691,#1687,.T.) ;
#30838 = EDGE_CURVE('',#23692,#23691,#6191,.T.) ;
#30839 = EDGE_CURVE('',#23633,#23692,#1688,.T.) ;
#30840 = EDGE_CURVE('',#23674,#23692,#19541,.T.) ;
#30841 = EDGE_CURVE('',#23693,#23673,#19542,.T.) ;
#30842 = EDGE_CURVE('',#23608,#23693,#1689,.T.) ;
#30843 = EDGE_CURVE('',#23694,#23693,#6192,.T.) ;
#30844 = EDGE_CURVE('',#23635,#23694,#1690,.T.) ;
#30845 = EDGE_CURVE('',#23672,#23694,#19543,.T.) ;
#30846 = EDGE_CURVE('',#23695,#23671,#19544,.T.) ;
#30847 = EDGE_CURVE('',#23606,#23695,#1691,.T.) ;
#30848 = EDGE_CURVE('',#23696,#23695,#6193,.T.) ;
#30849 = EDGE_CURVE('',#23637,#23696,#1692,.T.) ;
#30850 = EDGE_CURVE('',#23670,#23696,#19545,.T.) ;
#30851 = EDGE_CURVE('',#23697,#23669,#19546,.T.) ;
#30852 = EDGE_CURVE('',#23604,#23697,#1693,.T.) ;
#30853 = EDGE_CURVE('',#23698,#23697,#6194,.T.) ;
#30854 = EDGE_CURVE('',#23639,#23698,#1694,.T.) ;
#30855 = EDGE_CURVE('',#23668,#23698,#19547,.T.) ;
#30856 = EDGE_CURVE('',#23699,#23667,#19548,.T.) ;
#30857 = EDGE_CURVE('',#23602,#23699,#1695,.T.) ;
#30858 = EDGE_CURVE('',#23700,#23699,#6195,.T.) ;
#30859 = EDGE_CURVE('',#23641,#23700,#1696,.T.) ;
#30860 = EDGE_CURVE('',#23665,#23700,#19549,.T.) ;
#30861 = EDGE_CURVE('',#23666,#23664,#19550,.T.) ;
#30862 = EDGE_CURVE('',#23390,#23663,#6196,.T.) ;
#30863 = EDGE_CURVE('',#23662,#23388,#6197,.T.) ;
#30864 = EDGE_CURVE('',#23664,#23386,#6198,.T.) ;
#30865 = EDGE_CURVE('',#23666,#23384,#6199,.T.) ;
#30866 = EDGE_CURVE('',#23683,#23460,#6200,.T.) ;
#30867 = EDGE_CURVE('',#23684,#23458,#6201,.T.) ;
#30868 = EDGE_CURVE('',#23682,#23456,#6202,.T.) ;
#30869 = EDGE_CURVE('',#23454,#23681,#6203,.T.) ;
#30870 = EDGE_CURVE('',#23685,#23452,#6204,.T.) ;
#30871 = EDGE_CURVE('',#23686,#23450,#6205,.T.) ;
#30872 = EDGE_CURVE('',#23680,#23448,#6206,.T.) ;
#30873 = EDGE_CURVE('',#23446,#23679,#6207,.T.) ;
#30874 = EDGE_CURVE('',#23687,#23444,#6208,.T.) ;
#30875 = EDGE_CURVE('',#23688,#23442,#6209,.T.) ;
#30876 = EDGE_CURVE('',#23678,#23440,#6210,.T.) ;
#30877 = EDGE_CURVE('',#23438,#23677,#6211,.T.) ;
#30878 = EDGE_CURVE('',#23689,#23436,#6212,.T.) ;
#30879 = EDGE_CURVE('',#23690,#23434,#6213,.T.) ;
#30880 = EDGE_CURVE('',#23676,#23432,#6214,.T.) ;
#30881 = EDGE_CURVE('',#23430,#23675,#6215,.T.) ;
#30882 = EDGE_CURVE('',#23691,#23428,#6216,.T.) ;
#30883 = EDGE_CURVE('',#23692,#23426,#6217,.T.) ;
#30884 = EDGE_CURVE('',#23674,#23424,#6218,.T.) ;
#30885 = EDGE_CURVE('',#23422,#23673,#6219,.T.) ;
#30886 = EDGE_CURVE('',#23693,#23420,#6220,.T.) ;
#30887 = EDGE_CURVE('',#23694,#23418,#6221,.T.) ;
#30888 = EDGE_CURVE('',#23672,#23416,#6222,.T.) ;
#30889 = EDGE_CURVE('',#23414,#23671,#6223,.T.) ;
#30890 = EDGE_CURVE('',#23695,#23412,#6224,.T.) ;
#30891 = EDGE_CURVE('',#23696,#23410,#6225,.T.) ;
#30892 = EDGE_CURVE('',#23670,#23408,#6226,.T.) ;
#30893 = EDGE_CURVE('',#23406,#23669,#6227,.T.) ;
#30894 = EDGE_CURVE('',#23697,#23404,#6228,.T.) ;
#30895 = EDGE_CURVE('',#23698,#23402,#6229,.T.) ;
#30896 = EDGE_CURVE('',#23668,#23400,#6230,.T.) ;
#30897 = EDGE_CURVE('',#23398,#23667,#6231,.T.) ;
#30898 = EDGE_CURVE('',#23699,#23396,#6232,.T.) ;
#30899 = EDGE_CURVE('',#23700,#23394,#6233,.T.) ;
#30900 = EDGE_CURVE('',#23665,#23392,#6234,.T.) ;
#30901 = EDGE_CURVE('',#23373,#23374,#6235,.T.) ;
#30902 = EDGE_CURVE('',#23701,#23702,#6236,.T.) ;
#30903 = EDGE_CURVE('',#23703,#23701,#1697,.F.) ;
#30904 = EDGE_CURVE('',#23704,#23703,#19551,.T.) ;
#30905 = EDGE_CURVE('',#23704,#23702,#1698,.T.) ;
#30906 = EDGE_CURVE('',#23705,#23706,#6237,.T.) ;
#30907 = EDGE_CURVE('',#23701,#23705,#1699,.F.) ;
#30908 = EDGE_CURVE('',#23702,#23706,#1700,.T.) ;
#30909 = EDGE_CURVE('',#23707,#23708,#6238,.T.) ;
#30910 = EDGE_CURVE('',#23709,#23707,#1701,.T.) ;
#30911 = EDGE_CURVE('',#23705,#23709,#1702,.F.) ;
#30912 = EDGE_CURVE('',#23706,#23710,#1703,.T.) ;
#30913 = EDGE_CURVE('',#23710,#23708,#1704,.T.) ;
#30914 = EDGE_CURVE('',#23711,#23712,#6239,.T.) ;
#30915 = EDGE_CURVE('',#23713,#23711,#1705,.T.) ;
#30916 = EDGE_CURVE('',#23707,#23713,#1706,.T.) ;
#30917 = EDGE_CURVE('',#23708,#23714,#1707,.T.) ;
#30918 = EDGE_CURVE('',#23714,#23712,#1708,.F.) ;
#30919 = EDGE_CURVE('',#23715,#23716,#6240,.T.) ;
#30920 = EDGE_CURVE('',#23717,#23715,#1709,.T.) ;
#30921 = EDGE_CURVE('',#23718,#23717,#19552,.T.) ;
#30922 = EDGE_CURVE('',#23718,#23716,#1710,.T.) ;
#30923 = EDGE_CURVE('',#23719,#23720,#6241,.T.) ;
#30924 = EDGE_CURVE('',#23721,#23719,#1711,.F.) ;
#30925 = EDGE_CURVE('',#23715,#23721,#1712,.T.) ;
#30926 = EDGE_CURVE('',#23716,#23720,#1713,.T.) ;
#30927 = EDGE_CURVE('',#23722,#23723,#6242,.T.) ;
#30928 = EDGE_CURVE('',#23719,#23722,#1714,.F.) ;
#30929 = EDGE_CURVE('',#23720,#23723,#1715,.T.) ;
#30930 = EDGE_CURVE('',#23724,#23725,#6243,.T.) ;
#30931 = EDGE_CURVE('',#23726,#23724,#1716,.F.) ;
#30932 = EDGE_CURVE('',#23722,#23726,#1717,.F.) ;
#30933 = EDGE_CURVE('',#23723,#23725,#1718,.T.) ;
#30934 = EDGE_CURVE('',#23727,#23728,#6244,.T.) ;
#30935 = EDGE_CURVE('',#23724,#23727,#1719,.F.) ;
#30936 = EDGE_CURVE('',#23725,#23728,#1720,.T.) ;
#30937 = EDGE_CURVE('',#23729,#23730,#6245,.T.) ;
#30938 = EDGE_CURVE('',#23731,#23729,#1721,.T.) ;
#30939 = EDGE_CURVE('',#23727,#23731,#1722,.F.) ;
#30940 = EDGE_CURVE('',#23728,#23730,#1723,.T.) ;
#30941 = EDGE_CURVE('',#23732,#23732,#19553,.T.) ;
#30942 = EDGE_CURVE('',#23733,#23734,#19554,.T.) ;
#30943 = EDGE_CURVE('',#23734,#23735,#1724,.T.) ;
#30944 = EDGE_CURVE('',#23735,#23736,#1725,.T.) ;
#30945 = EDGE_CURVE('',#23736,#23737,#1726,.T.) ;
#30946 = EDGE_CURVE('',#23737,#23738,#1727,.T.) ;
#30947 = EDGE_CURVE('',#23738,#23739,#1728,.T.) ;
#30948 = EDGE_CURVE('',#23739,#23740,#1729,.T.) ;
#30949 = EDGE_CURVE('',#23740,#23741,#19555,.T.) ;
#30950 = EDGE_CURVE('',#23741,#23742,#1730,.T.) ;
#30951 = EDGE_CURVE('',#23742,#23743,#1731,.T.) ;
#30952 = EDGE_CURVE('',#23743,#23744,#1732,.T.) ;
#30953 = EDGE_CURVE('',#23744,#23745,#1733,.T.) ;
#30954 = EDGE_CURVE('',#23745,#23746,#1734,.T.) ;
#30955 = EDGE_CURVE('',#23746,#23733,#1735,.T.) ;
#30956 = EDGE_CURVE('',#23747,#23748,#19556,.T.) ;
#30957 = EDGE_CURVE('',#23748,#23749,#1736,.T.) ;
#30958 = EDGE_CURVE('',#23749,#23750,#1737,.T.) ;
#30959 = EDGE_CURVE('',#23750,#23751,#1738,.T.) ;
#30960 = EDGE_CURVE('',#23751,#23752,#1739,.T.) ;
#30961 = EDGE_CURVE('',#23752,#23753,#1740,.T.) ;
#30962 = EDGE_CURVE('',#23753,#23754,#1741,.T.) ;
#30963 = EDGE_CURVE('',#23754,#23755,#1742,.T.) ;
#30964 = EDGE_CURVE('',#23755,#23756,#1743,.T.) ;
#30965 = EDGE_CURVE('',#23756,#23757,#19557,.T.) ;
#30966 = EDGE_CURVE('',#23757,#23758,#1744,.T.) ;
#30967 = EDGE_CURVE('',#23758,#23759,#1745,.T.) ;
#30968 = EDGE_CURVE('',#23759,#23760,#1746,.T.) ;
#30969 = EDGE_CURVE('',#23760,#23761,#1747,.T.) ;
#30970 = EDGE_CURVE('',#23761,#23762,#1748,.T.) ;
#30971 = EDGE_CURVE('',#23762,#23763,#1749,.T.) ;
#30972 = EDGE_CURVE('',#23763,#23764,#1750,.T.) ;
#30973 = EDGE_CURVE('',#23764,#23747,#1751,.T.) ;
#30974 = EDGE_CURVE('',#23765,#23765,#19558,.F.) ;
#30975 = EDGE_CURVE('',#23730,#23766,#1752,.T.) ;
#30976 = EDGE_CURVE('',#23767,#23766,#19559,.T.) ;
#30977 = EDGE_CURVE('',#23768,#23767,#1753,.T.) ;
#30978 = EDGE_CURVE('',#23729,#23768,#1754,.T.) ;
#30979 = EDGE_CURVE('',#23712,#23769,#1755,.F.) ;
#30980 = EDGE_CURVE('',#23770,#23769,#19560,.T.) ;
#30981 = EDGE_CURVE('',#23771,#23770,#1756,.T.) ;
#30982 = EDGE_CURVE('',#23711,#23771,#1757,.T.) ;
#30983 = EDGE_CURVE('',#23733,#23770,#1758,.T.) ;
#30984 = EDGE_CURVE('',#23769,#23772,#1759,.T.) ;
#30985 = EDGE_CURVE('',#23772,#23734,#1760,.T.) ;
#30986 = EDGE_CURVE('',#23773,#23741,#1761,.T.) ;
#30987 = EDGE_CURVE('',#23773,#23703,#1762,.T.) ;
#30988 = EDGE_CURVE('',#23740,#23704,#1763,.T.) ;
#30989 = EDGE_CURVE('',#23747,#23767,#1764,.T.) ;
#30990 = EDGE_CURVE('',#23766,#23774,#1765,.T.) ;
#30991 = EDGE_CURVE('',#23774,#23748,#1766,.T.) ;
#30992 = EDGE_CURVE('',#23717,#23757,#1767,.T.) ;
#30993 = EDGE_CURVE('',#23756,#23718,#1768,.T.) ;
#30994 = ORIENTED_EDGE('',*,*,#23775,.T.) ;
#30995 = ORIENTED_EDGE('',*,*,#23776,.T.) ;
#30996 = ORIENTED_EDGE('',*,*,#23777,.T.) ;
#30997 = ORIENTED_EDGE('',*,*,#23776,.F.) ;
#30998 = ORIENTED_EDGE('',*,*,#23777,.F.) ;
#30999 = ORIENTED_EDGE('',*,*,#23778,.T.) ;
#31000 = ORIENTED_EDGE('',*,*,#23779,.F.) ;
#31001 = ORIENTED_EDGE('',*,*,#23780,.F.) ;
#31002 = ORIENTED_EDGE('',*,*,#23781,.F.) ;
#31003 = ORIENTED_EDGE('',*,*,#23782,.F.) ;
#31004 = ORIENTED_EDGE('',*,*,#23783,.F.) ;
#31005 = ORIENTED_EDGE('',*,*,#23784,.F.) ;
#31006 = ORIENTED_EDGE('',*,*,#23785,.F.) ;
#31007 = ORIENTED_EDGE('',*,*,#23786,.F.) ;
#31008 = ORIENTED_EDGE('',*,*,#23787,.F.) ;
#31009 = ORIENTED_EDGE('',*,*,#23788,.F.) ;
#31010 = ORIENTED_EDGE('',*,*,#23789,.F.) ;
#31011 = ORIENTED_EDGE('',*,*,#23790,.F.) ;
#31012 = ORIENTED_EDGE('',*,*,#23791,.F.) ;
#31013 = ORIENTED_EDGE('',*,*,#23792,.F.) ;
#31014 = ORIENTED_EDGE('',*,*,#23793,.F.) ;
#31015 = ORIENTED_EDGE('',*,*,#23794,.F.) ;
#31016 = ORIENTED_EDGE('',*,*,#23795,.F.) ;
#31017 = ORIENTED_EDGE('',*,*,#23796,.F.) ;
#31018 = ORIENTED_EDGE('',*,*,#23797,.F.) ;
#31019 = ORIENTED_EDGE('',*,*,#23798,.F.) ;
#31020 = ORIENTED_EDGE('',*,*,#23799,.F.) ;
#31021 = ORIENTED_EDGE('',*,*,#23800,.F.) ;
#31022 = ORIENTED_EDGE('',*,*,#23801,.F.) ;
#31023 = ORIENTED_EDGE('',*,*,#23802,.F.) ;
#31024 = ORIENTED_EDGE('',*,*,#23803,.F.) ;
#31025 = ORIENTED_EDGE('',*,*,#23804,.F.) ;
#31026 = ORIENTED_EDGE('',*,*,#23805,.F.) ;
#31027 = ORIENTED_EDGE('',*,*,#23806,.F.) ;
#31028 = ORIENTED_EDGE('',*,*,#23807,.F.) ;
#31029 = ORIENTED_EDGE('',*,*,#23808,.F.) ;
#31030 = ORIENTED_EDGE('',*,*,#23809,.F.) ;
#31031 = ORIENTED_EDGE('',*,*,#23810,.F.) ;
#31032 = ORIENTED_EDGE('',*,*,#23811,.F.) ;
#31033 = ORIENTED_EDGE('',*,*,#23812,.F.) ;
#31034 = ORIENTED_EDGE('',*,*,#23813,.F.) ;
#31035 = ORIENTED_EDGE('',*,*,#23814,.F.) ;
#31036 = ORIENTED_EDGE('',*,*,#23815,.F.) ;
#31037 = ORIENTED_EDGE('',*,*,#23816,.F.) ;
#31038 = ORIENTED_EDGE('',*,*,#23817,.F.) ;
#31039 = ORIENTED_EDGE('',*,*,#23818,.F.) ;
#31040 = ORIENTED_EDGE('',*,*,#23819,.F.) ;
#31041 = ORIENTED_EDGE('',*,*,#23820,.F.) ;
#31042 = ORIENTED_EDGE('',*,*,#23821,.F.) ;
#31043 = ORIENTED_EDGE('',*,*,#23822,.F.) ;
#31044 = ORIENTED_EDGE('',*,*,#23823,.F.) ;
#31045 = ORIENTED_EDGE('',*,*,#23824,.F.) ;
#31046 = ORIENTED_EDGE('',*,*,#23825,.F.) ;
#31047 = ORIENTED_EDGE('',*,*,#23826,.F.) ;
#31048 = ORIENTED_EDGE('',*,*,#23827,.F.) ;
#31049 = ORIENTED_EDGE('',*,*,#23828,.F.) ;
#31050 = ORIENTED_EDGE('',*,*,#23829,.F.) ;
#31051 = ORIENTED_EDGE('',*,*,#23830,.F.) ;
#31052 = ORIENTED_EDGE('',*,*,#23831,.F.) ;
#31053 = ORIENTED_EDGE('',*,*,#23832,.F.) ;
#31054 = ORIENTED_EDGE('',*,*,#23833,.F.) ;
#31055 = ORIENTED_EDGE('',*,*,#23834,.F.) ;
#31056 = ORIENTED_EDGE('',*,*,#23835,.F.) ;
#31057 = ORIENTED_EDGE('',*,*,#23836,.F.) ;
#31058 = ORIENTED_EDGE('',*,*,#23837,.F.) ;
#31059 = ORIENTED_EDGE('',*,*,#23838,.F.) ;
#31060 = ORIENTED_EDGE('',*,*,#23839,.F.) ;
#31061 = ORIENTED_EDGE('',*,*,#23840,.F.) ;
#31062 = ORIENTED_EDGE('',*,*,#23841,.F.) ;
#31063 = ORIENTED_EDGE('',*,*,#23842,.F.) ;
#31064 = ORIENTED_EDGE('',*,*,#23843,.F.) ;
#31065 = ORIENTED_EDGE('',*,*,#23844,.F.) ;
#31066 = ORIENTED_EDGE('',*,*,#23845,.F.) ;
#31067 = ORIENTED_EDGE('',*,*,#23846,.F.) ;
#31068 = ORIENTED_EDGE('',*,*,#23847,.F.) ;
#31069 = ORIENTED_EDGE('',*,*,#23848,.F.) ;
#31070 = ORIENTED_EDGE('',*,*,#23849,.F.) ;
#31071 = ORIENTED_EDGE('',*,*,#23850,.F.) ;
#31072 = ORIENTED_EDGE('',*,*,#23851,.F.) ;
#31073 = ORIENTED_EDGE('',*,*,#23852,.F.) ;
#31074 = ORIENTED_EDGE('',*,*,#23853,.F.) ;
#31075 = ORIENTED_EDGE('',*,*,#23854,.F.) ;
#31076 = ORIENTED_EDGE('',*,*,#23855,.F.) ;
#31077 = ORIENTED_EDGE('',*,*,#23856,.F.) ;
#31078 = ORIENTED_EDGE('',*,*,#23857,.F.) ;
#31079 = ORIENTED_EDGE('',*,*,#23858,.F.) ;
#31080 = ORIENTED_EDGE('',*,*,#23859,.F.) ;
#31081 = ORIENTED_EDGE('',*,*,#23778,.F.) ;
#31082 = ORIENTED_EDGE('',*,*,#23775,.F.) ;
#31083 = ORIENTED_EDGE('',*,*,#23860,.T.) ;
#31084 = ORIENTED_EDGE('',*,*,#23861,.T.) ;
#31085 = ORIENTED_EDGE('',*,*,#23862,.T.) ;
#31086 = ORIENTED_EDGE('',*,*,#23863,.T.) ;
#31087 = ORIENTED_EDGE('',*,*,#23864,.T.) ;
#31088 = ORIENTED_EDGE('',*,*,#23865,.T.) ;
#31089 = ORIENTED_EDGE('',*,*,#23866,.T.) ;
#31090 = ORIENTED_EDGE('',*,*,#23867,.T.) ;
#31091 = ORIENTED_EDGE('',*,*,#23868,.T.) ;
#31092 = ORIENTED_EDGE('',*,*,#23869,.T.) ;
#31093 = ORIENTED_EDGE('',*,*,#23866,.F.) ;
#31094 = ORIENTED_EDGE('',*,*,#23870,.T.) ;
#31095 = ORIENTED_EDGE('',*,*,#23871,.T.) ;
#31096 = ORIENTED_EDGE('',*,*,#23872,.T.) ;
#31097 = ORIENTED_EDGE('',*,*,#23868,.F.) ;
#31098 = ORIENTED_EDGE('',*,*,#23873,.T.) ;
#31099 = ORIENTED_EDGE('',*,*,#23874,.T.) ;
#31100 = ORIENTED_EDGE('',*,*,#23875,.T.) ;
#31101 = ORIENTED_EDGE('',*,*,#23876,.T.) ;
#31102 = ORIENTED_EDGE('',*,*,#23877,.T.) ;
#31103 = ORIENTED_EDGE('',*,*,#23878,.T.) ;
#31104 = ORIENTED_EDGE('',*,*,#23879,.T.) ;
#31105 = ORIENTED_EDGE('',*,*,#23880,.T.) ;
#31106 = ORIENTED_EDGE('',*,*,#23881,.T.) ;
#31107 = ORIENTED_EDGE('',*,*,#23882,.T.) ;
#31108 = ORIENTED_EDGE('',*,*,#23883,.T.) ;
#31109 = ORIENTED_EDGE('',*,*,#23880,.F.) ;
#31110 = ORIENTED_EDGE('',*,*,#23884,.T.) ;
#31111 = ORIENTED_EDGE('',*,*,#23885,.T.) ;
#31112 = ORIENTED_EDGE('',*,*,#23886,.T.) ;
#31113 = ORIENTED_EDGE('',*,*,#23882,.F.) ;
#31114 = ORIENTED_EDGE('',*,*,#23887,.T.) ;
#31115 = ORIENTED_EDGE('',*,*,#23888,.T.) ;
#31116 = ORIENTED_EDGE('',*,*,#23889,.T.) ;
#31117 = ORIENTED_EDGE('',*,*,#23890,.T.) ;
#31118 = ORIENTED_EDGE('',*,*,#23891,.T.) ;
#31119 = ORIENTED_EDGE('',*,*,#23892,.T.) ;
#31120 = ORIENTED_EDGE('',*,*,#23893,.T.) ;
#31121 = ORIENTED_EDGE('',*,*,#23894,.T.) ;
#31122 = ORIENTED_EDGE('',*,*,#23895,.T.) ;
#31123 = ORIENTED_EDGE('',*,*,#23896,.T.) ;
#31124 = ORIENTED_EDGE('',*,*,#23897,.T.) ;
#31125 = ORIENTED_EDGE('',*,*,#23894,.F.) ;
#31126 = ORIENTED_EDGE('',*,*,#23898,.T.) ;
#31127 = ORIENTED_EDGE('',*,*,#23899,.T.) ;
#31128 = ORIENTED_EDGE('',*,*,#23900,.T.) ;
#31129 = ORIENTED_EDGE('',*,*,#23896,.F.) ;
#31130 = ORIENTED_EDGE('',*,*,#23901,.T.) ;
#31131 = ORIENTED_EDGE('',*,*,#23902,.T.) ;
#31132 = ORIENTED_EDGE('',*,*,#23903,.T.) ;
#31133 = ORIENTED_EDGE('',*,*,#23904,.T.) ;
#31134 = ORIENTED_EDGE('',*,*,#23905,.T.) ;
#31135 = ORIENTED_EDGE('',*,*,#23906,.T.) ;
#31136 = ORIENTED_EDGE('',*,*,#23907,.T.) ;
#31137 = ORIENTED_EDGE('',*,*,#23908,.T.) ;
#31138 = ORIENTED_EDGE('',*,*,#23909,.T.) ;
#31139 = ORIENTED_EDGE('',*,*,#23910,.T.) ;
#31140 = ORIENTED_EDGE('',*,*,#23911,.T.) ;
#31141 = ORIENTED_EDGE('',*,*,#23908,.F.) ;
#31142 = ORIENTED_EDGE('',*,*,#23912,.T.) ;
#31143 = ORIENTED_EDGE('',*,*,#23913,.T.) ;
#31144 = ORIENTED_EDGE('',*,*,#23914,.T.) ;
#31145 = ORIENTED_EDGE('',*,*,#23906,.F.) ;
#31146 = ORIENTED_EDGE('',*,*,#23915,.T.) ;
#31147 = ORIENTED_EDGE('',*,*,#23910,.F.) ;
#31148 = ORIENTED_EDGE('',*,*,#23902,.F.) ;
#31149 = ORIENTED_EDGE('',*,*,#23916,.T.) ;
#31150 = ORIENTED_EDGE('',*,*,#23904,.F.) ;
#31151 = ORIENTED_EDGE('',*,*,#23892,.F.) ;
#31152 = ORIENTED_EDGE('',*,*,#23917,.T.) ;
#31153 = ORIENTED_EDGE('',*,*,#23899,.F.) ;
#31154 = ORIENTED_EDGE('',*,*,#23888,.F.) ;
#31155 = ORIENTED_EDGE('',*,*,#23918,.T.) ;
#31156 = ORIENTED_EDGE('',*,*,#23890,.F.) ;
#31157 = ORIENTED_EDGE('',*,*,#23878,.F.) ;
#31158 = ORIENTED_EDGE('',*,*,#23919,.T.) ;
#31159 = ORIENTED_EDGE('',*,*,#23885,.F.) ;
#31160 = ORIENTED_EDGE('',*,*,#23874,.F.) ;
#31161 = ORIENTED_EDGE('',*,*,#23920,.T.) ;
#31162 = ORIENTED_EDGE('',*,*,#23876,.F.) ;
#31163 = ORIENTED_EDGE('',*,*,#23864,.F.) ;
#31164 = ORIENTED_EDGE('',*,*,#23921,.T.) ;
#31165 = ORIENTED_EDGE('',*,*,#23871,.F.) ;
#31166 = ORIENTED_EDGE('',*,*,#23860,.F.) ;
#31167 = ORIENTED_EDGE('',*,*,#23922,.T.) ;
#31168 = ORIENTED_EDGE('',*,*,#23862,.F.) ;
#31169 = ORIENTED_EDGE('',*,*,#23913,.F.) ;
#31170 = ORIENTED_EDGE('',*,*,#23923,.T.) ;
#31171 = ORIENTED_EDGE('',*,*,#23886,.F.) ;
#31172 = ORIENTED_EDGE('',*,*,#23924,.F.) ;
#31173 = ORIENTED_EDGE('',*,*,#23925,.F.) ;
#31174 = ORIENTED_EDGE('',*,*,#23926,.F.) ;
#31175 = ORIENTED_EDGE('',*,*,#23920,.F.) ;
#31176 = ORIENTED_EDGE('',*,*,#23927,.T.) ;
#31177 = ORIENTED_EDGE('',*,*,#23928,.T.) ;
#31178 = ORIENTED_EDGE('',*,*,#23924,.T.) ;
#31179 = ORIENTED_EDGE('',*,*,#23877,.F.) ;
#31180 = ORIENTED_EDGE('',*,*,#23929,.F.) ;
#31181 = ORIENTED_EDGE('',*,*,#23930,.F.) ;
#31182 = ORIENTED_EDGE('',*,*,#23927,.F.) ;
#31183 = ORIENTED_EDGE('',*,*,#23921,.F.) ;
#31184 = ORIENTED_EDGE('',*,*,#23931,.T.) ;
#31185 = ORIENTED_EDGE('',*,*,#23932,.T.) ;
#31186 = ORIENTED_EDGE('',*,*,#23929,.T.) ;
#31187 = ORIENTED_EDGE('',*,*,#23867,.F.) ;
#31188 = ORIENTED_EDGE('',*,*,#23933,.F.) ;
#31189 = ORIENTED_EDGE('',*,*,#23934,.F.) ;
#31190 = ORIENTED_EDGE('',*,*,#23931,.F.) ;
#31191 = ORIENTED_EDGE('',*,*,#23869,.F.) ;
#31192 = ORIENTED_EDGE('',*,*,#23935,.T.) ;
#31193 = ORIENTED_EDGE('',*,*,#23936,.F.) ;
#31194 = ORIENTED_EDGE('',*,*,#23933,.T.) ;
#31195 = ORIENTED_EDGE('',*,*,#23872,.F.) ;
#31196 = ORIENTED_EDGE('',*,*,#23937,.F.) ;
#31197 = ORIENTED_EDGE('',*,*,#23938,.F.) ;
#31198 = ORIENTED_EDGE('',*,*,#23935,.F.) ;
#31199 = ORIENTED_EDGE('',*,*,#23922,.F.) ;
#31200 = ORIENTED_EDGE('',*,*,#23939,.T.) ;
#31201 = ORIENTED_EDGE('',*,*,#23940,.T.) ;
#31202 = ORIENTED_EDGE('',*,*,#23937,.T.) ;
#31203 = ORIENTED_EDGE('',*,*,#23863,.F.) ;
#31204 = ORIENTED_EDGE('',*,*,#23941,.F.) ;
#31205 = ORIENTED_EDGE('',*,*,#23942,.F.) ;
#31206 = ORIENTED_EDGE('',*,*,#23939,.F.) ;
#31207 = ORIENTED_EDGE('',*,*,#23923,.F.) ;
#31208 = ORIENTED_EDGE('',*,*,#23943,.T.) ;
#31209 = ORIENTED_EDGE('',*,*,#23944,.T.) ;
#31210 = ORIENTED_EDGE('',*,*,#23941,.T.) ;
#31211 = ORIENTED_EDGE('',*,*,#23915,.F.) ;
#31212 = ORIENTED_EDGE('',*,*,#23945,.F.) ;
#31213 = ORIENTED_EDGE('',*,*,#23946,.F.) ;
#31214 = ORIENTED_EDGE('',*,*,#23943,.F.) ;
#31215 = ORIENTED_EDGE('',*,*,#23909,.F.) ;
#31216 = ORIENTED_EDGE('',*,*,#23947,.T.) ;
#31217 = ORIENTED_EDGE('',*,*,#23948,.F.) ;
#31218 = ORIENTED_EDGE('',*,*,#23945,.T.) ;
#31219 = ORIENTED_EDGE('',*,*,#23907,.F.) ;
#31220 = ORIENTED_EDGE('',*,*,#23914,.F.) ;
#31221 = ORIENTED_EDGE('',*,*,#23861,.F.) ;
#31222 = ORIENTED_EDGE('',*,*,#23873,.F.) ;
#31223 = ORIENTED_EDGE('',*,*,#23870,.F.) ;
#31224 = ORIENTED_EDGE('',*,*,#23865,.F.) ;
#31225 = ORIENTED_EDGE('',*,*,#23875,.F.) ;
#31226 = ORIENTED_EDGE('',*,*,#23887,.F.) ;
#31227 = ORIENTED_EDGE('',*,*,#23884,.F.) ;
#31228 = ORIENTED_EDGE('',*,*,#23879,.F.) ;
#31229 = ORIENTED_EDGE('',*,*,#23889,.F.) ;
#31230 = ORIENTED_EDGE('',*,*,#23901,.F.) ;
#31231 = ORIENTED_EDGE('',*,*,#23898,.F.) ;
#31232 = ORIENTED_EDGE('',*,*,#23893,.F.) ;
#31233 = ORIENTED_EDGE('',*,*,#23903,.F.) ;
#31234 = ORIENTED_EDGE('',*,*,#23912,.F.) ;
#31235 = ORIENTED_EDGE('',*,*,#23949,.F.) ;
#31236 = ORIENTED_EDGE('',*,*,#23950,.F.) ;
#31237 = ORIENTED_EDGE('',*,*,#23951,.F.) ;
#31238 = ORIENTED_EDGE('',*,*,#23952,.F.) ;
#31239 = ORIENTED_EDGE('',*,*,#23953,.F.) ;
#31240 = ORIENTED_EDGE('',*,*,#23954,.F.) ;
#31241 = ORIENTED_EDGE('',*,*,#23955,.F.) ;
#31242 = ORIENTED_EDGE('',*,*,#23956,.F.) ;
#31243 = ORIENTED_EDGE('',*,*,#23957,.F.) ;
#31244 = ORIENTED_EDGE('',*,*,#23951,.T.) ;
#31245 = ORIENTED_EDGE('',*,*,#23958,.T.) ;
#31246 = ORIENTED_EDGE('',*,*,#23956,.T.) ;
#31247 = ORIENTED_EDGE('',*,*,#23845,.T.) ;
#31248 = ORIENTED_EDGE('',*,*,#23959,.F.) ;
#31249 = ORIENTED_EDGE('',*,*,#23960,.F.) ;
#31250 = ORIENTED_EDGE('',*,*,#23961,.F.) ;
#31251 = ORIENTED_EDGE('',*,*,#23962,.F.) ;
#31252 = ORIENTED_EDGE('',*,*,#23963,.F.) ;
#31253 = ORIENTED_EDGE('',*,*,#23964,.F.) ;
#31254 = ORIENTED_EDGE('',*,*,#23957,.T.) ;
#31255 = ORIENTED_EDGE('',*,*,#23965,.T.) ;
#31256 = ORIENTED_EDGE('',*,*,#23963,.T.) ;
#31257 = ORIENTED_EDGE('',*,*,#23966,.T.) ;
#31258 = ORIENTED_EDGE('',*,*,#23967,.F.) ;
#31259 = ORIENTED_EDGE('',*,*,#23968,.F.) ;
#31260 = ORIENTED_EDGE('',*,*,#23969,.F.) ;
#31261 = ORIENTED_EDGE('',*,*,#23970,.F.) ;
#31262 = ORIENTED_EDGE('',*,*,#23971,.F.) ;
#31263 = ORIENTED_EDGE('',*,*,#23972,.F.) ;
#31264 = ORIENTED_EDGE('',*,*,#23964,.T.) ;
#31265 = ORIENTED_EDGE('',*,*,#23973,.T.) ;
#31266 = ORIENTED_EDGE('',*,*,#23971,.T.) ;
#31267 = ORIENTED_EDGE('',*,*,#23849,.T.) ;
#31268 = ORIENTED_EDGE('',*,*,#23974,.F.) ;
#31269 = ORIENTED_EDGE('',*,*,#23975,.F.) ;
#31270 = ORIENTED_EDGE('',*,*,#23976,.F.) ;
#31271 = ORIENTED_EDGE('',*,*,#23977,.F.) ;
#31272 = ORIENTED_EDGE('',*,*,#23978,.F.) ;
#31273 = ORIENTED_EDGE('',*,*,#23979,.F.) ;
#31274 = ORIENTED_EDGE('',*,*,#23972,.T.) ;
#31275 = ORIENTED_EDGE('',*,*,#23980,.T.) ;
#31276 = ORIENTED_EDGE('',*,*,#23978,.T.) ;
#31277 = ORIENTED_EDGE('',*,*,#23981,.T.) ;
#31278 = ORIENTED_EDGE('',*,*,#23982,.F.) ;
#31279 = ORIENTED_EDGE('',*,*,#23983,.F.) ;
#31280 = ORIENTED_EDGE('',*,*,#23984,.F.) ;
#31281 = ORIENTED_EDGE('',*,*,#23985,.F.) ;
#31282 = ORIENTED_EDGE('',*,*,#23986,.F.) ;
#31283 = ORIENTED_EDGE('',*,*,#23987,.F.) ;
#31284 = ORIENTED_EDGE('',*,*,#23979,.T.) ;
#31285 = ORIENTED_EDGE('',*,*,#23988,.T.) ;
#31286 = ORIENTED_EDGE('',*,*,#23986,.T.) ;
#31287 = ORIENTED_EDGE('',*,*,#23853,.T.) ;
#31288 = ORIENTED_EDGE('',*,*,#23989,.F.) ;
#31289 = ORIENTED_EDGE('',*,*,#23990,.F.) ;
#31290 = ORIENTED_EDGE('',*,*,#23991,.F.) ;
#31291 = ORIENTED_EDGE('',*,*,#23992,.F.) ;
#31292 = ORIENTED_EDGE('',*,*,#23993,.F.) ;
#31293 = ORIENTED_EDGE('',*,*,#23994,.F.) ;
#31294 = ORIENTED_EDGE('',*,*,#23987,.T.) ;
#31295 = ORIENTED_EDGE('',*,*,#23995,.T.) ;
#31296 = ORIENTED_EDGE('',*,*,#23993,.T.) ;
#31297 = ORIENTED_EDGE('',*,*,#23996,.T.) ;
#31298 = ORIENTED_EDGE('',*,*,#23997,.F.) ;
#31299 = ORIENTED_EDGE('',*,*,#23998,.F.) ;
#31300 = ORIENTED_EDGE('',*,*,#23999,.F.) ;
#31301 = ORIENTED_EDGE('',*,*,#24000,.F.) ;
#31302 = ORIENTED_EDGE('',*,*,#24001,.F.) ;
#31303 = ORIENTED_EDGE('',*,*,#24002,.F.) ;
#31304 = ORIENTED_EDGE('',*,*,#23994,.T.) ;
#31305 = ORIENTED_EDGE('',*,*,#24003,.T.) ;
#31306 = ORIENTED_EDGE('',*,*,#24001,.T.) ;
#31307 = ORIENTED_EDGE('',*,*,#23857,.T.) ;
#31308 = ORIENTED_EDGE('',*,*,#24004,.F.) ;
#31309 = ORIENTED_EDGE('',*,*,#24005,.F.) ;
#31310 = ORIENTED_EDGE('',*,*,#24006,.F.) ;
#31311 = ORIENTED_EDGE('',*,*,#24007,.F.) ;
#31312 = ORIENTED_EDGE('',*,*,#24008,.F.) ;
#31313 = ORIENTED_EDGE('',*,*,#24009,.F.) ;
#31314 = ORIENTED_EDGE('',*,*,#24002,.T.) ;
#31315 = ORIENTED_EDGE('',*,*,#24010,.T.) ;
#31316 = ORIENTED_EDGE('',*,*,#24011,.T.) ;
#31317 = ORIENTED_EDGE('',*,*,#24008,.T.) ;
#31318 = ORIENTED_EDGE('',*,*,#24012,.T.) ;
#31319 = ORIENTED_EDGE('',*,*,#24013,.F.) ;
#31320 = ORIENTED_EDGE('',*,*,#24014,.F.) ;
#31321 = ORIENTED_EDGE('',*,*,#24015,.F.) ;
#31322 = ORIENTED_EDGE('',*,*,#24016,.F.) ;
#31323 = ORIENTED_EDGE('',*,*,#24017,.F.) ;
#31324 = ORIENTED_EDGE('',*,*,#24018,.F.) ;
#31325 = ORIENTED_EDGE('',*,*,#24009,.T.) ;
#31326 = ORIENTED_EDGE('',*,*,#24019,.T.) ;
#31327 = ORIENTED_EDGE('',*,*,#24017,.T.) ;
#31328 = ORIENTED_EDGE('',*,*,#23781,.T.) ;
#31329 = ORIENTED_EDGE('',*,*,#24020,.F.) ;
#31330 = ORIENTED_EDGE('',*,*,#24021,.F.) ;
#31331 = ORIENTED_EDGE('',*,*,#24022,.F.) ;
#31332 = ORIENTED_EDGE('',*,*,#24023,.F.) ;
#31333 = ORIENTED_EDGE('',*,*,#24024,.F.) ;
#31334 = ORIENTED_EDGE('',*,*,#24025,.F.) ;
#31335 = ORIENTED_EDGE('',*,*,#24018,.T.) ;
#31336 = ORIENTED_EDGE('',*,*,#24026,.T.) ;
#31337 = ORIENTED_EDGE('',*,*,#24024,.T.) ;
#31338 = ORIENTED_EDGE('',*,*,#24027,.T.) ;
#31339 = ORIENTED_EDGE('',*,*,#24028,.F.) ;
#31340 = ORIENTED_EDGE('',*,*,#24029,.F.) ;
#31341 = ORIENTED_EDGE('',*,*,#24030,.F.) ;
#31342 = ORIENTED_EDGE('',*,*,#24031,.F.) ;
#31343 = ORIENTED_EDGE('',*,*,#24032,.F.) ;
#31344 = ORIENTED_EDGE('',*,*,#24033,.F.) ;
#31345 = ORIENTED_EDGE('',*,*,#24025,.T.) ;
#31346 = ORIENTED_EDGE('',*,*,#24034,.T.) ;
#31347 = ORIENTED_EDGE('',*,*,#24032,.T.) ;
#31348 = ORIENTED_EDGE('',*,*,#23785,.T.) ;
#31349 = ORIENTED_EDGE('',*,*,#24035,.F.) ;
#31350 = ORIENTED_EDGE('',*,*,#24036,.F.) ;
#31351 = ORIENTED_EDGE('',*,*,#24037,.F.) ;
#31352 = ORIENTED_EDGE('',*,*,#24038,.F.) ;
#31353 = ORIENTED_EDGE('',*,*,#24039,.F.) ;
#31354 = ORIENTED_EDGE('',*,*,#24040,.F.) ;
#31355 = ORIENTED_EDGE('',*,*,#24033,.T.) ;
#31356 = ORIENTED_EDGE('',*,*,#24041,.T.) ;
#31357 = ORIENTED_EDGE('',*,*,#24039,.T.) ;
#31358 = ORIENTED_EDGE('',*,*,#24042,.T.) ;
#31359 = ORIENTED_EDGE('',*,*,#24043,.F.) ;
#31360 = ORIENTED_EDGE('',*,*,#24044,.F.) ;
#31361 = ORIENTED_EDGE('',*,*,#24045,.F.) ;
#31362 = ORIENTED_EDGE('',*,*,#24046,.F.) ;
#31363 = ORIENTED_EDGE('',*,*,#24047,.F.) ;
#31364 = ORIENTED_EDGE('',*,*,#24048,.F.) ;
#31365 = ORIENTED_EDGE('',*,*,#24040,.T.) ;
#31366 = ORIENTED_EDGE('',*,*,#24049,.T.) ;
#31367 = ORIENTED_EDGE('',*,*,#24047,.T.) ;
#31368 = ORIENTED_EDGE('',*,*,#23789,.T.) ;
#31369 = ORIENTED_EDGE('',*,*,#24050,.F.) ;
#31370 = ORIENTED_EDGE('',*,*,#24051,.F.) ;
#31371 = ORIENTED_EDGE('',*,*,#24052,.F.) ;
#31372 = ORIENTED_EDGE('',*,*,#24053,.F.) ;
#31373 = ORIENTED_EDGE('',*,*,#24054,.F.) ;
#31374 = ORIENTED_EDGE('',*,*,#24055,.F.) ;
#31375 = ORIENTED_EDGE('',*,*,#24048,.T.) ;
#31376 = ORIENTED_EDGE('',*,*,#24056,.T.) ;
#31377 = ORIENTED_EDGE('',*,*,#24054,.T.) ;
#31378 = ORIENTED_EDGE('',*,*,#24057,.T.) ;
#31379 = ORIENTED_EDGE('',*,*,#24058,.F.) ;
#31380 = ORIENTED_EDGE('',*,*,#24059,.F.) ;
#31381 = ORIENTED_EDGE('',*,*,#24060,.F.) ;
#31382 = ORIENTED_EDGE('',*,*,#24061,.F.) ;
#31383 = ORIENTED_EDGE('',*,*,#24062,.F.) ;
#31384 = ORIENTED_EDGE('',*,*,#24063,.F.) ;
#31385 = ORIENTED_EDGE('',*,*,#24055,.T.) ;
#31386 = ORIENTED_EDGE('',*,*,#24064,.T.) ;
#31387 = ORIENTED_EDGE('',*,*,#24062,.T.) ;
#31388 = ORIENTED_EDGE('',*,*,#23793,.T.) ;
#31389 = ORIENTED_EDGE('',*,*,#24065,.F.) ;
#31390 = ORIENTED_EDGE('',*,*,#24066,.F.) ;
#31391 = ORIENTED_EDGE('',*,*,#24067,.F.) ;
#31392 = ORIENTED_EDGE('',*,*,#24068,.F.) ;
#31393 = ORIENTED_EDGE('',*,*,#24069,.F.) ;
#31394 = ORIENTED_EDGE('',*,*,#24070,.F.) ;
#31395 = ORIENTED_EDGE('',*,*,#24063,.T.) ;
#31396 = ORIENTED_EDGE('',*,*,#24071,.T.) ;
#31397 = ORIENTED_EDGE('',*,*,#24069,.T.) ;
#31398 = ORIENTED_EDGE('',*,*,#24072,.T.) ;
#31399 = ORIENTED_EDGE('',*,*,#24073,.F.) ;
#31400 = ORIENTED_EDGE('',*,*,#24074,.F.) ;
#31401 = ORIENTED_EDGE('',*,*,#24075,.F.) ;
#31402 = ORIENTED_EDGE('',*,*,#24076,.F.) ;
#31403 = ORIENTED_EDGE('',*,*,#24077,.F.) ;
#31404 = ORIENTED_EDGE('',*,*,#24078,.F.) ;
#31405 = ORIENTED_EDGE('',*,*,#24070,.T.) ;
#31406 = ORIENTED_EDGE('',*,*,#24079,.T.) ;
#31407 = ORIENTED_EDGE('',*,*,#24077,.T.) ;
#31408 = ORIENTED_EDGE('',*,*,#23797,.T.) ;
#31409 = ORIENTED_EDGE('',*,*,#24080,.F.) ;
#31410 = ORIENTED_EDGE('',*,*,#24081,.F.) ;
#31411 = ORIENTED_EDGE('',*,*,#24082,.F.) ;
#31412 = ORIENTED_EDGE('',*,*,#24083,.F.) ;
#31413 = ORIENTED_EDGE('',*,*,#24084,.F.) ;
#31414 = ORIENTED_EDGE('',*,*,#24085,.F.) ;
#31415 = ORIENTED_EDGE('',*,*,#24078,.T.) ;
#31416 = ORIENTED_EDGE('',*,*,#24086,.T.) ;
#31417 = ORIENTED_EDGE('',*,*,#24084,.T.) ;
#31418 = ORIENTED_EDGE('',*,*,#24087,.T.) ;
#31419 = ORIENTED_EDGE('',*,*,#24088,.F.) ;
#31420 = ORIENTED_EDGE('',*,*,#24089,.F.) ;
#31421 = ORIENTED_EDGE('',*,*,#24090,.F.) ;
#31422 = ORIENTED_EDGE('',*,*,#24091,.F.) ;
#31423 = ORIENTED_EDGE('',*,*,#24092,.F.) ;
#31424 = ORIENTED_EDGE('',*,*,#24093,.F.) ;
#31425 = ORIENTED_EDGE('',*,*,#24085,.T.) ;
#31426 = ORIENTED_EDGE('',*,*,#24094,.T.) ;
#31427 = ORIENTED_EDGE('',*,*,#24092,.T.) ;
#31428 = ORIENTED_EDGE('',*,*,#23801,.T.) ;
#31429 = ORIENTED_EDGE('',*,*,#24095,.F.) ;
#31430 = ORIENTED_EDGE('',*,*,#24096,.F.) ;
#31431 = ORIENTED_EDGE('',*,*,#24097,.F.) ;
#31432 = ORIENTED_EDGE('',*,*,#24093,.T.) ;
#31433 = ORIENTED_EDGE('',*,*,#24098,.T.) ;
#31434 = ORIENTED_EDGE('',*,*,#24096,.T.) ;
#31435 = ORIENTED_EDGE('',*,*,#24099,.T.) ;
#31436 = ORIENTED_EDGE('',*,*,#24097,.T.) ;
#31437 = ORIENTED_EDGE('',*,*,#24100,.T.) ;
#31438 = ORIENTED_EDGE('',*,*,#24089,.T.) ;
#31439 = ORIENTED_EDGE('',*,*,#23805,.T.) ;
#31440 = ORIENTED_EDGE('',*,*,#24101,.T.) ;
#31441 = ORIENTED_EDGE('',*,*,#24095,.T.) ;
#31442 = ORIENTED_EDGE('',*,*,#23804,.T.) ;
#31443 = ORIENTED_EDGE('',*,*,#24102,.T.) ;
#31444 = ORIENTED_EDGE('',*,*,#23802,.T.) ;
#31445 = ORIENTED_EDGE('',*,*,#24091,.T.) ;
#31446 = ORIENTED_EDGE('',*,*,#24103,.T.) ;
#31447 = ORIENTED_EDGE('',*,*,#24104,.T.) ;
#31448 = ORIENTED_EDGE('',*,*,#24090,.T.) ;
#31449 = ORIENTED_EDGE('',*,*,#24105,.T.) ;
#31450 = ORIENTED_EDGE('',*,*,#24081,.T.) ;
#31451 = ORIENTED_EDGE('',*,*,#24106,.T.) ;
#31452 = ORIENTED_EDGE('',*,*,#23806,.T.) ;
#31453 = ORIENTED_EDGE('',*,*,#24088,.T.) ;
#31454 = ORIENTED_EDGE('',*,*,#24107,.T.) ;
#31455 = ORIENTED_EDGE('',*,*,#24108,.T.) ;
#31456 = ORIENTED_EDGE('',*,*,#23803,.T.) ;
#31457 = ORIENTED_EDGE('',*,*,#24104,.F.) ;
#31458 = ORIENTED_EDGE('',*,*,#24109,.T.) ;
#31459 = ORIENTED_EDGE('',*,*,#24110,.T.) ;
#31460 = ORIENTED_EDGE('',*,*,#24111,.T.) ;
#31461 = ORIENTED_EDGE('',*,*,#24102,.F.) ;
#31462 = ORIENTED_EDGE('',*,*,#24112,.T.) ;
#31463 = ORIENTED_EDGE('',*,*,#24083,.T.) ;
#31464 = ORIENTED_EDGE('',*,*,#23800,.T.) ;
#31465 = ORIENTED_EDGE('',*,*,#24113,.T.) ;
#31466 = ORIENTED_EDGE('',*,*,#24082,.T.) ;
#31467 = ORIENTED_EDGE('',*,*,#24114,.T.) ;
#31468 = ORIENTED_EDGE('',*,*,#24074,.T.) ;
#31469 = ORIENTED_EDGE('',*,*,#23809,.T.) ;
#31470 = ORIENTED_EDGE('',*,*,#24115,.T.) ;
#31471 = ORIENTED_EDGE('',*,*,#24080,.T.) ;
#31472 = ORIENTED_EDGE('',*,*,#23808,.T.) ;
#31473 = ORIENTED_EDGE('',*,*,#24116,.T.) ;
#31474 = ORIENTED_EDGE('',*,*,#23807,.T.) ;
#31475 = ORIENTED_EDGE('',*,*,#24108,.F.) ;
#31476 = ORIENTED_EDGE('',*,*,#24117,.T.) ;
#31477 = ORIENTED_EDGE('',*,*,#24118,.T.) ;
#31478 = ORIENTED_EDGE('',*,*,#24119,.T.) ;
#31479 = ORIENTED_EDGE('',*,*,#24116,.F.) ;
#31480 = ORIENTED_EDGE('',*,*,#23798,.T.) ;
#31481 = ORIENTED_EDGE('',*,*,#24076,.T.) ;
#31482 = ORIENTED_EDGE('',*,*,#24120,.T.) ;
#31483 = ORIENTED_EDGE('',*,*,#24121,.T.) ;
#31484 = ORIENTED_EDGE('',*,*,#23799,.T.) ;
#31485 = ORIENTED_EDGE('',*,*,#24121,.F.) ;
#31486 = ORIENTED_EDGE('',*,*,#24122,.T.) ;
#31487 = ORIENTED_EDGE('',*,*,#24123,.T.) ;
#31488 = ORIENTED_EDGE('',*,*,#24124,.T.) ;
#31489 = ORIENTED_EDGE('',*,*,#24113,.F.) ;
#31490 = ORIENTED_EDGE('',*,*,#24075,.T.) ;
#31491 = ORIENTED_EDGE('',*,*,#24125,.T.) ;
#31492 = ORIENTED_EDGE('',*,*,#24066,.T.) ;
#31493 = ORIENTED_EDGE('',*,*,#24126,.T.) ;
#31494 = ORIENTED_EDGE('',*,*,#23810,.T.) ;
#31495 = ORIENTED_EDGE('',*,*,#24073,.T.) ;
#31496 = ORIENTED_EDGE('',*,*,#24127,.T.) ;
#31497 = ORIENTED_EDGE('',*,*,#24128,.T.) ;
#31498 = ORIENTED_EDGE('',*,*,#24129,.T.) ;
#31499 = ORIENTED_EDGE('',*,*,#24068,.T.) ;
#31500 = ORIENTED_EDGE('',*,*,#23796,.T.) ;
#31501 = ORIENTED_EDGE('',*,*,#24130,.T.) ;
#31502 = ORIENTED_EDGE('',*,*,#24067,.T.) ;
#31503 = ORIENTED_EDGE('',*,*,#24131,.T.) ;
#31504 = ORIENTED_EDGE('',*,*,#24059,.T.) ;
#31505 = ORIENTED_EDGE('',*,*,#23813,.T.) ;
#31506 = ORIENTED_EDGE('',*,*,#24132,.T.) ;
#31507 = ORIENTED_EDGE('',*,*,#24065,.T.) ;
#31508 = ORIENTED_EDGE('',*,*,#23812,.T.) ;
#31509 = ORIENTED_EDGE('',*,*,#24133,.T.) ;
#31510 = ORIENTED_EDGE('',*,*,#23811,.T.) ;
#31511 = ORIENTED_EDGE('',*,*,#24128,.F.) ;
#31512 = ORIENTED_EDGE('',*,*,#24134,.T.) ;
#31513 = ORIENTED_EDGE('',*,*,#24135,.T.) ;
#31514 = ORIENTED_EDGE('',*,*,#24136,.T.) ;
#31515 = ORIENTED_EDGE('',*,*,#24133,.F.) ;
#31516 = ORIENTED_EDGE('',*,*,#23794,.T.) ;
#31517 = ORIENTED_EDGE('',*,*,#24061,.T.) ;
#31518 = ORIENTED_EDGE('',*,*,#24137,.T.) ;
#31519 = ORIENTED_EDGE('',*,*,#24138,.T.) ;
#31520 = ORIENTED_EDGE('',*,*,#23795,.T.) ;
#31521 = ORIENTED_EDGE('',*,*,#24138,.F.) ;
#31522 = ORIENTED_EDGE('',*,*,#24139,.T.) ;
#31523 = ORIENTED_EDGE('',*,*,#24140,.T.) ;
#31524 = ORIENTED_EDGE('',*,*,#24141,.T.) ;
#31525 = ORIENTED_EDGE('',*,*,#24130,.F.) ;
#31526 = ORIENTED_EDGE('',*,*,#24060,.T.) ;
#31527 = ORIENTED_EDGE('',*,*,#24142,.T.) ;
#31528 = ORIENTED_EDGE('',*,*,#24051,.T.) ;
#31529 = ORIENTED_EDGE('',*,*,#24143,.T.) ;
#31530 = ORIENTED_EDGE('',*,*,#23814,.T.) ;
#31531 = ORIENTED_EDGE('',*,*,#24058,.T.) ;
#31532 = ORIENTED_EDGE('',*,*,#24144,.T.) ;
#31533 = ORIENTED_EDGE('',*,*,#24145,.T.) ;
#31534 = ORIENTED_EDGE('',*,*,#24146,.T.) ;
#31535 = ORIENTED_EDGE('',*,*,#24053,.T.) ;
#31536 = ORIENTED_EDGE('',*,*,#23792,.T.) ;
#31537 = ORIENTED_EDGE('',*,*,#24147,.T.) ;
#31538 = ORIENTED_EDGE('',*,*,#24052,.T.) ;
#31539 = ORIENTED_EDGE('',*,*,#24148,.T.) ;
#31540 = ORIENTED_EDGE('',*,*,#24044,.T.) ;
#31541 = ORIENTED_EDGE('',*,*,#23817,.T.) ;
#31542 = ORIENTED_EDGE('',*,*,#24149,.T.) ;
#31543 = ORIENTED_EDGE('',*,*,#24050,.T.) ;
#31544 = ORIENTED_EDGE('',*,*,#23816,.T.) ;
#31545 = ORIENTED_EDGE('',*,*,#24150,.T.) ;
#31546 = ORIENTED_EDGE('',*,*,#23815,.T.) ;
#31547 = ORIENTED_EDGE('',*,*,#24145,.F.) ;
#31548 = ORIENTED_EDGE('',*,*,#24151,.T.) ;
#31549 = ORIENTED_EDGE('',*,*,#24152,.T.) ;
#31550 = ORIENTED_EDGE('',*,*,#24153,.T.) ;
#31551 = ORIENTED_EDGE('',*,*,#24150,.F.) ;
#31552 = ORIENTED_EDGE('',*,*,#23790,.T.) ;
#31553 = ORIENTED_EDGE('',*,*,#24046,.T.) ;
#31554 = ORIENTED_EDGE('',*,*,#24154,.T.) ;
#31555 = ORIENTED_EDGE('',*,*,#24155,.T.) ;
#31556 = ORIENTED_EDGE('',*,*,#23791,.T.) ;
#31557 = ORIENTED_EDGE('',*,*,#24155,.F.) ;
#31558 = ORIENTED_EDGE('',*,*,#24156,.T.) ;
#31559 = ORIENTED_EDGE('',*,*,#24157,.T.) ;
#31560 = ORIENTED_EDGE('',*,*,#24158,.T.) ;
#31561 = ORIENTED_EDGE('',*,*,#24147,.F.) ;
#31562 = ORIENTED_EDGE('',*,*,#24045,.T.) ;
#31563 = ORIENTED_EDGE('',*,*,#24159,.T.) ;
#31564 = ORIENTED_EDGE('',*,*,#24036,.T.) ;
#31565 = ORIENTED_EDGE('',*,*,#24160,.T.) ;
#31566 = ORIENTED_EDGE('',*,*,#23818,.T.) ;
#31567 = ORIENTED_EDGE('',*,*,#24043,.T.) ;
#31568 = ORIENTED_EDGE('',*,*,#24161,.T.) ;
#31569 = ORIENTED_EDGE('',*,*,#24162,.T.) ;
#31570 = ORIENTED_EDGE('',*,*,#24163,.T.) ;
#31571 = ORIENTED_EDGE('',*,*,#24038,.T.) ;
#31572 = ORIENTED_EDGE('',*,*,#23788,.T.) ;
#31573 = ORIENTED_EDGE('',*,*,#24164,.T.) ;
#31574 = ORIENTED_EDGE('',*,*,#24037,.T.) ;
#31575 = ORIENTED_EDGE('',*,*,#24165,.T.) ;
#31576 = ORIENTED_EDGE('',*,*,#24029,.T.) ;
#31577 = ORIENTED_EDGE('',*,*,#23821,.T.) ;
#31578 = ORIENTED_EDGE('',*,*,#24166,.T.) ;
#31579 = ORIENTED_EDGE('',*,*,#24035,.T.) ;
#31580 = ORIENTED_EDGE('',*,*,#23820,.T.) ;
#31581 = ORIENTED_EDGE('',*,*,#24167,.T.) ;
#31582 = ORIENTED_EDGE('',*,*,#23819,.T.) ;
#31583 = ORIENTED_EDGE('',*,*,#24162,.F.) ;
#31584 = ORIENTED_EDGE('',*,*,#24168,.T.) ;
#31585 = ORIENTED_EDGE('',*,*,#24169,.T.) ;
#31586 = ORIENTED_EDGE('',*,*,#24170,.T.) ;
#31587 = ORIENTED_EDGE('',*,*,#24167,.F.) ;
#31588 = ORIENTED_EDGE('',*,*,#23786,.T.) ;
#31589 = ORIENTED_EDGE('',*,*,#24031,.T.) ;
#31590 = ORIENTED_EDGE('',*,*,#24171,.T.) ;
#31591 = ORIENTED_EDGE('',*,*,#24172,.T.) ;
#31592 = ORIENTED_EDGE('',*,*,#23787,.T.) ;
#31593 = ORIENTED_EDGE('',*,*,#24172,.F.) ;
#31594 = ORIENTED_EDGE('',*,*,#24173,.T.) ;
#31595 = ORIENTED_EDGE('',*,*,#24174,.T.) ;
#31596 = ORIENTED_EDGE('',*,*,#24175,.T.) ;
#31597 = ORIENTED_EDGE('',*,*,#24164,.F.) ;
#31598 = ORIENTED_EDGE('',*,*,#24030,.T.) ;
#31599 = ORIENTED_EDGE('',*,*,#24176,.T.) ;
#31600 = ORIENTED_EDGE('',*,*,#24021,.T.) ;
#31601 = ORIENTED_EDGE('',*,*,#24177,.T.) ;
#31602 = ORIENTED_EDGE('',*,*,#23822,.T.) ;
#31603 = ORIENTED_EDGE('',*,*,#24028,.T.) ;
#31604 = ORIENTED_EDGE('',*,*,#24178,.T.) ;
#31605 = ORIENTED_EDGE('',*,*,#24179,.T.) ;
#31606 = ORIENTED_EDGE('',*,*,#24180,.T.) ;
#31607 = ORIENTED_EDGE('',*,*,#24023,.T.) ;
#31608 = ORIENTED_EDGE('',*,*,#23784,.T.) ;
#31609 = ORIENTED_EDGE('',*,*,#24181,.T.) ;
#31610 = ORIENTED_EDGE('',*,*,#24022,.T.) ;
#31611 = ORIENTED_EDGE('',*,*,#24182,.T.) ;
#31612 = ORIENTED_EDGE('',*,*,#24014,.T.) ;
#31613 = ORIENTED_EDGE('',*,*,#23825,.T.) ;
#31614 = ORIENTED_EDGE('',*,*,#24183,.T.) ;
#31615 = ORIENTED_EDGE('',*,*,#24020,.T.) ;
#31616 = ORIENTED_EDGE('',*,*,#23824,.T.) ;
#31617 = ORIENTED_EDGE('',*,*,#24184,.T.) ;
#31618 = ORIENTED_EDGE('',*,*,#23823,.T.) ;
#31619 = ORIENTED_EDGE('',*,*,#24179,.F.) ;
#31620 = ORIENTED_EDGE('',*,*,#24185,.T.) ;
#31621 = ORIENTED_EDGE('',*,*,#24186,.T.) ;
#31622 = ORIENTED_EDGE('',*,*,#24187,.T.) ;
#31623 = ORIENTED_EDGE('',*,*,#24184,.F.) ;
#31624 = ORIENTED_EDGE('',*,*,#23782,.T.) ;
#31625 = ORIENTED_EDGE('',*,*,#24016,.T.) ;
#31626 = ORIENTED_EDGE('',*,*,#24188,.T.) ;
#31627 = ORIENTED_EDGE('',*,*,#24189,.T.) ;
#31628 = ORIENTED_EDGE('',*,*,#23783,.T.) ;
#31629 = ORIENTED_EDGE('',*,*,#24189,.F.) ;
#31630 = ORIENTED_EDGE('',*,*,#24190,.T.) ;
#31631 = ORIENTED_EDGE('',*,*,#24191,.T.) ;
#31632 = ORIENTED_EDGE('',*,*,#24192,.T.) ;
#31633 = ORIENTED_EDGE('',*,*,#24181,.F.) ;
#31634 = ORIENTED_EDGE('',*,*,#24015,.T.) ;
#31635 = ORIENTED_EDGE('',*,*,#24193,.T.) ;
#31636 = ORIENTED_EDGE('',*,*,#24005,.T.) ;
#31637 = ORIENTED_EDGE('',*,*,#24194,.T.) ;
#31638 = ORIENTED_EDGE('',*,*,#23826,.T.) ;
#31639 = ORIENTED_EDGE('',*,*,#24013,.T.) ;
#31640 = ORIENTED_EDGE('',*,*,#24195,.T.) ;
#31641 = ORIENTED_EDGE('',*,*,#24196,.T.) ;
#31642 = ORIENTED_EDGE('',*,*,#24197,.T.) ;
#31643 = ORIENTED_EDGE('',*,*,#24007,.T.) ;
#31644 = ORIENTED_EDGE('',*,*,#23780,.T.) ;
#31645 = ORIENTED_EDGE('',*,*,#24198,.T.) ;
#31646 = ORIENTED_EDGE('',*,*,#24006,.T.) ;
#31647 = ORIENTED_EDGE('',*,*,#24199,.T.) ;
#31648 = ORIENTED_EDGE('',*,*,#23998,.T.) ;
#31649 = ORIENTED_EDGE('',*,*,#23829,.T.) ;
#31650 = ORIENTED_EDGE('',*,*,#24200,.T.) ;
#31651 = ORIENTED_EDGE('',*,*,#24004,.T.) ;
#31652 = ORIENTED_EDGE('',*,*,#23828,.T.) ;
#31653 = ORIENTED_EDGE('',*,*,#24201,.T.) ;
#31654 = ORIENTED_EDGE('',*,*,#23827,.T.) ;
#31655 = ORIENTED_EDGE('',*,*,#24196,.F.) ;
#31656 = ORIENTED_EDGE('',*,*,#24202,.T.) ;
#31657 = ORIENTED_EDGE('',*,*,#24203,.T.) ;
#31658 = ORIENTED_EDGE('',*,*,#24204,.T.) ;
#31659 = ORIENTED_EDGE('',*,*,#24201,.F.) ;
#31660 = ORIENTED_EDGE('',*,*,#23858,.T.) ;
#31661 = ORIENTED_EDGE('',*,*,#24000,.T.) ;
#31662 = ORIENTED_EDGE('',*,*,#24205,.T.) ;
#31663 = ORIENTED_EDGE('',*,*,#24206,.T.) ;
#31664 = ORIENTED_EDGE('',*,*,#23779,.T.) ;
#31665 = ORIENTED_EDGE('',*,*,#23859,.T.) ;
#31666 = ORIENTED_EDGE('',*,*,#24206,.F.) ;
#31667 = ORIENTED_EDGE('',*,*,#24207,.T.) ;
#31668 = ORIENTED_EDGE('',*,*,#24208,.T.) ;
#31669 = ORIENTED_EDGE('',*,*,#24209,.T.) ;
#31670 = ORIENTED_EDGE('',*,*,#24198,.F.) ;
#31671 = ORIENTED_EDGE('',*,*,#23999,.T.) ;
#31672 = ORIENTED_EDGE('',*,*,#24210,.T.) ;
#31673 = ORIENTED_EDGE('',*,*,#23990,.T.) ;
#31674 = ORIENTED_EDGE('',*,*,#24211,.T.) ;
#31675 = ORIENTED_EDGE('',*,*,#23830,.T.) ;
#31676 = ORIENTED_EDGE('',*,*,#23997,.T.) ;
#31677 = ORIENTED_EDGE('',*,*,#24212,.T.) ;
#31678 = ORIENTED_EDGE('',*,*,#24213,.T.) ;
#31679 = ORIENTED_EDGE('',*,*,#24214,.T.) ;
#31680 = ORIENTED_EDGE('',*,*,#23992,.T.) ;
#31681 = ORIENTED_EDGE('',*,*,#23856,.T.) ;
#31682 = ORIENTED_EDGE('',*,*,#24215,.T.) ;
#31683 = ORIENTED_EDGE('',*,*,#23991,.T.) ;
#31684 = ORIENTED_EDGE('',*,*,#24216,.T.) ;
#31685 = ORIENTED_EDGE('',*,*,#23983,.T.) ;
#31686 = ORIENTED_EDGE('',*,*,#23833,.T.) ;
#31687 = ORIENTED_EDGE('',*,*,#24217,.T.) ;
#31688 = ORIENTED_EDGE('',*,*,#23989,.T.) ;
#31689 = ORIENTED_EDGE('',*,*,#23832,.T.) ;
#31690 = ORIENTED_EDGE('',*,*,#24218,.T.) ;
#31691 = ORIENTED_EDGE('',*,*,#23831,.T.) ;
#31692 = ORIENTED_EDGE('',*,*,#24213,.F.) ;
#31693 = ORIENTED_EDGE('',*,*,#24219,.T.) ;
#31694 = ORIENTED_EDGE('',*,*,#24220,.T.) ;
#31695 = ORIENTED_EDGE('',*,*,#24221,.T.) ;
#31696 = ORIENTED_EDGE('',*,*,#24218,.F.) ;
#31697 = ORIENTED_EDGE('',*,*,#23854,.T.) ;
#31698 = ORIENTED_EDGE('',*,*,#23985,.T.) ;
#31699 = ORIENTED_EDGE('',*,*,#24222,.T.) ;
#31700 = ORIENTED_EDGE('',*,*,#24223,.T.) ;
#31701 = ORIENTED_EDGE('',*,*,#23855,.T.) ;
#31702 = ORIENTED_EDGE('',*,*,#24223,.F.) ;
#31703 = ORIENTED_EDGE('',*,*,#24224,.T.) ;
#31704 = ORIENTED_EDGE('',*,*,#24225,.T.) ;
#31705 = ORIENTED_EDGE('',*,*,#24226,.T.) ;
#31706 = ORIENTED_EDGE('',*,*,#24215,.F.) ;
#31707 = ORIENTED_EDGE('',*,*,#23984,.T.) ;
#31708 = ORIENTED_EDGE('',*,*,#24227,.T.) ;
#31709 = ORIENTED_EDGE('',*,*,#23975,.T.) ;
#31710 = ORIENTED_EDGE('',*,*,#24228,.T.) ;
#31711 = ORIENTED_EDGE('',*,*,#23834,.T.) ;
#31712 = ORIENTED_EDGE('',*,*,#23982,.T.) ;
#31713 = ORIENTED_EDGE('',*,*,#24229,.T.) ;
#31714 = ORIENTED_EDGE('',*,*,#24230,.T.) ;
#31715 = ORIENTED_EDGE('',*,*,#24231,.T.) ;
#31716 = ORIENTED_EDGE('',*,*,#23977,.T.) ;
#31717 = ORIENTED_EDGE('',*,*,#23852,.T.) ;
#31718 = ORIENTED_EDGE('',*,*,#24232,.T.) ;
#31719 = ORIENTED_EDGE('',*,*,#23976,.T.) ;
#31720 = ORIENTED_EDGE('',*,*,#24233,.T.) ;
#31721 = ORIENTED_EDGE('',*,*,#23968,.T.) ;
#31722 = ORIENTED_EDGE('',*,*,#23837,.T.) ;
#31723 = ORIENTED_EDGE('',*,*,#24234,.T.) ;
#31724 = ORIENTED_EDGE('',*,*,#23974,.T.) ;
#31725 = ORIENTED_EDGE('',*,*,#23836,.T.) ;
#31726 = ORIENTED_EDGE('',*,*,#24235,.T.) ;
#31727 = ORIENTED_EDGE('',*,*,#23835,.T.) ;
#31728 = ORIENTED_EDGE('',*,*,#24230,.F.) ;
#31729 = ORIENTED_EDGE('',*,*,#24236,.T.) ;
#31730 = ORIENTED_EDGE('',*,*,#24237,.T.) ;
#31731 = ORIENTED_EDGE('',*,*,#24238,.T.) ;
#31732 = ORIENTED_EDGE('',*,*,#24235,.F.) ;
#31733 = ORIENTED_EDGE('',*,*,#23850,.T.) ;
#31734 = ORIENTED_EDGE('',*,*,#23970,.T.) ;
#31735 = ORIENTED_EDGE('',*,*,#24239,.T.) ;
#31736 = ORIENTED_EDGE('',*,*,#24240,.T.) ;
#31737 = ORIENTED_EDGE('',*,*,#23851,.T.) ;
#31738 = ORIENTED_EDGE('',*,*,#24240,.F.) ;
#31739 = ORIENTED_EDGE('',*,*,#24241,.T.) ;
#31740 = ORIENTED_EDGE('',*,*,#24242,.T.) ;
#31741 = ORIENTED_EDGE('',*,*,#24243,.T.) ;
#31742 = ORIENTED_EDGE('',*,*,#24232,.F.) ;
#31743 = ORIENTED_EDGE('',*,*,#23969,.T.) ;
#31744 = ORIENTED_EDGE('',*,*,#24244,.T.) ;
#31745 = ORIENTED_EDGE('',*,*,#23960,.T.) ;
#31746 = ORIENTED_EDGE('',*,*,#24245,.T.) ;
#31747 = ORIENTED_EDGE('',*,*,#23838,.T.) ;
#31748 = ORIENTED_EDGE('',*,*,#23967,.T.) ;
#31749 = ORIENTED_EDGE('',*,*,#24246,.T.) ;
#31750 = ORIENTED_EDGE('',*,*,#24247,.T.) ;
#31751 = ORIENTED_EDGE('',*,*,#24248,.T.) ;
#31752 = ORIENTED_EDGE('',*,*,#23962,.T.) ;
#31753 = ORIENTED_EDGE('',*,*,#23848,.T.) ;
#31754 = ORIENTED_EDGE('',*,*,#24249,.T.) ;
#31755 = ORIENTED_EDGE('',*,*,#23961,.T.) ;
#31756 = ORIENTED_EDGE('',*,*,#24250,.T.) ;
#31757 = ORIENTED_EDGE('',*,*,#23953,.T.) ;
#31758 = ORIENTED_EDGE('',*,*,#23841,.T.) ;
#31759 = ORIENTED_EDGE('',*,*,#24251,.T.) ;
#31760 = ORIENTED_EDGE('',*,*,#23959,.T.) ;
#31761 = ORIENTED_EDGE('',*,*,#23840,.T.) ;
#31762 = ORIENTED_EDGE('',*,*,#24252,.T.) ;
#31763 = ORIENTED_EDGE('',*,*,#23839,.T.) ;
#31764 = ORIENTED_EDGE('',*,*,#24247,.F.) ;
#31765 = ORIENTED_EDGE('',*,*,#24253,.T.) ;
#31766 = ORIENTED_EDGE('',*,*,#24254,.T.) ;
#31767 = ORIENTED_EDGE('',*,*,#24255,.T.) ;
#31768 = ORIENTED_EDGE('',*,*,#24252,.F.) ;
#31769 = ORIENTED_EDGE('',*,*,#23846,.T.) ;
#31770 = ORIENTED_EDGE('',*,*,#23955,.T.) ;
#31771 = ORIENTED_EDGE('',*,*,#24256,.T.) ;
#31772 = ORIENTED_EDGE('',*,*,#24257,.T.) ;
#31773 = ORIENTED_EDGE('',*,*,#23847,.T.) ;
#31774 = ORIENTED_EDGE('',*,*,#24257,.F.) ;
#31775 = ORIENTED_EDGE('',*,*,#24258,.T.) ;
#31776 = ORIENTED_EDGE('',*,*,#24259,.T.) ;
#31777 = ORIENTED_EDGE('',*,*,#24260,.T.) ;
#31778 = ORIENTED_EDGE('',*,*,#24249,.F.) ;
#31779 = ORIENTED_EDGE('',*,*,#23954,.T.) ;
#31780 = ORIENTED_EDGE('',*,*,#24261,.T.) ;
#31781 = ORIENTED_EDGE('',*,*,#23950,.T.) ;
#31782 = ORIENTED_EDGE('',*,*,#24262,.T.) ;
#31783 = ORIENTED_EDGE('',*,*,#23842,.T.) ;
#31784 = ORIENTED_EDGE('',*,*,#23952,.T.) ;
#31785 = ORIENTED_EDGE('',*,*,#24263,.T.) ;
#31786 = ORIENTED_EDGE('',*,*,#24264,.T.) ;
#31787 = ORIENTED_EDGE('',*,*,#24265,.T.) ;
#31788 = ORIENTED_EDGE('',*,*,#23949,.T.) ;
#31789 = ORIENTED_EDGE('',*,*,#23844,.T.) ;
#31790 = ORIENTED_EDGE('',*,*,#24266,.T.) ;
#31791 = ORIENTED_EDGE('',*,*,#23843,.T.) ;
#31792 = ORIENTED_EDGE('',*,*,#24264,.F.) ;
#31793 = ORIENTED_EDGE('',*,*,#24267,.T.) ;
#31794 = ORIENTED_EDGE('',*,*,#24268,.T.) ;
#31795 = ORIENTED_EDGE('',*,*,#24269,.T.) ;
#31796 = ORIENTED_EDGE('',*,*,#24266,.F.) ;
#31797 = ORIENTED_EDGE('',*,*,#24256,.F.) ;
#31798 = ORIENTED_EDGE('',*,*,#23966,.F.) ;
#31799 = ORIENTED_EDGE('',*,*,#24248,.F.) ;
#31800 = ORIENTED_EDGE('',*,*,#24260,.F.) ;
#31801 = ORIENTED_EDGE('',*,*,#24270,.F.) ;
#31802 = ORIENTED_EDGE('',*,*,#24258,.F.) ;
#31803 = ORIENTED_EDGE('',*,*,#24239,.F.) ;
#31804 = ORIENTED_EDGE('',*,*,#23981,.F.) ;
#31805 = ORIENTED_EDGE('',*,*,#24231,.F.) ;
#31806 = ORIENTED_EDGE('',*,*,#24243,.F.) ;
#31807 = ORIENTED_EDGE('',*,*,#24271,.F.) ;
#31808 = ORIENTED_EDGE('',*,*,#24241,.F.) ;
#31809 = ORIENTED_EDGE('',*,*,#24222,.F.) ;
#31810 = ORIENTED_EDGE('',*,*,#23996,.F.) ;
#31811 = ORIENTED_EDGE('',*,*,#24214,.F.) ;
#31812 = ORIENTED_EDGE('',*,*,#24226,.F.) ;
#31813 = ORIENTED_EDGE('',*,*,#24272,.F.) ;
#31814 = ORIENTED_EDGE('',*,*,#24224,.F.) ;
#31815 = ORIENTED_EDGE('',*,*,#24205,.F.) ;
#31816 = ORIENTED_EDGE('',*,*,#24012,.F.) ;
#31817 = ORIENTED_EDGE('',*,*,#24197,.F.) ;
#31818 = ORIENTED_EDGE('',*,*,#24209,.F.) ;
#31819 = ORIENTED_EDGE('',*,*,#24273,.F.) ;
#31820 = ORIENTED_EDGE('',*,*,#24207,.F.) ;
#31821 = ORIENTED_EDGE('',*,*,#24188,.F.) ;
#31822 = ORIENTED_EDGE('',*,*,#24027,.F.) ;
#31823 = ORIENTED_EDGE('',*,*,#24180,.F.) ;
#31824 = ORIENTED_EDGE('',*,*,#24192,.F.) ;
#31825 = ORIENTED_EDGE('',*,*,#24274,.F.) ;
#31826 = ORIENTED_EDGE('',*,*,#24190,.F.) ;
#31827 = ORIENTED_EDGE('',*,*,#24171,.F.) ;
#31828 = ORIENTED_EDGE('',*,*,#24042,.F.) ;
#31829 = ORIENTED_EDGE('',*,*,#24163,.F.) ;
#31830 = ORIENTED_EDGE('',*,*,#24175,.F.) ;
#31831 = ORIENTED_EDGE('',*,*,#24275,.F.) ;
#31832 = ORIENTED_EDGE('',*,*,#24173,.F.) ;
#31833 = ORIENTED_EDGE('',*,*,#24154,.F.) ;
#31834 = ORIENTED_EDGE('',*,*,#24057,.F.) ;
#31835 = ORIENTED_EDGE('',*,*,#24146,.F.) ;
#31836 = ORIENTED_EDGE('',*,*,#24158,.F.) ;
#31837 = ORIENTED_EDGE('',*,*,#24276,.F.) ;
#31838 = ORIENTED_EDGE('',*,*,#24156,.F.) ;
#31839 = ORIENTED_EDGE('',*,*,#24137,.F.) ;
#31840 = ORIENTED_EDGE('',*,*,#24072,.F.) ;
#31841 = ORIENTED_EDGE('',*,*,#24129,.F.) ;
#31842 = ORIENTED_EDGE('',*,*,#24141,.F.) ;
#31843 = ORIENTED_EDGE('',*,*,#24277,.F.) ;
#31844 = ORIENTED_EDGE('',*,*,#24139,.F.) ;
#31845 = ORIENTED_EDGE('',*,*,#24120,.F.) ;
#31846 = ORIENTED_EDGE('',*,*,#24087,.F.) ;
#31847 = ORIENTED_EDGE('',*,*,#24112,.F.) ;
#31848 = ORIENTED_EDGE('',*,*,#24124,.F.) ;
#31849 = ORIENTED_EDGE('',*,*,#24278,.F.) ;
#31850 = ORIENTED_EDGE('',*,*,#24122,.F.) ;
#31851 = ORIENTED_EDGE('',*,*,#24103,.F.) ;
#31852 = ORIENTED_EDGE('',*,*,#24099,.F.) ;
#31853 = ORIENTED_EDGE('',*,*,#24101,.F.) ;
#31854 = ORIENTED_EDGE('',*,*,#24111,.F.) ;
#31855 = ORIENTED_EDGE('',*,*,#24279,.F.) ;
#31856 = ORIENTED_EDGE('',*,*,#24109,.F.) ;
#31857 = ORIENTED_EDGE('',*,*,#24107,.F.) ;
#31858 = ORIENTED_EDGE('',*,*,#24106,.F.) ;
#31859 = ORIENTED_EDGE('',*,*,#24115,.F.) ;
#31860 = ORIENTED_EDGE('',*,*,#24119,.F.) ;
#31861 = ORIENTED_EDGE('',*,*,#24280,.F.) ;
#31862 = ORIENTED_EDGE('',*,*,#24117,.F.) ;
#31863 = ORIENTED_EDGE('',*,*,#24127,.F.) ;
#31864 = ORIENTED_EDGE('',*,*,#24126,.F.) ;
#31865 = ORIENTED_EDGE('',*,*,#24132,.F.) ;
#31866 = ORIENTED_EDGE('',*,*,#24136,.F.) ;
#31867 = ORIENTED_EDGE('',*,*,#24281,.F.) ;
#31868 = ORIENTED_EDGE('',*,*,#24134,.F.) ;
#31869 = ORIENTED_EDGE('',*,*,#24144,.F.) ;
#31870 = ORIENTED_EDGE('',*,*,#24143,.F.) ;
#31871 = ORIENTED_EDGE('',*,*,#24149,.F.) ;
#31872 = ORIENTED_EDGE('',*,*,#24153,.F.) ;
#31873 = ORIENTED_EDGE('',*,*,#24282,.F.) ;
#31874 = ORIENTED_EDGE('',*,*,#24151,.F.) ;
#31875 = ORIENTED_EDGE('',*,*,#24161,.F.) ;
#31876 = ORIENTED_EDGE('',*,*,#24160,.F.) ;
#31877 = ORIENTED_EDGE('',*,*,#24166,.F.) ;
#31878 = ORIENTED_EDGE('',*,*,#24170,.F.) ;
#31879 = ORIENTED_EDGE('',*,*,#24283,.F.) ;
#31880 = ORIENTED_EDGE('',*,*,#24168,.F.) ;
#31881 = ORIENTED_EDGE('',*,*,#24178,.F.) ;
#31882 = ORIENTED_EDGE('',*,*,#24177,.F.) ;
#31883 = ORIENTED_EDGE('',*,*,#24183,.F.) ;
#31884 = ORIENTED_EDGE('',*,*,#24187,.F.) ;
#31885 = ORIENTED_EDGE('',*,*,#24284,.F.) ;
#31886 = ORIENTED_EDGE('',*,*,#24185,.F.) ;
#31887 = ORIENTED_EDGE('',*,*,#24195,.F.) ;
#31888 = ORIENTED_EDGE('',*,*,#24194,.F.) ;
#31889 = ORIENTED_EDGE('',*,*,#24200,.F.) ;
#31890 = ORIENTED_EDGE('',*,*,#24204,.F.) ;
#31891 = ORIENTED_EDGE('',*,*,#24285,.F.) ;
#31892 = ORIENTED_EDGE('',*,*,#24202,.F.) ;
#31893 = ORIENTED_EDGE('',*,*,#24212,.F.) ;
#31894 = ORIENTED_EDGE('',*,*,#24211,.F.) ;
#31895 = ORIENTED_EDGE('',*,*,#24217,.F.) ;
#31896 = ORIENTED_EDGE('',*,*,#24221,.F.) ;
#31897 = ORIENTED_EDGE('',*,*,#24286,.F.) ;
#31898 = ORIENTED_EDGE('',*,*,#24219,.F.) ;
#31899 = ORIENTED_EDGE('',*,*,#24229,.F.) ;
#31900 = ORIENTED_EDGE('',*,*,#24228,.F.) ;
#31901 = ORIENTED_EDGE('',*,*,#24234,.F.) ;
#31902 = ORIENTED_EDGE('',*,*,#24238,.F.) ;
#31903 = ORIENTED_EDGE('',*,*,#24287,.F.) ;
#31904 = ORIENTED_EDGE('',*,*,#24236,.F.) ;
#31905 = ORIENTED_EDGE('',*,*,#24246,.F.) ;
#31906 = ORIENTED_EDGE('',*,*,#24245,.F.) ;
#31907 = ORIENTED_EDGE('',*,*,#24251,.F.) ;
#31908 = ORIENTED_EDGE('',*,*,#24255,.F.) ;
#31909 = ORIENTED_EDGE('',*,*,#24288,.F.) ;
#31910 = ORIENTED_EDGE('',*,*,#24253,.F.) ;
#31911 = ORIENTED_EDGE('',*,*,#24263,.F.) ;
#31912 = ORIENTED_EDGE('',*,*,#24262,.F.) ;
#31913 = ORIENTED_EDGE('',*,*,#24265,.F.) ;
#31914 = ORIENTED_EDGE('',*,*,#24269,.F.) ;
#31915 = ORIENTED_EDGE('',*,*,#24289,.F.) ;
#31916 = ORIENTED_EDGE('',*,*,#24267,.F.) ;
#31917 = ORIENTED_EDGE('',*,*,#24010,.F.) ;
#31918 = ORIENTED_EDGE('',*,*,#24003,.F.) ;
#31919 = ORIENTED_EDGE('',*,*,#23995,.F.) ;
#31920 = ORIENTED_EDGE('',*,*,#23988,.F.) ;
#31921 = ORIENTED_EDGE('',*,*,#23980,.F.) ;
#31922 = ORIENTED_EDGE('',*,*,#23973,.F.) ;
#31923 = ORIENTED_EDGE('',*,*,#23965,.F.) ;
#31924 = ORIENTED_EDGE('',*,*,#23958,.F.) ;
#31925 = ORIENTED_EDGE('',*,*,#24261,.F.) ;
#31926 = ORIENTED_EDGE('',*,*,#24250,.F.) ;
#31927 = ORIENTED_EDGE('',*,*,#24244,.F.) ;
#31928 = ORIENTED_EDGE('',*,*,#24233,.F.) ;
#31929 = ORIENTED_EDGE('',*,*,#24227,.F.) ;
#31930 = ORIENTED_EDGE('',*,*,#24216,.F.) ;
#31931 = ORIENTED_EDGE('',*,*,#24210,.F.) ;
#31932 = ORIENTED_EDGE('',*,*,#24199,.F.) ;
#31933 = ORIENTED_EDGE('',*,*,#24193,.F.) ;
#31934 = ORIENTED_EDGE('',*,*,#24182,.F.) ;
#31935 = ORIENTED_EDGE('',*,*,#24176,.F.) ;
#31936 = ORIENTED_EDGE('',*,*,#24165,.F.) ;
#31937 = ORIENTED_EDGE('',*,*,#24159,.F.) ;
#31938 = ORIENTED_EDGE('',*,*,#24148,.F.) ;
#31939 = ORIENTED_EDGE('',*,*,#24142,.F.) ;
#31940 = ORIENTED_EDGE('',*,*,#24131,.F.) ;
#31941 = ORIENTED_EDGE('',*,*,#24125,.F.) ;
#31942 = ORIENTED_EDGE('',*,*,#24114,.F.) ;
#31943 = ORIENTED_EDGE('',*,*,#24105,.F.) ;
#31944 = ORIENTED_EDGE('',*,*,#24100,.F.) ;
#31945 = ORIENTED_EDGE('',*,*,#24098,.F.) ;
#31946 = ORIENTED_EDGE('',*,*,#24094,.F.) ;
#31947 = ORIENTED_EDGE('',*,*,#24086,.F.) ;
#31948 = ORIENTED_EDGE('',*,*,#24079,.F.) ;
#31949 = ORIENTED_EDGE('',*,*,#24071,.F.) ;
#31950 = ORIENTED_EDGE('',*,*,#24064,.F.) ;
#31951 = ORIENTED_EDGE('',*,*,#24056,.F.) ;
#31952 = ORIENTED_EDGE('',*,*,#24049,.F.) ;
#31953 = ORIENTED_EDGE('',*,*,#24041,.F.) ;
#31954 = ORIENTED_EDGE('',*,*,#24034,.F.) ;
#31955 = ORIENTED_EDGE('',*,*,#24026,.F.) ;
#31956 = ORIENTED_EDGE('',*,*,#24019,.F.) ;
#31957 = ORIENTED_EDGE('',*,*,#24011,.F.) ;
#31958 = ORIENTED_EDGE('',*,*,#24290,.T.) ;
#31959 = ORIENTED_EDGE('',*,*,#24291,.F.) ;
#31960 = ORIENTED_EDGE('',*,*,#24290,.F.) ;
#31961 = ORIENTED_EDGE('',*,*,#24292,.T.) ;
#31962 = ORIENTED_EDGE('',*,*,#24293,.T.) ;
#31963 = ORIENTED_EDGE('',*,*,#24294,.T.) ;
#31964 = ORIENTED_EDGE('',*,*,#23948,.T.) ;
#31965 = ORIENTED_EDGE('',*,*,#24295,.F.) ;
#31966 = ORIENTED_EDGE('',*,*,#24293,.F.) ;
#31967 = ORIENTED_EDGE('',*,*,#24296,.F.) ;
#31968 = ORIENTED_EDGE('',*,*,#24297,.F.) ;
#31969 = ORIENTED_EDGE('',*,*,#24298,.F.) ;
#31970 = ORIENTED_EDGE('',*,*,#24299,.F.) ;
#31971 = ORIENTED_EDGE('',*,*,#24300,.F.) ;
#31972 = ORIENTED_EDGE('',*,*,#24301,.F.) ;
#31973 = ORIENTED_EDGE('',*,*,#24302,.F.) ;
#31974 = ORIENTED_EDGE('',*,*,#24303,.F.) ;
#31975 = ORIENTED_EDGE('',*,*,#24304,.F.) ;
#31976 = ORIENTED_EDGE('',*,*,#24305,.F.) ;
#31977 = ORIENTED_EDGE('',*,*,#24306,.F.) ;
#31978 = ORIENTED_EDGE('',*,*,#24307,.F.) ;
#31979 = ORIENTED_EDGE('',*,*,#24308,.F.) ;
#31980 = ORIENTED_EDGE('',*,*,#24309,.F.) ;
#31981 = ORIENTED_EDGE('',*,*,#24310,.F.) ;
#31982 = ORIENTED_EDGE('',*,*,#24311,.F.) ;
#31983 = ORIENTED_EDGE('',*,*,#24312,.F.) ;
#31984 = ORIENTED_EDGE('',*,*,#24313,.F.) ;
#31985 = ORIENTED_EDGE('',*,*,#24314,.F.) ;
#31986 = ORIENTED_EDGE('',*,*,#24315,.F.) ;
#31987 = ORIENTED_EDGE('',*,*,#24316,.F.) ;
#31988 = ORIENTED_EDGE('',*,*,#24317,.F.) ;
#31989 = ORIENTED_EDGE('',*,*,#24318,.F.) ;
#31990 = ORIENTED_EDGE('',*,*,#24292,.F.) ;
#31991 = ORIENTED_EDGE('',*,*,#24319,.T.) ;
#31992 = ORIENTED_EDGE('',*,*,#24320,.T.) ;
#31993 = ORIENTED_EDGE('',*,*,#24296,.T.) ;
#31994 = ORIENTED_EDGE('',*,*,#23911,.F.) ;
#31995 = ORIENTED_EDGE('',*,*,#24321,.F.) ;
#31996 = ORIENTED_EDGE('',*,*,#24319,.F.) ;
#31997 = ORIENTED_EDGE('',*,*,#23947,.F.) ;
#31998 = ORIENTED_EDGE('',*,*,#24322,.T.) ;
#31999 = ORIENTED_EDGE('',*,*,#24313,.T.) ;
#32000 = ORIENTED_EDGE('',*,*,#24323,.T.) ;
#32001 = ORIENTED_EDGE('',*,*,#23936,.T.) ;
#32002 = ORIENTED_EDGE('',*,*,#24322,.F.) ;
#32003 = ORIENTED_EDGE('',*,*,#23938,.T.) ;
#32004 = ORIENTED_EDGE('',*,*,#24324,.T.) ;
#32005 = ORIENTED_EDGE('',*,*,#24314,.T.) ;
#32006 = ORIENTED_EDGE('',*,*,#24325,.T.) ;
#32007 = ORIENTED_EDGE('',*,*,#24301,.T.) ;
#32008 = ORIENTED_EDGE('',*,*,#24326,.T.) ;
#32009 = ORIENTED_EDGE('',*,*,#24327,.T.) ;
#32010 = ORIENTED_EDGE('',*,*,#23897,.F.) ;
#32011 = ORIENTED_EDGE('',*,*,#24328,.T.) ;
#32012 = ORIENTED_EDGE('',*,*,#24327,.F.) ;
#32013 = ORIENTED_EDGE('',*,*,#24329,.T.) ;
#32014 = ORIENTED_EDGE('',*,*,#24325,.F.) ;
#32015 = ORIENTED_EDGE('',*,*,#24330,.T.) ;
#32016 = ORIENTED_EDGE('',*,*,#24331,.T.) ;
#32017 = ORIENTED_EDGE('',*,*,#24302,.T.) ;
#32018 = ORIENTED_EDGE('',*,*,#23900,.F.) ;
#32019 = ORIENTED_EDGE('',*,*,#24332,.F.) ;
#32020 = ORIENTED_EDGE('',*,*,#24330,.F.) ;
#32021 = ORIENTED_EDGE('',*,*,#24328,.F.) ;
#32022 = ORIENTED_EDGE('',*,*,#24333,.T.) ;
#32023 = ORIENTED_EDGE('',*,*,#24307,.T.) ;
#32024 = ORIENTED_EDGE('',*,*,#24334,.T.) ;
#32025 = ORIENTED_EDGE('',*,*,#24335,.T.) ;
#32026 = ORIENTED_EDGE('',*,*,#23883,.F.) ;
#32027 = ORIENTED_EDGE('',*,*,#23926,.T.) ;
#32028 = ORIENTED_EDGE('',*,*,#24335,.F.) ;
#32029 = ORIENTED_EDGE('',*,*,#24336,.T.) ;
#32030 = ORIENTED_EDGE('',*,*,#24333,.F.) ;
#32031 = ORIENTED_EDGE('',*,*,#23925,.T.) ;
#32032 = ORIENTED_EDGE('',*,*,#24337,.T.) ;
#32033 = ORIENTED_EDGE('',*,*,#24308,.T.) ;
#32034 = ORIENTED_EDGE('',*,*,#24291,.T.) ;
#32035 = ORIENTED_EDGE('',*,*,#24338,.T.) ;
#32036 = ORIENTED_EDGE('',*,*,#24295,.T.) ;
#32037 = ORIENTED_EDGE('',*,*,#24338,.F.) ;
#32038 = ORIENTED_EDGE('',*,*,#24315,.T.) ;
#32039 = ORIENTED_EDGE('',*,*,#24324,.F.) ;
#32040 = ORIENTED_EDGE('',*,*,#23940,.F.) ;
#32041 = ORIENTED_EDGE('',*,*,#24339,.F.) ;
#32042 = ORIENTED_EDGE('',*,*,#24317,.T.) ;
#32043 = ORIENTED_EDGE('',*,*,#24340,.F.) ;
#32044 = ORIENTED_EDGE('',*,*,#23944,.F.) ;
#32045 = ORIENTED_EDGE('',*,*,#24341,.F.) ;
#32046 = ORIENTED_EDGE('',*,*,#24340,.T.) ;
#32047 = ORIENTED_EDGE('',*,*,#24316,.T.) ;
#32048 = ORIENTED_EDGE('',*,*,#24339,.T.) ;
#32049 = ORIENTED_EDGE('',*,*,#23942,.T.) ;
#32050 = ORIENTED_EDGE('',*,*,#23932,.F.) ;
#32051 = ORIENTED_EDGE('',*,*,#24342,.F.) ;
#32052 = ORIENTED_EDGE('',*,*,#24311,.T.) ;
#32053 = ORIENTED_EDGE('',*,*,#24343,.F.) ;
#32054 = ORIENTED_EDGE('',*,*,#24323,.F.) ;
#32055 = ORIENTED_EDGE('',*,*,#24312,.T.) ;
#32056 = ORIENTED_EDGE('',*,*,#24342,.T.) ;
#32057 = ORIENTED_EDGE('',*,*,#23934,.T.) ;
#32058 = ORIENTED_EDGE('',*,*,#24294,.F.) ;
#32059 = ORIENTED_EDGE('',*,*,#24318,.T.) ;
#32060 = ORIENTED_EDGE('',*,*,#24341,.T.) ;
#32061 = ORIENTED_EDGE('',*,*,#23946,.T.) ;
#32062 = ORIENTED_EDGE('',*,*,#24309,.T.) ;
#32063 = ORIENTED_EDGE('',*,*,#24337,.F.) ;
#32064 = ORIENTED_EDGE('',*,*,#23928,.F.) ;
#32065 = ORIENTED_EDGE('',*,*,#24344,.F.) ;
#32066 = ORIENTED_EDGE('',*,*,#24297,.T.) ;
#32067 = ORIENTED_EDGE('',*,*,#24320,.F.) ;
#32068 = ORIENTED_EDGE('',*,*,#24345,.F.) ;
#32069 = ORIENTED_EDGE('',*,*,#24346,.F.) ;
#32070 = ORIENTED_EDGE('',*,*,#23916,.F.) ;
#32071 = ORIENTED_EDGE('',*,*,#24347,.T.) ;
#32072 = ORIENTED_EDGE('',*,*,#24345,.T.) ;
#32073 = ORIENTED_EDGE('',*,*,#24321,.T.) ;
#32074 = ORIENTED_EDGE('',*,*,#24299,.T.) ;
#32075 = ORIENTED_EDGE('',*,*,#24348,.F.) ;
#32076 = ORIENTED_EDGE('',*,*,#24349,.F.) ;
#32077 = ORIENTED_EDGE('',*,*,#24350,.F.) ;
#32078 = ORIENTED_EDGE('',*,*,#24348,.T.) ;
#32079 = ORIENTED_EDGE('',*,*,#24298,.T.) ;
#32080 = ORIENTED_EDGE('',*,*,#24346,.T.) ;
#32081 = ORIENTED_EDGE('',*,*,#24351,.T.) ;
#32082 = ORIENTED_EDGE('',*,*,#23917,.F.) ;
#32083 = ORIENTED_EDGE('',*,*,#24352,.T.) ;
#32084 = ORIENTED_EDGE('',*,*,#24349,.T.) ;
#32085 = ORIENTED_EDGE('',*,*,#24353,.T.) ;
#32086 = ORIENTED_EDGE('',*,*,#24305,.T.) ;
#32087 = ORIENTED_EDGE('',*,*,#24354,.F.) ;
#32088 = ORIENTED_EDGE('',*,*,#24355,.F.) ;
#32089 = ORIENTED_EDGE('',*,*,#24356,.F.) ;
#32090 = ORIENTED_EDGE('',*,*,#24326,.F.) ;
#32091 = ORIENTED_EDGE('',*,*,#24300,.T.) ;
#32092 = ORIENTED_EDGE('',*,*,#24350,.T.) ;
#32093 = ORIENTED_EDGE('',*,*,#24357,.T.) ;
#32094 = ORIENTED_EDGE('',*,*,#24303,.T.) ;
#32095 = ORIENTED_EDGE('',*,*,#24331,.F.) ;
#32096 = ORIENTED_EDGE('',*,*,#24358,.F.) ;
#32097 = ORIENTED_EDGE('',*,*,#24359,.F.) ;
#32098 = ORIENTED_EDGE('',*,*,#23918,.F.) ;
#32099 = ORIENTED_EDGE('',*,*,#24360,.T.) ;
#32100 = ORIENTED_EDGE('',*,*,#24358,.T.) ;
#32101 = ORIENTED_EDGE('',*,*,#24332,.T.) ;
#32102 = ORIENTED_EDGE('',*,*,#24354,.T.) ;
#32103 = ORIENTED_EDGE('',*,*,#24304,.T.) ;
#32104 = ORIENTED_EDGE('',*,*,#24359,.T.) ;
#32105 = ORIENTED_EDGE('',*,*,#24361,.T.) ;
#32106 = ORIENTED_EDGE('',*,*,#23919,.F.) ;
#32107 = ORIENTED_EDGE('',*,*,#24362,.T.) ;
#32108 = ORIENTED_EDGE('',*,*,#24355,.T.) ;
#32109 = ORIENTED_EDGE('',*,*,#24363,.T.) ;
#32110 = ORIENTED_EDGE('',*,*,#24334,.F.) ;
#32111 = ORIENTED_EDGE('',*,*,#24306,.T.) ;
#32112 = ORIENTED_EDGE('',*,*,#24356,.T.) ;
#32113 = ORIENTED_EDGE('',*,*,#24364,.T.) ;
#32114 = ORIENTED_EDGE('',*,*,#24343,.T.) ;
#32115 = ORIENTED_EDGE('',*,*,#24310,.T.) ;
#32116 = ORIENTED_EDGE('',*,*,#24344,.T.) ;
#32117 = ORIENTED_EDGE('',*,*,#23930,.T.) ;
#32118 = ORIENTED_EDGE('',*,*,#24110,.F.) ;
#32119 = ORIENTED_EDGE('',*,*,#24279,.T.) ;
#32120 = ORIENTED_EDGE('',*,*,#24118,.F.) ;
#32121 = ORIENTED_EDGE('',*,*,#24280,.T.) ;
#32122 = ORIENTED_EDGE('',*,*,#24135,.F.) ;
#32123 = ORIENTED_EDGE('',*,*,#24281,.T.) ;
#32124 = ORIENTED_EDGE('',*,*,#24152,.F.) ;
#32125 = ORIENTED_EDGE('',*,*,#24282,.T.) ;
#32126 = ORIENTED_EDGE('',*,*,#24169,.F.) ;
#32127 = ORIENTED_EDGE('',*,*,#24283,.T.) ;
#32128 = ORIENTED_EDGE('',*,*,#24186,.F.) ;
#32129 = ORIENTED_EDGE('',*,*,#24284,.T.) ;
#32130 = ORIENTED_EDGE('',*,*,#24203,.F.) ;
#32131 = ORIENTED_EDGE('',*,*,#24285,.T.) ;
#32132 = ORIENTED_EDGE('',*,*,#24220,.F.) ;
#32133 = ORIENTED_EDGE('',*,*,#24286,.T.) ;
#32134 = ORIENTED_EDGE('',*,*,#24237,.F.) ;
#32135 = ORIENTED_EDGE('',*,*,#24287,.T.) ;
#32136 = ORIENTED_EDGE('',*,*,#24254,.F.) ;
#32137 = ORIENTED_EDGE('',*,*,#24288,.T.) ;
#32138 = ORIENTED_EDGE('',*,*,#24268,.F.) ;
#32139 = ORIENTED_EDGE('',*,*,#24289,.T.) ;
#32140 = ORIENTED_EDGE('',*,*,#24259,.F.) ;
#32141 = ORIENTED_EDGE('',*,*,#24270,.T.) ;
#32142 = ORIENTED_EDGE('',*,*,#24242,.F.) ;
#32143 = ORIENTED_EDGE('',*,*,#24271,.T.) ;
#32144 = ORIENTED_EDGE('',*,*,#24225,.F.) ;
#32145 = ORIENTED_EDGE('',*,*,#24272,.T.) ;
#32146 = ORIENTED_EDGE('',*,*,#24208,.F.) ;
#32147 = ORIENTED_EDGE('',*,*,#24273,.T.) ;
#32148 = ORIENTED_EDGE('',*,*,#24191,.F.) ;
#32149 = ORIENTED_EDGE('',*,*,#24274,.T.) ;
#32150 = ORIENTED_EDGE('',*,*,#24174,.F.) ;
#32151 = ORIENTED_EDGE('',*,*,#24275,.T.) ;
#32152 = ORIENTED_EDGE('',*,*,#24157,.F.) ;
#32153 = ORIENTED_EDGE('',*,*,#24276,.T.) ;
#32154 = ORIENTED_EDGE('',*,*,#24140,.F.) ;
#32155 = ORIENTED_EDGE('',*,*,#24277,.T.) ;
#32156 = ORIENTED_EDGE('',*,*,#24123,.F.) ;
#32157 = ORIENTED_EDGE('',*,*,#24278,.T.) ;
#32158 = ORIENTED_EDGE('',*,*,#23895,.F.) ;
#32159 = ORIENTED_EDGE('',*,*,#24329,.F.) ;
#32160 = ORIENTED_EDGE('',*,*,#24357,.F.) ;
#32161 = ORIENTED_EDGE('',*,*,#24352,.F.) ;
#32162 = ORIENTED_EDGE('',*,*,#23891,.F.) ;
#32163 = ORIENTED_EDGE('',*,*,#24363,.F.) ;
#32164 = ORIENTED_EDGE('',*,*,#24361,.F.) ;
#32165 = ORIENTED_EDGE('',*,*,#24360,.F.) ;
#32166 = ORIENTED_EDGE('',*,*,#23881,.F.) ;
#32167 = ORIENTED_EDGE('',*,*,#24336,.F.) ;
#32168 = ORIENTED_EDGE('',*,*,#24364,.F.) ;
#32169 = ORIENTED_EDGE('',*,*,#24362,.F.) ;
#32170 = ORIENTED_EDGE('',*,*,#23905,.F.) ;
#32171 = ORIENTED_EDGE('',*,*,#24353,.F.) ;
#32172 = ORIENTED_EDGE('',*,*,#24351,.F.) ;
#32173 = ORIENTED_EDGE('',*,*,#24347,.F.) ;
#32174 = ORIENTED_EDGE('',*,*,#24365,.T.) ;
#32175 = ORIENTED_EDGE('',*,*,#24366,.T.) ;
#32176 = ORIENTED_EDGE('',*,*,#24367,.T.) ;
#32177 = ORIENTED_EDGE('',*,*,#24368,.T.) ;
#32178 = ORIENTED_EDGE('',*,*,#24369,.T.) ;
#32179 = ORIENTED_EDGE('',*,*,#24370,.T.) ;
#32180 = ORIENTED_EDGE('',*,*,#24371,.T.) ;
#32181 = ORIENTED_EDGE('',*,*,#24372,.T.) ;
#32182 = ORIENTED_EDGE('',*,*,#24373,.T.) ;
#32183 = ORIENTED_EDGE('',*,*,#24374,.T.) ;
#32184 = ORIENTED_EDGE('',*,*,#24369,.F.) ;
#32185 = ORIENTED_EDGE('',*,*,#24375,.T.) ;
#32186 = ORIENTED_EDGE('',*,*,#24376,.T.) ;
#32187 = ORIENTED_EDGE('',*,*,#24377,.T.) ;
#32188 = ORIENTED_EDGE('',*,*,#24373,.F.) ;
#32189 = ORIENTED_EDGE('',*,*,#24378,.T.) ;
#32190 = ORIENTED_EDGE('',*,*,#24371,.F.) ;
#32191 = ORIENTED_EDGE('',*,*,#24379,.T.) ;
#32192 = ORIENTED_EDGE('',*,*,#24365,.F.) ;
#32193 = ORIENTED_EDGE('',*,*,#24380,.T.) ;
#32194 = ORIENTED_EDGE('',*,*,#24375,.F.) ;
#32195 = ORIENTED_EDGE('',*,*,#24381,.F.) ;
#32196 = ORIENTED_EDGE('',*,*,#24382,.F.) ;
#32197 = ORIENTED_EDGE('',*,*,#24383,.F.) ;
#32198 = ORIENTED_EDGE('',*,*,#24372,.F.) ;
#32199 = ORIENTED_EDGE('',*,*,#24380,.F.) ;
#32200 = ORIENTED_EDGE('',*,*,#24368,.F.) ;
#32201 = ORIENTED_EDGE('',*,*,#24384,.T.) ;
#32202 = ORIENTED_EDGE('',*,*,#24385,.F.) ;
#32203 = ORIENTED_EDGE('',*,*,#24381,.T.) ;
#32204 = ORIENTED_EDGE('',*,*,#24366,.F.) ;
#32205 = ORIENTED_EDGE('',*,*,#24386,.F.) ;
#32206 = ORIENTED_EDGE('',*,*,#24387,.T.) ;
#32207 = ORIENTED_EDGE('',*,*,#24367,.F.) ;
#32208 = ORIENTED_EDGE('',*,*,#24379,.F.) ;
#32209 = ORIENTED_EDGE('',*,*,#24388,.T.) ;
#32210 = ORIENTED_EDGE('',*,*,#24389,.F.) ;
#32211 = ORIENTED_EDGE('',*,*,#24390,.T.) ;
#32212 = ORIENTED_EDGE('',*,*,#24386,.T.) ;
#32213 = ORIENTED_EDGE('',*,*,#24391,.T.) ;
#32214 = ORIENTED_EDGE('',*,*,#24392,.T.) ;
#32215 = ORIENTED_EDGE('',*,*,#24393,.T.) ;
#32216 = ORIENTED_EDGE('',*,*,#24394,.T.) ;
#32217 = ORIENTED_EDGE('',*,*,#24391,.F.) ;
#32218 = ORIENTED_EDGE('',*,*,#24395,.T.) ;
#32219 = ORIENTED_EDGE('',*,*,#24396,.T.) ;
#32220 = ORIENTED_EDGE('',*,*,#24397,.T.) ;
#32221 = ORIENTED_EDGE('',*,*,#24398,.T.) ;
#32222 = ORIENTED_EDGE('',*,*,#24399,.T.) ;
#32223 = ORIENTED_EDGE('',*,*,#24396,.F.) ;
#32224 = ORIENTED_EDGE('',*,*,#24400,.T.) ;
#32225 = ORIENTED_EDGE('',*,*,#24398,.F.) ;
#32226 = ORIENTED_EDGE('',*,*,#24401,.T.) ;
#32227 = ORIENTED_EDGE('',*,*,#24402,.T.) ;
#32228 = ORIENTED_EDGE('',*,*,#24403,.T.) ;
#32229 = ORIENTED_EDGE('',*,*,#24404,.T.) ;
#32230 = ORIENTED_EDGE('',*,*,#24405,.T.) ;
#32231 = ORIENTED_EDGE('',*,*,#24402,.F.) ;
#32232 = ORIENTED_EDGE('',*,*,#24406,.T.) ;
#32233 = ORIENTED_EDGE('',*,*,#24404,.F.) ;
#32234 = ORIENTED_EDGE('',*,*,#24407,.T.) ;
#32235 = ORIENTED_EDGE('',*,*,#24408,.T.) ;
#32236 = ORIENTED_EDGE('',*,*,#24409,.T.) ;
#32237 = ORIENTED_EDGE('',*,*,#24410,.T.) ;
#32238 = ORIENTED_EDGE('',*,*,#24411,.T.) ;
#32239 = ORIENTED_EDGE('',*,*,#24408,.F.) ;
#32240 = ORIENTED_EDGE('',*,*,#24412,.T.) ;
#32241 = ORIENTED_EDGE('',*,*,#24410,.F.) ;
#32242 = ORIENTED_EDGE('',*,*,#24413,.T.) ;
#32243 = ORIENTED_EDGE('',*,*,#24393,.F.) ;
#32244 = ORIENTED_EDGE('',*,*,#24414,.T.) ;
#32245 = ORIENTED_EDGE('',*,*,#24401,.F.) ;
#32246 = ORIENTED_EDGE('',*,*,#24415,.T.) ;
#32247 = ORIENTED_EDGE('',*,*,#24416,.F.) ;
#32248 = ORIENTED_EDGE('',*,*,#24417,.T.) ;
#32249 = ORIENTED_EDGE('',*,*,#24400,.F.) ;
#32250 = ORIENTED_EDGE('',*,*,#24418,.F.) ;
#32251 = ORIENTED_EDGE('',*,*,#24419,.F.) ;
#32252 = ORIENTED_EDGE('',*,*,#24415,.F.) ;
#32253 = ORIENTED_EDGE('',*,*,#24395,.F.) ;
#32254 = ORIENTED_EDGE('',*,*,#24420,.T.) ;
#32255 = ORIENTED_EDGE('',*,*,#24421,.F.) ;
#32256 = ORIENTED_EDGE('',*,*,#24418,.T.) ;
#32257 = ORIENTED_EDGE('',*,*,#24394,.F.) ;
#32258 = ORIENTED_EDGE('',*,*,#24422,.F.) ;
#32259 = ORIENTED_EDGE('',*,*,#24423,.F.) ;
#32260 = ORIENTED_EDGE('',*,*,#24420,.F.) ;
#32261 = ORIENTED_EDGE('',*,*,#24424,.F.) ;
#32262 = ORIENTED_EDGE('',*,*,#24425,.F.) ;
#32263 = ORIENTED_EDGE('',*,*,#24426,.F.) ;
#32264 = ORIENTED_EDGE('',*,*,#24427,.F.) ;
#32265 = ORIENTED_EDGE('',*,*,#24428,.F.) ;
#32266 = ORIENTED_EDGE('',*,*,#24429,.F.) ;
#32267 = ORIENTED_EDGE('',*,*,#24430,.F.) ;
#32268 = ORIENTED_EDGE('',*,*,#24431,.F.) ;
#32269 = ORIENTED_EDGE('',*,*,#24432,.F.) ;
#32270 = ORIENTED_EDGE('',*,*,#24433,.F.) ;
#32271 = ORIENTED_EDGE('',*,*,#24434,.F.) ;
#32272 = ORIENTED_EDGE('',*,*,#24435,.F.) ;
#32273 = ORIENTED_EDGE('',*,*,#24436,.F.) ;
#32274 = ORIENTED_EDGE('',*,*,#24437,.F.) ;
#32275 = ORIENTED_EDGE('',*,*,#24438,.F.) ;
#32276 = ORIENTED_EDGE('',*,*,#24439,.F.) ;
#32277 = ORIENTED_EDGE('',*,*,#24440,.F.) ;
#32278 = ORIENTED_EDGE('',*,*,#24441,.F.) ;
#32279 = ORIENTED_EDGE('',*,*,#24442,.F.) ;
#32280 = ORIENTED_EDGE('',*,*,#24443,.F.) ;
#32281 = ORIENTED_EDGE('',*,*,#24444,.F.) ;
#32282 = ORIENTED_EDGE('',*,*,#24445,.F.) ;
#32283 = ORIENTED_EDGE('',*,*,#24446,.F.) ;
#32284 = ORIENTED_EDGE('',*,*,#24447,.F.) ;
#32285 = ORIENTED_EDGE('',*,*,#24448,.F.) ;
#32286 = ORIENTED_EDGE('',*,*,#24449,.F.) ;
#32287 = ORIENTED_EDGE('',*,*,#24450,.F.) ;
#32288 = ORIENTED_EDGE('',*,*,#24451,.F.) ;
#32289 = ORIENTED_EDGE('',*,*,#24452,.F.) ;
#32290 = ORIENTED_EDGE('',*,*,#24453,.F.) ;
#32291 = ORIENTED_EDGE('',*,*,#24454,.F.) ;
#32292 = ORIENTED_EDGE('',*,*,#24455,.F.) ;
#32293 = ORIENTED_EDGE('',*,*,#24456,.F.) ;
#32294 = ORIENTED_EDGE('',*,*,#24457,.F.) ;
#32295 = ORIENTED_EDGE('',*,*,#24458,.F.) ;
#32296 = ORIENTED_EDGE('',*,*,#24459,.F.) ;
#32297 = ORIENTED_EDGE('',*,*,#24460,.F.) ;
#32298 = ORIENTED_EDGE('',*,*,#24461,.F.) ;
#32299 = ORIENTED_EDGE('',*,*,#24462,.F.) ;
#32300 = ORIENTED_EDGE('',*,*,#24463,.F.) ;
#32301 = ORIENTED_EDGE('',*,*,#24392,.F.) ;
#32302 = ORIENTED_EDGE('',*,*,#24397,.F.) ;
#32303 = ORIENTED_EDGE('',*,*,#24399,.F.) ;
#32304 = ORIENTED_EDGE('',*,*,#24403,.F.) ;
#32305 = ORIENTED_EDGE('',*,*,#24405,.F.) ;
#32306 = ORIENTED_EDGE('',*,*,#24409,.F.) ;
#32307 = ORIENTED_EDGE('',*,*,#24411,.F.) ;
#32308 = ORIENTED_EDGE('',*,*,#24414,.F.) ;
#32309 = ORIENTED_EDGE('',*,*,#24464,.T.) ;
#32310 = ORIENTED_EDGE('',*,*,#24465,.T.) ;
#32311 = ORIENTED_EDGE('',*,*,#24466,.T.) ;
#32312 = ORIENTED_EDGE('',*,*,#24444,.T.) ;
#32313 = ORIENTED_EDGE('',*,*,#24466,.F.) ;
#32314 = ORIENTED_EDGE('',*,*,#24467,.T.) ;
#32315 = ORIENTED_EDGE('',*,*,#24468,.T.) ;
#32316 = ORIENTED_EDGE('',*,*,#24445,.T.) ;
#32317 = ORIENTED_EDGE('',*,*,#24469,.T.) ;
#32318 = ORIENTED_EDGE('',*,*,#24446,.T.) ;
#32319 = ORIENTED_EDGE('',*,*,#24468,.F.) ;
#32320 = ORIENTED_EDGE('',*,*,#24470,.T.) ;
#32321 = ORIENTED_EDGE('',*,*,#24469,.F.) ;
#32322 = ORIENTED_EDGE('',*,*,#24471,.T.) ;
#32323 = ORIENTED_EDGE('',*,*,#24472,.T.) ;
#32324 = ORIENTED_EDGE('',*,*,#24447,.T.) ;
#32325 = ORIENTED_EDGE('',*,*,#24473,.T.) ;
#32326 = ORIENTED_EDGE('',*,*,#24448,.T.) ;
#32327 = ORIENTED_EDGE('',*,*,#24472,.F.) ;
#32328 = ORIENTED_EDGE('',*,*,#24474,.T.) ;
#32329 = ORIENTED_EDGE('',*,*,#24473,.F.) ;
#32330 = ORIENTED_EDGE('',*,*,#24475,.T.) ;
#32331 = ORIENTED_EDGE('',*,*,#24476,.T.) ;
#32332 = ORIENTED_EDGE('',*,*,#24449,.T.) ;
#32333 = ORIENTED_EDGE('',*,*,#24477,.T.) ;
#32334 = ORIENTED_EDGE('',*,*,#24450,.T.) ;
#32335 = ORIENTED_EDGE('',*,*,#24476,.F.) ;
#32336 = ORIENTED_EDGE('',*,*,#24478,.T.) ;
#32337 = ORIENTED_EDGE('',*,*,#24477,.F.) ;
#32338 = ORIENTED_EDGE('',*,*,#24479,.T.) ;
#32339 = ORIENTED_EDGE('',*,*,#24464,.F.) ;
#32340 = ORIENTED_EDGE('',*,*,#24451,.T.) ;
#32341 = ORIENTED_EDGE('',*,*,#24471,.F.) ;
#32342 = ORIENTED_EDGE('',*,*,#24480,.T.) ;
#32343 = ORIENTED_EDGE('',*,*,#24481,.F.) ;
#32344 = ORIENTED_EDGE('',*,*,#24482,.T.) ;
#32345 = ORIENTED_EDGE('',*,*,#24470,.F.) ;
#32346 = ORIENTED_EDGE('',*,*,#24483,.F.) ;
#32347 = ORIENTED_EDGE('',*,*,#24484,.F.) ;
#32348 = ORIENTED_EDGE('',*,*,#24480,.F.) ;
#32349 = ORIENTED_EDGE('',*,*,#24467,.F.) ;
#32350 = ORIENTED_EDGE('',*,*,#24485,.T.) ;
#32351 = ORIENTED_EDGE('',*,*,#24486,.F.) ;
#32352 = ORIENTED_EDGE('',*,*,#24483,.T.) ;
#32353 = ORIENTED_EDGE('',*,*,#24465,.F.) ;
#32354 = ORIENTED_EDGE('',*,*,#24487,.F.) ;
#32355 = ORIENTED_EDGE('',*,*,#24488,.F.) ;
#32356 = ORIENTED_EDGE('',*,*,#24485,.F.) ;
#32357 = ORIENTED_EDGE('',*,*,#24463,.T.) ;
#32358 = ORIENTED_EDGE('',*,*,#24489,.T.) ;
#32359 = ORIENTED_EDGE('',*,*,#24490,.T.) ;
#32360 = ORIENTED_EDGE('',*,*,#24489,.F.) ;
#32361 = ORIENTED_EDGE('',*,*,#24491,.F.) ;
#32362 = ORIENTED_EDGE('',*,*,#24492,.T.) ;
#32363 = ORIENTED_EDGE('',*,*,#24490,.F.) ;
#32364 = ORIENTED_EDGE('',*,*,#24492,.F.) ;
#32365 = ORIENTED_EDGE('',*,*,#24424,.T.) ;
#32366 = ORIENTED_EDGE('',*,*,#24493,.T.) ;
#32367 = ORIENTED_EDGE('',*,*,#24494,.T.) ;
#32368 = ORIENTED_EDGE('',*,*,#24495,.F.) ;
#32369 = ORIENTED_EDGE('',*,*,#24443,.T.) ;
#32370 = ORIENTED_EDGE('',*,*,#24496,.T.) ;
#32371 = ORIENTED_EDGE('',*,*,#24497,.T.) ;
#32372 = ORIENTED_EDGE('',*,*,#24493,.F.) ;
#32373 = ORIENTED_EDGE('',*,*,#24442,.T.) ;
#32374 = ORIENTED_EDGE('',*,*,#24498,.T.) ;
#32375 = ORIENTED_EDGE('',*,*,#24499,.T.) ;
#32376 = ORIENTED_EDGE('',*,*,#24496,.F.) ;
#32377 = ORIENTED_EDGE('',*,*,#24441,.T.) ;
#32378 = ORIENTED_EDGE('',*,*,#24500,.T.) ;
#32379 = ORIENTED_EDGE('',*,*,#24501,.T.) ;
#32380 = ORIENTED_EDGE('',*,*,#24498,.F.) ;
#32381 = ORIENTED_EDGE('',*,*,#24500,.F.) ;
#32382 = ORIENTED_EDGE('',*,*,#24440,.T.) ;
#32383 = ORIENTED_EDGE('',*,*,#24502,.T.) ;
#32384 = ORIENTED_EDGE('',*,*,#24503,.T.) ;
#32385 = ORIENTED_EDGE('',*,*,#24502,.F.) ;
#32386 = ORIENTED_EDGE('',*,*,#24439,.T.) ;
#32387 = ORIENTED_EDGE('',*,*,#24504,.T.) ;
#32388 = ORIENTED_EDGE('',*,*,#24505,.T.) ;
#32389 = ORIENTED_EDGE('',*,*,#24504,.F.) ;
#32390 = ORIENTED_EDGE('',*,*,#24438,.T.) ;
#32391 = ORIENTED_EDGE('',*,*,#24506,.T.) ;
#32392 = ORIENTED_EDGE('',*,*,#24507,.T.) ;
#32393 = ORIENTED_EDGE('',*,*,#24506,.F.) ;
#32394 = ORIENTED_EDGE('',*,*,#24437,.T.) ;
#32395 = ORIENTED_EDGE('',*,*,#24508,.T.) ;
#32396 = ORIENTED_EDGE('',*,*,#24509,.T.) ;
#32397 = ORIENTED_EDGE('',*,*,#24510,.T.) ;
#32398 = ORIENTED_EDGE('',*,*,#24511,.T.) ;
#32399 = ORIENTED_EDGE('',*,*,#24508,.F.) ;
#32400 = ORIENTED_EDGE('',*,*,#24436,.T.) ;
#32401 = ORIENTED_EDGE('',*,*,#24512,.T.) ;
#32402 = ORIENTED_EDGE('',*,*,#24513,.T.) ;
#32403 = ORIENTED_EDGE('',*,*,#24510,.F.) ;
#32404 = ORIENTED_EDGE('',*,*,#24435,.T.) ;
#32405 = ORIENTED_EDGE('',*,*,#24514,.T.) ;
#32406 = ORIENTED_EDGE('',*,*,#24515,.T.) ;
#32407 = ORIENTED_EDGE('',*,*,#24512,.F.) ;
#32408 = ORIENTED_EDGE('',*,*,#24434,.T.) ;
#32409 = ORIENTED_EDGE('',*,*,#24514,.F.) ;
#32410 = ORIENTED_EDGE('',*,*,#24433,.T.) ;
#32411 = ORIENTED_EDGE('',*,*,#24516,.T.) ;
#32412 = ORIENTED_EDGE('',*,*,#24517,.T.) ;
#32413 = ORIENTED_EDGE('',*,*,#24516,.F.) ;
#32414 = ORIENTED_EDGE('',*,*,#24432,.T.) ;
#32415 = ORIENTED_EDGE('',*,*,#24518,.T.) ;
#32416 = ORIENTED_EDGE('',*,*,#24519,.T.) ;
#32417 = ORIENTED_EDGE('',*,*,#24518,.F.) ;
#32418 = ORIENTED_EDGE('',*,*,#24431,.T.) ;
#32419 = ORIENTED_EDGE('',*,*,#24520,.T.) ;
#32420 = ORIENTED_EDGE('',*,*,#24521,.T.) ;
#32421 = ORIENTED_EDGE('',*,*,#24520,.F.) ;
#32422 = ORIENTED_EDGE('',*,*,#24430,.T.) ;
#32423 = ORIENTED_EDGE('',*,*,#24522,.T.) ;
#32424 = ORIENTED_EDGE('',*,*,#24523,.T.) ;
#32425 = ORIENTED_EDGE('',*,*,#24522,.F.) ;
#32426 = ORIENTED_EDGE('',*,*,#24429,.T.) ;
#32427 = ORIENTED_EDGE('',*,*,#24524,.T.) ;
#32428 = ORIENTED_EDGE('',*,*,#24525,.T.) ;
#32429 = ORIENTED_EDGE('',*,*,#24526,.T.) ;
#32430 = ORIENTED_EDGE('',*,*,#24527,.T.) ;
#32431 = ORIENTED_EDGE('',*,*,#24524,.F.) ;
#32432 = ORIENTED_EDGE('',*,*,#24428,.T.) ;
#32433 = ORIENTED_EDGE('',*,*,#24528,.T.) ;
#32434 = ORIENTED_EDGE('',*,*,#24526,.F.) ;
#32435 = ORIENTED_EDGE('',*,*,#24427,.T.) ;
#32436 = ORIENTED_EDGE('',*,*,#24529,.T.) ;
#32437 = ORIENTED_EDGE('',*,*,#24530,.T.) ;
#32438 = ORIENTED_EDGE('',*,*,#24529,.F.) ;
#32439 = ORIENTED_EDGE('',*,*,#24426,.T.) ;
#32440 = ORIENTED_EDGE('',*,*,#24531,.T.) ;
#32441 = ORIENTED_EDGE('',*,*,#24532,.T.) ;
#32442 = ORIENTED_EDGE('',*,*,#24531,.F.) ;
#32443 = ORIENTED_EDGE('',*,*,#24425,.T.) ;
#32444 = ORIENTED_EDGE('',*,*,#24495,.T.) ;
#32445 = ORIENTED_EDGE('',*,*,#24517,.F.) ;
#32446 = ORIENTED_EDGE('',*,*,#24533,.T.) ;
#32447 = ORIENTED_EDGE('',*,*,#24534,.F.) ;
#32448 = ORIENTED_EDGE('',*,*,#24535,.F.) ;
#32449 = ORIENTED_EDGE('',*,*,#24519,.F.) ;
#32450 = ORIENTED_EDGE('',*,*,#24536,.F.) ;
#32451 = ORIENTED_EDGE('',*,*,#24537,.F.) ;
#32452 = ORIENTED_EDGE('',*,*,#24533,.F.) ;
#32453 = ORIENTED_EDGE('',*,*,#24521,.F.) ;
#32454 = ORIENTED_EDGE('',*,*,#24538,.F.) ;
#32455 = ORIENTED_EDGE('',*,*,#24539,.F.) ;
#32456 = ORIENTED_EDGE('',*,*,#24536,.T.) ;
#32457 = ORIENTED_EDGE('',*,*,#24523,.F.) ;
#32458 = ORIENTED_EDGE('',*,*,#24540,.F.) ;
#32459 = ORIENTED_EDGE('',*,*,#24541,.F.) ;
#32460 = ORIENTED_EDGE('',*,*,#24542,.F.) ;
#32461 = ORIENTED_EDGE('',*,*,#24543,.F.) ;
#32462 = ORIENTED_EDGE('',*,*,#24544,.F.) ;
#32463 = ORIENTED_EDGE('',*,*,#24538,.T.) ;
#32464 = ORIENTED_EDGE('',*,*,#24525,.F.) ;
#32465 = ORIENTED_EDGE('',*,*,#24545,.F.) ;
#32466 = ORIENTED_EDGE('',*,*,#24546,.T.) ;
#32467 = ORIENTED_EDGE('',*,*,#24376,.F.) ;
#32468 = ORIENTED_EDGE('',*,*,#24542,.T.) ;
#32469 = ORIENTED_EDGE('',*,*,#24541,.T.) ;
#32470 = ORIENTED_EDGE('',*,*,#24540,.T.) ;
#32471 = ORIENTED_EDGE('',*,*,#24527,.F.) ;
#32472 = ORIENTED_EDGE('',*,*,#24547,.T.) ;
#32473 = ORIENTED_EDGE('',*,*,#24548,.T.) ;
#32474 = ORIENTED_EDGE('',*,*,#24545,.T.) ;
#32475 = ORIENTED_EDGE('',*,*,#24528,.F.) ;
#32476 = ORIENTED_EDGE('',*,*,#24549,.F.) ;
#32477 = ORIENTED_EDGE('',*,*,#24550,.T.) ;
#32478 = ORIENTED_EDGE('',*,*,#24547,.F.) ;
#32479 = ORIENTED_EDGE('',*,*,#24530,.F.) ;
#32480 = ORIENTED_EDGE('',*,*,#24551,.F.) ;
#32481 = ORIENTED_EDGE('',*,*,#24552,.T.) ;
#32482 = ORIENTED_EDGE('',*,*,#24549,.T.) ;
#32483 = ORIENTED_EDGE('',*,*,#24532,.F.) ;
#32484 = ORIENTED_EDGE('',*,*,#24553,.F.) ;
#32485 = ORIENTED_EDGE('',*,*,#24554,.T.) ;
#32486 = ORIENTED_EDGE('',*,*,#24551,.T.) ;
#32487 = ORIENTED_EDGE('',*,*,#24494,.F.) ;
#32488 = ORIENTED_EDGE('',*,*,#24555,.F.) ;
#32489 = ORIENTED_EDGE('',*,*,#24556,.T.) ;
#32490 = ORIENTED_EDGE('',*,*,#24553,.T.) ;
#32491 = ORIENTED_EDGE('',*,*,#24461,.T.) ;
#32492 = ORIENTED_EDGE('',*,*,#24557,.T.) ;
#32493 = ORIENTED_EDGE('',*,*,#24558,.T.) ;
#32494 = ORIENTED_EDGE('',*,*,#24559,.F.) ;
#32495 = ORIENTED_EDGE('',*,*,#24560,.F.) ;
#32496 = ORIENTED_EDGE('',*,*,#24561,.F.) ;
#32497 = ORIENTED_EDGE('',*,*,#24562,.F.) ;
#32498 = ORIENTED_EDGE('',*,*,#24457,.T.) ;
#32499 = ORIENTED_EDGE('',*,*,#24563,.F.) ;
#32500 = ORIENTED_EDGE('',*,*,#24564,.F.) ;
#32501 = ORIENTED_EDGE('',*,*,#24565,.F.) ;
#32502 = ORIENTED_EDGE('',*,*,#24561,.T.) ;
#32503 = ORIENTED_EDGE('',*,*,#24566,.T.) ;
#32504 = ORIENTED_EDGE('',*,*,#24564,.T.) ;
#32505 = ORIENTED_EDGE('',*,*,#24567,.T.) ;
#32506 = ORIENTED_EDGE('',*,*,#24568,.F.) ;
#32507 = ORIENTED_EDGE('',*,*,#24569,.F.) ;
#32508 = ORIENTED_EDGE('',*,*,#24570,.F.) ;
#32509 = ORIENTED_EDGE('',*,*,#24455,.T.) ;
#32510 = ORIENTED_EDGE('',*,*,#24571,.F.) ;
#32511 = ORIENTED_EDGE('',*,*,#24572,.F.) ;
#32512 = ORIENTED_EDGE('',*,*,#24573,.F.) ;
#32513 = ORIENTED_EDGE('',*,*,#24574,.F.) ;
#32514 = ORIENTED_EDGE('',*,*,#24569,.T.) ;
#32515 = ORIENTED_EDGE('',*,*,#24575,.T.) ;
#32516 = ORIENTED_EDGE('',*,*,#24573,.T.) ;
#32517 = ORIENTED_EDGE('',*,*,#24572,.T.) ;
#32518 = ORIENTED_EDGE('',*,*,#24576,.T.) ;
#32519 = ORIENTED_EDGE('',*,*,#24577,.T.) ;
#32520 = ORIENTED_EDGE('',*,*,#24578,.T.) ;
#32521 = ORIENTED_EDGE('',*,*,#24579,.T.) ;
#32522 = ORIENTED_EDGE('',*,*,#24580,.T.) ;
#32523 = ORIENTED_EDGE('',*,*,#24574,.T.) ;
#32524 = ORIENTED_EDGE('',*,*,#24581,.T.) ;
#32525 = ORIENTED_EDGE('',*,*,#24579,.F.) ;
#32526 = ORIENTED_EDGE('',*,*,#24582,.T.) ;
#32527 = ORIENTED_EDGE('',*,*,#24565,.T.) ;
#32528 = ORIENTED_EDGE('',*,*,#24583,.T.) ;
#32529 = ORIENTED_EDGE('',*,*,#24571,.T.) ;
#32530 = ORIENTED_EDGE('',*,*,#24584,.T.) ;
#32531 = ORIENTED_EDGE('',*,*,#24560,.T.) ;
#32532 = ORIENTED_EDGE('',*,*,#24456,.T.) ;
#32533 = ORIENTED_EDGE('',*,*,#24570,.T.) ;
#32534 = ORIENTED_EDGE('',*,*,#24585,.T.) ;
#32535 = ORIENTED_EDGE('',*,*,#24586,.T.) ;
#32536 = ORIENTED_EDGE('',*,*,#24587,.T.) ;
#32537 = ORIENTED_EDGE('',*,*,#24452,.T.) ;
#32538 = ORIENTED_EDGE('',*,*,#24588,.T.) ;
#32539 = ORIENTED_EDGE('',*,*,#24589,.T.) ;
#32540 = ORIENTED_EDGE('',*,*,#24453,.T.) ;
#32541 = ORIENTED_EDGE('',*,*,#24587,.F.) ;
#32542 = ORIENTED_EDGE('',*,*,#24590,.T.) ;
#32543 = ORIENTED_EDGE('',*,*,#24568,.T.) ;
#32544 = ORIENTED_EDGE('',*,*,#24454,.T.) ;
#32545 = ORIENTED_EDGE('',*,*,#24589,.F.) ;
#32546 = ORIENTED_EDGE('',*,*,#24591,.T.) ;
#32547 = ORIENTED_EDGE('',*,*,#24563,.T.) ;
#32548 = ORIENTED_EDGE('',*,*,#24592,.T.) ;
#32549 = ORIENTED_EDGE('',*,*,#24593,.T.) ;
#32550 = ORIENTED_EDGE('',*,*,#24594,.T.) ;
#32551 = ORIENTED_EDGE('',*,*,#24595,.T.) ;
#32552 = ORIENTED_EDGE('',*,*,#24596,.T.) ;
#32553 = ORIENTED_EDGE('',*,*,#24593,.F.) ;
#32554 = ORIENTED_EDGE('',*,*,#24597,.T.) ;
#32555 = ORIENTED_EDGE('',*,*,#24598,.F.) ;
#32556 = ORIENTED_EDGE('',*,*,#24599,.T.) ;
#32557 = ORIENTED_EDGE('',*,*,#24595,.F.) ;
#32558 = ORIENTED_EDGE('',*,*,#24600,.T.) ;
#32559 = ORIENTED_EDGE('',*,*,#24601,.T.) ;
#32560 = ORIENTED_EDGE('',*,*,#24588,.F.) ;
#32561 = ORIENTED_EDGE('',*,*,#24462,.T.) ;
#32562 = ORIENTED_EDGE('',*,*,#24559,.T.) ;
#32563 = ORIENTED_EDGE('',*,*,#24562,.T.) ;
#32564 = ORIENTED_EDGE('',*,*,#24602,.T.) ;
#32565 = ORIENTED_EDGE('',*,*,#24603,.T.) ;
#32566 = ORIENTED_EDGE('',*,*,#24458,.T.) ;
#32567 = ORIENTED_EDGE('',*,*,#24603,.F.) ;
#32568 = ORIENTED_EDGE('',*,*,#24604,.T.) ;
#32569 = ORIENTED_EDGE('',*,*,#24605,.T.) ;
#32570 = ORIENTED_EDGE('',*,*,#24459,.T.) ;
#32571 = ORIENTED_EDGE('',*,*,#24460,.T.) ;
#32572 = ORIENTED_EDGE('',*,*,#24605,.F.) ;
#32573 = ORIENTED_EDGE('',*,*,#24606,.T.) ;
#32574 = ORIENTED_EDGE('',*,*,#24557,.F.) ;
#32575 = ORIENTED_EDGE('',*,*,#24607,.T.) ;
#32576 = ORIENTED_EDGE('',*,*,#24608,.T.) ;
#32577 = ORIENTED_EDGE('',*,*,#24577,.F.) ;
#32578 = ORIENTED_EDGE('',*,*,#24600,.F.) ;
#32579 = ORIENTED_EDGE('',*,*,#24597,.F.) ;
#32580 = ORIENTED_EDGE('',*,*,#24592,.F.) ;
#32581 = ORIENTED_EDGE('',*,*,#24584,.F.) ;
#32582 = ORIENTED_EDGE('',*,*,#24582,.F.) ;
#32583 = ORIENTED_EDGE('',*,*,#24578,.F.) ;
#32584 = ORIENTED_EDGE('',*,*,#24608,.F.) ;
#32585 = ORIENTED_EDGE('',*,*,#24609,.T.) ;
#32586 = ORIENTED_EDGE('',*,*,#24610,.F.) ;
#32587 = ORIENTED_EDGE('',*,*,#24611,.F.) ;
#32588 = ORIENTED_EDGE('',*,*,#24581,.F.) ;
#32589 = ORIENTED_EDGE('',*,*,#24575,.F.) ;
#32590 = ORIENTED_EDGE('',*,*,#24591,.F.) ;
#32591 = ORIENTED_EDGE('',*,*,#24612,.F.) ;
#32592 = ORIENTED_EDGE('',*,*,#24580,.F.) ;
#32593 = ORIENTED_EDGE('',*,*,#24612,.T.) ;
#32594 = ORIENTED_EDGE('',*,*,#24590,.F.) ;
#32595 = ORIENTED_EDGE('',*,*,#24613,.F.) ;
#32596 = ORIENTED_EDGE('',*,*,#24586,.F.) ;
#32597 = ORIENTED_EDGE('',*,*,#24614,.F.) ;
#32598 = ORIENTED_EDGE('',*,*,#24615,.T.) ;
#32599 = ORIENTED_EDGE('',*,*,#24616,.T.) ;
#32600 = ORIENTED_EDGE('',*,*,#24613,.T.) ;
#32601 = ORIENTED_EDGE('',*,*,#24576,.F.) ;
#32602 = ORIENTED_EDGE('',*,*,#24583,.F.) ;
#32603 = ORIENTED_EDGE('',*,*,#24566,.F.) ;
#32604 = ORIENTED_EDGE('',*,*,#24585,.F.) ;
#32605 = ORIENTED_EDGE('',*,*,#24617,.T.) ;
#32606 = ORIENTED_EDGE('',*,*,#24618,.T.) ;
#32607 = ORIENTED_EDGE('',*,*,#24619,.T.) ;
#32608 = ORIENTED_EDGE('',*,*,#24481,.T.) ;
#32609 = ORIENTED_EDGE('',*,*,#24617,.F.) ;
#32610 = ORIENTED_EDGE('',*,*,#24484,.T.) ;
#32611 = ORIENTED_EDGE('',*,*,#24620,.T.) ;
#32612 = ORIENTED_EDGE('',*,*,#24621,.T.) ;
#32613 = ORIENTED_EDGE('',*,*,#24622,.T.) ;
#32614 = ORIENTED_EDGE('',*,*,#24623,.T.) ;
#32615 = ORIENTED_EDGE('',*,*,#24620,.F.) ;
#32616 = ORIENTED_EDGE('',*,*,#24486,.T.) ;
#32617 = ORIENTED_EDGE('',*,*,#24624,.T.) ;
#32618 = ORIENTED_EDGE('',*,*,#24625,.T.) ;
#32619 = ORIENTED_EDGE('',*,*,#24622,.F.) ;
#32620 = ORIENTED_EDGE('',*,*,#24488,.T.) ;
#32621 = ORIENTED_EDGE('',*,*,#24626,.T.) ;
#32622 = ORIENTED_EDGE('',*,*,#24627,.T.) ;
#32623 = ORIENTED_EDGE('',*,*,#24624,.F.) ;
#32624 = ORIENTED_EDGE('',*,*,#24628,.T.) ;
#32625 = ORIENTED_EDGE('',*,*,#24626,.F.) ;
#32626 = ORIENTED_EDGE('',*,*,#24629,.T.) ;
#32627 = ORIENTED_EDGE('',*,*,#24630,.T.) ;
#32628 = ORIENTED_EDGE('',*,*,#24631,.T.) ;
#32629 = ORIENTED_EDGE('',*,*,#24632,.T.) ;
#32630 = ORIENTED_EDGE('',*,*,#24633,.T.) ;
#32631 = ORIENTED_EDGE('',*,*,#24630,.F.) ;
#32632 = ORIENTED_EDGE('',*,*,#24634,.T.) ;
#32633 = ORIENTED_EDGE('',*,*,#24632,.F.) ;
#32634 = ORIENTED_EDGE('',*,*,#24635,.T.) ;
#32635 = ORIENTED_EDGE('',*,*,#24619,.F.) ;
#32636 = ORIENTED_EDGE('',*,*,#24636,.T.) ;
#32637 = ORIENTED_EDGE('',*,*,#24618,.F.) ;
#32638 = ORIENTED_EDGE('',*,*,#24621,.F.) ;
#32639 = ORIENTED_EDGE('',*,*,#24623,.F.) ;
#32640 = ORIENTED_EDGE('',*,*,#24625,.F.) ;
#32641 = ORIENTED_EDGE('',*,*,#24627,.F.) ;
#32642 = ORIENTED_EDGE('',*,*,#24631,.F.) ;
#32643 = ORIENTED_EDGE('',*,*,#24633,.F.) ;
#32644 = ORIENTED_EDGE('',*,*,#24636,.F.) ;
#32645 = ORIENTED_EDGE('',*,*,#24637,.T.) ;
#32646 = ORIENTED_EDGE('',*,*,#24638,.T.) ;
#32647 = ORIENTED_EDGE('',*,*,#24639,.T.) ;
#32648 = ORIENTED_EDGE('',*,*,#24640,.T.) ;
#32649 = ORIENTED_EDGE('',*,*,#24637,.F.) ;
#32650 = ORIENTED_EDGE('',*,*,#24641,.T.) ;
#32651 = ORIENTED_EDGE('',*,*,#24642,.T.) ;
#32652 = ORIENTED_EDGE('',*,*,#24643,.T.) ;
#32653 = ORIENTED_EDGE('',*,*,#24644,.T.) ;
#32654 = ORIENTED_EDGE('',*,*,#24645,.T.) ;
#32655 = ORIENTED_EDGE('',*,*,#24642,.F.) ;
#32656 = ORIENTED_EDGE('',*,*,#24416,.T.) ;
#32657 = ORIENTED_EDGE('',*,*,#24646,.T.) ;
#32658 = ORIENTED_EDGE('',*,*,#24647,.T.) ;
#32659 = ORIENTED_EDGE('',*,*,#24644,.F.) ;
#32660 = ORIENTED_EDGE('',*,*,#24419,.T.) ;
#32661 = ORIENTED_EDGE('',*,*,#24648,.T.) ;
#32662 = ORIENTED_EDGE('',*,*,#24649,.T.) ;
#32663 = ORIENTED_EDGE('',*,*,#24646,.F.) ;
#32664 = ORIENTED_EDGE('',*,*,#24421,.T.) ;
#32665 = ORIENTED_EDGE('',*,*,#24648,.F.) ;
#32666 = ORIENTED_EDGE('',*,*,#24423,.T.) ;
#32667 = ORIENTED_EDGE('',*,*,#24650,.T.) ;
#32668 = ORIENTED_EDGE('',*,*,#24651,.T.) ;
#32669 = ORIENTED_EDGE('',*,*,#24652,.T.) ;
#32670 = ORIENTED_EDGE('',*,*,#24653,.T.) ;
#32671 = ORIENTED_EDGE('',*,*,#24650,.F.) ;
#32672 = ORIENTED_EDGE('',*,*,#24654,.T.) ;
#32673 = ORIENTED_EDGE('',*,*,#24652,.F.) ;
#32674 = ORIENTED_EDGE('',*,*,#24655,.T.) ;
#32675 = ORIENTED_EDGE('',*,*,#24639,.F.) ;
#32676 = ORIENTED_EDGE('',*,*,#24656,.T.) ;
#32677 = ORIENTED_EDGE('',*,*,#24406,.F.) ;
#32678 = ORIENTED_EDGE('',*,*,#24417,.F.) ;
#32679 = ORIENTED_EDGE('',*,*,#24641,.F.) ;
#32680 = ORIENTED_EDGE('',*,*,#24657,.F.) ;
#32681 = ORIENTED_EDGE('',*,*,#24407,.F.) ;
#32682 = ORIENTED_EDGE('',*,*,#24657,.T.) ;
#32683 = ORIENTED_EDGE('',*,*,#24640,.F.) ;
#32684 = ORIENTED_EDGE('',*,*,#24658,.T.) ;
#32685 = ORIENTED_EDGE('',*,*,#24638,.F.) ;
#32686 = ORIENTED_EDGE('',*,*,#24643,.F.) ;
#32687 = ORIENTED_EDGE('',*,*,#24645,.F.) ;
#32688 = ORIENTED_EDGE('',*,*,#24647,.F.) ;
#32689 = ORIENTED_EDGE('',*,*,#24649,.F.) ;
#32690 = ORIENTED_EDGE('',*,*,#24651,.F.) ;
#32691 = ORIENTED_EDGE('',*,*,#24653,.F.) ;
#32692 = ORIENTED_EDGE('',*,*,#24656,.F.) ;
#32693 = ORIENTED_EDGE('',*,*,#24659,.F.) ;
#32694 = ORIENTED_EDGE('',*,*,#24660,.F.) ;
#32695 = ORIENTED_EDGE('',*,*,#24661,.F.) ;
#32696 = ORIENTED_EDGE('',*,*,#24662,.F.) ;
#32697 = ORIENTED_EDGE('',*,*,#24663,.F.) ;
#32698 = ORIENTED_EDGE('',*,*,#24664,.F.) ;
#32699 = ORIENTED_EDGE('',*,*,#24665,.T.) ;
#32700 = ORIENTED_EDGE('',*,*,#24663,.T.) ;
#32701 = ORIENTED_EDGE('',*,*,#24666,.T.) ;
#32702 = ORIENTED_EDGE('',*,*,#24660,.T.) ;
#32703 = ORIENTED_EDGE('',*,*,#24667,.T.) ;
#32704 = ORIENTED_EDGE('',*,*,#24668,.F.) ;
#32705 = ORIENTED_EDGE('',*,*,#24669,.F.) ;
#32706 = ORIENTED_EDGE('',*,*,#24670,.F.) ;
#32707 = ORIENTED_EDGE('',*,*,#24671,.F.) ;
#32708 = ORIENTED_EDGE('',*,*,#24672,.F.) ;
#32709 = ORIENTED_EDGE('',*,*,#24669,.T.) ;
#32710 = ORIENTED_EDGE('',*,*,#24673,.T.) ;
#32711 = ORIENTED_EDGE('',*,*,#24659,.T.) ;
#32712 = ORIENTED_EDGE('',*,*,#24674,.T.) ;
#32713 = ORIENTED_EDGE('',*,*,#24670,.T.) ;
#32714 = ORIENTED_EDGE('',*,*,#24675,.T.) ;
#32715 = ORIENTED_EDGE('',*,*,#24676,.T.) ;
#32716 = ORIENTED_EDGE('',*,*,#24677,.T.) ;
#32717 = ORIENTED_EDGE('',*,*,#24676,.F.) ;
#32718 = ORIENTED_EDGE('',*,*,#24678,.T.) ;
#32719 = ORIENTED_EDGE('',*,*,#24679,.T.) ;
#32720 = ORIENTED_EDGE('',*,*,#24680,.T.) ;
#32721 = ORIENTED_EDGE('',*,*,#24681,.T.) ;
#32722 = ORIENTED_EDGE('',*,*,#24682,.T.) ;
#32723 = ORIENTED_EDGE('',*,*,#24679,.F.) ;
#32724 = ORIENTED_EDGE('',*,*,#24683,.T.) ;
#32725 = ORIENTED_EDGE('',*,*,#24681,.F.) ;
#32726 = ORIENTED_EDGE('',*,*,#24684,.T.) ;
#32727 = ORIENTED_EDGE('',*,*,#24685,.T.) ;
#32728 = ORIENTED_EDGE('',*,*,#24686,.T.) ;
#32729 = ORIENTED_EDGE('',*,*,#24661,.T.) ;
#32730 = ORIENTED_EDGE('',*,*,#24687,.T.) ;
#32731 = ORIENTED_EDGE('',*,*,#24685,.F.) ;
#32732 = ORIENTED_EDGE('',*,*,#24688,.T.) ;
#32733 = ORIENTED_EDGE('',*,*,#24689,.T.) ;
#32734 = ORIENTED_EDGE('',*,*,#24690,.T.) ;
#32735 = ORIENTED_EDGE('',*,*,#24691,.F.) ;
#32736 = ORIENTED_EDGE('',*,*,#24692,.F.) ;
#32737 = ORIENTED_EDGE('',*,*,#24693,.F.) ;
#32738 = ORIENTED_EDGE('',*,*,#24694,.T.) ;
#32739 = ORIENTED_EDGE('',*,*,#24668,.T.) ;
#32740 = ORIENTED_EDGE('',*,*,#24672,.T.) ;
#32741 = ORIENTED_EDGE('',*,*,#24671,.T.) ;
#32742 = ORIENTED_EDGE('',*,*,#24695,.T.) ;
#32743 = ORIENTED_EDGE('',*,*,#24692,.T.) ;
#32744 = ORIENTED_EDGE('',*,*,#24696,.T.) ;
#32745 = ORIENTED_EDGE('',*,*,#24693,.T.) ;
#32746 = ORIENTED_EDGE('',*,*,#24697,.T.) ;
#32747 = ORIENTED_EDGE('',*,*,#24698,.T.) ;
#32748 = ORIENTED_EDGE('',*,*,#24699,.T.) ;
#32749 = ORIENTED_EDGE('',*,*,#24698,.F.) ;
#32750 = ORIENTED_EDGE('',*,*,#24700,.T.) ;
#32751 = ORIENTED_EDGE('',*,*,#24701,.T.) ;
#32752 = ORIENTED_EDGE('',*,*,#24702,.T.) ;
#32753 = ORIENTED_EDGE('',*,*,#24703,.T.) ;
#32754 = ORIENTED_EDGE('',*,*,#24704,.T.) ;
#32755 = ORIENTED_EDGE('',*,*,#24701,.F.) ;
#32756 = ORIENTED_EDGE('',*,*,#24705,.T.) ;
#32757 = ORIENTED_EDGE('',*,*,#24703,.F.) ;
#32758 = ORIENTED_EDGE('',*,*,#24706,.T.) ;
#32759 = ORIENTED_EDGE('',*,*,#24707,.T.) ;
#32760 = ORIENTED_EDGE('',*,*,#24708,.T.) ;
#32761 = ORIENTED_EDGE('',*,*,#24662,.T.) ;
#32762 = ORIENTED_EDGE('',*,*,#24709,.T.) ;
#32763 = ORIENTED_EDGE('',*,*,#24707,.F.) ;
#32764 = ORIENTED_EDGE('',*,*,#24710,.T.) ;
#32765 = ORIENTED_EDGE('',*,*,#24691,.T.) ;
#32766 = ORIENTED_EDGE('',*,*,#24711,.T.) ;
#32767 = ORIENTED_EDGE('',*,*,#24664,.T.) ;
#32768 = ORIENTED_EDGE('',*,*,#24712,.T.) ;
#32769 = ORIENTED_EDGE('',*,*,#24706,.F.) ;
#32770 = ORIENTED_EDGE('',*,*,#24713,.T.) ;
#32771 = ORIENTED_EDGE('',*,*,#24686,.F.) ;
#32772 = ORIENTED_EDGE('',*,*,#24714,.T.) ;
#32773 = ORIENTED_EDGE('',*,*,#24697,.F.) ;
#32774 = ORIENTED_EDGE('',*,*,#24695,.F.) ;
#32775 = ORIENTED_EDGE('',*,*,#24677,.F.) ;
#32776 = ORIENTED_EDGE('',*,*,#24715,.F.) ;
#32777 = ORIENTED_EDGE('',*,*,#24705,.F.) ;
#32778 = ORIENTED_EDGE('',*,*,#24716,.F.) ;
#32779 = ORIENTED_EDGE('',*,*,#24682,.F.) ;
#32780 = ORIENTED_EDGE('',*,*,#24713,.F.) ;
#32781 = ORIENTED_EDGE('',*,*,#24700,.F.) ;
#32782 = ORIENTED_EDGE('',*,*,#24715,.T.) ;
#32783 = ORIENTED_EDGE('',*,*,#24680,.F.) ;
#32784 = ORIENTED_EDGE('',*,*,#24716,.T.) ;
#32785 = ORIENTED_EDGE('',*,*,#24717,.F.) ;
#32786 = ORIENTED_EDGE('',*,*,#24718,.F.) ;
#32787 = ORIENTED_EDGE('',*,*,#24719,.F.) ;
#32788 = ORIENTED_EDGE('',*,*,#24720,.F.) ;
#32789 = ORIENTED_EDGE('',*,*,#24721,.F.) ;
#32790 = ORIENTED_EDGE('',*,*,#24722,.F.) ;
#32791 = ORIENTED_EDGE('',*,*,#24723,.F.) ;
#32792 = ORIENTED_EDGE('',*,*,#24724,.F.) ;
#32793 = ORIENTED_EDGE('',*,*,#24725,.F.) ;
#32794 = ORIENTED_EDGE('',*,*,#24726,.F.) ;
#32795 = ORIENTED_EDGE('',*,*,#24727,.F.) ;
#32796 = ORIENTED_EDGE('',*,*,#24728,.F.) ;
#32797 = ORIENTED_EDGE('',*,*,#24729,.F.) ;
#32798 = ORIENTED_EDGE('',*,*,#24730,.F.) ;
#32799 = ORIENTED_EDGE('',*,*,#24731,.F.) ;
#32800 = ORIENTED_EDGE('',*,*,#24732,.F.) ;
#32801 = ORIENTED_EDGE('',*,*,#24733,.F.) ;
#32802 = ORIENTED_EDGE('',*,*,#24734,.F.) ;
#32803 = ORIENTED_EDGE('',*,*,#24735,.F.) ;
#32804 = ORIENTED_EDGE('',*,*,#24694,.F.) ;
#32805 = ORIENTED_EDGE('',*,*,#24699,.F.) ;
#32806 = ORIENTED_EDGE('',*,*,#24702,.F.) ;
#32807 = ORIENTED_EDGE('',*,*,#24704,.F.) ;
#32808 = ORIENTED_EDGE('',*,*,#24708,.F.) ;
#32809 = ORIENTED_EDGE('',*,*,#24709,.F.) ;
#32810 = ORIENTED_EDGE('',*,*,#24665,.F.) ;
#32811 = ORIENTED_EDGE('',*,*,#24711,.F.) ;
#32812 = ORIENTED_EDGE('',*,*,#24690,.F.) ;
#32813 = ORIENTED_EDGE('',*,*,#24689,.F.) ;
#32814 = ORIENTED_EDGE('',*,*,#24667,.F.) ;
#32815 = ORIENTED_EDGE('',*,*,#24673,.F.) ;
#32816 = ORIENTED_EDGE('',*,*,#24696,.F.) ;
#32817 = ORIENTED_EDGE('',*,*,#24712,.F.) ;
#32818 = ORIENTED_EDGE('',*,*,#24674,.F.) ;
#32819 = ORIENTED_EDGE('',*,*,#24688,.F.) ;
#32820 = ORIENTED_EDGE('',*,*,#24684,.F.) ;
#32821 = ORIENTED_EDGE('',*,*,#24683,.F.) ;
#32822 = ORIENTED_EDGE('',*,*,#24678,.F.) ;
#32823 = ORIENTED_EDGE('',*,*,#24675,.F.) ;
#32824 = ORIENTED_EDGE('',*,*,#24736,.F.) ;
#32825 = ORIENTED_EDGE('',*,*,#24737,.F.) ;
#32826 = ORIENTED_EDGE('',*,*,#24738,.F.) ;
#32827 = ORIENTED_EDGE('',*,*,#24732,.T.) ;
#32828 = ORIENTED_EDGE('',*,*,#24739,.F.) ;
#32829 = ORIENTED_EDGE('',*,*,#24740,.F.) ;
#32830 = ORIENTED_EDGE('',*,*,#24741,.F.) ;
#32831 = ORIENTED_EDGE('',*,*,#24737,.T.) ;
#32832 = ORIENTED_EDGE('',*,*,#24742,.T.) ;
#32833 = ORIENTED_EDGE('',*,*,#24740,.T.) ;
#32834 = ORIENTED_EDGE('',*,*,#24743,.T.) ;
#32835 = ORIENTED_EDGE('',*,*,#24744,.F.) ;
#32836 = ORIENTED_EDGE('',*,*,#24745,.F.) ;
#32837 = ORIENTED_EDGE('',*,*,#24746,.F.) ;
#32838 = ORIENTED_EDGE('',*,*,#24730,.T.) ;
#32839 = ORIENTED_EDGE('',*,*,#24747,.F.) ;
#32840 = ORIENTED_EDGE('',*,*,#24748,.F.) ;
#32841 = ORIENTED_EDGE('',*,*,#24749,.F.) ;
#32842 = ORIENTED_EDGE('',*,*,#24734,.T.) ;
#32843 = ORIENTED_EDGE('',*,*,#24750,.F.) ;
#32844 = ORIENTED_EDGE('',*,*,#24751,.F.) ;
#32845 = ORIENTED_EDGE('',*,*,#24752,.F.) ;
#32846 = ORIENTED_EDGE('',*,*,#24745,.T.) ;
#32847 = ORIENTED_EDGE('',*,*,#24753,.T.) ;
#32848 = ORIENTED_EDGE('',*,*,#24751,.T.) ;
#32849 = ORIENTED_EDGE('',*,*,#24754,.T.) ;
#32850 = ORIENTED_EDGE('',*,*,#24755,.F.) ;
#32851 = ORIENTED_EDGE('',*,*,#24756,.F.) ;
#32852 = ORIENTED_EDGE('',*,*,#24757,.F.) ;
#32853 = ORIENTED_EDGE('',*,*,#24756,.T.) ;
#32854 = ORIENTED_EDGE('',*,*,#24758,.T.) ;
#32855 = ORIENTED_EDGE('',*,*,#24739,.T.) ;
#32856 = ORIENTED_EDGE('',*,*,#24759,.T.) ;
#32857 = ORIENTED_EDGE('',*,*,#24760,.F.) ;
#32858 = ORIENTED_EDGE('',*,*,#24761,.F.) ;
#32859 = ORIENTED_EDGE('',*,*,#24762,.F.) ;
#32860 = ORIENTED_EDGE('',*,*,#24728,.T.) ;
#32861 = ORIENTED_EDGE('',*,*,#24763,.F.) ;
#32862 = ORIENTED_EDGE('',*,*,#24764,.F.) ;
#32863 = ORIENTED_EDGE('',*,*,#24765,.F.) ;
#32864 = ORIENTED_EDGE('',*,*,#24766,.F.) ;
#32865 = ORIENTED_EDGE('',*,*,#24761,.T.) ;
#32866 = ORIENTED_EDGE('',*,*,#24767,.T.) ;
#32867 = ORIENTED_EDGE('',*,*,#24765,.T.) ;
#32868 = ORIENTED_EDGE('',*,*,#24764,.T.) ;
#32869 = ORIENTED_EDGE('',*,*,#24768,.T.) ;
#32870 = ORIENTED_EDGE('',*,*,#24766,.T.) ;
#32871 = ORIENTED_EDGE('',*,*,#24769,.T.) ;
#32872 = ORIENTED_EDGE('',*,*,#24757,.T.) ;
#32873 = ORIENTED_EDGE('',*,*,#24770,.T.) ;
#32874 = ORIENTED_EDGE('',*,*,#24752,.T.) ;
#32875 = ORIENTED_EDGE('',*,*,#24771,.T.) ;
#32876 = ORIENTED_EDGE('',*,*,#24763,.T.) ;
#32877 = ORIENTED_EDGE('',*,*,#24772,.T.) ;
#32878 = ORIENTED_EDGE('',*,*,#24744,.T.) ;
#32879 = ORIENTED_EDGE('',*,*,#24729,.T.) ;
#32880 = ORIENTED_EDGE('',*,*,#24762,.T.) ;
#32881 = ORIENTED_EDGE('',*,*,#24773,.T.) ;
#32882 = ORIENTED_EDGE('',*,*,#24760,.T.) ;
#32883 = ORIENTED_EDGE('',*,*,#24735,.T.) ;
#32884 = ORIENTED_EDGE('',*,*,#24749,.T.) ;
#32885 = ORIENTED_EDGE('',*,*,#24774,.T.) ;
#32886 = ORIENTED_EDGE('',*,*,#24755,.T.) ;
#32887 = ORIENTED_EDGE('',*,*,#24775,.T.) ;
#32888 = ORIENTED_EDGE('',*,*,#24748,.T.) ;
#32889 = ORIENTED_EDGE('',*,*,#24776,.T.) ;
#32890 = ORIENTED_EDGE('',*,*,#24741,.T.) ;
#32891 = ORIENTED_EDGE('',*,*,#24777,.T.) ;
#32892 = ORIENTED_EDGE('',*,*,#24750,.T.) ;
#32893 = ORIENTED_EDGE('',*,*,#24778,.T.) ;
#32894 = ORIENTED_EDGE('',*,*,#24747,.T.) ;
#32895 = ORIENTED_EDGE('',*,*,#24733,.T.) ;
#32896 = ORIENTED_EDGE('',*,*,#24738,.T.) ;
#32897 = ORIENTED_EDGE('',*,*,#24779,.T.) ;
#32898 = ORIENTED_EDGE('',*,*,#24736,.T.) ;
#32899 = ORIENTED_EDGE('',*,*,#24731,.T.) ;
#32900 = ORIENTED_EDGE('',*,*,#24746,.T.) ;
#32901 = ORIENTED_EDGE('',*,*,#24780,.T.) ;
#32902 = ORIENTED_EDGE('',*,*,#24743,.F.) ;
#32903 = ORIENTED_EDGE('',*,*,#24758,.F.) ;
#32904 = ORIENTED_EDGE('',*,*,#24776,.F.) ;
#32905 = ORIENTED_EDGE('',*,*,#24779,.F.) ;
#32906 = ORIENTED_EDGE('',*,*,#24754,.F.) ;
#32907 = ORIENTED_EDGE('',*,*,#24777,.F.) ;
#32908 = ORIENTED_EDGE('',*,*,#24742,.F.) ;
#32909 = ORIENTED_EDGE('',*,*,#24780,.F.) ;
#32910 = ORIENTED_EDGE('',*,*,#24759,.F.) ;
#32911 = ORIENTED_EDGE('',*,*,#24778,.F.) ;
#32912 = ORIENTED_EDGE('',*,*,#24772,.F.) ;
#32913 = ORIENTED_EDGE('',*,*,#24770,.F.) ;
#32914 = ORIENTED_EDGE('',*,*,#24768,.F.) ;
#32915 = ORIENTED_EDGE('',*,*,#24771,.F.) ;
#32916 = ORIENTED_EDGE('',*,*,#24753,.F.) ;
#32917 = ORIENTED_EDGE('',*,*,#24773,.F.) ;
#32918 = ORIENTED_EDGE('',*,*,#24767,.F.) ;
#32919 = ORIENTED_EDGE('',*,*,#24774,.F.) ;
#32920 = ORIENTED_EDGE('',*,*,#24775,.F.) ;
#32921 = ORIENTED_EDGE('',*,*,#24769,.F.) ;
#32922 = ORIENTED_EDGE('',*,*,#24781,.T.) ;
#32923 = ORIENTED_EDGE('',*,*,#24782,.T.) ;
#32924 = ORIENTED_EDGE('',*,*,#24783,.T.) ;
#32925 = ORIENTED_EDGE('',*,*,#24784,.T.) ;
#32926 = ORIENTED_EDGE('',*,*,#24389,.T.) ;
#32927 = ORIENTED_EDGE('',*,*,#24785,.T.) ;
#32928 = ORIENTED_EDGE('',*,*,#24783,.F.) ;
#32929 = ORIENTED_EDGE('',*,*,#24786,.T.) ;
#32930 = ORIENTED_EDGE('',*,*,#24505,.F.) ;
#32931 = ORIENTED_EDGE('',*,*,#24787,.F.) ;
#32932 = ORIENTED_EDGE('',*,*,#24390,.F.) ;
#32933 = ORIENTED_EDGE('',*,*,#24788,.T.) ;
#32934 = ORIENTED_EDGE('',*,*,#24503,.F.) ;
#32935 = ORIENTED_EDGE('',*,*,#24788,.F.) ;
#32936 = ORIENTED_EDGE('',*,*,#24786,.F.) ;
#32937 = ORIENTED_EDGE('',*,*,#24789,.T.) ;
#32938 = ORIENTED_EDGE('',*,*,#24501,.F.) ;
#32939 = ORIENTED_EDGE('',*,*,#24789,.F.) ;
#32940 = ORIENTED_EDGE('',*,*,#24782,.F.) ;
#32941 = ORIENTED_EDGE('',*,*,#24790,.T.) ;
#32942 = ORIENTED_EDGE('',*,*,#24499,.F.) ;
#32943 = ORIENTED_EDGE('',*,*,#24790,.F.) ;
#32944 = ORIENTED_EDGE('',*,*,#24781,.F.) ;
#32945 = ORIENTED_EDGE('',*,*,#24791,.F.) ;
#32946 = ORIENTED_EDGE('',*,*,#24792,.T.) ;
#32947 = ORIENTED_EDGE('',*,*,#24793,.F.) ;
#32948 = ORIENTED_EDGE('',*,*,#24794,.F.) ;
#32949 = ORIENTED_EDGE('',*,*,#24795,.F.) ;
#32950 = ORIENTED_EDGE('',*,*,#24796,.F.) ;
#32951 = ORIENTED_EDGE('',*,*,#24378,.F.) ;
#32952 = ORIENTED_EDGE('',*,*,#24383,.T.) ;
#32953 = ORIENTED_EDGE('',*,*,#24795,.T.) ;
#32954 = ORIENTED_EDGE('',*,*,#24794,.T.) ;
#32955 = ORIENTED_EDGE('',*,*,#24543,.T.) ;
#32956 = ORIENTED_EDGE('',*,*,#24793,.T.) ;
#32957 = ORIENTED_EDGE('',*,*,#24717,.T.) ;
#32958 = ORIENTED_EDGE('',*,*,#24797,.T.) ;
#32959 = ORIENTED_EDGE('',*,*,#24544,.T.) ;
#32960 = ORIENTED_EDGE('',*,*,#24797,.F.) ;
#32961 = ORIENTED_EDGE('',*,*,#24727,.T.) ;
#32962 = ORIENTED_EDGE('',*,*,#24798,.T.) ;
#32963 = ORIENTED_EDGE('',*,*,#24539,.T.) ;
#32964 = ORIENTED_EDGE('',*,*,#24798,.F.) ;
#32965 = ORIENTED_EDGE('',*,*,#24726,.T.) ;
#32966 = ORIENTED_EDGE('',*,*,#24799,.T.) ;
#32967 = ORIENTED_EDGE('',*,*,#24537,.T.) ;
#32968 = ORIENTED_EDGE('',*,*,#24799,.F.) ;
#32969 = ORIENTED_EDGE('',*,*,#24725,.T.) ;
#32970 = ORIENTED_EDGE('',*,*,#24800,.T.) ;
#32971 = ORIENTED_EDGE('',*,*,#24534,.T.) ;
#32972 = ORIENTED_EDGE('',*,*,#24801,.T.) ;
#32973 = ORIENTED_EDGE('',*,*,#24802,.T.) ;
#32974 = ORIENTED_EDGE('',*,*,#24800,.F.) ;
#32975 = ORIENTED_EDGE('',*,*,#24724,.T.) ;
#32976 = ORIENTED_EDGE('',*,*,#24803,.T.) ;
#32977 = ORIENTED_EDGE('',*,*,#24804,.T.) ;
#32978 = ORIENTED_EDGE('',*,*,#24801,.F.) ;
#32979 = ORIENTED_EDGE('',*,*,#24723,.T.) ;
#32980 = ORIENTED_EDGE('',*,*,#24805,.T.) ;
#32981 = ORIENTED_EDGE('',*,*,#24806,.T.) ;
#32982 = ORIENTED_EDGE('',*,*,#24803,.F.) ;
#32983 = ORIENTED_EDGE('',*,*,#24722,.T.) ;
#32984 = ORIENTED_EDGE('',*,*,#24805,.F.) ;
#32985 = ORIENTED_EDGE('',*,*,#24721,.T.) ;
#32986 = ORIENTED_EDGE('',*,*,#24807,.T.) ;
#32987 = ORIENTED_EDGE('',*,*,#24808,.T.) ;
#32988 = ORIENTED_EDGE('',*,*,#24807,.F.) ;
#32989 = ORIENTED_EDGE('',*,*,#24720,.T.) ;
#32990 = ORIENTED_EDGE('',*,*,#24809,.T.) ;
#32991 = ORIENTED_EDGE('',*,*,#24810,.T.) ;
#32992 = ORIENTED_EDGE('',*,*,#24811,.T.) ;
#32993 = ORIENTED_EDGE('',*,*,#24385,.T.) ;
#32994 = ORIENTED_EDGE('',*,*,#24809,.F.) ;
#32995 = ORIENTED_EDGE('',*,*,#24719,.T.) ;
#32996 = ORIENTED_EDGE('',*,*,#24811,.F.) ;
#32997 = ORIENTED_EDGE('',*,*,#24718,.T.) ;
#32998 = ORIENTED_EDGE('',*,*,#24796,.T.) ;
#32999 = ORIENTED_EDGE('',*,*,#24382,.T.) ;
#33000 = ORIENTED_EDGE('',*,*,#24513,.F.) ;
#33001 = ORIENTED_EDGE('',*,*,#24812,.F.) ;
#33002 = ORIENTED_EDGE('',*,*,#24804,.F.) ;
#33003 = ORIENTED_EDGE('',*,*,#24813,.F.) ;
#33004 = ORIENTED_EDGE('',*,*,#24511,.F.) ;
#33005 = ORIENTED_EDGE('',*,*,#24813,.T.) ;
#33006 = ORIENTED_EDGE('',*,*,#24806,.F.) ;
#33007 = ORIENTED_EDGE('',*,*,#24814,.T.) ;
#33008 = ORIENTED_EDGE('',*,*,#24509,.F.) ;
#33009 = ORIENTED_EDGE('',*,*,#24814,.F.) ;
#33010 = ORIENTED_EDGE('',*,*,#24808,.F.) ;
#33011 = ORIENTED_EDGE('',*,*,#24815,.T.) ;
#33012 = ORIENTED_EDGE('',*,*,#24507,.F.) ;
#33013 = ORIENTED_EDGE('',*,*,#24815,.F.) ;
#33014 = ORIENTED_EDGE('',*,*,#24810,.F.) ;
#33015 = ORIENTED_EDGE('',*,*,#24384,.F.) ;
#33016 = ORIENTED_EDGE('',*,*,#24387,.F.) ;
#33017 = ORIENTED_EDGE('',*,*,#24787,.T.) ;
#33018 = ORIENTED_EDGE('',*,*,#24816,.T.) ;
#33019 = ORIENTED_EDGE('',*,*,#24817,.F.) ;
#33020 = ORIENTED_EDGE('',*,*,#24609,.F.) ;
#33021 = ORIENTED_EDGE('',*,*,#24607,.F.) ;
#33022 = ORIENTED_EDGE('',*,*,#24616,.F.) ;
#33023 = ORIENTED_EDGE('',*,*,#24594,.F.) ;
#33024 = ORIENTED_EDGE('',*,*,#24818,.F.) ;
#33025 = ORIENTED_EDGE('',*,*,#24602,.F.) ;
#33026 = ORIENTED_EDGE('',*,*,#24567,.F.) ;
#33027 = ORIENTED_EDGE('',*,*,#24596,.F.) ;
#33028 = ORIENTED_EDGE('',*,*,#24819,.T.) ;
#33029 = ORIENTED_EDGE('',*,*,#24604,.F.) ;
#33030 = ORIENTED_EDGE('',*,*,#24818,.T.) ;
#33031 = ORIENTED_EDGE('',*,*,#24475,.F.) ;
#33032 = ORIENTED_EDGE('',*,*,#24820,.T.) ;
#33033 = ORIENTED_EDGE('',*,*,#24634,.F.) ;
#33034 = ORIENTED_EDGE('',*,*,#24821,.T.) ;
#33035 = ORIENTED_EDGE('',*,*,#24474,.F.) ;
#33036 = ORIENTED_EDGE('',*,*,#24482,.F.) ;
#33037 = ORIENTED_EDGE('',*,*,#24635,.F.) ;
#33038 = ORIENTED_EDGE('',*,*,#24820,.F.) ;
#33039 = ORIENTED_EDGE('',*,*,#24479,.F.) ;
#33040 = ORIENTED_EDGE('',*,*,#24822,.T.) ;
#33041 = ORIENTED_EDGE('',*,*,#24628,.F.) ;
#33042 = ORIENTED_EDGE('',*,*,#24487,.T.) ;
#33043 = ORIENTED_EDGE('',*,*,#24413,.F.) ;
#33044 = ORIENTED_EDGE('',*,*,#24823,.T.) ;
#33045 = ORIENTED_EDGE('',*,*,#24654,.F.) ;
#33046 = ORIENTED_EDGE('',*,*,#24422,.T.) ;
#33047 = ORIENTED_EDGE('',*,*,#24515,.F.) ;
#33048 = ORIENTED_EDGE('',*,*,#24535,.T.) ;
#33049 = ORIENTED_EDGE('',*,*,#24802,.F.) ;
#33050 = ORIENTED_EDGE('',*,*,#24812,.T.) ;
#33051 = ORIENTED_EDGE('',*,*,#24710,.F.) ;
#33052 = ORIENTED_EDGE('',*,*,#24714,.F.) ;
#33053 = ORIENTED_EDGE('',*,*,#24687,.F.) ;
#33054 = ORIENTED_EDGE('',*,*,#24666,.F.) ;
#33055 = ORIENTED_EDGE('',*,*,#24412,.F.) ;
#33056 = ORIENTED_EDGE('',*,*,#24658,.F.) ;
#33057 = ORIENTED_EDGE('',*,*,#24655,.F.) ;
#33058 = ORIENTED_EDGE('',*,*,#24823,.F.) ;
#33059 = ORIENTED_EDGE('',*,*,#24478,.F.) ;
#33060 = ORIENTED_EDGE('',*,*,#24821,.F.) ;
#33061 = ORIENTED_EDGE('',*,*,#24629,.F.) ;
#33062 = ORIENTED_EDGE('',*,*,#24822,.F.) ;
#33063 = ORIENTED_EDGE('',*,*,#24599,.F.) ;
#33064 = ORIENTED_EDGE('',*,*,#24824,.T.) ;
#33065 = ORIENTED_EDGE('',*,*,#24606,.F.) ;
#33066 = ORIENTED_EDGE('',*,*,#24819,.F.) ;
#33067 = ORIENTED_EDGE('',*,*,#24377,.F.) ;
#33068 = ORIENTED_EDGE('',*,*,#24546,.F.) ;
#33069 = ORIENTED_EDGE('',*,*,#24548,.F.) ;
#33070 = ORIENTED_EDGE('',*,*,#24550,.F.) ;
#33071 = ORIENTED_EDGE('',*,*,#24552,.F.) ;
#33072 = ORIENTED_EDGE('',*,*,#24554,.F.) ;
#33073 = ORIENTED_EDGE('',*,*,#24556,.F.) ;
#33074 = ORIENTED_EDGE('',*,*,#24825,.F.) ;
#33075 = ORIENTED_EDGE('',*,*,#24791,.T.) ;
#33076 = ORIENTED_EDGE('',*,*,#24784,.F.) ;
#33077 = ORIENTED_EDGE('',*,*,#24785,.F.) ;
#33078 = ORIENTED_EDGE('',*,*,#24388,.F.) ;
#33079 = ORIENTED_EDGE('',*,*,#24370,.F.) ;
#33080 = ORIENTED_EDGE('',*,*,#24374,.F.) ;
#33081 = ORIENTED_EDGE('',*,*,#24615,.F.) ;
#33082 = ORIENTED_EDGE('',*,*,#24826,.T.) ;
#33083 = ORIENTED_EDGE('',*,*,#24816,.F.) ;
#33084 = ORIENTED_EDGE('',*,*,#24491,.T.) ;
#33085 = ORIENTED_EDGE('',*,*,#24601,.F.) ;
#33086 = ORIENTED_EDGE('',*,*,#24827,.F.) ;
#33087 = ORIENTED_EDGE('',*,*,#24610,.T.) ;
#33088 = ORIENTED_EDGE('',*,*,#24817,.T.) ;
#33089 = ORIENTED_EDGE('',*,*,#24826,.F.) ;
#33090 = ORIENTED_EDGE('',*,*,#24614,.T.) ;
#33091 = ORIENTED_EDGE('',*,*,#24598,.T.) ;
#33092 = ORIENTED_EDGE('',*,*,#24611,.T.) ;
#33093 = ORIENTED_EDGE('',*,*,#24827,.T.) ;
#33094 = ORIENTED_EDGE('',*,*,#24558,.F.) ;
#33095 = ORIENTED_EDGE('',*,*,#24824,.F.) ;
#33096 = ORIENTED_EDGE('',*,*,#24497,.F.) ;
#33097 = ORIENTED_EDGE('',*,*,#24792,.F.) ;
#33098 = ORIENTED_EDGE('',*,*,#24825,.T.) ;
#33099 = ORIENTED_EDGE('',*,*,#24555,.T.) ;
#33100 = ORIENTED_EDGE('',*,*,#24828,.T.) ;
#33101 = ORIENTED_EDGE('',*,*,#24829,.T.) ;
#33102 = ORIENTED_EDGE('',*,*,#24830,.T.) ;
#33103 = ORIENTED_EDGE('',*,*,#24831,.F.) ;
#33104 = ORIENTED_EDGE('',*,*,#24832,.T.) ;
#33105 = ORIENTED_EDGE('',*,*,#24833,.T.) ;
#33106 = ORIENTED_EDGE('',*,*,#24834,.T.) ;
#33107 = ORIENTED_EDGE('',*,*,#24835,.T.) ;
#33108 = ORIENTED_EDGE('',*,*,#24836,.T.) ;
#33109 = ORIENTED_EDGE('',*,*,#24837,.T.) ;
#33110 = ORIENTED_EDGE('',*,*,#24838,.T.) ;
#33111 = ORIENTED_EDGE('',*,*,#24829,.F.) ;
#33112 = ORIENTED_EDGE('',*,*,#24839,.T.) ;
#33113 = ORIENTED_EDGE('',*,*,#24840,.T.) ;
#33114 = ORIENTED_EDGE('',*,*,#24841,.T.) ;
#33115 = ORIENTED_EDGE('',*,*,#24837,.F.) ;
#33116 = ORIENTED_EDGE('',*,*,#24842,.T.) ;
#33117 = ORIENTED_EDGE('',*,*,#24840,.F.) ;
#33118 = ORIENTED_EDGE('',*,*,#24843,.T.) ;
#33119 = ORIENTED_EDGE('',*,*,#24844,.T.) ;
#33120 = ORIENTED_EDGE('',*,*,#24833,.F.) ;
#33121 = ORIENTED_EDGE('',*,*,#24845,.T.) ;
#33122 = ORIENTED_EDGE('',*,*,#24844,.F.) ;
#33123 = ORIENTED_EDGE('',*,*,#24846,.T.) ;
#33124 = ORIENTED_EDGE('',*,*,#24847,.T.) ;
#33125 = ORIENTED_EDGE('',*,*,#24835,.F.) ;
#33126 = ORIENTED_EDGE('',*,*,#24848,.T.) ;
#33127 = ORIENTED_EDGE('',*,*,#24849,.T.) ;
#33128 = ORIENTED_EDGE('',*,*,#24850,.T.) ;
#33129 = ORIENTED_EDGE('',*,*,#24849,.F.) ;
#33130 = ORIENTED_EDGE('',*,*,#24851,.T.) ;
#33131 = ORIENTED_EDGE('',*,*,#24831,.T.) ;
#33132 = ORIENTED_EDGE('',*,*,#24841,.F.) ;
#33133 = ORIENTED_EDGE('',*,*,#24852,.F.) ;
#33134 = ORIENTED_EDGE('',*,*,#24853,.F.) ;
#33135 = ORIENTED_EDGE('',*,*,#24854,.T.) ;
#33136 = ORIENTED_EDGE('',*,*,#24842,.F.) ;
#33137 = ORIENTED_EDGE('',*,*,#24855,.F.) ;
#33138 = ORIENTED_EDGE('',*,*,#24856,.F.) ;
#33139 = ORIENTED_EDGE('',*,*,#24852,.T.) ;
#33140 = ORIENTED_EDGE('',*,*,#24845,.F.) ;
#33141 = ORIENTED_EDGE('',*,*,#24857,.F.) ;
#33142 = ORIENTED_EDGE('',*,*,#24858,.F.) ;
#33143 = ORIENTED_EDGE('',*,*,#24855,.T.) ;
#33144 = ORIENTED_EDGE('',*,*,#24832,.F.) ;
#33145 = ORIENTED_EDGE('',*,*,#24859,.F.) ;
#33146 = ORIENTED_EDGE('',*,*,#24860,.F.) ;
#33147 = ORIENTED_EDGE('',*,*,#24857,.T.) ;
#33148 = ORIENTED_EDGE('',*,*,#24861,.F.) ;
#33149 = ORIENTED_EDGE('',*,*,#24862,.F.) ;
#33150 = ORIENTED_EDGE('',*,*,#24863,.F.) ;
#33151 = ORIENTED_EDGE('',*,*,#24864,.F.) ;
#33152 = ORIENTED_EDGE('',*,*,#24865,.F.) ;
#33153 = ORIENTED_EDGE('',*,*,#24866,.F.) ;
#33154 = ORIENTED_EDGE('',*,*,#24867,.F.) ;
#33155 = ORIENTED_EDGE('',*,*,#24868,.F.) ;
#33156 = ORIENTED_EDGE('',*,*,#24869,.F.) ;
#33157 = ORIENTED_EDGE('',*,*,#24870,.F.) ;
#33158 = ORIENTED_EDGE('',*,*,#24871,.F.) ;
#33159 = ORIENTED_EDGE('',*,*,#24872,.F.) ;
#33160 = ORIENTED_EDGE('',*,*,#24873,.F.) ;
#33161 = ORIENTED_EDGE('',*,*,#24874,.F.) ;
#33162 = ORIENTED_EDGE('',*,*,#24875,.F.) ;
#33163 = ORIENTED_EDGE('',*,*,#24876,.F.) ;
#33164 = ORIENTED_EDGE('',*,*,#24877,.F.) ;
#33165 = ORIENTED_EDGE('',*,*,#24878,.F.) ;
#33166 = ORIENTED_EDGE('',*,*,#24879,.F.) ;
#33167 = ORIENTED_EDGE('',*,*,#24834,.F.) ;
#33168 = ORIENTED_EDGE('',*,*,#24846,.F.) ;
#33169 = ORIENTED_EDGE('',*,*,#24843,.F.) ;
#33170 = ORIENTED_EDGE('',*,*,#24839,.F.) ;
#33171 = ORIENTED_EDGE('',*,*,#24836,.F.) ;
#33172 = ORIENTED_EDGE('',*,*,#24828,.F.) ;
#33173 = ORIENTED_EDGE('',*,*,#24851,.F.) ;
#33174 = ORIENTED_EDGE('',*,*,#24848,.F.) ;
#33175 = ORIENTED_EDGE('',*,*,#24868,.T.) ;
#33176 = ORIENTED_EDGE('',*,*,#24880,.T.) ;
#33177 = ORIENTED_EDGE('',*,*,#24881,.T.) ;
#33178 = ORIENTED_EDGE('',*,*,#24882,.F.) ;
#33179 = ORIENTED_EDGE('',*,*,#24867,.T.) ;
#33180 = ORIENTED_EDGE('',*,*,#24883,.T.) ;
#33181 = ORIENTED_EDGE('',*,*,#24884,.T.) ;
#33182 = ORIENTED_EDGE('',*,*,#24880,.F.) ;
#33183 = ORIENTED_EDGE('',*,*,#24866,.T.) ;
#33184 = ORIENTED_EDGE('',*,*,#24885,.T.) ;
#33185 = ORIENTED_EDGE('',*,*,#24886,.T.) ;
#33186 = ORIENTED_EDGE('',*,*,#24883,.F.) ;
#33187 = ORIENTED_EDGE('',*,*,#24865,.T.) ;
#33188 = ORIENTED_EDGE('',*,*,#24887,.T.) ;
#33189 = ORIENTED_EDGE('',*,*,#24888,.T.) ;
#33190 = ORIENTED_EDGE('',*,*,#24885,.F.) ;
#33191 = ORIENTED_EDGE('',*,*,#24864,.T.) ;
#33192 = ORIENTED_EDGE('',*,*,#24889,.T.) ;
#33193 = ORIENTED_EDGE('',*,*,#24890,.T.) ;
#33194 = ORIENTED_EDGE('',*,*,#24887,.F.) ;
#33195 = ORIENTED_EDGE('',*,*,#24891,.T.) ;
#33196 = ORIENTED_EDGE('',*,*,#24892,.T.) ;
#33197 = ORIENTED_EDGE('',*,*,#24875,.T.) ;
#33198 = ORIENTED_EDGE('',*,*,#24893,.T.) ;
#33199 = ORIENTED_EDGE('',*,*,#24863,.T.) ;
#33200 = ORIENTED_EDGE('',*,*,#24894,.T.) ;
#33201 = ORIENTED_EDGE('',*,*,#24895,.T.) ;
#33202 = ORIENTED_EDGE('',*,*,#24889,.F.) ;
#33203 = ORIENTED_EDGE('',*,*,#24896,.T.) ;
#33204 = ORIENTED_EDGE('',*,*,#24897,.T.) ;
#33205 = ORIENTED_EDGE('',*,*,#24861,.T.) ;
#33206 = ORIENTED_EDGE('',*,*,#24898,.T.) ;
#33207 = ORIENTED_EDGE('',*,*,#24862,.T.) ;
#33208 = ORIENTED_EDGE('',*,*,#24897,.F.) ;
#33209 = ORIENTED_EDGE('',*,*,#24899,.T.) ;
#33210 = ORIENTED_EDGE('',*,*,#24894,.F.) ;
#33211 = ORIENTED_EDGE('',*,*,#24879,.T.) ;
#33212 = ORIENTED_EDGE('',*,*,#24900,.T.) ;
#33213 = ORIENTED_EDGE('',*,*,#24901,.T.) ;
#33214 = ORIENTED_EDGE('',*,*,#24898,.F.) ;
#33215 = ORIENTED_EDGE('',*,*,#24902,.T.) ;
#33216 = ORIENTED_EDGE('',*,*,#24900,.F.) ;
#33217 = ORIENTED_EDGE('',*,*,#24878,.T.) ;
#33218 = ORIENTED_EDGE('',*,*,#24903,.T.) ;
#33219 = ORIENTED_EDGE('',*,*,#24904,.T.) ;
#33220 = ORIENTED_EDGE('',*,*,#24903,.F.) ;
#33221 = ORIENTED_EDGE('',*,*,#24877,.T.) ;
#33222 = ORIENTED_EDGE('',*,*,#24905,.T.) ;
#33223 = ORIENTED_EDGE('',*,*,#24892,.F.) ;
#33224 = ORIENTED_EDGE('',*,*,#24906,.T.) ;
#33225 = ORIENTED_EDGE('',*,*,#24905,.F.) ;
#33226 = ORIENTED_EDGE('',*,*,#24876,.T.) ;
#33227 = ORIENTED_EDGE('',*,*,#24907,.T.) ;
#33228 = ORIENTED_EDGE('',*,*,#24893,.F.) ;
#33229 = ORIENTED_EDGE('',*,*,#24874,.T.) ;
#33230 = ORIENTED_EDGE('',*,*,#24908,.T.) ;
#33231 = ORIENTED_EDGE('',*,*,#24909,.T.) ;
#33232 = ORIENTED_EDGE('',*,*,#24908,.F.) ;
#33233 = ORIENTED_EDGE('',*,*,#24873,.T.) ;
#33234 = ORIENTED_EDGE('',*,*,#24910,.T.) ;
#33235 = ORIENTED_EDGE('',*,*,#24911,.T.) ;
#33236 = ORIENTED_EDGE('',*,*,#24910,.F.) ;
#33237 = ORIENTED_EDGE('',*,*,#24872,.T.) ;
#33238 = ORIENTED_EDGE('',*,*,#24912,.T.) ;
#33239 = ORIENTED_EDGE('',*,*,#24913,.T.) ;
#33240 = ORIENTED_EDGE('',*,*,#24912,.F.) ;
#33241 = ORIENTED_EDGE('',*,*,#24871,.T.) ;
#33242 = ORIENTED_EDGE('',*,*,#24914,.T.) ;
#33243 = ORIENTED_EDGE('',*,*,#24915,.T.) ;
#33244 = ORIENTED_EDGE('',*,*,#24914,.F.) ;
#33245 = ORIENTED_EDGE('',*,*,#24870,.T.) ;
#33246 = ORIENTED_EDGE('',*,*,#24916,.T.) ;
#33247 = ORIENTED_EDGE('',*,*,#24917,.T.) ;
#33248 = ORIENTED_EDGE('',*,*,#24916,.F.) ;
#33249 = ORIENTED_EDGE('',*,*,#24869,.T.) ;
#33250 = ORIENTED_EDGE('',*,*,#24882,.T.) ;
#33251 = ORIENTED_EDGE('',*,*,#24915,.F.) ;
#33252 = ORIENTED_EDGE('',*,*,#24918,.F.) ;
#33253 = ORIENTED_EDGE('',*,*,#24919,.F.) ;
#33254 = ORIENTED_EDGE('',*,*,#24920,.T.) ;
#33255 = ORIENTED_EDGE('',*,*,#24917,.F.) ;
#33256 = ORIENTED_EDGE('',*,*,#24921,.F.) ;
#33257 = ORIENTED_EDGE('',*,*,#24922,.F.) ;
#33258 = ORIENTED_EDGE('',*,*,#24918,.T.) ;
#33259 = ORIENTED_EDGE('',*,*,#24881,.F.) ;
#33260 = ORIENTED_EDGE('',*,*,#24923,.F.) ;
#33261 = ORIENTED_EDGE('',*,*,#24924,.F.) ;
#33262 = ORIENTED_EDGE('',*,*,#24921,.T.) ;
#33263 = ORIENTED_EDGE('',*,*,#24884,.F.) ;
#33264 = ORIENTED_EDGE('',*,*,#24925,.F.) ;
#33265 = ORIENTED_EDGE('',*,*,#24926,.F.) ;
#33266 = ORIENTED_EDGE('',*,*,#24923,.T.) ;
#33267 = ORIENTED_EDGE('',*,*,#24886,.F.) ;
#33268 = ORIENTED_EDGE('',*,*,#24927,.F.) ;
#33269 = ORIENTED_EDGE('',*,*,#24928,.F.) ;
#33270 = ORIENTED_EDGE('',*,*,#24925,.T.) ;
#33271 = ORIENTED_EDGE('',*,*,#24888,.F.) ;
#33272 = ORIENTED_EDGE('',*,*,#24929,.F.) ;
#33273 = ORIENTED_EDGE('',*,*,#24930,.F.) ;
#33274 = ORIENTED_EDGE('',*,*,#24927,.T.) ;
#33275 = ORIENTED_EDGE('',*,*,#24890,.F.) ;
#33276 = ORIENTED_EDGE('',*,*,#24931,.F.) ;
#33277 = ORIENTED_EDGE('',*,*,#24932,.F.) ;
#33278 = ORIENTED_EDGE('',*,*,#24929,.T.) ;
#33279 = ORIENTED_EDGE('',*,*,#24895,.F.) ;
#33280 = ORIENTED_EDGE('',*,*,#24933,.F.) ;
#33281 = ORIENTED_EDGE('',*,*,#24934,.F.) ;
#33282 = ORIENTED_EDGE('',*,*,#24931,.T.) ;
#33283 = ORIENTED_EDGE('',*,*,#24899,.F.) ;
#33284 = ORIENTED_EDGE('',*,*,#24935,.F.) ;
#33285 = ORIENTED_EDGE('',*,*,#24936,.F.) ;
#33286 = ORIENTED_EDGE('',*,*,#24933,.T.) ;
#33287 = ORIENTED_EDGE('',*,*,#24896,.F.) ;
#33288 = ORIENTED_EDGE('',*,*,#24937,.F.) ;
#33289 = ORIENTED_EDGE('',*,*,#24938,.F.) ;
#33290 = ORIENTED_EDGE('',*,*,#24935,.T.) ;
#33291 = ORIENTED_EDGE('',*,*,#24939,.T.) ;
#33292 = ORIENTED_EDGE('',*,*,#24940,.T.) ;
#33293 = ORIENTED_EDGE('',*,*,#24941,.T.) ;
#33294 = ORIENTED_EDGE('',*,*,#24942,.F.) ;
#33295 = ORIENTED_EDGE('',*,*,#24943,.T.) ;
#33296 = ORIENTED_EDGE('',*,*,#24944,.T.) ;
#33297 = ORIENTED_EDGE('',*,*,#24945,.T.) ;
#33298 = ORIENTED_EDGE('',*,*,#24858,.T.) ;
#33299 = ORIENTED_EDGE('',*,*,#24946,.T.) ;
#33300 = ORIENTED_EDGE('',*,*,#24947,.T.) ;
#33301 = ORIENTED_EDGE('',*,*,#24853,.T.) ;
#33302 = ORIENTED_EDGE('',*,*,#24948,.T.) ;
#33303 = ORIENTED_EDGE('',*,*,#24949,.T.) ;
#33304 = ORIENTED_EDGE('',*,*,#24947,.F.) ;
#33305 = ORIENTED_EDGE('',*,*,#24950,.T.) ;
#33306 = ORIENTED_EDGE('',*,*,#24951,.T.) ;
#33307 = ORIENTED_EDGE('',*,*,#24952,.T.) ;
#33308 = ORIENTED_EDGE('',*,*,#24948,.F.) ;
#33309 = ORIENTED_EDGE('',*,*,#24856,.T.) ;
#33310 = ORIENTED_EDGE('',*,*,#24945,.F.) ;
#33311 = ORIENTED_EDGE('',*,*,#24953,.T.) ;
#33312 = ORIENTED_EDGE('',*,*,#24951,.F.) ;
#33313 = ORIENTED_EDGE('',*,*,#24954,.T.) ;
#33314 = ORIENTED_EDGE('',*,*,#24955,.T.) ;
#33315 = ORIENTED_EDGE('',*,*,#24956,.T.) ;
#33316 = ORIENTED_EDGE('',*,*,#24955,.F.) ;
#33317 = ORIENTED_EDGE('',*,*,#24957,.T.) ;
#33318 = ORIENTED_EDGE('',*,*,#24942,.T.) ;
#33319 = ORIENTED_EDGE('',*,*,#24958,.T.) ;
#33320 = ORIENTED_EDGE('',*,*,#24943,.F.) ;
#33321 = ORIENTED_EDGE('',*,*,#24860,.T.) ;
#33322 = ORIENTED_EDGE('',*,*,#24940,.F.) ;
#33323 = ORIENTED_EDGE('',*,*,#24946,.F.) ;
#33324 = ORIENTED_EDGE('',*,*,#24952,.F.) ;
#33325 = ORIENTED_EDGE('',*,*,#24944,.F.) ;
#33326 = ORIENTED_EDGE('',*,*,#24958,.F.) ;
#33327 = ORIENTED_EDGE('',*,*,#24939,.F.) ;
#33328 = ORIENTED_EDGE('',*,*,#24957,.F.) ;
#33329 = ORIENTED_EDGE('',*,*,#24954,.F.) ;
#33330 = ORIENTED_EDGE('',*,*,#24950,.F.) ;
#33331 = ORIENTED_EDGE('',*,*,#24959,.T.) ;
#33332 = ORIENTED_EDGE('',*,*,#24960,.T.) ;
#33333 = ORIENTED_EDGE('',*,*,#24961,.T.) ;
#33334 = ORIENTED_EDGE('',*,*,#24962,.F.) ;
#33335 = ORIENTED_EDGE('',*,*,#24963,.T.) ;
#33336 = ORIENTED_EDGE('',*,*,#24960,.F.) ;
#33337 = ORIENTED_EDGE('',*,*,#24964,.T.) ;
#33338 = ORIENTED_EDGE('',*,*,#24965,.T.) ;
#33339 = ORIENTED_EDGE('',*,*,#24966,.T.) ;
#33340 = ORIENTED_EDGE('',*,*,#24965,.F.) ;
#33341 = ORIENTED_EDGE('',*,*,#24967,.T.) ;
#33342 = ORIENTED_EDGE('',*,*,#24962,.T.) ;
#33343 = ORIENTED_EDGE('',*,*,#24966,.F.) ;
#33344 = ORIENTED_EDGE('',*,*,#24968,.F.) ;
#33345 = ORIENTED_EDGE('',*,*,#24969,.F.) ;
#33346 = ORIENTED_EDGE('',*,*,#24970,.T.) ;
#33347 = ORIENTED_EDGE('',*,*,#24961,.F.) ;
#33348 = ORIENTED_EDGE('',*,*,#24971,.F.) ;
#33349 = ORIENTED_EDGE('',*,*,#24972,.F.) ;
#33350 = ORIENTED_EDGE('',*,*,#24968,.T.) ;
#33351 = ORIENTED_EDGE('',*,*,#24959,.F.) ;
#33352 = ORIENTED_EDGE('',*,*,#24967,.F.) ;
#33353 = ORIENTED_EDGE('',*,*,#24964,.F.) ;
#33354 = ORIENTED_EDGE('',*,*,#24973,.T.) ;
#33355 = ORIENTED_EDGE('',*,*,#24974,.T.) ;
#33356 = ORIENTED_EDGE('',*,*,#24975,.T.) ;
#33357 = ORIENTED_EDGE('',*,*,#24976,.F.) ;
#33358 = ORIENTED_EDGE('',*,*,#24977,.T.) ;
#33359 = ORIENTED_EDGE('',*,*,#24974,.F.) ;
#33360 = ORIENTED_EDGE('',*,*,#24978,.T.) ;
#33361 = ORIENTED_EDGE('',*,*,#24979,.T.) ;
#33362 = ORIENTED_EDGE('',*,*,#24980,.T.) ;
#33363 = ORIENTED_EDGE('',*,*,#24979,.F.) ;
#33364 = ORIENTED_EDGE('',*,*,#24981,.T.) ;
#33365 = ORIENTED_EDGE('',*,*,#24982,.T.) ;
#33366 = ORIENTED_EDGE('',*,*,#24983,.T.) ;
#33367 = ORIENTED_EDGE('',*,*,#24982,.F.) ;
#33368 = ORIENTED_EDGE('',*,*,#24984,.T.) ;
#33369 = ORIENTED_EDGE('',*,*,#24976,.T.) ;
#33370 = ORIENTED_EDGE('',*,*,#24983,.F.) ;
#33371 = ORIENTED_EDGE('',*,*,#24985,.F.) ;
#33372 = ORIENTED_EDGE('',*,*,#24986,.F.) ;
#33373 = ORIENTED_EDGE('',*,*,#24987,.T.) ;
#33374 = ORIENTED_EDGE('',*,*,#24975,.F.) ;
#33375 = ORIENTED_EDGE('',*,*,#24988,.F.) ;
#33376 = ORIENTED_EDGE('',*,*,#24989,.F.) ;
#33377 = ORIENTED_EDGE('',*,*,#24985,.T.) ;
#33378 = ORIENTED_EDGE('',*,*,#24973,.F.) ;
#33379 = ORIENTED_EDGE('',*,*,#24984,.F.) ;
#33380 = ORIENTED_EDGE('',*,*,#24981,.F.) ;
#33381 = ORIENTED_EDGE('',*,*,#24978,.F.) ;
#33382 = ORIENTED_EDGE('',*,*,#24990,.T.) ;
#33383 = ORIENTED_EDGE('',*,*,#24991,.T.) ;
#33384 = ORIENTED_EDGE('',*,*,#24992,.T.) ;
#33385 = ORIENTED_EDGE('',*,*,#24993,.F.) ;
#33386 = ORIENTED_EDGE('',*,*,#24994,.T.) ;
#33387 = ORIENTED_EDGE('',*,*,#24991,.F.) ;
#33388 = ORIENTED_EDGE('',*,*,#24995,.T.) ;
#33389 = ORIENTED_EDGE('',*,*,#24996,.T.) ;
#33390 = ORIENTED_EDGE('',*,*,#24997,.T.) ;
#33391 = ORIENTED_EDGE('',*,*,#24996,.F.) ;
#33392 = ORIENTED_EDGE('',*,*,#24998,.T.) ;
#33393 = ORIENTED_EDGE('',*,*,#24993,.T.) ;
#33394 = ORIENTED_EDGE('',*,*,#24997,.F.) ;
#33395 = ORIENTED_EDGE('',*,*,#24999,.F.) ;
#33396 = ORIENTED_EDGE('',*,*,#25000,.F.) ;
#33397 = ORIENTED_EDGE('',*,*,#25001,.T.) ;
#33398 = ORIENTED_EDGE('',*,*,#24992,.F.) ;
#33399 = ORIENTED_EDGE('',*,*,#25002,.F.) ;
#33400 = ORIENTED_EDGE('',*,*,#25003,.F.) ;
#33401 = ORIENTED_EDGE('',*,*,#24999,.T.) ;
#33402 = ORIENTED_EDGE('',*,*,#24990,.F.) ;
#33403 = ORIENTED_EDGE('',*,*,#24998,.F.) ;
#33404 = ORIENTED_EDGE('',*,*,#24995,.F.) ;
#33405 = ORIENTED_EDGE('',*,*,#25004,.T.) ;
#33406 = ORIENTED_EDGE('',*,*,#25005,.T.) ;
#33407 = ORIENTED_EDGE('',*,*,#24924,.T.) ;
#33408 = ORIENTED_EDGE('',*,*,#25006,.F.) ;
#33409 = ORIENTED_EDGE('',*,*,#25007,.T.) ;
#33410 = ORIENTED_EDGE('',*,*,#25008,.T.) ;
#33411 = ORIENTED_EDGE('',*,*,#24922,.T.) ;
#33412 = ORIENTED_EDGE('',*,*,#25005,.F.) ;
#33413 = ORIENTED_EDGE('',*,*,#25009,.T.) ;
#33414 = ORIENTED_EDGE('',*,*,#25010,.T.) ;
#33415 = ORIENTED_EDGE('',*,*,#24919,.T.) ;
#33416 = ORIENTED_EDGE('',*,*,#25008,.F.) ;
#33417 = ORIENTED_EDGE('',*,*,#24928,.T.) ;
#33418 = ORIENTED_EDGE('',*,*,#25011,.T.) ;
#33419 = ORIENTED_EDGE('',*,*,#25012,.T.) ;
#33420 = ORIENTED_EDGE('',*,*,#25013,.T.) ;
#33421 = ORIENTED_EDGE('',*,*,#25014,.T.) ;
#33422 = ORIENTED_EDGE('',*,*,#25015,.T.) ;
#33423 = ORIENTED_EDGE('',*,*,#25016,.T.) ;
#33424 = ORIENTED_EDGE('',*,*,#25010,.F.) ;
#33425 = ORIENTED_EDGE('',*,*,#25017,.T.) ;
#33426 = ORIENTED_EDGE('',*,*,#25018,.T.) ;
#33427 = ORIENTED_EDGE('',*,*,#25019,.T.) ;
#33428 = ORIENTED_EDGE('',*,*,#25015,.F.) ;
#33429 = ORIENTED_EDGE('',*,*,#25020,.T.) ;
#33430 = ORIENTED_EDGE('',*,*,#25021,.T.) ;
#33431 = ORIENTED_EDGE('',*,*,#25022,.T.) ;
#33432 = ORIENTED_EDGE('',*,*,#25018,.F.) ;
#33433 = ORIENTED_EDGE('',*,*,#25023,.T.) ;
#33434 = ORIENTED_EDGE('',*,*,#25024,.T.) ;
#33435 = ORIENTED_EDGE('',*,*,#25025,.T.) ;
#33436 = ORIENTED_EDGE('',*,*,#25021,.F.) ;
#33437 = ORIENTED_EDGE('',*,*,#25026,.T.) ;
#33438 = ORIENTED_EDGE('',*,*,#25027,.T.) ;
#33439 = ORIENTED_EDGE('',*,*,#25028,.T.) ;
#33440 = ORIENTED_EDGE('',*,*,#25024,.F.) ;
#33441 = ORIENTED_EDGE('',*,*,#25029,.T.) ;
#33442 = ORIENTED_EDGE('',*,*,#25030,.T.) ;
#33443 = ORIENTED_EDGE('',*,*,#25031,.T.) ;
#33444 = ORIENTED_EDGE('',*,*,#25032,.T.) ;
#33445 = ORIENTED_EDGE('',*,*,#25033,.T.) ;
#33446 = ORIENTED_EDGE('',*,*,#25034,.T.) ;
#33447 = ORIENTED_EDGE('',*,*,#25035,.T.) ;
#33448 = ORIENTED_EDGE('',*,*,#25027,.F.) ;
#33449 = ORIENTED_EDGE('',*,*,#25036,.T.) ;
#33450 = ORIENTED_EDGE('',*,*,#25037,.T.) ;
#33451 = ORIENTED_EDGE('',*,*,#25038,.T.) ;
#33452 = ORIENTED_EDGE('',*,*,#25034,.F.) ;
#33453 = ORIENTED_EDGE('',*,*,#25039,.T.) ;
#33454 = ORIENTED_EDGE('',*,*,#25037,.F.) ;
#33455 = ORIENTED_EDGE('',*,*,#25040,.T.) ;
#33456 = ORIENTED_EDGE('',*,*,#25030,.F.) ;
#33457 = ORIENTED_EDGE('',*,*,#24936,.T.) ;
#33458 = ORIENTED_EDGE('',*,*,#25041,.T.) ;
#33459 = ORIENTED_EDGE('',*,*,#25042,.T.) ;
#33460 = ORIENTED_EDGE('',*,*,#25043,.T.) ;
#33461 = ORIENTED_EDGE('',*,*,#25044,.T.) ;
#33462 = ORIENTED_EDGE('',*,*,#25041,.F.) ;
#33463 = ORIENTED_EDGE('',*,*,#24938,.T.) ;
#33464 = ORIENTED_EDGE('',*,*,#25032,.F.) ;
#33465 = ORIENTED_EDGE('',*,*,#24934,.T.) ;
#33466 = ORIENTED_EDGE('',*,*,#25043,.F.) ;
#33467 = ORIENTED_EDGE('',*,*,#25045,.T.) ;
#33468 = ORIENTED_EDGE('',*,*,#25046,.T.) ;
#33469 = ORIENTED_EDGE('',*,*,#24932,.T.) ;
#33470 = ORIENTED_EDGE('',*,*,#25046,.F.) ;
#33471 = ORIENTED_EDGE('',*,*,#25047,.T.) ;
#33472 = ORIENTED_EDGE('',*,*,#25048,.T.) ;
#33473 = ORIENTED_EDGE('',*,*,#25011,.F.) ;
#33474 = ORIENTED_EDGE('',*,*,#24930,.T.) ;
#33475 = ORIENTED_EDGE('',*,*,#25048,.F.) ;
#33476 = ORIENTED_EDGE('',*,*,#25049,.T.) ;
#33477 = ORIENTED_EDGE('',*,*,#24926,.T.) ;
#33478 = ORIENTED_EDGE('',*,*,#25013,.F.) ;
#33479 = ORIENTED_EDGE('',*,*,#25050,.T.) ;
#33480 = ORIENTED_EDGE('',*,*,#25006,.T.) ;
#33481 = ORIENTED_EDGE('',*,*,#24911,.F.) ;
#33482 = ORIENTED_EDGE('',*,*,#25051,.F.) ;
#33483 = ORIENTED_EDGE('',*,*,#25019,.F.) ;
#33484 = ORIENTED_EDGE('',*,*,#25052,.T.) ;
#33485 = ORIENTED_EDGE('',*,*,#24909,.F.) ;
#33486 = ORIENTED_EDGE('',*,*,#25052,.F.) ;
#33487 = ORIENTED_EDGE('',*,*,#25022,.F.) ;
#33488 = ORIENTED_EDGE('',*,*,#25053,.T.) ;
#33489 = ORIENTED_EDGE('',*,*,#24907,.F.) ;
#33490 = ORIENTED_EDGE('',*,*,#25053,.F.) ;
#33491 = ORIENTED_EDGE('',*,*,#25025,.F.) ;
#33492 = ORIENTED_EDGE('',*,*,#25054,.T.) ;
#33493 = ORIENTED_EDGE('',*,*,#24891,.F.) ;
#33494 = ORIENTED_EDGE('',*,*,#25054,.F.) ;
#33495 = ORIENTED_EDGE('',*,*,#25028,.F.) ;
#33496 = ORIENTED_EDGE('',*,*,#25055,.T.) ;
#33497 = ORIENTED_EDGE('',*,*,#24906,.F.) ;
#33498 = ORIENTED_EDGE('',*,*,#25055,.F.) ;
#33499 = ORIENTED_EDGE('',*,*,#25035,.F.) ;
#33500 = ORIENTED_EDGE('',*,*,#25056,.T.) ;
#33501 = ORIENTED_EDGE('',*,*,#24904,.F.) ;
#33502 = ORIENTED_EDGE('',*,*,#25056,.F.) ;
#33503 = ORIENTED_EDGE('',*,*,#25038,.F.) ;
#33504 = ORIENTED_EDGE('',*,*,#25057,.T.) ;
#33505 = ORIENTED_EDGE('',*,*,#24902,.F.) ;
#33506 = ORIENTED_EDGE('',*,*,#25057,.F.) ;
#33507 = ORIENTED_EDGE('',*,*,#25039,.F.) ;
#33508 = ORIENTED_EDGE('',*,*,#25058,.T.) ;
#33509 = ORIENTED_EDGE('',*,*,#24901,.F.) ;
#33510 = ORIENTED_EDGE('',*,*,#25058,.F.) ;
#33511 = ORIENTED_EDGE('',*,*,#25029,.F.) ;
#33512 = ORIENTED_EDGE('',*,*,#24937,.T.) ;
#33513 = ORIENTED_EDGE('',*,*,#25059,.F.) ;
#33514 = ORIENTED_EDGE('',*,*,#25060,.F.) ;
#33515 = ORIENTED_EDGE('',*,*,#25061,.F.) ;
#33516 = ORIENTED_EDGE('',*,*,#25062,.F.) ;
#33517 = ORIENTED_EDGE('',*,*,#25063,.F.) ;
#33518 = ORIENTED_EDGE('',*,*,#25064,.F.) ;
#33519 = ORIENTED_EDGE('',*,*,#25065,.F.) ;
#33520 = ORIENTED_EDGE('',*,*,#25066,.F.) ;
#33521 = ORIENTED_EDGE('',*,*,#25067,.F.) ;
#33522 = ORIENTED_EDGE('',*,*,#25068,.F.) ;
#33523 = ORIENTED_EDGE('',*,*,#25069,.F.) ;
#33524 = ORIENTED_EDGE('',*,*,#25070,.F.) ;
#33525 = ORIENTED_EDGE('',*,*,#25071,.F.) ;
#33526 = ORIENTED_EDGE('',*,*,#25072,.F.) ;
#33527 = ORIENTED_EDGE('',*,*,#25073,.F.) ;
#33528 = ORIENTED_EDGE('',*,*,#25074,.F.) ;
#33529 = ORIENTED_EDGE('',*,*,#25075,.F.) ;
#33530 = ORIENTED_EDGE('',*,*,#25076,.F.) ;
#33531 = ORIENTED_EDGE('',*,*,#25077,.F.) ;
#33532 = ORIENTED_EDGE('',*,*,#25078,.F.) ;
#33533 = ORIENTED_EDGE('',*,*,#25079,.F.) ;
#33534 = ORIENTED_EDGE('',*,*,#25080,.F.) ;
#33535 = ORIENTED_EDGE('',*,*,#25081,.F.) ;
#33536 = ORIENTED_EDGE('',*,*,#25082,.F.) ;
#33537 = ORIENTED_EDGE('',*,*,#25083,.F.) ;
#33538 = ORIENTED_EDGE('',*,*,#25084,.F.) ;
#33539 = ORIENTED_EDGE('',*,*,#25085,.F.) ;
#33540 = ORIENTED_EDGE('',*,*,#25086,.F.) ;
#33541 = ORIENTED_EDGE('',*,*,#25087,.F.) ;
#33542 = ORIENTED_EDGE('',*,*,#25088,.F.) ;
#33543 = ORIENTED_EDGE('',*,*,#25089,.F.) ;
#33544 = ORIENTED_EDGE('',*,*,#25090,.F.) ;
#33545 = ORIENTED_EDGE('',*,*,#25091,.F.) ;
#33546 = ORIENTED_EDGE('',*,*,#25092,.F.) ;
#33547 = ORIENTED_EDGE('',*,*,#25093,.F.) ;
#33548 = ORIENTED_EDGE('',*,*,#25094,.F.) ;
#33549 = ORIENTED_EDGE('',*,*,#25095,.F.) ;
#33550 = ORIENTED_EDGE('',*,*,#25096,.F.) ;
#33551 = ORIENTED_EDGE('',*,*,#25097,.F.) ;
#33552 = ORIENTED_EDGE('',*,*,#25098,.F.) ;
#33553 = ORIENTED_EDGE('',*,*,#25099,.F.) ;
#33554 = ORIENTED_EDGE('',*,*,#25100,.F.) ;
#33555 = ORIENTED_EDGE('',*,*,#25101,.F.) ;
#33556 = ORIENTED_EDGE('',*,*,#25102,.F.) ;
#33557 = ORIENTED_EDGE('',*,*,#25103,.F.) ;
#33558 = ORIENTED_EDGE('',*,*,#25104,.F.) ;
#33559 = ORIENTED_EDGE('',*,*,#25105,.F.) ;
#33560 = ORIENTED_EDGE('',*,*,#25106,.F.) ;
#33561 = ORIENTED_EDGE('',*,*,#25107,.F.) ;
#33562 = ORIENTED_EDGE('',*,*,#25108,.F.) ;
#33563 = ORIENTED_EDGE('',*,*,#25109,.F.) ;
#33564 = ORIENTED_EDGE('',*,*,#25110,.F.) ;
#33565 = ORIENTED_EDGE('',*,*,#25111,.F.) ;
#33566 = ORIENTED_EDGE('',*,*,#25112,.F.) ;
#33567 = ORIENTED_EDGE('',*,*,#25113,.F.) ;
#33568 = ORIENTED_EDGE('',*,*,#25114,.F.) ;
#33569 = ORIENTED_EDGE('',*,*,#25115,.F.) ;
#33570 = ORIENTED_EDGE('',*,*,#25116,.F.) ;
#33571 = ORIENTED_EDGE('',*,*,#25117,.F.) ;
#33572 = ORIENTED_EDGE('',*,*,#25118,.F.) ;
#33573 = ORIENTED_EDGE('',*,*,#25119,.F.) ;
#33574 = ORIENTED_EDGE('',*,*,#25120,.F.) ;
#33575 = ORIENTED_EDGE('',*,*,#25121,.F.) ;
#33576 = ORIENTED_EDGE('',*,*,#25122,.F.) ;
#33577 = ORIENTED_EDGE('',*,*,#25123,.F.) ;
#33578 = ORIENTED_EDGE('',*,*,#25124,.F.) ;
#33579 = ORIENTED_EDGE('',*,*,#25125,.F.) ;
#33580 = ORIENTED_EDGE('',*,*,#25126,.F.) ;
#33581 = ORIENTED_EDGE('',*,*,#25127,.F.) ;
#33582 = ORIENTED_EDGE('',*,*,#25128,.T.) ;
#33583 = ORIENTED_EDGE('',*,*,#25129,.F.) ;
#33584 = ORIENTED_EDGE('',*,*,#25130,.F.) ;
#33585 = ORIENTED_EDGE('',*,*,#25131,.F.) ;
#33586 = ORIENTED_EDGE('',*,*,#25132,.T.) ;
#33587 = ORIENTED_EDGE('',*,*,#25133,.F.) ;
#33588 = ORIENTED_EDGE('',*,*,#25134,.F.) ;
#33589 = ORIENTED_EDGE('',*,*,#25135,.F.) ;
#33590 = ORIENTED_EDGE('',*,*,#25136,.F.) ;
#33591 = ORIENTED_EDGE('',*,*,#25137,.F.) ;
#33592 = ORIENTED_EDGE('',*,*,#25138,.F.) ;
#33593 = ORIENTED_EDGE('',*,*,#25139,.F.) ;
#33594 = ORIENTED_EDGE('',*,*,#25140,.F.) ;
#33595 = ORIENTED_EDGE('',*,*,#25141,.F.) ;
#33596 = ORIENTED_EDGE('',*,*,#25142,.F.) ;
#33597 = ORIENTED_EDGE('',*,*,#25143,.F.) ;
#33598 = ORIENTED_EDGE('',*,*,#25144,.F.) ;
#33599 = ORIENTED_EDGE('',*,*,#25145,.F.) ;
#33600 = ORIENTED_EDGE('',*,*,#25146,.F.) ;
#33601 = ORIENTED_EDGE('',*,*,#25147,.F.) ;
#33602 = ORIENTED_EDGE('',*,*,#25148,.F.) ;
#33603 = ORIENTED_EDGE('',*,*,#25149,.F.) ;
#33604 = ORIENTED_EDGE('',*,*,#25150,.F.) ;
#33605 = ORIENTED_EDGE('',*,*,#25151,.F.) ;
#33606 = ORIENTED_EDGE('',*,*,#25152,.F.) ;
#33607 = ORIENTED_EDGE('',*,*,#25153,.F.) ;
#33608 = ORIENTED_EDGE('',*,*,#25154,.F.) ;
#33609 = ORIENTED_EDGE('',*,*,#25155,.F.) ;
#33610 = ORIENTED_EDGE('',*,*,#25156,.F.) ;
#33611 = ORIENTED_EDGE('',*,*,#25157,.F.) ;
#33612 = ORIENTED_EDGE('',*,*,#25158,.F.) ;
#33613 = ORIENTED_EDGE('',*,*,#25159,.F.) ;
#33614 = ORIENTED_EDGE('',*,*,#25160,.F.) ;
#33615 = ORIENTED_EDGE('',*,*,#25161,.F.) ;
#33616 = ORIENTED_EDGE('',*,*,#25162,.F.) ;
#33617 = ORIENTED_EDGE('',*,*,#25163,.F.) ;
#33618 = ORIENTED_EDGE('',*,*,#25164,.F.) ;
#33619 = ORIENTED_EDGE('',*,*,#25165,.F.) ;
#33620 = ORIENTED_EDGE('',*,*,#25166,.F.) ;
#33621 = ORIENTED_EDGE('',*,*,#25167,.F.) ;
#33622 = ORIENTED_EDGE('',*,*,#25168,.F.) ;
#33623 = ORIENTED_EDGE('',*,*,#25169,.F.) ;
#33624 = ORIENTED_EDGE('',*,*,#25170,.F.) ;
#33625 = ORIENTED_EDGE('',*,*,#25171,.F.) ;
#33626 = ORIENTED_EDGE('',*,*,#25172,.T.) ;
#33627 = ORIENTED_EDGE('',*,*,#25173,.F.) ;
#33628 = ORIENTED_EDGE('',*,*,#25174,.F.) ;
#33629 = ORIENTED_EDGE('',*,*,#25175,.F.) ;
#33630 = ORIENTED_EDGE('',*,*,#25176,.T.) ;
#33631 = ORIENTED_EDGE('',*,*,#25177,.F.) ;
#33632 = ORIENTED_EDGE('',*,*,#25178,.F.) ;
#33633 = ORIENTED_EDGE('',*,*,#25179,.F.) ;
#33634 = ORIENTED_EDGE('',*,*,#25180,.F.) ;
#33635 = ORIENTED_EDGE('',*,*,#25181,.F.) ;
#33636 = ORIENTED_EDGE('',*,*,#25182,.F.) ;
#33637 = ORIENTED_EDGE('',*,*,#25183,.F.) ;
#33638 = ORIENTED_EDGE('',*,*,#25184,.F.) ;
#33639 = ORIENTED_EDGE('',*,*,#25185,.F.) ;
#33640 = ORIENTED_EDGE('',*,*,#25186,.F.) ;
#33641 = ORIENTED_EDGE('',*,*,#25187,.T.) ;
#33642 = ORIENTED_EDGE('',*,*,#25188,.F.) ;
#33643 = ORIENTED_EDGE('',*,*,#25189,.F.) ;
#33644 = ORIENTED_EDGE('',*,*,#25190,.F.) ;
#33645 = ORIENTED_EDGE('',*,*,#25191,.F.) ;
#33646 = ORIENTED_EDGE('',*,*,#25192,.F.) ;
#33647 = ORIENTED_EDGE('',*,*,#25193,.F.) ;
#33648 = ORIENTED_EDGE('',*,*,#25194,.F.) ;
#33649 = ORIENTED_EDGE('',*,*,#25195,.F.) ;
#33650 = ORIENTED_EDGE('',*,*,#25196,.F.) ;
#33651 = ORIENTED_EDGE('',*,*,#25197,.F.) ;
#33652 = ORIENTED_EDGE('',*,*,#25198,.T.) ;
#33653 = ORIENTED_EDGE('',*,*,#25199,.F.) ;
#33654 = ORIENTED_EDGE('',*,*,#25200,.F.) ;
#33655 = ORIENTED_EDGE('',*,*,#25201,.F.) ;
#33656 = ORIENTED_EDGE('',*,*,#25202,.F.) ;
#33657 = ORIENTED_EDGE('',*,*,#25203,.F.) ;
#33658 = ORIENTED_EDGE('',*,*,#25204,.F.) ;
#33659 = ORIENTED_EDGE('',*,*,#25205,.T.) ;
#33660 = ORIENTED_EDGE('',*,*,#25206,.F.) ;
#33661 = ORIENTED_EDGE('',*,*,#25207,.F.) ;
#33662 = ORIENTED_EDGE('',*,*,#25208,.F.) ;
#33663 = ORIENTED_EDGE('',*,*,#25209,.F.) ;
#33664 = ORIENTED_EDGE('',*,*,#25210,.F.) ;
#33665 = ORIENTED_EDGE('',*,*,#25211,.F.) ;
#33666 = ORIENTED_EDGE('',*,*,#25212,.F.) ;
#33667 = ORIENTED_EDGE('',*,*,#25213,.F.) ;
#33668 = ORIENTED_EDGE('',*,*,#25214,.F.) ;
#33669 = ORIENTED_EDGE('',*,*,#25215,.T.) ;
#33670 = ORIENTED_EDGE('',*,*,#25216,.F.) ;
#33671 = ORIENTED_EDGE('',*,*,#25217,.F.) ;
#33672 = ORIENTED_EDGE('',*,*,#25218,.F.) ;
#33673 = ORIENTED_EDGE('',*,*,#25219,.F.) ;
#33674 = ORIENTED_EDGE('',*,*,#25220,.F.) ;
#33675 = ORIENTED_EDGE('',*,*,#25221,.F.) ;
#33676 = ORIENTED_EDGE('',*,*,#25222,.F.) ;
#33677 = ORIENTED_EDGE('',*,*,#25223,.F.) ;
#33678 = ORIENTED_EDGE('',*,*,#25224,.F.) ;
#33679 = ORIENTED_EDGE('',*,*,#25225,.F.) ;
#33680 = ORIENTED_EDGE('',*,*,#25226,.F.) ;
#33681 = ORIENTED_EDGE('',*,*,#25227,.F.) ;
#33682 = ORIENTED_EDGE('',*,*,#25228,.F.) ;
#33683 = ORIENTED_EDGE('',*,*,#25229,.F.) ;
#33684 = ORIENTED_EDGE('',*,*,#25230,.F.) ;
#33685 = ORIENTED_EDGE('',*,*,#25231,.F.) ;
#33686 = ORIENTED_EDGE('',*,*,#25232,.F.) ;
#33687 = ORIENTED_EDGE('',*,*,#25233,.F.) ;
#33688 = ORIENTED_EDGE('',*,*,#25234,.F.) ;
#33689 = ORIENTED_EDGE('',*,*,#25235,.F.) ;
#33690 = ORIENTED_EDGE('',*,*,#25236,.F.) ;
#33691 = ORIENTED_EDGE('',*,*,#25237,.F.) ;
#33692 = ORIENTED_EDGE('',*,*,#25238,.F.) ;
#33693 = ORIENTED_EDGE('',*,*,#25239,.F.) ;
#33694 = ORIENTED_EDGE('',*,*,#25240,.F.) ;
#33695 = ORIENTED_EDGE('',*,*,#25241,.F.) ;
#33696 = ORIENTED_EDGE('',*,*,#25242,.F.) ;
#33697 = ORIENTED_EDGE('',*,*,#25243,.F.) ;
#33698 = ORIENTED_EDGE('',*,*,#25244,.F.) ;
#33699 = ORIENTED_EDGE('',*,*,#25245,.F.) ;
#33700 = ORIENTED_EDGE('',*,*,#25042,.F.) ;
#33701 = ORIENTED_EDGE('',*,*,#25044,.F.) ;
#33702 = ORIENTED_EDGE('',*,*,#25031,.F.) ;
#33703 = ORIENTED_EDGE('',*,*,#25040,.F.) ;
#33704 = ORIENTED_EDGE('',*,*,#25036,.F.) ;
#33705 = ORIENTED_EDGE('',*,*,#25033,.F.) ;
#33706 = ORIENTED_EDGE('',*,*,#25026,.F.) ;
#33707 = ORIENTED_EDGE('',*,*,#25023,.F.) ;
#33708 = ORIENTED_EDGE('',*,*,#25020,.F.) ;
#33709 = ORIENTED_EDGE('',*,*,#25017,.F.) ;
#33710 = ORIENTED_EDGE('',*,*,#25014,.F.) ;
#33711 = ORIENTED_EDGE('',*,*,#25009,.F.) ;
#33712 = ORIENTED_EDGE('',*,*,#25007,.F.) ;
#33713 = ORIENTED_EDGE('',*,*,#25004,.F.) ;
#33714 = ORIENTED_EDGE('',*,*,#25050,.F.) ;
#33715 = ORIENTED_EDGE('',*,*,#25012,.F.) ;
#33716 = ORIENTED_EDGE('',*,*,#25049,.F.) ;
#33717 = ORIENTED_EDGE('',*,*,#25047,.F.) ;
#33718 = ORIENTED_EDGE('',*,*,#25045,.F.) ;
#33719 = ORIENTED_EDGE('',*,*,#25108,.T.) ;
#33720 = ORIENTED_EDGE('',*,*,#25246,.T.) ;
#33721 = ORIENTED_EDGE('',*,*,#24972,.T.) ;
#33722 = ORIENTED_EDGE('',*,*,#25247,.T.) ;
#33723 = ORIENTED_EDGE('',*,*,#25110,.T.) ;
#33724 = ORIENTED_EDGE('',*,*,#25248,.T.) ;
#33725 = ORIENTED_EDGE('',*,*,#24969,.T.) ;
#33726 = ORIENTED_EDGE('',*,*,#25246,.F.) ;
#33727 = ORIENTED_EDGE('',*,*,#25249,.T.) ;
#33728 = ORIENTED_EDGE('',*,*,#25248,.F.) ;
#33729 = ORIENTED_EDGE('',*,*,#25109,.T.) ;
#33730 = ORIENTED_EDGE('',*,*,#25247,.F.) ;
#33731 = ORIENTED_EDGE('',*,*,#24963,.F.) ;
#33732 = ORIENTED_EDGE('',*,*,#24970,.F.) ;
#33733 = ORIENTED_EDGE('',*,*,#25249,.F.) ;
#33734 = ORIENTED_EDGE('',*,*,#24971,.T.) ;
#33735 = ORIENTED_EDGE('',*,*,#25242,.T.) ;
#33736 = ORIENTED_EDGE('',*,*,#25250,.T.) ;
#33737 = ORIENTED_EDGE('',*,*,#24989,.T.) ;
#33738 = ORIENTED_EDGE('',*,*,#25251,.T.) ;
#33739 = ORIENTED_EDGE('',*,*,#25245,.T.) ;
#33740 = ORIENTED_EDGE('',*,*,#25252,.T.) ;
#33741 = ORIENTED_EDGE('',*,*,#24986,.T.) ;
#33742 = ORIENTED_EDGE('',*,*,#25250,.F.) ;
#33743 = ORIENTED_EDGE('',*,*,#25253,.T.) ;
#33744 = ORIENTED_EDGE('',*,*,#25252,.F.) ;
#33745 = ORIENTED_EDGE('',*,*,#25244,.T.) ;
#33746 = ORIENTED_EDGE('',*,*,#25254,.T.) ;
#33747 = ORIENTED_EDGE('',*,*,#25243,.T.) ;
#33748 = ORIENTED_EDGE('',*,*,#25251,.F.) ;
#33749 = ORIENTED_EDGE('',*,*,#25255,.T.) ;
#33750 = ORIENTED_EDGE('',*,*,#25254,.F.) ;
#33751 = ORIENTED_EDGE('',*,*,#24977,.F.) ;
#33752 = ORIENTED_EDGE('',*,*,#25256,.F.) ;
#33753 = ORIENTED_EDGE('',*,*,#25255,.F.) ;
#33754 = ORIENTED_EDGE('',*,*,#24988,.T.) ;
#33755 = ORIENTED_EDGE('',*,*,#25111,.T.) ;
#33756 = ORIENTED_EDGE('',*,*,#25257,.T.) ;
#33757 = ORIENTED_EDGE('',*,*,#25003,.T.) ;
#33758 = ORIENTED_EDGE('',*,*,#25258,.T.) ;
#33759 = ORIENTED_EDGE('',*,*,#25000,.T.) ;
#33760 = ORIENTED_EDGE('',*,*,#25257,.F.) ;
#33761 = ORIENTED_EDGE('',*,*,#25113,.T.) ;
#33762 = ORIENTED_EDGE('',*,*,#25259,.T.) ;
#33763 = ORIENTED_EDGE('',*,*,#25112,.T.) ;
#33764 = ORIENTED_EDGE('',*,*,#25258,.F.) ;
#33765 = ORIENTED_EDGE('',*,*,#25260,.T.) ;
#33766 = ORIENTED_EDGE('',*,*,#25259,.F.) ;
#33767 = ORIENTED_EDGE('',*,*,#24994,.F.) ;
#33768 = ORIENTED_EDGE('',*,*,#25001,.F.) ;
#33769 = ORIENTED_EDGE('',*,*,#25260,.F.) ;
#33770 = ORIENTED_EDGE('',*,*,#25002,.T.) ;
#33771 = ORIENTED_EDGE('',*,*,#24980,.F.) ;
#33772 = ORIENTED_EDGE('',*,*,#24987,.F.) ;
#33773 = ORIENTED_EDGE('',*,*,#25253,.F.) ;
#33774 = ORIENTED_EDGE('',*,*,#25256,.T.) ;
#33775 = ORIENTED_EDGE('',*,*,#24838,.F.) ;
#33776 = ORIENTED_EDGE('',*,*,#24854,.F.) ;
#33777 = ORIENTED_EDGE('',*,*,#24949,.F.) ;
#33778 = ORIENTED_EDGE('',*,*,#25261,.T.) ;
#33779 = ORIENTED_EDGE('',*,*,#24830,.F.) ;
#33780 = ORIENTED_EDGE('',*,*,#25261,.F.) ;
#33781 = ORIENTED_EDGE('',*,*,#24953,.F.) ;
#33782 = ORIENTED_EDGE('',*,*,#25262,.T.) ;
#33783 = ORIENTED_EDGE('',*,*,#24850,.F.) ;
#33784 = ORIENTED_EDGE('',*,*,#25262,.F.) ;
#33785 = ORIENTED_EDGE('',*,*,#24956,.F.) ;
#33786 = ORIENTED_EDGE('',*,*,#25263,.T.) ;
#33787 = ORIENTED_EDGE('',*,*,#24847,.F.) ;
#33788 = ORIENTED_EDGE('',*,*,#25263,.F.) ;
#33789 = ORIENTED_EDGE('',*,*,#24941,.F.) ;
#33790 = ORIENTED_EDGE('',*,*,#24859,.T.) ;
#33791 = ORIENTED_EDGE('',*,*,#24913,.F.) ;
#33792 = ORIENTED_EDGE('',*,*,#24920,.F.) ;
#33793 = ORIENTED_EDGE('',*,*,#25016,.F.) ;
#33794 = ORIENTED_EDGE('',*,*,#25051,.T.) ;
#33795 = ORIENTED_EDGE('',*,*,#25264,.T.) ;
#33796 = ORIENTED_EDGE('',*,*,#25265,.T.) ;
#33797 = ORIENTED_EDGE('',*,*,#25266,.T.) ;
#33798 = ORIENTED_EDGE('',*,*,#25265,.F.) ;
#33799 = ORIENTED_EDGE('',*,*,#25267,.T.) ;
#33800 = ORIENTED_EDGE('',*,*,#25268,.F.) ;
#33801 = ORIENTED_EDGE('',*,*,#25266,.F.) ;
#33802 = ORIENTED_EDGE('',*,*,#25264,.F.) ;
#33803 = ORIENTED_EDGE('',*,*,#25269,.T.) ;
#33804 = ORIENTED_EDGE('',*,*,#25270,.F.) ;
#33805 = ORIENTED_EDGE('',*,*,#25269,.F.) ;
#33806 = ORIENTED_EDGE('',*,*,#25267,.F.) ;
#33807 = ORIENTED_EDGE('',*,*,#25271,.T.) ;
#33808 = ORIENTED_EDGE('',*,*,#25272,.T.) ;
#33809 = ORIENTED_EDGE('',*,*,#25268,.T.) ;
#33810 = ORIENTED_EDGE('',*,*,#25272,.F.) ;
#33811 = ORIENTED_EDGE('',*,*,#25273,.F.) ;
#33812 = ORIENTED_EDGE('',*,*,#25274,.T.) ;
#33813 = ORIENTED_EDGE('',*,*,#25271,.F.) ;
#33814 = ORIENTED_EDGE('',*,*,#25274,.F.) ;
#33815 = ORIENTED_EDGE('',*,*,#25275,.T.) ;
#33816 = ORIENTED_EDGE('',*,*,#25276,.T.) ;
#33817 = ORIENTED_EDGE('',*,*,#25273,.T.) ;
#33818 = ORIENTED_EDGE('',*,*,#25276,.F.) ;
#33819 = ORIENTED_EDGE('',*,*,#25277,.F.) ;
#33820 = ORIENTED_EDGE('',*,*,#25278,.F.) ;
#33821 = ORIENTED_EDGE('',*,*,#25279,.F.) ;
#33822 = ORIENTED_EDGE('',*,*,#25280,.F.) ;
#33823 = ORIENTED_EDGE('',*,*,#25281,.T.) ;
#33824 = ORIENTED_EDGE('',*,*,#25282,.T.) ;
#33825 = ORIENTED_EDGE('',*,*,#25283,.F.) ;
#33826 = ORIENTED_EDGE('',*,*,#25284,.F.) ;
#33827 = ORIENTED_EDGE('',*,*,#25285,.F.) ;
#33828 = ORIENTED_EDGE('',*,*,#25286,.F.) ;
#33829 = ORIENTED_EDGE('',*,*,#25287,.F.) ;
#33830 = ORIENTED_EDGE('',*,*,#25288,.F.) ;
#33831 = ORIENTED_EDGE('',*,*,#25289,.F.) ;
#33832 = ORIENTED_EDGE('',*,*,#25290,.F.) ;
#33833 = ORIENTED_EDGE('',*,*,#25291,.T.) ;
#33834 = ORIENTED_EDGE('',*,*,#25292,.F.) ;
#33835 = ORIENTED_EDGE('',*,*,#25293,.T.) ;
#33836 = ORIENTED_EDGE('',*,*,#25294,.F.) ;
#33837 = ORIENTED_EDGE('',*,*,#25295,.F.) ;
#33838 = ORIENTED_EDGE('',*,*,#25296,.F.) ;
#33839 = ORIENTED_EDGE('',*,*,#25297,.T.) ;
#33840 = ORIENTED_EDGE('',*,*,#25298,.F.) ;
#33841 = ORIENTED_EDGE('',*,*,#25299,.T.) ;
#33842 = ORIENTED_EDGE('',*,*,#25300,.F.) ;
#33843 = ORIENTED_EDGE('',*,*,#25301,.F.) ;
#33844 = ORIENTED_EDGE('',*,*,#25302,.F.) ;
#33845 = ORIENTED_EDGE('',*,*,#25303,.F.) ;
#33846 = ORIENTED_EDGE('',*,*,#25304,.F.) ;
#33847 = ORIENTED_EDGE('',*,*,#25305,.F.) ;
#33848 = ORIENTED_EDGE('',*,*,#25306,.F.) ;
#33849 = ORIENTED_EDGE('',*,*,#25307,.F.) ;
#33850 = ORIENTED_EDGE('',*,*,#25308,.F.) ;
#33851 = ORIENTED_EDGE('',*,*,#25309,.F.) ;
#33852 = ORIENTED_EDGE('',*,*,#25310,.F.) ;
#33853 = ORIENTED_EDGE('',*,*,#25311,.F.) ;
#33854 = ORIENTED_EDGE('',*,*,#25312,.F.) ;
#33855 = ORIENTED_EDGE('',*,*,#25313,.F.) ;
#33856 = ORIENTED_EDGE('',*,*,#25314,.F.) ;
#33857 = ORIENTED_EDGE('',*,*,#25315,.F.) ;
#33858 = ORIENTED_EDGE('',*,*,#25316,.F.) ;
#33859 = ORIENTED_EDGE('',*,*,#25317,.F.) ;
#33860 = ORIENTED_EDGE('',*,*,#25318,.F.) ;
#33861 = ORIENTED_EDGE('',*,*,#25319,.F.) ;
#33862 = ORIENTED_EDGE('',*,*,#25320,.F.) ;
#33863 = ORIENTED_EDGE('',*,*,#25321,.F.) ;
#33864 = ORIENTED_EDGE('',*,*,#25322,.F.) ;
#33865 = ORIENTED_EDGE('',*,*,#25323,.F.) ;
#33866 = ORIENTED_EDGE('',*,*,#25324,.F.) ;
#33867 = ORIENTED_EDGE('',*,*,#25325,.F.) ;
#33868 = ORIENTED_EDGE('',*,*,#25326,.F.) ;
#33869 = ORIENTED_EDGE('',*,*,#25327,.T.) ;
#33870 = ORIENTED_EDGE('',*,*,#25328,.F.) ;
#33871 = ORIENTED_EDGE('',*,*,#25329,.F.) ;
#33872 = ORIENTED_EDGE('',*,*,#25330,.F.) ;
#33873 = ORIENTED_EDGE('',*,*,#25331,.F.) ;
#33874 = ORIENTED_EDGE('',*,*,#25332,.F.) ;
#33875 = ORIENTED_EDGE('',*,*,#25333,.F.) ;
#33876 = ORIENTED_EDGE('',*,*,#25334,.F.) ;
#33877 = ORIENTED_EDGE('',*,*,#25335,.F.) ;
#33878 = ORIENTED_EDGE('',*,*,#25336,.F.) ;
#33879 = ORIENTED_EDGE('',*,*,#25337,.F.) ;
#33880 = ORIENTED_EDGE('',*,*,#25338,.F.) ;
#33881 = ORIENTED_EDGE('',*,*,#25339,.F.) ;
#33882 = ORIENTED_EDGE('',*,*,#25340,.F.) ;
#33883 = ORIENTED_EDGE('',*,*,#25341,.F.) ;
#33884 = ORIENTED_EDGE('',*,*,#25342,.F.) ;
#33885 = ORIENTED_EDGE('',*,*,#25343,.F.) ;
#33886 = ORIENTED_EDGE('',*,*,#25344,.F.) ;
#33887 = ORIENTED_EDGE('',*,*,#25345,.F.) ;
#33888 = ORIENTED_EDGE('',*,*,#25346,.F.) ;
#33889 = ORIENTED_EDGE('',*,*,#25347,.F.) ;
#33890 = ORIENTED_EDGE('',*,*,#25348,.F.) ;
#33891 = ORIENTED_EDGE('',*,*,#25349,.F.) ;
#33892 = ORIENTED_EDGE('',*,*,#25350,.T.) ;
#33893 = ORIENTED_EDGE('',*,*,#25351,.F.) ;
#33894 = ORIENTED_EDGE('',*,*,#25352,.F.) ;
#33895 = ORIENTED_EDGE('',*,*,#25353,.F.) ;
#33896 = ORIENTED_EDGE('',*,*,#25354,.F.) ;
#33897 = ORIENTED_EDGE('',*,*,#25355,.F.) ;
#33898 = ORIENTED_EDGE('',*,*,#25356,.F.) ;
#33899 = ORIENTED_EDGE('',*,*,#25357,.F.) ;
#33900 = ORIENTED_EDGE('',*,*,#25358,.F.) ;
#33901 = ORIENTED_EDGE('',*,*,#25359,.F.) ;
#33902 = ORIENTED_EDGE('',*,*,#25360,.F.) ;
#33903 = ORIENTED_EDGE('',*,*,#25361,.F.) ;
#33904 = ORIENTED_EDGE('',*,*,#25362,.F.) ;
#33905 = ORIENTED_EDGE('',*,*,#25363,.F.) ;
#33906 = ORIENTED_EDGE('',*,*,#25364,.F.) ;
#33907 = ORIENTED_EDGE('',*,*,#25365,.F.) ;
#33908 = ORIENTED_EDGE('',*,*,#25366,.T.) ;
#33909 = ORIENTED_EDGE('',*,*,#25367,.T.) ;
#33910 = ORIENTED_EDGE('',*,*,#25368,.T.) ;
#33911 = ORIENTED_EDGE('',*,*,#25369,.F.) ;
#33912 = ORIENTED_EDGE('',*,*,#25370,.F.) ;
#33913 = ORIENTED_EDGE('',*,*,#25371,.F.) ;
#33914 = ORIENTED_EDGE('',*,*,#25372,.T.) ;
#33915 = ORIENTED_EDGE('',*,*,#25373,.F.) ;
#33916 = ORIENTED_EDGE('',*,*,#25374,.F.) ;
#33917 = ORIENTED_EDGE('',*,*,#25375,.F.) ;
#33918 = ORIENTED_EDGE('',*,*,#25376,.T.) ;
#33919 = ORIENTED_EDGE('',*,*,#25377,.F.) ;
#33920 = ORIENTED_EDGE('',*,*,#25378,.T.) ;
#33921 = ORIENTED_EDGE('',*,*,#25379,.T.) ;
#33922 = ORIENTED_EDGE('',*,*,#25380,.T.) ;
#33923 = ORIENTED_EDGE('',*,*,#25381,.F.) ;
#33924 = ORIENTED_EDGE('',*,*,#25382,.F.) ;
#33925 = ORIENTED_EDGE('',*,*,#25383,.F.) ;
#33926 = ORIENTED_EDGE('',*,*,#25384,.F.) ;
#33927 = ORIENTED_EDGE('',*,*,#25385,.F.) ;
#33928 = ORIENTED_EDGE('',*,*,#25386,.F.) ;
#33929 = ORIENTED_EDGE('',*,*,#25387,.F.) ;
#33930 = ORIENTED_EDGE('',*,*,#25388,.F.) ;
#33931 = ORIENTED_EDGE('',*,*,#25389,.F.) ;
#33932 = ORIENTED_EDGE('',*,*,#25390,.T.) ;
#33933 = ORIENTED_EDGE('',*,*,#25391,.T.) ;
#33934 = ORIENTED_EDGE('',*,*,#25392,.T.) ;
#33935 = ORIENTED_EDGE('',*,*,#25393,.F.) ;
#33936 = ORIENTED_EDGE('',*,*,#25394,.F.) ;
#33937 = ORIENTED_EDGE('',*,*,#25395,.F.) ;
#33938 = ORIENTED_EDGE('',*,*,#25396,.F.) ;
#33939 = ORIENTED_EDGE('',*,*,#25397,.F.) ;
#33940 = ORIENTED_EDGE('',*,*,#25398,.F.) ;
#33941 = ORIENTED_EDGE('',*,*,#25399,.F.) ;
#33942 = ORIENTED_EDGE('',*,*,#25400,.F.) ;
#33943 = ORIENTED_EDGE('',*,*,#25401,.F.) ;
#33944 = ORIENTED_EDGE('',*,*,#25402,.F.) ;
#33945 = ORIENTED_EDGE('',*,*,#25403,.F.) ;
#33946 = ORIENTED_EDGE('',*,*,#25404,.T.) ;
#33947 = ORIENTED_EDGE('',*,*,#25405,.F.) ;
#33948 = ORIENTED_EDGE('',*,*,#25406,.F.) ;
#33949 = ORIENTED_EDGE('',*,*,#25407,.F.) ;
#33950 = ORIENTED_EDGE('',*,*,#25408,.F.) ;
#33951 = ORIENTED_EDGE('',*,*,#25409,.F.) ;
#33952 = ORIENTED_EDGE('',*,*,#25410,.F.) ;
#33953 = ORIENTED_EDGE('',*,*,#25411,.F.) ;
#33954 = ORIENTED_EDGE('',*,*,#25412,.F.) ;
#33955 = ORIENTED_EDGE('',*,*,#25413,.F.) ;
#33956 = ORIENTED_EDGE('',*,*,#25414,.F.) ;
#33957 = ORIENTED_EDGE('',*,*,#25415,.F.) ;
#33958 = ORIENTED_EDGE('',*,*,#25416,.F.) ;
#33959 = ORIENTED_EDGE('',*,*,#25417,.F.) ;
#33960 = ORIENTED_EDGE('',*,*,#25418,.F.) ;
#33961 = ORIENTED_EDGE('',*,*,#25419,.F.) ;
#33962 = ORIENTED_EDGE('',*,*,#25420,.F.) ;
#33963 = ORIENTED_EDGE('',*,*,#25421,.F.) ;
#33964 = ORIENTED_EDGE('',*,*,#25422,.F.) ;
#33965 = ORIENTED_EDGE('',*,*,#25423,.F.) ;
#33966 = ORIENTED_EDGE('',*,*,#25424,.F.) ;
#33967 = ORIENTED_EDGE('',*,*,#25425,.F.) ;
#33968 = ORIENTED_EDGE('',*,*,#25426,.F.) ;
#33969 = ORIENTED_EDGE('',*,*,#25427,.F.) ;
#33970 = ORIENTED_EDGE('',*,*,#25428,.F.) ;
#33971 = ORIENTED_EDGE('',*,*,#25429,.F.) ;
#33972 = ORIENTED_EDGE('',*,*,#25430,.F.) ;
#33973 = ORIENTED_EDGE('',*,*,#25431,.F.) ;
#33974 = ORIENTED_EDGE('',*,*,#25432,.F.) ;
#33975 = ORIENTED_EDGE('',*,*,#25433,.F.) ;
#33976 = ORIENTED_EDGE('',*,*,#25434,.F.) ;
#33977 = ORIENTED_EDGE('',*,*,#25435,.F.) ;
#33978 = ORIENTED_EDGE('',*,*,#25436,.F.) ;
#33979 = ORIENTED_EDGE('',*,*,#25437,.F.) ;
#33980 = ORIENTED_EDGE('',*,*,#25438,.F.) ;
#33981 = ORIENTED_EDGE('',*,*,#25439,.F.) ;
#33982 = ORIENTED_EDGE('',*,*,#25440,.F.) ;
#33983 = ORIENTED_EDGE('',*,*,#25441,.F.) ;
#33984 = ORIENTED_EDGE('',*,*,#25442,.F.) ;
#33985 = ORIENTED_EDGE('',*,*,#25443,.F.) ;
#33986 = ORIENTED_EDGE('',*,*,#25444,.F.) ;
#33987 = ORIENTED_EDGE('',*,*,#25445,.F.) ;
#33988 = ORIENTED_EDGE('',*,*,#25446,.F.) ;
#33989 = ORIENTED_EDGE('',*,*,#25275,.F.) ;
#33990 = ORIENTED_EDGE('',*,*,#25447,.T.) ;
#33991 = ORIENTED_EDGE('',*,*,#25448,.F.) ;
#33992 = ORIENTED_EDGE('',*,*,#25449,.T.) ;
#33993 = ORIENTED_EDGE('',*,*,#25450,.T.) ;
#33994 = ORIENTED_EDGE('',*,*,#25451,.T.) ;
#33995 = ORIENTED_EDGE('',*,*,#25452,.T.) ;
#33996 = ORIENTED_EDGE('',*,*,#25447,.F.) ;
#33997 = ORIENTED_EDGE('',*,*,#25453,.T.) ;
#33998 = ORIENTED_EDGE('',*,*,#25454,.T.) ;
#33999 = ORIENTED_EDGE('',*,*,#25455,.T.) ;
#34000 = ORIENTED_EDGE('',*,*,#25451,.F.) ;
#34001 = ORIENTED_EDGE('',*,*,#25456,.T.) ;
#34002 = ORIENTED_EDGE('',*,*,#25457,.T.) ;
#34003 = ORIENTED_EDGE('',*,*,#25458,.T.) ;
#34004 = ORIENTED_EDGE('',*,*,#25454,.F.) ;
#34005 = ORIENTED_EDGE('',*,*,#25459,.T.) ;
#34006 = ORIENTED_EDGE('',*,*,#25460,.T.) ;
#34007 = ORIENTED_EDGE('',*,*,#25461,.T.) ;
#34008 = ORIENTED_EDGE('',*,*,#25457,.F.) ;
#34009 = ORIENTED_EDGE('',*,*,#25462,.T.) ;
#34010 = ORIENTED_EDGE('',*,*,#25463,.T.) ;
#34011 = ORIENTED_EDGE('',*,*,#25464,.T.) ;
#34012 = ORIENTED_EDGE('',*,*,#25460,.F.) ;
#34013 = ORIENTED_EDGE('',*,*,#25465,.T.) ;
#34014 = ORIENTED_EDGE('',*,*,#25466,.T.) ;
#34015 = ORIENTED_EDGE('',*,*,#25467,.T.) ;
#34016 = ORIENTED_EDGE('',*,*,#25463,.F.) ;
#34017 = ORIENTED_EDGE('',*,*,#25468,.T.) ;
#34018 = ORIENTED_EDGE('',*,*,#25469,.T.) ;
#34019 = ORIENTED_EDGE('',*,*,#25470,.T.) ;
#34020 = ORIENTED_EDGE('',*,*,#25466,.F.) ;
#34021 = ORIENTED_EDGE('',*,*,#25471,.T.) ;
#34022 = ORIENTED_EDGE('',*,*,#25472,.T.) ;
#34023 = ORIENTED_EDGE('',*,*,#25473,.T.) ;
#34024 = ORIENTED_EDGE('',*,*,#25469,.F.) ;
#34025 = ORIENTED_EDGE('',*,*,#25474,.T.) ;
#34026 = ORIENTED_EDGE('',*,*,#25475,.T.) ;
#34027 = ORIENTED_EDGE('',*,*,#25476,.T.) ;
#34028 = ORIENTED_EDGE('',*,*,#25472,.F.) ;
#34029 = ORIENTED_EDGE('',*,*,#25477,.T.) ;
#34030 = ORIENTED_EDGE('',*,*,#25478,.T.) ;
#34031 = ORIENTED_EDGE('',*,*,#25479,.T.) ;
#34032 = ORIENTED_EDGE('',*,*,#25475,.F.) ;
#34033 = ORIENTED_EDGE('',*,*,#25480,.T.) ;
#34034 = ORIENTED_EDGE('',*,*,#25481,.T.) ;
#34035 = ORIENTED_EDGE('',*,*,#25482,.T.) ;
#34036 = ORIENTED_EDGE('',*,*,#25478,.F.) ;
#34037 = ORIENTED_EDGE('',*,*,#25483,.T.) ;
#34038 = ORIENTED_EDGE('',*,*,#25481,.F.) ;
#34039 = ORIENTED_EDGE('',*,*,#25484,.T.) ;
#34040 = ORIENTED_EDGE('',*,*,#25485,.T.) ;
#34041 = ORIENTED_EDGE('',*,*,#25486,.F.) ;
#34042 = ORIENTED_EDGE('',*,*,#25484,.F.) ;
#34043 = ORIENTED_EDGE('',*,*,#25483,.F.) ;
#34044 = ORIENTED_EDGE('',*,*,#25487,.F.) ;
#34045 = ORIENTED_EDGE('',*,*,#25488,.F.) ;
#34046 = ORIENTED_EDGE('',*,*,#25489,.F.) ;
#34047 = ORIENTED_EDGE('',*,*,#25490,.F.) ;
#34048 = ORIENTED_EDGE('',*,*,#25491,.F.) ;
#34049 = ORIENTED_EDGE('',*,*,#25492,.F.) ;
#34050 = ORIENTED_EDGE('',*,*,#25480,.F.) ;
#34051 = ORIENTED_EDGE('',*,*,#25493,.T.) ;
#34052 = ORIENTED_EDGE('',*,*,#25494,.F.) ;
#34053 = ORIENTED_EDGE('',*,*,#25487,.T.) ;
#34054 = ORIENTED_EDGE('',*,*,#25477,.F.) ;
#34055 = ORIENTED_EDGE('',*,*,#25495,.F.) ;
#34056 = ORIENTED_EDGE('',*,*,#25496,.F.) ;
#34057 = ORIENTED_EDGE('',*,*,#25493,.F.) ;
#34058 = ORIENTED_EDGE('',*,*,#25474,.F.) ;
#34059 = ORIENTED_EDGE('',*,*,#25497,.T.) ;
#34060 = ORIENTED_EDGE('',*,*,#25498,.F.) ;
#34061 = ORIENTED_EDGE('',*,*,#25495,.T.) ;
#34062 = ORIENTED_EDGE('',*,*,#25471,.F.) ;
#34063 = ORIENTED_EDGE('',*,*,#25499,.T.) ;
#34064 = ORIENTED_EDGE('',*,*,#25500,.F.) ;
#34065 = ORIENTED_EDGE('',*,*,#25497,.F.) ;
#34066 = ORIENTED_EDGE('',*,*,#25468,.F.) ;
#34067 = ORIENTED_EDGE('',*,*,#25501,.T.) ;
#34068 = ORIENTED_EDGE('',*,*,#25502,.F.) ;
#34069 = ORIENTED_EDGE('',*,*,#25499,.F.) ;
#34070 = ORIENTED_EDGE('',*,*,#25465,.F.) ;
#34071 = ORIENTED_EDGE('',*,*,#25503,.F.) ;
#34072 = ORIENTED_EDGE('',*,*,#25504,.F.) ;
#34073 = ORIENTED_EDGE('',*,*,#25501,.F.) ;
#34074 = ORIENTED_EDGE('',*,*,#25462,.F.) ;
#34075 = ORIENTED_EDGE('',*,*,#25505,.T.) ;
#34076 = ORIENTED_EDGE('',*,*,#25506,.F.) ;
#34077 = ORIENTED_EDGE('',*,*,#25503,.T.) ;
#34078 = ORIENTED_EDGE('',*,*,#25459,.F.) ;
#34079 = ORIENTED_EDGE('',*,*,#25507,.F.) ;
#34080 = ORIENTED_EDGE('',*,*,#25508,.F.) ;
#34081 = ORIENTED_EDGE('',*,*,#25505,.F.) ;
#34082 = ORIENTED_EDGE('',*,*,#25456,.F.) ;
#34083 = ORIENTED_EDGE('',*,*,#25509,.T.) ;
#34084 = ORIENTED_EDGE('',*,*,#25510,.F.) ;
#34085 = ORIENTED_EDGE('',*,*,#25507,.T.) ;
#34086 = ORIENTED_EDGE('',*,*,#25453,.F.) ;
#34087 = ORIENTED_EDGE('',*,*,#25450,.F.) ;
#34088 = ORIENTED_EDGE('',*,*,#25511,.F.) ;
#34089 = ORIENTED_EDGE('',*,*,#25512,.F.) ;
#34090 = ORIENTED_EDGE('',*,*,#25513,.F.) ;
#34091 = ORIENTED_EDGE('',*,*,#25514,.F.) ;
#34092 = ORIENTED_EDGE('',*,*,#25515,.F.) ;
#34093 = ORIENTED_EDGE('',*,*,#25509,.F.) ;
#34094 = ORIENTED_EDGE('',*,*,#25334,.T.) ;
#34095 = ORIENTED_EDGE('',*,*,#25516,.T.) ;
#34096 = ORIENTED_EDGE('',*,*,#25517,.T.) ;
#34097 = ORIENTED_EDGE('',*,*,#25516,.F.) ;
#34098 = ORIENTED_EDGE('',*,*,#25517,.F.) ;
#34099 = ORIENTED_EDGE('',*,*,#25518,.T.) ;
#34100 = ORIENTED_EDGE('',*,*,#25519,.T.) ;
#34101 = ORIENTED_EDGE('',*,*,#25518,.F.) ;
#34102 = ORIENTED_EDGE('',*,*,#25520,.T.) ;
#34103 = ORIENTED_EDGE('',*,*,#25521,.T.) ;
#34104 = ORIENTED_EDGE('',*,*,#25522,.T.) ;
#34105 = ORIENTED_EDGE('',*,*,#25520,.F.) ;
#34106 = ORIENTED_EDGE('',*,*,#25446,.T.) ;
#34107 = ORIENTED_EDGE('',*,*,#25521,.F.) ;
#34108 = ORIENTED_EDGE('',*,*,#25522,.F.) ;
#34109 = ORIENTED_EDGE('',*,*,#25523,.T.) ;
#34110 = ORIENTED_EDGE('',*,*,#25524,.T.) ;
#34111 = ORIENTED_EDGE('',*,*,#25523,.F.) ;
#34112 = ORIENTED_EDGE('',*,*,#25524,.F.) ;
#34113 = ORIENTED_EDGE('',*,*,#25525,.F.) ;
#34114 = ORIENTED_EDGE('',*,*,#25526,.T.) ;
#34115 = ORIENTED_EDGE('',*,*,#25527,.T.) ;
#34116 = ORIENTED_EDGE('',*,*,#25525,.T.) ;
#34117 = ORIENTED_EDGE('',*,*,#25527,.F.) ;
#34118 = ORIENTED_EDGE('',*,*,#25528,.T.) ;
#34119 = ORIENTED_EDGE('',*,*,#25526,.F.) ;
#34120 = ORIENTED_EDGE('',*,*,#25529,.T.) ;
#34121 = ORIENTED_EDGE('',*,*,#25530,.F.) ;
#34122 = ORIENTED_EDGE('',*,*,#25529,.F.) ;
#34123 = ORIENTED_EDGE('',*,*,#25528,.F.) ;
#34124 = ORIENTED_EDGE('',*,*,#25531,.T.) ;
#34125 = ORIENTED_EDGE('',*,*,#25532,.T.) ;
#34126 = ORIENTED_EDGE('',*,*,#25533,.T.) ;
#34127 = ORIENTED_EDGE('',*,*,#25534,.T.) ;
#34128 = ORIENTED_EDGE('',*,*,#25532,.F.) ;
#34129 = ORIENTED_EDGE('',*,*,#25534,.F.) ;
#34130 = ORIENTED_EDGE('',*,*,#25535,.T.) ;
#34131 = ORIENTED_EDGE('',*,*,#25536,.F.) ;
#34132 = ORIENTED_EDGE('',*,*,#25537,.F.) ;
#34133 = ORIENTED_EDGE('',*,*,#25535,.F.) ;
#34134 = ORIENTED_EDGE('',*,*,#25533,.F.) ;
#34135 = ORIENTED_EDGE('',*,*,#25538,.F.) ;
#34136 = ORIENTED_EDGE('',*,*,#25539,.F.) ;
#34137 = ORIENTED_EDGE('',*,*,#25540,.F.) ;
#34138 = ORIENTED_EDGE('',*,*,#25541,.T.) ;
#34139 = ORIENTED_EDGE('',*,*,#25542,.F.) ;
#34140 = ORIENTED_EDGE('',*,*,#25543,.F.) ;
#34141 = ORIENTED_EDGE('',*,*,#25531,.F.) ;
#34142 = ORIENTED_EDGE('',*,*,#25544,.T.) ;
#34143 = ORIENTED_EDGE('',*,*,#25545,.T.) ;
#34144 = ORIENTED_EDGE('',*,*,#25536,.T.) ;
#34145 = ORIENTED_EDGE('',*,*,#25537,.T.) ;
#34146 = ORIENTED_EDGE('',*,*,#25545,.F.) ;
#34147 = ORIENTED_EDGE('',*,*,#25546,.T.) ;
#34148 = ORIENTED_EDGE('',*,*,#25547,.T.) ;
#34149 = ORIENTED_EDGE('',*,*,#25298,.T.) ;
#34150 = ORIENTED_EDGE('',*,*,#25548,.T.) ;
#34151 = ORIENTED_EDGE('',*,*,#25549,.T.) ;
#34152 = ORIENTED_EDGE('',*,*,#25550,.F.) ;
#34153 = ORIENTED_EDGE('',*,*,#25544,.F.) ;
#34154 = ORIENTED_EDGE('',*,*,#25551,.T.) ;
#34155 = ORIENTED_EDGE('',*,*,#25552,.T.) ;
#34156 = ORIENTED_EDGE('',*,*,#25553,.T.) ;
#34157 = ORIENTED_EDGE('',*,*,#25554,.T.) ;
#34158 = ORIENTED_EDGE('',*,*,#25552,.F.) ;
#34159 = ORIENTED_EDGE('',*,*,#25554,.F.) ;
#34160 = ORIENTED_EDGE('',*,*,#25555,.T.) ;
#34161 = ORIENTED_EDGE('',*,*,#25556,.F.) ;
#34162 = ORIENTED_EDGE('',*,*,#25557,.F.) ;
#34163 = ORIENTED_EDGE('',*,*,#25555,.F.) ;
#34164 = ORIENTED_EDGE('',*,*,#25553,.F.) ;
#34165 = ORIENTED_EDGE('',*,*,#25558,.F.) ;
#34166 = ORIENTED_EDGE('',*,*,#25559,.F.) ;
#34167 = ORIENTED_EDGE('',*,*,#25560,.F.) ;
#34168 = ORIENTED_EDGE('',*,*,#25561,.T.) ;
#34169 = ORIENTED_EDGE('',*,*,#25562,.F.) ;
#34170 = ORIENTED_EDGE('',*,*,#25563,.F.) ;
#34171 = ORIENTED_EDGE('',*,*,#25551,.F.) ;
#34172 = ORIENTED_EDGE('',*,*,#25564,.T.) ;
#34173 = ORIENTED_EDGE('',*,*,#25565,.T.) ;
#34174 = ORIENTED_EDGE('',*,*,#25556,.T.) ;
#34175 = ORIENTED_EDGE('',*,*,#25557,.T.) ;
#34176 = ORIENTED_EDGE('',*,*,#25565,.F.) ;
#34177 = ORIENTED_EDGE('',*,*,#25566,.T.) ;
#34178 = ORIENTED_EDGE('',*,*,#25567,.F.) ;
#34179 = ORIENTED_EDGE('',*,*,#25568,.T.) ;
#34180 = ORIENTED_EDGE('',*,*,#25569,.T.) ;
#34181 = ORIENTED_EDGE('',*,*,#25292,.T.) ;
#34182 = ORIENTED_EDGE('',*,*,#25570,.T.) ;
#34183 = ORIENTED_EDGE('',*,*,#25564,.F.) ;
#34184 = ORIENTED_EDGE('',*,*,#25571,.T.) ;
#34185 = ORIENTED_EDGE('',*,*,#25572,.T.) ;
#34186 = ORIENTED_EDGE('',*,*,#25573,.T.) ;
#34187 = ORIENTED_EDGE('',*,*,#25506,.T.) ;
#34188 = ORIENTED_EDGE('',*,*,#25574,.T.) ;
#34189 = ORIENTED_EDGE('',*,*,#25504,.T.) ;
#34190 = ORIENTED_EDGE('',*,*,#25573,.F.) ;
#34191 = ORIENTED_EDGE('',*,*,#25575,.T.) ;
#34192 = ORIENTED_EDGE('',*,*,#25576,.T.) ;
#34193 = ORIENTED_EDGE('',*,*,#25502,.T.) ;
#34194 = ORIENTED_EDGE('',*,*,#25574,.F.) ;
#34195 = ORIENTED_EDGE('',*,*,#25577,.T.) ;
#34196 = ORIENTED_EDGE('',*,*,#25578,.T.) ;
#34197 = ORIENTED_EDGE('',*,*,#25500,.T.) ;
#34198 = ORIENTED_EDGE('',*,*,#25576,.F.) ;
#34199 = ORIENTED_EDGE('',*,*,#25579,.T.) ;
#34200 = ORIENTED_EDGE('',*,*,#25580,.T.) ;
#34201 = ORIENTED_EDGE('',*,*,#25498,.T.) ;
#34202 = ORIENTED_EDGE('',*,*,#25578,.F.) ;
#34203 = ORIENTED_EDGE('',*,*,#25581,.T.) ;
#34204 = ORIENTED_EDGE('',*,*,#25581,.F.) ;
#34205 = ORIENTED_EDGE('',*,*,#25579,.F.) ;
#34206 = ORIENTED_EDGE('',*,*,#25577,.F.) ;
#34207 = ORIENTED_EDGE('',*,*,#25575,.F.) ;
#34208 = ORIENTED_EDGE('',*,*,#25572,.F.) ;
#34209 = ORIENTED_EDGE('',*,*,#25582,.F.) ;
#34210 = ORIENTED_EDGE('',*,*,#25583,.F.) ;
#34211 = ORIENTED_EDGE('',*,*,#25584,.F.) ;
#34212 = ORIENTED_EDGE('',*,*,#25585,.F.) ;
#34213 = ORIENTED_EDGE('',*,*,#25586,.F.) ;
#34214 = ORIENTED_EDGE('',*,*,#25587,.F.) ;
#34215 = ORIENTED_EDGE('',*,*,#25561,.F.) ;
#34216 = ORIENTED_EDGE('',*,*,#25588,.F.) ;
#34217 = ORIENTED_EDGE('',*,*,#25589,.F.) ;
#34218 = ORIENTED_EDGE('',*,*,#25590,.F.) ;
#34219 = ORIENTED_EDGE('',*,*,#25591,.F.) ;
#34220 = ORIENTED_EDGE('',*,*,#25592,.F.) ;
#34221 = ORIENTED_EDGE('',*,*,#25541,.F.) ;
#34222 = ORIENTED_EDGE('',*,*,#25593,.F.) ;
#34223 = ORIENTED_EDGE('',*,*,#25594,.F.) ;
#34224 = ORIENTED_EDGE('',*,*,#25595,.F.) ;
#34225 = ORIENTED_EDGE('',*,*,#25596,.F.) ;
#34226 = ORIENTED_EDGE('',*,*,#25597,.F.) ;
#34227 = ORIENTED_EDGE('',*,*,#25598,.F.) ;
#34228 = ORIENTED_EDGE('',*,*,#25571,.F.) ;
#34229 = ORIENTED_EDGE('',*,*,#25508,.T.) ;
#34230 = ORIENTED_EDGE('',*,*,#25599,.F.) ;
#34231 = ORIENTED_EDGE('',*,*,#25582,.T.) ;
#34232 = ORIENTED_EDGE('',*,*,#25482,.F.) ;
#34233 = ORIENTED_EDGE('',*,*,#25600,.F.) ;
#34234 = ORIENTED_EDGE('',*,*,#25601,.F.) ;
#34235 = ORIENTED_EDGE('',*,*,#25602,.T.) ;
#34236 = ORIENTED_EDGE('',*,*,#25550,.T.) ;
#34237 = ORIENTED_EDGE('',*,*,#25603,.T.) ;
#34238 = ORIENTED_EDGE('',*,*,#25604,.F.) ;
#34239 = ORIENTED_EDGE('',*,*,#25605,.F.) ;
#34240 = ORIENTED_EDGE('',*,*,#25295,.T.) ;
#34241 = ORIENTED_EDGE('',*,*,#25606,.T.) ;
#34242 = ORIENTED_EDGE('',*,*,#25607,.F.) ;
#34243 = ORIENTED_EDGE('',*,*,#25608,.T.) ;
#34244 = ORIENTED_EDGE('',*,*,#25567,.T.) ;
#34245 = ORIENTED_EDGE('',*,*,#25609,.T.) ;
#34246 = ORIENTED_EDGE('',*,*,#25610,.F.) ;
#34247 = ORIENTED_EDGE('',*,*,#25611,.F.) ;
#34248 = ORIENTED_EDGE('',*,*,#25612,.F.) ;
#34249 = ORIENTED_EDGE('',*,*,#25613,.F.) ;
#34250 = ORIENTED_EDGE('',*,*,#25614,.F.) ;
#34251 = ORIENTED_EDGE('',*,*,#25615,.F.) ;
#34252 = ORIENTED_EDGE('',*,*,#25616,.F.) ;
#34253 = ORIENTED_EDGE('',*,*,#25452,.F.) ;
#34254 = ORIENTED_EDGE('',*,*,#25455,.F.) ;
#34255 = ORIENTED_EDGE('',*,*,#25458,.F.) ;
#34256 = ORIENTED_EDGE('',*,*,#25461,.F.) ;
#34257 = ORIENTED_EDGE('',*,*,#25464,.F.) ;
#34258 = ORIENTED_EDGE('',*,*,#25467,.F.) ;
#34259 = ORIENTED_EDGE('',*,*,#25470,.F.) ;
#34260 = ORIENTED_EDGE('',*,*,#25473,.F.) ;
#34261 = ORIENTED_EDGE('',*,*,#25476,.F.) ;
#34262 = ORIENTED_EDGE('',*,*,#25479,.F.) ;
#34263 = ORIENTED_EDGE('',*,*,#25580,.F.) ;
#34264 = ORIENTED_EDGE('',*,*,#25598,.T.) ;
#34265 = ORIENTED_EDGE('',*,*,#25617,.T.) ;
#34266 = ORIENTED_EDGE('',*,*,#25496,.T.) ;
#34267 = ORIENTED_EDGE('',*,*,#25618,.F.) ;
#34268 = ORIENTED_EDGE('',*,*,#25290,.T.) ;
#34269 = ORIENTED_EDGE('',*,*,#25619,.T.) ;
#34270 = ORIENTED_EDGE('',*,*,#25611,.T.) ;
#34271 = ORIENTED_EDGE('',*,*,#25620,.T.) ;
#34272 = ORIENTED_EDGE('',*,*,#25612,.T.) ;
#34273 = ORIENTED_EDGE('',*,*,#25619,.F.) ;
#34274 = ORIENTED_EDGE('',*,*,#25621,.T.) ;
#34275 = ORIENTED_EDGE('',*,*,#25622,.T.) ;
#34276 = ORIENTED_EDGE('',*,*,#25613,.T.) ;
#34277 = ORIENTED_EDGE('',*,*,#25620,.F.) ;
#34278 = ORIENTED_EDGE('',*,*,#25623,.T.) ;
#34279 = ORIENTED_EDGE('',*,*,#25624,.T.) ;
#34280 = ORIENTED_EDGE('',*,*,#25614,.T.) ;
#34281 = ORIENTED_EDGE('',*,*,#25622,.F.) ;
#34282 = ORIENTED_EDGE('',*,*,#25625,.T.) ;
#34283 = ORIENTED_EDGE('',*,*,#25626,.T.) ;
#34284 = ORIENTED_EDGE('',*,*,#25615,.T.) ;
#34285 = ORIENTED_EDGE('',*,*,#25624,.F.) ;
#34286 = ORIENTED_EDGE('',*,*,#25627,.T.) ;
#34287 = ORIENTED_EDGE('',*,*,#25626,.F.) ;
#34288 = ORIENTED_EDGE('',*,*,#25277,.T.) ;
#34289 = ORIENTED_EDGE('',*,*,#25448,.T.) ;
#34290 = ORIENTED_EDGE('',*,*,#25616,.T.) ;
#34291 = ORIENTED_EDGE('',*,*,#25449,.F.) ;
#34292 = ORIENTED_EDGE('',*,*,#25333,.T.) ;
#34293 = ORIENTED_EDGE('',*,*,#25628,.T.) ;
#34294 = ORIENTED_EDGE('',*,*,#25511,.T.) ;
#34295 = ORIENTED_EDGE('',*,*,#25627,.F.) ;
#34296 = ORIENTED_EDGE('',*,*,#25629,.F.) ;
#34297 = ORIENTED_EDGE('',*,*,#25630,.T.) ;
#34298 = ORIENTED_EDGE('',*,*,#25631,.T.) ;
#34299 = ORIENTED_EDGE('',*,*,#25278,.T.) ;
#34300 = ORIENTED_EDGE('',*,*,#25625,.F.) ;
#34301 = ORIENTED_EDGE('',*,*,#25632,.F.) ;
#34302 = ORIENTED_EDGE('',*,*,#25633,.T.) ;
#34303 = ORIENTED_EDGE('',*,*,#25629,.T.) ;
#34304 = ORIENTED_EDGE('',*,*,#25623,.F.) ;
#34305 = ORIENTED_EDGE('',*,*,#25634,.F.) ;
#34306 = ORIENTED_EDGE('',*,*,#25635,.T.) ;
#34307 = ORIENTED_EDGE('',*,*,#25632,.T.) ;
#34308 = ORIENTED_EDGE('',*,*,#25621,.F.) ;
#34309 = ORIENTED_EDGE('',*,*,#25289,.T.) ;
#34310 = ORIENTED_EDGE('',*,*,#25636,.F.) ;
#34311 = ORIENTED_EDGE('',*,*,#25637,.T.) ;
#34312 = ORIENTED_EDGE('',*,*,#25634,.T.) ;
#34313 = ORIENTED_EDGE('',*,*,#25638,.F.) ;
#34314 = ORIENTED_EDGE('',*,*,#25600,.T.) ;
#34315 = ORIENTED_EDGE('',*,*,#25486,.T.) ;
#34316 = ORIENTED_EDGE('',*,*,#25300,.T.) ;
#34317 = ORIENTED_EDGE('',*,*,#25638,.T.) ;
#34318 = ORIENTED_EDGE('',*,*,#25299,.F.) ;
#34319 = ORIENTED_EDGE('',*,*,#25547,.F.) ;
#34320 = ORIENTED_EDGE('',*,*,#25639,.F.) ;
#34321 = ORIENTED_EDGE('',*,*,#25601,.T.) ;
#34322 = ORIENTED_EDGE('',*,*,#25640,.F.) ;
#34323 = ORIENTED_EDGE('',*,*,#25641,.F.) ;
#34324 = ORIENTED_EDGE('',*,*,#25642,.F.) ;
#34325 = ORIENTED_EDGE('',*,*,#25643,.T.) ;
#34326 = ORIENTED_EDGE('',*,*,#25644,.T.) ;
#34327 = ORIENTED_EDGE('',*,*,#25641,.T.) ;
#34328 = ORIENTED_EDGE('',*,*,#25159,.T.) ;
#34329 = ORIENTED_EDGE('',*,*,#25643,.F.) ;
#34330 = ORIENTED_EDGE('',*,*,#25158,.T.) ;
#34331 = ORIENTED_EDGE('',*,*,#25645,.T.) ;
#34332 = ORIENTED_EDGE('',*,*,#25646,.F.) ;
#34333 = ORIENTED_EDGE('',*,*,#25647,.T.) ;
#34334 = ORIENTED_EDGE('',*,*,#25648,.T.) ;
#34335 = ORIENTED_EDGE('',*,*,#25649,.T.) ;
#34336 = ORIENTED_EDGE('',*,*,#25647,.F.) ;
#34337 = ORIENTED_EDGE('',*,*,#25650,.T.) ;
#34338 = ORIENTED_EDGE('',*,*,#25642,.T.) ;
#34339 = ORIENTED_EDGE('',*,*,#25651,.T.) ;
#34340 = ORIENTED_EDGE('',*,*,#25163,.T.) ;
#34341 = ORIENTED_EDGE('',*,*,#25652,.F.) ;
#34342 = ORIENTED_EDGE('',*,*,#25653,.F.) ;
#34343 = ORIENTED_EDGE('',*,*,#25654,.F.) ;
#34344 = ORIENTED_EDGE('',*,*,#25655,.F.) ;
#34345 = ORIENTED_EDGE('',*,*,#25656,.F.) ;
#34346 = ORIENTED_EDGE('',*,*,#25161,.T.) ;
#34347 = ORIENTED_EDGE('',*,*,#25657,.F.) ;
#34348 = ORIENTED_EDGE('',*,*,#25652,.T.) ;
#34349 = ORIENTED_EDGE('',*,*,#25162,.T.) ;
#34350 = ORIENTED_EDGE('',*,*,#25656,.T.) ;
#34351 = ORIENTED_EDGE('',*,*,#25658,.T.) ;
#34352 = ORIENTED_EDGE('',*,*,#25657,.T.) ;
#34353 = ORIENTED_EDGE('',*,*,#25160,.T.) ;
#34354 = ORIENTED_EDGE('',*,*,#25640,.T.) ;
#34355 = ORIENTED_EDGE('',*,*,#25659,.T.) ;
#34356 = ORIENTED_EDGE('',*,*,#25660,.T.) ;
#34357 = ORIENTED_EDGE('',*,*,#25661,.T.) ;
#34358 = ORIENTED_EDGE('',*,*,#25405,.T.) ;
#34359 = ORIENTED_EDGE('',*,*,#25662,.T.) ;
#34360 = ORIENTED_EDGE('',*,*,#25655,.T.) ;
#34361 = ORIENTED_EDGE('',*,*,#25663,.T.) ;
#34362 = ORIENTED_EDGE('',*,*,#25660,.F.) ;
#34363 = ORIENTED_EDGE('',*,*,#25664,.T.) ;
#34364 = ORIENTED_EDGE('',*,*,#25665,.T.) ;
#34365 = ORIENTED_EDGE('',*,*,#25666,.T.) ;
#34366 = ORIENTED_EDGE('',*,*,#25653,.T.) ;
#34367 = ORIENTED_EDGE('',*,*,#25667,.T.) ;
#34368 = ORIENTED_EDGE('',*,*,#25417,.T.) ;
#34369 = ORIENTED_EDGE('',*,*,#25668,.T.) ;
#34370 = ORIENTED_EDGE('',*,*,#25665,.F.) ;
#34371 = ORIENTED_EDGE('',*,*,#25669,.T.) ;
#34372 = ORIENTED_EDGE('',*,*,#25670,.T.) ;
#34373 = ORIENTED_EDGE('',*,*,#25164,.T.) ;
#34374 = ORIENTED_EDGE('',*,*,#25654,.T.) ;
#34375 = ORIENTED_EDGE('',*,*,#25671,.T.) ;
#34376 = ORIENTED_EDGE('',*,*,#25670,.F.) ;
#34377 = ORIENTED_EDGE('',*,*,#25672,.T.) ;
#34378 = ORIENTED_EDGE('',*,*,#25673,.T.) ;
#34379 = ORIENTED_EDGE('',*,*,#25648,.F.) ;
#34380 = ORIENTED_EDGE('',*,*,#25674,.T.) ;
#34381 = ORIENTED_EDGE('',*,*,#25675,.T.) ;
#34382 = ORIENTED_EDGE('',*,*,#25407,.T.) ;
#34383 = ORIENTED_EDGE('',*,*,#25651,.F.) ;
#34384 = ORIENTED_EDGE('',*,*,#25644,.F.) ;
#34385 = ORIENTED_EDGE('',*,*,#25676,.F.) ;
#34386 = ORIENTED_EDGE('',*,*,#25674,.F.) ;
#34387 = ORIENTED_EDGE('',*,*,#25673,.F.) ;
#34388 = ORIENTED_EDGE('',*,*,#25677,.T.) ;
#34389 = ORIENTED_EDGE('',*,*,#25678,.T.) ;
#34390 = ORIENTED_EDGE('',*,*,#25165,.T.) ;
#34391 = ORIENTED_EDGE('',*,*,#25672,.F.) ;
#34392 = ORIENTED_EDGE('',*,*,#25679,.T.) ;
#34393 = ORIENTED_EDGE('',*,*,#25680,.F.) ;
#34394 = ORIENTED_EDGE('',*,*,#25681,.T.) ;
#34395 = ORIENTED_EDGE('',*,*,#25671,.F.) ;
#34396 = ORIENTED_EDGE('',*,*,#25666,.F.) ;
#34397 = ORIENTED_EDGE('',*,*,#25682,.F.) ;
#34398 = ORIENTED_EDGE('',*,*,#25679,.F.) ;
#34399 = ORIENTED_EDGE('',*,*,#25683,.T.) ;
#34400 = ORIENTED_EDGE('',*,*,#25684,.T.) ;
#34401 = ORIENTED_EDGE('',*,*,#25393,.T.) ;
#34402 = ORIENTED_EDGE('',*,*,#25685,.T.) ;
#34403 = ORIENTED_EDGE('',*,*,#25686,.T.) ;
#34404 = ORIENTED_EDGE('',*,*,#25687,.T.) ;
#34405 = ORIENTED_EDGE('',*,*,#25683,.F.) ;
#34406 = ORIENTED_EDGE('',*,*,#25688,.T.) ;
#34407 = ORIENTED_EDGE('',*,*,#25686,.F.) ;
#34408 = ORIENTED_EDGE('',*,*,#25689,.T.) ;
#34409 = ORIENTED_EDGE('',*,*,#25690,.T.) ;
#34410 = ORIENTED_EDGE('',*,*,#25689,.F.) ;
#34411 = ORIENTED_EDGE('',*,*,#25691,.T.) ;
#34412 = ORIENTED_EDGE('',*,*,#25692,.F.) ;
#34413 = ORIENTED_EDGE('',*,*,#25215,.F.) ;
#34414 = ORIENTED_EDGE('',*,*,#25688,.F.) ;
#34415 = ORIENTED_EDGE('',*,*,#25685,.F.) ;
#34416 = ORIENTED_EDGE('',*,*,#25392,.F.) ;
#34417 = ORIENTED_EDGE('',*,*,#25693,.T.) ;
#34418 = ORIENTED_EDGE('',*,*,#25691,.F.) ;
#34419 = ORIENTED_EDGE('',*,*,#25694,.T.) ;
#34420 = ORIENTED_EDGE('',*,*,#25695,.T.) ;
#34421 = ORIENTED_EDGE('',*,*,#25696,.T.) ;
#34422 = ORIENTED_EDGE('',*,*,#25697,.T.) ;
#34423 = ORIENTED_EDGE('',*,*,#25698,.T.) ;
#34424 = ORIENTED_EDGE('',*,*,#25694,.F.) ;
#34425 = ORIENTED_EDGE('',*,*,#25699,.T.) ;
#34426 = ORIENTED_EDGE('',*,*,#25403,.T.) ;
#34427 = ORIENTED_EDGE('',*,*,#25700,.T.) ;
#34428 = ORIENTED_EDGE('',*,*,#25697,.F.) ;
#34429 = ORIENTED_EDGE('',*,*,#25701,.T.) ;
#34430 = ORIENTED_EDGE('',*,*,#25701,.F.) ;
#34431 = ORIENTED_EDGE('',*,*,#25699,.F.) ;
#34432 = ORIENTED_EDGE('',*,*,#25702,.F.) ;
#34433 = ORIENTED_EDGE('',*,*,#25703,.T.) ;
#34434 = ORIENTED_EDGE('',*,*,#25390,.F.) ;
#34435 = ORIENTED_EDGE('',*,*,#25696,.F.) ;
#34436 = ORIENTED_EDGE('',*,*,#25205,.F.) ;
#34437 = ORIENTED_EDGE('',*,*,#25704,.T.) ;
#34438 = ORIENTED_EDGE('',*,*,#25702,.T.) ;
#34439 = ORIENTED_EDGE('',*,*,#25705,.T.) ;
#34440 = ORIENTED_EDGE('',*,*,#25283,.T.) ;
#34441 = ORIENTED_EDGE('',*,*,#25706,.T.) ;
#34442 = ORIENTED_EDGE('',*,*,#25707,.T.) ;
#34443 = ORIENTED_EDGE('',*,*,#25708,.T.) ;
#34444 = ORIENTED_EDGE('',*,*,#25284,.T.) ;
#34445 = ORIENTED_EDGE('',*,*,#25705,.F.) ;
#34446 = ORIENTED_EDGE('',*,*,#25709,.T.) ;
#34447 = ORIENTED_EDGE('',*,*,#25710,.T.) ;
#34448 = ORIENTED_EDGE('',*,*,#25285,.T.) ;
#34449 = ORIENTED_EDGE('',*,*,#25708,.F.) ;
#34450 = ORIENTED_EDGE('',*,*,#25711,.T.) ;
#34451 = ORIENTED_EDGE('',*,*,#25712,.T.) ;
#34452 = ORIENTED_EDGE('',*,*,#25286,.T.) ;
#34453 = ORIENTED_EDGE('',*,*,#25710,.F.) ;
#34454 = ORIENTED_EDGE('',*,*,#25713,.T.) ;
#34455 = ORIENTED_EDGE('',*,*,#25714,.T.) ;
#34456 = ORIENTED_EDGE('',*,*,#25287,.T.) ;
#34457 = ORIENTED_EDGE('',*,*,#25712,.F.) ;
#34458 = ORIENTED_EDGE('',*,*,#25715,.T.) ;
#34459 = ORIENTED_EDGE('',*,*,#25636,.T.) ;
#34460 = ORIENTED_EDGE('',*,*,#25288,.T.) ;
#34461 = ORIENTED_EDGE('',*,*,#25714,.F.) ;
#34462 = ORIENTED_EDGE('',*,*,#25716,.T.) ;
#34463 = ORIENTED_EDGE('',*,*,#25717,.F.) ;
#34464 = ORIENTED_EDGE('',*,*,#25279,.T.) ;
#34465 = ORIENTED_EDGE('',*,*,#25631,.F.) ;
#34466 = ORIENTED_EDGE('',*,*,#25718,.T.) ;
#34467 = ORIENTED_EDGE('',*,*,#25718,.F.) ;
#34468 = ORIENTED_EDGE('',*,*,#25719,.F.) ;
#34469 = ORIENTED_EDGE('',*,*,#25720,.F.) ;
#34470 = ORIENTED_EDGE('',*,*,#25721,.T.) ;
#34471 = ORIENTED_EDGE('',*,*,#25630,.F.) ;
#34472 = ORIENTED_EDGE('',*,*,#25722,.T.) ;
#34473 = ORIENTED_EDGE('',*,*,#25723,.T.) ;
#34474 = ORIENTED_EDGE('',*,*,#25719,.T.) ;
#34475 = ORIENTED_EDGE('',*,*,#25633,.F.) ;
#34476 = ORIENTED_EDGE('',*,*,#25724,.F.) ;
#34477 = ORIENTED_EDGE('',*,*,#25725,.F.) ;
#34478 = ORIENTED_EDGE('',*,*,#25722,.F.) ;
#34479 = ORIENTED_EDGE('',*,*,#25635,.F.) ;
#34480 = ORIENTED_EDGE('',*,*,#25726,.T.) ;
#34481 = ORIENTED_EDGE('',*,*,#25727,.T.) ;
#34482 = ORIENTED_EDGE('',*,*,#25724,.T.) ;
#34483 = ORIENTED_EDGE('',*,*,#25637,.F.) ;
#34484 = ORIENTED_EDGE('',*,*,#25728,.F.) ;
#34485 = ORIENTED_EDGE('',*,*,#25729,.F.) ;
#34486 = ORIENTED_EDGE('',*,*,#25726,.F.) ;
#34487 = ORIENTED_EDGE('',*,*,#25716,.F.) ;
#34488 = ORIENTED_EDGE('',*,*,#25730,.T.) ;
#34489 = ORIENTED_EDGE('',*,*,#25731,.T.) ;
#34490 = ORIENTED_EDGE('',*,*,#25728,.T.) ;
#34491 = ORIENTED_EDGE('',*,*,#25715,.F.) ;
#34492 = ORIENTED_EDGE('',*,*,#25732,.F.) ;
#34493 = ORIENTED_EDGE('',*,*,#25733,.F.) ;
#34494 = ORIENTED_EDGE('',*,*,#25730,.F.) ;
#34495 = ORIENTED_EDGE('',*,*,#25713,.F.) ;
#34496 = ORIENTED_EDGE('',*,*,#25734,.T.) ;
#34497 = ORIENTED_EDGE('',*,*,#25735,.T.) ;
#34498 = ORIENTED_EDGE('',*,*,#25732,.T.) ;
#34499 = ORIENTED_EDGE('',*,*,#25711,.F.) ;
#34500 = ORIENTED_EDGE('',*,*,#25736,.F.) ;
#34501 = ORIENTED_EDGE('',*,*,#25737,.F.) ;
#34502 = ORIENTED_EDGE('',*,*,#25734,.F.) ;
#34503 = ORIENTED_EDGE('',*,*,#25709,.F.) ;
#34504 = ORIENTED_EDGE('',*,*,#25738,.T.) ;
#34505 = ORIENTED_EDGE('',*,*,#25739,.T.) ;
#34506 = ORIENTED_EDGE('',*,*,#25736,.T.) ;
#34507 = ORIENTED_EDGE('',*,*,#25707,.F.) ;
#34508 = ORIENTED_EDGE('',*,*,#25740,.T.) ;
#34509 = ORIENTED_EDGE('',*,*,#25741,.F.) ;
#34510 = ORIENTED_EDGE('',*,*,#25738,.F.) ;
#34511 = ORIENTED_EDGE('',*,*,#25742,.T.) ;
#34512 = ORIENTED_EDGE('',*,*,#25743,.T.) ;
#34513 = ORIENTED_EDGE('',*,*,#25744,.T.) ;
#34514 = ORIENTED_EDGE('',*,*,#25335,.T.) ;
#34515 = ORIENTED_EDGE('',*,*,#25745,.T.) ;
#34516 = ORIENTED_EDGE('',*,*,#25746,.T.) ;
#34517 = ORIENTED_EDGE('',*,*,#25742,.F.) ;
#34518 = ORIENTED_EDGE('',*,*,#25348,.T.) ;
#34519 = ORIENTED_EDGE('',*,*,#25747,.T.) ;
#34520 = ORIENTED_EDGE('',*,*,#25748,.T.) ;
#34521 = ORIENTED_EDGE('',*,*,#25745,.F.) ;
#34522 = ORIENTED_EDGE('',*,*,#25347,.T.) ;
#34523 = ORIENTED_EDGE('',*,*,#25749,.T.) ;
#34524 = ORIENTED_EDGE('',*,*,#25750,.T.) ;
#34525 = ORIENTED_EDGE('',*,*,#25747,.F.) ;
#34526 = ORIENTED_EDGE('',*,*,#25346,.T.) ;
#34527 = ORIENTED_EDGE('',*,*,#25751,.T.) ;
#34528 = ORIENTED_EDGE('',*,*,#25752,.T.) ;
#34529 = ORIENTED_EDGE('',*,*,#25749,.F.) ;
#34530 = ORIENTED_EDGE('',*,*,#25345,.T.) ;
#34531 = ORIENTED_EDGE('',*,*,#25753,.T.) ;
#34532 = ORIENTED_EDGE('',*,*,#25754,.T.) ;
#34533 = ORIENTED_EDGE('',*,*,#25751,.F.) ;
#34534 = ORIENTED_EDGE('',*,*,#25344,.T.) ;
#34535 = ORIENTED_EDGE('',*,*,#25755,.T.) ;
#34536 = ORIENTED_EDGE('',*,*,#25756,.T.) ;
#34537 = ORIENTED_EDGE('',*,*,#25753,.F.) ;
#34538 = ORIENTED_EDGE('',*,*,#25343,.T.) ;
#34539 = ORIENTED_EDGE('',*,*,#25757,.T.) ;
#34540 = ORIENTED_EDGE('',*,*,#25758,.T.) ;
#34541 = ORIENTED_EDGE('',*,*,#25755,.F.) ;
#34542 = ORIENTED_EDGE('',*,*,#25342,.T.) ;
#34543 = ORIENTED_EDGE('',*,*,#25759,.T.) ;
#34544 = ORIENTED_EDGE('',*,*,#25760,.T.) ;
#34545 = ORIENTED_EDGE('',*,*,#25757,.F.) ;
#34546 = ORIENTED_EDGE('',*,*,#25341,.T.) ;
#34547 = ORIENTED_EDGE('',*,*,#25761,.T.) ;
#34548 = ORIENTED_EDGE('',*,*,#25762,.T.) ;
#34549 = ORIENTED_EDGE('',*,*,#25763,.T.) ;
#34550 = ORIENTED_EDGE('',*,*,#25340,.T.) ;
#34551 = ORIENTED_EDGE('',*,*,#25764,.T.) ;
#34552 = ORIENTED_EDGE('',*,*,#25765,.T.) ;
#34553 = ORIENTED_EDGE('',*,*,#25761,.F.) ;
#34554 = ORIENTED_EDGE('',*,*,#25339,.T.) ;
#34555 = ORIENTED_EDGE('',*,*,#25766,.T.) ;
#34556 = ORIENTED_EDGE('',*,*,#25767,.T.) ;
#34557 = ORIENTED_EDGE('',*,*,#25764,.F.) ;
#34558 = ORIENTED_EDGE('',*,*,#25338,.T.) ;
#34559 = ORIENTED_EDGE('',*,*,#25768,.T.) ;
#34560 = ORIENTED_EDGE('',*,*,#25769,.T.) ;
#34561 = ORIENTED_EDGE('',*,*,#25766,.F.) ;
#34562 = ORIENTED_EDGE('',*,*,#25337,.T.) ;
#34563 = ORIENTED_EDGE('',*,*,#25770,.T.) ;
#34564 = ORIENTED_EDGE('',*,*,#25771,.T.) ;
#34565 = ORIENTED_EDGE('',*,*,#25768,.F.) ;
#34566 = ORIENTED_EDGE('',*,*,#25336,.T.) ;
#34567 = ORIENTED_EDGE('',*,*,#25763,.F.) ;
#34568 = ORIENTED_EDGE('',*,*,#25772,.T.) ;
#34569 = ORIENTED_EDGE('',*,*,#25759,.F.) ;
#34570 = ORIENTED_EDGE('',*,*,#25744,.F.) ;
#34571 = ORIENTED_EDGE('',*,*,#25773,.T.) ;
#34572 = ORIENTED_EDGE('',*,*,#25770,.F.) ;
#34573 = ORIENTED_EDGE('',*,*,#25750,.F.) ;
#34574 = ORIENTED_EDGE('',*,*,#25774,.T.) ;
#34575 = ORIENTED_EDGE('',*,*,#25775,.T.) ;
#34576 = ORIENTED_EDGE('',*,*,#25776,.T.) ;
#34577 = ORIENTED_EDGE('',*,*,#25752,.F.) ;
#34578 = ORIENTED_EDGE('',*,*,#25777,.F.) ;
#34579 = ORIENTED_EDGE('',*,*,#25778,.F.) ;
#34580 = ORIENTED_EDGE('',*,*,#25774,.F.) ;
#34581 = ORIENTED_EDGE('',*,*,#25754,.F.) ;
#34582 = ORIENTED_EDGE('',*,*,#25779,.T.) ;
#34583 = ORIENTED_EDGE('',*,*,#25780,.T.) ;
#34584 = ORIENTED_EDGE('',*,*,#25777,.T.) ;
#34585 = ORIENTED_EDGE('',*,*,#25756,.F.) ;
#34586 = ORIENTED_EDGE('',*,*,#25781,.F.) ;
#34587 = ORIENTED_EDGE('',*,*,#25782,.F.) ;
#34588 = ORIENTED_EDGE('',*,*,#25779,.F.) ;
#34589 = ORIENTED_EDGE('',*,*,#25758,.F.) ;
#34590 = ORIENTED_EDGE('',*,*,#25783,.T.) ;
#34591 = ORIENTED_EDGE('',*,*,#25784,.T.) ;
#34592 = ORIENTED_EDGE('',*,*,#25781,.T.) ;
#34593 = ORIENTED_EDGE('',*,*,#25760,.F.) ;
#34594 = ORIENTED_EDGE('',*,*,#25785,.F.) ;
#34595 = ORIENTED_EDGE('',*,*,#25786,.F.) ;
#34596 = ORIENTED_EDGE('',*,*,#25783,.F.) ;
#34597 = ORIENTED_EDGE('',*,*,#25772,.F.) ;
#34598 = ORIENTED_EDGE('',*,*,#25787,.T.) ;
#34599 = ORIENTED_EDGE('',*,*,#25788,.T.) ;
#34600 = ORIENTED_EDGE('',*,*,#25785,.T.) ;
#34601 = ORIENTED_EDGE('',*,*,#25762,.F.) ;
#34602 = ORIENTED_EDGE('',*,*,#25789,.F.) ;
#34603 = ORIENTED_EDGE('',*,*,#25790,.F.) ;
#34604 = ORIENTED_EDGE('',*,*,#25787,.F.) ;
#34605 = ORIENTED_EDGE('',*,*,#25363,.T.) ;
#34606 = ORIENTED_EDGE('',*,*,#25791,.F.) ;
#34607 = ORIENTED_EDGE('',*,*,#25792,.F.) ;
#34608 = ORIENTED_EDGE('',*,*,#25793,.F.) ;
#34609 = ORIENTED_EDGE('',*,*,#25794,.F.) ;
#34610 = ORIENTED_EDGE('',*,*,#25795,.F.) ;
#34611 = ORIENTED_EDGE('',*,*,#25353,.T.) ;
#34612 = ORIENTED_EDGE('',*,*,#25796,.F.) ;
#34613 = ORIENTED_EDGE('',*,*,#25797,.T.) ;
#34614 = ORIENTED_EDGE('',*,*,#25354,.T.) ;
#34615 = ORIENTED_EDGE('',*,*,#25795,.T.) ;
#34616 = ORIENTED_EDGE('',*,*,#25798,.T.) ;
#34617 = ORIENTED_EDGE('',*,*,#25799,.T.) ;
#34618 = ORIENTED_EDGE('',*,*,#25355,.T.) ;
#34619 = ORIENTED_EDGE('',*,*,#25797,.F.) ;
#34620 = ORIENTED_EDGE('',*,*,#25800,.T.) ;
#34621 = ORIENTED_EDGE('',*,*,#25801,.T.) ;
#34622 = ORIENTED_EDGE('',*,*,#25356,.T.) ;
#34623 = ORIENTED_EDGE('',*,*,#25799,.F.) ;
#34624 = ORIENTED_EDGE('',*,*,#25802,.T.) ;
#34625 = ORIENTED_EDGE('',*,*,#25803,.T.) ;
#34626 = ORIENTED_EDGE('',*,*,#25357,.T.) ;
#34627 = ORIENTED_EDGE('',*,*,#25801,.F.) ;
#34628 = ORIENTED_EDGE('',*,*,#25804,.T.) ;
#34629 = ORIENTED_EDGE('',*,*,#25805,.T.) ;
#34630 = ORIENTED_EDGE('',*,*,#25358,.T.) ;
#34631 = ORIENTED_EDGE('',*,*,#25803,.F.) ;
#34632 = ORIENTED_EDGE('',*,*,#25806,.T.) ;
#34633 = ORIENTED_EDGE('',*,*,#25807,.T.) ;
#34634 = ORIENTED_EDGE('',*,*,#25359,.T.) ;
#34635 = ORIENTED_EDGE('',*,*,#25805,.F.) ;
#34636 = ORIENTED_EDGE('',*,*,#25808,.T.) ;
#34637 = ORIENTED_EDGE('',*,*,#25809,.T.) ;
#34638 = ORIENTED_EDGE('',*,*,#25360,.T.) ;
#34639 = ORIENTED_EDGE('',*,*,#25807,.F.) ;
#34640 = ORIENTED_EDGE('',*,*,#25810,.T.) ;
#34641 = ORIENTED_EDGE('',*,*,#25811,.T.) ;
#34642 = ORIENTED_EDGE('',*,*,#25361,.T.) ;
#34643 = ORIENTED_EDGE('',*,*,#25809,.F.) ;
#34644 = ORIENTED_EDGE('',*,*,#25812,.T.) ;
#34645 = ORIENTED_EDGE('',*,*,#25791,.T.) ;
#34646 = ORIENTED_EDGE('',*,*,#25362,.T.) ;
#34647 = ORIENTED_EDGE('',*,*,#25811,.F.) ;
#34648 = ORIENTED_EDGE('',*,*,#25813,.T.) ;
#34649 = ORIENTED_EDGE('',*,*,#25814,.T.) ;
#34650 = ORIENTED_EDGE('',*,*,#25815,.T.) ;
#34651 = ORIENTED_EDGE('',*,*,#25796,.T.) ;
#34652 = ORIENTED_EDGE('',*,*,#25352,.T.) ;
#34653 = ORIENTED_EDGE('',*,*,#25816,.T.) ;
#34654 = ORIENTED_EDGE('',*,*,#25817,.T.) ;
#34655 = ORIENTED_EDGE('',*,*,#25794,.T.) ;
#34656 = ORIENTED_EDGE('',*,*,#25818,.T.) ;
#34657 = ORIENTED_EDGE('',*,*,#25816,.F.) ;
#34658 = ORIENTED_EDGE('',*,*,#25819,.T.) ;
#34659 = ORIENTED_EDGE('',*,*,#25820,.T.) ;
#34660 = ORIENTED_EDGE('',*,*,#25821,.T.) ;
#34661 = ORIENTED_EDGE('',*,*,#25822,.T.) ;
#34662 = ORIENTED_EDGE('',*,*,#25792,.T.) ;
#34663 = ORIENTED_EDGE('',*,*,#25823,.T.) ;
#34664 = ORIENTED_EDGE('',*,*,#25821,.F.) ;
#34665 = ORIENTED_EDGE('',*,*,#25824,.T.) ;
#34666 = ORIENTED_EDGE('',*,*,#25825,.T.) ;
#34667 = ORIENTED_EDGE('',*,*,#25826,.F.) ;
#34668 = ORIENTED_EDGE('',*,*,#25364,.T.) ;
#34669 = ORIENTED_EDGE('',*,*,#25793,.T.) ;
#34670 = ORIENTED_EDGE('',*,*,#25827,.T.) ;
#34671 = ORIENTED_EDGE('',*,*,#25818,.F.) ;
#34672 = ORIENTED_EDGE('',*,*,#25815,.F.) ;
#34673 = ORIENTED_EDGE('',*,*,#25828,.T.) ;
#34674 = ORIENTED_EDGE('',*,*,#25829,.F.) ;
#34675 = ORIENTED_EDGE('',*,*,#25830,.T.) ;
#34676 = ORIENTED_EDGE('',*,*,#25831,.T.) ;
#34677 = ORIENTED_EDGE('',*,*,#25832,.T.) ;
#34678 = ORIENTED_EDGE('',*,*,#25432,.T.) ;
#34679 = ORIENTED_EDGE('',*,*,#25833,.T.) ;
#34680 = ORIENTED_EDGE('',*,*,#25834,.T.) ;
#34681 = ORIENTED_EDGE('',*,*,#25830,.F.) ;
#34682 = ORIENTED_EDGE('',*,*,#25445,.T.) ;
#34683 = ORIENTED_EDGE('',*,*,#25835,.T.) ;
#34684 = ORIENTED_EDGE('',*,*,#25836,.T.) ;
#34685 = ORIENTED_EDGE('',*,*,#25837,.T.) ;
#34686 = ORIENTED_EDGE('',*,*,#25444,.T.) ;
#34687 = ORIENTED_EDGE('',*,*,#25838,.T.) ;
#34688 = ORIENTED_EDGE('',*,*,#25839,.T.) ;
#34689 = ORIENTED_EDGE('',*,*,#25835,.F.) ;
#34690 = ORIENTED_EDGE('',*,*,#25443,.T.) ;
#34691 = ORIENTED_EDGE('',*,*,#25840,.T.) ;
#34692 = ORIENTED_EDGE('',*,*,#25841,.T.) ;
#34693 = ORIENTED_EDGE('',*,*,#25838,.F.) ;
#34694 = ORIENTED_EDGE('',*,*,#25442,.T.) ;
#34695 = ORIENTED_EDGE('',*,*,#25842,.T.) ;
#34696 = ORIENTED_EDGE('',*,*,#25843,.T.) ;
#34697 = ORIENTED_EDGE('',*,*,#25840,.F.) ;
#34698 = ORIENTED_EDGE('',*,*,#25441,.T.) ;
#34699 = ORIENTED_EDGE('',*,*,#25844,.T.) ;
#34700 = ORIENTED_EDGE('',*,*,#25845,.T.) ;
#34701 = ORIENTED_EDGE('',*,*,#25842,.F.) ;
#34702 = ORIENTED_EDGE('',*,*,#25440,.T.) ;
#34703 = ORIENTED_EDGE('',*,*,#25837,.F.) ;
#34704 = ORIENTED_EDGE('',*,*,#25846,.T.) ;
#34705 = ORIENTED_EDGE('',*,*,#25833,.F.) ;
#34706 = ORIENTED_EDGE('',*,*,#25847,.T.) ;
#34707 = ORIENTED_EDGE('',*,*,#25848,.T.) ;
#34708 = ORIENTED_EDGE('',*,*,#25849,.T.) ;
#34709 = ORIENTED_EDGE('',*,*,#25439,.T.) ;
#34710 = ORIENTED_EDGE('',*,*,#25847,.F.) ;
#34711 = ORIENTED_EDGE('',*,*,#25438,.T.) ;
#34712 = ORIENTED_EDGE('',*,*,#25850,.T.) ;
#34713 = ORIENTED_EDGE('',*,*,#25851,.F.) ;
#34714 = ORIENTED_EDGE('',*,*,#25849,.F.) ;
#34715 = ORIENTED_EDGE('',*,*,#25852,.T.) ;
#34716 = ORIENTED_EDGE('',*,*,#25844,.F.) ;
#34717 = ORIENTED_EDGE('',*,*,#25834,.F.) ;
#34718 = ORIENTED_EDGE('',*,*,#25853,.F.) ;
#34719 = ORIENTED_EDGE('',*,*,#25854,.F.) ;
#34720 = ORIENTED_EDGE('',*,*,#25855,.F.) ;
#34721 = ORIENTED_EDGE('',*,*,#25846,.F.) ;
#34722 = ORIENTED_EDGE('',*,*,#25856,.T.) ;
#34723 = ORIENTED_EDGE('',*,*,#25857,.T.) ;
#34724 = ORIENTED_EDGE('',*,*,#25853,.T.) ;
#34725 = ORIENTED_EDGE('',*,*,#25836,.F.) ;
#34726 = ORIENTED_EDGE('',*,*,#25858,.F.) ;
#34727 = ORIENTED_EDGE('',*,*,#25859,.F.) ;
#34728 = ORIENTED_EDGE('',*,*,#25856,.F.) ;
#34729 = ORIENTED_EDGE('',*,*,#25839,.F.) ;
#34730 = ORIENTED_EDGE('',*,*,#25860,.T.) ;
#34731 = ORIENTED_EDGE('',*,*,#25861,.T.) ;
#34732 = ORIENTED_EDGE('',*,*,#25858,.T.) ;
#34733 = ORIENTED_EDGE('',*,*,#25841,.F.) ;
#34734 = ORIENTED_EDGE('',*,*,#25862,.F.) ;
#34735 = ORIENTED_EDGE('',*,*,#25863,.F.) ;
#34736 = ORIENTED_EDGE('',*,*,#25860,.F.) ;
#34737 = ORIENTED_EDGE('',*,*,#25843,.F.) ;
#34738 = ORIENTED_EDGE('',*,*,#25864,.T.) ;
#34739 = ORIENTED_EDGE('',*,*,#25865,.T.) ;
#34740 = ORIENTED_EDGE('',*,*,#25862,.T.) ;
#34741 = ORIENTED_EDGE('',*,*,#25845,.F.) ;
#34742 = ORIENTED_EDGE('',*,*,#25866,.F.) ;
#34743 = ORIENTED_EDGE('',*,*,#25867,.F.) ;
#34744 = ORIENTED_EDGE('',*,*,#25864,.F.) ;
#34745 = ORIENTED_EDGE('',*,*,#25852,.F.) ;
#34746 = ORIENTED_EDGE('',*,*,#25868,.T.) ;
#34747 = ORIENTED_EDGE('',*,*,#25869,.T.) ;
#34748 = ORIENTED_EDGE('',*,*,#25866,.T.) ;
#34749 = ORIENTED_EDGE('',*,*,#25848,.F.) ;
#34750 = ORIENTED_EDGE('',*,*,#25870,.F.) ;
#34751 = ORIENTED_EDGE('',*,*,#25871,.F.) ;
#34752 = ORIENTED_EDGE('',*,*,#25868,.F.) ;
#34753 = ORIENTED_EDGE('',*,*,#25872,.T.) ;
#34754 = ORIENTED_EDGE('',*,*,#25873,.T.) ;
#34755 = ORIENTED_EDGE('',*,*,#25874,.T.) ;
#34756 = ORIENTED_EDGE('',*,*,#25418,.T.) ;
#34757 = ORIENTED_EDGE('',*,*,#25875,.T.) ;
#34758 = ORIENTED_EDGE('',*,*,#25876,.T.) ;
#34759 = ORIENTED_EDGE('',*,*,#25872,.F.) ;
#34760 = ORIENTED_EDGE('',*,*,#25431,.T.) ;
#34761 = ORIENTED_EDGE('',*,*,#25877,.T.) ;
#34762 = ORIENTED_EDGE('',*,*,#25878,.T.) ;
#34763 = ORIENTED_EDGE('',*,*,#25879,.T.) ;
#34764 = ORIENTED_EDGE('',*,*,#25430,.T.) ;
#34765 = ORIENTED_EDGE('',*,*,#25880,.T.) ;
#34766 = ORIENTED_EDGE('',*,*,#25881,.T.) ;
#34767 = ORIENTED_EDGE('',*,*,#25877,.F.) ;
#34768 = ORIENTED_EDGE('',*,*,#25429,.T.) ;
#34769 = ORIENTED_EDGE('',*,*,#25882,.T.) ;
#34770 = ORIENTED_EDGE('',*,*,#25883,.T.) ;
#34771 = ORIENTED_EDGE('',*,*,#25880,.F.) ;
#34772 = ORIENTED_EDGE('',*,*,#25428,.T.) ;
#34773 = ORIENTED_EDGE('',*,*,#25884,.T.) ;
#34774 = ORIENTED_EDGE('',*,*,#25885,.T.) ;
#34775 = ORIENTED_EDGE('',*,*,#25882,.F.) ;
#34776 = ORIENTED_EDGE('',*,*,#25427,.T.) ;
#34777 = ORIENTED_EDGE('',*,*,#25886,.T.) ;
#34778 = ORIENTED_EDGE('',*,*,#25887,.T.) ;
#34779 = ORIENTED_EDGE('',*,*,#25884,.F.) ;
#34780 = ORIENTED_EDGE('',*,*,#25426,.T.) ;
#34781 = ORIENTED_EDGE('',*,*,#25879,.F.) ;
#34782 = ORIENTED_EDGE('',*,*,#25888,.T.) ;
#34783 = ORIENTED_EDGE('',*,*,#25875,.F.) ;
#34784 = ORIENTED_EDGE('',*,*,#25889,.T.) ;
#34785 = ORIENTED_EDGE('',*,*,#25890,.T.) ;
#34786 = ORIENTED_EDGE('',*,*,#25891,.T.) ;
#34787 = ORIENTED_EDGE('',*,*,#25425,.T.) ;
#34788 = ORIENTED_EDGE('',*,*,#25889,.F.) ;
#34789 = ORIENTED_EDGE('',*,*,#25424,.T.) ;
#34790 = ORIENTED_EDGE('',*,*,#25892,.T.) ;
#34791 = ORIENTED_EDGE('',*,*,#25893,.F.) ;
#34792 = ORIENTED_EDGE('',*,*,#25891,.F.) ;
#34793 = ORIENTED_EDGE('',*,*,#25894,.T.) ;
#34794 = ORIENTED_EDGE('',*,*,#25886,.F.) ;
#34795 = ORIENTED_EDGE('',*,*,#25876,.F.) ;
#34796 = ORIENTED_EDGE('',*,*,#25895,.F.) ;
#34797 = ORIENTED_EDGE('',*,*,#25896,.F.) ;
#34798 = ORIENTED_EDGE('',*,*,#25897,.F.) ;
#34799 = ORIENTED_EDGE('',*,*,#25888,.F.) ;
#34800 = ORIENTED_EDGE('',*,*,#25898,.T.) ;
#34801 = ORIENTED_EDGE('',*,*,#25899,.T.) ;
#34802 = ORIENTED_EDGE('',*,*,#25895,.T.) ;
#34803 = ORIENTED_EDGE('',*,*,#25878,.F.) ;
#34804 = ORIENTED_EDGE('',*,*,#25900,.F.) ;
#34805 = ORIENTED_EDGE('',*,*,#25901,.F.) ;
#34806 = ORIENTED_EDGE('',*,*,#25898,.F.) ;
#34807 = ORIENTED_EDGE('',*,*,#25881,.F.) ;
#34808 = ORIENTED_EDGE('',*,*,#25902,.T.) ;
#34809 = ORIENTED_EDGE('',*,*,#25903,.T.) ;
#34810 = ORIENTED_EDGE('',*,*,#25900,.T.) ;
#34811 = ORIENTED_EDGE('',*,*,#25883,.F.) ;
#34812 = ORIENTED_EDGE('',*,*,#25904,.F.) ;
#34813 = ORIENTED_EDGE('',*,*,#25905,.F.) ;
#34814 = ORIENTED_EDGE('',*,*,#25902,.F.) ;
#34815 = ORIENTED_EDGE('',*,*,#25885,.F.) ;
#34816 = ORIENTED_EDGE('',*,*,#25906,.T.) ;
#34817 = ORIENTED_EDGE('',*,*,#25907,.T.) ;
#34818 = ORIENTED_EDGE('',*,*,#25904,.T.) ;
#34819 = ORIENTED_EDGE('',*,*,#25887,.F.) ;
#34820 = ORIENTED_EDGE('',*,*,#25908,.F.) ;
#34821 = ORIENTED_EDGE('',*,*,#25909,.F.) ;
#34822 = ORIENTED_EDGE('',*,*,#25906,.F.) ;
#34823 = ORIENTED_EDGE('',*,*,#25894,.F.) ;
#34824 = ORIENTED_EDGE('',*,*,#25910,.T.) ;
#34825 = ORIENTED_EDGE('',*,*,#25911,.T.) ;
#34826 = ORIENTED_EDGE('',*,*,#25908,.T.) ;
#34827 = ORIENTED_EDGE('',*,*,#25890,.F.) ;
#34828 = ORIENTED_EDGE('',*,*,#25912,.F.) ;
#34829 = ORIENTED_EDGE('',*,*,#25913,.F.) ;
#34830 = ORIENTED_EDGE('',*,*,#25910,.F.) ;
#34831 = ORIENTED_EDGE('',*,*,#25668,.F.) ;
#34832 = ORIENTED_EDGE('',*,*,#25416,.T.) ;
#34833 = ORIENTED_EDGE('',*,*,#25914,.T.) ;
#34834 = ORIENTED_EDGE('',*,*,#25682,.T.) ;
#34835 = ORIENTED_EDGE('',*,*,#25915,.T.) ;
#34836 = ORIENTED_EDGE('',*,*,#25916,.T.) ;
#34837 = ORIENTED_EDGE('',*,*,#25917,.T.) ;
#34838 = ORIENTED_EDGE('',*,*,#25415,.T.) ;
#34839 = ORIENTED_EDGE('',*,*,#25915,.F.) ;
#34840 = ORIENTED_EDGE('',*,*,#25414,.T.) ;
#34841 = ORIENTED_EDGE('',*,*,#25918,.T.) ;
#34842 = ORIENTED_EDGE('',*,*,#25919,.F.) ;
#34843 = ORIENTED_EDGE('',*,*,#25917,.F.) ;
#34844 = ORIENTED_EDGE('',*,*,#25680,.T.) ;
#34845 = ORIENTED_EDGE('',*,*,#25914,.F.) ;
#34846 = ORIENTED_EDGE('',*,*,#25916,.F.) ;
#34847 = ORIENTED_EDGE('',*,*,#25920,.F.) ;
#34848 = ORIENTED_EDGE('',*,*,#25677,.F.) ;
#34849 = ORIENTED_EDGE('',*,*,#25681,.F.) ;
#34850 = ORIENTED_EDGE('',*,*,#25649,.F.) ;
#34851 = ORIENTED_EDGE('',*,*,#25406,.T.) ;
#34852 = ORIENTED_EDGE('',*,*,#25661,.F.) ;
#34853 = ORIENTED_EDGE('',*,*,#25921,.T.) ;
#34854 = ORIENTED_EDGE('',*,*,#25675,.F.) ;
#34855 = ORIENTED_EDGE('',*,*,#25922,.T.) ;
#34856 = ORIENTED_EDGE('',*,*,#25923,.T.) ;
#34857 = ORIENTED_EDGE('',*,*,#25408,.T.) ;
#34858 = ORIENTED_EDGE('',*,*,#25650,.F.) ;
#34859 = ORIENTED_EDGE('',*,*,#25921,.F.) ;
#34860 = ORIENTED_EDGE('',*,*,#25663,.F.) ;
#34861 = ORIENTED_EDGE('',*,*,#25659,.F.) ;
#34862 = ORIENTED_EDGE('',*,*,#25684,.F.) ;
#34863 = ORIENTED_EDGE('',*,*,#25924,.T.) ;
#34864 = ORIENTED_EDGE('',*,*,#25925,.T.) ;
#34865 = ORIENTED_EDGE('',*,*,#25394,.T.) ;
#34866 = ORIENTED_EDGE('',*,*,#25926,.T.) ;
#34867 = ORIENTED_EDGE('',*,*,#25395,.T.) ;
#34868 = ORIENTED_EDGE('',*,*,#25925,.F.) ;
#34869 = ORIENTED_EDGE('',*,*,#25927,.T.) ;
#34870 = ORIENTED_EDGE('',*,*,#25928,.T.) ;
#34871 = ORIENTED_EDGE('',*,*,#25396,.T.) ;
#34872 = ORIENTED_EDGE('',*,*,#25926,.F.) ;
#34873 = ORIENTED_EDGE('',*,*,#25929,.T.) ;
#34874 = ORIENTED_EDGE('',*,*,#25930,.T.) ;
#34875 = ORIENTED_EDGE('',*,*,#25397,.T.) ;
#34876 = ORIENTED_EDGE('',*,*,#25928,.F.) ;
#34877 = ORIENTED_EDGE('',*,*,#25931,.T.) ;
#34878 = ORIENTED_EDGE('',*,*,#25932,.T.) ;
#34879 = ORIENTED_EDGE('',*,*,#25398,.T.) ;
#34880 = ORIENTED_EDGE('',*,*,#25930,.F.) ;
#34881 = ORIENTED_EDGE('',*,*,#25933,.T.) ;
#34882 = ORIENTED_EDGE('',*,*,#25934,.T.) ;
#34883 = ORIENTED_EDGE('',*,*,#25399,.T.) ;
#34884 = ORIENTED_EDGE('',*,*,#25932,.F.) ;
#34885 = ORIENTED_EDGE('',*,*,#25935,.T.) ;
#34886 = ORIENTED_EDGE('',*,*,#25936,.T.) ;
#34887 = ORIENTED_EDGE('',*,*,#25400,.T.) ;
#34888 = ORIENTED_EDGE('',*,*,#25934,.F.) ;
#34889 = ORIENTED_EDGE('',*,*,#25937,.T.) ;
#34890 = ORIENTED_EDGE('',*,*,#25938,.T.) ;
#34891 = ORIENTED_EDGE('',*,*,#25401,.T.) ;
#34892 = ORIENTED_EDGE('',*,*,#25936,.F.) ;
#34893 = ORIENTED_EDGE('',*,*,#25939,.T.) ;
#34894 = ORIENTED_EDGE('',*,*,#25700,.F.) ;
#34895 = ORIENTED_EDGE('',*,*,#25402,.T.) ;
#34896 = ORIENTED_EDGE('',*,*,#25938,.F.) ;
#34897 = ORIENTED_EDGE('',*,*,#25940,.T.) ;
#34898 = ORIENTED_EDGE('',*,*,#25698,.F.) ;
#34899 = ORIENTED_EDGE('',*,*,#25940,.F.) ;
#34900 = ORIENTED_EDGE('',*,*,#25941,.F.) ;
#34901 = ORIENTED_EDGE('',*,*,#25942,.F.) ;
#34902 = ORIENTED_EDGE('',*,*,#25939,.F.) ;
#34903 = ORIENTED_EDGE('',*,*,#25943,.T.) ;
#34904 = ORIENTED_EDGE('',*,*,#25944,.T.) ;
#34905 = ORIENTED_EDGE('',*,*,#25941,.T.) ;
#34906 = ORIENTED_EDGE('',*,*,#25937,.F.) ;
#34907 = ORIENTED_EDGE('',*,*,#25945,.F.) ;
#34908 = ORIENTED_EDGE('',*,*,#25946,.F.) ;
#34909 = ORIENTED_EDGE('',*,*,#25943,.F.) ;
#34910 = ORIENTED_EDGE('',*,*,#25935,.F.) ;
#34911 = ORIENTED_EDGE('',*,*,#25947,.T.) ;
#34912 = ORIENTED_EDGE('',*,*,#25948,.T.) ;
#34913 = ORIENTED_EDGE('',*,*,#25945,.T.) ;
#34914 = ORIENTED_EDGE('',*,*,#25933,.F.) ;
#34915 = ORIENTED_EDGE('',*,*,#25949,.F.) ;
#34916 = ORIENTED_EDGE('',*,*,#25950,.F.) ;
#34917 = ORIENTED_EDGE('',*,*,#25947,.F.) ;
#34918 = ORIENTED_EDGE('',*,*,#25931,.F.) ;
#34919 = ORIENTED_EDGE('',*,*,#25951,.T.) ;
#34920 = ORIENTED_EDGE('',*,*,#25952,.T.) ;
#34921 = ORIENTED_EDGE('',*,*,#25949,.T.) ;
#34922 = ORIENTED_EDGE('',*,*,#25929,.F.) ;
#34923 = ORIENTED_EDGE('',*,*,#25953,.F.) ;
#34924 = ORIENTED_EDGE('',*,*,#25954,.F.) ;
#34925 = ORIENTED_EDGE('',*,*,#25951,.F.) ;
#34926 = ORIENTED_EDGE('',*,*,#25927,.F.) ;
#34927 = ORIENTED_EDGE('',*,*,#25955,.T.) ;
#34928 = ORIENTED_EDGE('',*,*,#25956,.T.) ;
#34929 = ORIENTED_EDGE('',*,*,#25953,.T.) ;
#34930 = ORIENTED_EDGE('',*,*,#25687,.F.) ;
#34931 = ORIENTED_EDGE('',*,*,#25957,.F.) ;
#34932 = ORIENTED_EDGE('',*,*,#25955,.F.) ;
#34933 = ORIENTED_EDGE('',*,*,#25924,.F.) ;
#34934 = ORIENTED_EDGE('',*,*,#25646,.T.) ;
#34935 = ORIENTED_EDGE('',*,*,#25958,.T.) ;
#34936 = ORIENTED_EDGE('',*,*,#25922,.F.) ;
#34937 = ORIENTED_EDGE('',*,*,#25676,.T.) ;
#34938 = ORIENTED_EDGE('',*,*,#25959,.F.) ;
#34939 = ORIENTED_EDGE('',*,*,#25960,.T.) ;
#34940 = ORIENTED_EDGE('',*,*,#25961,.T.) ;
#34941 = ORIENTED_EDGE('',*,*,#25412,.T.) ;
#34942 = ORIENTED_EDGE('',*,*,#25962,.F.) ;
#34943 = ORIENTED_EDGE('',*,*,#25963,.F.) ;
#34944 = ORIENTED_EDGE('',*,*,#25964,.F.) ;
#34945 = ORIENTED_EDGE('',*,*,#25965,.F.) ;
#34946 = ORIENTED_EDGE('',*,*,#25166,.T.) ;
#34947 = ORIENTED_EDGE('',*,*,#25678,.F.) ;
#34948 = ORIENTED_EDGE('',*,*,#25966,.F.) ;
#34949 = ORIENTED_EDGE('',*,*,#25967,.F.) ;
#34950 = ORIENTED_EDGE('',*,*,#25919,.T.) ;
#34951 = ORIENTED_EDGE('',*,*,#25968,.T.) ;
#34952 = ORIENTED_EDGE('',*,*,#25966,.T.) ;
#34953 = ORIENTED_EDGE('',*,*,#25920,.T.) ;
#34954 = ORIENTED_EDGE('',*,*,#25170,.T.) ;
#34955 = ORIENTED_EDGE('',*,*,#25969,.F.) ;
#34956 = ORIENTED_EDGE('',*,*,#25970,.F.) ;
#34957 = ORIENTED_EDGE('',*,*,#25971,.F.) ;
#34958 = ORIENTED_EDGE('',*,*,#25168,.T.) ;
#34959 = ORIENTED_EDGE('',*,*,#25972,.F.) ;
#34960 = ORIENTED_EDGE('',*,*,#25973,.F.) ;
#34961 = ORIENTED_EDGE('',*,*,#25974,.F.) ;
#34962 = ORIENTED_EDGE('',*,*,#25972,.T.) ;
#34963 = ORIENTED_EDGE('',*,*,#25167,.T.) ;
#34964 = ORIENTED_EDGE('',*,*,#25967,.T.) ;
#34965 = ORIENTED_EDGE('',*,*,#25975,.T.) ;
#34966 = ORIENTED_EDGE('',*,*,#25973,.T.) ;
#34967 = ORIENTED_EDGE('',*,*,#25976,.T.) ;
#34968 = ORIENTED_EDGE('',*,*,#25960,.F.) ;
#34969 = ORIENTED_EDGE('',*,*,#25965,.T.) ;
#34970 = ORIENTED_EDGE('',*,*,#25969,.T.) ;
#34971 = ORIENTED_EDGE('',*,*,#25169,.T.) ;
#34972 = ORIENTED_EDGE('',*,*,#25974,.T.) ;
#34973 = ORIENTED_EDGE('',*,*,#25964,.T.) ;
#34974 = ORIENTED_EDGE('',*,*,#25977,.F.) ;
#34975 = ORIENTED_EDGE('',*,*,#25978,.F.) ;
#34976 = ORIENTED_EDGE('',*,*,#25410,.T.) ;
#34977 = ORIENTED_EDGE('',*,*,#25979,.F.) ;
#34978 = ORIENTED_EDGE('',*,*,#25411,.T.) ;
#34979 = ORIENTED_EDGE('',*,*,#25978,.T.) ;
#34980 = ORIENTED_EDGE('',*,*,#25962,.T.) ;
#34981 = ORIENTED_EDGE('',*,*,#25959,.T.) ;
#34982 = ORIENTED_EDGE('',*,*,#25923,.F.) ;
#34983 = ORIENTED_EDGE('',*,*,#25980,.T.) ;
#34984 = ORIENTED_EDGE('',*,*,#25979,.T.) ;
#34985 = ORIENTED_EDGE('',*,*,#25409,.T.) ;
#34986 = ORIENTED_EDGE('',*,*,#25970,.T.) ;
#34987 = ORIENTED_EDGE('',*,*,#25963,.T.) ;
#34988 = ORIENTED_EDGE('',*,*,#25977,.T.) ;
#34989 = ORIENTED_EDGE('',*,*,#25981,.T.) ;
#34990 = ORIENTED_EDGE('',*,*,#25645,.F.) ;
#34991 = ORIENTED_EDGE('',*,*,#25171,.T.) ;
#34992 = ORIENTED_EDGE('',*,*,#25971,.T.) ;
#34993 = ORIENTED_EDGE('',*,*,#25982,.T.) ;
#34994 = ORIENTED_EDGE('',*,*,#25976,.F.) ;
#34995 = ORIENTED_EDGE('',*,*,#25975,.F.) ;
#34996 = ORIENTED_EDGE('',*,*,#25968,.F.) ;
#34997 = ORIENTED_EDGE('',*,*,#25983,.F.) ;
#34998 = ORIENTED_EDGE('',*,*,#25961,.F.) ;
#34999 = ORIENTED_EDGE('',*,*,#25983,.T.) ;
#35000 = ORIENTED_EDGE('',*,*,#25918,.F.) ;
#35001 = ORIENTED_EDGE('',*,*,#25413,.T.) ;
#35002 = ORIENTED_EDGE('',*,*,#25984,.T.) ;
#35003 = ORIENTED_EDGE('',*,*,#25434,.T.) ;
#35004 = ORIENTED_EDGE('',*,*,#25985,.T.) ;
#35005 = ORIENTED_EDGE('',*,*,#25986,.F.) ;
#35006 = ORIENTED_EDGE('',*,*,#25987,.F.) ;
#35007 = ORIENTED_EDGE('',*,*,#25988,.T.) ;
#35008 = ORIENTED_EDGE('',*,*,#25989,.T.) ;
#35009 = ORIENTED_EDGE('',*,*,#25436,.T.) ;
#35010 = ORIENTED_EDGE('',*,*,#25990,.F.) ;
#35011 = ORIENTED_EDGE('',*,*,#25991,.F.) ;
#35012 = ORIENTED_EDGE('',*,*,#25992,.F.) ;
#35013 = ORIENTED_EDGE('',*,*,#25993,.F.) ;
#35014 = ORIENTED_EDGE('',*,*,#25861,.F.) ;
#35015 = ORIENTED_EDGE('',*,*,#25994,.F.) ;
#35016 = ORIENTED_EDGE('',*,*,#25121,.T.) ;
#35017 = ORIENTED_EDGE('',*,*,#25995,.F.) ;
#35018 = ORIENTED_EDGE('',*,*,#25123,.T.) ;
#35019 = ORIENTED_EDGE('',*,*,#25996,.F.) ;
#35020 = ORIENTED_EDGE('',*,*,#25865,.F.) ;
#35021 = ORIENTED_EDGE('',*,*,#25997,.F.) ;
#35022 = ORIENTED_EDGE('',*,*,#25996,.T.) ;
#35023 = ORIENTED_EDGE('',*,*,#25122,.T.) ;
#35024 = ORIENTED_EDGE('',*,*,#25994,.T.) ;
#35025 = ORIENTED_EDGE('',*,*,#25863,.T.) ;
#35026 = ORIENTED_EDGE('',*,*,#25998,.F.) ;
#35027 = ORIENTED_EDGE('',*,*,#25999,.F.) ;
#35028 = ORIENTED_EDGE('',*,*,#25857,.F.) ;
#35029 = ORIENTED_EDGE('',*,*,#26000,.F.) ;
#35030 = ORIENTED_EDGE('',*,*,#26001,.F.) ;
#35031 = ORIENTED_EDGE('',*,*,#25869,.F.) ;
#35032 = ORIENTED_EDGE('',*,*,#26001,.T.) ;
#35033 = ORIENTED_EDGE('',*,*,#25124,.T.) ;
#35034 = ORIENTED_EDGE('',*,*,#25997,.T.) ;
#35035 = ORIENTED_EDGE('',*,*,#25867,.T.) ;
#35036 = ORIENTED_EDGE('',*,*,#25118,.T.) ;
#35037 = ORIENTED_EDGE('',*,*,#26002,.F.) ;
#35038 = ORIENTED_EDGE('',*,*,#26003,.F.) ;
#35039 = ORIENTED_EDGE('',*,*,#26004,.F.) ;
#35040 = ORIENTED_EDGE('',*,*,#25126,.T.) ;
#35041 = ORIENTED_EDGE('',*,*,#26005,.F.) ;
#35042 = ORIENTED_EDGE('',*,*,#26006,.F.) ;
#35043 = ORIENTED_EDGE('',*,*,#26007,.F.) ;
#35044 = ORIENTED_EDGE('',*,*,#26005,.T.) ;
#35045 = ORIENTED_EDGE('',*,*,#25125,.T.) ;
#35046 = ORIENTED_EDGE('',*,*,#26000,.T.) ;
#35047 = ORIENTED_EDGE('',*,*,#25871,.T.) ;
#35048 = ORIENTED_EDGE('',*,*,#25851,.T.) ;
#35049 = ORIENTED_EDGE('',*,*,#26008,.T.) ;
#35050 = ORIENTED_EDGE('',*,*,#26006,.T.) ;
#35051 = ORIENTED_EDGE('',*,*,#25870,.T.) ;
#35052 = ORIENTED_EDGE('',*,*,#25116,.T.) ;
#35053 = ORIENTED_EDGE('',*,*,#26009,.F.) ;
#35054 = ORIENTED_EDGE('',*,*,#26010,.F.) ;
#35055 = ORIENTED_EDGE('',*,*,#26011,.F.) ;
#35056 = ORIENTED_EDGE('',*,*,#25114,.T.) ;
#35057 = ORIENTED_EDGE('',*,*,#26012,.F.) ;
#35058 = ORIENTED_EDGE('',*,*,#26013,.F.) ;
#35059 = ORIENTED_EDGE('',*,*,#26014,.F.) ;
#35060 = ORIENTED_EDGE('',*,*,#26012,.T.) ;
#35061 = ORIENTED_EDGE('',*,*,#25127,.T.) ;
#35062 = ORIENTED_EDGE('',*,*,#26007,.T.) ;
#35063 = ORIENTED_EDGE('',*,*,#26015,.T.) ;
#35064 = ORIENTED_EDGE('',*,*,#26013,.T.) ;
#35065 = ORIENTED_EDGE('',*,*,#26016,.T.) ;
#35066 = ORIENTED_EDGE('',*,*,#25988,.F.) ;
#35067 = ORIENTED_EDGE('',*,*,#25993,.T.) ;
#35068 = ORIENTED_EDGE('',*,*,#26009,.T.) ;
#35069 = ORIENTED_EDGE('',*,*,#25115,.T.) ;
#35070 = ORIENTED_EDGE('',*,*,#26014,.T.) ;
#35071 = ORIENTED_EDGE('',*,*,#25992,.T.) ;
#35072 = ORIENTED_EDGE('',*,*,#25986,.T.) ;
#35073 = ORIENTED_EDGE('',*,*,#26017,.T.) ;
#35074 = ORIENTED_EDGE('',*,*,#26010,.T.) ;
#35075 = ORIENTED_EDGE('',*,*,#25991,.T.) ;
#35076 = ORIENTED_EDGE('',*,*,#26002,.T.) ;
#35077 = ORIENTED_EDGE('',*,*,#25117,.T.) ;
#35078 = ORIENTED_EDGE('',*,*,#26011,.T.) ;
#35079 = ORIENTED_EDGE('',*,*,#26018,.T.) ;
#35080 = ORIENTED_EDGE('',*,*,#26003,.T.) ;
#35081 = ORIENTED_EDGE('',*,*,#26019,.T.) ;
#35082 = ORIENTED_EDGE('',*,*,#25831,.F.) ;
#35083 = ORIENTED_EDGE('',*,*,#25855,.T.) ;
#35084 = ORIENTED_EDGE('',*,*,#25999,.T.) ;
#35085 = ORIENTED_EDGE('',*,*,#25119,.T.) ;
#35086 = ORIENTED_EDGE('',*,*,#26004,.T.) ;
#35087 = ORIENTED_EDGE('',*,*,#25854,.T.) ;
#35088 = ORIENTED_EDGE('',*,*,#25995,.T.) ;
#35089 = ORIENTED_EDGE('',*,*,#25120,.T.) ;
#35090 = ORIENTED_EDGE('',*,*,#25998,.T.) ;
#35091 = ORIENTED_EDGE('',*,*,#25859,.T.) ;
#35092 = ORIENTED_EDGE('',*,*,#25435,.T.) ;
#35093 = ORIENTED_EDGE('',*,*,#25984,.F.) ;
#35094 = ORIENTED_EDGE('',*,*,#25990,.T.) ;
#35095 = ORIENTED_EDGE('',*,*,#25987,.T.) ;
#35096 = ORIENTED_EDGE('',*,*,#26016,.F.) ;
#35097 = ORIENTED_EDGE('',*,*,#26015,.F.) ;
#35098 = ORIENTED_EDGE('',*,*,#26008,.F.) ;
#35099 = ORIENTED_EDGE('',*,*,#26020,.F.) ;
#35100 = ORIENTED_EDGE('',*,*,#25989,.F.) ;
#35101 = ORIENTED_EDGE('',*,*,#26020,.T.) ;
#35102 = ORIENTED_EDGE('',*,*,#25850,.F.) ;
#35103 = ORIENTED_EDGE('',*,*,#25437,.T.) ;
#35104 = ORIENTED_EDGE('',*,*,#26021,.T.) ;
#35105 = ORIENTED_EDGE('',*,*,#25420,.T.) ;
#35106 = ORIENTED_EDGE('',*,*,#26022,.T.) ;
#35107 = ORIENTED_EDGE('',*,*,#26023,.F.) ;
#35108 = ORIENTED_EDGE('',*,*,#26024,.F.) ;
#35109 = ORIENTED_EDGE('',*,*,#26025,.T.) ;
#35110 = ORIENTED_EDGE('',*,*,#26026,.T.) ;
#35111 = ORIENTED_EDGE('',*,*,#25422,.T.) ;
#35112 = ORIENTED_EDGE('',*,*,#26027,.F.) ;
#35113 = ORIENTED_EDGE('',*,*,#26028,.F.) ;
#35114 = ORIENTED_EDGE('',*,*,#26029,.F.) ;
#35115 = ORIENTED_EDGE('',*,*,#26030,.F.) ;
#35116 = ORIENTED_EDGE('',*,*,#25235,.T.) ;
#35117 = ORIENTED_EDGE('',*,*,#26031,.F.) ;
#35118 = ORIENTED_EDGE('',*,*,#25903,.F.) ;
#35119 = ORIENTED_EDGE('',*,*,#26032,.F.) ;
#35120 = ORIENTED_EDGE('',*,*,#25899,.F.) ;
#35121 = ORIENTED_EDGE('',*,*,#26033,.F.) ;
#35122 = ORIENTED_EDGE('',*,*,#26034,.F.) ;
#35123 = ORIENTED_EDGE('',*,*,#26031,.T.) ;
#35124 = ORIENTED_EDGE('',*,*,#25234,.T.) ;
#35125 = ORIENTED_EDGE('',*,*,#26033,.T.) ;
#35126 = ORIENTED_EDGE('',*,*,#25901,.T.) ;
#35127 = ORIENTED_EDGE('',*,*,#25237,.T.) ;
#35128 = ORIENTED_EDGE('',*,*,#26035,.F.) ;
#35129 = ORIENTED_EDGE('',*,*,#25907,.F.) ;
#35130 = ORIENTED_EDGE('',*,*,#26036,.F.) ;
#35131 = ORIENTED_EDGE('',*,*,#26035,.T.) ;
#35132 = ORIENTED_EDGE('',*,*,#25236,.T.) ;
#35133 = ORIENTED_EDGE('',*,*,#26032,.T.) ;
#35134 = ORIENTED_EDGE('',*,*,#25905,.T.) ;
#35135 = ORIENTED_EDGE('',*,*,#25232,.T.) ;
#35136 = ORIENTED_EDGE('',*,*,#26037,.F.) ;
#35137 = ORIENTED_EDGE('',*,*,#26038,.F.) ;
#35138 = ORIENTED_EDGE('',*,*,#26039,.F.) ;
#35139 = ORIENTED_EDGE('',*,*,#26040,.F.) ;
#35140 = ORIENTED_EDGE('',*,*,#26041,.F.) ;
#35141 = ORIENTED_EDGE('',*,*,#25911,.F.) ;
#35142 = ORIENTED_EDGE('',*,*,#26041,.T.) ;
#35143 = ORIENTED_EDGE('',*,*,#25238,.T.) ;
#35144 = ORIENTED_EDGE('',*,*,#26036,.T.) ;
#35145 = ORIENTED_EDGE('',*,*,#25909,.T.) ;
#35146 = ORIENTED_EDGE('',*,*,#25230,.T.) ;
#35147 = ORIENTED_EDGE('',*,*,#26042,.F.) ;
#35148 = ORIENTED_EDGE('',*,*,#26043,.F.) ;
#35149 = ORIENTED_EDGE('',*,*,#26044,.F.) ;
#35150 = ORIENTED_EDGE('',*,*,#25240,.T.) ;
#35151 = ORIENTED_EDGE('',*,*,#26045,.F.) ;
#35152 = ORIENTED_EDGE('',*,*,#26046,.F.) ;
#35153 = ORIENTED_EDGE('',*,*,#26047,.F.) ;
#35154 = ORIENTED_EDGE('',*,*,#26045,.T.) ;
#35155 = ORIENTED_EDGE('',*,*,#25239,.T.) ;
#35156 = ORIENTED_EDGE('',*,*,#26040,.T.) ;
#35157 = ORIENTED_EDGE('',*,*,#25913,.T.) ;
#35158 = ORIENTED_EDGE('',*,*,#25893,.T.) ;
#35159 = ORIENTED_EDGE('',*,*,#26048,.T.) ;
#35160 = ORIENTED_EDGE('',*,*,#26046,.T.) ;
#35161 = ORIENTED_EDGE('',*,*,#25912,.T.) ;
#35162 = ORIENTED_EDGE('',*,*,#25228,.T.) ;
#35163 = ORIENTED_EDGE('',*,*,#26049,.F.) ;
#35164 = ORIENTED_EDGE('',*,*,#26050,.F.) ;
#35165 = ORIENTED_EDGE('',*,*,#26051,.F.) ;
#35166 = ORIENTED_EDGE('',*,*,#26049,.T.) ;
#35167 = ORIENTED_EDGE('',*,*,#25241,.T.) ;
#35168 = ORIENTED_EDGE('',*,*,#26047,.T.) ;
#35169 = ORIENTED_EDGE('',*,*,#26052,.T.) ;
#35170 = ORIENTED_EDGE('',*,*,#26050,.T.) ;
#35171 = ORIENTED_EDGE('',*,*,#26053,.T.) ;
#35172 = ORIENTED_EDGE('',*,*,#26025,.F.) ;
#35173 = ORIENTED_EDGE('',*,*,#26030,.T.) ;
#35174 = ORIENTED_EDGE('',*,*,#26042,.T.) ;
#35175 = ORIENTED_EDGE('',*,*,#25229,.T.) ;
#35176 = ORIENTED_EDGE('',*,*,#26051,.T.) ;
#35177 = ORIENTED_EDGE('',*,*,#26029,.T.) ;
#35178 = ORIENTED_EDGE('',*,*,#26023,.T.) ;
#35179 = ORIENTED_EDGE('',*,*,#26054,.T.) ;
#35180 = ORIENTED_EDGE('',*,*,#26043,.T.) ;
#35181 = ORIENTED_EDGE('',*,*,#26028,.T.) ;
#35182 = ORIENTED_EDGE('',*,*,#26037,.T.) ;
#35183 = ORIENTED_EDGE('',*,*,#25231,.T.) ;
#35184 = ORIENTED_EDGE('',*,*,#26044,.T.) ;
#35185 = ORIENTED_EDGE('',*,*,#26055,.T.) ;
#35186 = ORIENTED_EDGE('',*,*,#26038,.T.) ;
#35187 = ORIENTED_EDGE('',*,*,#26056,.T.) ;
#35188 = ORIENTED_EDGE('',*,*,#25873,.F.) ;
#35189 = ORIENTED_EDGE('',*,*,#25897,.T.) ;
#35190 = ORIENTED_EDGE('',*,*,#26034,.T.) ;
#35191 = ORIENTED_EDGE('',*,*,#25233,.T.) ;
#35192 = ORIENTED_EDGE('',*,*,#26039,.T.) ;
#35193 = ORIENTED_EDGE('',*,*,#25896,.T.) ;
#35194 = ORIENTED_EDGE('',*,*,#25421,.T.) ;
#35195 = ORIENTED_EDGE('',*,*,#26021,.F.) ;
#35196 = ORIENTED_EDGE('',*,*,#26027,.T.) ;
#35197 = ORIENTED_EDGE('',*,*,#26024,.T.) ;
#35198 = ORIENTED_EDGE('',*,*,#26053,.F.) ;
#35199 = ORIENTED_EDGE('',*,*,#26052,.F.) ;
#35200 = ORIENTED_EDGE('',*,*,#26048,.F.) ;
#35201 = ORIENTED_EDGE('',*,*,#26057,.F.) ;
#35202 = ORIENTED_EDGE('',*,*,#26026,.F.) ;
#35203 = ORIENTED_EDGE('',*,*,#26057,.T.) ;
#35204 = ORIENTED_EDGE('',*,*,#25892,.F.) ;
#35205 = ORIENTED_EDGE('',*,*,#25423,.T.) ;
#35206 = ORIENTED_EDGE('',*,*,#25083,.T.) ;
#35207 = ORIENTED_EDGE('',*,*,#26058,.F.) ;
#35208 = ORIENTED_EDGE('',*,*,#26059,.F.) ;
#35209 = ORIENTED_EDGE('',*,*,#26060,.F.) ;
#35210 = ORIENTED_EDGE('',*,*,#25081,.T.) ;
#35211 = ORIENTED_EDGE('',*,*,#26061,.F.) ;
#35212 = ORIENTED_EDGE('',*,*,#26062,.F.) ;
#35213 = ORIENTED_EDGE('',*,*,#26063,.F.) ;
#35214 = ORIENTED_EDGE('',*,*,#26064,.T.) ;
#35215 = ORIENTED_EDGE('',*,*,#25515,.T.) ;
#35216 = ORIENTED_EDGE('',*,*,#26065,.T.) ;
#35217 = ORIENTED_EDGE('',*,*,#25584,.T.) ;
#35218 = ORIENTED_EDGE('',*,*,#26066,.T.) ;
#35219 = ORIENTED_EDGE('',*,*,#26067,.T.) ;
#35220 = ORIENTED_EDGE('',*,*,#26065,.F.) ;
#35221 = ORIENTED_EDGE('',*,*,#25514,.T.) ;
#35222 = ORIENTED_EDGE('',*,*,#26068,.T.) ;
#35223 = ORIENTED_EDGE('',*,*,#25076,.T.) ;
#35224 = ORIENTED_EDGE('',*,*,#26066,.F.) ;
#35225 = ORIENTED_EDGE('',*,*,#25513,.T.) ;
#35226 = ORIENTED_EDGE('',*,*,#26069,.T.) ;
#35227 = ORIENTED_EDGE('',*,*,#25077,.T.) ;
#35228 = ORIENTED_EDGE('',*,*,#26068,.F.) ;
#35229 = ORIENTED_EDGE('',*,*,#26070,.T.) ;
#35230 = ORIENTED_EDGE('',*,*,#26071,.T.) ;
#35231 = ORIENTED_EDGE('',*,*,#25078,.T.) ;
#35232 = ORIENTED_EDGE('',*,*,#26069,.F.) ;
#35233 = ORIENTED_EDGE('',*,*,#26072,.T.) ;
#35234 = ORIENTED_EDGE('',*,*,#26073,.T.) ;
#35235 = ORIENTED_EDGE('',*,*,#25079,.T.) ;
#35236 = ORIENTED_EDGE('',*,*,#26071,.F.) ;
#35237 = ORIENTED_EDGE('',*,*,#26074,.T.) ;
#35238 = ORIENTED_EDGE('',*,*,#26061,.T.) ;
#35239 = ORIENTED_EDGE('',*,*,#25080,.T.) ;
#35240 = ORIENTED_EDGE('',*,*,#26073,.F.) ;
#35241 = ORIENTED_EDGE('',*,*,#26075,.T.) ;
#35242 = ORIENTED_EDGE('',*,*,#25599,.T.) ;
#35243 = ORIENTED_EDGE('',*,*,#25510,.T.) ;
#35244 = ORIENTED_EDGE('',*,*,#26064,.F.) ;
#35245 = ORIENTED_EDGE('',*,*,#25583,.T.) ;
#35246 = ORIENTED_EDGE('',*,*,#26076,.T.) ;
#35247 = ORIENTED_EDGE('',*,*,#25494,.T.) ;
#35248 = ORIENTED_EDGE('',*,*,#25617,.F.) ;
#35249 = ORIENTED_EDGE('',*,*,#25597,.T.) ;
#35250 = ORIENTED_EDGE('',*,*,#26077,.T.) ;
#35251 = ORIENTED_EDGE('',*,*,#25488,.T.) ;
#35252 = ORIENTED_EDGE('',*,*,#26076,.F.) ;
#35253 = ORIENTED_EDGE('',*,*,#25596,.T.) ;
#35254 = ORIENTED_EDGE('',*,*,#26078,.T.) ;
#35255 = ORIENTED_EDGE('',*,*,#25489,.T.) ;
#35256 = ORIENTED_EDGE('',*,*,#26077,.F.) ;
#35257 = ORIENTED_EDGE('',*,*,#26079,.T.) ;
#35258 = ORIENTED_EDGE('',*,*,#26080,.T.) ;
#35259 = ORIENTED_EDGE('',*,*,#25490,.T.) ;
#35260 = ORIENTED_EDGE('',*,*,#26078,.F.) ;
#35261 = ORIENTED_EDGE('',*,*,#25059,.T.) ;
#35262 = ORIENTED_EDGE('',*,*,#26081,.T.) ;
#35263 = ORIENTED_EDGE('',*,*,#26082,.T.) ;
#35264 = ORIENTED_EDGE('',*,*,#26080,.F.) ;
#35265 = ORIENTED_EDGE('',*,*,#25107,.T.) ;
#35266 = ORIENTED_EDGE('',*,*,#26083,.T.) ;
#35267 = ORIENTED_EDGE('',*,*,#26084,.T.) ;
#35268 = ORIENTED_EDGE('',*,*,#26081,.F.) ;
#35269 = ORIENTED_EDGE('',*,*,#25106,.T.) ;
#35270 = ORIENTED_EDGE('',*,*,#26085,.T.) ;
#35271 = ORIENTED_EDGE('',*,*,#26086,.T.) ;
#35272 = ORIENTED_EDGE('',*,*,#26083,.F.) ;
#35273 = ORIENTED_EDGE('',*,*,#25105,.T.) ;
#35274 = ORIENTED_EDGE('',*,*,#26087,.T.) ;
#35275 = ORIENTED_EDGE('',*,*,#26088,.T.) ;
#35276 = ORIENTED_EDGE('',*,*,#26085,.F.) ;
#35277 = ORIENTED_EDGE('',*,*,#25104,.T.) ;
#35278 = ORIENTED_EDGE('',*,*,#26089,.T.) ;
#35279 = ORIENTED_EDGE('',*,*,#26090,.T.) ;
#35280 = ORIENTED_EDGE('',*,*,#26087,.F.) ;
#35281 = ORIENTED_EDGE('',*,*,#25103,.T.) ;
#35282 = ORIENTED_EDGE('',*,*,#26091,.T.) ;
#35283 = ORIENTED_EDGE('',*,*,#26092,.T.) ;
#35284 = ORIENTED_EDGE('',*,*,#26089,.F.) ;
#35285 = ORIENTED_EDGE('',*,*,#25102,.T.) ;
#35286 = ORIENTED_EDGE('',*,*,#26093,.T.) ;
#35287 = ORIENTED_EDGE('',*,*,#26094,.T.) ;
#35288 = ORIENTED_EDGE('',*,*,#26091,.F.) ;
#35289 = ORIENTED_EDGE('',*,*,#25101,.T.) ;
#35290 = ORIENTED_EDGE('',*,*,#26095,.T.) ;
#35291 = ORIENTED_EDGE('',*,*,#26096,.T.) ;
#35292 = ORIENTED_EDGE('',*,*,#26093,.F.) ;
#35293 = ORIENTED_EDGE('',*,*,#25100,.T.) ;
#35294 = ORIENTED_EDGE('',*,*,#26097,.T.) ;
#35295 = ORIENTED_EDGE('',*,*,#26098,.T.) ;
#35296 = ORIENTED_EDGE('',*,*,#26095,.F.) ;
#35297 = ORIENTED_EDGE('',*,*,#25099,.T.) ;
#35298 = ORIENTED_EDGE('',*,*,#26099,.T.) ;
#35299 = ORIENTED_EDGE('',*,*,#26100,.T.) ;
#35300 = ORIENTED_EDGE('',*,*,#26097,.F.) ;
#35301 = ORIENTED_EDGE('',*,*,#25098,.T.) ;
#35302 = ORIENTED_EDGE('',*,*,#26101,.T.) ;
#35303 = ORIENTED_EDGE('',*,*,#26102,.T.) ;
#35304 = ORIENTED_EDGE('',*,*,#26099,.F.) ;
#35305 = ORIENTED_EDGE('',*,*,#25097,.T.) ;
#35306 = ORIENTED_EDGE('',*,*,#26103,.T.) ;
#35307 = ORIENTED_EDGE('',*,*,#26104,.T.) ;
#35308 = ORIENTED_EDGE('',*,*,#26101,.F.) ;
#35309 = ORIENTED_EDGE('',*,*,#25096,.T.) ;
#35310 = ORIENTED_EDGE('',*,*,#26105,.T.) ;
#35311 = ORIENTED_EDGE('',*,*,#26106,.T.) ;
#35312 = ORIENTED_EDGE('',*,*,#26103,.F.) ;
#35313 = ORIENTED_EDGE('',*,*,#25095,.T.) ;
#35314 = ORIENTED_EDGE('',*,*,#26107,.T.) ;
#35315 = ORIENTED_EDGE('',*,*,#26108,.T.) ;
#35316 = ORIENTED_EDGE('',*,*,#26105,.F.) ;
#35317 = ORIENTED_EDGE('',*,*,#25094,.T.) ;
#35318 = ORIENTED_EDGE('',*,*,#26109,.T.) ;
#35319 = ORIENTED_EDGE('',*,*,#26110,.T.) ;
#35320 = ORIENTED_EDGE('',*,*,#26107,.F.) ;
#35321 = ORIENTED_EDGE('',*,*,#25093,.T.) ;
#35322 = ORIENTED_EDGE('',*,*,#26111,.T.) ;
#35323 = ORIENTED_EDGE('',*,*,#26112,.T.) ;
#35324 = ORIENTED_EDGE('',*,*,#26109,.F.) ;
#35325 = ORIENTED_EDGE('',*,*,#25092,.T.) ;
#35326 = ORIENTED_EDGE('',*,*,#26113,.T.) ;
#35327 = ORIENTED_EDGE('',*,*,#26114,.T.) ;
#35328 = ORIENTED_EDGE('',*,*,#26111,.F.) ;
#35329 = ORIENTED_EDGE('',*,*,#25091,.T.) ;
#35330 = ORIENTED_EDGE('',*,*,#26115,.T.) ;
#35331 = ORIENTED_EDGE('',*,*,#26116,.T.) ;
#35332 = ORIENTED_EDGE('',*,*,#26113,.F.) ;
#35333 = ORIENTED_EDGE('',*,*,#25090,.T.) ;
#35334 = ORIENTED_EDGE('',*,*,#26117,.T.) ;
#35335 = ORIENTED_EDGE('',*,*,#26118,.T.) ;
#35336 = ORIENTED_EDGE('',*,*,#26115,.F.) ;
#35337 = ORIENTED_EDGE('',*,*,#25089,.T.) ;
#35338 = ORIENTED_EDGE('',*,*,#26119,.T.) ;
#35339 = ORIENTED_EDGE('',*,*,#26120,.T.) ;
#35340 = ORIENTED_EDGE('',*,*,#26117,.F.) ;
#35341 = ORIENTED_EDGE('',*,*,#25088,.T.) ;
#35342 = ORIENTED_EDGE('',*,*,#26121,.T.) ;
#35343 = ORIENTED_EDGE('',*,*,#26122,.T.) ;
#35344 = ORIENTED_EDGE('',*,*,#26119,.F.) ;
#35345 = ORIENTED_EDGE('',*,*,#25087,.T.) ;
#35346 = ORIENTED_EDGE('',*,*,#26123,.T.) ;
#35347 = ORIENTED_EDGE('',*,*,#26124,.T.) ;
#35348 = ORIENTED_EDGE('',*,*,#26121,.F.) ;
#35349 = ORIENTED_EDGE('',*,*,#25086,.T.) ;
#35350 = ORIENTED_EDGE('',*,*,#26125,.T.) ;
#35351 = ORIENTED_EDGE('',*,*,#26126,.T.) ;
#35352 = ORIENTED_EDGE('',*,*,#26123,.F.) ;
#35353 = ORIENTED_EDGE('',*,*,#25085,.T.) ;
#35354 = ORIENTED_EDGE('',*,*,#26125,.F.) ;
#35355 = ORIENTED_EDGE('',*,*,#25084,.T.) ;
#35356 = ORIENTED_EDGE('',*,*,#26060,.T.) ;
#35357 = ORIENTED_EDGE('',*,*,#26127,.T.) ;
#35358 = ORIENTED_EDGE('',*,*,#26128,.T.) ;
#35359 = ORIENTED_EDGE('',*,*,#26129,.T.) ;
#35360 = ORIENTED_EDGE('',*,*,#25328,.T.) ;
#35361 = ORIENTED_EDGE('',*,*,#26130,.T.) ;
#35362 = ORIENTED_EDGE('',*,*,#26062,.T.) ;
#35363 = ORIENTED_EDGE('',*,*,#26131,.T.) ;
#35364 = ORIENTED_EDGE('',*,*,#26128,.F.) ;
#35365 = ORIENTED_EDGE('',*,*,#26132,.T.) ;
#35366 = ORIENTED_EDGE('',*,*,#26058,.T.) ;
#35367 = ORIENTED_EDGE('',*,*,#25082,.T.) ;
#35368 = ORIENTED_EDGE('',*,*,#26063,.T.) ;
#35369 = ORIENTED_EDGE('',*,*,#26133,.T.) ;
#35370 = ORIENTED_EDGE('',*,*,#26134,.T.) ;
#35371 = ORIENTED_EDGE('',*,*,#26135,.T.) ;
#35372 = ORIENTED_EDGE('',*,*,#26059,.T.) ;
#35373 = ORIENTED_EDGE('',*,*,#26136,.T.) ;
#35374 = ORIENTED_EDGE('',*,*,#25326,.T.) ;
#35375 = ORIENTED_EDGE('',*,*,#26137,.T.) ;
#35376 = ORIENTED_EDGE('',*,*,#26134,.F.) ;
#35377 = ORIENTED_EDGE('',*,*,#26138,.T.) ;
#35378 = ORIENTED_EDGE('',*,*,#26079,.F.) ;
#35379 = ORIENTED_EDGE('',*,*,#25595,.T.) ;
#35380 = ORIENTED_EDGE('',*,*,#26139,.F.) ;
#35381 = ORIENTED_EDGE('',*,*,#26140,.F.) ;
#35382 = ORIENTED_EDGE('',*,*,#25060,.T.) ;
#35383 = ORIENTED_EDGE('',*,*,#26084,.F.) ;
#35384 = ORIENTED_EDGE('',*,*,#26141,.F.) ;
#35385 = ORIENTED_EDGE('',*,*,#26142,.F.) ;
#35386 = ORIENTED_EDGE('',*,*,#26143,.F.) ;
#35387 = ORIENTED_EDGE('',*,*,#26086,.F.) ;
#35388 = ORIENTED_EDGE('',*,*,#26144,.T.) ;
#35389 = ORIENTED_EDGE('',*,*,#26145,.F.) ;
#35390 = ORIENTED_EDGE('',*,*,#26141,.T.) ;
#35391 = ORIENTED_EDGE('',*,*,#26088,.F.) ;
#35392 = ORIENTED_EDGE('',*,*,#26146,.F.) ;
#35393 = ORIENTED_EDGE('',*,*,#26147,.F.) ;
#35394 = ORIENTED_EDGE('',*,*,#26144,.F.) ;
#35395 = ORIENTED_EDGE('',*,*,#26090,.F.) ;
#35396 = ORIENTED_EDGE('',*,*,#26148,.T.) ;
#35397 = ORIENTED_EDGE('',*,*,#26149,.F.) ;
#35398 = ORIENTED_EDGE('',*,*,#26146,.T.) ;
#35399 = ORIENTED_EDGE('',*,*,#26092,.F.) ;
#35400 = ORIENTED_EDGE('',*,*,#26150,.F.) ;
#35401 = ORIENTED_EDGE('',*,*,#26151,.F.) ;
#35402 = ORIENTED_EDGE('',*,*,#26148,.F.) ;
#35403 = ORIENTED_EDGE('',*,*,#26094,.F.) ;
#35404 = ORIENTED_EDGE('',*,*,#26152,.F.) ;
#35405 = ORIENTED_EDGE('',*,*,#26153,.F.) ;
#35406 = ORIENTED_EDGE('',*,*,#26150,.T.) ;
#35407 = ORIENTED_EDGE('',*,*,#26096,.F.) ;
#35408 = ORIENTED_EDGE('',*,*,#26154,.F.) ;
#35409 = ORIENTED_EDGE('',*,*,#26155,.F.) ;
#35410 = ORIENTED_EDGE('',*,*,#26152,.T.) ;
#35411 = ORIENTED_EDGE('',*,*,#26098,.F.) ;
#35412 = ORIENTED_EDGE('',*,*,#26156,.T.) ;
#35413 = ORIENTED_EDGE('',*,*,#26157,.F.) ;
#35414 = ORIENTED_EDGE('',*,*,#26154,.T.) ;
#35415 = ORIENTED_EDGE('',*,*,#26100,.F.) ;
#35416 = ORIENTED_EDGE('',*,*,#26158,.F.) ;
#35417 = ORIENTED_EDGE('',*,*,#26159,.F.) ;
#35418 = ORIENTED_EDGE('',*,*,#26156,.F.) ;
#35419 = ORIENTED_EDGE('',*,*,#26102,.F.) ;
#35420 = ORIENTED_EDGE('',*,*,#26160,.T.) ;
#35421 = ORIENTED_EDGE('',*,*,#26161,.F.) ;
#35422 = ORIENTED_EDGE('',*,*,#26158,.T.) ;
#35423 = ORIENTED_EDGE('',*,*,#26104,.F.) ;
#35424 = ORIENTED_EDGE('',*,*,#26162,.F.) ;
#35425 = ORIENTED_EDGE('',*,*,#26163,.F.) ;
#35426 = ORIENTED_EDGE('',*,*,#26160,.F.) ;
#35427 = ORIENTED_EDGE('',*,*,#26106,.F.) ;
#35428 = ORIENTED_EDGE('',*,*,#26164,.T.) ;
#35429 = ORIENTED_EDGE('',*,*,#26165,.F.) ;
#35430 = ORIENTED_EDGE('',*,*,#26162,.T.) ;
#35431 = ORIENTED_EDGE('',*,*,#26108,.F.) ;
#35432 = ORIENTED_EDGE('',*,*,#26166,.F.) ;
#35433 = ORIENTED_EDGE('',*,*,#26167,.F.) ;
#35434 = ORIENTED_EDGE('',*,*,#26164,.F.) ;
#35435 = ORIENTED_EDGE('',*,*,#26110,.F.) ;
#35436 = ORIENTED_EDGE('',*,*,#26168,.F.) ;
#35437 = ORIENTED_EDGE('',*,*,#26169,.F.) ;
#35438 = ORIENTED_EDGE('',*,*,#26166,.T.) ;
#35439 = ORIENTED_EDGE('',*,*,#26112,.F.) ;
#35440 = ORIENTED_EDGE('',*,*,#26170,.F.) ;
#35441 = ORIENTED_EDGE('',*,*,#26171,.F.) ;
#35442 = ORIENTED_EDGE('',*,*,#26168,.T.) ;
#35443 = ORIENTED_EDGE('',*,*,#26114,.F.) ;
#35444 = ORIENTED_EDGE('',*,*,#26172,.T.) ;
#35445 = ORIENTED_EDGE('',*,*,#26173,.F.) ;
#35446 = ORIENTED_EDGE('',*,*,#26170,.T.) ;
#35447 = ORIENTED_EDGE('',*,*,#26116,.F.) ;
#35448 = ORIENTED_EDGE('',*,*,#26174,.F.) ;
#35449 = ORIENTED_EDGE('',*,*,#26175,.F.) ;
#35450 = ORIENTED_EDGE('',*,*,#26172,.F.) ;
#35451 = ORIENTED_EDGE('',*,*,#26118,.F.) ;
#35452 = ORIENTED_EDGE('',*,*,#26176,.T.) ;
#35453 = ORIENTED_EDGE('',*,*,#26177,.F.) ;
#35454 = ORIENTED_EDGE('',*,*,#26174,.T.) ;
#35455 = ORIENTED_EDGE('',*,*,#26120,.F.) ;
#35456 = ORIENTED_EDGE('',*,*,#26178,.F.) ;
#35457 = ORIENTED_EDGE('',*,*,#26179,.F.) ;
#35458 = ORIENTED_EDGE('',*,*,#26176,.F.) ;
#35459 = ORIENTED_EDGE('',*,*,#26122,.F.) ;
#35460 = ORIENTED_EDGE('',*,*,#26180,.T.) ;
#35461 = ORIENTED_EDGE('',*,*,#26181,.F.) ;
#35462 = ORIENTED_EDGE('',*,*,#26178,.T.) ;
#35463 = ORIENTED_EDGE('',*,*,#26124,.F.) ;
#35464 = ORIENTED_EDGE('',*,*,#26182,.F.) ;
#35465 = ORIENTED_EDGE('',*,*,#26183,.F.) ;
#35466 = ORIENTED_EDGE('',*,*,#26180,.F.) ;
#35467 = ORIENTED_EDGE('',*,*,#26126,.F.) ;
#35468 = ORIENTED_EDGE('',*,*,#26184,.T.) ;
#35469 = ORIENTED_EDGE('',*,*,#26185,.F.) ;
#35470 = ORIENTED_EDGE('',*,*,#26182,.T.) ;
#35471 = ORIENTED_EDGE('',*,*,#26127,.F.) ;
#35472 = ORIENTED_EDGE('',*,*,#26135,.F.) ;
#35473 = ORIENTED_EDGE('',*,*,#26186,.F.) ;
#35474 = ORIENTED_EDGE('',*,*,#26184,.F.) ;
#35475 = ORIENTED_EDGE('',*,*,#26137,.F.) ;
#35476 = ORIENTED_EDGE('',*,*,#25325,.T.) ;
#35477 = ORIENTED_EDGE('',*,*,#26187,.F.) ;
#35478 = ORIENTED_EDGE('',*,*,#26186,.T.) ;
#35479 = ORIENTED_EDGE('',*,*,#26188,.T.) ;
#35480 = ORIENTED_EDGE('',*,*,#26189,.T.) ;
#35481 = ORIENTED_EDGE('',*,*,#26190,.T.) ;
#35482 = ORIENTED_EDGE('',*,*,#26191,.T.) ;
#35483 = ORIENTED_EDGE('',*,*,#26192,.T.) ;
#35484 = ORIENTED_EDGE('',*,*,#26193,.T.) ;
#35485 = ORIENTED_EDGE('',*,*,#26190,.F.) ;
#35486 = ORIENTED_EDGE('',*,*,#26194,.T.) ;
#35487 = ORIENTED_EDGE('',*,*,#26195,.T.) ;
#35488 = ORIENTED_EDGE('',*,*,#26192,.F.) ;
#35489 = ORIENTED_EDGE('',*,*,#25129,.T.) ;
#35490 = ORIENTED_EDGE('',*,*,#26194,.F.) ;
#35491 = ORIENTED_EDGE('',*,*,#26196,.T.) ;
#35492 = ORIENTED_EDGE('',*,*,#26197,.F.) ;
#35493 = ORIENTED_EDGE('',*,*,#25130,.T.) ;
#35494 = ORIENTED_EDGE('',*,*,#26189,.F.) ;
#35495 = ORIENTED_EDGE('',*,*,#26198,.F.) ;
#35496 = ORIENTED_EDGE('',*,*,#26199,.F.) ;
#35497 = ORIENTED_EDGE('',*,*,#26196,.F.) ;
#35498 = ORIENTED_EDGE('',*,*,#26188,.F.) ;
#35499 = ORIENTED_EDGE('',*,*,#26200,.T.) ;
#35500 = ORIENTED_EDGE('',*,*,#26201,.T.) ;
#35501 = ORIENTED_EDGE('',*,*,#26202,.T.) ;
#35502 = ORIENTED_EDGE('',*,*,#26203,.F.) ;
#35503 = ORIENTED_EDGE('',*,*,#26198,.T.) ;
#35504 = ORIENTED_EDGE('',*,*,#26203,.T.) ;
#35505 = ORIENTED_EDGE('',*,*,#26204,.T.) ;
#35506 = ORIENTED_EDGE('',*,*,#26205,.T.) ;
#35507 = ORIENTED_EDGE('',*,*,#26199,.T.) ;
#35508 = ORIENTED_EDGE('',*,*,#26206,.T.) ;
#35509 = ORIENTED_EDGE('',*,*,#26197,.T.) ;
#35510 = ORIENTED_EDGE('',*,*,#26205,.F.) ;
#35511 = ORIENTED_EDGE('',*,*,#26207,.T.) ;
#35512 = ORIENTED_EDGE('',*,*,#26208,.F.) ;
#35513 = ORIENTED_EDGE('',*,*,#25131,.T.) ;
#35514 = ORIENTED_EDGE('',*,*,#26206,.F.) ;
#35515 = ORIENTED_EDGE('',*,*,#26207,.F.) ;
#35516 = ORIENTED_EDGE('',*,*,#26204,.F.) ;
#35517 = ORIENTED_EDGE('',*,*,#26202,.F.) ;
#35518 = ORIENTED_EDGE('',*,*,#26209,.T.) ;
#35519 = ORIENTED_EDGE('',*,*,#26210,.F.) ;
#35520 = ORIENTED_EDGE('',*,*,#25143,.T.) ;
#35521 = ORIENTED_EDGE('',*,*,#26211,.F.) ;
#35522 = ORIENTED_EDGE('',*,*,#26212,.F.) ;
#35523 = ORIENTED_EDGE('',*,*,#26213,.F.) ;
#35524 = ORIENTED_EDGE('',*,*,#26214,.F.) ;
#35525 = ORIENTED_EDGE('',*,*,#26215,.F.) ;
#35526 = ORIENTED_EDGE('',*,*,#25141,.T.) ;
#35527 = ORIENTED_EDGE('',*,*,#26216,.F.) ;
#35528 = ORIENTED_EDGE('',*,*,#26211,.T.) ;
#35529 = ORIENTED_EDGE('',*,*,#25142,.T.) ;
#35530 = ORIENTED_EDGE('',*,*,#26215,.T.) ;
#35531 = ORIENTED_EDGE('',*,*,#26217,.T.) ;
#35532 = ORIENTED_EDGE('',*,*,#26218,.F.) ;
#35533 = ORIENTED_EDGE('',*,*,#26219,.F.) ;
#35534 = ORIENTED_EDGE('',*,*,#25139,.T.) ;
#35535 = ORIENTED_EDGE('',*,*,#26220,.F.) ;
#35536 = ORIENTED_EDGE('',*,*,#26219,.T.) ;
#35537 = ORIENTED_EDGE('',*,*,#26221,.T.) ;
#35538 = ORIENTED_EDGE('',*,*,#26216,.T.) ;
#35539 = ORIENTED_EDGE('',*,*,#25140,.T.) ;
#35540 = ORIENTED_EDGE('',*,*,#26222,.F.) ;
#35541 = ORIENTED_EDGE('',*,*,#26223,.F.) ;
#35542 = ORIENTED_EDGE('',*,*,#25137,.T.) ;
#35543 = ORIENTED_EDGE('',*,*,#26224,.F.) ;
#35544 = ORIENTED_EDGE('',*,*,#26220,.T.) ;
#35545 = ORIENTED_EDGE('',*,*,#25138,.T.) ;
#35546 = ORIENTED_EDGE('',*,*,#26223,.T.) ;
#35547 = ORIENTED_EDGE('',*,*,#26225,.T.) ;
#35548 = ORIENTED_EDGE('',*,*,#26226,.F.) ;
#35549 = ORIENTED_EDGE('',*,*,#26227,.F.) ;
#35550 = ORIENTED_EDGE('',*,*,#25135,.T.) ;
#35551 = ORIENTED_EDGE('',*,*,#26228,.F.) ;
#35552 = ORIENTED_EDGE('',*,*,#26227,.T.) ;
#35553 = ORIENTED_EDGE('',*,*,#26229,.T.) ;
#35554 = ORIENTED_EDGE('',*,*,#26224,.T.) ;
#35555 = ORIENTED_EDGE('',*,*,#25136,.T.) ;
#35556 = ORIENTED_EDGE('',*,*,#25133,.T.) ;
#35557 = ORIENTED_EDGE('',*,*,#26230,.F.) ;
#35558 = ORIENTED_EDGE('',*,*,#26231,.F.) ;
#35559 = ORIENTED_EDGE('',*,*,#26232,.F.) ;
#35560 = ORIENTED_EDGE('',*,*,#26233,.T.) ;
#35561 = ORIENTED_EDGE('',*,*,#26230,.T.) ;
#35562 = ORIENTED_EDGE('',*,*,#25132,.F.) ;
#35563 = ORIENTED_EDGE('',*,*,#26208,.T.) ;
#35564 = ORIENTED_EDGE('',*,*,#25377,.T.) ;
#35565 = ORIENTED_EDGE('',*,*,#26234,.T.) ;
#35566 = ORIENTED_EDGE('',*,*,#26231,.T.) ;
#35567 = ORIENTED_EDGE('',*,*,#26235,.T.) ;
#35568 = ORIENTED_EDGE('',*,*,#26228,.T.) ;
#35569 = ORIENTED_EDGE('',*,*,#25134,.T.) ;
#35570 = ORIENTED_EDGE('',*,*,#26232,.T.) ;
#35571 = ORIENTED_EDGE('',*,*,#26236,.T.) ;
#35572 = ORIENTED_EDGE('',*,*,#25375,.T.) ;
#35573 = ORIENTED_EDGE('',*,*,#26237,.T.) ;
#35574 = ORIENTED_EDGE('',*,*,#26226,.T.) ;
#35575 = ORIENTED_EDGE('',*,*,#26238,.T.) ;
#35576 = ORIENTED_EDGE('',*,*,#25373,.T.) ;
#35577 = ORIENTED_EDGE('',*,*,#26239,.T.) ;
#35578 = ORIENTED_EDGE('',*,*,#26222,.T.) ;
#35579 = ORIENTED_EDGE('',*,*,#26240,.T.) ;
#35580 = ORIENTED_EDGE('',*,*,#25371,.T.) ;
#35581 = ORIENTED_EDGE('',*,*,#26241,.T.) ;
#35582 = ORIENTED_EDGE('',*,*,#26218,.T.) ;
#35583 = ORIENTED_EDGE('',*,*,#26242,.T.) ;
#35584 = ORIENTED_EDGE('',*,*,#25369,.T.) ;
#35585 = ORIENTED_EDGE('',*,*,#26243,.T.) ;
#35586 = ORIENTED_EDGE('',*,*,#26214,.T.) ;
#35587 = ORIENTED_EDGE('',*,*,#26244,.T.) ;
#35588 = ORIENTED_EDGE('',*,*,#25381,.T.) ;
#35589 = ORIENTED_EDGE('',*,*,#26245,.T.) ;
#35590 = ORIENTED_EDGE('',*,*,#26212,.T.) ;
#35591 = ORIENTED_EDGE('',*,*,#26246,.T.) ;
#35592 = ORIENTED_EDGE('',*,*,#25128,.F.) ;
#35593 = ORIENTED_EDGE('',*,*,#26213,.T.) ;
#35594 = ORIENTED_EDGE('',*,*,#26247,.T.) ;
#35595 = ORIENTED_EDGE('',*,*,#26195,.F.) ;
#35596 = ORIENTED_EDGE('',*,*,#26238,.F.) ;
#35597 = ORIENTED_EDGE('',*,*,#26236,.F.) ;
#35598 = ORIENTED_EDGE('',*,*,#26234,.F.) ;
#35599 = ORIENTED_EDGE('',*,*,#25376,.F.) ;
#35600 = ORIENTED_EDGE('',*,*,#26235,.F.) ;
#35601 = ORIENTED_EDGE('',*,*,#26233,.F.) ;
#35602 = ORIENTED_EDGE('',*,*,#26210,.T.) ;
#35603 = ORIENTED_EDGE('',*,*,#25378,.F.) ;
#35604 = ORIENTED_EDGE('',*,*,#26248,.F.) ;
#35605 = ORIENTED_EDGE('',*,*,#26249,.F.) ;
#35606 = ORIENTED_EDGE('',*,*,#26250,.F.) ;
#35607 = ORIENTED_EDGE('',*,*,#25152,.T.) ;
#35608 = ORIENTED_EDGE('',*,*,#26251,.F.) ;
#35609 = ORIENTED_EDGE('',*,*,#26252,.F.) ;
#35610 = ORIENTED_EDGE('',*,*,#26253,.F.) ;
#35611 = ORIENTED_EDGE('',*,*,#26251,.T.) ;
#35612 = ORIENTED_EDGE('',*,*,#25151,.T.) ;
#35613 = ORIENTED_EDGE('',*,*,#26248,.T.) ;
#35614 = ORIENTED_EDGE('',*,*,#26254,.T.) ;
#35615 = ORIENTED_EDGE('',*,*,#25746,.F.) ;
#35616 = ORIENTED_EDGE('',*,*,#26255,.T.) ;
#35617 = ORIENTED_EDGE('',*,*,#26252,.T.) ;
#35618 = ORIENTED_EDGE('',*,*,#26256,.T.) ;
#35619 = ORIENTED_EDGE('',*,*,#25149,.T.) ;
#35620 = ORIENTED_EDGE('',*,*,#26257,.F.) ;
#35621 = ORIENTED_EDGE('',*,*,#26258,.F.) ;
#35622 = ORIENTED_EDGE('',*,*,#26259,.F.) ;
#35623 = ORIENTED_EDGE('',*,*,#25154,.T.) ;
#35624 = ORIENTED_EDGE('',*,*,#26260,.F.) ;
#35625 = ORIENTED_EDGE('',*,*,#25775,.F.) ;
#35626 = ORIENTED_EDGE('',*,*,#26261,.F.) ;
#35627 = ORIENTED_EDGE('',*,*,#26260,.T.) ;
#35628 = ORIENTED_EDGE('',*,*,#25153,.T.) ;
#35629 = ORIENTED_EDGE('',*,*,#26253,.T.) ;
#35630 = ORIENTED_EDGE('',*,*,#26262,.T.) ;
#35631 = ORIENTED_EDGE('',*,*,#26263,.F.) ;
#35632 = ORIENTED_EDGE('',*,*,#26264,.F.) ;
#35633 = ORIENTED_EDGE('',*,*,#25147,.T.) ;
#35634 = ORIENTED_EDGE('',*,*,#26265,.F.) ;
#35635 = ORIENTED_EDGE('',*,*,#26257,.T.) ;
#35636 = ORIENTED_EDGE('',*,*,#25148,.T.) ;
#35637 = ORIENTED_EDGE('',*,*,#26264,.T.) ;
#35638 = ORIENTED_EDGE('',*,*,#26266,.T.) ;
#35639 = ORIENTED_EDGE('',*,*,#25156,.T.) ;
#35640 = ORIENTED_EDGE('',*,*,#26267,.F.) ;
#35641 = ORIENTED_EDGE('',*,*,#25780,.F.) ;
#35642 = ORIENTED_EDGE('',*,*,#26268,.F.) ;
#35643 = ORIENTED_EDGE('',*,*,#26267,.T.) ;
#35644 = ORIENTED_EDGE('',*,*,#25155,.T.) ;
#35645 = ORIENTED_EDGE('',*,*,#26261,.T.) ;
#35646 = ORIENTED_EDGE('',*,*,#25778,.T.) ;
#35647 = ORIENTED_EDGE('',*,*,#26269,.F.) ;
#35648 = ORIENTED_EDGE('',*,*,#26270,.F.) ;
#35649 = ORIENTED_EDGE('',*,*,#25788,.F.) ;
#35650 = ORIENTED_EDGE('',*,*,#25144,.T.) ;
#35651 = ORIENTED_EDGE('',*,*,#26271,.F.) ;
#35652 = ORIENTED_EDGE('',*,*,#25784,.F.) ;
#35653 = ORIENTED_EDGE('',*,*,#26272,.F.) ;
#35654 = ORIENTED_EDGE('',*,*,#26271,.T.) ;
#35655 = ORIENTED_EDGE('',*,*,#25157,.T.) ;
#35656 = ORIENTED_EDGE('',*,*,#26268,.T.) ;
#35657 = ORIENTED_EDGE('',*,*,#25782,.T.) ;
#35658 = ORIENTED_EDGE('',*,*,#26270,.T.) ;
#35659 = ORIENTED_EDGE('',*,*,#25145,.T.) ;
#35660 = ORIENTED_EDGE('',*,*,#26272,.T.) ;
#35661 = ORIENTED_EDGE('',*,*,#25786,.T.) ;
#35662 = ORIENTED_EDGE('',*,*,#26265,.T.) ;
#35663 = ORIENTED_EDGE('',*,*,#25146,.T.) ;
#35664 = ORIENTED_EDGE('',*,*,#26269,.T.) ;
#35665 = ORIENTED_EDGE('',*,*,#25790,.T.) ;
#35666 = ORIENTED_EDGE('',*,*,#25765,.F.) ;
#35667 = ORIENTED_EDGE('',*,*,#26273,.T.) ;
#35668 = ORIENTED_EDGE('',*,*,#26263,.T.) ;
#35669 = ORIENTED_EDGE('',*,*,#25789,.T.) ;
#35670 = ORIENTED_EDGE('',*,*,#25769,.F.) ;
#35671 = ORIENTED_EDGE('',*,*,#26274,.T.) ;
#35672 = ORIENTED_EDGE('',*,*,#26258,.T.) ;
#35673 = ORIENTED_EDGE('',*,*,#26275,.T.) ;
#35674 = ORIENTED_EDGE('',*,*,#26249,.T.) ;
#35675 = ORIENTED_EDGE('',*,*,#25150,.T.) ;
#35676 = ORIENTED_EDGE('',*,*,#26259,.T.) ;
#35677 = ORIENTED_EDGE('',*,*,#26276,.T.) ;
#35678 = ORIENTED_EDGE('',*,*,#25773,.F.) ;
#35679 = ORIENTED_EDGE('',*,*,#26277,.T.) ;
#35680 = ORIENTED_EDGE('',*,*,#26250,.T.) ;
#35681 = ORIENTED_EDGE('',*,*,#26278,.T.) ;
#35682 = ORIENTED_EDGE('',*,*,#25748,.F.) ;
#35683 = ORIENTED_EDGE('',*,*,#25776,.F.) ;
#35684 = ORIENTED_EDGE('',*,*,#26262,.F.) ;
#35685 = ORIENTED_EDGE('',*,*,#26255,.F.) ;
#35686 = ORIENTED_EDGE('',*,*,#25743,.F.) ;
#35687 = ORIENTED_EDGE('',*,*,#26256,.F.) ;
#35688 = ORIENTED_EDGE('',*,*,#26254,.F.) ;
#35689 = ORIENTED_EDGE('',*,*,#26277,.F.) ;
#35690 = ORIENTED_EDGE('',*,*,#26279,.T.) ;
#35691 = ORIENTED_EDGE('',*,*,#26280,.T.) ;
#35692 = ORIENTED_EDGE('',*,*,#26281,.T.) ;
#35693 = ORIENTED_EDGE('',*,*,#26282,.T.) ;
#35694 = ORIENTED_EDGE('',*,*,#26283,.T.) ;
#35695 = ORIENTED_EDGE('',*,*,#26284,.T.) ;
#35696 = ORIENTED_EDGE('',*,*,#26281,.F.) ;
#35697 = ORIENTED_EDGE('',*,*,#26285,.T.) ;
#35698 = ORIENTED_EDGE('',*,*,#25704,.F.) ;
#35699 = ORIENTED_EDGE('',*,*,#25204,.T.) ;
#35700 = ORIENTED_EDGE('',*,*,#26283,.F.) ;
#35701 = ORIENTED_EDGE('',*,*,#26285,.F.) ;
#35702 = ORIENTED_EDGE('',*,*,#26280,.F.) ;
#35703 = ORIENTED_EDGE('',*,*,#26286,.F.) ;
#35704 = ORIENTED_EDGE('',*,*,#26287,.T.) ;
#35705 = ORIENTED_EDGE('',*,*,#25703,.F.) ;
#35706 = ORIENTED_EDGE('',*,*,#26288,.T.) ;
#35707 = ORIENTED_EDGE('',*,*,#26289,.T.) ;
#35708 = ORIENTED_EDGE('',*,*,#26290,.T.) ;
#35709 = ORIENTED_EDGE('',*,*,#26291,.T.) ;
#35710 = ORIENTED_EDGE('',*,*,#26292,.T.) ;
#35711 = ORIENTED_EDGE('',*,*,#26293,.T.) ;
#35712 = ORIENTED_EDGE('',*,*,#26290,.F.) ;
#35713 = ORIENTED_EDGE('',*,*,#26294,.T.) ;
#35714 = ORIENTED_EDGE('',*,*,#25692,.T.) ;
#35715 = ORIENTED_EDGE('',*,*,#26292,.F.) ;
#35716 = ORIENTED_EDGE('',*,*,#25216,.T.) ;
#35717 = ORIENTED_EDGE('',*,*,#26284,.F.) ;
#35718 = ORIENTED_EDGE('',*,*,#25217,.T.) ;
#35719 = ORIENTED_EDGE('',*,*,#26294,.F.) ;
#35720 = ORIENTED_EDGE('',*,*,#26295,.T.) ;
#35721 = ORIENTED_EDGE('',*,*,#26282,.F.) ;
#35722 = ORIENTED_EDGE('',*,*,#26295,.F.) ;
#35723 = ORIENTED_EDGE('',*,*,#26289,.F.) ;
#35724 = ORIENTED_EDGE('',*,*,#26296,.F.) ;
#35725 = ORIENTED_EDGE('',*,*,#25956,.F.) ;
#35726 = ORIENTED_EDGE('',*,*,#26297,.F.) ;
#35727 = ORIENTED_EDGE('',*,*,#25213,.T.) ;
#35728 = ORIENTED_EDGE('',*,*,#26298,.F.) ;
#35729 = ORIENTED_EDGE('',*,*,#25690,.F.) ;
#35730 = ORIENTED_EDGE('',*,*,#25214,.T.) ;
#35731 = ORIENTED_EDGE('',*,*,#26297,.T.) ;
#35732 = ORIENTED_EDGE('',*,*,#25957,.T.) ;
#35733 = ORIENTED_EDGE('',*,*,#25952,.F.) ;
#35734 = ORIENTED_EDGE('',*,*,#26299,.F.) ;
#35735 = ORIENTED_EDGE('',*,*,#25211,.T.) ;
#35736 = ORIENTED_EDGE('',*,*,#26300,.F.) ;
#35737 = ORIENTED_EDGE('',*,*,#26299,.T.) ;
#35738 = ORIENTED_EDGE('',*,*,#25954,.T.) ;
#35739 = ORIENTED_EDGE('',*,*,#26298,.T.) ;
#35740 = ORIENTED_EDGE('',*,*,#25212,.T.) ;
#35741 = ORIENTED_EDGE('',*,*,#25948,.F.) ;
#35742 = ORIENTED_EDGE('',*,*,#26301,.F.) ;
#35743 = ORIENTED_EDGE('',*,*,#25209,.T.) ;
#35744 = ORIENTED_EDGE('',*,*,#26302,.F.) ;
#35745 = ORIENTED_EDGE('',*,*,#26300,.T.) ;
#35746 = ORIENTED_EDGE('',*,*,#25210,.T.) ;
#35747 = ORIENTED_EDGE('',*,*,#26301,.T.) ;
#35748 = ORIENTED_EDGE('',*,*,#25950,.T.) ;
#35749 = ORIENTED_EDGE('',*,*,#25944,.F.) ;
#35750 = ORIENTED_EDGE('',*,*,#26303,.F.) ;
#35751 = ORIENTED_EDGE('',*,*,#25207,.T.) ;
#35752 = ORIENTED_EDGE('',*,*,#26304,.F.) ;
#35753 = ORIENTED_EDGE('',*,*,#26303,.T.) ;
#35754 = ORIENTED_EDGE('',*,*,#25946,.T.) ;
#35755 = ORIENTED_EDGE('',*,*,#26302,.T.) ;
#35756 = ORIENTED_EDGE('',*,*,#25208,.T.) ;
#35757 = ORIENTED_EDGE('',*,*,#25695,.F.) ;
#35758 = ORIENTED_EDGE('',*,*,#25942,.T.) ;
#35759 = ORIENTED_EDGE('',*,*,#26304,.T.) ;
#35760 = ORIENTED_EDGE('',*,*,#25206,.T.) ;
#35761 = ORIENTED_EDGE('',*,*,#26305,.T.) ;
#35762 = ORIENTED_EDGE('',*,*,#26306,.T.) ;
#35763 = ORIENTED_EDGE('',*,*,#26307,.T.) ;
#35764 = ORIENTED_EDGE('',*,*,#26308,.T.) ;
#35765 = ORIENTED_EDGE('',*,*,#26309,.T.) ;
#35766 = ORIENTED_EDGE('',*,*,#26310,.T.) ;
#35767 = ORIENTED_EDGE('',*,*,#26307,.F.) ;
#35768 = ORIENTED_EDGE('',*,*,#26311,.T.) ;
#35769 = ORIENTED_EDGE('',*,*,#26312,.T.) ;
#35770 = ORIENTED_EDGE('',*,*,#26309,.F.) ;
#35771 = ORIENTED_EDGE('',*,*,#25173,.T.) ;
#35772 = ORIENTED_EDGE('',*,*,#26311,.F.) ;
#35773 = ORIENTED_EDGE('',*,*,#26313,.T.) ;
#35774 = ORIENTED_EDGE('',*,*,#26314,.F.) ;
#35775 = ORIENTED_EDGE('',*,*,#25174,.T.) ;
#35776 = ORIENTED_EDGE('',*,*,#26306,.F.) ;
#35777 = ORIENTED_EDGE('',*,*,#26315,.F.) ;
#35778 = ORIENTED_EDGE('',*,*,#26316,.F.) ;
#35779 = ORIENTED_EDGE('',*,*,#26313,.F.) ;
#35780 = ORIENTED_EDGE('',*,*,#26305,.F.) ;
#35781 = ORIENTED_EDGE('',*,*,#26317,.T.) ;
#35782 = ORIENTED_EDGE('',*,*,#26318,.T.) ;
#35783 = ORIENTED_EDGE('',*,*,#26319,.T.) ;
#35784 = ORIENTED_EDGE('',*,*,#26320,.F.) ;
#35785 = ORIENTED_EDGE('',*,*,#26315,.T.) ;
#35786 = ORIENTED_EDGE('',*,*,#26320,.T.) ;
#35787 = ORIENTED_EDGE('',*,*,#26321,.T.) ;
#35788 = ORIENTED_EDGE('',*,*,#26322,.T.) ;
#35789 = ORIENTED_EDGE('',*,*,#26316,.T.) ;
#35790 = ORIENTED_EDGE('',*,*,#26323,.T.) ;
#35791 = ORIENTED_EDGE('',*,*,#26314,.T.) ;
#35792 = ORIENTED_EDGE('',*,*,#26322,.F.) ;
#35793 = ORIENTED_EDGE('',*,*,#26324,.T.) ;
#35794 = ORIENTED_EDGE('',*,*,#26325,.F.) ;
#35795 = ORIENTED_EDGE('',*,*,#25175,.T.) ;
#35796 = ORIENTED_EDGE('',*,*,#26323,.F.) ;
#35797 = ORIENTED_EDGE('',*,*,#26324,.F.) ;
#35798 = ORIENTED_EDGE('',*,*,#26321,.F.) ;
#35799 = ORIENTED_EDGE('',*,*,#26319,.F.) ;
#35800 = ORIENTED_EDGE('',*,*,#26326,.T.) ;
#35801 = ORIENTED_EDGE('',*,*,#25365,.T.) ;
#35802 = ORIENTED_EDGE('',*,*,#25826,.T.) ;
#35803 = ORIENTED_EDGE('',*,*,#26327,.F.) ;
#35804 = ORIENTED_EDGE('',*,*,#26328,.F.) ;
#35805 = ORIENTED_EDGE('',*,*,#26329,.F.) ;
#35806 = ORIENTED_EDGE('',*,*,#25178,.T.) ;
#35807 = ORIENTED_EDGE('',*,*,#26330,.F.) ;
#35808 = ORIENTED_EDGE('',*,*,#26331,.F.) ;
#35809 = ORIENTED_EDGE('',*,*,#26332,.F.) ;
#35810 = ORIENTED_EDGE('',*,*,#25180,.T.) ;
#35811 = ORIENTED_EDGE('',*,*,#26333,.F.) ;
#35812 = ORIENTED_EDGE('',*,*,#26334,.F.) ;
#35813 = ORIENTED_EDGE('',*,*,#26335,.F.) ;
#35814 = ORIENTED_EDGE('',*,*,#25182,.T.) ;
#35815 = ORIENTED_EDGE('',*,*,#26336,.F.) ;
#35816 = ORIENTED_EDGE('',*,*,#26337,.F.) ;
#35817 = ORIENTED_EDGE('',*,*,#26338,.F.) ;
#35818 = ORIENTED_EDGE('',*,*,#25184,.T.) ;
#35819 = ORIENTED_EDGE('',*,*,#26339,.F.) ;
#35820 = ORIENTED_EDGE('',*,*,#25820,.F.) ;
#35821 = ORIENTED_EDGE('',*,*,#25185,.T.) ;
#35822 = ORIENTED_EDGE('',*,*,#26338,.T.) ;
#35823 = ORIENTED_EDGE('',*,*,#26340,.T.) ;
#35824 = ORIENTED_EDGE('',*,*,#25819,.F.) ;
#35825 = ORIENTED_EDGE('',*,*,#25829,.T.) ;
#35826 = ORIENTED_EDGE('',*,*,#26312,.F.) ;
#35827 = ORIENTED_EDGE('',*,*,#25172,.F.) ;
#35828 = ORIENTED_EDGE('',*,*,#26335,.T.) ;
#35829 = ORIENTED_EDGE('',*,*,#26341,.T.) ;
#35830 = ORIENTED_EDGE('',*,*,#26339,.T.) ;
#35831 = ORIENTED_EDGE('',*,*,#25183,.T.) ;
#35832 = ORIENTED_EDGE('',*,*,#25800,.F.) ;
#35833 = ORIENTED_EDGE('',*,*,#26342,.T.) ;
#35834 = ORIENTED_EDGE('',*,*,#26337,.T.) ;
#35835 = ORIENTED_EDGE('',*,*,#26343,.T.) ;
#35836 = ORIENTED_EDGE('',*,*,#26336,.T.) ;
#35837 = ORIENTED_EDGE('',*,*,#25181,.T.) ;
#35838 = ORIENTED_EDGE('',*,*,#26332,.T.) ;
#35839 = ORIENTED_EDGE('',*,*,#26344,.T.) ;
#35840 = ORIENTED_EDGE('',*,*,#25804,.F.) ;
#35841 = ORIENTED_EDGE('',*,*,#26345,.T.) ;
#35842 = ORIENTED_EDGE('',*,*,#26334,.T.) ;
#35843 = ORIENTED_EDGE('',*,*,#26346,.T.) ;
#35844 = ORIENTED_EDGE('',*,*,#26329,.T.) ;
#35845 = ORIENTED_EDGE('',*,*,#26347,.T.) ;
#35846 = ORIENTED_EDGE('',*,*,#26333,.T.) ;
#35847 = ORIENTED_EDGE('',*,*,#25179,.T.) ;
#35848 = ORIENTED_EDGE('',*,*,#25808,.F.) ;
#35849 = ORIENTED_EDGE('',*,*,#26348,.T.) ;
#35850 = ORIENTED_EDGE('',*,*,#26331,.T.) ;
#35851 = ORIENTED_EDGE('',*,*,#26349,.T.) ;
#35852 = ORIENTED_EDGE('',*,*,#25824,.F.) ;
#35853 = ORIENTED_EDGE('',*,*,#26350,.T.) ;
#35854 = ORIENTED_EDGE('',*,*,#26330,.T.) ;
#35855 = ORIENTED_EDGE('',*,*,#25177,.T.) ;
#35856 = ORIENTED_EDGE('',*,*,#25812,.F.) ;
#35857 = ORIENTED_EDGE('',*,*,#26351,.T.) ;
#35858 = ORIENTED_EDGE('',*,*,#26328,.T.) ;
#35859 = ORIENTED_EDGE('',*,*,#26352,.T.) ;
#35860 = ORIENTED_EDGE('',*,*,#25825,.F.) ;
#35861 = ORIENTED_EDGE('',*,*,#25176,.F.) ;
#35862 = ORIENTED_EDGE('',*,*,#26325,.T.) ;
#35863 = ORIENTED_EDGE('',*,*,#26353,.T.) ;
#35864 = ORIENTED_EDGE('',*,*,#25802,.F.) ;
#35865 = ORIENTED_EDGE('',*,*,#26343,.F.) ;
#35866 = ORIENTED_EDGE('',*,*,#26341,.F.) ;
#35867 = ORIENTED_EDGE('',*,*,#26345,.F.) ;
#35868 = ORIENTED_EDGE('',*,*,#25806,.F.) ;
#35869 = ORIENTED_EDGE('',*,*,#26346,.F.) ;
#35870 = ORIENTED_EDGE('',*,*,#26344,.F.) ;
#35871 = ORIENTED_EDGE('',*,*,#26348,.F.) ;
#35872 = ORIENTED_EDGE('',*,*,#25810,.F.) ;
#35873 = ORIENTED_EDGE('',*,*,#26349,.F.) ;
#35874 = ORIENTED_EDGE('',*,*,#26347,.F.) ;
#35875 = ORIENTED_EDGE('',*,*,#26351,.F.) ;
#35876 = ORIENTED_EDGE('',*,*,#25813,.F.) ;
#35877 = ORIENTED_EDGE('',*,*,#26352,.F.) ;
#35878 = ORIENTED_EDGE('',*,*,#26350,.F.) ;
#35879 = ORIENTED_EDGE('',*,*,#25823,.F.) ;
#35880 = ORIENTED_EDGE('',*,*,#25822,.F.) ;
#35881 = ORIENTED_EDGE('',*,*,#26353,.F.) ;
#35882 = ORIENTED_EDGE('',*,*,#26327,.T.) ;
#35883 = ORIENTED_EDGE('',*,*,#25827,.F.) ;
#35884 = ORIENTED_EDGE('',*,*,#25985,.F.) ;
#35885 = ORIENTED_EDGE('',*,*,#25433,.T.) ;
#35886 = ORIENTED_EDGE('',*,*,#25832,.F.) ;
#35887 = ORIENTED_EDGE('',*,*,#26354,.T.) ;
#35888 = ORIENTED_EDGE('',*,*,#26017,.F.) ;
#35889 = ORIENTED_EDGE('',*,*,#26354,.F.) ;
#35890 = ORIENTED_EDGE('',*,*,#26019,.F.) ;
#35891 = ORIENTED_EDGE('',*,*,#26018,.F.) ;
#35892 = ORIENTED_EDGE('',*,*,#26022,.F.) ;
#35893 = ORIENTED_EDGE('',*,*,#25419,.T.) ;
#35894 = ORIENTED_EDGE('',*,*,#25874,.F.) ;
#35895 = ORIENTED_EDGE('',*,*,#26355,.T.) ;
#35896 = ORIENTED_EDGE('',*,*,#26054,.F.) ;
#35897 = ORIENTED_EDGE('',*,*,#26355,.F.) ;
#35898 = ORIENTED_EDGE('',*,*,#26056,.F.) ;
#35899 = ORIENTED_EDGE('',*,*,#26055,.F.) ;
#35900 = ORIENTED_EDGE('',*,*,#25224,.T.) ;
#35901 = ORIENTED_EDGE('',*,*,#26356,.F.) ;
#35902 = ORIENTED_EDGE('',*,*,#26357,.F.) ;
#35903 = ORIENTED_EDGE('',*,*,#26358,.F.) ;
#35904 = ORIENTED_EDGE('',*,*,#26359,.F.) ;
#35905 = ORIENTED_EDGE('',*,*,#26360,.F.) ;
#35906 = ORIENTED_EDGE('',*,*,#25386,.T.) ;
#35907 = ORIENTED_EDGE('',*,*,#26361,.F.) ;
#35908 = ORIENTED_EDGE('',*,*,#25222,.T.) ;
#35909 = ORIENTED_EDGE('',*,*,#26362,.F.) ;
#35910 = ORIENTED_EDGE('',*,*,#26363,.F.) ;
#35911 = ORIENTED_EDGE('',*,*,#26364,.F.) ;
#35912 = ORIENTED_EDGE('',*,*,#26365,.F.) ;
#35913 = ORIENTED_EDGE('',*,*,#26366,.F.) ;
#35914 = ORIENTED_EDGE('',*,*,#25226,.T.) ;
#35915 = ORIENTED_EDGE('',*,*,#26367,.F.) ;
#35916 = ORIENTED_EDGE('',*,*,#25384,.T.) ;
#35917 = ORIENTED_EDGE('',*,*,#26368,.F.) ;
#35918 = ORIENTED_EDGE('',*,*,#26369,.F.) ;
#35919 = ORIENTED_EDGE('',*,*,#26370,.F.) ;
#35920 = ORIENTED_EDGE('',*,*,#26371,.F.) ;
#35921 = ORIENTED_EDGE('',*,*,#26372,.F.) ;
#35922 = ORIENTED_EDGE('',*,*,#25388,.T.) ;
#35923 = ORIENTED_EDGE('',*,*,#26373,.F.) ;
#35924 = ORIENTED_EDGE('',*,*,#25220,.T.) ;
#35925 = ORIENTED_EDGE('',*,*,#26374,.F.) ;
#35926 = ORIENTED_EDGE('',*,*,#26375,.F.) ;
#35927 = ORIENTED_EDGE('',*,*,#26376,.F.) ;
#35928 = ORIENTED_EDGE('',*,*,#26374,.T.) ;
#35929 = ORIENTED_EDGE('',*,*,#25227,.T.) ;
#35930 = ORIENTED_EDGE('',*,*,#26366,.T.) ;
#35931 = ORIENTED_EDGE('',*,*,#26377,.T.) ;
#35932 = ORIENTED_EDGE('',*,*,#26378,.F.) ;
#35933 = ORIENTED_EDGE('',*,*,#26379,.F.) ;
#35934 = ORIENTED_EDGE('',*,*,#25382,.T.) ;
#35935 = ORIENTED_EDGE('',*,*,#26380,.F.) ;
#35936 = ORIENTED_EDGE('',*,*,#26368,.T.) ;
#35937 = ORIENTED_EDGE('',*,*,#25383,.T.) ;
#35938 = ORIENTED_EDGE('',*,*,#26379,.T.) ;
#35939 = ORIENTED_EDGE('',*,*,#26381,.T.) ;
#35940 = ORIENTED_EDGE('',*,*,#26380,.T.) ;
#35941 = ORIENTED_EDGE('',*,*,#25389,.T.) ;
#35942 = ORIENTED_EDGE('',*,*,#26372,.T.) ;
#35943 = ORIENTED_EDGE('',*,*,#26382,.T.) ;
#35944 = ORIENTED_EDGE('',*,*,#26375,.T.) ;
#35945 = ORIENTED_EDGE('',*,*,#26383,.T.) ;
#35946 = ORIENTED_EDGE('',*,*,#26378,.T.) ;
#35947 = ORIENTED_EDGE('',*,*,#26384,.T.) ;
#35948 = ORIENTED_EDGE('',*,*,#26362,.T.) ;
#35949 = ORIENTED_EDGE('',*,*,#25221,.T.) ;
#35950 = ORIENTED_EDGE('',*,*,#26376,.T.) ;
#35951 = ORIENTED_EDGE('',*,*,#26385,.T.) ;
#35952 = ORIENTED_EDGE('',*,*,#26373,.T.) ;
#35953 = ORIENTED_EDGE('',*,*,#25387,.T.) ;
#35954 = ORIENTED_EDGE('',*,*,#26360,.T.) ;
#35955 = ORIENTED_EDGE('',*,*,#26386,.T.) ;
#35956 = ORIENTED_EDGE('',*,*,#26363,.T.) ;
#35957 = ORIENTED_EDGE('',*,*,#26387,.T.) ;
#35958 = ORIENTED_EDGE('',*,*,#26371,.T.) ;
#35959 = ORIENTED_EDGE('',*,*,#26388,.T.) ;
#35960 = ORIENTED_EDGE('',*,*,#26365,.T.) ;
#35961 = ORIENTED_EDGE('',*,*,#26389,.T.) ;
#35962 = ORIENTED_EDGE('',*,*,#26369,.T.) ;
#35963 = ORIENTED_EDGE('',*,*,#26390,.T.) ;
#35964 = ORIENTED_EDGE('',*,*,#26361,.T.) ;
#35965 = ORIENTED_EDGE('',*,*,#25385,.T.) ;
#35966 = ORIENTED_EDGE('',*,*,#26370,.T.) ;
#35967 = ORIENTED_EDGE('',*,*,#26391,.T.) ;
#35968 = ORIENTED_EDGE('',*,*,#26367,.T.) ;
#35969 = ORIENTED_EDGE('',*,*,#25225,.T.) ;
#35970 = ORIENTED_EDGE('',*,*,#26358,.T.) ;
#35971 = ORIENTED_EDGE('',*,*,#26392,.T.) ;
#35972 = ORIENTED_EDGE('',*,*,#26356,.T.) ;
#35973 = ORIENTED_EDGE('',*,*,#25223,.T.) ;
#35974 = ORIENTED_EDGE('',*,*,#26364,.T.) ;
#35975 = ORIENTED_EDGE('',*,*,#26393,.T.) ;
#35976 = ORIENTED_EDGE('',*,*,#26357,.T.) ;
#35977 = ORIENTED_EDGE('',*,*,#26394,.T.) ;
#35978 = ORIENTED_EDGE('',*,*,#26359,.T.) ;
#35979 = ORIENTED_EDGE('',*,*,#26395,.T.) ;
#35980 = ORIENTED_EDGE('',*,*,#26381,.F.) ;
#35981 = ORIENTED_EDGE('',*,*,#26383,.F.) ;
#35982 = ORIENTED_EDGE('',*,*,#26377,.F.) ;
#35983 = ORIENTED_EDGE('',*,*,#26390,.F.) ;
#35984 = ORIENTED_EDGE('',*,*,#26382,.F.) ;
#35985 = ORIENTED_EDGE('',*,*,#26387,.F.) ;
#35986 = ORIENTED_EDGE('',*,*,#26385,.F.) ;
#35987 = ORIENTED_EDGE('',*,*,#26384,.F.) ;
#35988 = ORIENTED_EDGE('',*,*,#26386,.F.) ;
#35989 = ORIENTED_EDGE('',*,*,#26394,.F.) ;
#35990 = ORIENTED_EDGE('',*,*,#26393,.F.) ;
#35991 = ORIENTED_EDGE('',*,*,#26388,.F.) ;
#35992 = ORIENTED_EDGE('',*,*,#26389,.F.) ;
#35993 = ORIENTED_EDGE('',*,*,#26392,.F.) ;
#35994 = ORIENTED_EDGE('',*,*,#26395,.F.) ;
#35995 = ORIENTED_EDGE('',*,*,#26391,.F.) ;
#35996 = ORIENTED_EDGE('',*,*,#25349,.T.) ;
#35997 = ORIENTED_EDGE('',*,*,#26396,.T.) ;
#35998 = ORIENTED_EDGE('',*,*,#26397,.T.) ;
#35999 = ORIENTED_EDGE('',*,*,#26396,.F.) ;
#36000 = ORIENTED_EDGE('',*,*,#26397,.F.) ;
#36001 = ORIENTED_EDGE('',*,*,#26398,.T.) ;
#36002 = ORIENTED_EDGE('',*,*,#26399,.F.) ;
#36003 = ORIENTED_EDGE('',*,*,#26400,.F.) ;
#36004 = ORIENTED_EDGE('',*,*,#26398,.F.) ;
#36005 = ORIENTED_EDGE('',*,*,#25186,.T.) ;
#36006 = ORIENTED_EDGE('',*,*,#26401,.T.) ;
#36007 = ORIENTED_EDGE('',*,*,#26399,.T.) ;
#36008 = ORIENTED_EDGE('',*,*,#26400,.T.) ;
#36009 = ORIENTED_EDGE('',*,*,#26401,.F.) ;
#36010 = ORIENTED_EDGE('',*,*,#26402,.T.) ;
#36011 = ORIENTED_EDGE('',*,*,#26403,.T.) ;
#36012 = ORIENTED_EDGE('',*,*,#26404,.T.) ;
#36013 = ORIENTED_EDGE('',*,*,#26405,.T.) ;
#36014 = ORIENTED_EDGE('',*,*,#26406,.T.) ;
#36015 = ORIENTED_EDGE('',*,*,#26407,.T.) ;
#36016 = ORIENTED_EDGE('',*,*,#26404,.F.) ;
#36017 = ORIENTED_EDGE('',*,*,#26408,.T.) ;
#36018 = ORIENTED_EDGE('',*,*,#26409,.F.) ;
#36019 = ORIENTED_EDGE('',*,*,#25201,.T.) ;
#36020 = ORIENTED_EDGE('',*,*,#26406,.F.) ;
#36021 = ORIENTED_EDGE('',*,*,#26408,.F.) ;
#36022 = ORIENTED_EDGE('',*,*,#26403,.F.) ;
#36023 = ORIENTED_EDGE('',*,*,#26410,.F.) ;
#36024 = ORIENTED_EDGE('',*,*,#26411,.T.) ;
#36025 = ORIENTED_EDGE('',*,*,#25280,.T.) ;
#36026 = ORIENTED_EDGE('',*,*,#25717,.T.) ;
#36027 = ORIENTED_EDGE('',*,*,#25721,.F.) ;
#36028 = ORIENTED_EDGE('',*,*,#26402,.F.) ;
#36029 = ORIENTED_EDGE('',*,*,#26412,.T.) ;
#36030 = ORIENTED_EDGE('',*,*,#26413,.F.) ;
#36031 = ORIENTED_EDGE('',*,*,#26414,.T.) ;
#36032 = ORIENTED_EDGE('',*,*,#26415,.T.) ;
#36033 = ORIENTED_EDGE('',*,*,#26410,.T.) ;
#36034 = ORIENTED_EDGE('',*,*,#26405,.F.) ;
#36035 = ORIENTED_EDGE('',*,*,#26416,.F.) ;
#36036 = ORIENTED_EDGE('',*,*,#26417,.F.) ;
#36037 = ORIENTED_EDGE('',*,*,#26412,.F.) ;
#36038 = ORIENTED_EDGE('',*,*,#26413,.T.) ;
#36039 = ORIENTED_EDGE('',*,*,#26417,.T.) ;
#36040 = ORIENTED_EDGE('',*,*,#26418,.T.) ;
#36041 = ORIENTED_EDGE('',*,*,#26419,.T.) ;
#36042 = ORIENTED_EDGE('',*,*,#26420,.T.) ;
#36043 = ORIENTED_EDGE('',*,*,#26421,.T.) ;
#36044 = ORIENTED_EDGE('',*,*,#26418,.F.) ;
#36045 = ORIENTED_EDGE('',*,*,#26422,.T.) ;
#36046 = ORIENTED_EDGE('',*,*,#26423,.T.) ;
#36047 = ORIENTED_EDGE('',*,*,#26420,.F.) ;
#36048 = ORIENTED_EDGE('',*,*,#25199,.T.) ;
#36049 = ORIENTED_EDGE('',*,*,#26407,.F.) ;
#36050 = ORIENTED_EDGE('',*,*,#25200,.T.) ;
#36051 = ORIENTED_EDGE('',*,*,#26422,.F.) ;
#36052 = ORIENTED_EDGE('',*,*,#26416,.T.) ;
#36053 = ORIENTED_EDGE('',*,*,#25739,.F.) ;
#36054 = ORIENTED_EDGE('',*,*,#26424,.F.) ;
#36055 = ORIENTED_EDGE('',*,*,#25196,.T.) ;
#36056 = ORIENTED_EDGE('',*,*,#26425,.F.) ;
#36057 = ORIENTED_EDGE('',*,*,#25197,.T.) ;
#36058 = ORIENTED_EDGE('',*,*,#26424,.T.) ;
#36059 = ORIENTED_EDGE('',*,*,#25741,.T.) ;
#36060 = ORIENTED_EDGE('',*,*,#26426,.T.) ;
#36061 = ORIENTED_EDGE('',*,*,#25735,.F.) ;
#36062 = ORIENTED_EDGE('',*,*,#26427,.F.) ;
#36063 = ORIENTED_EDGE('',*,*,#25194,.T.) ;
#36064 = ORIENTED_EDGE('',*,*,#26428,.F.) ;
#36065 = ORIENTED_EDGE('',*,*,#26427,.T.) ;
#36066 = ORIENTED_EDGE('',*,*,#25737,.T.) ;
#36067 = ORIENTED_EDGE('',*,*,#26425,.T.) ;
#36068 = ORIENTED_EDGE('',*,*,#25195,.T.) ;
#36069 = ORIENTED_EDGE('',*,*,#25731,.F.) ;
#36070 = ORIENTED_EDGE('',*,*,#26429,.F.) ;
#36071 = ORIENTED_EDGE('',*,*,#25192,.T.) ;
#36072 = ORIENTED_EDGE('',*,*,#26430,.F.) ;
#36073 = ORIENTED_EDGE('',*,*,#26428,.T.) ;
#36074 = ORIENTED_EDGE('',*,*,#25193,.T.) ;
#36075 = ORIENTED_EDGE('',*,*,#26429,.T.) ;
#36076 = ORIENTED_EDGE('',*,*,#25733,.T.) ;
#36077 = ORIENTED_EDGE('',*,*,#25727,.F.) ;
#36078 = ORIENTED_EDGE('',*,*,#26431,.F.) ;
#36079 = ORIENTED_EDGE('',*,*,#25190,.T.) ;
#36080 = ORIENTED_EDGE('',*,*,#26432,.F.) ;
#36081 = ORIENTED_EDGE('',*,*,#26431,.T.) ;
#36082 = ORIENTED_EDGE('',*,*,#25729,.T.) ;
#36083 = ORIENTED_EDGE('',*,*,#26430,.T.) ;
#36084 = ORIENTED_EDGE('',*,*,#25191,.T.) ;
#36085 = ORIENTED_EDGE('',*,*,#25723,.F.) ;
#36086 = ORIENTED_EDGE('',*,*,#26433,.F.) ;
#36087 = ORIENTED_EDGE('',*,*,#25188,.T.) ;
#36088 = ORIENTED_EDGE('',*,*,#26434,.F.) ;
#36089 = ORIENTED_EDGE('',*,*,#26432,.T.) ;
#36090 = ORIENTED_EDGE('',*,*,#25189,.T.) ;
#36091 = ORIENTED_EDGE('',*,*,#26433,.T.) ;
#36092 = ORIENTED_EDGE('',*,*,#25725,.T.) ;
#36093 = ORIENTED_EDGE('',*,*,#25720,.T.) ;
#36094 = ORIENTED_EDGE('',*,*,#26434,.T.) ;
#36095 = ORIENTED_EDGE('',*,*,#25187,.F.) ;
#36096 = ORIENTED_EDGE('',*,*,#26409,.T.) ;
#36097 = ORIENTED_EDGE('',*,*,#26435,.T.) ;
#36098 = ORIENTED_EDGE('',*,*,#26423,.F.) ;
#36099 = ORIENTED_EDGE('',*,*,#25198,.F.) ;
#36100 = ORIENTED_EDGE('',*,*,#26426,.F.) ;
#36101 = ORIENTED_EDGE('',*,*,#25068,.T.) ;
#36102 = ORIENTED_EDGE('',*,*,#26436,.T.) ;
#36103 = ORIENTED_EDGE('',*,*,#26437,.T.) ;
#36104 = ORIENTED_EDGE('',*,*,#26438,.T.) ;
#36105 = ORIENTED_EDGE('',*,*,#26436,.F.) ;
#36106 = ORIENTED_EDGE('',*,*,#25067,.T.) ;
#36107 = ORIENTED_EDGE('',*,*,#25350,.F.) ;
#36108 = ORIENTED_EDGE('',*,*,#26439,.T.) ;
#36109 = ORIENTED_EDGE('',*,*,#26437,.F.) ;
#36110 = ORIENTED_EDGE('',*,*,#26438,.F.) ;
#36111 = ORIENTED_EDGE('',*,*,#26439,.F.) ;
#36112 = ORIENTED_EDGE('',*,*,#25219,.T.) ;
#36113 = ORIENTED_EDGE('',*,*,#26440,.T.) ;
#36114 = ORIENTED_EDGE('',*,*,#26441,.T.) ;
#36115 = ORIENTED_EDGE('',*,*,#26442,.T.) ;
#36116 = ORIENTED_EDGE('',*,*,#26440,.F.) ;
#36117 = ORIENTED_EDGE('',*,*,#25367,.F.) ;
#36118 = ORIENTED_EDGE('',*,*,#26443,.T.) ;
#36119 = ORIENTED_EDGE('',*,*,#26441,.F.) ;
#36120 = ORIENTED_EDGE('',*,*,#26442,.F.) ;
#36121 = ORIENTED_EDGE('',*,*,#26443,.F.) ;
#36122 = ORIENTED_EDGE('',*,*,#25485,.F.) ;
#36123 = ORIENTED_EDGE('',*,*,#25492,.T.) ;
#36124 = ORIENTED_EDGE('',*,*,#26444,.T.) ;
#36125 = ORIENTED_EDGE('',*,*,#25301,.T.) ;
#36126 = ORIENTED_EDGE('',*,*,#26445,.T.) ;
#36127 = ORIENTED_EDGE('',*,*,#25302,.T.) ;
#36128 = ORIENTED_EDGE('',*,*,#26444,.F.) ;
#36129 = ORIENTED_EDGE('',*,*,#26446,.T.) ;
#36130 = ORIENTED_EDGE('',*,*,#26447,.T.) ;
#36131 = ORIENTED_EDGE('',*,*,#25303,.T.) ;
#36132 = ORIENTED_EDGE('',*,*,#26445,.F.) ;
#36133 = ORIENTED_EDGE('',*,*,#26142,.T.) ;
#36134 = ORIENTED_EDGE('',*,*,#26448,.T.) ;
#36135 = ORIENTED_EDGE('',*,*,#25304,.T.) ;
#36136 = ORIENTED_EDGE('',*,*,#26447,.F.) ;
#36137 = ORIENTED_EDGE('',*,*,#26145,.T.) ;
#36138 = ORIENTED_EDGE('',*,*,#26449,.T.) ;
#36139 = ORIENTED_EDGE('',*,*,#25305,.T.) ;
#36140 = ORIENTED_EDGE('',*,*,#26448,.F.) ;
#36141 = ORIENTED_EDGE('',*,*,#26147,.T.) ;
#36142 = ORIENTED_EDGE('',*,*,#26450,.T.) ;
#36143 = ORIENTED_EDGE('',*,*,#25306,.T.) ;
#36144 = ORIENTED_EDGE('',*,*,#26449,.F.) ;
#36145 = ORIENTED_EDGE('',*,*,#26149,.T.) ;
#36146 = ORIENTED_EDGE('',*,*,#26451,.T.) ;
#36147 = ORIENTED_EDGE('',*,*,#25307,.T.) ;
#36148 = ORIENTED_EDGE('',*,*,#26450,.F.) ;
#36149 = ORIENTED_EDGE('',*,*,#26151,.T.) ;
#36150 = ORIENTED_EDGE('',*,*,#26452,.T.) ;
#36151 = ORIENTED_EDGE('',*,*,#25308,.T.) ;
#36152 = ORIENTED_EDGE('',*,*,#26451,.F.) ;
#36153 = ORIENTED_EDGE('',*,*,#26153,.T.) ;
#36154 = ORIENTED_EDGE('',*,*,#26453,.T.) ;
#36155 = ORIENTED_EDGE('',*,*,#25309,.T.) ;
#36156 = ORIENTED_EDGE('',*,*,#26452,.F.) ;
#36157 = ORIENTED_EDGE('',*,*,#26155,.T.) ;
#36158 = ORIENTED_EDGE('',*,*,#26454,.T.) ;
#36159 = ORIENTED_EDGE('',*,*,#25310,.T.) ;
#36160 = ORIENTED_EDGE('',*,*,#26453,.F.) ;
#36161 = ORIENTED_EDGE('',*,*,#26157,.T.) ;
#36162 = ORIENTED_EDGE('',*,*,#26455,.T.) ;
#36163 = ORIENTED_EDGE('',*,*,#25311,.T.) ;
#36164 = ORIENTED_EDGE('',*,*,#26454,.F.) ;
#36165 = ORIENTED_EDGE('',*,*,#26159,.T.) ;
#36166 = ORIENTED_EDGE('',*,*,#26456,.T.) ;
#36167 = ORIENTED_EDGE('',*,*,#25312,.T.) ;
#36168 = ORIENTED_EDGE('',*,*,#26455,.F.) ;
#36169 = ORIENTED_EDGE('',*,*,#26161,.T.) ;
#36170 = ORIENTED_EDGE('',*,*,#26457,.T.) ;
#36171 = ORIENTED_EDGE('',*,*,#25313,.T.) ;
#36172 = ORIENTED_EDGE('',*,*,#26456,.F.) ;
#36173 = ORIENTED_EDGE('',*,*,#26163,.T.) ;
#36174 = ORIENTED_EDGE('',*,*,#26458,.T.) ;
#36175 = ORIENTED_EDGE('',*,*,#25314,.T.) ;
#36176 = ORIENTED_EDGE('',*,*,#26457,.F.) ;
#36177 = ORIENTED_EDGE('',*,*,#26165,.T.) ;
#36178 = ORIENTED_EDGE('',*,*,#26459,.T.) ;
#36179 = ORIENTED_EDGE('',*,*,#25315,.T.) ;
#36180 = ORIENTED_EDGE('',*,*,#26458,.F.) ;
#36181 = ORIENTED_EDGE('',*,*,#26167,.T.) ;
#36182 = ORIENTED_EDGE('',*,*,#26460,.T.) ;
#36183 = ORIENTED_EDGE('',*,*,#25316,.T.) ;
#36184 = ORIENTED_EDGE('',*,*,#26459,.F.) ;
#36185 = ORIENTED_EDGE('',*,*,#26169,.T.) ;
#36186 = ORIENTED_EDGE('',*,*,#26461,.T.) ;
#36187 = ORIENTED_EDGE('',*,*,#25317,.T.) ;
#36188 = ORIENTED_EDGE('',*,*,#26460,.F.) ;
#36189 = ORIENTED_EDGE('',*,*,#26171,.T.) ;
#36190 = ORIENTED_EDGE('',*,*,#26462,.T.) ;
#36191 = ORIENTED_EDGE('',*,*,#25318,.T.) ;
#36192 = ORIENTED_EDGE('',*,*,#26461,.F.) ;
#36193 = ORIENTED_EDGE('',*,*,#26173,.T.) ;
#36194 = ORIENTED_EDGE('',*,*,#26463,.T.) ;
#36195 = ORIENTED_EDGE('',*,*,#25319,.T.) ;
#36196 = ORIENTED_EDGE('',*,*,#26462,.F.) ;
#36197 = ORIENTED_EDGE('',*,*,#26175,.T.) ;
#36198 = ORIENTED_EDGE('',*,*,#26464,.T.) ;
#36199 = ORIENTED_EDGE('',*,*,#25320,.T.) ;
#36200 = ORIENTED_EDGE('',*,*,#26463,.F.) ;
#36201 = ORIENTED_EDGE('',*,*,#26177,.T.) ;
#36202 = ORIENTED_EDGE('',*,*,#26465,.T.) ;
#36203 = ORIENTED_EDGE('',*,*,#25321,.T.) ;
#36204 = ORIENTED_EDGE('',*,*,#26464,.F.) ;
#36205 = ORIENTED_EDGE('',*,*,#26179,.T.) ;
#36206 = ORIENTED_EDGE('',*,*,#26466,.T.) ;
#36207 = ORIENTED_EDGE('',*,*,#25322,.T.) ;
#36208 = ORIENTED_EDGE('',*,*,#26465,.F.) ;
#36209 = ORIENTED_EDGE('',*,*,#26181,.T.) ;
#36210 = ORIENTED_EDGE('',*,*,#26467,.T.) ;
#36211 = ORIENTED_EDGE('',*,*,#25323,.T.) ;
#36212 = ORIENTED_EDGE('',*,*,#26466,.F.) ;
#36213 = ORIENTED_EDGE('',*,*,#26183,.T.) ;
#36214 = ORIENTED_EDGE('',*,*,#26187,.T.) ;
#36215 = ORIENTED_EDGE('',*,*,#25324,.T.) ;
#36216 = ORIENTED_EDGE('',*,*,#26467,.F.) ;
#36217 = ORIENTED_EDGE('',*,*,#26185,.T.) ;
#36218 = ORIENTED_EDGE('',*,*,#26082,.F.) ;
#36219 = ORIENTED_EDGE('',*,*,#26143,.T.) ;
#36220 = ORIENTED_EDGE('',*,*,#26446,.F.) ;
#36221 = ORIENTED_EDGE('',*,*,#25491,.T.) ;
#36222 = ORIENTED_EDGE('',*,*,#26468,.T.) ;
#36223 = ORIENTED_EDGE('',*,*,#26469,.T.) ;
#36224 = ORIENTED_EDGE('',*,*,#25628,.F.) ;
#36225 = ORIENTED_EDGE('',*,*,#25332,.T.) ;
#36226 = ORIENTED_EDGE('',*,*,#26470,.T.) ;
#36227 = ORIENTED_EDGE('',*,*,#26471,.T.) ;
#36228 = ORIENTED_EDGE('',*,*,#26468,.F.) ;
#36229 = ORIENTED_EDGE('',*,*,#25331,.T.) ;
#36230 = ORIENTED_EDGE('',*,*,#26472,.T.) ;
#36231 = ORIENTED_EDGE('',*,*,#26473,.T.) ;
#36232 = ORIENTED_EDGE('',*,*,#26470,.F.) ;
#36233 = ORIENTED_EDGE('',*,*,#25330,.T.) ;
#36234 = ORIENTED_EDGE('',*,*,#26129,.F.) ;
#36235 = ORIENTED_EDGE('',*,*,#26474,.T.) ;
#36236 = ORIENTED_EDGE('',*,*,#26472,.F.) ;
#36237 = ORIENTED_EDGE('',*,*,#25329,.T.) ;
#36238 = ORIENTED_EDGE('',*,*,#25530,.T.) ;
#36239 = ORIENTED_EDGE('',*,*,#26475,.T.) ;
#36240 = ORIENTED_EDGE('',*,*,#26476,.T.) ;
#36241 = ORIENTED_EDGE('',*,*,#26475,.F.) ;
#36242 = ORIENTED_EDGE('',*,*,#26477,.F.) ;
#36243 = ORIENTED_EDGE('',*,*,#26476,.F.) ;
#36244 = ORIENTED_EDGE('',*,*,#26478,.T.) ;
#36245 = ORIENTED_EDGE('',*,*,#26479,.T.) ;
#36246 = ORIENTED_EDGE('',*,*,#26477,.T.) ;
#36247 = ORIENTED_EDGE('',*,*,#26479,.F.) ;
#36248 = ORIENTED_EDGE('',*,*,#26480,.T.) ;
#36249 = ORIENTED_EDGE('',*,*,#26481,.F.) ;
#36250 = ORIENTED_EDGE('',*,*,#26482,.T.) ;
#36251 = ORIENTED_EDGE('',*,*,#26480,.F.) ;
#36252 = ORIENTED_EDGE('',*,*,#26478,.F.) ;
#36253 = ORIENTED_EDGE('',*,*,#26482,.F.) ;
#36254 = ORIENTED_EDGE('',*,*,#26481,.T.) ;
#36255 = ORIENTED_EDGE('',*,*,#26483,.T.) ;
#36256 = ORIENTED_EDGE('',*,*,#26484,.T.) ;
#36257 = ORIENTED_EDGE('',*,*,#26485,.T.) ;
#36258 = ORIENTED_EDGE('',*,*,#26483,.F.) ;
#36259 = ORIENTED_EDGE('',*,*,#26486,.T.) ;
#36260 = ORIENTED_EDGE('',*,*,#26487,.T.) ;
#36261 = ORIENTED_EDGE('',*,*,#26488,.T.) ;
#36262 = ORIENTED_EDGE('',*,*,#26489,.T.) ;
#36263 = ORIENTED_EDGE('',*,*,#26487,.F.) ;
#36264 = ORIENTED_EDGE('',*,*,#26486,.F.) ;
#36265 = ORIENTED_EDGE('',*,*,#26490,.T.) ;
#36266 = ORIENTED_EDGE('',*,*,#26491,.F.) ;
#36267 = ORIENTED_EDGE('',*,*,#26492,.F.) ;
#36268 = ORIENTED_EDGE('',*,*,#26490,.F.) ;
#36269 = ORIENTED_EDGE('',*,*,#26491,.T.) ;
#36270 = ORIENTED_EDGE('',*,*,#26492,.T.) ;
#36271 = ORIENTED_EDGE('',*,*,#26493,.T.) ;
#36272 = ORIENTED_EDGE('',*,*,#26494,.T.) ;
#36273 = ORIENTED_EDGE('',*,*,#26493,.F.) ;
#36274 = ORIENTED_EDGE('',*,*,#26494,.F.) ;
#36275 = ORIENTED_EDGE('',*,*,#26495,.F.) ;
#36276 = ORIENTED_EDGE('',*,*,#26496,.T.) ;
#36277 = ORIENTED_EDGE('',*,*,#26497,.T.) ;
#36278 = ORIENTED_EDGE('',*,*,#26495,.T.) ;
#36279 = ORIENTED_EDGE('',*,*,#26497,.F.) ;
#36280 = ORIENTED_EDGE('',*,*,#26498,.T.) ;
#36281 = ORIENTED_EDGE('',*,*,#26499,.T.) ;
#36282 = ORIENTED_EDGE('',*,*,#26496,.F.) ;
#36283 = ORIENTED_EDGE('',*,*,#26499,.F.) ;
#36284 = ORIENTED_EDGE('',*,*,#26500,.T.) ;
#36285 = ORIENTED_EDGE('',*,*,#26501,.T.) ;
#36286 = ORIENTED_EDGE('',*,*,#26502,.T.) ;
#36287 = ORIENTED_EDGE('',*,*,#26503,.T.) ;
#36288 = ORIENTED_EDGE('',*,*,#26501,.F.) ;
#36289 = ORIENTED_EDGE('',*,*,#26500,.F.) ;
#36290 = ORIENTED_EDGE('',*,*,#26504,.T.) ;
#36291 = ORIENTED_EDGE('',*,*,#26505,.F.) ;
#36292 = ORIENTED_EDGE('',*,*,#26506,.F.) ;
#36293 = ORIENTED_EDGE('',*,*,#26504,.F.) ;
#36294 = ORIENTED_EDGE('',*,*,#25270,.T.) ;
#36295 = ORIENTED_EDGE('',*,*,#26507,.T.) ;
#36296 = ORIENTED_EDGE('',*,*,#26508,.T.) ;
#36297 = ORIENTED_EDGE('',*,*,#26507,.F.) ;
#36298 = ORIENTED_EDGE('',*,*,#26509,.F.) ;
#36299 = ORIENTED_EDGE('',*,*,#26508,.F.) ;
#36300 = ORIENTED_EDGE('',*,*,#26505,.T.) ;
#36301 = ORIENTED_EDGE('',*,*,#26506,.T.) ;
#36302 = ORIENTED_EDGE('',*,*,#26510,.T.) ;
#36303 = ORIENTED_EDGE('',*,*,#26509,.T.) ;
#36304 = ORIENTED_EDGE('',*,*,#26510,.F.) ;
#36305 = ORIENTED_EDGE('',*,*,#26485,.F.) ;
#36306 = ORIENTED_EDGE('',*,*,#26511,.T.) ;
#36307 = ORIENTED_EDGE('',*,*,#25202,.T.) ;
#36308 = ORIENTED_EDGE('',*,*,#26511,.F.) ;
#36309 = ORIENTED_EDGE('',*,*,#26484,.F.) ;
#36310 = ORIENTED_EDGE('',*,*,#26489,.F.) ;
#36311 = ORIENTED_EDGE('',*,*,#26512,.T.) ;
#36312 = ORIENTED_EDGE('',*,*,#25218,.T.) ;
#36313 = ORIENTED_EDGE('',*,*,#26512,.F.) ;
#36314 = ORIENTED_EDGE('',*,*,#26488,.F.) ;
#36315 = ORIENTED_EDGE('',*,*,#26503,.F.) ;
#36316 = ORIENTED_EDGE('',*,*,#26513,.T.) ;
#36317 = ORIENTED_EDGE('',*,*,#25203,.T.) ;
#36318 = ORIENTED_EDGE('',*,*,#26513,.F.) ;
#36319 = ORIENTED_EDGE('',*,*,#26502,.F.) ;
#36320 = ORIENTED_EDGE('',*,*,#25519,.F.) ;
#36321 = ORIENTED_EDGE('',*,*,#26498,.F.) ;
#36322 = ORIENTED_EDGE('',*,*,#26074,.F.) ;
#36323 = ORIENTED_EDGE('',*,*,#26514,.T.) ;
#36324 = ORIENTED_EDGE('',*,*,#26473,.F.) ;
#36325 = ORIENTED_EDGE('',*,*,#26515,.T.) ;
#36326 = ORIENTED_EDGE('',*,*,#26072,.F.) ;
#36327 = ORIENTED_EDGE('',*,*,#26516,.F.) ;
#36328 = ORIENTED_EDGE('',*,*,#26471,.F.) ;
#36329 = ORIENTED_EDGE('',*,*,#26514,.F.) ;
#36330 = ORIENTED_EDGE('',*,*,#26070,.F.) ;
#36331 = ORIENTED_EDGE('',*,*,#25512,.T.) ;
#36332 = ORIENTED_EDGE('',*,*,#26469,.F.) ;
#36333 = ORIENTED_EDGE('',*,*,#26516,.T.) ;
#36334 = ORIENTED_EDGE('',*,*,#26237,.F.) ;
#36335 = ORIENTED_EDGE('',*,*,#25374,.T.) ;
#36336 = ORIENTED_EDGE('',*,*,#26240,.F.) ;
#36337 = ORIENTED_EDGE('',*,*,#26229,.F.) ;
#36338 = ORIENTED_EDGE('',*,*,#26239,.F.) ;
#36339 = ORIENTED_EDGE('',*,*,#25372,.F.) ;
#36340 = ORIENTED_EDGE('',*,*,#26242,.F.) ;
#36341 = ORIENTED_EDGE('',*,*,#26225,.F.) ;
#36342 = ORIENTED_EDGE('',*,*,#26241,.F.) ;
#36343 = ORIENTED_EDGE('',*,*,#25370,.T.) ;
#36344 = ORIENTED_EDGE('',*,*,#26244,.F.) ;
#36345 = ORIENTED_EDGE('',*,*,#26221,.F.) ;
#36346 = ORIENTED_EDGE('',*,*,#26243,.F.) ;
#36347 = ORIENTED_EDGE('',*,*,#25368,.F.) ;
#36348 = ORIENTED_EDGE('',*,*,#26246,.F.) ;
#36349 = ORIENTED_EDGE('',*,*,#26217,.F.) ;
#36350 = ORIENTED_EDGE('',*,*,#25817,.F.) ;
#36351 = ORIENTED_EDGE('',*,*,#26340,.F.) ;
#36352 = ORIENTED_EDGE('',*,*,#26342,.F.) ;
#36353 = ORIENTED_EDGE('',*,*,#25798,.F.) ;
#36354 = ORIENTED_EDGE('',*,*,#26517,.T.) ;
#36355 = ORIENTED_EDGE('',*,*,#26518,.T.) ;
#36356 = ORIENTED_EDGE('',*,*,#26519,.T.) ;
#36357 = ORIENTED_EDGE('',*,*,#26520,.T.) ;
#36358 = ORIENTED_EDGE('',*,*,#26521,.T.) ;
#36359 = ORIENTED_EDGE('',*,*,#26522,.T.) ;
#36360 = ORIENTED_EDGE('',*,*,#26523,.T.) ;
#36361 = ORIENTED_EDGE('',*,*,#26524,.T.) ;
#36362 = ORIENTED_EDGE('',*,*,#26525,.T.) ;
#36363 = ORIENTED_EDGE('',*,*,#26526,.T.) ;
#36364 = ORIENTED_EDGE('',*,*,#26527,.T.) ;
#36365 = ORIENTED_EDGE('',*,*,#26528,.T.) ;
#36366 = ORIENTED_EDGE('',*,*,#26529,.T.) ;
#36367 = ORIENTED_EDGE('',*,*,#26530,.T.) ;
#36368 = ORIENTED_EDGE('',*,*,#26531,.T.) ;
#36369 = ORIENTED_EDGE('',*,*,#26140,.T.) ;
#36370 = ORIENTED_EDGE('',*,*,#26139,.T.) ;
#36371 = ORIENTED_EDGE('',*,*,#26532,.T.) ;
#36372 = ORIENTED_EDGE('',*,*,#26530,.F.) ;
#36373 = ORIENTED_EDGE('',*,*,#26533,.T.) ;
#36374 = ORIENTED_EDGE('',*,*,#26534,.T.) ;
#36375 = ORIENTED_EDGE('',*,*,#25061,.T.) ;
#36376 = ORIENTED_EDGE('',*,*,#26531,.F.) ;
#36377 = ORIENTED_EDGE('',*,*,#26535,.T.) ;
#36378 = ORIENTED_EDGE('',*,*,#25062,.T.) ;
#36379 = ORIENTED_EDGE('',*,*,#26534,.F.) ;
#36380 = ORIENTED_EDGE('',*,*,#26536,.T.) ;
#36381 = ORIENTED_EDGE('',*,*,#26537,.T.) ;
#36382 = ORIENTED_EDGE('',*,*,#25063,.T.) ;
#36383 = ORIENTED_EDGE('',*,*,#26535,.F.) ;
#36384 = ORIENTED_EDGE('',*,*,#25538,.T.) ;
#36385 = ORIENTED_EDGE('',*,*,#26538,.T.) ;
#36386 = ORIENTED_EDGE('',*,*,#25064,.T.) ;
#36387 = ORIENTED_EDGE('',*,*,#26537,.F.) ;
#36388 = ORIENTED_EDGE('',*,*,#26539,.T.) ;
#36389 = ORIENTED_EDGE('',*,*,#26527,.F.) ;
#36390 = ORIENTED_EDGE('',*,*,#25065,.T.) ;
#36391 = ORIENTED_EDGE('',*,*,#26538,.F.) ;
#36392 = ORIENTED_EDGE('',*,*,#26540,.T.) ;
#36393 = ORIENTED_EDGE('',*,*,#26528,.F.) ;
#36394 = ORIENTED_EDGE('',*,*,#26522,.F.) ;
#36395 = ORIENTED_EDGE('',*,*,#25069,.T.) ;
#36396 = ORIENTED_EDGE('',*,*,#25066,.T.) ;
#36397 = ORIENTED_EDGE('',*,*,#26526,.F.) ;
#36398 = ORIENTED_EDGE('',*,*,#26525,.F.) ;
#36399 = ORIENTED_EDGE('',*,*,#25590,.T.) ;
#36400 = ORIENTED_EDGE('',*,*,#26523,.F.) ;
#36401 = ORIENTED_EDGE('',*,*,#26520,.F.) ;
#36402 = ORIENTED_EDGE('',*,*,#26541,.T.) ;
#36403 = ORIENTED_EDGE('',*,*,#26542,.T.) ;
#36404 = ORIENTED_EDGE('',*,*,#25070,.T.) ;
#36405 = ORIENTED_EDGE('',*,*,#26521,.F.) ;
#36406 = ORIENTED_EDGE('',*,*,#26543,.T.) ;
#36407 = ORIENTED_EDGE('',*,*,#25071,.T.) ;
#36408 = ORIENTED_EDGE('',*,*,#26542,.F.) ;
#36409 = ORIENTED_EDGE('',*,*,#26544,.T.) ;
#36410 = ORIENTED_EDGE('',*,*,#26545,.T.) ;
#36411 = ORIENTED_EDGE('',*,*,#25072,.T.) ;
#36412 = ORIENTED_EDGE('',*,*,#26543,.F.) ;
#36413 = ORIENTED_EDGE('',*,*,#25558,.T.) ;
#36414 = ORIENTED_EDGE('',*,*,#26546,.T.) ;
#36415 = ORIENTED_EDGE('',*,*,#25073,.T.) ;
#36416 = ORIENTED_EDGE('',*,*,#26545,.F.) ;
#36417 = ORIENTED_EDGE('',*,*,#26547,.T.) ;
#36418 = ORIENTED_EDGE('',*,*,#26518,.F.) ;
#36419 = ORIENTED_EDGE('',*,*,#25074,.T.) ;
#36420 = ORIENTED_EDGE('',*,*,#26546,.F.) ;
#36421 = ORIENTED_EDGE('',*,*,#26548,.T.) ;
#36422 = ORIENTED_EDGE('',*,*,#26067,.F.) ;
#36423 = ORIENTED_EDGE('',*,*,#25075,.T.) ;
#36424 = ORIENTED_EDGE('',*,*,#26517,.F.) ;
#36425 = ORIENTED_EDGE('',*,*,#25585,.T.) ;
#36426 = ORIENTED_EDGE('',*,*,#26547,.F.) ;
#36427 = ORIENTED_EDGE('',*,*,#25563,.T.) ;
#36428 = ORIENTED_EDGE('',*,*,#26549,.T.) ;
#36429 = ORIENTED_EDGE('',*,*,#26550,.T.) ;
#36430 = ORIENTED_EDGE('',*,*,#26544,.F.) ;
#36431 = ORIENTED_EDGE('',*,*,#26551,.T.) ;
#36432 = ORIENTED_EDGE('',*,*,#26552,.T.) ;
#36433 = ORIENTED_EDGE('',*,*,#25559,.T.) ;
#36434 = ORIENTED_EDGE('',*,*,#26541,.F.) ;
#36435 = ORIENTED_EDGE('',*,*,#26553,.F.) ;
#36436 = ORIENTED_EDGE('',*,*,#26551,.F.) ;
#36437 = ORIENTED_EDGE('',*,*,#26524,.F.) ;
#36438 = ORIENTED_EDGE('',*,*,#25589,.T.) ;
#36439 = ORIENTED_EDGE('',*,*,#26554,.F.) ;
#36440 = ORIENTED_EDGE('',*,*,#26553,.T.) ;
#36441 = ORIENTED_EDGE('',*,*,#26529,.F.) ;
#36442 = ORIENTED_EDGE('',*,*,#26555,.T.) ;
#36443 = ORIENTED_EDGE('',*,*,#26556,.F.) ;
#36444 = ORIENTED_EDGE('',*,*,#25591,.T.) ;
#36445 = ORIENTED_EDGE('',*,*,#26540,.F.) ;
#36446 = ORIENTED_EDGE('',*,*,#26557,.F.) ;
#36447 = ORIENTED_EDGE('',*,*,#26555,.F.) ;
#36448 = ORIENTED_EDGE('',*,*,#26539,.F.) ;
#36449 = ORIENTED_EDGE('',*,*,#25543,.T.) ;
#36450 = ORIENTED_EDGE('',*,*,#26558,.T.) ;
#36451 = ORIENTED_EDGE('',*,*,#26557,.T.) ;
#36452 = ORIENTED_EDGE('',*,*,#26536,.F.) ;
#36453 = ORIENTED_EDGE('',*,*,#26559,.T.) ;
#36454 = ORIENTED_EDGE('',*,*,#26560,.T.) ;
#36455 = ORIENTED_EDGE('',*,*,#25539,.T.) ;
#36456 = ORIENTED_EDGE('',*,*,#26533,.F.) ;
#36457 = ORIENTED_EDGE('',*,*,#26561,.F.) ;
#36458 = ORIENTED_EDGE('',*,*,#26559,.F.) ;
#36459 = ORIENTED_EDGE('',*,*,#26532,.F.) ;
#36460 = ORIENTED_EDGE('',*,*,#25594,.T.) ;
#36461 = ORIENTED_EDGE('',*,*,#26562,.F.) ;
#36462 = ORIENTED_EDGE('',*,*,#26561,.T.) ;
#36463 = ORIENTED_EDGE('',*,*,#26293,.F.) ;
#36464 = ORIENTED_EDGE('',*,*,#25693,.F.) ;
#36465 = ORIENTED_EDGE('',*,*,#26563,.F.) ;
#36466 = ORIENTED_EDGE('',*,*,#26564,.F.) ;
#36467 = ORIENTED_EDGE('',*,*,#26291,.F.) ;
#36468 = ORIENTED_EDGE('',*,*,#25391,.F.) ;
#36469 = ORIENTED_EDGE('',*,*,#26287,.F.) ;
#36470 = ORIENTED_EDGE('',*,*,#26565,.F.) ;
#36471 = ORIENTED_EDGE('',*,*,#26563,.T.) ;
#36472 = ORIENTED_EDGE('',*,*,#26279,.F.) ;
#36473 = ORIENTED_EDGE('',*,*,#26296,.T.) ;
#36474 = ORIENTED_EDGE('',*,*,#26288,.F.) ;
#36475 = ORIENTED_EDGE('',*,*,#26564,.T.) ;
#36476 = ORIENTED_EDGE('',*,*,#26565,.T.) ;
#36477 = ORIENTED_EDGE('',*,*,#26286,.T.) ;
#36478 = ORIENTED_EDGE('',*,*,#26421,.F.) ;
#36479 = ORIENTED_EDGE('',*,*,#26566,.F.) ;
#36480 = ORIENTED_EDGE('',*,*,#26567,.F.) ;
#36481 = ORIENTED_EDGE('',*,*,#26414,.F.) ;
#36482 = ORIENTED_EDGE('',*,*,#26419,.F.) ;
#36483 = ORIENTED_EDGE('',*,*,#25281,.F.) ;
#36484 = ORIENTED_EDGE('',*,*,#26411,.F.) ;
#36485 = ORIENTED_EDGE('',*,*,#26415,.F.) ;
#36486 = ORIENTED_EDGE('',*,*,#26567,.T.) ;
#36487 = ORIENTED_EDGE('',*,*,#26435,.F.) ;
#36488 = ORIENTED_EDGE('',*,*,#25740,.F.) ;
#36489 = ORIENTED_EDGE('',*,*,#25706,.F.) ;
#36490 = ORIENTED_EDGE('',*,*,#25282,.F.) ;
#36491 = ORIENTED_EDGE('',*,*,#26566,.T.) ;
#36492 = ORIENTED_EDGE('',*,*,#26193,.F.) ;
#36493 = ORIENTED_EDGE('',*,*,#26568,.F.) ;
#36494 = ORIENTED_EDGE('',*,*,#26569,.F.) ;
#36495 = ORIENTED_EDGE('',*,*,#26200,.F.) ;
#36496 = ORIENTED_EDGE('',*,*,#26191,.F.) ;
#36497 = ORIENTED_EDGE('',*,*,#25379,.F.) ;
#36498 = ORIENTED_EDGE('',*,*,#26209,.F.) ;
#36499 = ORIENTED_EDGE('',*,*,#26201,.F.) ;
#36500 = ORIENTED_EDGE('',*,*,#26569,.T.) ;
#36501 = ORIENTED_EDGE('',*,*,#26245,.F.) ;
#36502 = ORIENTED_EDGE('',*,*,#25380,.F.) ;
#36503 = ORIENTED_EDGE('',*,*,#26568,.T.) ;
#36504 = ORIENTED_EDGE('',*,*,#26247,.F.) ;
#36505 = ORIENTED_EDGE('',*,*,#26310,.F.) ;
#36506 = ORIENTED_EDGE('',*,*,#25828,.F.) ;
#36507 = ORIENTED_EDGE('',*,*,#25814,.F.) ;
#36508 = ORIENTED_EDGE('',*,*,#25351,.T.) ;
#36509 = ORIENTED_EDGE('',*,*,#26570,.F.) ;
#36510 = ORIENTED_EDGE('',*,*,#26317,.F.) ;
#36511 = ORIENTED_EDGE('',*,*,#26308,.F.) ;
#36512 = ORIENTED_EDGE('',*,*,#25366,.F.) ;
#36513 = ORIENTED_EDGE('',*,*,#26326,.F.) ;
#36514 = ORIENTED_EDGE('',*,*,#26318,.F.) ;
#36515 = ORIENTED_EDGE('',*,*,#26570,.T.) ;
#36516 = ORIENTED_EDGE('',*,*,#25662,.F.) ;
#36517 = ORIENTED_EDGE('',*,*,#25404,.F.) ;
#36518 = ORIENTED_EDGE('',*,*,#25669,.F.) ;
#36519 = ORIENTED_EDGE('',*,*,#25667,.F.) ;
#36520 = ORIENTED_EDGE('',*,*,#25658,.F.) ;
#36521 = ORIENTED_EDGE('',*,*,#25664,.F.) ;
#36522 = ORIENTED_EDGE('',*,*,#25958,.F.) ;
#36523 = ORIENTED_EDGE('',*,*,#25982,.F.) ;
#36524 = ORIENTED_EDGE('',*,*,#25981,.F.) ;
#36525 = ORIENTED_EDGE('',*,*,#25980,.F.) ;
#36526 = ORIENTED_EDGE('',*,*,#25771,.F.) ;
#36527 = ORIENTED_EDGE('',*,*,#26278,.F.) ;
#36528 = ORIENTED_EDGE('',*,*,#26276,.F.) ;
#36529 = ORIENTED_EDGE('',*,*,#26274,.F.) ;
#36530 = ORIENTED_EDGE('',*,*,#25767,.F.) ;
#36531 = ORIENTED_EDGE('',*,*,#26275,.F.) ;
#36532 = ORIENTED_EDGE('',*,*,#26266,.F.) ;
#36533 = ORIENTED_EDGE('',*,*,#26273,.F.) ;
#36534 = ORIENTED_EDGE('',*,*,#26130,.F.) ;
#36535 = ORIENTED_EDGE('',*,*,#25327,.F.) ;
#36536 = ORIENTED_EDGE('',*,*,#26138,.F.) ;
#36537 = ORIENTED_EDGE('',*,*,#26136,.F.) ;
#36538 = ORIENTED_EDGE('',*,*,#26133,.F.) ;
#36539 = ORIENTED_EDGE('',*,*,#26132,.F.) ;
#36540 = ORIENTED_EDGE('',*,*,#26075,.F.) ;
#36541 = ORIENTED_EDGE('',*,*,#26515,.F.) ;
#36542 = ORIENTED_EDGE('',*,*,#26474,.F.) ;
#36543 = ORIENTED_EDGE('',*,*,#26131,.F.) ;
#36544 = ORIENTED_EDGE('',*,*,#25618,.T.) ;
#36545 = ORIENTED_EDGE('',*,*,#25610,.T.) ;
#36546 = ORIENTED_EDGE('',*,*,#26571,.F.) ;
#36547 = ORIENTED_EDGE('',*,*,#25570,.F.) ;
#36548 = ORIENTED_EDGE('',*,*,#25291,.F.) ;
#36549 = ORIENTED_EDGE('',*,*,#25604,.T.) ;
#36550 = ORIENTED_EDGE('',*,*,#26572,.F.) ;
#36551 = ORIENTED_EDGE('',*,*,#25548,.F.) ;
#36552 = ORIENTED_EDGE('',*,*,#25297,.F.) ;
#36553 = ORIENTED_EDGE('',*,*,#26573,.F.) ;
#36554 = ORIENTED_EDGE('',*,*,#25607,.T.) ;
#36555 = ORIENTED_EDGE('',*,*,#26574,.F.) ;
#36556 = ORIENTED_EDGE('',*,*,#25293,.F.) ;
#36557 = ORIENTED_EDGE('',*,*,#25569,.F.) ;
#36558 = ORIENTED_EDGE('',*,*,#26575,.F.) ;
#36559 = ORIENTED_EDGE('',*,*,#25602,.F.) ;
#36560 = ORIENTED_EDGE('',*,*,#25639,.T.) ;
#36561 = ORIENTED_EDGE('',*,*,#25546,.F.) ;
#36562 = ORIENTED_EDGE('',*,*,#25609,.F.) ;
#36563 = ORIENTED_EDGE('',*,*,#25566,.F.) ;
#36564 = ORIENTED_EDGE('',*,*,#26571,.T.) ;
#36565 = ORIENTED_EDGE('',*,*,#25603,.F.) ;
#36566 = ORIENTED_EDGE('',*,*,#25549,.F.) ;
#36567 = ORIENTED_EDGE('',*,*,#26572,.T.) ;
#36568 = ORIENTED_EDGE('',*,*,#25605,.T.) ;
#36569 = ORIENTED_EDGE('',*,*,#26573,.T.) ;
#36570 = ORIENTED_EDGE('',*,*,#25296,.T.) ;
#36571 = ORIENTED_EDGE('',*,*,#25608,.F.) ;
#36572 = ORIENTED_EDGE('',*,*,#26575,.T.) ;
#36573 = ORIENTED_EDGE('',*,*,#25568,.F.) ;
#36574 = ORIENTED_EDGE('',*,*,#25606,.F.) ;
#36575 = ORIENTED_EDGE('',*,*,#25294,.T.) ;
#36576 = ORIENTED_EDGE('',*,*,#26574,.T.) ;
#36577 = ORIENTED_EDGE('',*,*,#25587,.T.) ;
#36578 = ORIENTED_EDGE('',*,*,#26576,.T.) ;
#36579 = ORIENTED_EDGE('',*,*,#26549,.F.) ;
#36580 = ORIENTED_EDGE('',*,*,#25562,.T.) ;
#36581 = ORIENTED_EDGE('',*,*,#25588,.T.) ;
#36582 = ORIENTED_EDGE('',*,*,#25560,.T.) ;
#36583 = ORIENTED_EDGE('',*,*,#26552,.F.) ;
#36584 = ORIENTED_EDGE('',*,*,#26554,.T.) ;
#36585 = ORIENTED_EDGE('',*,*,#25593,.T.) ;
#36586 = ORIENTED_EDGE('',*,*,#25540,.T.) ;
#36587 = ORIENTED_EDGE('',*,*,#26560,.F.) ;
#36588 = ORIENTED_EDGE('',*,*,#26562,.T.) ;
#36589 = ORIENTED_EDGE('',*,*,#25592,.T.) ;
#36590 = ORIENTED_EDGE('',*,*,#26556,.T.) ;
#36591 = ORIENTED_EDGE('',*,*,#26558,.F.) ;
#36592 = ORIENTED_EDGE('',*,*,#25542,.T.) ;
#36593 = ORIENTED_EDGE('',*,*,#26519,.F.) ;
#36594 = ORIENTED_EDGE('',*,*,#26577,.T.) ;
#36595 = ORIENTED_EDGE('',*,*,#26576,.F.) ;
#36596 = ORIENTED_EDGE('',*,*,#25586,.T.) ;
#36597 = ORIENTED_EDGE('',*,*,#26548,.F.) ;
#36598 = ORIENTED_EDGE('',*,*,#26550,.F.) ;
#36599 = ORIENTED_EDGE('',*,*,#26577,.F.) ;
#36600 = ORIENTED_EDGE('',*,*,#26578,.T.) ;
#36601 = ORIENTED_EDGE('',*,*,#26579,.T.) ;
#36602 = ORIENTED_EDGE('',*,*,#26580,.T.) ;
#36603 = ORIENTED_EDGE('',*,*,#26581,.T.) ;
#36604 = ORIENTED_EDGE('',*,*,#26582,.T.) ;
#36605 = ORIENTED_EDGE('',*,*,#26583,.T.) ;
#36606 = ORIENTED_EDGE('',*,*,#26584,.T.) ;
#36607 = ORIENTED_EDGE('',*,*,#26581,.F.) ;
#36608 = ORIENTED_EDGE('',*,*,#26585,.T.) ;
#36609 = ORIENTED_EDGE('',*,*,#26586,.T.) ;
#36610 = ORIENTED_EDGE('',*,*,#26587,.T.) ;
#36611 = ORIENTED_EDGE('',*,*,#26583,.F.) ;
#36612 = ORIENTED_EDGE('',*,*,#26588,.F.) ;
#36613 = ORIENTED_EDGE('',*,*,#26589,.F.) ;
#36614 = ORIENTED_EDGE('',*,*,#26590,.F.) ;
#36615 = ORIENTED_EDGE('',*,*,#26591,.T.) ;
#36616 = ORIENTED_EDGE('',*,*,#26592,.T.) ;
#36617 = ORIENTED_EDGE('',*,*,#26589,.T.) ;
#36618 = ORIENTED_EDGE('',*,*,#26593,.T.) ;
#36619 = ORIENTED_EDGE('',*,*,#26594,.T.) ;
#36620 = ORIENTED_EDGE('',*,*,#26595,.T.) ;
#36621 = ORIENTED_EDGE('',*,*,#26590,.T.) ;
#36622 = ORIENTED_EDGE('',*,*,#26596,.T.) ;
#36623 = ORIENTED_EDGE('',*,*,#26597,.T.) ;
#36624 = ORIENTED_EDGE('',*,*,#26588,.T.) ;
#36625 = ORIENTED_EDGE('',*,*,#26598,.T.) ;
#36626 = ORIENTED_EDGE('',*,*,#26586,.F.) ;
#36627 = ORIENTED_EDGE('',*,*,#26578,.F.) ;
#36628 = ORIENTED_EDGE('',*,*,#26599,.T.) ;
#36629 = ORIENTED_EDGE('',*,*,#26600,.F.) ;
#36630 = ORIENTED_EDGE('',*,*,#26601,.F.) ;
#36631 = ORIENTED_EDGE('',*,*,#26579,.F.) ;
#36632 = ORIENTED_EDGE('',*,*,#26601,.T.) ;
#36633 = ORIENTED_EDGE('',*,*,#26602,.F.) ;
#36634 = ORIENTED_EDGE('',*,*,#26603,.F.) ;
#36635 = ORIENTED_EDGE('',*,*,#26591,.F.) ;
#36636 = ORIENTED_EDGE('',*,*,#26604,.F.) ;
#36637 = ORIENTED_EDGE('',*,*,#26584,.F.) ;
#36638 = ORIENTED_EDGE('',*,*,#26605,.T.) ;
#36639 = ORIENTED_EDGE('',*,*,#26606,.F.) ;
#36640 = ORIENTED_EDGE('',*,*,#26599,.F.) ;
#36641 = ORIENTED_EDGE('',*,*,#26587,.F.) ;
#36642 = ORIENTED_EDGE('',*,*,#26607,.T.) ;
#36643 = ORIENTED_EDGE('',*,*,#26608,.F.) ;
#36644 = ORIENTED_EDGE('',*,*,#26605,.F.) ;
#36645 = ORIENTED_EDGE('',*,*,#26598,.F.) ;
#36646 = ORIENTED_EDGE('',*,*,#26595,.F.) ;
#36647 = ORIENTED_EDGE('',*,*,#26609,.F.) ;
#36648 = ORIENTED_EDGE('',*,*,#26607,.F.) ;
#36649 = ORIENTED_EDGE('',*,*,#26592,.F.) ;
#36650 = ORIENTED_EDGE('',*,*,#26603,.T.) ;
#36651 = ORIENTED_EDGE('',*,*,#26610,.F.) ;
#36652 = ORIENTED_EDGE('',*,*,#26596,.F.) ;
#36653 = ORIENTED_EDGE('',*,*,#26594,.F.) ;
#36654 = ORIENTED_EDGE('',*,*,#26610,.T.) ;
#36655 = ORIENTED_EDGE('',*,*,#26602,.T.) ;
#36656 = ORIENTED_EDGE('',*,*,#26600,.T.) ;
#36657 = ORIENTED_EDGE('',*,*,#26606,.T.) ;
#36658 = ORIENTED_EDGE('',*,*,#26608,.T.) ;
#36659 = ORIENTED_EDGE('',*,*,#26609,.T.) ;
#36660 = ORIENTED_EDGE('',*,*,#26580,.F.) ;
#36661 = ORIENTED_EDGE('',*,*,#26604,.T.) ;
#36662 = ORIENTED_EDGE('',*,*,#26593,.F.) ;
#36663 = ORIENTED_EDGE('',*,*,#26597,.F.) ;
#36664 = ORIENTED_EDGE('',*,*,#26585,.F.) ;
#36665 = ORIENTED_EDGE('',*,*,#26582,.F.) ;
#36666 = ORIENTED_EDGE('',*,*,#26611,.T.) ;
#36667 = ORIENTED_EDGE('',*,*,#26612,.T.) ;
#36668 = ORIENTED_EDGE('',*,*,#26613,.T.) ;
#36669 = ORIENTED_EDGE('',*,*,#26614,.T.) ;
#36670 = ORIENTED_EDGE('',*,*,#26615,.T.) ;
#36671 = ORIENTED_EDGE('',*,*,#26616,.T.) ;
#36672 = ORIENTED_EDGE('',*,*,#26617,.T.) ;
#36673 = ORIENTED_EDGE('',*,*,#26618,.T.) ;
#36674 = ORIENTED_EDGE('',*,*,#26619,.T.) ;
#36675 = ORIENTED_EDGE('',*,*,#26620,.T.) ;
#36676 = ORIENTED_EDGE('',*,*,#26621,.T.) ;
#36677 = ORIENTED_EDGE('',*,*,#26622,.T.) ;
#36678 = ORIENTED_EDGE('',*,*,#26621,.F.) ;
#36679 = ORIENTED_EDGE('',*,*,#26623,.T.) ;
#36680 = ORIENTED_EDGE('',*,*,#26617,.F.) ;
#36681 = ORIENTED_EDGE('',*,*,#26615,.F.) ;
#36682 = ORIENTED_EDGE('',*,*,#26624,.T.) ;
#36683 = ORIENTED_EDGE('',*,*,#26613,.F.) ;
#36684 = ORIENTED_EDGE('',*,*,#26614,.F.) ;
#36685 = ORIENTED_EDGE('',*,*,#26625,.F.) ;
#36686 = ORIENTED_EDGE('',*,*,#26626,.F.) ;
#36687 = ORIENTED_EDGE('',*,*,#26627,.F.) ;
#36688 = ORIENTED_EDGE('',*,*,#26628,.F.) ;
#36689 = ORIENTED_EDGE('',*,*,#26629,.F.) ;
#36690 = ORIENTED_EDGE('',*,*,#26630,.F.) ;
#36691 = ORIENTED_EDGE('',*,*,#26631,.F.) ;
#36692 = ORIENTED_EDGE('',*,*,#26632,.F.) ;
#36693 = ORIENTED_EDGE('',*,*,#26633,.F.) ;
#36694 = ORIENTED_EDGE('',*,*,#26634,.F.) ;
#36695 = ORIENTED_EDGE('',*,*,#26635,.F.) ;
#36696 = ORIENTED_EDGE('',*,*,#26636,.F.) ;
#36697 = ORIENTED_EDGE('',*,*,#26637,.F.) ;
#36698 = ORIENTED_EDGE('',*,*,#26638,.F.) ;
#36699 = ORIENTED_EDGE('',*,*,#26639,.F.) ;
#36700 = ORIENTED_EDGE('',*,*,#26640,.F.) ;
#36701 = ORIENTED_EDGE('',*,*,#26641,.F.) ;
#36702 = ORIENTED_EDGE('',*,*,#26642,.F.) ;
#36703 = ORIENTED_EDGE('',*,*,#26643,.F.) ;
#36704 = ORIENTED_EDGE('',*,*,#26644,.F.) ;
#36705 = ORIENTED_EDGE('',*,*,#26645,.F.) ;
#36706 = ORIENTED_EDGE('',*,*,#26646,.F.) ;
#36707 = ORIENTED_EDGE('',*,*,#26647,.T.) ;
#36708 = ORIENTED_EDGE('',*,*,#26648,.T.) ;
#36709 = ORIENTED_EDGE('',*,*,#26649,.F.) ;
#36710 = ORIENTED_EDGE('',*,*,#26650,.F.) ;
#36711 = ORIENTED_EDGE('',*,*,#26651,.F.) ;
#36712 = ORIENTED_EDGE('',*,*,#26652,.F.) ;
#36713 = ORIENTED_EDGE('',*,*,#26653,.F.) ;
#36714 = ORIENTED_EDGE('',*,*,#26654,.F.) ;
#36715 = ORIENTED_EDGE('',*,*,#26655,.F.) ;
#36716 = ORIENTED_EDGE('',*,*,#26656,.F.) ;
#36717 = ORIENTED_EDGE('',*,*,#26657,.F.) ;
#36718 = ORIENTED_EDGE('',*,*,#26658,.F.) ;
#36719 = ORIENTED_EDGE('',*,*,#26659,.F.) ;
#36720 = ORIENTED_EDGE('',*,*,#26660,.F.) ;
#36721 = ORIENTED_EDGE('',*,*,#26661,.T.) ;
#36722 = ORIENTED_EDGE('',*,*,#26662,.F.) ;
#36723 = ORIENTED_EDGE('',*,*,#26663,.T.) ;
#36724 = ORIENTED_EDGE('',*,*,#26664,.F.) ;
#36725 = ORIENTED_EDGE('',*,*,#26665,.T.) ;
#36726 = ORIENTED_EDGE('',*,*,#26666,.F.) ;
#36727 = ORIENTED_EDGE('',*,*,#26667,.T.) ;
#36728 = ORIENTED_EDGE('',*,*,#26668,.F.) ;
#36729 = ORIENTED_EDGE('',*,*,#26669,.T.) ;
#36730 = ORIENTED_EDGE('',*,*,#26670,.F.) ;
#36731 = ORIENTED_EDGE('',*,*,#26671,.T.) ;
#36732 = ORIENTED_EDGE('',*,*,#26672,.F.) ;
#36733 = ORIENTED_EDGE('',*,*,#26673,.T.) ;
#36734 = ORIENTED_EDGE('',*,*,#26674,.F.) ;
#36735 = ORIENTED_EDGE('',*,*,#26675,.T.) ;
#36736 = ORIENTED_EDGE('',*,*,#26676,.F.) ;
#36737 = ORIENTED_EDGE('',*,*,#26677,.T.) ;
#36738 = ORIENTED_EDGE('',*,*,#26678,.F.) ;
#36739 = ORIENTED_EDGE('',*,*,#26679,.T.) ;
#36740 = ORIENTED_EDGE('',*,*,#26680,.F.) ;
#36741 = ORIENTED_EDGE('',*,*,#26681,.T.) ;
#36742 = ORIENTED_EDGE('',*,*,#26682,.F.) ;
#36743 = ORIENTED_EDGE('',*,*,#26683,.T.) ;
#36744 = ORIENTED_EDGE('',*,*,#26684,.F.) ;
#36745 = ORIENTED_EDGE('',*,*,#26624,.F.) ;
#36746 = ORIENTED_EDGE('',*,*,#26685,.T.) ;
#36747 = ORIENTED_EDGE('',*,*,#26686,.F.) ;
#36748 = ORIENTED_EDGE('',*,*,#26625,.T.) ;
#36749 = ORIENTED_EDGE('',*,*,#26618,.F.) ;
#36750 = ORIENTED_EDGE('',*,*,#26687,.F.) ;
#36751 = ORIENTED_EDGE('',*,*,#26688,.F.) ;
#36752 = ORIENTED_EDGE('',*,*,#26685,.F.) ;
#36753 = ORIENTED_EDGE('',*,*,#26623,.F.) ;
#36754 = ORIENTED_EDGE('',*,*,#26689,.T.) ;
#36755 = ORIENTED_EDGE('',*,*,#26690,.F.) ;
#36756 = ORIENTED_EDGE('',*,*,#26687,.T.) ;
#36757 = ORIENTED_EDGE('',*,*,#26620,.F.) ;
#36758 = ORIENTED_EDGE('',*,*,#26691,.T.) ;
#36759 = ORIENTED_EDGE('',*,*,#26692,.T.) ;
#36760 = ORIENTED_EDGE('',*,*,#26693,.T.) ;
#36761 = ORIENTED_EDGE('',*,*,#26694,.T.) ;
#36762 = ORIENTED_EDGE('',*,*,#26695,.T.) ;
#36763 = ORIENTED_EDGE('',*,*,#26696,.T.) ;
#36764 = ORIENTED_EDGE('',*,*,#26697,.T.) ;
#36765 = ORIENTED_EDGE('',*,*,#26698,.T.) ;
#36766 = ORIENTED_EDGE('',*,*,#26699,.F.) ;
#36767 = ORIENTED_EDGE('',*,*,#26700,.F.) ;
#36768 = ORIENTED_EDGE('',*,*,#26701,.F.) ;
#36769 = ORIENTED_EDGE('',*,*,#26702,.F.) ;
#36770 = ORIENTED_EDGE('',*,*,#26703,.F.) ;
#36771 = ORIENTED_EDGE('',*,*,#26704,.F.) ;
#36772 = ORIENTED_EDGE('',*,*,#26705,.F.) ;
#36773 = ORIENTED_EDGE('',*,*,#26706,.F.) ;
#36774 = ORIENTED_EDGE('',*,*,#26707,.F.) ;
#36775 = ORIENTED_EDGE('',*,*,#26708,.F.) ;
#36776 = ORIENTED_EDGE('',*,*,#26709,.F.) ;
#36777 = ORIENTED_EDGE('',*,*,#26710,.F.) ;
#36778 = ORIENTED_EDGE('',*,*,#26711,.T.) ;
#36779 = ORIENTED_EDGE('',*,*,#26712,.T.) ;
#36780 = ORIENTED_EDGE('',*,*,#26713,.F.) ;
#36781 = ORIENTED_EDGE('',*,*,#26689,.F.) ;
#36782 = ORIENTED_EDGE('',*,*,#26714,.T.) ;
#36783 = ORIENTED_EDGE('',*,*,#26715,.T.) ;
#36784 = ORIENTED_EDGE('',*,*,#26716,.T.) ;
#36785 = ORIENTED_EDGE('',*,*,#26717,.T.) ;
#36786 = ORIENTED_EDGE('',*,*,#26718,.T.) ;
#36787 = ORIENTED_EDGE('',*,*,#26719,.T.) ;
#36788 = ORIENTED_EDGE('',*,*,#26720,.T.) ;
#36789 = ORIENTED_EDGE('',*,*,#26721,.T.) ;
#36790 = ORIENTED_EDGE('',*,*,#26722,.T.) ;
#36791 = ORIENTED_EDGE('',*,*,#26723,.T.) ;
#36792 = ORIENTED_EDGE('',*,*,#26724,.T.) ;
#36793 = ORIENTED_EDGE('',*,*,#26699,.T.) ;
#36794 = ORIENTED_EDGE('',*,*,#26725,.T.) ;
#36795 = ORIENTED_EDGE('',*,*,#26640,.T.) ;
#36796 = ORIENTED_EDGE('',*,*,#26726,.T.) ;
#36797 = ORIENTED_EDGE('',*,*,#26727,.T.) ;
#36798 = ORIENTED_EDGE('',*,*,#26723,.F.) ;
#36799 = ORIENTED_EDGE('',*,*,#26728,.F.) ;
#36800 = ORIENTED_EDGE('',*,*,#26727,.F.) ;
#36801 = ORIENTED_EDGE('',*,*,#26729,.T.) ;
#36802 = ORIENTED_EDGE('',*,*,#26730,.T.) ;
#36803 = ORIENTED_EDGE('',*,*,#26703,.T.) ;
#36804 = ORIENTED_EDGE('',*,*,#26731,.T.) ;
#36805 = ORIENTED_EDGE('',*,*,#26732,.T.) ;
#36806 = ORIENTED_EDGE('',*,*,#26733,.T.) ;
#36807 = ORIENTED_EDGE('',*,*,#26734,.T.) ;
#36808 = ORIENTED_EDGE('',*,*,#26735,.T.) ;
#36809 = ORIENTED_EDGE('',*,*,#26636,.T.) ;
#36810 = ORIENTED_EDGE('',*,*,#26734,.F.) ;
#36811 = ORIENTED_EDGE('',*,*,#26736,.T.) ;
#36812 = ORIENTED_EDGE('',*,*,#26732,.F.) ;
#36813 = ORIENTED_EDGE('',*,*,#26737,.T.) ;
#36814 = ORIENTED_EDGE('',*,*,#26736,.F.) ;
#36815 = ORIENTED_EDGE('',*,*,#26738,.F.) ;
#36816 = ORIENTED_EDGE('',*,*,#26739,.F.) ;
#36817 = ORIENTED_EDGE('',*,*,#26740,.F.) ;
#36818 = ORIENTED_EDGE('',*,*,#26733,.F.) ;
#36819 = ORIENTED_EDGE('',*,*,#26635,.T.) ;
#36820 = ORIENTED_EDGE('',*,*,#26741,.F.) ;
#36821 = ORIENTED_EDGE('',*,*,#26738,.T.) ;
#36822 = ORIENTED_EDGE('',*,*,#26735,.F.) ;
#36823 = ORIENTED_EDGE('',*,*,#26742,.T.) ;
#36824 = ORIENTED_EDGE('',*,*,#26743,.F.) ;
#36825 = ORIENTED_EDGE('',*,*,#26637,.T.) ;
#36826 = ORIENTED_EDGE('',*,*,#26744,.T.) ;
#36827 = ORIENTED_EDGE('',*,*,#26701,.T.) ;
#36828 = ORIENTED_EDGE('',*,*,#26745,.T.) ;
#36829 = ORIENTED_EDGE('',*,*,#26746,.T.) ;
#36830 = ORIENTED_EDGE('',*,*,#26743,.T.) ;
#36831 = ORIENTED_EDGE('',*,*,#26747,.T.) ;
#36832 = ORIENTED_EDGE('',*,*,#26748,.T.) ;
#36833 = ORIENTED_EDGE('',*,*,#26638,.T.) ;
#36834 = ORIENTED_EDGE('',*,*,#26747,.F.) ;
#36835 = ORIENTED_EDGE('',*,*,#26749,.T.) ;
#36836 = ORIENTED_EDGE('',*,*,#26746,.F.) ;
#36837 = ORIENTED_EDGE('',*,*,#26750,.T.) ;
#36838 = ORIENTED_EDGE('',*,*,#26731,.F.) ;
#36839 = ORIENTED_EDGE('',*,*,#26702,.T.) ;
#36840 = ORIENTED_EDGE('',*,*,#26744,.F.) ;
#36841 = ORIENTED_EDGE('',*,*,#26751,.T.) ;
#36842 = ORIENTED_EDGE('',*,*,#26737,.F.) ;
#36843 = ORIENTED_EDGE('',*,*,#26751,.F.) ;
#36844 = ORIENTED_EDGE('',*,*,#26749,.F.) ;
#36845 = ORIENTED_EDGE('',*,*,#26742,.F.) ;
#36846 = ORIENTED_EDGE('',*,*,#26752,.T.) ;
#36847 = ORIENTED_EDGE('',*,*,#26705,.T.) ;
#36848 = ORIENTED_EDGE('',*,*,#26753,.T.) ;
#36849 = ORIENTED_EDGE('',*,*,#26754,.T.) ;
#36850 = ORIENTED_EDGE('',*,*,#26755,.T.) ;
#36851 = ORIENTED_EDGE('',*,*,#26756,.T.) ;
#36852 = ORIENTED_EDGE('',*,*,#26741,.T.) ;
#36853 = ORIENTED_EDGE('',*,*,#26634,.T.) ;
#36854 = ORIENTED_EDGE('',*,*,#26756,.F.) ;
#36855 = ORIENTED_EDGE('',*,*,#26757,.T.) ;
#36856 = ORIENTED_EDGE('',*,*,#26754,.F.) ;
#36857 = ORIENTED_EDGE('',*,*,#26739,.T.) ;
#36858 = ORIENTED_EDGE('',*,*,#26752,.F.) ;
#36859 = ORIENTED_EDGE('',*,*,#26758,.T.) ;
#36860 = ORIENTED_EDGE('',*,*,#26759,.F.) ;
#36861 = ORIENTED_EDGE('',*,*,#26706,.T.) ;
#36862 = ORIENTED_EDGE('',*,*,#26757,.F.) ;
#36863 = ORIENTED_EDGE('',*,*,#26760,.F.) ;
#36864 = ORIENTED_EDGE('',*,*,#26761,.F.) ;
#36865 = ORIENTED_EDGE('',*,*,#26758,.F.) ;
#36866 = ORIENTED_EDGE('',*,*,#26755,.F.) ;
#36867 = ORIENTED_EDGE('',*,*,#26633,.T.) ;
#36868 = ORIENTED_EDGE('',*,*,#26762,.F.) ;
#36869 = ORIENTED_EDGE('',*,*,#26760,.T.) ;
#36870 = ORIENTED_EDGE('',*,*,#26763,.T.) ;
#36871 = ORIENTED_EDGE('',*,*,#26764,.T.) ;
#36872 = ORIENTED_EDGE('',*,*,#26765,.T.) ;
#36873 = ORIENTED_EDGE('',*,*,#26766,.T.) ;
#36874 = ORIENTED_EDGE('',*,*,#26767,.T.) ;
#36875 = ORIENTED_EDGE('',*,*,#26763,.F.) ;
#36876 = ORIENTED_EDGE('',*,*,#26768,.T.) ;
#36877 = ORIENTED_EDGE('',*,*,#26769,.T.) ;
#36878 = ORIENTED_EDGE('',*,*,#26770,.T.) ;
#36879 = ORIENTED_EDGE('',*,*,#26769,.F.) ;
#36880 = ORIENTED_EDGE('',*,*,#26771,.T.) ;
#36881 = ORIENTED_EDGE('',*,*,#26772,.T.) ;
#36882 = ORIENTED_EDGE('',*,*,#26773,.T.) ;
#36883 = ORIENTED_EDGE('',*,*,#26774,.T.) ;
#36884 = ORIENTED_EDGE('',*,*,#26768,.F.) ;
#36885 = ORIENTED_EDGE('',*,*,#26775,.F.) ;
#36886 = ORIENTED_EDGE('',*,*,#26776,.T.) ;
#36887 = ORIENTED_EDGE('',*,*,#26777,.F.) ;
#36888 = ORIENTED_EDGE('',*,*,#26766,.F.) ;
#36889 = ORIENTED_EDGE('',*,*,#26630,.T.) ;
#36890 = ORIENTED_EDGE('',*,*,#26778,.T.) ;
#36891 = ORIENTED_EDGE('',*,*,#26775,.T.) ;
#36892 = ORIENTED_EDGE('',*,*,#26767,.F.) ;
#36893 = ORIENTED_EDGE('',*,*,#26764,.F.) ;
#36894 = ORIENTED_EDGE('',*,*,#26779,.T.) ;
#36895 = ORIENTED_EDGE('',*,*,#26780,.F.) ;
#36896 = ORIENTED_EDGE('',*,*,#26631,.T.) ;
#36897 = ORIENTED_EDGE('',*,*,#26765,.F.) ;
#36898 = ORIENTED_EDGE('',*,*,#26781,.T.) ;
#36899 = ORIENTED_EDGE('',*,*,#26707,.T.) ;
#36900 = ORIENTED_EDGE('',*,*,#26759,.T.) ;
#36901 = ORIENTED_EDGE('',*,*,#26782,.T.) ;
#36902 = ORIENTED_EDGE('',*,*,#26780,.T.) ;
#36903 = ORIENTED_EDGE('',*,*,#26783,.T.) ;
#36904 = ORIENTED_EDGE('',*,*,#26762,.T.) ;
#36905 = ORIENTED_EDGE('',*,*,#26632,.T.) ;
#36906 = ORIENTED_EDGE('',*,*,#26783,.F.) ;
#36907 = ORIENTED_EDGE('',*,*,#26784,.T.) ;
#36908 = ORIENTED_EDGE('',*,*,#26782,.F.) ;
#36909 = ORIENTED_EDGE('',*,*,#26761,.T.) ;
#36910 = ORIENTED_EDGE('',*,*,#26773,.F.) ;
#36911 = ORIENTED_EDGE('',*,*,#26708,.T.) ;
#36912 = ORIENTED_EDGE('',*,*,#26781,.F.) ;
#36913 = ORIENTED_EDGE('',*,*,#26785,.T.) ;
#36914 = ORIENTED_EDGE('',*,*,#26774,.F.) ;
#36915 = ORIENTED_EDGE('',*,*,#26770,.F.) ;
#36916 = ORIENTED_EDGE('',*,*,#26785,.F.) ;
#36917 = ORIENTED_EDGE('',*,*,#26784,.F.) ;
#36918 = ORIENTED_EDGE('',*,*,#26779,.F.) ;
#36919 = ORIENTED_EDGE('',*,*,#26786,.T.) ;
#36920 = ORIENTED_EDGE('',*,*,#26649,.T.) ;
#36921 = ORIENTED_EDGE('',*,*,#26787,.T.) ;
#36922 = ORIENTED_EDGE('',*,*,#26788,.T.) ;
#36923 = ORIENTED_EDGE('',*,*,#26789,.T.) ;
#36924 = ORIENTED_EDGE('',*,*,#26790,.T.) ;
#36925 = ORIENTED_EDGE('',*,*,#26787,.F.) ;
#36926 = ORIENTED_EDGE('',*,*,#26652,.T.) ;
#36927 = ORIENTED_EDGE('',*,*,#26791,.T.) ;
#36928 = ORIENTED_EDGE('',*,*,#26792,.T.) ;
#36929 = ORIENTED_EDGE('',*,*,#26789,.F.) ;
#36930 = ORIENTED_EDGE('',*,*,#26651,.T.) ;
#36931 = ORIENTED_EDGE('',*,*,#26786,.F.) ;
#36932 = ORIENTED_EDGE('',*,*,#26793,.T.) ;
#36933 = ORIENTED_EDGE('',*,*,#26791,.F.) ;
#36934 = ORIENTED_EDGE('',*,*,#26650,.T.) ;
#36935 = ORIENTED_EDGE('',*,*,#26793,.F.) ;
#36936 = ORIENTED_EDGE('',*,*,#26794,.T.) ;
#36937 = ORIENTED_EDGE('',*,*,#26714,.F.) ;
#36938 = ORIENTED_EDGE('',*,*,#26795,.F.) ;
#36939 = ORIENTED_EDGE('',*,*,#26788,.F.) ;
#36940 = ORIENTED_EDGE('',*,*,#26796,.T.) ;
#36941 = ORIENTED_EDGE('',*,*,#26715,.F.) ;
#36942 = ORIENTED_EDGE('',*,*,#26794,.F.) ;
#36943 = ORIENTED_EDGE('',*,*,#26797,.T.) ;
#36944 = ORIENTED_EDGE('',*,*,#26626,.T.) ;
#36945 = ORIENTED_EDGE('',*,*,#26686,.T.) ;
#36946 = ORIENTED_EDGE('',*,*,#26798,.T.) ;
#36947 = ORIENTED_EDGE('',*,*,#26799,.T.) ;
#36948 = ORIENTED_EDGE('',*,*,#26799,.F.) ;
#36949 = ORIENTED_EDGE('',*,*,#26800,.T.) ;
#36950 = ORIENTED_EDGE('',*,*,#26801,.F.) ;
#36951 = ORIENTED_EDGE('',*,*,#26802,.F.) ;
#36952 = ORIENTED_EDGE('',*,*,#26798,.F.) ;
#36953 = ORIENTED_EDGE('',*,*,#26688,.T.) ;
#36954 = ORIENTED_EDGE('',*,*,#26803,.F.) ;
#36955 = ORIENTED_EDGE('',*,*,#26800,.F.) ;
#36956 = ORIENTED_EDGE('',*,*,#26612,.F.) ;
#36957 = ORIENTED_EDGE('',*,*,#26804,.T.) ;
#36958 = ORIENTED_EDGE('',*,*,#26622,.F.) ;
#36959 = ORIENTED_EDGE('',*,*,#26616,.F.) ;
#36960 = ORIENTED_EDGE('',*,*,#26801,.T.) ;
#36961 = ORIENTED_EDGE('',*,*,#26803,.T.) ;
#36962 = ORIENTED_EDGE('',*,*,#26690,.T.) ;
#36963 = ORIENTED_EDGE('',*,*,#26713,.T.) ;
#36964 = ORIENTED_EDGE('',*,*,#26805,.T.) ;
#36965 = ORIENTED_EDGE('',*,*,#26797,.F.) ;
#36966 = ORIENTED_EDGE('',*,*,#26802,.T.) ;
#36967 = ORIENTED_EDGE('',*,*,#26805,.F.) ;
#36968 = ORIENTED_EDGE('',*,*,#26712,.F.) ;
#36969 = ORIENTED_EDGE('',*,*,#26806,.F.) ;
#36970 = ORIENTED_EDGE('',*,*,#26627,.T.) ;
#36971 = ORIENTED_EDGE('',*,*,#26807,.T.) ;
#36972 = ORIENTED_EDGE('',*,*,#26808,.T.) ;
#36973 = ORIENTED_EDGE('',*,*,#26710,.T.) ;
#36974 = ORIENTED_EDGE('',*,*,#26809,.T.) ;
#36975 = ORIENTED_EDGE('',*,*,#26771,.F.) ;
#36976 = ORIENTED_EDGE('',*,*,#26777,.T.) ;
#36977 = ORIENTED_EDGE('',*,*,#26809,.F.) ;
#36978 = ORIENTED_EDGE('',*,*,#26709,.T.) ;
#36979 = ORIENTED_EDGE('',*,*,#26772,.F.) ;
#36980 = ORIENTED_EDGE('',*,*,#26730,.F.) ;
#36981 = ORIENTED_EDGE('',*,*,#26740,.T.) ;
#36982 = ORIENTED_EDGE('',*,*,#26753,.F.) ;
#36983 = ORIENTED_EDGE('',*,*,#26704,.T.) ;
#36984 = ORIENTED_EDGE('',*,*,#26745,.F.) ;
#36985 = ORIENTED_EDGE('',*,*,#26700,.T.) ;
#36986 = ORIENTED_EDGE('',*,*,#26724,.F.) ;
#36987 = ORIENTED_EDGE('',*,*,#26810,.T.) ;
#36988 = ORIENTED_EDGE('',*,*,#26808,.F.) ;
#36989 = ORIENTED_EDGE('',*,*,#26811,.F.) ;
#36990 = ORIENTED_EDGE('',*,*,#26812,.F.) ;
#36991 = ORIENTED_EDGE('',*,*,#26628,.T.) ;
#36992 = ORIENTED_EDGE('',*,*,#26806,.T.) ;
#36993 = ORIENTED_EDGE('',*,*,#26711,.F.) ;
#36994 = ORIENTED_EDGE('',*,*,#26807,.F.) ;
#36995 = ORIENTED_EDGE('',*,*,#26776,.F.) ;
#36996 = ORIENTED_EDGE('',*,*,#26813,.F.) ;
#36997 = ORIENTED_EDGE('',*,*,#26811,.T.) ;
#36998 = ORIENTED_EDGE('',*,*,#26750,.F.) ;
#36999 = ORIENTED_EDGE('',*,*,#26810,.F.) ;
#37000 = ORIENTED_EDGE('',*,*,#26729,.F.) ;
#37001 = ORIENTED_EDGE('',*,*,#26814,.F.) ;
#37002 = ORIENTED_EDGE('',*,*,#26748,.F.) ;
#37003 = ORIENTED_EDGE('',*,*,#26814,.T.) ;
#37004 = ORIENTED_EDGE('',*,*,#26726,.F.) ;
#37005 = ORIENTED_EDGE('',*,*,#26639,.T.) ;
#37006 = ORIENTED_EDGE('',*,*,#26629,.T.) ;
#37007 = ORIENTED_EDGE('',*,*,#26812,.T.) ;
#37008 = ORIENTED_EDGE('',*,*,#26813,.T.) ;
#37009 = ORIENTED_EDGE('',*,*,#26778,.F.) ;
#37010 = ORIENTED_EDGE('',*,*,#26815,.T.) ;
#37011 = ORIENTED_EDGE('',*,*,#26816,.T.) ;
#37012 = ORIENTED_EDGE('',*,*,#26680,.T.) ;
#37013 = ORIENTED_EDGE('',*,*,#26817,.T.) ;
#37014 = ORIENTED_EDGE('',*,*,#26818,.T.) ;
#37015 = ORIENTED_EDGE('',*,*,#26819,.T.) ;
#37016 = ORIENTED_EDGE('',*,*,#26815,.F.) ;
#37017 = ORIENTED_EDGE('',*,*,#26820,.T.) ;
#37018 = ORIENTED_EDGE('',*,*,#26678,.T.) ;
#37019 = ORIENTED_EDGE('',*,*,#26821,.T.) ;
#37020 = ORIENTED_EDGE('',*,*,#26818,.F.) ;
#37021 = ORIENTED_EDGE('',*,*,#26822,.T.) ;
#37022 = ORIENTED_EDGE('',*,*,#26822,.F.) ;
#37023 = ORIENTED_EDGE('',*,*,#26820,.F.) ;
#37024 = ORIENTED_EDGE('',*,*,#26817,.F.) ;
#37025 = ORIENTED_EDGE('',*,*,#26679,.F.) ;
#37026 = ORIENTED_EDGE('',*,*,#26823,.T.) ;
#37027 = ORIENTED_EDGE('',*,*,#26824,.T.) ;
#37028 = ORIENTED_EDGE('',*,*,#26684,.T.) ;
#37029 = ORIENTED_EDGE('',*,*,#26825,.T.) ;
#37030 = ORIENTED_EDGE('',*,*,#26826,.T.) ;
#37031 = ORIENTED_EDGE('',*,*,#26827,.T.) ;
#37032 = ORIENTED_EDGE('',*,*,#26823,.F.) ;
#37033 = ORIENTED_EDGE('',*,*,#26828,.T.) ;
#37034 = ORIENTED_EDGE('',*,*,#26682,.T.) ;
#37035 = ORIENTED_EDGE('',*,*,#26829,.T.) ;
#37036 = ORIENTED_EDGE('',*,*,#26826,.F.) ;
#37037 = ORIENTED_EDGE('',*,*,#26830,.T.) ;
#37038 = ORIENTED_EDGE('',*,*,#26830,.F.) ;
#37039 = ORIENTED_EDGE('',*,*,#26828,.F.) ;
#37040 = ORIENTED_EDGE('',*,*,#26825,.F.) ;
#37041 = ORIENTED_EDGE('',*,*,#26683,.F.) ;
#37042 = ORIENTED_EDGE('',*,*,#26831,.T.) ;
#37043 = ORIENTED_EDGE('',*,*,#26832,.T.) ;
#37044 = ORIENTED_EDGE('',*,*,#26668,.T.) ;
#37045 = ORIENTED_EDGE('',*,*,#26833,.T.) ;
#37046 = ORIENTED_EDGE('',*,*,#26834,.T.) ;
#37047 = ORIENTED_EDGE('',*,*,#26835,.T.) ;
#37048 = ORIENTED_EDGE('',*,*,#26831,.F.) ;
#37049 = ORIENTED_EDGE('',*,*,#26836,.T.) ;
#37050 = ORIENTED_EDGE('',*,*,#26666,.T.) ;
#37051 = ORIENTED_EDGE('',*,*,#26837,.T.) ;
#37052 = ORIENTED_EDGE('',*,*,#26834,.F.) ;
#37053 = ORIENTED_EDGE('',*,*,#26838,.T.) ;
#37054 = ORIENTED_EDGE('',*,*,#26838,.F.) ;
#37055 = ORIENTED_EDGE('',*,*,#26836,.F.) ;
#37056 = ORIENTED_EDGE('',*,*,#26833,.F.) ;
#37057 = ORIENTED_EDGE('',*,*,#26667,.F.) ;
#37058 = ORIENTED_EDGE('',*,*,#26839,.T.) ;
#37059 = ORIENTED_EDGE('',*,*,#26840,.T.) ;
#37060 = ORIENTED_EDGE('',*,*,#26664,.T.) ;
#37061 = ORIENTED_EDGE('',*,*,#26841,.T.) ;
#37062 = ORIENTED_EDGE('',*,*,#26842,.T.) ;
#37063 = ORIENTED_EDGE('',*,*,#26843,.T.) ;
#37064 = ORIENTED_EDGE('',*,*,#26839,.F.) ;
#37065 = ORIENTED_EDGE('',*,*,#26844,.T.) ;
#37066 = ORIENTED_EDGE('',*,*,#26662,.T.) ;
#37067 = ORIENTED_EDGE('',*,*,#26845,.T.) ;
#37068 = ORIENTED_EDGE('',*,*,#26842,.F.) ;
#37069 = ORIENTED_EDGE('',*,*,#26846,.T.) ;
#37070 = ORIENTED_EDGE('',*,*,#26846,.F.) ;
#37071 = ORIENTED_EDGE('',*,*,#26844,.F.) ;
#37072 = ORIENTED_EDGE('',*,*,#26841,.F.) ;
#37073 = ORIENTED_EDGE('',*,*,#26663,.F.) ;
#37074 = ORIENTED_EDGE('',*,*,#26847,.T.) ;
#37075 = ORIENTED_EDGE('',*,*,#26848,.T.) ;
#37076 = ORIENTED_EDGE('',*,*,#26676,.T.) ;
#37077 = ORIENTED_EDGE('',*,*,#26849,.T.) ;
#37078 = ORIENTED_EDGE('',*,*,#26850,.T.) ;
#37079 = ORIENTED_EDGE('',*,*,#26851,.T.) ;
#37080 = ORIENTED_EDGE('',*,*,#26847,.F.) ;
#37081 = ORIENTED_EDGE('',*,*,#26852,.T.) ;
#37082 = ORIENTED_EDGE('',*,*,#26674,.T.) ;
#37083 = ORIENTED_EDGE('',*,*,#26853,.T.) ;
#37084 = ORIENTED_EDGE('',*,*,#26850,.F.) ;
#37085 = ORIENTED_EDGE('',*,*,#26854,.T.) ;
#37086 = ORIENTED_EDGE('',*,*,#26854,.F.) ;
#37087 = ORIENTED_EDGE('',*,*,#26852,.F.) ;
#37088 = ORIENTED_EDGE('',*,*,#26849,.F.) ;
#37089 = ORIENTED_EDGE('',*,*,#26675,.F.) ;
#37090 = ORIENTED_EDGE('',*,*,#26855,.T.) ;
#37091 = ORIENTED_EDGE('',*,*,#26856,.T.) ;
#37092 = ORIENTED_EDGE('',*,*,#26672,.T.) ;
#37093 = ORIENTED_EDGE('',*,*,#26857,.T.) ;
#37094 = ORIENTED_EDGE('',*,*,#26858,.T.) ;
#37095 = ORIENTED_EDGE('',*,*,#26859,.T.) ;
#37096 = ORIENTED_EDGE('',*,*,#26855,.F.) ;
#37097 = ORIENTED_EDGE('',*,*,#26860,.T.) ;
#37098 = ORIENTED_EDGE('',*,*,#26670,.T.) ;
#37099 = ORIENTED_EDGE('',*,*,#26861,.T.) ;
#37100 = ORIENTED_EDGE('',*,*,#26858,.F.) ;
#37101 = ORIENTED_EDGE('',*,*,#26862,.T.) ;
#37102 = ORIENTED_EDGE('',*,*,#26862,.F.) ;
#37103 = ORIENTED_EDGE('',*,*,#26860,.F.) ;
#37104 = ORIENTED_EDGE('',*,*,#26857,.F.) ;
#37105 = ORIENTED_EDGE('',*,*,#26671,.F.) ;
#37106 = ORIENTED_EDGE('',*,*,#26863,.T.) ;
#37107 = ORIENTED_EDGE('',*,*,#26864,.T.) ;
#37108 = ORIENTED_EDGE('',*,*,#26653,.T.) ;
#37109 = ORIENTED_EDGE('',*,*,#26865,.T.) ;
#37110 = ORIENTED_EDGE('',*,*,#26866,.T.) ;
#37111 = ORIENTED_EDGE('',*,*,#26867,.T.) ;
#37112 = ORIENTED_EDGE('',*,*,#26863,.F.) ;
#37113 = ORIENTED_EDGE('',*,*,#26868,.T.) ;
#37114 = ORIENTED_EDGE('',*,*,#26659,.T.) ;
#37115 = ORIENTED_EDGE('',*,*,#26869,.T.) ;
#37116 = ORIENTED_EDGE('',*,*,#26866,.F.) ;
#37117 = ORIENTED_EDGE('',*,*,#26870,.T.) ;
#37118 = ORIENTED_EDGE('',*,*,#26870,.F.) ;
#37119 = ORIENTED_EDGE('',*,*,#26868,.F.) ;
#37120 = ORIENTED_EDGE('',*,*,#26865,.F.) ;
#37121 = ORIENTED_EDGE('',*,*,#26660,.T.) ;
#37122 = ORIENTED_EDGE('',*,*,#26871,.T.) ;
#37123 = ORIENTED_EDGE('',*,*,#26872,.T.) ;
#37124 = ORIENTED_EDGE('',*,*,#26657,.T.) ;
#37125 = ORIENTED_EDGE('',*,*,#26873,.T.) ;
#37126 = ORIENTED_EDGE('',*,*,#26874,.T.) ;
#37127 = ORIENTED_EDGE('',*,*,#26875,.T.) ;
#37128 = ORIENTED_EDGE('',*,*,#26871,.F.) ;
#37129 = ORIENTED_EDGE('',*,*,#26876,.T.) ;
#37130 = ORIENTED_EDGE('',*,*,#26655,.T.) ;
#37131 = ORIENTED_EDGE('',*,*,#26877,.T.) ;
#37132 = ORIENTED_EDGE('',*,*,#26874,.F.) ;
#37133 = ORIENTED_EDGE('',*,*,#26878,.T.) ;
#37134 = ORIENTED_EDGE('',*,*,#26878,.F.) ;
#37135 = ORIENTED_EDGE('',*,*,#26876,.F.) ;
#37136 = ORIENTED_EDGE('',*,*,#26873,.F.) ;
#37137 = ORIENTED_EDGE('',*,*,#26656,.T.) ;
#37138 = ORIENTED_EDGE('',*,*,#26869,.F.) ;
#37139 = ORIENTED_EDGE('',*,*,#26658,.T.) ;
#37140 = ORIENTED_EDGE('',*,*,#26872,.F.) ;
#37141 = ORIENTED_EDGE('',*,*,#26879,.T.) ;
#37142 = ORIENTED_EDGE('',*,*,#26867,.F.) ;
#37143 = ORIENTED_EDGE('',*,*,#26879,.F.) ;
#37144 = ORIENTED_EDGE('',*,*,#26875,.F.) ;
#37145 = ORIENTED_EDGE('',*,*,#26880,.F.) ;
#37146 = ORIENTED_EDGE('',*,*,#26864,.F.) ;
#37147 = ORIENTED_EDGE('',*,*,#26880,.T.) ;
#37148 = ORIENTED_EDGE('',*,*,#26877,.F.) ;
#37149 = ORIENTED_EDGE('',*,*,#26654,.T.) ;
#37150 = ORIENTED_EDGE('',*,*,#26853,.F.) ;
#37151 = ORIENTED_EDGE('',*,*,#26673,.F.) ;
#37152 = ORIENTED_EDGE('',*,*,#26856,.F.) ;
#37153 = ORIENTED_EDGE('',*,*,#26881,.T.) ;
#37154 = ORIENTED_EDGE('',*,*,#26851,.F.) ;
#37155 = ORIENTED_EDGE('',*,*,#26881,.F.) ;
#37156 = ORIENTED_EDGE('',*,*,#26859,.F.) ;
#37157 = ORIENTED_EDGE('',*,*,#26882,.F.) ;
#37158 = ORIENTED_EDGE('',*,*,#26848,.F.) ;
#37159 = ORIENTED_EDGE('',*,*,#26882,.T.) ;
#37160 = ORIENTED_EDGE('',*,*,#26861,.F.) ;
#37161 = ORIENTED_EDGE('',*,*,#26669,.F.) ;
#37162 = ORIENTED_EDGE('',*,*,#26832,.F.) ;
#37163 = ORIENTED_EDGE('',*,*,#26883,.T.) ;
#37164 = ORIENTED_EDGE('',*,*,#26845,.F.) ;
#37165 = ORIENTED_EDGE('',*,*,#26661,.F.) ;
#37166 = ORIENTED_EDGE('',*,*,#26835,.F.) ;
#37167 = ORIENTED_EDGE('',*,*,#26884,.F.) ;
#37168 = ORIENTED_EDGE('',*,*,#26843,.F.) ;
#37169 = ORIENTED_EDGE('',*,*,#26883,.F.) ;
#37170 = ORIENTED_EDGE('',*,*,#26837,.F.) ;
#37171 = ORIENTED_EDGE('',*,*,#26665,.F.) ;
#37172 = ORIENTED_EDGE('',*,*,#26840,.F.) ;
#37173 = ORIENTED_EDGE('',*,*,#26884,.T.) ;
#37174 = ORIENTED_EDGE('',*,*,#26816,.F.) ;
#37175 = ORIENTED_EDGE('',*,*,#26885,.T.) ;
#37176 = ORIENTED_EDGE('',*,*,#26829,.F.) ;
#37177 = ORIENTED_EDGE('',*,*,#26681,.F.) ;
#37178 = ORIENTED_EDGE('',*,*,#26819,.F.) ;
#37179 = ORIENTED_EDGE('',*,*,#26886,.F.) ;
#37180 = ORIENTED_EDGE('',*,*,#26827,.F.) ;
#37181 = ORIENTED_EDGE('',*,*,#26885,.F.) ;
#37182 = ORIENTED_EDGE('',*,*,#26821,.F.) ;
#37183 = ORIENTED_EDGE('',*,*,#26677,.F.) ;
#37184 = ORIENTED_EDGE('',*,*,#26824,.F.) ;
#37185 = ORIENTED_EDGE('',*,*,#26886,.T.) ;
#37186 = ORIENTED_EDGE('',*,*,#26887,.F.) ;
#37187 = ORIENTED_EDGE('',*,*,#26888,.F.) ;
#37188 = ORIENTED_EDGE('',*,*,#26889,.F.) ;
#37189 = ORIENTED_EDGE('',*,*,#26890,.F.) ;
#37190 = ORIENTED_EDGE('',*,*,#26890,.T.) ;
#37191 = ORIENTED_EDGE('',*,*,#26891,.T.) ;
#37192 = ORIENTED_EDGE('',*,*,#26719,.F.) ;
#37193 = ORIENTED_EDGE('',*,*,#26892,.F.) ;
#37194 = ORIENTED_EDGE('',*,*,#26889,.T.) ;
#37195 = ORIENTED_EDGE('',*,*,#26893,.T.) ;
#37196 = ORIENTED_EDGE('',*,*,#26720,.F.) ;
#37197 = ORIENTED_EDGE('',*,*,#26891,.F.) ;
#37198 = ORIENTED_EDGE('',*,*,#26611,.F.) ;
#37199 = ORIENTED_EDGE('',*,*,#26648,.F.) ;
#37200 = ORIENTED_EDGE('',*,*,#26894,.F.) ;
#37201 = ORIENTED_EDGE('',*,*,#26691,.F.) ;
#37202 = ORIENTED_EDGE('',*,*,#26619,.F.) ;
#37203 = ORIENTED_EDGE('',*,*,#26804,.F.) ;
#37204 = ORIENTED_EDGE('',*,*,#26894,.T.) ;
#37205 = ORIENTED_EDGE('',*,*,#26647,.F.) ;
#37206 = ORIENTED_EDGE('',*,*,#26895,.T.) ;
#37207 = ORIENTED_EDGE('',*,*,#26692,.F.) ;
#37208 = ORIENTED_EDGE('',*,*,#26792,.F.) ;
#37209 = ORIENTED_EDGE('',*,*,#26795,.T.) ;
#37210 = ORIENTED_EDGE('',*,*,#26717,.F.) ;
#37211 = ORIENTED_EDGE('',*,*,#26896,.F.) ;
#37212 = ORIENTED_EDGE('',*,*,#26790,.F.) ;
#37213 = ORIENTED_EDGE('',*,*,#26896,.T.) ;
#37214 = ORIENTED_EDGE('',*,*,#26716,.F.) ;
#37215 = ORIENTED_EDGE('',*,*,#26796,.F.) ;
#37216 = ORIENTED_EDGE('',*,*,#26888,.T.) ;
#37217 = ORIENTED_EDGE('',*,*,#26897,.T.) ;
#37218 = ORIENTED_EDGE('',*,*,#26721,.F.) ;
#37219 = ORIENTED_EDGE('',*,*,#26893,.F.) ;
#37220 = ORIENTED_EDGE('',*,*,#26887,.T.) ;
#37221 = ORIENTED_EDGE('',*,*,#26892,.T.) ;
#37222 = ORIENTED_EDGE('',*,*,#26718,.F.) ;
#37223 = ORIENTED_EDGE('',*,*,#26897,.F.) ;
#37224 = ORIENTED_EDGE('',*,*,#26722,.F.) ;
#37225 = ORIENTED_EDGE('',*,*,#26698,.F.) ;
#37226 = ORIENTED_EDGE('',*,*,#26898,.F.) ;
#37227 = ORIENTED_EDGE('',*,*,#26641,.T.) ;
#37228 = ORIENTED_EDGE('',*,*,#26725,.F.) ;
#37229 = ORIENTED_EDGE('',*,*,#26728,.T.) ;
#37230 = ORIENTED_EDGE('',*,*,#26642,.T.) ;
#37231 = ORIENTED_EDGE('',*,*,#26898,.T.) ;
#37232 = ORIENTED_EDGE('',*,*,#26697,.F.) ;
#37233 = ORIENTED_EDGE('',*,*,#26899,.F.) ;
#37234 = ORIENTED_EDGE('',*,*,#26643,.T.) ;
#37235 = ORIENTED_EDGE('',*,*,#26899,.T.) ;
#37236 = ORIENTED_EDGE('',*,*,#26696,.F.) ;
#37237 = ORIENTED_EDGE('',*,*,#26900,.F.) ;
#37238 = ORIENTED_EDGE('',*,*,#26644,.T.) ;
#37239 = ORIENTED_EDGE('',*,*,#26900,.T.) ;
#37240 = ORIENTED_EDGE('',*,*,#26695,.F.) ;
#37241 = ORIENTED_EDGE('',*,*,#26901,.F.) ;
#37242 = ORIENTED_EDGE('',*,*,#26645,.T.) ;
#37243 = ORIENTED_EDGE('',*,*,#26901,.T.) ;
#37244 = ORIENTED_EDGE('',*,*,#26694,.F.) ;
#37245 = ORIENTED_EDGE('',*,*,#26902,.F.) ;
#37246 = ORIENTED_EDGE('',*,*,#26646,.T.) ;
#37247 = ORIENTED_EDGE('',*,*,#26902,.T.) ;
#37248 = ORIENTED_EDGE('',*,*,#26693,.F.) ;
#37249 = ORIENTED_EDGE('',*,*,#26895,.F.) ;
#37250 = ORIENTED_EDGE('',*,*,#26903,.T.) ;
#37251 = ORIENTED_EDGE('',*,*,#26904,.T.) ;
#37252 = ORIENTED_EDGE('',*,*,#26905,.F.) ;
#37253 = ORIENTED_EDGE('',*,*,#26906,.F.) ;
#37254 = ORIENTED_EDGE('',*,*,#26907,.T.) ;
#37255 = ORIENTED_EDGE('',*,*,#26906,.T.) ;
#37256 = ORIENTED_EDGE('',*,*,#26908,.F.) ;
#37257 = ORIENTED_EDGE('',*,*,#26909,.F.) ;
#37258 = ORIENTED_EDGE('',*,*,#26910,.T.) ;
#37259 = ORIENTED_EDGE('',*,*,#26909,.T.) ;
#37260 = ORIENTED_EDGE('',*,*,#26911,.F.) ;
#37261 = ORIENTED_EDGE('',*,*,#26912,.F.) ;
#37262 = ORIENTED_EDGE('',*,*,#26913,.T.) ;
#37263 = ORIENTED_EDGE('',*,*,#26912,.T.) ;
#37264 = ORIENTED_EDGE('',*,*,#26914,.F.) ;
#37265 = ORIENTED_EDGE('',*,*,#26904,.F.) ;
#37266 = ORIENTED_EDGE('',*,*,#26914,.T.) ;
#37267 = ORIENTED_EDGE('',*,*,#26911,.T.) ;
#37268 = ORIENTED_EDGE('',*,*,#26908,.T.) ;
#37269 = ORIENTED_EDGE('',*,*,#26905,.T.) ;
#37270 = ORIENTED_EDGE('',*,*,#26913,.F.) ;
#37271 = ORIENTED_EDGE('',*,*,#26903,.F.) ;
#37272 = ORIENTED_EDGE('',*,*,#26907,.F.) ;
#37273 = ORIENTED_EDGE('',*,*,#26910,.F.) ;
#37274 = ORIENTED_EDGE('',*,*,#26915,.T.) ;
#37275 = ORIENTED_EDGE('',*,*,#26916,.T.) ;
#37276 = ORIENTED_EDGE('',*,*,#26917,.F.) ;
#37277 = ORIENTED_EDGE('',*,*,#26918,.F.) ;
#37278 = ORIENTED_EDGE('',*,*,#26916,.F.) ;
#37279 = ORIENTED_EDGE('',*,*,#26919,.T.) ;
#37280 = ORIENTED_EDGE('',*,*,#26915,.F.) ;
#37281 = ORIENTED_EDGE('',*,*,#26920,.T.) ;
#37282 = ORIENTED_EDGE('',*,*,#26921,.F.) ;
#37283 = ORIENTED_EDGE('',*,*,#26920,.F.) ;
#37284 = ORIENTED_EDGE('',*,*,#26919,.F.) ;
#37285 = ORIENTED_EDGE('',*,*,#26922,.F.) ;
#37286 = ORIENTED_EDGE('',*,*,#26923,.T.) ;
#37287 = ORIENTED_EDGE('',*,*,#26917,.T.) ;
#37288 = ORIENTED_EDGE('',*,*,#26918,.T.) ;
#37289 = ORIENTED_EDGE('',*,*,#26923,.F.) ;
#37290 = ORIENTED_EDGE('',*,*,#26922,.T.) ;
#37291 = ORIENTED_EDGE('',*,*,#26921,.T.) ;
#37292 = ORIENTED_EDGE('',*,*,#26924,.T.) ;
#37293 = ORIENTED_EDGE('',*,*,#26925,.T.) ;
#37294 = ORIENTED_EDGE('',*,*,#26926,.F.) ;
#37295 = ORIENTED_EDGE('',*,*,#26927,.F.) ;
#37296 = ORIENTED_EDGE('',*,*,#26925,.F.) ;
#37297 = ORIENTED_EDGE('',*,*,#26928,.T.) ;
#37298 = ORIENTED_EDGE('',*,*,#26924,.F.) ;
#37299 = ORIENTED_EDGE('',*,*,#26929,.T.) ;
#37300 = ORIENTED_EDGE('',*,*,#26930,.F.) ;
#37301 = ORIENTED_EDGE('',*,*,#26929,.F.) ;
#37302 = ORIENTED_EDGE('',*,*,#26928,.F.) ;
#37303 = ORIENTED_EDGE('',*,*,#26931,.F.) ;
#37304 = ORIENTED_EDGE('',*,*,#26932,.T.) ;
#37305 = ORIENTED_EDGE('',*,*,#26926,.T.) ;
#37306 = ORIENTED_EDGE('',*,*,#26927,.T.) ;
#37307 = ORIENTED_EDGE('',*,*,#26932,.F.) ;
#37308 = ORIENTED_EDGE('',*,*,#26931,.T.) ;
#37309 = ORIENTED_EDGE('',*,*,#26930,.T.) ;
#37310 = ORIENTED_EDGE('',*,*,#26933,.T.) ;
#37311 = ORIENTED_EDGE('',*,*,#26934,.T.) ;
#37312 = ORIENTED_EDGE('',*,*,#26935,.T.) ;
#37313 = ORIENTED_EDGE('',*,*,#26934,.F.) ;
#37314 = ORIENTED_EDGE('',*,*,#26933,.F.) ;
#37315 = ORIENTED_EDGE('',*,*,#26936,.T.) ;
#37316 = ORIENTED_EDGE('',*,*,#26937,.F.) ;
#37317 = ORIENTED_EDGE('',*,*,#26936,.F.) ;
#37318 = ORIENTED_EDGE('',*,*,#26938,.F.) ;
#37319 = ORIENTED_EDGE('',*,*,#26935,.F.) ;
#37320 = ORIENTED_EDGE('',*,*,#26939,.F.) ;
#37321 = ORIENTED_EDGE('',*,*,#26940,.T.) ;
#37322 = ORIENTED_EDGE('',*,*,#26938,.T.) ;
#37323 = ORIENTED_EDGE('',*,*,#26940,.F.) ;
#37324 = ORIENTED_EDGE('',*,*,#26939,.T.) ;
#37325 = ORIENTED_EDGE('',*,*,#26937,.T.) ;
#37326 = ORIENTED_EDGE('',*,*,#26941,.F.) ;
#37327 = ORIENTED_EDGE('',*,*,#26942,.F.) ;
#37328 = ORIENTED_EDGE('',*,*,#26943,.F.) ;
#37329 = ORIENTED_EDGE('',*,*,#26944,.T.) ;
#37330 = ORIENTED_EDGE('',*,*,#26945,.T.) ;
#37331 = ORIENTED_EDGE('',*,*,#26946,.T.) ;
#37332 = ORIENTED_EDGE('',*,*,#26947,.T.) ;
#37333 = ORIENTED_EDGE('',*,*,#26945,.F.) ;
#37334 = ORIENTED_EDGE('',*,*,#26948,.T.) ;
#37335 = ORIENTED_EDGE('',*,*,#26942,.T.) ;
#37336 = ORIENTED_EDGE('',*,*,#26949,.T.) ;
#37337 = ORIENTED_EDGE('',*,*,#26950,.F.) ;
#37338 = ORIENTED_EDGE('',*,*,#26951,.F.) ;
#37339 = ORIENTED_EDGE('',*,*,#26952,.F.) ;
#37340 = ORIENTED_EDGE('',*,*,#26953,.T.) ;
#37341 = ORIENTED_EDGE('',*,*,#26954,.T.) ;
#37342 = ORIENTED_EDGE('',*,*,#26955,.T.) ;
#37343 = ORIENTED_EDGE('',*,*,#26956,.T.) ;
#37344 = ORIENTED_EDGE('',*,*,#26957,.T.) ;
#37345 = ORIENTED_EDGE('',*,*,#26953,.F.) ;
#37346 = ORIENTED_EDGE('',*,*,#26958,.T.) ;
#37347 = ORIENTED_EDGE('',*,*,#26951,.T.) ;
#37348 = ORIENTED_EDGE('',*,*,#26959,.T.) ;
#37349 = ORIENTED_EDGE('',*,*,#26960,.F.) ;
#37350 = ORIENTED_EDGE('',*,*,#26961,.F.) ;
#37351 = ORIENTED_EDGE('',*,*,#26962,.F.) ;
#37352 = ORIENTED_EDGE('',*,*,#26963,.T.) ;
#37353 = ORIENTED_EDGE('',*,*,#26964,.T.) ;
#37354 = ORIENTED_EDGE('',*,*,#26965,.T.) ;
#37355 = ORIENTED_EDGE('',*,*,#26966,.T.) ;
#37356 = ORIENTED_EDGE('',*,*,#26964,.F.) ;
#37357 = ORIENTED_EDGE('',*,*,#26967,.T.) ;
#37358 = ORIENTED_EDGE('',*,*,#26961,.T.) ;
#37359 = ORIENTED_EDGE('',*,*,#26968,.T.) ;
#37360 = ORIENTED_EDGE('',*,*,#26941,.T.) ;
#37361 = ORIENTED_EDGE('',*,*,#26969,.T.) ;
#37362 = ORIENTED_EDGE('',*,*,#26962,.T.) ;
#37363 = ORIENTED_EDGE('',*,*,#26970,.T.) ;
#37364 = ORIENTED_EDGE('',*,*,#26971,.F.) ;
#37365 = ORIENTED_EDGE('',*,*,#26972,.F.) ;
#37366 = ORIENTED_EDGE('',*,*,#26973,.F.) ;
#37367 = ORIENTED_EDGE('',*,*,#26974,.T.) ;
#37368 = ORIENTED_EDGE('',*,*,#26975,.T.) ;
#37369 = ORIENTED_EDGE('',*,*,#26976,.T.) ;
#37370 = ORIENTED_EDGE('',*,*,#26977,.T.) ;
#37371 = ORIENTED_EDGE('',*,*,#26975,.F.) ;
#37372 = ORIENTED_EDGE('',*,*,#26978,.T.) ;
#37373 = ORIENTED_EDGE('',*,*,#26972,.T.) ;
#37374 = ORIENTED_EDGE('',*,*,#26979,.T.) ;
#37375 = ORIENTED_EDGE('',*,*,#26980,.F.) ;
#37376 = ORIENTED_EDGE('',*,*,#26981,.F.) ;
#37377 = ORIENTED_EDGE('',*,*,#26982,.F.) ;
#37378 = ORIENTED_EDGE('',*,*,#26983,.T.) ;
#37379 = ORIENTED_EDGE('',*,*,#26984,.T.) ;
#37380 = ORIENTED_EDGE('',*,*,#26985,.T.) ;
#37381 = ORIENTED_EDGE('',*,*,#26986,.T.) ;
#37382 = ORIENTED_EDGE('',*,*,#26987,.T.) ;
#37383 = ORIENTED_EDGE('',*,*,#26983,.F.) ;
#37384 = ORIENTED_EDGE('',*,*,#26988,.T.) ;
#37385 = ORIENTED_EDGE('',*,*,#26981,.T.) ;
#37386 = ORIENTED_EDGE('',*,*,#26989,.T.) ;
#37387 = ORIENTED_EDGE('',*,*,#26960,.T.) ;
#37388 = ORIENTED_EDGE('',*,*,#26990,.T.) ;
#37389 = ORIENTED_EDGE('',*,*,#26982,.T.) ;
#37390 = ORIENTED_EDGE('',*,*,#26991,.T.) ;
#37391 = ORIENTED_EDGE('',*,*,#26992,.F.) ;
#37392 = ORIENTED_EDGE('',*,*,#26993,.F.) ;
#37393 = ORIENTED_EDGE('',*,*,#26994,.F.) ;
#37394 = ORIENTED_EDGE('',*,*,#26995,.T.) ;
#37395 = ORIENTED_EDGE('',*,*,#26996,.T.) ;
#37396 = ORIENTED_EDGE('',*,*,#26997,.T.) ;
#37397 = ORIENTED_EDGE('',*,*,#26998,.T.) ;
#37398 = ORIENTED_EDGE('',*,*,#26996,.F.) ;
#37399 = ORIENTED_EDGE('',*,*,#26999,.T.) ;
#37400 = ORIENTED_EDGE('',*,*,#26993,.T.) ;
#37401 = ORIENTED_EDGE('',*,*,#27000,.T.) ;
#37402 = ORIENTED_EDGE('',*,*,#27001,.F.) ;
#37403 = ORIENTED_EDGE('',*,*,#27002,.F.) ;
#37404 = ORIENTED_EDGE('',*,*,#27003,.F.) ;
#37405 = ORIENTED_EDGE('',*,*,#27004,.T.) ;
#37406 = ORIENTED_EDGE('',*,*,#27005,.T.) ;
#37407 = ORIENTED_EDGE('',*,*,#27006,.T.) ;
#37408 = ORIENTED_EDGE('',*,*,#27007,.T.) ;
#37409 = ORIENTED_EDGE('',*,*,#27005,.F.) ;
#37410 = ORIENTED_EDGE('',*,*,#27008,.T.) ;
#37411 = ORIENTED_EDGE('',*,*,#27002,.T.) ;
#37412 = ORIENTED_EDGE('',*,*,#27009,.T.) ;
#37413 = ORIENTED_EDGE('',*,*,#26980,.T.) ;
#37414 = ORIENTED_EDGE('',*,*,#27010,.T.) ;
#37415 = ORIENTED_EDGE('',*,*,#27003,.T.) ;
#37416 = ORIENTED_EDGE('',*,*,#27011,.T.) ;
#37417 = ORIENTED_EDGE('',*,*,#27012,.F.) ;
#37418 = ORIENTED_EDGE('',*,*,#27013,.F.) ;
#37419 = ORIENTED_EDGE('',*,*,#27014,.F.) ;
#37420 = ORIENTED_EDGE('',*,*,#27015,.T.) ;
#37421 = ORIENTED_EDGE('',*,*,#27016,.T.) ;
#37422 = ORIENTED_EDGE('',*,*,#27017,.T.) ;
#37423 = ORIENTED_EDGE('',*,*,#27018,.T.) ;
#37424 = ORIENTED_EDGE('',*,*,#27019,.T.) ;
#37425 = ORIENTED_EDGE('',*,*,#27015,.F.) ;
#37426 = ORIENTED_EDGE('',*,*,#27020,.T.) ;
#37427 = ORIENTED_EDGE('',*,*,#27013,.T.) ;
#37428 = ORIENTED_EDGE('',*,*,#27021,.T.) ;
#37429 = ORIENTED_EDGE('',*,*,#27022,.F.) ;
#37430 = ORIENTED_EDGE('',*,*,#27023,.F.) ;
#37431 = ORIENTED_EDGE('',*,*,#27024,.F.) ;
#37432 = ORIENTED_EDGE('',*,*,#27025,.T.) ;
#37433 = ORIENTED_EDGE('',*,*,#27026,.T.) ;
#37434 = ORIENTED_EDGE('',*,*,#27027,.T.) ;
#37435 = ORIENTED_EDGE('',*,*,#27028,.T.) ;
#37436 = ORIENTED_EDGE('',*,*,#27026,.F.) ;
#37437 = ORIENTED_EDGE('',*,*,#27029,.T.) ;
#37438 = ORIENTED_EDGE('',*,*,#27023,.T.) ;
#37439 = ORIENTED_EDGE('',*,*,#27030,.T.) ;
#37440 = ORIENTED_EDGE('',*,*,#27001,.T.) ;
#37441 = ORIENTED_EDGE('',*,*,#27031,.T.) ;
#37442 = ORIENTED_EDGE('',*,*,#27024,.T.) ;
#37443 = ORIENTED_EDGE('',*,*,#27032,.T.) ;
#37444 = ORIENTED_EDGE('',*,*,#27033,.F.) ;
#37445 = ORIENTED_EDGE('',*,*,#27034,.F.) ;
#37446 = ORIENTED_EDGE('',*,*,#27035,.F.) ;
#37447 = ORIENTED_EDGE('',*,*,#27036,.T.) ;
#37448 = ORIENTED_EDGE('',*,*,#27037,.T.) ;
#37449 = ORIENTED_EDGE('',*,*,#27038,.T.) ;
#37450 = ORIENTED_EDGE('',*,*,#27039,.T.) ;
#37451 = ORIENTED_EDGE('',*,*,#27037,.F.) ;
#37452 = ORIENTED_EDGE('',*,*,#27040,.T.) ;
#37453 = ORIENTED_EDGE('',*,*,#27034,.T.) ;
#37454 = ORIENTED_EDGE('',*,*,#27041,.T.) ;
#37455 = ORIENTED_EDGE('',*,*,#27042,.F.) ;
#37456 = ORIENTED_EDGE('',*,*,#27043,.F.) ;
#37457 = ORIENTED_EDGE('',*,*,#27044,.F.) ;
#37458 = ORIENTED_EDGE('',*,*,#27045,.T.) ;
#37459 = ORIENTED_EDGE('',*,*,#27046,.T.) ;
#37460 = ORIENTED_EDGE('',*,*,#27047,.T.) ;
#37461 = ORIENTED_EDGE('',*,*,#27048,.T.) ;
#37462 = ORIENTED_EDGE('',*,*,#27049,.T.) ;
#37463 = ORIENTED_EDGE('',*,*,#27045,.F.) ;
#37464 = ORIENTED_EDGE('',*,*,#27050,.T.) ;
#37465 = ORIENTED_EDGE('',*,*,#27043,.T.) ;
#37466 = ORIENTED_EDGE('',*,*,#27051,.T.) ;
#37467 = ORIENTED_EDGE('',*,*,#27022,.T.) ;
#37468 = ORIENTED_EDGE('',*,*,#27052,.T.) ;
#37469 = ORIENTED_EDGE('',*,*,#27044,.T.) ;
#37470 = ORIENTED_EDGE('',*,*,#27053,.T.) ;
#37471 = ORIENTED_EDGE('',*,*,#27054,.F.) ;
#37472 = ORIENTED_EDGE('',*,*,#27055,.F.) ;
#37473 = ORIENTED_EDGE('',*,*,#27056,.F.) ;
#37474 = ORIENTED_EDGE('',*,*,#27057,.T.) ;
#37475 = ORIENTED_EDGE('',*,*,#27058,.T.) ;
#37476 = ORIENTED_EDGE('',*,*,#27059,.T.) ;
#37477 = ORIENTED_EDGE('',*,*,#27060,.T.) ;
#37478 = ORIENTED_EDGE('',*,*,#27058,.F.) ;
#37479 = ORIENTED_EDGE('',*,*,#27061,.T.) ;
#37480 = ORIENTED_EDGE('',*,*,#27055,.T.) ;
#37481 = ORIENTED_EDGE('',*,*,#27062,.T.) ;
#37482 = ORIENTED_EDGE('',*,*,#27042,.T.) ;
#37483 = ORIENTED_EDGE('',*,*,#27063,.T.) ;
#37484 = ORIENTED_EDGE('',*,*,#27056,.T.) ;
#37485 = ORIENTED_EDGE('',*,*,#27064,.T.) ;
#37486 = ORIENTED_EDGE('',*,*,#27054,.T.) ;
#37487 = ORIENTED_EDGE('',*,*,#27065,.T.) ;
#37488 = ORIENTED_EDGE('',*,*,#27035,.T.) ;
#37489 = ORIENTED_EDGE('',*,*,#27066,.T.) ;
#37490 = ORIENTED_EDGE('',*,*,#27033,.T.) ;
#37491 = ORIENTED_EDGE('',*,*,#27067,.T.) ;
#37492 = ORIENTED_EDGE('',*,*,#27014,.T.) ;
#37493 = ORIENTED_EDGE('',*,*,#27068,.T.) ;
#37494 = ORIENTED_EDGE('',*,*,#27012,.T.) ;
#37495 = ORIENTED_EDGE('',*,*,#27069,.T.) ;
#37496 = ORIENTED_EDGE('',*,*,#26994,.T.) ;
#37497 = ORIENTED_EDGE('',*,*,#27070,.T.) ;
#37498 = ORIENTED_EDGE('',*,*,#26992,.T.) ;
#37499 = ORIENTED_EDGE('',*,*,#27071,.T.) ;
#37500 = ORIENTED_EDGE('',*,*,#26973,.T.) ;
#37501 = ORIENTED_EDGE('',*,*,#27072,.T.) ;
#37502 = ORIENTED_EDGE('',*,*,#26971,.T.) ;
#37503 = ORIENTED_EDGE('',*,*,#27073,.T.) ;
#37504 = ORIENTED_EDGE('',*,*,#26952,.T.) ;
#37505 = ORIENTED_EDGE('',*,*,#27074,.T.) ;
#37506 = ORIENTED_EDGE('',*,*,#26950,.T.) ;
#37507 = ORIENTED_EDGE('',*,*,#27075,.T.) ;
#37508 = ORIENTED_EDGE('',*,*,#26943,.T.) ;
#37509 = ORIENTED_EDGE('',*,*,#27076,.T.) ;
#37510 = ORIENTED_EDGE('',*,*,#26949,.F.) ;
#37511 = ORIENTED_EDGE('',*,*,#26970,.F.) ;
#37512 = ORIENTED_EDGE('',*,*,#26967,.F.) ;
#37513 = ORIENTED_EDGE('',*,*,#27077,.F.) ;
#37514 = ORIENTED_EDGE('',*,*,#26968,.F.) ;
#37515 = ORIENTED_EDGE('',*,*,#26991,.F.) ;
#37516 = ORIENTED_EDGE('',*,*,#26988,.F.) ;
#37517 = ORIENTED_EDGE('',*,*,#27078,.F.) ;
#37518 = ORIENTED_EDGE('',*,*,#26965,.F.) ;
#37519 = ORIENTED_EDGE('',*,*,#27078,.T.) ;
#37520 = ORIENTED_EDGE('',*,*,#26987,.F.) ;
#37521 = ORIENTED_EDGE('',*,*,#26986,.F.) ;
#37522 = ORIENTED_EDGE('',*,*,#27079,.T.) ;
#37523 = ORIENTED_EDGE('',*,*,#26989,.F.) ;
#37524 = ORIENTED_EDGE('',*,*,#27011,.F.) ;
#37525 = ORIENTED_EDGE('',*,*,#27008,.F.) ;
#37526 = ORIENTED_EDGE('',*,*,#27080,.F.) ;
#37527 = ORIENTED_EDGE('',*,*,#26984,.F.) ;
#37528 = ORIENTED_EDGE('',*,*,#27080,.T.) ;
#37529 = ORIENTED_EDGE('',*,*,#27007,.F.) ;
#37530 = ORIENTED_EDGE('',*,*,#27081,.T.) ;
#37531 = ORIENTED_EDGE('',*,*,#26985,.F.) ;
#37532 = ORIENTED_EDGE('',*,*,#27009,.F.) ;
#37533 = ORIENTED_EDGE('',*,*,#27032,.F.) ;
#37534 = ORIENTED_EDGE('',*,*,#27029,.F.) ;
#37535 = ORIENTED_EDGE('',*,*,#27082,.F.) ;
#37536 = ORIENTED_EDGE('',*,*,#27006,.F.) ;
#37537 = ORIENTED_EDGE('',*,*,#27082,.T.) ;
#37538 = ORIENTED_EDGE('',*,*,#27028,.F.) ;
#37539 = ORIENTED_EDGE('',*,*,#27083,.T.) ;
#37540 = ORIENTED_EDGE('',*,*,#27030,.F.) ;
#37541 = ORIENTED_EDGE('',*,*,#27053,.F.) ;
#37542 = ORIENTED_EDGE('',*,*,#27050,.F.) ;
#37543 = ORIENTED_EDGE('',*,*,#27084,.F.) ;
#37544 = ORIENTED_EDGE('',*,*,#27027,.F.) ;
#37545 = ORIENTED_EDGE('',*,*,#27084,.T.) ;
#37546 = ORIENTED_EDGE('',*,*,#27049,.F.) ;
#37547 = ORIENTED_EDGE('',*,*,#27048,.F.) ;
#37548 = ORIENTED_EDGE('',*,*,#27085,.T.) ;
#37549 = ORIENTED_EDGE('',*,*,#27051,.F.) ;
#37550 = ORIENTED_EDGE('',*,*,#27064,.F.) ;
#37551 = ORIENTED_EDGE('',*,*,#27061,.F.) ;
#37552 = ORIENTED_EDGE('',*,*,#27086,.F.) ;
#37553 = ORIENTED_EDGE('',*,*,#27046,.F.) ;
#37554 = ORIENTED_EDGE('',*,*,#27086,.T.) ;
#37555 = ORIENTED_EDGE('',*,*,#27060,.F.) ;
#37556 = ORIENTED_EDGE('',*,*,#27087,.T.) ;
#37557 = ORIENTED_EDGE('',*,*,#27047,.F.) ;
#37558 = ORIENTED_EDGE('',*,*,#27088,.F.) ;
#37559 = ORIENTED_EDGE('',*,*,#27057,.F.) ;
#37560 = ORIENTED_EDGE('',*,*,#27063,.F.) ;
#37561 = ORIENTED_EDGE('',*,*,#27052,.F.) ;
#37562 = ORIENTED_EDGE('',*,*,#27025,.F.) ;
#37563 = ORIENTED_EDGE('',*,*,#27031,.F.) ;
#37564 = ORIENTED_EDGE('',*,*,#27004,.F.) ;
#37565 = ORIENTED_EDGE('',*,*,#27010,.F.) ;
#37566 = ORIENTED_EDGE('',*,*,#26990,.F.) ;
#37567 = ORIENTED_EDGE('',*,*,#26963,.F.) ;
#37568 = ORIENTED_EDGE('',*,*,#26969,.F.) ;
#37569 = ORIENTED_EDGE('',*,*,#26944,.F.) ;
#37570 = ORIENTED_EDGE('',*,*,#27075,.F.) ;
#37571 = ORIENTED_EDGE('',*,*,#27073,.F.) ;
#37572 = ORIENTED_EDGE('',*,*,#26974,.F.) ;
#37573 = ORIENTED_EDGE('',*,*,#27071,.F.) ;
#37574 = ORIENTED_EDGE('',*,*,#26995,.F.) ;
#37575 = ORIENTED_EDGE('',*,*,#27069,.F.) ;
#37576 = ORIENTED_EDGE('',*,*,#27067,.F.) ;
#37577 = ORIENTED_EDGE('',*,*,#27036,.F.) ;
#37578 = ORIENTED_EDGE('',*,*,#27065,.F.) ;
#37579 = ORIENTED_EDGE('',*,*,#27018,.F.) ;
#37580 = ORIENTED_EDGE('',*,*,#27089,.T.) ;
#37581 = ORIENTED_EDGE('',*,*,#27038,.F.) ;
#37582 = ORIENTED_EDGE('',*,*,#27090,.T.) ;
#37583 = ORIENTED_EDGE('',*,*,#27019,.F.) ;
#37584 = ORIENTED_EDGE('',*,*,#27039,.F.) ;
#37585 = ORIENTED_EDGE('',*,*,#27091,.T.) ;
#37586 = ORIENTED_EDGE('',*,*,#27059,.F.) ;
#37587 = ORIENTED_EDGE('',*,*,#27092,.T.) ;
#37588 = ORIENTED_EDGE('',*,*,#26946,.F.) ;
#37589 = ORIENTED_EDGE('',*,*,#27077,.T.) ;
#37590 = ORIENTED_EDGE('',*,*,#26966,.F.) ;
#37591 = ORIENTED_EDGE('',*,*,#27093,.T.) ;
#37592 = ORIENTED_EDGE('',*,*,#26947,.F.) ;
#37593 = ORIENTED_EDGE('',*,*,#27094,.T.) ;
#37594 = ORIENTED_EDGE('',*,*,#26955,.F.) ;
#37595 = ORIENTED_EDGE('',*,*,#26954,.F.) ;
#37596 = ORIENTED_EDGE('',*,*,#27095,.T.) ;
#37597 = ORIENTED_EDGE('',*,*,#26956,.F.) ;
#37598 = ORIENTED_EDGE('',*,*,#27096,.T.) ;
#37599 = ORIENTED_EDGE('',*,*,#26976,.F.) ;
#37600 = ORIENTED_EDGE('',*,*,#27097,.T.) ;
#37601 = ORIENTED_EDGE('',*,*,#26957,.F.) ;
#37602 = ORIENTED_EDGE('',*,*,#26977,.F.) ;
#37603 = ORIENTED_EDGE('',*,*,#27098,.T.) ;
#37604 = ORIENTED_EDGE('',*,*,#26997,.F.) ;
#37605 = ORIENTED_EDGE('',*,*,#27099,.T.) ;
#37606 = ORIENTED_EDGE('',*,*,#26998,.F.) ;
#37607 = ORIENTED_EDGE('',*,*,#27100,.T.) ;
#37608 = ORIENTED_EDGE('',*,*,#27017,.F.) ;
#37609 = ORIENTED_EDGE('',*,*,#27016,.F.) ;
#37610 = ORIENTED_EDGE('',*,*,#27101,.T.) ;
#37611 = ORIENTED_EDGE('',*,*,#26948,.F.) ;
#37612 = ORIENTED_EDGE('',*,*,#27095,.F.) ;
#37613 = ORIENTED_EDGE('',*,*,#26959,.F.) ;
#37614 = ORIENTED_EDGE('',*,*,#27076,.F.) ;
#37615 = ORIENTED_EDGE('',*,*,#26958,.F.) ;
#37616 = ORIENTED_EDGE('',*,*,#27097,.F.) ;
#37617 = ORIENTED_EDGE('',*,*,#26979,.F.) ;
#37618 = ORIENTED_EDGE('',*,*,#27074,.F.) ;
#37619 = ORIENTED_EDGE('',*,*,#26978,.F.) ;
#37620 = ORIENTED_EDGE('',*,*,#27099,.F.) ;
#37621 = ORIENTED_EDGE('',*,*,#27000,.F.) ;
#37622 = ORIENTED_EDGE('',*,*,#27072,.F.) ;
#37623 = ORIENTED_EDGE('',*,*,#26999,.F.) ;
#37624 = ORIENTED_EDGE('',*,*,#27101,.F.) ;
#37625 = ORIENTED_EDGE('',*,*,#27021,.F.) ;
#37626 = ORIENTED_EDGE('',*,*,#27070,.F.) ;
#37627 = ORIENTED_EDGE('',*,*,#27020,.F.) ;
#37628 = ORIENTED_EDGE('',*,*,#27090,.F.) ;
#37629 = ORIENTED_EDGE('',*,*,#27041,.F.) ;
#37630 = ORIENTED_EDGE('',*,*,#27068,.F.) ;
#37631 = ORIENTED_EDGE('',*,*,#27089,.F.) ;
#37632 = ORIENTED_EDGE('',*,*,#27100,.F.) ;
#37633 = ORIENTED_EDGE('',*,*,#27098,.F.) ;
#37634 = ORIENTED_EDGE('',*,*,#27096,.F.) ;
#37635 = ORIENTED_EDGE('',*,*,#27094,.F.) ;
#37636 = ORIENTED_EDGE('',*,*,#27093,.F.) ;
#37637 = ORIENTED_EDGE('',*,*,#27079,.F.) ;
#37638 = ORIENTED_EDGE('',*,*,#27081,.F.) ;
#37639 = ORIENTED_EDGE('',*,*,#27083,.F.) ;
#37640 = ORIENTED_EDGE('',*,*,#27085,.F.) ;
#37641 = ORIENTED_EDGE('',*,*,#27087,.F.) ;
#37642 = ORIENTED_EDGE('',*,*,#27091,.F.) ;
#37643 = ORIENTED_EDGE('',*,*,#27088,.T.) ;
#37644 = ORIENTED_EDGE('',*,*,#27102,.T.) ;
#37645 = ORIENTED_EDGE('',*,*,#27103,.T.) ;
#37646 = ORIENTED_EDGE('',*,*,#27102,.F.) ;
#37647 = ORIENTED_EDGE('',*,*,#27103,.F.) ;
#37648 = ORIENTED_EDGE('',*,*,#27104,.T.) ;
#37649 = ORIENTED_EDGE('',*,*,#27105,.F.) ;
#37650 = ORIENTED_EDGE('',*,*,#27106,.F.) ;
#37651 = ORIENTED_EDGE('',*,*,#27104,.F.) ;
#37652 = ORIENTED_EDGE('',*,*,#27107,.T.) ;
#37653 = ORIENTED_EDGE('',*,*,#27108,.T.) ;
#37654 = ORIENTED_EDGE('',*,*,#27105,.T.) ;
#37655 = ORIENTED_EDGE('',*,*,#27106,.T.) ;
#37656 = ORIENTED_EDGE('',*,*,#27108,.F.) ;
#37657 = ORIENTED_EDGE('',*,*,#27107,.F.) ;
#37658 = ORIENTED_EDGE('',*,*,#27040,.F.) ;
#37659 = ORIENTED_EDGE('',*,*,#27092,.F.) ;
#37660 = ORIENTED_EDGE('',*,*,#27062,.F.) ;
#37661 = ORIENTED_EDGE('',*,*,#27066,.F.) ;
#37662 = ORIENTED_EDGE('',*,*,#27109,.F.) ;
#37663 = ORIENTED_EDGE('',*,*,#27110,.F.) ;
#37664 = ORIENTED_EDGE('',*,*,#27111,.F.) ;
#37665 = ORIENTED_EDGE('',*,*,#27112,.F.) ;
#37666 = ORIENTED_EDGE('',*,*,#27113,.F.) ;
#37667 = ORIENTED_EDGE('',*,*,#27114,.F.) ;
#37668 = ORIENTED_EDGE('',*,*,#27115,.F.) ;
#37669 = ORIENTED_EDGE('',*,*,#27116,.F.) ;
#37670 = ORIENTED_EDGE('',*,*,#27117,.F.) ;
#37671 = ORIENTED_EDGE('',*,*,#27118,.T.) ;
#37672 = ORIENTED_EDGE('',*,*,#27116,.T.) ;
#37673 = ORIENTED_EDGE('',*,*,#27119,.T.) ;
#37674 = ORIENTED_EDGE('',*,*,#27120,.T.) ;
#37675 = ORIENTED_EDGE('',*,*,#27113,.T.) ;
#37676 = ORIENTED_EDGE('',*,*,#27121,.T.) ;
#37677 = ORIENTED_EDGE('',*,*,#27117,.T.) ;
#37678 = ORIENTED_EDGE('',*,*,#27122,.T.) ;
#37679 = ORIENTED_EDGE('',*,*,#27123,.F.) ;
#37680 = ORIENTED_EDGE('',*,*,#27124,.F.) ;
#37681 = ORIENTED_EDGE('',*,*,#27125,.F.) ;
#37682 = ORIENTED_EDGE('',*,*,#27126,.F.) ;
#37683 = ORIENTED_EDGE('',*,*,#27127,.F.) ;
#37684 = ORIENTED_EDGE('',*,*,#27128,.F.) ;
#37685 = ORIENTED_EDGE('',*,*,#27127,.T.) ;
#37686 = ORIENTED_EDGE('',*,*,#27129,.T.) ;
#37687 = ORIENTED_EDGE('',*,*,#27115,.T.) ;
#37688 = ORIENTED_EDGE('',*,*,#27130,.T.) ;
#37689 = ORIENTED_EDGE('',*,*,#27124,.T.) ;
#37690 = ORIENTED_EDGE('',*,*,#27131,.T.) ;
#37691 = ORIENTED_EDGE('',*,*,#27128,.T.) ;
#37692 = ORIENTED_EDGE('',*,*,#27132,.T.) ;
#37693 = ORIENTED_EDGE('',*,*,#27133,.T.) ;
#37694 = ORIENTED_EDGE('',*,*,#27134,.T.) ;
#37695 = ORIENTED_EDGE('',*,*,#27126,.T.) ;
#37696 = ORIENTED_EDGE('',*,*,#27135,.T.) ;
#37697 = ORIENTED_EDGE('',*,*,#27112,.T.) ;
#37698 = ORIENTED_EDGE('',*,*,#27136,.T.) ;
#37699 = ORIENTED_EDGE('',*,*,#27125,.T.) ;
#37700 = ORIENTED_EDGE('',*,*,#27137,.T.) ;
#37701 = ORIENTED_EDGE('',*,*,#27138,.T.) ;
#37702 = ORIENTED_EDGE('',*,*,#27123,.T.) ;
#37703 = ORIENTED_EDGE('',*,*,#27139,.T.) ;
#37704 = ORIENTED_EDGE('',*,*,#27140,.T.) ;
#37705 = ORIENTED_EDGE('',*,*,#27109,.T.) ;
#37706 = ORIENTED_EDGE('',*,*,#27141,.T.) ;
#37707 = ORIENTED_EDGE('',*,*,#27114,.T.) ;
#37708 = ORIENTED_EDGE('',*,*,#27142,.T.) ;
#37709 = ORIENTED_EDGE('',*,*,#27143,.T.) ;
#37710 = ORIENTED_EDGE('',*,*,#27111,.T.) ;
#37711 = ORIENTED_EDGE('',*,*,#27144,.T.) ;
#37712 = ORIENTED_EDGE('',*,*,#27140,.F.) ;
#37713 = ORIENTED_EDGE('',*,*,#27145,.T.) ;
#37714 = ORIENTED_EDGE('',*,*,#27110,.T.) ;
#37715 = ORIENTED_EDGE('',*,*,#27146,.T.) ;
#37716 = ORIENTED_EDGE('',*,*,#27120,.F.) ;
#37717 = ORIENTED_EDGE('',*,*,#27119,.F.) ;
#37718 = ORIENTED_EDGE('',*,*,#27129,.F.) ;
#37719 = ORIENTED_EDGE('',*,*,#27134,.F.) ;
#37720 = ORIENTED_EDGE('',*,*,#27147,.F.) ;
#37721 = ORIENTED_EDGE('',*,*,#27135,.F.) ;
#37722 = ORIENTED_EDGE('',*,*,#27131,.F.) ;
#37723 = ORIENTED_EDGE('',*,*,#27138,.F.) ;
#37724 = ORIENTED_EDGE('',*,*,#27148,.F.) ;
#37725 = ORIENTED_EDGE('',*,*,#27118,.F.) ;
#37726 = ORIENTED_EDGE('',*,*,#27146,.F.) ;
#37727 = ORIENTED_EDGE('',*,*,#27142,.F.) ;
#37728 = ORIENTED_EDGE('',*,*,#27122,.F.) ;
#37729 = ORIENTED_EDGE('',*,*,#27121,.F.) ;
#37730 = ORIENTED_EDGE('',*,*,#27137,.F.) ;
#37731 = ORIENTED_EDGE('',*,*,#27132,.F.) ;
#37732 = ORIENTED_EDGE('',*,*,#27130,.F.) ;
#37733 = ORIENTED_EDGE('',*,*,#27136,.F.) ;
#37734 = ORIENTED_EDGE('',*,*,#27141,.F.) ;
#37735 = ORIENTED_EDGE('',*,*,#27143,.F.) ;
#37736 = ORIENTED_EDGE('',*,*,#27139,.F.) ;
#37737 = ORIENTED_EDGE('',*,*,#27145,.F.) ;
#37738 = ORIENTED_EDGE('',*,*,#27147,.T.) ;
#37739 = ORIENTED_EDGE('',*,*,#27133,.F.) ;
#37740 = ORIENTED_EDGE('',*,*,#27148,.T.) ;
#37741 = ORIENTED_EDGE('',*,*,#27144,.F.) ;
#37742 = ORIENTED_EDGE('',*,*,#27149,.T.) ;
#37743 = ORIENTED_EDGE('',*,*,#27150,.T.) ;
#37744 = ORIENTED_EDGE('',*,*,#27151,.T.) ;
#37745 = ORIENTED_EDGE('',*,*,#27152,.T.) ;
#37746 = ORIENTED_EDGE('',*,*,#27150,.F.) ;
#37747 = ORIENTED_EDGE('',*,*,#27152,.F.) ;
#37748 = ORIENTED_EDGE('',*,*,#27153,.T.) ;
#37749 = ORIENTED_EDGE('',*,*,#27154,.F.) ;
#37750 = ORIENTED_EDGE('',*,*,#27155,.F.) ;
#37751 = ORIENTED_EDGE('',*,*,#27153,.F.) ;
#37752 = ORIENTED_EDGE('',*,*,#27151,.F.) ;
#37753 = ORIENTED_EDGE('',*,*,#27149,.F.) ;
#37754 = ORIENTED_EDGE('',*,*,#27156,.T.) ;
#37755 = ORIENTED_EDGE('',*,*,#27157,.T.) ;
#37756 = ORIENTED_EDGE('',*,*,#27158,.T.) ;
#37757 = ORIENTED_EDGE('',*,*,#27159,.F.) ;
#37758 = ORIENTED_EDGE('',*,*,#27160,.T.) ;
#37759 = ORIENTED_EDGE('',*,*,#27161,.T.) ;
#37760 = ORIENTED_EDGE('',*,*,#27162,.T.) ;
#37761 = ORIENTED_EDGE('',*,*,#27157,.F.) ;
#37762 = ORIENTED_EDGE('',*,*,#27163,.T.) ;
#37763 = ORIENTED_EDGE('',*,*,#27164,.T.) ;
#37764 = ORIENTED_EDGE('',*,*,#27165,.T.) ;
#37765 = ORIENTED_EDGE('',*,*,#27161,.F.) ;
#37766 = ORIENTED_EDGE('',*,*,#27166,.T.) ;
#37767 = ORIENTED_EDGE('',*,*,#27167,.T.) ;
#37768 = ORIENTED_EDGE('',*,*,#27168,.T.) ;
#37769 = ORIENTED_EDGE('',*,*,#27164,.F.) ;
#37770 = ORIENTED_EDGE('',*,*,#27169,.T.) ;
#37771 = ORIENTED_EDGE('',*,*,#27170,.T.) ;
#37772 = ORIENTED_EDGE('',*,*,#27171,.T.) ;
#37773 = ORIENTED_EDGE('',*,*,#27167,.F.) ;
#37774 = ORIENTED_EDGE('',*,*,#27172,.T.) ;
#37775 = ORIENTED_EDGE('',*,*,#27173,.T.) ;
#37776 = ORIENTED_EDGE('',*,*,#27174,.T.) ;
#37777 = ORIENTED_EDGE('',*,*,#27175,.T.) ;
#37778 = ORIENTED_EDGE('',*,*,#27176,.T.) ;
#37779 = ORIENTED_EDGE('',*,*,#27173,.F.) ;
#37780 = ORIENTED_EDGE('',*,*,#27177,.T.) ;
#37781 = ORIENTED_EDGE('',*,*,#27178,.T.) ;
#37782 = ORIENTED_EDGE('',*,*,#27179,.T.) ;
#37783 = ORIENTED_EDGE('',*,*,#27175,.F.) ;
#37784 = ORIENTED_EDGE('',*,*,#27180,.T.) ;
#37785 = ORIENTED_EDGE('',*,*,#27170,.F.) ;
#37786 = ORIENTED_EDGE('',*,*,#27181,.T.) ;
#37787 = ORIENTED_EDGE('',*,*,#27178,.F.) ;
#37788 = ORIENTED_EDGE('',*,*,#27182,.T.) ;
#37789 = ORIENTED_EDGE('',*,*,#27183,.T.) ;
#37790 = ORIENTED_EDGE('',*,*,#27184,.T.) ;
#37791 = ORIENTED_EDGE('',*,*,#27183,.F.) ;
#37792 = ORIENTED_EDGE('',*,*,#27185,.T.) ;
#37793 = ORIENTED_EDGE('',*,*,#27186,.T.) ;
#37794 = ORIENTED_EDGE('',*,*,#27187,.T.) ;
#37795 = ORIENTED_EDGE('',*,*,#27186,.F.) ;
#37796 = ORIENTED_EDGE('',*,*,#27188,.T.) ;
#37797 = ORIENTED_EDGE('',*,*,#27189,.T.) ;
#37798 = ORIENTED_EDGE('',*,*,#27190,.T.) ;
#37799 = ORIENTED_EDGE('',*,*,#27189,.F.) ;
#37800 = ORIENTED_EDGE('',*,*,#27191,.T.) ;
#37801 = ORIENTED_EDGE('',*,*,#27159,.T.) ;
#37802 = ORIENTED_EDGE('',*,*,#27162,.F.) ;
#37803 = ORIENTED_EDGE('',*,*,#27192,.T.) ;
#37804 = ORIENTED_EDGE('',*,*,#27193,.F.) ;
#37805 = ORIENTED_EDGE('',*,*,#27194,.F.) ;
#37806 = ORIENTED_EDGE('',*,*,#27165,.F.) ;
#37807 = ORIENTED_EDGE('',*,*,#27195,.T.) ;
#37808 = ORIENTED_EDGE('',*,*,#27196,.F.) ;
#37809 = ORIENTED_EDGE('',*,*,#27192,.F.) ;
#37810 = ORIENTED_EDGE('',*,*,#27168,.F.) ;
#37811 = ORIENTED_EDGE('',*,*,#27197,.T.) ;
#37812 = ORIENTED_EDGE('',*,*,#27198,.F.) ;
#37813 = ORIENTED_EDGE('',*,*,#27195,.F.) ;
#37814 = ORIENTED_EDGE('',*,*,#27171,.F.) ;
#37815 = ORIENTED_EDGE('',*,*,#27199,.T.) ;
#37816 = ORIENTED_EDGE('',*,*,#27200,.F.) ;
#37817 = ORIENTED_EDGE('',*,*,#27197,.F.) ;
#37818 = ORIENTED_EDGE('',*,*,#27180,.F.) ;
#37819 = ORIENTED_EDGE('',*,*,#27201,.T.) ;
#37820 = ORIENTED_EDGE('',*,*,#27202,.F.) ;
#37821 = ORIENTED_EDGE('',*,*,#27199,.F.) ;
#37822 = ORIENTED_EDGE('',*,*,#27174,.F.) ;
#37823 = ORIENTED_EDGE('',*,*,#27203,.T.) ;
#37824 = ORIENTED_EDGE('',*,*,#27204,.F.) ;
#37825 = ORIENTED_EDGE('',*,*,#27201,.F.) ;
#37826 = ORIENTED_EDGE('',*,*,#27205,.F.) ;
#37827 = ORIENTED_EDGE('',*,*,#27172,.F.) ;
#37828 = ORIENTED_EDGE('',*,*,#27179,.F.) ;
#37829 = ORIENTED_EDGE('',*,*,#27169,.F.) ;
#37830 = ORIENTED_EDGE('',*,*,#27166,.F.) ;
#37831 = ORIENTED_EDGE('',*,*,#27163,.F.) ;
#37832 = ORIENTED_EDGE('',*,*,#27160,.F.) ;
#37833 = ORIENTED_EDGE('',*,*,#27156,.F.) ;
#37834 = ORIENTED_EDGE('',*,*,#27191,.F.) ;
#37835 = ORIENTED_EDGE('',*,*,#27188,.F.) ;
#37836 = ORIENTED_EDGE('',*,*,#27185,.F.) ;
#37837 = ORIENTED_EDGE('',*,*,#27182,.F.) ;
#37838 = ORIENTED_EDGE('',*,*,#27177,.F.) ;
#37839 = ORIENTED_EDGE('',*,*,#27206,.T.) ;
#37840 = ORIENTED_EDGE('',*,*,#27207,.T.) ;
#37841 = ORIENTED_EDGE('',*,*,#27208,.T.) ;
#37842 = ORIENTED_EDGE('',*,*,#27209,.F.) ;
#37843 = ORIENTED_EDGE('',*,*,#27210,.T.) ;
#37844 = ORIENTED_EDGE('',*,*,#27211,.T.) ;
#37845 = ORIENTED_EDGE('',*,*,#27212,.T.) ;
#37846 = ORIENTED_EDGE('',*,*,#27207,.F.) ;
#37847 = ORIENTED_EDGE('',*,*,#27213,.T.) ;
#37848 = ORIENTED_EDGE('',*,*,#27214,.T.) ;
#37849 = ORIENTED_EDGE('',*,*,#27215,.T.) ;
#37850 = ORIENTED_EDGE('',*,*,#27211,.F.) ;
#37851 = ORIENTED_EDGE('',*,*,#27216,.T.) ;
#37852 = ORIENTED_EDGE('',*,*,#27217,.T.) ;
#37853 = ORIENTED_EDGE('',*,*,#27218,.T.) ;
#37854 = ORIENTED_EDGE('',*,*,#27214,.F.) ;
#37855 = ORIENTED_EDGE('',*,*,#27219,.T.) ;
#37856 = ORIENTED_EDGE('',*,*,#27220,.T.) ;
#37857 = ORIENTED_EDGE('',*,*,#27204,.T.) ;
#37858 = ORIENTED_EDGE('',*,*,#27217,.F.) ;
#37859 = ORIENTED_EDGE('',*,*,#27202,.T.) ;
#37860 = ORIENTED_EDGE('',*,*,#27220,.F.) ;
#37861 = ORIENTED_EDGE('',*,*,#27221,.T.) ;
#37862 = ORIENTED_EDGE('',*,*,#27222,.T.) ;
#37863 = ORIENTED_EDGE('',*,*,#27200,.T.) ;
#37864 = ORIENTED_EDGE('',*,*,#27222,.F.) ;
#37865 = ORIENTED_EDGE('',*,*,#27223,.T.) ;
#37866 = ORIENTED_EDGE('',*,*,#27224,.T.) ;
#37867 = ORIENTED_EDGE('',*,*,#27198,.T.) ;
#37868 = ORIENTED_EDGE('',*,*,#27224,.F.) ;
#37869 = ORIENTED_EDGE('',*,*,#27225,.T.) ;
#37870 = ORIENTED_EDGE('',*,*,#27226,.T.) ;
#37871 = ORIENTED_EDGE('',*,*,#27196,.T.) ;
#37872 = ORIENTED_EDGE('',*,*,#27226,.F.) ;
#37873 = ORIENTED_EDGE('',*,*,#27227,.T.) ;
#37874 = ORIENTED_EDGE('',*,*,#27228,.T.) ;
#37875 = ORIENTED_EDGE('',*,*,#27193,.T.) ;
#37876 = ORIENTED_EDGE('',*,*,#27228,.F.) ;
#37877 = ORIENTED_EDGE('',*,*,#27229,.T.) ;
#37878 = ORIENTED_EDGE('',*,*,#27230,.T.) ;
#37879 = ORIENTED_EDGE('',*,*,#27231,.T.) ;
#37880 = ORIENTED_EDGE('',*,*,#27230,.F.) ;
#37881 = ORIENTED_EDGE('',*,*,#27232,.T.) ;
#37882 = ORIENTED_EDGE('',*,*,#27233,.T.) ;
#37883 = ORIENTED_EDGE('',*,*,#27234,.T.) ;
#37884 = ORIENTED_EDGE('',*,*,#27233,.F.) ;
#37885 = ORIENTED_EDGE('',*,*,#27235,.T.) ;
#37886 = ORIENTED_EDGE('',*,*,#27209,.T.) ;
#37887 = ORIENTED_EDGE('',*,*,#27158,.F.) ;
#37888 = ORIENTED_EDGE('',*,*,#27194,.T.) ;
#37889 = ORIENTED_EDGE('',*,*,#27231,.F.) ;
#37890 = ORIENTED_EDGE('',*,*,#27236,.F.) ;
#37891 = ORIENTED_EDGE('',*,*,#27190,.F.) ;
#37892 = ORIENTED_EDGE('',*,*,#27236,.T.) ;
#37893 = ORIENTED_EDGE('',*,*,#27234,.F.) ;
#37894 = ORIENTED_EDGE('',*,*,#27237,.F.) ;
#37895 = ORIENTED_EDGE('',*,*,#27187,.F.) ;
#37896 = ORIENTED_EDGE('',*,*,#27237,.T.) ;
#37897 = ORIENTED_EDGE('',*,*,#27208,.F.) ;
#37898 = ORIENTED_EDGE('',*,*,#27238,.F.) ;
#37899 = ORIENTED_EDGE('',*,*,#27206,.F.) ;
#37900 = ORIENTED_EDGE('',*,*,#27235,.F.) ;
#37901 = ORIENTED_EDGE('',*,*,#27232,.F.) ;
#37902 = ORIENTED_EDGE('',*,*,#27229,.F.) ;
#37903 = ORIENTED_EDGE('',*,*,#27227,.F.) ;
#37904 = ORIENTED_EDGE('',*,*,#27225,.F.) ;
#37905 = ORIENTED_EDGE('',*,*,#27223,.F.) ;
#37906 = ORIENTED_EDGE('',*,*,#27221,.F.) ;
#37907 = ORIENTED_EDGE('',*,*,#27219,.F.) ;
#37908 = ORIENTED_EDGE('',*,*,#27216,.F.) ;
#37909 = ORIENTED_EDGE('',*,*,#27213,.F.) ;
#37910 = ORIENTED_EDGE('',*,*,#27210,.F.) ;
#37911 = ORIENTED_EDGE('',*,*,#27154,.T.) ;
#37912 = ORIENTED_EDGE('',*,*,#27155,.T.) ;
#37913 = ORIENTED_EDGE('',*,*,#27239,.T.) ;
#37914 = ORIENTED_EDGE('',*,*,#27205,.T.) ;
#37915 = ORIENTED_EDGE('',*,*,#27239,.F.) ;
#37916 = ORIENTED_EDGE('',*,*,#27184,.F.) ;
#37917 = ORIENTED_EDGE('',*,*,#27238,.T.) ;
#37918 = ORIENTED_EDGE('',*,*,#27212,.F.) ;
#37919 = ORIENTED_EDGE('',*,*,#27240,.F.) ;
#37920 = ORIENTED_EDGE('',*,*,#27181,.F.) ;
#37921 = ORIENTED_EDGE('',*,*,#27240,.T.) ;
#37922 = ORIENTED_EDGE('',*,*,#27215,.F.) ;
#37923 = ORIENTED_EDGE('',*,*,#27241,.F.) ;
#37924 = ORIENTED_EDGE('',*,*,#27176,.F.) ;
#37925 = ORIENTED_EDGE('',*,*,#27241,.T.) ;
#37926 = ORIENTED_EDGE('',*,*,#27218,.F.) ;
#37927 = ORIENTED_EDGE('',*,*,#27203,.F.) ;
#37928 = ORIENTED_EDGE('',*,*,#27242,.T.) ;
#37929 = ORIENTED_EDGE('',*,*,#27243,.T.) ;
#37930 = ORIENTED_EDGE('',*,*,#27244,.T.) ;
#37931 = ORIENTED_EDGE('',*,*,#27245,.F.) ;
#37932 = ORIENTED_EDGE('',*,*,#27246,.T.) ;
#37933 = ORIENTED_EDGE('',*,*,#27247,.T.) ;
#37934 = ORIENTED_EDGE('',*,*,#27248,.T.) ;
#37935 = ORIENTED_EDGE('',*,*,#27243,.F.) ;
#37936 = ORIENTED_EDGE('',*,*,#27249,.T.) ;
#37937 = ORIENTED_EDGE('',*,*,#27250,.T.) ;
#37938 = ORIENTED_EDGE('',*,*,#27251,.T.) ;
#37939 = ORIENTED_EDGE('',*,*,#27247,.F.) ;
#37940 = ORIENTED_EDGE('',*,*,#27252,.T.) ;
#37941 = ORIENTED_EDGE('',*,*,#27253,.T.) ;
#37942 = ORIENTED_EDGE('',*,*,#27254,.T.) ;
#37943 = ORIENTED_EDGE('',*,*,#27250,.F.) ;
#37944 = ORIENTED_EDGE('',*,*,#27255,.T.) ;
#37945 = ORIENTED_EDGE('',*,*,#27256,.T.) ;
#37946 = ORIENTED_EDGE('',*,*,#27257,.T.) ;
#37947 = ORIENTED_EDGE('',*,*,#27253,.F.) ;
#37948 = ORIENTED_EDGE('',*,*,#27258,.T.) ;
#37949 = ORIENTED_EDGE('',*,*,#27256,.F.) ;
#37950 = ORIENTED_EDGE('',*,*,#27259,.T.) ;
#37951 = ORIENTED_EDGE('',*,*,#27260,.T.) ;
#37952 = ORIENTED_EDGE('',*,*,#27261,.T.) ;
#37953 = ORIENTED_EDGE('',*,*,#27260,.F.) ;
#37954 = ORIENTED_EDGE('',*,*,#27262,.T.) ;
#37955 = ORIENTED_EDGE('',*,*,#27263,.T.) ;
#37956 = ORIENTED_EDGE('',*,*,#27264,.T.) ;
#37957 = ORIENTED_EDGE('',*,*,#27263,.F.) ;
#37958 = ORIENTED_EDGE('',*,*,#27265,.T.) ;
#37959 = ORIENTED_EDGE('',*,*,#27266,.T.) ;
#37960 = ORIENTED_EDGE('',*,*,#27267,.T.) ;
#37961 = ORIENTED_EDGE('',*,*,#27266,.F.) ;
#37962 = ORIENTED_EDGE('',*,*,#27268,.T.) ;
#37963 = ORIENTED_EDGE('',*,*,#27269,.T.) ;
#37964 = ORIENTED_EDGE('',*,*,#27270,.T.) ;
#37965 = ORIENTED_EDGE('',*,*,#27269,.F.) ;
#37966 = ORIENTED_EDGE('',*,*,#27271,.T.) ;
#37967 = ORIENTED_EDGE('',*,*,#27272,.T.) ;
#37968 = ORIENTED_EDGE('',*,*,#27273,.T.) ;
#37969 = ORIENTED_EDGE('',*,*,#27272,.F.) ;
#37970 = ORIENTED_EDGE('',*,*,#27274,.T.) ;
#37971 = ORIENTED_EDGE('',*,*,#27275,.T.) ;
#37972 = ORIENTED_EDGE('',*,*,#27276,.T.) ;
#37973 = ORIENTED_EDGE('',*,*,#27275,.F.) ;
#37974 = ORIENTED_EDGE('',*,*,#27277,.T.) ;
#37975 = ORIENTED_EDGE('',*,*,#27245,.T.) ;
#37976 = ORIENTED_EDGE('',*,*,#27264,.F.) ;
#37977 = ORIENTED_EDGE('',*,*,#27278,.F.) ;
#37978 = ORIENTED_EDGE('',*,*,#27279,.F.) ;
#37979 = ORIENTED_EDGE('',*,*,#27280,.T.) ;
#37980 = ORIENTED_EDGE('',*,*,#27267,.F.) ;
#37981 = ORIENTED_EDGE('',*,*,#27281,.F.) ;
#37982 = ORIENTED_EDGE('',*,*,#27282,.F.) ;
#37983 = ORIENTED_EDGE('',*,*,#27278,.T.) ;
#37984 = ORIENTED_EDGE('',*,*,#27270,.F.) ;
#37985 = ORIENTED_EDGE('',*,*,#27283,.F.) ;
#37986 = ORIENTED_EDGE('',*,*,#27284,.F.) ;
#37987 = ORIENTED_EDGE('',*,*,#27281,.T.) ;
#37988 = ORIENTED_EDGE('',*,*,#27273,.F.) ;
#37989 = ORIENTED_EDGE('',*,*,#27285,.F.) ;
#37990 = ORIENTED_EDGE('',*,*,#27286,.F.) ;
#37991 = ORIENTED_EDGE('',*,*,#27283,.T.) ;
#37992 = ORIENTED_EDGE('',*,*,#27276,.F.) ;
#37993 = ORIENTED_EDGE('',*,*,#27287,.F.) ;
#37994 = ORIENTED_EDGE('',*,*,#27288,.F.) ;
#37995 = ORIENTED_EDGE('',*,*,#27285,.T.) ;
#37996 = ORIENTED_EDGE('',*,*,#27244,.F.) ;
#37997 = ORIENTED_EDGE('',*,*,#27289,.F.) ;
#37998 = ORIENTED_EDGE('',*,*,#27290,.F.) ;
#37999 = ORIENTED_EDGE('',*,*,#27287,.T.) ;
#38000 = ORIENTED_EDGE('',*,*,#27242,.F.) ;
#38001 = ORIENTED_EDGE('',*,*,#27277,.F.) ;
#38002 = ORIENTED_EDGE('',*,*,#27274,.F.) ;
#38003 = ORIENTED_EDGE('',*,*,#27271,.F.) ;
#38004 = ORIENTED_EDGE('',*,*,#27268,.F.) ;
#38005 = ORIENTED_EDGE('',*,*,#27265,.F.) ;
#38006 = ORIENTED_EDGE('',*,*,#27262,.F.) ;
#38007 = ORIENTED_EDGE('',*,*,#27259,.F.) ;
#38008 = ORIENTED_EDGE('',*,*,#27255,.F.) ;
#38009 = ORIENTED_EDGE('',*,*,#27252,.F.) ;
#38010 = ORIENTED_EDGE('',*,*,#27249,.F.) ;
#38011 = ORIENTED_EDGE('',*,*,#27246,.F.) ;
#38012 = ORIENTED_EDGE('',*,*,#27291,.T.) ;
#38013 = ORIENTED_EDGE('',*,*,#27292,.T.) ;
#38014 = ORIENTED_EDGE('',*,*,#27293,.T.) ;
#38015 = ORIENTED_EDGE('',*,*,#27294,.T.) ;
#38016 = ORIENTED_EDGE('',*,*,#27292,.F.) ;
#38017 = ORIENTED_EDGE('',*,*,#27294,.F.) ;
#38018 = ORIENTED_EDGE('',*,*,#27295,.T.) ;
#38019 = ORIENTED_EDGE('',*,*,#27296,.F.) ;
#38020 = ORIENTED_EDGE('',*,*,#27297,.F.) ;
#38021 = ORIENTED_EDGE('',*,*,#27295,.F.) ;
#38022 = ORIENTED_EDGE('',*,*,#27293,.F.) ;
#38023 = ORIENTED_EDGE('',*,*,#27291,.F.) ;
#38024 = ORIENTED_EDGE('',*,*,#27298,.T.) ;
#38025 = ORIENTED_EDGE('',*,*,#27299,.T.) ;
#38026 = ORIENTED_EDGE('',*,*,#27286,.T.) ;
#38027 = ORIENTED_EDGE('',*,*,#27300,.F.) ;
#38028 = ORIENTED_EDGE('',*,*,#27301,.T.) ;
#38029 = ORIENTED_EDGE('',*,*,#27302,.T.) ;
#38030 = ORIENTED_EDGE('',*,*,#27284,.T.) ;
#38031 = ORIENTED_EDGE('',*,*,#27299,.F.) ;
#38032 = ORIENTED_EDGE('',*,*,#27303,.T.) ;
#38033 = ORIENTED_EDGE('',*,*,#27304,.T.) ;
#38034 = ORIENTED_EDGE('',*,*,#27282,.T.) ;
#38035 = ORIENTED_EDGE('',*,*,#27302,.F.) ;
#38036 = ORIENTED_EDGE('',*,*,#27305,.T.) ;
#38037 = ORIENTED_EDGE('',*,*,#27306,.T.) ;
#38038 = ORIENTED_EDGE('',*,*,#27279,.T.) ;
#38039 = ORIENTED_EDGE('',*,*,#27304,.F.) ;
#38040 = ORIENTED_EDGE('',*,*,#27307,.T.) ;
#38041 = ORIENTED_EDGE('',*,*,#27308,.T.) ;
#38042 = ORIENTED_EDGE('',*,*,#27309,.T.) ;
#38043 = ORIENTED_EDGE('',*,*,#27306,.F.) ;
#38044 = ORIENTED_EDGE('',*,*,#27310,.T.) ;
#38045 = ORIENTED_EDGE('',*,*,#27311,.T.) ;
#38046 = ORIENTED_EDGE('',*,*,#27312,.T.) ;
#38047 = ORIENTED_EDGE('',*,*,#27313,.T.) ;
#38048 = ORIENTED_EDGE('',*,*,#27314,.T.) ;
#38049 = ORIENTED_EDGE('',*,*,#27311,.F.) ;
#38050 = ORIENTED_EDGE('',*,*,#27315,.T.) ;
#38051 = ORIENTED_EDGE('',*,*,#27316,.T.) ;
#38052 = ORIENTED_EDGE('',*,*,#27317,.T.) ;
#38053 = ORIENTED_EDGE('',*,*,#27313,.F.) ;
#38054 = ORIENTED_EDGE('',*,*,#27318,.T.) ;
#38055 = ORIENTED_EDGE('',*,*,#27308,.F.) ;
#38056 = ORIENTED_EDGE('',*,*,#27319,.T.) ;
#38057 = ORIENTED_EDGE('',*,*,#27316,.F.) ;
#38058 = ORIENTED_EDGE('',*,*,#27320,.T.) ;
#38059 = ORIENTED_EDGE('',*,*,#27321,.T.) ;
#38060 = ORIENTED_EDGE('',*,*,#27322,.T.) ;
#38061 = ORIENTED_EDGE('',*,*,#27321,.F.) ;
#38062 = ORIENTED_EDGE('',*,*,#27323,.T.) ;
#38063 = ORIENTED_EDGE('',*,*,#27324,.T.) ;
#38064 = ORIENTED_EDGE('',*,*,#27290,.T.) ;
#38065 = ORIENTED_EDGE('',*,*,#27324,.F.) ;
#38066 = ORIENTED_EDGE('',*,*,#27325,.T.) ;
#38067 = ORIENTED_EDGE('',*,*,#27326,.T.) ;
#38068 = ORIENTED_EDGE('',*,*,#27288,.T.) ;
#38069 = ORIENTED_EDGE('',*,*,#27326,.F.) ;
#38070 = ORIENTED_EDGE('',*,*,#27327,.T.) ;
#38071 = ORIENTED_EDGE('',*,*,#27300,.T.) ;
#38072 = ORIENTED_EDGE('',*,*,#27261,.F.) ;
#38073 = ORIENTED_EDGE('',*,*,#27280,.F.) ;
#38074 = ORIENTED_EDGE('',*,*,#27309,.F.) ;
#38075 = ORIENTED_EDGE('',*,*,#27328,.T.) ;
#38076 = ORIENTED_EDGE('',*,*,#27258,.F.) ;
#38077 = ORIENTED_EDGE('',*,*,#27328,.F.) ;
#38078 = ORIENTED_EDGE('',*,*,#27318,.F.) ;
#38079 = ORIENTED_EDGE('',*,*,#27329,.T.) ;
#38080 = ORIENTED_EDGE('',*,*,#27257,.F.) ;
#38081 = ORIENTED_EDGE('',*,*,#27329,.F.) ;
#38082 = ORIENTED_EDGE('',*,*,#27312,.F.) ;
#38083 = ORIENTED_EDGE('',*,*,#27330,.T.) ;
#38084 = ORIENTED_EDGE('',*,*,#27331,.F.) ;
#38085 = ORIENTED_EDGE('',*,*,#27310,.F.) ;
#38086 = ORIENTED_EDGE('',*,*,#27317,.F.) ;
#38087 = ORIENTED_EDGE('',*,*,#27307,.F.) ;
#38088 = ORIENTED_EDGE('',*,*,#27305,.F.) ;
#38089 = ORIENTED_EDGE('',*,*,#27303,.F.) ;
#38090 = ORIENTED_EDGE('',*,*,#27301,.F.) ;
#38091 = ORIENTED_EDGE('',*,*,#27298,.F.) ;
#38092 = ORIENTED_EDGE('',*,*,#27327,.F.) ;
#38093 = ORIENTED_EDGE('',*,*,#27325,.F.) ;
#38094 = ORIENTED_EDGE('',*,*,#27323,.F.) ;
#38095 = ORIENTED_EDGE('',*,*,#27320,.F.) ;
#38096 = ORIENTED_EDGE('',*,*,#27315,.F.) ;
#38097 = ORIENTED_EDGE('',*,*,#27296,.T.) ;
#38098 = ORIENTED_EDGE('',*,*,#27297,.T.) ;
#38099 = ORIENTED_EDGE('',*,*,#27332,.T.) ;
#38100 = ORIENTED_EDGE('',*,*,#27331,.T.) ;
#38101 = ORIENTED_EDGE('',*,*,#27332,.F.) ;
#38102 = ORIENTED_EDGE('',*,*,#27248,.F.) ;
#38103 = ORIENTED_EDGE('',*,*,#27333,.F.) ;
#38104 = ORIENTED_EDGE('',*,*,#27322,.F.) ;
#38105 = ORIENTED_EDGE('',*,*,#27289,.T.) ;
#38106 = ORIENTED_EDGE('',*,*,#27251,.F.) ;
#38107 = ORIENTED_EDGE('',*,*,#27334,.F.) ;
#38108 = ORIENTED_EDGE('',*,*,#27319,.F.) ;
#38109 = ORIENTED_EDGE('',*,*,#27333,.T.) ;
#38110 = ORIENTED_EDGE('',*,*,#27254,.F.) ;
#38111 = ORIENTED_EDGE('',*,*,#27330,.F.) ;
#38112 = ORIENTED_EDGE('',*,*,#27314,.F.) ;
#38113 = ORIENTED_EDGE('',*,*,#27334,.T.) ;
#38114 = ORIENTED_EDGE('',*,*,#27335,.T.) ;
#38115 = ORIENTED_EDGE('',*,*,#27336,.T.) ;
#38116 = ORIENTED_EDGE('',*,*,#27337,.T.) ;
#38117 = ORIENTED_EDGE('',*,*,#27338,.F.) ;
#38118 = ORIENTED_EDGE('',*,*,#27339,.T.) ;
#38119 = ORIENTED_EDGE('',*,*,#27340,.T.) ;
#38120 = ORIENTED_EDGE('',*,*,#27341,.T.) ;
#38121 = ORIENTED_EDGE('',*,*,#27336,.F.) ;
#38122 = ORIENTED_EDGE('',*,*,#27342,.T.) ;
#38123 = ORIENTED_EDGE('',*,*,#27343,.T.) ;
#38124 = ORIENTED_EDGE('',*,*,#27344,.T.) ;
#38125 = ORIENTED_EDGE('',*,*,#27340,.F.) ;
#38126 = ORIENTED_EDGE('',*,*,#27345,.T.) ;
#38127 = ORIENTED_EDGE('',*,*,#27346,.T.) ;
#38128 = ORIENTED_EDGE('',*,*,#27347,.T.) ;
#38129 = ORIENTED_EDGE('',*,*,#27343,.F.) ;
#38130 = ORIENTED_EDGE('',*,*,#27348,.T.) ;
#38131 = ORIENTED_EDGE('',*,*,#27349,.T.) ;
#38132 = ORIENTED_EDGE('',*,*,#27350,.T.) ;
#38133 = ORIENTED_EDGE('',*,*,#27346,.F.) ;
#38134 = ORIENTED_EDGE('',*,*,#27351,.T.) ;
#38135 = ORIENTED_EDGE('',*,*,#27349,.F.) ;
#38136 = ORIENTED_EDGE('',*,*,#27352,.T.) ;
#38137 = ORIENTED_EDGE('',*,*,#27353,.T.) ;
#38138 = ORIENTED_EDGE('',*,*,#27354,.T.) ;
#38139 = ORIENTED_EDGE('',*,*,#27353,.F.) ;
#38140 = ORIENTED_EDGE('',*,*,#27355,.T.) ;
#38141 = ORIENTED_EDGE('',*,*,#27356,.T.) ;
#38142 = ORIENTED_EDGE('',*,*,#27357,.T.) ;
#38143 = ORIENTED_EDGE('',*,*,#27356,.F.) ;
#38144 = ORIENTED_EDGE('',*,*,#27358,.T.) ;
#38145 = ORIENTED_EDGE('',*,*,#27359,.T.) ;
#38146 = ORIENTED_EDGE('',*,*,#27360,.T.) ;
#38147 = ORIENTED_EDGE('',*,*,#27359,.F.) ;
#38148 = ORIENTED_EDGE('',*,*,#27361,.T.) ;
#38149 = ORIENTED_EDGE('',*,*,#27362,.T.) ;
#38150 = ORIENTED_EDGE('',*,*,#27363,.T.) ;
#38151 = ORIENTED_EDGE('',*,*,#27362,.F.) ;
#38152 = ORIENTED_EDGE('',*,*,#27364,.T.) ;
#38153 = ORIENTED_EDGE('',*,*,#27365,.T.) ;
#38154 = ORIENTED_EDGE('',*,*,#27366,.T.) ;
#38155 = ORIENTED_EDGE('',*,*,#27365,.F.) ;
#38156 = ORIENTED_EDGE('',*,*,#27367,.T.) ;
#38157 = ORIENTED_EDGE('',*,*,#27368,.T.) ;
#38158 = ORIENTED_EDGE('',*,*,#27369,.T.) ;
#38159 = ORIENTED_EDGE('',*,*,#27368,.F.) ;
#38160 = ORIENTED_EDGE('',*,*,#27370,.T.) ;
#38161 = ORIENTED_EDGE('',*,*,#27338,.T.) ;
#38162 = ORIENTED_EDGE('',*,*,#27357,.F.) ;
#38163 = ORIENTED_EDGE('',*,*,#27371,.F.) ;
#38164 = ORIENTED_EDGE('',*,*,#27372,.F.) ;
#38165 = ORIENTED_EDGE('',*,*,#27373,.T.) ;
#38166 = ORIENTED_EDGE('',*,*,#27360,.F.) ;
#38167 = ORIENTED_EDGE('',*,*,#27374,.F.) ;
#38168 = ORIENTED_EDGE('',*,*,#27375,.F.) ;
#38169 = ORIENTED_EDGE('',*,*,#27371,.T.) ;
#38170 = ORIENTED_EDGE('',*,*,#27363,.F.) ;
#38171 = ORIENTED_EDGE('',*,*,#27376,.F.) ;
#38172 = ORIENTED_EDGE('',*,*,#27377,.F.) ;
#38173 = ORIENTED_EDGE('',*,*,#27374,.T.) ;
#38174 = ORIENTED_EDGE('',*,*,#27366,.F.) ;
#38175 = ORIENTED_EDGE('',*,*,#27378,.F.) ;
#38176 = ORIENTED_EDGE('',*,*,#27379,.F.) ;
#38177 = ORIENTED_EDGE('',*,*,#27376,.T.) ;
#38178 = ORIENTED_EDGE('',*,*,#27369,.F.) ;
#38179 = ORIENTED_EDGE('',*,*,#27380,.F.) ;
#38180 = ORIENTED_EDGE('',*,*,#27381,.F.) ;
#38181 = ORIENTED_EDGE('',*,*,#27378,.T.) ;
#38182 = ORIENTED_EDGE('',*,*,#27337,.F.) ;
#38183 = ORIENTED_EDGE('',*,*,#27382,.F.) ;
#38184 = ORIENTED_EDGE('',*,*,#27383,.F.) ;
#38185 = ORIENTED_EDGE('',*,*,#27380,.T.) ;
#38186 = ORIENTED_EDGE('',*,*,#27335,.F.) ;
#38187 = ORIENTED_EDGE('',*,*,#27370,.F.) ;
#38188 = ORIENTED_EDGE('',*,*,#27367,.F.) ;
#38189 = ORIENTED_EDGE('',*,*,#27364,.F.) ;
#38190 = ORIENTED_EDGE('',*,*,#27361,.F.) ;
#38191 = ORIENTED_EDGE('',*,*,#27358,.F.) ;
#38192 = ORIENTED_EDGE('',*,*,#27355,.F.) ;
#38193 = ORIENTED_EDGE('',*,*,#27352,.F.) ;
#38194 = ORIENTED_EDGE('',*,*,#27348,.F.) ;
#38195 = ORIENTED_EDGE('',*,*,#27345,.F.) ;
#38196 = ORIENTED_EDGE('',*,*,#27342,.F.) ;
#38197 = ORIENTED_EDGE('',*,*,#27339,.F.) ;
#38198 = ORIENTED_EDGE('',*,*,#27384,.T.) ;
#38199 = ORIENTED_EDGE('',*,*,#27385,.T.) ;
#38200 = ORIENTED_EDGE('',*,*,#27386,.T.) ;
#38201 = ORIENTED_EDGE('',*,*,#27387,.T.) ;
#38202 = ORIENTED_EDGE('',*,*,#27385,.F.) ;
#38203 = ORIENTED_EDGE('',*,*,#27387,.F.) ;
#38204 = ORIENTED_EDGE('',*,*,#27388,.T.) ;
#38205 = ORIENTED_EDGE('',*,*,#27389,.F.) ;
#38206 = ORIENTED_EDGE('',*,*,#27390,.F.) ;
#38207 = ORIENTED_EDGE('',*,*,#27388,.F.) ;
#38208 = ORIENTED_EDGE('',*,*,#27386,.F.) ;
#38209 = ORIENTED_EDGE('',*,*,#27384,.F.) ;
#38210 = ORIENTED_EDGE('',*,*,#27391,.T.) ;
#38211 = ORIENTED_EDGE('',*,*,#27392,.T.) ;
#38212 = ORIENTED_EDGE('',*,*,#27379,.T.) ;
#38213 = ORIENTED_EDGE('',*,*,#27393,.F.) ;
#38214 = ORIENTED_EDGE('',*,*,#27394,.T.) ;
#38215 = ORIENTED_EDGE('',*,*,#27395,.T.) ;
#38216 = ORIENTED_EDGE('',*,*,#27377,.T.) ;
#38217 = ORIENTED_EDGE('',*,*,#27392,.F.) ;
#38218 = ORIENTED_EDGE('',*,*,#27396,.T.) ;
#38219 = ORIENTED_EDGE('',*,*,#27397,.T.) ;
#38220 = ORIENTED_EDGE('',*,*,#27375,.T.) ;
#38221 = ORIENTED_EDGE('',*,*,#27395,.F.) ;
#38222 = ORIENTED_EDGE('',*,*,#27398,.T.) ;
#38223 = ORIENTED_EDGE('',*,*,#27399,.T.) ;
#38224 = ORIENTED_EDGE('',*,*,#27372,.T.) ;
#38225 = ORIENTED_EDGE('',*,*,#27397,.F.) ;
#38226 = ORIENTED_EDGE('',*,*,#27400,.T.) ;
#38227 = ORIENTED_EDGE('',*,*,#27401,.T.) ;
#38228 = ORIENTED_EDGE('',*,*,#27402,.T.) ;
#38229 = ORIENTED_EDGE('',*,*,#27399,.F.) ;
#38230 = ORIENTED_EDGE('',*,*,#27403,.T.) ;
#38231 = ORIENTED_EDGE('',*,*,#27404,.T.) ;
#38232 = ORIENTED_EDGE('',*,*,#27405,.T.) ;
#38233 = ORIENTED_EDGE('',*,*,#27406,.T.) ;
#38234 = ORIENTED_EDGE('',*,*,#27407,.T.) ;
#38235 = ORIENTED_EDGE('',*,*,#27404,.F.) ;
#38236 = ORIENTED_EDGE('',*,*,#27408,.T.) ;
#38237 = ORIENTED_EDGE('',*,*,#27409,.T.) ;
#38238 = ORIENTED_EDGE('',*,*,#27410,.T.) ;
#38239 = ORIENTED_EDGE('',*,*,#27406,.F.) ;
#38240 = ORIENTED_EDGE('',*,*,#27411,.T.) ;
#38241 = ORIENTED_EDGE('',*,*,#27401,.F.) ;
#38242 = ORIENTED_EDGE('',*,*,#27412,.T.) ;
#38243 = ORIENTED_EDGE('',*,*,#27409,.F.) ;
#38244 = ORIENTED_EDGE('',*,*,#27413,.T.) ;
#38245 = ORIENTED_EDGE('',*,*,#27414,.T.) ;
#38246 = ORIENTED_EDGE('',*,*,#27415,.T.) ;
#38247 = ORIENTED_EDGE('',*,*,#27414,.F.) ;
#38248 = ORIENTED_EDGE('',*,*,#27416,.T.) ;
#38249 = ORIENTED_EDGE('',*,*,#27417,.T.) ;
#38250 = ORIENTED_EDGE('',*,*,#27383,.T.) ;
#38251 = ORIENTED_EDGE('',*,*,#27417,.F.) ;
#38252 = ORIENTED_EDGE('',*,*,#27418,.T.) ;
#38253 = ORIENTED_EDGE('',*,*,#27419,.T.) ;
#38254 = ORIENTED_EDGE('',*,*,#27381,.T.) ;
#38255 = ORIENTED_EDGE('',*,*,#27419,.F.) ;
#38256 = ORIENTED_EDGE('',*,*,#27420,.T.) ;
#38257 = ORIENTED_EDGE('',*,*,#27393,.T.) ;
#38258 = ORIENTED_EDGE('',*,*,#27354,.F.) ;
#38259 = ORIENTED_EDGE('',*,*,#27373,.F.) ;
#38260 = ORIENTED_EDGE('',*,*,#27402,.F.) ;
#38261 = ORIENTED_EDGE('',*,*,#27421,.T.) ;
#38262 = ORIENTED_EDGE('',*,*,#27351,.F.) ;
#38263 = ORIENTED_EDGE('',*,*,#27421,.F.) ;
#38264 = ORIENTED_EDGE('',*,*,#27411,.F.) ;
#38265 = ORIENTED_EDGE('',*,*,#27422,.T.) ;
#38266 = ORIENTED_EDGE('',*,*,#27350,.F.) ;
#38267 = ORIENTED_EDGE('',*,*,#27422,.F.) ;
#38268 = ORIENTED_EDGE('',*,*,#27405,.F.) ;
#38269 = ORIENTED_EDGE('',*,*,#27423,.T.) ;
#38270 = ORIENTED_EDGE('',*,*,#27424,.F.) ;
#38271 = ORIENTED_EDGE('',*,*,#27403,.F.) ;
#38272 = ORIENTED_EDGE('',*,*,#27410,.F.) ;
#38273 = ORIENTED_EDGE('',*,*,#27400,.F.) ;
#38274 = ORIENTED_EDGE('',*,*,#27398,.F.) ;
#38275 = ORIENTED_EDGE('',*,*,#27396,.F.) ;
#38276 = ORIENTED_EDGE('',*,*,#27394,.F.) ;
#38277 = ORIENTED_EDGE('',*,*,#27391,.F.) ;
#38278 = ORIENTED_EDGE('',*,*,#27420,.F.) ;
#38279 = ORIENTED_EDGE('',*,*,#27418,.F.) ;
#38280 = ORIENTED_EDGE('',*,*,#27416,.F.) ;
#38281 = ORIENTED_EDGE('',*,*,#27413,.F.) ;
#38282 = ORIENTED_EDGE('',*,*,#27408,.F.) ;
#38283 = ORIENTED_EDGE('',*,*,#27389,.T.) ;
#38284 = ORIENTED_EDGE('',*,*,#27390,.T.) ;
#38285 = ORIENTED_EDGE('',*,*,#27425,.T.) ;
#38286 = ORIENTED_EDGE('',*,*,#27424,.T.) ;
#38287 = ORIENTED_EDGE('',*,*,#27425,.F.) ;
#38288 = ORIENTED_EDGE('',*,*,#27341,.F.) ;
#38289 = ORIENTED_EDGE('',*,*,#27426,.F.) ;
#38290 = ORIENTED_EDGE('',*,*,#27415,.F.) ;
#38291 = ORIENTED_EDGE('',*,*,#27382,.T.) ;
#38292 = ORIENTED_EDGE('',*,*,#27344,.F.) ;
#38293 = ORIENTED_EDGE('',*,*,#27427,.F.) ;
#38294 = ORIENTED_EDGE('',*,*,#27412,.F.) ;
#38295 = ORIENTED_EDGE('',*,*,#27426,.T.) ;
#38296 = ORIENTED_EDGE('',*,*,#27347,.F.) ;
#38297 = ORIENTED_EDGE('',*,*,#27423,.F.) ;
#38298 = ORIENTED_EDGE('',*,*,#27407,.F.) ;
#38299 = ORIENTED_EDGE('',*,*,#27427,.T.) ;
#38300 = ORIENTED_EDGE('',*,*,#27428,.F.) ;
#38301 = ORIENTED_EDGE('',*,*,#27429,.F.) ;
#38302 = ORIENTED_EDGE('',*,*,#27430,.F.) ;
#38303 = ORIENTED_EDGE('',*,*,#27431,.F.) ;
#38304 = ORIENTED_EDGE('',*,*,#27432,.F.) ;
#38305 = ORIENTED_EDGE('',*,*,#27433,.F.) ;
#38306 = ORIENTED_EDGE('',*,*,#27432,.T.) ;
#38307 = ORIENTED_EDGE('',*,*,#27434,.T.) ;
#38308 = ORIENTED_EDGE('',*,*,#27430,.T.) ;
#38309 = ORIENTED_EDGE('',*,*,#27435,.T.) ;
#38310 = ORIENTED_EDGE('',*,*,#27436,.F.) ;
#38311 = ORIENTED_EDGE('',*,*,#27437,.F.) ;
#38312 = ORIENTED_EDGE('',*,*,#27438,.F.) ;
#38313 = ORIENTED_EDGE('',*,*,#27429,.T.) ;
#38314 = ORIENTED_EDGE('',*,*,#27439,.T.) ;
#38315 = ORIENTED_EDGE('',*,*,#27437,.T.) ;
#38316 = ORIENTED_EDGE('',*,*,#27440,.T.) ;
#38317 = ORIENTED_EDGE('',*,*,#27441,.F.) ;
#38318 = ORIENTED_EDGE('',*,*,#27442,.F.) ;
#38319 = ORIENTED_EDGE('',*,*,#27443,.T.) ;
#38320 = ORIENTED_EDGE('',*,*,#27444,.F.) ;
#38321 = ORIENTED_EDGE('',*,*,#27445,.T.) ;
#38322 = ORIENTED_EDGE('',*,*,#27446,.F.) ;
#38323 = ORIENTED_EDGE('',*,*,#27447,.F.) ;
#38324 = ORIENTED_EDGE('',*,*,#27448,.F.) ;
#38325 = ORIENTED_EDGE('',*,*,#27446,.T.) ;
#38326 = ORIENTED_EDGE('',*,*,#27449,.T.) ;
#38327 = ORIENTED_EDGE('',*,*,#27442,.T.) ;
#38328 = ORIENTED_EDGE('',*,*,#27450,.T.) ;
#38329 = ORIENTED_EDGE('',*,*,#27431,.T.) ;
#38330 = ORIENTED_EDGE('',*,*,#27451,.T.) ;
#38331 = ORIENTED_EDGE('',*,*,#27447,.T.) ;
#38332 = ORIENTED_EDGE('',*,*,#27452,.T.) ;
#38333 = ORIENTED_EDGE('',*,*,#27453,.F.) ;
#38334 = ORIENTED_EDGE('',*,*,#27454,.F.) ;
#38335 = ORIENTED_EDGE('',*,*,#27455,.F.) ;
#38336 = ORIENTED_EDGE('',*,*,#27433,.T.) ;
#38337 = ORIENTED_EDGE('',*,*,#27456,.T.) ;
#38338 = ORIENTED_EDGE('',*,*,#27454,.T.) ;
#38339 = ORIENTED_EDGE('',*,*,#27457,.T.) ;
#38340 = ORIENTED_EDGE('',*,*,#27436,.T.) ;
#38341 = ORIENTED_EDGE('',*,*,#27458,.T.) ;
#38342 = ORIENTED_EDGE('',*,*,#27455,.T.) ;
#38343 = ORIENTED_EDGE('',*,*,#27459,.T.) ;
#38344 = ORIENTED_EDGE('',*,*,#27460,.T.) ;
#38345 = ORIENTED_EDGE('',*,*,#27461,.F.) ;
#38346 = ORIENTED_EDGE('',*,*,#27462,.F.) ;
#38347 = ORIENTED_EDGE('',*,*,#27463,.F.) ;
#38348 = ORIENTED_EDGE('',*,*,#27464,.T.) ;
#38349 = ORIENTED_EDGE('',*,*,#27465,.F.) ;
#38350 = ORIENTED_EDGE('',*,*,#27466,.F.) ;
#38351 = ORIENTED_EDGE('',*,*,#27467,.F.) ;
#38352 = ORIENTED_EDGE('',*,*,#27461,.T.) ;
#38353 = ORIENTED_EDGE('',*,*,#27468,.T.) ;
#38354 = ORIENTED_EDGE('',*,*,#27467,.T.) ;
#38355 = ORIENTED_EDGE('',*,*,#27469,.T.) ;
#38356 = ORIENTED_EDGE('',*,*,#27448,.T.) ;
#38357 = ORIENTED_EDGE('',*,*,#27470,.T.) ;
#38358 = ORIENTED_EDGE('',*,*,#27465,.T.) ;
#38359 = ORIENTED_EDGE('',*,*,#27471,.T.) ;
#38360 = ORIENTED_EDGE('',*,*,#27466,.T.) ;
#38361 = ORIENTED_EDGE('',*,*,#27472,.T.) ;
#38362 = ORIENTED_EDGE('',*,*,#27453,.T.) ;
#38363 = ORIENTED_EDGE('',*,*,#27473,.T.) ;
#38364 = ORIENTED_EDGE('',*,*,#27462,.T.) ;
#38365 = ORIENTED_EDGE('',*,*,#27474,.T.) ;
#38366 = ORIENTED_EDGE('',*,*,#27438,.T.) ;
#38367 = ORIENTED_EDGE('',*,*,#27475,.T.) ;
#38368 = ORIENTED_EDGE('',*,*,#27444,.T.) ;
#38369 = ORIENTED_EDGE('',*,*,#27476,.T.) ;
#38370 = ORIENTED_EDGE('',*,*,#27463,.T.) ;
#38371 = ORIENTED_EDGE('',*,*,#27477,.T.) ;
#38372 = ORIENTED_EDGE('',*,*,#27441,.T.) ;
#38373 = ORIENTED_EDGE('',*,*,#27478,.T.) ;
#38374 = ORIENTED_EDGE('',*,*,#27428,.T.) ;
#38375 = ORIENTED_EDGE('',*,*,#27479,.T.) ;
#38376 = ORIENTED_EDGE('',*,*,#27435,.F.) ;
#38377 = ORIENTED_EDGE('',*,*,#27440,.F.) ;
#38378 = ORIENTED_EDGE('',*,*,#27459,.F.) ;
#38379 = ORIENTED_EDGE('',*,*,#27456,.F.) ;
#38380 = ORIENTED_EDGE('',*,*,#27439,.F.) ;
#38381 = ORIENTED_EDGE('',*,*,#27478,.F.) ;
#38382 = ORIENTED_EDGE('',*,*,#27477,.F.) ;
#38383 = ORIENTED_EDGE('',*,*,#27475,.F.) ;
#38384 = ORIENTED_EDGE('',*,*,#27450,.F.) ;
#38385 = ORIENTED_EDGE('',*,*,#27479,.F.) ;
#38386 = ORIENTED_EDGE('',*,*,#27434,.F.) ;
#38387 = ORIENTED_EDGE('',*,*,#27452,.F.) ;
#38388 = ORIENTED_EDGE('',*,*,#27451,.F.) ;
#38389 = ORIENTED_EDGE('',*,*,#27457,.F.) ;
#38390 = ORIENTED_EDGE('',*,*,#27472,.F.) ;
#38391 = ORIENTED_EDGE('',*,*,#27470,.F.) ;
#38392 = ORIENTED_EDGE('',*,*,#27469,.F.) ;
#38393 = ORIENTED_EDGE('',*,*,#27473,.F.) ;
#38394 = ORIENTED_EDGE('',*,*,#27458,.F.) ;
#38395 = ORIENTED_EDGE('',*,*,#27474,.F.) ;
#38396 = ORIENTED_EDGE('',*,*,#27480,.F.) ;
#38397 = ORIENTED_EDGE('',*,*,#27481,.F.) ;
#38398 = ORIENTED_EDGE('',*,*,#27482,.F.) ;
#38399 = ORIENTED_EDGE('',*,*,#27483,.F.) ;
#38400 = ORIENTED_EDGE('',*,*,#27484,.F.) ;
#38401 = ORIENTED_EDGE('',*,*,#27485,.F.) ;
#38402 = ORIENTED_EDGE('',*,*,#27484,.T.) ;
#38403 = ORIENTED_EDGE('',*,*,#27486,.T.) ;
#38404 = ORIENTED_EDGE('',*,*,#27482,.T.) ;
#38405 = ORIENTED_EDGE('',*,*,#27487,.T.) ;
#38406 = ORIENTED_EDGE('',*,*,#27488,.T.) ;
#38407 = ORIENTED_EDGE('',*,*,#27481,.T.) ;
#38408 = ORIENTED_EDGE('',*,*,#27489,.T.) ;
#38409 = ORIENTED_EDGE('',*,*,#27490,.T.) ;
#38410 = ORIENTED_EDGE('',*,*,#27491,.F.) ;
#38411 = ORIENTED_EDGE('',*,*,#27492,.F.) ;
#38412 = ORIENTED_EDGE('',*,*,#27493,.F.) ;
#38413 = ORIENTED_EDGE('',*,*,#27492,.T.) ;
#38414 = ORIENTED_EDGE('',*,*,#27494,.T.) ;
#38415 = ORIENTED_EDGE('',*,*,#27485,.T.) ;
#38416 = ORIENTED_EDGE('',*,*,#27495,.T.) ;
#38417 = ORIENTED_EDGE('',*,*,#27496,.T.) ;
#38418 = ORIENTED_EDGE('',*,*,#27493,.T.) ;
#38419 = ORIENTED_EDGE('',*,*,#27497,.T.) ;
#38420 = ORIENTED_EDGE('',*,*,#27490,.F.) ;
#38421 = ORIENTED_EDGE('',*,*,#27498,.T.) ;
#38422 = ORIENTED_EDGE('',*,*,#27499,.T.) ;
#38423 = ORIENTED_EDGE('',*,*,#27500,.T.) ;
#38424 = ORIENTED_EDGE('',*,*,#27491,.T.) ;
#38425 = ORIENTED_EDGE('',*,*,#27501,.T.) ;
#38426 = ORIENTED_EDGE('',*,*,#27502,.T.) ;
#38427 = ORIENTED_EDGE('',*,*,#27503,.T.) ;
#38428 = ORIENTED_EDGE('',*,*,#27483,.T.) ;
#38429 = ORIENTED_EDGE('',*,*,#27504,.T.) ;
#38430 = ORIENTED_EDGE('',*,*,#27505,.T.) ;
#38431 = ORIENTED_EDGE('',*,*,#27506,.T.) ;
#38432 = ORIENTED_EDGE('',*,*,#27480,.T.) ;
#38433 = ORIENTED_EDGE('',*,*,#27507,.T.) ;
#38434 = ORIENTED_EDGE('',*,*,#27504,.F.) ;
#38435 = ORIENTED_EDGE('',*,*,#27494,.F.) ;
#38436 = ORIENTED_EDGE('',*,*,#27500,.F.) ;
#38437 = ORIENTED_EDGE('',*,*,#27508,.F.) ;
#38438 = ORIENTED_EDGE('',*,*,#27502,.F.) ;
#38439 = ORIENTED_EDGE('',*,*,#27508,.T.) ;
#38440 = ORIENTED_EDGE('',*,*,#27499,.F.) ;
#38441 = ORIENTED_EDGE('',*,*,#27509,.F.) ;
#38442 = ORIENTED_EDGE('',*,*,#27510,.T.) ;
#38443 = ORIENTED_EDGE('',*,*,#27505,.F.) ;
#38444 = ORIENTED_EDGE('',*,*,#27511,.T.) ;
#38445 = ORIENTED_EDGE('',*,*,#27501,.F.) ;
#38446 = ORIENTED_EDGE('',*,*,#27496,.F.) ;
#38447 = ORIENTED_EDGE('',*,*,#27512,.T.) ;
#38448 = ORIENTED_EDGE('',*,*,#27509,.T.) ;
#38449 = ORIENTED_EDGE('',*,*,#27487,.F.) ;
#38450 = ORIENTED_EDGE('',*,*,#27488,.F.) ;
#38451 = ORIENTED_EDGE('',*,*,#27497,.F.) ;
#38452 = ORIENTED_EDGE('',*,*,#27495,.F.) ;
#38453 = ORIENTED_EDGE('',*,*,#27445,.F.) ;
#38454 = ORIENTED_EDGE('',*,*,#27471,.F.) ;
#38455 = ORIENTED_EDGE('',*,*,#27464,.F.) ;
#38456 = ORIENTED_EDGE('',*,*,#27468,.F.) ;
#38457 = ORIENTED_EDGE('',*,*,#27460,.F.) ;
#38458 = ORIENTED_EDGE('',*,*,#27476,.F.) ;
#38459 = ORIENTED_EDGE('',*,*,#27443,.F.) ;
#38460 = ORIENTED_EDGE('',*,*,#27449,.F.) ;
#38461 = ORIENTED_EDGE('',*,*,#27506,.F.) ;
#38462 = ORIENTED_EDGE('',*,*,#27510,.F.) ;
#38463 = ORIENTED_EDGE('',*,*,#27512,.F.) ;
#38464 = ORIENTED_EDGE('',*,*,#27498,.F.) ;
#38465 = ORIENTED_EDGE('',*,*,#27489,.F.) ;
#38466 = ORIENTED_EDGE('',*,*,#27503,.F.) ;
#38467 = ORIENTED_EDGE('',*,*,#27511,.F.) ;
#38468 = ORIENTED_EDGE('',*,*,#27507,.F.) ;
#38469 = ORIENTED_EDGE('',*,*,#27486,.F.) ;
#38470 = ORIENTED_EDGE('',*,*,#27513,.F.) ;
#38471 = ORIENTED_EDGE('',*,*,#27514,.T.) ;
#38472 = ORIENTED_EDGE('',*,*,#27515,.T.) ;
#38473 = ORIENTED_EDGE('',*,*,#27516,.F.) ;
#38474 = ORIENTED_EDGE('',*,*,#27514,.F.) ;
#38475 = ORIENTED_EDGE('',*,*,#27517,.T.) ;
#38476 = ORIENTED_EDGE('',*,*,#27518,.F.) ;
#38477 = ORIENTED_EDGE('',*,*,#27519,.T.) ;
#38478 = ORIENTED_EDGE('',*,*,#27517,.F.) ;
#38479 = ORIENTED_EDGE('',*,*,#27520,.T.) ;
#38480 = ORIENTED_EDGE('',*,*,#27521,.T.) ;
#38481 = ORIENTED_EDGE('',*,*,#27522,.T.) ;
#38482 = ORIENTED_EDGE('',*,*,#27523,.F.) ;
#38483 = ORIENTED_EDGE('',*,*,#27520,.F.) ;
#38484 = ORIENTED_EDGE('',*,*,#27524,.T.) ;
#38485 = ORIENTED_EDGE('',*,*,#27525,.F.) ;
#38486 = ORIENTED_EDGE('',*,*,#27526,.T.) ;
#38487 = ORIENTED_EDGE('',*,*,#27524,.F.) ;
#38488 = ORIENTED_EDGE('',*,*,#27527,.T.) ;
#38489 = ORIENTED_EDGE('',*,*,#27528,.T.) ;
#38490 = ORIENTED_EDGE('',*,*,#27529,.F.) ;
#38491 = ORIENTED_EDGE('',*,*,#27530,.F.) ;
#38492 = ORIENTED_EDGE('',*,*,#27531,.T.) ;
#38493 = ORIENTED_EDGE('',*,*,#27532,.T.) ;
#38494 = ORIENTED_EDGE('',*,*,#27533,.F.) ;
#38495 = ORIENTED_EDGE('',*,*,#27534,.F.) ;
#38496 = ORIENTED_EDGE('',*,*,#27535,.T.) ;
#38497 = ORIENTED_EDGE('',*,*,#27536,.T.) ;
#38498 = ORIENTED_EDGE('',*,*,#27531,.F.) ;
#38499 = ORIENTED_EDGE('',*,*,#27537,.F.) ;
#38500 = ORIENTED_EDGE('',*,*,#27538,.T.) ;
#38501 = ORIENTED_EDGE('',*,*,#27539,.T.) ;
#38502 = ORIENTED_EDGE('',*,*,#27535,.F.) ;
#38503 = ORIENTED_EDGE('',*,*,#27540,.F.) ;
#38504 = ORIENTED_EDGE('',*,*,#27541,.T.) ;
#38505 = ORIENTED_EDGE('',*,*,#27542,.T.) ;
#38506 = ORIENTED_EDGE('',*,*,#27538,.F.) ;
#38507 = ORIENTED_EDGE('',*,*,#27543,.F.) ;
#38508 = ORIENTED_EDGE('',*,*,#27544,.T.) ;
#38509 = ORIENTED_EDGE('',*,*,#27545,.T.) ;
#38510 = ORIENTED_EDGE('',*,*,#27541,.F.) ;
#38511 = ORIENTED_EDGE('',*,*,#27546,.F.) ;
#38512 = ORIENTED_EDGE('',*,*,#27547,.T.) ;
#38513 = ORIENTED_EDGE('',*,*,#27548,.T.) ;
#38514 = ORIENTED_EDGE('',*,*,#27544,.F.) ;
#38515 = ORIENTED_EDGE('',*,*,#27549,.F.) ;
#38516 = ORIENTED_EDGE('',*,*,#27550,.T.) ;
#38517 = ORIENTED_EDGE('',*,*,#27551,.T.) ;
#38518 = ORIENTED_EDGE('',*,*,#27547,.F.) ;
#38519 = ORIENTED_EDGE('',*,*,#27552,.F.) ;
#38520 = ORIENTED_EDGE('',*,*,#27533,.T.) ;
#38521 = ORIENTED_EDGE('',*,*,#27553,.T.) ;
#38522 = ORIENTED_EDGE('',*,*,#27550,.F.) ;
#38523 = ORIENTED_EDGE('',*,*,#27554,.F.) ;
#38524 = ORIENTED_EDGE('',*,*,#27555,.T.) ;
#38525 = ORIENTED_EDGE('',*,*,#27556,.T.) ;
#38526 = ORIENTED_EDGE('',*,*,#27557,.F.) ;
#38527 = ORIENTED_EDGE('',*,*,#27558,.F.) ;
#38528 = ORIENTED_EDGE('',*,*,#27559,.T.) ;
#38529 = ORIENTED_EDGE('',*,*,#27560,.T.) ;
#38530 = ORIENTED_EDGE('',*,*,#27555,.F.) ;
#38531 = ORIENTED_EDGE('',*,*,#27561,.F.) ;
#38532 = ORIENTED_EDGE('',*,*,#27562,.T.) ;
#38533 = ORIENTED_EDGE('',*,*,#27563,.T.) ;
#38534 = ORIENTED_EDGE('',*,*,#27559,.F.) ;
#38535 = ORIENTED_EDGE('',*,*,#27564,.F.) ;
#38536 = ORIENTED_EDGE('',*,*,#27565,.T.) ;
#38537 = ORIENTED_EDGE('',*,*,#27566,.T.) ;
#38538 = ORIENTED_EDGE('',*,*,#27562,.F.) ;
#38539 = ORIENTED_EDGE('',*,*,#27567,.F.) ;
#38540 = ORIENTED_EDGE('',*,*,#27568,.T.) ;
#38541 = ORIENTED_EDGE('',*,*,#27569,.T.) ;
#38542 = ORIENTED_EDGE('',*,*,#27565,.F.) ;
#38543 = ORIENTED_EDGE('',*,*,#27570,.F.) ;
#38544 = ORIENTED_EDGE('',*,*,#27571,.T.) ;
#38545 = ORIENTED_EDGE('',*,*,#27572,.T.) ;
#38546 = ORIENTED_EDGE('',*,*,#27568,.F.) ;
#38547 = ORIENTED_EDGE('',*,*,#27573,.F.) ;
#38548 = ORIENTED_EDGE('',*,*,#27574,.T.) ;
#38549 = ORIENTED_EDGE('',*,*,#27575,.T.) ;
#38550 = ORIENTED_EDGE('',*,*,#27571,.F.) ;
#38551 = ORIENTED_EDGE('',*,*,#27576,.F.) ;
#38552 = ORIENTED_EDGE('',*,*,#27577,.T.) ;
#38553 = ORIENTED_EDGE('',*,*,#27578,.T.) ;
#38554 = ORIENTED_EDGE('',*,*,#27574,.F.) ;
#38555 = ORIENTED_EDGE('',*,*,#27579,.F.) ;
#38556 = ORIENTED_EDGE('',*,*,#27580,.T.) ;
#38557 = ORIENTED_EDGE('',*,*,#27581,.T.) ;
#38558 = ORIENTED_EDGE('',*,*,#27577,.F.) ;
#38559 = ORIENTED_EDGE('',*,*,#27582,.F.) ;
#38560 = ORIENTED_EDGE('',*,*,#27583,.T.) ;
#38561 = ORIENTED_EDGE('',*,*,#27584,.T.) ;
#38562 = ORIENTED_EDGE('',*,*,#27580,.F.) ;
#38563 = ORIENTED_EDGE('',*,*,#27585,.F.) ;
#38564 = ORIENTED_EDGE('',*,*,#27586,.T.) ;
#38565 = ORIENTED_EDGE('',*,*,#27587,.T.) ;
#38566 = ORIENTED_EDGE('',*,*,#27583,.F.) ;
#38567 = ORIENTED_EDGE('',*,*,#27588,.F.) ;
#38568 = ORIENTED_EDGE('',*,*,#27589,.T.) ;
#38569 = ORIENTED_EDGE('',*,*,#27590,.T.) ;
#38570 = ORIENTED_EDGE('',*,*,#27586,.F.) ;
#38571 = ORIENTED_EDGE('',*,*,#27591,.F.) ;
#38572 = ORIENTED_EDGE('',*,*,#27592,.T.) ;
#38573 = ORIENTED_EDGE('',*,*,#27593,.T.) ;
#38574 = ORIENTED_EDGE('',*,*,#27589,.F.) ;
#38575 = ORIENTED_EDGE('',*,*,#27594,.F.) ;
#38576 = ORIENTED_EDGE('',*,*,#27595,.T.) ;
#38577 = ORIENTED_EDGE('',*,*,#27596,.T.) ;
#38578 = ORIENTED_EDGE('',*,*,#27592,.F.) ;
#38579 = ORIENTED_EDGE('',*,*,#27597,.F.) ;
#38580 = ORIENTED_EDGE('',*,*,#27598,.T.) ;
#38581 = ORIENTED_EDGE('',*,*,#27599,.T.) ;
#38582 = ORIENTED_EDGE('',*,*,#27595,.F.) ;
#38583 = ORIENTED_EDGE('',*,*,#27600,.F.) ;
#38584 = ORIENTED_EDGE('',*,*,#27601,.T.) ;
#38585 = ORIENTED_EDGE('',*,*,#27602,.T.) ;
#38586 = ORIENTED_EDGE('',*,*,#27598,.F.) ;
#38587 = ORIENTED_EDGE('',*,*,#27603,.F.) ;
#38588 = ORIENTED_EDGE('',*,*,#27604,.T.) ;
#38589 = ORIENTED_EDGE('',*,*,#27605,.T.) ;
#38590 = ORIENTED_EDGE('',*,*,#27601,.F.) ;
#38591 = ORIENTED_EDGE('',*,*,#27606,.F.) ;
#38592 = ORIENTED_EDGE('',*,*,#27607,.T.) ;
#38593 = ORIENTED_EDGE('',*,*,#27608,.T.) ;
#38594 = ORIENTED_EDGE('',*,*,#27604,.F.) ;
#38595 = ORIENTED_EDGE('',*,*,#27609,.F.) ;
#38596 = ORIENTED_EDGE('',*,*,#27557,.T.) ;
#38597 = ORIENTED_EDGE('',*,*,#27610,.T.) ;
#38598 = ORIENTED_EDGE('',*,*,#27607,.F.) ;
#38599 = ORIENTED_EDGE('',*,*,#27610,.F.) ;
#38600 = ORIENTED_EDGE('',*,*,#27556,.F.) ;
#38601 = ORIENTED_EDGE('',*,*,#27560,.F.) ;
#38602 = ORIENTED_EDGE('',*,*,#27563,.F.) ;
#38603 = ORIENTED_EDGE('',*,*,#27566,.F.) ;
#38604 = ORIENTED_EDGE('',*,*,#27569,.F.) ;
#38605 = ORIENTED_EDGE('',*,*,#27572,.F.) ;
#38606 = ORIENTED_EDGE('',*,*,#27575,.F.) ;
#38607 = ORIENTED_EDGE('',*,*,#27578,.F.) ;
#38608 = ORIENTED_EDGE('',*,*,#27581,.F.) ;
#38609 = ORIENTED_EDGE('',*,*,#27584,.F.) ;
#38610 = ORIENTED_EDGE('',*,*,#27587,.F.) ;
#38611 = ORIENTED_EDGE('',*,*,#27590,.F.) ;
#38612 = ORIENTED_EDGE('',*,*,#27593,.F.) ;
#38613 = ORIENTED_EDGE('',*,*,#27596,.F.) ;
#38614 = ORIENTED_EDGE('',*,*,#27599,.F.) ;
#38615 = ORIENTED_EDGE('',*,*,#27602,.F.) ;
#38616 = ORIENTED_EDGE('',*,*,#27605,.F.) ;
#38617 = ORIENTED_EDGE('',*,*,#27608,.F.) ;
#38618 = ORIENTED_EDGE('',*,*,#27553,.F.) ;
#38619 = ORIENTED_EDGE('',*,*,#27532,.F.) ;
#38620 = ORIENTED_EDGE('',*,*,#27536,.F.) ;
#38621 = ORIENTED_EDGE('',*,*,#27539,.F.) ;
#38622 = ORIENTED_EDGE('',*,*,#27542,.F.) ;
#38623 = ORIENTED_EDGE('',*,*,#27545,.F.) ;
#38624 = ORIENTED_EDGE('',*,*,#27548,.F.) ;
#38625 = ORIENTED_EDGE('',*,*,#27551,.F.) ;
#38626 = ORIENTED_EDGE('',*,*,#27611,.F.) ;
#38627 = ORIENTED_EDGE('',*,*,#27612,.F.) ;
#38628 = ORIENTED_EDGE('',*,*,#27613,.T.) ;
#38629 = ORIENTED_EDGE('',*,*,#27614,.F.) ;
#38630 = ORIENTED_EDGE('',*,*,#27615,.F.) ;
#38631 = ORIENTED_EDGE('',*,*,#27616,.F.) ;
#38632 = ORIENTED_EDGE('',*,*,#27617,.F.) ;
#38633 = ORIENTED_EDGE('',*,*,#27618,.F.) ;
#38634 = ORIENTED_EDGE('',*,*,#27619,.F.) ;
#38635 = ORIENTED_EDGE('',*,*,#27620,.F.) ;
#38636 = ORIENTED_EDGE('',*,*,#27621,.F.) ;
#38637 = ORIENTED_EDGE('',*,*,#27622,.F.) ;
#38638 = ORIENTED_EDGE('',*,*,#27623,.F.) ;
#38639 = ORIENTED_EDGE('',*,*,#27624,.F.) ;
#38640 = ORIENTED_EDGE('',*,*,#27625,.F.) ;
#38641 = ORIENTED_EDGE('',*,*,#27626,.F.) ;
#38642 = ORIENTED_EDGE('',*,*,#27627,.F.) ;
#38643 = ORIENTED_EDGE('',*,*,#27628,.F.) ;
#38644 = ORIENTED_EDGE('',*,*,#27629,.F.) ;
#38645 = ORIENTED_EDGE('',*,*,#27630,.F.) ;
#38646 = ORIENTED_EDGE('',*,*,#27631,.F.) ;
#38647 = ORIENTED_EDGE('',*,*,#27632,.F.) ;
#38648 = ORIENTED_EDGE('',*,*,#27554,.T.) ;
#38649 = ORIENTED_EDGE('',*,*,#27609,.T.) ;
#38650 = ORIENTED_EDGE('',*,*,#27606,.T.) ;
#38651 = ORIENTED_EDGE('',*,*,#27603,.T.) ;
#38652 = ORIENTED_EDGE('',*,*,#27600,.T.) ;
#38653 = ORIENTED_EDGE('',*,*,#27597,.T.) ;
#38654 = ORIENTED_EDGE('',*,*,#27594,.T.) ;
#38655 = ORIENTED_EDGE('',*,*,#27591,.T.) ;
#38656 = ORIENTED_EDGE('',*,*,#27588,.T.) ;
#38657 = ORIENTED_EDGE('',*,*,#27585,.T.) ;
#38658 = ORIENTED_EDGE('',*,*,#27582,.T.) ;
#38659 = ORIENTED_EDGE('',*,*,#27579,.T.) ;
#38660 = ORIENTED_EDGE('',*,*,#27576,.T.) ;
#38661 = ORIENTED_EDGE('',*,*,#27573,.T.) ;
#38662 = ORIENTED_EDGE('',*,*,#27570,.T.) ;
#38663 = ORIENTED_EDGE('',*,*,#27567,.T.) ;
#38664 = ORIENTED_EDGE('',*,*,#27564,.T.) ;
#38665 = ORIENTED_EDGE('',*,*,#27561,.T.) ;
#38666 = ORIENTED_EDGE('',*,*,#27558,.T.) ;
#38667 = ORIENTED_EDGE('',*,*,#27633,.F.) ;
#38668 = ORIENTED_EDGE('',*,*,#27634,.T.) ;
#38669 = ORIENTED_EDGE('',*,*,#27635,.T.) ;
#38670 = ORIENTED_EDGE('',*,*,#27636,.T.) ;
#38671 = ORIENTED_EDGE('',*,*,#27636,.F.) ;
#38672 = ORIENTED_EDGE('',*,*,#27637,.T.) ;
#38673 = ORIENTED_EDGE('',*,*,#27638,.T.) ;
#38674 = ORIENTED_EDGE('',*,*,#27639,.T.) ;
#38675 = ORIENTED_EDGE('',*,*,#27640,.T.) ;
#38676 = ORIENTED_EDGE('',*,*,#27641,.T.) ;
#38677 = ORIENTED_EDGE('',*,*,#27642,.T.) ;
#38678 = ORIENTED_EDGE('',*,*,#27643,.T.) ;
#38679 = ORIENTED_EDGE('',*,*,#27644,.T.) ;
#38680 = ORIENTED_EDGE('',*,*,#27645,.T.) ;
#38681 = ORIENTED_EDGE('',*,*,#27640,.F.) ;
#38682 = ORIENTED_EDGE('',*,*,#27646,.T.) ;
#38683 = ORIENTED_EDGE('',*,*,#27647,.T.) ;
#38684 = ORIENTED_EDGE('',*,*,#27648,.T.) ;
#38685 = ORIENTED_EDGE('',*,*,#27644,.F.) ;
#38686 = ORIENTED_EDGE('',*,*,#27649,.T.) ;
#38687 = ORIENTED_EDGE('',*,*,#27650,.T.) ;
#38688 = ORIENTED_EDGE('',*,*,#27651,.T.) ;
#38689 = ORIENTED_EDGE('',*,*,#27652,.T.) ;
#38690 = ORIENTED_EDGE('',*,*,#27647,.F.) ;
#38691 = ORIENTED_EDGE('',*,*,#27653,.T.) ;
#38692 = ORIENTED_EDGE('',*,*,#27654,.F.) ;
#38693 = ORIENTED_EDGE('',*,*,#27655,.F.) ;
#38694 = ORIENTED_EDGE('',*,*,#27656,.F.) ;
#38695 = ORIENTED_EDGE('',*,*,#27650,.F.) ;
#38696 = ORIENTED_EDGE('',*,*,#27657,.T.) ;
#38697 = ORIENTED_EDGE('',*,*,#27657,.F.) ;
#38698 = ORIENTED_EDGE('',*,*,#27653,.F.) ;
#38699 = ORIENTED_EDGE('',*,*,#27658,.F.) ;
#38700 = ORIENTED_EDGE('',*,*,#27659,.F.) ;
#38701 = ORIENTED_EDGE('',*,*,#27660,.F.) ;
#38702 = ORIENTED_EDGE('',*,*,#27661,.F.) ;
#38703 = ORIENTED_EDGE('',*,*,#27662,.T.) ;
#38704 = ORIENTED_EDGE('',*,*,#27649,.F.) ;
#38705 = ORIENTED_EDGE('',*,*,#27663,.T.) ;
#38706 = ORIENTED_EDGE('',*,*,#27664,.T.) ;
#38707 = ORIENTED_EDGE('',*,*,#27658,.T.) ;
#38708 = ORIENTED_EDGE('',*,*,#27646,.F.) ;
#38709 = ORIENTED_EDGE('',*,*,#27643,.F.) ;
#38710 = ORIENTED_EDGE('',*,*,#27665,.F.) ;
#38711 = ORIENTED_EDGE('',*,*,#27666,.F.) ;
#38712 = ORIENTED_EDGE('',*,*,#27663,.F.) ;
#38713 = ORIENTED_EDGE('',*,*,#27667,.F.) ;
#38714 = ORIENTED_EDGE('',*,*,#27668,.T.) ;
#38715 = ORIENTED_EDGE('',*,*,#27669,.T.) ;
#38716 = ORIENTED_EDGE('',*,*,#27670,.T.) ;
#38717 = ORIENTED_EDGE('',*,*,#27671,.T.) ;
#38718 = ORIENTED_EDGE('',*,*,#27672,.T.) ;
#38719 = ORIENTED_EDGE('',*,*,#27673,.T.) ;
#38720 = ORIENTED_EDGE('',*,*,#27674,.T.) ;
#38721 = ORIENTED_EDGE('',*,*,#27675,.T.) ;
#38722 = ORIENTED_EDGE('',*,*,#27669,.F.) ;
#38723 = ORIENTED_EDGE('',*,*,#27676,.T.) ;
#38724 = ORIENTED_EDGE('',*,*,#27677,.T.) ;
#38725 = ORIENTED_EDGE('',*,*,#27678,.T.) ;
#38726 = ORIENTED_EDGE('',*,*,#27674,.F.) ;
#38727 = ORIENTED_EDGE('',*,*,#27679,.T.) ;
#38728 = ORIENTED_EDGE('',*,*,#27680,.T.) ;
#38729 = ORIENTED_EDGE('',*,*,#27681,.T.) ;
#38730 = ORIENTED_EDGE('',*,*,#27677,.F.) ;
#38731 = ORIENTED_EDGE('',*,*,#27682,.T.) ;
#38732 = ORIENTED_EDGE('',*,*,#27683,.T.) ;
#38733 = ORIENTED_EDGE('',*,*,#27684,.T.) ;
#38734 = ORIENTED_EDGE('',*,*,#27680,.F.) ;
#38735 = ORIENTED_EDGE('',*,*,#27685,.T.) ;
#38736 = ORIENTED_EDGE('',*,*,#27685,.F.) ;
#38737 = ORIENTED_EDGE('',*,*,#27682,.F.) ;
#38738 = ORIENTED_EDGE('',*,*,#27686,.F.) ;
#38739 = ORIENTED_EDGE('',*,*,#27687,.F.) ;
#38740 = ORIENTED_EDGE('',*,*,#27688,.F.) ;
#38741 = ORIENTED_EDGE('',*,*,#27679,.F.) ;
#38742 = ORIENTED_EDGE('',*,*,#27689,.T.) ;
#38743 = ORIENTED_EDGE('',*,*,#27690,.T.) ;
#38744 = ORIENTED_EDGE('',*,*,#27686,.T.) ;
#38745 = ORIENTED_EDGE('',*,*,#27676,.F.) ;
#38746 = ORIENTED_EDGE('',*,*,#27668,.F.) ;
#38747 = ORIENTED_EDGE('',*,*,#27691,.F.) ;
#38748 = ORIENTED_EDGE('',*,*,#27692,.F.) ;
#38749 = ORIENTED_EDGE('',*,*,#27689,.F.) ;
#38750 = ORIENTED_EDGE('',*,*,#27693,.T.) ;
#38751 = ORIENTED_EDGE('',*,*,#27694,.F.) ;
#38752 = ORIENTED_EDGE('',*,*,#27695,.T.) ;
#38753 = ORIENTED_EDGE('',*,*,#27696,.T.) ;
#38754 = ORIENTED_EDGE('',*,*,#27673,.F.) ;
#38755 = ORIENTED_EDGE('',*,*,#27697,.T.) ;
#38756 = ORIENTED_EDGE('',*,*,#27693,.F.) ;
#38757 = ORIENTED_EDGE('',*,*,#27672,.F.) ;
#38758 = ORIENTED_EDGE('',*,*,#27698,.F.) ;
#38759 = ORIENTED_EDGE('',*,*,#27699,.T.) ;
#38760 = ORIENTED_EDGE('',*,*,#27700,.F.) ;
#38761 = ORIENTED_EDGE('',*,*,#27701,.F.) ;
#38762 = ORIENTED_EDGE('',*,*,#27702,.F.) ;
#38763 = ORIENTED_EDGE('',*,*,#27703,.F.) ;
#38764 = ORIENTED_EDGE('',*,*,#27704,.F.) ;
#38765 = ORIENTED_EDGE('',*,*,#27705,.F.) ;
#38766 = ORIENTED_EDGE('',*,*,#27706,.F.) ;
#38767 = ORIENTED_EDGE('',*,*,#27707,.F.) ;
#38768 = ORIENTED_EDGE('',*,*,#27708,.F.) ;
#38769 = ORIENTED_EDGE('',*,*,#27709,.F.) ;
#38770 = ORIENTED_EDGE('',*,*,#27710,.F.) ;
#38771 = ORIENTED_EDGE('',*,*,#27711,.F.) ;
#38772 = ORIENTED_EDGE('',*,*,#27694,.T.) ;
#38773 = ORIENTED_EDGE('',*,*,#27697,.F.) ;
#38774 = ORIENTED_EDGE('',*,*,#27712,.T.) ;
#38775 = ORIENTED_EDGE('',*,*,#27713,.T.) ;
#38776 = ORIENTED_EDGE('',*,*,#27714,.T.) ;
#38777 = ORIENTED_EDGE('',*,*,#27715,.T.) ;
#38778 = ORIENTED_EDGE('',*,*,#27716,.T.) ;
#38779 = ORIENTED_EDGE('',*,*,#27717,.T.) ;
#38780 = ORIENTED_EDGE('',*,*,#27718,.T.) ;
#38781 = ORIENTED_EDGE('',*,*,#27712,.F.) ;
#38782 = ORIENTED_EDGE('',*,*,#27719,.T.) ;
#38783 = ORIENTED_EDGE('',*,*,#27720,.T.) ;
#38784 = ORIENTED_EDGE('',*,*,#27721,.T.) ;
#38785 = ORIENTED_EDGE('',*,*,#27717,.F.) ;
#38786 = ORIENTED_EDGE('',*,*,#27722,.T.) ;
#38787 = ORIENTED_EDGE('',*,*,#27723,.T.) ;
#38788 = ORIENTED_EDGE('',*,*,#27724,.T.) ;
#38789 = ORIENTED_EDGE('',*,*,#27720,.F.) ;
#38790 = ORIENTED_EDGE('',*,*,#27723,.F.) ;
#38791 = ORIENTED_EDGE('',*,*,#27722,.F.) ;
#38792 = ORIENTED_EDGE('',*,*,#27725,.T.) ;
#38793 = ORIENTED_EDGE('',*,*,#27726,.T.) ;
#38794 = ORIENTED_EDGE('',*,*,#27727,.T.) ;
#38795 = ORIENTED_EDGE('',*,*,#27719,.F.) ;
#38796 = ORIENTED_EDGE('',*,*,#27728,.F.) ;
#38797 = ORIENTED_EDGE('',*,*,#27729,.F.) ;
#38798 = ORIENTED_EDGE('',*,*,#27730,.F.) ;
#38799 = ORIENTED_EDGE('',*,*,#27725,.F.) ;
#38800 = ORIENTED_EDGE('',*,*,#27715,.F.) ;
#38801 = ORIENTED_EDGE('',*,*,#27731,.T.) ;
#38802 = ORIENTED_EDGE('',*,*,#27732,.F.) ;
#38803 = ORIENTED_EDGE('',*,*,#27728,.T.) ;
#38804 = ORIENTED_EDGE('',*,*,#27716,.F.) ;
#38805 = ORIENTED_EDGE('',*,*,#27733,.T.) ;
#38806 = ORIENTED_EDGE('',*,*,#27734,.T.) ;
#38807 = ORIENTED_EDGE('',*,*,#27735,.T.) ;
#38808 = ORIENTED_EDGE('',*,*,#27736,.T.) ;
#38809 = ORIENTED_EDGE('',*,*,#27737,.T.) ;
#38810 = ORIENTED_EDGE('',*,*,#27738,.T.) ;
#38811 = ORIENTED_EDGE('',*,*,#27739,.T.) ;
#38812 = ORIENTED_EDGE('',*,*,#27733,.F.) ;
#38813 = ORIENTED_EDGE('',*,*,#27740,.T.) ;
#38814 = ORIENTED_EDGE('',*,*,#27741,.T.) ;
#38815 = ORIENTED_EDGE('',*,*,#27742,.T.) ;
#38816 = ORIENTED_EDGE('',*,*,#27738,.F.) ;
#38817 = ORIENTED_EDGE('',*,*,#27743,.T.) ;
#38818 = ORIENTED_EDGE('',*,*,#27741,.F.) ;
#38819 = ORIENTED_EDGE('',*,*,#27744,.T.) ;
#38820 = ORIENTED_EDGE('',*,*,#27745,.T.) ;
#38821 = ORIENTED_EDGE('',*,*,#27746,.T.) ;
#38822 = ORIENTED_EDGE('',*,*,#27747,.T.) ;
#38823 = ORIENTED_EDGE('',*,*,#27721,.F.) ;
#38824 = ORIENTED_EDGE('',*,*,#27748,.F.) ;
#38825 = ORIENTED_EDGE('',*,*,#27749,.F.) ;
#38826 = ORIENTED_EDGE('',*,*,#27750,.F.) ;
#38827 = ORIENTED_EDGE('',*,*,#27751,.F.) ;
#38828 = ORIENTED_EDGE('',*,*,#27752,.F.) ;
#38829 = ORIENTED_EDGE('',*,*,#27753,.F.) ;
#38830 = ORIENTED_EDGE('',*,*,#27754,.F.) ;
#38831 = ORIENTED_EDGE('',*,*,#27743,.F.) ;
#38832 = ORIENTED_EDGE('',*,*,#27740,.F.) ;
#38833 = ORIENTED_EDGE('',*,*,#27755,.F.) ;
#38834 = ORIENTED_EDGE('',*,*,#27756,.F.) ;
#38835 = ORIENTED_EDGE('',*,*,#27757,.F.) ;
#38836 = ORIENTED_EDGE('',*,*,#27758,.F.) ;
#38837 = ORIENTED_EDGE('',*,*,#27759,.F.) ;
#38838 = ORIENTED_EDGE('',*,*,#27718,.F.) ;
#38839 = ORIENTED_EDGE('',*,*,#27736,.F.) ;
#38840 = ORIENTED_EDGE('',*,*,#27760,.T.) ;
#38841 = ORIENTED_EDGE('',*,*,#27761,.T.) ;
#38842 = ORIENTED_EDGE('',*,*,#27755,.T.) ;
#38843 = ORIENTED_EDGE('',*,*,#27737,.F.) ;
#38844 = ORIENTED_EDGE('',*,*,#27734,.F.) ;
#38845 = ORIENTED_EDGE('',*,*,#27762,.T.) ;
#38846 = ORIENTED_EDGE('',*,*,#27763,.F.) ;
#38847 = ORIENTED_EDGE('',*,*,#27764,.T.) ;
#38848 = ORIENTED_EDGE('',*,*,#27735,.F.) ;
#38849 = ORIENTED_EDGE('',*,*,#27765,.T.) ;
#38850 = ORIENTED_EDGE('',*,*,#27766,.T.) ;
#38851 = ORIENTED_EDGE('',*,*,#27767,.T.) ;
#38852 = ORIENTED_EDGE('',*,*,#27766,.F.) ;
#38853 = ORIENTED_EDGE('',*,*,#27768,.T.) ;
#38854 = ORIENTED_EDGE('',*,*,#27769,.T.) ;
#38855 = ORIENTED_EDGE('',*,*,#27770,.T.) ;
#38856 = ORIENTED_EDGE('',*,*,#27765,.F.) ;
#38857 = ORIENTED_EDGE('',*,*,#27771,.T.) ;
#38858 = ORIENTED_EDGE('',*,*,#27772,.T.) ;
#38859 = ORIENTED_EDGE('',*,*,#27773,.T.) ;
#38860 = ORIENTED_EDGE('',*,*,#27774,.T.) ;
#38861 = ORIENTED_EDGE('',*,*,#27775,.T.) ;
#38862 = ORIENTED_EDGE('',*,*,#27769,.F.) ;
#38863 = ORIENTED_EDGE('',*,*,#27776,.T.) ;
#38864 = ORIENTED_EDGE('',*,*,#27777,.F.) ;
#38865 = ORIENTED_EDGE('',*,*,#27778,.F.) ;
#38866 = ORIENTED_EDGE('',*,*,#27779,.F.) ;
#38867 = ORIENTED_EDGE('',*,*,#27780,.F.) ;
#38868 = ORIENTED_EDGE('',*,*,#27781,.F.) ;
#38869 = ORIENTED_EDGE('',*,*,#27782,.F.) ;
#38870 = ORIENTED_EDGE('',*,*,#27783,.F.) ;
#38871 = ORIENTED_EDGE('',*,*,#27768,.F.) ;
#38872 = ORIENTED_EDGE('',*,*,#27775,.F.) ;
#38873 = ORIENTED_EDGE('',*,*,#27784,.F.) ;
#38874 = ORIENTED_EDGE('',*,*,#27776,.F.) ;
#38875 = ORIENTED_EDGE('',*,*,#27774,.F.) ;
#38876 = ORIENTED_EDGE('',*,*,#27785,.T.) ;
#38877 = ORIENTED_EDGE('',*,*,#27786,.F.) ;
#38878 = ORIENTED_EDGE('',*,*,#27777,.T.) ;
#38879 = ORIENTED_EDGE('',*,*,#27784,.T.) ;
#38880 = ORIENTED_EDGE('',*,*,#27773,.F.) ;
#38881 = ORIENTED_EDGE('',*,*,#27787,.T.) ;
#38882 = ORIENTED_EDGE('',*,*,#27788,.T.) ;
#38883 = ORIENTED_EDGE('',*,*,#27785,.F.) ;
#38884 = ORIENTED_EDGE('',*,*,#27641,.F.) ;
#38885 = ORIENTED_EDGE('',*,*,#27789,.T.) ;
#38886 = ORIENTED_EDGE('',*,*,#27790,.F.) ;
#38887 = ORIENTED_EDGE('',*,*,#27791,.T.) ;
#38888 = ORIENTED_EDGE('',*,*,#27652,.F.) ;
#38889 = ORIENTED_EDGE('',*,*,#27792,.F.) ;
#38890 = ORIENTED_EDGE('',*,*,#27793,.F.) ;
#38891 = ORIENTED_EDGE('',*,*,#27789,.F.) ;
#38892 = ORIENTED_EDGE('',*,*,#27645,.F.) ;
#38893 = ORIENTED_EDGE('',*,*,#27648,.F.) ;
#38894 = ORIENTED_EDGE('',*,*,#27794,.T.) ;
#38895 = ORIENTED_EDGE('',*,*,#27795,.T.) ;
#38896 = ORIENTED_EDGE('',*,*,#27796,.T.) ;
#38897 = ORIENTED_EDGE('',*,*,#27797,.T.) ;
#38898 = ORIENTED_EDGE('',*,*,#27684,.F.) ;
#38899 = ORIENTED_EDGE('',*,*,#27798,.T.) ;
#38900 = ORIENTED_EDGE('',*,*,#27795,.F.) ;
#38901 = ORIENTED_EDGE('',*,*,#27799,.T.) ;
#38902 = ORIENTED_EDGE('',*,*,#27797,.F.) ;
#38903 = ORIENTED_EDGE('',*,*,#27800,.F.) ;
#38904 = ORIENTED_EDGE('',*,*,#27801,.F.) ;
#38905 = ORIENTED_EDGE('',*,*,#27802,.F.) ;
#38906 = ORIENTED_EDGE('',*,*,#27803,.F.) ;
#38907 = ORIENTED_EDGE('',*,*,#27796,.F.) ;
#38908 = ORIENTED_EDGE('',*,*,#27804,.T.) ;
#38909 = ORIENTED_EDGE('',*,*,#27805,.T.) ;
#38910 = ORIENTED_EDGE('',*,*,#27800,.T.) ;
#38911 = ORIENTED_EDGE('',*,*,#27688,.T.) ;
#38912 = ORIENTED_EDGE('',*,*,#27806,.T.) ;
#38913 = ORIENTED_EDGE('',*,*,#27807,.T.) ;
#38914 = ORIENTED_EDGE('',*,*,#27808,.T.) ;
#38915 = ORIENTED_EDGE('',*,*,#27809,.F.) ;
#38916 = ORIENTED_EDGE('',*,*,#27810,.F.) ;
#38917 = ORIENTED_EDGE('',*,*,#27804,.F.) ;
#38918 = ORIENTED_EDGE('',*,*,#27798,.F.) ;
#38919 = ORIENTED_EDGE('',*,*,#27683,.F.) ;
#38920 = ORIENTED_EDGE('',*,*,#27811,.T.) ;
#38921 = ORIENTED_EDGE('',*,*,#27812,.T.) ;
#38922 = ORIENTED_EDGE('',*,*,#27813,.T.) ;
#38923 = ORIENTED_EDGE('',*,*,#27814,.T.) ;
#38924 = ORIENTED_EDGE('',*,*,#27724,.F.) ;
#38925 = ORIENTED_EDGE('',*,*,#27815,.T.) ;
#38926 = ORIENTED_EDGE('',*,*,#27812,.F.) ;
#38927 = ORIENTED_EDGE('',*,*,#27748,.T.) ;
#38928 = ORIENTED_EDGE('',*,*,#27813,.F.) ;
#38929 = ORIENTED_EDGE('',*,*,#27816,.T.) ;
#38930 = ORIENTED_EDGE('',*,*,#27817,.F.) ;
#38931 = ORIENTED_EDGE('',*,*,#27818,.T.) ;
#38932 = ORIENTED_EDGE('',*,*,#27815,.F.) ;
#38933 = ORIENTED_EDGE('',*,*,#27727,.F.) ;
#38934 = ORIENTED_EDGE('',*,*,#27819,.F.) ;
#38935 = ORIENTED_EDGE('',*,*,#27820,.F.) ;
#38936 = ORIENTED_EDGE('',*,*,#27821,.F.) ;
#38937 = ORIENTED_EDGE('',*,*,#27822,.F.) ;
#38938 = ORIENTED_EDGE('',*,*,#27816,.F.) ;
#38939 = ORIENTED_EDGE('',*,*,#27823,.T.) ;
#38940 = ORIENTED_EDGE('',*,*,#27824,.T.) ;
#38941 = ORIENTED_EDGE('',*,*,#27825,.T.) ;
#38942 = ORIENTED_EDGE('',*,*,#27826,.T.) ;
#38943 = ORIENTED_EDGE('',*,*,#27744,.F.) ;
#38944 = ORIENTED_EDGE('',*,*,#27754,.T.) ;
#38945 = ORIENTED_EDGE('',*,*,#27826,.F.) ;
#38946 = ORIENTED_EDGE('',*,*,#27706,.T.) ;
#38947 = ORIENTED_EDGE('',*,*,#27745,.F.) ;
#38948 = ORIENTED_EDGE('',*,*,#27823,.F.) ;
#38949 = ORIENTED_EDGE('',*,*,#27753,.T.) ;
#38950 = ORIENTED_EDGE('',*,*,#27827,.T.) ;
#38951 = ORIENTED_EDGE('',*,*,#27828,.T.) ;
#38952 = ORIENTED_EDGE('',*,*,#27732,.T.) ;
#38953 = ORIENTED_EDGE('',*,*,#27829,.T.) ;
#38954 = ORIENTED_EDGE('',*,*,#27830,.T.) ;
#38955 = ORIENTED_EDGE('',*,*,#27831,.T.) ;
#38956 = ORIENTED_EDGE('',*,*,#27832,.T.) ;
#38957 = ORIENTED_EDGE('',*,*,#27833,.T.) ;
#38958 = ORIENTED_EDGE('',*,*,#27726,.F.) ;
#38959 = ORIENTED_EDGE('',*,*,#27730,.T.) ;
#38960 = ORIENTED_EDGE('',*,*,#27831,.F.) ;
#38961 = ORIENTED_EDGE('',*,*,#27834,.T.) ;
#38962 = ORIENTED_EDGE('',*,*,#27832,.F.) ;
#38963 = ORIENTED_EDGE('',*,*,#27729,.T.) ;
#38964 = ORIENTED_EDGE('',*,*,#27763,.T.) ;
#38965 = ORIENTED_EDGE('',*,*,#27835,.T.) ;
#38966 = ORIENTED_EDGE('',*,*,#27836,.T.) ;
#38967 = ORIENTED_EDGE('',*,*,#27837,.T.) ;
#38968 = ORIENTED_EDGE('',*,*,#27838,.T.) ;
#38969 = ORIENTED_EDGE('',*,*,#27839,.T.) ;
#38970 = ORIENTED_EDGE('',*,*,#27835,.F.) ;
#38971 = ORIENTED_EDGE('',*,*,#27840,.T.) ;
#38972 = ORIENTED_EDGE('',*,*,#27841,.T.) ;
#38973 = ORIENTED_EDGE('',*,*,#27842,.T.) ;
#38974 = ORIENTED_EDGE('',*,*,#27838,.F.) ;
#38975 = ORIENTED_EDGE('',*,*,#27843,.T.) ;
#38976 = ORIENTED_EDGE('',*,*,#27746,.F.) ;
#38977 = ORIENTED_EDGE('',*,*,#27705,.T.) ;
#38978 = ORIENTED_EDGE('',*,*,#27841,.F.) ;
#38979 = ORIENTED_EDGE('',*,*,#27844,.T.) ;
#38980 = ORIENTED_EDGE('',*,*,#27742,.F.) ;
#38981 = ORIENTED_EDGE('',*,*,#27747,.F.) ;
#38982 = ORIENTED_EDGE('',*,*,#27837,.F.) ;
#38983 = ORIENTED_EDGE('',*,*,#27845,.F.) ;
#38984 = ORIENTED_EDGE('',*,*,#27846,.F.) ;
#38985 = ORIENTED_EDGE('',*,*,#27847,.T.) ;
#38986 = ORIENTED_EDGE('',*,*,#27848,.T.) ;
#38987 = ORIENTED_EDGE('',*,*,#27849,.F.) ;
#38988 = ORIENTED_EDGE('',*,*,#27850,.T.) ;
#38989 = ORIENTED_EDGE('',*,*,#27760,.F.) ;
#38990 = ORIENTED_EDGE('',*,*,#27764,.F.) ;
#38991 = ORIENTED_EDGE('',*,*,#27836,.F.) ;
#38992 = ORIENTED_EDGE('',*,*,#27851,.T.) ;
#38993 = ORIENTED_EDGE('',*,*,#27852,.F.) ;
#38994 = ORIENTED_EDGE('',*,*,#27845,.T.) ;
#38995 = ORIENTED_EDGE('',*,*,#27839,.F.) ;
#38996 = ORIENTED_EDGE('',*,*,#27853,.F.) ;
#38997 = ORIENTED_EDGE('',*,*,#27854,.F.) ;
#38998 = ORIENTED_EDGE('',*,*,#27855,.F.) ;
#38999 = ORIENTED_EDGE('',*,*,#27856,.F.) ;
#39000 = ORIENTED_EDGE('',*,*,#27857,.F.) ;
#39001 = ORIENTED_EDGE('',*,*,#27858,.F.) ;
#39002 = ORIENTED_EDGE('',*,*,#27851,.F.) ;
#39003 = ORIENTED_EDGE('',*,*,#27842,.F.) ;
#39004 = ORIENTED_EDGE('',*,*,#27704,.T.) ;
#39005 = ORIENTED_EDGE('',*,*,#27859,.F.) ;
#39006 = ORIENTED_EDGE('',*,*,#27860,.F.) ;
#39007 = ORIENTED_EDGE('',*,*,#27853,.T.) ;
#39008 = ORIENTED_EDGE('',*,*,#27861,.F.) ;
#39009 = ORIENTED_EDGE('',*,*,#27862,.F.) ;
#39010 = ORIENTED_EDGE('',*,*,#27863,.F.) ;
#39011 = ORIENTED_EDGE('',*,*,#27864,.T.) ;
#39012 = ORIENTED_EDGE('',*,*,#27865,.T.) ;
#39013 = ORIENTED_EDGE('',*,*,#27862,.T.) ;
#39014 = ORIENTED_EDGE('',*,*,#27866,.T.) ;
#39015 = ORIENTED_EDGE('',*,*,#27867,.T.) ;
#39016 = ORIENTED_EDGE('',*,*,#27868,.T.) ;
#39017 = ORIENTED_EDGE('',*,*,#27869,.T.) ;
#39018 = ORIENTED_EDGE('',*,*,#27870,.T.) ;
#39019 = ORIENTED_EDGE('',*,*,#27871,.T.) ;
#39020 = ORIENTED_EDGE('',*,*,#27872,.T.) ;
#39021 = ORIENTED_EDGE('',*,*,#27869,.F.) ;
#39022 = ORIENTED_EDGE('',*,*,#27873,.T.) ;
#39023 = ORIENTED_EDGE('',*,*,#27874,.T.) ;
#39024 = ORIENTED_EDGE('',*,*,#27875,.T.) ;
#39025 = ORIENTED_EDGE('',*,*,#27871,.F.) ;
#39026 = ORIENTED_EDGE('',*,*,#27876,.T.) ;
#39027 = ORIENTED_EDGE('',*,*,#27877,.T.) ;
#39028 = ORIENTED_EDGE('',*,*,#27878,.T.) ;
#39029 = ORIENTED_EDGE('',*,*,#27874,.F.) ;
#39030 = ORIENTED_EDGE('',*,*,#27879,.T.) ;
#39031 = ORIENTED_EDGE('',*,*,#27880,.T.) ;
#39032 = ORIENTED_EDGE('',*,*,#27881,.T.) ;
#39033 = ORIENTED_EDGE('',*,*,#27877,.F.) ;
#39034 = ORIENTED_EDGE('',*,*,#27882,.T.) ;
#39035 = ORIENTED_EDGE('',*,*,#27883,.T.) ;
#39036 = ORIENTED_EDGE('',*,*,#27884,.T.) ;
#39037 = ORIENTED_EDGE('',*,*,#27880,.F.) ;
#39038 = ORIENTED_EDGE('',*,*,#27885,.T.) ;
#39039 = ORIENTED_EDGE('',*,*,#27863,.T.) ;
#39040 = ORIENTED_EDGE('',*,*,#27886,.T.) ;
#39041 = ORIENTED_EDGE('',*,*,#27883,.F.) ;
#39042 = ORIENTED_EDGE('',*,*,#27887,.T.) ;
#39043 = ORIENTED_EDGE('',*,*,#27888,.T.) ;
#39044 = ORIENTED_EDGE('',*,*,#27889,.T.) ;
#39045 = ORIENTED_EDGE('',*,*,#27861,.T.) ;
#39046 = ORIENTED_EDGE('',*,*,#27890,.T.) ;
#39047 = ORIENTED_EDGE('',*,*,#27891,.T.) ;
#39048 = ORIENTED_EDGE('',*,*,#27892,.T.) ;
#39049 = ORIENTED_EDGE('',*,*,#27888,.F.) ;
#39050 = ORIENTED_EDGE('',*,*,#27893,.T.) ;
#39051 = ORIENTED_EDGE('',*,*,#27870,.F.) ;
#39052 = ORIENTED_EDGE('',*,*,#27872,.F.) ;
#39053 = ORIENTED_EDGE('',*,*,#27875,.F.) ;
#39054 = ORIENTED_EDGE('',*,*,#27878,.F.) ;
#39055 = ORIENTED_EDGE('',*,*,#27881,.F.) ;
#39056 = ORIENTED_EDGE('',*,*,#27884,.F.) ;
#39057 = ORIENTED_EDGE('',*,*,#27886,.F.) ;
#39058 = ORIENTED_EDGE('',*,*,#27865,.F.) ;
#39059 = ORIENTED_EDGE('',*,*,#27894,.F.) ;
#39060 = ORIENTED_EDGE('',*,*,#27895,.T.) ;
#39061 = ORIENTED_EDGE('',*,*,#27896,.F.) ;
#39062 = ORIENTED_EDGE('',*,*,#27897,.T.) ;
#39063 = ORIENTED_EDGE('',*,*,#27898,.F.) ;
#39064 = ORIENTED_EDGE('',*,*,#27899,.F.) ;
#39065 = ORIENTED_EDGE('',*,*,#27900,.T.) ;
#39066 = ORIENTED_EDGE('',*,*,#27901,.F.) ;
#39067 = ORIENTED_EDGE('',*,*,#27902,.T.) ;
#39068 = ORIENTED_EDGE('',*,*,#27903,.F.) ;
#39069 = ORIENTED_EDGE('',*,*,#27864,.F.) ;
#39070 = ORIENTED_EDGE('',*,*,#27904,.T.) ;
#39071 = ORIENTED_EDGE('',*,*,#27905,.T.) ;
#39072 = ORIENTED_EDGE('',*,*,#27894,.T.) ;
#39073 = ORIENTED_EDGE('',*,*,#27866,.F.) ;
#39074 = ORIENTED_EDGE('',*,*,#27889,.F.) ;
#39075 = ORIENTED_EDGE('',*,*,#27892,.F.) ;
#39076 = ORIENTED_EDGE('',*,*,#27906,.F.) ;
#39077 = ORIENTED_EDGE('',*,*,#27907,.F.) ;
#39078 = ORIENTED_EDGE('',*,*,#27908,.F.) ;
#39079 = ORIENTED_EDGE('',*,*,#27909,.T.) ;
#39080 = ORIENTED_EDGE('',*,*,#27910,.T.) ;
#39081 = ORIENTED_EDGE('',*,*,#27911,.T.) ;
#39082 = ORIENTED_EDGE('',*,*,#27912,.F.) ;
#39083 = ORIENTED_EDGE('',*,*,#27913,.T.) ;
#39084 = ORIENTED_EDGE('',*,*,#27914,.T.) ;
#39085 = ORIENTED_EDGE('',*,*,#27910,.F.) ;
#39086 = ORIENTED_EDGE('',*,*,#27915,.T.) ;
#39087 = ORIENTED_EDGE('',*,*,#27915,.F.) ;
#39088 = ORIENTED_EDGE('',*,*,#27909,.F.) ;
#39089 = ORIENTED_EDGE('',*,*,#27916,.F.) ;
#39090 = ORIENTED_EDGE('',*,*,#27917,.F.) ;
#39091 = ORIENTED_EDGE('',*,*,#27918,.T.) ;
#39092 = ORIENTED_EDGE('',*,*,#27893,.F.) ;
#39093 = ORIENTED_EDGE('',*,*,#27919,.T.) ;
#39094 = ORIENTED_EDGE('',*,*,#27920,.T.) ;
#39095 = ORIENTED_EDGE('',*,*,#27921,.T.) ;
#39096 = ORIENTED_EDGE('',*,*,#27922,.T.) ;
#39097 = ORIENTED_EDGE('',*,*,#27923,.T.) ;
#39098 = ORIENTED_EDGE('',*,*,#27924,.T.) ;
#39099 = ORIENTED_EDGE('',*,*,#27920,.F.) ;
#39100 = ORIENTED_EDGE('',*,*,#27887,.F.) ;
#39101 = ORIENTED_EDGE('',*,*,#27925,.T.) ;
#39102 = ORIENTED_EDGE('',*,*,#27926,.F.) ;
#39103 = ORIENTED_EDGE('',*,*,#27927,.F.) ;
#39104 = ORIENTED_EDGE('',*,*,#27922,.F.) ;
#39105 = ORIENTED_EDGE('',*,*,#27919,.F.) ;
#39106 = ORIENTED_EDGE('',*,*,#27890,.F.) ;
#39107 = ORIENTED_EDGE('',*,*,#27928,.T.) ;
#39108 = ORIENTED_EDGE('',*,*,#27929,.F.) ;
#39109 = ORIENTED_EDGE('',*,*,#27930,.F.) ;
#39110 = ORIENTED_EDGE('',*,*,#27931,.F.) ;
#39111 = ORIENTED_EDGE('',*,*,#27932,.T.) ;
#39112 = ORIENTED_EDGE('',*,*,#27857,.T.) ;
#39113 = ORIENTED_EDGE('',*,*,#27929,.T.) ;
#39114 = ORIENTED_EDGE('',*,*,#27933,.T.) ;
#39115 = ORIENTED_EDGE('',*,*,#27852,.T.) ;
#39116 = ORIENTED_EDGE('',*,*,#27858,.T.) ;
#39117 = ORIENTED_EDGE('',*,*,#27932,.F.) ;
#39118 = ORIENTED_EDGE('',*,*,#27934,.T.) ;
#39119 = ORIENTED_EDGE('',*,*,#27935,.T.) ;
#39120 = ORIENTED_EDGE('',*,*,#27936,.T.) ;
#39121 = ORIENTED_EDGE('',*,*,#27930,.T.) ;
#39122 = ORIENTED_EDGE('',*,*,#27856,.T.) ;
#39123 = ORIENTED_EDGE('',*,*,#27935,.F.) ;
#39124 = ORIENTED_EDGE('',*,*,#27937,.T.) ;
#39125 = ORIENTED_EDGE('',*,*,#27938,.T.) ;
#39126 = ORIENTED_EDGE('',*,*,#27939,.T.) ;
#39127 = ORIENTED_EDGE('',*,*,#27940,.T.) ;
#39128 = ORIENTED_EDGE('',*,*,#27941,.T.) ;
#39129 = ORIENTED_EDGE('',*,*,#27938,.F.) ;
#39130 = ORIENTED_EDGE('',*,*,#27942,.T.) ;
#39131 = ORIENTED_EDGE('',*,*,#27943,.T.) ;
#39132 = ORIENTED_EDGE('',*,*,#27944,.T.) ;
#39133 = ORIENTED_EDGE('',*,*,#27940,.F.) ;
#39134 = ORIENTED_EDGE('',*,*,#27945,.T.) ;
#39135 = ORIENTED_EDGE('',*,*,#27946,.T.) ;
#39136 = ORIENTED_EDGE('',*,*,#27947,.T.) ;
#39137 = ORIENTED_EDGE('',*,*,#27943,.F.) ;
#39138 = ORIENTED_EDGE('',*,*,#27948,.T.) ;
#39139 = ORIENTED_EDGE('',*,*,#27949,.T.) ;
#39140 = ORIENTED_EDGE('',*,*,#27950,.T.) ;
#39141 = ORIENTED_EDGE('',*,*,#27951,.T.) ;
#39142 = ORIENTED_EDGE('',*,*,#27952,.T.) ;
#39143 = ORIENTED_EDGE('',*,*,#27626,.T.) ;
#39144 = ORIENTED_EDGE('',*,*,#27953,.T.) ;
#39145 = ORIENTED_EDGE('',*,*,#27627,.T.) ;
#39146 = ORIENTED_EDGE('',*,*,#27952,.F.) ;
#39147 = ORIENTED_EDGE('',*,*,#27954,.T.) ;
#39148 = ORIENTED_EDGE('',*,*,#27955,.T.) ;
#39149 = ORIENTED_EDGE('',*,*,#27628,.T.) ;
#39150 = ORIENTED_EDGE('',*,*,#27953,.F.) ;
#39151 = ORIENTED_EDGE('',*,*,#27956,.T.) ;
#39152 = ORIENTED_EDGE('',*,*,#27957,.T.) ;
#39153 = ORIENTED_EDGE('',*,*,#27611,.T.) ;
#39154 = ORIENTED_EDGE('',*,*,#27955,.F.) ;
#39155 = ORIENTED_EDGE('',*,*,#27958,.T.) ;
#39156 = ORIENTED_EDGE('',*,*,#27959,.T.) ;
#39157 = ORIENTED_EDGE('',*,*,#27960,.T.) ;
#39158 = ORIENTED_EDGE('',*,*,#27957,.F.) ;
#39159 = ORIENTED_EDGE('',*,*,#27961,.T.) ;
#39160 = ORIENTED_EDGE('',*,*,#27962,.T.) ;
#39161 = ORIENTED_EDGE('',*,*,#27963,.T.) ;
#39162 = ORIENTED_EDGE('',*,*,#27959,.F.) ;
#39163 = ORIENTED_EDGE('',*,*,#27964,.T.) ;
#39164 = ORIENTED_EDGE('',*,*,#27931,.T.) ;
#39165 = ORIENTED_EDGE('',*,*,#27965,.T.) ;
#39166 = ORIENTED_EDGE('',*,*,#27962,.F.) ;
#39167 = ORIENTED_EDGE('',*,*,#27966,.T.) ;
#39168 = ORIENTED_EDGE('',*,*,#27934,.F.) ;
#39169 = ORIENTED_EDGE('',*,*,#27967,.F.) ;
#39170 = ORIENTED_EDGE('',*,*,#27968,.F.) ;
#39171 = ORIENTED_EDGE('',*,*,#27846,.T.) ;
#39172 = ORIENTED_EDGE('',*,*,#27933,.F.) ;
#39173 = ORIENTED_EDGE('',*,*,#27928,.F.) ;
#39174 = ORIENTED_EDGE('',*,*,#27966,.F.) ;
#39175 = ORIENTED_EDGE('',*,*,#27964,.F.) ;
#39176 = ORIENTED_EDGE('',*,*,#27961,.F.) ;
#39177 = ORIENTED_EDGE('',*,*,#27958,.F.) ;
#39178 = ORIENTED_EDGE('',*,*,#27969,.F.) ;
#39179 = ORIENTED_EDGE('',*,*,#27970,.T.) ;
#39180 = ORIENTED_EDGE('',*,*,#27967,.T.) ;
#39181 = ORIENTED_EDGE('',*,*,#27956,.F.) ;
#39182 = ORIENTED_EDGE('',*,*,#27971,.F.) ;
#39183 = ORIENTED_EDGE('',*,*,#27972,.T.) ;
#39184 = ORIENTED_EDGE('',*,*,#27969,.T.) ;
#39185 = ORIENTED_EDGE('',*,*,#27954,.F.) ;
#39186 = ORIENTED_EDGE('',*,*,#27973,.F.) ;
#39187 = ORIENTED_EDGE('',*,*,#27974,.F.) ;
#39188 = ORIENTED_EDGE('',*,*,#27975,.F.) ;
#39189 = ORIENTED_EDGE('',*,*,#27976,.T.) ;
#39190 = ORIENTED_EDGE('',*,*,#27971,.T.) ;
#39191 = ORIENTED_EDGE('',*,*,#27951,.F.) ;
#39192 = ORIENTED_EDGE('',*,*,#27977,.F.) ;
#39193 = ORIENTED_EDGE('',*,*,#27978,.F.) ;
#39194 = ORIENTED_EDGE('',*,*,#27973,.T.) ;
#39195 = ORIENTED_EDGE('',*,*,#27950,.F.) ;
#39196 = ORIENTED_EDGE('',*,*,#27625,.T.) ;
#39197 = ORIENTED_EDGE('',*,*,#27979,.F.) ;
#39198 = ORIENTED_EDGE('',*,*,#27980,.T.) ;
#39199 = ORIENTED_EDGE('',*,*,#27981,.T.) ;
#39200 = ORIENTED_EDGE('',*,*,#27982,.T.) ;
#39201 = ORIENTED_EDGE('',*,*,#27983,.T.) ;
#39202 = ORIENTED_EDGE('',*,*,#27984,.T.) ;
#39203 = ORIENTED_EDGE('',*,*,#27985,.T.) ;
#39204 = ORIENTED_EDGE('',*,*,#27986,.T.) ;
#39205 = ORIENTED_EDGE('',*,*,#27987,.T.) ;
#39206 = ORIENTED_EDGE('',*,*,#27981,.F.) ;
#39207 = ORIENTED_EDGE('',*,*,#27988,.T.) ;
#39208 = ORIENTED_EDGE('',*,*,#27989,.T.) ;
#39209 = ORIENTED_EDGE('',*,*,#27990,.T.) ;
#39210 = ORIENTED_EDGE('',*,*,#27986,.F.) ;
#39211 = ORIENTED_EDGE('',*,*,#27991,.T.) ;
#39212 = ORIENTED_EDGE('',*,*,#27992,.T.) ;
#39213 = ORIENTED_EDGE('',*,*,#27993,.T.) ;
#39214 = ORIENTED_EDGE('',*,*,#27989,.F.) ;
#39215 = ORIENTED_EDGE('',*,*,#27994,.T.) ;
#39216 = ORIENTED_EDGE('',*,*,#27995,.T.) ;
#39217 = ORIENTED_EDGE('',*,*,#27996,.T.) ;
#39218 = ORIENTED_EDGE('',*,*,#27992,.F.) ;
#39219 = ORIENTED_EDGE('',*,*,#27997,.T.) ;
#39220 = ORIENTED_EDGE('',*,*,#27995,.F.) ;
#39221 = ORIENTED_EDGE('',*,*,#27998,.T.) ;
#39222 = ORIENTED_EDGE('',*,*,#27999,.T.) ;
#39223 = ORIENTED_EDGE('',*,*,#28000,.T.) ;
#39224 = ORIENTED_EDGE('',*,*,#27998,.F.) ;
#39225 = ORIENTED_EDGE('',*,*,#27997,.F.) ;
#39226 = ORIENTED_EDGE('',*,*,#27994,.F.) ;
#39227 = ORIENTED_EDGE('',*,*,#28001,.T.) ;
#39228 = ORIENTED_EDGE('',*,*,#28002,.F.) ;
#39229 = ORIENTED_EDGE('',*,*,#28003,.F.) ;
#39230 = ORIENTED_EDGE('',*,*,#28004,.T.) ;
#39231 = ORIENTED_EDGE('',*,*,#27993,.F.) ;
#39232 = ORIENTED_EDGE('',*,*,#28005,.F.) ;
#39233 = ORIENTED_EDGE('',*,*,#28006,.F.) ;
#39234 = ORIENTED_EDGE('',*,*,#28007,.T.) ;
#39235 = ORIENTED_EDGE('',*,*,#28008,.F.) ;
#39236 = ORIENTED_EDGE('',*,*,#28009,.F.) ;
#39237 = ORIENTED_EDGE('',*,*,#28010,.F.) ;
#39238 = ORIENTED_EDGE('',*,*,#27987,.F.) ;
#39239 = ORIENTED_EDGE('',*,*,#27990,.F.) ;
#39240 = ORIENTED_EDGE('',*,*,#27991,.F.) ;
#39241 = ORIENTED_EDGE('',*,*,#28011,.F.) ;
#39242 = ORIENTED_EDGE('',*,*,#28001,.F.) ;
#39243 = ORIENTED_EDGE('',*,*,#27988,.F.) ;
#39244 = ORIENTED_EDGE('',*,*,#27985,.F.) ;
#39245 = ORIENTED_EDGE('',*,*,#27984,.F.) ;
#39246 = ORIENTED_EDGE('',*,*,#28012,.T.) ;
#39247 = ORIENTED_EDGE('',*,*,#28013,.F.) ;
#39248 = ORIENTED_EDGE('',*,*,#28011,.T.) ;
#39249 = ORIENTED_EDGE('',*,*,#27629,.T.) ;
#39250 = ORIENTED_EDGE('',*,*,#28014,.T.) ;
#39251 = ORIENTED_EDGE('',*,*,#28015,.T.) ;
#39252 = ORIENTED_EDGE('',*,*,#28016,.T.) ;
#39253 = ORIENTED_EDGE('',*,*,#28017,.T.) ;
#39254 = ORIENTED_EDGE('',*,*,#28018,.T.) ;
#39255 = ORIENTED_EDGE('',*,*,#27630,.T.) ;
#39256 = ORIENTED_EDGE('',*,*,#28016,.F.) ;
#39257 = ORIENTED_EDGE('',*,*,#27631,.T.) ;
#39258 = ORIENTED_EDGE('',*,*,#28018,.F.) ;
#39259 = ORIENTED_EDGE('',*,*,#28019,.T.) ;
#39260 = ORIENTED_EDGE('',*,*,#28020,.T.) ;
#39261 = ORIENTED_EDGE('',*,*,#27632,.T.) ;
#39262 = ORIENTED_EDGE('',*,*,#28020,.F.) ;
#39263 = ORIENTED_EDGE('',*,*,#28021,.T.) ;
#39264 = ORIENTED_EDGE('',*,*,#28014,.F.) ;
#39265 = ORIENTED_EDGE('',*,*,#28017,.F.) ;
#39266 = ORIENTED_EDGE('',*,*,#28022,.F.) ;
#39267 = ORIENTED_EDGE('',*,*,#28023,.F.) ;
#39268 = ORIENTED_EDGE('',*,*,#28024,.T.) ;
#39269 = ORIENTED_EDGE('',*,*,#28015,.F.) ;
#39270 = ORIENTED_EDGE('',*,*,#28025,.T.) ;
#39271 = ORIENTED_EDGE('',*,*,#28026,.F.) ;
#39272 = ORIENTED_EDGE('',*,*,#28022,.T.) ;
#39273 = ORIENTED_EDGE('',*,*,#27530,.T.) ;
#39274 = ORIENTED_EDGE('',*,*,#27552,.T.) ;
#39275 = ORIENTED_EDGE('',*,*,#27549,.T.) ;
#39276 = ORIENTED_EDGE('',*,*,#27546,.T.) ;
#39277 = ORIENTED_EDGE('',*,*,#27543,.T.) ;
#39278 = ORIENTED_EDGE('',*,*,#27540,.T.) ;
#39279 = ORIENTED_EDGE('',*,*,#27537,.T.) ;
#39280 = ORIENTED_EDGE('',*,*,#27534,.T.) ;
#39281 = ORIENTED_EDGE('',*,*,#28027,.T.) ;
#39282 = ORIENTED_EDGE('',*,*,#28028,.T.) ;
#39283 = ORIENTED_EDGE('',*,*,#28029,.T.) ;
#39284 = ORIENTED_EDGE('',*,*,#28030,.T.) ;
#39285 = ORIENTED_EDGE('',*,*,#28031,.T.) ;
#39286 = ORIENTED_EDGE('',*,*,#28027,.F.) ;
#39287 = ORIENTED_EDGE('',*,*,#28032,.T.) ;
#39288 = ORIENTED_EDGE('',*,*,#28033,.T.) ;
#39289 = ORIENTED_EDGE('',*,*,#28034,.T.) ;
#39290 = ORIENTED_EDGE('',*,*,#28030,.F.) ;
#39291 = ORIENTED_EDGE('',*,*,#28035,.T.) ;
#39292 = ORIENTED_EDGE('',*,*,#28035,.F.) ;
#39293 = ORIENTED_EDGE('',*,*,#28036,.F.) ;
#39294 = ORIENTED_EDGE('',*,*,#28037,.T.) ;
#39295 = ORIENTED_EDGE('',*,*,#28038,.T.) ;
#39296 = ORIENTED_EDGE('',*,*,#28039,.T.) ;
#39297 = ORIENTED_EDGE('',*,*,#28040,.T.) ;
#39298 = ORIENTED_EDGE('',*,*,#28032,.F.) ;
#39299 = ORIENTED_EDGE('',*,*,#28029,.F.) ;
#39300 = ORIENTED_EDGE('',*,*,#28041,.T.) ;
#39301 = ORIENTED_EDGE('',*,*,#28042,.T.) ;
#39302 = ORIENTED_EDGE('',*,*,#28036,.T.) ;
#39303 = ORIENTED_EDGE('',*,*,#28028,.F.) ;
#39304 = ORIENTED_EDGE('',*,*,#28043,.T.) ;
#39305 = ORIENTED_EDGE('',*,*,#28044,.F.) ;
#39306 = ORIENTED_EDGE('',*,*,#28045,.T.) ;
#39307 = ORIENTED_EDGE('',*,*,#28046,.F.) ;
#39308 = ORIENTED_EDGE('',*,*,#28047,.F.) ;
#39309 = ORIENTED_EDGE('',*,*,#28048,.F.) ;
#39310 = ORIENTED_EDGE('',*,*,#27780,.T.) ;
#39311 = ORIENTED_EDGE('',*,*,#28049,.T.) ;
#39312 = ORIENTED_EDGE('',*,*,#28047,.T.) ;
#39313 = ORIENTED_EDGE('',*,*,#28050,.T.) ;
#39314 = ORIENTED_EDGE('',*,*,#27912,.T.) ;
#39315 = ORIENTED_EDGE('',*,*,#28051,.T.) ;
#39316 = ORIENTED_EDGE('',*,*,#28048,.T.) ;
#39317 = ORIENTED_EDGE('',*,*,#28052,.T.) ;
#39318 = ORIENTED_EDGE('',*,*,#28053,.F.) ;
#39319 = ORIENTED_EDGE('',*,*,#28054,.F.) ;
#39320 = ORIENTED_EDGE('',*,*,#28055,.T.) ;
#39321 = ORIENTED_EDGE('',*,*,#28056,.F.) ;
#39322 = ORIENTED_EDGE('',*,*,#27914,.F.) ;
#39323 = ORIENTED_EDGE('',*,*,#28057,.T.) ;
#39324 = ORIENTED_EDGE('',*,*,#28054,.T.) ;
#39325 = ORIENTED_EDGE('',*,*,#28058,.T.) ;
#39326 = ORIENTED_EDGE('',*,*,#27782,.T.) ;
#39327 = ORIENTED_EDGE('',*,*,#28059,.T.) ;
#39328 = ORIENTED_EDGE('',*,*,#28056,.T.) ;
#39329 = ORIENTED_EDGE('',*,*,#28060,.T.) ;
#39330 = ORIENTED_EDGE('',*,*,#28046,.T.) ;
#39331 = ORIENTED_EDGE('',*,*,#28061,.T.) ;
#39332 = ORIENTED_EDGE('',*,*,#28053,.T.) ;
#39333 = ORIENTED_EDGE('',*,*,#28062,.T.) ;
#39334 = ORIENTED_EDGE('',*,*,#27908,.T.) ;
#39335 = ORIENTED_EDGE('',*,*,#28052,.F.) ;
#39336 = ORIENTED_EDGE('',*,*,#28049,.F.) ;
#39337 = ORIENTED_EDGE('',*,*,#27779,.T.) ;
#39338 = ORIENTED_EDGE('',*,*,#28063,.F.) ;
#39339 = ORIENTED_EDGE('',*,*,#28064,.F.) ;
#39340 = ORIENTED_EDGE('',*,*,#28065,.F.) ;
#39341 = ORIENTED_EDGE('',*,*,#28066,.T.) ;
#39342 = ORIENTED_EDGE('',*,*,#28067,.T.) ;
#39343 = ORIENTED_EDGE('',*,*,#28068,.T.) ;
#39344 = ORIENTED_EDGE('',*,*,#28069,.F.) ;
#39345 = ORIENTED_EDGE('',*,*,#28070,.F.) ;
#39346 = ORIENTED_EDGE('',*,*,#28071,.F.) ;
#39347 = ORIENTED_EDGE('',*,*,#28072,.F.) ;
#39348 = ORIENTED_EDGE('',*,*,#28073,.F.) ;
#39349 = ORIENTED_EDGE('',*,*,#28074,.F.) ;
#39350 = ORIENTED_EDGE('',*,*,#28075,.F.) ;
#39351 = ORIENTED_EDGE('',*,*,#28076,.F.) ;
#39352 = ORIENTED_EDGE('',*,*,#28077,.F.) ;
#39353 = ORIENTED_EDGE('',*,*,#28078,.F.) ;
#39354 = ORIENTED_EDGE('',*,*,#28079,.F.) ;
#39355 = ORIENTED_EDGE('',*,*,#28080,.F.) ;
#39356 = ORIENTED_EDGE('',*,*,#28081,.F.) ;
#39357 = ORIENTED_EDGE('',*,*,#28082,.T.) ;
#39358 = ORIENTED_EDGE('',*,*,#28083,.T.) ;
#39359 = ORIENTED_EDGE('',*,*,#28084,.T.) ;
#39360 = ORIENTED_EDGE('',*,*,#28085,.T.) ;
#39361 = ORIENTED_EDGE('',*,*,#28086,.F.) ;
#39362 = ORIENTED_EDGE('',*,*,#28087,.F.) ;
#39363 = ORIENTED_EDGE('',*,*,#28088,.F.) ;
#39364 = ORIENTED_EDGE('',*,*,#28089,.F.) ;
#39365 = ORIENTED_EDGE('',*,*,#28090,.F.) ;
#39366 = ORIENTED_EDGE('',*,*,#28091,.F.) ;
#39367 = ORIENTED_EDGE('',*,*,#28092,.T.) ;
#39368 = ORIENTED_EDGE('',*,*,#28093,.T.) ;
#39369 = ORIENTED_EDGE('',*,*,#28094,.T.) ;
#39370 = ORIENTED_EDGE('',*,*,#28095,.T.) ;
#39371 = ORIENTED_EDGE('',*,*,#28096,.T.) ;
#39372 = ORIENTED_EDGE('',*,*,#28097,.T.) ;
#39373 = ORIENTED_EDGE('',*,*,#28098,.F.) ;
#39374 = ORIENTED_EDGE('',*,*,#28099,.F.) ;
#39375 = ORIENTED_EDGE('',*,*,#28100,.T.) ;
#39376 = ORIENTED_EDGE('',*,*,#28101,.T.) ;
#39377 = ORIENTED_EDGE('',*,*,#28102,.T.) ;
#39378 = ORIENTED_EDGE('',*,*,#28103,.T.) ;
#39379 = ORIENTED_EDGE('',*,*,#28104,.T.) ;
#39380 = ORIENTED_EDGE('',*,*,#28105,.T.) ;
#39381 = ORIENTED_EDGE('',*,*,#28106,.F.) ;
#39382 = ORIENTED_EDGE('',*,*,#28107,.T.) ;
#39383 = ORIENTED_EDGE('',*,*,#28108,.T.) ;
#39384 = ORIENTED_EDGE('',*,*,#28109,.T.) ;
#39385 = ORIENTED_EDGE('',*,*,#28110,.T.) ;
#39386 = ORIENTED_EDGE('',*,*,#28111,.T.) ;
#39387 = ORIENTED_EDGE('',*,*,#28112,.T.) ;
#39388 = ORIENTED_EDGE('',*,*,#28113,.T.) ;
#39389 = ORIENTED_EDGE('',*,*,#28114,.T.) ;
#39390 = ORIENTED_EDGE('',*,*,#28115,.T.) ;
#39391 = ORIENTED_EDGE('',*,*,#28116,.T.) ;
#39392 = ORIENTED_EDGE('',*,*,#28117,.T.) ;
#39393 = ORIENTED_EDGE('',*,*,#28118,.F.) ;
#39394 = ORIENTED_EDGE('',*,*,#28119,.T.) ;
#39395 = ORIENTED_EDGE('',*,*,#28120,.T.) ;
#39396 = ORIENTED_EDGE('',*,*,#28121,.T.) ;
#39397 = ORIENTED_EDGE('',*,*,#28039,.F.) ;
#39398 = ORIENTED_EDGE('',*,*,#28122,.T.) ;
#39399 = ORIENTED_EDGE('',*,*,#28123,.F.) ;
#39400 = ORIENTED_EDGE('',*,*,#28124,.F.) ;
#39401 = ORIENTED_EDGE('',*,*,#28125,.F.) ;
#39402 = ORIENTED_EDGE('',*,*,#28126,.F.) ;
#39403 = ORIENTED_EDGE('',*,*,#28127,.F.) ;
#39404 = ORIENTED_EDGE('',*,*,#28128,.T.) ;
#39405 = ORIENTED_EDGE('',*,*,#28129,.F.) ;
#39406 = ORIENTED_EDGE('',*,*,#28130,.T.) ;
#39407 = ORIENTED_EDGE('',*,*,#28131,.F.) ;
#39408 = ORIENTED_EDGE('',*,*,#28132,.F.) ;
#39409 = ORIENTED_EDGE('',*,*,#28133,.T.) ;
#39410 = ORIENTED_EDGE('',*,*,#28134,.F.) ;
#39411 = ORIENTED_EDGE('',*,*,#28135,.T.) ;
#39412 = ORIENTED_EDGE('',*,*,#28136,.F.) ;
#39413 = ORIENTED_EDGE('',*,*,#28137,.F.) ;
#39414 = ORIENTED_EDGE('',*,*,#28138,.T.) ;
#39415 = ORIENTED_EDGE('',*,*,#28139,.F.) ;
#39416 = ORIENTED_EDGE('',*,*,#28140,.T.) ;
#39417 = ORIENTED_EDGE('',*,*,#28141,.T.) ;
#39418 = ORIENTED_EDGE('',*,*,#28142,.T.) ;
#39419 = ORIENTED_EDGE('',*,*,#28143,.F.) ;
#39420 = ORIENTED_EDGE('',*,*,#28144,.F.) ;
#39421 = ORIENTED_EDGE('',*,*,#28145,.F.) ;
#39422 = ORIENTED_EDGE('',*,*,#28146,.F.) ;
#39423 = ORIENTED_EDGE('',*,*,#28147,.F.) ;
#39424 = ORIENTED_EDGE('',*,*,#28148,.F.) ;
#39425 = ORIENTED_EDGE('',*,*,#28149,.F.) ;
#39426 = ORIENTED_EDGE('',*,*,#28150,.F.) ;
#39427 = ORIENTED_EDGE('',*,*,#28151,.F.) ;
#39428 = ORIENTED_EDGE('',*,*,#28152,.T.) ;
#39429 = ORIENTED_EDGE('',*,*,#27906,.T.) ;
#39430 = ORIENTED_EDGE('',*,*,#27891,.F.) ;
#39431 = ORIENTED_EDGE('',*,*,#27921,.F.) ;
#39432 = ORIENTED_EDGE('',*,*,#28153,.F.) ;
#39433 = ORIENTED_EDGE('',*,*,#28154,.F.) ;
#39434 = ORIENTED_EDGE('',*,*,#28155,.F.) ;
#39435 = ORIENTED_EDGE('',*,*,#28156,.F.) ;
#39436 = ORIENTED_EDGE('',*,*,#28157,.F.) ;
#39437 = ORIENTED_EDGE('',*,*,#28158,.F.) ;
#39438 = ORIENTED_EDGE('',*,*,#28159,.F.) ;
#39439 = ORIENTED_EDGE('',*,*,#28160,.F.) ;
#39440 = ORIENTED_EDGE('',*,*,#28161,.F.) ;
#39441 = ORIENTED_EDGE('',*,*,#28162,.T.) ;
#39442 = ORIENTED_EDGE('',*,*,#28163,.T.) ;
#39443 = ORIENTED_EDGE('',*,*,#28164,.T.) ;
#39444 = ORIENTED_EDGE('',*,*,#27916,.T.) ;
#39445 = ORIENTED_EDGE('',*,*,#28165,.F.) ;
#39446 = ORIENTED_EDGE('',*,*,#28166,.F.) ;
#39447 = ORIENTED_EDGE('',*,*,#28167,.F.) ;
#39448 = ORIENTED_EDGE('',*,*,#28168,.F.) ;
#39449 = ORIENTED_EDGE('',*,*,#28169,.F.) ;
#39450 = ORIENTED_EDGE('',*,*,#28170,.F.) ;
#39451 = ORIENTED_EDGE('',*,*,#28171,.F.) ;
#39452 = ORIENTED_EDGE('',*,*,#28172,.F.) ;
#39453 = ORIENTED_EDGE('',*,*,#28173,.F.) ;
#39454 = ORIENTED_EDGE('',*,*,#28174,.F.) ;
#39455 = ORIENTED_EDGE('',*,*,#28175,.F.) ;
#39456 = ORIENTED_EDGE('',*,*,#28176,.F.) ;
#39457 = ORIENTED_EDGE('',*,*,#28177,.F.) ;
#39458 = ORIENTED_EDGE('',*,*,#28178,.F.) ;
#39459 = ORIENTED_EDGE('',*,*,#28179,.F.) ;
#39460 = ORIENTED_EDGE('',*,*,#28180,.F.) ;
#39461 = ORIENTED_EDGE('',*,*,#28181,.F.) ;
#39462 = ORIENTED_EDGE('',*,*,#28182,.F.) ;
#39463 = ORIENTED_EDGE('',*,*,#28183,.F.) ;
#39464 = ORIENTED_EDGE('',*,*,#28184,.F.) ;
#39465 = ORIENTED_EDGE('',*,*,#28185,.F.) ;
#39466 = ORIENTED_EDGE('',*,*,#28186,.F.) ;
#39467 = ORIENTED_EDGE('',*,*,#28187,.F.) ;
#39468 = ORIENTED_EDGE('',*,*,#28188,.F.) ;
#39469 = ORIENTED_EDGE('',*,*,#28189,.F.) ;
#39470 = ORIENTED_EDGE('',*,*,#28190,.F.) ;
#39471 = ORIENTED_EDGE('',*,*,#28191,.F.) ;
#39472 = ORIENTED_EDGE('',*,*,#28192,.F.) ;
#39473 = ORIENTED_EDGE('',*,*,#28193,.F.) ;
#39474 = ORIENTED_EDGE('',*,*,#28194,.F.) ;
#39475 = ORIENTED_EDGE('',*,*,#28195,.F.) ;
#39476 = ORIENTED_EDGE('',*,*,#28196,.F.) ;
#39477 = ORIENTED_EDGE('',*,*,#28197,.F.) ;
#39478 = ORIENTED_EDGE('',*,*,#28198,.F.) ;
#39479 = ORIENTED_EDGE('',*,*,#28199,.F.) ;
#39480 = ORIENTED_EDGE('',*,*,#28200,.F.) ;
#39481 = ORIENTED_EDGE('',*,*,#28201,.F.) ;
#39482 = ORIENTED_EDGE('',*,*,#28202,.F.) ;
#39483 = ORIENTED_EDGE('',*,*,#27637,.F.) ;
#39484 = ORIENTED_EDGE('',*,*,#27635,.F.) ;
#39485 = ORIENTED_EDGE('',*,*,#28203,.F.) ;
#39486 = ORIENTED_EDGE('',*,*,#28204,.F.) ;
#39487 = ORIENTED_EDGE('',*,*,#28205,.F.) ;
#39488 = ORIENTED_EDGE('',*,*,#28206,.F.) ;
#39489 = ORIENTED_EDGE('',*,*,#28207,.F.) ;
#39490 = ORIENTED_EDGE('',*,*,#28208,.F.) ;
#39491 = ORIENTED_EDGE('',*,*,#28209,.F.) ;
#39492 = ORIENTED_EDGE('',*,*,#28210,.F.) ;
#39493 = ORIENTED_EDGE('',*,*,#28211,.F.) ;
#39494 = ORIENTED_EDGE('',*,*,#28212,.F.) ;
#39495 = ORIENTED_EDGE('',*,*,#28213,.F.) ;
#39496 = ORIENTED_EDGE('',*,*,#28214,.F.) ;
#39497 = ORIENTED_EDGE('',*,*,#28215,.F.) ;
#39498 = ORIENTED_EDGE('',*,*,#28216,.F.) ;
#39499 = ORIENTED_EDGE('',*,*,#28217,.F.) ;
#39500 = ORIENTED_EDGE('',*,*,#28218,.F.) ;
#39501 = ORIENTED_EDGE('',*,*,#28219,.F.) ;
#39502 = ORIENTED_EDGE('',*,*,#28220,.F.) ;
#39503 = ORIENTED_EDGE('',*,*,#28221,.F.) ;
#39504 = ORIENTED_EDGE('',*,*,#28222,.F.) ;
#39505 = ORIENTED_EDGE('',*,*,#28223,.F.) ;
#39506 = ORIENTED_EDGE('',*,*,#28224,.F.) ;
#39507 = ORIENTED_EDGE('',*,*,#28225,.F.) ;
#39508 = ORIENTED_EDGE('',*,*,#28226,.F.) ;
#39509 = ORIENTED_EDGE('',*,*,#28227,.F.) ;
#39510 = ORIENTED_EDGE('',*,*,#28050,.F.) ;
#39511 = ORIENTED_EDGE('',*,*,#28062,.F.) ;
#39512 = ORIENTED_EDGE('',*,*,#28059,.F.) ;
#39513 = ORIENTED_EDGE('',*,*,#27781,.T.) ;
#39514 = ORIENTED_EDGE('',*,*,#28228,.T.) ;
#39515 = ORIENTED_EDGE('',*,*,#28229,.F.) ;
#39516 = ORIENTED_EDGE('',*,*,#28230,.F.) ;
#39517 = ORIENTED_EDGE('',*,*,#28231,.F.) ;
#39518 = ORIENTED_EDGE('',*,*,#27867,.F.) ;
#39519 = ORIENTED_EDGE('',*,*,#27903,.T.) ;
#39520 = ORIENTED_EDGE('',*,*,#28232,.T.) ;
#39521 = ORIENTED_EDGE('',*,*,#28229,.T.) ;
#39522 = ORIENTED_EDGE('',*,*,#28233,.T.) ;
#39523 = ORIENTED_EDGE('',*,*,#28234,.T.) ;
#39524 = ORIENTED_EDGE('',*,*,#28126,.T.) ;
#39525 = ORIENTED_EDGE('',*,*,#28230,.T.) ;
#39526 = ORIENTED_EDGE('',*,*,#28235,.T.) ;
#39527 = ORIENTED_EDGE('',*,*,#28236,.T.) ;
#39528 = ORIENTED_EDGE('',*,*,#28237,.T.) ;
#39529 = ORIENTED_EDGE('',*,*,#28231,.T.) ;
#39530 = ORIENTED_EDGE('',*,*,#28125,.T.) ;
#39531 = ORIENTED_EDGE('',*,*,#28238,.T.) ;
#39532 = ORIENTED_EDGE('',*,*,#28239,.T.) ;
#39533 = ORIENTED_EDGE('',*,*,#28236,.F.) ;
#39534 = ORIENTED_EDGE('',*,*,#28124,.T.) ;
#39535 = ORIENTED_EDGE('',*,*,#28235,.F.) ;
#39536 = ORIENTED_EDGE('',*,*,#28232,.F.) ;
#39537 = ORIENTED_EDGE('',*,*,#27902,.F.) ;
#39538 = ORIENTED_EDGE('',*,*,#28240,.F.) ;
#39539 = ORIENTED_EDGE('',*,*,#27868,.F.) ;
#39540 = ORIENTED_EDGE('',*,*,#28233,.F.) ;
#39541 = ORIENTED_EDGE('',*,*,#28228,.F.) ;
#39542 = ORIENTED_EDGE('',*,*,#28237,.F.) ;
#39543 = ORIENTED_EDGE('',*,*,#28241,.T.) ;
#39544 = ORIENTED_EDGE('',*,*,#28242,.F.) ;
#39545 = ORIENTED_EDGE('',*,*,#28243,.F.) ;
#39546 = ORIENTED_EDGE('',*,*,#28239,.F.) ;
#39547 = ORIENTED_EDGE('',*,*,#28244,.F.) ;
#39548 = ORIENTED_EDGE('',*,*,#28245,.T.) ;
#39549 = ORIENTED_EDGE('',*,*,#28041,.F.) ;
#39550 = ORIENTED_EDGE('',*,*,#28045,.F.) ;
#39551 = ORIENTED_EDGE('',*,*,#28246,.T.) ;
#39552 = ORIENTED_EDGE('',*,*,#28247,.F.) ;
#39553 = ORIENTED_EDGE('',*,*,#28241,.F.) ;
#39554 = ORIENTED_EDGE('',*,*,#27905,.F.) ;
#39555 = ORIENTED_EDGE('',*,*,#28248,.T.) ;
#39556 = ORIENTED_EDGE('',*,*,#28151,.T.) ;
#39557 = ORIENTED_EDGE('',*,*,#28249,.T.) ;
#39558 = ORIENTED_EDGE('',*,*,#28250,.T.) ;
#39559 = ORIENTED_EDGE('',*,*,#28251,.F.) ;
#39560 = ORIENTED_EDGE('',*,*,#28252,.F.) ;
#39561 = ORIENTED_EDGE('',*,*,#28253,.F.) ;
#39562 = ORIENTED_EDGE('',*,*,#28254,.F.) ;
#39563 = ORIENTED_EDGE('',*,*,#27767,.F.) ;
#39564 = ORIENTED_EDGE('',*,*,#28255,.T.) ;
#39565 = ORIENTED_EDGE('',*,*,#28256,.T.) ;
#39566 = ORIENTED_EDGE('',*,*,#28257,.T.) ;
#39567 = ORIENTED_EDGE('',*,*,#28258,.T.) ;
#39568 = ORIENTED_EDGE('',*,*,#28259,.T.) ;
#39569 = ORIENTED_EDGE('',*,*,#28256,.F.) ;
#39570 = ORIENTED_EDGE('',*,*,#28260,.T.) ;
#39571 = ORIENTED_EDGE('',*,*,#28261,.T.) ;
#39572 = ORIENTED_EDGE('',*,*,#28262,.T.) ;
#39573 = ORIENTED_EDGE('',*,*,#28258,.F.) ;
#39574 = ORIENTED_EDGE('',*,*,#28263,.T.) ;
#39575 = ORIENTED_EDGE('',*,*,#28264,.T.) ;
#39576 = ORIENTED_EDGE('',*,*,#28265,.T.) ;
#39577 = ORIENTED_EDGE('',*,*,#28261,.F.) ;
#39578 = ORIENTED_EDGE('',*,*,#28266,.T.) ;
#39579 = ORIENTED_EDGE('',*,*,#28253,.T.) ;
#39580 = ORIENTED_EDGE('',*,*,#28267,.T.) ;
#39581 = ORIENTED_EDGE('',*,*,#28264,.F.) ;
#39582 = ORIENTED_EDGE('',*,*,#28268,.T.) ;
#39583 = ORIENTED_EDGE('',*,*,#28269,.T.) ;
#39584 = ORIENTED_EDGE('',*,*,#28270,.T.) ;
#39585 = ORIENTED_EDGE('',*,*,#28271,.T.) ;
#39586 = ORIENTED_EDGE('',*,*,#28272,.T.) ;
#39587 = ORIENTED_EDGE('',*,*,#28273,.T.) ;
#39588 = ORIENTED_EDGE('',*,*,#28274,.T.) ;
#39589 = ORIENTED_EDGE('',*,*,#28271,.F.) ;
#39590 = ORIENTED_EDGE('',*,*,#28275,.T.) ;
#39591 = ORIENTED_EDGE('',*,*,#28254,.T.) ;
#39592 = ORIENTED_EDGE('',*,*,#28276,.T.) ;
#39593 = ORIENTED_EDGE('',*,*,#28273,.F.) ;
#39594 = ORIENTED_EDGE('',*,*,#28277,.T.) ;
#39595 = ORIENTED_EDGE('',*,*,#28278,.F.) ;
#39596 = ORIENTED_EDGE('',*,*,#28279,.F.) ;
#39597 = ORIENTED_EDGE('',*,*,#28280,.T.) ;
#39598 = ORIENTED_EDGE('',*,*,#28281,.F.) ;
#39599 = ORIENTED_EDGE('',*,*,#27923,.F.) ;
#39600 = ORIENTED_EDGE('',*,*,#28282,.T.) ;
#39601 = ORIENTED_EDGE('',*,*,#28283,.T.) ;
#39602 = ORIENTED_EDGE('',*,*,#28153,.T.) ;
#39603 = ORIENTED_EDGE('',*,*,#27924,.F.) ;
#39604 = ORIENTED_EDGE('',*,*,#28284,.T.) ;
#39605 = ORIENTED_EDGE('',*,*,#28154,.T.) ;
#39606 = ORIENTED_EDGE('',*,*,#28283,.F.) ;
#39607 = ORIENTED_EDGE('',*,*,#28285,.T.) ;
#39608 = ORIENTED_EDGE('',*,*,#28286,.T.) ;
#39609 = ORIENTED_EDGE('',*,*,#28155,.T.) ;
#39610 = ORIENTED_EDGE('',*,*,#28284,.F.) ;
#39611 = ORIENTED_EDGE('',*,*,#28287,.T.) ;
#39612 = ORIENTED_EDGE('',*,*,#28288,.T.) ;
#39613 = ORIENTED_EDGE('',*,*,#28156,.T.) ;
#39614 = ORIENTED_EDGE('',*,*,#28286,.F.) ;
#39615 = ORIENTED_EDGE('',*,*,#28289,.T.) ;
#39616 = ORIENTED_EDGE('',*,*,#28288,.F.) ;
#39617 = ORIENTED_EDGE('',*,*,#28290,.T.) ;
#39618 = ORIENTED_EDGE('',*,*,#28279,.T.) ;
#39619 = ORIENTED_EDGE('',*,*,#28157,.T.) ;
#39620 = ORIENTED_EDGE('',*,*,#28281,.T.) ;
#39621 = ORIENTED_EDGE('',*,*,#28291,.T.) ;
#39622 = ORIENTED_EDGE('',*,*,#28252,.T.) ;
#39623 = ORIENTED_EDGE('',*,*,#28292,.T.) ;
#39624 = ORIENTED_EDGE('',*,*,#28293,.T.) ;
#39625 = ORIENTED_EDGE('',*,*,#28158,.T.) ;
#39626 = ORIENTED_EDGE('',*,*,#28278,.T.) ;
#39627 = ORIENTED_EDGE('',*,*,#28294,.T.) ;
#39628 = ORIENTED_EDGE('',*,*,#28295,.T.) ;
#39629 = ORIENTED_EDGE('',*,*,#28159,.T.) ;
#39630 = ORIENTED_EDGE('',*,*,#28293,.F.) ;
#39631 = ORIENTED_EDGE('',*,*,#28296,.T.) ;
#39632 = ORIENTED_EDGE('',*,*,#28297,.T.) ;
#39633 = ORIENTED_EDGE('',*,*,#28160,.T.) ;
#39634 = ORIENTED_EDGE('',*,*,#28295,.F.) ;
#39635 = ORIENTED_EDGE('',*,*,#28298,.T.) ;
#39636 = ORIENTED_EDGE('',*,*,#28299,.F.) ;
#39637 = ORIENTED_EDGE('',*,*,#28161,.T.) ;
#39638 = ORIENTED_EDGE('',*,*,#28297,.F.) ;
#39639 = ORIENTED_EDGE('',*,*,#28300,.F.) ;
#39640 = ORIENTED_EDGE('',*,*,#27770,.F.) ;
#39641 = ORIENTED_EDGE('',*,*,#27783,.T.) ;
#39642 = ORIENTED_EDGE('',*,*,#28060,.F.) ;
#39643 = ORIENTED_EDGE('',*,*,#28055,.F.) ;
#39644 = ORIENTED_EDGE('',*,*,#28057,.F.) ;
#39645 = ORIENTED_EDGE('',*,*,#27913,.F.) ;
#39646 = ORIENTED_EDGE('',*,*,#27918,.F.) ;
#39647 = ORIENTED_EDGE('',*,*,#28301,.T.) ;
#39648 = ORIENTED_EDGE('',*,*,#28302,.T.) ;
#39649 = ORIENTED_EDGE('',*,*,#28303,.T.) ;
#39650 = ORIENTED_EDGE('',*,*,#28272,.F.) ;
#39651 = ORIENTED_EDGE('',*,*,#28274,.F.) ;
#39652 = ORIENTED_EDGE('',*,*,#28276,.F.) ;
#39653 = ORIENTED_EDGE('',*,*,#28268,.F.) ;
#39654 = ORIENTED_EDGE('',*,*,#28266,.F.) ;
#39655 = ORIENTED_EDGE('',*,*,#28263,.F.) ;
#39656 = ORIENTED_EDGE('',*,*,#28260,.F.) ;
#39657 = ORIENTED_EDGE('',*,*,#28255,.F.) ;
#39658 = ORIENTED_EDGE('',*,*,#27771,.F.) ;
#39659 = ORIENTED_EDGE('',*,*,#28257,.F.) ;
#39660 = ORIENTED_EDGE('',*,*,#28304,.T.) ;
#39661 = ORIENTED_EDGE('',*,*,#28305,.F.) ;
#39662 = ORIENTED_EDGE('',*,*,#28306,.F.) ;
#39663 = ORIENTED_EDGE('',*,*,#28307,.F.) ;
#39664 = ORIENTED_EDGE('',*,*,#28259,.F.) ;
#39665 = ORIENTED_EDGE('',*,*,#28308,.T.) ;
#39666 = ORIENTED_EDGE('',*,*,#28309,.F.) ;
#39667 = ORIENTED_EDGE('',*,*,#28304,.F.) ;
#39668 = ORIENTED_EDGE('',*,*,#28262,.F.) ;
#39669 = ORIENTED_EDGE('',*,*,#28310,.F.) ;
#39670 = ORIENTED_EDGE('',*,*,#28311,.F.) ;
#39671 = ORIENTED_EDGE('',*,*,#28308,.F.) ;
#39672 = ORIENTED_EDGE('',*,*,#28265,.F.) ;
#39673 = ORIENTED_EDGE('',*,*,#28312,.T.) ;
#39674 = ORIENTED_EDGE('',*,*,#28313,.F.) ;
#39675 = ORIENTED_EDGE('',*,*,#28310,.T.) ;
#39676 = ORIENTED_EDGE('',*,*,#28267,.F.) ;
#39677 = ORIENTED_EDGE('',*,*,#28291,.F.) ;
#39678 = ORIENTED_EDGE('',*,*,#28280,.F.) ;
#39679 = ORIENTED_EDGE('',*,*,#28290,.F.) ;
#39680 = ORIENTED_EDGE('',*,*,#28314,.T.) ;
#39681 = ORIENTED_EDGE('',*,*,#28315,.F.) ;
#39682 = ORIENTED_EDGE('',*,*,#28316,.F.) ;
#39683 = ORIENTED_EDGE('',*,*,#28317,.F.) ;
#39684 = ORIENTED_EDGE('',*,*,#28318,.F.) ;
#39685 = ORIENTED_EDGE('',*,*,#28319,.F.) ;
#39686 = ORIENTED_EDGE('',*,*,#28320,.F.) ;
#39687 = ORIENTED_EDGE('',*,*,#28321,.F.) ;
#39688 = ORIENTED_EDGE('',*,*,#28312,.F.) ;
#39689 = ORIENTED_EDGE('',*,*,#28289,.F.) ;
#39690 = ORIENTED_EDGE('',*,*,#28322,.T.) ;
#39691 = ORIENTED_EDGE('',*,*,#28323,.F.) ;
#39692 = ORIENTED_EDGE('',*,*,#28314,.F.) ;
#39693 = ORIENTED_EDGE('',*,*,#28287,.F.) ;
#39694 = ORIENTED_EDGE('',*,*,#28324,.T.) ;
#39695 = ORIENTED_EDGE('',*,*,#28325,.F.) ;
#39696 = ORIENTED_EDGE('',*,*,#28322,.F.) ;
#39697 = ORIENTED_EDGE('',*,*,#28285,.F.) ;
#39698 = ORIENTED_EDGE('',*,*,#28326,.F.) ;
#39699 = ORIENTED_EDGE('',*,*,#28327,.F.) ;
#39700 = ORIENTED_EDGE('',*,*,#28324,.F.) ;
#39701 = ORIENTED_EDGE('',*,*,#28282,.F.) ;
#39702 = ORIENTED_EDGE('',*,*,#27927,.T.) ;
#39703 = ORIENTED_EDGE('',*,*,#28328,.F.) ;
#39704 = ORIENTED_EDGE('',*,*,#28329,.F.) ;
#39705 = ORIENTED_EDGE('',*,*,#28330,.F.) ;
#39706 = ORIENTED_EDGE('',*,*,#28326,.T.) ;
#39707 = ORIENTED_EDGE('',*,*,#28331,.F.) ;
#39708 = ORIENTED_EDGE('',*,*,#28332,.F.) ;
#39709 = ORIENTED_EDGE('',*,*,#28333,.F.) ;
#39710 = ORIENTED_EDGE('',*,*,#28334,.T.) ;
#39711 = ORIENTED_EDGE('',*,*,#28335,.F.) ;
#39712 = ORIENTED_EDGE('',*,*,#28336,.T.) ;
#39713 = ORIENTED_EDGE('',*,*,#28332,.T.) ;
#39714 = ORIENTED_EDGE('',*,*,#28337,.T.) ;
#39715 = ORIENTED_EDGE('',*,*,#28338,.F.) ;
#39716 = ORIENTED_EDGE('',*,*,#28339,.F.) ;
#39717 = ORIENTED_EDGE('',*,*,#28340,.T.) ;
#39718 = ORIENTED_EDGE('',*,*,#28341,.F.) ;
#39719 = ORIENTED_EDGE('',*,*,#28342,.T.) ;
#39720 = ORIENTED_EDGE('',*,*,#28343,.T.) ;
#39721 = ORIENTED_EDGE('',*,*,#28339,.T.) ;
#39722 = ORIENTED_EDGE('',*,*,#28344,.T.) ;
#39723 = ORIENTED_EDGE('',*,*,#28342,.F.) ;
#39724 = ORIENTED_EDGE('',*,*,#28345,.T.) ;
#39725 = ORIENTED_EDGE('',*,*,#28331,.T.) ;
#39726 = ORIENTED_EDGE('',*,*,#28346,.T.) ;
#39727 = ORIENTED_EDGE('',*,*,#28347,.T.) ;
#39728 = ORIENTED_EDGE('',*,*,#28348,.F.) ;
#39729 = ORIENTED_EDGE('',*,*,#28349,.F.) ;
#39730 = ORIENTED_EDGE('',*,*,#28350,.F.) ;
#39731 = ORIENTED_EDGE('',*,*,#28351,.F.) ;
#39732 = ORIENTED_EDGE('',*,*,#28352,.F.) ;
#39733 = ORIENTED_EDGE('',*,*,#28353,.T.) ;
#39734 = ORIENTED_EDGE('',*,*,#28354,.F.) ;
#39735 = ORIENTED_EDGE('',*,*,#28355,.T.) ;
#39736 = ORIENTED_EDGE('',*,*,#28356,.T.) ;
#39737 = ORIENTED_EDGE('',*,*,#28352,.T.) ;
#39738 = ORIENTED_EDGE('',*,*,#28357,.T.) ;
#39739 = ORIENTED_EDGE('',*,*,#28348,.T.) ;
#39740 = ORIENTED_EDGE('',*,*,#28358,.T.) ;
#39741 = ORIENTED_EDGE('',*,*,#28355,.F.) ;
#39742 = ORIENTED_EDGE('',*,*,#28359,.T.) ;
#39743 = ORIENTED_EDGE('',*,*,#28360,.T.) ;
#39744 = ORIENTED_EDGE('',*,*,#28361,.T.) ;
#39745 = ORIENTED_EDGE('',*,*,#28354,.T.) ;
#39746 = ORIENTED_EDGE('',*,*,#28362,.T.) ;
#39747 = ORIENTED_EDGE('',*,*,#28363,.T.) ;
#39748 = ORIENTED_EDGE('',*,*,#28364,.T.) ;
#39749 = ORIENTED_EDGE('',*,*,#28360,.F.) ;
#39750 = ORIENTED_EDGE('',*,*,#28365,.T.) ;
#39751 = ORIENTED_EDGE('',*,*,#28366,.T.) ;
#39752 = ORIENTED_EDGE('',*,*,#28367,.T.) ;
#39753 = ORIENTED_EDGE('',*,*,#28363,.F.) ;
#39754 = ORIENTED_EDGE('',*,*,#27708,.T.) ;
#39755 = ORIENTED_EDGE('',*,*,#27825,.F.) ;
#39756 = ORIENTED_EDGE('',*,*,#28368,.T.) ;
#39757 = ORIENTED_EDGE('',*,*,#28366,.F.) ;
#39758 = ORIENTED_EDGE('',*,*,#27707,.T.) ;
#39759 = ORIENTED_EDGE('',*,*,#28369,.F.) ;
#39760 = ORIENTED_EDGE('',*,*,#28370,.T.) ;
#39761 = ORIENTED_EDGE('',*,*,#28351,.T.) ;
#39762 = ORIENTED_EDGE('',*,*,#28371,.T.) ;
#39763 = ORIENTED_EDGE('',*,*,#28372,.T.) ;
#39764 = ORIENTED_EDGE('',*,*,#28373,.T.) ;
#39765 = ORIENTED_EDGE('',*,*,#27827,.F.) ;
#39766 = ORIENTED_EDGE('',*,*,#27752,.T.) ;
#39767 = ORIENTED_EDGE('',*,*,#28374,.T.) ;
#39768 = ORIENTED_EDGE('',*,*,#28375,.T.) ;
#39769 = ORIENTED_EDGE('',*,*,#28372,.F.) ;
#39770 = ORIENTED_EDGE('',*,*,#27751,.T.) ;
#39771 = ORIENTED_EDGE('',*,*,#28376,.T.) ;
#39772 = ORIENTED_EDGE('',*,*,#28377,.T.) ;
#39773 = ORIENTED_EDGE('',*,*,#28374,.F.) ;
#39774 = ORIENTED_EDGE('',*,*,#27750,.T.) ;
#39775 = ORIENTED_EDGE('',*,*,#27811,.F.) ;
#39776 = ORIENTED_EDGE('',*,*,#28378,.T.) ;
#39777 = ORIENTED_EDGE('',*,*,#28376,.F.) ;
#39778 = ORIENTED_EDGE('',*,*,#27749,.T.) ;
#39779 = ORIENTED_EDGE('',*,*,#28379,.F.) ;
#39780 = ORIENTED_EDGE('',*,*,#28380,.T.) ;
#39781 = ORIENTED_EDGE('',*,*,#28349,.T.) ;
#39782 = ORIENTED_EDGE('',*,*,#28381,.T.) ;
#39783 = ORIENTED_EDGE('',*,*,#28382,.T.) ;
#39784 = ORIENTED_EDGE('',*,*,#28383,.T.) ;
#39785 = ORIENTED_EDGE('',*,*,#28350,.T.) ;
#39786 = ORIENTED_EDGE('',*,*,#28384,.T.) ;
#39787 = ORIENTED_EDGE('',*,*,#28385,.T.) ;
#39788 = ORIENTED_EDGE('',*,*,#28386,.T.) ;
#39789 = ORIENTED_EDGE('',*,*,#28382,.F.) ;
#39790 = ORIENTED_EDGE('',*,*,#28387,.T.) ;
#39791 = ORIENTED_EDGE('',*,*,#28388,.T.) ;
#39792 = ORIENTED_EDGE('',*,*,#28389,.T.) ;
#39793 = ORIENTED_EDGE('',*,*,#28385,.F.) ;
#39794 = ORIENTED_EDGE('',*,*,#28390,.T.) ;
#39795 = ORIENTED_EDGE('',*,*,#28391,.T.) ;
#39796 = ORIENTED_EDGE('',*,*,#28392,.T.) ;
#39797 = ORIENTED_EDGE('',*,*,#28388,.F.) ;
#39798 = ORIENTED_EDGE('',*,*,#28393,.T.) ;
#39799 = ORIENTED_EDGE('',*,*,#28394,.T.) ;
#39800 = ORIENTED_EDGE('',*,*,#28395,.T.) ;
#39801 = ORIENTED_EDGE('',*,*,#28391,.F.) ;
#39802 = ORIENTED_EDGE('',*,*,#28396,.T.) ;
#39803 = ORIENTED_EDGE('',*,*,#28397,.T.) ;
#39804 = ORIENTED_EDGE('',*,*,#28398,.T.) ;
#39805 = ORIENTED_EDGE('',*,*,#28394,.F.) ;
#39806 = ORIENTED_EDGE('',*,*,#28399,.T.) ;
#39807 = ORIENTED_EDGE('',*,*,#28400,.T.) ;
#39808 = ORIENTED_EDGE('',*,*,#28401,.T.) ;
#39809 = ORIENTED_EDGE('',*,*,#28397,.F.) ;
#39810 = ORIENTED_EDGE('',*,*,#28402,.T.) ;
#39811 = ORIENTED_EDGE('',*,*,#28403,.T.) ;
#39812 = ORIENTED_EDGE('',*,*,#28404,.T.) ;
#39813 = ORIENTED_EDGE('',*,*,#28400,.F.) ;
#39814 = ORIENTED_EDGE('',*,*,#28405,.T.) ;
#39815 = ORIENTED_EDGE('',*,*,#28341,.T.) ;
#39816 = ORIENTED_EDGE('',*,*,#28406,.T.) ;
#39817 = ORIENTED_EDGE('',*,*,#28403,.F.) ;
#39818 = ORIENTED_EDGE('',*,*,#28407,.T.) ;
#39819 = ORIENTED_EDGE('',*,*,#28408,.T.) ;
#39820 = ORIENTED_EDGE('',*,*,#28409,.T.) ;
#39821 = ORIENTED_EDGE('',*,*,#28333,.T.) ;
#39822 = ORIENTED_EDGE('',*,*,#28410,.T.) ;
#39823 = ORIENTED_EDGE('',*,*,#28408,.F.) ;
#39824 = ORIENTED_EDGE('',*,*,#28411,.T.) ;
#39825 = ORIENTED_EDGE('',*,*,#28412,.T.) ;
#39826 = ORIENTED_EDGE('',*,*,#28413,.T.) ;
#39827 = ORIENTED_EDGE('',*,*,#27817,.T.) ;
#39828 = ORIENTED_EDGE('',*,*,#27822,.T.) ;
#39829 = ORIENTED_EDGE('',*,*,#28412,.F.) ;
#39830 = ORIENTED_EDGE('',*,*,#28414,.T.) ;
#39831 = ORIENTED_EDGE('',*,*,#28415,.F.) ;
#39832 = ORIENTED_EDGE('',*,*,#28416,.T.) ;
#39833 = ORIENTED_EDGE('',*,*,#28338,.T.) ;
#39834 = ORIENTED_EDGE('',*,*,#28417,.T.) ;
#39835 = ORIENTED_EDGE('',*,*,#28346,.F.) ;
#39836 = ORIENTED_EDGE('',*,*,#28334,.F.) ;
#39837 = ORIENTED_EDGE('',*,*,#28409,.F.) ;
#39838 = ORIENTED_EDGE('',*,*,#28413,.F.) ;
#39839 = ORIENTED_EDGE('',*,*,#27821,.T.) ;
#39840 = ORIENTED_EDGE('',*,*,#28418,.F.) ;
#39841 = ORIENTED_EDGE('',*,*,#28419,.T.) ;
#39842 = ORIENTED_EDGE('',*,*,#28365,.F.) ;
#39843 = ORIENTED_EDGE('',*,*,#28362,.F.) ;
#39844 = ORIENTED_EDGE('',*,*,#28353,.F.) ;
#39845 = ORIENTED_EDGE('',*,*,#28356,.F.) ;
#39846 = ORIENTED_EDGE('',*,*,#28420,.T.) ;
#39847 = ORIENTED_EDGE('',*,*,#28421,.T.) ;
#39848 = ORIENTED_EDGE('',*,*,#27709,.T.) ;
#39849 = ORIENTED_EDGE('',*,*,#28364,.F.) ;
#39850 = ORIENTED_EDGE('',*,*,#28367,.F.) ;
#39851 = ORIENTED_EDGE('',*,*,#28422,.T.) ;
#39852 = ORIENTED_EDGE('',*,*,#28423,.T.) ;
#39853 = ORIENTED_EDGE('',*,*,#28424,.T.) ;
#39854 = ORIENTED_EDGE('',*,*,#28373,.F.) ;
#39855 = ORIENTED_EDGE('',*,*,#28425,.F.) ;
#39856 = ORIENTED_EDGE('',*,*,#28165,.T.) ;
#39857 = ORIENTED_EDGE('',*,*,#28426,.T.) ;
#39858 = ORIENTED_EDGE('',*,*,#28375,.F.) ;
#39859 = ORIENTED_EDGE('',*,*,#28427,.F.) ;
#39860 = ORIENTED_EDGE('',*,*,#28166,.T.) ;
#39861 = ORIENTED_EDGE('',*,*,#28425,.T.) ;
#39862 = ORIENTED_EDGE('',*,*,#28377,.F.) ;
#39863 = ORIENTED_EDGE('',*,*,#28428,.F.) ;
#39864 = ORIENTED_EDGE('',*,*,#28167,.T.) ;
#39865 = ORIENTED_EDGE('',*,*,#28427,.T.) ;
#39866 = ORIENTED_EDGE('',*,*,#28414,.F.) ;
#39867 = ORIENTED_EDGE('',*,*,#28411,.F.) ;
#39868 = ORIENTED_EDGE('',*,*,#28429,.T.) ;
#39869 = ORIENTED_EDGE('',*,*,#28430,.T.) ;
#39870 = ORIENTED_EDGE('',*,*,#28431,.T.) ;
#39871 = ORIENTED_EDGE('',*,*,#27824,.F.) ;
#39872 = ORIENTED_EDGE('',*,*,#27828,.F.) ;
#39873 = ORIENTED_EDGE('',*,*,#28426,.F.) ;
#39874 = ORIENTED_EDGE('',*,*,#28172,.T.) ;
#39875 = ORIENTED_EDGE('',*,*,#28432,.T.) ;
#39876 = ORIENTED_EDGE('',*,*,#28390,.F.) ;
#39877 = ORIENTED_EDGE('',*,*,#28433,.F.) ;
#39878 = ORIENTED_EDGE('',*,*,#28434,.T.) ;
#39879 = ORIENTED_EDGE('',*,*,#28422,.F.) ;
#39880 = ORIENTED_EDGE('',*,*,#28368,.F.) ;
#39881 = ORIENTED_EDGE('',*,*,#28410,.F.) ;
#39882 = ORIENTED_EDGE('',*,*,#28336,.F.) ;
#39883 = ORIENTED_EDGE('',*,*,#28435,.T.) ;
#39884 = ORIENTED_EDGE('',*,*,#28429,.F.) ;
#39885 = ORIENTED_EDGE('',*,*,#27814,.F.) ;
#39886 = ORIENTED_EDGE('',*,*,#27818,.F.) ;
#39887 = ORIENTED_EDGE('',*,*,#28431,.F.) ;
#39888 = ORIENTED_EDGE('',*,*,#28436,.T.) ;
#39889 = ORIENTED_EDGE('',*,*,#28437,.F.) ;
#39890 = ORIENTED_EDGE('',*,*,#28402,.F.) ;
#39891 = ORIENTED_EDGE('',*,*,#28438,.F.) ;
#39892 = ORIENTED_EDGE('',*,*,#28168,.T.) ;
#39893 = ORIENTED_EDGE('',*,*,#28428,.T.) ;
#39894 = ORIENTED_EDGE('',*,*,#28378,.F.) ;
#39895 = ORIENTED_EDGE('',*,*,#28337,.F.) ;
#39896 = ORIENTED_EDGE('',*,*,#28345,.F.) ;
#39897 = ORIENTED_EDGE('',*,*,#28344,.F.) ;
#39898 = ORIENTED_EDGE('',*,*,#28416,.F.) ;
#39899 = ORIENTED_EDGE('',*,*,#28439,.T.) ;
#39900 = ORIENTED_EDGE('',*,*,#28335,.T.) ;
#39901 = ORIENTED_EDGE('',*,*,#28439,.F.) ;
#39902 = ORIENTED_EDGE('',*,*,#28415,.T.) ;
#39903 = ORIENTED_EDGE('',*,*,#28440,.F.) ;
#39904 = ORIENTED_EDGE('',*,*,#28441,.F.) ;
#39905 = ORIENTED_EDGE('',*,*,#28436,.F.) ;
#39906 = ORIENTED_EDGE('',*,*,#28430,.F.) ;
#39907 = ORIENTED_EDGE('',*,*,#28435,.F.) ;
#39908 = ORIENTED_EDGE('',*,*,#28442,.T.) ;
#39909 = ORIENTED_EDGE('',*,*,#28443,.T.) ;
#39910 = ORIENTED_EDGE('',*,*,#28444,.T.) ;
#39911 = ORIENTED_EDGE('',*,*,#28445,.T.) ;
#39912 = ORIENTED_EDGE('',*,*,#28443,.F.) ;
#39913 = ORIENTED_EDGE('',*,*,#28446,.F.) ;
#39914 = ORIENTED_EDGE('',*,*,#28447,.F.) ;
#39915 = ORIENTED_EDGE('',*,*,#28448,.F.) ;
#39916 = ORIENTED_EDGE('',*,*,#28449,.T.) ;
#39917 = ORIENTED_EDGE('',*,*,#28447,.T.) ;
#39918 = ORIENTED_EDGE('',*,*,#28450,.T.) ;
#39919 = ORIENTED_EDGE('',*,*,#28451,.T.) ;
#39920 = ORIENTED_EDGE('',*,*,#28452,.T.) ;
#39921 = ORIENTED_EDGE('',*,*,#28453,.F.) ;
#39922 = ORIENTED_EDGE('',*,*,#28454,.F.) ;
#39923 = ORIENTED_EDGE('',*,*,#28455,.F.) ;
#39924 = ORIENTED_EDGE('',*,*,#28456,.F.) ;
#39925 = ORIENTED_EDGE('',*,*,#28457,.F.) ;
#39926 = ORIENTED_EDGE('',*,*,#28458,.T.) ;
#39927 = ORIENTED_EDGE('',*,*,#28459,.F.) ;
#39928 = ORIENTED_EDGE('',*,*,#28453,.T.) ;
#39929 = ORIENTED_EDGE('',*,*,#28460,.T.) ;
#39930 = ORIENTED_EDGE('',*,*,#28457,.T.) ;
#39931 = ORIENTED_EDGE('',*,*,#28461,.T.) ;
#39932 = ORIENTED_EDGE('',*,*,#28462,.T.) ;
#39933 = ORIENTED_EDGE('',*,*,#28463,.T.) ;
#39934 = ORIENTED_EDGE('',*,*,#28464,.T.) ;
#39935 = ORIENTED_EDGE('',*,*,#28465,.T.) ;
#39936 = ORIENTED_EDGE('',*,*,#28466,.T.) ;
#39937 = ORIENTED_EDGE('',*,*,#28467,.T.) ;
#39938 = ORIENTED_EDGE('',*,*,#28462,.F.) ;
#39939 = ORIENTED_EDGE('',*,*,#28468,.T.) ;
#39940 = ORIENTED_EDGE('',*,*,#28459,.T.) ;
#39941 = ORIENTED_EDGE('',*,*,#28469,.T.) ;
#39942 = ORIENTED_EDGE('',*,*,#28466,.F.) ;
#39943 = ORIENTED_EDGE('',*,*,#28470,.T.) ;
#39944 = ORIENTED_EDGE('',*,*,#28471,.F.) ;
#39945 = ORIENTED_EDGE('',*,*,#28472,.T.) ;
#39946 = ORIENTED_EDGE('',*,*,#28456,.T.) ;
#39947 = ORIENTED_EDGE('',*,*,#28473,.T.) ;
#39948 = ORIENTED_EDGE('',*,*,#28474,.F.) ;
#39949 = ORIENTED_EDGE('',*,*,#28475,.T.) ;
#39950 = ORIENTED_EDGE('',*,*,#28454,.T.) ;
#39951 = ORIENTED_EDGE('',*,*,#28476,.T.) ;
#39952 = ORIENTED_EDGE('',*,*,#28477,.T.) ;
#39953 = ORIENTED_EDGE('',*,*,#28478,.T.) ;
#39954 = ORIENTED_EDGE('',*,*,#28455,.T.) ;
#39955 = ORIENTED_EDGE('',*,*,#28479,.T.) ;
#39956 = ORIENTED_EDGE('',*,*,#28480,.T.) ;
#39957 = ORIENTED_EDGE('',*,*,#28481,.T.) ;
#39958 = ORIENTED_EDGE('',*,*,#28477,.F.) ;
#39959 = ORIENTED_EDGE('',*,*,#28482,.T.) ;
#39960 = ORIENTED_EDGE('',*,*,#28483,.T.) ;
#39961 = ORIENTED_EDGE('',*,*,#28484,.T.) ;
#39962 = ORIENTED_EDGE('',*,*,#28480,.F.) ;
#39963 = ORIENTED_EDGE('',*,*,#28485,.T.) ;
#39964 = ORIENTED_EDGE('',*,*,#28467,.F.) ;
#39965 = ORIENTED_EDGE('',*,*,#28486,.T.) ;
#39966 = ORIENTED_EDGE('',*,*,#28487,.F.) ;
#39967 = ORIENTED_EDGE('',*,*,#28488,.F.) ;
#39968 = ORIENTED_EDGE('',*,*,#28469,.F.) ;
#39969 = ORIENTED_EDGE('',*,*,#28458,.F.) ;
#39970 = ORIENTED_EDGE('',*,*,#28460,.F.) ;
#39971 = ORIENTED_EDGE('',*,*,#28452,.F.) ;
#39972 = ORIENTED_EDGE('',*,*,#28478,.F.) ;
#39973 = ORIENTED_EDGE('',*,*,#28489,.F.) ;
#39974 = ORIENTED_EDGE('',*,*,#28490,.F.) ;
#39975 = ORIENTED_EDGE('',*,*,#28491,.F.) ;
#39976 = ORIENTED_EDGE('',*,*,#28492,.F.) ;
#39977 = ORIENTED_EDGE('',*,*,#28493,.F.) ;
#39978 = ORIENTED_EDGE('',*,*,#28494,.F.) ;
#39979 = ORIENTED_EDGE('',*,*,#28495,.F.) ;
#39980 = ORIENTED_EDGE('',*,*,#28496,.F.) ;
#39981 = ORIENTED_EDGE('',*,*,#28497,.F.) ;
#39982 = ORIENTED_EDGE('',*,*,#28498,.F.) ;
#39983 = ORIENTED_EDGE('',*,*,#28499,.F.) ;
#39984 = ORIENTED_EDGE('',*,*,#28486,.F.) ;
#39985 = ORIENTED_EDGE('',*,*,#28481,.F.) ;
#39986 = ORIENTED_EDGE('',*,*,#28500,.F.) ;
#39987 = ORIENTED_EDGE('',*,*,#28501,.F.) ;
#39988 = ORIENTED_EDGE('',*,*,#28489,.T.) ;
#39989 = ORIENTED_EDGE('',*,*,#27829,.F.) ;
#39990 = ORIENTED_EDGE('',*,*,#27731,.F.) ;
#39991 = ORIENTED_EDGE('',*,*,#28502,.F.) ;
#39992 = ORIENTED_EDGE('',*,*,#28503,.T.) ;
#39993 = ORIENTED_EDGE('',*,*,#28504,.F.) ;
#39994 = ORIENTED_EDGE('',*,*,#28505,.F.) ;
#39995 = ORIENTED_EDGE('',*,*,#28506,.F.) ;
#39996 = ORIENTED_EDGE('',*,*,#28500,.T.) ;
#39997 = ORIENTED_EDGE('',*,*,#28484,.F.) ;
#39998 = ORIENTED_EDGE('',*,*,#28507,.T.) ;
#39999 = ORIENTED_EDGE('',*,*,#28463,.F.) ;
#40000 = ORIENTED_EDGE('',*,*,#28488,.T.) ;
#40001 = ORIENTED_EDGE('',*,*,#28508,.F.) ;
#40002 = ORIENTED_EDGE('',*,*,#28305,.T.) ;
#40003 = ORIENTED_EDGE('',*,*,#28509,.T.) ;
#40004 = ORIENTED_EDGE('',*,*,#28510,.T.) ;
#40005 = ORIENTED_EDGE('',*,*,#28511,.T.) ;
#40006 = ORIENTED_EDGE('',*,*,#27772,.F.) ;
#40007 = ORIENTED_EDGE('',*,*,#28307,.T.) ;
#40008 = ORIENTED_EDGE('',*,*,#28512,.T.) ;
#40009 = ORIENTED_EDGE('',*,*,#28513,.T.) ;
#40010 = ORIENTED_EDGE('',*,*,#27787,.F.) ;
#40011 = ORIENTED_EDGE('',*,*,#28514,.T.) ;
#40012 = ORIENTED_EDGE('',*,*,#28512,.F.) ;
#40013 = ORIENTED_EDGE('',*,*,#28306,.T.) ;
#40014 = ORIENTED_EDGE('',*,*,#28511,.F.) ;
#40015 = ORIENTED_EDGE('',*,*,#28515,.T.) ;
#40016 = ORIENTED_EDGE('',*,*,#28516,.T.) ;
#40017 = ORIENTED_EDGE('',*,*,#28509,.F.) ;
#40018 = ORIENTED_EDGE('',*,*,#28309,.T.) ;
#40019 = ORIENTED_EDGE('',*,*,#28517,.T.) ;
#40020 = ORIENTED_EDGE('',*,*,#28518,.T.) ;
#40021 = ORIENTED_EDGE('',*,*,#28515,.F.) ;
#40022 = ORIENTED_EDGE('',*,*,#28311,.T.) ;
#40023 = ORIENTED_EDGE('',*,*,#28519,.T.) ;
#40024 = ORIENTED_EDGE('',*,*,#28520,.T.) ;
#40025 = ORIENTED_EDGE('',*,*,#28517,.F.) ;
#40026 = ORIENTED_EDGE('',*,*,#28313,.T.) ;
#40027 = ORIENTED_EDGE('',*,*,#28521,.T.) ;
#40028 = ORIENTED_EDGE('',*,*,#28522,.T.) ;
#40029 = ORIENTED_EDGE('',*,*,#28519,.F.) ;
#40030 = ORIENTED_EDGE('',*,*,#28321,.T.) ;
#40031 = ORIENTED_EDGE('',*,*,#28523,.T.) ;
#40032 = ORIENTED_EDGE('',*,*,#28524,.T.) ;
#40033 = ORIENTED_EDGE('',*,*,#28521,.F.) ;
#40034 = ORIENTED_EDGE('',*,*,#28320,.T.) ;
#40035 = ORIENTED_EDGE('',*,*,#28525,.T.) ;
#40036 = ORIENTED_EDGE('',*,*,#28526,.T.) ;
#40037 = ORIENTED_EDGE('',*,*,#28523,.F.) ;
#40038 = ORIENTED_EDGE('',*,*,#28319,.T.) ;
#40039 = ORIENTED_EDGE('',*,*,#28527,.T.) ;
#40040 = ORIENTED_EDGE('',*,*,#28528,.T.) ;
#40041 = ORIENTED_EDGE('',*,*,#28525,.F.) ;
#40042 = ORIENTED_EDGE('',*,*,#28318,.T.) ;
#40043 = ORIENTED_EDGE('',*,*,#28529,.T.) ;
#40044 = ORIENTED_EDGE('',*,*,#28530,.T.) ;
#40045 = ORIENTED_EDGE('',*,*,#28527,.F.) ;
#40046 = ORIENTED_EDGE('',*,*,#28317,.T.) ;
#40047 = ORIENTED_EDGE('',*,*,#28531,.T.) ;
#40048 = ORIENTED_EDGE('',*,*,#28532,.T.) ;
#40049 = ORIENTED_EDGE('',*,*,#28529,.F.) ;
#40050 = ORIENTED_EDGE('',*,*,#28316,.T.) ;
#40051 = ORIENTED_EDGE('',*,*,#28533,.T.) ;
#40052 = ORIENTED_EDGE('',*,*,#28534,.T.) ;
#40053 = ORIENTED_EDGE('',*,*,#28531,.F.) ;
#40054 = ORIENTED_EDGE('',*,*,#28315,.T.) ;
#40055 = ORIENTED_EDGE('',*,*,#28535,.T.) ;
#40056 = ORIENTED_EDGE('',*,*,#28536,.T.) ;
#40057 = ORIENTED_EDGE('',*,*,#28533,.F.) ;
#40058 = ORIENTED_EDGE('',*,*,#28323,.T.) ;
#40059 = ORIENTED_EDGE('',*,*,#28537,.T.) ;
#40060 = ORIENTED_EDGE('',*,*,#28538,.T.) ;
#40061 = ORIENTED_EDGE('',*,*,#28535,.F.) ;
#40062 = ORIENTED_EDGE('',*,*,#28325,.T.) ;
#40063 = ORIENTED_EDGE('',*,*,#28539,.T.) ;
#40064 = ORIENTED_EDGE('',*,*,#28540,.T.) ;
#40065 = ORIENTED_EDGE('',*,*,#28537,.F.) ;
#40066 = ORIENTED_EDGE('',*,*,#28327,.T.) ;
#40067 = ORIENTED_EDGE('',*,*,#28541,.T.) ;
#40068 = ORIENTED_EDGE('',*,*,#28542,.T.) ;
#40069 = ORIENTED_EDGE('',*,*,#28539,.F.) ;
#40070 = ORIENTED_EDGE('',*,*,#28330,.T.) ;
#40071 = ORIENTED_EDGE('',*,*,#28543,.T.) ;
#40072 = ORIENTED_EDGE('',*,*,#28544,.T.) ;
#40073 = ORIENTED_EDGE('',*,*,#28541,.F.) ;
#40074 = ORIENTED_EDGE('',*,*,#28329,.T.) ;
#40075 = ORIENTED_EDGE('',*,*,#28545,.T.) ;
#40076 = ORIENTED_EDGE('',*,*,#27615,.T.) ;
#40077 = ORIENTED_EDGE('',*,*,#28543,.F.) ;
#40078 = ORIENTED_EDGE('',*,*,#28328,.T.) ;
#40079 = ORIENTED_EDGE('',*,*,#28546,.T.) ;
#40080 = ORIENTED_EDGE('',*,*,#27616,.T.) ;
#40081 = ORIENTED_EDGE('',*,*,#28545,.F.) ;
#40082 = ORIENTED_EDGE('',*,*,#27926,.T.) ;
#40083 = ORIENTED_EDGE('',*,*,#28547,.T.) ;
#40084 = ORIENTED_EDGE('',*,*,#27617,.T.) ;
#40085 = ORIENTED_EDGE('',*,*,#28546,.F.) ;
#40086 = ORIENTED_EDGE('',*,*,#28548,.T.) ;
#40087 = ORIENTED_EDGE('',*,*,#28549,.T.) ;
#40088 = ORIENTED_EDGE('',*,*,#27618,.T.) ;
#40089 = ORIENTED_EDGE('',*,*,#28547,.F.) ;
#40090 = ORIENTED_EDGE('',*,*,#28550,.T.) ;
#40091 = ORIENTED_EDGE('',*,*,#28551,.T.) ;
#40092 = ORIENTED_EDGE('',*,*,#27619,.T.) ;
#40093 = ORIENTED_EDGE('',*,*,#28549,.F.) ;
#40094 = ORIENTED_EDGE('',*,*,#28552,.T.) ;
#40095 = ORIENTED_EDGE('',*,*,#28553,.T.) ;
#40096 = ORIENTED_EDGE('',*,*,#27620,.T.) ;
#40097 = ORIENTED_EDGE('',*,*,#28551,.F.) ;
#40098 = ORIENTED_EDGE('',*,*,#28554,.T.) ;
#40099 = ORIENTED_EDGE('',*,*,#28555,.T.) ;
#40100 = ORIENTED_EDGE('',*,*,#27621,.T.) ;
#40101 = ORIENTED_EDGE('',*,*,#28553,.F.) ;
#40102 = ORIENTED_EDGE('',*,*,#28556,.T.) ;
#40103 = ORIENTED_EDGE('',*,*,#28557,.T.) ;
#40104 = ORIENTED_EDGE('',*,*,#27622,.T.) ;
#40105 = ORIENTED_EDGE('',*,*,#28555,.F.) ;
#40106 = ORIENTED_EDGE('',*,*,#28242,.T.) ;
#40107 = ORIENTED_EDGE('',*,*,#28558,.T.) ;
#40108 = ORIENTED_EDGE('',*,*,#27623,.T.) ;
#40109 = ORIENTED_EDGE('',*,*,#28557,.F.) ;
#40110 = ORIENTED_EDGE('',*,*,#28247,.T.) ;
#40111 = ORIENTED_EDGE('',*,*,#27979,.T.) ;
#40112 = ORIENTED_EDGE('',*,*,#27624,.T.) ;
#40113 = ORIENTED_EDGE('',*,*,#28558,.F.) ;
#40114 = ORIENTED_EDGE('',*,*,#28559,.T.) ;
#40115 = ORIENTED_EDGE('',*,*,#27980,.F.) ;
#40116 = ORIENTED_EDGE('',*,*,#28560,.F.) ;
#40117 = ORIENTED_EDGE('',*,*,#28561,.F.) ;
#40118 = ORIENTED_EDGE('',*,*,#27977,.T.) ;
#40119 = ORIENTED_EDGE('',*,*,#28559,.F.) ;
#40120 = ORIENTED_EDGE('',*,*,#28246,.F.) ;
#40121 = ORIENTED_EDGE('',*,*,#28562,.F.) ;
#40122 = ORIENTED_EDGE('',*,*,#28560,.T.) ;
#40123 = ORIENTED_EDGE('',*,*,#27873,.F.) ;
#40124 = ORIENTED_EDGE('',*,*,#28243,.T.) ;
#40125 = ORIENTED_EDGE('',*,*,#28556,.F.) ;
#40126 = ORIENTED_EDGE('',*,*,#28563,.F.) ;
#40127 = ORIENTED_EDGE('',*,*,#27876,.F.) ;
#40128 = ORIENTED_EDGE('',*,*,#28563,.T.) ;
#40129 = ORIENTED_EDGE('',*,*,#28554,.F.) ;
#40130 = ORIENTED_EDGE('',*,*,#28564,.T.) ;
#40131 = ORIENTED_EDGE('',*,*,#27879,.F.) ;
#40132 = ORIENTED_EDGE('',*,*,#28564,.F.) ;
#40133 = ORIENTED_EDGE('',*,*,#28552,.F.) ;
#40134 = ORIENTED_EDGE('',*,*,#28565,.F.) ;
#40135 = ORIENTED_EDGE('',*,*,#27882,.F.) ;
#40136 = ORIENTED_EDGE('',*,*,#28565,.T.) ;
#40137 = ORIENTED_EDGE('',*,*,#28550,.F.) ;
#40138 = ORIENTED_EDGE('',*,*,#28566,.F.) ;
#40139 = ORIENTED_EDGE('',*,*,#27885,.F.) ;
#40140 = ORIENTED_EDGE('',*,*,#28566,.T.) ;
#40141 = ORIENTED_EDGE('',*,*,#28548,.F.) ;
#40142 = ORIENTED_EDGE('',*,*,#27925,.F.) ;
#40143 = ORIENTED_EDGE('',*,*,#27830,.F.) ;
#40144 = ORIENTED_EDGE('',*,*,#28508,.T.) ;
#40145 = ORIENTED_EDGE('',*,*,#28567,.T.) ;
#40146 = ORIENTED_EDGE('',*,*,#28568,.T.) ;
#40147 = ORIENTED_EDGE('',*,*,#27713,.F.) ;
#40148 = ORIENTED_EDGE('',*,*,#27759,.T.) ;
#40149 = ORIENTED_EDGE('',*,*,#28569,.T.) ;
#40150 = ORIENTED_EDGE('',*,*,#28502,.T.) ;
#40151 = ORIENTED_EDGE('',*,*,#27714,.F.) ;
#40152 = ORIENTED_EDGE('',*,*,#28570,.T.) ;
#40153 = ORIENTED_EDGE('',*,*,#28571,.T.) ;
#40154 = ORIENTED_EDGE('',*,*,#27756,.T.) ;
#40155 = ORIENTED_EDGE('',*,*,#27761,.F.) ;
#40156 = ORIENTED_EDGE('',*,*,#28572,.T.) ;
#40157 = ORIENTED_EDGE('',*,*,#27757,.T.) ;
#40158 = ORIENTED_EDGE('',*,*,#28571,.F.) ;
#40159 = ORIENTED_EDGE('',*,*,#28573,.T.) ;
#40160 = ORIENTED_EDGE('',*,*,#27758,.T.) ;
#40161 = ORIENTED_EDGE('',*,*,#28572,.F.) ;
#40162 = ORIENTED_EDGE('',*,*,#28574,.T.) ;
#40163 = ORIENTED_EDGE('',*,*,#28569,.F.) ;
#40164 = ORIENTED_EDGE('',*,*,#28575,.T.) ;
#40165 = ORIENTED_EDGE('',*,*,#28576,.T.) ;
#40166 = ORIENTED_EDGE('',*,*,#28567,.F.) ;
#40167 = ORIENTED_EDGE('',*,*,#28487,.T.) ;
#40168 = ORIENTED_EDGE('',*,*,#28577,.T.) ;
#40169 = ORIENTED_EDGE('',*,*,#28578,.T.) ;
#40170 = ORIENTED_EDGE('',*,*,#28575,.F.) ;
#40171 = ORIENTED_EDGE('',*,*,#28499,.T.) ;
#40172 = ORIENTED_EDGE('',*,*,#28579,.T.) ;
#40173 = ORIENTED_EDGE('',*,*,#28580,.T.) ;
#40174 = ORIENTED_EDGE('',*,*,#28577,.F.) ;
#40175 = ORIENTED_EDGE('',*,*,#28498,.T.) ;
#40176 = ORIENTED_EDGE('',*,*,#28581,.T.) ;
#40177 = ORIENTED_EDGE('',*,*,#27820,.T.) ;
#40178 = ORIENTED_EDGE('',*,*,#28579,.F.) ;
#40179 = ORIENTED_EDGE('',*,*,#28497,.T.) ;
#40180 = ORIENTED_EDGE('',*,*,#28582,.T.) ;
#40181 = ORIENTED_EDGE('',*,*,#28418,.T.) ;
#40182 = ORIENTED_EDGE('',*,*,#28581,.F.) ;
#40183 = ORIENTED_EDGE('',*,*,#28496,.T.) ;
#40184 = ORIENTED_EDGE('',*,*,#28583,.T.) ;
#40185 = ORIENTED_EDGE('',*,*,#28584,.T.) ;
#40186 = ORIENTED_EDGE('',*,*,#28582,.F.) ;
#40187 = ORIENTED_EDGE('',*,*,#28495,.T.) ;
#40188 = ORIENTED_EDGE('',*,*,#28585,.T.) ;
#40189 = ORIENTED_EDGE('',*,*,#28586,.T.) ;
#40190 = ORIENTED_EDGE('',*,*,#28583,.F.) ;
#40191 = ORIENTED_EDGE('',*,*,#28494,.T.) ;
#40192 = ORIENTED_EDGE('',*,*,#28587,.T.) ;
#40193 = ORIENTED_EDGE('',*,*,#28585,.F.) ;
#40194 = ORIENTED_EDGE('',*,*,#28493,.T.) ;
#40195 = ORIENTED_EDGE('',*,*,#28588,.T.) ;
#40196 = ORIENTED_EDGE('',*,*,#28589,.T.) ;
#40197 = ORIENTED_EDGE('',*,*,#28590,.T.) ;
#40198 = ORIENTED_EDGE('',*,*,#28591,.T.) ;
#40199 = ORIENTED_EDGE('',*,*,#28592,.T.) ;
#40200 = ORIENTED_EDGE('',*,*,#28593,.T.) ;
#40201 = ORIENTED_EDGE('',*,*,#28594,.T.) ;
#40202 = ORIENTED_EDGE('',*,*,#28591,.F.) ;
#40203 = ORIENTED_EDGE('',*,*,#28595,.T.) ;
#40204 = ORIENTED_EDGE('',*,*,#28596,.T.) ;
#40205 = ORIENTED_EDGE('',*,*,#28506,.T.) ;
#40206 = ORIENTED_EDGE('',*,*,#28593,.F.) ;
#40207 = ORIENTED_EDGE('',*,*,#28597,.T.) ;
#40208 = ORIENTED_EDGE('',*,*,#28598,.T.) ;
#40209 = ORIENTED_EDGE('',*,*,#28501,.T.) ;
#40210 = ORIENTED_EDGE('',*,*,#28596,.F.) ;
#40211 = ORIENTED_EDGE('',*,*,#28599,.T.) ;
#40212 = ORIENTED_EDGE('',*,*,#28600,.T.) ;
#40213 = ORIENTED_EDGE('',*,*,#28490,.T.) ;
#40214 = ORIENTED_EDGE('',*,*,#28598,.F.) ;
#40215 = ORIENTED_EDGE('',*,*,#28601,.T.) ;
#40216 = ORIENTED_EDGE('',*,*,#28602,.T.) ;
#40217 = ORIENTED_EDGE('',*,*,#28491,.T.) ;
#40218 = ORIENTED_EDGE('',*,*,#28600,.F.) ;
#40219 = ORIENTED_EDGE('',*,*,#28603,.T.) ;
#40220 = ORIENTED_EDGE('',*,*,#28492,.T.) ;
#40221 = ORIENTED_EDGE('',*,*,#28602,.F.) ;
#40222 = ORIENTED_EDGE('',*,*,#28604,.T.) ;
#40223 = ORIENTED_EDGE('',*,*,#28588,.F.) ;
#40224 = ORIENTED_EDGE('',*,*,#27739,.F.) ;
#40225 = ORIENTED_EDGE('',*,*,#27844,.F.) ;
#40226 = ORIENTED_EDGE('',*,*,#27843,.F.) ;
#40227 = ORIENTED_EDGE('',*,*,#27840,.F.) ;
#40228 = ORIENTED_EDGE('',*,*,#27762,.F.) ;
#40229 = ORIENTED_EDGE('',*,*,#27834,.F.) ;
#40230 = ORIENTED_EDGE('',*,*,#28568,.F.) ;
#40231 = ORIENTED_EDGE('',*,*,#28576,.F.) ;
#40232 = ORIENTED_EDGE('',*,*,#28578,.F.) ;
#40233 = ORIENTED_EDGE('',*,*,#28605,.F.) ;
#40234 = ORIENTED_EDGE('',*,*,#27833,.F.) ;
#40235 = ORIENTED_EDGE('',*,*,#28605,.T.) ;
#40236 = ORIENTED_EDGE('',*,*,#28580,.F.) ;
#40237 = ORIENTED_EDGE('',*,*,#27819,.T.) ;
#40238 = ORIENTED_EDGE('',*,*,#28343,.F.) ;
#40239 = ORIENTED_EDGE('',*,*,#28419,.F.) ;
#40240 = ORIENTED_EDGE('',*,*,#28584,.F.) ;
#40241 = ORIENTED_EDGE('',*,*,#28606,.F.) ;
#40242 = ORIENTED_EDGE('',*,*,#28607,.F.) ;
#40243 = ORIENTED_EDGE('',*,*,#28608,.F.) ;
#40244 = ORIENTED_EDGE('',*,*,#28609,.F.) ;
#40245 = ORIENTED_EDGE('',*,*,#28610,.F.) ;
#40246 = ORIENTED_EDGE('',*,*,#28611,.F.) ;
#40247 = ORIENTED_EDGE('',*,*,#28420,.F.) ;
#40248 = ORIENTED_EDGE('',*,*,#28358,.F.) ;
#40249 = ORIENTED_EDGE('',*,*,#28347,.F.) ;
#40250 = ORIENTED_EDGE('',*,*,#28383,.F.) ;
#40251 = ORIENTED_EDGE('',*,*,#28386,.F.) ;
#40252 = ORIENTED_EDGE('',*,*,#28389,.F.) ;
#40253 = ORIENTED_EDGE('',*,*,#28392,.F.) ;
#40254 = ORIENTED_EDGE('',*,*,#28395,.F.) ;
#40255 = ORIENTED_EDGE('',*,*,#28398,.F.) ;
#40256 = ORIENTED_EDGE('',*,*,#28401,.F.) ;
#40257 = ORIENTED_EDGE('',*,*,#28404,.F.) ;
#40258 = ORIENTED_EDGE('',*,*,#28406,.F.) ;
#40259 = ORIENTED_EDGE('',*,*,#28340,.F.) ;
#40260 = ORIENTED_EDGE('',*,*,#28612,.F.) ;
#40261 = ORIENTED_EDGE('',*,*,#28613,.F.) ;
#40262 = ORIENTED_EDGE('',*,*,#28614,.F.) ;
#40263 = ORIENTED_EDGE('',*,*,#28615,.F.) ;
#40264 = ORIENTED_EDGE('',*,*,#28616,.F.) ;
#40265 = ORIENTED_EDGE('',*,*,#28617,.F.) ;
#40266 = ORIENTED_EDGE('',*,*,#28618,.F.) ;
#40267 = ORIENTED_EDGE('',*,*,#28619,.F.) ;
#40268 = ORIENTED_EDGE('',*,*,#28620,.F.) ;
#40269 = ORIENTED_EDGE('',*,*,#28621,.F.) ;
#40270 = ORIENTED_EDGE('',*,*,#28622,.F.) ;
#40271 = ORIENTED_EDGE('',*,*,#28623,.F.) ;
#40272 = ORIENTED_EDGE('',*,*,#28624,.F.) ;
#40273 = ORIENTED_EDGE('',*,*,#28625,.F.) ;
#40274 = ORIENTED_EDGE('',*,*,#28586,.F.) ;
#40275 = ORIENTED_EDGE('',*,*,#28626,.T.) ;
#40276 = ORIENTED_EDGE('',*,*,#28627,.T.) ;
#40277 = ORIENTED_EDGE('',*,*,#28606,.T.) ;
#40278 = ORIENTED_EDGE('',*,*,#28587,.F.) ;
#40279 = ORIENTED_EDGE('',*,*,#28628,.T.) ;
#40280 = ORIENTED_EDGE('',*,*,#28629,.F.) ;
#40281 = ORIENTED_EDGE('',*,*,#28630,.F.) ;
#40282 = ORIENTED_EDGE('',*,*,#28626,.F.) ;
#40283 = ORIENTED_EDGE('',*,*,#28604,.F.) ;
#40284 = ORIENTED_EDGE('',*,*,#28631,.F.) ;
#40285 = ORIENTED_EDGE('',*,*,#28632,.T.) ;
#40286 = ORIENTED_EDGE('',*,*,#28100,.F.) ;
#40287 = ORIENTED_EDGE('',*,*,#28633,.F.) ;
#40288 = ORIENTED_EDGE('',*,*,#28634,.F.) ;
#40289 = ORIENTED_EDGE('',*,*,#28628,.F.) ;
#40290 = ORIENTED_EDGE('',*,*,#28635,.T.) ;
#40291 = ORIENTED_EDGE('',*,*,#28603,.F.) ;
#40292 = ORIENTED_EDGE('',*,*,#28636,.T.) ;
#40293 = ORIENTED_EDGE('',*,*,#28637,.T.) ;
#40294 = ORIENTED_EDGE('',*,*,#28631,.T.) ;
#40295 = ORIENTED_EDGE('',*,*,#28601,.F.) ;
#40296 = ORIENTED_EDGE('',*,*,#28599,.F.) ;
#40297 = ORIENTED_EDGE('',*,*,#28597,.F.) ;
#40298 = ORIENTED_EDGE('',*,*,#28595,.F.) ;
#40299 = ORIENTED_EDGE('',*,*,#28590,.F.) ;
#40300 = ORIENTED_EDGE('',*,*,#28638,.T.) ;
#40301 = ORIENTED_EDGE('',*,*,#28639,.T.) ;
#40302 = ORIENTED_EDGE('',*,*,#28640,.F.) ;
#40303 = ORIENTED_EDGE('',*,*,#28641,.F.) ;
#40304 = ORIENTED_EDGE('',*,*,#28636,.F.) ;
#40305 = ORIENTED_EDGE('',*,*,#28589,.F.) ;
#40306 = ORIENTED_EDGE('',*,*,#28642,.T.) ;
#40307 = ORIENTED_EDGE('',*,*,#28104,.F.) ;
#40308 = ORIENTED_EDGE('',*,*,#28643,.F.) ;
#40309 = ORIENTED_EDGE('',*,*,#28638,.F.) ;
#40310 = ORIENTED_EDGE('',*,*,#28644,.T.) ;
#40311 = ORIENTED_EDGE('',*,*,#28645,.F.) ;
#40312 = ORIENTED_EDGE('',*,*,#28646,.F.) ;
#40313 = ORIENTED_EDGE('',*,*,#28647,.F.) ;
#40314 = ORIENTED_EDGE('',*,*,#28648,.T.) ;
#40315 = ORIENTED_EDGE('',*,*,#28649,.F.) ;
#40316 = ORIENTED_EDGE('',*,*,#28650,.F.) ;
#40317 = ORIENTED_EDGE('',*,*,#28651,.F.) ;
#40318 = ORIENTED_EDGE('',*,*,#27947,.F.) ;
#40319 = ORIENTED_EDGE('',*,*,#28652,.T.) ;
#40320 = ORIENTED_EDGE('',*,*,#28653,.T.) ;
#40321 = ORIENTED_EDGE('',*,*,#28654,.T.) ;
#40322 = ORIENTED_EDGE('',*,*,#28655,.T.) ;
#40323 = ORIENTED_EDGE('',*,*,#28656,.T.) ;
#40324 = ORIENTED_EDGE('',*,*,#28653,.F.) ;
#40325 = ORIENTED_EDGE('',*,*,#28657,.T.) ;
#40326 = ORIENTED_EDGE('',*,*,#28658,.T.) ;
#40327 = ORIENTED_EDGE('',*,*,#28659,.T.) ;
#40328 = ORIENTED_EDGE('',*,*,#28655,.F.) ;
#40329 = ORIENTED_EDGE('',*,*,#28660,.T.) ;
#40330 = ORIENTED_EDGE('',*,*,#28649,.T.) ;
#40331 = ORIENTED_EDGE('',*,*,#28661,.T.) ;
#40332 = ORIENTED_EDGE('',*,*,#28658,.F.) ;
#40333 = ORIENTED_EDGE('',*,*,#28662,.T.) ;
#40334 = ORIENTED_EDGE('',*,*,#28663,.F.) ;
#40335 = ORIENTED_EDGE('',*,*,#28664,.T.) ;
#40336 = ORIENTED_EDGE('',*,*,#28650,.T.) ;
#40337 = ORIENTED_EDGE('',*,*,#28665,.T.) ;
#40338 = ORIENTED_EDGE('',*,*,#28645,.T.) ;
#40339 = ORIENTED_EDGE('',*,*,#28666,.T.) ;
#40340 = ORIENTED_EDGE('',*,*,#28651,.T.) ;
#40341 = ORIENTED_EDGE('',*,*,#28667,.T.) ;
#40342 = ORIENTED_EDGE('',*,*,#28668,.F.) ;
#40343 = ORIENTED_EDGE('',*,*,#28669,.T.) ;
#40344 = ORIENTED_EDGE('',*,*,#28646,.T.) ;
#40345 = ORIENTED_EDGE('',*,*,#28670,.T.) ;
#40346 = ORIENTED_EDGE('',*,*,#28671,.T.) ;
#40347 = ORIENTED_EDGE('',*,*,#28672,.T.) ;
#40348 = ORIENTED_EDGE('',*,*,#28647,.T.) ;
#40349 = ORIENTED_EDGE('',*,*,#28673,.T.) ;
#40350 = ORIENTED_EDGE('',*,*,#28674,.T.) ;
#40351 = ORIENTED_EDGE('',*,*,#28675,.T.) ;
#40352 = ORIENTED_EDGE('',*,*,#28671,.F.) ;
#40353 = ORIENTED_EDGE('',*,*,#28003,.T.) ;
#40354 = ORIENTED_EDGE('',*,*,#28013,.T.) ;
#40355 = ORIENTED_EDGE('',*,*,#28676,.T.) ;
#40356 = ORIENTED_EDGE('',*,*,#28674,.F.) ;
#40357 = ORIENTED_EDGE('',*,*,#28002,.T.) ;
#40358 = ORIENTED_EDGE('',*,*,#28657,.F.) ;
#40359 = ORIENTED_EDGE('',*,*,#28652,.F.) ;
#40360 = ORIENTED_EDGE('',*,*,#27946,.F.) ;
#40361 = ORIENTED_EDGE('',*,*,#28677,.T.) ;
#40362 = ORIENTED_EDGE('',*,*,#28678,.T.) ;
#40363 = ORIENTED_EDGE('',*,*,#28679,.T.) ;
#40364 = ORIENTED_EDGE('',*,*,#27944,.F.) ;
#40365 = ORIENTED_EDGE('',*,*,#28654,.F.) ;
#40366 = ORIENTED_EDGE('',*,*,#28680,.F.) ;
#40367 = ORIENTED_EDGE('',*,*,#27941,.F.) ;
#40368 = ORIENTED_EDGE('',*,*,#28680,.T.) ;
#40369 = ORIENTED_EDGE('',*,*,#28656,.F.) ;
#40370 = ORIENTED_EDGE('',*,*,#28659,.F.) ;
#40371 = ORIENTED_EDGE('',*,*,#28681,.T.) ;
#40372 = ORIENTED_EDGE('',*,*,#27965,.F.) ;
#40373 = ORIENTED_EDGE('',*,*,#27936,.F.) ;
#40374 = ORIENTED_EDGE('',*,*,#27939,.F.) ;
#40375 = ORIENTED_EDGE('',*,*,#27963,.F.) ;
#40376 = ORIENTED_EDGE('',*,*,#28681,.F.) ;
#40377 = ORIENTED_EDGE('',*,*,#28661,.F.) ;
#40378 = ORIENTED_EDGE('',*,*,#28648,.F.) ;
#40379 = ORIENTED_EDGE('',*,*,#28666,.F.) ;
#40380 = ORIENTED_EDGE('',*,*,#28644,.F.) ;
#40381 = ORIENTED_EDGE('',*,*,#28672,.F.) ;
#40382 = ORIENTED_EDGE('',*,*,#28675,.F.) ;
#40383 = ORIENTED_EDGE('',*,*,#28682,.F.) ;
#40384 = ORIENTED_EDGE('',*,*,#28683,.T.) ;
#40385 = ORIENTED_EDGE('',*,*,#28684,.F.) ;
#40386 = ORIENTED_EDGE('',*,*,#28676,.F.) ;
#40387 = ORIENTED_EDGE('',*,*,#28012,.F.) ;
#40388 = ORIENTED_EDGE('',*,*,#28685,.T.) ;
#40389 = ORIENTED_EDGE('',*,*,#28686,.F.) ;
#40390 = ORIENTED_EDGE('',*,*,#28687,.T.) ;
#40391 = ORIENTED_EDGE('',*,*,#28688,.T.) ;
#40392 = ORIENTED_EDGE('',*,*,#28682,.T.) ;
#40393 = ORIENTED_EDGE('',*,*,#28689,.T.) ;
#40394 = ORIENTED_EDGE('',*,*,#28690,.T.) ;
#40395 = ORIENTED_EDGE('',*,*,#28006,.T.) ;
#40396 = ORIENTED_EDGE('',*,*,#28691,.T.) ;
#40397 = ORIENTED_EDGE('',*,*,#27996,.F.) ;
#40398 = ORIENTED_EDGE('',*,*,#28692,.T.) ;
#40399 = ORIENTED_EDGE('',*,*,#28693,.T.) ;
#40400 = ORIENTED_EDGE('',*,*,#28694,.T.) ;
#40401 = ORIENTED_EDGE('',*,*,#28695,.T.) ;
#40402 = ORIENTED_EDGE('',*,*,#28691,.F.) ;
#40403 = ORIENTED_EDGE('',*,*,#28005,.T.) ;
#40404 = ORIENTED_EDGE('',*,*,#27791,.F.) ;
#40405 = ORIENTED_EDGE('',*,*,#28696,.F.) ;
#40406 = ORIENTED_EDGE('',*,*,#28689,.F.) ;
#40407 = ORIENTED_EDGE('',*,*,#28695,.F.) ;
#40408 = ORIENTED_EDGE('',*,*,#28697,.F.) ;
#40409 = ORIENTED_EDGE('',*,*,#28698,.T.) ;
#40410 = ORIENTED_EDGE('',*,*,#28699,.F.) ;
#40411 = ORIENTED_EDGE('',*,*,#28700,.T.) ;
#40412 = ORIENTED_EDGE('',*,*,#27665,.T.) ;
#40413 = ORIENTED_EDGE('',*,*,#27642,.F.) ;
#40414 = ORIENTED_EDGE('',*,*,#28694,.F.) ;
#40415 = ORIENTED_EDGE('',*,*,#28701,.T.) ;
#40416 = ORIENTED_EDGE('',*,*,#28702,.F.) ;
#40417 = ORIENTED_EDGE('',*,*,#28697,.T.) ;
#40418 = ORIENTED_EDGE('',*,*,#28669,.F.) ;
#40419 = ORIENTED_EDGE('',*,*,#28703,.F.) ;
#40420 = ORIENTED_EDGE('',*,*,#28701,.F.) ;
#40421 = ORIENTED_EDGE('',*,*,#28693,.F.) ;
#40422 = ORIENTED_EDGE('',*,*,#28704,.F.) ;
#40423 = ORIENTED_EDGE('',*,*,#27999,.F.) ;
#40424 = ORIENTED_EDGE('',*,*,#28004,.F.) ;
#40425 = ORIENTED_EDGE('',*,*,#28673,.F.) ;
#40426 = ORIENTED_EDGE('',*,*,#27671,.F.) ;
#40427 = ORIENTED_EDGE('',*,*,#28705,.T.) ;
#40428 = ORIENTED_EDGE('',*,*,#28706,.F.) ;
#40429 = ORIENTED_EDGE('',*,*,#27699,.F.) ;
#40430 = ORIENTED_EDGE('',*,*,#27698,.T.) ;
#40431 = ORIENTED_EDGE('',*,*,#28707,.T.) ;
#40432 = ORIENTED_EDGE('',*,*,#27701,.T.) ;
#40433 = ORIENTED_EDGE('',*,*,#28708,.T.) ;
#40434 = ORIENTED_EDGE('',*,*,#27802,.T.) ;
#40435 = ORIENTED_EDGE('',*,*,#28706,.T.) ;
#40436 = ORIENTED_EDGE('',*,*,#28709,.T.) ;
#40437 = ORIENTED_EDGE('',*,*,#28708,.F.) ;
#40438 = ORIENTED_EDGE('',*,*,#27700,.T.) ;
#40439 = ORIENTED_EDGE('',*,*,#28710,.T.) ;
#40440 = ORIENTED_EDGE('',*,*,#27702,.T.) ;
#40441 = ORIENTED_EDGE('',*,*,#28707,.F.) ;
#40442 = ORIENTED_EDGE('',*,*,#28711,.T.) ;
#40443 = ORIENTED_EDGE('',*,*,#28712,.T.) ;
#40444 = ORIENTED_EDGE('',*,*,#27703,.T.) ;
#40445 = ORIENTED_EDGE('',*,*,#28710,.F.) ;
#40446 = ORIENTED_EDGE('',*,*,#28713,.T.) ;
#40447 = ORIENTED_EDGE('',*,*,#28714,.T.) ;
#40448 = ORIENTED_EDGE('',*,*,#27859,.T.) ;
#40449 = ORIENTED_EDGE('',*,*,#28712,.F.) ;
#40450 = ORIENTED_EDGE('',*,*,#28715,.T.) ;
#40451 = ORIENTED_EDGE('',*,*,#27670,.F.) ;
#40452 = ORIENTED_EDGE('',*,*,#28716,.T.) ;
#40453 = ORIENTED_EDGE('',*,*,#27794,.F.) ;
#40454 = ORIENTED_EDGE('',*,*,#27803,.T.) ;
#40455 = ORIENTED_EDGE('',*,*,#28709,.F.) ;
#40456 = ORIENTED_EDGE('',*,*,#28705,.F.) ;
#40457 = ORIENTED_EDGE('',*,*,#27695,.F.) ;
#40458 = ORIENTED_EDGE('',*,*,#27711,.T.) ;
#40459 = ORIENTED_EDGE('',*,*,#28717,.T.) ;
#40460 = ORIENTED_EDGE('',*,*,#28718,.T.) ;
#40461 = ORIENTED_EDGE('',*,*,#28719,.T.) ;
#40462 = ORIENTED_EDGE('',*,*,#28720,.T.) ;
#40463 = ORIENTED_EDGE('',*,*,#28721,.F.) ;
#40464 = ORIENTED_EDGE('',*,*,#28722,.F.) ;
#40465 = ORIENTED_EDGE('',*,*,#27696,.F.) ;
#40466 = ORIENTED_EDGE('',*,*,#28723,.F.) ;
#40467 = ORIENTED_EDGE('',*,*,#28721,.T.) ;
#40468 = ORIENTED_EDGE('',*,*,#28724,.T.) ;
#40469 = ORIENTED_EDGE('',*,*,#28725,.T.) ;
#40470 = ORIENTED_EDGE('',*,*,#27792,.T.) ;
#40471 = ORIENTED_EDGE('',*,*,#27651,.F.) ;
#40472 = ORIENTED_EDGE('',*,*,#27656,.T.) ;
#40473 = ORIENTED_EDGE('',*,*,#27655,.T.) ;
#40474 = ORIENTED_EDGE('',*,*,#28726,.T.) ;
#40475 = ORIENTED_EDGE('',*,*,#28727,.T.) ;
#40476 = ORIENTED_EDGE('',*,*,#28724,.F.) ;
#40477 = ORIENTED_EDGE('',*,*,#28728,.T.) ;
#40478 = ORIENTED_EDGE('',*,*,#28729,.T.) ;
#40479 = ORIENTED_EDGE('',*,*,#28730,.T.) ;
#40480 = ORIENTED_EDGE('',*,*,#28726,.F.) ;
#40481 = ORIENTED_EDGE('',*,*,#28731,.T.) ;
#40482 = ORIENTED_EDGE('',*,*,#28008,.T.) ;
#40483 = ORIENTED_EDGE('',*,*,#28729,.F.) ;
#40484 = ORIENTED_EDGE('',*,*,#28732,.T.) ;
#40485 = ORIENTED_EDGE('',*,*,#28733,.T.) ;
#40486 = ORIENTED_EDGE('',*,*,#28530,.F.) ;
#40487 = ORIENTED_EDGE('',*,*,#28734,.F.) ;
#40488 = ORIENTED_EDGE('',*,*,#28735,.T.) ;
#40489 = ORIENTED_EDGE('',*,*,#28736,.T.) ;
#40490 = ORIENTED_EDGE('',*,*,#28737,.T.) ;
#40491 = ORIENTED_EDGE('',*,*,#28738,.T.) ;
#40492 = ORIENTED_EDGE('',*,*,#28739,.T.) ;
#40493 = ORIENTED_EDGE('',*,*,#28687,.F.) ;
#40494 = ORIENTED_EDGE('',*,*,#28740,.F.) ;
#40495 = ORIENTED_EDGE('',*,*,#28741,.F.) ;
#40496 = ORIENTED_EDGE('',*,*,#28742,.F.) ;
#40497 = ORIENTED_EDGE('',*,*,#28743,.F.) ;
#40498 = ORIENTED_EDGE('',*,*,#28744,.F.) ;
#40499 = ORIENTED_EDGE('',*,*,#28745,.F.) ;
#40500 = ORIENTED_EDGE('',*,*,#28746,.F.) ;
#40501 = ORIENTED_EDGE('',*,*,#28747,.F.) ;
#40502 = ORIENTED_EDGE('',*,*,#28748,.F.) ;
#40503 = ORIENTED_EDGE('',*,*,#28749,.F.) ;
#40504 = ORIENTED_EDGE('',*,*,#28750,.F.) ;
#40505 = ORIENTED_EDGE('',*,*,#28751,.F.) ;
#40506 = ORIENTED_EDGE('',*,*,#28752,.F.) ;
#40507 = ORIENTED_EDGE('',*,*,#28753,.T.) ;
#40508 = ORIENTED_EDGE('',*,*,#28754,.F.) ;
#40509 = ORIENTED_EDGE('',*,*,#28755,.F.) ;
#40510 = ORIENTED_EDGE('',*,*,#28756,.F.) ;
#40511 = ORIENTED_EDGE('',*,*,#28757,.F.) ;
#40512 = ORIENTED_EDGE('',*,*,#28758,.F.) ;
#40513 = ORIENTED_EDGE('',*,*,#28759,.F.) ;
#40514 = ORIENTED_EDGE('',*,*,#28760,.F.) ;
#40515 = ORIENTED_EDGE('',*,*,#28761,.F.) ;
#40516 = ORIENTED_EDGE('',*,*,#28762,.F.) ;
#40517 = ORIENTED_EDGE('',*,*,#28763,.F.) ;
#40518 = ORIENTED_EDGE('',*,*,#28764,.F.) ;
#40519 = ORIENTED_EDGE('',*,*,#28765,.F.) ;
#40520 = ORIENTED_EDGE('',*,*,#28766,.F.) ;
#40521 = ORIENTED_EDGE('',*,*,#28767,.F.) ;
#40522 = ORIENTED_EDGE('',*,*,#28528,.F.) ;
#40523 = ORIENTED_EDGE('',*,*,#28741,.T.) ;
#40524 = ORIENTED_EDGE('',*,*,#28768,.F.) ;
#40525 = ORIENTED_EDGE('',*,*,#28732,.F.) ;
#40526 = ORIENTED_EDGE('',*,*,#28731,.F.) ;
#40527 = ORIENTED_EDGE('',*,*,#28769,.T.) ;
#40528 = ORIENTED_EDGE('',*,*,#28526,.F.) ;
#40529 = ORIENTED_EDGE('',*,*,#28769,.F.) ;
#40530 = ORIENTED_EDGE('',*,*,#28728,.F.) ;
#40531 = ORIENTED_EDGE('',*,*,#28720,.F.) ;
#40532 = ORIENTED_EDGE('',*,*,#28770,.F.) ;
#40533 = ORIENTED_EDGE('',*,*,#28771,.F.) ;
#40534 = ORIENTED_EDGE('',*,*,#28772,.T.) ;
#40535 = ORIENTED_EDGE('',*,*,#28009,.T.) ;
#40536 = ORIENTED_EDGE('',*,*,#28733,.F.) ;
#40537 = ORIENTED_EDGE('',*,*,#28768,.T.) ;
#40538 = ORIENTED_EDGE('',*,*,#28740,.T.) ;
#40539 = ORIENTED_EDGE('',*,*,#27982,.F.) ;
#40540 = ORIENTED_EDGE('',*,*,#28010,.T.) ;
#40541 = ORIENTED_EDGE('',*,*,#28772,.F.) ;
#40542 = ORIENTED_EDGE('',*,*,#28686,.T.) ;
#40543 = ORIENTED_EDGE('',*,*,#28685,.F.) ;
#40544 = ORIENTED_EDGE('',*,*,#27983,.F.) ;
#40545 = ORIENTED_EDGE('',*,*,#28711,.F.) ;
#40546 = ORIENTED_EDGE('',*,*,#27801,.T.) ;
#40547 = ORIENTED_EDGE('',*,*,#27805,.F.) ;
#40548 = ORIENTED_EDGE('',*,*,#28773,.F.) ;
#40549 = ORIENTED_EDGE('',*,*,#28774,.F.) ;
#40550 = ORIENTED_EDGE('',*,*,#28713,.F.) ;
#40551 = ORIENTED_EDGE('',*,*,#28774,.T.) ;
#40552 = ORIENTED_EDGE('',*,*,#28775,.T.) ;
#40553 = ORIENTED_EDGE('',*,*,#28776,.T.) ;
#40554 = ORIENTED_EDGE('',*,*,#28715,.F.) ;
#40555 = ORIENTED_EDGE('',*,*,#28777,.T.) ;
#40556 = ORIENTED_EDGE('',*,*,#28778,.T.) ;
#40557 = ORIENTED_EDGE('',*,*,#28773,.T.) ;
#40558 = ORIENTED_EDGE('',*,*,#27810,.T.) ;
#40559 = ORIENTED_EDGE('',*,*,#27681,.F.) ;
#40560 = ORIENTED_EDGE('',*,*,#27799,.F.) ;
#40561 = ORIENTED_EDGE('',*,*,#28716,.F.) ;
#40562 = ORIENTED_EDGE('',*,*,#27675,.F.) ;
#40563 = ORIENTED_EDGE('',*,*,#27678,.F.) ;
#40564 = ORIENTED_EDGE('',*,*,#28714,.F.) ;
#40565 = ORIENTED_EDGE('',*,*,#28776,.F.) ;
#40566 = ORIENTED_EDGE('',*,*,#28779,.F.) ;
#40567 = ORIENTED_EDGE('',*,*,#28780,.T.) ;
#40568 = ORIENTED_EDGE('',*,*,#27860,.T.) ;
#40569 = ORIENTED_EDGE('',*,*,#28781,.F.) ;
#40570 = ORIENTED_EDGE('',*,*,#27854,.T.) ;
#40571 = ORIENTED_EDGE('',*,*,#28780,.F.) ;
#40572 = ORIENTED_EDGE('',*,*,#28782,.F.) ;
#40573 = ORIENTED_EDGE('',*,*,#27937,.F.) ;
#40574 = ORIENTED_EDGE('',*,*,#27855,.T.) ;
#40575 = ORIENTED_EDGE('',*,*,#28781,.T.) ;
#40576 = ORIENTED_EDGE('',*,*,#28783,.T.) ;
#40577 = ORIENTED_EDGE('',*,*,#27942,.F.) ;
#40578 = ORIENTED_EDGE('',*,*,#28783,.F.) ;
#40579 = ORIENTED_EDGE('',*,*,#28782,.T.) ;
#40580 = ORIENTED_EDGE('',*,*,#28779,.T.) ;
#40581 = ORIENTED_EDGE('',*,*,#28775,.F.) ;
#40582 = ORIENTED_EDGE('',*,*,#28778,.F.) ;
#40583 = ORIENTED_EDGE('',*,*,#28784,.F.) ;
#40584 = ORIENTED_EDGE('',*,*,#28785,.F.) ;
#40585 = ORIENTED_EDGE('',*,*,#27948,.F.) ;
#40586 = ORIENTED_EDGE('',*,*,#27945,.F.) ;
#40587 = ORIENTED_EDGE('',*,*,#28722,.T.) ;
#40588 = ORIENTED_EDGE('',*,*,#28723,.T.) ;
#40589 = ORIENTED_EDGE('',*,*,#27654,.T.) ;
#40590 = ORIENTED_EDGE('',*,*,#27662,.F.) ;
#40591 = ORIENTED_EDGE('',*,*,#28786,.F.) ;
#40592 = ORIENTED_EDGE('',*,*,#28787,.T.) ;
#40593 = ORIENTED_EDGE('',*,*,#27691,.T.) ;
#40594 = ORIENTED_EDGE('',*,*,#27667,.T.) ;
#40595 = ORIENTED_EDGE('',*,*,#27660,.T.) ;
#40596 = ORIENTED_EDGE('',*,*,#28788,.T.) ;
#40597 = ORIENTED_EDGE('',*,*,#28699,.T.) ;
#40598 = ORIENTED_EDGE('',*,*,#28789,.F.) ;
#40599 = ORIENTED_EDGE('',*,*,#28544,.F.) ;
#40600 = ORIENTED_EDGE('',*,*,#27614,.T.) ;
#40601 = ORIENTED_EDGE('',*,*,#28790,.T.) ;
#40602 = ORIENTED_EDGE('',*,*,#28791,.T.) ;
#40603 = ORIENTED_EDGE('',*,*,#28790,.F.) ;
#40604 = ORIENTED_EDGE('',*,*,#27613,.F.) ;
#40605 = ORIENTED_EDGE('',*,*,#28792,.F.) ;
#40606 = ORIENTED_EDGE('',*,*,#28683,.F.) ;
#40607 = ORIENTED_EDGE('',*,*,#28688,.F.) ;
#40608 = ORIENTED_EDGE('',*,*,#28739,.F.) ;
#40609 = ORIENTED_EDGE('',*,*,#28793,.T.) ;
#40610 = ORIENTED_EDGE('',*,*,#28794,.T.) ;
#40611 = ORIENTED_EDGE('',*,*,#28795,.F.) ;
#40612 = ORIENTED_EDGE('',*,*,#28735,.F.) ;
#40613 = ORIENTED_EDGE('',*,*,#28796,.F.) ;
#40614 = ORIENTED_EDGE('',*,*,#28797,.F.) ;
#40615 = ORIENTED_EDGE('',*,*,#27790,.T.) ;
#40616 = ORIENTED_EDGE('',*,*,#27793,.T.) ;
#40617 = ORIENTED_EDGE('',*,*,#28725,.F.) ;
#40618 = ORIENTED_EDGE('',*,*,#28727,.F.) ;
#40619 = ORIENTED_EDGE('',*,*,#28730,.F.) ;
#40620 = ORIENTED_EDGE('',*,*,#28007,.F.) ;
#40621 = ORIENTED_EDGE('',*,*,#28690,.F.) ;
#40622 = ORIENTED_EDGE('',*,*,#28696,.T.) ;
#40623 = ORIENTED_EDGE('',*,*,#28532,.F.) ;
#40624 = ORIENTED_EDGE('',*,*,#28798,.T.) ;
#40625 = ORIENTED_EDGE('',*,*,#28796,.T.) ;
#40626 = ORIENTED_EDGE('',*,*,#28734,.T.) ;
#40627 = ORIENTED_EDGE('',*,*,#28660,.F.) ;
#40628 = ORIENTED_EDGE('',*,*,#28679,.F.) ;
#40629 = ORIENTED_EDGE('',*,*,#28799,.F.) ;
#40630 = ORIENTED_EDGE('',*,*,#28665,.F.) ;
#40631 = ORIENTED_EDGE('',*,*,#28662,.F.) ;
#40632 = ORIENTED_EDGE('',*,*,#27960,.F.) ;
#40633 = ORIENTED_EDGE('',*,*,#28684,.T.) ;
#40634 = ORIENTED_EDGE('',*,*,#28792,.T.) ;
#40635 = ORIENTED_EDGE('',*,*,#27612,.T.) ;
#40636 = ORIENTED_EDGE('',*,*,#28800,.F.) ;
#40637 = ORIENTED_EDGE('',*,*,#28801,.F.) ;
#40638 = ORIENTED_EDGE('',*,*,#28802,.F.) ;
#40639 = ORIENTED_EDGE('',*,*,#28803,.T.) ;
#40640 = ORIENTED_EDGE('',*,*,#28115,.F.) ;
#40641 = ORIENTED_EDGE('',*,*,#28804,.F.) ;
#40642 = ORIENTED_EDGE('',*,*,#28116,.F.) ;
#40643 = ORIENTED_EDGE('',*,*,#28803,.F.) ;
#40644 = ORIENTED_EDGE('',*,*,#28805,.F.) ;
#40645 = ORIENTED_EDGE('',*,*,#28806,.F.) ;
#40646 = ORIENTED_EDGE('',*,*,#28120,.F.) ;
#40647 = ORIENTED_EDGE('',*,*,#28807,.F.) ;
#40648 = ORIENTED_EDGE('',*,*,#28808,.T.) ;
#40649 = ORIENTED_EDGE('',*,*,#28809,.T.) ;
#40650 = ORIENTED_EDGE('',*,*,#28121,.F.) ;
#40651 = ORIENTED_EDGE('',*,*,#28809,.F.) ;
#40652 = ORIENTED_EDGE('',*,*,#28810,.T.) ;
#40653 = ORIENTED_EDGE('',*,*,#28033,.F.) ;
#40654 = ORIENTED_EDGE('',*,*,#28040,.F.) ;
#40655 = ORIENTED_EDGE('',*,*,#28811,.F.) ;
#40656 = ORIENTED_EDGE('',*,*,#28812,.F.) ;
#40657 = ORIENTED_EDGE('',*,*,#28813,.F.) ;
#40658 = ORIENTED_EDGE('',*,*,#28801,.T.) ;
#40659 = ORIENTED_EDGE('',*,*,#28119,.F.) ;
#40660 = ORIENTED_EDGE('',*,*,#28814,.F.) ;
#40661 = ORIENTED_EDGE('',*,*,#28815,.F.) ;
#40662 = ORIENTED_EDGE('',*,*,#28807,.T.) ;
#40663 = ORIENTED_EDGE('',*,*,#28804,.T.) ;
#40664 = ORIENTED_EDGE('',*,*,#28114,.F.) ;
#40665 = ORIENTED_EDGE('',*,*,#28816,.F.) ;
#40666 = ORIENTED_EDGE('',*,*,#28817,.T.) ;
#40667 = ORIENTED_EDGE('',*,*,#28814,.T.) ;
#40668 = ORIENTED_EDGE('',*,*,#28118,.T.) ;
#40669 = ORIENTED_EDGE('',*,*,#28818,.T.) ;
#40670 = ORIENTED_EDGE('',*,*,#28819,.T.) ;
#40671 = ORIENTED_EDGE('',*,*,#28806,.T.) ;
#40672 = ORIENTED_EDGE('',*,*,#28820,.T.) ;
#40673 = ORIENTED_EDGE('',*,*,#28818,.F.) ;
#40674 = ORIENTED_EDGE('',*,*,#28117,.F.) ;
#40675 = ORIENTED_EDGE('',*,*,#28810,.F.) ;
#40676 = ORIENTED_EDGE('',*,*,#28808,.F.) ;
#40677 = ORIENTED_EDGE('',*,*,#28815,.T.) ;
#40678 = ORIENTED_EDGE('',*,*,#28819,.F.) ;
#40679 = ORIENTED_EDGE('',*,*,#28820,.F.) ;
#40680 = ORIENTED_EDGE('',*,*,#28805,.T.) ;
#40681 = ORIENTED_EDGE('',*,*,#28802,.T.) ;
#40682 = ORIENTED_EDGE('',*,*,#28813,.T.) ;
#40683 = ORIENTED_EDGE('',*,*,#28821,.F.) ;
#40684 = ORIENTED_EDGE('',*,*,#28822,.F.) ;
#40685 = ORIENTED_EDGE('',*,*,#28823,.F.) ;
#40686 = ORIENTED_EDGE('',*,*,#28824,.F.) ;
#40687 = ORIENTED_EDGE('',*,*,#28825,.F.) ;
#40688 = ORIENTED_EDGE('',*,*,#28043,.F.) ;
#40689 = ORIENTED_EDGE('',*,*,#28031,.F.) ;
#40690 = ORIENTED_EDGE('',*,*,#28034,.F.) ;
#40691 = ORIENTED_EDGE('',*,*,#28026,.T.) ;
#40692 = ORIENTED_EDGE('',*,*,#28826,.T.) ;
#40693 = ORIENTED_EDGE('',*,*,#28827,.T.) ;
#40694 = ORIENTED_EDGE('',*,*,#28023,.T.) ;
#40695 = ORIENTED_EDGE('',*,*,#28823,.T.) ;
#40696 = ORIENTED_EDGE('',*,*,#28828,.T.) ;
#40697 = ORIENTED_EDGE('',*,*,#27978,.T.) ;
#40698 = ORIENTED_EDGE('',*,*,#28829,.T.) ;
#40699 = ORIENTED_EDGE('',*,*,#28561,.T.) ;
#40700 = ORIENTED_EDGE('',*,*,#28830,.T.) ;
#40701 = ORIENTED_EDGE('',*,*,#28824,.T.) ;
#40702 = ORIENTED_EDGE('',*,*,#28829,.F.) ;
#40703 = ORIENTED_EDGE('',*,*,#28044,.T.) ;
#40704 = ORIENTED_EDGE('',*,*,#28825,.T.) ;
#40705 = ORIENTED_EDGE('',*,*,#28830,.F.) ;
#40706 = ORIENTED_EDGE('',*,*,#28562,.T.) ;
#40707 = ORIENTED_EDGE('',*,*,#28831,.T.) ;
#40708 = ORIENTED_EDGE('',*,*,#27974,.T.) ;
#40709 = ORIENTED_EDGE('',*,*,#28828,.F.) ;
#40710 = ORIENTED_EDGE('',*,*,#28822,.T.) ;
#40711 = ORIENTED_EDGE('',*,*,#28832,.F.) ;
#40712 = ORIENTED_EDGE('',*,*,#27975,.T.) ;
#40713 = ORIENTED_EDGE('',*,*,#28831,.F.) ;
#40714 = ORIENTED_EDGE('',*,*,#28821,.T.) ;
#40715 = ORIENTED_EDGE('',*,*,#28812,.T.) ;
#40716 = ORIENTED_EDGE('',*,*,#28445,.F.) ;
#40717 = ORIENTED_EDGE('',*,*,#28833,.F.) ;
#40718 = ORIENTED_EDGE('',*,*,#28834,.F.) ;
#40719 = ORIENTED_EDGE('',*,*,#28835,.F.) ;
#40720 = ORIENTED_EDGE('',*,*,#28451,.F.) ;
#40721 = ORIENTED_EDGE('',*,*,#28836,.F.) ;
#40722 = ORIENTED_EDGE('',*,*,#28837,.F.) ;
#40723 = ORIENTED_EDGE('',*,*,#28838,.F.) ;
#40724 = ORIENTED_EDGE('',*,*,#28839,.F.) ;
#40725 = ORIENTED_EDGE('',*,*,#28837,.T.) ;
#40726 = ORIENTED_EDGE('',*,*,#28840,.F.) ;
#40727 = ORIENTED_EDGE('',*,*,#28834,.T.) ;
#40728 = ORIENTED_EDGE('',*,*,#28475,.F.) ;
#40729 = ORIENTED_EDGE('',*,*,#28841,.T.) ;
#40730 = ORIENTED_EDGE('',*,*,#28485,.F.) ;
#40731 = ORIENTED_EDGE('',*,*,#28482,.F.) ;
#40732 = ORIENTED_EDGE('',*,*,#28479,.F.) ;
#40733 = ORIENTED_EDGE('',*,*,#28838,.T.) ;
#40734 = ORIENTED_EDGE('',*,*,#28839,.T.) ;
#40735 = ORIENTED_EDGE('',*,*,#28833,.T.) ;
#40736 = ORIENTED_EDGE('',*,*,#28444,.F.) ;
#40737 = ORIENTED_EDGE('',*,*,#28448,.T.) ;
#40738 = ORIENTED_EDGE('',*,*,#28449,.F.) ;
#40739 = ORIENTED_EDGE('',*,*,#28472,.F.) ;
#40740 = ORIENTED_EDGE('',*,*,#28842,.T.) ;
#40741 = ORIENTED_EDGE('',*,*,#28476,.F.) ;
#40742 = ORIENTED_EDGE('',*,*,#28461,.F.) ;
#40743 = ORIENTED_EDGE('',*,*,#28465,.F.) ;
#40744 = ORIENTED_EDGE('',*,*,#28843,.T.) ;
#40745 = ORIENTED_EDGE('',*,*,#28473,.F.) ;
#40746 = ORIENTED_EDGE('',*,*,#28470,.F.) ;
#40747 = ORIENTED_EDGE('',*,*,#28468,.F.) ;
#40748 = ORIENTED_EDGE('',*,*,#28836,.T.) ;
#40749 = ORIENTED_EDGE('',*,*,#28450,.F.) ;
#40750 = ORIENTED_EDGE('',*,*,#28446,.T.) ;
#40751 = ORIENTED_EDGE('',*,*,#28442,.F.) ;
#40752 = ORIENTED_EDGE('',*,*,#28835,.T.) ;
#40753 = ORIENTED_EDGE('',*,*,#28840,.T.) ;
#40754 = ORIENTED_EDGE('',*,*,#28471,.T.) ;
#40755 = ORIENTED_EDGE('',*,*,#28843,.F.) ;
#40756 = ORIENTED_EDGE('',*,*,#28464,.F.) ;
#40757 = ORIENTED_EDGE('',*,*,#28507,.F.) ;
#40758 = ORIENTED_EDGE('',*,*,#28483,.F.) ;
#40759 = ORIENTED_EDGE('',*,*,#28841,.F.) ;
#40760 = ORIENTED_EDGE('',*,*,#28474,.T.) ;
#40761 = ORIENTED_EDGE('',*,*,#28842,.F.) ;
#40762 = ORIENTED_EDGE('',*,*,#28844,.T.) ;
#40763 = ORIENTED_EDGE('',*,*,#28845,.T.) ;
#40764 = ORIENTED_EDGE('',*,*,#28846,.T.) ;
#40765 = ORIENTED_EDGE('',*,*,#28847,.F.) ;
#40766 = ORIENTED_EDGE('',*,*,#28848,.T.) ;
#40767 = ORIENTED_EDGE('',*,*,#28849,.T.) ;
#40768 = ORIENTED_EDGE('',*,*,#28850,.T.) ;
#40769 = ORIENTED_EDGE('',*,*,#28845,.F.) ;
#40770 = ORIENTED_EDGE('',*,*,#28851,.T.) ;
#40771 = ORIENTED_EDGE('',*,*,#28852,.T.) ;
#40772 = ORIENTED_EDGE('',*,*,#28853,.T.) ;
#40773 = ORIENTED_EDGE('',*,*,#28849,.F.) ;
#40774 = ORIENTED_EDGE('',*,*,#28854,.T.) ;
#40775 = ORIENTED_EDGE('',*,*,#28852,.F.) ;
#40776 = ORIENTED_EDGE('',*,*,#28855,.T.) ;
#40777 = ORIENTED_EDGE('',*,*,#28856,.T.) ;
#40778 = ORIENTED_EDGE('',*,*,#28857,.T.) ;
#40779 = ORIENTED_EDGE('',*,*,#28856,.F.) ;
#40780 = ORIENTED_EDGE('',*,*,#28858,.T.) ;
#40781 = ORIENTED_EDGE('',*,*,#28859,.T.) ;
#40782 = ORIENTED_EDGE('',*,*,#28860,.T.) ;
#40783 = ORIENTED_EDGE('',*,*,#28859,.F.) ;
#40784 = ORIENTED_EDGE('',*,*,#28861,.T.) ;
#40785 = ORIENTED_EDGE('',*,*,#28862,.T.) ;
#40786 = ORIENTED_EDGE('',*,*,#28863,.T.) ;
#40787 = ORIENTED_EDGE('',*,*,#28862,.F.) ;
#40788 = ORIENTED_EDGE('',*,*,#28864,.T.) ;
#40789 = ORIENTED_EDGE('',*,*,#28847,.T.) ;
#40790 = ORIENTED_EDGE('',*,*,#28857,.F.) ;
#40791 = ORIENTED_EDGE('',*,*,#28865,.F.) ;
#40792 = ORIENTED_EDGE('',*,*,#28866,.F.) ;
#40793 = ORIENTED_EDGE('',*,*,#28867,.T.) ;
#40794 = ORIENTED_EDGE('',*,*,#28860,.F.) ;
#40795 = ORIENTED_EDGE('',*,*,#28868,.F.) ;
#40796 = ORIENTED_EDGE('',*,*,#28869,.F.) ;
#40797 = ORIENTED_EDGE('',*,*,#28865,.T.) ;
#40798 = ORIENTED_EDGE('',*,*,#28863,.F.) ;
#40799 = ORIENTED_EDGE('',*,*,#28870,.F.) ;
#40800 = ORIENTED_EDGE('',*,*,#28871,.F.) ;
#40801 = ORIENTED_EDGE('',*,*,#28868,.T.) ;
#40802 = ORIENTED_EDGE('',*,*,#28846,.F.) ;
#40803 = ORIENTED_EDGE('',*,*,#28872,.F.) ;
#40804 = ORIENTED_EDGE('',*,*,#28873,.F.) ;
#40805 = ORIENTED_EDGE('',*,*,#28870,.T.) ;
#40806 = ORIENTED_EDGE('',*,*,#28844,.F.) ;
#40807 = ORIENTED_EDGE('',*,*,#28864,.F.) ;
#40808 = ORIENTED_EDGE('',*,*,#28861,.F.) ;
#40809 = ORIENTED_EDGE('',*,*,#28858,.F.) ;
#40810 = ORIENTED_EDGE('',*,*,#28855,.F.) ;
#40811 = ORIENTED_EDGE('',*,*,#28851,.F.) ;
#40812 = ORIENTED_EDGE('',*,*,#28848,.F.) ;
#40813 = ORIENTED_EDGE('',*,*,#28874,.T.) ;
#40814 = ORIENTED_EDGE('',*,*,#28875,.T.) ;
#40815 = ORIENTED_EDGE('',*,*,#28876,.T.) ;
#40816 = ORIENTED_EDGE('',*,*,#28877,.F.) ;
#40817 = ORIENTED_EDGE('',*,*,#28878,.T.) ;
#40818 = ORIENTED_EDGE('',*,*,#28879,.T.) ;
#40819 = ORIENTED_EDGE('',*,*,#28880,.T.) ;
#40820 = ORIENTED_EDGE('',*,*,#28875,.F.) ;
#40821 = ORIENTED_EDGE('',*,*,#28881,.T.) ;
#40822 = ORIENTED_EDGE('',*,*,#28882,.T.) ;
#40823 = ORIENTED_EDGE('',*,*,#28883,.T.) ;
#40824 = ORIENTED_EDGE('',*,*,#28879,.F.) ;
#40825 = ORIENTED_EDGE('',*,*,#28884,.T.) ;
#40826 = ORIENTED_EDGE('',*,*,#28882,.F.) ;
#40827 = ORIENTED_EDGE('',*,*,#28885,.T.) ;
#40828 = ORIENTED_EDGE('',*,*,#28886,.T.) ;
#40829 = ORIENTED_EDGE('',*,*,#28887,.T.) ;
#40830 = ORIENTED_EDGE('',*,*,#28886,.F.) ;
#40831 = ORIENTED_EDGE('',*,*,#28888,.T.) ;
#40832 = ORIENTED_EDGE('',*,*,#28889,.T.) ;
#40833 = ORIENTED_EDGE('',*,*,#28890,.T.) ;
#40834 = ORIENTED_EDGE('',*,*,#28889,.F.) ;
#40835 = ORIENTED_EDGE('',*,*,#28891,.T.) ;
#40836 = ORIENTED_EDGE('',*,*,#28892,.T.) ;
#40837 = ORIENTED_EDGE('',*,*,#28893,.T.) ;
#40838 = ORIENTED_EDGE('',*,*,#28892,.F.) ;
#40839 = ORIENTED_EDGE('',*,*,#28894,.T.) ;
#40840 = ORIENTED_EDGE('',*,*,#28877,.T.) ;
#40841 = ORIENTED_EDGE('',*,*,#28887,.F.) ;
#40842 = ORIENTED_EDGE('',*,*,#28895,.F.) ;
#40843 = ORIENTED_EDGE('',*,*,#28896,.F.) ;
#40844 = ORIENTED_EDGE('',*,*,#28897,.T.) ;
#40845 = ORIENTED_EDGE('',*,*,#28890,.F.) ;
#40846 = ORIENTED_EDGE('',*,*,#28898,.F.) ;
#40847 = ORIENTED_EDGE('',*,*,#28899,.F.) ;
#40848 = ORIENTED_EDGE('',*,*,#28895,.T.) ;
#40849 = ORIENTED_EDGE('',*,*,#28893,.F.) ;
#40850 = ORIENTED_EDGE('',*,*,#28900,.F.) ;
#40851 = ORIENTED_EDGE('',*,*,#28901,.F.) ;
#40852 = ORIENTED_EDGE('',*,*,#28898,.T.) ;
#40853 = ORIENTED_EDGE('',*,*,#28876,.F.) ;
#40854 = ORIENTED_EDGE('',*,*,#28902,.F.) ;
#40855 = ORIENTED_EDGE('',*,*,#28903,.F.) ;
#40856 = ORIENTED_EDGE('',*,*,#28900,.T.) ;
#40857 = ORIENTED_EDGE('',*,*,#28874,.F.) ;
#40858 = ORIENTED_EDGE('',*,*,#28894,.F.) ;
#40859 = ORIENTED_EDGE('',*,*,#28891,.F.) ;
#40860 = ORIENTED_EDGE('',*,*,#28888,.F.) ;
#40861 = ORIENTED_EDGE('',*,*,#28885,.F.) ;
#40862 = ORIENTED_EDGE('',*,*,#28881,.F.) ;
#40863 = ORIENTED_EDGE('',*,*,#28878,.F.) ;
#40864 = ORIENTED_EDGE('',*,*,#28904,.T.) ;
#40865 = ORIENTED_EDGE('',*,*,#28905,.T.) ;
#40866 = ORIENTED_EDGE('',*,*,#28906,.T.) ;
#40867 = ORIENTED_EDGE('',*,*,#28907,.F.) ;
#40868 = ORIENTED_EDGE('',*,*,#28908,.T.) ;
#40869 = ORIENTED_EDGE('',*,*,#28909,.T.) ;
#40870 = ORIENTED_EDGE('',*,*,#28910,.T.) ;
#40871 = ORIENTED_EDGE('',*,*,#28905,.F.) ;
#40872 = ORIENTED_EDGE('',*,*,#28911,.T.) ;
#40873 = ORIENTED_EDGE('',*,*,#28912,.T.) ;
#40874 = ORIENTED_EDGE('',*,*,#28913,.T.) ;
#40875 = ORIENTED_EDGE('',*,*,#28909,.F.) ;
#40876 = ORIENTED_EDGE('',*,*,#28914,.T.) ;
#40877 = ORIENTED_EDGE('',*,*,#28912,.F.) ;
#40878 = ORIENTED_EDGE('',*,*,#28915,.T.) ;
#40879 = ORIENTED_EDGE('',*,*,#28916,.T.) ;
#40880 = ORIENTED_EDGE('',*,*,#28917,.T.) ;
#40881 = ORIENTED_EDGE('',*,*,#28916,.F.) ;
#40882 = ORIENTED_EDGE('',*,*,#28918,.T.) ;
#40883 = ORIENTED_EDGE('',*,*,#28919,.T.) ;
#40884 = ORIENTED_EDGE('',*,*,#28920,.T.) ;
#40885 = ORIENTED_EDGE('',*,*,#28919,.F.) ;
#40886 = ORIENTED_EDGE('',*,*,#28921,.T.) ;
#40887 = ORIENTED_EDGE('',*,*,#28922,.T.) ;
#40888 = ORIENTED_EDGE('',*,*,#28923,.T.) ;
#40889 = ORIENTED_EDGE('',*,*,#28922,.F.) ;
#40890 = ORIENTED_EDGE('',*,*,#28924,.T.) ;
#40891 = ORIENTED_EDGE('',*,*,#28907,.T.) ;
#40892 = ORIENTED_EDGE('',*,*,#28917,.F.) ;
#40893 = ORIENTED_EDGE('',*,*,#28925,.F.) ;
#40894 = ORIENTED_EDGE('',*,*,#28926,.F.) ;
#40895 = ORIENTED_EDGE('',*,*,#28927,.T.) ;
#40896 = ORIENTED_EDGE('',*,*,#28920,.F.) ;
#40897 = ORIENTED_EDGE('',*,*,#28928,.F.) ;
#40898 = ORIENTED_EDGE('',*,*,#28929,.F.) ;
#40899 = ORIENTED_EDGE('',*,*,#28925,.T.) ;
#40900 = ORIENTED_EDGE('',*,*,#28923,.F.) ;
#40901 = ORIENTED_EDGE('',*,*,#28930,.F.) ;
#40902 = ORIENTED_EDGE('',*,*,#28931,.F.) ;
#40903 = ORIENTED_EDGE('',*,*,#28928,.T.) ;
#40904 = ORIENTED_EDGE('',*,*,#28906,.F.) ;
#40905 = ORIENTED_EDGE('',*,*,#28932,.F.) ;
#40906 = ORIENTED_EDGE('',*,*,#28933,.F.) ;
#40907 = ORIENTED_EDGE('',*,*,#28930,.T.) ;
#40908 = ORIENTED_EDGE('',*,*,#28904,.F.) ;
#40909 = ORIENTED_EDGE('',*,*,#28924,.F.) ;
#40910 = ORIENTED_EDGE('',*,*,#28921,.F.) ;
#40911 = ORIENTED_EDGE('',*,*,#28918,.F.) ;
#40912 = ORIENTED_EDGE('',*,*,#28915,.F.) ;
#40913 = ORIENTED_EDGE('',*,*,#28911,.F.) ;
#40914 = ORIENTED_EDGE('',*,*,#28908,.F.) ;
#40915 = ORIENTED_EDGE('',*,*,#28934,.T.) ;
#40916 = ORIENTED_EDGE('',*,*,#28935,.T.) ;
#40917 = ORIENTED_EDGE('',*,*,#28936,.T.) ;
#40918 = ORIENTED_EDGE('',*,*,#28937,.F.) ;
#40919 = ORIENTED_EDGE('',*,*,#28938,.T.) ;
#40920 = ORIENTED_EDGE('',*,*,#28935,.F.) ;
#40921 = ORIENTED_EDGE('',*,*,#28939,.T.) ;
#40922 = ORIENTED_EDGE('',*,*,#28940,.T.) ;
#40923 = ORIENTED_EDGE('',*,*,#28941,.T.) ;
#40924 = ORIENTED_EDGE('',*,*,#28940,.F.) ;
#40925 = ORIENTED_EDGE('',*,*,#28942,.T.) ;
#40926 = ORIENTED_EDGE('',*,*,#28943,.T.) ;
#40927 = ORIENTED_EDGE('',*,*,#28944,.T.) ;
#40928 = ORIENTED_EDGE('',*,*,#28943,.F.) ;
#40929 = ORIENTED_EDGE('',*,*,#28945,.T.) ;
#40930 = ORIENTED_EDGE('',*,*,#28937,.T.) ;
#40931 = ORIENTED_EDGE('',*,*,#28944,.F.) ;
#40932 = ORIENTED_EDGE('',*,*,#28946,.F.) ;
#40933 = ORIENTED_EDGE('',*,*,#28947,.F.) ;
#40934 = ORIENTED_EDGE('',*,*,#28948,.T.) ;
#40935 = ORIENTED_EDGE('',*,*,#28936,.F.) ;
#40936 = ORIENTED_EDGE('',*,*,#28949,.F.) ;
#40937 = ORIENTED_EDGE('',*,*,#28950,.F.) ;
#40938 = ORIENTED_EDGE('',*,*,#28946,.T.) ;
#40939 = ORIENTED_EDGE('',*,*,#28934,.F.) ;
#40940 = ORIENTED_EDGE('',*,*,#28945,.F.) ;
#40941 = ORIENTED_EDGE('',*,*,#28942,.F.) ;
#40942 = ORIENTED_EDGE('',*,*,#28939,.F.) ;
#40943 = ORIENTED_EDGE('',*,*,#28951,.T.) ;
#40944 = ORIENTED_EDGE('',*,*,#28952,.T.) ;
#40945 = ORIENTED_EDGE('',*,*,#28953,.T.) ;
#40946 = ORIENTED_EDGE('',*,*,#28954,.F.) ;
#40947 = ORIENTED_EDGE('',*,*,#28955,.T.) ;
#40948 = ORIENTED_EDGE('',*,*,#28956,.T.) ;
#40949 = ORIENTED_EDGE('',*,*,#28957,.T.) ;
#40950 = ORIENTED_EDGE('',*,*,#28952,.F.) ;
#40951 = ORIENTED_EDGE('',*,*,#28958,.T.) ;
#40952 = ORIENTED_EDGE('',*,*,#28959,.T.) ;
#40953 = ORIENTED_EDGE('',*,*,#28960,.T.) ;
#40954 = ORIENTED_EDGE('',*,*,#28956,.F.) ;
#40955 = ORIENTED_EDGE('',*,*,#28961,.T.) ;
#40956 = ORIENTED_EDGE('',*,*,#28959,.F.) ;
#40957 = ORIENTED_EDGE('',*,*,#28962,.T.) ;
#40958 = ORIENTED_EDGE('',*,*,#28963,.T.) ;
#40959 = ORIENTED_EDGE('',*,*,#28964,.T.) ;
#40960 = ORIENTED_EDGE('',*,*,#28963,.F.) ;
#40961 = ORIENTED_EDGE('',*,*,#28965,.T.) ;
#40962 = ORIENTED_EDGE('',*,*,#28966,.T.) ;
#40963 = ORIENTED_EDGE('',*,*,#28967,.T.) ;
#40964 = ORIENTED_EDGE('',*,*,#28966,.F.) ;
#40965 = ORIENTED_EDGE('',*,*,#28968,.T.) ;
#40966 = ORIENTED_EDGE('',*,*,#28969,.T.) ;
#40967 = ORIENTED_EDGE('',*,*,#28970,.T.) ;
#40968 = ORIENTED_EDGE('',*,*,#28969,.F.) ;
#40969 = ORIENTED_EDGE('',*,*,#28971,.T.) ;
#40970 = ORIENTED_EDGE('',*,*,#28954,.T.) ;
#40971 = ORIENTED_EDGE('',*,*,#28964,.F.) ;
#40972 = ORIENTED_EDGE('',*,*,#28972,.F.) ;
#40973 = ORIENTED_EDGE('',*,*,#28973,.F.) ;
#40974 = ORIENTED_EDGE('',*,*,#28974,.T.) ;
#40975 = ORIENTED_EDGE('',*,*,#28967,.F.) ;
#40976 = ORIENTED_EDGE('',*,*,#28975,.F.) ;
#40977 = ORIENTED_EDGE('',*,*,#28976,.F.) ;
#40978 = ORIENTED_EDGE('',*,*,#28972,.T.) ;
#40979 = ORIENTED_EDGE('',*,*,#28970,.F.) ;
#40980 = ORIENTED_EDGE('',*,*,#28977,.F.) ;
#40981 = ORIENTED_EDGE('',*,*,#28978,.F.) ;
#40982 = ORIENTED_EDGE('',*,*,#28975,.T.) ;
#40983 = ORIENTED_EDGE('',*,*,#28953,.F.) ;
#40984 = ORIENTED_EDGE('',*,*,#28979,.F.) ;
#40985 = ORIENTED_EDGE('',*,*,#28980,.F.) ;
#40986 = ORIENTED_EDGE('',*,*,#28977,.T.) ;
#40987 = ORIENTED_EDGE('',*,*,#28951,.F.) ;
#40988 = ORIENTED_EDGE('',*,*,#28971,.F.) ;
#40989 = ORIENTED_EDGE('',*,*,#28968,.F.) ;
#40990 = ORIENTED_EDGE('',*,*,#28965,.F.) ;
#40991 = ORIENTED_EDGE('',*,*,#28962,.F.) ;
#40992 = ORIENTED_EDGE('',*,*,#28958,.F.) ;
#40993 = ORIENTED_EDGE('',*,*,#28955,.F.) ;
#40994 = ORIENTED_EDGE('',*,*,#28981,.T.) ;
#40995 = ORIENTED_EDGE('',*,*,#28982,.T.) ;
#40996 = ORIENTED_EDGE('',*,*,#28983,.T.) ;
#40997 = ORIENTED_EDGE('',*,*,#28984,.F.) ;
#40998 = ORIENTED_EDGE('',*,*,#28985,.T.) ;
#40999 = ORIENTED_EDGE('',*,*,#28982,.F.) ;
#41000 = ORIENTED_EDGE('',*,*,#28986,.T.) ;
#41001 = ORIENTED_EDGE('',*,*,#28987,.T.) ;
#41002 = ORIENTED_EDGE('',*,*,#28988,.T.) ;
#41003 = ORIENTED_EDGE('',*,*,#28987,.F.) ;
#41004 = ORIENTED_EDGE('',*,*,#28989,.T.) ;
#41005 = ORIENTED_EDGE('',*,*,#28990,.T.) ;
#41006 = ORIENTED_EDGE('',*,*,#28991,.T.) ;
#41007 = ORIENTED_EDGE('',*,*,#28990,.F.) ;
#41008 = ORIENTED_EDGE('',*,*,#28992,.T.) ;
#41009 = ORIENTED_EDGE('',*,*,#28984,.T.) ;
#41010 = ORIENTED_EDGE('',*,*,#28991,.F.) ;
#41011 = ORIENTED_EDGE('',*,*,#28993,.F.) ;
#41012 = ORIENTED_EDGE('',*,*,#28994,.F.) ;
#41013 = ORIENTED_EDGE('',*,*,#28995,.T.) ;
#41014 = ORIENTED_EDGE('',*,*,#28983,.F.) ;
#41015 = ORIENTED_EDGE('',*,*,#28996,.F.) ;
#41016 = ORIENTED_EDGE('',*,*,#28997,.F.) ;
#41017 = ORIENTED_EDGE('',*,*,#28993,.T.) ;
#41018 = ORIENTED_EDGE('',*,*,#28981,.F.) ;
#41019 = ORIENTED_EDGE('',*,*,#28992,.F.) ;
#41020 = ORIENTED_EDGE('',*,*,#28989,.F.) ;
#41021 = ORIENTED_EDGE('',*,*,#28986,.F.) ;
#41022 = ORIENTED_EDGE('',*,*,#28998,.T.) ;
#41023 = ORIENTED_EDGE('',*,*,#28999,.T.) ;
#41024 = ORIENTED_EDGE('',*,*,#29000,.T.) ;
#41025 = ORIENTED_EDGE('',*,*,#29001,.F.) ;
#41026 = ORIENTED_EDGE('',*,*,#29002,.T.) ;
#41027 = ORIENTED_EDGE('',*,*,#29003,.T.) ;
#41028 = ORIENTED_EDGE('',*,*,#29004,.T.) ;
#41029 = ORIENTED_EDGE('',*,*,#28999,.F.) ;
#41030 = ORIENTED_EDGE('',*,*,#29005,.T.) ;
#41031 = ORIENTED_EDGE('',*,*,#29006,.T.) ;
#41032 = ORIENTED_EDGE('',*,*,#29007,.T.) ;
#41033 = ORIENTED_EDGE('',*,*,#29003,.F.) ;
#41034 = ORIENTED_EDGE('',*,*,#29008,.T.) ;
#41035 = ORIENTED_EDGE('',*,*,#29009,.T.) ;
#41036 = ORIENTED_EDGE('',*,*,#29006,.F.) ;
#41037 = ORIENTED_EDGE('',*,*,#29010,.T.) ;
#41038 = ORIENTED_EDGE('',*,*,#29011,.T.) ;
#41039 = ORIENTED_EDGE('',*,*,#29008,.F.) ;
#41040 = ORIENTED_EDGE('',*,*,#29012,.T.) ;
#41041 = ORIENTED_EDGE('',*,*,#29013,.T.) ;
#41042 = ORIENTED_EDGE('',*,*,#29014,.T.) ;
#41043 = ORIENTED_EDGE('',*,*,#29013,.F.) ;
#41044 = ORIENTED_EDGE('',*,*,#29015,.T.) ;
#41045 = ORIENTED_EDGE('',*,*,#29016,.T.) ;
#41046 = ORIENTED_EDGE('',*,*,#29017,.T.) ;
#41047 = ORIENTED_EDGE('',*,*,#29018,.T.) ;
#41048 = ORIENTED_EDGE('',*,*,#29019,.T.) ;
#41049 = ORIENTED_EDGE('',*,*,#29016,.F.) ;
#41050 = ORIENTED_EDGE('',*,*,#29020,.T.) ;
#41051 = ORIENTED_EDGE('',*,*,#29021,.T.) ;
#41052 = ORIENTED_EDGE('',*,*,#29018,.F.) ;
#41053 = ORIENTED_EDGE('',*,*,#29022,.T.) ;
#41054 = ORIENTED_EDGE('',*,*,#29023,.T.) ;
#41055 = ORIENTED_EDGE('',*,*,#29020,.F.) ;
#41056 = ORIENTED_EDGE('',*,*,#29024,.T.) ;
#41057 = ORIENTED_EDGE('',*,*,#29025,.T.) ;
#41058 = ORIENTED_EDGE('',*,*,#29026,.T.) ;
#41059 = ORIENTED_EDGE('',*,*,#29025,.F.) ;
#41060 = ORIENTED_EDGE('',*,*,#29027,.T.) ;
#41061 = ORIENTED_EDGE('',*,*,#29028,.T.) ;
#41062 = ORIENTED_EDGE('',*,*,#29029,.T.) ;
#41063 = ORIENTED_EDGE('',*,*,#29028,.F.) ;
#41064 = ORIENTED_EDGE('',*,*,#29030,.T.) ;
#41065 = ORIENTED_EDGE('',*,*,#29001,.T.) ;
#41066 = ORIENTED_EDGE('',*,*,#29019,.F.) ;
#41067 = ORIENTED_EDGE('',*,*,#29031,.F.) ;
#41068 = ORIENTED_EDGE('',*,*,#29032,.F.) ;
#41069 = ORIENTED_EDGE('',*,*,#29033,.T.) ;
#41070 = ORIENTED_EDGE('',*,*,#29021,.F.) ;
#41071 = ORIENTED_EDGE('',*,*,#29034,.F.) ;
#41072 = ORIENTED_EDGE('',*,*,#29035,.F.) ;
#41073 = ORIENTED_EDGE('',*,*,#29031,.T.) ;
#41074 = ORIENTED_EDGE('',*,*,#29023,.F.) ;
#41075 = ORIENTED_EDGE('',*,*,#29036,.F.) ;
#41076 = ORIENTED_EDGE('',*,*,#29037,.F.) ;
#41077 = ORIENTED_EDGE('',*,*,#29034,.T.) ;
#41078 = ORIENTED_EDGE('',*,*,#29026,.F.) ;
#41079 = ORIENTED_EDGE('',*,*,#29038,.F.) ;
#41080 = ORIENTED_EDGE('',*,*,#29039,.F.) ;
#41081 = ORIENTED_EDGE('',*,*,#29036,.T.) ;
#41082 = ORIENTED_EDGE('',*,*,#29029,.F.) ;
#41083 = ORIENTED_EDGE('',*,*,#29040,.F.) ;
#41084 = ORIENTED_EDGE('',*,*,#29041,.F.) ;
#41085 = ORIENTED_EDGE('',*,*,#29038,.T.) ;
#41086 = ORIENTED_EDGE('',*,*,#29000,.F.) ;
#41087 = ORIENTED_EDGE('',*,*,#29042,.F.) ;
#41088 = ORIENTED_EDGE('',*,*,#29043,.F.) ;
#41089 = ORIENTED_EDGE('',*,*,#29040,.T.) ;
#41090 = ORIENTED_EDGE('',*,*,#28998,.F.) ;
#41091 = ORIENTED_EDGE('',*,*,#29030,.F.) ;
#41092 = ORIENTED_EDGE('',*,*,#29027,.F.) ;
#41093 = ORIENTED_EDGE('',*,*,#29024,.F.) ;
#41094 = ORIENTED_EDGE('',*,*,#29022,.F.) ;
#41095 = ORIENTED_EDGE('',*,*,#29017,.F.) ;
#41096 = ORIENTED_EDGE('',*,*,#29015,.F.) ;
#41097 = ORIENTED_EDGE('',*,*,#29012,.F.) ;
#41098 = ORIENTED_EDGE('',*,*,#29010,.F.) ;
#41099 = ORIENTED_EDGE('',*,*,#29005,.F.) ;
#41100 = ORIENTED_EDGE('',*,*,#29002,.F.) ;
#41101 = ORIENTED_EDGE('',*,*,#29044,.T.) ;
#41102 = ORIENTED_EDGE('',*,*,#29045,.T.) ;
#41103 = ORIENTED_EDGE('',*,*,#29046,.T.) ;
#41104 = ORIENTED_EDGE('',*,*,#29047,.F.) ;
#41105 = ORIENTED_EDGE('',*,*,#29048,.T.) ;
#41106 = ORIENTED_EDGE('',*,*,#29049,.T.) ;
#41107 = ORIENTED_EDGE('',*,*,#29050,.T.) ;
#41108 = ORIENTED_EDGE('',*,*,#29045,.F.) ;
#41109 = ORIENTED_EDGE('',*,*,#29051,.T.) ;
#41110 = ORIENTED_EDGE('',*,*,#29052,.T.) ;
#41111 = ORIENTED_EDGE('',*,*,#29049,.F.) ;
#41112 = ORIENTED_EDGE('',*,*,#29053,.T.) ;
#41113 = ORIENTED_EDGE('',*,*,#29054,.T.) ;
#41114 = ORIENTED_EDGE('',*,*,#29051,.F.) ;
#41115 = ORIENTED_EDGE('',*,*,#29055,.T.) ;
#41116 = ORIENTED_EDGE('',*,*,#29056,.T.) ;
#41117 = ORIENTED_EDGE('',*,*,#29057,.T.) ;
#41118 = ORIENTED_EDGE('',*,*,#29058,.T.) ;
#41119 = ORIENTED_EDGE('',*,*,#29059,.T.) ;
#41120 = ORIENTED_EDGE('',*,*,#29056,.F.) ;
#41121 = ORIENTED_EDGE('',*,*,#29060,.T.) ;
#41122 = ORIENTED_EDGE('',*,*,#29061,.T.) ;
#41123 = ORIENTED_EDGE('',*,*,#29062,.T.) ;
#41124 = ORIENTED_EDGE('',*,*,#29058,.F.) ;
#41125 = ORIENTED_EDGE('',*,*,#29063,.T.) ;
#41126 = ORIENTED_EDGE('',*,*,#29064,.T.) ;
#41127 = ORIENTED_EDGE('',*,*,#29061,.F.) ;
#41128 = ORIENTED_EDGE('',*,*,#29065,.T.) ;
#41129 = ORIENTED_EDGE('',*,*,#29066,.T.) ;
#41130 = ORIENTED_EDGE('',*,*,#29063,.F.) ;
#41131 = ORIENTED_EDGE('',*,*,#29067,.T.) ;
#41132 = ORIENTED_EDGE('',*,*,#29068,.T.) ;
#41133 = ORIENTED_EDGE('',*,*,#29069,.T.) ;
#41134 = ORIENTED_EDGE('',*,*,#29068,.F.) ;
#41135 = ORIENTED_EDGE('',*,*,#29070,.T.) ;
#41136 = ORIENTED_EDGE('',*,*,#29071,.T.) ;
#41137 = ORIENTED_EDGE('',*,*,#29072,.T.) ;
#41138 = ORIENTED_EDGE('',*,*,#29071,.F.) ;
#41139 = ORIENTED_EDGE('',*,*,#29073,.T.) ;
#41140 = ORIENTED_EDGE('',*,*,#29074,.T.) ;
#41141 = ORIENTED_EDGE('',*,*,#29075,.T.) ;
#41142 = ORIENTED_EDGE('',*,*,#29074,.F.) ;
#41143 = ORIENTED_EDGE('',*,*,#29076,.T.) ;
#41144 = ORIENTED_EDGE('',*,*,#29047,.T.) ;
#41145 = ORIENTED_EDGE('',*,*,#29064,.F.) ;
#41146 = ORIENTED_EDGE('',*,*,#29077,.F.) ;
#41147 = ORIENTED_EDGE('',*,*,#29078,.F.) ;
#41148 = ORIENTED_EDGE('',*,*,#29079,.T.) ;
#41149 = ORIENTED_EDGE('',*,*,#29066,.F.) ;
#41150 = ORIENTED_EDGE('',*,*,#29080,.F.) ;
#41151 = ORIENTED_EDGE('',*,*,#29081,.F.) ;
#41152 = ORIENTED_EDGE('',*,*,#29077,.T.) ;
#41153 = ORIENTED_EDGE('',*,*,#29069,.F.) ;
#41154 = ORIENTED_EDGE('',*,*,#29082,.F.) ;
#41155 = ORIENTED_EDGE('',*,*,#29083,.F.) ;
#41156 = ORIENTED_EDGE('',*,*,#29080,.T.) ;
#41157 = ORIENTED_EDGE('',*,*,#29072,.F.) ;
#41158 = ORIENTED_EDGE('',*,*,#29084,.F.) ;
#41159 = ORIENTED_EDGE('',*,*,#29085,.F.) ;
#41160 = ORIENTED_EDGE('',*,*,#29082,.T.) ;
#41161 = ORIENTED_EDGE('',*,*,#29075,.F.) ;
#41162 = ORIENTED_EDGE('',*,*,#29086,.F.) ;
#41163 = ORIENTED_EDGE('',*,*,#29087,.F.) ;
#41164 = ORIENTED_EDGE('',*,*,#29084,.T.) ;
#41165 = ORIENTED_EDGE('',*,*,#29046,.F.) ;
#41166 = ORIENTED_EDGE('',*,*,#29088,.F.) ;
#41167 = ORIENTED_EDGE('',*,*,#29089,.F.) ;
#41168 = ORIENTED_EDGE('',*,*,#29086,.T.) ;
#41169 = ORIENTED_EDGE('',*,*,#29044,.F.) ;
#41170 = ORIENTED_EDGE('',*,*,#29076,.F.) ;
#41171 = ORIENTED_EDGE('',*,*,#29073,.F.) ;
#41172 = ORIENTED_EDGE('',*,*,#29070,.F.) ;
#41173 = ORIENTED_EDGE('',*,*,#29067,.F.) ;
#41174 = ORIENTED_EDGE('',*,*,#29065,.F.) ;
#41175 = ORIENTED_EDGE('',*,*,#29060,.F.) ;
#41176 = ORIENTED_EDGE('',*,*,#29057,.F.) ;
#41177 = ORIENTED_EDGE('',*,*,#29055,.F.) ;
#41178 = ORIENTED_EDGE('',*,*,#29053,.F.) ;
#41179 = ORIENTED_EDGE('',*,*,#29048,.F.) ;
#41180 = ORIENTED_EDGE('',*,*,#28612,.T.) ;
#41181 = ORIENTED_EDGE('',*,*,#29090,.T.) ;
#41182 = ORIENTED_EDGE('',*,*,#29091,.T.) ;
#41183 = ORIENTED_EDGE('',*,*,#29092,.F.) ;
#41184 = ORIENTED_EDGE('',*,*,#29093,.T.) ;
#41185 = ORIENTED_EDGE('',*,*,#29094,.T.) ;
#41186 = ORIENTED_EDGE('',*,*,#28613,.T.) ;
#41187 = ORIENTED_EDGE('',*,*,#29092,.T.) ;
#41188 = ORIENTED_EDGE('',*,*,#28618,.T.) ;
#41189 = ORIENTED_EDGE('',*,*,#29095,.T.) ;
#41190 = ORIENTED_EDGE('',*,*,#28873,.T.) ;
#41191 = ORIENTED_EDGE('',*,*,#29090,.F.) ;
#41192 = ORIENTED_EDGE('',*,*,#28617,.T.) ;
#41193 = ORIENTED_EDGE('',*,*,#29096,.T.) ;
#41194 = ORIENTED_EDGE('',*,*,#28871,.T.) ;
#41195 = ORIENTED_EDGE('',*,*,#29095,.F.) ;
#41196 = ORIENTED_EDGE('',*,*,#28616,.T.) ;
#41197 = ORIENTED_EDGE('',*,*,#29097,.T.) ;
#41198 = ORIENTED_EDGE('',*,*,#28869,.T.) ;
#41199 = ORIENTED_EDGE('',*,*,#29096,.F.) ;
#41200 = ORIENTED_EDGE('',*,*,#28866,.T.) ;
#41201 = ORIENTED_EDGE('',*,*,#29097,.F.) ;
#41202 = ORIENTED_EDGE('',*,*,#28615,.T.) ;
#41203 = ORIENTED_EDGE('',*,*,#29098,.T.) ;
#41204 = ORIENTED_EDGE('',*,*,#29099,.T.) ;
#41205 = ORIENTED_EDGE('',*,*,#29098,.F.) ;
#41206 = ORIENTED_EDGE('',*,*,#28614,.T.) ;
#41207 = ORIENTED_EDGE('',*,*,#29094,.F.) ;
#41208 = ORIENTED_EDGE('',*,*,#28854,.F.) ;
#41209 = ORIENTED_EDGE('',*,*,#28867,.F.) ;
#41210 = ORIENTED_EDGE('',*,*,#29099,.F.) ;
#41211 = ORIENTED_EDGE('',*,*,#29100,.T.) ;
#41212 = ORIENTED_EDGE('',*,*,#28853,.F.) ;
#41213 = ORIENTED_EDGE('',*,*,#29100,.F.) ;
#41214 = ORIENTED_EDGE('',*,*,#29093,.F.) ;
#41215 = ORIENTED_EDGE('',*,*,#29101,.T.) ;
#41216 = ORIENTED_EDGE('',*,*,#28850,.F.) ;
#41217 = ORIENTED_EDGE('',*,*,#29101,.F.) ;
#41218 = ORIENTED_EDGE('',*,*,#29091,.F.) ;
#41219 = ORIENTED_EDGE('',*,*,#28872,.T.) ;
#41220 = ORIENTED_EDGE('',*,*,#28622,.T.) ;
#41221 = ORIENTED_EDGE('',*,*,#29102,.T.) ;
#41222 = ORIENTED_EDGE('',*,*,#28899,.T.) ;
#41223 = ORIENTED_EDGE('',*,*,#29103,.F.) ;
#41224 = ORIENTED_EDGE('',*,*,#28621,.T.) ;
#41225 = ORIENTED_EDGE('',*,*,#29104,.T.) ;
#41226 = ORIENTED_EDGE('',*,*,#28896,.T.) ;
#41227 = ORIENTED_EDGE('',*,*,#29102,.F.) ;
#41228 = ORIENTED_EDGE('',*,*,#28619,.T.) ;
#41229 = ORIENTED_EDGE('',*,*,#29105,.T.) ;
#41230 = ORIENTED_EDGE('',*,*,#29106,.T.) ;
#41231 = ORIENTED_EDGE('',*,*,#29107,.T.) ;
#41232 = ORIENTED_EDGE('',*,*,#29108,.T.) ;
#41233 = ORIENTED_EDGE('',*,*,#29105,.F.) ;
#41234 = ORIENTED_EDGE('',*,*,#28625,.T.) ;
#41235 = ORIENTED_EDGE('',*,*,#29109,.T.) ;
#41236 = ORIENTED_EDGE('',*,*,#28620,.T.) ;
#41237 = ORIENTED_EDGE('',*,*,#29107,.F.) ;
#41238 = ORIENTED_EDGE('',*,*,#29110,.T.) ;
#41239 = ORIENTED_EDGE('',*,*,#29104,.F.) ;
#41240 = ORIENTED_EDGE('',*,*,#28903,.T.) ;
#41241 = ORIENTED_EDGE('',*,*,#29109,.F.) ;
#41242 = ORIENTED_EDGE('',*,*,#28624,.T.) ;
#41243 = ORIENTED_EDGE('',*,*,#29111,.T.) ;
#41244 = ORIENTED_EDGE('',*,*,#28901,.T.) ;
#41245 = ORIENTED_EDGE('',*,*,#29111,.F.) ;
#41246 = ORIENTED_EDGE('',*,*,#28623,.T.) ;
#41247 = ORIENTED_EDGE('',*,*,#29103,.T.) ;
#41248 = ORIENTED_EDGE('',*,*,#28884,.F.) ;
#41249 = ORIENTED_EDGE('',*,*,#28897,.F.) ;
#41250 = ORIENTED_EDGE('',*,*,#29110,.F.) ;
#41251 = ORIENTED_EDGE('',*,*,#29112,.T.) ;
#41252 = ORIENTED_EDGE('',*,*,#28883,.F.) ;
#41253 = ORIENTED_EDGE('',*,*,#29112,.F.) ;
#41254 = ORIENTED_EDGE('',*,*,#29106,.F.) ;
#41255 = ORIENTED_EDGE('',*,*,#29113,.T.) ;
#41256 = ORIENTED_EDGE('',*,*,#29114,.T.) ;
#41257 = ORIENTED_EDGE('',*,*,#29115,.T.) ;
#41258 = ORIENTED_EDGE('',*,*,#29116,.T.) ;
#41259 = ORIENTED_EDGE('',*,*,#29117,.F.) ;
#41260 = ORIENTED_EDGE('',*,*,#29118,.T.) ;
#41261 = ORIENTED_EDGE('',*,*,#29119,.T.) ;
#41262 = ORIENTED_EDGE('',*,*,#29120,.T.) ;
#41263 = ORIENTED_EDGE('',*,*,#29117,.T.) ;
#41264 = ORIENTED_EDGE('',*,*,#29121,.T.) ;
#41265 = ORIENTED_EDGE('',*,*,#29122,.T.) ;
#41266 = ORIENTED_EDGE('',*,*,#28933,.T.) ;
#41267 = ORIENTED_EDGE('',*,*,#29115,.F.) ;
#41268 = ORIENTED_EDGE('',*,*,#29123,.T.) ;
#41269 = ORIENTED_EDGE('',*,*,#29124,.T.) ;
#41270 = ORIENTED_EDGE('',*,*,#28931,.T.) ;
#41271 = ORIENTED_EDGE('',*,*,#29122,.F.) ;
#41272 = ORIENTED_EDGE('',*,*,#29125,.T.) ;
#41273 = ORIENTED_EDGE('',*,*,#29126,.T.) ;
#41274 = ORIENTED_EDGE('',*,*,#28929,.T.) ;
#41275 = ORIENTED_EDGE('',*,*,#29124,.F.) ;
#41276 = ORIENTED_EDGE('',*,*,#28926,.T.) ;
#41277 = ORIENTED_EDGE('',*,*,#29126,.F.) ;
#41278 = ORIENTED_EDGE('',*,*,#29127,.T.) ;
#41279 = ORIENTED_EDGE('',*,*,#29128,.T.) ;
#41280 = ORIENTED_EDGE('',*,*,#29129,.T.) ;
#41281 = ORIENTED_EDGE('',*,*,#29128,.F.) ;
#41282 = ORIENTED_EDGE('',*,*,#29130,.T.) ;
#41283 = ORIENTED_EDGE('',*,*,#29119,.F.) ;
#41284 = ORIENTED_EDGE('',*,*,#28914,.F.) ;
#41285 = ORIENTED_EDGE('',*,*,#28927,.F.) ;
#41286 = ORIENTED_EDGE('',*,*,#29129,.F.) ;
#41287 = ORIENTED_EDGE('',*,*,#29131,.T.) ;
#41288 = ORIENTED_EDGE('',*,*,#28913,.F.) ;
#41289 = ORIENTED_EDGE('',*,*,#29131,.F.) ;
#41290 = ORIENTED_EDGE('',*,*,#29118,.F.) ;
#41291 = ORIENTED_EDGE('',*,*,#29132,.T.) ;
#41292 = ORIENTED_EDGE('',*,*,#28910,.F.) ;
#41293 = ORIENTED_EDGE('',*,*,#29132,.F.) ;
#41294 = ORIENTED_EDGE('',*,*,#29116,.F.) ;
#41295 = ORIENTED_EDGE('',*,*,#28932,.T.) ;
#41296 = ORIENTED_EDGE('',*,*,#29133,.F.) ;
#41297 = ORIENTED_EDGE('',*,*,#29134,.F.) ;
#41298 = ORIENTED_EDGE('',*,*,#29135,.F.) ;
#41299 = ORIENTED_EDGE('',*,*,#29136,.F.) ;
#41300 = ORIENTED_EDGE('',*,*,#28718,.F.) ;
#41301 = ORIENTED_EDGE('',*,*,#29137,.F.) ;
#41302 = ORIENTED_EDGE('',*,*,#29138,.F.) ;
#41303 = ORIENTED_EDGE('',*,*,#29139,.F.) ;
#41304 = ORIENTED_EDGE('',*,*,#29140,.F.) ;
#41305 = ORIENTED_EDGE('',*,*,#27528,.F.) ;
#41306 = ORIENTED_EDGE('',*,*,#29141,.F.) ;
#41307 = ORIENTED_EDGE('',*,*,#29142,.F.) ;
#41308 = ORIENTED_EDGE('',*,*,#29143,.F.) ;
#41309 = ORIENTED_EDGE('',*,*,#29144,.F.) ;
#41310 = ORIENTED_EDGE('',*,*,#29145,.F.) ;
#41311 = ORIENTED_EDGE('',*,*,#29146,.F.) ;
#41312 = ORIENTED_EDGE('',*,*,#29147,.F.) ;
#41313 = ORIENTED_EDGE('',*,*,#29148,.F.) ;
#41314 = ORIENTED_EDGE('',*,*,#29149,.F.) ;
#41315 = ORIENTED_EDGE('',*,*,#29150,.F.) ;
#41316 = ORIENTED_EDGE('',*,*,#29151,.F.) ;
#41317 = ORIENTED_EDGE('',*,*,#29152,.F.) ;
#41318 = ORIENTED_EDGE('',*,*,#29153,.F.) ;
#41319 = ORIENTED_EDGE('',*,*,#29154,.F.) ;
#41320 = ORIENTED_EDGE('',*,*,#29114,.F.) ;
#41321 = ORIENTED_EDGE('',*,*,#29120,.F.) ;
#41322 = ORIENTED_EDGE('',*,*,#29130,.F.) ;
#41323 = ORIENTED_EDGE('',*,*,#29127,.F.) ;
#41324 = ORIENTED_EDGE('',*,*,#29125,.F.) ;
#41325 = ORIENTED_EDGE('',*,*,#29123,.F.) ;
#41326 = ORIENTED_EDGE('',*,*,#29121,.F.) ;
#41327 = ORIENTED_EDGE('',*,*,#29144,.T.) ;
#41328 = ORIENTED_EDGE('',*,*,#29155,.T.) ;
#41329 = ORIENTED_EDGE('',*,*,#28950,.T.) ;
#41330 = ORIENTED_EDGE('',*,*,#29156,.T.) ;
#41331 = ORIENTED_EDGE('',*,*,#29147,.T.) ;
#41332 = ORIENTED_EDGE('',*,*,#29157,.T.) ;
#41333 = ORIENTED_EDGE('',*,*,#28947,.T.) ;
#41334 = ORIENTED_EDGE('',*,*,#29155,.F.) ;
#41335 = ORIENTED_EDGE('',*,*,#29158,.T.) ;
#41336 = ORIENTED_EDGE('',*,*,#29157,.F.) ;
#41337 = ORIENTED_EDGE('',*,*,#29146,.T.) ;
#41338 = ORIENTED_EDGE('',*,*,#29159,.T.) ;
#41339 = ORIENTED_EDGE('',*,*,#29145,.T.) ;
#41340 = ORIENTED_EDGE('',*,*,#29156,.F.) ;
#41341 = ORIENTED_EDGE('',*,*,#29160,.T.) ;
#41342 = ORIENTED_EDGE('',*,*,#29159,.F.) ;
#41343 = ORIENTED_EDGE('',*,*,#28938,.F.) ;
#41344 = ORIENTED_EDGE('',*,*,#29161,.F.) ;
#41345 = ORIENTED_EDGE('',*,*,#29160,.F.) ;
#41346 = ORIENTED_EDGE('',*,*,#28949,.T.) ;
#41347 = ORIENTED_EDGE('',*,*,#29148,.T.) ;
#41348 = ORIENTED_EDGE('',*,*,#29162,.T.) ;
#41349 = ORIENTED_EDGE('',*,*,#29163,.T.) ;
#41350 = ORIENTED_EDGE('',*,*,#29164,.T.) ;
#41351 = ORIENTED_EDGE('',*,*,#29154,.T.) ;
#41352 = ORIENTED_EDGE('',*,*,#29165,.T.) ;
#41353 = ORIENTED_EDGE('',*,*,#29166,.T.) ;
#41354 = ORIENTED_EDGE('',*,*,#29162,.F.) ;
#41355 = ORIENTED_EDGE('',*,*,#29153,.T.) ;
#41356 = ORIENTED_EDGE('',*,*,#29167,.T.) ;
#41357 = ORIENTED_EDGE('',*,*,#28980,.T.) ;
#41358 = ORIENTED_EDGE('',*,*,#29165,.F.) ;
#41359 = ORIENTED_EDGE('',*,*,#29152,.T.) ;
#41360 = ORIENTED_EDGE('',*,*,#29168,.T.) ;
#41361 = ORIENTED_EDGE('',*,*,#28978,.T.) ;
#41362 = ORIENTED_EDGE('',*,*,#29167,.F.) ;
#41363 = ORIENTED_EDGE('',*,*,#28976,.T.) ;
#41364 = ORIENTED_EDGE('',*,*,#29168,.F.) ;
#41365 = ORIENTED_EDGE('',*,*,#29151,.T.) ;
#41366 = ORIENTED_EDGE('',*,*,#29169,.T.) ;
#41367 = ORIENTED_EDGE('',*,*,#28973,.T.) ;
#41368 = ORIENTED_EDGE('',*,*,#29169,.F.) ;
#41369 = ORIENTED_EDGE('',*,*,#29150,.T.) ;
#41370 = ORIENTED_EDGE('',*,*,#29170,.T.) ;
#41371 = ORIENTED_EDGE('',*,*,#29171,.T.) ;
#41372 = ORIENTED_EDGE('',*,*,#29170,.F.) ;
#41373 = ORIENTED_EDGE('',*,*,#29149,.T.) ;
#41374 = ORIENTED_EDGE('',*,*,#29164,.F.) ;
#41375 = ORIENTED_EDGE('',*,*,#28961,.F.) ;
#41376 = ORIENTED_EDGE('',*,*,#28974,.F.) ;
#41377 = ORIENTED_EDGE('',*,*,#29171,.F.) ;
#41378 = ORIENTED_EDGE('',*,*,#29172,.T.) ;
#41379 = ORIENTED_EDGE('',*,*,#28960,.F.) ;
#41380 = ORIENTED_EDGE('',*,*,#29172,.F.) ;
#41381 = ORIENTED_EDGE('',*,*,#29163,.F.) ;
#41382 = ORIENTED_EDGE('',*,*,#29173,.T.) ;
#41383 = ORIENTED_EDGE('',*,*,#28764,.T.) ;
#41384 = ORIENTED_EDGE('',*,*,#29174,.T.) ;
#41385 = ORIENTED_EDGE('',*,*,#28994,.T.) ;
#41386 = ORIENTED_EDGE('',*,*,#29175,.F.) ;
#41387 = ORIENTED_EDGE('',*,*,#28767,.T.) ;
#41388 = ORIENTED_EDGE('',*,*,#29176,.T.) ;
#41389 = ORIENTED_EDGE('',*,*,#29177,.T.) ;
#41390 = ORIENTED_EDGE('',*,*,#29174,.F.) ;
#41391 = ORIENTED_EDGE('',*,*,#28997,.T.) ;
#41392 = ORIENTED_EDGE('',*,*,#29178,.T.) ;
#41393 = ORIENTED_EDGE('',*,*,#28765,.T.) ;
#41394 = ORIENTED_EDGE('',*,*,#29175,.T.) ;
#41395 = ORIENTED_EDGE('',*,*,#28766,.T.) ;
#41396 = ORIENTED_EDGE('',*,*,#29178,.F.) ;
#41397 = ORIENTED_EDGE('',*,*,#29179,.T.) ;
#41398 = ORIENTED_EDGE('',*,*,#29176,.F.) ;
#41399 = ORIENTED_EDGE('',*,*,#29180,.T.) ;
#41400 = ORIENTED_EDGE('',*,*,#29181,.T.) ;
#41401 = ORIENTED_EDGE('',*,*,#28761,.T.) ;
#41402 = ORIENTED_EDGE('',*,*,#29182,.T.) ;
#41403 = ORIENTED_EDGE('',*,*,#28760,.T.) ;
#41404 = ORIENTED_EDGE('',*,*,#29183,.T.) ;
#41405 = ORIENTED_EDGE('',*,*,#29184,.T.) ;
#41406 = ORIENTED_EDGE('',*,*,#29182,.F.) ;
#41407 = ORIENTED_EDGE('',*,*,#28759,.T.) ;
#41408 = ORIENTED_EDGE('',*,*,#29185,.T.) ;
#41409 = ORIENTED_EDGE('',*,*,#29043,.T.) ;
#41410 = ORIENTED_EDGE('',*,*,#29183,.F.) ;
#41411 = ORIENTED_EDGE('',*,*,#28758,.T.) ;
#41412 = ORIENTED_EDGE('',*,*,#29186,.T.) ;
#41413 = ORIENTED_EDGE('',*,*,#29041,.T.) ;
#41414 = ORIENTED_EDGE('',*,*,#29185,.F.) ;
#41415 = ORIENTED_EDGE('',*,*,#28757,.T.) ;
#41416 = ORIENTED_EDGE('',*,*,#29187,.T.) ;
#41417 = ORIENTED_EDGE('',*,*,#29039,.T.) ;
#41418 = ORIENTED_EDGE('',*,*,#29186,.F.) ;
#41419 = ORIENTED_EDGE('',*,*,#29188,.T.) ;
#41420 = ORIENTED_EDGE('',*,*,#28754,.T.) ;
#41421 = ORIENTED_EDGE('',*,*,#29189,.T.) ;
#41422 = ORIENTED_EDGE('',*,*,#29032,.T.) ;
#41423 = ORIENTED_EDGE('',*,*,#29190,.T.) ;
#41424 = ORIENTED_EDGE('',*,*,#28755,.T.) ;
#41425 = ORIENTED_EDGE('',*,*,#29188,.F.) ;
#41426 = ORIENTED_EDGE('',*,*,#29035,.T.) ;
#41427 = ORIENTED_EDGE('',*,*,#28756,.T.) ;
#41428 = ORIENTED_EDGE('',*,*,#29190,.F.) ;
#41429 = ORIENTED_EDGE('',*,*,#29037,.T.) ;
#41430 = ORIENTED_EDGE('',*,*,#29187,.F.) ;
#41431 = ORIENTED_EDGE('',*,*,#29191,.T.) ;
#41432 = ORIENTED_EDGE('',*,*,#28762,.T.) ;
#41433 = ORIENTED_EDGE('',*,*,#29181,.F.) ;
#41434 = ORIENTED_EDGE('',*,*,#29192,.T.) ;
#41435 = ORIENTED_EDGE('',*,*,#29193,.T.) ;
#41436 = ORIENTED_EDGE('',*,*,#28763,.T.) ;
#41437 = ORIENTED_EDGE('',*,*,#29191,.F.) ;
#41438 = ORIENTED_EDGE('',*,*,#29194,.T.) ;
#41439 = ORIENTED_EDGE('',*,*,#29011,.F.) ;
#41440 = ORIENTED_EDGE('',*,*,#29195,.F.) ;
#41441 = ORIENTED_EDGE('',*,*,#29194,.F.) ;
#41442 = ORIENTED_EDGE('',*,*,#29196,.T.) ;
#41443 = ORIENTED_EDGE('',*,*,#29009,.F.) ;
#41444 = ORIENTED_EDGE('',*,*,#29196,.F.) ;
#41445 = ORIENTED_EDGE('',*,*,#29192,.F.) ;
#41446 = ORIENTED_EDGE('',*,*,#29197,.T.) ;
#41447 = ORIENTED_EDGE('',*,*,#29007,.F.) ;
#41448 = ORIENTED_EDGE('',*,*,#29197,.F.) ;
#41449 = ORIENTED_EDGE('',*,*,#29180,.F.) ;
#41450 = ORIENTED_EDGE('',*,*,#29198,.T.) ;
#41451 = ORIENTED_EDGE('',*,*,#29004,.F.) ;
#41452 = ORIENTED_EDGE('',*,*,#29198,.F.) ;
#41453 = ORIENTED_EDGE('',*,*,#29184,.F.) ;
#41454 = ORIENTED_EDGE('',*,*,#29042,.T.) ;
#41455 = ORIENTED_EDGE('',*,*,#28745,.T.) ;
#41456 = ORIENTED_EDGE('',*,*,#29199,.T.) ;
#41457 = ORIENTED_EDGE('',*,*,#29200,.T.) ;
#41458 = ORIENTED_EDGE('',*,*,#29201,.T.) ;
#41459 = ORIENTED_EDGE('',*,*,#29202,.T.) ;
#41460 = ORIENTED_EDGE('',*,*,#29203,.T.) ;
#41461 = ORIENTED_EDGE('',*,*,#28742,.T.) ;
#41462 = ORIENTED_EDGE('',*,*,#29204,.T.) ;
#41463 = ORIENTED_EDGE('',*,*,#28752,.T.) ;
#41464 = ORIENTED_EDGE('',*,*,#29205,.T.) ;
#41465 = ORIENTED_EDGE('',*,*,#29089,.T.) ;
#41466 = ORIENTED_EDGE('',*,*,#29204,.F.) ;
#41467 = ORIENTED_EDGE('',*,*,#28751,.T.) ;
#41468 = ORIENTED_EDGE('',*,*,#29206,.T.) ;
#41469 = ORIENTED_EDGE('',*,*,#29087,.T.) ;
#41470 = ORIENTED_EDGE('',*,*,#29205,.F.) ;
#41471 = ORIENTED_EDGE('',*,*,#29085,.T.) ;
#41472 = ORIENTED_EDGE('',*,*,#29206,.F.) ;
#41473 = ORIENTED_EDGE('',*,*,#28750,.T.) ;
#41474 = ORIENTED_EDGE('',*,*,#29207,.T.) ;
#41475 = ORIENTED_EDGE('',*,*,#29083,.T.) ;
#41476 = ORIENTED_EDGE('',*,*,#29207,.F.) ;
#41477 = ORIENTED_EDGE('',*,*,#28749,.T.) ;
#41478 = ORIENTED_EDGE('',*,*,#29208,.T.) ;
#41479 = ORIENTED_EDGE('',*,*,#29209,.T.) ;
#41480 = ORIENTED_EDGE('',*,*,#28743,.T.) ;
#41481 = ORIENTED_EDGE('',*,*,#29203,.F.) ;
#41482 = ORIENTED_EDGE('',*,*,#29210,.T.) ;
#41483 = ORIENTED_EDGE('',*,*,#28744,.T.) ;
#41484 = ORIENTED_EDGE('',*,*,#29209,.F.) ;
#41485 = ORIENTED_EDGE('',*,*,#29211,.T.) ;
#41486 = ORIENTED_EDGE('',*,*,#29199,.F.) ;
#41487 = ORIENTED_EDGE('',*,*,#29212,.T.) ;
#41488 = ORIENTED_EDGE('',*,*,#29213,.T.) ;
#41489 = ORIENTED_EDGE('',*,*,#28746,.T.) ;
#41490 = ORIENTED_EDGE('',*,*,#29201,.F.) ;
#41491 = ORIENTED_EDGE('',*,*,#29214,.T.) ;
#41492 = ORIENTED_EDGE('',*,*,#28747,.T.) ;
#41493 = ORIENTED_EDGE('',*,*,#29213,.F.) ;
#41494 = ORIENTED_EDGE('',*,*,#29078,.T.) ;
#41495 = ORIENTED_EDGE('',*,*,#28748,.T.) ;
#41496 = ORIENTED_EDGE('',*,*,#29214,.F.) ;
#41497 = ORIENTED_EDGE('',*,*,#29081,.T.) ;
#41498 = ORIENTED_EDGE('',*,*,#29208,.F.) ;
#41499 = ORIENTED_EDGE('',*,*,#29062,.F.) ;
#41500 = ORIENTED_EDGE('',*,*,#29079,.F.) ;
#41501 = ORIENTED_EDGE('',*,*,#29212,.F.) ;
#41502 = ORIENTED_EDGE('',*,*,#29215,.T.) ;
#41503 = ORIENTED_EDGE('',*,*,#29059,.F.) ;
#41504 = ORIENTED_EDGE('',*,*,#29215,.F.) ;
#41505 = ORIENTED_EDGE('',*,*,#29200,.F.) ;
#41506 = ORIENTED_EDGE('',*,*,#29216,.T.) ;
#41507 = ORIENTED_EDGE('',*,*,#29054,.F.) ;
#41508 = ORIENTED_EDGE('',*,*,#29216,.F.) ;
#41509 = ORIENTED_EDGE('',*,*,#29211,.F.) ;
#41510 = ORIENTED_EDGE('',*,*,#29217,.T.) ;
#41511 = ORIENTED_EDGE('',*,*,#29052,.F.) ;
#41512 = ORIENTED_EDGE('',*,*,#29217,.F.) ;
#41513 = ORIENTED_EDGE('',*,*,#29210,.F.) ;
#41514 = ORIENTED_EDGE('',*,*,#29218,.T.) ;
#41515 = ORIENTED_EDGE('',*,*,#29050,.F.) ;
#41516 = ORIENTED_EDGE('',*,*,#29218,.F.) ;
#41517 = ORIENTED_EDGE('',*,*,#29202,.F.) ;
#41518 = ORIENTED_EDGE('',*,*,#29088,.T.) ;
#41519 = ORIENTED_EDGE('',*,*,#29014,.F.) ;
#41520 = ORIENTED_EDGE('',*,*,#29033,.F.) ;
#41521 = ORIENTED_EDGE('',*,*,#29189,.F.) ;
#41522 = ORIENTED_EDGE('',*,*,#28753,.F.) ;
#41523 = ORIENTED_EDGE('',*,*,#29193,.F.) ;
#41524 = ORIENTED_EDGE('',*,*,#29195,.T.) ;
#41525 = ORIENTED_EDGE('',*,*,#28988,.F.) ;
#41526 = ORIENTED_EDGE('',*,*,#28995,.F.) ;
#41527 = ORIENTED_EDGE('',*,*,#29177,.F.) ;
#41528 = ORIENTED_EDGE('',*,*,#29219,.T.) ;
#41529 = ORIENTED_EDGE('',*,*,#28985,.F.) ;
#41530 = ORIENTED_EDGE('',*,*,#29219,.F.) ;
#41531 = ORIENTED_EDGE('',*,*,#29179,.F.) ;
#41532 = ORIENTED_EDGE('',*,*,#28996,.T.) ;
#41533 = ORIENTED_EDGE('',*,*,#28941,.F.) ;
#41534 = ORIENTED_EDGE('',*,*,#28948,.F.) ;
#41535 = ORIENTED_EDGE('',*,*,#29158,.F.) ;
#41536 = ORIENTED_EDGE('',*,*,#29161,.T.) ;
#41537 = ORIENTED_EDGE('',*,*,#28880,.F.) ;
#41538 = ORIENTED_EDGE('',*,*,#29113,.F.) ;
#41539 = ORIENTED_EDGE('',*,*,#29108,.F.) ;
#41540 = ORIENTED_EDGE('',*,*,#28902,.T.) ;
#41541 = ORIENTED_EDGE('',*,*,#28957,.F.) ;
#41542 = ORIENTED_EDGE('',*,*,#29173,.F.) ;
#41543 = ORIENTED_EDGE('',*,*,#29166,.F.) ;
#41544 = ORIENTED_EDGE('',*,*,#28979,.T.) ;
#41545 = ORIENTED_EDGE('',*,*,#28042,.F.) ;
#41546 = ORIENTED_EDGE('',*,*,#28245,.F.) ;
#41547 = ORIENTED_EDGE('',*,*,#29220,.T.) ;
#41548 = ORIENTED_EDGE('',*,*,#29221,.T.) ;
#41549 = ORIENTED_EDGE('',*,*,#28037,.F.) ;
#41550 = ORIENTED_EDGE('',*,*,#28522,.F.) ;
#41551 = ORIENTED_EDGE('',*,*,#29222,.F.) ;
#41552 = ORIENTED_EDGE('',*,*,#29223,.F.) ;
#41553 = ORIENTED_EDGE('',*,*,#29224,.F.) ;
#41554 = ORIENTED_EDGE('',*,*,#29225,.F.) ;
#41555 = ORIENTED_EDGE('',*,*,#29226,.F.) ;
#41556 = ORIENTED_EDGE('',*,*,#29227,.F.) ;
#41557 = ORIENTED_EDGE('',*,*,#28510,.F.) ;
#41558 = ORIENTED_EDGE('',*,*,#28516,.F.) ;
#41559 = ORIENTED_EDGE('',*,*,#28518,.F.) ;
#41560 = ORIENTED_EDGE('',*,*,#28520,.F.) ;
#41561 = ORIENTED_EDGE('',*,*,#28637,.F.) ;
#41562 = ORIENTED_EDGE('',*,*,#28641,.T.) ;
#41563 = ORIENTED_EDGE('',*,*,#29228,.T.) ;
#41564 = ORIENTED_EDGE('',*,*,#28101,.F.) ;
#41565 = ORIENTED_EDGE('',*,*,#28632,.F.) ;
#41566 = ORIENTED_EDGE('',*,*,#28113,.F.) ;
#41567 = ORIENTED_EDGE('',*,*,#29229,.F.) ;
#41568 = ORIENTED_EDGE('',*,*,#29230,.F.) ;
#41569 = ORIENTED_EDGE('',*,*,#28816,.T.) ;
#41570 = ORIENTED_EDGE('',*,*,#28112,.F.) ;
#41571 = ORIENTED_EDGE('',*,*,#29231,.F.) ;
#41572 = ORIENTED_EDGE('',*,*,#29232,.T.) ;
#41573 = ORIENTED_EDGE('',*,*,#29229,.T.) ;
#41574 = ORIENTED_EDGE('',*,*,#28111,.F.) ;
#41575 = ORIENTED_EDGE('',*,*,#29233,.F.) ;
#41576 = ORIENTED_EDGE('',*,*,#29234,.T.) ;
#41577 = ORIENTED_EDGE('',*,*,#29231,.T.) ;
#41578 = ORIENTED_EDGE('',*,*,#28110,.F.) ;
#41579 = ORIENTED_EDGE('',*,*,#29235,.F.) ;
#41580 = ORIENTED_EDGE('',*,*,#29236,.T.) ;
#41581 = ORIENTED_EDGE('',*,*,#29233,.T.) ;
#41582 = ORIENTED_EDGE('',*,*,#28109,.F.) ;
#41583 = ORIENTED_EDGE('',*,*,#29237,.F.) ;
#41584 = ORIENTED_EDGE('',*,*,#29238,.T.) ;
#41585 = ORIENTED_EDGE('',*,*,#29235,.T.) ;
#41586 = ORIENTED_EDGE('',*,*,#28108,.F.) ;
#41587 = ORIENTED_EDGE('',*,*,#29239,.F.) ;
#41588 = ORIENTED_EDGE('',*,*,#29240,.F.) ;
#41589 = ORIENTED_EDGE('',*,*,#29237,.T.) ;
#41590 = ORIENTED_EDGE('',*,*,#28800,.T.) ;
#41591 = ORIENTED_EDGE('',*,*,#28817,.F.) ;
#41592 = ORIENTED_EDGE('',*,*,#29230,.T.) ;
#41593 = ORIENTED_EDGE('',*,*,#29232,.F.) ;
#41594 = ORIENTED_EDGE('',*,*,#29234,.F.) ;
#41595 = ORIENTED_EDGE('',*,*,#29236,.F.) ;
#41596 = ORIENTED_EDGE('',*,*,#29238,.F.) ;
#41597 = ORIENTED_EDGE('',*,*,#29240,.T.) ;
#41598 = ORIENTED_EDGE('',*,*,#29241,.F.) ;
#41599 = ORIENTED_EDGE('',*,*,#29242,.F.) ;
#41600 = ORIENTED_EDGE('',*,*,#27847,.F.) ;
#41601 = ORIENTED_EDGE('',*,*,#27968,.T.) ;
#41602 = ORIENTED_EDGE('',*,*,#27970,.F.) ;
#41603 = ORIENTED_EDGE('',*,*,#27972,.F.) ;
#41604 = ORIENTED_EDGE('',*,*,#27976,.F.) ;
#41605 = ORIENTED_EDGE('',*,*,#28832,.T.) ;
#41606 = ORIENTED_EDGE('',*,*,#28811,.T.) ;
#41607 = ORIENTED_EDGE('',*,*,#29243,.T.) ;
#41608 = ORIENTED_EDGE('',*,*,#29244,.F.) ;
#41609 = ORIENTED_EDGE('',*,*,#27848,.F.) ;
#41610 = ORIENTED_EDGE('',*,*,#29242,.T.) ;
#41611 = ORIENTED_EDGE('',*,*,#29245,.T.) ;
#41612 = ORIENTED_EDGE('',*,*,#29246,.F.) ;
#41613 = ORIENTED_EDGE('',*,*,#29243,.F.) ;
#41614 = ORIENTED_EDGE('',*,*,#29241,.T.) ;
#41615 = ORIENTED_EDGE('',*,*,#29239,.T.) ;
#41616 = ORIENTED_EDGE('',*,*,#28103,.F.) ;
#41617 = ORIENTED_EDGE('',*,*,#29247,.F.) ;
#41618 = ORIENTED_EDGE('',*,*,#28639,.F.) ;
#41619 = ORIENTED_EDGE('',*,*,#28643,.T.) ;
#41620 = ORIENTED_EDGE('',*,*,#28102,.F.) ;
#41621 = ORIENTED_EDGE('',*,*,#29228,.F.) ;
#41622 = ORIENTED_EDGE('',*,*,#28640,.T.) ;
#41623 = ORIENTED_EDGE('',*,*,#29247,.T.) ;
#41624 = ORIENTED_EDGE('',*,*,#28592,.F.) ;
#41625 = ORIENTED_EDGE('',*,*,#29248,.T.) ;
#41626 = ORIENTED_EDGE('',*,*,#29249,.F.) ;
#41627 = ORIENTED_EDGE('',*,*,#29250,.F.) ;
#41628 = ORIENTED_EDGE('',*,*,#28642,.F.) ;
#41629 = ORIENTED_EDGE('',*,*,#28736,.F.) ;
#41630 = ORIENTED_EDGE('',*,*,#28795,.T.) ;
#41631 = ORIENTED_EDGE('',*,*,#29251,.T.) ;
#41632 = ORIENTED_EDGE('',*,*,#29252,.F.) ;
#41633 = ORIENTED_EDGE('',*,*,#28737,.F.) ;
#41634 = ORIENTED_EDGE('',*,*,#29252,.T.) ;
#41635 = ORIENTED_EDGE('',*,*,#29253,.T.) ;
#41636 = ORIENTED_EDGE('',*,*,#29254,.F.) ;
#41637 = ORIENTED_EDGE('',*,*,#28738,.F.) ;
#41638 = ORIENTED_EDGE('',*,*,#29254,.T.) ;
#41639 = ORIENTED_EDGE('',*,*,#29255,.T.) ;
#41640 = ORIENTED_EDGE('',*,*,#28793,.F.) ;
#41641 = ORIENTED_EDGE('',*,*,#29251,.F.) ;
#41642 = ORIENTED_EDGE('',*,*,#28794,.F.) ;
#41643 = ORIENTED_EDGE('',*,*,#29255,.F.) ;
#41644 = ORIENTED_EDGE('',*,*,#29253,.F.) ;
#41645 = ORIENTED_EDGE('',*,*,#29256,.F.) ;
#41646 = ORIENTED_EDGE('',*,*,#29257,.T.) ;
#41647 = ORIENTED_EDGE('',*,*,#29258,.F.) ;
#41648 = ORIENTED_EDGE('',*,*,#29259,.F.) ;
#41649 = ORIENTED_EDGE('',*,*,#28573,.F.) ;
#41650 = ORIENTED_EDGE('',*,*,#29260,.T.) ;
#41651 = ORIENTED_EDGE('',*,*,#29261,.F.) ;
#41652 = ORIENTED_EDGE('',*,*,#29262,.F.) ;
#41653 = ORIENTED_EDGE('',*,*,#28574,.F.) ;
#41654 = ORIENTED_EDGE('',*,*,#29262,.T.) ;
#41655 = ORIENTED_EDGE('',*,*,#29263,.F.) ;
#41656 = ORIENTED_EDGE('',*,*,#29257,.F.) ;
#41657 = ORIENTED_EDGE('',*,*,#28503,.F.) ;
#41658 = ORIENTED_EDGE('',*,*,#28570,.F.) ;
#41659 = ORIENTED_EDGE('',*,*,#27850,.F.) ;
#41660 = ORIENTED_EDGE('',*,*,#29259,.T.) ;
#41661 = ORIENTED_EDGE('',*,*,#29264,.F.) ;
#41662 = ORIENTED_EDGE('',*,*,#29260,.F.) ;
#41663 = ORIENTED_EDGE('',*,*,#29264,.T.) ;
#41664 = ORIENTED_EDGE('',*,*,#29258,.T.) ;
#41665 = ORIENTED_EDGE('',*,*,#29263,.T.) ;
#41666 = ORIENTED_EDGE('',*,*,#29261,.T.) ;
#41667 = ORIENTED_EDGE('',*,*,#28677,.F.) ;
#41668 = ORIENTED_EDGE('',*,*,#27949,.F.) ;
#41669 = ORIENTED_EDGE('',*,*,#28785,.T.) ;
#41670 = ORIENTED_EDGE('',*,*,#29265,.T.) ;
#41671 = ORIENTED_EDGE('',*,*,#29266,.F.) ;
#41672 = ORIENTED_EDGE('',*,*,#28542,.F.) ;
#41673 = ORIENTED_EDGE('',*,*,#28791,.F.) ;
#41674 = ORIENTED_EDGE('',*,*,#28797,.T.) ;
#41675 = ORIENTED_EDGE('',*,*,#28798,.F.) ;
#41676 = ORIENTED_EDGE('',*,*,#28534,.F.) ;
#41677 = ORIENTED_EDGE('',*,*,#28536,.F.) ;
#41678 = ORIENTED_EDGE('',*,*,#28538,.F.) ;
#41679 = ORIENTED_EDGE('',*,*,#28540,.F.) ;
#41680 = ORIENTED_EDGE('',*,*,#28788,.F.) ;
#41681 = ORIENTED_EDGE('',*,*,#27659,.T.) ;
#41682 = ORIENTED_EDGE('',*,*,#27664,.F.) ;
#41683 = ORIENTED_EDGE('',*,*,#27666,.T.) ;
#41684 = ORIENTED_EDGE('',*,*,#28700,.F.) ;
#41685 = ORIENTED_EDGE('',*,*,#29267,.F.) ;
#41686 = ORIENTED_EDGE('',*,*,#27806,.F.) ;
#41687 = ORIENTED_EDGE('',*,*,#27687,.T.) ;
#41688 = ORIENTED_EDGE('',*,*,#27690,.F.) ;
#41689 = ORIENTED_EDGE('',*,*,#27692,.T.) ;
#41690 = ORIENTED_EDGE('',*,*,#28663,.T.) ;
#41691 = ORIENTED_EDGE('',*,*,#28799,.T.) ;
#41692 = ORIENTED_EDGE('',*,*,#28678,.F.) ;
#41693 = ORIENTED_EDGE('',*,*,#29266,.T.) ;
#41694 = ORIENTED_EDGE('',*,*,#29268,.T.) ;
#41695 = ORIENTED_EDGE('',*,*,#27808,.F.) ;
#41696 = ORIENTED_EDGE('',*,*,#29269,.F.) ;
#41697 = ORIENTED_EDGE('',*,*,#28786,.T.) ;
#41698 = ORIENTED_EDGE('',*,*,#27661,.T.) ;
#41699 = ORIENTED_EDGE('',*,*,#28789,.T.) ;
#41700 = ORIENTED_EDGE('',*,*,#28698,.F.) ;
#41701 = ORIENTED_EDGE('',*,*,#28702,.T.) ;
#41702 = ORIENTED_EDGE('',*,*,#28703,.T.) ;
#41703 = ORIENTED_EDGE('',*,*,#28668,.T.) ;
#41704 = ORIENTED_EDGE('',*,*,#29270,.T.) ;
#41705 = ORIENTED_EDGE('',*,*,#29265,.F.) ;
#41706 = ORIENTED_EDGE('',*,*,#28784,.T.) ;
#41707 = ORIENTED_EDGE('',*,*,#28777,.F.) ;
#41708 = ORIENTED_EDGE('',*,*,#27809,.T.) ;
#41709 = ORIENTED_EDGE('',*,*,#29268,.F.) ;
#41710 = ORIENTED_EDGE('',*,*,#28387,.F.) ;
#41711 = ORIENTED_EDGE('',*,*,#29271,.T.) ;
#41712 = ORIENTED_EDGE('',*,*,#29272,.T.) ;
#41713 = ORIENTED_EDGE('',*,*,#28433,.T.) ;
#41714 = ORIENTED_EDGE('',*,*,#28380,.F.) ;
#41715 = ORIENTED_EDGE('',*,*,#29273,.T.) ;
#41716 = ORIENTED_EDGE('',*,*,#29271,.F.) ;
#41717 = ORIENTED_EDGE('',*,*,#28384,.F.) ;
#41718 = ORIENTED_EDGE('',*,*,#28405,.F.) ;
#41719 = ORIENTED_EDGE('',*,*,#28437,.T.) ;
#41720 = ORIENTED_EDGE('',*,*,#28441,.T.) ;
#41721 = ORIENTED_EDGE('',*,*,#29274,.T.) ;
#41722 = ORIENTED_EDGE('',*,*,#29267,.T.) ;
#41723 = ORIENTED_EDGE('',*,*,#28787,.F.) ;
#41724 = ORIENTED_EDGE('',*,*,#29269,.T.) ;
#41725 = ORIENTED_EDGE('',*,*,#27807,.F.) ;
#41726 = ORIENTED_EDGE('',*,*,#28019,.F.) ;
#41727 = ORIENTED_EDGE('',*,*,#28024,.F.) ;
#41728 = ORIENTED_EDGE('',*,*,#28827,.F.) ;
#41729 = ORIENTED_EDGE('',*,*,#29275,.T.) ;
#41730 = ORIENTED_EDGE('',*,*,#28021,.F.) ;
#41731 = ORIENTED_EDGE('',*,*,#29275,.F.) ;
#41732 = ORIENTED_EDGE('',*,*,#28826,.F.) ;
#41733 = ORIENTED_EDGE('',*,*,#28025,.F.) ;
#41734 = ORIENTED_EDGE('',*,*,#28664,.F.) ;
#41735 = ORIENTED_EDGE('',*,*,#29270,.F.) ;
#41736 = ORIENTED_EDGE('',*,*,#28670,.F.) ;
#41737 = ORIENTED_EDGE('',*,*,#28667,.F.) ;
#41738 = ORIENTED_EDGE('',*,*,#28000,.F.) ;
#41739 = ORIENTED_EDGE('',*,*,#28704,.T.) ;
#41740 = ORIENTED_EDGE('',*,*,#28692,.F.) ;
#41741 = ORIENTED_EDGE('',*,*,#29226,.T.) ;
#41742 = ORIENTED_EDGE('',*,*,#29276,.T.) ;
#41743 = ORIENTED_EDGE('',*,*,#29277,.T.) ;
#41744 = ORIENTED_EDGE('',*,*,#29278,.T.) ;
#41745 = ORIENTED_EDGE('',*,*,#29279,.F.) ;
#41746 = ORIENTED_EDGE('',*,*,#29280,.F.) ;
#41747 = ORIENTED_EDGE('',*,*,#29281,.F.) ;
#41748 = ORIENTED_EDGE('',*,*,#29225,.T.) ;
#41749 = ORIENTED_EDGE('',*,*,#29282,.T.) ;
#41750 = ORIENTED_EDGE('',*,*,#29283,.T.) ;
#41751 = ORIENTED_EDGE('',*,*,#29276,.F.) ;
#41752 = ORIENTED_EDGE('',*,*,#27513,.T.) ;
#41753 = ORIENTED_EDGE('',*,*,#29284,.F.) ;
#41754 = ORIENTED_EDGE('',*,*,#29141,.T.) ;
#41755 = ORIENTED_EDGE('',*,*,#27527,.F.) ;
#41756 = ORIENTED_EDGE('',*,*,#29284,.T.) ;
#41757 = ORIENTED_EDGE('',*,*,#27516,.T.) ;
#41758 = ORIENTED_EDGE('',*,*,#29285,.T.) ;
#41759 = ORIENTED_EDGE('',*,*,#29280,.T.) ;
#41760 = ORIENTED_EDGE('',*,*,#29142,.T.) ;
#41761 = ORIENTED_EDGE('',*,*,#29286,.T.) ;
#41762 = ORIENTED_EDGE('',*,*,#29287,.F.) ;
#41763 = ORIENTED_EDGE('',*,*,#29288,.F.) ;
#41764 = ORIENTED_EDGE('',*,*,#29289,.F.) ;
#41765 = ORIENTED_EDGE('',*,*,#29290,.T.) ;
#41766 = ORIENTED_EDGE('',*,*,#29223,.T.) ;
#41767 = ORIENTED_EDGE('',*,*,#29287,.T.) ;
#41768 = ORIENTED_EDGE('',*,*,#29291,.T.) ;
#41769 = ORIENTED_EDGE('',*,*,#29224,.T.) ;
#41770 = ORIENTED_EDGE('',*,*,#29290,.F.) ;
#41771 = ORIENTED_EDGE('',*,*,#29292,.T.) ;
#41772 = ORIENTED_EDGE('',*,*,#29282,.F.) ;
#41773 = ORIENTED_EDGE('',*,*,#28524,.F.) ;
#41774 = ORIENTED_EDGE('',*,*,#28771,.T.) ;
#41775 = ORIENTED_EDGE('',*,*,#29288,.T.) ;
#41776 = ORIENTED_EDGE('',*,*,#29222,.T.) ;
#41777 = ORIENTED_EDGE('',*,*,#29293,.F.) ;
#41778 = ORIENTED_EDGE('',*,*,#28627,.F.) ;
#41779 = ORIENTED_EDGE('',*,*,#29294,.F.) ;
#41780 = ORIENTED_EDGE('',*,*,#29295,.T.) ;
#41781 = ORIENTED_EDGE('',*,*,#29296,.T.) ;
#41782 = ORIENTED_EDGE('',*,*,#29294,.T.) ;
#41783 = ORIENTED_EDGE('',*,*,#28630,.T.) ;
#41784 = ORIENTED_EDGE('',*,*,#28634,.T.) ;
#41785 = ORIENTED_EDGE('',*,*,#29297,.T.) ;
#41786 = ORIENTED_EDGE('',*,*,#29295,.F.) ;
#41787 = ORIENTED_EDGE('',*,*,#28629,.T.) ;
#41788 = ORIENTED_EDGE('',*,*,#29298,.T.) ;
#41789 = ORIENTED_EDGE('',*,*,#29299,.T.) ;
#41790 = ORIENTED_EDGE('',*,*,#29139,.T.) ;
#41791 = ORIENTED_EDGE('',*,*,#29300,.T.) ;
#41792 = ORIENTED_EDGE('',*,*,#28719,.F.) ;
#41793 = ORIENTED_EDGE('',*,*,#29301,.F.) ;
#41794 = ORIENTED_EDGE('',*,*,#29302,.T.) ;
#41795 = ORIENTED_EDGE('',*,*,#29303,.F.) ;
#41796 = ORIENTED_EDGE('',*,*,#29304,.T.) ;
#41797 = ORIENTED_EDGE('',*,*,#29305,.T.) ;
#41798 = ORIENTED_EDGE('',*,*,#29135,.T.) ;
#41799 = ORIENTED_EDGE('',*,*,#29306,.T.) ;
#41800 = ORIENTED_EDGE('',*,*,#29301,.T.) ;
#41801 = ORIENTED_EDGE('',*,*,#29136,.T.) ;
#41802 = ORIENTED_EDGE('',*,*,#29305,.F.) ;
#41803 = ORIENTED_EDGE('',*,*,#29307,.T.) ;
#41804 = ORIENTED_EDGE('',*,*,#29289,.T.) ;
#41805 = ORIENTED_EDGE('',*,*,#28770,.T.) ;
#41806 = ORIENTED_EDGE('',*,*,#29303,.T.) ;
#41807 = ORIENTED_EDGE('',*,*,#29308,.T.) ;
#41808 = ORIENTED_EDGE('',*,*,#29309,.T.) ;
#41809 = ORIENTED_EDGE('',*,*,#29310,.F.) ;
#41810 = ORIENTED_EDGE('',*,*,#28717,.F.) ;
#41811 = ORIENTED_EDGE('',*,*,#29311,.F.) ;
#41812 = ORIENTED_EDGE('',*,*,#29312,.T.) ;
#41813 = ORIENTED_EDGE('',*,*,#29137,.T.) ;
#41814 = ORIENTED_EDGE('',*,*,#29310,.T.) ;
#41815 = ORIENTED_EDGE('',*,*,#29313,.T.) ;
#41816 = ORIENTED_EDGE('',*,*,#29138,.T.) ;
#41817 = ORIENTED_EDGE('',*,*,#29312,.F.) ;
#41818 = ORIENTED_EDGE('',*,*,#29314,.T.) ;
#41819 = ORIENTED_EDGE('',*,*,#29300,.F.) ;
#41820 = ORIENTED_EDGE('',*,*,#28421,.F.) ;
#41821 = ORIENTED_EDGE('',*,*,#29315,.F.) ;
#41822 = ORIENTED_EDGE('',*,*,#29316,.T.) ;
#41823 = ORIENTED_EDGE('',*,*,#29317,.F.) ;
#41824 = ORIENTED_EDGE('',*,*,#29318,.T.) ;
#41825 = ORIENTED_EDGE('',*,*,#29319,.T.) ;
#41826 = ORIENTED_EDGE('',*,*,#28610,.T.) ;
#41827 = ORIENTED_EDGE('',*,*,#29320,.T.) ;
#41828 = ORIENTED_EDGE('',*,*,#29315,.T.) ;
#41829 = ORIENTED_EDGE('',*,*,#28611,.T.) ;
#41830 = ORIENTED_EDGE('',*,*,#29319,.F.) ;
#41831 = ORIENTED_EDGE('',*,*,#29321,.T.) ;
#41832 = ORIENTED_EDGE('',*,*,#29311,.T.) ;
#41833 = ORIENTED_EDGE('',*,*,#27710,.T.) ;
#41834 = ORIENTED_EDGE('',*,*,#29317,.T.) ;
#41835 = ORIENTED_EDGE('',*,*,#29322,.T.) ;
#41836 = ORIENTED_EDGE('',*,*,#29323,.T.) ;
#41837 = ORIENTED_EDGE('',*,*,#29324,.T.) ;
#41838 = ORIENTED_EDGE('',*,*,#29325,.T.) ;
#41839 = ORIENTED_EDGE('',*,*,#28608,.T.) ;
#41840 = ORIENTED_EDGE('',*,*,#28609,.T.) ;
#41841 = ORIENTED_EDGE('',*,*,#29325,.F.) ;
#41842 = ORIENTED_EDGE('',*,*,#29326,.T.) ;
#41843 = ORIENTED_EDGE('',*,*,#29320,.F.) ;
#41844 = ORIENTED_EDGE('',*,*,#29293,.T.) ;
#41845 = ORIENTED_EDGE('',*,*,#29327,.T.) ;
#41846 = ORIENTED_EDGE('',*,*,#29323,.F.) ;
#41847 = ORIENTED_EDGE('',*,*,#28607,.T.) ;
#41848 = ORIENTED_EDGE('',*,*,#27525,.T.) ;
#41849 = ORIENTED_EDGE('',*,*,#27529,.T.) ;
#41850 = ORIENTED_EDGE('',*,*,#29140,.T.) ;
#41851 = ORIENTED_EDGE('',*,*,#29299,.F.) ;
#41852 = ORIENTED_EDGE('',*,*,#29328,.T.) ;
#41853 = ORIENTED_EDGE('',*,*,#29329,.T.) ;
#41854 = ORIENTED_EDGE('',*,*,#29330,.T.) ;
#41855 = ORIENTED_EDGE('',*,*,#29331,.T.) ;
#41856 = ORIENTED_EDGE('',*,*,#29133,.T.) ;
#41857 = ORIENTED_EDGE('',*,*,#29134,.T.) ;
#41858 = ORIENTED_EDGE('',*,*,#29331,.F.) ;
#41859 = ORIENTED_EDGE('',*,*,#29332,.T.) ;
#41860 = ORIENTED_EDGE('',*,*,#29306,.F.) ;
#41861 = ORIENTED_EDGE('',*,*,#29333,.T.) ;
#41862 = ORIENTED_EDGE('',*,*,#29334,.T.) ;
#41863 = ORIENTED_EDGE('',*,*,#29335,.T.) ;
#41864 = ORIENTED_EDGE('',*,*,#29336,.T.) ;
#41865 = ORIENTED_EDGE('',*,*,#27518,.T.) ;
#41866 = ORIENTED_EDGE('',*,*,#27523,.T.) ;
#41867 = ORIENTED_EDGE('',*,*,#29337,.T.) ;
#41868 = ORIENTED_EDGE('',*,*,#29335,.F.) ;
#41869 = ORIENTED_EDGE('',*,*,#29338,.T.) ;
#41870 = ORIENTED_EDGE('',*,*,#29279,.T.) ;
#41871 = ORIENTED_EDGE('',*,*,#29339,.T.) ;
#41872 = ORIENTED_EDGE('',*,*,#29329,.F.) ;
#41873 = ORIENTED_EDGE('',*,*,#29143,.T.) ;
#41874 = ORIENTED_EDGE('',*,*,#29340,.T.) ;
#41875 = ORIENTED_EDGE('',*,*,#29341,.T.) ;
#41876 = ORIENTED_EDGE('',*,*,#29281,.T.) ;
#41877 = ORIENTED_EDGE('',*,*,#29342,.T.) ;
#41878 = ORIENTED_EDGE('',*,*,#29343,.T.) ;
#41879 = ORIENTED_EDGE('',*,*,#29344,.T.) ;
#41880 = ORIENTED_EDGE('',*,*,#29340,.F.) ;
#41881 = ORIENTED_EDGE('',*,*,#29345,.T.) ;
#41882 = ORIENTED_EDGE('',*,*,#28513,.F.) ;
#41883 = ORIENTED_EDGE('',*,*,#29346,.T.) ;
#41884 = ORIENTED_EDGE('',*,*,#29347,.T.) ;
#41885 = ORIENTED_EDGE('',*,*,#29348,.T.) ;
#41886 = ORIENTED_EDGE('',*,*,#29349,.T.) ;
#41887 = ORIENTED_EDGE('',*,*,#29350,.T.) ;
#41888 = ORIENTED_EDGE('',*,*,#29347,.F.) ;
#41889 = ORIENTED_EDGE('',*,*,#29351,.T.) ;
#41890 = ORIENTED_EDGE('',*,*,#29352,.T.) ;
#41891 = ORIENTED_EDGE('',*,*,#29349,.F.) ;
#41892 = ORIENTED_EDGE('',*,*,#29353,.T.) ;
#41893 = ORIENTED_EDGE('',*,*,#29278,.F.) ;
#41894 = ORIENTED_EDGE('',*,*,#29318,.F.) ;
#41895 = ORIENTED_EDGE('',*,*,#29354,.F.) ;
#41896 = ORIENTED_EDGE('',*,*,#28095,.F.) ;
#41897 = ORIENTED_EDGE('',*,*,#29355,.T.) ;
#41898 = ORIENTED_EDGE('',*,*,#29326,.F.) ;
#41899 = ORIENTED_EDGE('',*,*,#29356,.F.) ;
#41900 = ORIENTED_EDGE('',*,*,#28096,.F.) ;
#41901 = ORIENTED_EDGE('',*,*,#29354,.T.) ;
#41902 = ORIENTED_EDGE('',*,*,#29324,.F.) ;
#41903 = ORIENTED_EDGE('',*,*,#29357,.F.) ;
#41904 = ORIENTED_EDGE('',*,*,#28097,.F.) ;
#41905 = ORIENTED_EDGE('',*,*,#29356,.T.) ;
#41906 = ORIENTED_EDGE('',*,*,#29327,.F.) ;
#41907 = ORIENTED_EDGE('',*,*,#29296,.F.) ;
#41908 = ORIENTED_EDGE('',*,*,#29358,.T.) ;
#41909 = ORIENTED_EDGE('',*,*,#28098,.T.) ;
#41910 = ORIENTED_EDGE('',*,*,#29357,.T.) ;
#41911 = ORIENTED_EDGE('',*,*,#29297,.F.) ;
#41912 = ORIENTED_EDGE('',*,*,#28633,.T.) ;
#41913 = ORIENTED_EDGE('',*,*,#28099,.T.) ;
#41914 = ORIENTED_EDGE('',*,*,#29358,.F.) ;
#41915 = ORIENTED_EDGE('',*,*,#28514,.F.) ;
#41916 = ORIENTED_EDGE('',*,*,#29227,.T.) ;
#41917 = ORIENTED_EDGE('',*,*,#29353,.F.) ;
#41918 = ORIENTED_EDGE('',*,*,#29351,.F.) ;
#41919 = ORIENTED_EDGE('',*,*,#29346,.F.) ;
#41920 = ORIENTED_EDGE('',*,*,#28594,.F.) ;
#41921 = ORIENTED_EDGE('',*,*,#28505,.T.) ;
#41922 = ORIENTED_EDGE('',*,*,#29359,.F.) ;
#41923 = ORIENTED_EDGE('',*,*,#29248,.F.) ;
#41924 = ORIENTED_EDGE('',*,*,#29298,.F.) ;
#41925 = ORIENTED_EDGE('',*,*,#29360,.T.) ;
#41926 = ORIENTED_EDGE('',*,*,#28092,.F.) ;
#41927 = ORIENTED_EDGE('',*,*,#29361,.T.) ;
#41928 = ORIENTED_EDGE('',*,*,#29332,.F.) ;
#41929 = ORIENTED_EDGE('',*,*,#29362,.F.) ;
#41930 = ORIENTED_EDGE('',*,*,#28084,.F.) ;
#41931 = ORIENTED_EDGE('',*,*,#29363,.T.) ;
#41932 = ORIENTED_EDGE('',*,*,#29364,.T.) ;
#41933 = ORIENTED_EDGE('',*,*,#28139,.T.) ;
#41934 = ORIENTED_EDGE('',*,*,#29365,.T.) ;
#41935 = ORIENTED_EDGE('',*,*,#29366,.T.) ;
#41936 = ORIENTED_EDGE('',*,*,#29367,.T.) ;
#41937 = ORIENTED_EDGE('',*,*,#29365,.F.) ;
#41938 = ORIENTED_EDGE('',*,*,#28138,.F.) ;
#41939 = ORIENTED_EDGE('',*,*,#29368,.T.) ;
#41940 = ORIENTED_EDGE('',*,*,#29369,.T.) ;
#41941 = ORIENTED_EDGE('',*,*,#29368,.F.) ;
#41942 = ORIENTED_EDGE('',*,*,#28137,.T.) ;
#41943 = ORIENTED_EDGE('',*,*,#29370,.T.) ;
#41944 = ORIENTED_EDGE('',*,*,#29371,.T.) ;
#41945 = ORIENTED_EDGE('',*,*,#29370,.F.) ;
#41946 = ORIENTED_EDGE('',*,*,#28136,.T.) ;
#41947 = ORIENTED_EDGE('',*,*,#29372,.T.) ;
#41948 = ORIENTED_EDGE('',*,*,#29373,.T.) ;
#41949 = ORIENTED_EDGE('',*,*,#29372,.F.) ;
#41950 = ORIENTED_EDGE('',*,*,#28135,.F.) ;
#41951 = ORIENTED_EDGE('',*,*,#29374,.T.) ;
#41952 = ORIENTED_EDGE('',*,*,#29375,.T.) ;
#41953 = ORIENTED_EDGE('',*,*,#29374,.F.) ;
#41954 = ORIENTED_EDGE('',*,*,#28134,.T.) ;
#41955 = ORIENTED_EDGE('',*,*,#29376,.T.) ;
#41956 = ORIENTED_EDGE('',*,*,#29377,.T.) ;
#41957 = ORIENTED_EDGE('',*,*,#29376,.F.) ;
#41958 = ORIENTED_EDGE('',*,*,#28133,.F.) ;
#41959 = ORIENTED_EDGE('',*,*,#29378,.T.) ;
#41960 = ORIENTED_EDGE('',*,*,#29379,.T.) ;
#41961 = ORIENTED_EDGE('',*,*,#29378,.F.) ;
#41962 = ORIENTED_EDGE('',*,*,#28132,.T.) ;
#41963 = ORIENTED_EDGE('',*,*,#29380,.T.) ;
#41964 = ORIENTED_EDGE('',*,*,#29381,.T.) ;
#41965 = ORIENTED_EDGE('',*,*,#29380,.F.) ;
#41966 = ORIENTED_EDGE('',*,*,#28131,.T.) ;
#41967 = ORIENTED_EDGE('',*,*,#29382,.T.) ;
#41968 = ORIENTED_EDGE('',*,*,#28107,.F.) ;
#41969 = ORIENTED_EDGE('',*,*,#29383,.T.) ;
#41970 = ORIENTED_EDGE('',*,*,#29384,.F.) ;
#41971 = ORIENTED_EDGE('',*,*,#29245,.F.) ;
#41972 = ORIENTED_EDGE('',*,*,#28106,.T.) ;
#41973 = ORIENTED_EDGE('',*,*,#29385,.T.) ;
#41974 = ORIENTED_EDGE('',*,*,#29386,.F.) ;
#41975 = ORIENTED_EDGE('',*,*,#29383,.F.) ;
#41976 = ORIENTED_EDGE('',*,*,#28105,.F.) ;
#41977 = ORIENTED_EDGE('',*,*,#29250,.T.) ;
#41978 = ORIENTED_EDGE('',*,*,#29387,.F.) ;
#41979 = ORIENTED_EDGE('',*,*,#29385,.F.) ;
#41980 = ORIENTED_EDGE('',*,*,#28393,.F.) ;
#41981 = ORIENTED_EDGE('',*,*,#28432,.F.) ;
#41982 = ORIENTED_EDGE('',*,*,#28171,.T.) ;
#41983 = ORIENTED_EDGE('',*,*,#29388,.T.) ;
#41984 = ORIENTED_EDGE('',*,*,#28396,.F.) ;
#41985 = ORIENTED_EDGE('',*,*,#29388,.F.) ;
#41986 = ORIENTED_EDGE('',*,*,#28170,.T.) ;
#41987 = ORIENTED_EDGE('',*,*,#29389,.T.) ;
#41988 = ORIENTED_EDGE('',*,*,#29390,.T.) ;
#41989 = ORIENTED_EDGE('',*,*,#28399,.F.) ;
#41990 = ORIENTED_EDGE('',*,*,#29389,.F.) ;
#41991 = ORIENTED_EDGE('',*,*,#28169,.T.) ;
#41992 = ORIENTED_EDGE('',*,*,#28438,.T.) ;
#41993 = ORIENTED_EDGE('',*,*,#28173,.T.) ;
#41994 = ORIENTED_EDGE('',*,*,#29391,.T.) ;
#41995 = ORIENTED_EDGE('',*,*,#29392,.T.) ;
#41996 = ORIENTED_EDGE('',*,*,#29391,.F.) ;
#41997 = ORIENTED_EDGE('',*,*,#29393,.T.) ;
#41998 = ORIENTED_EDGE('',*,*,#28081,.T.) ;
#41999 = ORIENTED_EDGE('',*,*,#29394,.T.) ;
#42000 = ORIENTED_EDGE('',*,*,#29395,.T.) ;
#42001 = ORIENTED_EDGE('',*,*,#29396,.T.) ;
#42002 = ORIENTED_EDGE('',*,*,#29394,.F.) ;
#42003 = ORIENTED_EDGE('',*,*,#28080,.T.) ;
#42004 = ORIENTED_EDGE('',*,*,#29397,.T.) ;
#42005 = ORIENTED_EDGE('',*,*,#29398,.T.) ;
#42006 = ORIENTED_EDGE('',*,*,#29397,.F.) ;
#42007 = ORIENTED_EDGE('',*,*,#28079,.T.) ;
#42008 = ORIENTED_EDGE('',*,*,#29399,.T.) ;
#42009 = ORIENTED_EDGE('',*,*,#29400,.T.) ;
#42010 = ORIENTED_EDGE('',*,*,#29399,.F.) ;
#42011 = ORIENTED_EDGE('',*,*,#28078,.T.) ;
#42012 = ORIENTED_EDGE('',*,*,#29401,.T.) ;
#42013 = ORIENTED_EDGE('',*,*,#29402,.T.) ;
#42014 = ORIENTED_EDGE('',*,*,#29401,.F.) ;
#42015 = ORIENTED_EDGE('',*,*,#28077,.T.) ;
#42016 = ORIENTED_EDGE('',*,*,#29403,.T.) ;
#42017 = ORIENTED_EDGE('',*,*,#29404,.T.) ;
#42018 = ORIENTED_EDGE('',*,*,#29405,.F.) ;
#42019 = ORIENTED_EDGE('',*,*,#28181,.T.) ;
#42020 = ORIENTED_EDGE('',*,*,#29406,.T.) ;
#42021 = ORIENTED_EDGE('',*,*,#29407,.T.) ;
#42022 = ORIENTED_EDGE('',*,*,#29406,.F.) ;
#42023 = ORIENTED_EDGE('',*,*,#28180,.T.) ;
#42024 = ORIENTED_EDGE('',*,*,#29408,.T.) ;
#42025 = ORIENTED_EDGE('',*,*,#29409,.T.) ;
#42026 = ORIENTED_EDGE('',*,*,#29408,.F.) ;
#42027 = ORIENTED_EDGE('',*,*,#28179,.T.) ;
#42028 = ORIENTED_EDGE('',*,*,#29410,.T.) ;
#42029 = ORIENTED_EDGE('',*,*,#29411,.T.) ;
#42030 = ORIENTED_EDGE('',*,*,#29410,.F.) ;
#42031 = ORIENTED_EDGE('',*,*,#28178,.T.) ;
#42032 = ORIENTED_EDGE('',*,*,#29412,.T.) ;
#42033 = ORIENTED_EDGE('',*,*,#29413,.T.) ;
#42034 = ORIENTED_EDGE('',*,*,#29412,.F.) ;
#42035 = ORIENTED_EDGE('',*,*,#28177,.T.) ;
#42036 = ORIENTED_EDGE('',*,*,#29414,.T.) ;
#42037 = ORIENTED_EDGE('',*,*,#29415,.T.) ;
#42038 = ORIENTED_EDGE('',*,*,#29414,.F.) ;
#42039 = ORIENTED_EDGE('',*,*,#28176,.T.) ;
#42040 = ORIENTED_EDGE('',*,*,#29416,.T.) ;
#42041 = ORIENTED_EDGE('',*,*,#29417,.T.) ;
#42042 = ORIENTED_EDGE('',*,*,#29416,.F.) ;
#42043 = ORIENTED_EDGE('',*,*,#28175,.T.) ;
#42044 = ORIENTED_EDGE('',*,*,#29418,.T.) ;
#42045 = ORIENTED_EDGE('',*,*,#28188,.T.) ;
#42046 = ORIENTED_EDGE('',*,*,#29419,.T.) ;
#42047 = ORIENTED_EDGE('',*,*,#29420,.T.) ;
#42048 = ORIENTED_EDGE('',*,*,#29419,.F.) ;
#42049 = ORIENTED_EDGE('',*,*,#29421,.T.) ;
#42050 = ORIENTED_EDGE('',*,*,#29422,.F.) ;
#42051 = ORIENTED_EDGE('',*,*,#28195,.T.) ;
#42052 = ORIENTED_EDGE('',*,*,#29423,.T.) ;
#42053 = ORIENTED_EDGE('',*,*,#29424,.T.) ;
#42054 = ORIENTED_EDGE('',*,*,#29423,.F.) ;
#42055 = ORIENTED_EDGE('',*,*,#28194,.T.) ;
#42056 = ORIENTED_EDGE('',*,*,#29425,.T.) ;
#42057 = ORIENTED_EDGE('',*,*,#29426,.T.) ;
#42058 = ORIENTED_EDGE('',*,*,#29425,.F.) ;
#42059 = ORIENTED_EDGE('',*,*,#28193,.T.) ;
#42060 = ORIENTED_EDGE('',*,*,#29427,.T.) ;
#42061 = ORIENTED_EDGE('',*,*,#29428,.T.) ;
#42062 = ORIENTED_EDGE('',*,*,#29427,.F.) ;
#42063 = ORIENTED_EDGE('',*,*,#28192,.T.) ;
#42064 = ORIENTED_EDGE('',*,*,#29429,.T.) ;
#42065 = ORIENTED_EDGE('',*,*,#29430,.T.) ;
#42066 = ORIENTED_EDGE('',*,*,#29429,.F.) ;
#42067 = ORIENTED_EDGE('',*,*,#28191,.T.) ;
#42068 = ORIENTED_EDGE('',*,*,#29431,.T.) ;
#42069 = ORIENTED_EDGE('',*,*,#29432,.T.) ;
#42070 = ORIENTED_EDGE('',*,*,#29431,.F.) ;
#42071 = ORIENTED_EDGE('',*,*,#28190,.T.) ;
#42072 = ORIENTED_EDGE('',*,*,#29433,.T.) ;
#42073 = ORIENTED_EDGE('',*,*,#29434,.T.) ;
#42074 = ORIENTED_EDGE('',*,*,#29435,.F.) ;
#42075 = ORIENTED_EDGE('',*,*,#28207,.T.) ;
#42076 = ORIENTED_EDGE('',*,*,#29436,.T.) ;
#42077 = ORIENTED_EDGE('',*,*,#29437,.T.) ;
#42078 = ORIENTED_EDGE('',*,*,#29436,.F.) ;
#42079 = ORIENTED_EDGE('',*,*,#28206,.T.) ;
#42080 = ORIENTED_EDGE('',*,*,#29438,.T.) ;
#42081 = ORIENTED_EDGE('',*,*,#29439,.T.) ;
#42082 = ORIENTED_EDGE('',*,*,#29438,.F.) ;
#42083 = ORIENTED_EDGE('',*,*,#28205,.T.) ;
#42084 = ORIENTED_EDGE('',*,*,#29440,.T.) ;
#42085 = ORIENTED_EDGE('',*,*,#29441,.T.) ;
#42086 = ORIENTED_EDGE('',*,*,#29440,.F.) ;
#42087 = ORIENTED_EDGE('',*,*,#28204,.T.) ;
#42088 = ORIENTED_EDGE('',*,*,#29442,.T.) ;
#42089 = ORIENTED_EDGE('',*,*,#27634,.F.) ;
#42090 = ORIENTED_EDGE('',*,*,#29443,.T.) ;
#42091 = ORIENTED_EDGE('',*,*,#29442,.F.) ;
#42092 = ORIENTED_EDGE('',*,*,#28203,.T.) ;
#42093 = ORIENTED_EDGE('',*,*,#29444,.T.) ;
#42094 = ORIENTED_EDGE('',*,*,#27638,.F.) ;
#42095 = ORIENTED_EDGE('',*,*,#28202,.T.) ;
#42096 = ORIENTED_EDGE('',*,*,#29445,.T.) ;
#42097 = ORIENTED_EDGE('',*,*,#29446,.T.) ;
#42098 = ORIENTED_EDGE('',*,*,#29447,.F.) ;
#42099 = ORIENTED_EDGE('',*,*,#28144,.T.) ;
#42100 = ORIENTED_EDGE('',*,*,#29448,.T.) ;
#42101 = ORIENTED_EDGE('',*,*,#29449,.T.) ;
#42102 = ORIENTED_EDGE('',*,*,#29448,.F.) ;
#42103 = ORIENTED_EDGE('',*,*,#28143,.T.) ;
#42104 = ORIENTED_EDGE('',*,*,#29450,.F.) ;
#42105 = ORIENTED_EDGE('',*,*,#27898,.T.) ;
#42106 = ORIENTED_EDGE('',*,*,#29451,.T.) ;
#42107 = ORIENTED_EDGE('',*,*,#29452,.T.) ;
#42108 = ORIENTED_EDGE('',*,*,#29451,.F.) ;
#42109 = ORIENTED_EDGE('',*,*,#27897,.F.) ;
#42110 = ORIENTED_EDGE('',*,*,#29453,.T.) ;
#42111 = ORIENTED_EDGE('',*,*,#29454,.T.) ;
#42112 = ORIENTED_EDGE('',*,*,#29453,.F.) ;
#42113 = ORIENTED_EDGE('',*,*,#27896,.T.) ;
#42114 = ORIENTED_EDGE('',*,*,#29455,.T.) ;
#42115 = ORIENTED_EDGE('',*,*,#29456,.T.) ;
#42116 = ORIENTED_EDGE('',*,*,#29455,.F.) ;
#42117 = ORIENTED_EDGE('',*,*,#27895,.F.) ;
#42118 = ORIENTED_EDGE('',*,*,#28251,.T.) ;
#42119 = ORIENTED_EDGE('',*,*,#29457,.T.) ;
#42120 = ORIENTED_EDGE('',*,*,#29458,.F.) ;
#42121 = ORIENTED_EDGE('',*,*,#28221,.T.) ;
#42122 = ORIENTED_EDGE('',*,*,#29459,.T.) ;
#42123 = ORIENTED_EDGE('',*,*,#29460,.T.) ;
#42124 = ORIENTED_EDGE('',*,*,#29459,.F.) ;
#42125 = ORIENTED_EDGE('',*,*,#28220,.T.) ;
#42126 = ORIENTED_EDGE('',*,*,#29461,.T.) ;
#42127 = ORIENTED_EDGE('',*,*,#29462,.T.) ;
#42128 = ORIENTED_EDGE('',*,*,#29461,.F.) ;
#42129 = ORIENTED_EDGE('',*,*,#28219,.T.) ;
#42130 = ORIENTED_EDGE('',*,*,#29463,.T.) ;
#42131 = ORIENTED_EDGE('',*,*,#29464,.T.) ;
#42132 = ORIENTED_EDGE('',*,*,#29463,.F.) ;
#42133 = ORIENTED_EDGE('',*,*,#28218,.T.) ;
#42134 = ORIENTED_EDGE('',*,*,#29465,.T.) ;
#42135 = ORIENTED_EDGE('',*,*,#29466,.T.) ;
#42136 = ORIENTED_EDGE('',*,*,#29465,.F.) ;
#42137 = ORIENTED_EDGE('',*,*,#28217,.T.) ;
#42138 = ORIENTED_EDGE('',*,*,#29467,.T.) ;
#42139 = ORIENTED_EDGE('',*,*,#29468,.T.) ;
#42140 = ORIENTED_EDGE('',*,*,#29467,.F.) ;
#42141 = ORIENTED_EDGE('',*,*,#28216,.T.) ;
#42142 = ORIENTED_EDGE('',*,*,#29469,.T.) ;
#42143 = ORIENTED_EDGE('',*,*,#29470,.T.) ;
#42144 = ORIENTED_EDGE('',*,*,#29469,.F.) ;
#42145 = ORIENTED_EDGE('',*,*,#28215,.T.) ;
#42146 = ORIENTED_EDGE('',*,*,#29471,.T.) ;
#42147 = ORIENTED_EDGE('',*,*,#29472,.T.) ;
#42148 = ORIENTED_EDGE('',*,*,#29471,.F.) ;
#42149 = ORIENTED_EDGE('',*,*,#28214,.T.) ;
#42150 = ORIENTED_EDGE('',*,*,#29473,.T.) ;
#42151 = ORIENTED_EDGE('',*,*,#29474,.T.) ;
#42152 = ORIENTED_EDGE('',*,*,#29473,.F.) ;
#42153 = ORIENTED_EDGE('',*,*,#28227,.T.) ;
#42154 = ORIENTED_EDGE('',*,*,#29475,.T.) ;
#42155 = ORIENTED_EDGE('',*,*,#29476,.T.) ;
#42156 = ORIENTED_EDGE('',*,*,#29475,.F.) ;
#42157 = ORIENTED_EDGE('',*,*,#28226,.T.) ;
#42158 = ORIENTED_EDGE('',*,*,#29477,.T.) ;
#42159 = ORIENTED_EDGE('',*,*,#29478,.T.) ;
#42160 = ORIENTED_EDGE('',*,*,#29477,.F.) ;
#42161 = ORIENTED_EDGE('',*,*,#28225,.T.) ;
#42162 = ORIENTED_EDGE('',*,*,#29479,.T.) ;
#42163 = ORIENTED_EDGE('',*,*,#29480,.T.) ;
#42164 = ORIENTED_EDGE('',*,*,#29479,.F.) ;
#42165 = ORIENTED_EDGE('',*,*,#28224,.T.) ;
#42166 = ORIENTED_EDGE('',*,*,#29481,.T.) ;
#42167 = ORIENTED_EDGE('',*,*,#29482,.T.) ;
#42168 = ORIENTED_EDGE('',*,*,#29481,.F.) ;
#42169 = ORIENTED_EDGE('',*,*,#28223,.T.) ;
#42170 = ORIENTED_EDGE('',*,*,#29483,.T.) ;
#42171 = ORIENTED_EDGE('',*,*,#29484,.T.) ;
#42172 = ORIENTED_EDGE('',*,*,#29483,.F.) ;
#42173 = ORIENTED_EDGE('',*,*,#28222,.T.) ;
#42174 = ORIENTED_EDGE('',*,*,#29458,.T.) ;
#42175 = ORIENTED_EDGE('',*,*,#29472,.F.) ;
#42176 = ORIENTED_EDGE('',*,*,#29474,.F.) ;
#42177 = ORIENTED_EDGE('',*,*,#29476,.F.) ;
#42178 = ORIENTED_EDGE('',*,*,#29478,.F.) ;
#42179 = ORIENTED_EDGE('',*,*,#29480,.F.) ;
#42180 = ORIENTED_EDGE('',*,*,#29482,.F.) ;
#42181 = ORIENTED_EDGE('',*,*,#29484,.F.) ;
#42182 = ORIENTED_EDGE('',*,*,#29457,.F.) ;
#42183 = ORIENTED_EDGE('',*,*,#29460,.F.) ;
#42184 = ORIENTED_EDGE('',*,*,#29462,.F.) ;
#42185 = ORIENTED_EDGE('',*,*,#29464,.F.) ;
#42186 = ORIENTED_EDGE('',*,*,#29466,.F.) ;
#42187 = ORIENTED_EDGE('',*,*,#29468,.F.) ;
#42188 = ORIENTED_EDGE('',*,*,#29470,.F.) ;
#42189 = ORIENTED_EDGE('',*,*,#29485,.T.) ;
#42190 = ORIENTED_EDGE('',*,*,#29433,.F.) ;
#42191 = ORIENTED_EDGE('',*,*,#28189,.T.) ;
#42192 = ORIENTED_EDGE('',*,*,#29486,.T.) ;
#42193 = ORIENTED_EDGE('',*,*,#29487,.T.) ;
#42194 = ORIENTED_EDGE('',*,*,#29486,.F.) ;
#42195 = ORIENTED_EDGE('',*,*,#28200,.T.) ;
#42196 = ORIENTED_EDGE('',*,*,#29488,.T.) ;
#42197 = ORIENTED_EDGE('',*,*,#29489,.T.) ;
#42198 = ORIENTED_EDGE('',*,*,#29488,.F.) ;
#42199 = ORIENTED_EDGE('',*,*,#28199,.T.) ;
#42200 = ORIENTED_EDGE('',*,*,#29490,.T.) ;
#42201 = ORIENTED_EDGE('',*,*,#29491,.T.) ;
#42202 = ORIENTED_EDGE('',*,*,#29490,.F.) ;
#42203 = ORIENTED_EDGE('',*,*,#28198,.T.) ;
#42204 = ORIENTED_EDGE('',*,*,#29492,.T.) ;
#42205 = ORIENTED_EDGE('',*,*,#29493,.T.) ;
#42206 = ORIENTED_EDGE('',*,*,#29492,.F.) ;
#42207 = ORIENTED_EDGE('',*,*,#28197,.T.) ;
#42208 = ORIENTED_EDGE('',*,*,#29494,.T.) ;
#42209 = ORIENTED_EDGE('',*,*,#29495,.T.) ;
#42210 = ORIENTED_EDGE('',*,*,#29494,.F.) ;
#42211 = ORIENTED_EDGE('',*,*,#28196,.T.) ;
#42212 = ORIENTED_EDGE('',*,*,#29422,.T.) ;
#42213 = ORIENTED_EDGE('',*,*,#29485,.F.) ;
#42214 = ORIENTED_EDGE('',*,*,#29487,.F.) ;
#42215 = ORIENTED_EDGE('',*,*,#29489,.F.) ;
#42216 = ORIENTED_EDGE('',*,*,#29491,.F.) ;
#42217 = ORIENTED_EDGE('',*,*,#29493,.F.) ;
#42218 = ORIENTED_EDGE('',*,*,#29495,.F.) ;
#42219 = ORIENTED_EDGE('',*,*,#29421,.F.) ;
#42220 = ORIENTED_EDGE('',*,*,#29424,.F.) ;
#42221 = ORIENTED_EDGE('',*,*,#29426,.F.) ;
#42222 = ORIENTED_EDGE('',*,*,#29428,.F.) ;
#42223 = ORIENTED_EDGE('',*,*,#29430,.F.) ;
#42224 = ORIENTED_EDGE('',*,*,#29432,.F.) ;
#42225 = ORIENTED_EDGE('',*,*,#29496,.T.) ;
#42226 = ORIENTED_EDGE('',*,*,#29445,.F.) ;
#42227 = ORIENTED_EDGE('',*,*,#28201,.T.) ;
#42228 = ORIENTED_EDGE('',*,*,#29497,.T.) ;
#42229 = ORIENTED_EDGE('',*,*,#29498,.T.) ;
#42230 = ORIENTED_EDGE('',*,*,#29497,.F.) ;
#42231 = ORIENTED_EDGE('',*,*,#28213,.T.) ;
#42232 = ORIENTED_EDGE('',*,*,#29499,.T.) ;
#42233 = ORIENTED_EDGE('',*,*,#29500,.T.) ;
#42234 = ORIENTED_EDGE('',*,*,#29499,.F.) ;
#42235 = ORIENTED_EDGE('',*,*,#28212,.T.) ;
#42236 = ORIENTED_EDGE('',*,*,#29501,.T.) ;
#42237 = ORIENTED_EDGE('',*,*,#29502,.T.) ;
#42238 = ORIENTED_EDGE('',*,*,#29501,.F.) ;
#42239 = ORIENTED_EDGE('',*,*,#28211,.T.) ;
#42240 = ORIENTED_EDGE('',*,*,#29503,.T.) ;
#42241 = ORIENTED_EDGE('',*,*,#29504,.T.) ;
#42242 = ORIENTED_EDGE('',*,*,#29503,.F.) ;
#42243 = ORIENTED_EDGE('',*,*,#28210,.T.) ;
#42244 = ORIENTED_EDGE('',*,*,#29505,.T.) ;
#42245 = ORIENTED_EDGE('',*,*,#29506,.T.) ;
#42246 = ORIENTED_EDGE('',*,*,#29505,.F.) ;
#42247 = ORIENTED_EDGE('',*,*,#28209,.T.) ;
#42248 = ORIENTED_EDGE('',*,*,#29507,.T.) ;
#42249 = ORIENTED_EDGE('',*,*,#29508,.T.) ;
#42250 = ORIENTED_EDGE('',*,*,#29507,.F.) ;
#42251 = ORIENTED_EDGE('',*,*,#28208,.T.) ;
#42252 = ORIENTED_EDGE('',*,*,#29435,.T.) ;
#42253 = ORIENTED_EDGE('',*,*,#27633,.T.) ;
#42254 = ORIENTED_EDGE('',*,*,#27639,.F.) ;
#42255 = ORIENTED_EDGE('',*,*,#29444,.F.) ;
#42256 = ORIENTED_EDGE('',*,*,#29496,.F.) ;
#42257 = ORIENTED_EDGE('',*,*,#29498,.F.) ;
#42258 = ORIENTED_EDGE('',*,*,#29500,.F.) ;
#42259 = ORIENTED_EDGE('',*,*,#29502,.F.) ;
#42260 = ORIENTED_EDGE('',*,*,#29504,.F.) ;
#42261 = ORIENTED_EDGE('',*,*,#29506,.F.) ;
#42262 = ORIENTED_EDGE('',*,*,#29508,.F.) ;
#42263 = ORIENTED_EDGE('',*,*,#29434,.F.) ;
#42264 = ORIENTED_EDGE('',*,*,#29437,.F.) ;
#42265 = ORIENTED_EDGE('',*,*,#29439,.F.) ;
#42266 = ORIENTED_EDGE('',*,*,#29441,.F.) ;
#42267 = ORIENTED_EDGE('',*,*,#29443,.F.) ;
#42268 = ORIENTED_EDGE('',*,*,#29509,.T.) ;
#42269 = ORIENTED_EDGE('',*,*,#29403,.F.) ;
#42270 = ORIENTED_EDGE('',*,*,#28076,.T.) ;
#42271 = ORIENTED_EDGE('',*,*,#29510,.T.) ;
#42272 = ORIENTED_EDGE('',*,*,#29511,.T.) ;
#42273 = ORIENTED_EDGE('',*,*,#29510,.F.) ;
#42274 = ORIENTED_EDGE('',*,*,#28075,.T.) ;
#42275 = ORIENTED_EDGE('',*,*,#29512,.T.) ;
#42276 = ORIENTED_EDGE('',*,*,#29513,.T.) ;
#42277 = ORIENTED_EDGE('',*,*,#29512,.F.) ;
#42278 = ORIENTED_EDGE('',*,*,#28074,.T.) ;
#42279 = ORIENTED_EDGE('',*,*,#29514,.T.) ;
#42280 = ORIENTED_EDGE('',*,*,#29515,.T.) ;
#42281 = ORIENTED_EDGE('',*,*,#29514,.F.) ;
#42282 = ORIENTED_EDGE('',*,*,#28073,.T.) ;
#42283 = ORIENTED_EDGE('',*,*,#29516,.T.) ;
#42284 = ORIENTED_EDGE('',*,*,#29517,.T.) ;
#42285 = ORIENTED_EDGE('',*,*,#29516,.F.) ;
#42286 = ORIENTED_EDGE('',*,*,#28072,.T.) ;
#42287 = ORIENTED_EDGE('',*,*,#29518,.T.) ;
#42288 = ORIENTED_EDGE('',*,*,#29519,.T.) ;
#42289 = ORIENTED_EDGE('',*,*,#29518,.F.) ;
#42290 = ORIENTED_EDGE('',*,*,#28071,.T.) ;
#42291 = ORIENTED_EDGE('',*,*,#29520,.T.) ;
#42292 = ORIENTED_EDGE('',*,*,#29521,.T.) ;
#42293 = ORIENTED_EDGE('',*,*,#29520,.F.) ;
#42294 = ORIENTED_EDGE('',*,*,#28070,.T.) ;
#42295 = ORIENTED_EDGE('',*,*,#29522,.T.) ;
#42296 = ORIENTED_EDGE('',*,*,#29523,.T.) ;
#42297 = ORIENTED_EDGE('',*,*,#29395,.F.) ;
#42298 = ORIENTED_EDGE('',*,*,#29396,.F.) ;
#42299 = ORIENTED_EDGE('',*,*,#29398,.F.) ;
#42300 = ORIENTED_EDGE('',*,*,#29400,.F.) ;
#42301 = ORIENTED_EDGE('',*,*,#29402,.F.) ;
#42302 = ORIENTED_EDGE('',*,*,#29509,.F.) ;
#42303 = ORIENTED_EDGE('',*,*,#29511,.F.) ;
#42304 = ORIENTED_EDGE('',*,*,#29513,.F.) ;
#42305 = ORIENTED_EDGE('',*,*,#29515,.F.) ;
#42306 = ORIENTED_EDGE('',*,*,#29517,.F.) ;
#42307 = ORIENTED_EDGE('',*,*,#29519,.F.) ;
#42308 = ORIENTED_EDGE('',*,*,#29521,.F.) ;
#42309 = ORIENTED_EDGE('',*,*,#29524,.F.) ;
#42310 = ORIENTED_EDGE('',*,*,#29525,.T.) ;
#42311 = ORIENTED_EDGE('',*,*,#29418,.F.) ;
#42312 = ORIENTED_EDGE('',*,*,#28174,.T.) ;
#42313 = ORIENTED_EDGE('',*,*,#29526,.T.) ;
#42314 = ORIENTED_EDGE('',*,*,#29527,.T.) ;
#42315 = ORIENTED_EDGE('',*,*,#29526,.F.) ;
#42316 = ORIENTED_EDGE('',*,*,#28187,.T.) ;
#42317 = ORIENTED_EDGE('',*,*,#29528,.T.) ;
#42318 = ORIENTED_EDGE('',*,*,#29529,.T.) ;
#42319 = ORIENTED_EDGE('',*,*,#29528,.F.) ;
#42320 = ORIENTED_EDGE('',*,*,#28186,.T.) ;
#42321 = ORIENTED_EDGE('',*,*,#29530,.T.) ;
#42322 = ORIENTED_EDGE('',*,*,#29531,.T.) ;
#42323 = ORIENTED_EDGE('',*,*,#29530,.F.) ;
#42324 = ORIENTED_EDGE('',*,*,#28185,.T.) ;
#42325 = ORIENTED_EDGE('',*,*,#29532,.T.) ;
#42326 = ORIENTED_EDGE('',*,*,#29533,.T.) ;
#42327 = ORIENTED_EDGE('',*,*,#29532,.F.) ;
#42328 = ORIENTED_EDGE('',*,*,#28184,.T.) ;
#42329 = ORIENTED_EDGE('',*,*,#29534,.T.) ;
#42330 = ORIENTED_EDGE('',*,*,#29535,.T.) ;
#42331 = ORIENTED_EDGE('',*,*,#29534,.F.) ;
#42332 = ORIENTED_EDGE('',*,*,#28183,.T.) ;
#42333 = ORIENTED_EDGE('',*,*,#29536,.T.) ;
#42334 = ORIENTED_EDGE('',*,*,#29537,.T.) ;
#42335 = ORIENTED_EDGE('',*,*,#29536,.F.) ;
#42336 = ORIENTED_EDGE('',*,*,#28182,.T.) ;
#42337 = ORIENTED_EDGE('',*,*,#29405,.T.) ;
#42338 = ORIENTED_EDGE('',*,*,#29525,.F.) ;
#42339 = ORIENTED_EDGE('',*,*,#29527,.F.) ;
#42340 = ORIENTED_EDGE('',*,*,#29529,.F.) ;
#42341 = ORIENTED_EDGE('',*,*,#29531,.F.) ;
#42342 = ORIENTED_EDGE('',*,*,#29533,.F.) ;
#42343 = ORIENTED_EDGE('',*,*,#29535,.F.) ;
#42344 = ORIENTED_EDGE('',*,*,#29537,.F.) ;
#42345 = ORIENTED_EDGE('',*,*,#29404,.F.) ;
#42346 = ORIENTED_EDGE('',*,*,#29407,.F.) ;
#42347 = ORIENTED_EDGE('',*,*,#29409,.F.) ;
#42348 = ORIENTED_EDGE('',*,*,#29411,.F.) ;
#42349 = ORIENTED_EDGE('',*,*,#29413,.F.) ;
#42350 = ORIENTED_EDGE('',*,*,#29415,.F.) ;
#42351 = ORIENTED_EDGE('',*,*,#29417,.F.) ;
#42352 = ORIENTED_EDGE('',*,*,#29538,.T.) ;
#42353 = ORIENTED_EDGE('',*,*,#28249,.F.) ;
#42354 = ORIENTED_EDGE('',*,*,#28150,.T.) ;
#42355 = ORIENTED_EDGE('',*,*,#29539,.T.) ;
#42356 = ORIENTED_EDGE('',*,*,#29540,.T.) ;
#42357 = ORIENTED_EDGE('',*,*,#29539,.F.) ;
#42358 = ORIENTED_EDGE('',*,*,#28149,.T.) ;
#42359 = ORIENTED_EDGE('',*,*,#29541,.T.) ;
#42360 = ORIENTED_EDGE('',*,*,#29542,.T.) ;
#42361 = ORIENTED_EDGE('',*,*,#29541,.F.) ;
#42362 = ORIENTED_EDGE('',*,*,#28148,.T.) ;
#42363 = ORIENTED_EDGE('',*,*,#29543,.T.) ;
#42364 = ORIENTED_EDGE('',*,*,#29544,.T.) ;
#42365 = ORIENTED_EDGE('',*,*,#29543,.F.) ;
#42366 = ORIENTED_EDGE('',*,*,#28147,.T.) ;
#42367 = ORIENTED_EDGE('',*,*,#29545,.T.) ;
#42368 = ORIENTED_EDGE('',*,*,#29546,.T.) ;
#42369 = ORIENTED_EDGE('',*,*,#29545,.F.) ;
#42370 = ORIENTED_EDGE('',*,*,#28146,.T.) ;
#42371 = ORIENTED_EDGE('',*,*,#29547,.T.) ;
#42372 = ORIENTED_EDGE('',*,*,#29548,.T.) ;
#42373 = ORIENTED_EDGE('',*,*,#29547,.F.) ;
#42374 = ORIENTED_EDGE('',*,*,#28145,.T.) ;
#42375 = ORIENTED_EDGE('',*,*,#29447,.T.) ;
#42376 = ORIENTED_EDGE('',*,*,#29538,.F.) ;
#42377 = ORIENTED_EDGE('',*,*,#29540,.F.) ;
#42378 = ORIENTED_EDGE('',*,*,#29542,.F.) ;
#42379 = ORIENTED_EDGE('',*,*,#29544,.F.) ;
#42380 = ORIENTED_EDGE('',*,*,#29546,.F.) ;
#42381 = ORIENTED_EDGE('',*,*,#29548,.F.) ;
#42382 = ORIENTED_EDGE('',*,*,#29446,.F.) ;
#42383 = ORIENTED_EDGE('',*,*,#29449,.F.) ;
#42384 = ORIENTED_EDGE('',*,*,#29452,.F.) ;
#42385 = ORIENTED_EDGE('',*,*,#29454,.F.) ;
#42386 = ORIENTED_EDGE('',*,*,#29456,.F.) ;
#42387 = ORIENTED_EDGE('',*,*,#28250,.F.) ;
#42388 = ORIENTED_EDGE('',*,*,#29392,.F.) ;
#42389 = ORIENTED_EDGE('',*,*,#29549,.T.) ;
#42390 = ORIENTED_EDGE('',*,*,#29382,.F.) ;
#42391 = ORIENTED_EDGE('',*,*,#28130,.F.) ;
#42392 = ORIENTED_EDGE('',*,*,#29550,.T.) ;
#42393 = ORIENTED_EDGE('',*,*,#29551,.T.) ;
#42394 = ORIENTED_EDGE('',*,*,#29550,.F.) ;
#42395 = ORIENTED_EDGE('',*,*,#28129,.T.) ;
#42396 = ORIENTED_EDGE('',*,*,#29552,.T.) ;
#42397 = ORIENTED_EDGE('',*,*,#29420,.F.) ;
#42398 = ORIENTED_EDGE('',*,*,#29336,.F.) ;
#42399 = ORIENTED_EDGE('',*,*,#29553,.F.) ;
#42400 = ORIENTED_EDGE('',*,*,#28089,.T.) ;
#42401 = ORIENTED_EDGE('',*,*,#29554,.T.) ;
#42402 = ORIENTED_EDGE('',*,*,#29333,.F.) ;
#42403 = ORIENTED_EDGE('',*,*,#29554,.F.) ;
#42404 = ORIENTED_EDGE('',*,*,#28088,.T.) ;
#42405 = ORIENTED_EDGE('',*,*,#29555,.F.) ;
#42406 = ORIENTED_EDGE('',*,*,#29343,.F.) ;
#42407 = ORIENTED_EDGE('',*,*,#29556,.F.) ;
#42408 = ORIENTED_EDGE('',*,*,#29344,.F.) ;
#42409 = ORIENTED_EDGE('',*,*,#29555,.T.) ;
#42410 = ORIENTED_EDGE('',*,*,#28087,.T.) ;
#42411 = ORIENTED_EDGE('',*,*,#29557,.F.) ;
#42412 = ORIENTED_EDGE('',*,*,#29277,.F.) ;
#42413 = ORIENTED_EDGE('',*,*,#29558,.F.) ;
#42414 = ORIENTED_EDGE('',*,*,#28065,.T.) ;
#42415 = ORIENTED_EDGE('',*,*,#29559,.F.) ;
#42416 = ORIENTED_EDGE('',*,*,#29352,.F.) ;
#42417 = ORIENTED_EDGE('',*,*,#27911,.F.) ;
#42418 = ORIENTED_EDGE('',*,*,#28058,.F.) ;
#42419 = ORIENTED_EDGE('',*,*,#28061,.F.) ;
#42420 = ORIENTED_EDGE('',*,*,#28051,.F.) ;
#42421 = ORIENTED_EDGE('',*,*,#28164,.F.) ;
#42422 = ORIENTED_EDGE('',*,*,#29560,.F.) ;
#42423 = ORIENTED_EDGE('',*,*,#28301,.F.) ;
#42424 = ORIENTED_EDGE('',*,*,#27917,.T.) ;
#42425 = ORIENTED_EDGE('',*,*,#28277,.F.) ;
#42426 = ORIENTED_EDGE('',*,*,#29561,.T.) ;
#42427 = ORIENTED_EDGE('',*,*,#28294,.F.) ;
#42428 = ORIENTED_EDGE('',*,*,#28292,.F.) ;
#42429 = ORIENTED_EDGE('',*,*,#28275,.F.) ;
#42430 = ORIENTED_EDGE('',*,*,#29562,.T.) ;
#42431 = ORIENTED_EDGE('',*,*,#28296,.F.) ;
#42432 = ORIENTED_EDGE('',*,*,#29561,.F.) ;
#42433 = ORIENTED_EDGE('',*,*,#28270,.F.) ;
#42434 = ORIENTED_EDGE('',*,*,#29563,.T.) ;
#42435 = ORIENTED_EDGE('',*,*,#28298,.F.) ;
#42436 = ORIENTED_EDGE('',*,*,#29562,.F.) ;
#42437 = ORIENTED_EDGE('',*,*,#28269,.F.) ;
#42438 = ORIENTED_EDGE('',*,*,#28303,.F.) ;
#42439 = ORIENTED_EDGE('',*,*,#29564,.T.) ;
#42440 = ORIENTED_EDGE('',*,*,#28162,.F.) ;
#42441 = ORIENTED_EDGE('',*,*,#28299,.T.) ;
#42442 = ORIENTED_EDGE('',*,*,#28300,.T.) ;
#42443 = ORIENTED_EDGE('',*,*,#29563,.F.) ;
#42444 = ORIENTED_EDGE('',*,*,#28163,.F.) ;
#42445 = ORIENTED_EDGE('',*,*,#29564,.F.) ;
#42446 = ORIENTED_EDGE('',*,*,#28302,.F.) ;
#42447 = ORIENTED_EDGE('',*,*,#29560,.T.) ;
#42448 = ORIENTED_EDGE('',*,*,#29565,.T.) ;
#42449 = ORIENTED_EDGE('',*,*,#29366,.F.) ;
#42450 = ORIENTED_EDGE('',*,*,#29367,.F.) ;
#42451 = ORIENTED_EDGE('',*,*,#29369,.F.) ;
#42452 = ORIENTED_EDGE('',*,*,#29371,.F.) ;
#42453 = ORIENTED_EDGE('',*,*,#29373,.F.) ;
#42454 = ORIENTED_EDGE('',*,*,#29375,.F.) ;
#42455 = ORIENTED_EDGE('',*,*,#29377,.F.) ;
#42456 = ORIENTED_EDGE('',*,*,#29379,.F.) ;
#42457 = ORIENTED_EDGE('',*,*,#29381,.F.) ;
#42458 = ORIENTED_EDGE('',*,*,#29549,.F.) ;
#42459 = ORIENTED_EDGE('',*,*,#29551,.F.) ;
#42460 = ORIENTED_EDGE('',*,*,#29566,.F.) ;
#42461 = ORIENTED_EDGE('',*,*,#29567,.T.) ;
#42462 = ORIENTED_EDGE('',*,*,#29566,.T.) ;
#42463 = ORIENTED_EDGE('',*,*,#29552,.F.) ;
#42464 = ORIENTED_EDGE('',*,*,#28128,.F.) ;
#42465 = ORIENTED_EDGE('',*,*,#27904,.F.) ;
#42466 = ORIENTED_EDGE('',*,*,#27907,.T.) ;
#42467 = ORIENTED_EDGE('',*,*,#28152,.F.) ;
#42468 = ORIENTED_EDGE('',*,*,#28248,.F.) ;
#42469 = ORIENTED_EDGE('',*,*,#28240,.T.) ;
#42470 = ORIENTED_EDGE('',*,*,#27901,.T.) ;
#42471 = ORIENTED_EDGE('',*,*,#29568,.T.) ;
#42472 = ORIENTED_EDGE('',*,*,#28140,.F.) ;
#42473 = ORIENTED_EDGE('',*,*,#29364,.F.) ;
#42474 = ORIENTED_EDGE('',*,*,#29565,.F.) ;
#42475 = ORIENTED_EDGE('',*,*,#29567,.F.) ;
#42476 = ORIENTED_EDGE('',*,*,#28127,.T.) ;
#42477 = ORIENTED_EDGE('',*,*,#28234,.F.) ;
#42478 = ORIENTED_EDGE('',*,*,#28141,.F.) ;
#42479 = ORIENTED_EDGE('',*,*,#29568,.F.) ;
#42480 = ORIENTED_EDGE('',*,*,#27900,.F.) ;
#42481 = ORIENTED_EDGE('',*,*,#29569,.T.) ;
#42482 = ORIENTED_EDGE('',*,*,#28142,.F.) ;
#42483 = ORIENTED_EDGE('',*,*,#29569,.F.) ;
#42484 = ORIENTED_EDGE('',*,*,#27899,.T.) ;
#42485 = ORIENTED_EDGE('',*,*,#29450,.T.) ;
#42486 = ORIENTED_EDGE('',*,*,#29220,.F.) ;
#42487 = ORIENTED_EDGE('',*,*,#28244,.T.) ;
#42488 = ORIENTED_EDGE('',*,*,#28238,.F.) ;
#42489 = ORIENTED_EDGE('',*,*,#28123,.T.) ;
#42490 = ORIENTED_EDGE('',*,*,#29570,.T.) ;
#42491 = ORIENTED_EDGE('',*,*,#29570,.F.) ;
#42492 = ORIENTED_EDGE('',*,*,#28122,.F.) ;
#42493 = ORIENTED_EDGE('',*,*,#28038,.F.) ;
#42494 = ORIENTED_EDGE('',*,*,#29221,.F.) ;
#42495 = ORIENTED_EDGE('',*,*,#29330,.F.) ;
#42496 = ORIENTED_EDGE('',*,*,#29571,.F.) ;
#42497 = ORIENTED_EDGE('',*,*,#28085,.F.) ;
#42498 = ORIENTED_EDGE('',*,*,#29362,.T.) ;
#42499 = ORIENTED_EDGE('',*,*,#29341,.F.) ;
#42500 = ORIENTED_EDGE('',*,*,#29557,.T.) ;
#42501 = ORIENTED_EDGE('',*,*,#28086,.T.) ;
#42502 = ORIENTED_EDGE('',*,*,#29571,.T.) ;
#42503 = ORIENTED_EDGE('',*,*,#29339,.F.) ;
#42504 = ORIENTED_EDGE('',*,*,#27788,.F.) ;
#42505 = ORIENTED_EDGE('',*,*,#29348,.F.) ;
#42506 = ORIENTED_EDGE('',*,*,#29572,.F.) ;
#42507 = ORIENTED_EDGE('',*,*,#28063,.T.) ;
#42508 = ORIENTED_EDGE('',*,*,#27778,.T.) ;
#42509 = ORIENTED_EDGE('',*,*,#27786,.T.) ;
#42510 = ORIENTED_EDGE('',*,*,#29350,.F.) ;
#42511 = ORIENTED_EDGE('',*,*,#29559,.T.) ;
#42512 = ORIENTED_EDGE('',*,*,#28064,.T.) ;
#42513 = ORIENTED_EDGE('',*,*,#29572,.T.) ;
#42514 = ORIENTED_EDGE('',*,*,#29334,.F.) ;
#42515 = ORIENTED_EDGE('',*,*,#29556,.T.) ;
#42516 = ORIENTED_EDGE('',*,*,#29345,.F.) ;
#42517 = ORIENTED_EDGE('',*,*,#29342,.F.) ;
#42518 = ORIENTED_EDGE('',*,*,#29285,.F.) ;
#42519 = ORIENTED_EDGE('',*,*,#27515,.F.) ;
#42520 = ORIENTED_EDGE('',*,*,#27519,.F.) ;
#42521 = ORIENTED_EDGE('',*,*,#29338,.F.) ;
#42522 = ORIENTED_EDGE('',*,*,#29328,.F.) ;
#42523 = ORIENTED_EDGE('',*,*,#29361,.F.) ;
#42524 = ORIENTED_EDGE('',*,*,#28091,.T.) ;
#42525 = ORIENTED_EDGE('',*,*,#29573,.F.) ;
#42526 = ORIENTED_EDGE('',*,*,#27521,.F.) ;
#42527 = ORIENTED_EDGE('',*,*,#27526,.F.) ;
#42528 = ORIENTED_EDGE('',*,*,#27522,.F.) ;
#42529 = ORIENTED_EDGE('',*,*,#29573,.T.) ;
#42530 = ORIENTED_EDGE('',*,*,#28090,.T.) ;
#42531 = ORIENTED_EDGE('',*,*,#29553,.T.) ;
#42532 = ORIENTED_EDGE('',*,*,#29337,.F.) ;
#42533 = ORIENTED_EDGE('',*,*,#28635,.F.) ;
#42534 = ORIENTED_EDGE('',*,*,#29574,.T.) ;
#42535 = ORIENTED_EDGE('',*,*,#29390,.F.) ;
#42536 = ORIENTED_EDGE('',*,*,#29574,.F.) ;
#42537 = ORIENTED_EDGE('',*,*,#29575,.T.) ;
#42538 = ORIENTED_EDGE('',*,*,#29524,.T.) ;
#42539 = ORIENTED_EDGE('',*,*,#29522,.F.) ;
#42540 = ORIENTED_EDGE('',*,*,#28069,.T.) ;
#42541 = ORIENTED_EDGE('',*,*,#29283,.F.) ;
#42542 = ORIENTED_EDGE('',*,*,#29576,.T.) ;
#42543 = ORIENTED_EDGE('',*,*,#28066,.F.) ;
#42544 = ORIENTED_EDGE('',*,*,#29558,.T.) ;
#42545 = ORIENTED_EDGE('',*,*,#29304,.F.) ;
#42546 = ORIENTED_EDGE('',*,*,#29363,.F.) ;
#42547 = ORIENTED_EDGE('',*,*,#28083,.F.) ;
#42548 = ORIENTED_EDGE('',*,*,#29577,.T.) ;
#42549 = ORIENTED_EDGE('',*,*,#29307,.F.) ;
#42550 = ORIENTED_EDGE('',*,*,#29577,.F.) ;
#42551 = ORIENTED_EDGE('',*,*,#28082,.F.) ;
#42552 = ORIENTED_EDGE('',*,*,#29393,.F.) ;
#42553 = ORIENTED_EDGE('',*,*,#29523,.F.) ;
#42554 = ORIENTED_EDGE('',*,*,#29575,.F.) ;
#42555 = ORIENTED_EDGE('',*,*,#28068,.F.) ;
#42556 = ORIENTED_EDGE('',*,*,#29578,.T.) ;
#42557 = ORIENTED_EDGE('',*,*,#29291,.F.) ;
#42558 = ORIENTED_EDGE('',*,*,#29286,.F.) ;
#42559 = ORIENTED_EDGE('',*,*,#29308,.F.) ;
#42560 = ORIENTED_EDGE('',*,*,#29302,.F.) ;
#42561 = ORIENTED_EDGE('',*,*,#29292,.F.) ;
#42562 = ORIENTED_EDGE('',*,*,#29578,.F.) ;
#42563 = ORIENTED_EDGE('',*,*,#28067,.F.) ;
#42564 = ORIENTED_EDGE('',*,*,#29576,.F.) ;
#42565 = ORIENTED_EDGE('',*,*,#29314,.F.) ;
#42566 = ORIENTED_EDGE('',*,*,#29579,.F.) ;
#42567 = ORIENTED_EDGE('',*,*,#28093,.F.) ;
#42568 = ORIENTED_EDGE('',*,*,#29360,.F.) ;
#42569 = ORIENTED_EDGE('',*,*,#29321,.F.) ;
#42570 = ORIENTED_EDGE('',*,*,#29355,.F.) ;
#42571 = ORIENTED_EDGE('',*,*,#28094,.F.) ;
#42572 = ORIENTED_EDGE('',*,*,#29579,.T.) ;
#42573 = ORIENTED_EDGE('',*,*,#29313,.F.) ;
#42574 = ORIENTED_EDGE('',*,*,#29309,.F.) ;
#42575 = ORIENTED_EDGE('',*,*,#29322,.F.) ;
#42576 = ORIENTED_EDGE('',*,*,#29316,.F.) ;
#42577 = ORIENTED_EDGE('',*,*,#28369,.T.) ;
#42578 = ORIENTED_EDGE('',*,*,#29580,.F.) ;
#42579 = ORIENTED_EDGE('',*,*,#28423,.F.) ;
#42580 = ORIENTED_EDGE('',*,*,#28434,.F.) ;
#42581 = ORIENTED_EDGE('',*,*,#29272,.F.) ;
#42582 = ORIENTED_EDGE('',*,*,#29273,.F.) ;
#42583 = ORIENTED_EDGE('',*,*,#28379,.T.) ;
#42584 = ORIENTED_EDGE('',*,*,#29581,.F.) ;
#42585 = ORIENTED_EDGE('',*,*,#28370,.F.) ;
#42586 = ORIENTED_EDGE('',*,*,#29581,.T.) ;
#42587 = ORIENTED_EDGE('',*,*,#28381,.F.) ;
#42588 = ORIENTED_EDGE('',*,*,#28359,.F.) ;
#42589 = ORIENTED_EDGE('',*,*,#28357,.F.) ;
#42590 = ORIENTED_EDGE('',*,*,#28407,.F.) ;
#42591 = ORIENTED_EDGE('',*,*,#29274,.F.) ;
#42592 = ORIENTED_EDGE('',*,*,#28440,.T.) ;
#42593 = ORIENTED_EDGE('',*,*,#28417,.F.) ;
#42594 = ORIENTED_EDGE('',*,*,#29244,.T.) ;
#42595 = ORIENTED_EDGE('',*,*,#29246,.T.) ;
#42596 = ORIENTED_EDGE('',*,*,#29384,.T.) ;
#42597 = ORIENTED_EDGE('',*,*,#29386,.T.) ;
#42598 = ORIENTED_EDGE('',*,*,#29387,.T.) ;
#42599 = ORIENTED_EDGE('',*,*,#29249,.T.) ;
#42600 = ORIENTED_EDGE('',*,*,#29359,.T.) ;
#42601 = ORIENTED_EDGE('',*,*,#28504,.T.) ;
#42602 = ORIENTED_EDGE('',*,*,#29256,.T.) ;
#42603 = ORIENTED_EDGE('',*,*,#27849,.T.) ;
#42604 = ORIENTED_EDGE('',*,*,#28361,.F.) ;
#42605 = ORIENTED_EDGE('',*,*,#28424,.F.) ;
#42606 = ORIENTED_EDGE('',*,*,#29580,.T.) ;
#42607 = ORIENTED_EDGE('',*,*,#28371,.F.) ;
#42608 = ORIENTED_EDGE('',*,*,#29582,.T.) ;
#42609 = ORIENTED_EDGE('',*,*,#29583,.F.) ;
#42610 = ORIENTED_EDGE('',*,*,#29584,.F.) ;
#42611 = ORIENTED_EDGE('',*,*,#29585,.F.) ;
#42612 = ORIENTED_EDGE('',*,*,#29586,.T.) ;
#42613 = ORIENTED_EDGE('',*,*,#29585,.T.) ;
#42614 = ORIENTED_EDGE('',*,*,#29587,.F.) ;
#42615 = ORIENTED_EDGE('',*,*,#29588,.F.) ;
#42616 = ORIENTED_EDGE('',*,*,#29589,.T.) ;
#42617 = ORIENTED_EDGE('',*,*,#29588,.T.) ;
#42618 = ORIENTED_EDGE('',*,*,#29590,.F.) ;
#42619 = ORIENTED_EDGE('',*,*,#29591,.F.) ;
#42620 = ORIENTED_EDGE('',*,*,#29592,.T.) ;
#42621 = ORIENTED_EDGE('',*,*,#29591,.T.) ;
#42622 = ORIENTED_EDGE('',*,*,#29593,.F.) ;
#42623 = ORIENTED_EDGE('',*,*,#29594,.F.) ;
#42624 = ORIENTED_EDGE('',*,*,#29595,.T.) ;
#42625 = ORIENTED_EDGE('',*,*,#29594,.T.) ;
#42626 = ORIENTED_EDGE('',*,*,#29596,.F.) ;
#42627 = ORIENTED_EDGE('',*,*,#29597,.F.) ;
#42628 = ORIENTED_EDGE('',*,*,#29598,.T.) ;
#42629 = ORIENTED_EDGE('',*,*,#29597,.T.) ;
#42630 = ORIENTED_EDGE('',*,*,#29599,.F.) ;
#42631 = ORIENTED_EDGE('',*,*,#29600,.F.) ;
#42632 = ORIENTED_EDGE('',*,*,#29601,.T.) ;
#42633 = ORIENTED_EDGE('',*,*,#29600,.T.) ;
#42634 = ORIENTED_EDGE('',*,*,#29602,.F.) ;
#42635 = ORIENTED_EDGE('',*,*,#29603,.F.) ;
#42636 = ORIENTED_EDGE('',*,*,#29602,.T.) ;
#42637 = ORIENTED_EDGE('',*,*,#29599,.T.) ;
#42638 = ORIENTED_EDGE('',*,*,#29596,.T.) ;
#42639 = ORIENTED_EDGE('',*,*,#29593,.T.) ;
#42640 = ORIENTED_EDGE('',*,*,#29590,.T.) ;
#42641 = ORIENTED_EDGE('',*,*,#29587,.T.) ;
#42642 = ORIENTED_EDGE('',*,*,#29584,.T.) ;
#42643 = ORIENTED_EDGE('',*,*,#29604,.F.) ;
#42644 = ORIENTED_EDGE('',*,*,#29601,.F.) ;
#42645 = ORIENTED_EDGE('',*,*,#29605,.F.) ;
#42646 = ORIENTED_EDGE('',*,*,#29582,.F.) ;
#42647 = ORIENTED_EDGE('',*,*,#29586,.F.) ;
#42648 = ORIENTED_EDGE('',*,*,#29589,.F.) ;
#42649 = ORIENTED_EDGE('',*,*,#29592,.F.) ;
#42650 = ORIENTED_EDGE('',*,*,#29595,.F.) ;
#42651 = ORIENTED_EDGE('',*,*,#29598,.F.) ;
#42652 = ORIENTED_EDGE('',*,*,#29606,.T.) ;
#42653 = ORIENTED_EDGE('',*,*,#29607,.T.) ;
#42654 = ORIENTED_EDGE('',*,*,#29608,.F.) ;
#42655 = ORIENTED_EDGE('',*,*,#29609,.F.) ;
#42656 = ORIENTED_EDGE('',*,*,#29605,.T.) ;
#42657 = ORIENTED_EDGE('',*,*,#29610,.F.) ;
#42658 = ORIENTED_EDGE('',*,*,#29611,.T.) ;
#42659 = ORIENTED_EDGE('',*,*,#29609,.T.) ;
#42660 = ORIENTED_EDGE('',*,*,#29612,.F.) ;
#42661 = ORIENTED_EDGE('',*,*,#29613,.F.) ;
#42662 = ORIENTED_EDGE('',*,*,#29604,.T.) ;
#42663 = ORIENTED_EDGE('',*,*,#29583,.T.) ;
#42664 = ORIENTED_EDGE('',*,*,#29614,.T.) ;
#42665 = ORIENTED_EDGE('',*,*,#29610,.T.) ;
#42666 = ORIENTED_EDGE('',*,*,#29603,.T.) ;
#42667 = ORIENTED_EDGE('',*,*,#29613,.T.) ;
#42668 = ORIENTED_EDGE('',*,*,#29615,.F.) ;
#42669 = ORIENTED_EDGE('',*,*,#29616,.F.) ;
#42670 = ORIENTED_EDGE('',*,*,#29617,.T.) ;
#42671 = ORIENTED_EDGE('',*,*,#29616,.T.) ;
#42672 = ORIENTED_EDGE('',*,*,#29618,.F.) ;
#42673 = ORIENTED_EDGE('',*,*,#29607,.F.) ;
#42674 = ORIENTED_EDGE('',*,*,#29618,.T.) ;
#42675 = ORIENTED_EDGE('',*,*,#29615,.T.) ;
#42676 = ORIENTED_EDGE('',*,*,#29612,.T.) ;
#42677 = ORIENTED_EDGE('',*,*,#29608,.T.) ;
#42678 = ORIENTED_EDGE('',*,*,#29617,.F.) ;
#42679 = ORIENTED_EDGE('',*,*,#29606,.F.) ;
#42680 = ORIENTED_EDGE('',*,*,#29611,.F.) ;
#42681 = ORIENTED_EDGE('',*,*,#29614,.F.) ;
#42682 = ORIENTED_EDGE('',*,*,#29619,.F.) ;
#42683 = ORIENTED_EDGE('',*,*,#29620,.F.) ;
#42684 = ORIENTED_EDGE('',*,*,#29621,.F.) ;
#42685 = ORIENTED_EDGE('',*,*,#29622,.T.) ;
#42686 = ORIENTED_EDGE('',*,*,#29623,.F.) ;
#42687 = ORIENTED_EDGE('',*,*,#29624,.F.) ;
#42688 = ORIENTED_EDGE('',*,*,#29619,.T.) ;
#42689 = ORIENTED_EDGE('',*,*,#29625,.T.) ;
#42690 = ORIENTED_EDGE('',*,*,#29626,.F.) ;
#42691 = ORIENTED_EDGE('',*,*,#29627,.F.) ;
#42692 = ORIENTED_EDGE('',*,*,#29628,.F.) ;
#42693 = ORIENTED_EDGE('',*,*,#29623,.T.) ;
#42694 = ORIENTED_EDGE('',*,*,#29629,.T.) ;
#42695 = ORIENTED_EDGE('',*,*,#29630,.T.) ;
#42696 = ORIENTED_EDGE('',*,*,#29631,.F.) ;
#42697 = ORIENTED_EDGE('',*,*,#29632,.F.) ;
#42698 = ORIENTED_EDGE('',*,*,#29633,.F.) ;
#42699 = ORIENTED_EDGE('',*,*,#29626,.T.) ;
#42700 = ORIENTED_EDGE('',*,*,#29634,.T.) ;
#42701 = ORIENTED_EDGE('',*,*,#29635,.T.) ;
#42702 = ORIENTED_EDGE('',*,*,#29636,.T.) ;
#42703 = ORIENTED_EDGE('',*,*,#29637,.T.) ;
#42704 = ORIENTED_EDGE('',*,*,#29638,.T.) ;
#42705 = ORIENTED_EDGE('',*,*,#29639,.T.) ;
#42706 = ORIENTED_EDGE('',*,*,#29640,.T.) ;
#42707 = ORIENTED_EDGE('',*,*,#29641,.T.) ;
#42708 = ORIENTED_EDGE('',*,*,#29642,.F.) ;
#42709 = ORIENTED_EDGE('',*,*,#29643,.T.) ;
#42710 = ORIENTED_EDGE('',*,*,#29644,.T.) ;
#42711 = ORIENTED_EDGE('',*,*,#29645,.T.) ;
#42712 = ORIENTED_EDGE('',*,*,#29646,.T.) ;
#42713 = ORIENTED_EDGE('',*,*,#29647,.T.) ;
#42714 = ORIENTED_EDGE('',*,*,#29648,.T.) ;
#42715 = ORIENTED_EDGE('',*,*,#29649,.F.) ;
#42716 = ORIENTED_EDGE('',*,*,#29631,.T.) ;
#42717 = ORIENTED_EDGE('',*,*,#29650,.T.) ;
#42718 = ORIENTED_EDGE('',*,*,#29651,.F.) ;
#42719 = ORIENTED_EDGE('',*,*,#29652,.F.) ;
#42720 = ORIENTED_EDGE('',*,*,#29653,.F.) ;
#42721 = ORIENTED_EDGE('',*,*,#29636,.F.) ;
#42722 = ORIENTED_EDGE('',*,*,#29654,.T.) ;
#42723 = ORIENTED_EDGE('',*,*,#29651,.T.) ;
#42724 = ORIENTED_EDGE('',*,*,#29655,.T.) ;
#42725 = ORIENTED_EDGE('',*,*,#29656,.T.) ;
#42726 = ORIENTED_EDGE('',*,*,#29654,.F.) ;
#42727 = ORIENTED_EDGE('',*,*,#29648,.F.) ;
#42728 = ORIENTED_EDGE('',*,*,#29647,.F.) ;
#42729 = ORIENTED_EDGE('',*,*,#29646,.F.) ;
#42730 = ORIENTED_EDGE('',*,*,#29645,.F.) ;
#42731 = ORIENTED_EDGE('',*,*,#29644,.F.) ;
#42732 = ORIENTED_EDGE('',*,*,#29643,.F.) ;
#42733 = ORIENTED_EDGE('',*,*,#29657,.F.) ;
#42734 = ORIENTED_EDGE('',*,*,#29658,.T.) ;
#42735 = ORIENTED_EDGE('',*,*,#29620,.T.) ;
#42736 = ORIENTED_EDGE('',*,*,#29624,.T.) ;
#42737 = ORIENTED_EDGE('',*,*,#29628,.T.) ;
#42738 = ORIENTED_EDGE('',*,*,#29627,.T.) ;
#42739 = ORIENTED_EDGE('',*,*,#29633,.T.) ;
#42740 = ORIENTED_EDGE('',*,*,#29632,.T.) ;
#42741 = ORIENTED_EDGE('',*,*,#29653,.T.) ;
#42742 = ORIENTED_EDGE('',*,*,#29652,.T.) ;
#42743 = ORIENTED_EDGE('',*,*,#29656,.F.) ;
#42744 = ORIENTED_EDGE('',*,*,#29655,.F.) ;
#42745 = ORIENTED_EDGE('',*,*,#29650,.F.) ;
#42746 = ORIENTED_EDGE('',*,*,#29635,.F.) ;
#42747 = ORIENTED_EDGE('',*,*,#29634,.F.) ;
#42748 = ORIENTED_EDGE('',*,*,#29630,.F.) ;
#42749 = ORIENTED_EDGE('',*,*,#29629,.F.) ;
#42750 = ORIENTED_EDGE('',*,*,#29625,.F.) ;
#42751 = ORIENTED_EDGE('',*,*,#29622,.F.) ;
#42752 = ORIENTED_EDGE('',*,*,#29659,.F.) ;
#42753 = ORIENTED_EDGE('',*,*,#29641,.F.) ;
#42754 = ORIENTED_EDGE('',*,*,#29640,.F.) ;
#42755 = ORIENTED_EDGE('',*,*,#29639,.F.) ;
#42756 = ORIENTED_EDGE('',*,*,#29638,.F.) ;
#42757 = ORIENTED_EDGE('',*,*,#29637,.F.) ;
#42758 = ORIENTED_EDGE('',*,*,#29657,.T.) ;
#42759 = ORIENTED_EDGE('',*,*,#29642,.T.) ;
#42760 = ORIENTED_EDGE('',*,*,#29659,.T.) ;
#42761 = ORIENTED_EDGE('',*,*,#29621,.T.) ;
#42762 = ORIENTED_EDGE('',*,*,#29658,.F.) ;
#42763 = ORIENTED_EDGE('',*,*,#29649,.T.) ;
#42764 = ORIENTED_EDGE('',*,*,#29660,.F.) ;
#42765 = ORIENTED_EDGE('',*,*,#29661,.T.) ;
#42766 = ORIENTED_EDGE('',*,*,#29662,.T.) ;
#42767 = ORIENTED_EDGE('',*,*,#29661,.F.) ;
#42768 = ORIENTED_EDGE('',*,*,#29663,.F.) ;
#42769 = ORIENTED_EDGE('',*,*,#29662,.F.) ;
#42770 = ORIENTED_EDGE('',*,*,#29664,.T.) ;
#42771 = ORIENTED_EDGE('',*,*,#29665,.T.) ;
#42772 = ORIENTED_EDGE('',*,*,#29666,.F.) ;
#42773 = ORIENTED_EDGE('',*,*,#29665,.F.) ;
#42774 = ORIENTED_EDGE('',*,*,#29667,.F.) ;
#42775 = ORIENTED_EDGE('',*,*,#29664,.F.) ;
#42776 = ORIENTED_EDGE('',*,*,#29666,.T.) ;
#42777 = ORIENTED_EDGE('',*,*,#29668,.T.) ;
#42778 = ORIENTED_EDGE('',*,*,#29660,.T.) ;
#42779 = ORIENTED_EDGE('',*,*,#29669,.T.) ;
#42780 = ORIENTED_EDGE('',*,*,#29670,.T.) ;
#42781 = ORIENTED_EDGE('',*,*,#29671,.T.) ;
#42782 = ORIENTED_EDGE('',*,*,#29672,.T.) ;
#42783 = ORIENTED_EDGE('',*,*,#29670,.F.) ;
#42784 = ORIENTED_EDGE('',*,*,#29663,.T.) ;
#42785 = ORIENTED_EDGE('',*,*,#29673,.T.) ;
#42786 = ORIENTED_EDGE('',*,*,#29674,.T.) ;
#42787 = ORIENTED_EDGE('',*,*,#29675,.T.) ;
#42788 = ORIENTED_EDGE('',*,*,#29673,.F.) ;
#42789 = ORIENTED_EDGE('',*,*,#29667,.T.) ;
#42790 = ORIENTED_EDGE('',*,*,#29676,.F.) ;
#42791 = ORIENTED_EDGE('',*,*,#29677,.T.) ;
#42792 = ORIENTED_EDGE('',*,*,#29678,.T.) ;
#42793 = ORIENTED_EDGE('',*,*,#29679,.F.) ;
#42794 = ORIENTED_EDGE('',*,*,#29680,.T.) ;
#42795 = ORIENTED_EDGE('',*,*,#29681,.T.) ;
#42796 = ORIENTED_EDGE('',*,*,#29682,.T.) ;
#42797 = ORIENTED_EDGE('',*,*,#29677,.F.) ;
#42798 = ORIENTED_EDGE('',*,*,#29683,.T.) ;
#42799 = ORIENTED_EDGE('',*,*,#29684,.T.) ;
#42800 = ORIENTED_EDGE('',*,*,#29685,.T.) ;
#42801 = ORIENTED_EDGE('',*,*,#29681,.F.) ;
#42802 = ORIENTED_EDGE('',*,*,#29686,.T.) ;
#42803 = ORIENTED_EDGE('',*,*,#29687,.T.) ;
#42804 = ORIENTED_EDGE('',*,*,#29688,.T.) ;
#42805 = ORIENTED_EDGE('',*,*,#29684,.F.) ;
#42806 = ORIENTED_EDGE('',*,*,#29689,.F.) ;
#42807 = ORIENTED_EDGE('',*,*,#29690,.T.) ;
#42808 = ORIENTED_EDGE('',*,*,#29691,.T.) ;
#42809 = ORIENTED_EDGE('',*,*,#29687,.F.) ;
#42810 = ORIENTED_EDGE('',*,*,#29692,.T.) ;
#42811 = ORIENTED_EDGE('',*,*,#29693,.T.) ;
#42812 = ORIENTED_EDGE('',*,*,#29694,.T.) ;
#42813 = ORIENTED_EDGE('',*,*,#29690,.F.) ;
#42814 = ORIENTED_EDGE('',*,*,#29695,.T.) ;
#42815 = ORIENTED_EDGE('',*,*,#29696,.T.) ;
#42816 = ORIENTED_EDGE('',*,*,#29697,.T.) ;
#42817 = ORIENTED_EDGE('',*,*,#29693,.F.) ;
#42818 = ORIENTED_EDGE('',*,*,#29698,.T.) ;
#42819 = ORIENTED_EDGE('',*,*,#29699,.T.) ;
#42820 = ORIENTED_EDGE('',*,*,#29700,.T.) ;
#42821 = ORIENTED_EDGE('',*,*,#29696,.F.) ;
#42822 = ORIENTED_EDGE('',*,*,#29701,.F.) ;
#42823 = ORIENTED_EDGE('',*,*,#29702,.T.) ;
#42824 = ORIENTED_EDGE('',*,*,#29703,.T.) ;
#42825 = ORIENTED_EDGE('',*,*,#29699,.F.) ;
#42826 = ORIENTED_EDGE('',*,*,#29704,.T.) ;
#42827 = ORIENTED_EDGE('',*,*,#29705,.T.) ;
#42828 = ORIENTED_EDGE('',*,*,#29706,.T.) ;
#42829 = ORIENTED_EDGE('',*,*,#29702,.F.) ;
#42830 = ORIENTED_EDGE('',*,*,#29707,.T.) ;
#42831 = ORIENTED_EDGE('',*,*,#29708,.T.) ;
#42832 = ORIENTED_EDGE('',*,*,#29709,.T.) ;
#42833 = ORIENTED_EDGE('',*,*,#29705,.F.) ;
#42834 = ORIENTED_EDGE('',*,*,#29710,.T.) ;
#42835 = ORIENTED_EDGE('',*,*,#29711,.T.) ;
#42836 = ORIENTED_EDGE('',*,*,#29712,.T.) ;
#42837 = ORIENTED_EDGE('',*,*,#29708,.F.) ;
#42838 = ORIENTED_EDGE('',*,*,#29713,.F.) ;
#42839 = ORIENTED_EDGE('',*,*,#29714,.T.) ;
#42840 = ORIENTED_EDGE('',*,*,#29715,.T.) ;
#42841 = ORIENTED_EDGE('',*,*,#29711,.F.) ;
#42842 = ORIENTED_EDGE('',*,*,#29716,.T.) ;
#42843 = ORIENTED_EDGE('',*,*,#29717,.T.) ;
#42844 = ORIENTED_EDGE('',*,*,#29718,.T.) ;
#42845 = ORIENTED_EDGE('',*,*,#29714,.F.) ;
#42846 = ORIENTED_EDGE('',*,*,#29719,.T.) ;
#42847 = ORIENTED_EDGE('',*,*,#29720,.T.) ;
#42848 = ORIENTED_EDGE('',*,*,#29721,.T.) ;
#42849 = ORIENTED_EDGE('',*,*,#29717,.F.) ;
#42850 = ORIENTED_EDGE('',*,*,#29722,.T.) ;
#42851 = ORIENTED_EDGE('',*,*,#29723,.T.) ;
#42852 = ORIENTED_EDGE('',*,*,#29724,.T.) ;
#42853 = ORIENTED_EDGE('',*,*,#29720,.F.) ;
#42854 = ORIENTED_EDGE('',*,*,#29725,.F.) ;
#42855 = ORIENTED_EDGE('',*,*,#29726,.T.) ;
#42856 = ORIENTED_EDGE('',*,*,#29727,.T.) ;
#42857 = ORIENTED_EDGE('',*,*,#29723,.F.) ;
#42858 = ORIENTED_EDGE('',*,*,#29728,.T.) ;
#42859 = ORIENTED_EDGE('',*,*,#29729,.T.) ;
#42860 = ORIENTED_EDGE('',*,*,#29730,.T.) ;
#42861 = ORIENTED_EDGE('',*,*,#29726,.F.) ;
#42862 = ORIENTED_EDGE('',*,*,#29731,.T.) ;
#42863 = ORIENTED_EDGE('',*,*,#29732,.T.) ;
#42864 = ORIENTED_EDGE('',*,*,#29733,.T.) ;
#42865 = ORIENTED_EDGE('',*,*,#29729,.F.) ;
#42866 = ORIENTED_EDGE('',*,*,#29734,.T.) ;
#42867 = ORIENTED_EDGE('',*,*,#29735,.T.) ;
#42868 = ORIENTED_EDGE('',*,*,#29736,.T.) ;
#42869 = ORIENTED_EDGE('',*,*,#29732,.F.) ;
#42870 = ORIENTED_EDGE('',*,*,#29737,.F.) ;
#42871 = ORIENTED_EDGE('',*,*,#29738,.T.) ;
#42872 = ORIENTED_EDGE('',*,*,#29739,.T.) ;
#42873 = ORIENTED_EDGE('',*,*,#29735,.F.) ;
#42874 = ORIENTED_EDGE('',*,*,#29740,.T.) ;
#42875 = ORIENTED_EDGE('',*,*,#29741,.T.) ;
#42876 = ORIENTED_EDGE('',*,*,#29742,.T.) ;
#42877 = ORIENTED_EDGE('',*,*,#29738,.F.) ;
#42878 = ORIENTED_EDGE('',*,*,#29743,.T.) ;
#42879 = ORIENTED_EDGE('',*,*,#29744,.T.) ;
#42880 = ORIENTED_EDGE('',*,*,#29745,.T.) ;
#42881 = ORIENTED_EDGE('',*,*,#29741,.F.) ;
#42882 = ORIENTED_EDGE('',*,*,#29746,.T.) ;
#42883 = ORIENTED_EDGE('',*,*,#29747,.T.) ;
#42884 = ORIENTED_EDGE('',*,*,#29748,.T.) ;
#42885 = ORIENTED_EDGE('',*,*,#29744,.F.) ;
#42886 = ORIENTED_EDGE('',*,*,#29749,.F.) ;
#42887 = ORIENTED_EDGE('',*,*,#29750,.T.) ;
#42888 = ORIENTED_EDGE('',*,*,#29751,.T.) ;
#42889 = ORIENTED_EDGE('',*,*,#29747,.F.) ;
#42890 = ORIENTED_EDGE('',*,*,#29752,.T.) ;
#42891 = ORIENTED_EDGE('',*,*,#29753,.T.) ;
#42892 = ORIENTED_EDGE('',*,*,#29754,.T.) ;
#42893 = ORIENTED_EDGE('',*,*,#29750,.F.) ;
#42894 = ORIENTED_EDGE('',*,*,#29755,.T.) ;
#42895 = ORIENTED_EDGE('',*,*,#29756,.T.) ;
#42896 = ORIENTED_EDGE('',*,*,#29757,.T.) ;
#42897 = ORIENTED_EDGE('',*,*,#29753,.F.) ;
#42898 = ORIENTED_EDGE('',*,*,#29758,.T.) ;
#42899 = ORIENTED_EDGE('',*,*,#29759,.T.) ;
#42900 = ORIENTED_EDGE('',*,*,#29760,.T.) ;
#42901 = ORIENTED_EDGE('',*,*,#29756,.F.) ;
#42902 = ORIENTED_EDGE('',*,*,#29761,.F.) ;
#42903 = ORIENTED_EDGE('',*,*,#29762,.T.) ;
#42904 = ORIENTED_EDGE('',*,*,#29763,.T.) ;
#42905 = ORIENTED_EDGE('',*,*,#29759,.F.) ;
#42906 = ORIENTED_EDGE('',*,*,#29764,.T.) ;
#42907 = ORIENTED_EDGE('',*,*,#29765,.T.) ;
#42908 = ORIENTED_EDGE('',*,*,#29766,.T.) ;
#42909 = ORIENTED_EDGE('',*,*,#29762,.F.) ;
#42910 = ORIENTED_EDGE('',*,*,#29767,.T.) ;
#42911 = ORIENTED_EDGE('',*,*,#29768,.T.) ;
#42912 = ORIENTED_EDGE('',*,*,#29769,.T.) ;
#42913 = ORIENTED_EDGE('',*,*,#29765,.F.) ;
#42914 = ORIENTED_EDGE('',*,*,#29770,.T.) ;
#42915 = ORIENTED_EDGE('',*,*,#29771,.T.) ;
#42916 = ORIENTED_EDGE('',*,*,#29772,.T.) ;
#42917 = ORIENTED_EDGE('',*,*,#29768,.F.) ;
#42918 = ORIENTED_EDGE('',*,*,#29773,.F.) ;
#42919 = ORIENTED_EDGE('',*,*,#29774,.T.) ;
#42920 = ORIENTED_EDGE('',*,*,#29775,.T.) ;
#42921 = ORIENTED_EDGE('',*,*,#29771,.F.) ;
#42922 = ORIENTED_EDGE('',*,*,#29776,.T.) ;
#42923 = ORIENTED_EDGE('',*,*,#29777,.T.) ;
#42924 = ORIENTED_EDGE('',*,*,#29778,.T.) ;
#42925 = ORIENTED_EDGE('',*,*,#29774,.F.) ;
#42926 = ORIENTED_EDGE('',*,*,#29779,.T.) ;
#42927 = ORIENTED_EDGE('',*,*,#29780,.T.) ;
#42928 = ORIENTED_EDGE('',*,*,#29781,.T.) ;
#42929 = ORIENTED_EDGE('',*,*,#29777,.F.) ;
#42930 = ORIENTED_EDGE('',*,*,#29782,.T.) ;
#42931 = ORIENTED_EDGE('',*,*,#29783,.T.) ;
#42932 = ORIENTED_EDGE('',*,*,#29784,.T.) ;
#42933 = ORIENTED_EDGE('',*,*,#29780,.F.) ;
#42934 = ORIENTED_EDGE('',*,*,#29785,.F.) ;
#42935 = ORIENTED_EDGE('',*,*,#29786,.T.) ;
#42936 = ORIENTED_EDGE('',*,*,#29787,.T.) ;
#42937 = ORIENTED_EDGE('',*,*,#29783,.F.) ;
#42938 = ORIENTED_EDGE('',*,*,#29788,.T.) ;
#42939 = ORIENTED_EDGE('',*,*,#29789,.T.) ;
#42940 = ORIENTED_EDGE('',*,*,#29790,.T.) ;
#42941 = ORIENTED_EDGE('',*,*,#29786,.F.) ;
#42942 = ORIENTED_EDGE('',*,*,#29791,.T.) ;
#42943 = ORIENTED_EDGE('',*,*,#29792,.T.) ;
#42944 = ORIENTED_EDGE('',*,*,#29793,.T.) ;
#42945 = ORIENTED_EDGE('',*,*,#29789,.F.) ;
#42946 = ORIENTED_EDGE('',*,*,#29794,.T.) ;
#42947 = ORIENTED_EDGE('',*,*,#29795,.T.) ;
#42948 = ORIENTED_EDGE('',*,*,#29796,.T.) ;
#42949 = ORIENTED_EDGE('',*,*,#29792,.F.) ;
#42950 = ORIENTED_EDGE('',*,*,#29797,.F.) ;
#42951 = ORIENTED_EDGE('',*,*,#29798,.T.) ;
#42952 = ORIENTED_EDGE('',*,*,#29799,.T.) ;
#42953 = ORIENTED_EDGE('',*,*,#29795,.F.) ;
#42954 = ORIENTED_EDGE('',*,*,#29800,.T.) ;
#42955 = ORIENTED_EDGE('',*,*,#29798,.F.) ;
#42956 = ORIENTED_EDGE('',*,*,#29801,.T.) ;
#42957 = ORIENTED_EDGE('',*,*,#29802,.T.) ;
#42958 = ORIENTED_EDGE('',*,*,#29803,.T.) ;
#42959 = ORIENTED_EDGE('',*,*,#29802,.F.) ;
#42960 = ORIENTED_EDGE('',*,*,#29804,.T.) ;
#42961 = ORIENTED_EDGE('',*,*,#29805,.T.) ;
#42962 = ORIENTED_EDGE('',*,*,#29806,.T.) ;
#42963 = ORIENTED_EDGE('',*,*,#29805,.F.) ;
#42964 = ORIENTED_EDGE('',*,*,#29807,.T.) ;
#42965 = ORIENTED_EDGE('',*,*,#29808,.T.) ;
#42966 = ORIENTED_EDGE('',*,*,#29809,.T.) ;
#42967 = ORIENTED_EDGE('',*,*,#29808,.F.) ;
#42968 = ORIENTED_EDGE('',*,*,#29810,.F.) ;
#42969 = ORIENTED_EDGE('',*,*,#29811,.T.) ;
#42970 = ORIENTED_EDGE('',*,*,#29812,.T.) ;
#42971 = ORIENTED_EDGE('',*,*,#29811,.F.) ;
#42972 = ORIENTED_EDGE('',*,*,#29813,.T.) ;
#42973 = ORIENTED_EDGE('',*,*,#29814,.T.) ;
#42974 = ORIENTED_EDGE('',*,*,#29815,.T.) ;
#42975 = ORIENTED_EDGE('',*,*,#29814,.F.) ;
#42976 = ORIENTED_EDGE('',*,*,#29816,.T.) ;
#42977 = ORIENTED_EDGE('',*,*,#29817,.T.) ;
#42978 = ORIENTED_EDGE('',*,*,#29818,.T.) ;
#42979 = ORIENTED_EDGE('',*,*,#29817,.F.) ;
#42980 = ORIENTED_EDGE('',*,*,#29819,.T.) ;
#42981 = ORIENTED_EDGE('',*,*,#29820,.T.) ;
#42982 = ORIENTED_EDGE('',*,*,#29821,.T.) ;
#42983 = ORIENTED_EDGE('',*,*,#29820,.F.) ;
#42984 = ORIENTED_EDGE('',*,*,#29822,.F.) ;
#42985 = ORIENTED_EDGE('',*,*,#29823,.T.) ;
#42986 = ORIENTED_EDGE('',*,*,#29824,.T.) ;
#42987 = ORIENTED_EDGE('',*,*,#29823,.F.) ;
#42988 = ORIENTED_EDGE('',*,*,#29825,.T.) ;
#42989 = ORIENTED_EDGE('',*,*,#29826,.T.) ;
#42990 = ORIENTED_EDGE('',*,*,#29827,.T.) ;
#42991 = ORIENTED_EDGE('',*,*,#29826,.F.) ;
#42992 = ORIENTED_EDGE('',*,*,#29828,.T.) ;
#42993 = ORIENTED_EDGE('',*,*,#29829,.T.) ;
#42994 = ORIENTED_EDGE('',*,*,#29830,.T.) ;
#42995 = ORIENTED_EDGE('',*,*,#29829,.F.) ;
#42996 = ORIENTED_EDGE('',*,*,#29831,.T.) ;
#42997 = ORIENTED_EDGE('',*,*,#29832,.T.) ;
#42998 = ORIENTED_EDGE('',*,*,#29833,.T.) ;
#42999 = ORIENTED_EDGE('',*,*,#29832,.F.) ;
#43000 = ORIENTED_EDGE('',*,*,#29834,.F.) ;
#43001 = ORIENTED_EDGE('',*,*,#29835,.T.) ;
#43002 = ORIENTED_EDGE('',*,*,#29836,.T.) ;
#43003 = ORIENTED_EDGE('',*,*,#29835,.F.) ;
#43004 = ORIENTED_EDGE('',*,*,#29837,.T.) ;
#43005 = ORIENTED_EDGE('',*,*,#29838,.T.) ;
#43006 = ORIENTED_EDGE('',*,*,#29839,.T.) ;
#43007 = ORIENTED_EDGE('',*,*,#29838,.F.) ;
#43008 = ORIENTED_EDGE('',*,*,#29840,.T.) ;
#43009 = ORIENTED_EDGE('',*,*,#29841,.T.) ;
#43010 = ORIENTED_EDGE('',*,*,#29842,.T.) ;
#43011 = ORIENTED_EDGE('',*,*,#29841,.F.) ;
#43012 = ORIENTED_EDGE('',*,*,#29843,.T.) ;
#43013 = ORIENTED_EDGE('',*,*,#29844,.T.) ;
#43014 = ORIENTED_EDGE('',*,*,#29845,.T.) ;
#43015 = ORIENTED_EDGE('',*,*,#29844,.F.) ;
#43016 = ORIENTED_EDGE('',*,*,#29846,.F.) ;
#43017 = ORIENTED_EDGE('',*,*,#29847,.T.) ;
#43018 = ORIENTED_EDGE('',*,*,#29848,.T.) ;
#43019 = ORIENTED_EDGE('',*,*,#29847,.F.) ;
#43020 = ORIENTED_EDGE('',*,*,#29849,.T.) ;
#43021 = ORIENTED_EDGE('',*,*,#29850,.T.) ;
#43022 = ORIENTED_EDGE('',*,*,#29851,.T.) ;
#43023 = ORIENTED_EDGE('',*,*,#29850,.F.) ;
#43024 = ORIENTED_EDGE('',*,*,#29852,.T.) ;
#43025 = ORIENTED_EDGE('',*,*,#29853,.T.) ;
#43026 = ORIENTED_EDGE('',*,*,#29854,.T.) ;
#43027 = ORIENTED_EDGE('',*,*,#29853,.F.) ;
#43028 = ORIENTED_EDGE('',*,*,#29855,.T.) ;
#43029 = ORIENTED_EDGE('',*,*,#29856,.T.) ;
#43030 = ORIENTED_EDGE('',*,*,#29857,.T.) ;
#43031 = ORIENTED_EDGE('',*,*,#29856,.F.) ;
#43032 = ORIENTED_EDGE('',*,*,#29858,.F.) ;
#43033 = ORIENTED_EDGE('',*,*,#29859,.T.) ;
#43034 = ORIENTED_EDGE('',*,*,#29860,.T.) ;
#43035 = ORIENTED_EDGE('',*,*,#29859,.F.) ;
#43036 = ORIENTED_EDGE('',*,*,#29861,.T.) ;
#43037 = ORIENTED_EDGE('',*,*,#29862,.T.) ;
#43038 = ORIENTED_EDGE('',*,*,#29863,.T.) ;
#43039 = ORIENTED_EDGE('',*,*,#29862,.F.) ;
#43040 = ORIENTED_EDGE('',*,*,#29864,.T.) ;
#43041 = ORIENTED_EDGE('',*,*,#29865,.T.) ;
#43042 = ORIENTED_EDGE('',*,*,#29866,.T.) ;
#43043 = ORIENTED_EDGE('',*,*,#29865,.F.) ;
#43044 = ORIENTED_EDGE('',*,*,#29867,.T.) ;
#43045 = ORIENTED_EDGE('',*,*,#29868,.T.) ;
#43046 = ORIENTED_EDGE('',*,*,#29869,.T.) ;
#43047 = ORIENTED_EDGE('',*,*,#29868,.F.) ;
#43048 = ORIENTED_EDGE('',*,*,#29870,.F.) ;
#43049 = ORIENTED_EDGE('',*,*,#29871,.T.) ;
#43050 = ORIENTED_EDGE('',*,*,#29872,.T.) ;
#43051 = ORIENTED_EDGE('',*,*,#29871,.F.) ;
#43052 = ORIENTED_EDGE('',*,*,#29873,.T.) ;
#43053 = ORIENTED_EDGE('',*,*,#29874,.T.) ;
#43054 = ORIENTED_EDGE('',*,*,#29875,.T.) ;
#43055 = ORIENTED_EDGE('',*,*,#29874,.F.) ;
#43056 = ORIENTED_EDGE('',*,*,#29876,.T.) ;
#43057 = ORIENTED_EDGE('',*,*,#29877,.T.) ;
#43058 = ORIENTED_EDGE('',*,*,#29878,.T.) ;
#43059 = ORIENTED_EDGE('',*,*,#29877,.F.) ;
#43060 = ORIENTED_EDGE('',*,*,#29879,.T.) ;
#43061 = ORIENTED_EDGE('',*,*,#29880,.T.) ;
#43062 = ORIENTED_EDGE('',*,*,#29881,.T.) ;
#43063 = ORIENTED_EDGE('',*,*,#29880,.F.) ;
#43064 = ORIENTED_EDGE('',*,*,#29882,.F.) ;
#43065 = ORIENTED_EDGE('',*,*,#29883,.T.) ;
#43066 = ORIENTED_EDGE('',*,*,#29884,.T.) ;
#43067 = ORIENTED_EDGE('',*,*,#29883,.F.) ;
#43068 = ORIENTED_EDGE('',*,*,#29885,.T.) ;
#43069 = ORIENTED_EDGE('',*,*,#29886,.T.) ;
#43070 = ORIENTED_EDGE('',*,*,#29887,.T.) ;
#43071 = ORIENTED_EDGE('',*,*,#29886,.F.) ;
#43072 = ORIENTED_EDGE('',*,*,#29888,.T.) ;
#43073 = ORIENTED_EDGE('',*,*,#29889,.T.) ;
#43074 = ORIENTED_EDGE('',*,*,#29890,.T.) ;
#43075 = ORIENTED_EDGE('',*,*,#29889,.F.) ;
#43076 = ORIENTED_EDGE('',*,*,#29891,.T.) ;
#43077 = ORIENTED_EDGE('',*,*,#29892,.T.) ;
#43078 = ORIENTED_EDGE('',*,*,#29893,.T.) ;
#43079 = ORIENTED_EDGE('',*,*,#29892,.F.) ;
#43080 = ORIENTED_EDGE('',*,*,#29894,.F.) ;
#43081 = ORIENTED_EDGE('',*,*,#29895,.T.) ;
#43082 = ORIENTED_EDGE('',*,*,#29896,.T.) ;
#43083 = ORIENTED_EDGE('',*,*,#29895,.F.) ;
#43084 = ORIENTED_EDGE('',*,*,#29897,.T.) ;
#43085 = ORIENTED_EDGE('',*,*,#29898,.T.) ;
#43086 = ORIENTED_EDGE('',*,*,#29899,.T.) ;
#43087 = ORIENTED_EDGE('',*,*,#29898,.F.) ;
#43088 = ORIENTED_EDGE('',*,*,#29900,.T.) ;
#43089 = ORIENTED_EDGE('',*,*,#29901,.T.) ;
#43090 = ORIENTED_EDGE('',*,*,#29902,.T.) ;
#43091 = ORIENTED_EDGE('',*,*,#29901,.F.) ;
#43092 = ORIENTED_EDGE('',*,*,#29903,.T.) ;
#43093 = ORIENTED_EDGE('',*,*,#29904,.T.) ;
#43094 = ORIENTED_EDGE('',*,*,#29905,.T.) ;
#43095 = ORIENTED_EDGE('',*,*,#29904,.F.) ;
#43096 = ORIENTED_EDGE('',*,*,#29906,.F.) ;
#43097 = ORIENTED_EDGE('',*,*,#29907,.T.) ;
#43098 = ORIENTED_EDGE('',*,*,#29908,.T.) ;
#43099 = ORIENTED_EDGE('',*,*,#29907,.F.) ;
#43100 = ORIENTED_EDGE('',*,*,#29909,.T.) ;
#43101 = ORIENTED_EDGE('',*,*,#29910,.T.) ;
#43102 = ORIENTED_EDGE('',*,*,#29911,.T.) ;
#43103 = ORIENTED_EDGE('',*,*,#29910,.F.) ;
#43104 = ORIENTED_EDGE('',*,*,#29912,.T.) ;
#43105 = ORIENTED_EDGE('',*,*,#29913,.T.) ;
#43106 = ORIENTED_EDGE('',*,*,#29914,.T.) ;
#43107 = ORIENTED_EDGE('',*,*,#29913,.F.) ;
#43108 = ORIENTED_EDGE('',*,*,#29915,.T.) ;
#43109 = ORIENTED_EDGE('',*,*,#29679,.T.) ;
#43110 = ORIENTED_EDGE('',*,*,#29800,.F.) ;
#43111 = ORIENTED_EDGE('',*,*,#29916,.F.) ;
#43112 = ORIENTED_EDGE('',*,*,#29917,.F.) ;
#43113 = ORIENTED_EDGE('',*,*,#29918,.F.) ;
#43114 = ORIENTED_EDGE('',*,*,#29803,.F.) ;
#43115 = ORIENTED_EDGE('',*,*,#29919,.F.) ;
#43116 = ORIENTED_EDGE('',*,*,#29920,.F.) ;
#43117 = ORIENTED_EDGE('',*,*,#29916,.T.) ;
#43118 = ORIENTED_EDGE('',*,*,#29806,.F.) ;
#43119 = ORIENTED_EDGE('',*,*,#29921,.F.) ;
#43120 = ORIENTED_EDGE('',*,*,#29922,.F.) ;
#43121 = ORIENTED_EDGE('',*,*,#29919,.T.) ;
#43122 = ORIENTED_EDGE('',*,*,#29809,.F.) ;
#43123 = ORIENTED_EDGE('',*,*,#29923,.T.) ;
#43124 = ORIENTED_EDGE('',*,*,#29924,.F.) ;
#43125 = ORIENTED_EDGE('',*,*,#29921,.T.) ;
#43126 = ORIENTED_EDGE('',*,*,#29812,.F.) ;
#43127 = ORIENTED_EDGE('',*,*,#29925,.F.) ;
#43128 = ORIENTED_EDGE('',*,*,#29926,.F.) ;
#43129 = ORIENTED_EDGE('',*,*,#29923,.F.) ;
#43130 = ORIENTED_EDGE('',*,*,#29815,.F.) ;
#43131 = ORIENTED_EDGE('',*,*,#29927,.F.) ;
#43132 = ORIENTED_EDGE('',*,*,#29928,.F.) ;
#43133 = ORIENTED_EDGE('',*,*,#29925,.T.) ;
#43134 = ORIENTED_EDGE('',*,*,#29818,.F.) ;
#43135 = ORIENTED_EDGE('',*,*,#29929,.F.) ;
#43136 = ORIENTED_EDGE('',*,*,#29930,.F.) ;
#43137 = ORIENTED_EDGE('',*,*,#29927,.T.) ;
#43138 = ORIENTED_EDGE('',*,*,#29821,.F.) ;
#43139 = ORIENTED_EDGE('',*,*,#29931,.T.) ;
#43140 = ORIENTED_EDGE('',*,*,#29932,.F.) ;
#43141 = ORIENTED_EDGE('',*,*,#29929,.T.) ;
#43142 = ORIENTED_EDGE('',*,*,#29824,.F.) ;
#43143 = ORIENTED_EDGE('',*,*,#29933,.F.) ;
#43144 = ORIENTED_EDGE('',*,*,#29934,.F.) ;
#43145 = ORIENTED_EDGE('',*,*,#29931,.F.) ;
#43146 = ORIENTED_EDGE('',*,*,#29827,.F.) ;
#43147 = ORIENTED_EDGE('',*,*,#29935,.F.) ;
#43148 = ORIENTED_EDGE('',*,*,#29936,.F.) ;
#43149 = ORIENTED_EDGE('',*,*,#29933,.T.) ;
#43150 = ORIENTED_EDGE('',*,*,#29830,.F.) ;
#43151 = ORIENTED_EDGE('',*,*,#29937,.F.) ;
#43152 = ORIENTED_EDGE('',*,*,#29938,.F.) ;
#43153 = ORIENTED_EDGE('',*,*,#29935,.T.) ;
#43154 = ORIENTED_EDGE('',*,*,#29833,.F.) ;
#43155 = ORIENTED_EDGE('',*,*,#29939,.T.) ;
#43156 = ORIENTED_EDGE('',*,*,#29940,.F.) ;
#43157 = ORIENTED_EDGE('',*,*,#29937,.T.) ;
#43158 = ORIENTED_EDGE('',*,*,#29836,.F.) ;
#43159 = ORIENTED_EDGE('',*,*,#29941,.F.) ;
#43160 = ORIENTED_EDGE('',*,*,#29942,.F.) ;
#43161 = ORIENTED_EDGE('',*,*,#29939,.F.) ;
#43162 = ORIENTED_EDGE('',*,*,#29839,.F.) ;
#43163 = ORIENTED_EDGE('',*,*,#29943,.F.) ;
#43164 = ORIENTED_EDGE('',*,*,#29944,.F.) ;
#43165 = ORIENTED_EDGE('',*,*,#29941,.T.) ;
#43166 = ORIENTED_EDGE('',*,*,#29842,.F.) ;
#43167 = ORIENTED_EDGE('',*,*,#29945,.F.) ;
#43168 = ORIENTED_EDGE('',*,*,#29946,.F.) ;
#43169 = ORIENTED_EDGE('',*,*,#29943,.T.) ;
#43170 = ORIENTED_EDGE('',*,*,#29845,.F.) ;
#43171 = ORIENTED_EDGE('',*,*,#29947,.T.) ;
#43172 = ORIENTED_EDGE('',*,*,#29948,.F.) ;
#43173 = ORIENTED_EDGE('',*,*,#29945,.T.) ;
#43174 = ORIENTED_EDGE('',*,*,#29848,.F.) ;
#43175 = ORIENTED_EDGE('',*,*,#29949,.F.) ;
#43176 = ORIENTED_EDGE('',*,*,#29950,.F.) ;
#43177 = ORIENTED_EDGE('',*,*,#29947,.F.) ;
#43178 = ORIENTED_EDGE('',*,*,#29851,.F.) ;
#43179 = ORIENTED_EDGE('',*,*,#29951,.F.) ;
#43180 = ORIENTED_EDGE('',*,*,#29952,.F.) ;
#43181 = ORIENTED_EDGE('',*,*,#29949,.T.) ;
#43182 = ORIENTED_EDGE('',*,*,#29854,.F.) ;
#43183 = ORIENTED_EDGE('',*,*,#29953,.F.) ;
#43184 = ORIENTED_EDGE('',*,*,#29954,.F.) ;
#43185 = ORIENTED_EDGE('',*,*,#29951,.T.) ;
#43186 = ORIENTED_EDGE('',*,*,#29857,.F.) ;
#43187 = ORIENTED_EDGE('',*,*,#29955,.T.) ;
#43188 = ORIENTED_EDGE('',*,*,#29956,.F.) ;
#43189 = ORIENTED_EDGE('',*,*,#29953,.T.) ;
#43190 = ORIENTED_EDGE('',*,*,#29860,.F.) ;
#43191 = ORIENTED_EDGE('',*,*,#29957,.F.) ;
#43192 = ORIENTED_EDGE('',*,*,#29958,.F.) ;
#43193 = ORIENTED_EDGE('',*,*,#29955,.F.) ;
#43194 = ORIENTED_EDGE('',*,*,#29863,.F.) ;
#43195 = ORIENTED_EDGE('',*,*,#29959,.F.) ;
#43196 = ORIENTED_EDGE('',*,*,#29960,.F.) ;
#43197 = ORIENTED_EDGE('',*,*,#29957,.T.) ;
#43198 = ORIENTED_EDGE('',*,*,#29866,.F.) ;
#43199 = ORIENTED_EDGE('',*,*,#29961,.F.) ;
#43200 = ORIENTED_EDGE('',*,*,#29962,.F.) ;
#43201 = ORIENTED_EDGE('',*,*,#29959,.T.) ;
#43202 = ORIENTED_EDGE('',*,*,#29869,.F.) ;
#43203 = ORIENTED_EDGE('',*,*,#29963,.T.) ;
#43204 = ORIENTED_EDGE('',*,*,#29964,.F.) ;
#43205 = ORIENTED_EDGE('',*,*,#29961,.T.) ;
#43206 = ORIENTED_EDGE('',*,*,#29872,.F.) ;
#43207 = ORIENTED_EDGE('',*,*,#29965,.F.) ;
#43208 = ORIENTED_EDGE('',*,*,#29966,.F.) ;
#43209 = ORIENTED_EDGE('',*,*,#29963,.F.) ;
#43210 = ORIENTED_EDGE('',*,*,#29875,.F.) ;
#43211 = ORIENTED_EDGE('',*,*,#29967,.F.) ;
#43212 = ORIENTED_EDGE('',*,*,#29968,.F.) ;
#43213 = ORIENTED_EDGE('',*,*,#29965,.T.) ;
#43214 = ORIENTED_EDGE('',*,*,#29878,.F.) ;
#43215 = ORIENTED_EDGE('',*,*,#29969,.F.) ;
#43216 = ORIENTED_EDGE('',*,*,#29970,.F.) ;
#43217 = ORIENTED_EDGE('',*,*,#29967,.T.) ;
#43218 = ORIENTED_EDGE('',*,*,#29881,.F.) ;
#43219 = ORIENTED_EDGE('',*,*,#29971,.T.) ;
#43220 = ORIENTED_EDGE('',*,*,#29972,.F.) ;
#43221 = ORIENTED_EDGE('',*,*,#29969,.T.) ;
#43222 = ORIENTED_EDGE('',*,*,#29884,.F.) ;
#43223 = ORIENTED_EDGE('',*,*,#29973,.F.) ;
#43224 = ORIENTED_EDGE('',*,*,#29974,.F.) ;
#43225 = ORIENTED_EDGE('',*,*,#29971,.F.) ;
#43226 = ORIENTED_EDGE('',*,*,#29887,.F.) ;
#43227 = ORIENTED_EDGE('',*,*,#29975,.F.) ;
#43228 = ORIENTED_EDGE('',*,*,#29976,.F.) ;
#43229 = ORIENTED_EDGE('',*,*,#29973,.T.) ;
#43230 = ORIENTED_EDGE('',*,*,#29890,.F.) ;
#43231 = ORIENTED_EDGE('',*,*,#29977,.F.) ;
#43232 = ORIENTED_EDGE('',*,*,#29978,.F.) ;
#43233 = ORIENTED_EDGE('',*,*,#29975,.T.) ;
#43234 = ORIENTED_EDGE('',*,*,#29893,.F.) ;
#43235 = ORIENTED_EDGE('',*,*,#29979,.T.) ;
#43236 = ORIENTED_EDGE('',*,*,#29980,.F.) ;
#43237 = ORIENTED_EDGE('',*,*,#29977,.T.) ;
#43238 = ORIENTED_EDGE('',*,*,#29896,.F.) ;
#43239 = ORIENTED_EDGE('',*,*,#29981,.F.) ;
#43240 = ORIENTED_EDGE('',*,*,#29982,.F.) ;
#43241 = ORIENTED_EDGE('',*,*,#29979,.F.) ;
#43242 = ORIENTED_EDGE('',*,*,#29899,.F.) ;
#43243 = ORIENTED_EDGE('',*,*,#29983,.F.) ;
#43244 = ORIENTED_EDGE('',*,*,#29984,.F.) ;
#43245 = ORIENTED_EDGE('',*,*,#29981,.T.) ;
#43246 = ORIENTED_EDGE('',*,*,#29902,.F.) ;
#43247 = ORIENTED_EDGE('',*,*,#29985,.F.) ;
#43248 = ORIENTED_EDGE('',*,*,#29986,.F.) ;
#43249 = ORIENTED_EDGE('',*,*,#29983,.T.) ;
#43250 = ORIENTED_EDGE('',*,*,#29905,.F.) ;
#43251 = ORIENTED_EDGE('',*,*,#29987,.T.) ;
#43252 = ORIENTED_EDGE('',*,*,#29988,.F.) ;
#43253 = ORIENTED_EDGE('',*,*,#29985,.T.) ;
#43254 = ORIENTED_EDGE('',*,*,#29908,.F.) ;
#43255 = ORIENTED_EDGE('',*,*,#29989,.F.) ;
#43256 = ORIENTED_EDGE('',*,*,#29990,.F.) ;
#43257 = ORIENTED_EDGE('',*,*,#29987,.F.) ;
#43258 = ORIENTED_EDGE('',*,*,#29911,.F.) ;
#43259 = ORIENTED_EDGE('',*,*,#29991,.F.) ;
#43260 = ORIENTED_EDGE('',*,*,#29992,.F.) ;
#43261 = ORIENTED_EDGE('',*,*,#29989,.T.) ;
#43262 = ORIENTED_EDGE('',*,*,#29914,.F.) ;
#43263 = ORIENTED_EDGE('',*,*,#29993,.F.) ;
#43264 = ORIENTED_EDGE('',*,*,#29994,.F.) ;
#43265 = ORIENTED_EDGE('',*,*,#29991,.T.) ;
#43266 = ORIENTED_EDGE('',*,*,#29678,.F.) ;
#43267 = ORIENTED_EDGE('',*,*,#29995,.T.) ;
#43268 = ORIENTED_EDGE('',*,*,#29996,.F.) ;
#43269 = ORIENTED_EDGE('',*,*,#29993,.T.) ;
#43270 = ORIENTED_EDGE('',*,*,#29807,.F.) ;
#43271 = ORIENTED_EDGE('',*,*,#29804,.F.) ;
#43272 = ORIENTED_EDGE('',*,*,#29801,.F.) ;
#43273 = ORIENTED_EDGE('',*,*,#29997,.F.) ;
#43274 = ORIENTED_EDGE('',*,*,#29819,.F.) ;
#43275 = ORIENTED_EDGE('',*,*,#29816,.F.) ;
#43276 = ORIENTED_EDGE('',*,*,#29813,.F.) ;
#43277 = ORIENTED_EDGE('',*,*,#29998,.F.) ;
#43278 = ORIENTED_EDGE('',*,*,#29788,.F.) ;
#43279 = ORIENTED_EDGE('',*,*,#29999,.F.) ;
#43280 = ORIENTED_EDGE('',*,*,#29794,.F.) ;
#43281 = ORIENTED_EDGE('',*,*,#29791,.F.) ;
#43282 = ORIENTED_EDGE('',*,*,#29831,.F.) ;
#43283 = ORIENTED_EDGE('',*,*,#29828,.F.) ;
#43284 = ORIENTED_EDGE('',*,*,#29825,.F.) ;
#43285 = ORIENTED_EDGE('',*,*,#30000,.F.) ;
#43286 = ORIENTED_EDGE('',*,*,#29776,.F.) ;
#43287 = ORIENTED_EDGE('',*,*,#30001,.F.) ;
#43288 = ORIENTED_EDGE('',*,*,#29782,.F.) ;
#43289 = ORIENTED_EDGE('',*,*,#29779,.F.) ;
#43290 = ORIENTED_EDGE('',*,*,#29843,.F.) ;
#43291 = ORIENTED_EDGE('',*,*,#29840,.F.) ;
#43292 = ORIENTED_EDGE('',*,*,#29837,.F.) ;
#43293 = ORIENTED_EDGE('',*,*,#30002,.F.) ;
#43294 = ORIENTED_EDGE('',*,*,#29764,.F.) ;
#43295 = ORIENTED_EDGE('',*,*,#30003,.F.) ;
#43296 = ORIENTED_EDGE('',*,*,#29770,.F.) ;
#43297 = ORIENTED_EDGE('',*,*,#29767,.F.) ;
#43298 = ORIENTED_EDGE('',*,*,#29855,.F.) ;
#43299 = ORIENTED_EDGE('',*,*,#29852,.F.) ;
#43300 = ORIENTED_EDGE('',*,*,#29849,.F.) ;
#43301 = ORIENTED_EDGE('',*,*,#30004,.F.) ;
#43302 = ORIENTED_EDGE('',*,*,#29752,.F.) ;
#43303 = ORIENTED_EDGE('',*,*,#30005,.F.) ;
#43304 = ORIENTED_EDGE('',*,*,#29758,.F.) ;
#43305 = ORIENTED_EDGE('',*,*,#29755,.F.) ;
#43306 = ORIENTED_EDGE('',*,*,#29867,.F.) ;
#43307 = ORIENTED_EDGE('',*,*,#29864,.F.) ;
#43308 = ORIENTED_EDGE('',*,*,#29861,.F.) ;
#43309 = ORIENTED_EDGE('',*,*,#30006,.F.) ;
#43310 = ORIENTED_EDGE('',*,*,#29740,.F.) ;
#43311 = ORIENTED_EDGE('',*,*,#30007,.F.) ;
#43312 = ORIENTED_EDGE('',*,*,#29746,.F.) ;
#43313 = ORIENTED_EDGE('',*,*,#29743,.F.) ;
#43314 = ORIENTED_EDGE('',*,*,#29879,.F.) ;
#43315 = ORIENTED_EDGE('',*,*,#29876,.F.) ;
#43316 = ORIENTED_EDGE('',*,*,#29873,.F.) ;
#43317 = ORIENTED_EDGE('',*,*,#30008,.F.) ;
#43318 = ORIENTED_EDGE('',*,*,#29728,.F.) ;
#43319 = ORIENTED_EDGE('',*,*,#30009,.F.) ;
#43320 = ORIENTED_EDGE('',*,*,#29734,.F.) ;
#43321 = ORIENTED_EDGE('',*,*,#29731,.F.) ;
#43322 = ORIENTED_EDGE('',*,*,#29891,.F.) ;
#43323 = ORIENTED_EDGE('',*,*,#29888,.F.) ;
#43324 = ORIENTED_EDGE('',*,*,#29885,.F.) ;
#43325 = ORIENTED_EDGE('',*,*,#30010,.F.) ;
#43326 = ORIENTED_EDGE('',*,*,#29716,.F.) ;
#43327 = ORIENTED_EDGE('',*,*,#30011,.F.) ;
#43328 = ORIENTED_EDGE('',*,*,#29722,.F.) ;
#43329 = ORIENTED_EDGE('',*,*,#29719,.F.) ;
#43330 = ORIENTED_EDGE('',*,*,#29903,.F.) ;
#43331 = ORIENTED_EDGE('',*,*,#29900,.F.) ;
#43332 = ORIENTED_EDGE('',*,*,#29897,.F.) ;
#43333 = ORIENTED_EDGE('',*,*,#30012,.F.) ;
#43334 = ORIENTED_EDGE('',*,*,#29704,.F.) ;
#43335 = ORIENTED_EDGE('',*,*,#30013,.F.) ;
#43336 = ORIENTED_EDGE('',*,*,#29710,.F.) ;
#43337 = ORIENTED_EDGE('',*,*,#29707,.F.) ;
#43338 = ORIENTED_EDGE('',*,*,#29915,.F.) ;
#43339 = ORIENTED_EDGE('',*,*,#29912,.F.) ;
#43340 = ORIENTED_EDGE('',*,*,#29909,.F.) ;
#43341 = ORIENTED_EDGE('',*,*,#30014,.F.) ;
#43342 = ORIENTED_EDGE('',*,*,#29692,.F.) ;
#43343 = ORIENTED_EDGE('',*,*,#30015,.F.) ;
#43344 = ORIENTED_EDGE('',*,*,#30016,.F.) ;
#43345 = ORIENTED_EDGE('',*,*,#29698,.F.) ;
#43346 = ORIENTED_EDGE('',*,*,#29695,.F.) ;
#43347 = ORIENTED_EDGE('',*,*,#29671,.F.) ;
#43348 = ORIENTED_EDGE('',*,*,#29672,.F.) ;
#43349 = ORIENTED_EDGE('',*,*,#30017,.T.) ;
#43350 = ORIENTED_EDGE('',*,*,#30015,.T.) ;
#43351 = ORIENTED_EDGE('',*,*,#29689,.T.) ;
#43352 = ORIENTED_EDGE('',*,*,#30018,.T.) ;
#43353 = ORIENTED_EDGE('',*,*,#29676,.T.) ;
#43354 = ORIENTED_EDGE('',*,*,#30014,.T.) ;
#43355 = ORIENTED_EDGE('',*,*,#29906,.T.) ;
#43356 = ORIENTED_EDGE('',*,*,#30012,.T.) ;
#43357 = ORIENTED_EDGE('',*,*,#29894,.T.) ;
#43358 = ORIENTED_EDGE('',*,*,#30010,.T.) ;
#43359 = ORIENTED_EDGE('',*,*,#29882,.T.) ;
#43360 = ORIENTED_EDGE('',*,*,#30008,.T.) ;
#43361 = ORIENTED_EDGE('',*,*,#29870,.T.) ;
#43362 = ORIENTED_EDGE('',*,*,#30006,.T.) ;
#43363 = ORIENTED_EDGE('',*,*,#29858,.T.) ;
#43364 = ORIENTED_EDGE('',*,*,#30004,.T.) ;
#43365 = ORIENTED_EDGE('',*,*,#29846,.T.) ;
#43366 = ORIENTED_EDGE('',*,*,#30002,.T.) ;
#43367 = ORIENTED_EDGE('',*,*,#29834,.T.) ;
#43368 = ORIENTED_EDGE('',*,*,#30000,.T.) ;
#43369 = ORIENTED_EDGE('',*,*,#29822,.T.) ;
#43370 = ORIENTED_EDGE('',*,*,#29998,.T.) ;
#43371 = ORIENTED_EDGE('',*,*,#29810,.T.) ;
#43372 = ORIENTED_EDGE('',*,*,#29997,.T.) ;
#43373 = ORIENTED_EDGE('',*,*,#29797,.T.) ;
#43374 = ORIENTED_EDGE('',*,*,#29999,.T.) ;
#43375 = ORIENTED_EDGE('',*,*,#29785,.T.) ;
#43376 = ORIENTED_EDGE('',*,*,#30001,.T.) ;
#43377 = ORIENTED_EDGE('',*,*,#29773,.T.) ;
#43378 = ORIENTED_EDGE('',*,*,#30003,.T.) ;
#43379 = ORIENTED_EDGE('',*,*,#29761,.T.) ;
#43380 = ORIENTED_EDGE('',*,*,#30005,.T.) ;
#43381 = ORIENTED_EDGE('',*,*,#29749,.T.) ;
#43382 = ORIENTED_EDGE('',*,*,#30007,.T.) ;
#43383 = ORIENTED_EDGE('',*,*,#29737,.T.) ;
#43384 = ORIENTED_EDGE('',*,*,#30009,.T.) ;
#43385 = ORIENTED_EDGE('',*,*,#29725,.T.) ;
#43386 = ORIENTED_EDGE('',*,*,#30011,.T.) ;
#43387 = ORIENTED_EDGE('',*,*,#29713,.T.) ;
#43388 = ORIENTED_EDGE('',*,*,#30013,.T.) ;
#43389 = ORIENTED_EDGE('',*,*,#29701,.T.) ;
#43390 = ORIENTED_EDGE('',*,*,#30016,.T.) ;
#43391 = ORIENTED_EDGE('',*,*,#30017,.F.) ;
#43392 = ORIENTED_EDGE('',*,*,#29680,.F.) ;
#43393 = ORIENTED_EDGE('',*,*,#30018,.F.) ;
#43394 = ORIENTED_EDGE('',*,*,#29686,.F.) ;
#43395 = ORIENTED_EDGE('',*,*,#29683,.F.) ;
#43396 = ORIENTED_EDGE('',*,*,#29674,.F.) ;
#43397 = ORIENTED_EDGE('',*,*,#29675,.F.) ;
#43398 = ORIENTED_EDGE('',*,*,#30019,.T.) ;
#43399 = ORIENTED_EDGE('',*,*,#30020,.T.) ;
#43400 = ORIENTED_EDGE('',*,*,#30021,.F.) ;
#43401 = ORIENTED_EDGE('',*,*,#30022,.T.) ;
#43402 = ORIENTED_EDGE('',*,*,#30023,.F.) ;
#43403 = ORIENTED_EDGE('',*,*,#30024,.T.) ;
#43404 = ORIENTED_EDGE('',*,*,#30025,.F.) ;
#43405 = ORIENTED_EDGE('',*,*,#30026,.T.) ;
#43406 = ORIENTED_EDGE('',*,*,#30027,.F.) ;
#43407 = ORIENTED_EDGE('',*,*,#30028,.T.) ;
#43408 = ORIENTED_EDGE('',*,*,#30029,.F.) ;
#43409 = ORIENTED_EDGE('',*,*,#30030,.T.) ;
#43410 = ORIENTED_EDGE('',*,*,#30031,.F.) ;
#43411 = ORIENTED_EDGE('',*,*,#30032,.T.) ;
#43412 = ORIENTED_EDGE('',*,*,#30033,.F.) ;
#43413 = ORIENTED_EDGE('',*,*,#30034,.T.) ;
#43414 = ORIENTED_EDGE('',*,*,#30035,.F.) ;
#43415 = ORIENTED_EDGE('',*,*,#30036,.T.) ;
#43416 = ORIENTED_EDGE('',*,*,#30037,.F.) ;
#43417 = ORIENTED_EDGE('',*,*,#30038,.T.) ;
#43418 = ORIENTED_EDGE('',*,*,#30039,.F.) ;
#43419 = ORIENTED_EDGE('',*,*,#30040,.T.) ;
#43420 = ORIENTED_EDGE('',*,*,#30041,.F.) ;
#43421 = ORIENTED_EDGE('',*,*,#30042,.T.) ;
#43422 = ORIENTED_EDGE('',*,*,#30043,.F.) ;
#43423 = ORIENTED_EDGE('',*,*,#30044,.T.) ;
#43424 = ORIENTED_EDGE('',*,*,#30045,.F.) ;
#43425 = ORIENTED_EDGE('',*,*,#30046,.T.) ;
#43426 = ORIENTED_EDGE('',*,*,#30047,.F.) ;
#43427 = ORIENTED_EDGE('',*,*,#30048,.T.) ;
#43428 = ORIENTED_EDGE('',*,*,#30049,.F.) ;
#43429 = ORIENTED_EDGE('',*,*,#30050,.T.) ;
#43430 = ORIENTED_EDGE('',*,*,#30051,.F.) ;
#43431 = ORIENTED_EDGE('',*,*,#30052,.T.) ;
#43432 = ORIENTED_EDGE('',*,*,#30053,.F.) ;
#43433 = ORIENTED_EDGE('',*,*,#30054,.T.) ;
#43434 = ORIENTED_EDGE('',*,*,#30055,.F.) ;
#43435 = ORIENTED_EDGE('',*,*,#30056,.T.) ;
#43436 = ORIENTED_EDGE('',*,*,#30057,.F.) ;
#43437 = ORIENTED_EDGE('',*,*,#30058,.T.) ;
#43438 = ORIENTED_EDGE('',*,*,#30059,.F.) ;
#43439 = ORIENTED_EDGE('',*,*,#30060,.T.) ;
#43440 = ORIENTED_EDGE('',*,*,#30019,.F.) ;
#43441 = ORIENTED_EDGE('',*,*,#30058,.F.) ;
#43442 = ORIENTED_EDGE('',*,*,#30061,.F.) ;
#43443 = ORIENTED_EDGE('',*,*,#30062,.F.) ;
#43444 = ORIENTED_EDGE('',*,*,#30063,.F.) ;
#43445 = ORIENTED_EDGE('',*,*,#30056,.F.) ;
#43446 = ORIENTED_EDGE('',*,*,#30064,.F.) ;
#43447 = ORIENTED_EDGE('',*,*,#30065,.F.) ;
#43448 = ORIENTED_EDGE('',*,*,#30066,.F.) ;
#43449 = ORIENTED_EDGE('',*,*,#30054,.F.) ;
#43450 = ORIENTED_EDGE('',*,*,#30067,.F.) ;
#43451 = ORIENTED_EDGE('',*,*,#30068,.F.) ;
#43452 = ORIENTED_EDGE('',*,*,#30069,.F.) ;
#43453 = ORIENTED_EDGE('',*,*,#30052,.F.) ;
#43454 = ORIENTED_EDGE('',*,*,#30070,.F.) ;
#43455 = ORIENTED_EDGE('',*,*,#30071,.F.) ;
#43456 = ORIENTED_EDGE('',*,*,#30072,.F.) ;
#43457 = ORIENTED_EDGE('',*,*,#30050,.F.) ;
#43458 = ORIENTED_EDGE('',*,*,#30073,.F.) ;
#43459 = ORIENTED_EDGE('',*,*,#30074,.F.) ;
#43460 = ORIENTED_EDGE('',*,*,#30075,.F.) ;
#43461 = ORIENTED_EDGE('',*,*,#30048,.F.) ;
#43462 = ORIENTED_EDGE('',*,*,#30076,.F.) ;
#43463 = ORIENTED_EDGE('',*,*,#30077,.F.) ;
#43464 = ORIENTED_EDGE('',*,*,#30078,.F.) ;
#43465 = ORIENTED_EDGE('',*,*,#30046,.F.) ;
#43466 = ORIENTED_EDGE('',*,*,#30079,.F.) ;
#43467 = ORIENTED_EDGE('',*,*,#30080,.F.) ;
#43468 = ORIENTED_EDGE('',*,*,#30081,.F.) ;
#43469 = ORIENTED_EDGE('',*,*,#30044,.F.) ;
#43470 = ORIENTED_EDGE('',*,*,#30082,.F.) ;
#43471 = ORIENTED_EDGE('',*,*,#30083,.F.) ;
#43472 = ORIENTED_EDGE('',*,*,#30084,.F.) ;
#43473 = ORIENTED_EDGE('',*,*,#30042,.F.) ;
#43474 = ORIENTED_EDGE('',*,*,#30085,.F.) ;
#43475 = ORIENTED_EDGE('',*,*,#30086,.F.) ;
#43476 = ORIENTED_EDGE('',*,*,#30087,.F.) ;
#43477 = ORIENTED_EDGE('',*,*,#30040,.F.) ;
#43478 = ORIENTED_EDGE('',*,*,#30088,.F.) ;
#43479 = ORIENTED_EDGE('',*,*,#30089,.F.) ;
#43480 = ORIENTED_EDGE('',*,*,#30090,.F.) ;
#43481 = ORIENTED_EDGE('',*,*,#30038,.F.) ;
#43482 = ORIENTED_EDGE('',*,*,#30091,.F.) ;
#43483 = ORIENTED_EDGE('',*,*,#30092,.F.) ;
#43484 = ORIENTED_EDGE('',*,*,#30093,.F.) ;
#43485 = ORIENTED_EDGE('',*,*,#30036,.F.) ;
#43486 = ORIENTED_EDGE('',*,*,#30094,.F.) ;
#43487 = ORIENTED_EDGE('',*,*,#30095,.F.) ;
#43488 = ORIENTED_EDGE('',*,*,#30096,.F.) ;
#43489 = ORIENTED_EDGE('',*,*,#30034,.F.) ;
#43490 = ORIENTED_EDGE('',*,*,#30097,.F.) ;
#43491 = ORIENTED_EDGE('',*,*,#30098,.F.) ;
#43492 = ORIENTED_EDGE('',*,*,#30099,.F.) ;
#43493 = ORIENTED_EDGE('',*,*,#30032,.F.) ;
#43494 = ORIENTED_EDGE('',*,*,#30100,.F.) ;
#43495 = ORIENTED_EDGE('',*,*,#30101,.F.) ;
#43496 = ORIENTED_EDGE('',*,*,#30102,.F.) ;
#43497 = ORIENTED_EDGE('',*,*,#30030,.F.) ;
#43498 = ORIENTED_EDGE('',*,*,#30103,.F.) ;
#43499 = ORIENTED_EDGE('',*,*,#30104,.F.) ;
#43500 = ORIENTED_EDGE('',*,*,#30105,.F.) ;
#43501 = ORIENTED_EDGE('',*,*,#30028,.F.) ;
#43502 = ORIENTED_EDGE('',*,*,#30106,.F.) ;
#43503 = ORIENTED_EDGE('',*,*,#30107,.F.) ;
#43504 = ORIENTED_EDGE('',*,*,#30108,.F.) ;
#43505 = ORIENTED_EDGE('',*,*,#30026,.F.) ;
#43506 = ORIENTED_EDGE('',*,*,#30109,.F.) ;
#43507 = ORIENTED_EDGE('',*,*,#30110,.F.) ;
#43508 = ORIENTED_EDGE('',*,*,#30111,.F.) ;
#43509 = ORIENTED_EDGE('',*,*,#30024,.F.) ;
#43510 = ORIENTED_EDGE('',*,*,#30112,.F.) ;
#43511 = ORIENTED_EDGE('',*,*,#30113,.F.) ;
#43512 = ORIENTED_EDGE('',*,*,#30114,.F.) ;
#43513 = ORIENTED_EDGE('',*,*,#30022,.F.) ;
#43514 = ORIENTED_EDGE('',*,*,#30115,.F.) ;
#43515 = ORIENTED_EDGE('',*,*,#30116,.F.) ;
#43516 = ORIENTED_EDGE('',*,*,#30117,.F.) ;
#43517 = ORIENTED_EDGE('',*,*,#30060,.F.) ;
#43518 = ORIENTED_EDGE('',*,*,#30118,.F.) ;
#43519 = ORIENTED_EDGE('',*,*,#30119,.F.) ;
#43520 = ORIENTED_EDGE('',*,*,#30120,.F.) ;
#43521 = ORIENTED_EDGE('',*,*,#30020,.F.) ;
#43522 = ORIENTED_EDGE('',*,*,#30039,.T.) ;
#43523 = ORIENTED_EDGE('',*,*,#30121,.T.) ;
#43524 = ORIENTED_EDGE('',*,*,#30122,.T.) ;
#43525 = ORIENTED_EDGE('',*,*,#30123,.F.) ;
#43526 = ORIENTED_EDGE('',*,*,#30093,.T.) ;
#43527 = ORIENTED_EDGE('',*,*,#30124,.T.) ;
#43528 = ORIENTED_EDGE('',*,*,#30125,.T.) ;
#43529 = ORIENTED_EDGE('',*,*,#30121,.F.) ;
#43530 = ORIENTED_EDGE('',*,*,#30126,.T.) ;
#43531 = ORIENTED_EDGE('',*,*,#30127,.T.) ;
#43532 = ORIENTED_EDGE('',*,*,#30088,.T.) ;
#43533 = ORIENTED_EDGE('',*,*,#30123,.T.) ;
#43534 = ORIENTED_EDGE('',*,*,#30091,.T.) ;
#43535 = ORIENTED_EDGE('',*,*,#30128,.T.) ;
#43536 = ORIENTED_EDGE('',*,*,#30129,.T.) ;
#43537 = ORIENTED_EDGE('',*,*,#30130,.T.) ;
#43538 = ORIENTED_EDGE('',*,*,#30037,.T.) ;
#43539 = ORIENTED_EDGE('',*,*,#30131,.T.) ;
#43540 = ORIENTED_EDGE('',*,*,#29996,.T.) ;
#43541 = ORIENTED_EDGE('',*,*,#30128,.F.) ;
#43542 = ORIENTED_EDGE('',*,*,#30096,.T.) ;
#43543 = ORIENTED_EDGE('',*,*,#30132,.T.) ;
#43544 = ORIENTED_EDGE('',*,*,#29994,.T.) ;
#43545 = ORIENTED_EDGE('',*,*,#30131,.F.) ;
#43546 = ORIENTED_EDGE('',*,*,#30133,.T.) ;
#43547 = ORIENTED_EDGE('',*,*,#30134,.T.) ;
#43548 = ORIENTED_EDGE('',*,*,#30085,.T.) ;
#43549 = ORIENTED_EDGE('',*,*,#30135,.T.) ;
#43550 = ORIENTED_EDGE('',*,*,#30094,.T.) ;
#43551 = ORIENTED_EDGE('',*,*,#30136,.T.) ;
#43552 = ORIENTED_EDGE('',*,*,#29990,.T.) ;
#43553 = ORIENTED_EDGE('',*,*,#30137,.T.) ;
#43554 = ORIENTED_EDGE('',*,*,#30035,.T.) ;
#43555 = ORIENTED_EDGE('',*,*,#30138,.T.) ;
#43556 = ORIENTED_EDGE('',*,*,#29988,.T.) ;
#43557 = ORIENTED_EDGE('',*,*,#30136,.F.) ;
#43558 = ORIENTED_EDGE('',*,*,#30099,.T.) ;
#43559 = ORIENTED_EDGE('',*,*,#30139,.T.) ;
#43560 = ORIENTED_EDGE('',*,*,#29986,.T.) ;
#43561 = ORIENTED_EDGE('',*,*,#30138,.F.) ;
#43562 = ORIENTED_EDGE('',*,*,#30140,.T.) ;
#43563 = ORIENTED_EDGE('',*,*,#30141,.T.) ;
#43564 = ORIENTED_EDGE('',*,*,#30082,.T.) ;
#43565 = ORIENTED_EDGE('',*,*,#30142,.T.) ;
#43566 = ORIENTED_EDGE('',*,*,#30097,.T.) ;
#43567 = ORIENTED_EDGE('',*,*,#30143,.T.) ;
#43568 = ORIENTED_EDGE('',*,*,#29982,.T.) ;
#43569 = ORIENTED_EDGE('',*,*,#30144,.T.) ;
#43570 = ORIENTED_EDGE('',*,*,#30033,.T.) ;
#43571 = ORIENTED_EDGE('',*,*,#30145,.T.) ;
#43572 = ORIENTED_EDGE('',*,*,#29980,.T.) ;
#43573 = ORIENTED_EDGE('',*,*,#30143,.F.) ;
#43574 = ORIENTED_EDGE('',*,*,#30102,.T.) ;
#43575 = ORIENTED_EDGE('',*,*,#30146,.T.) ;
#43576 = ORIENTED_EDGE('',*,*,#29978,.T.) ;
#43577 = ORIENTED_EDGE('',*,*,#30145,.F.) ;
#43578 = ORIENTED_EDGE('',*,*,#30147,.T.) ;
#43579 = ORIENTED_EDGE('',*,*,#30148,.T.) ;
#43580 = ORIENTED_EDGE('',*,*,#30079,.T.) ;
#43581 = ORIENTED_EDGE('',*,*,#30149,.T.) ;
#43582 = ORIENTED_EDGE('',*,*,#30100,.T.) ;
#43583 = ORIENTED_EDGE('',*,*,#30150,.T.) ;
#43584 = ORIENTED_EDGE('',*,*,#29974,.T.) ;
#43585 = ORIENTED_EDGE('',*,*,#30151,.T.) ;
#43586 = ORIENTED_EDGE('',*,*,#30031,.T.) ;
#43587 = ORIENTED_EDGE('',*,*,#30152,.T.) ;
#43588 = ORIENTED_EDGE('',*,*,#29972,.T.) ;
#43589 = ORIENTED_EDGE('',*,*,#30150,.F.) ;
#43590 = ORIENTED_EDGE('',*,*,#30105,.T.) ;
#43591 = ORIENTED_EDGE('',*,*,#30153,.T.) ;
#43592 = ORIENTED_EDGE('',*,*,#29970,.T.) ;
#43593 = ORIENTED_EDGE('',*,*,#30152,.F.) ;
#43594 = ORIENTED_EDGE('',*,*,#30154,.T.) ;
#43595 = ORIENTED_EDGE('',*,*,#30155,.T.) ;
#43596 = ORIENTED_EDGE('',*,*,#30076,.T.) ;
#43597 = ORIENTED_EDGE('',*,*,#30156,.T.) ;
#43598 = ORIENTED_EDGE('',*,*,#30103,.T.) ;
#43599 = ORIENTED_EDGE('',*,*,#30157,.T.) ;
#43600 = ORIENTED_EDGE('',*,*,#29966,.T.) ;
#43601 = ORIENTED_EDGE('',*,*,#30158,.T.) ;
#43602 = ORIENTED_EDGE('',*,*,#30029,.T.) ;
#43603 = ORIENTED_EDGE('',*,*,#30159,.T.) ;
#43604 = ORIENTED_EDGE('',*,*,#29964,.T.) ;
#43605 = ORIENTED_EDGE('',*,*,#30157,.F.) ;
#43606 = ORIENTED_EDGE('',*,*,#30108,.T.) ;
#43607 = ORIENTED_EDGE('',*,*,#30160,.T.) ;
#43608 = ORIENTED_EDGE('',*,*,#29962,.T.) ;
#43609 = ORIENTED_EDGE('',*,*,#30159,.F.) ;
#43610 = ORIENTED_EDGE('',*,*,#30161,.T.) ;
#43611 = ORIENTED_EDGE('',*,*,#30162,.T.) ;
#43612 = ORIENTED_EDGE('',*,*,#30073,.T.) ;
#43613 = ORIENTED_EDGE('',*,*,#30163,.T.) ;
#43614 = ORIENTED_EDGE('',*,*,#30106,.T.) ;
#43615 = ORIENTED_EDGE('',*,*,#30164,.T.) ;
#43616 = ORIENTED_EDGE('',*,*,#29958,.T.) ;
#43617 = ORIENTED_EDGE('',*,*,#30165,.T.) ;
#43618 = ORIENTED_EDGE('',*,*,#30027,.T.) ;
#43619 = ORIENTED_EDGE('',*,*,#30166,.T.) ;
#43620 = ORIENTED_EDGE('',*,*,#29956,.T.) ;
#43621 = ORIENTED_EDGE('',*,*,#30164,.F.) ;
#43622 = ORIENTED_EDGE('',*,*,#30111,.T.) ;
#43623 = ORIENTED_EDGE('',*,*,#30167,.T.) ;
#43624 = ORIENTED_EDGE('',*,*,#29954,.T.) ;
#43625 = ORIENTED_EDGE('',*,*,#30166,.F.) ;
#43626 = ORIENTED_EDGE('',*,*,#30168,.T.) ;
#43627 = ORIENTED_EDGE('',*,*,#30169,.T.) ;
#43628 = ORIENTED_EDGE('',*,*,#30070,.T.) ;
#43629 = ORIENTED_EDGE('',*,*,#30170,.T.) ;
#43630 = ORIENTED_EDGE('',*,*,#30109,.T.) ;
#43631 = ORIENTED_EDGE('',*,*,#30171,.T.) ;
#43632 = ORIENTED_EDGE('',*,*,#29950,.T.) ;
#43633 = ORIENTED_EDGE('',*,*,#30172,.T.) ;
#43634 = ORIENTED_EDGE('',*,*,#30025,.T.) ;
#43635 = ORIENTED_EDGE('',*,*,#30173,.T.) ;
#43636 = ORIENTED_EDGE('',*,*,#29948,.T.) ;
#43637 = ORIENTED_EDGE('',*,*,#30171,.F.) ;
#43638 = ORIENTED_EDGE('',*,*,#30114,.T.) ;
#43639 = ORIENTED_EDGE('',*,*,#30174,.T.) ;
#43640 = ORIENTED_EDGE('',*,*,#29946,.T.) ;
#43641 = ORIENTED_EDGE('',*,*,#30173,.F.) ;
#43642 = ORIENTED_EDGE('',*,*,#30175,.T.) ;
#43643 = ORIENTED_EDGE('',*,*,#30176,.T.) ;
#43644 = ORIENTED_EDGE('',*,*,#30067,.T.) ;
#43645 = ORIENTED_EDGE('',*,*,#30177,.T.) ;
#43646 = ORIENTED_EDGE('',*,*,#30112,.T.) ;
#43647 = ORIENTED_EDGE('',*,*,#30178,.T.) ;
#43648 = ORIENTED_EDGE('',*,*,#29942,.T.) ;
#43649 = ORIENTED_EDGE('',*,*,#30179,.T.) ;
#43650 = ORIENTED_EDGE('',*,*,#30023,.T.) ;
#43651 = ORIENTED_EDGE('',*,*,#30180,.T.) ;
#43652 = ORIENTED_EDGE('',*,*,#29940,.T.) ;
#43653 = ORIENTED_EDGE('',*,*,#30178,.F.) ;
#43654 = ORIENTED_EDGE('',*,*,#30117,.T.) ;
#43655 = ORIENTED_EDGE('',*,*,#30181,.T.) ;
#43656 = ORIENTED_EDGE('',*,*,#29938,.T.) ;
#43657 = ORIENTED_EDGE('',*,*,#30180,.F.) ;
#43658 = ORIENTED_EDGE('',*,*,#30182,.T.) ;
#43659 = ORIENTED_EDGE('',*,*,#30183,.T.) ;
#43660 = ORIENTED_EDGE('',*,*,#30064,.T.) ;
#43661 = ORIENTED_EDGE('',*,*,#30184,.T.) ;
#43662 = ORIENTED_EDGE('',*,*,#30115,.T.) ;
#43663 = ORIENTED_EDGE('',*,*,#30185,.T.) ;
#43664 = ORIENTED_EDGE('',*,*,#29934,.T.) ;
#43665 = ORIENTED_EDGE('',*,*,#30186,.T.) ;
#43666 = ORIENTED_EDGE('',*,*,#30021,.T.) ;
#43667 = ORIENTED_EDGE('',*,*,#30187,.T.) ;
#43668 = ORIENTED_EDGE('',*,*,#29932,.T.) ;
#43669 = ORIENTED_EDGE('',*,*,#30185,.F.) ;
#43670 = ORIENTED_EDGE('',*,*,#30120,.T.) ;
#43671 = ORIENTED_EDGE('',*,*,#30188,.T.) ;
#43672 = ORIENTED_EDGE('',*,*,#29930,.T.) ;
#43673 = ORIENTED_EDGE('',*,*,#30187,.F.) ;
#43674 = ORIENTED_EDGE('',*,*,#29917,.T.) ;
#43675 = ORIENTED_EDGE('',*,*,#30189,.T.) ;
#43676 = ORIENTED_EDGE('',*,*,#30061,.T.) ;
#43677 = ORIENTED_EDGE('',*,*,#30190,.T.) ;
#43678 = ORIENTED_EDGE('',*,*,#30118,.T.) ;
#43679 = ORIENTED_EDGE('',*,*,#30191,.T.) ;
#43680 = ORIENTED_EDGE('',*,*,#29926,.T.) ;
#43681 = ORIENTED_EDGE('',*,*,#30192,.T.) ;
#43682 = ORIENTED_EDGE('',*,*,#30059,.T.) ;
#43683 = ORIENTED_EDGE('',*,*,#30193,.T.) ;
#43684 = ORIENTED_EDGE('',*,*,#29924,.T.) ;
#43685 = ORIENTED_EDGE('',*,*,#30191,.F.) ;
#43686 = ORIENTED_EDGE('',*,*,#29922,.T.) ;
#43687 = ORIENTED_EDGE('',*,*,#30193,.F.) ;
#43688 = ORIENTED_EDGE('',*,*,#30063,.T.) ;
#43689 = ORIENTED_EDGE('',*,*,#30194,.T.) ;
#43690 = ORIENTED_EDGE('',*,*,#29920,.T.) ;
#43691 = ORIENTED_EDGE('',*,*,#30194,.F.) ;
#43692 = ORIENTED_EDGE('',*,*,#30062,.T.) ;
#43693 = ORIENTED_EDGE('',*,*,#30189,.F.) ;
#43694 = ORIENTED_EDGE('',*,*,#30119,.T.) ;
#43695 = ORIENTED_EDGE('',*,*,#30192,.F.) ;
#43696 = ORIENTED_EDGE('',*,*,#29928,.T.) ;
#43697 = ORIENTED_EDGE('',*,*,#30188,.F.) ;
#43698 = ORIENTED_EDGE('',*,*,#30195,.T.) ;
#43699 = ORIENTED_EDGE('',*,*,#30190,.F.) ;
#43700 = ORIENTED_EDGE('',*,*,#30057,.T.) ;
#43701 = ORIENTED_EDGE('',*,*,#30196,.T.) ;
#43702 = ORIENTED_EDGE('',*,*,#30197,.T.) ;
#43703 = ORIENTED_EDGE('',*,*,#30196,.F.) ;
#43704 = ORIENTED_EDGE('',*,*,#30066,.T.) ;
#43705 = ORIENTED_EDGE('',*,*,#30198,.T.) ;
#43706 = ORIENTED_EDGE('',*,*,#30199,.T.) ;
#43707 = ORIENTED_EDGE('',*,*,#30198,.F.) ;
#43708 = ORIENTED_EDGE('',*,*,#30065,.T.) ;
#43709 = ORIENTED_EDGE('',*,*,#30183,.F.) ;
#43710 = ORIENTED_EDGE('',*,*,#30116,.T.) ;
#43711 = ORIENTED_EDGE('',*,*,#30186,.F.) ;
#43712 = ORIENTED_EDGE('',*,*,#29936,.T.) ;
#43713 = ORIENTED_EDGE('',*,*,#30181,.F.) ;
#43714 = ORIENTED_EDGE('',*,*,#30200,.T.) ;
#43715 = ORIENTED_EDGE('',*,*,#30184,.F.) ;
#43716 = ORIENTED_EDGE('',*,*,#30055,.T.) ;
#43717 = ORIENTED_EDGE('',*,*,#30201,.T.) ;
#43718 = ORIENTED_EDGE('',*,*,#30202,.T.) ;
#43719 = ORIENTED_EDGE('',*,*,#30201,.F.) ;
#43720 = ORIENTED_EDGE('',*,*,#30069,.T.) ;
#43721 = ORIENTED_EDGE('',*,*,#30203,.T.) ;
#43722 = ORIENTED_EDGE('',*,*,#30204,.T.) ;
#43723 = ORIENTED_EDGE('',*,*,#30203,.F.) ;
#43724 = ORIENTED_EDGE('',*,*,#30068,.T.) ;
#43725 = ORIENTED_EDGE('',*,*,#30176,.F.) ;
#43726 = ORIENTED_EDGE('',*,*,#30113,.T.) ;
#43727 = ORIENTED_EDGE('',*,*,#30179,.F.) ;
#43728 = ORIENTED_EDGE('',*,*,#29944,.T.) ;
#43729 = ORIENTED_EDGE('',*,*,#30174,.F.) ;
#43730 = ORIENTED_EDGE('',*,*,#30205,.T.) ;
#43731 = ORIENTED_EDGE('',*,*,#30177,.F.) ;
#43732 = ORIENTED_EDGE('',*,*,#30053,.T.) ;
#43733 = ORIENTED_EDGE('',*,*,#30206,.T.) ;
#43734 = ORIENTED_EDGE('',*,*,#30207,.T.) ;
#43735 = ORIENTED_EDGE('',*,*,#30206,.F.) ;
#43736 = ORIENTED_EDGE('',*,*,#30072,.T.) ;
#43737 = ORIENTED_EDGE('',*,*,#30208,.T.) ;
#43738 = ORIENTED_EDGE('',*,*,#30209,.T.) ;
#43739 = ORIENTED_EDGE('',*,*,#30208,.F.) ;
#43740 = ORIENTED_EDGE('',*,*,#30071,.T.) ;
#43741 = ORIENTED_EDGE('',*,*,#30169,.F.) ;
#43742 = ORIENTED_EDGE('',*,*,#30110,.T.) ;
#43743 = ORIENTED_EDGE('',*,*,#30172,.F.) ;
#43744 = ORIENTED_EDGE('',*,*,#29952,.T.) ;
#43745 = ORIENTED_EDGE('',*,*,#30167,.F.) ;
#43746 = ORIENTED_EDGE('',*,*,#30210,.T.) ;
#43747 = ORIENTED_EDGE('',*,*,#30170,.F.) ;
#43748 = ORIENTED_EDGE('',*,*,#30051,.T.) ;
#43749 = ORIENTED_EDGE('',*,*,#30211,.T.) ;
#43750 = ORIENTED_EDGE('',*,*,#30212,.T.) ;
#43751 = ORIENTED_EDGE('',*,*,#30211,.F.) ;
#43752 = ORIENTED_EDGE('',*,*,#30075,.T.) ;
#43753 = ORIENTED_EDGE('',*,*,#30213,.T.) ;
#43754 = ORIENTED_EDGE('',*,*,#30214,.T.) ;
#43755 = ORIENTED_EDGE('',*,*,#30213,.F.) ;
#43756 = ORIENTED_EDGE('',*,*,#30074,.T.) ;
#43757 = ORIENTED_EDGE('',*,*,#30162,.F.) ;
#43758 = ORIENTED_EDGE('',*,*,#30107,.T.) ;
#43759 = ORIENTED_EDGE('',*,*,#30165,.F.) ;
#43760 = ORIENTED_EDGE('',*,*,#29960,.T.) ;
#43761 = ORIENTED_EDGE('',*,*,#30160,.F.) ;
#43762 = ORIENTED_EDGE('',*,*,#30215,.T.) ;
#43763 = ORIENTED_EDGE('',*,*,#30163,.F.) ;
#43764 = ORIENTED_EDGE('',*,*,#30049,.T.) ;
#43765 = ORIENTED_EDGE('',*,*,#30216,.T.) ;
#43766 = ORIENTED_EDGE('',*,*,#30217,.T.) ;
#43767 = ORIENTED_EDGE('',*,*,#30216,.F.) ;
#43768 = ORIENTED_EDGE('',*,*,#30078,.T.) ;
#43769 = ORIENTED_EDGE('',*,*,#30218,.T.) ;
#43770 = ORIENTED_EDGE('',*,*,#30219,.T.) ;
#43771 = ORIENTED_EDGE('',*,*,#30218,.F.) ;
#43772 = ORIENTED_EDGE('',*,*,#30077,.T.) ;
#43773 = ORIENTED_EDGE('',*,*,#30155,.F.) ;
#43774 = ORIENTED_EDGE('',*,*,#30104,.T.) ;
#43775 = ORIENTED_EDGE('',*,*,#30158,.F.) ;
#43776 = ORIENTED_EDGE('',*,*,#29968,.T.) ;
#43777 = ORIENTED_EDGE('',*,*,#30153,.F.) ;
#43778 = ORIENTED_EDGE('',*,*,#30220,.T.) ;
#43779 = ORIENTED_EDGE('',*,*,#30156,.F.) ;
#43780 = ORIENTED_EDGE('',*,*,#30047,.T.) ;
#43781 = ORIENTED_EDGE('',*,*,#30221,.T.) ;
#43782 = ORIENTED_EDGE('',*,*,#30222,.T.) ;
#43783 = ORIENTED_EDGE('',*,*,#30221,.F.) ;
#43784 = ORIENTED_EDGE('',*,*,#30081,.T.) ;
#43785 = ORIENTED_EDGE('',*,*,#30223,.T.) ;
#43786 = ORIENTED_EDGE('',*,*,#30224,.T.) ;
#43787 = ORIENTED_EDGE('',*,*,#30223,.F.) ;
#43788 = ORIENTED_EDGE('',*,*,#30080,.T.) ;
#43789 = ORIENTED_EDGE('',*,*,#30148,.F.) ;
#43790 = ORIENTED_EDGE('',*,*,#30101,.T.) ;
#43791 = ORIENTED_EDGE('',*,*,#30151,.F.) ;
#43792 = ORIENTED_EDGE('',*,*,#29976,.T.) ;
#43793 = ORIENTED_EDGE('',*,*,#30146,.F.) ;
#43794 = ORIENTED_EDGE('',*,*,#30225,.T.) ;
#43795 = ORIENTED_EDGE('',*,*,#30149,.F.) ;
#43796 = ORIENTED_EDGE('',*,*,#30045,.T.) ;
#43797 = ORIENTED_EDGE('',*,*,#30226,.T.) ;
#43798 = ORIENTED_EDGE('',*,*,#30227,.T.) ;
#43799 = ORIENTED_EDGE('',*,*,#30226,.F.) ;
#43800 = ORIENTED_EDGE('',*,*,#30084,.T.) ;
#43801 = ORIENTED_EDGE('',*,*,#30228,.T.) ;
#43802 = ORIENTED_EDGE('',*,*,#30229,.T.) ;
#43803 = ORIENTED_EDGE('',*,*,#30228,.F.) ;
#43804 = ORIENTED_EDGE('',*,*,#30083,.T.) ;
#43805 = ORIENTED_EDGE('',*,*,#30141,.F.) ;
#43806 = ORIENTED_EDGE('',*,*,#30098,.T.) ;
#43807 = ORIENTED_EDGE('',*,*,#30144,.F.) ;
#43808 = ORIENTED_EDGE('',*,*,#29984,.T.) ;
#43809 = ORIENTED_EDGE('',*,*,#30139,.F.) ;
#43810 = ORIENTED_EDGE('',*,*,#30230,.T.) ;
#43811 = ORIENTED_EDGE('',*,*,#30142,.F.) ;
#43812 = ORIENTED_EDGE('',*,*,#30043,.T.) ;
#43813 = ORIENTED_EDGE('',*,*,#30231,.T.) ;
#43814 = ORIENTED_EDGE('',*,*,#30232,.T.) ;
#43815 = ORIENTED_EDGE('',*,*,#30231,.F.) ;
#43816 = ORIENTED_EDGE('',*,*,#30087,.T.) ;
#43817 = ORIENTED_EDGE('',*,*,#30233,.T.) ;
#43818 = ORIENTED_EDGE('',*,*,#30234,.T.) ;
#43819 = ORIENTED_EDGE('',*,*,#30233,.F.) ;
#43820 = ORIENTED_EDGE('',*,*,#30086,.T.) ;
#43821 = ORIENTED_EDGE('',*,*,#30134,.F.) ;
#43822 = ORIENTED_EDGE('',*,*,#30095,.T.) ;
#43823 = ORIENTED_EDGE('',*,*,#30137,.F.) ;
#43824 = ORIENTED_EDGE('',*,*,#29992,.T.) ;
#43825 = ORIENTED_EDGE('',*,*,#30132,.F.) ;
#43826 = ORIENTED_EDGE('',*,*,#30235,.T.) ;
#43827 = ORIENTED_EDGE('',*,*,#30135,.F.) ;
#43828 = ORIENTED_EDGE('',*,*,#30041,.T.) ;
#43829 = ORIENTED_EDGE('',*,*,#30236,.T.) ;
#43830 = ORIENTED_EDGE('',*,*,#30237,.T.) ;
#43831 = ORIENTED_EDGE('',*,*,#30236,.F.) ;
#43832 = ORIENTED_EDGE('',*,*,#30090,.T.) ;
#43833 = ORIENTED_EDGE('',*,*,#30238,.T.) ;
#43834 = ORIENTED_EDGE('',*,*,#30239,.T.) ;
#43835 = ORIENTED_EDGE('',*,*,#30238,.F.) ;
#43836 = ORIENTED_EDGE('',*,*,#30089,.T.) ;
#43837 = ORIENTED_EDGE('',*,*,#30127,.F.) ;
#43838 = ORIENTED_EDGE('',*,*,#30092,.T.) ;
#43839 = ORIENTED_EDGE('',*,*,#30130,.F.) ;
#43840 = ORIENTED_EDGE('',*,*,#30240,.T.) ;
#43841 = ORIENTED_EDGE('',*,*,#30124,.F.) ;
#43842 = ORIENTED_EDGE('',*,*,#29691,.F.) ;
#43843 = ORIENTED_EDGE('',*,*,#30241,.T.) ;
#43844 = ORIENTED_EDGE('',*,*,#30122,.F.) ;
#43845 = ORIENTED_EDGE('',*,*,#30242,.T.) ;
#43846 = ORIENTED_EDGE('',*,*,#29688,.F.) ;
#43847 = ORIENTED_EDGE('',*,*,#30242,.F.) ;
#43848 = ORIENTED_EDGE('',*,*,#30125,.F.) ;
#43849 = ORIENTED_EDGE('',*,*,#30243,.T.) ;
#43850 = ORIENTED_EDGE('',*,*,#29685,.F.) ;
#43851 = ORIENTED_EDGE('',*,*,#30243,.F.) ;
#43852 = ORIENTED_EDGE('',*,*,#30240,.F.) ;
#43853 = ORIENTED_EDGE('',*,*,#30244,.T.) ;
#43854 = ORIENTED_EDGE('',*,*,#29682,.F.) ;
#43855 = ORIENTED_EDGE('',*,*,#30244,.F.) ;
#43856 = ORIENTED_EDGE('',*,*,#30129,.F.) ;
#43857 = ORIENTED_EDGE('',*,*,#29995,.F.) ;
#43858 = ORIENTED_EDGE('',*,*,#29796,.F.) ;
#43859 = ORIENTED_EDGE('',*,*,#30245,.F.) ;
#43860 = ORIENTED_EDGE('',*,*,#30197,.F.) ;
#43861 = ORIENTED_EDGE('',*,*,#30246,.T.) ;
#43862 = ORIENTED_EDGE('',*,*,#29790,.F.) ;
#43863 = ORIENTED_EDGE('',*,*,#30247,.F.) ;
#43864 = ORIENTED_EDGE('',*,*,#30182,.F.) ;
#43865 = ORIENTED_EDGE('',*,*,#30248,.F.) ;
#43866 = ORIENTED_EDGE('',*,*,#29793,.F.) ;
#43867 = ORIENTED_EDGE('',*,*,#30246,.F.) ;
#43868 = ORIENTED_EDGE('',*,*,#30199,.F.) ;
#43869 = ORIENTED_EDGE('',*,*,#30247,.T.) ;
#43870 = ORIENTED_EDGE('',*,*,#29784,.F.) ;
#43871 = ORIENTED_EDGE('',*,*,#30249,.F.) ;
#43872 = ORIENTED_EDGE('',*,*,#30202,.F.) ;
#43873 = ORIENTED_EDGE('',*,*,#30250,.T.) ;
#43874 = ORIENTED_EDGE('',*,*,#29778,.F.) ;
#43875 = ORIENTED_EDGE('',*,*,#30251,.F.) ;
#43876 = ORIENTED_EDGE('',*,*,#30175,.F.) ;
#43877 = ORIENTED_EDGE('',*,*,#30252,.F.) ;
#43878 = ORIENTED_EDGE('',*,*,#29781,.F.) ;
#43879 = ORIENTED_EDGE('',*,*,#30250,.F.) ;
#43880 = ORIENTED_EDGE('',*,*,#30204,.F.) ;
#43881 = ORIENTED_EDGE('',*,*,#30251,.T.) ;
#43882 = ORIENTED_EDGE('',*,*,#29772,.F.) ;
#43883 = ORIENTED_EDGE('',*,*,#30253,.F.) ;
#43884 = ORIENTED_EDGE('',*,*,#30207,.F.) ;
#43885 = ORIENTED_EDGE('',*,*,#30254,.T.) ;
#43886 = ORIENTED_EDGE('',*,*,#29766,.F.) ;
#43887 = ORIENTED_EDGE('',*,*,#30255,.F.) ;
#43888 = ORIENTED_EDGE('',*,*,#30168,.F.) ;
#43889 = ORIENTED_EDGE('',*,*,#30256,.F.) ;
#43890 = ORIENTED_EDGE('',*,*,#29769,.F.) ;
#43891 = ORIENTED_EDGE('',*,*,#30254,.F.) ;
#43892 = ORIENTED_EDGE('',*,*,#30209,.F.) ;
#43893 = ORIENTED_EDGE('',*,*,#30255,.T.) ;
#43894 = ORIENTED_EDGE('',*,*,#29760,.F.) ;
#43895 = ORIENTED_EDGE('',*,*,#30257,.F.) ;
#43896 = ORIENTED_EDGE('',*,*,#30212,.F.) ;
#43897 = ORIENTED_EDGE('',*,*,#30258,.T.) ;
#43898 = ORIENTED_EDGE('',*,*,#29754,.F.) ;
#43899 = ORIENTED_EDGE('',*,*,#30259,.F.) ;
#43900 = ORIENTED_EDGE('',*,*,#30161,.F.) ;
#43901 = ORIENTED_EDGE('',*,*,#30260,.F.) ;
#43902 = ORIENTED_EDGE('',*,*,#29757,.F.) ;
#43903 = ORIENTED_EDGE('',*,*,#30258,.F.) ;
#43904 = ORIENTED_EDGE('',*,*,#30214,.F.) ;
#43905 = ORIENTED_EDGE('',*,*,#30259,.T.) ;
#43906 = ORIENTED_EDGE('',*,*,#29748,.F.) ;
#43907 = ORIENTED_EDGE('',*,*,#30261,.F.) ;
#43908 = ORIENTED_EDGE('',*,*,#30217,.F.) ;
#43909 = ORIENTED_EDGE('',*,*,#30262,.T.) ;
#43910 = ORIENTED_EDGE('',*,*,#29742,.F.) ;
#43911 = ORIENTED_EDGE('',*,*,#30263,.F.) ;
#43912 = ORIENTED_EDGE('',*,*,#30154,.F.) ;
#43913 = ORIENTED_EDGE('',*,*,#30264,.F.) ;
#43914 = ORIENTED_EDGE('',*,*,#29745,.F.) ;
#43915 = ORIENTED_EDGE('',*,*,#30262,.F.) ;
#43916 = ORIENTED_EDGE('',*,*,#30219,.F.) ;
#43917 = ORIENTED_EDGE('',*,*,#30263,.T.) ;
#43918 = ORIENTED_EDGE('',*,*,#29736,.F.) ;
#43919 = ORIENTED_EDGE('',*,*,#30265,.F.) ;
#43920 = ORIENTED_EDGE('',*,*,#30222,.F.) ;
#43921 = ORIENTED_EDGE('',*,*,#30266,.T.) ;
#43922 = ORIENTED_EDGE('',*,*,#29730,.F.) ;
#43923 = ORIENTED_EDGE('',*,*,#30267,.F.) ;
#43924 = ORIENTED_EDGE('',*,*,#30147,.F.) ;
#43925 = ORIENTED_EDGE('',*,*,#30268,.F.) ;
#43926 = ORIENTED_EDGE('',*,*,#29733,.F.) ;
#43927 = ORIENTED_EDGE('',*,*,#30266,.F.) ;
#43928 = ORIENTED_EDGE('',*,*,#30224,.F.) ;
#43929 = ORIENTED_EDGE('',*,*,#30267,.T.) ;
#43930 = ORIENTED_EDGE('',*,*,#29724,.F.) ;
#43931 = ORIENTED_EDGE('',*,*,#30269,.F.) ;
#43932 = ORIENTED_EDGE('',*,*,#30227,.F.) ;
#43933 = ORIENTED_EDGE('',*,*,#30270,.T.) ;
#43934 = ORIENTED_EDGE('',*,*,#29718,.F.) ;
#43935 = ORIENTED_EDGE('',*,*,#30271,.F.) ;
#43936 = ORIENTED_EDGE('',*,*,#30140,.F.) ;
#43937 = ORIENTED_EDGE('',*,*,#30272,.F.) ;
#43938 = ORIENTED_EDGE('',*,*,#29721,.F.) ;
#43939 = ORIENTED_EDGE('',*,*,#30270,.F.) ;
#43940 = ORIENTED_EDGE('',*,*,#30229,.F.) ;
#43941 = ORIENTED_EDGE('',*,*,#30271,.T.) ;
#43942 = ORIENTED_EDGE('',*,*,#29712,.F.) ;
#43943 = ORIENTED_EDGE('',*,*,#30273,.F.) ;
#43944 = ORIENTED_EDGE('',*,*,#30232,.F.) ;
#43945 = ORIENTED_EDGE('',*,*,#30274,.T.) ;
#43946 = ORIENTED_EDGE('',*,*,#29706,.F.) ;
#43947 = ORIENTED_EDGE('',*,*,#30275,.F.) ;
#43948 = ORIENTED_EDGE('',*,*,#30133,.F.) ;
#43949 = ORIENTED_EDGE('',*,*,#30276,.F.) ;
#43950 = ORIENTED_EDGE('',*,*,#29709,.F.) ;
#43951 = ORIENTED_EDGE('',*,*,#30274,.F.) ;
#43952 = ORIENTED_EDGE('',*,*,#30234,.F.) ;
#43953 = ORIENTED_EDGE('',*,*,#30275,.T.) ;
#43954 = ORIENTED_EDGE('',*,*,#29700,.F.) ;
#43955 = ORIENTED_EDGE('',*,*,#30277,.F.) ;
#43956 = ORIENTED_EDGE('',*,*,#30237,.F.) ;
#43957 = ORIENTED_EDGE('',*,*,#30278,.T.) ;
#43958 = ORIENTED_EDGE('',*,*,#29694,.F.) ;
#43959 = ORIENTED_EDGE('',*,*,#30279,.F.) ;
#43960 = ORIENTED_EDGE('',*,*,#30126,.F.) ;
#43961 = ORIENTED_EDGE('',*,*,#30241,.F.) ;
#43962 = ORIENTED_EDGE('',*,*,#29697,.F.) ;
#43963 = ORIENTED_EDGE('',*,*,#30278,.F.) ;
#43964 = ORIENTED_EDGE('',*,*,#30239,.F.) ;
#43965 = ORIENTED_EDGE('',*,*,#30279,.T.) ;
#43966 = ORIENTED_EDGE('',*,*,#29703,.F.) ;
#43967 = ORIENTED_EDGE('',*,*,#30276,.T.) ;
#43968 = ORIENTED_EDGE('',*,*,#30235,.F.) ;
#43969 = ORIENTED_EDGE('',*,*,#30277,.T.) ;
#43970 = ORIENTED_EDGE('',*,*,#29715,.F.) ;
#43971 = ORIENTED_EDGE('',*,*,#30272,.T.) ;
#43972 = ORIENTED_EDGE('',*,*,#30230,.F.) ;
#43973 = ORIENTED_EDGE('',*,*,#30273,.T.) ;
#43974 = ORIENTED_EDGE('',*,*,#29727,.F.) ;
#43975 = ORIENTED_EDGE('',*,*,#30268,.T.) ;
#43976 = ORIENTED_EDGE('',*,*,#30225,.F.) ;
#43977 = ORIENTED_EDGE('',*,*,#30269,.T.) ;
#43978 = ORIENTED_EDGE('',*,*,#29739,.F.) ;
#43979 = ORIENTED_EDGE('',*,*,#30264,.T.) ;
#43980 = ORIENTED_EDGE('',*,*,#30220,.F.) ;
#43981 = ORIENTED_EDGE('',*,*,#30265,.T.) ;
#43982 = ORIENTED_EDGE('',*,*,#29751,.F.) ;
#43983 = ORIENTED_EDGE('',*,*,#30260,.T.) ;
#43984 = ORIENTED_EDGE('',*,*,#30215,.F.) ;
#43985 = ORIENTED_EDGE('',*,*,#30261,.T.) ;
#43986 = ORIENTED_EDGE('',*,*,#29763,.F.) ;
#43987 = ORIENTED_EDGE('',*,*,#30256,.T.) ;
#43988 = ORIENTED_EDGE('',*,*,#30210,.F.) ;
#43989 = ORIENTED_EDGE('',*,*,#30257,.T.) ;
#43990 = ORIENTED_EDGE('',*,*,#29775,.F.) ;
#43991 = ORIENTED_EDGE('',*,*,#30252,.T.) ;
#43992 = ORIENTED_EDGE('',*,*,#30205,.F.) ;
#43993 = ORIENTED_EDGE('',*,*,#30253,.T.) ;
#43994 = ORIENTED_EDGE('',*,*,#29787,.F.) ;
#43995 = ORIENTED_EDGE('',*,*,#30248,.T.) ;
#43996 = ORIENTED_EDGE('',*,*,#30200,.F.) ;
#43997 = ORIENTED_EDGE('',*,*,#30249,.T.) ;
#43998 = ORIENTED_EDGE('',*,*,#29799,.F.) ;
#43999 = ORIENTED_EDGE('',*,*,#29918,.T.) ;
#44000 = ORIENTED_EDGE('',*,*,#30195,.F.) ;
#44001 = ORIENTED_EDGE('',*,*,#30245,.T.) ;
#44002 = ORIENTED_EDGE('',*,*,#29668,.F.) ;
#44003 = ORIENTED_EDGE('',*,*,#30280,.T.) ;
#44004 = ORIENTED_EDGE('',*,*,#29669,.F.) ;
#44005 = ORIENTED_EDGE('',*,*,#30280,.F.) ;
#44006 = ORIENTED_EDGE('',*,*,#30281,.F.) ;
#44007 = ORIENTED_EDGE('',*,*,#30282,.T.) ;
#44008 = ORIENTED_EDGE('',*,*,#30283,.T.) ;
#44009 = ORIENTED_EDGE('',*,*,#30282,.F.) ;
#44010 = ORIENTED_EDGE('',*,*,#30284,.F.) ;
#44011 = ORIENTED_EDGE('',*,*,#30283,.F.) ;
#44012 = ORIENTED_EDGE('',*,*,#30285,.T.) ;
#44013 = ORIENTED_EDGE('',*,*,#30286,.T.) ;
#44014 = ORIENTED_EDGE('',*,*,#30287,.F.) ;
#44015 = ORIENTED_EDGE('',*,*,#30286,.F.) ;
#44016 = ORIENTED_EDGE('',*,*,#30288,.F.) ;
#44017 = ORIENTED_EDGE('',*,*,#30285,.F.) ;
#44018 = ORIENTED_EDGE('',*,*,#30287,.T.) ;
#44019 = ORIENTED_EDGE('',*,*,#30289,.T.) ;
#44020 = ORIENTED_EDGE('',*,*,#30281,.T.) ;
#44021 = ORIENTED_EDGE('',*,*,#30290,.T.) ;
#44022 = ORIENTED_EDGE('',*,*,#30291,.T.) ;
#44023 = ORIENTED_EDGE('',*,*,#30292,.T.) ;
#44024 = ORIENTED_EDGE('',*,*,#30293,.T.) ;
#44025 = ORIENTED_EDGE('',*,*,#30291,.F.) ;
#44026 = ORIENTED_EDGE('',*,*,#30284,.T.) ;
#44027 = ORIENTED_EDGE('',*,*,#30294,.T.) ;
#44028 = ORIENTED_EDGE('',*,*,#30295,.T.) ;
#44029 = ORIENTED_EDGE('',*,*,#30296,.T.) ;
#44030 = ORIENTED_EDGE('',*,*,#30294,.F.) ;
#44031 = ORIENTED_EDGE('',*,*,#30288,.T.) ;
#44032 = ORIENTED_EDGE('',*,*,#30297,.F.) ;
#44033 = ORIENTED_EDGE('',*,*,#30298,.T.) ;
#44034 = ORIENTED_EDGE('',*,*,#30299,.T.) ;
#44035 = ORIENTED_EDGE('',*,*,#30300,.F.) ;
#44036 = ORIENTED_EDGE('',*,*,#30301,.T.) ;
#44037 = ORIENTED_EDGE('',*,*,#30302,.T.) ;
#44038 = ORIENTED_EDGE('',*,*,#30303,.T.) ;
#44039 = ORIENTED_EDGE('',*,*,#30298,.F.) ;
#44040 = ORIENTED_EDGE('',*,*,#30304,.T.) ;
#44041 = ORIENTED_EDGE('',*,*,#30305,.T.) ;
#44042 = ORIENTED_EDGE('',*,*,#30306,.T.) ;
#44043 = ORIENTED_EDGE('',*,*,#30302,.F.) ;
#44044 = ORIENTED_EDGE('',*,*,#30307,.T.) ;
#44045 = ORIENTED_EDGE('',*,*,#30308,.T.) ;
#44046 = ORIENTED_EDGE('',*,*,#30309,.T.) ;
#44047 = ORIENTED_EDGE('',*,*,#30305,.F.) ;
#44048 = ORIENTED_EDGE('',*,*,#30310,.F.) ;
#44049 = ORIENTED_EDGE('',*,*,#30311,.T.) ;
#44050 = ORIENTED_EDGE('',*,*,#30312,.T.) ;
#44051 = ORIENTED_EDGE('',*,*,#30308,.F.) ;
#44052 = ORIENTED_EDGE('',*,*,#30313,.T.) ;
#44053 = ORIENTED_EDGE('',*,*,#30314,.T.) ;
#44054 = ORIENTED_EDGE('',*,*,#30315,.T.) ;
#44055 = ORIENTED_EDGE('',*,*,#30311,.F.) ;
#44056 = ORIENTED_EDGE('',*,*,#30316,.T.) ;
#44057 = ORIENTED_EDGE('',*,*,#30317,.T.) ;
#44058 = ORIENTED_EDGE('',*,*,#30318,.T.) ;
#44059 = ORIENTED_EDGE('',*,*,#30314,.F.) ;
#44060 = ORIENTED_EDGE('',*,*,#30319,.T.) ;
#44061 = ORIENTED_EDGE('',*,*,#30320,.T.) ;
#44062 = ORIENTED_EDGE('',*,*,#30321,.T.) ;
#44063 = ORIENTED_EDGE('',*,*,#30317,.F.) ;
#44064 = ORIENTED_EDGE('',*,*,#30322,.F.) ;
#44065 = ORIENTED_EDGE('',*,*,#30323,.T.) ;
#44066 = ORIENTED_EDGE('',*,*,#30324,.T.) ;
#44067 = ORIENTED_EDGE('',*,*,#30320,.F.) ;
#44068 = ORIENTED_EDGE('',*,*,#30325,.T.) ;
#44069 = ORIENTED_EDGE('',*,*,#30326,.T.) ;
#44070 = ORIENTED_EDGE('',*,*,#30327,.T.) ;
#44071 = ORIENTED_EDGE('',*,*,#30323,.F.) ;
#44072 = ORIENTED_EDGE('',*,*,#30328,.T.) ;
#44073 = ORIENTED_EDGE('',*,*,#30329,.T.) ;
#44074 = ORIENTED_EDGE('',*,*,#30330,.T.) ;
#44075 = ORIENTED_EDGE('',*,*,#30326,.F.) ;
#44076 = ORIENTED_EDGE('',*,*,#30331,.T.) ;
#44077 = ORIENTED_EDGE('',*,*,#30332,.T.) ;
#44078 = ORIENTED_EDGE('',*,*,#30333,.T.) ;
#44079 = ORIENTED_EDGE('',*,*,#30329,.F.) ;
#44080 = ORIENTED_EDGE('',*,*,#30334,.F.) ;
#44081 = ORIENTED_EDGE('',*,*,#30335,.T.) ;
#44082 = ORIENTED_EDGE('',*,*,#30336,.T.) ;
#44083 = ORIENTED_EDGE('',*,*,#30332,.F.) ;
#44084 = ORIENTED_EDGE('',*,*,#30337,.T.) ;
#44085 = ORIENTED_EDGE('',*,*,#30338,.T.) ;
#44086 = ORIENTED_EDGE('',*,*,#30339,.T.) ;
#44087 = ORIENTED_EDGE('',*,*,#30335,.F.) ;
#44088 = ORIENTED_EDGE('',*,*,#30340,.T.) ;
#44089 = ORIENTED_EDGE('',*,*,#30341,.T.) ;
#44090 = ORIENTED_EDGE('',*,*,#30342,.T.) ;
#44091 = ORIENTED_EDGE('',*,*,#30338,.F.) ;
#44092 = ORIENTED_EDGE('',*,*,#30343,.T.) ;
#44093 = ORIENTED_EDGE('',*,*,#30344,.T.) ;
#44094 = ORIENTED_EDGE('',*,*,#30345,.T.) ;
#44095 = ORIENTED_EDGE('',*,*,#30341,.F.) ;
#44096 = ORIENTED_EDGE('',*,*,#30346,.F.) ;
#44097 = ORIENTED_EDGE('',*,*,#30347,.T.) ;
#44098 = ORIENTED_EDGE('',*,*,#30348,.T.) ;
#44099 = ORIENTED_EDGE('',*,*,#30344,.F.) ;
#44100 = ORIENTED_EDGE('',*,*,#30349,.T.) ;
#44101 = ORIENTED_EDGE('',*,*,#30350,.T.) ;
#44102 = ORIENTED_EDGE('',*,*,#30351,.T.) ;
#44103 = ORIENTED_EDGE('',*,*,#30347,.F.) ;
#44104 = ORIENTED_EDGE('',*,*,#30352,.T.) ;
#44105 = ORIENTED_EDGE('',*,*,#30353,.T.) ;
#44106 = ORIENTED_EDGE('',*,*,#30354,.T.) ;
#44107 = ORIENTED_EDGE('',*,*,#30350,.F.) ;
#44108 = ORIENTED_EDGE('',*,*,#30355,.T.) ;
#44109 = ORIENTED_EDGE('',*,*,#30356,.T.) ;
#44110 = ORIENTED_EDGE('',*,*,#30357,.T.) ;
#44111 = ORIENTED_EDGE('',*,*,#30353,.F.) ;
#44112 = ORIENTED_EDGE('',*,*,#30358,.F.) ;
#44113 = ORIENTED_EDGE('',*,*,#30359,.T.) ;
#44114 = ORIENTED_EDGE('',*,*,#30360,.T.) ;
#44115 = ORIENTED_EDGE('',*,*,#30356,.F.) ;
#44116 = ORIENTED_EDGE('',*,*,#30361,.T.) ;
#44117 = ORIENTED_EDGE('',*,*,#30362,.T.) ;
#44118 = ORIENTED_EDGE('',*,*,#30363,.T.) ;
#44119 = ORIENTED_EDGE('',*,*,#30359,.F.) ;
#44120 = ORIENTED_EDGE('',*,*,#30364,.T.) ;
#44121 = ORIENTED_EDGE('',*,*,#30365,.T.) ;
#44122 = ORIENTED_EDGE('',*,*,#30366,.T.) ;
#44123 = ORIENTED_EDGE('',*,*,#30362,.F.) ;
#44124 = ORIENTED_EDGE('',*,*,#30367,.T.) ;
#44125 = ORIENTED_EDGE('',*,*,#30368,.T.) ;
#44126 = ORIENTED_EDGE('',*,*,#30369,.T.) ;
#44127 = ORIENTED_EDGE('',*,*,#30365,.F.) ;
#44128 = ORIENTED_EDGE('',*,*,#30370,.F.) ;
#44129 = ORIENTED_EDGE('',*,*,#30371,.T.) ;
#44130 = ORIENTED_EDGE('',*,*,#30372,.T.) ;
#44131 = ORIENTED_EDGE('',*,*,#30368,.F.) ;
#44132 = ORIENTED_EDGE('',*,*,#30373,.T.) ;
#44133 = ORIENTED_EDGE('',*,*,#30374,.T.) ;
#44134 = ORIENTED_EDGE('',*,*,#30375,.T.) ;
#44135 = ORIENTED_EDGE('',*,*,#30371,.F.) ;
#44136 = ORIENTED_EDGE('',*,*,#30376,.T.) ;
#44137 = ORIENTED_EDGE('',*,*,#30377,.T.) ;
#44138 = ORIENTED_EDGE('',*,*,#30378,.T.) ;
#44139 = ORIENTED_EDGE('',*,*,#30374,.F.) ;
#44140 = ORIENTED_EDGE('',*,*,#30379,.T.) ;
#44141 = ORIENTED_EDGE('',*,*,#30380,.T.) ;
#44142 = ORIENTED_EDGE('',*,*,#30381,.T.) ;
#44143 = ORIENTED_EDGE('',*,*,#30377,.F.) ;
#44144 = ORIENTED_EDGE('',*,*,#30382,.F.) ;
#44145 = ORIENTED_EDGE('',*,*,#30383,.T.) ;
#44146 = ORIENTED_EDGE('',*,*,#30384,.T.) ;
#44147 = ORIENTED_EDGE('',*,*,#30380,.F.) ;
#44148 = ORIENTED_EDGE('',*,*,#30385,.T.) ;
#44149 = ORIENTED_EDGE('',*,*,#30386,.T.) ;
#44150 = ORIENTED_EDGE('',*,*,#30387,.T.) ;
#44151 = ORIENTED_EDGE('',*,*,#30383,.F.) ;
#44152 = ORIENTED_EDGE('',*,*,#30388,.T.) ;
#44153 = ORIENTED_EDGE('',*,*,#30389,.T.) ;
#44154 = ORIENTED_EDGE('',*,*,#30390,.T.) ;
#44155 = ORIENTED_EDGE('',*,*,#30386,.F.) ;
#44156 = ORIENTED_EDGE('',*,*,#30391,.T.) ;
#44157 = ORIENTED_EDGE('',*,*,#30392,.T.) ;
#44158 = ORIENTED_EDGE('',*,*,#30393,.T.) ;
#44159 = ORIENTED_EDGE('',*,*,#30389,.F.) ;
#44160 = ORIENTED_EDGE('',*,*,#30394,.F.) ;
#44161 = ORIENTED_EDGE('',*,*,#30395,.T.) ;
#44162 = ORIENTED_EDGE('',*,*,#30396,.T.) ;
#44163 = ORIENTED_EDGE('',*,*,#30392,.F.) ;
#44164 = ORIENTED_EDGE('',*,*,#30397,.T.) ;
#44165 = ORIENTED_EDGE('',*,*,#30398,.T.) ;
#44166 = ORIENTED_EDGE('',*,*,#30399,.T.) ;
#44167 = ORIENTED_EDGE('',*,*,#30395,.F.) ;
#44168 = ORIENTED_EDGE('',*,*,#30400,.T.) ;
#44169 = ORIENTED_EDGE('',*,*,#30401,.T.) ;
#44170 = ORIENTED_EDGE('',*,*,#30402,.T.) ;
#44171 = ORIENTED_EDGE('',*,*,#30398,.F.) ;
#44172 = ORIENTED_EDGE('',*,*,#30403,.T.) ;
#44173 = ORIENTED_EDGE('',*,*,#30404,.T.) ;
#44174 = ORIENTED_EDGE('',*,*,#30405,.T.) ;
#44175 = ORIENTED_EDGE('',*,*,#30401,.F.) ;
#44176 = ORIENTED_EDGE('',*,*,#30406,.F.) ;
#44177 = ORIENTED_EDGE('',*,*,#30407,.T.) ;
#44178 = ORIENTED_EDGE('',*,*,#30408,.T.) ;
#44179 = ORIENTED_EDGE('',*,*,#30404,.F.) ;
#44180 = ORIENTED_EDGE('',*,*,#30409,.T.) ;
#44181 = ORIENTED_EDGE('',*,*,#30410,.T.) ;
#44182 = ORIENTED_EDGE('',*,*,#30411,.T.) ;
#44183 = ORIENTED_EDGE('',*,*,#30407,.F.) ;
#44184 = ORIENTED_EDGE('',*,*,#30412,.T.) ;
#44185 = ORIENTED_EDGE('',*,*,#30413,.T.) ;
#44186 = ORIENTED_EDGE('',*,*,#30414,.T.) ;
#44187 = ORIENTED_EDGE('',*,*,#30410,.F.) ;
#44188 = ORIENTED_EDGE('',*,*,#30415,.T.) ;
#44189 = ORIENTED_EDGE('',*,*,#30416,.T.) ;
#44190 = ORIENTED_EDGE('',*,*,#30417,.T.) ;
#44191 = ORIENTED_EDGE('',*,*,#30413,.F.) ;
#44192 = ORIENTED_EDGE('',*,*,#30418,.F.) ;
#44193 = ORIENTED_EDGE('',*,*,#30419,.T.) ;
#44194 = ORIENTED_EDGE('',*,*,#30420,.T.) ;
#44195 = ORIENTED_EDGE('',*,*,#30416,.F.) ;
#44196 = ORIENTED_EDGE('',*,*,#30421,.T.) ;
#44197 = ORIENTED_EDGE('',*,*,#30419,.F.) ;
#44198 = ORIENTED_EDGE('',*,*,#30422,.T.) ;
#44199 = ORIENTED_EDGE('',*,*,#30423,.T.) ;
#44200 = ORIENTED_EDGE('',*,*,#30424,.T.) ;
#44201 = ORIENTED_EDGE('',*,*,#30423,.F.) ;
#44202 = ORIENTED_EDGE('',*,*,#30425,.T.) ;
#44203 = ORIENTED_EDGE('',*,*,#30426,.T.) ;
#44204 = ORIENTED_EDGE('',*,*,#30427,.T.) ;
#44205 = ORIENTED_EDGE('',*,*,#30426,.F.) ;
#44206 = ORIENTED_EDGE('',*,*,#30428,.T.) ;
#44207 = ORIENTED_EDGE('',*,*,#30429,.T.) ;
#44208 = ORIENTED_EDGE('',*,*,#30430,.T.) ;
#44209 = ORIENTED_EDGE('',*,*,#30429,.F.) ;
#44210 = ORIENTED_EDGE('',*,*,#30431,.F.) ;
#44211 = ORIENTED_EDGE('',*,*,#30432,.T.) ;
#44212 = ORIENTED_EDGE('',*,*,#30433,.T.) ;
#44213 = ORIENTED_EDGE('',*,*,#30432,.F.) ;
#44214 = ORIENTED_EDGE('',*,*,#30434,.T.) ;
#44215 = ORIENTED_EDGE('',*,*,#30435,.T.) ;
#44216 = ORIENTED_EDGE('',*,*,#30436,.T.) ;
#44217 = ORIENTED_EDGE('',*,*,#30435,.F.) ;
#44218 = ORIENTED_EDGE('',*,*,#30437,.T.) ;
#44219 = ORIENTED_EDGE('',*,*,#30438,.T.) ;
#44220 = ORIENTED_EDGE('',*,*,#30439,.T.) ;
#44221 = ORIENTED_EDGE('',*,*,#30438,.F.) ;
#44222 = ORIENTED_EDGE('',*,*,#30440,.T.) ;
#44223 = ORIENTED_EDGE('',*,*,#30441,.T.) ;
#44224 = ORIENTED_EDGE('',*,*,#30442,.T.) ;
#44225 = ORIENTED_EDGE('',*,*,#30441,.F.) ;
#44226 = ORIENTED_EDGE('',*,*,#30443,.F.) ;
#44227 = ORIENTED_EDGE('',*,*,#30444,.T.) ;
#44228 = ORIENTED_EDGE('',*,*,#30445,.T.) ;
#44229 = ORIENTED_EDGE('',*,*,#30444,.F.) ;
#44230 = ORIENTED_EDGE('',*,*,#30446,.T.) ;
#44231 = ORIENTED_EDGE('',*,*,#30447,.T.) ;
#44232 = ORIENTED_EDGE('',*,*,#30448,.T.) ;
#44233 = ORIENTED_EDGE('',*,*,#30447,.F.) ;
#44234 = ORIENTED_EDGE('',*,*,#30449,.T.) ;
#44235 = ORIENTED_EDGE('',*,*,#30450,.T.) ;
#44236 = ORIENTED_EDGE('',*,*,#30451,.T.) ;
#44237 = ORIENTED_EDGE('',*,*,#30450,.F.) ;
#44238 = ORIENTED_EDGE('',*,*,#30452,.T.) ;
#44239 = ORIENTED_EDGE('',*,*,#30453,.T.) ;
#44240 = ORIENTED_EDGE('',*,*,#30454,.T.) ;
#44241 = ORIENTED_EDGE('',*,*,#30453,.F.) ;
#44242 = ORIENTED_EDGE('',*,*,#30455,.F.) ;
#44243 = ORIENTED_EDGE('',*,*,#30456,.T.) ;
#44244 = ORIENTED_EDGE('',*,*,#30457,.T.) ;
#44245 = ORIENTED_EDGE('',*,*,#30456,.F.) ;
#44246 = ORIENTED_EDGE('',*,*,#30458,.T.) ;
#44247 = ORIENTED_EDGE('',*,*,#30459,.T.) ;
#44248 = ORIENTED_EDGE('',*,*,#30460,.T.) ;
#44249 = ORIENTED_EDGE('',*,*,#30459,.F.) ;
#44250 = ORIENTED_EDGE('',*,*,#30461,.T.) ;
#44251 = ORIENTED_EDGE('',*,*,#30462,.T.) ;
#44252 = ORIENTED_EDGE('',*,*,#30463,.T.) ;
#44253 = ORIENTED_EDGE('',*,*,#30462,.F.) ;
#44254 = ORIENTED_EDGE('',*,*,#30464,.T.) ;
#44255 = ORIENTED_EDGE('',*,*,#30465,.T.) ;
#44256 = ORIENTED_EDGE('',*,*,#30466,.T.) ;
#44257 = ORIENTED_EDGE('',*,*,#30465,.F.) ;
#44258 = ORIENTED_EDGE('',*,*,#30467,.F.) ;
#44259 = ORIENTED_EDGE('',*,*,#30468,.T.) ;
#44260 = ORIENTED_EDGE('',*,*,#30469,.T.) ;
#44261 = ORIENTED_EDGE('',*,*,#30468,.F.) ;
#44262 = ORIENTED_EDGE('',*,*,#30470,.T.) ;
#44263 = ORIENTED_EDGE('',*,*,#30471,.T.) ;
#44264 = ORIENTED_EDGE('',*,*,#30472,.T.) ;
#44265 = ORIENTED_EDGE('',*,*,#30471,.F.) ;
#44266 = ORIENTED_EDGE('',*,*,#30473,.T.) ;
#44267 = ORIENTED_EDGE('',*,*,#30474,.T.) ;
#44268 = ORIENTED_EDGE('',*,*,#30475,.T.) ;
#44269 = ORIENTED_EDGE('',*,*,#30474,.F.) ;
#44270 = ORIENTED_EDGE('',*,*,#30476,.T.) ;
#44271 = ORIENTED_EDGE('',*,*,#30477,.T.) ;
#44272 = ORIENTED_EDGE('',*,*,#30478,.T.) ;
#44273 = ORIENTED_EDGE('',*,*,#30477,.F.) ;
#44274 = ORIENTED_EDGE('',*,*,#30479,.F.) ;
#44275 = ORIENTED_EDGE('',*,*,#30480,.T.) ;
#44276 = ORIENTED_EDGE('',*,*,#30481,.T.) ;
#44277 = ORIENTED_EDGE('',*,*,#30480,.F.) ;
#44278 = ORIENTED_EDGE('',*,*,#30482,.T.) ;
#44279 = ORIENTED_EDGE('',*,*,#30483,.T.) ;
#44280 = ORIENTED_EDGE('',*,*,#30484,.T.) ;
#44281 = ORIENTED_EDGE('',*,*,#30483,.F.) ;
#44282 = ORIENTED_EDGE('',*,*,#30485,.T.) ;
#44283 = ORIENTED_EDGE('',*,*,#30486,.T.) ;
#44284 = ORIENTED_EDGE('',*,*,#30487,.T.) ;
#44285 = ORIENTED_EDGE('',*,*,#30486,.F.) ;
#44286 = ORIENTED_EDGE('',*,*,#30488,.T.) ;
#44287 = ORIENTED_EDGE('',*,*,#30489,.T.) ;
#44288 = ORIENTED_EDGE('',*,*,#30490,.T.) ;
#44289 = ORIENTED_EDGE('',*,*,#30489,.F.) ;
#44290 = ORIENTED_EDGE('',*,*,#30491,.F.) ;
#44291 = ORIENTED_EDGE('',*,*,#30492,.T.) ;
#44292 = ORIENTED_EDGE('',*,*,#30493,.T.) ;
#44293 = ORIENTED_EDGE('',*,*,#30492,.F.) ;
#44294 = ORIENTED_EDGE('',*,*,#30494,.T.) ;
#44295 = ORIENTED_EDGE('',*,*,#30495,.T.) ;
#44296 = ORIENTED_EDGE('',*,*,#30496,.T.) ;
#44297 = ORIENTED_EDGE('',*,*,#30495,.F.) ;
#44298 = ORIENTED_EDGE('',*,*,#30497,.T.) ;
#44299 = ORIENTED_EDGE('',*,*,#30498,.T.) ;
#44300 = ORIENTED_EDGE('',*,*,#30499,.T.) ;
#44301 = ORIENTED_EDGE('',*,*,#30498,.F.) ;
#44302 = ORIENTED_EDGE('',*,*,#30500,.T.) ;
#44303 = ORIENTED_EDGE('',*,*,#30501,.T.) ;
#44304 = ORIENTED_EDGE('',*,*,#30502,.T.) ;
#44305 = ORIENTED_EDGE('',*,*,#30501,.F.) ;
#44306 = ORIENTED_EDGE('',*,*,#30503,.F.) ;
#44307 = ORIENTED_EDGE('',*,*,#30504,.T.) ;
#44308 = ORIENTED_EDGE('',*,*,#30505,.T.) ;
#44309 = ORIENTED_EDGE('',*,*,#30504,.F.) ;
#44310 = ORIENTED_EDGE('',*,*,#30506,.T.) ;
#44311 = ORIENTED_EDGE('',*,*,#30507,.T.) ;
#44312 = ORIENTED_EDGE('',*,*,#30508,.T.) ;
#44313 = ORIENTED_EDGE('',*,*,#30507,.F.) ;
#44314 = ORIENTED_EDGE('',*,*,#30509,.T.) ;
#44315 = ORIENTED_EDGE('',*,*,#30510,.T.) ;
#44316 = ORIENTED_EDGE('',*,*,#30511,.T.) ;
#44317 = ORIENTED_EDGE('',*,*,#30510,.F.) ;
#44318 = ORIENTED_EDGE('',*,*,#30512,.T.) ;
#44319 = ORIENTED_EDGE('',*,*,#30513,.T.) ;
#44320 = ORIENTED_EDGE('',*,*,#30514,.T.) ;
#44321 = ORIENTED_EDGE('',*,*,#30513,.F.) ;
#44322 = ORIENTED_EDGE('',*,*,#30515,.F.) ;
#44323 = ORIENTED_EDGE('',*,*,#30516,.T.) ;
#44324 = ORIENTED_EDGE('',*,*,#30517,.T.) ;
#44325 = ORIENTED_EDGE('',*,*,#30516,.F.) ;
#44326 = ORIENTED_EDGE('',*,*,#30518,.T.) ;
#44327 = ORIENTED_EDGE('',*,*,#30519,.T.) ;
#44328 = ORIENTED_EDGE('',*,*,#30520,.T.) ;
#44329 = ORIENTED_EDGE('',*,*,#30519,.F.) ;
#44330 = ORIENTED_EDGE('',*,*,#30521,.T.) ;
#44331 = ORIENTED_EDGE('',*,*,#30522,.T.) ;
#44332 = ORIENTED_EDGE('',*,*,#30523,.T.) ;
#44333 = ORIENTED_EDGE('',*,*,#30522,.F.) ;
#44334 = ORIENTED_EDGE('',*,*,#30524,.T.) ;
#44335 = ORIENTED_EDGE('',*,*,#30525,.T.) ;
#44336 = ORIENTED_EDGE('',*,*,#30526,.T.) ;
#44337 = ORIENTED_EDGE('',*,*,#30525,.F.) ;
#44338 = ORIENTED_EDGE('',*,*,#30527,.F.) ;
#44339 = ORIENTED_EDGE('',*,*,#30528,.T.) ;
#44340 = ORIENTED_EDGE('',*,*,#30529,.T.) ;
#44341 = ORIENTED_EDGE('',*,*,#30528,.F.) ;
#44342 = ORIENTED_EDGE('',*,*,#30530,.T.) ;
#44343 = ORIENTED_EDGE('',*,*,#30531,.T.) ;
#44344 = ORIENTED_EDGE('',*,*,#30532,.T.) ;
#44345 = ORIENTED_EDGE('',*,*,#30531,.F.) ;
#44346 = ORIENTED_EDGE('',*,*,#30533,.T.) ;
#44347 = ORIENTED_EDGE('',*,*,#30534,.T.) ;
#44348 = ORIENTED_EDGE('',*,*,#30535,.T.) ;
#44349 = ORIENTED_EDGE('',*,*,#30534,.F.) ;
#44350 = ORIENTED_EDGE('',*,*,#30536,.T.) ;
#44351 = ORIENTED_EDGE('',*,*,#30300,.T.) ;
#44352 = ORIENTED_EDGE('',*,*,#30421,.F.) ;
#44353 = ORIENTED_EDGE('',*,*,#30537,.F.) ;
#44354 = ORIENTED_EDGE('',*,*,#30538,.F.) ;
#44355 = ORIENTED_EDGE('',*,*,#30539,.F.) ;
#44356 = ORIENTED_EDGE('',*,*,#30424,.F.) ;
#44357 = ORIENTED_EDGE('',*,*,#30540,.F.) ;
#44358 = ORIENTED_EDGE('',*,*,#30541,.F.) ;
#44359 = ORIENTED_EDGE('',*,*,#30537,.T.) ;
#44360 = ORIENTED_EDGE('',*,*,#30427,.F.) ;
#44361 = ORIENTED_EDGE('',*,*,#30542,.F.) ;
#44362 = ORIENTED_EDGE('',*,*,#30543,.F.) ;
#44363 = ORIENTED_EDGE('',*,*,#30540,.T.) ;
#44364 = ORIENTED_EDGE('',*,*,#30430,.F.) ;
#44365 = ORIENTED_EDGE('',*,*,#30544,.T.) ;
#44366 = ORIENTED_EDGE('',*,*,#30545,.F.) ;
#44367 = ORIENTED_EDGE('',*,*,#30542,.T.) ;
#44368 = ORIENTED_EDGE('',*,*,#30433,.F.) ;
#44369 = ORIENTED_EDGE('',*,*,#30546,.F.) ;
#44370 = ORIENTED_EDGE('',*,*,#30547,.F.) ;
#44371 = ORIENTED_EDGE('',*,*,#30544,.F.) ;
#44372 = ORIENTED_EDGE('',*,*,#30436,.F.) ;
#44373 = ORIENTED_EDGE('',*,*,#30548,.F.) ;
#44374 = ORIENTED_EDGE('',*,*,#30549,.F.) ;
#44375 = ORIENTED_EDGE('',*,*,#30546,.T.) ;
#44376 = ORIENTED_EDGE('',*,*,#30439,.F.) ;
#44377 = ORIENTED_EDGE('',*,*,#30550,.F.) ;
#44378 = ORIENTED_EDGE('',*,*,#30551,.F.) ;
#44379 = ORIENTED_EDGE('',*,*,#30548,.T.) ;
#44380 = ORIENTED_EDGE('',*,*,#30442,.F.) ;
#44381 = ORIENTED_EDGE('',*,*,#30552,.T.) ;
#44382 = ORIENTED_EDGE('',*,*,#30553,.F.) ;
#44383 = ORIENTED_EDGE('',*,*,#30550,.T.) ;
#44384 = ORIENTED_EDGE('',*,*,#30445,.F.) ;
#44385 = ORIENTED_EDGE('',*,*,#30554,.F.) ;
#44386 = ORIENTED_EDGE('',*,*,#30555,.F.) ;
#44387 = ORIENTED_EDGE('',*,*,#30552,.F.) ;
#44388 = ORIENTED_EDGE('',*,*,#30448,.F.) ;
#44389 = ORIENTED_EDGE('',*,*,#30556,.F.) ;
#44390 = ORIENTED_EDGE('',*,*,#30557,.F.) ;
#44391 = ORIENTED_EDGE('',*,*,#30554,.T.) ;
#44392 = ORIENTED_EDGE('',*,*,#30451,.F.) ;
#44393 = ORIENTED_EDGE('',*,*,#30558,.F.) ;
#44394 = ORIENTED_EDGE('',*,*,#30559,.F.) ;
#44395 = ORIENTED_EDGE('',*,*,#30556,.T.) ;
#44396 = ORIENTED_EDGE('',*,*,#30454,.F.) ;
#44397 = ORIENTED_EDGE('',*,*,#30560,.T.) ;
#44398 = ORIENTED_EDGE('',*,*,#30561,.F.) ;
#44399 = ORIENTED_EDGE('',*,*,#30558,.T.) ;
#44400 = ORIENTED_EDGE('',*,*,#30457,.F.) ;
#44401 = ORIENTED_EDGE('',*,*,#30562,.F.) ;
#44402 = ORIENTED_EDGE('',*,*,#30563,.F.) ;
#44403 = ORIENTED_EDGE('',*,*,#30560,.F.) ;
#44404 = ORIENTED_EDGE('',*,*,#30460,.F.) ;
#44405 = ORIENTED_EDGE('',*,*,#30564,.F.) ;
#44406 = ORIENTED_EDGE('',*,*,#30565,.F.) ;
#44407 = ORIENTED_EDGE('',*,*,#30562,.T.) ;
#44408 = ORIENTED_EDGE('',*,*,#30463,.F.) ;
#44409 = ORIENTED_EDGE('',*,*,#30566,.F.) ;
#44410 = ORIENTED_EDGE('',*,*,#30567,.F.) ;
#44411 = ORIENTED_EDGE('',*,*,#30564,.T.) ;
#44412 = ORIENTED_EDGE('',*,*,#30466,.F.) ;
#44413 = ORIENTED_EDGE('',*,*,#30568,.T.) ;
#44414 = ORIENTED_EDGE('',*,*,#30569,.F.) ;
#44415 = ORIENTED_EDGE('',*,*,#30566,.T.) ;
#44416 = ORIENTED_EDGE('',*,*,#30469,.F.) ;
#44417 = ORIENTED_EDGE('',*,*,#30570,.F.) ;
#44418 = ORIENTED_EDGE('',*,*,#30571,.F.) ;
#44419 = ORIENTED_EDGE('',*,*,#30568,.F.) ;
#44420 = ORIENTED_EDGE('',*,*,#30472,.F.) ;
#44421 = ORIENTED_EDGE('',*,*,#30572,.F.) ;
#44422 = ORIENTED_EDGE('',*,*,#30573,.F.) ;
#44423 = ORIENTED_EDGE('',*,*,#30570,.T.) ;
#44424 = ORIENTED_EDGE('',*,*,#30475,.F.) ;
#44425 = ORIENTED_EDGE('',*,*,#30574,.F.) ;
#44426 = ORIENTED_EDGE('',*,*,#30575,.F.) ;
#44427 = ORIENTED_EDGE('',*,*,#30572,.T.) ;
#44428 = ORIENTED_EDGE('',*,*,#30478,.F.) ;
#44429 = ORIENTED_EDGE('',*,*,#30576,.T.) ;
#44430 = ORIENTED_EDGE('',*,*,#30577,.F.) ;
#44431 = ORIENTED_EDGE('',*,*,#30574,.T.) ;
#44432 = ORIENTED_EDGE('',*,*,#30481,.F.) ;
#44433 = ORIENTED_EDGE('',*,*,#30578,.F.) ;
#44434 = ORIENTED_EDGE('',*,*,#30579,.F.) ;
#44435 = ORIENTED_EDGE('',*,*,#30576,.F.) ;
#44436 = ORIENTED_EDGE('',*,*,#30484,.F.) ;
#44437 = ORIENTED_EDGE('',*,*,#30580,.F.) ;
#44438 = ORIENTED_EDGE('',*,*,#30581,.F.) ;
#44439 = ORIENTED_EDGE('',*,*,#30578,.T.) ;
#44440 = ORIENTED_EDGE('',*,*,#30487,.F.) ;
#44441 = ORIENTED_EDGE('',*,*,#30582,.F.) ;
#44442 = ORIENTED_EDGE('',*,*,#30583,.F.) ;
#44443 = ORIENTED_EDGE('',*,*,#30580,.T.) ;
#44444 = ORIENTED_EDGE('',*,*,#30490,.F.) ;
#44445 = ORIENTED_EDGE('',*,*,#30584,.T.) ;
#44446 = ORIENTED_EDGE('',*,*,#30585,.F.) ;
#44447 = ORIENTED_EDGE('',*,*,#30582,.T.) ;
#44448 = ORIENTED_EDGE('',*,*,#30493,.F.) ;
#44449 = ORIENTED_EDGE('',*,*,#30586,.F.) ;
#44450 = ORIENTED_EDGE('',*,*,#30587,.F.) ;
#44451 = ORIENTED_EDGE('',*,*,#30584,.F.) ;
#44452 = ORIENTED_EDGE('',*,*,#30496,.F.) ;
#44453 = ORIENTED_EDGE('',*,*,#30588,.F.) ;
#44454 = ORIENTED_EDGE('',*,*,#30589,.F.) ;
#44455 = ORIENTED_EDGE('',*,*,#30586,.T.) ;
#44456 = ORIENTED_EDGE('',*,*,#30499,.F.) ;
#44457 = ORIENTED_EDGE('',*,*,#30590,.F.) ;
#44458 = ORIENTED_EDGE('',*,*,#30591,.F.) ;
#44459 = ORIENTED_EDGE('',*,*,#30588,.T.) ;
#44460 = ORIENTED_EDGE('',*,*,#30502,.F.) ;
#44461 = ORIENTED_EDGE('',*,*,#30592,.T.) ;
#44462 = ORIENTED_EDGE('',*,*,#30593,.F.) ;
#44463 = ORIENTED_EDGE('',*,*,#30590,.T.) ;
#44464 = ORIENTED_EDGE('',*,*,#30505,.F.) ;
#44465 = ORIENTED_EDGE('',*,*,#30594,.F.) ;
#44466 = ORIENTED_EDGE('',*,*,#30595,.F.) ;
#44467 = ORIENTED_EDGE('',*,*,#30592,.F.) ;
#44468 = ORIENTED_EDGE('',*,*,#30508,.F.) ;
#44469 = ORIENTED_EDGE('',*,*,#30596,.F.) ;
#44470 = ORIENTED_EDGE('',*,*,#30597,.F.) ;
#44471 = ORIENTED_EDGE('',*,*,#30594,.T.) ;
#44472 = ORIENTED_EDGE('',*,*,#30511,.F.) ;
#44473 = ORIENTED_EDGE('',*,*,#30598,.F.) ;
#44474 = ORIENTED_EDGE('',*,*,#30599,.F.) ;
#44475 = ORIENTED_EDGE('',*,*,#30596,.T.) ;
#44476 = ORIENTED_EDGE('',*,*,#30514,.F.) ;
#44477 = ORIENTED_EDGE('',*,*,#30600,.T.) ;
#44478 = ORIENTED_EDGE('',*,*,#30601,.F.) ;
#44479 = ORIENTED_EDGE('',*,*,#30598,.T.) ;
#44480 = ORIENTED_EDGE('',*,*,#30517,.F.) ;
#44481 = ORIENTED_EDGE('',*,*,#30602,.F.) ;
#44482 = ORIENTED_EDGE('',*,*,#30603,.F.) ;
#44483 = ORIENTED_EDGE('',*,*,#30600,.F.) ;
#44484 = ORIENTED_EDGE('',*,*,#30520,.F.) ;
#44485 = ORIENTED_EDGE('',*,*,#30604,.F.) ;
#44486 = ORIENTED_EDGE('',*,*,#30605,.F.) ;
#44487 = ORIENTED_EDGE('',*,*,#30602,.T.) ;
#44488 = ORIENTED_EDGE('',*,*,#30523,.F.) ;
#44489 = ORIENTED_EDGE('',*,*,#30606,.F.) ;
#44490 = ORIENTED_EDGE('',*,*,#30607,.F.) ;
#44491 = ORIENTED_EDGE('',*,*,#30604,.T.) ;
#44492 = ORIENTED_EDGE('',*,*,#30526,.F.) ;
#44493 = ORIENTED_EDGE('',*,*,#30608,.T.) ;
#44494 = ORIENTED_EDGE('',*,*,#30609,.F.) ;
#44495 = ORIENTED_EDGE('',*,*,#30606,.T.) ;
#44496 = ORIENTED_EDGE('',*,*,#30529,.F.) ;
#44497 = ORIENTED_EDGE('',*,*,#30610,.F.) ;
#44498 = ORIENTED_EDGE('',*,*,#30611,.F.) ;
#44499 = ORIENTED_EDGE('',*,*,#30608,.F.) ;
#44500 = ORIENTED_EDGE('',*,*,#30532,.F.) ;
#44501 = ORIENTED_EDGE('',*,*,#30612,.F.) ;
#44502 = ORIENTED_EDGE('',*,*,#30613,.F.) ;
#44503 = ORIENTED_EDGE('',*,*,#30610,.T.) ;
#44504 = ORIENTED_EDGE('',*,*,#30535,.F.) ;
#44505 = ORIENTED_EDGE('',*,*,#30614,.F.) ;
#44506 = ORIENTED_EDGE('',*,*,#30615,.F.) ;
#44507 = ORIENTED_EDGE('',*,*,#30612,.T.) ;
#44508 = ORIENTED_EDGE('',*,*,#30299,.F.) ;
#44509 = ORIENTED_EDGE('',*,*,#30616,.T.) ;
#44510 = ORIENTED_EDGE('',*,*,#30617,.F.) ;
#44511 = ORIENTED_EDGE('',*,*,#30614,.T.) ;
#44512 = ORIENTED_EDGE('',*,*,#30428,.F.) ;
#44513 = ORIENTED_EDGE('',*,*,#30425,.F.) ;
#44514 = ORIENTED_EDGE('',*,*,#30422,.F.) ;
#44515 = ORIENTED_EDGE('',*,*,#30618,.F.) ;
#44516 = ORIENTED_EDGE('',*,*,#30440,.F.) ;
#44517 = ORIENTED_EDGE('',*,*,#30437,.F.) ;
#44518 = ORIENTED_EDGE('',*,*,#30434,.F.) ;
#44519 = ORIENTED_EDGE('',*,*,#30619,.F.) ;
#44520 = ORIENTED_EDGE('',*,*,#30409,.F.) ;
#44521 = ORIENTED_EDGE('',*,*,#30620,.F.) ;
#44522 = ORIENTED_EDGE('',*,*,#30415,.F.) ;
#44523 = ORIENTED_EDGE('',*,*,#30412,.F.) ;
#44524 = ORIENTED_EDGE('',*,*,#30452,.F.) ;
#44525 = ORIENTED_EDGE('',*,*,#30449,.F.) ;
#44526 = ORIENTED_EDGE('',*,*,#30446,.F.) ;
#44527 = ORIENTED_EDGE('',*,*,#30621,.F.) ;
#44528 = ORIENTED_EDGE('',*,*,#30397,.F.) ;
#44529 = ORIENTED_EDGE('',*,*,#30622,.F.) ;
#44530 = ORIENTED_EDGE('',*,*,#30403,.F.) ;
#44531 = ORIENTED_EDGE('',*,*,#30400,.F.) ;
#44532 = ORIENTED_EDGE('',*,*,#30464,.F.) ;
#44533 = ORIENTED_EDGE('',*,*,#30461,.F.) ;
#44534 = ORIENTED_EDGE('',*,*,#30458,.F.) ;
#44535 = ORIENTED_EDGE('',*,*,#30623,.F.) ;
#44536 = ORIENTED_EDGE('',*,*,#30385,.F.) ;
#44537 = ORIENTED_EDGE('',*,*,#30624,.F.) ;
#44538 = ORIENTED_EDGE('',*,*,#30391,.F.) ;
#44539 = ORIENTED_EDGE('',*,*,#30388,.F.) ;
#44540 = ORIENTED_EDGE('',*,*,#30476,.F.) ;
#44541 = ORIENTED_EDGE('',*,*,#30473,.F.) ;
#44542 = ORIENTED_EDGE('',*,*,#30470,.F.) ;
#44543 = ORIENTED_EDGE('',*,*,#30625,.F.) ;
#44544 = ORIENTED_EDGE('',*,*,#30373,.F.) ;
#44545 = ORIENTED_EDGE('',*,*,#30626,.F.) ;
#44546 = ORIENTED_EDGE('',*,*,#30379,.F.) ;
#44547 = ORIENTED_EDGE('',*,*,#30376,.F.) ;
#44548 = ORIENTED_EDGE('',*,*,#30488,.F.) ;
#44549 = ORIENTED_EDGE('',*,*,#30485,.F.) ;
#44550 = ORIENTED_EDGE('',*,*,#30482,.F.) ;
#44551 = ORIENTED_EDGE('',*,*,#30627,.F.) ;
#44552 = ORIENTED_EDGE('',*,*,#30361,.F.) ;
#44553 = ORIENTED_EDGE('',*,*,#30628,.F.) ;
#44554 = ORIENTED_EDGE('',*,*,#30367,.F.) ;
#44555 = ORIENTED_EDGE('',*,*,#30364,.F.) ;
#44556 = ORIENTED_EDGE('',*,*,#30500,.F.) ;
#44557 = ORIENTED_EDGE('',*,*,#30497,.F.) ;
#44558 = ORIENTED_EDGE('',*,*,#30494,.F.) ;
#44559 = ORIENTED_EDGE('',*,*,#30629,.F.) ;
#44560 = ORIENTED_EDGE('',*,*,#30349,.F.) ;
#44561 = ORIENTED_EDGE('',*,*,#30630,.F.) ;
#44562 = ORIENTED_EDGE('',*,*,#30355,.F.) ;
#44563 = ORIENTED_EDGE('',*,*,#30352,.F.) ;
#44564 = ORIENTED_EDGE('',*,*,#30512,.F.) ;
#44565 = ORIENTED_EDGE('',*,*,#30509,.F.) ;
#44566 = ORIENTED_EDGE('',*,*,#30506,.F.) ;
#44567 = ORIENTED_EDGE('',*,*,#30631,.F.) ;
#44568 = ORIENTED_EDGE('',*,*,#30337,.F.) ;
#44569 = ORIENTED_EDGE('',*,*,#30632,.F.) ;
#44570 = ORIENTED_EDGE('',*,*,#30343,.F.) ;
#44571 = ORIENTED_EDGE('',*,*,#30340,.F.) ;
#44572 = ORIENTED_EDGE('',*,*,#30524,.F.) ;
#44573 = ORIENTED_EDGE('',*,*,#30521,.F.) ;
#44574 = ORIENTED_EDGE('',*,*,#30518,.F.) ;
#44575 = ORIENTED_EDGE('',*,*,#30633,.F.) ;
#44576 = ORIENTED_EDGE('',*,*,#30325,.F.) ;
#44577 = ORIENTED_EDGE('',*,*,#30634,.F.) ;
#44578 = ORIENTED_EDGE('',*,*,#30331,.F.) ;
#44579 = ORIENTED_EDGE('',*,*,#30328,.F.) ;
#44580 = ORIENTED_EDGE('',*,*,#30536,.F.) ;
#44581 = ORIENTED_EDGE('',*,*,#30533,.F.) ;
#44582 = ORIENTED_EDGE('',*,*,#30530,.F.) ;
#44583 = ORIENTED_EDGE('',*,*,#30635,.F.) ;
#44584 = ORIENTED_EDGE('',*,*,#30313,.F.) ;
#44585 = ORIENTED_EDGE('',*,*,#30636,.F.) ;
#44586 = ORIENTED_EDGE('',*,*,#30637,.F.) ;
#44587 = ORIENTED_EDGE('',*,*,#30319,.F.) ;
#44588 = ORIENTED_EDGE('',*,*,#30316,.F.) ;
#44589 = ORIENTED_EDGE('',*,*,#30292,.F.) ;
#44590 = ORIENTED_EDGE('',*,*,#30293,.F.) ;
#44591 = ORIENTED_EDGE('',*,*,#30638,.T.) ;
#44592 = ORIENTED_EDGE('',*,*,#30636,.T.) ;
#44593 = ORIENTED_EDGE('',*,*,#30310,.T.) ;
#44594 = ORIENTED_EDGE('',*,*,#30639,.T.) ;
#44595 = ORIENTED_EDGE('',*,*,#30297,.T.) ;
#44596 = ORIENTED_EDGE('',*,*,#30635,.T.) ;
#44597 = ORIENTED_EDGE('',*,*,#30527,.T.) ;
#44598 = ORIENTED_EDGE('',*,*,#30633,.T.) ;
#44599 = ORIENTED_EDGE('',*,*,#30515,.T.) ;
#44600 = ORIENTED_EDGE('',*,*,#30631,.T.) ;
#44601 = ORIENTED_EDGE('',*,*,#30503,.T.) ;
#44602 = ORIENTED_EDGE('',*,*,#30629,.T.) ;
#44603 = ORIENTED_EDGE('',*,*,#30491,.T.) ;
#44604 = ORIENTED_EDGE('',*,*,#30627,.T.) ;
#44605 = ORIENTED_EDGE('',*,*,#30479,.T.) ;
#44606 = ORIENTED_EDGE('',*,*,#30625,.T.) ;
#44607 = ORIENTED_EDGE('',*,*,#30467,.T.) ;
#44608 = ORIENTED_EDGE('',*,*,#30623,.T.) ;
#44609 = ORIENTED_EDGE('',*,*,#30455,.T.) ;
#44610 = ORIENTED_EDGE('',*,*,#30621,.T.) ;
#44611 = ORIENTED_EDGE('',*,*,#30443,.T.) ;
#44612 = ORIENTED_EDGE('',*,*,#30619,.T.) ;
#44613 = ORIENTED_EDGE('',*,*,#30431,.T.) ;
#44614 = ORIENTED_EDGE('',*,*,#30618,.T.) ;
#44615 = ORIENTED_EDGE('',*,*,#30418,.T.) ;
#44616 = ORIENTED_EDGE('',*,*,#30620,.T.) ;
#44617 = ORIENTED_EDGE('',*,*,#30406,.T.) ;
#44618 = ORIENTED_EDGE('',*,*,#30622,.T.) ;
#44619 = ORIENTED_EDGE('',*,*,#30394,.T.) ;
#44620 = ORIENTED_EDGE('',*,*,#30624,.T.) ;
#44621 = ORIENTED_EDGE('',*,*,#30382,.T.) ;
#44622 = ORIENTED_EDGE('',*,*,#30626,.T.) ;
#44623 = ORIENTED_EDGE('',*,*,#30370,.T.) ;
#44624 = ORIENTED_EDGE('',*,*,#30628,.T.) ;
#44625 = ORIENTED_EDGE('',*,*,#30358,.T.) ;
#44626 = ORIENTED_EDGE('',*,*,#30630,.T.) ;
#44627 = ORIENTED_EDGE('',*,*,#30346,.T.) ;
#44628 = ORIENTED_EDGE('',*,*,#30632,.T.) ;
#44629 = ORIENTED_EDGE('',*,*,#30334,.T.) ;
#44630 = ORIENTED_EDGE('',*,*,#30634,.T.) ;
#44631 = ORIENTED_EDGE('',*,*,#30322,.T.) ;
#44632 = ORIENTED_EDGE('',*,*,#30637,.T.) ;
#44633 = ORIENTED_EDGE('',*,*,#30638,.F.) ;
#44634 = ORIENTED_EDGE('',*,*,#30301,.F.) ;
#44635 = ORIENTED_EDGE('',*,*,#30639,.F.) ;
#44636 = ORIENTED_EDGE('',*,*,#30307,.F.) ;
#44637 = ORIENTED_EDGE('',*,*,#30304,.F.) ;
#44638 = ORIENTED_EDGE('',*,*,#30295,.F.) ;
#44639 = ORIENTED_EDGE('',*,*,#30296,.F.) ;
#44640 = ORIENTED_EDGE('',*,*,#30640,.T.) ;
#44641 = ORIENTED_EDGE('',*,*,#30641,.T.) ;
#44642 = ORIENTED_EDGE('',*,*,#30642,.F.) ;
#44643 = ORIENTED_EDGE('',*,*,#30643,.T.) ;
#44644 = ORIENTED_EDGE('',*,*,#30644,.F.) ;
#44645 = ORIENTED_EDGE('',*,*,#30645,.T.) ;
#44646 = ORIENTED_EDGE('',*,*,#30646,.F.) ;
#44647 = ORIENTED_EDGE('',*,*,#30647,.T.) ;
#44648 = ORIENTED_EDGE('',*,*,#30648,.F.) ;
#44649 = ORIENTED_EDGE('',*,*,#30649,.T.) ;
#44650 = ORIENTED_EDGE('',*,*,#30650,.F.) ;
#44651 = ORIENTED_EDGE('',*,*,#30651,.T.) ;
#44652 = ORIENTED_EDGE('',*,*,#30652,.F.) ;
#44653 = ORIENTED_EDGE('',*,*,#30653,.T.) ;
#44654 = ORIENTED_EDGE('',*,*,#30654,.F.) ;
#44655 = ORIENTED_EDGE('',*,*,#30655,.T.) ;
#44656 = ORIENTED_EDGE('',*,*,#30656,.F.) ;
#44657 = ORIENTED_EDGE('',*,*,#30657,.T.) ;
#44658 = ORIENTED_EDGE('',*,*,#30658,.F.) ;
#44659 = ORIENTED_EDGE('',*,*,#30659,.T.) ;
#44660 = ORIENTED_EDGE('',*,*,#30660,.F.) ;
#44661 = ORIENTED_EDGE('',*,*,#30661,.T.) ;
#44662 = ORIENTED_EDGE('',*,*,#30662,.F.) ;
#44663 = ORIENTED_EDGE('',*,*,#30663,.T.) ;
#44664 = ORIENTED_EDGE('',*,*,#30664,.F.) ;
#44665 = ORIENTED_EDGE('',*,*,#30665,.T.) ;
#44666 = ORIENTED_EDGE('',*,*,#30666,.F.) ;
#44667 = ORIENTED_EDGE('',*,*,#30667,.T.) ;
#44668 = ORIENTED_EDGE('',*,*,#30668,.F.) ;
#44669 = ORIENTED_EDGE('',*,*,#30669,.T.) ;
#44670 = ORIENTED_EDGE('',*,*,#30670,.F.) ;
#44671 = ORIENTED_EDGE('',*,*,#30671,.T.) ;
#44672 = ORIENTED_EDGE('',*,*,#30672,.F.) ;
#44673 = ORIENTED_EDGE('',*,*,#30673,.T.) ;
#44674 = ORIENTED_EDGE('',*,*,#30674,.F.) ;
#44675 = ORIENTED_EDGE('',*,*,#30675,.T.) ;
#44676 = ORIENTED_EDGE('',*,*,#30676,.F.) ;
#44677 = ORIENTED_EDGE('',*,*,#30677,.T.) ;
#44678 = ORIENTED_EDGE('',*,*,#30678,.F.) ;
#44679 = ORIENTED_EDGE('',*,*,#30679,.T.) ;
#44680 = ORIENTED_EDGE('',*,*,#30680,.F.) ;
#44681 = ORIENTED_EDGE('',*,*,#30681,.T.) ;
#44682 = ORIENTED_EDGE('',*,*,#30640,.F.) ;
#44683 = ORIENTED_EDGE('',*,*,#30679,.F.) ;
#44684 = ORIENTED_EDGE('',*,*,#30682,.F.) ;
#44685 = ORIENTED_EDGE('',*,*,#30683,.F.) ;
#44686 = ORIENTED_EDGE('',*,*,#30684,.F.) ;
#44687 = ORIENTED_EDGE('',*,*,#30677,.F.) ;
#44688 = ORIENTED_EDGE('',*,*,#30685,.F.) ;
#44689 = ORIENTED_EDGE('',*,*,#30686,.F.) ;
#44690 = ORIENTED_EDGE('',*,*,#30687,.F.) ;
#44691 = ORIENTED_EDGE('',*,*,#30675,.F.) ;
#44692 = ORIENTED_EDGE('',*,*,#30688,.F.) ;
#44693 = ORIENTED_EDGE('',*,*,#30689,.F.) ;
#44694 = ORIENTED_EDGE('',*,*,#30690,.F.) ;
#44695 = ORIENTED_EDGE('',*,*,#30673,.F.) ;
#44696 = ORIENTED_EDGE('',*,*,#30691,.F.) ;
#44697 = ORIENTED_EDGE('',*,*,#30692,.F.) ;
#44698 = ORIENTED_EDGE('',*,*,#30693,.F.) ;
#44699 = ORIENTED_EDGE('',*,*,#30671,.F.) ;
#44700 = ORIENTED_EDGE('',*,*,#30694,.F.) ;
#44701 = ORIENTED_EDGE('',*,*,#30695,.F.) ;
#44702 = ORIENTED_EDGE('',*,*,#30696,.F.) ;
#44703 = ORIENTED_EDGE('',*,*,#30669,.F.) ;
#44704 = ORIENTED_EDGE('',*,*,#30697,.F.) ;
#44705 = ORIENTED_EDGE('',*,*,#30698,.F.) ;
#44706 = ORIENTED_EDGE('',*,*,#30699,.F.) ;
#44707 = ORIENTED_EDGE('',*,*,#30667,.F.) ;
#44708 = ORIENTED_EDGE('',*,*,#30700,.F.) ;
#44709 = ORIENTED_EDGE('',*,*,#30701,.F.) ;
#44710 = ORIENTED_EDGE('',*,*,#30702,.F.) ;
#44711 = ORIENTED_EDGE('',*,*,#30665,.F.) ;
#44712 = ORIENTED_EDGE('',*,*,#30703,.F.) ;
#44713 = ORIENTED_EDGE('',*,*,#30704,.F.) ;
#44714 = ORIENTED_EDGE('',*,*,#30705,.F.) ;
#44715 = ORIENTED_EDGE('',*,*,#30663,.F.) ;
#44716 = ORIENTED_EDGE('',*,*,#30706,.F.) ;
#44717 = ORIENTED_EDGE('',*,*,#30707,.F.) ;
#44718 = ORIENTED_EDGE('',*,*,#30708,.F.) ;
#44719 = ORIENTED_EDGE('',*,*,#30661,.F.) ;
#44720 = ORIENTED_EDGE('',*,*,#30709,.F.) ;
#44721 = ORIENTED_EDGE('',*,*,#30710,.F.) ;
#44722 = ORIENTED_EDGE('',*,*,#30711,.F.) ;
#44723 = ORIENTED_EDGE('',*,*,#30659,.F.) ;
#44724 = ORIENTED_EDGE('',*,*,#30712,.F.) ;
#44725 = ORIENTED_EDGE('',*,*,#30713,.F.) ;
#44726 = ORIENTED_EDGE('',*,*,#30714,.F.) ;
#44727 = ORIENTED_EDGE('',*,*,#30657,.F.) ;
#44728 = ORIENTED_EDGE('',*,*,#30715,.F.) ;
#44729 = ORIENTED_EDGE('',*,*,#30716,.F.) ;
#44730 = ORIENTED_EDGE('',*,*,#30717,.F.) ;
#44731 = ORIENTED_EDGE('',*,*,#30655,.F.) ;
#44732 = ORIENTED_EDGE('',*,*,#30718,.F.) ;
#44733 = ORIENTED_EDGE('',*,*,#30719,.F.) ;
#44734 = ORIENTED_EDGE('',*,*,#30720,.F.) ;
#44735 = ORIENTED_EDGE('',*,*,#30653,.F.) ;
#44736 = ORIENTED_EDGE('',*,*,#30721,.F.) ;
#44737 = ORIENTED_EDGE('',*,*,#30722,.F.) ;
#44738 = ORIENTED_EDGE('',*,*,#30723,.F.) ;
#44739 = ORIENTED_EDGE('',*,*,#30651,.F.) ;
#44740 = ORIENTED_EDGE('',*,*,#30724,.F.) ;
#44741 = ORIENTED_EDGE('',*,*,#30725,.F.) ;
#44742 = ORIENTED_EDGE('',*,*,#30726,.F.) ;
#44743 = ORIENTED_EDGE('',*,*,#30649,.F.) ;
#44744 = ORIENTED_EDGE('',*,*,#30727,.F.) ;
#44745 = ORIENTED_EDGE('',*,*,#30728,.F.) ;
#44746 = ORIENTED_EDGE('',*,*,#30729,.F.) ;
#44747 = ORIENTED_EDGE('',*,*,#30647,.F.) ;
#44748 = ORIENTED_EDGE('',*,*,#30730,.F.) ;
#44749 = ORIENTED_EDGE('',*,*,#30731,.F.) ;
#44750 = ORIENTED_EDGE('',*,*,#30732,.F.) ;
#44751 = ORIENTED_EDGE('',*,*,#30645,.F.) ;
#44752 = ORIENTED_EDGE('',*,*,#30733,.F.) ;
#44753 = ORIENTED_EDGE('',*,*,#30734,.F.) ;
#44754 = ORIENTED_EDGE('',*,*,#30735,.F.) ;
#44755 = ORIENTED_EDGE('',*,*,#30643,.F.) ;
#44756 = ORIENTED_EDGE('',*,*,#30736,.F.) ;
#44757 = ORIENTED_EDGE('',*,*,#30737,.F.) ;
#44758 = ORIENTED_EDGE('',*,*,#30738,.F.) ;
#44759 = ORIENTED_EDGE('',*,*,#30681,.F.) ;
#44760 = ORIENTED_EDGE('',*,*,#30739,.F.) ;
#44761 = ORIENTED_EDGE('',*,*,#30740,.F.) ;
#44762 = ORIENTED_EDGE('',*,*,#30741,.F.) ;
#44763 = ORIENTED_EDGE('',*,*,#30641,.F.) ;
#44764 = ORIENTED_EDGE('',*,*,#30660,.T.) ;
#44765 = ORIENTED_EDGE('',*,*,#30742,.T.) ;
#44766 = ORIENTED_EDGE('',*,*,#30743,.T.) ;
#44767 = ORIENTED_EDGE('',*,*,#30744,.F.) ;
#44768 = ORIENTED_EDGE('',*,*,#30714,.T.) ;
#44769 = ORIENTED_EDGE('',*,*,#30745,.T.) ;
#44770 = ORIENTED_EDGE('',*,*,#30746,.T.) ;
#44771 = ORIENTED_EDGE('',*,*,#30742,.F.) ;
#44772 = ORIENTED_EDGE('',*,*,#30747,.T.) ;
#44773 = ORIENTED_EDGE('',*,*,#30748,.T.) ;
#44774 = ORIENTED_EDGE('',*,*,#30709,.T.) ;
#44775 = ORIENTED_EDGE('',*,*,#30744,.T.) ;
#44776 = ORIENTED_EDGE('',*,*,#30712,.T.) ;
#44777 = ORIENTED_EDGE('',*,*,#30749,.T.) ;
#44778 = ORIENTED_EDGE('',*,*,#30750,.T.) ;
#44779 = ORIENTED_EDGE('',*,*,#30751,.T.) ;
#44780 = ORIENTED_EDGE('',*,*,#30658,.T.) ;
#44781 = ORIENTED_EDGE('',*,*,#30752,.T.) ;
#44782 = ORIENTED_EDGE('',*,*,#30617,.T.) ;
#44783 = ORIENTED_EDGE('',*,*,#30749,.F.) ;
#44784 = ORIENTED_EDGE('',*,*,#30717,.T.) ;
#44785 = ORIENTED_EDGE('',*,*,#30753,.T.) ;
#44786 = ORIENTED_EDGE('',*,*,#30615,.T.) ;
#44787 = ORIENTED_EDGE('',*,*,#30752,.F.) ;
#44788 = ORIENTED_EDGE('',*,*,#30754,.T.) ;
#44789 = ORIENTED_EDGE('',*,*,#30755,.T.) ;
#44790 = ORIENTED_EDGE('',*,*,#30706,.T.) ;
#44791 = ORIENTED_EDGE('',*,*,#30756,.T.) ;
#44792 = ORIENTED_EDGE('',*,*,#30715,.T.) ;
#44793 = ORIENTED_EDGE('',*,*,#30757,.T.) ;
#44794 = ORIENTED_EDGE('',*,*,#30611,.T.) ;
#44795 = ORIENTED_EDGE('',*,*,#30758,.T.) ;
#44796 = ORIENTED_EDGE('',*,*,#30656,.T.) ;
#44797 = ORIENTED_EDGE('',*,*,#30759,.T.) ;
#44798 = ORIENTED_EDGE('',*,*,#30609,.T.) ;
#44799 = ORIENTED_EDGE('',*,*,#30757,.F.) ;
#44800 = ORIENTED_EDGE('',*,*,#30720,.T.) ;
#44801 = ORIENTED_EDGE('',*,*,#30760,.T.) ;
#44802 = ORIENTED_EDGE('',*,*,#30607,.T.) ;
#44803 = ORIENTED_EDGE('',*,*,#30759,.F.) ;
#44804 = ORIENTED_EDGE('',*,*,#30761,.T.) ;
#44805 = ORIENTED_EDGE('',*,*,#30762,.T.) ;
#44806 = ORIENTED_EDGE('',*,*,#30703,.T.) ;
#44807 = ORIENTED_EDGE('',*,*,#30763,.T.) ;
#44808 = ORIENTED_EDGE('',*,*,#30718,.T.) ;
#44809 = ORIENTED_EDGE('',*,*,#30764,.T.) ;
#44810 = ORIENTED_EDGE('',*,*,#30603,.T.) ;
#44811 = ORIENTED_EDGE('',*,*,#30765,.T.) ;
#44812 = ORIENTED_EDGE('',*,*,#30654,.T.) ;
#44813 = ORIENTED_EDGE('',*,*,#30766,.T.) ;
#44814 = ORIENTED_EDGE('',*,*,#30601,.T.) ;
#44815 = ORIENTED_EDGE('',*,*,#30764,.F.) ;
#44816 = ORIENTED_EDGE('',*,*,#30723,.T.) ;
#44817 = ORIENTED_EDGE('',*,*,#30767,.T.) ;
#44818 = ORIENTED_EDGE('',*,*,#30599,.T.) ;
#44819 = ORIENTED_EDGE('',*,*,#30766,.F.) ;
#44820 = ORIENTED_EDGE('',*,*,#30768,.T.) ;
#44821 = ORIENTED_EDGE('',*,*,#30769,.T.) ;
#44822 = ORIENTED_EDGE('',*,*,#30700,.T.) ;
#44823 = ORIENTED_EDGE('',*,*,#30770,.T.) ;
#44824 = ORIENTED_EDGE('',*,*,#30721,.T.) ;
#44825 = ORIENTED_EDGE('',*,*,#30771,.T.) ;
#44826 = ORIENTED_EDGE('',*,*,#30595,.T.) ;
#44827 = ORIENTED_EDGE('',*,*,#30772,.T.) ;
#44828 = ORIENTED_EDGE('',*,*,#30652,.T.) ;
#44829 = ORIENTED_EDGE('',*,*,#30773,.T.) ;
#44830 = ORIENTED_EDGE('',*,*,#30593,.T.) ;
#44831 = ORIENTED_EDGE('',*,*,#30771,.F.) ;
#44832 = ORIENTED_EDGE('',*,*,#30726,.T.) ;
#44833 = ORIENTED_EDGE('',*,*,#30774,.T.) ;
#44834 = ORIENTED_EDGE('',*,*,#30591,.T.) ;
#44835 = ORIENTED_EDGE('',*,*,#30773,.F.) ;
#44836 = ORIENTED_EDGE('',*,*,#30775,.T.) ;
#44837 = ORIENTED_EDGE('',*,*,#30776,.T.) ;
#44838 = ORIENTED_EDGE('',*,*,#30697,.T.) ;
#44839 = ORIENTED_EDGE('',*,*,#30777,.T.) ;
#44840 = ORIENTED_EDGE('',*,*,#30724,.T.) ;
#44841 = ORIENTED_EDGE('',*,*,#30778,.T.) ;
#44842 = ORIENTED_EDGE('',*,*,#30587,.T.) ;
#44843 = ORIENTED_EDGE('',*,*,#30779,.T.) ;
#44844 = ORIENTED_EDGE('',*,*,#30650,.T.) ;
#44845 = ORIENTED_EDGE('',*,*,#30780,.T.) ;
#44846 = ORIENTED_EDGE('',*,*,#30585,.T.) ;
#44847 = ORIENTED_EDGE('',*,*,#30778,.F.) ;
#44848 = ORIENTED_EDGE('',*,*,#30729,.T.) ;
#44849 = ORIENTED_EDGE('',*,*,#30781,.T.) ;
#44850 = ORIENTED_EDGE('',*,*,#30583,.T.) ;
#44851 = ORIENTED_EDGE('',*,*,#30780,.F.) ;
#44852 = ORIENTED_EDGE('',*,*,#30782,.T.) ;
#44853 = ORIENTED_EDGE('',*,*,#30783,.T.) ;
#44854 = ORIENTED_EDGE('',*,*,#30694,.T.) ;
#44855 = ORIENTED_EDGE('',*,*,#30784,.T.) ;
#44856 = ORIENTED_EDGE('',*,*,#30727,.T.) ;
#44857 = ORIENTED_EDGE('',*,*,#30785,.T.) ;
#44858 = ORIENTED_EDGE('',*,*,#30579,.T.) ;
#44859 = ORIENTED_EDGE('',*,*,#30786,.T.) ;
#44860 = ORIENTED_EDGE('',*,*,#30648,.T.) ;
#44861 = ORIENTED_EDGE('',*,*,#30787,.T.) ;
#44862 = ORIENTED_EDGE('',*,*,#30577,.T.) ;
#44863 = ORIENTED_EDGE('',*,*,#30785,.F.) ;
#44864 = ORIENTED_EDGE('',*,*,#30732,.T.) ;
#44865 = ORIENTED_EDGE('',*,*,#30788,.T.) ;
#44866 = ORIENTED_EDGE('',*,*,#30575,.T.) ;
#44867 = ORIENTED_EDGE('',*,*,#30787,.F.) ;
#44868 = ORIENTED_EDGE('',*,*,#30789,.T.) ;
#44869 = ORIENTED_EDGE('',*,*,#30790,.T.) ;
#44870 = ORIENTED_EDGE('',*,*,#30691,.T.) ;
#44871 = ORIENTED_EDGE('',*,*,#30791,.T.) ;
#44872 = ORIENTED_EDGE('',*,*,#30730,.T.) ;
#44873 = ORIENTED_EDGE('',*,*,#30792,.T.) ;
#44874 = ORIENTED_EDGE('',*,*,#30571,.T.) ;
#44875 = ORIENTED_EDGE('',*,*,#30793,.T.) ;
#44876 = ORIENTED_EDGE('',*,*,#30646,.T.) ;
#44877 = ORIENTED_EDGE('',*,*,#30794,.T.) ;
#44878 = ORIENTED_EDGE('',*,*,#30569,.T.) ;
#44879 = ORIENTED_EDGE('',*,*,#30792,.F.) ;
#44880 = ORIENTED_EDGE('',*,*,#30735,.T.) ;
#44881 = ORIENTED_EDGE('',*,*,#30795,.T.) ;
#44882 = ORIENTED_EDGE('',*,*,#30567,.T.) ;
#44883 = ORIENTED_EDGE('',*,*,#30794,.F.) ;
#44884 = ORIENTED_EDGE('',*,*,#30796,.T.) ;
#44885 = ORIENTED_EDGE('',*,*,#30797,.T.) ;
#44886 = ORIENTED_EDGE('',*,*,#30688,.T.) ;
#44887 = ORIENTED_EDGE('',*,*,#30798,.T.) ;
#44888 = ORIENTED_EDGE('',*,*,#30733,.T.) ;
#44889 = ORIENTED_EDGE('',*,*,#30799,.T.) ;
#44890 = ORIENTED_EDGE('',*,*,#30563,.T.) ;
#44891 = ORIENTED_EDGE('',*,*,#30800,.T.) ;
#44892 = ORIENTED_EDGE('',*,*,#30644,.T.) ;
#44893 = ORIENTED_EDGE('',*,*,#30801,.T.) ;
#44894 = ORIENTED_EDGE('',*,*,#30561,.T.) ;
#44895 = ORIENTED_EDGE('',*,*,#30799,.F.) ;
#44896 = ORIENTED_EDGE('',*,*,#30738,.T.) ;
#44897 = ORIENTED_EDGE('',*,*,#30802,.T.) ;
#44898 = ORIENTED_EDGE('',*,*,#30559,.T.) ;
#44899 = ORIENTED_EDGE('',*,*,#30801,.F.) ;
#44900 = ORIENTED_EDGE('',*,*,#30803,.T.) ;
#44901 = ORIENTED_EDGE('',*,*,#30804,.T.) ;
#44902 = ORIENTED_EDGE('',*,*,#30685,.T.) ;
#44903 = ORIENTED_EDGE('',*,*,#30805,.T.) ;
#44904 = ORIENTED_EDGE('',*,*,#30736,.T.) ;
#44905 = ORIENTED_EDGE('',*,*,#30806,.T.) ;
#44906 = ORIENTED_EDGE('',*,*,#30555,.T.) ;
#44907 = ORIENTED_EDGE('',*,*,#30807,.T.) ;
#44908 = ORIENTED_EDGE('',*,*,#30642,.T.) ;
#44909 = ORIENTED_EDGE('',*,*,#30808,.T.) ;
#44910 = ORIENTED_EDGE('',*,*,#30553,.T.) ;
#44911 = ORIENTED_EDGE('',*,*,#30806,.F.) ;
#44912 = ORIENTED_EDGE('',*,*,#30741,.T.) ;
#44913 = ORIENTED_EDGE('',*,*,#30809,.T.) ;
#44914 = ORIENTED_EDGE('',*,*,#30551,.T.) ;
#44915 = ORIENTED_EDGE('',*,*,#30808,.F.) ;
#44916 = ORIENTED_EDGE('',*,*,#30538,.T.) ;
#44917 = ORIENTED_EDGE('',*,*,#30810,.T.) ;
#44918 = ORIENTED_EDGE('',*,*,#30682,.T.) ;
#44919 = ORIENTED_EDGE('',*,*,#30811,.T.) ;
#44920 = ORIENTED_EDGE('',*,*,#30739,.T.) ;
#44921 = ORIENTED_EDGE('',*,*,#30812,.T.) ;
#44922 = ORIENTED_EDGE('',*,*,#30547,.T.) ;
#44923 = ORIENTED_EDGE('',*,*,#30813,.T.) ;
#44924 = ORIENTED_EDGE('',*,*,#30680,.T.) ;
#44925 = ORIENTED_EDGE('',*,*,#30814,.T.) ;
#44926 = ORIENTED_EDGE('',*,*,#30545,.T.) ;
#44927 = ORIENTED_EDGE('',*,*,#30812,.F.) ;
#44928 = ORIENTED_EDGE('',*,*,#30543,.T.) ;
#44929 = ORIENTED_EDGE('',*,*,#30814,.F.) ;
#44930 = ORIENTED_EDGE('',*,*,#30684,.T.) ;
#44931 = ORIENTED_EDGE('',*,*,#30815,.T.) ;
#44932 = ORIENTED_EDGE('',*,*,#30541,.T.) ;
#44933 = ORIENTED_EDGE('',*,*,#30815,.F.) ;
#44934 = ORIENTED_EDGE('',*,*,#30683,.T.) ;
#44935 = ORIENTED_EDGE('',*,*,#30810,.F.) ;
#44936 = ORIENTED_EDGE('',*,*,#30740,.T.) ;
#44937 = ORIENTED_EDGE('',*,*,#30813,.F.) ;
#44938 = ORIENTED_EDGE('',*,*,#30549,.T.) ;
#44939 = ORIENTED_EDGE('',*,*,#30809,.F.) ;
#44940 = ORIENTED_EDGE('',*,*,#30816,.T.) ;
#44941 = ORIENTED_EDGE('',*,*,#30811,.F.) ;
#44942 = ORIENTED_EDGE('',*,*,#30678,.T.) ;
#44943 = ORIENTED_EDGE('',*,*,#30817,.T.) ;
#44944 = ORIENTED_EDGE('',*,*,#30818,.T.) ;
#44945 = ORIENTED_EDGE('',*,*,#30817,.F.) ;
#44946 = ORIENTED_EDGE('',*,*,#30687,.T.) ;
#44947 = ORIENTED_EDGE('',*,*,#30819,.T.) ;
#44948 = ORIENTED_EDGE('',*,*,#30820,.T.) ;
#44949 = ORIENTED_EDGE('',*,*,#30819,.F.) ;
#44950 = ORIENTED_EDGE('',*,*,#30686,.T.) ;
#44951 = ORIENTED_EDGE('',*,*,#30804,.F.) ;
#44952 = ORIENTED_EDGE('',*,*,#30737,.T.) ;
#44953 = ORIENTED_EDGE('',*,*,#30807,.F.) ;
#44954 = ORIENTED_EDGE('',*,*,#30557,.T.) ;
#44955 = ORIENTED_EDGE('',*,*,#30802,.F.) ;
#44956 = ORIENTED_EDGE('',*,*,#30821,.T.) ;
#44957 = ORIENTED_EDGE('',*,*,#30805,.F.) ;
#44958 = ORIENTED_EDGE('',*,*,#30676,.T.) ;
#44959 = ORIENTED_EDGE('',*,*,#30822,.T.) ;
#44960 = ORIENTED_EDGE('',*,*,#30823,.T.) ;
#44961 = ORIENTED_EDGE('',*,*,#30822,.F.) ;
#44962 = ORIENTED_EDGE('',*,*,#30690,.T.) ;
#44963 = ORIENTED_EDGE('',*,*,#30824,.T.) ;
#44964 = ORIENTED_EDGE('',*,*,#30825,.T.) ;
#44965 = ORIENTED_EDGE('',*,*,#30824,.F.) ;
#44966 = ORIENTED_EDGE('',*,*,#30689,.T.) ;
#44967 = ORIENTED_EDGE('',*,*,#30797,.F.) ;
#44968 = ORIENTED_EDGE('',*,*,#30734,.T.) ;
#44969 = ORIENTED_EDGE('',*,*,#30800,.F.) ;
#44970 = ORIENTED_EDGE('',*,*,#30565,.T.) ;
#44971 = ORIENTED_EDGE('',*,*,#30795,.F.) ;
#44972 = ORIENTED_EDGE('',*,*,#30826,.T.) ;
#44973 = ORIENTED_EDGE('',*,*,#30798,.F.) ;
#44974 = ORIENTED_EDGE('',*,*,#30674,.T.) ;
#44975 = ORIENTED_EDGE('',*,*,#30827,.T.) ;
#44976 = ORIENTED_EDGE('',*,*,#30828,.T.) ;
#44977 = ORIENTED_EDGE('',*,*,#30827,.F.) ;
#44978 = ORIENTED_EDGE('',*,*,#30693,.T.) ;
#44979 = ORIENTED_EDGE('',*,*,#30829,.T.) ;
#44980 = ORIENTED_EDGE('',*,*,#30830,.T.) ;
#44981 = ORIENTED_EDGE('',*,*,#30829,.F.) ;
#44982 = ORIENTED_EDGE('',*,*,#30692,.T.) ;
#44983 = ORIENTED_EDGE('',*,*,#30790,.F.) ;
#44984 = ORIENTED_EDGE('',*,*,#30731,.T.) ;
#44985 = ORIENTED_EDGE('',*,*,#30793,.F.) ;
#44986 = ORIENTED_EDGE('',*,*,#30573,.T.) ;
#44987 = ORIENTED_EDGE('',*,*,#30788,.F.) ;
#44988 = ORIENTED_EDGE('',*,*,#30831,.T.) ;
#44989 = ORIENTED_EDGE('',*,*,#30791,.F.) ;
#44990 = ORIENTED_EDGE('',*,*,#30672,.T.) ;
#44991 = ORIENTED_EDGE('',*,*,#30832,.T.) ;
#44992 = ORIENTED_EDGE('',*,*,#30833,.T.) ;
#44993 = ORIENTED_EDGE('',*,*,#30832,.F.) ;
#44994 = ORIENTED_EDGE('',*,*,#30696,.T.) ;
#44995 = ORIENTED_EDGE('',*,*,#30834,.T.) ;
#44996 = ORIENTED_EDGE('',*,*,#30835,.T.) ;
#44997 = ORIENTED_EDGE('',*,*,#30834,.F.) ;
#44998 = ORIENTED_EDGE('',*,*,#30695,.T.) ;
#44999 = ORIENTED_EDGE('',*,*,#30783,.F.) ;
#45000 = ORIENTED_EDGE('',*,*,#30728,.T.) ;
#45001 = ORIENTED_EDGE('',*,*,#30786,.F.) ;
#45002 = ORIENTED_EDGE('',*,*,#30581,.T.) ;
#45003 = ORIENTED_EDGE('',*,*,#30781,.F.) ;
#45004 = ORIENTED_EDGE('',*,*,#30836,.T.) ;
#45005 = ORIENTED_EDGE('',*,*,#30784,.F.) ;
#45006 = ORIENTED_EDGE('',*,*,#30670,.T.) ;
#45007 = ORIENTED_EDGE('',*,*,#30837,.T.) ;
#45008 = ORIENTED_EDGE('',*,*,#30838,.T.) ;
#45009 = ORIENTED_EDGE('',*,*,#30837,.F.) ;
#45010 = ORIENTED_EDGE('',*,*,#30699,.T.) ;
#45011 = ORIENTED_EDGE('',*,*,#30839,.T.) ;
#45012 = ORIENTED_EDGE('',*,*,#30840,.T.) ;
#45013 = ORIENTED_EDGE('',*,*,#30839,.F.) ;
#45014 = ORIENTED_EDGE('',*,*,#30698,.T.) ;
#45015 = ORIENTED_EDGE('',*,*,#30776,.F.) ;
#45016 = ORIENTED_EDGE('',*,*,#30725,.T.) ;
#45017 = ORIENTED_EDGE('',*,*,#30779,.F.) ;
#45018 = ORIENTED_EDGE('',*,*,#30589,.T.) ;
#45019 = ORIENTED_EDGE('',*,*,#30774,.F.) ;
#45020 = ORIENTED_EDGE('',*,*,#30841,.T.) ;
#45021 = ORIENTED_EDGE('',*,*,#30777,.F.) ;
#45022 = ORIENTED_EDGE('',*,*,#30668,.T.) ;
#45023 = ORIENTED_EDGE('',*,*,#30842,.T.) ;
#45024 = ORIENTED_EDGE('',*,*,#30843,.T.) ;
#45025 = ORIENTED_EDGE('',*,*,#30842,.F.) ;
#45026 = ORIENTED_EDGE('',*,*,#30702,.T.) ;
#45027 = ORIENTED_EDGE('',*,*,#30844,.T.) ;
#45028 = ORIENTED_EDGE('',*,*,#30845,.T.) ;
#45029 = ORIENTED_EDGE('',*,*,#30844,.F.) ;
#45030 = ORIENTED_EDGE('',*,*,#30701,.T.) ;
#45031 = ORIENTED_EDGE('',*,*,#30769,.F.) ;
#45032 = ORIENTED_EDGE('',*,*,#30722,.T.) ;
#45033 = ORIENTED_EDGE('',*,*,#30772,.F.) ;
#45034 = ORIENTED_EDGE('',*,*,#30597,.T.) ;
#45035 = ORIENTED_EDGE('',*,*,#30767,.F.) ;
#45036 = ORIENTED_EDGE('',*,*,#30846,.T.) ;
#45037 = ORIENTED_EDGE('',*,*,#30770,.F.) ;
#45038 = ORIENTED_EDGE('',*,*,#30666,.T.) ;
#45039 = ORIENTED_EDGE('',*,*,#30847,.T.) ;
#45040 = ORIENTED_EDGE('',*,*,#30848,.T.) ;
#45041 = ORIENTED_EDGE('',*,*,#30847,.F.) ;
#45042 = ORIENTED_EDGE('',*,*,#30705,.T.) ;
#45043 = ORIENTED_EDGE('',*,*,#30849,.T.) ;
#45044 = ORIENTED_EDGE('',*,*,#30850,.T.) ;
#45045 = ORIENTED_EDGE('',*,*,#30849,.F.) ;
#45046 = ORIENTED_EDGE('',*,*,#30704,.T.) ;
#45047 = ORIENTED_EDGE('',*,*,#30762,.F.) ;
#45048 = ORIENTED_EDGE('',*,*,#30719,.T.) ;
#45049 = ORIENTED_EDGE('',*,*,#30765,.F.) ;
#45050 = ORIENTED_EDGE('',*,*,#30605,.T.) ;
#45051 = ORIENTED_EDGE('',*,*,#30760,.F.) ;
#45052 = ORIENTED_EDGE('',*,*,#30851,.T.) ;
#45053 = ORIENTED_EDGE('',*,*,#30763,.F.) ;
#45054 = ORIENTED_EDGE('',*,*,#30664,.T.) ;
#45055 = ORIENTED_EDGE('',*,*,#30852,.T.) ;
#45056 = ORIENTED_EDGE('',*,*,#30853,.T.) ;
#45057 = ORIENTED_EDGE('',*,*,#30852,.F.) ;
#45058 = ORIENTED_EDGE('',*,*,#30708,.T.) ;
#45059 = ORIENTED_EDGE('',*,*,#30854,.T.) ;
#45060 = ORIENTED_EDGE('',*,*,#30855,.T.) ;
#45061 = ORIENTED_EDGE('',*,*,#30854,.F.) ;
#45062 = ORIENTED_EDGE('',*,*,#30707,.T.) ;
#45063 = ORIENTED_EDGE('',*,*,#30755,.F.) ;
#45064 = ORIENTED_EDGE('',*,*,#30716,.T.) ;
#45065 = ORIENTED_EDGE('',*,*,#30758,.F.) ;
#45066 = ORIENTED_EDGE('',*,*,#30613,.T.) ;
#45067 = ORIENTED_EDGE('',*,*,#30753,.F.) ;
#45068 = ORIENTED_EDGE('',*,*,#30856,.T.) ;
#45069 = ORIENTED_EDGE('',*,*,#30756,.F.) ;
#45070 = ORIENTED_EDGE('',*,*,#30662,.T.) ;
#45071 = ORIENTED_EDGE('',*,*,#30857,.T.) ;
#45072 = ORIENTED_EDGE('',*,*,#30858,.T.) ;
#45073 = ORIENTED_EDGE('',*,*,#30857,.F.) ;
#45074 = ORIENTED_EDGE('',*,*,#30711,.T.) ;
#45075 = ORIENTED_EDGE('',*,*,#30859,.T.) ;
#45076 = ORIENTED_EDGE('',*,*,#30860,.T.) ;
#45077 = ORIENTED_EDGE('',*,*,#30859,.F.) ;
#45078 = ORIENTED_EDGE('',*,*,#30710,.T.) ;
#45079 = ORIENTED_EDGE('',*,*,#30748,.F.) ;
#45080 = ORIENTED_EDGE('',*,*,#30713,.T.) ;
#45081 = ORIENTED_EDGE('',*,*,#30751,.F.) ;
#45082 = ORIENTED_EDGE('',*,*,#30861,.T.) ;
#45083 = ORIENTED_EDGE('',*,*,#30745,.F.) ;
#45084 = ORIENTED_EDGE('',*,*,#30312,.F.) ;
#45085 = ORIENTED_EDGE('',*,*,#30862,.T.) ;
#45086 = ORIENTED_EDGE('',*,*,#30743,.F.) ;
#45087 = ORIENTED_EDGE('',*,*,#30863,.T.) ;
#45088 = ORIENTED_EDGE('',*,*,#30309,.F.) ;
#45089 = ORIENTED_EDGE('',*,*,#30863,.F.) ;
#45090 = ORIENTED_EDGE('',*,*,#30746,.F.) ;
#45091 = ORIENTED_EDGE('',*,*,#30864,.T.) ;
#45092 = ORIENTED_EDGE('',*,*,#30306,.F.) ;
#45093 = ORIENTED_EDGE('',*,*,#30864,.F.) ;
#45094 = ORIENTED_EDGE('',*,*,#30861,.F.) ;
#45095 = ORIENTED_EDGE('',*,*,#30865,.T.) ;
#45096 = ORIENTED_EDGE('',*,*,#30303,.F.) ;
#45097 = ORIENTED_EDGE('',*,*,#30865,.F.) ;
#45098 = ORIENTED_EDGE('',*,*,#30750,.F.) ;
#45099 = ORIENTED_EDGE('',*,*,#30616,.F.) ;
#45100 = ORIENTED_EDGE('',*,*,#30417,.F.) ;
#45101 = ORIENTED_EDGE('',*,*,#30866,.F.) ;
#45102 = ORIENTED_EDGE('',*,*,#30818,.F.) ;
#45103 = ORIENTED_EDGE('',*,*,#30867,.T.) ;
#45104 = ORIENTED_EDGE('',*,*,#30411,.F.) ;
#45105 = ORIENTED_EDGE('',*,*,#30868,.F.) ;
#45106 = ORIENTED_EDGE('',*,*,#30803,.F.) ;
#45107 = ORIENTED_EDGE('',*,*,#30869,.F.) ;
#45108 = ORIENTED_EDGE('',*,*,#30414,.F.) ;
#45109 = ORIENTED_EDGE('',*,*,#30867,.F.) ;
#45110 = ORIENTED_EDGE('',*,*,#30820,.F.) ;
#45111 = ORIENTED_EDGE('',*,*,#30868,.T.) ;
#45112 = ORIENTED_EDGE('',*,*,#30405,.F.) ;
#45113 = ORIENTED_EDGE('',*,*,#30870,.F.) ;
#45114 = ORIENTED_EDGE('',*,*,#30823,.F.) ;
#45115 = ORIENTED_EDGE('',*,*,#30871,.T.) ;
#45116 = ORIENTED_EDGE('',*,*,#30399,.F.) ;
#45117 = ORIENTED_EDGE('',*,*,#30872,.F.) ;
#45118 = ORIENTED_EDGE('',*,*,#30796,.F.) ;
#45119 = ORIENTED_EDGE('',*,*,#30873,.F.) ;
#45120 = ORIENTED_EDGE('',*,*,#30402,.F.) ;
#45121 = ORIENTED_EDGE('',*,*,#30871,.F.) ;
#45122 = ORIENTED_EDGE('',*,*,#30825,.F.) ;
#45123 = ORIENTED_EDGE('',*,*,#30872,.T.) ;
#45124 = ORIENTED_EDGE('',*,*,#30393,.F.) ;
#45125 = ORIENTED_EDGE('',*,*,#30874,.F.) ;
#45126 = ORIENTED_EDGE('',*,*,#30828,.F.) ;
#45127 = ORIENTED_EDGE('',*,*,#30875,.T.) ;
#45128 = ORIENTED_EDGE('',*,*,#30387,.F.) ;
#45129 = ORIENTED_EDGE('',*,*,#30876,.F.) ;
#45130 = ORIENTED_EDGE('',*,*,#30789,.F.) ;
#45131 = ORIENTED_EDGE('',*,*,#30877,.F.) ;
#45132 = ORIENTED_EDGE('',*,*,#30390,.F.) ;
#45133 = ORIENTED_EDGE('',*,*,#30875,.F.) ;
#45134 = ORIENTED_EDGE('',*,*,#30830,.F.) ;
#45135 = ORIENTED_EDGE('',*,*,#30876,.T.) ;
#45136 = ORIENTED_EDGE('',*,*,#30381,.F.) ;
#45137 = ORIENTED_EDGE('',*,*,#30878,.F.) ;
#45138 = ORIENTED_EDGE('',*,*,#30833,.F.) ;
#45139 = ORIENTED_EDGE('',*,*,#30879,.T.) ;
#45140 = ORIENTED_EDGE('',*,*,#30375,.F.) ;
#45141 = ORIENTED_EDGE('',*,*,#30880,.F.) ;
#45142 = ORIENTED_EDGE('',*,*,#30782,.F.) ;
#45143 = ORIENTED_EDGE('',*,*,#30881,.F.) ;
#45144 = ORIENTED_EDGE('',*,*,#30378,.F.) ;
#45145 = ORIENTED_EDGE('',*,*,#30879,.F.) ;
#45146 = ORIENTED_EDGE('',*,*,#30835,.F.) ;
#45147 = ORIENTED_EDGE('',*,*,#30880,.T.) ;
#45148 = ORIENTED_EDGE('',*,*,#30369,.F.) ;
#45149 = ORIENTED_EDGE('',*,*,#30882,.F.) ;
#45150 = ORIENTED_EDGE('',*,*,#30838,.F.) ;
#45151 = ORIENTED_EDGE('',*,*,#30883,.T.) ;
#45152 = ORIENTED_EDGE('',*,*,#30363,.F.) ;
#45153 = ORIENTED_EDGE('',*,*,#30884,.F.) ;
#45154 = ORIENTED_EDGE('',*,*,#30775,.F.) ;
#45155 = ORIENTED_EDGE('',*,*,#30885,.F.) ;
#45156 = ORIENTED_EDGE('',*,*,#30366,.F.) ;
#45157 = ORIENTED_EDGE('',*,*,#30883,.F.) ;
#45158 = ORIENTED_EDGE('',*,*,#30840,.F.) ;
#45159 = ORIENTED_EDGE('',*,*,#30884,.T.) ;
#45160 = ORIENTED_EDGE('',*,*,#30357,.F.) ;
#45161 = ORIENTED_EDGE('',*,*,#30886,.F.) ;
#45162 = ORIENTED_EDGE('',*,*,#30843,.F.) ;
#45163 = ORIENTED_EDGE('',*,*,#30887,.T.) ;
#45164 = ORIENTED_EDGE('',*,*,#30351,.F.) ;
#45165 = ORIENTED_EDGE('',*,*,#30888,.F.) ;
#45166 = ORIENTED_EDGE('',*,*,#30768,.F.) ;
#45167 = ORIENTED_EDGE('',*,*,#30889,.F.) ;
#45168 = ORIENTED_EDGE('',*,*,#30354,.F.) ;
#45169 = ORIENTED_EDGE('',*,*,#30887,.F.) ;
#45170 = ORIENTED_EDGE('',*,*,#30845,.F.) ;
#45171 = ORIENTED_EDGE('',*,*,#30888,.T.) ;
#45172 = ORIENTED_EDGE('',*,*,#30345,.F.) ;
#45173 = ORIENTED_EDGE('',*,*,#30890,.F.) ;
#45174 = ORIENTED_EDGE('',*,*,#30848,.F.) ;
#45175 = ORIENTED_EDGE('',*,*,#30891,.T.) ;
#45176 = ORIENTED_EDGE('',*,*,#30339,.F.) ;
#45177 = ORIENTED_EDGE('',*,*,#30892,.F.) ;
#45178 = ORIENTED_EDGE('',*,*,#30761,.F.) ;
#45179 = ORIENTED_EDGE('',*,*,#30893,.F.) ;
#45180 = ORIENTED_EDGE('',*,*,#30342,.F.) ;
#45181 = ORIENTED_EDGE('',*,*,#30891,.F.) ;
#45182 = ORIENTED_EDGE('',*,*,#30850,.F.) ;
#45183 = ORIENTED_EDGE('',*,*,#30892,.T.) ;
#45184 = ORIENTED_EDGE('',*,*,#30333,.F.) ;
#45185 = ORIENTED_EDGE('',*,*,#30894,.F.) ;
#45186 = ORIENTED_EDGE('',*,*,#30853,.F.) ;
#45187 = ORIENTED_EDGE('',*,*,#30895,.T.) ;
#45188 = ORIENTED_EDGE('',*,*,#30327,.F.) ;
#45189 = ORIENTED_EDGE('',*,*,#30896,.F.) ;
#45190 = ORIENTED_EDGE('',*,*,#30754,.F.) ;
#45191 = ORIENTED_EDGE('',*,*,#30897,.F.) ;
#45192 = ORIENTED_EDGE('',*,*,#30330,.F.) ;
#45193 = ORIENTED_EDGE('',*,*,#30895,.F.) ;
#45194 = ORIENTED_EDGE('',*,*,#30855,.F.) ;
#45195 = ORIENTED_EDGE('',*,*,#30896,.T.) ;
#45196 = ORIENTED_EDGE('',*,*,#30321,.F.) ;
#45197 = ORIENTED_EDGE('',*,*,#30898,.F.) ;
#45198 = ORIENTED_EDGE('',*,*,#30858,.F.) ;
#45199 = ORIENTED_EDGE('',*,*,#30899,.T.) ;
#45200 = ORIENTED_EDGE('',*,*,#30315,.F.) ;
#45201 = ORIENTED_EDGE('',*,*,#30900,.F.) ;
#45202 = ORIENTED_EDGE('',*,*,#30747,.F.) ;
#45203 = ORIENTED_EDGE('',*,*,#30862,.F.) ;
#45204 = ORIENTED_EDGE('',*,*,#30318,.F.) ;
#45205 = ORIENTED_EDGE('',*,*,#30899,.F.) ;
#45206 = ORIENTED_EDGE('',*,*,#30860,.F.) ;
#45207 = ORIENTED_EDGE('',*,*,#30900,.T.) ;
#45208 = ORIENTED_EDGE('',*,*,#30324,.F.) ;
#45209 = ORIENTED_EDGE('',*,*,#30897,.T.) ;
#45210 = ORIENTED_EDGE('',*,*,#30856,.F.) ;
#45211 = ORIENTED_EDGE('',*,*,#30898,.T.) ;
#45212 = ORIENTED_EDGE('',*,*,#30336,.F.) ;
#45213 = ORIENTED_EDGE('',*,*,#30893,.T.) ;
#45214 = ORIENTED_EDGE('',*,*,#30851,.F.) ;
#45215 = ORIENTED_EDGE('',*,*,#30894,.T.) ;
#45216 = ORIENTED_EDGE('',*,*,#30348,.F.) ;
#45217 = ORIENTED_EDGE('',*,*,#30889,.T.) ;
#45218 = ORIENTED_EDGE('',*,*,#30846,.F.) ;
#45219 = ORIENTED_EDGE('',*,*,#30890,.T.) ;
#45220 = ORIENTED_EDGE('',*,*,#30360,.F.) ;
#45221 = ORIENTED_EDGE('',*,*,#30885,.T.) ;
#45222 = ORIENTED_EDGE('',*,*,#30841,.F.) ;
#45223 = ORIENTED_EDGE('',*,*,#30886,.T.) ;
#45224 = ORIENTED_EDGE('',*,*,#30372,.F.) ;
#45225 = ORIENTED_EDGE('',*,*,#30881,.T.) ;
#45226 = ORIENTED_EDGE('',*,*,#30836,.F.) ;
#45227 = ORIENTED_EDGE('',*,*,#30882,.T.) ;
#45228 = ORIENTED_EDGE('',*,*,#30384,.F.) ;
#45229 = ORIENTED_EDGE('',*,*,#30877,.T.) ;
#45230 = ORIENTED_EDGE('',*,*,#30831,.F.) ;
#45231 = ORIENTED_EDGE('',*,*,#30878,.T.) ;
#45232 = ORIENTED_EDGE('',*,*,#30396,.F.) ;
#45233 = ORIENTED_EDGE('',*,*,#30873,.T.) ;
#45234 = ORIENTED_EDGE('',*,*,#30826,.F.) ;
#45235 = ORIENTED_EDGE('',*,*,#30874,.T.) ;
#45236 = ORIENTED_EDGE('',*,*,#30408,.F.) ;
#45237 = ORIENTED_EDGE('',*,*,#30869,.T.) ;
#45238 = ORIENTED_EDGE('',*,*,#30821,.F.) ;
#45239 = ORIENTED_EDGE('',*,*,#30870,.T.) ;
#45240 = ORIENTED_EDGE('',*,*,#30420,.F.) ;
#45241 = ORIENTED_EDGE('',*,*,#30539,.T.) ;
#45242 = ORIENTED_EDGE('',*,*,#30816,.F.) ;
#45243 = ORIENTED_EDGE('',*,*,#30866,.T.) ;
#45244 = ORIENTED_EDGE('',*,*,#30289,.F.) ;
#45245 = ORIENTED_EDGE('',*,*,#30901,.T.) ;
#45246 = ORIENTED_EDGE('',*,*,#30290,.F.) ;
#45247 = ORIENTED_EDGE('',*,*,#30901,.F.) ;
#45248 = ORIENTED_EDGE('',*,*,#30902,.F.) ;
#45249 = ORIENTED_EDGE('',*,*,#30903,.F.) ;
#45250 = ORIENTED_EDGE('',*,*,#30904,.F.) ;
#45251 = ORIENTED_EDGE('',*,*,#30905,.T.) ;
#45252 = ORIENTED_EDGE('',*,*,#30906,.F.) ;
#45253 = ORIENTED_EDGE('',*,*,#30907,.F.) ;
#45254 = ORIENTED_EDGE('',*,*,#30902,.T.) ;
#45255 = ORIENTED_EDGE('',*,*,#30908,.T.) ;
#45256 = ORIENTED_EDGE('',*,*,#30909,.F.) ;
#45257 = ORIENTED_EDGE('',*,*,#30910,.F.) ;
#45258 = ORIENTED_EDGE('',*,*,#30911,.F.) ;
#45259 = ORIENTED_EDGE('',*,*,#30906,.T.) ;
#45260 = ORIENTED_EDGE('',*,*,#30912,.T.) ;
#45261 = ORIENTED_EDGE('',*,*,#30913,.T.) ;
#45262 = ORIENTED_EDGE('',*,*,#30914,.F.) ;
#45263 = ORIENTED_EDGE('',*,*,#30915,.F.) ;
#45264 = ORIENTED_EDGE('',*,*,#30916,.F.) ;
#45265 = ORIENTED_EDGE('',*,*,#30909,.T.) ;
#45266 = ORIENTED_EDGE('',*,*,#30917,.T.) ;
#45267 = ORIENTED_EDGE('',*,*,#30918,.T.) ;
#45268 = ORIENTED_EDGE('',*,*,#30919,.F.) ;
#45269 = ORIENTED_EDGE('',*,*,#30920,.F.) ;
#45270 = ORIENTED_EDGE('',*,*,#30921,.F.) ;
#45271 = ORIENTED_EDGE('',*,*,#30922,.T.) ;
#45272 = ORIENTED_EDGE('',*,*,#30923,.F.) ;
#45273 = ORIENTED_EDGE('',*,*,#30924,.F.) ;
#45274 = ORIENTED_EDGE('',*,*,#30925,.F.) ;
#45275 = ORIENTED_EDGE('',*,*,#30919,.T.) ;
#45276 = ORIENTED_EDGE('',*,*,#30926,.T.) ;
#45277 = ORIENTED_EDGE('',*,*,#30927,.F.) ;
#45278 = ORIENTED_EDGE('',*,*,#30928,.F.) ;
#45279 = ORIENTED_EDGE('',*,*,#30923,.T.) ;
#45280 = ORIENTED_EDGE('',*,*,#30929,.T.) ;
#45281 = ORIENTED_EDGE('',*,*,#30930,.F.) ;
#45282 = ORIENTED_EDGE('',*,*,#30931,.F.) ;
#45283 = ORIENTED_EDGE('',*,*,#30932,.F.) ;
#45284 = ORIENTED_EDGE('',*,*,#30927,.T.) ;
#45285 = ORIENTED_EDGE('',*,*,#30933,.T.) ;
#45286 = ORIENTED_EDGE('',*,*,#30934,.F.) ;
#45287 = ORIENTED_EDGE('',*,*,#30935,.F.) ;
#45288 = ORIENTED_EDGE('',*,*,#30930,.T.) ;
#45289 = ORIENTED_EDGE('',*,*,#30936,.T.) ;
#45290 = ORIENTED_EDGE('',*,*,#30937,.F.) ;
#45291 = ORIENTED_EDGE('',*,*,#30938,.F.) ;
#45292 = ORIENTED_EDGE('',*,*,#30939,.F.) ;
#45293 = ORIENTED_EDGE('',*,*,#30934,.T.) ;
#45294 = ORIENTED_EDGE('',*,*,#30940,.T.) ;
#45295 = ORIENTED_EDGE('',*,*,#30941,.F.) ;
#45296 = ORIENTED_EDGE('',*,*,#30942,.T.) ;
#45297 = ORIENTED_EDGE('',*,*,#30943,.T.) ;
#45298 = ORIENTED_EDGE('',*,*,#30944,.T.) ;
#45299 = ORIENTED_EDGE('',*,*,#30945,.T.) ;
#45300 = ORIENTED_EDGE('',*,*,#30946,.T.) ;
#45301 = ORIENTED_EDGE('',*,*,#30947,.T.) ;
#45302 = ORIENTED_EDGE('',*,*,#30948,.T.) ;
#45303 = ORIENTED_EDGE('',*,*,#30949,.T.) ;
#45304 = ORIENTED_EDGE('',*,*,#30950,.T.) ;
#45305 = ORIENTED_EDGE('',*,*,#30951,.T.) ;
#45306 = ORIENTED_EDGE('',*,*,#30952,.T.) ;
#45307 = ORIENTED_EDGE('',*,*,#30953,.T.) ;
#45308 = ORIENTED_EDGE('',*,*,#30954,.T.) ;
#45309 = ORIENTED_EDGE('',*,*,#30955,.T.) ;
#45310 = ORIENTED_EDGE('',*,*,#30956,.T.) ;
#45311 = ORIENTED_EDGE('',*,*,#30957,.T.) ;
#45312 = ORIENTED_EDGE('',*,*,#30958,.T.) ;
#45313 = ORIENTED_EDGE('',*,*,#30959,.T.) ;
#45314 = ORIENTED_EDGE('',*,*,#30960,.T.) ;
#45315 = ORIENTED_EDGE('',*,*,#30961,.T.) ;
#45316 = ORIENTED_EDGE('',*,*,#30962,.T.) ;
#45317 = ORIENTED_EDGE('',*,*,#30963,.T.) ;
#45318 = ORIENTED_EDGE('',*,*,#30964,.T.) ;
#45319 = ORIENTED_EDGE('',*,*,#30965,.T.) ;
#45320 = ORIENTED_EDGE('',*,*,#30966,.T.) ;
#45321 = ORIENTED_EDGE('',*,*,#30967,.T.) ;
#45322 = ORIENTED_EDGE('',*,*,#30968,.T.) ;
#45323 = ORIENTED_EDGE('',*,*,#30969,.T.) ;
#45324 = ORIENTED_EDGE('',*,*,#30970,.T.) ;
#45325 = ORIENTED_EDGE('',*,*,#30971,.T.) ;
#45326 = ORIENTED_EDGE('',*,*,#30972,.T.) ;
#45327 = ORIENTED_EDGE('',*,*,#30973,.T.) ;
#45328 = ORIENTED_EDGE('',*,*,#30974,.F.) ;
#45329 = ORIENTED_EDGE('',*,*,#30937,.T.) ;
#45330 = ORIENTED_EDGE('',*,*,#30975,.T.) ;
#45331 = ORIENTED_EDGE('',*,*,#30976,.F.) ;
#45332 = ORIENTED_EDGE('',*,*,#30977,.F.) ;
#45333 = ORIENTED_EDGE('',*,*,#30978,.F.) ;
#45334 = ORIENTED_EDGE('',*,*,#30914,.T.) ;
#45335 = ORIENTED_EDGE('',*,*,#30979,.T.) ;
#45336 = ORIENTED_EDGE('',*,*,#30980,.F.) ;
#45337 = ORIENTED_EDGE('',*,*,#30981,.F.) ;
#45338 = ORIENTED_EDGE('',*,*,#30982,.F.) ;
#45339 = ORIENTED_EDGE('',*,*,#30942,.F.) ;
#45340 = ORIENTED_EDGE('',*,*,#30983,.T.) ;
#45341 = ORIENTED_EDGE('',*,*,#30980,.T.) ;
#45342 = ORIENTED_EDGE('',*,*,#30984,.T.) ;
#45343 = ORIENTED_EDGE('',*,*,#30985,.T.) ;
#45344 = ORIENTED_EDGE('',*,*,#30983,.F.) ;
#45345 = ORIENTED_EDGE('',*,*,#30955,.F.) ;
#45346 = ORIENTED_EDGE('',*,*,#30954,.F.) ;
#45347 = ORIENTED_EDGE('',*,*,#30953,.F.) ;
#45348 = ORIENTED_EDGE('',*,*,#30952,.F.) ;
#45349 = ORIENTED_EDGE('',*,*,#30951,.F.) ;
#45350 = ORIENTED_EDGE('',*,*,#30950,.F.) ;
#45351 = ORIENTED_EDGE('',*,*,#30986,.F.) ;
#45352 = ORIENTED_EDGE('',*,*,#30987,.T.) ;
#45353 = ORIENTED_EDGE('',*,*,#30903,.T.) ;
#45354 = ORIENTED_EDGE('',*,*,#30907,.T.) ;
#45355 = ORIENTED_EDGE('',*,*,#30911,.T.) ;
#45356 = ORIENTED_EDGE('',*,*,#30910,.T.) ;
#45357 = ORIENTED_EDGE('',*,*,#30916,.T.) ;
#45358 = ORIENTED_EDGE('',*,*,#30915,.T.) ;
#45359 = ORIENTED_EDGE('',*,*,#30982,.T.) ;
#45360 = ORIENTED_EDGE('',*,*,#30981,.T.) ;
#45361 = ORIENTED_EDGE('',*,*,#30949,.F.) ;
#45362 = ORIENTED_EDGE('',*,*,#30988,.T.) ;
#45363 = ORIENTED_EDGE('',*,*,#30904,.T.) ;
#45364 = ORIENTED_EDGE('',*,*,#30987,.F.) ;
#45365 = ORIENTED_EDGE('',*,*,#30986,.T.) ;
#45366 = ORIENTED_EDGE('',*,*,#30985,.F.) ;
#45367 = ORIENTED_EDGE('',*,*,#30984,.F.) ;
#45368 = ORIENTED_EDGE('',*,*,#30979,.F.) ;
#45369 = ORIENTED_EDGE('',*,*,#30918,.F.) ;
#45370 = ORIENTED_EDGE('',*,*,#30917,.F.) ;
#45371 = ORIENTED_EDGE('',*,*,#30913,.F.) ;
#45372 = ORIENTED_EDGE('',*,*,#30912,.F.) ;
#45373 = ORIENTED_EDGE('',*,*,#30908,.F.) ;
#45374 = ORIENTED_EDGE('',*,*,#30905,.F.) ;
#45375 = ORIENTED_EDGE('',*,*,#30988,.F.) ;
#45376 = ORIENTED_EDGE('',*,*,#30948,.F.) ;
#45377 = ORIENTED_EDGE('',*,*,#30947,.F.) ;
#45378 = ORIENTED_EDGE('',*,*,#30946,.F.) ;
#45379 = ORIENTED_EDGE('',*,*,#30945,.F.) ;
#45380 = ORIENTED_EDGE('',*,*,#30944,.F.) ;
#45381 = ORIENTED_EDGE('',*,*,#30943,.F.) ;
#45382 = ORIENTED_EDGE('',*,*,#30956,.F.) ;
#45383 = ORIENTED_EDGE('',*,*,#30989,.T.) ;
#45384 = ORIENTED_EDGE('',*,*,#30976,.T.) ;
#45385 = ORIENTED_EDGE('',*,*,#30990,.T.) ;
#45386 = ORIENTED_EDGE('',*,*,#30991,.T.) ;
#45387 = ORIENTED_EDGE('',*,*,#30989,.F.) ;
#45388 = ORIENTED_EDGE('',*,*,#30973,.F.) ;
#45389 = ORIENTED_EDGE('',*,*,#30972,.F.) ;
#45390 = ORIENTED_EDGE('',*,*,#30971,.F.) ;
#45391 = ORIENTED_EDGE('',*,*,#30970,.F.) ;
#45392 = ORIENTED_EDGE('',*,*,#30969,.F.) ;
#45393 = ORIENTED_EDGE('',*,*,#30968,.F.) ;
#45394 = ORIENTED_EDGE('',*,*,#30967,.F.) ;
#45395 = ORIENTED_EDGE('',*,*,#30966,.F.) ;
#45396 = ORIENTED_EDGE('',*,*,#30992,.F.) ;
#45397 = ORIENTED_EDGE('',*,*,#30920,.T.) ;
#45398 = ORIENTED_EDGE('',*,*,#30925,.T.) ;
#45399 = ORIENTED_EDGE('',*,*,#30924,.T.) ;
#45400 = ORIENTED_EDGE('',*,*,#30928,.T.) ;
#45401 = ORIENTED_EDGE('',*,*,#30932,.T.) ;
#45402 = ORIENTED_EDGE('',*,*,#30931,.T.) ;
#45403 = ORIENTED_EDGE('',*,*,#30935,.T.) ;
#45404 = ORIENTED_EDGE('',*,*,#30939,.T.) ;
#45405 = ORIENTED_EDGE('',*,*,#30938,.T.) ;
#45406 = ORIENTED_EDGE('',*,*,#30978,.T.) ;
#45407 = ORIENTED_EDGE('',*,*,#30977,.T.) ;
#45408 = ORIENTED_EDGE('',*,*,#30965,.F.) ;
#45409 = ORIENTED_EDGE('',*,*,#30993,.T.) ;
#45410 = ORIENTED_EDGE('',*,*,#30921,.T.) ;
#45411 = ORIENTED_EDGE('',*,*,#30992,.T.) ;
#45412 = ORIENTED_EDGE('',*,*,#30991,.F.) ;
#45413 = ORIENTED_EDGE('',*,*,#30990,.F.) ;
#45414 = ORIENTED_EDGE('',*,*,#30975,.F.) ;
#45415 = ORIENTED_EDGE('',*,*,#30940,.F.) ;
#45416 = ORIENTED_EDGE('',*,*,#30936,.F.) ;
#45417 = ORIENTED_EDGE('',*,*,#30933,.F.) ;
#45418 = ORIENTED_EDGE('',*,*,#30929,.F.) ;
#45419 = ORIENTED_EDGE('',*,*,#30926,.F.) ;
#45420 = ORIENTED_EDGE('',*,*,#30922,.F.) ;
#45421 = ORIENTED_EDGE('',*,*,#30993,.F.) ;
#45422 = ORIENTED_EDGE('',*,*,#30964,.F.) ;
#45423 = ORIENTED_EDGE('',*,*,#30963,.F.) ;
#45424 = ORIENTED_EDGE('',*,*,#30962,.F.) ;
#45425 = ORIENTED_EDGE('',*,*,#30961,.F.) ;
#45426 = ORIENTED_EDGE('',*,*,#30960,.F.) ;
#45427 = ORIENTED_EDGE('',*,*,#30959,.F.) ;
#45428 = ORIENTED_EDGE('',*,*,#30958,.F.) ;
#45429 = ORIENTED_EDGE('',*,*,#30957,.F.) ;
#45430 = ORIENTED_EDGE('',*,*,#30941,.T.) ;
#45431 = ORIENTED_EDGE('',*,*,#30974,.T.) ;
#45432 = TOROIDAL_SURFACE('',#49312,5.8,0.2) ;
#45433 = TOROIDAL_SURFACE('',#49365,1.15,0.2) ;
#45434 = TOROIDAL_SURFACE('',#49377,1.15,0.2) ;
#45435 = TOROIDAL_SURFACE('',#49389,1.15,0.2) ;
#45436 = TOROIDAL_SURFACE('',#49398,1.15,0.2) ;
#45437 = TOROIDAL_SURFACE('',#49454,5.8,0.2) ;
#45438 = TOROIDAL_SURFACE('',#49472,5.8,0.2) ;
#45439 = TOROIDAL_SURFACE('',#49490,5.8,0.2) ;
#45440 = TOROIDAL_SURFACE('',#49508,5.8,0.2) ;
#45441 = TOROIDAL_SURFACE('',#49526,5.8,0.2) ;
#45442 = TOROIDAL_SURFACE('',#49544,5.8,0.2) ;
#45443 = TOROIDAL_SURFACE('',#49562,5.8,0.2) ;
#45444 = TOROIDAL_SURFACE('',#49580,5.8,0.2) ;
#45445 = TOROIDAL_SURFACE('',#49598,5.8,0.2) ;
#45446 = TOROIDAL_SURFACE('',#49616,5.8,0.2) ;
#45447 = TOROIDAL_SURFACE('',#49622,5.8,0.2) ;
#45448 = TOROIDAL_SURFACE('',#49627,5.8,0.2) ;
#45449 = TOROIDAL_SURFACE('',#49630,5.8,0.2) ;
#45450 = TOROIDAL_SURFACE('',#49633,5.8,0.2) ;
#45451 = TOROIDAL_SURFACE('',#49636,5.8,0.2) ;
#45452 = TOROIDAL_SURFACE('',#49640,5.8,0.2) ;
#45453 = TOROIDAL_SURFACE('',#49643,5.8,0.2) ;
#45454 = TOROIDAL_SURFACE('',#49646,5.8,0.2) ;
#45455 = TOROIDAL_SURFACE('',#49650,5.8,0.2) ;
#45456 = TOROIDAL_SURFACE('',#49653,5.8,0.2) ;
#45457 = TOROIDAL_SURFACE('',#49656,5.8,0.2) ;
#45458 = TOROIDAL_SURFACE('',#49660,5.8,0.2) ;
#45459 = TOROIDAL_SURFACE('',#49663,5.8,0.2) ;
#45460 = TOROIDAL_SURFACE('',#49666,5.8,0.2) ;
#45461 = TOROIDAL_SURFACE('',#49670,5.8,0.2) ;
#45462 = TOROIDAL_SURFACE('',#49673,5.8,0.2) ;
#45463 = TOROIDAL_SURFACE('',#49676,5.8,0.2) ;
#45464 = TOROIDAL_SURFACE('',#49680,5.8,0.2) ;
#45465 = TOROIDAL_SURFACE('',#49683,5.8,0.2) ;
#45466 = TOROIDAL_SURFACE('',#49686,5.8,0.2) ;
#45467 = TOROIDAL_SURFACE('',#49690,5.8,0.2) ;
#45468 = TOROIDAL_SURFACE('',#49693,5.8,0.2) ;
#45469 = TOROIDAL_SURFACE('',#49696,5.8,0.2) ;
#45470 = TOROIDAL_SURFACE('',#49700,5.8,0.2) ;
#45471 = TOROIDAL_SURFACE('',#49703,5.8,0.2) ;
#45472 = TOROIDAL_SURFACE('',#49706,5.8,0.2) ;
#45473 = TOROIDAL_SURFACE('',#49710,5.8,0.2) ;
#45474 = TOROIDAL_SURFACE('',#49713,5.8,0.2) ;
#45475 = TOROIDAL_SURFACE('',#49716,5.8,0.2) ;
#45476 = TOROIDAL_SURFACE('',#49720,5.8,0.2) ;
#45477 = TOROIDAL_SURFACE('',#49764,0.75,0.2) ;
#45478 = TOROIDAL_SURFACE('',#49784,0.75,0.2) ;
#45479 = TOROIDAL_SURFACE('',#49789,0.75,0.2) ;
#45480 = TOROIDAL_SURFACE('',#49797,0.75,0.2) ;
#45481 = TOROIDAL_SURFACE('',#49804,5.13915047169858,0.2) ;
#45482 = TOROIDAL_SURFACE('',#49806,0.399999999999991,0.2) ;
#45483 = TOROIDAL_SURFACE('',#49808,0.399999999999991,0.2) ;
#45484 = TOROIDAL_SURFACE('',#49812,0.399999999999956,0.199999999999996) ;
#45485 = TOROIDAL_SURFACE('',#49817,0.399999999999991,0.2) ;
#45486 = TOROIDAL_SURFACE('',#49819,0.399999999999991,0.2) ;
#45487 = TOROIDAL_SURFACE('',#49823,0.399999999999991,0.2) ;
#45488 = TOROIDAL_SURFACE('',#49829,0.399999999999991,0.2) ;
#45489 = TOROIDAL_SURFACE('',#49834,0.399999999999991,0.2) ;
#45490 = TOROIDAL_SURFACE('',#49930,2.12,0.12) ;
#45491 = TOROIDAL_SURFACE('',#49938,3.48,0.12) ;
#45492 = TOROIDAL_SURFACE('',#49968,3.48,0.12) ;
#45493 = TOROIDAL_SURFACE('',#49981,3.48,0.12) ;
#45494 = TOROIDAL_SURFACE('',#50349,2.1,0.1) ;
#45495 = TOROIDAL_SURFACE('',#50358,2.89999999999999,0.1) ;
#45496 = TOROIDAL_SURFACE('',#50363,3.09999999999999,0.1) ;
#45497 = TOROIDAL_SURFACE('',#50436,0.5,0.1) ;
#45498 = TOROIDAL_SURFACE('',#50443,1.9,0.1) ;
#45499 = TOROIDAL_SURFACE('',#50449,1.9,0.1) ;
#45500 = TOROIDAL_SURFACE('',#50455,2.7,0.1) ;
#45501 = TOROIDAL_SURFACE('',#50461,1.9,0.1) ;
#45502 = TOROIDAL_SURFACE('',#50467,1.9,0.1) ;
#45503 = TOROIDAL_SURFACE('',#50473,0.5,0.1) ;
#45504 = TOROIDAL_SURFACE('',#50495,4.,1.) ;
#45505 = TOROIDAL_SURFACE('',#50500,2.88,0.12) ;
#45506 = TOROIDAL_SURFACE('',#50505,2.12,0.12) ;
#45507 = TOROIDAL_SURFACE('',#50511,1.97000000000001,0.12) ;
#45508 = TOROIDAL_SURFACE('',#50522,1.97000000000001,0.12) ;
#45509 = TOROIDAL_SURFACE('',#50526,1.97,0.12) ;
#45510 = TOROIDAL_SURFACE('',#50537,1.97,0.12) ;
#45511 = TOROIDAL_SURFACE('',#50541,1.9,0.1) ;
#45512 = TOROIDAL_SURFACE('',#50547,2.7,0.1) ;
#45513 = TOROIDAL_SURFACE('',#50552,1.9,0.1) ;
#45514 = TOROIDAL_SURFACE('',#50579,0.2,0.1) ;
#45515 = TOROIDAL_SURFACE('',#50585,0.2,0.1) ;
#45516 = TOROIDAL_SURFACE('',#50598,0.2,0.1) ;
#45517 = TOROIDAL_SURFACE('',#50606,0.199999999999996,0.0999999999999934) ;
#45518 = TOROIDAL_SURFACE('',#50610,0.199999999999996,0.0999999999999979) ;
#45519 = TOROIDAL_SURFACE('',#50616,0.2,0.1) ;
#45520 = TOROIDAL_SURFACE('',#50623,0.2,0.1) ;
#45521 = TOROIDAL_SURFACE('',#50639,0.2,0.1) ;
#45522 = TOROIDAL_SURFACE('',#50655,0.2,0.1) ;
#45523 = TOROIDAL_SURFACE('',#50664,0.2,0.1) ;
#45524 = TOROIDAL_SURFACE('',#50669,0.2,0.1) ;
#45525 = TOROIDAL_SURFACE('',#50674,0.2,0.1) ;
#45526 = TOROIDAL_SURFACE('',#50697,0.2,0.1) ;
#45527 = TOROIDAL_SURFACE('',#50702,0.2,0.1) ;
#45528 = TOROIDAL_SURFACE('',#50707,0.2,0.1) ;
#45529 = TOROIDAL_SURFACE('',#50712,0.2,0.1) ;
#45530 = TOROIDAL_SURFACE('',#50720,0.2,0.1) ;
#45531 = TOROIDAL_SURFACE('',#50725,0.2,0.1) ;
#45532 = TOROIDAL_SURFACE('',#50746,0.199999999999996,0.0999999999999934) ;
#45533 = TOROIDAL_SURFACE('',#50750,0.199999999999996,0.0999999999999979) ;
#45534 = TOROIDAL_SURFACE('',#50756,0.2,0.1) ;
#45535 = TOROIDAL_SURFACE('',#50761,0.2,0.1) ;
#45536 = TOROIDAL_SURFACE('',#50766,0.2,0.1) ;
#45537 = TOROIDAL_SURFACE('',#50771,0.2,0.1) ;
#45538 = TOROIDAL_SURFACE('',#50788,0.2,0.1) ;
#45539 = TOROIDAL_SURFACE('',#50797,0.2,0.1) ;
#45540 = TOROIDAL_SURFACE('',#50802,0.2,0.1) ;
#45541 = TOROIDAL_SURFACE('',#50812,0.2,0.1) ;
#45542 = TOROIDAL_SURFACE('',#50830,0.2,0.1) ;
#45543 = TOROIDAL_SURFACE('',#50839,0.2,0.1) ;
#45544 = TOROIDAL_SURFACE('',#50844,0.2,0.1) ;
#45545 = TOROIDAL_SURFACE('',#50854,0.2,0.1) ;
#45546 = TOROIDAL_SURFACE('',#50877,0.2,0.1) ;
#45547 = TOROIDAL_SURFACE('',#50883,0.2,0.1) ;
#45548 = TOROIDAL_SURFACE('',#50889,0.2,0.1) ;
#45549 = TOROIDAL_SURFACE('',#50894,0.2,0.1) ;
#45550 = TOROIDAL_SURFACE('',#50899,0.2,0.1) ;
#45551 = TOROIDAL_SURFACE('',#50904,0.2,0.1) ;
#45552 = TOROIDAL_SURFACE('',#50922,0.2,0.1) ;
#45553 = TOROIDAL_SURFACE('',#50927,0.199999999999996,0.0999999999999934) ;
#45554 = TOROIDAL_SURFACE('',#50931,0.199999999999996,0.0999999999999979) ;
#45555 = TOROIDAL_SURFACE('',#50935,0.200000000000031,0.0999999999999979) ;
#45556 = TOROIDAL_SURFACE('',#50942,0.199999999999996,0.0999999999999979) ;
#45557 = TOROIDAL_SURFACE('',#50952,0.2,0.1) ;
#45558 = TOROIDAL_SURFACE('',#50956,0.2,0.1) ;
#45559 = TOROIDAL_SURFACE('',#50961,0.199999999999996,0.0999999999999979) ;
#45560 = TOROIDAL_SURFACE('',#50964,0.199999999999996,0.0999999999999979) ;
#45561 = TOROIDAL_SURFACE('',#50975,0.200000000000031,0.0999999999999979) ;
#45562 = TOROIDAL_SURFACE('',#50979,0.199999999999996,0.0999999999999979) ;
#45563 = TOROIDAL_SURFACE('',#50985,0.199999999999996,0.0999999999999979) ;
#45564 = TOROIDAL_SURFACE('',#50989,0.200000000000031,0.0999999999999979) ;
#45565 = TOROIDAL_SURFACE('',#51004,0.2,0.1) ;
#45566 = TOROIDAL_SURFACE('',#51008,0.2,0.1) ;
#45567 = TOROIDAL_SURFACE('',#51013,0.200000000000031,0.0999999999999979) ;
#45568 = TOROIDAL_SURFACE('',#51020,0.199999999999996,0.0999999999999979) ;
#45569 = TOROIDAL_SURFACE('',#51024,0.200000000000031,0.0999999999999979) ;
#45570 = TOROIDAL_SURFACE('',#51032,0.199999999999996,0.0999999999999979) ;
#45571 = TOROIDAL_SURFACE('',#51036,0.199999999999996,0.0999999999999979) ;
#45572 = TOROIDAL_SURFACE('',#51042,0.200000000000031,0.0999999999999979) ;
#45573 = TOROIDAL_SURFACE('',#51056,0.199999999999996,0.0999999999999979) ;
#45574 = TOROIDAL_SURFACE('',#51060,0.200000000000031,0.0999999999999979) ;
#45575 = TOROIDAL_SURFACE('',#51067,1.1,0.1) ;
#45576 = TOROIDAL_SURFACE('',#51072,0.5,0.1) ;
#45577 = TOROIDAL_SURFACE('',#51077,0.5,0.1) ;
#45578 = TOROIDAL_SURFACE('',#51081,1.9,0.1) ;
#45579 = TOROIDAL_SURFACE('',#51082,1.9,0.1) ;
#45580 = TOROIDAL_SURFACE('',#51086,1.1,0.1) ;
#45581 = TOROIDAL_SURFACE('',#51091,0.7,0.1) ;
#45582 = TOROIDAL_SURFACE('',#51096,0.5,0.1) ;
#45583 = TOROIDAL_SURFACE('',#51101,0.500000000000005,0.1) ;
#45584 = TOROIDAL_SURFACE('',#51104,2.59999999999996,0.1) ;
#45585 = TOROIDAL_SURFACE('',#51109,2.59999999999999,0.1) ;
#45586 = TOROIDAL_SURFACE('',#51112,0.500000000000023,0.1) ;
#45587 = TOROIDAL_SURFACE('',#51117,0.5,0.1) ;
#45588 = TOROIDAL_SURFACE('',#51122,0.7,0.1) ;
#45589 = TOROIDAL_SURFACE('',#51127,3.9,0.1) ;
#45590 = TOROIDAL_SURFACE('',#51132,3.9,0.1) ;
#45591 = TOROIDAL_SURFACE('',#51137,3.9,0.1) ;
#45592 = TOROIDAL_SURFACE('',#51142,0.7,0.1) ;
#45593 = TOROIDAL_SURFACE('',#51147,0.5,0.1) ;
#45594 = TOROIDAL_SURFACE('',#51151,0.2,0.1) ;
#45595 = TOROIDAL_SURFACE('',#51159,0.2,0.1) ;
#45596 = TOROIDAL_SURFACE('',#51205,0.9,0.1) ;
#45597 = TOROIDAL_SURFACE('',#51218,0.9,0.1) ;
#45598 = TOROIDAL_SURFACE('',#51224,0.199999999999996,0.100000000000002) ;
#45599 = TOROIDAL_SURFACE('',#51228,0.199999999999995,0.0999999999999784) ;
#45600 = TOROIDAL_SURFACE('',#51233,0.199999999999987,0.0999999999999979) ;
#45601 = TOROIDAL_SURFACE('',#51238,0.199999999999969,0.0999999999999847) ;
#45602 = TOROIDAL_SURFACE('',#51243,0.200000000000031,0.100000000000016) ;
#45603 = TOROIDAL_SURFACE('',#51248,0.200000000000031,0.0999999999999979) ;
#45604 = TOROIDAL_SURFACE('',#51267,0.199999999999996,0.100000000000002) ;
#45605 = TOROIDAL_SURFACE('',#51273,0.199999999999996,0.100000000000002) ;
#45606 = TOROIDAL_SURFACE('',#51277,0.200000000000031,0.0999999999999979) ;
#45607 = TOROIDAL_SURFACE('',#51281,0.199999999999996,0.0999999999999979) ;
#45608 = TOROIDAL_SURFACE('',#51286,0.199999999999996,0.100000000000002) ;
#45609 = TOROIDAL_SURFACE('',#51293,0.200000000000031,0.0999999999999979) ;
#45610 = TOROIDAL_SURFACE('',#51308,0.9,0.1) ;
#45611 = TOROIDAL_SURFACE('',#51317,0.900000000000001,0.1) ;
#45612 = TOROIDAL_SURFACE('',#51324,0.199999999999919,0.0999999999999784) ;
#45613 = TOROIDAL_SURFACE('',#51328,0.199999999999987,0.0999999999999979) ;
#45614 = TOROIDAL_SURFACE('',#51332,0.199999999999982,0.099999999999991) ;
#45615 = TOROIDAL_SURFACE('',#51336,0.199999999999996,0.100000000000016) ;
#45616 = TOROIDAL_SURFACE('',#51344,0.9,0.1) ;
#45617 = TOROIDAL_SURFACE('',#51357,0.9,0.1) ;
#45618 = TOROIDAL_SURFACE('',#51363,0.200000000000031,0.100000000000016) ;
#45619 = TOROIDAL_SURFACE('',#51367,0.199999999999982,0.099999999999991) ;
#45620 = TOROIDAL_SURFACE('',#51371,0.199999999999987,0.0999999999999979) ;
#45621 = TOROIDAL_SURFACE('',#51375,0.199999999999976,0.0999999999999847) ;
#45622 = TOROIDAL_SURFACE('',#51399,0.200000000000031,0.0999999999999979) ;
#45623 = TOROIDAL_SURFACE('',#51403,0.200000000000031,0.100000000000016) ;
#45624 = TOROIDAL_SURFACE('',#51407,0.199999999999996,0.0999999999999979) ;
#45625 = TOROIDAL_SURFACE('',#51411,0.200000000000031,0.100000000000016) ;
#45626 = TOROIDAL_SURFACE('',#51415,0.200000000000031,0.0999999999999934) ;
#45627 = TOROIDAL_SURFACE('',#51419,0.199999999999996,0.0999999999999979) ;
#45628 = TOROIDAL_SURFACE('',#51423,0.200000000000031,0.0999999999999979) ;
#45629 = TOROIDAL_SURFACE('',#51428,0.200000000000031,0.100000000000016) ;
#45630 = TOROIDAL_SURFACE('',#51447,2.6,0.1) ;
#45631 = TOROIDAL_SURFACE('',#51453,2.6,0.1) ;
#45632 = TOROIDAL_SURFACE('',#51458,0.900000000000001,0.1) ;
#45633 = TOROIDAL_SURFACE('',#51470,0.9,0.1) ;
#45634 = TOROIDAL_SURFACE('',#51477,0.199999999999969,0.099999999999991) ;
#45635 = TOROIDAL_SURFACE('',#51482,0.199999999999991,0.0999999999999979) ;
#45636 = TOROIDAL_SURFACE('',#51486,0.199999999999969,0.0999999999999847) ;
#45637 = TOROIDAL_SURFACE('',#51490,0.200000000000031,0.100000000000016) ;
#45638 = TOROIDAL_SURFACE('',#51494,0.199999999999996,0.0999999999999979) ;
#45639 = TOROIDAL_SURFACE('',#51500,2.6,0.1) ;
#45640 = TOROIDAL_SURFACE('',#51505,2.1,0.1) ;
#45641 = TOROIDAL_SURFACE('',#51512,0.7,0.1) ;
#45642 = TOROIDAL_SURFACE('',#51517,0.5,0.1) ;
#45643 = TOROIDAL_SURFACE('',#51521,0.500000000000005,0.1) ;
#45644 = TOROIDAL_SURFACE('',#51523,2.59999999999996,0.1) ;
#45645 = TOROIDAL_SURFACE('',#51527,2.59999999999999,0.1) ;
#45646 = TOROIDAL_SURFACE('',#51529,0.500000000000023,0.1) ;
#45647 = TOROIDAL_SURFACE('',#51533,0.5,0.1) ;
#45648 = TOROIDAL_SURFACE('',#51537,0.7,0.1) ;
#45649 = TOROIDAL_SURFACE('',#51541,3.9,0.1) ;
#45650 = TOROIDAL_SURFACE('',#51545,3.9,0.1) ;
#45651 = TOROIDAL_SURFACE('',#51549,3.9,0.1) ;
#45652 = TOROIDAL_SURFACE('',#51553,0.7,0.1) ;
#45653 = TOROIDAL_SURFACE('',#51557,0.5,0.1) ;
#45654 = TOROIDAL_SURFACE('',#51559,0.5,0.1) ;
#45655 = TOROIDAL_SURFACE('',#51564,0.5,0.1) ;
#45656 = TOROIDAL_SURFACE('',#51568,2.2,0.2) ;
#45657 = TOROIDAL_SURFACE('',#51573,2.6,0.2) ;
#45658 = TOROIDAL_SURFACE('',#51579,3.,0.2) ;
#45659 = TOROIDAL_SURFACE('',#51583,3.,0.2) ;
#45660 = TOROIDAL_SURFACE('',#51591,2.6,0.2) ;
#45661 = TOROIDAL_SURFACE('',#51596,2.2,0.2) ;
#45662 = TOROIDAL_SURFACE('',#51601,2.99999999999999,0.2) ;
#45663 = TOROIDAL_SURFACE('',#51609,2.2,0.2) ;
#45664 = TOROIDAL_SURFACE('',#51614,2.59999999999999,0.2) ;
#45665 = TOROIDAL_SURFACE('',#51616,4.06491106406735,1.3) ;
#45666 = TOROIDAL_SURFACE('',#51618,4.06491106406736,1.3) ;
#45667 = TOROIDAL_SURFACE('',#51620,4.06491106406735,1.3) ;
#45668 = TOROIDAL_SURFACE('',#51776,0.4,0.1) ;
#45669 = TOROIDAL_SURFACE('',#51780,0.4,0.1) ;
#45670 = TOROIDAL_SURFACE('',#51790,0.4,0.1) ;
#45671 = TOROIDAL_SURFACE('',#51794,0.4,0.1) ;
#45672 = TOROIDAL_SURFACE('',#51800,0.4,0.1) ;
#45673 = TOROIDAL_SURFACE('',#51804,0.4,0.1) ;
#45674 = TOROIDAL_SURFACE('',#51838,1.55266329058736,0.1) ;
#45675 = TOROIDAL_SURFACE('',#51843,1.55266329058736,0.1) ;
#45676 = TOROIDAL_SURFACE('',#51847,3.1,0.1) ;
#45677 = TOROIDAL_SURFACE('',#51853,3.1,0.1) ;
#45678 = TOROIDAL_SURFACE('',#51867,0.899999999999993,0.3) ;
#45679 = TOROIDAL_SURFACE('',#51873,0.899999999999993,0.3) ;
#45680 = TOROIDAL_SURFACE('',#51877,0.899999999999993,0.3) ;
#45681 = TOROIDAL_SURFACE('',#51883,0.899999999999993,0.3) ;
#45682 = TOROIDAL_SURFACE('',#51887,0.899999999999993,0.3) ;
#45683 = TOROIDAL_SURFACE('',#51893,0.899999999999993,0.3) ;
#45684 = TOROIDAL_SURFACE('',#51897,0.899999999999993,0.3) ;
#45685 = TOROIDAL_SURFACE('',#51903,0.899999999999993,0.3) ;
#45686 = TOROIDAL_SURFACE('',#51907,0.899999999999993,0.3) ;
#45687 = TOROIDAL_SURFACE('',#51913,0.899999999999993,0.3) ;
#45688 = TOROIDAL_SURFACE('',#51917,0.899999999999993,0.3) ;
#45689 = TOROIDAL_SURFACE('',#51923,0.899999999999993,0.3) ;
#45690 = TOROIDAL_SURFACE('',#51927,0.899999999999993,0.3) ;
#45691 = TOROIDAL_SURFACE('',#51933,0.899999999999993,0.3) ;
#45692 = TOROIDAL_SURFACE('',#51937,0.899999999999993,0.3) ;
#45693 = TOROIDAL_SURFACE('',#51943,0.899999999999993,0.3) ;
#45694 = TOROIDAL_SURFACE('',#51982,2.45,0.45) ;
#45695 = TOROIDAL_SURFACE('',#51994,2.94999999999999,0.45) ;
#45696 = TOROIDAL_SURFACE('',#52006,2.95,0.45) ;
#45697 = TOROIDAL_SURFACE('',#52018,0.240000000000009,0.120000000000005) ;
#45698 = TOROIDAL_SURFACE('',#52037,0.240000000000009,0.120000000000005) ;
#45699 = TOROIDAL_SURFACE('',#52047,0.240000000000009,0.120000000000005) ;
#45700 = TOROIDAL_SURFACE('',#52067,0.240000000000009,0.120000000000005) ;
#45701 = TOROIDAL_SURFACE('',#52076,0.240000000000009,0.120000000000005) ;
#45702 = TOROIDAL_SURFACE('',#52096,0.240000000000009,0.120000000000005) ;
#45703 = TOROIDAL_SURFACE('',#52106,0.240000000000009,0.120000000000005) ;
#45704 = TOROIDAL_SURFACE('',#52126,0.24,0.119999999999996) ;
#45705 = TOROIDAL_SURFACE('',#52168,1.74999999999999,0.25) ;
#45706 = TOROIDAL_SURFACE('',#52174,1.74999999999999,0.25) ;
#45707 = TOROIDAL_SURFACE('',#52220,1.9,0.1) ;
#45708 = TOROIDAL_SURFACE('',#52289,1.8,0.2) ;
#45709 = TOROIDAL_SURFACE('',#52326,2.39999999999999,0.1) ;
#45710 = TOROIDAL_SURFACE('',#52364,2.29999999999999,0.2) ;
#45711 = TOROIDAL_SURFACE('',#52401,2.4,0.1) ;
#45712 = TOROIDAL_SURFACE('',#52439,2.3,0.2) ;
#45713 = TOROIDAL_SURFACE('',#52459,0.0999999999999801,0.0499999999999901) ;
#45714 = TOROIDAL_SURFACE('',#52476,0.0999999999999801,0.0500000000000034) ;
#45715 = TOROIDAL_SURFACE('',#52557,0.48,0.24) ;
#45716 = TOROIDAL_SURFACE('',#52583,0.48,0.24) ;
#45717 = TOROIDAL_SURFACE('',#52659,0.14,0.1) ;
#45718 = TOROIDAL_SURFACE('',#52669,0.14,0.1) ;
#45719 = TOROIDAL_SURFACE('',#52677,0.2,0.1) ;
#45720 = TOROIDAL_SURFACE('',#52681,0.45,0.3) ;
#45721 = TOROIDAL_SURFACE('',#52685,0.2,0.1) ;
#45722 = TOROIDAL_SURFACE('',#52691,0.45,0.3) ;
#45723 = TOROIDAL_SURFACE('',#52709,4.09999999999997,0.1) ;
#45724 = TOROIDAL_SURFACE('',#52715,0.9,0.1) ;
#45725 = TOROIDAL_SURFACE('',#52719,0.700000000000129,0.1) ;
#45726 = TOROIDAL_SURFACE('',#52725,0.500000000000129,0.1) ;
#45727 = TOROIDAL_SURFACE('',#52732,0.2,0.1) ;
#45728 = TOROIDAL_SURFACE('',#52754,0.200000000000002,0.100000000000002) ;
#45729 = TOROIDAL_SURFACE('',#52761,0.800000000000003,0.1) ;
#45730 = TOROIDAL_SURFACE('',#52773,3.79999999999997,0.1) ;
#45731 = TOROIDAL_SURFACE('',#52779,3.79999999999982,0.1) ;
#45732 = TOROIDAL_SURFACE('',#52784,0.65,0.1) ;
#45733 = TOROIDAL_SURFACE('',#52790,0.65,0.1) ;
#45734 = TOROIDAL_SURFACE('',#52826,1.9,0.1) ;
#45735 = TOROIDAL_SURFACE('',#52838,0.2,0.1) ;
#45736 = TOROIDAL_SURFACE('',#52854,0.199999999999969,0.0999999999999847) ;
#45737 = TOROIDAL_SURFACE('',#52931,3.,0.1) ;
#45738 = TOROIDAL_SURFACE('',#52933,4.09999999999997,0.1) ;
#45739 = TOROIDAL_SURFACE('',#52949,0.699999999999915,0.1) ;
#45740 = TOROIDAL_SURFACE('',#52955,0.9,0.1) ;
#45741 = TOROIDAL_SURFACE('',#52962,0.600000000000114,0.1) ;
#45742 = TOROIDAL_SURFACE('',#52971,1.1,0.1) ;
#45743 = TOROIDAL_SURFACE('',#52978,0.3999999999999,0.1) ;
#45744 = TOROIDAL_SURFACE('',#52985,0.400000000000114,0.1) ;
#45745 = TOROIDAL_SURFACE('',#53015,0.200000000000031,0.100000000000016) ;
#45746 = TOROIDAL_SURFACE('',#53022,0.6,0.1) ;
#45747 = TOROIDAL_SURFACE('',#53025,0.200000000000031,0.0999999999999979) ;
#45748 = TOROIDAL_SURFACE('',#53032,0.6,0.1) ;
#45749 = TOROIDAL_SURFACE('',#53045,0.299999999999996,0.1) ;
#45750 = TOROIDAL_SURFACE('',#53050,0.300000000000031,0.1) ;
#45751 = TOROIDAL_SURFACE('',#53058,0.3,0.1) ;
#45752 = TOROIDAL_SURFACE('',#53064,0.300000000000031,0.1) ;
#45753 = TOROIDAL_SURFACE('',#53070,0.3,0.1) ;
#45754 = TOROIDAL_SURFACE('',#53076,0.3,0.1) ;
#45755 = TOROIDAL_SURFACE('',#53110,0.199999999999996,0.0999999999999979) ;
#45756 = TOROIDAL_SURFACE('',#53115,0.199999999999996,0.0999999999999979) ;
#45757 = TOROIDAL_SURFACE('',#53124,0.400000000000007,0.1) ;
#45758 = TOROIDAL_SURFACE('',#53135,0.400000000000007,0.1) ;
#45759 = TOROIDAL_SURFACE('',#53157,0.699999999999915,0.1) ;
#45760 = TOROIDAL_SURFACE('',#53162,0.9,0.1) ;
#45761 = TOROIDAL_SURFACE('',#53167,0.6,0.1) ;
#45762 = TOROIDAL_SURFACE('',#53172,0.65,0.1) ;
#45763 = TOROIDAL_SURFACE('',#53177,0.85,0.1) ;
#45764 = TOROIDAL_SURFACE('',#53191,1.1,0.1) ;
#45765 = TOROIDAL_SURFACE('',#53195,0.500000000000129,0.1) ;
#45766 = TOROIDAL_SURFACE('',#53200,0.700000000000129,0.1) ;
#45767 = TOROIDAL_SURFACE('',#53203,0.9,0.1) ;
#45768 = TOROIDAL_SURFACE('',#53208,4.09999999999997,0.1) ;
#45769 = TOROIDAL_SURFACE('',#53212,1.40000000000004,0.1) ;
#45770 = TOROIDAL_SURFACE('',#53228,1.4,0.1) ;
#45771 = TOROIDAL_SURFACE('',#53232,0.400000000000007,0.1) ;
#45772 = TOROIDAL_SURFACE('',#53237,0.65,0.1) ;
#45773 = TOROIDAL_SURFACE('',#53242,0.6,0.1) ;
#45774 = TOROIDAL_SURFACE('',#53246,0.4,0.1) ;
#45775 = TOROIDAL_SURFACE('',#53254,0.400000000000043,0.1) ;
#45776 = TOROIDAL_SURFACE('',#53260,0.400000000000007,0.1) ;
#45777 = TOROIDAL_SURFACE('',#53265,0.3,0.1) ;
#45778 = TOROIDAL_SURFACE('',#53298,0.65,0.1) ;
#45779 = TOROIDAL_SURFACE('',#53399,3.79999999999997,0.1) ;
#45780 = TOROIDAL_SURFACE('',#53404,1.40000000000004,0.1) ;
#45781 = TOROIDAL_SURFACE('',#53506,0.599999999999972,0.1) ;
#45782 = TOROIDAL_SURFACE('',#53516,0.399999999999963,0.1) ;
#45783 = TOROIDAL_SURFACE('',#53538,0.599999999999972,0.1) ;
#45784 = TOROIDAL_SURFACE('',#53548,0.399999999999963,0.1) ;
#45785 = TOROIDAL_SURFACE('',#53656,0.199999999999963,0.1) ;
#45786 = TOROIDAL_SURFACE('',#53659,0.799999999999972,0.1) ;
#45787 = TOROIDAL_SURFACE('',#53682,0.799999999999972,0.1) ;
#45788 = TOROIDAL_SURFACE('',#53688,0.199999999999963,0.1) ;
#45789 = TOROIDAL_SURFACE('',#53755,4.56491106406736,0.5) ;
#45790 = TOROIDAL_SURFACE('',#53761,4.55,0.5) ;
#45791 = TOROIDAL_SURFACE('',#53772,4.56491106406736,0.5) ;
#45792 = TOROIDAL_SURFACE('',#53779,4.55,0.5) ;
#45793 = TOROIDAL_SURFACE('',#53784,4.55,0.5) ;
#45794 = TOROIDAL_SURFACE('',#53792,4.55,0.5) ;
#45795 = TOROIDAL_SURFACE('',#53798,4.56491106406736,0.5) ;
#45796 = TOROIDAL_SURFACE('',#53805,4.56491106406736,0.5) ;
#45797 = TOROIDAL_SURFACE('',#54043,3.96824583655185,1.) ;
#45798 = TOROIDAL_SURFACE('',#54048,4.,1.) ;
#45799 = TOROIDAL_SURFACE('',#54057,4.95,0.15) ;
#45800 = TOROIDAL_SURFACE('',#54061,0.350000000000003,0.15) ;
#45801 = TOROIDAL_SURFACE('',#54065,4.95,0.15) ;
#45802 = TOROIDAL_SURFACE('',#54069,0.350000000000003,0.15) ;
#45803 = TOROIDAL_SURFACE('',#54073,4.95,0.15) ;
#45804 = TOROIDAL_SURFACE('',#54077,0.350000000000003,0.15) ;
#45805 = TOROIDAL_SURFACE('',#54081,4.95,0.15) ;
#45806 = TOROIDAL_SURFACE('',#54085,0.350000000000003,0.15) ;
#45807 = TOROIDAL_SURFACE('',#54089,4.95,0.15) ;
#45808 = TOROIDAL_SURFACE('',#54093,0.350000000000003,0.15) ;
#45809 = TOROIDAL_SURFACE('',#54097,4.95,0.15) ;
#45810 = TOROIDAL_SURFACE('',#54101,0.350000000000003,0.15) ;
#45811 = TOROIDAL_SURFACE('',#54105,4.95,0.15) ;
#45812 = TOROIDAL_SURFACE('',#54109,0.350000000000003,0.15) ;
#45813 = TOROIDAL_SURFACE('',#54113,4.95,0.15) ;
#45814 = TOROIDAL_SURFACE('',#54117,0.350000000000003,0.15) ;
#45815 = TOROIDAL_SURFACE('',#54121,4.95,0.15) ;
#45816 = TOROIDAL_SURFACE('',#54125,0.350000000000003,0.15) ;
#45817 = TOROIDAL_SURFACE('',#54129,4.95,0.15) ;
#45818 = TOROIDAL_SURFACE('',#54133,0.350000000000003,0.15) ;
#45819 = TOROIDAL_SURFACE('',#54137,4.95,0.15) ;
#45820 = TOROIDAL_SURFACE('',#54141,0.350000000000003,0.15) ;
#45821 = TOROIDAL_SURFACE('',#54145,4.95,0.15) ;
#45822 = TOROIDAL_SURFACE('',#54149,0.350000000000003,0.15) ;
#45823 = TOROIDAL_SURFACE('',#54153,4.95,0.15) ;
#45824 = TOROIDAL_SURFACE('',#54157,0.350000000000003,0.15) ;
#45825 = TOROIDAL_SURFACE('',#54161,4.95,0.15) ;
#45826 = TOROIDAL_SURFACE('',#54165,0.350000000000003,0.15) ;
#45827 = TOROIDAL_SURFACE('',#54169,4.95,0.15) ;
#45828 = TOROIDAL_SURFACE('',#54173,0.350000000000003,0.15) ;
#45829 = TOROIDAL_SURFACE('',#54177,4.95,0.15) ;
#45830 = TOROIDAL_SURFACE('',#54181,0.350000000000003,0.15) ;
#45831 = TOROIDAL_SURFACE('',#54185,4.95,0.15) ;
#45832 = TOROIDAL_SURFACE('',#54189,0.350000000000003,0.15) ;
#45833 = TOROIDAL_SURFACE('',#54193,4.95,0.15) ;
#45834 = TOROIDAL_SURFACE('',#54197,0.350000000000003,0.15) ;
#45835 = TOROIDAL_SURFACE('',#54201,4.95,0.15) ;
#45836 = TOROIDAL_SURFACE('',#54205,0.350000000000003,0.15) ;
#45837 = TOROIDAL_SURFACE('',#54209,4.95,0.15) ;
#45838 = TOROIDAL_SURFACE('',#54213,0.350000000000003,0.15) ;
#45839 = TOROIDAL_SURFACE('',#54316,4.95,0.15) ;
#45840 = TOROIDAL_SURFACE('',#54320,4.95,0.15) ;
#45841 = TOROIDAL_SURFACE('',#54403,4.95,0.15) ;
#45842 = TOROIDAL_SURFACE('',#54408,4.95,0.15) ;
#45843 = TOROIDAL_SURFACE('',#54412,4.95,0.15) ;
#45844 = TOROIDAL_SURFACE('',#54416,4.95,0.15) ;
#45845 = TOROIDAL_SURFACE('',#54420,4.95,0.15) ;
#45846 = TOROIDAL_SURFACE('',#54424,4.95,0.15) ;
#45847 = TOROIDAL_SURFACE('',#54428,4.95,0.15) ;
#45848 = TOROIDAL_SURFACE('',#54432,4.95,0.15) ;
#45849 = TOROIDAL_SURFACE('',#54436,4.95,0.15) ;
#45850 = TOROIDAL_SURFACE('',#54440,4.95,0.15) ;
#45851 = TOROIDAL_SURFACE('',#54444,4.95,0.15) ;
#45852 = TOROIDAL_SURFACE('',#54446,0.350000000000003,0.15) ;
#45853 = TOROIDAL_SURFACE('',#54447,0.350000000000003,0.15) ;
#45854 = TOROIDAL_SURFACE('',#54448,4.95,0.15) ;
#45855 = TOROIDAL_SURFACE('',#54451,0.350000000000003,0.15) ;
#45856 = TOROIDAL_SURFACE('',#54453,0.350000000000003,0.15) ;
#45857 = TOROIDAL_SURFACE('',#54454,4.95,0.15) ;
#45858 = TOROIDAL_SURFACE('',#54457,0.350000000000003,0.15) ;
#45859 = TOROIDAL_SURFACE('',#54459,0.350000000000003,0.15) ;
#45860 = TOROIDAL_SURFACE('',#54460,4.95,0.15) ;
#45861 = TOROIDAL_SURFACE('',#54463,0.350000000000003,0.15) ;
#45862 = TOROIDAL_SURFACE('',#54465,0.350000000000003,0.15) ;
#45863 = TOROIDAL_SURFACE('',#54466,4.95,0.15) ;
#45864 = TOROIDAL_SURFACE('',#54469,0.350000000000003,0.15) ;
#45865 = TOROIDAL_SURFACE('',#54471,0.350000000000003,0.15) ;
#45866 = TOROIDAL_SURFACE('',#54472,4.95,0.15) ;
#45867 = TOROIDAL_SURFACE('',#54475,0.350000000000003,0.15) ;
#45868 = TOROIDAL_SURFACE('',#54477,0.350000000000003,0.15) ;
#45869 = TOROIDAL_SURFACE('',#54478,4.95,0.15) ;
#45870 = TOROIDAL_SURFACE('',#54481,0.350000000000003,0.15) ;
#45871 = TOROIDAL_SURFACE('',#54483,0.350000000000003,0.15) ;
#45872 = TOROIDAL_SURFACE('',#54484,4.95,0.15) ;
#45873 = TOROIDAL_SURFACE('',#54487,0.350000000000003,0.15) ;
#45874 = TOROIDAL_SURFACE('',#54489,0.350000000000003,0.15) ;
#45875 = TOROIDAL_SURFACE('',#54490,4.95,0.15) ;
#45876 = TOROIDAL_SURFACE('',#54493,0.350000000000003,0.15) ;
#45877 = TOROIDAL_SURFACE('',#54495,0.350000000000003,0.15) ;
#45878 = TOROIDAL_SURFACE('',#54496,4.95,0.15) ;
#45879 = TOROIDAL_SURFACE('',#54499,0.350000000000003,0.15) ;
#45880 = TOROIDAL_SURFACE('',#54501,0.350000000000003,0.15) ;
#45881 = TOROIDAL_SURFACE('',#54545,3.96824583655185,1.) ;
#45882 = TOROIDAL_SURFACE('',#54550,4.,1.) ;
#45883 = TOROIDAL_SURFACE('',#54559,4.95,0.15) ;
#45884 = TOROIDAL_SURFACE('',#54563,0.350000000000003,0.15) ;
#45885 = TOROIDAL_SURFACE('',#54567,4.95,0.15) ;
#45886 = TOROIDAL_SURFACE('',#54571,0.350000000000003,0.15) ;
#45887 = TOROIDAL_SURFACE('',#54575,4.95,0.15) ;
#45888 = TOROIDAL_SURFACE('',#54579,0.350000000000003,0.15) ;
#45889 = TOROIDAL_SURFACE('',#54583,4.95,0.15) ;
#45890 = TOROIDAL_SURFACE('',#54587,0.350000000000003,0.15) ;
#45891 = TOROIDAL_SURFACE('',#54591,4.95,0.15) ;
#45892 = TOROIDAL_SURFACE('',#54595,0.350000000000003,0.15) ;
#45893 = TOROIDAL_SURFACE('',#54599,4.95,0.15) ;
#45894 = TOROIDAL_SURFACE('',#54603,0.350000000000003,0.15) ;
#45895 = TOROIDAL_SURFACE('',#54607,4.95,0.15) ;
#45896 = TOROIDAL_SURFACE('',#54611,0.350000000000003,0.15) ;
#45897 = TOROIDAL_SURFACE('',#54615,4.95,0.15) ;
#45898 = TOROIDAL_SURFACE('',#54619,0.350000000000003,0.15) ;
#45899 = TOROIDAL_SURFACE('',#54623,4.95,0.15) ;
#45900 = TOROIDAL_SURFACE('',#54627,0.350000000000003,0.15) ;
#45901 = TOROIDAL_SURFACE('',#54631,4.95,0.15) ;
#45902 = TOROIDAL_SURFACE('',#54635,0.350000000000003,0.15) ;
#45903 = TOROIDAL_SURFACE('',#54639,4.95,0.15) ;
#45904 = TOROIDAL_SURFACE('',#54643,0.350000000000003,0.15) ;
#45905 = TOROIDAL_SURFACE('',#54647,4.95,0.15) ;
#45906 = TOROIDAL_SURFACE('',#54651,0.350000000000003,0.15) ;
#45907 = TOROIDAL_SURFACE('',#54655,4.95,0.15) ;
#45908 = TOROIDAL_SURFACE('',#54659,0.350000000000003,0.15) ;
#45909 = TOROIDAL_SURFACE('',#54663,4.95,0.15) ;
#45910 = TOROIDAL_SURFACE('',#54667,0.350000000000003,0.15) ;
#45911 = TOROIDAL_SURFACE('',#54671,4.95,0.15) ;
#45912 = TOROIDAL_SURFACE('',#54675,0.350000000000003,0.15) ;
#45913 = TOROIDAL_SURFACE('',#54679,4.95,0.15) ;
#45914 = TOROIDAL_SURFACE('',#54683,0.350000000000003,0.15) ;
#45915 = TOROIDAL_SURFACE('',#54687,4.95,0.15) ;
#45916 = TOROIDAL_SURFACE('',#54691,0.350000000000003,0.15) ;
#45917 = TOROIDAL_SURFACE('',#54695,4.95,0.15) ;
#45918 = TOROIDAL_SURFACE('',#54699,0.350000000000003,0.15) ;
#45919 = TOROIDAL_SURFACE('',#54703,4.95,0.15) ;
#45920 = TOROIDAL_SURFACE('',#54707,0.350000000000003,0.15) ;
#45921 = TOROIDAL_SURFACE('',#54711,4.95,0.15) ;
#45922 = TOROIDAL_SURFACE('',#54715,0.350000000000003,0.15) ;
#45923 = TOROIDAL_SURFACE('',#54818,4.95,0.15) ;
#45924 = TOROIDAL_SURFACE('',#54822,4.95,0.15) ;
#45925 = TOROIDAL_SURFACE('',#54905,4.95,0.15) ;
#45926 = TOROIDAL_SURFACE('',#54910,4.95,0.15) ;
#45927 = TOROIDAL_SURFACE('',#54914,4.95,0.15) ;
#45928 = TOROIDAL_SURFACE('',#54918,4.95,0.15) ;
#45929 = TOROIDAL_SURFACE('',#54922,4.95,0.15) ;
#45930 = TOROIDAL_SURFACE('',#54926,4.95,0.15) ;
#45931 = TOROIDAL_SURFACE('',#54930,4.95,0.15) ;
#45932 = TOROIDAL_SURFACE('',#54934,4.95,0.15) ;
#45933 = TOROIDAL_SURFACE('',#54938,4.95,0.15) ;
#45934 = TOROIDAL_SURFACE('',#54942,4.95,0.15) ;
#45935 = TOROIDAL_SURFACE('',#54946,4.95,0.15) ;
#45936 = TOROIDAL_SURFACE('',#54948,0.350000000000003,0.15) ;
#45937 = TOROIDAL_SURFACE('',#54949,0.350000000000003,0.15) ;
#45938 = TOROIDAL_SURFACE('',#54950,4.95,0.15) ;
#45939 = TOROIDAL_SURFACE('',#54953,0.350000000000003,0.15) ;
#45940 = TOROIDAL_SURFACE('',#54955,0.350000000000003,0.15) ;
#45941 = TOROIDAL_SURFACE('',#54956,4.95,0.15) ;
#45942 = TOROIDAL_SURFACE('',#54959,0.350000000000003,0.15) ;
#45943 = TOROIDAL_SURFACE('',#54961,0.350000000000003,0.15) ;
#45944 = TOROIDAL_SURFACE('',#54962,4.95,0.15) ;
#45945 = TOROIDAL_SURFACE('',#54965,0.350000000000003,0.15) ;
#45946 = TOROIDAL_SURFACE('',#54967,0.350000000000003,0.15) ;
#45947 = TOROIDAL_SURFACE('',#54968,4.95,0.15) ;
#45948 = TOROIDAL_SURFACE('',#54971,0.350000000000003,0.15) ;
#45949 = TOROIDAL_SURFACE('',#54973,0.350000000000003,0.15) ;
#45950 = TOROIDAL_SURFACE('',#54974,4.95,0.15) ;
#45951 = TOROIDAL_SURFACE('',#54977,0.350000000000003,0.15) ;
#45952 = TOROIDAL_SURFACE('',#54979,0.350000000000003,0.15) ;
#45953 = TOROIDAL_SURFACE('',#54980,4.95,0.15) ;
#45954 = TOROIDAL_SURFACE('',#54983,0.350000000000003,0.15) ;
#45955 = TOROIDAL_SURFACE('',#54985,0.350000000000003,0.15) ;
#45956 = TOROIDAL_SURFACE('',#54986,4.95,0.15) ;
#45957 = TOROIDAL_SURFACE('',#54989,0.350000000000003,0.15) ;
#45958 = TOROIDAL_SURFACE('',#54991,0.350000000000003,0.15) ;
#45959 = TOROIDAL_SURFACE('',#54992,4.95,0.15) ;
#45960 = TOROIDAL_SURFACE('',#54995,0.350000000000003,0.15) ;
#45961 = TOROIDAL_SURFACE('',#54997,0.350000000000003,0.15) ;
#45962 = TOROIDAL_SURFACE('',#54998,4.95,0.15) ;
#45963 = TOROIDAL_SURFACE('',#55001,0.350000000000003,0.15) ;
#45964 = TOROIDAL_SURFACE('',#55003,0.350000000000003,0.15) ;
#45965 = ADVANCED_FACE('',(#10747),#45432,.T.) ;
#45966 = ADVANCED_FACE('',(#10748),#9460,.T.) ;
#45967 = ADVANCED_FACE('',(#10749),#2216,.F.) ;
#45968 = ADVANCED_FACE('',(#10750),#9461,.F.) ;
#45969 = ADVANCED_FACE('',(#10751),#9462,.F.) ;
#45970 = ADVANCED_FACE('',(#10752),#45433,.F.) ;
#45971 = ADVANCED_FACE('',(#10753),#9463,.F.) ;
#45972 = ADVANCED_FACE('',(#10754),#9464,.F.) ;
#45973 = ADVANCED_FACE('',(#10755),#9465,.F.) ;
#45974 = ADVANCED_FACE('',(#10756),#45434,.F.) ;
#45975 = ADVANCED_FACE('',(#10757),#9466,.F.) ;
#45976 = ADVANCED_FACE('',(#10758),#9467,.F.) ;
#45977 = ADVANCED_FACE('',(#10759),#9468,.F.) ;
#45978 = ADVANCED_FACE('',(#10760),#45435,.F.) ;
#45979 = ADVANCED_FACE('',(#10761),#9469,.F.) ;
#45980 = ADVANCED_FACE('',(#10762),#9470,.F.) ;
#45981 = ADVANCED_FACE('',(#10763),#45436,.F.) ;
#45982 = ADVANCED_FACE('',(#10764),#9471,.F.) ;
#45983 = ADVANCED_FACE('',(#10765),#9472,.F.) ;
#45984 = ADVANCED_FACE('',(#10766),#2119,.F.) ;
#45985 = ADVANCED_FACE('',(#10767),#2120,.F.) ;
#45986 = ADVANCED_FACE('',(#10768),#2121,.F.) ;
#45987 = ADVANCED_FACE('',(#10769),#2122,.F.) ;
#45988 = ADVANCED_FACE('',(#10770),#2123,.F.) ;
#45989 = ADVANCED_FACE('',(#10771),#2124,.F.) ;
#45990 = ADVANCED_FACE('',(#10772),#2125,.F.) ;
#45991 = ADVANCED_FACE('',(#10773),#2126,.F.) ;
#45992 = ADVANCED_FACE('',(#10774),#2217,.F.) ;
#45993 = ADVANCED_FACE('',(#10775),#9473,.F.) ;
#45994 = ADVANCED_FACE('',(#10776),#2218,.F.) ;
#45995 = ADVANCED_FACE('',(#10777),#9474,.F.) ;
#45996 = ADVANCED_FACE('',(#10778),#2219,.F.) ;
#45997 = ADVANCED_FACE('',(#10779),#9475,.T.) ;
#45998 = ADVANCED_FACE('',(#10780),#2220,.F.) ;
#45999 = ADVANCED_FACE('',(#10781),#9476,.F.) ;
#46000 = ADVANCED_FACE('',(#10782),#2221,.F.) ;
#46001 = ADVANCED_FACE('',(#10783),#9477,.F.) ;
#46002 = ADVANCED_FACE('',(#10784),#2222,.F.) ;
#46003 = ADVANCED_FACE('',(#10785),#9478,.T.) ;
#46004 = ADVANCED_FACE('',(#10786),#2223,.T.) ;
#46005 = ADVANCED_FACE('',(#10787),#2127,.T.) ;
#46006 = ADVANCED_FACE('',(#10788),#2128,.T.) ;
#46007 = ADVANCED_FACE('',(#10789),#2129,.T.) ;
#46008 = ADVANCED_FACE('',(#10790),#45437,.T.) ;
#46009 = ADVANCED_FACE('',(#10791),#2130,.T.) ;
#46010 = ADVANCED_FACE('',(#10792),#2131,.T.) ;
#46011 = ADVANCED_FACE('',(#10793),#1769,.F.) ;
#46012 = ADVANCED_FACE('',(#10794),#2132,.T.) ;
#46013 = ADVANCED_FACE('',(#10795),#2133,.T.) ;
#46014 = ADVANCED_FACE('',(#10796),#45438,.T.) ;
#46015 = ADVANCED_FACE('',(#10797),#2134,.T.) ;
#46016 = ADVANCED_FACE('',(#10798),#2135,.T.) ;
#46017 = ADVANCED_FACE('',(#10799),#1770,.F.) ;
#46018 = ADVANCED_FACE('',(#10800),#2136,.T.) ;
#46019 = ADVANCED_FACE('',(#10801),#2137,.T.) ;
#46020 = ADVANCED_FACE('',(#10802),#45439,.T.) ;
#46021 = ADVANCED_FACE('',(#10803),#2138,.T.) ;
#46022 = ADVANCED_FACE('',(#10804),#2139,.T.) ;
#46023 = ADVANCED_FACE('',(#10805),#1771,.F.) ;
#46024 = ADVANCED_FACE('',(#10806),#2140,.T.) ;
#46025 = ADVANCED_FACE('',(#10807),#2141,.T.) ;
#46026 = ADVANCED_FACE('',(#10808),#45440,.T.) ;
#46027 = ADVANCED_FACE('',(#10809),#2142,.T.) ;
#46028 = ADVANCED_FACE('',(#10810),#2143,.T.) ;
#46029 = ADVANCED_FACE('',(#10811),#1772,.F.) ;
#46030 = ADVANCED_FACE('',(#10812),#2144,.T.) ;
#46031 = ADVANCED_FACE('',(#10813),#2145,.T.) ;
#46032 = ADVANCED_FACE('',(#10814),#45441,.T.) ;
#46033 = ADVANCED_FACE('',(#10815),#2146,.T.) ;
#46034 = ADVANCED_FACE('',(#10816),#2147,.T.) ;
#46035 = ADVANCED_FACE('',(#10817),#1773,.F.) ;
#46036 = ADVANCED_FACE('',(#10818),#2148,.T.) ;
#46037 = ADVANCED_FACE('',(#10819),#2149,.T.) ;
#46038 = ADVANCED_FACE('',(#10820),#45442,.T.) ;
#46039 = ADVANCED_FACE('',(#10821),#2150,.T.) ;
#46040 = ADVANCED_FACE('',(#10822),#2151,.T.) ;
#46041 = ADVANCED_FACE('',(#10823),#1774,.F.) ;
#46042 = ADVANCED_FACE('',(#10824),#2152,.T.) ;
#46043 = ADVANCED_FACE('',(#10825),#2153,.T.) ;
#46044 = ADVANCED_FACE('',(#10826),#45443,.T.) ;
#46045 = ADVANCED_FACE('',(#10827),#2154,.T.) ;
#46046 = ADVANCED_FACE('',(#10828),#2155,.T.) ;
#46047 = ADVANCED_FACE('',(#10829),#1775,.F.) ;
#46048 = ADVANCED_FACE('',(#10830),#2156,.T.) ;
#46049 = ADVANCED_FACE('',(#10831),#2157,.T.) ;
#46050 = ADVANCED_FACE('',(#10832),#45444,.T.) ;
#46051 = ADVANCED_FACE('',(#10833),#2158,.T.) ;
#46052 = ADVANCED_FACE('',(#10834),#2159,.T.) ;
#46053 = ADVANCED_FACE('',(#10835),#1776,.F.) ;
#46054 = ADVANCED_FACE('',(#10836),#2160,.T.) ;
#46055 = ADVANCED_FACE('',(#10837),#2161,.T.) ;
#46056 = ADVANCED_FACE('',(#10838),#45445,.T.) ;
#46057 = ADVANCED_FACE('',(#10839),#2162,.T.) ;
#46058 = ADVANCED_FACE('',(#10840),#2163,.T.) ;
#46059 = ADVANCED_FACE('',(#10841),#1777,.F.) ;
#46060 = ADVANCED_FACE('',(#10842),#2164,.T.) ;
#46061 = ADVANCED_FACE('',(#10843),#2165,.T.) ;
#46062 = ADVANCED_FACE('',(#10844),#45446,.T.) ;
#46063 = ADVANCED_FACE('',(#10845),#2166,.T.) ;
#46064 = ADVANCED_FACE('',(#10846),#1778,.F.) ;
#46065 = ADVANCED_FACE('',(#10847),#45447,.T.) ;
#46066 = ADVANCED_FACE('',(#10848),#9479,.T.) ;
#46067 = ADVANCED_FACE('',(#10849),#9480,.T.) ;
#46068 = ADVANCED_FACE('',(#10850),#1779,.F.) ;
#46069 = ADVANCED_FACE('',(#10851),#9481,.T.) ;
#46070 = ADVANCED_FACE('',(#10852),#45448,.T.) ;
#46071 = ADVANCED_FACE('',(#10853),#9482,.T.) ;
#46072 = ADVANCED_FACE('',(#10854),#45449,.T.) ;
#46073 = ADVANCED_FACE('',(#10855),#9483,.T.) ;
#46074 = ADVANCED_FACE('',(#10856),#45450,.T.) ;
#46075 = ADVANCED_FACE('',(#10857),#9484,.T.) ;
#46076 = ADVANCED_FACE('',(#10858),#45451,.T.) ;
#46077 = ADVANCED_FACE('',(#10859),#1780,.F.) ;
#46078 = ADVANCED_FACE('',(#10860),#9485,.T.) ;
#46079 = ADVANCED_FACE('',(#10861),#9486,.T.) ;
#46080 = ADVANCED_FACE('',(#10862),#45452,.T.) ;
#46081 = ADVANCED_FACE('',(#10863),#9487,.T.) ;
#46082 = ADVANCED_FACE('',(#10864),#45453,.T.) ;
#46083 = ADVANCED_FACE('',(#10865),#9488,.T.) ;
#46084 = ADVANCED_FACE('',(#10866),#45454,.T.) ;
#46085 = ADVANCED_FACE('',(#10867),#1781,.F.) ;
#46086 = ADVANCED_FACE('',(#10868),#9489,.T.) ;
#46087 = ADVANCED_FACE('',(#10869),#9490,.T.) ;
#46088 = ADVANCED_FACE('',(#10870),#45455,.T.) ;
#46089 = ADVANCED_FACE('',(#10871),#9491,.T.) ;
#46090 = ADVANCED_FACE('',(#10872),#45456,.T.) ;
#46091 = ADVANCED_FACE('',(#10873),#9492,.T.) ;
#46092 = ADVANCED_FACE('',(#10874),#45457,.T.) ;
#46093 = ADVANCED_FACE('',(#10875),#1782,.F.) ;
#46094 = ADVANCED_FACE('',(#10876),#9493,.T.) ;
#46095 = ADVANCED_FACE('',(#10877),#9494,.T.) ;
#46096 = ADVANCED_FACE('',(#10878),#45458,.T.) ;
#46097 = ADVANCED_FACE('',(#10879),#9495,.T.) ;
#46098 = ADVANCED_FACE('',(#10880),#45459,.T.) ;
#46099 = ADVANCED_FACE('',(#10881),#9496,.T.) ;
#46100 = ADVANCED_FACE('',(#10882),#45460,.T.) ;
#46101 = ADVANCED_FACE('',(#10883),#1783,.F.) ;
#46102 = ADVANCED_FACE('',(#10884),#9497,.T.) ;
#46103 = ADVANCED_FACE('',(#10885),#9498,.T.) ;
#46104 = ADVANCED_FACE('',(#10886),#45461,.T.) ;
#46105 = ADVANCED_FACE('',(#10887),#9499,.T.) ;
#46106 = ADVANCED_FACE('',(#10888),#45462,.T.) ;
#46107 = ADVANCED_FACE('',(#10889),#9500,.T.) ;
#46108 = ADVANCED_FACE('',(#10890),#45463,.T.) ;
#46109 = ADVANCED_FACE('',(#10891),#1784,.F.) ;
#46110 = ADVANCED_FACE('',(#10892),#9501,.T.) ;
#46111 = ADVANCED_FACE('',(#10893),#9502,.T.) ;
#46112 = ADVANCED_FACE('',(#10894),#45464,.T.) ;
#46113 = ADVANCED_FACE('',(#10895),#9503,.T.) ;
#46114 = ADVANCED_FACE('',(#10896),#45465,.T.) ;
#46115 = ADVANCED_FACE('',(#10897),#9504,.T.) ;
#46116 = ADVANCED_FACE('',(#10898),#45466,.T.) ;
#46117 = ADVANCED_FACE('',(#10899),#1785,.F.) ;
#46118 = ADVANCED_FACE('',(#10900),#9505,.T.) ;
#46119 = ADVANCED_FACE('',(#10901),#9506,.T.) ;
#46120 = ADVANCED_FACE('',(#10902),#45467,.T.) ;
#46121 = ADVANCED_FACE('',(#10903),#9507,.T.) ;
#46122 = ADVANCED_FACE('',(#10904),#45468,.T.) ;
#46123 = ADVANCED_FACE('',(#10905),#9508,.T.) ;
#46124 = ADVANCED_FACE('',(#10906),#45469,.T.) ;
#46125 = ADVANCED_FACE('',(#10907),#1786,.F.) ;
#46126 = ADVANCED_FACE('',(#10908),#9509,.T.) ;
#46127 = ADVANCED_FACE('',(#10909),#9510,.T.) ;
#46128 = ADVANCED_FACE('',(#10910),#45470,.T.) ;
#46129 = ADVANCED_FACE('',(#10911),#9511,.T.) ;
#46130 = ADVANCED_FACE('',(#10912),#45471,.T.) ;
#46131 = ADVANCED_FACE('',(#10913),#9512,.T.) ;
#46132 = ADVANCED_FACE('',(#10914),#45472,.T.) ;
#46133 = ADVANCED_FACE('',(#10915),#1787,.F.) ;
#46134 = ADVANCED_FACE('',(#10916),#9513,.T.) ;
#46135 = ADVANCED_FACE('',(#10917),#9514,.T.) ;
#46136 = ADVANCED_FACE('',(#10918),#45473,.T.) ;
#46137 = ADVANCED_FACE('',(#10919),#9515,.T.) ;
#46138 = ADVANCED_FACE('',(#10920),#45474,.T.) ;
#46139 = ADVANCED_FACE('',(#10921),#9516,.T.) ;
#46140 = ADVANCED_FACE('',(#10922),#45475,.T.) ;
#46141 = ADVANCED_FACE('',(#10923),#1788,.F.) ;
#46142 = ADVANCED_FACE('',(#10924),#9517,.T.) ;
#46143 = ADVANCED_FACE('',(#10925),#9518,.T.) ;
#46144 = ADVANCED_FACE('',(#10926),#45476,.T.) ;
#46145 = ADVANCED_FACE('',(#10927),#9519,.F.) ;
#46146 = ADVANCED_FACE('',(#10928),#9520,.F.) ;
#46147 = ADVANCED_FACE('',(#10929),#9521,.F.) ;
#46148 = ADVANCED_FACE('',(#10930),#9522,.F.) ;
#46149 = ADVANCED_FACE('',(#10931),#9523,.F.) ;
#46150 = ADVANCED_FACE('',(#10932),#9524,.F.) ;
#46151 = ADVANCED_FACE('',(#10933),#9525,.F.) ;
#46152 = ADVANCED_FACE('',(#10934),#9526,.F.) ;
#46153 = ADVANCED_FACE('',(#10935),#9527,.F.) ;
#46154 = ADVANCED_FACE('',(#10936),#9528,.F.) ;
#46155 = ADVANCED_FACE('',(#10937),#9529,.F.) ;
#46156 = ADVANCED_FACE('',(#10938),#9530,.F.) ;
#46157 = ADVANCED_FACE('',(#10939),#9531,.F.) ;
#46158 = ADVANCED_FACE('',(#10940),#9532,.F.) ;
#46159 = ADVANCED_FACE('',(#10941),#9533,.F.) ;
#46160 = ADVANCED_FACE('',(#10942),#9534,.F.) ;
#46161 = ADVANCED_FACE('',(#10943),#9535,.F.) ;
#46162 = ADVANCED_FACE('',(#10944),#9536,.F.) ;
#46163 = ADVANCED_FACE('',(#10945),#9537,.F.) ;
#46164 = ADVANCED_FACE('',(#10946),#9538,.F.) ;
#46165 = ADVANCED_FACE('',(#10947),#773,.T.) ;
#46166 = ADVANCED_FACE('',(#10948),#45477,.T.) ;
#46167 = ADVANCED_FACE('',(#10949,#670),#2224,.T.) ;
#46168 = ADVANCED_FACE('',(#10950),#9539,.T.) ;
#46169 = ADVANCED_FACE('',(#10951),#2225,.F.) ;
#46170 = ADVANCED_FACE('',(#10952),#45478,.T.) ;
#46171 = ADVANCED_FACE('',(#10953),#9540,.T.) ;
#46172 = ADVANCED_FACE('',(#10954),#45479,.T.) ;
#46173 = ADVANCED_FACE('',(#10955),#9541,.T.) ;
#46174 = ADVANCED_FACE('',(#10956),#9542,.T.) ;
#46175 = ADVANCED_FACE('',(#10957),#2226,.F.) ;
#46176 = ADVANCED_FACE('',(#10958),#45480,.T.) ;
#46177 = ADVANCED_FACE('',(#10959),#9543,.T.) ;
#46178 = ADVANCED_FACE('',(#10960),#9544,.T.) ;
#46179 = ADVANCED_FACE('',(#10961),#45481,.T.) ;
#46180 = ADVANCED_FACE('',(#10962),#45482,.T.) ;
#46181 = ADVANCED_FACE('',(#10963),#45483,.T.) ;
#46182 = ADVANCED_FACE('',(#10964),#9545,.T.) ;
#46183 = ADVANCED_FACE('',(#10965),#45484,.T.) ;
#46184 = ADVANCED_FACE('',(#10966),#9546,.T.) ;
#46185 = ADVANCED_FACE('',(#10967),#9547,.T.) ;
#46186 = ADVANCED_FACE('',(#10968),#45485,.T.) ;
#46187 = ADVANCED_FACE('',(#10969),#45486,.T.) ;
#46188 = ADVANCED_FACE('',(#10970),#9548,.F.) ;
#46189 = ADVANCED_FACE('',(#10971),#45487,.T.) ;
#46190 = ADVANCED_FACE('',(#10972),#9549,.T.) ;
#46191 = ADVANCED_FACE('',(#10973),#9550,.F.) ;
#46192 = ADVANCED_FACE('',(#10974),#45488,.T.) ;
#46193 = ADVANCED_FACE('',(#10975),#9551,.T.) ;
#46194 = ADVANCED_FACE('',(#10976),#45489,.T.) ;
#46195 = ADVANCED_FACE('',(#10977),#9552,.F.) ;
#46196 = ADVANCED_FACE('',(#10978),#9553,.T.) ;
#46197 = ADVANCED_FACE('',(#10979),#9554,.F.) ;
#46198 = ADVANCED_FACE('',(#10980),#9555,.T.) ;
#46199 = ADVANCED_FACE('',(#10981),#9556,.T.) ;
#46200 = ADVANCED_FACE('',(#10982),#2227,.T.) ;
#46201 = ADVANCED_FACE('',(#10983),#2228,.T.) ;
#46202 = ADVANCED_FACE('',(#10984),#2229,.T.) ;
#46203 = ADVANCED_FACE('',(#10985),#2230,.T.) ;
#46204 = ADVANCED_FACE('',(#10986),#2231,.T.) ;
#46205 = ADVANCED_FACE('',(#10987),#2232,.T.) ;
#46206 = ADVANCED_FACE('',(#10988),#2233,.T.) ;
#46207 = ADVANCED_FACE('',(#10989),#2234,.T.) ;
#46208 = ADVANCED_FACE('',(#10990),#2235,.T.) ;
#46209 = ADVANCED_FACE('',(#10991),#2236,.T.) ;
#46210 = ADVANCED_FACE('',(#10992),#2237,.T.) ;
#46211 = ADVANCED_FACE('',(#10993),#2238,.T.) ;
#46212 = ADVANCED_FACE('',(#10994),#2239,.T.) ;
#46213 = ADVANCED_FACE('',(#10995),#2240,.T.) ;
#46214 = ADVANCED_FACE('',(#10996),#2241,.T.) ;
#46215 = ADVANCED_FACE('',(#10997),#2242,.T.) ;
#46216 = ADVANCED_FACE('',(#10998),#2243,.T.) ;
#46217 = ADVANCED_FACE('',(#10999),#2244,.T.) ;
#46218 = ADVANCED_FACE('',(#11000),#2245,.T.) ;
#46219 = ADVANCED_FACE('',(#11001),#2246,.T.) ;
#46220 = ADVANCED_FACE('',(#11002),#2247,.F.) ;
#46221 = ADVANCED_FACE('',(#11003),#2248,.F.) ;
#46222 = ADVANCED_FACE('',(#11004),#2249,.F.) ;
#46223 = ADVANCED_FACE('',(#11005),#2250,.F.) ;
#46224 = ADVANCED_FACE('',(#11006),#1789,.T.) ;
#46225 = ADVANCED_FACE('',(#11007),#1790,.T.) ;
#46226 = ADVANCED_FACE('',(#11008),#9557,.F.) ;
#46227 = ADVANCED_FACE('',(#11009),#1791,.T.) ;
#46228 = ADVANCED_FACE('',(#11010),#1792,.T.) ;
#46229 = ADVANCED_FACE('',(#11011),#2251,.T.) ;
#46230 = ADVANCED_FACE('',(#11012),#1793,.F.) ;
#46231 = ADVANCED_FACE('',(#11013),#1794,.F.) ;
#46232 = ADVANCED_FACE('',(#11014),#1795,.F.) ;
#46233 = ADVANCED_FACE('',(#11015),#1796,.F.) ;
#46234 = ADVANCED_FACE('',(#11016),#1797,.F.) ;
#46235 = ADVANCED_FACE('',(#11017),#9558,.T.) ;
#46236 = ADVANCED_FACE('',(#11018),#1798,.F.) ;
#46237 = ADVANCED_FACE('',(#11019),#1799,.F.) ;
#46238 = ADVANCED_FACE('',(#11020),#1800,.F.) ;
#46239 = ADVANCED_FACE('',(#11021),#9559,.T.) ;
#46240 = ADVANCED_FACE('',(#11022),#1801,.F.) ;
#46241 = ADVANCED_FACE('',(#11023),#1802,.T.) ;
#46242 = ADVANCED_FACE('',(#11024),#2252,.T.) ;
#46243 = ADVANCED_FACE('',(#11025),#1803,.T.) ;
#46244 = ADVANCED_FACE('',(#11026),#1804,.T.) ;
#46245 = ADVANCED_FACE('',(#11027,#671,#672,#673,#674),#2253,.T.) ;
#46246 = ADVANCED_FACE('',(#11028),#9560,.T.) ;
#46247 = ADVANCED_FACE('',(#11029),#1805,.F.) ;
#46248 = ADVANCED_FACE('',(#11030),#1806,.F.) ;
#46249 = ADVANCED_FACE('',(#11031),#1807,.F.) ;
#46250 = ADVANCED_FACE('',(#11032),#9561,.T.) ;
#46251 = ADVANCED_FACE('',(#11033),#1808,.F.) ;
#46252 = ADVANCED_FACE('',(#11034),#1809,.F.) ;
#46253 = ADVANCED_FACE('',(#11035),#1810,.F.) ;
#46254 = ADVANCED_FACE('',(#11036),#1811,.T.) ;
#46255 = ADVANCED_FACE('',(#11037),#1812,.T.) ;
#46256 = ADVANCED_FACE('',(#11038),#1813,.T.) ;
#46257 = ADVANCED_FACE('',(#11039),#2254,.T.) ;
#46258 = ADVANCED_FACE('',(#11040),#45490,.T.) ;
#46259 = ADVANCED_FACE('',(#11041),#9562,.F.) ;
#46260 = ADVANCED_FACE('',(#11042),#9563,.T.) ;
#46261 = ADVANCED_FACE('',(#11043),#45491,.T.) ;
#46262 = ADVANCED_FACE('',(#11044),#9564,.T.) ;
#46263 = ADVANCED_FACE('',(#11045),#1814,.F.) ;
#46264 = ADVANCED_FACE('',(#11046),#1815,.F.) ;
#46265 = ADVANCED_FACE('',(#11047),#1816,.F.) ;
#46266 = ADVANCED_FACE('',(#11048),#1817,.F.) ;
#46267 = ADVANCED_FACE('',(#11049),#1818,.F.) ;
#46268 = ADVANCED_FACE('',(#11050),#1819,.F.) ;
#46269 = ADVANCED_FACE('',(#11051),#9565,.T.) ;
#46270 = ADVANCED_FACE('',(#11052),#1820,.F.) ;
#46271 = ADVANCED_FACE('',(#11053),#1821,.F.) ;
#46272 = ADVANCED_FACE('',(#11054),#1822,.F.) ;
#46273 = ADVANCED_FACE('',(#11055),#1823,.F.) ;
#46274 = ADVANCED_FACE('',(#11056),#1824,.F.) ;
#46275 = ADVANCED_FACE('',(#11057),#1825,.F.) ;
#46276 = ADVANCED_FACE('',(#11058),#1826,.F.) ;
#46277 = ADVANCED_FACE('',(#11059),#9566,.T.) ;
#46278 = ADVANCED_FACE('',(#11060),#9567,.T.) ;
#46279 = ADVANCED_FACE('',(#11061),#45492,.T.) ;
#46280 = ADVANCED_FACE('',(#11062),#1827,.T.) ;
#46281 = ADVANCED_FACE('',(#11063),#9568,.T.) ;
#46282 = ADVANCED_FACE('',(#11064),#1828,.T.) ;
#46283 = ADVANCED_FACE('',(#11065),#1829,.T.) ;
#46284 = ADVANCED_FACE('',(#11066),#1830,.T.) ;
#46285 = ADVANCED_FACE('',(#11067),#1831,.F.) ;
#46286 = ADVANCED_FACE('',(#11068),#2255,.T.) ;
#46287 = ADVANCED_FACE('',(#11069),#2256,.T.) ;
#46288 = ADVANCED_FACE('',(#11070),#9569,.T.) ;
#46289 = ADVANCED_FACE('',(#11071),#2257,.T.) ;
#46290 = ADVANCED_FACE('',(#11072),#45493,.T.) ;
#46291 = ADVANCED_FACE('',(#11073),#1832,.F.) ;
#46292 = ADVANCED_FACE('',(#11074),#2167,.F.) ;
#46293 = ADVANCED_FACE('',(#11075),#1833,.T.) ;
#46294 = ADVANCED_FACE('',(#11076),#1834,.F.) ;
#46295 = ADVANCED_FACE('',(#11077),#2168,.F.) ;
#46296 = ADVANCED_FACE('',(#11078),#1835,.T.) ;
#46297 = ADVANCED_FACE('',(#11079),#1836,.T.) ;
#46298 = ADVANCED_FACE('',(#11080),#1837,.T.) ;
#46299 = ADVANCED_FACE('',(#11081),#9570,.F.) ;
#46300 = ADVANCED_FACE('',(#11082),#9571,.T.) ;
#46301 = ADVANCED_FACE('',(#11083),#1838,.F.) ;
#46302 = ADVANCED_FACE('',(#11084),#1839,.F.) ;
#46303 = ADVANCED_FACE('',(#11085),#1840,.F.) ;
#46304 = ADVANCED_FACE('',(#11086),#1841,.T.) ;
#46305 = ADVANCED_FACE('',(#11087),#1842,.T.) ;
#46306 = ADVANCED_FACE('',(#11088),#9572,.F.) ;
#46307 = ADVANCED_FACE('',(#11089),#9573,.T.) ;
#46308 = ADVANCED_FACE('',(#11090),#1843,.F.) ;
#46309 = ADVANCED_FACE('',(#11091),#1844,.F.) ;
#46310 = ADVANCED_FACE('',(#11092),#9574,.T.) ;
#46311 = ADVANCED_FACE('',(#11093),#1845,.T.) ;
#46312 = ADVANCED_FACE('',(#11094),#2258,.T.) ;
#46313 = ADVANCED_FACE('',(#11095),#1846,.T.) ;
#46314 = ADVANCED_FACE('',(#11096),#1847,.T.) ;
#46315 = ADVANCED_FACE('',(#11097),#9575,.T.) ;
#46316 = ADVANCED_FACE('',(#11098),#2259,.T.) ;
#46317 = ADVANCED_FACE('',(#11099),#1848,.T.) ;
#46318 = ADVANCED_FACE('',(#11100),#1849,.T.) ;
#46319 = ADVANCED_FACE('',(#11101),#1850,.T.) ;
#46320 = ADVANCED_FACE('',(#11102),#9576,.F.) ;
#46321 = ADVANCED_FACE('',(#11103),#1851,.T.) ;
#46322 = ADVANCED_FACE('',(#11104),#1852,.T.) ;
#46323 = ADVANCED_FACE('',(#11105),#1853,.T.) ;
#46324 = ADVANCED_FACE('',(#11106),#9577,.F.) ;
#46325 = ADVANCED_FACE('',(#11107),#2260,.T.) ;
#46326 = ADVANCED_FACE('',(#11108),#1854,.T.) ;
#46327 = ADVANCED_FACE('',(#11109),#1855,.T.) ;
#46328 = ADVANCED_FACE('',(#11110),#1856,.T.) ;
#46329 = ADVANCED_FACE('',(#11111),#9578,.F.) ;
#46330 = ADVANCED_FACE('',(#11112),#1857,.T.) ;
#46331 = ADVANCED_FACE('',(#11113),#1858,.T.) ;
#46332 = ADVANCED_FACE('',(#11114),#1859,.T.) ;
#46333 = ADVANCED_FACE('',(#11115),#9579,.F.) ;
#46334 = ADVANCED_FACE('',(#11116),#1860,.T.) ;
#46335 = ADVANCED_FACE('',(#11117),#1861,.T.) ;
#46336 = ADVANCED_FACE('',(#11118),#2261,.T.) ;
#46337 = ADVANCED_FACE('',(#11119),#2169,.F.) ;
#46338 = ADVANCED_FACE('',(#11120),#1862,.F.) ;
#46339 = ADVANCED_FACE('',(#11121),#1863,.T.) ;
#46340 = ADVANCED_FACE('',(#11122),#2170,.F.) ;
#46341 = ADVANCED_FACE('',(#11123),#9580,.F.) ;
#46342 = ADVANCED_FACE('',(#11124),#1864,.T.) ;
#46343 = ADVANCED_FACE('',(#11125),#1865,.T.) ;
#46344 = ADVANCED_FACE('',(#11126),#9581,.F.) ;
#46345 = ADVANCED_FACE('',(#11127),#1866,.T.) ;
#46346 = ADVANCED_FACE('',(#11128),#1867,.T.) ;
#46347 = ADVANCED_FACE('',(#11129),#1868,.F.) ;
#46348 = ADVANCED_FACE('',(#11130),#1869,.T.) ;
#46349 = ADVANCED_FACE('',(#11131),#1870,.F.) ;
#46350 = ADVANCED_FACE('',(#11132),#1871,.F.) ;
#46351 = ADVANCED_FACE('',(#11133),#9582,.T.) ;
#46352 = ADVANCED_FACE('',(#11134),#1872,.F.) ;
#46353 = ADVANCED_FACE('',(#11135),#1873,.F.) ;
#46354 = ADVANCED_FACE('',(#11136),#9583,.T.) ;
#46355 = ADVANCED_FACE('',(#11137),#1874,.T.) ;
#46356 = ADVANCED_FACE('',(#11138),#1875,.T.) ;
#46357 = ADVANCED_FACE('',(#11139),#2262,.T.) ;
#46358 = ADVANCED_FACE('',(#11140),#1876,.T.) ;
#46359 = ADVANCED_FACE('',(#11141,#675,#676),#2263,.F.) ;
#46360 = ADVANCED_FACE('',(#11142),#2264,.T.) ;
#46361 = ADVANCED_FACE('',(#11143),#2265,.F.) ;
#46362 = ADVANCED_FACE('',(#11144),#1877,.F.) ;
#46363 = ADVANCED_FACE('',(#11145),#2171,.F.) ;
#46364 = ADVANCED_FACE('',(#11146),#1878,.T.) ;
#46365 = ADVANCED_FACE('',(#11147),#1879,.F.) ;
#46366 = ADVANCED_FACE('',(#11148),#1880,.F.) ;
#46367 = ADVANCED_FACE('',(#11149),#2172,.F.) ;
#46368 = ADVANCED_FACE('',(#11150),#1881,.T.) ;
#46369 = ADVANCED_FACE('',(#11151),#2173,.F.) ;
#46370 = ADVANCED_FACE('',(#11152),#1882,.T.) ;
#46371 = ADVANCED_FACE('',(#11153),#1883,.F.) ;
#46372 = ADVANCED_FACE('',(#11154),#2174,.F.) ;
#46373 = ADVANCED_FACE('',(#11155),#1884,.T.) ;
#46374 = ADVANCED_FACE('',(#11156),#9584,.F.) ;
#46375 = ADVANCED_FACE('',(#11157),#1885,.T.) ;
#46376 = ADVANCED_FACE('',(#11158),#1886,.F.) ;
#46377 = ADVANCED_FACE('',(#11159),#9585,.T.) ;
#46378 = ADVANCED_FACE('',(#11160),#1887,.T.) ;
#46379 = ADVANCED_FACE('',(#11161),#9586,.F.) ;
#46380 = ADVANCED_FACE('',(#11162),#1888,.F.) ;
#46381 = ADVANCED_FACE('',(#11163),#9587,.T.) ;
#46382 = ADVANCED_FACE('',(#11164),#1889,.T.) ;
#46383 = ADVANCED_FACE('',(#11165),#2266,.T.) ;
#46384 = ADVANCED_FACE('',(#11166),#2267,.F.) ;
#46385 = ADVANCED_FACE('',(#11167),#1890,.T.) ;
#46386 = ADVANCED_FACE('',(#11168),#2268,.T.) ;
#46387 = ADVANCED_FACE('',(#11169),#1891,.F.) ;
#46388 = ADVANCED_FACE('',(#11170),#1892,.F.) ;
#46389 = ADVANCED_FACE('',(#11171),#1893,.T.) ;
#46390 = ADVANCED_FACE('',(#11172),#1894,.T.) ;
#46391 = ADVANCED_FACE('',(#11173),#1895,.T.) ;
#46392 = ADVANCED_FACE('',(#11174),#2269,.T.) ;
#46393 = ADVANCED_FACE('',(#11175),#2175,.T.) ;
#46394 = ADVANCED_FACE('',(#11176),#1896,.F.) ;
#46395 = ADVANCED_FACE('',(#11177),#1897,.F.) ;
#46396 = ADVANCED_FACE('',(#11178),#1898,.F.) ;
#46397 = ADVANCED_FACE('',(#11179),#1899,.F.) ;
#46398 = ADVANCED_FACE('',(#11180),#1900,.F.) ;
#46399 = ADVANCED_FACE('',(#11181),#1901,.F.) ;
#46400 = ADVANCED_FACE('',(#11182),#9588,.T.) ;
#46401 = ADVANCED_FACE('',(#11183),#1902,.F.) ;
#46402 = ADVANCED_FACE('',(#11184),#1903,.F.) ;
#46403 = ADVANCED_FACE('',(#11185),#1904,.F.) ;
#46404 = ADVANCED_FACE('',(#11186),#1905,.F.) ;
#46405 = ADVANCED_FACE('',(#11187),#9589,.T.) ;
#46406 = ADVANCED_FACE('',(#11188),#2270,.T.) ;
#46407 = ADVANCED_FACE('',(#11189),#1906,.F.) ;
#46408 = ADVANCED_FACE('',(#11190),#1907,.T.) ;
#46409 = ADVANCED_FACE('',(#11191),#1908,.T.) ;
#46410 = ADVANCED_FACE('',(#11192),#2271,.T.) ;
#46411 = ADVANCED_FACE('',(#11193),#1909,.T.) ;
#46412 = ADVANCED_FACE('',(#11194),#1910,.T.) ;
#46413 = ADVANCED_FACE('',(#11195),#1911,.T.) ;
#46414 = ADVANCED_FACE('',(#11196),#2272,.T.) ;
#46415 = ADVANCED_FACE('',(#11197),#1912,.T.) ;
#46416 = ADVANCED_FACE('',(#11198),#1913,.T.) ;
#46417 = ADVANCED_FACE('',(#11199),#1914,.F.) ;
#46418 = ADVANCED_FACE('',(#11200),#1915,.T.) ;
#46419 = ADVANCED_FACE('',(#11201),#2273,.T.) ;
#46420 = ADVANCED_FACE('',(#11202),#1916,.T.) ;
#46421 = ADVANCED_FACE('',(#11203),#2274,.T.) ;
#46422 = ADVANCED_FACE('',(#11204,#677,#678),#2275,.F.) ;
#46423 = ADVANCED_FACE('',(#11205),#2276,.T.) ;
#46424 = ADVANCED_FACE('',(#11206),#9590,.T.) ;
#46425 = ADVANCED_FACE('',(#11207),#9591,.T.) ;
#46426 = ADVANCED_FACE('',(#11208),#1917,.T.) ;
#46427 = ADVANCED_FACE('',(#11209),#1918,.T.) ;
#46428 = ADVANCED_FACE('',(#11210),#1919,.T.) ;
#46429 = ADVANCED_FACE('',(#11211),#9592,.F.) ;
#46430 = ADVANCED_FACE('',(#11212),#9593,.F.) ;
#46431 = ADVANCED_FACE('',(#11213),#9594,.F.) ;
#46432 = ADVANCED_FACE('',(#11214),#1920,.T.) ;
#46433 = ADVANCED_FACE('',(#11215),#1921,.T.) ;
#46434 = ADVANCED_FACE('',(#11216),#2277,.F.) ;
#46435 = ADVANCED_FACE('',(#11217),#2278,.F.) ;
#46436 = ADVANCED_FACE('',(#11218),#2279,.F.) ;
#46437 = ADVANCED_FACE('',(#11219),#1922,.F.) ;
#46438 = ADVANCED_FACE('',(#11220,#679),#2280,.T.) ;
#46439 = ADVANCED_FACE('',(#11221),#9595,.F.) ;
#46440 = ADVANCED_FACE('',(#11222),#9596,.F.) ;
#46441 = ADVANCED_FACE('',(#11223),#9597,.F.) ;
#46442 = ADVANCED_FACE('',(#11224),#1923,.T.) ;
#46443 = ADVANCED_FACE('',(#11225),#1924,.T.) ;
#46444 = ADVANCED_FACE('',(#11226),#1925,.T.) ;
#46445 = ADVANCED_FACE('',(#11227),#1926,.T.) ;
#46446 = ADVANCED_FACE('',(#11228),#9598,.F.) ;
#46447 = ADVANCED_FACE('',(#11229),#1927,.T.) ;
#46448 = ADVANCED_FACE('',(#11230),#9599,.F.) ;
#46449 = ADVANCED_FACE('',(#11231),#9600,.F.) ;
#46450 = ADVANCED_FACE('',(#11232),#9601,.F.) ;
#46451 = ADVANCED_FACE('',(#11233),#9602,.F.) ;
#46452 = ADVANCED_FACE('',(#11234),#1928,.T.) ;
#46453 = ADVANCED_FACE('',(#11235),#1929,.T.) ;
#46454 = ADVANCED_FACE('',(#11236),#1930,.T.) ;
#46455 = ADVANCED_FACE('',(#11237),#1931,.T.) ;
#46456 = ADVANCED_FACE('',(#11238),#1932,.T.) ;
#46457 = ADVANCED_FACE('',(#11239),#1933,.T.) ;
#46458 = ADVANCED_FACE('',(#11240),#1934,.F.) ;
#46459 = ADVANCED_FACE('',(#11241),#1935,.F.) ;
#46460 = ADVANCED_FACE('',(#11242),#2281,.F.) ;
#46461 = ADVANCED_FACE('',(#11243),#2282,.F.) ;
#46462 = ADVANCED_FACE('',(#11244),#2283,.F.) ;
#46463 = ADVANCED_FACE('',(#11245),#1936,.F.) ;
#46464 = ADVANCED_FACE('',(#11246),#1937,.F.) ;
#46465 = ADVANCED_FACE('',(#11247),#1938,.F.) ;
#46466 = ADVANCED_FACE('',(#11248),#1939,.F.) ;
#46467 = ADVANCED_FACE('',(#11249),#2284,.F.) ;
#46468 = ADVANCED_FACE('',(#11250),#1940,.F.) ;
#46469 = ADVANCED_FACE('',(#11251),#9603,.T.) ;
#46470 = ADVANCED_FACE('',(#11252),#9604,.T.) ;
#46471 = ADVANCED_FACE('',(#11253),#1941,.F.) ;
#46472 = ADVANCED_FACE('',(#11254),#9605,.T.) ;
#46473 = ADVANCED_FACE('',(#11255),#1942,.F.) ;
#46474 = ADVANCED_FACE('',(#11256),#1943,.F.) ;
#46475 = ADVANCED_FACE('',(#11257),#1944,.F.) ;
#46476 = ADVANCED_FACE('',(#11258),#2285,.T.) ;
#46477 = ADVANCED_FACE('',(#11259),#9606,.F.) ;
#46478 = ADVANCED_FACE('',(#11260),#9607,.F.) ;
#46479 = ADVANCED_FACE('',(#11261),#9608,.F.) ;
#46480 = ADVANCED_FACE('',(#11262),#2286,.F.) ;
#46481 = ADVANCED_FACE('',(#11263),#2287,.F.) ;
#46482 = ADVANCED_FACE('',(#11264),#2288,.F.) ;
#46483 = ADVANCED_FACE('',(#11265),#9609,.F.) ;
#46484 = ADVANCED_FACE('',(#11266),#9610,.F.) ;
#46485 = ADVANCED_FACE('',(#11267),#9611,.F.) ;
#46486 = ADVANCED_FACE('',(#11268),#9612,.F.) ;
#46487 = ADVANCED_FACE('',(#11269),#2289,.F.) ;
#46488 = ADVANCED_FACE('',(#11270),#2290,.F.) ;
#46489 = ADVANCED_FACE('',(#11271),#2291,.F.) ;
#46490 = ADVANCED_FACE('',(#11272),#9613,.F.) ;
#46491 = ADVANCED_FACE('',(#11273),#9614,.F.) ;
#46492 = ADVANCED_FACE('',(#11274),#9615,.F.) ;
#46493 = ADVANCED_FACE('',(#11275),#2292,.F.) ;
#46494 = ADVANCED_FACE('',(#11276),#2293,.F.) ;
#46495 = ADVANCED_FACE('',(#11277),#2294,.F.) ;
#46496 = ADVANCED_FACE('',(#11278),#9616,.T.) ;
#46497 = ADVANCED_FACE('',(#11279),#1945,.F.) ;
#46498 = ADVANCED_FACE('',(#11280),#1946,.F.) ;
#46499 = ADVANCED_FACE('',(#11281),#9617,.T.) ;
#46500 = ADVANCED_FACE('',(#11282),#1947,.F.) ;
#46501 = ADVANCED_FACE('',(#11283),#1948,.F.) ;
#46502 = ADVANCED_FACE('',(#11284),#1949,.F.) ;
#46503 = ADVANCED_FACE('',(#11285),#1950,.F.) ;
#46504 = ADVANCED_FACE('',(#11286),#1951,.F.) ;
#46505 = ADVANCED_FACE('',(#11287),#9618,.T.) ;
#46506 = ADVANCED_FACE('',(#11288),#9619,.T.) ;
#46507 = ADVANCED_FACE('',(#11289),#9620,.T.) ;
#46508 = ADVANCED_FACE('',(#11290),#9621,.T.) ;
#46509 = ADVANCED_FACE('',(#11291),#1952,.F.) ;
#46510 = ADVANCED_FACE('',(#11292),#9622,.T.) ;
#46511 = ADVANCED_FACE('',(#11293),#1953,.F.) ;
#46512 = ADVANCED_FACE('',(#11294),#1954,.F.) ;
#46513 = ADVANCED_FACE('',(#11295),#1955,.F.) ;
#46514 = ADVANCED_FACE('',(#11296),#9623,.T.) ;
#46515 = ADVANCED_FACE('',(#11297),#1956,.F.) ;
#46516 = ADVANCED_FACE('',(#11298),#1957,.F.) ;
#46517 = ADVANCED_FACE('',(#11299),#1958,.F.) ;
#46518 = ADVANCED_FACE('',(#11300),#1959,.F.) ;
#46519 = ADVANCED_FACE('',(#11301),#2295,.F.) ;
#46520 = ADVANCED_FACE('',(#11302),#2296,.F.) ;
#46521 = ADVANCED_FACE('',(#11303),#2297,.F.) ;
#46522 = ADVANCED_FACE('',(#11304),#2298,.F.) ;
#46523 = ADVANCED_FACE('',(#11305,#680,#681,#682,#683,#684,#685,#686,#687,
#688,#689,#690,#691,#692,#693,#694,#695,#696,#697),#2299,.T.) ;
#46524 = ADVANCED_FACE('',(#11306),#9624,.T.) ;
#46525 = ADVANCED_FACE('',(#11307),#9625,.T.) ;
#46526 = ADVANCED_FACE('',(#11308),#9626,.T.) ;
#46527 = ADVANCED_FACE('',(#11309),#2300,.F.) ;
#46528 = ADVANCED_FACE('',(#11310),#9627,.T.) ;
#46529 = ADVANCED_FACE('',(#11311),#9628,.T.) ;
#46530 = ADVANCED_FACE('',(#11312),#9629,.T.) ;
#46531 = ADVANCED_FACE('',(#11313),#9630,.T.) ;
#46532 = ADVANCED_FACE('',(#11314),#2301,.F.) ;
#46533 = ADVANCED_FACE('',(#11315),#9631,.T.) ;
#46534 = ADVANCED_FACE('',(#11316),#9632,.T.) ;
#46535 = ADVANCED_FACE('',(#11317),#9633,.T.) ;
#46536 = ADVANCED_FACE('',(#11318),#2302,.F.) ;
#46537 = ADVANCED_FACE('',(#11319),#2303,.F.) ;
#46538 = ADVANCED_FACE('',(#11320),#1960,.F.) ;
#46539 = ADVANCED_FACE('',(#11321),#1961,.F.) ;
#46540 = ADVANCED_FACE('',(#11322),#1962,.F.) ;
#46541 = ADVANCED_FACE('',(#11323),#1963,.F.) ;
#46542 = ADVANCED_FACE('',(#11324),#1964,.F.) ;
#46543 = ADVANCED_FACE('',(#11325),#45494,.T.) ;
#46544 = ADVANCED_FACE('',(#11326,#698),#2304,.F.) ;
#46545 = ADVANCED_FACE('',(#11327),#9634,.F.) ;
#46546 = ADVANCED_FACE('',(#11328),#45495,.T.) ;
#46547 = ADVANCED_FACE('',(#11329),#9635,.T.) ;
#46548 = ADVANCED_FACE('',(#11330),#45496,.F.) ;
#46549 = ADVANCED_FACE('',(#11331,#699,#700,#701,#702,#703,#704,#705,#706,
#707,#708,#709,#710,#711,#712),#2305,.F.) ;
#46550 = ADVANCED_FACE('',(#11332),#45497,.T.) ;
#46551 = ADVANCED_FACE('',(#11333),#9636,.T.) ;
#46552 = ADVANCED_FACE('',(#11334),#45498,.T.) ;
#46553 = ADVANCED_FACE('',(#11335),#9637,.T.) ;
#46554 = ADVANCED_FACE('',(#11336),#45499,.T.) ;
#46555 = ADVANCED_FACE('',(#11337),#9638,.T.) ;
#46556 = ADVANCED_FACE('',(#11338),#45500,.T.) ;
#46557 = ADVANCED_FACE('',(#11339),#9639,.T.) ;
#46558 = ADVANCED_FACE('',(#11340),#45501,.T.) ;
#46559 = ADVANCED_FACE('',(#11341),#9640,.T.) ;
#46560 = ADVANCED_FACE('',(#11342),#45502,.T.) ;
#46561 = ADVANCED_FACE('',(#11343),#9641,.T.) ;
#46562 = ADVANCED_FACE('',(#11344),#45503,.T.) ;
#46563 = ADVANCED_FACE('',(#11345),#2306,.T.) ;
#46564 = ADVANCED_FACE('',(#11346),#9642,.T.) ;
#46565 = ADVANCED_FACE('',(#11347),#2307,.F.) ;
#46566 = ADVANCED_FACE('',(#11348),#9643,.T.) ;
#46567 = ADVANCED_FACE('',(#11349),#2308,.F.) ;
#46568 = ADVANCED_FACE('',(#11350),#9644,.F.) ;
#46569 = ADVANCED_FACE('',(#11351),#2309,.F.) ;
#46570 = ADVANCED_FACE('',(#11352),#9645,.T.) ;
#46571 = ADVANCED_FACE('',(#11353),#2310,.F.) ;
#46572 = ADVANCED_FACE('',(#11354),#9646,.T.) ;
#46573 = ADVANCED_FACE('',(#11355),#2311,.T.) ;
#46574 = ADVANCED_FACE('',(#11356),#45504,.F.) ;
#46575 = ADVANCED_FACE('',(#11357),#9647,.T.) ;
#46576 = ADVANCED_FACE('',(#11358),#1965,.T.) ;
#46577 = ADVANCED_FACE('',(#11359),#45505,.T.) ;
#46578 = ADVANCED_FACE('',(#11360,#713),#2312,.F.) ;
#46579 = ADVANCED_FACE('',(#11361),#45506,.T.) ;
#46580 = ADVANCED_FACE('',(#11362),#9648,.F.) ;
#46581 = ADVANCED_FACE('',(#11363),#45507,.T.) ;
#46582 = ADVANCED_FACE('',(#11364),#9649,.F.) ;
#46583 = ADVANCED_FACE('',(#11365,#714),#2313,.T.) ;
#46584 = ADVANCED_FACE('',(#11366),#45508,.T.) ;
#46585 = ADVANCED_FACE('',(#11367,#715),#2314,.F.) ;
#46586 = ADVANCED_FACE('',(#11368),#45509,.T.) ;
#46587 = ADVANCED_FACE('',(#11369),#9650,.F.) ;
#46588 = ADVANCED_FACE('',(#11370,#716),#2315,.T.) ;
#46589 = ADVANCED_FACE('',(#11371),#45510,.T.) ;
#46590 = ADVANCED_FACE('',(#11372,#717),#2316,.F.) ;
#46591 = ADVANCED_FACE('',(#11373),#45511,.T.) ;
#46592 = ADVANCED_FACE('',(#11374),#9651,.T.) ;
#46593 = ADVANCED_FACE('',(#11375),#45512,.T.) ;
#46594 = ADVANCED_FACE('',(#11376),#9652,.T.) ;
#46595 = ADVANCED_FACE('',(#11377),#45513,.T.) ;
#46596 = ADVANCED_FACE('',(#11378),#2317,.T.) ;
#46597 = ADVANCED_FACE('',(#11379),#9653,.T.) ;
#46598 = ADVANCED_FACE('',(#11380),#2318,.F.) ;
#46599 = ADVANCED_FACE('',(#11381),#9654,.T.) ;
#46600 = ADVANCED_FACE('',(#11382),#9655,.F.) ;
#46601 = ADVANCED_FACE('',(#11383),#1966,.T.) ;
#46602 = ADVANCED_FACE('',(#11384),#1967,.T.) ;
#46603 = ADVANCED_FACE('',(#11385),#9656,.F.) ;
#46604 = ADVANCED_FACE('',(#11386),#1968,.T.) ;
#46605 = ADVANCED_FACE('',(#11387),#9657,.F.) ;
#46606 = ADVANCED_FACE('',(#11388),#9658,.T.) ;
#46607 = ADVANCED_FACE('',(#11389),#45514,.T.) ;
#46608 = ADVANCED_FACE('',(#11390),#9659,.T.) ;
#46609 = ADVANCED_FACE('',(#11391),#45515,.T.) ;
#46610 = ADVANCED_FACE('',(#11392),#9660,.T.) ;
#46611 = ADVANCED_FACE('',(#11393),#9661,.F.) ;
#46612 = ADVANCED_FACE('',(#11394),#9662,.T.) ;
#46613 = ADVANCED_FACE('',(#11395),#2176,.T.) ;
#46614 = ADVANCED_FACE('',(#11396),#9663,.T.) ;
#46615 = ADVANCED_FACE('',(#11397),#45516,.T.) ;
#46616 = ADVANCED_FACE('',(#11398),#2177,.T.) ;
#46617 = ADVANCED_FACE('',(#11399),#9664,.T.) ;
#46618 = ADVANCED_FACE('',(#11400),#45517,.T.) ;
#46619 = ADVANCED_FACE('',(#11401),#45518,.T.) ;
#46620 = ADVANCED_FACE('',(#11402),#9665,.T.) ;
#46621 = ADVANCED_FACE('',(#11403),#9666,.T.) ;
#46622 = ADVANCED_FACE('',(#11404),#45519,.F.) ;
#46623 = ADVANCED_FACE('',(#11405),#9667,.F.) ;
#46624 = ADVANCED_FACE('',(#11406),#9668,.F.) ;
#46625 = ADVANCED_FACE('',(#11407),#45520,.F.) ;
#46626 = ADVANCED_FACE('',(#11408),#9669,.T.) ;
#46627 = ADVANCED_FACE('',(#11409),#2178,.T.) ;
#46628 = ADVANCED_FACE('',(#11410),#9670,.T.) ;
#46629 = ADVANCED_FACE('',(#11411),#2319,.F.) ;
#46630 = ADVANCED_FACE('',(#11412),#9671,.T.) ;
#46631 = ADVANCED_FACE('',(#11413),#9672,.T.) ;
#46632 = ADVANCED_FACE('',(#11414),#2320,.F.) ;
#46633 = ADVANCED_FACE('',(#11415),#45521,.F.) ;
#46634 = ADVANCED_FACE('',(#11416),#9673,.F.) ;
#46635 = ADVANCED_FACE('',(#11417),#1969,.T.) ;
#46636 = ADVANCED_FACE('',(#11418),#9674,.T.) ;
#46637 = ADVANCED_FACE('',(#11419),#2321,.F.) ;
#46638 = ADVANCED_FACE('',(#11420),#1970,.T.) ;
#46639 = ADVANCED_FACE('',(#11421),#9675,.F.) ;
#46640 = ADVANCED_FACE('',(#11422),#45522,.F.) ;
#46641 = ADVANCED_FACE('',(#11423),#2322,.F.) ;
#46642 = ADVANCED_FACE('',(#11424),#9676,.T.) ;
#46643 = ADVANCED_FACE('',(#11425),#9677,.T.) ;
#46644 = ADVANCED_FACE('',(#11426),#45523,.T.) ;
#46645 = ADVANCED_FACE('',(#11427),#9678,.T.) ;
#46646 = ADVANCED_FACE('',(#11428),#45524,.T.) ;
#46647 = ADVANCED_FACE('',(#11429),#9679,.T.) ;
#46648 = ADVANCED_FACE('',(#11430),#45525,.T.) ;
#46649 = ADVANCED_FACE('',(#11431),#9680,.T.) ;
#46650 = ADVANCED_FACE('',(#11432),#2323,.F.) ;
#46651 = ADVANCED_FACE('',(#11433),#9681,.F.) ;
#46652 = ADVANCED_FACE('',(#11434),#2324,.F.) ;
#46653 = ADVANCED_FACE('',(#11435),#9682,.F.) ;
#46654 = ADVANCED_FACE('',(#11436),#2325,.T.) ;
#46655 = ADVANCED_FACE('',(#11437),#9683,.F.) ;
#46656 = ADVANCED_FACE('',(#11438),#2326,.F.) ;
#46657 = ADVANCED_FACE('',(#11439),#9684,.F.) ;
#46658 = ADVANCED_FACE('',(#11440),#2327,.T.) ;
#46659 = ADVANCED_FACE('',(#11441),#9685,.F.) ;
#46660 = ADVANCED_FACE('',(#11442),#2328,.F.) ;
#46661 = ADVANCED_FACE('',(#11443),#9686,.T.) ;
#46662 = ADVANCED_FACE('',(#11444),#45526,.T.) ;
#46663 = ADVANCED_FACE('',(#11445),#9687,.T.) ;
#46664 = ADVANCED_FACE('',(#11446),#45527,.T.) ;
#46665 = ADVANCED_FACE('',(#11447),#9688,.T.) ;
#46666 = ADVANCED_FACE('',(#11448),#45528,.T.) ;
#46667 = ADVANCED_FACE('',(#11449),#9689,.T.) ;
#46668 = ADVANCED_FACE('',(#11450),#45529,.T.) ;
#46669 = ADVANCED_FACE('',(#11451),#9690,.T.) ;
#46670 = ADVANCED_FACE('',(#11452),#9691,.T.) ;
#46671 = ADVANCED_FACE('',(#11453),#45530,.T.) ;
#46672 = ADVANCED_FACE('',(#11454),#9692,.T.) ;
#46673 = ADVANCED_FACE('',(#11455),#45531,.T.) ;
#46674 = ADVANCED_FACE('',(#11456),#9693,.T.) ;
#46675 = ADVANCED_FACE('',(#11457),#2179,.T.) ;
#46676 = ADVANCED_FACE('',(#11458),#2180,.T.) ;
#46677 = ADVANCED_FACE('',(#11459),#9694,.F.) ;
#46678 = ADVANCED_FACE('',(#11460),#2329,.F.) ;
#46679 = ADVANCED_FACE('',(#11461),#9695,.F.) ;
#46680 = ADVANCED_FACE('',(#11462),#2330,.F.) ;
#46681 = ADVANCED_FACE('',(#11463),#9696,.F.) ;
#46682 = ADVANCED_FACE('',(#11464),#2331,.F.) ;
#46683 = ADVANCED_FACE('',(#11465),#9697,.T.) ;
#46684 = ADVANCED_FACE('',(#11466),#2332,.F.) ;
#46685 = ADVANCED_FACE('',(#11467),#45532,.T.) ;
#46686 = ADVANCED_FACE('',(#11468),#45533,.T.) ;
#46687 = ADVANCED_FACE('',(#11469),#9698,.T.) ;
#46688 = ADVANCED_FACE('',(#11470),#45534,.T.) ;
#46689 = ADVANCED_FACE('',(#11471),#9699,.T.) ;
#46690 = ADVANCED_FACE('',(#11472),#45535,.T.) ;
#46691 = ADVANCED_FACE('',(#11473),#9700,.T.) ;
#46692 = ADVANCED_FACE('',(#11474),#45536,.T.) ;
#46693 = ADVANCED_FACE('',(#11475),#9701,.T.) ;
#46694 = ADVANCED_FACE('',(#11476),#45537,.T.) ;
#46695 = ADVANCED_FACE('',(#11477),#9702,.T.) ;
#46696 = ADVANCED_FACE('',(#11478),#9703,.T.) ;
#46697 = ADVANCED_FACE('',(#11479),#9704,.F.) ;
#46698 = ADVANCED_FACE('',(#11480),#1971,.T.) ;
#46699 = ADVANCED_FACE('',(#11481),#9705,.F.) ;
#46700 = ADVANCED_FACE('',(#11482),#1972,.T.) ;
#46701 = ADVANCED_FACE('',(#11483),#9706,.T.) ;
#46702 = ADVANCED_FACE('',(#11484),#2333,.F.) ;
#46703 = ADVANCED_FACE('',(#11485),#45538,.T.) ;
#46704 = ADVANCED_FACE('',(#11486),#9707,.T.) ;
#46705 = ADVANCED_FACE('',(#11487),#9708,.T.) ;
#46706 = ADVANCED_FACE('',(#11488),#45539,.T.) ;
#46707 = ADVANCED_FACE('',(#11489),#9709,.T.) ;
#46708 = ADVANCED_FACE('',(#11490),#45540,.T.) ;
#46709 = ADVANCED_FACE('',(#11491),#9710,.T.) ;
#46710 = ADVANCED_FACE('',(#11492),#2181,.T.) ;
#46711 = ADVANCED_FACE('',(#11493),#9711,.T.) ;
#46712 = ADVANCED_FACE('',(#11494),#45541,.T.) ;
#46713 = ADVANCED_FACE('',(#11495),#2182,.T.) ;
#46714 = ADVANCED_FACE('',(#11496),#2334,.F.) ;
#46715 = ADVANCED_FACE('',(#11497),#9712,.T.) ;
#46716 = ADVANCED_FACE('',(#11498),#2335,.F.) ;
#46717 = ADVANCED_FACE('',(#11499),#9713,.F.) ;
#46718 = ADVANCED_FACE('',(#11500),#2336,.F.) ;
#46719 = ADVANCED_FACE('',(#11501),#9714,.F.) ;
#46720 = ADVANCED_FACE('',(#11502),#2337,.F.) ;
#46721 = ADVANCED_FACE('',(#11503),#9715,.T.) ;
#46722 = ADVANCED_FACE('',(#11504),#2338,.F.) ;
#46723 = ADVANCED_FACE('',(#11505),#45542,.T.) ;
#46724 = ADVANCED_FACE('',(#11506),#9716,.T.) ;
#46725 = ADVANCED_FACE('',(#11507),#9717,.T.) ;
#46726 = ADVANCED_FACE('',(#11508),#45543,.T.) ;
#46727 = ADVANCED_FACE('',(#11509),#9718,.T.) ;
#46728 = ADVANCED_FACE('',(#11510),#45544,.T.) ;
#46729 = ADVANCED_FACE('',(#11511),#9719,.T.) ;
#46730 = ADVANCED_FACE('',(#11512),#2183,.T.) ;
#46731 = ADVANCED_FACE('',(#11513),#9720,.T.) ;
#46732 = ADVANCED_FACE('',(#11514),#45545,.T.) ;
#46733 = ADVANCED_FACE('',(#11515),#2184,.T.) ;
#46734 = ADVANCED_FACE('',(#11516),#2339,.F.) ;
#46735 = ADVANCED_FACE('',(#11517),#9721,.T.) ;
#46736 = ADVANCED_FACE('',(#11518),#2340,.F.) ;
#46737 = ADVANCED_FACE('',(#11519),#9722,.F.) ;
#46738 = ADVANCED_FACE('',(#11520),#2341,.F.) ;
#46739 = ADVANCED_FACE('',(#11521),#9723,.F.) ;
#46740 = ADVANCED_FACE('',(#11522),#2342,.F.) ;
#46741 = ADVANCED_FACE('',(#11523),#9724,.T.) ;
#46742 = ADVANCED_FACE('',(#11524),#2343,.F.) ;
#46743 = ADVANCED_FACE('',(#11525),#9725,.T.) ;
#46744 = ADVANCED_FACE('',(#11526),#9726,.T.) ;
#46745 = ADVANCED_FACE('',(#11527),#45546,.T.) ;
#46746 = ADVANCED_FACE('',(#11528),#2185,.T.) ;
#46747 = ADVANCED_FACE('',(#11529),#2344,.F.) ;
#46748 = ADVANCED_FACE('',(#11530),#9727,.T.) ;
#46749 = ADVANCED_FACE('',(#11531),#45547,.T.) ;
#46750 = ADVANCED_FACE('',(#11532),#2345,.F.) ;
#46751 = ADVANCED_FACE('',(#11533),#9728,.T.) ;
#46752 = ADVANCED_FACE('',(#11534),#45548,.T.) ;
#46753 = ADVANCED_FACE('',(#11535),#9729,.T.) ;
#46754 = ADVANCED_FACE('',(#11536),#45549,.T.) ;
#46755 = ADVANCED_FACE('',(#11537),#9730,.T.) ;
#46756 = ADVANCED_FACE('',(#11538),#45550,.T.) ;
#46757 = ADVANCED_FACE('',(#11539),#9731,.T.) ;
#46758 = ADVANCED_FACE('',(#11540),#45551,.T.) ;
#46759 = ADVANCED_FACE('',(#11541),#9732,.T.) ;
#46760 = ADVANCED_FACE('',(#11542),#2346,.F.) ;
#46761 = ADVANCED_FACE('',(#11543),#9733,.F.) ;
#46762 = ADVANCED_FACE('',(#11544),#2347,.T.) ;
#46763 = ADVANCED_FACE('',(#11545),#9734,.F.) ;
#46764 = ADVANCED_FACE('',(#11546),#2348,.F.) ;
#46765 = ADVANCED_FACE('',(#11547),#9735,.F.) ;
#46766 = ADVANCED_FACE('',(#11548),#2349,.T.) ;
#46767 = ADVANCED_FACE('',(#11549),#9736,.F.) ;
#46768 = ADVANCED_FACE('',(#11550),#2350,.F.) ;
#46769 = ADVANCED_FACE('',(#11551),#9737,.F.) ;
#46770 = ADVANCED_FACE('',(#11552),#45552,.T.) ;
#46771 = ADVANCED_FACE('',(#11553),#2351,.F.) ;
#46772 = ADVANCED_FACE('',(#11554),#45553,.T.) ;
#46773 = ADVANCED_FACE('',(#11555),#9738,.F.) ;
#46774 = ADVANCED_FACE('',(#11556),#45554,.T.) ;
#46775 = ADVANCED_FACE('',(#11557),#45555,.T.) ;
#46776 = ADVANCED_FACE('',(#11558),#9739,.T.) ;
#46777 = ADVANCED_FACE('',(#11559),#9740,.F.) ;
#46778 = ADVANCED_FACE('',(#11560),#9741,.T.) ;
#46779 = ADVANCED_FACE('',(#11561),#45556,.T.) ;
#46780 = ADVANCED_FACE('',(#11562),#9742,.T.) ;
#46781 = ADVANCED_FACE('',(#11563),#9743,.T.) ;
#46782 = ADVANCED_FACE('',(#11564),#9744,.F.) ;
#46783 = ADVANCED_FACE('',(#11565),#9745,.T.) ;
#46784 = ADVANCED_FACE('',(#11566),#2352,.F.) ;
#46785 = ADVANCED_FACE('',(#11567),#9746,.T.) ;
#46786 = ADVANCED_FACE('',(#11568),#45557,.T.) ;
#46787 = ADVANCED_FACE('',(#11569),#45558,.T.) ;
#46788 = ADVANCED_FACE('',(#11570),#2353,.F.) ;
#46789 = ADVANCED_FACE('',(#11571),#45559,.T.) ;
#46790 = ADVANCED_FACE('',(#11572),#45560,.T.) ;
#46791 = ADVANCED_FACE('',(#11573),#9747,.T.) ;
#46792 = ADVANCED_FACE('',(#11574),#2186,.T.) ;
#46793 = ADVANCED_FACE('',(#11575),#2187,.T.) ;
#46794 = ADVANCED_FACE('',(#11576),#9748,.T.) ;
#46795 = ADVANCED_FACE('',(#11577),#45561,.T.) ;
#46796 = ADVANCED_FACE('',(#11578),#45562,.T.) ;
#46797 = ADVANCED_FACE('',(#11579),#9749,.T.) ;
#46798 = ADVANCED_FACE('',(#11580),#9750,.F.) ;
#46799 = ADVANCED_FACE('',(#11581),#45563,.T.) ;
#46800 = ADVANCED_FACE('',(#11582),#45564,.T.) ;
#46801 = ADVANCED_FACE('',(#11583),#9751,.T.) ;
#46802 = ADVANCED_FACE('',(#11584),#9752,.F.) ;
#46803 = ADVANCED_FACE('',(#11585),#9753,.T.) ;
#46804 = ADVANCED_FACE('',(#11586),#9754,.F.) ;
#46805 = ADVANCED_FACE('',(#11587),#9755,.T.) ;
#46806 = ADVANCED_FACE('',(#11588),#9756,.F.) ;
#46807 = ADVANCED_FACE('',(#11589),#9757,.T.) ;
#46808 = ADVANCED_FACE('',(#11590),#9758,.T.) ;
#46809 = ADVANCED_FACE('',(#11591),#9759,.T.) ;
#46810 = ADVANCED_FACE('',(#11592),#2354,.F.) ;
#46811 = ADVANCED_FACE('',(#11593),#9760,.T.) ;
#46812 = ADVANCED_FACE('',(#11594),#45565,.T.) ;
#46813 = ADVANCED_FACE('',(#11595),#45566,.T.) ;
#46814 = ADVANCED_FACE('',(#11596),#2355,.F.) ;
#46815 = ADVANCED_FACE('',(#11597),#45567,.T.) ;
#46816 = ADVANCED_FACE('',(#11598),#2188,.T.) ;
#46817 = ADVANCED_FACE('',(#11599),#9761,.T.) ;
#46818 = ADVANCED_FACE('',(#11600),#45568,.T.) ;
#46819 = ADVANCED_FACE('',(#11601),#9762,.T.) ;
#46820 = ADVANCED_FACE('',(#11602),#45569,.T.) ;
#46821 = ADVANCED_FACE('',(#11603),#2189,.T.) ;
#46822 = ADVANCED_FACE('',(#11604),#9763,.T.) ;
#46823 = ADVANCED_FACE('',(#11605),#45570,.T.) ;
#46824 = ADVANCED_FACE('',(#11606),#45571,.T.) ;
#46825 = ADVANCED_FACE('',(#11607),#9764,.T.) ;
#46826 = ADVANCED_FACE('',(#11608),#9765,.F.) ;
#46827 = ADVANCED_FACE('',(#11609),#45572,.T.) ;
#46828 = ADVANCED_FACE('',(#11610),#9766,.T.) ;
#46829 = ADVANCED_FACE('',(#11611),#9767,.F.) ;
#46830 = ADVANCED_FACE('',(#11612),#9768,.T.) ;
#46831 = ADVANCED_FACE('',(#11613),#9769,.F.) ;
#46832 = ADVANCED_FACE('',(#11614),#9770,.T.) ;
#46833 = ADVANCED_FACE('',(#11615),#9771,.F.) ;
#46834 = ADVANCED_FACE('',(#11616),#9772,.T.) ;
#46835 = ADVANCED_FACE('',(#11617),#9773,.T.) ;
#46836 = ADVANCED_FACE('',(#11618),#2356,.F.) ;
#46837 = ADVANCED_FACE('',(#11619),#9774,.T.) ;
#46838 = ADVANCED_FACE('',(#11620),#45573,.T.) ;
#46839 = ADVANCED_FACE('',(#11621),#45574,.T.) ;
#46840 = ADVANCED_FACE('',(#11622),#9775,.T.) ;
#46841 = ADVANCED_FACE('',(#11623),#45575,.T.) ;
#46842 = ADVANCED_FACE('',(#11624),#9776,.T.) ;
#46843 = ADVANCED_FACE('',(#11625),#45576,.T.) ;
#46844 = ADVANCED_FACE('',(#11626),#9777,.T.) ;
#46845 = ADVANCED_FACE('',(#11627),#45577,.T.) ;
#46846 = ADVANCED_FACE('',(#11628),#9778,.T.) ;
#46847 = ADVANCED_FACE('',(#11629),#45578,.T.) ;
#46848 = ADVANCED_FACE('',(#11630),#45579,.T.) ;
#46849 = ADVANCED_FACE('',(#11631),#9779,.T.) ;
#46850 = ADVANCED_FACE('',(#11632),#45580,.T.) ;
#46851 = ADVANCED_FACE('',(#11633),#9780,.T.) ;
#46852 = ADVANCED_FACE('',(#11634),#45581,.T.) ;
#46853 = ADVANCED_FACE('',(#11635),#9781,.T.) ;
#46854 = ADVANCED_FACE('',(#11636),#45582,.T.) ;
#46855 = ADVANCED_FACE('',(#11637),#9782,.T.) ;
#46856 = ADVANCED_FACE('',(#11638),#45583,.T.) ;
#46857 = ADVANCED_FACE('',(#11639),#45584,.T.) ;
#46858 = ADVANCED_FACE('',(#11640),#9783,.T.) ;
#46859 = ADVANCED_FACE('',(#11641),#45585,.T.) ;
#46860 = ADVANCED_FACE('',(#11642),#45586,.T.) ;
#46861 = ADVANCED_FACE('',(#11643),#9784,.T.) ;
#46862 = ADVANCED_FACE('',(#11644),#45587,.T.) ;
#46863 = ADVANCED_FACE('',(#11645),#9785,.T.) ;
#46864 = ADVANCED_FACE('',(#11646),#45588,.T.) ;
#46865 = ADVANCED_FACE('',(#11647),#9786,.T.) ;
#46866 = ADVANCED_FACE('',(#11648),#45589,.T.) ;
#46867 = ADVANCED_FACE('',(#11649),#9787,.T.) ;
#46868 = ADVANCED_FACE('',(#11650),#45590,.T.) ;
#46869 = ADVANCED_FACE('',(#11651),#9788,.T.) ;
#46870 = ADVANCED_FACE('',(#11652),#45591,.T.) ;
#46871 = ADVANCED_FACE('',(#11653),#9789,.T.) ;
#46872 = ADVANCED_FACE('',(#11654),#45592,.T.) ;
#46873 = ADVANCED_FACE('',(#11655),#9790,.T.) ;
#46874 = ADVANCED_FACE('',(#11656),#45593,.T.) ;
#46875 = ADVANCED_FACE('',(#11657),#9791,.T.) ;
#46876 = ADVANCED_FACE('',(#11658),#45594,.F.) ;
#46877 = ADVANCED_FACE('',(#11659),#9792,.F.) ;
#46878 = ADVANCED_FACE('',(#11660),#9793,.T.) ;
#46879 = ADVANCED_FACE('',(#11661),#9794,.F.) ;
#46880 = ADVANCED_FACE('',(#11662),#45595,.F.) ;
#46881 = ADVANCED_FACE('',(#11663),#9795,.T.) ;
#46882 = ADVANCED_FACE('',(#11664),#2357,.T.) ;
#46883 = ADVANCED_FACE('',(#11665),#9796,.T.) ;
#46884 = ADVANCED_FACE('',(#11666),#2358,.T.) ;
#46885 = ADVANCED_FACE('',(#11667),#9797,.T.) ;
#46886 = ADVANCED_FACE('',(#11668),#9798,.F.) ;
#46887 = ADVANCED_FACE('',(#11669),#2359,.T.) ;
#46888 = ADVANCED_FACE('',(#11670),#9799,.F.) ;
#46889 = ADVANCED_FACE('',(#11671),#9800,.T.) ;
#46890 = ADVANCED_FACE('',(#11672),#2360,.T.) ;
#46891 = ADVANCED_FACE('',(#11673),#9801,.T.) ;
#46892 = ADVANCED_FACE('',(#11674),#2361,.T.) ;
#46893 = ADVANCED_FACE('',(#11675),#9802,.F.) ;
#46894 = ADVANCED_FACE('',(#11676),#2362,.T.) ;
#46895 = ADVANCED_FACE('',(#11677),#9803,.T.) ;
#46896 = ADVANCED_FACE('',(#11678),#2363,.T.) ;
#46897 = ADVANCED_FACE('',(#11679),#9804,.T.) ;
#46898 = ADVANCED_FACE('',(#11680),#2364,.T.) ;
#46899 = ADVANCED_FACE('',(#11681),#9805,.T.) ;
#46900 = ADVANCED_FACE('',(#11682),#2365,.T.) ;
#46901 = ADVANCED_FACE('',(#11683),#9806,.F.) ;
#46902 = ADVANCED_FACE('',(#11684),#2366,.T.) ;
#46903 = ADVANCED_FACE('',(#11685),#9807,.T.) ;
#46904 = ADVANCED_FACE('',(#11686),#2367,.F.) ;
#46905 = ADVANCED_FACE('',(#11687),#9808,.T.) ;
#46906 = ADVANCED_FACE('',(#11688),#9809,.T.) ;
#46907 = ADVANCED_FACE('',(#11689),#45596,.T.) ;
#46908 = ADVANCED_FACE('',(#11690),#9810,.T.) ;
#46909 = ADVANCED_FACE('',(#11691),#9811,.T.) ;
#46910 = ADVANCED_FACE('',(#11692),#2368,.T.) ;
#46911 = ADVANCED_FACE('',(#11693),#2369,.F.) ;
#46912 = ADVANCED_FACE('',(#11694),#9812,.T.) ;
#46913 = ADVANCED_FACE('',(#11695),#45597,.T.) ;
#46914 = ADVANCED_FACE('',(#11696),#9813,.T.) ;
#46915 = ADVANCED_FACE('',(#11697),#2370,.T.) ;
#46916 = ADVANCED_FACE('',(#11698),#45598,.T.) ;
#46917 = ADVANCED_FACE('',(#11699),#45599,.T.) ;
#46918 = ADVANCED_FACE('',(#11700),#9814,.T.) ;
#46919 = ADVANCED_FACE('',(#11701),#45600,.T.) ;
#46920 = ADVANCED_FACE('',(#11702),#9815,.T.) ;
#46921 = ADVANCED_FACE('',(#11703),#45601,.T.) ;
#46922 = ADVANCED_FACE('',(#11704),#9816,.T.) ;
#46923 = ADVANCED_FACE('',(#11705),#45602,.T.) ;
#46924 = ADVANCED_FACE('',(#11706),#9817,.T.) ;
#46925 = ADVANCED_FACE('',(#11707),#45603,.T.) ;
#46926 = ADVANCED_FACE('',(#11708),#9818,.T.) ;
#46927 = ADVANCED_FACE('',(#11709),#9819,.F.) ;
#46928 = ADVANCED_FACE('',(#11710),#9820,.T.) ;
#46929 = ADVANCED_FACE('',(#11711),#9821,.F.) ;
#46930 = ADVANCED_FACE('',(#11712),#9822,.F.) ;
#46931 = ADVANCED_FACE('',(#11713),#9823,.F.) ;
#46932 = ADVANCED_FACE('',(#11714),#9824,.F.) ;
#46933 = ADVANCED_FACE('',(#11715),#9825,.F.) ;
#46934 = ADVANCED_FACE('',(#11716),#9826,.T.) ;
#46935 = ADVANCED_FACE('',(#11717),#2371,.F.) ;
#46936 = ADVANCED_FACE('',(#11718),#2372,.F.) ;
#46937 = ADVANCED_FACE('',(#11719),#2190,.T.) ;
#46938 = ADVANCED_FACE('',(#11720),#45604,.T.) ;
#46939 = ADVANCED_FACE('',(#11721),#9827,.T.) ;
#46940 = ADVANCED_FACE('',(#11722),#9828,.F.) ;
#46941 = ADVANCED_FACE('',(#11723),#45605,.T.) ;
#46942 = ADVANCED_FACE('',(#11724),#45606,.T.) ;
#46943 = ADVANCED_FACE('',(#11725),#9829,.T.) ;
#46944 = ADVANCED_FACE('',(#11726),#45607,.T.) ;
#46945 = ADVANCED_FACE('',(#11727),#9830,.T.) ;
#46946 = ADVANCED_FACE('',(#11728),#45608,.T.) ;
#46947 = ADVANCED_FACE('',(#11729),#9831,.T.) ;
#46948 = ADVANCED_FACE('',(#11730),#2191,.T.) ;
#46949 = ADVANCED_FACE('',(#11731),#45609,.T.) ;
#46950 = ADVANCED_FACE('',(#11732),#9832,.T.) ;
#46951 = ADVANCED_FACE('',(#11733),#9833,.T.) ;
#46952 = ADVANCED_FACE('',(#11734),#9834,.T.) ;
#46953 = ADVANCED_FACE('',(#11735),#9835,.F.) ;
#46954 = ADVANCED_FACE('',(#11736),#9836,.F.) ;
#46955 = ADVANCED_FACE('',(#11737),#9837,.T.) ;
#46956 = ADVANCED_FACE('',(#11738),#9838,.T.) ;
#46957 = ADVANCED_FACE('',(#11739),#2373,.F.) ;
#46958 = ADVANCED_FACE('',(#11740),#2374,.F.) ;
#46959 = ADVANCED_FACE('',(#11741),#9839,.T.) ;
#46960 = ADVANCED_FACE('',(#11742),#45610,.T.) ;
#46961 = ADVANCED_FACE('',(#11743),#9840,.T.) ;
#46962 = ADVANCED_FACE('',(#11744),#2375,.T.) ;
#46963 = ADVANCED_FACE('',(#11745),#9841,.T.) ;
#46964 = ADVANCED_FACE('',(#11746),#45611,.T.) ;
#46965 = ADVANCED_FACE('',(#11747),#9842,.T.) ;
#46966 = ADVANCED_FACE('',(#11748),#9843,.T.) ;
#46967 = ADVANCED_FACE('',(#11749),#2376,.T.) ;
#46968 = ADVANCED_FACE('',(#11750),#45612,.T.) ;
#46969 = ADVANCED_FACE('',(#11751),#9844,.T.) ;
#46970 = ADVANCED_FACE('',(#11752),#45613,.T.) ;
#46971 = ADVANCED_FACE('',(#11753),#9845,.T.) ;
#46972 = ADVANCED_FACE('',(#11754),#45614,.T.) ;
#46973 = ADVANCED_FACE('',(#11755),#9846,.T.) ;
#46974 = ADVANCED_FACE('',(#11756),#45615,.T.) ;
#46975 = ADVANCED_FACE('',(#11757),#9847,.T.) ;
#46976 = ADVANCED_FACE('',(#11758),#9848,.T.) ;
#46977 = ADVANCED_FACE('',(#11759),#9849,.T.) ;
#46978 = ADVANCED_FACE('',(#11760),#45616,.T.) ;
#46979 = ADVANCED_FACE('',(#11761),#9850,.T.) ;
#46980 = ADVANCED_FACE('',(#11762),#9851,.T.) ;
#46981 = ADVANCED_FACE('',(#11763),#2377,.T.) ;
#46982 = ADVANCED_FACE('',(#11764),#2378,.F.) ;
#46983 = ADVANCED_FACE('',(#11765),#9852,.T.) ;
#46984 = ADVANCED_FACE('',(#11766),#45617,.T.) ;
#46985 = ADVANCED_FACE('',(#11767),#9853,.T.) ;
#46986 = ADVANCED_FACE('',(#11768),#2379,.T.) ;
#46987 = ADVANCED_FACE('',(#11769),#45618,.T.) ;
#46988 = ADVANCED_FACE('',(#11770),#45619,.T.) ;
#46989 = ADVANCED_FACE('',(#11771),#45620,.T.) ;
#46990 = ADVANCED_FACE('',(#11772),#45621,.T.) ;
#46991 = ADVANCED_FACE('',(#11773),#9854,.T.) ;
#46992 = ADVANCED_FACE('',(#11774),#9855,.T.) ;
#46993 = ADVANCED_FACE('',(#11775),#9856,.T.) ;
#46994 = ADVANCED_FACE('',(#11776),#9857,.F.) ;
#46995 = ADVANCED_FACE('',(#11777),#9858,.T.) ;
#46996 = ADVANCED_FACE('',(#11778),#9859,.F.) ;
#46997 = ADVANCED_FACE('',(#11779),#9860,.T.) ;
#46998 = ADVANCED_FACE('',(#11780),#9861,.F.) ;
#46999 = ADVANCED_FACE('',(#11781),#9862,.T.) ;
#47000 = ADVANCED_FACE('',(#11782),#9863,.F.) ;
#47001 = ADVANCED_FACE('',(#11783),#9864,.T.) ;
#47002 = ADVANCED_FACE('',(#11784),#2380,.T.) ;
#47003 = ADVANCED_FACE('',(#11785),#2381,.F.) ;
#47004 = ADVANCED_FACE('',(#11786),#2382,.T.) ;
#47005 = ADVANCED_FACE('',(#11787),#2383,.F.) ;
#47006 = ADVANCED_FACE('',(#11788),#2384,.F.) ;
#47007 = ADVANCED_FACE('',(#11789),#9865,.T.) ;
#47008 = ADVANCED_FACE('',(#11790),#2385,.F.) ;
#47009 = ADVANCED_FACE('',(#11791),#9866,.T.) ;
#47010 = ADVANCED_FACE('',(#11792),#2386,.F.) ;
#47011 = ADVANCED_FACE('',(#11793),#45622,.T.) ;
#47012 = ADVANCED_FACE('',(#11794),#45623,.T.) ;
#47013 = ADVANCED_FACE('',(#11795),#45624,.T.) ;
#47014 = ADVANCED_FACE('',(#11796),#45625,.T.) ;
#47015 = ADVANCED_FACE('',(#11797),#45626,.T.) ;
#47016 = ADVANCED_FACE('',(#11798),#45627,.T.) ;
#47017 = ADVANCED_FACE('',(#11799),#45628,.T.) ;
#47018 = ADVANCED_FACE('',(#11800),#9867,.T.) ;
#47019 = ADVANCED_FACE('',(#11801),#45629,.T.) ;
#47020 = ADVANCED_FACE('',(#11802),#9868,.T.) ;
#47021 = ADVANCED_FACE('',(#11803),#9869,.T.) ;
#47022 = ADVANCED_FACE('',(#11804),#9870,.F.) ;
#47023 = ADVANCED_FACE('',(#11805),#9871,.T.) ;
#47024 = ADVANCED_FACE('',(#11806),#9872,.T.) ;
#47025 = ADVANCED_FACE('',(#11807),#9873,.F.) ;
#47026 = ADVANCED_FACE('',(#11808),#9874,.F.) ;
#47027 = ADVANCED_FACE('',(#11809),#9875,.T.) ;
#47028 = ADVANCED_FACE('',(#11810),#9876,.T.) ;
#47029 = ADVANCED_FACE('',(#11811),#9877,.T.) ;
#47030 = ADVANCED_FACE('',(#11812),#9878,.F.) ;
#47031 = ADVANCED_FACE('',(#11813),#2387,.F.) ;
#47032 = ADVANCED_FACE('',(#11814),#2388,.F.) ;
#47033 = ADVANCED_FACE('',(#11815),#2389,.F.) ;
#47034 = ADVANCED_FACE('',(#11816),#2390,.F.) ;
#47035 = ADVANCED_FACE('',(#11817),#45630,.T.) ;
#47036 = ADVANCED_FACE('',(#11818),#9879,.F.) ;
#47037 = ADVANCED_FACE('',(#11819),#45631,.T.) ;
#47038 = ADVANCED_FACE('',(#11820),#9880,.T.) ;
#47039 = ADVANCED_FACE('',(#11821),#45632,.T.) ;
#47040 = ADVANCED_FACE('',(#11822),#9881,.T.) ;
#47041 = ADVANCED_FACE('',(#11823),#2391,.T.) ;
#47042 = ADVANCED_FACE('',(#11824),#2392,.F.) ;
#47043 = ADVANCED_FACE('',(#11825),#2393,.T.) ;
#47044 = ADVANCED_FACE('',(#11826),#9882,.T.) ;
#47045 = ADVANCED_FACE('',(#11827),#45633,.T.) ;
#47046 = ADVANCED_FACE('',(#11828),#9883,.T.) ;
#47047 = ADVANCED_FACE('',(#11829),#9884,.T.) ;
#47048 = ADVANCED_FACE('',(#11830),#45634,.T.) ;
#47049 = ADVANCED_FACE('',(#11831),#9885,.T.) ;
#47050 = ADVANCED_FACE('',(#11832),#45635,.T.) ;
#47051 = ADVANCED_FACE('',(#11833),#9886,.T.) ;
#47052 = ADVANCED_FACE('',(#11834),#45636,.T.) ;
#47053 = ADVANCED_FACE('',(#11835),#9887,.T.) ;
#47054 = ADVANCED_FACE('',(#11836),#45637,.T.) ;
#47055 = ADVANCED_FACE('',(#11837),#9888,.T.) ;
#47056 = ADVANCED_FACE('',(#11838),#45638,.T.) ;
#47057 = ADVANCED_FACE('',(#11839),#9889,.T.) ;
#47058 = ADVANCED_FACE('',(#11840),#9890,.T.) ;
#47059 = ADVANCED_FACE('',(#11841),#9891,.T.) ;
#47060 = ADVANCED_FACE('',(#11842),#45639,.T.) ;
#47061 = ADVANCED_FACE('',(#11843),#9892,.F.) ;
#47062 = ADVANCED_FACE('',(#11844),#45640,.T.) ;
#47063 = ADVANCED_FACE('',(#11845),#9893,.F.) ;
#47064 = ADVANCED_FACE('',(#11846),#9894,.T.) ;
#47065 = ADVANCED_FACE('',(#11847),#45641,.T.) ;
#47066 = ADVANCED_FACE('',(#11848),#9895,.T.) ;
#47067 = ADVANCED_FACE('',(#11849),#45642,.T.) ;
#47068 = ADVANCED_FACE('',(#11850),#9896,.T.) ;
#47069 = ADVANCED_FACE('',(#11851),#45643,.T.) ;
#47070 = ADVANCED_FACE('',(#11852),#45644,.T.) ;
#47071 = ADVANCED_FACE('',(#11853),#9897,.T.) ;
#47072 = ADVANCED_FACE('',(#11854),#45645,.T.) ;
#47073 = ADVANCED_FACE('',(#11855),#45646,.T.) ;
#47074 = ADVANCED_FACE('',(#11856),#9898,.T.) ;
#47075 = ADVANCED_FACE('',(#11857),#45647,.T.) ;
#47076 = ADVANCED_FACE('',(#11858),#9899,.T.) ;
#47077 = ADVANCED_FACE('',(#11859),#45648,.T.) ;
#47078 = ADVANCED_FACE('',(#11860),#9900,.T.) ;
#47079 = ADVANCED_FACE('',(#11861),#45649,.T.) ;
#47080 = ADVANCED_FACE('',(#11862),#9901,.T.) ;
#47081 = ADVANCED_FACE('',(#11863),#45650,.T.) ;
#47082 = ADVANCED_FACE('',(#11864),#9902,.T.) ;
#47083 = ADVANCED_FACE('',(#11865),#45651,.T.) ;
#47084 = ADVANCED_FACE('',(#11866),#9903,.T.) ;
#47085 = ADVANCED_FACE('',(#11867),#45652,.T.) ;
#47086 = ADVANCED_FACE('',(#11868),#9904,.T.) ;
#47087 = ADVANCED_FACE('',(#11869),#45653,.T.) ;
#47088 = ADVANCED_FACE('',(#11870),#9905,.F.) ;
#47089 = ADVANCED_FACE('',(#11871),#45654,.T.) ;
#47090 = ADVANCED_FACE('',(#11872),#9906,.T.) ;
#47091 = ADVANCED_FACE('',(#11873),#45655,.T.) ;
#47092 = ADVANCED_FACE('',(#11874),#9907,.T.) ;
#47093 = ADVANCED_FACE('',(#11875),#45656,.T.) ;
#47094 = ADVANCED_FACE('',(#11876,#718),#2394,.T.) ;
#47095 = ADVANCED_FACE('',(#11877),#45657,.F.) ;
#47096 = ADVANCED_FACE('',(#11878),#9908,.F.) ;
#47097 = ADVANCED_FACE('',(#11879),#45658,.T.) ;
#47098 = ADVANCED_FACE('',(#11880),#45659,.T.) ;
#47099 = ADVANCED_FACE('',(#11881),#9909,.F.) ;
#47100 = ADVANCED_FACE('',(#11882),#45660,.F.) ;
#47101 = ADVANCED_FACE('',(#11883,#719),#2395,.T.) ;
#47102 = ADVANCED_FACE('',(#11884),#45661,.T.) ;
#47103 = ADVANCED_FACE('',(#11885),#9910,.F.) ;
#47104 = ADVANCED_FACE('',(#11886),#45662,.T.) ;
#47105 = ADVANCED_FACE('',(#11887),#9911,.F.) ;
#47106 = ADVANCED_FACE('',(#11888),#45663,.T.) ;
#47107 = ADVANCED_FACE('',(#11889,#720),#2396,.T.) ;
#47108 = ADVANCED_FACE('',(#11890),#45664,.F.) ;
#47109 = ADVANCED_FACE('',(#11891),#45665,.T.) ;
#47110 = ADVANCED_FACE('',(#11892),#45666,.T.) ;
#47111 = ADVANCED_FACE('',(#11893),#45667,.T.) ;
#47112 = ADVANCED_FACE('',(#11894,#721),#2397,.F.) ;
#47113 = ADVANCED_FACE('',(#11895),#9912,.T.) ;
#47114 = ADVANCED_FACE('',(#11896),#2398,.T.) ;
#47115 = ADVANCED_FACE('',(#11897),#9913,.T.) ;
#47116 = ADVANCED_FACE('',(#11898),#2399,.T.) ;
#47117 = ADVANCED_FACE('',(#11899),#2400,.F.) ;
#47118 = ADVANCED_FACE('',(#11900),#2401,.T.) ;
#47119 = ADVANCED_FACE('',(#11901),#2402,.F.) ;
#47120 = ADVANCED_FACE('',(#11902),#2403,.F.) ;
#47121 = ADVANCED_FACE('',(#11903),#1973,.F.) ;
#47122 = ADVANCED_FACE('',(#11904),#1974,.F.) ;
#47123 = ADVANCED_FACE('',(#11905),#1975,.F.) ;
#47124 = ADVANCED_FACE('',(#11906),#1976,.F.) ;
#47125 = ADVANCED_FACE('',(#11907),#9914,.T.) ;
#47126 = ADVANCED_FACE('',(#11908),#1977,.F.) ;
#47127 = ADVANCED_FACE('',(#11909),#9915,.T.) ;
#47128 = ADVANCED_FACE('',(#11910),#1978,.F.) ;
#47129 = ADVANCED_FACE('',(#11911),#9916,.T.) ;
#47130 = ADVANCED_FACE('',(#11912),#9917,.T.) ;
#47131 = ADVANCED_FACE('',(#11913),#9918,.T.) ;
#47132 = ADVANCED_FACE('',(#11914),#1979,.F.) ;
#47133 = ADVANCED_FACE('',(#11915),#9919,.T.) ;
#47134 = ADVANCED_FACE('',(#11916),#1980,.F.) ;
#47135 = ADVANCED_FACE('',(#11917),#9920,.T.) ;
#47136 = ADVANCED_FACE('',(#11918),#9921,.T.) ;
#47137 = ADVANCED_FACE('',(#11919),#9922,.F.) ;
#47138 = ADVANCED_FACE('',(#11920),#9923,.F.) ;
#47139 = ADVANCED_FACE('',(#11921),#2404,.T.) ;
#47140 = ADVANCED_FACE('',(#11922),#9924,.T.) ;
#47141 = ADVANCED_FACE('',(#11923),#9925,.T.) ;
#47142 = ADVANCED_FACE('',(#11924),#2405,.T.) ;
#47143 = ADVANCED_FACE('',(#11925),#9926,.F.) ;
#47144 = ADVANCED_FACE('',(#11926),#9927,.F.) ;
#47145 = ADVANCED_FACE('',(#11927),#2406,.T.) ;
#47146 = ADVANCED_FACE('',(#11928),#9928,.T.) ;
#47147 = ADVANCED_FACE('',(#11929),#2407,.T.) ;
#47148 = ADVANCED_FACE('',(#11930),#2408,.T.) ;
#47149 = ADVANCED_FACE('',(#11931),#2409,.F.) ;
#47150 = ADVANCED_FACE('',(#11932),#2410,.T.) ;
#47151 = ADVANCED_FACE('',(#11933),#2411,.T.) ;
#47152 = ADVANCED_FACE('',(#11934),#2412,.F.) ;
#47153 = ADVANCED_FACE('',(#11935),#2413,.T.) ;
#47154 = ADVANCED_FACE('',(#11936),#2414,.T.) ;
#47155 = ADVANCED_FACE('',(#11937),#2415,.F.) ;
#47156 = ADVANCED_FACE('',(#11938),#2416,.T.) ;
#47157 = ADVANCED_FACE('',(#11939),#2417,.T.) ;
#47158 = ADVANCED_FACE('',(#11940),#2418,.F.) ;
#47159 = ADVANCED_FACE('',(#11941),#2419,.F.) ;
#47160 = ADVANCED_FACE('',(#11942),#2420,.F.) ;
#47161 = ADVANCED_FACE('',(#11943),#2421,.F.) ;
#47162 = ADVANCED_FACE('',(#11944),#2422,.F.) ;
#47163 = ADVANCED_FACE('',(#11945),#2423,.F.) ;
#47164 = ADVANCED_FACE('',(#11946),#9929,.T.) ;
#47165 = ADVANCED_FACE('',(#11947),#9930,.T.) ;
#47166 = ADVANCED_FACE('',(#11948),#9931,.T.) ;
#47167 = ADVANCED_FACE('',(#11949),#1981,.F.) ;
#47168 = ADVANCED_FACE('',(#11950),#1982,.F.) ;
#47169 = ADVANCED_FACE('',(#11951),#1983,.F.) ;
#47170 = ADVANCED_FACE('',(#11952),#2424,.F.) ;
#47171 = ADVANCED_FACE('',(#11953),#1984,.F.) ;
#47172 = ADVANCED_FACE('',(#11954),#2425,.F.) ;
#47173 = ADVANCED_FACE('',(#11955),#1985,.T.) ;
#47174 = ADVANCED_FACE('',(#11956),#1986,.T.) ;
#47175 = ADVANCED_FACE('',(#11957),#1987,.T.) ;
#47176 = ADVANCED_FACE('',(#11958),#1988,.T.) ;
#47177 = ADVANCED_FACE('',(#11959),#9932,.T.) ;
#47178 = ADVANCED_FACE('',(#11960),#2426,.T.) ;
#47179 = ADVANCED_FACE('',(#11961),#9933,.T.) ;
#47180 = ADVANCED_FACE('',(#11962),#9934,.T.) ;
#47181 = ADVANCED_FACE('',(#11963),#9935,.T.) ;
#47182 = ADVANCED_FACE('',(#11964),#2192,.T.) ;
#47183 = ADVANCED_FACE('',(#11965),#9936,.T.) ;
#47184 = ADVANCED_FACE('',(#11966),#9937,.T.) ;
#47185 = ADVANCED_FACE('',(#11967),#9938,.T.) ;
#47186 = ADVANCED_FACE('',(#11968),#2427,.T.) ;
#47187 = ADVANCED_FACE('',(#11969),#2428,.T.) ;
#47188 = ADVANCED_FACE('',(#11970),#2429,.T.) ;
#47189 = ADVANCED_FACE('',(#11971),#2430,.T.) ;
#47190 = ADVANCED_FACE('',(#11972),#2431,.T.) ;
#47191 = ADVANCED_FACE('',(#11973),#2432,.T.) ;
#47192 = ADVANCED_FACE('',(#11974),#2433,.T.) ;
#47193 = ADVANCED_FACE('',(#11975),#2434,.F.) ;
#47194 = ADVANCED_FACE('',(#11976),#9939,.T.) ;
#47195 = ADVANCED_FACE('',(#11977),#9940,.T.) ;
#47196 = ADVANCED_FACE('',(#11978),#9941,.T.) ;
#47197 = ADVANCED_FACE('',(#11979),#2193,.T.) ;
#47198 = ADVANCED_FACE('',(#11980),#2194,.T.) ;
#47199 = ADVANCED_FACE('',(#11981,#722,#723,#724,#725,#726),#2435,.F.) ;
#47200 = ADVANCED_FACE('',(#11982),#9942,.T.) ;
#47201 = ADVANCED_FACE('',(#11983),#2436,.T.) ;
#47202 = ADVANCED_FACE('',(#11984),#9943,.T.) ;
#47203 = ADVANCED_FACE('',(#11985,#727,#728),#2437,.T.) ;
#47204 = ADVANCED_FACE('',(#11986),#9944,.T.) ;
#47205 = ADVANCED_FACE('',(#11987),#9945,.T.) ;
#47206 = ADVANCED_FACE('',(#11988),#2438,.T.) ;
#47207 = ADVANCED_FACE('',(#11989),#45668,.T.) ;
#47208 = ADVANCED_FACE('',(#11990),#45669,.T.) ;
#47209 = ADVANCED_FACE('',(#11991),#9946,.T.) ;
#47210 = ADVANCED_FACE('',(#11992),#2439,.T.) ;
#47211 = ADVANCED_FACE('',(#11993),#9947,.T.) ;
#47212 = ADVANCED_FACE('',(#11994),#9948,.T.) ;
#47213 = ADVANCED_FACE('',(#11995),#45670,.T.) ;
#47214 = ADVANCED_FACE('',(#11996),#45671,.T.) ;
#47215 = ADVANCED_FACE('',(#11997),#9949,.T.) ;
#47216 = ADVANCED_FACE('',(#11998),#9950,.T.) ;
#47217 = ADVANCED_FACE('',(#11999),#2440,.T.) ;
#47218 = ADVANCED_FACE('',(#12000),#45672,.T.) ;
#47219 = ADVANCED_FACE('',(#12001),#45673,.T.) ;
#47220 = ADVANCED_FACE('',(#12002),#9951,.T.) ;
#47221 = ADVANCED_FACE('',(#12003),#9952,.T.) ;
#47222 = ADVANCED_FACE('',(#12004),#2441,.T.) ;
#47223 = ADVANCED_FACE('',(#12005),#9953,.T.) ;
#47224 = ADVANCED_FACE('',(#12006),#1989,.T.) ;
#47225 = ADVANCED_FACE('',(#12007),#9954,.F.) ;
#47226 = ADVANCED_FACE('',(#12008),#1990,.T.) ;
#47227 = ADVANCED_FACE('',(#12009),#2442,.T.) ;
#47228 = ADVANCED_FACE('',(#12010),#9955,.T.) ;
#47229 = ADVANCED_FACE('',(#12011),#9956,.T.) ;
#47230 = ADVANCED_FACE('',(#12012),#95,.F.) ;
#47231 = ADVANCED_FACE('',(#12013),#96,.F.) ;
#47232 = ADVANCED_FACE('',(#12014),#9957,.T.) ;
#47233 = ADVANCED_FACE('',(#12015),#9958,.T.) ;
#47234 = ADVANCED_FACE('',(#12016),#2443,.T.) ;
#47235 = ADVANCED_FACE('',(#12017),#9959,.T.) ;
#47236 = ADVANCED_FACE('',(#12018),#45674,.T.) ;
#47237 = ADVANCED_FACE('',(#12019),#9960,.T.) ;
#47238 = ADVANCED_FACE('',(#12020),#45675,.T.) ;
#47239 = ADVANCED_FACE('',(#12021),#9961,.F.) ;
#47240 = ADVANCED_FACE('',(#12022),#2444,.T.) ;
#47241 = ADVANCED_FACE('',(#12023),#45676,.T.) ;
#47242 = ADVANCED_FACE('',(#12024),#2445,.T.) ;
#47243 = ADVANCED_FACE('',(#12025),#9962,.F.) ;
#47244 = ADVANCED_FACE('',(#12026),#2446,.T.) ;
#47245 = ADVANCED_FACE('',(#12027),#45677,.T.) ;
#47246 = ADVANCED_FACE('',(#12028),#2447,.T.) ;
#47247 = ADVANCED_FACE('',(#12029),#9963,.T.) ;
#47248 = ADVANCED_FACE('',(#12030),#9964,.T.) ;
#47249 = ADVANCED_FACE('',(#12031),#9965,.T.) ;
#47250 = ADVANCED_FACE('',(#12032),#9966,.T.) ;
#47251 = ADVANCED_FACE('',(#12033),#2448,.T.) ;
#47252 = ADVANCED_FACE('',(#12034),#2449,.T.) ;
#47253 = ADVANCED_FACE('',(#12035),#2450,.T.) ;
#47254 = ADVANCED_FACE('',(#12036),#9967,.T.) ;
#47255 = ADVANCED_FACE('',(#12037),#9968,.T.) ;
#47256 = ADVANCED_FACE('',(#12038),#45678,.T.) ;
#47257 = ADVANCED_FACE('',(#12039),#9969,.T.) ;
#47258 = ADVANCED_FACE('',(#12040),#45679,.T.) ;
#47259 = ADVANCED_FACE('',(#12041),#2451,.T.) ;
#47260 = ADVANCED_FACE('',(#12042),#45680,.T.) ;
#47261 = ADVANCED_FACE('',(#12043),#9970,.T.) ;
#47262 = ADVANCED_FACE('',(#12044),#45681,.T.) ;
#47263 = ADVANCED_FACE('',(#12045),#2452,.T.) ;
#47264 = ADVANCED_FACE('',(#12046),#45682,.T.) ;
#47265 = ADVANCED_FACE('',(#12047),#9971,.T.) ;
#47266 = ADVANCED_FACE('',(#12048),#45683,.T.) ;
#47267 = ADVANCED_FACE('',(#12049),#2453,.T.) ;
#47268 = ADVANCED_FACE('',(#12050),#45684,.T.) ;
#47269 = ADVANCED_FACE('',(#12051),#9972,.T.) ;
#47270 = ADVANCED_FACE('',(#12052),#45685,.T.) ;
#47271 = ADVANCED_FACE('',(#12053),#2454,.T.) ;
#47272 = ADVANCED_FACE('',(#12054),#45686,.T.) ;
#47273 = ADVANCED_FACE('',(#12055),#9973,.T.) ;
#47274 = ADVANCED_FACE('',(#12056),#45687,.T.) ;
#47275 = ADVANCED_FACE('',(#12057),#2455,.T.) ;
#47276 = ADVANCED_FACE('',(#12058),#45688,.T.) ;
#47277 = ADVANCED_FACE('',(#12059),#9974,.T.) ;
#47278 = ADVANCED_FACE('',(#12060),#45689,.T.) ;
#47279 = ADVANCED_FACE('',(#12061),#2456,.T.) ;
#47280 = ADVANCED_FACE('',(#12062),#45690,.T.) ;
#47281 = ADVANCED_FACE('',(#12063),#9975,.T.) ;
#47282 = ADVANCED_FACE('',(#12064),#45691,.T.) ;
#47283 = ADVANCED_FACE('',(#12065),#2457,.T.) ;
#47284 = ADVANCED_FACE('',(#12066),#45692,.T.) ;
#47285 = ADVANCED_FACE('',(#12067),#9976,.T.) ;
#47286 = ADVANCED_FACE('',(#12068),#45693,.T.) ;
#47287 = ADVANCED_FACE('',(#12069),#2458,.T.) ;
#47288 = ADVANCED_FACE('',(#12070),#9977,.T.) ;
#47289 = ADVANCED_FACE('',(#12071),#2459,.T.) ;
#47290 = ADVANCED_FACE('',(#12072),#9978,.T.) ;
#47291 = ADVANCED_FACE('',(#12073),#9979,.T.) ;
#47292 = ADVANCED_FACE('',(#12074),#2460,.T.) ;
#47293 = ADVANCED_FACE('',(#12075),#9980,.T.) ;
#47294 = ADVANCED_FACE('',(#12076),#9981,.T.) ;
#47295 = ADVANCED_FACE('',(#12077),#2461,.T.) ;
#47296 = ADVANCED_FACE('',(#12078),#9982,.T.) ;
#47297 = ADVANCED_FACE('',(#12079),#9983,.T.) ;
#47298 = ADVANCED_FACE('',(#12080),#2462,.T.) ;
#47299 = ADVANCED_FACE('',(#12081),#9984,.T.) ;
#47300 = ADVANCED_FACE('',(#12082),#2463,.T.) ;
#47301 = ADVANCED_FACE('',(#12083),#2464,.T.) ;
#47302 = ADVANCED_FACE('',(#12084),#2465,.T.) ;
#47303 = ADVANCED_FACE('',(#12085),#9985,.F.) ;
#47304 = ADVANCED_FACE('',(#12086),#2466,.T.) ;
#47305 = ADVANCED_FACE('',(#12087),#2467,.T.) ;
#47306 = ADVANCED_FACE('',(#12088),#9986,.F.) ;
#47307 = ADVANCED_FACE('',(#12089),#2468,.T.) ;
#47308 = ADVANCED_FACE('',(#12090),#2469,.T.) ;
#47309 = ADVANCED_FACE('',(#12091),#2470,.T.) ;
#47310 = ADVANCED_FACE('',(#12092),#2471,.T.) ;
#47311 = ADVANCED_FACE('',(#12093),#2472,.T.) ;
#47312 = ADVANCED_FACE('',(#12094),#2473,.T.) ;
#47313 = ADVANCED_FACE('',(#12095),#2474,.T.) ;
#47314 = ADVANCED_FACE('',(#12096),#2475,.T.) ;
#47315 = ADVANCED_FACE('',(#12097),#2476,.T.) ;
#47316 = ADVANCED_FACE('',(#12098),#2477,.T.) ;
#47317 = ADVANCED_FACE('',(#12099),#2478,.T.) ;
#47318 = ADVANCED_FACE('',(#12100),#2479,.T.) ;
#47319 = ADVANCED_FACE('',(#12101),#2480,.T.) ;
#47320 = ADVANCED_FACE('',(#12102),#2481,.F.) ;
#47321 = ADVANCED_FACE('',(#12103),#45694,.T.) ;
#47322 = ADVANCED_FACE('',(#12104),#9987,.F.) ;
#47323 = ADVANCED_FACE('',(#12105),#9988,.T.) ;
#47324 = ADVANCED_FACE('',(#12106,#729),#2482,.T.) ;
#47325 = ADVANCED_FACE('',(#12107),#45695,.T.) ;
#47326 = ADVANCED_FACE('',(#12108),#9989,.F.) ;
#47327 = ADVANCED_FACE('',(#12109),#9990,.T.) ;
#47328 = ADVANCED_FACE('',(#12110,#730),#2483,.T.) ;
#47329 = ADVANCED_FACE('',(#12111),#45696,.T.) ;
#47330 = ADVANCED_FACE('',(#12112),#9991,.F.) ;
#47331 = ADVANCED_FACE('',(#12113,#731),#2484,.F.) ;
#47332 = ADVANCED_FACE('',(#12114),#9992,.T.) ;
#47333 = ADVANCED_FACE('',(#12115,#732),#2485,.T.) ;
#47334 = ADVANCED_FACE('',(#12116),#45697,.T.) ;
#47335 = ADVANCED_FACE('',(#12117),#1991,.T.) ;
#47336 = ADVANCED_FACE('',(#12118),#9993,.F.) ;
#47337 = ADVANCED_FACE('',(#12119),#2195,.T.) ;
#47338 = ADVANCED_FACE('',(#12120),#1992,.F.) ;
#47339 = ADVANCED_FACE('',(#12121),#9994,.T.) ;
#47340 = ADVANCED_FACE('',(#12122),#45698,.T.) ;
#47341 = ADVANCED_FACE('',(#12123),#1993,.T.) ;
#47342 = ADVANCED_FACE('',(#12124),#9995,.F.) ;
#47343 = ADVANCED_FACE('',(#12125),#9996,.T.) ;
#47344 = ADVANCED_FACE('',(#12126),#45699,.T.) ;
#47345 = ADVANCED_FACE('',(#12127),#1994,.T.) ;
#47346 = ADVANCED_FACE('',(#12128),#9997,.F.) ;
#47347 = ADVANCED_FACE('',(#12129),#2196,.T.) ;
#47348 = ADVANCED_FACE('',(#12130),#1995,.F.) ;
#47349 = ADVANCED_FACE('',(#12131),#9998,.T.) ;
#47350 = ADVANCED_FACE('',(#12132),#9999,.T.) ;
#47351 = ADVANCED_FACE('',(#12133),#45700,.T.) ;
#47352 = ADVANCED_FACE('',(#12134),#1996,.T.) ;
#47353 = ADVANCED_FACE('',(#12135),#10000,.F.) ;
#47354 = ADVANCED_FACE('',(#12136),#45701,.T.) ;
#47355 = ADVANCED_FACE('',(#12137),#1997,.T.) ;
#47356 = ADVANCED_FACE('',(#12138),#10001,.F.) ;
#47357 = ADVANCED_FACE('',(#12139),#10002,.T.) ;
#47358 = ADVANCED_FACE('',(#12140),#2197,.T.) ;
#47359 = ADVANCED_FACE('',(#12141),#1998,.F.) ;
#47360 = ADVANCED_FACE('',(#12142),#10003,.T.) ;
#47361 = ADVANCED_FACE('',(#12143),#45702,.T.) ;
#47362 = ADVANCED_FACE('',(#12144),#1999,.T.) ;
#47363 = ADVANCED_FACE('',(#12145),#10004,.F.) ;
#47364 = ADVANCED_FACE('',(#12146),#10005,.T.) ;
#47365 = ADVANCED_FACE('',(#12147),#45703,.T.) ;
#47366 = ADVANCED_FACE('',(#12148),#2000,.T.) ;
#47367 = ADVANCED_FACE('',(#12149),#10006,.F.) ;
#47368 = ADVANCED_FACE('',(#12150),#2198,.T.) ;
#47369 = ADVANCED_FACE('',(#12151),#2001,.F.) ;
#47370 = ADVANCED_FACE('',(#12152),#10007,.T.) ;
#47371 = ADVANCED_FACE('',(#12153),#10008,.T.) ;
#47372 = ADVANCED_FACE('',(#12154),#45704,.T.) ;
#47373 = ADVANCED_FACE('',(#12155),#2002,.T.) ;
#47374 = ADVANCED_FACE('',(#12156),#10009,.F.) ;
#47375 = ADVANCED_FACE('',(#12157),#10010,.T.) ;
#47376 = ADVANCED_FACE('',(#12158),#10011,.T.) ;
#47377 = ADVANCED_FACE('',(#12159),#10012,.T.) ;
#47378 = ADVANCED_FACE('',(#12160),#10013,.T.) ;
#47379 = ADVANCED_FACE('',(#12161),#10014,.T.) ;
#47380 = ADVANCED_FACE('',(#12162),#10015,.T.) ;
#47381 = ADVANCED_FACE('',(#12163),#10016,.T.) ;
#47382 = ADVANCED_FACE('',(#12164),#2486,.T.) ;
#47383 = ADVANCED_FACE('',(#12165),#2487,.T.) ;
#47384 = ADVANCED_FACE('',(#12166),#10017,.F.) ;
#47385 = ADVANCED_FACE('',(#12167),#2488,.T.) ;
#47386 = ADVANCED_FACE('',(#12168),#10018,.F.) ;
#47387 = ADVANCED_FACE('',(#12169),#2489,.T.) ;
#47388 = ADVANCED_FACE('',(#12170),#10019,.F.) ;
#47389 = ADVANCED_FACE('',(#12171),#2490,.T.) ;
#47390 = ADVANCED_FACE('',(#12172),#10020,.F.) ;
#47391 = ADVANCED_FACE('',(#12173),#2491,.T.) ;
#47392 = ADVANCED_FACE('',(#12174),#10021,.F.) ;
#47393 = ADVANCED_FACE('',(#12175,#733),#2492,.F.) ;
#47394 = ADVANCED_FACE('',(#12176),#10022,.F.) ;
#47395 = ADVANCED_FACE('',(#12177),#10023,.F.) ;
#47396 = ADVANCED_FACE('',(#12178),#10024,.F.) ;
#47397 = ADVANCED_FACE('',(#12179),#10025,.F.) ;
#47398 = ADVANCED_FACE('',(#12180),#10026,.F.) ;
#47399 = ADVANCED_FACE('',(#12181),#10027,.F.) ;
#47400 = ADVANCED_FACE('',(#12182),#10028,.F.) ;
#47401 = ADVANCED_FACE('',(#12183),#2493,.T.) ;
#47402 = ADVANCED_FACE('',(#12184),#2494,.T.) ;
#47403 = ADVANCED_FACE('',(#12185),#2495,.T.) ;
#47404 = ADVANCED_FACE('',(#12186),#2496,.T.) ;
#47405 = ADVANCED_FACE('',(#12187),#2497,.T.) ;
#47406 = ADVANCED_FACE('',(#12188),#2498,.T.) ;
#47407 = ADVANCED_FACE('',(#12189),#45705,.T.) ;
#47408 = ADVANCED_FACE('',(#12190),#10029,.T.) ;
#47409 = ADVANCED_FACE('',(#12191),#45706,.T.) ;
#47410 = ADVANCED_FACE('',(#12192),#2499,.T.) ;
#47411 = ADVANCED_FACE('',(#12193),#2500,.T.) ;
#47412 = ADVANCED_FACE('',(#12194),#2199,.T.) ;
#47413 = ADVANCED_FACE('',(#12195),#2200,.T.) ;
#47414 = ADVANCED_FACE('',(#12196),#2201,.T.) ;
#47415 = ADVANCED_FACE('',(#12197),#10030,.T.) ;
#47416 = ADVANCED_FACE('',(#12198),#10031,.T.) ;
#47417 = ADVANCED_FACE('',(#12199),#2202,.T.) ;
#47418 = ADVANCED_FACE('',(#12200),#2203,.T.) ;
#47419 = ADVANCED_FACE('',(#12201),#10032,.T.) ;
#47420 = ADVANCED_FACE('',(#12202),#10033,.T.) ;
#47421 = ADVANCED_FACE('',(#12203),#10034,.T.) ;
#47422 = ADVANCED_FACE('',(#12204),#10035,.T.) ;
#47423 = ADVANCED_FACE('',(#12205),#10036,.T.) ;
#47424 = ADVANCED_FACE('',(#12206),#10037,.T.) ;
#47425 = ADVANCED_FACE('',(#12207),#10038,.T.) ;
#47426 = ADVANCED_FACE('',(#12208),#10039,.T.) ;
#47427 = ADVANCED_FACE('',(#12209),#2501,.T.) ;
#47428 = ADVANCED_FACE('',(#12210),#2502,.T.) ;
#47429 = ADVANCED_FACE('',(#12211),#2503,.T.) ;
#47430 = ADVANCED_FACE('',(#12212),#2504,.T.) ;
#47431 = ADVANCED_FACE('',(#12213),#2505,.T.) ;
#47432 = ADVANCED_FACE('',(#12214),#2506,.T.) ;
#47433 = ADVANCED_FACE('',(#12215),#45707,.T.) ;
#47434 = ADVANCED_FACE('',(#12216),#10040,.T.) ;
#47435 = ADVANCED_FACE('',(#12217),#2507,.T.) ;
#47436 = ADVANCED_FACE('',(#12218),#10041,.T.) ;
#47437 = ADVANCED_FACE('',(#12219),#10042,.T.) ;
#47438 = ADVANCED_FACE('',(#12220),#10043,.T.) ;
#47439 = ADVANCED_FACE('',(#12221),#10044,.T.) ;
#47440 = ADVANCED_FACE('',(#12222),#10045,.T.) ;
#47441 = ADVANCED_FACE('',(#12223),#10046,.T.) ;
#47442 = ADVANCED_FACE('',(#12224),#10047,.T.) ;
#47443 = ADVANCED_FACE('',(#12225),#10048,.T.) ;
#47444 = ADVANCED_FACE('',(#12226),#10049,.T.) ;
#47445 = ADVANCED_FACE('',(#12227),#10050,.T.) ;
#47446 = ADVANCED_FACE('',(#12228),#10051,.T.) ;
#47447 = ADVANCED_FACE('',(#12229),#10052,.T.) ;
#47448 = ADVANCED_FACE('',(#12230),#2508,.F.) ;
#47449 = ADVANCED_FACE('',(#12231),#2509,.F.) ;
#47450 = ADVANCED_FACE('',(#12232),#2510,.F.) ;
#47451 = ADVANCED_FACE('',(#12233),#2511,.F.) ;
#47452 = ADVANCED_FACE('',(#12234),#2512,.F.) ;
#47453 = ADVANCED_FACE('',(#12235),#2513,.F.) ;
#47454 = ADVANCED_FACE('',(#12236,#734),#2514,.F.) ;
#47455 = ADVANCED_FACE('',(#12237),#10053,.F.) ;
#47456 = ADVANCED_FACE('',(#12238),#10054,.F.) ;
#47457 = ADVANCED_FACE('',(#12239),#10055,.F.) ;
#47458 = ADVANCED_FACE('',(#12240),#10056,.F.) ;
#47459 = ADVANCED_FACE('',(#12241),#10057,.F.) ;
#47460 = ADVANCED_FACE('',(#12242),#10058,.F.) ;
#47461 = ADVANCED_FACE('',(#12243),#10059,.F.) ;
#47462 = ADVANCED_FACE('',(#12244),#10060,.F.) ;
#47463 = ADVANCED_FACE('',(#12245),#10061,.F.) ;
#47464 = ADVANCED_FACE('',(#12246),#10062,.F.) ;
#47465 = ADVANCED_FACE('',(#12247),#10063,.F.) ;
#47466 = ADVANCED_FACE('',(#12248),#10064,.F.) ;
#47467 = ADVANCED_FACE('',(#12249),#2515,.F.) ;
#47468 = ADVANCED_FACE('',(#12250),#2516,.F.) ;
#47469 = ADVANCED_FACE('',(#12251),#2517,.F.) ;
#47470 = ADVANCED_FACE('',(#12252),#2518,.F.) ;
#47471 = ADVANCED_FACE('',(#12253),#45708,.T.) ;
#47472 = ADVANCED_FACE('',(#12254),#2519,.F.) ;
#47473 = ADVANCED_FACE('',(#12255),#2520,.F.) ;
#47474 = ADVANCED_FACE('',(#12256),#2521,.F.) ;
#47475 = ADVANCED_FACE('',(#12257),#10065,.F.) ;
#47476 = ADVANCED_FACE('',(#12258),#10066,.F.) ;
#47477 = ADVANCED_FACE('',(#12259),#10067,.F.) ;
#47478 = ADVANCED_FACE('',(#12260),#10068,.F.) ;
#47479 = ADVANCED_FACE('',(#12261),#10069,.F.) ;
#47480 = ADVANCED_FACE('',(#12262),#10070,.F.) ;
#47481 = ADVANCED_FACE('',(#12263),#10071,.F.) ;
#47482 = ADVANCED_FACE('',(#12264),#10072,.F.) ;
#47483 = ADVANCED_FACE('',(#12265),#10073,.F.) ;
#47484 = ADVANCED_FACE('',(#12266),#10074,.F.) ;
#47485 = ADVANCED_FACE('',(#12267),#10075,.F.) ;
#47486 = ADVANCED_FACE('',(#12268),#10076,.F.) ;
#47487 = ADVANCED_FACE('',(#12269),#2522,.F.) ;
#47488 = ADVANCED_FACE('',(#12270),#2523,.F.) ;
#47489 = ADVANCED_FACE('',(#12271),#2524,.F.) ;
#47490 = ADVANCED_FACE('',(#12272),#2525,.F.) ;
#47491 = ADVANCED_FACE('',(#12273),#2526,.F.) ;
#47492 = ADVANCED_FACE('',(#12274),#2527,.F.) ;
#47493 = ADVANCED_FACE('',(#12275),#2528,.F.) ;
#47494 = ADVANCED_FACE('',(#12276),#45709,.T.) ;
#47495 = ADVANCED_FACE('',(#12277),#10077,.T.) ;
#47496 = ADVANCED_FACE('',(#12278),#2529,.T.) ;
#47497 = ADVANCED_FACE('',(#12279),#10078,.T.) ;
#47498 = ADVANCED_FACE('',(#12280),#10079,.T.) ;
#47499 = ADVANCED_FACE('',(#12281),#10080,.T.) ;
#47500 = ADVANCED_FACE('',(#12282),#10081,.T.) ;
#47501 = ADVANCED_FACE('',(#12283),#10082,.T.) ;
#47502 = ADVANCED_FACE('',(#12284),#10083,.T.) ;
#47503 = ADVANCED_FACE('',(#12285),#10084,.T.) ;
#47504 = ADVANCED_FACE('',(#12286),#10085,.T.) ;
#47505 = ADVANCED_FACE('',(#12287),#10086,.T.) ;
#47506 = ADVANCED_FACE('',(#12288),#10087,.T.) ;
#47507 = ADVANCED_FACE('',(#12289),#10088,.T.) ;
#47508 = ADVANCED_FACE('',(#12290),#10089,.T.) ;
#47509 = ADVANCED_FACE('',(#12291),#2530,.F.) ;
#47510 = ADVANCED_FACE('',(#12292),#2531,.F.) ;
#47511 = ADVANCED_FACE('',(#12293),#2532,.F.) ;
#47512 = ADVANCED_FACE('',(#12294,#735),#2533,.F.) ;
#47513 = ADVANCED_FACE('',(#12295),#45710,.T.) ;
#47514 = ADVANCED_FACE('',(#12296),#2534,.F.) ;
#47515 = ADVANCED_FACE('',(#12297),#2535,.F.) ;
#47516 = ADVANCED_FACE('',(#12298),#2536,.F.) ;
#47517 = ADVANCED_FACE('',(#12299),#10090,.F.) ;
#47518 = ADVANCED_FACE('',(#12300),#10091,.F.) ;
#47519 = ADVANCED_FACE('',(#12301),#10092,.F.) ;
#47520 = ADVANCED_FACE('',(#12302),#10093,.F.) ;
#47521 = ADVANCED_FACE('',(#12303),#10094,.F.) ;
#47522 = ADVANCED_FACE('',(#12304),#10095,.F.) ;
#47523 = ADVANCED_FACE('',(#12305),#10096,.F.) ;
#47524 = ADVANCED_FACE('',(#12306),#10097,.F.) ;
#47525 = ADVANCED_FACE('',(#12307),#10098,.F.) ;
#47526 = ADVANCED_FACE('',(#12308),#10099,.F.) ;
#47527 = ADVANCED_FACE('',(#12309),#10100,.F.) ;
#47528 = ADVANCED_FACE('',(#12310),#10101,.F.) ;
#47529 = ADVANCED_FACE('',(#12311),#2537,.F.) ;
#47530 = ADVANCED_FACE('',(#12312),#2538,.F.) ;
#47531 = ADVANCED_FACE('',(#12313),#2539,.F.) ;
#47532 = ADVANCED_FACE('',(#12314),#2540,.F.) ;
#47533 = ADVANCED_FACE('',(#12315),#2541,.F.) ;
#47534 = ADVANCED_FACE('',(#12316),#2542,.F.) ;
#47535 = ADVANCED_FACE('',(#12317),#2543,.F.) ;
#47536 = ADVANCED_FACE('',(#12318),#45711,.T.) ;
#47537 = ADVANCED_FACE('',(#12319),#10102,.T.) ;
#47538 = ADVANCED_FACE('',(#12320),#2544,.T.) ;
#47539 = ADVANCED_FACE('',(#12321),#10103,.T.) ;
#47540 = ADVANCED_FACE('',(#12322),#10104,.T.) ;
#47541 = ADVANCED_FACE('',(#12323),#10105,.T.) ;
#47542 = ADVANCED_FACE('',(#12324),#10106,.T.) ;
#47543 = ADVANCED_FACE('',(#12325),#10107,.T.) ;
#47544 = ADVANCED_FACE('',(#12326),#10108,.T.) ;
#47545 = ADVANCED_FACE('',(#12327),#10109,.T.) ;
#47546 = ADVANCED_FACE('',(#12328),#10110,.T.) ;
#47547 = ADVANCED_FACE('',(#12329),#10111,.T.) ;
#47548 = ADVANCED_FACE('',(#12330),#10112,.T.) ;
#47549 = ADVANCED_FACE('',(#12331),#10113,.T.) ;
#47550 = ADVANCED_FACE('',(#12332),#10114,.T.) ;
#47551 = ADVANCED_FACE('',(#12333),#2545,.F.) ;
#47552 = ADVANCED_FACE('',(#12334),#2546,.F.) ;
#47553 = ADVANCED_FACE('',(#12335),#2547,.F.) ;
#47554 = ADVANCED_FACE('',(#12336,#736),#2548,.F.) ;
#47555 = ADVANCED_FACE('',(#12337),#45712,.T.) ;
#47556 = ADVANCED_FACE('',(#12338),#2549,.F.) ;
#47557 = ADVANCED_FACE('',(#12339),#2550,.F.) ;
#47558 = ADVANCED_FACE('',(#12340),#2551,.F.) ;
#47559 = ADVANCED_FACE('',(#12341),#2204,.F.) ;
#47560 = ADVANCED_FACE('',(#12342),#2205,.F.) ;
#47561 = ADVANCED_FACE('',(#12343),#10115,.F.) ;
#47562 = ADVANCED_FACE('',(#12344),#2206,.F.) ;
#47563 = ADVANCED_FACE('',(#12345),#10116,.F.) ;
#47564 = ADVANCED_FACE('',(#12346),#45713,.T.) ;
#47565 = ADVANCED_FACE('',(#12347),#2003,.F.) ;
#47566 = ADVANCED_FACE('',(#12348),#10117,.T.) ;
#47567 = ADVANCED_FACE('',(#12349),#10118,.F.) ;
#47568 = ADVANCED_FACE('',(#12350),#2207,.F.) ;
#47569 = ADVANCED_FACE('',(#12351),#10119,.F.) ;
#47570 = ADVANCED_FACE('',(#12352),#10120,.F.) ;
#47571 = ADVANCED_FACE('',(#12353),#45714,.T.) ;
#47572 = ADVANCED_FACE('',(#12354),#2004,.F.) ;
#47573 = ADVANCED_FACE('',(#12355),#10121,.T.) ;
#47574 = ADVANCED_FACE('',(#12356),#10122,.T.) ;
#47575 = ADVANCED_FACE('',(#12357),#10123,.F.) ;
#47576 = ADVANCED_FACE('',(#12358),#10124,.F.) ;
#47577 = ADVANCED_FACE('',(#12359),#10125,.T.) ;
#47578 = ADVANCED_FACE('',(#12360),#10126,.F.) ;
#47579 = ADVANCED_FACE('',(#12361),#2552,.F.) ;
#47580 = ADVANCED_FACE('',(#12362),#2553,.F.) ;
#47581 = ADVANCED_FACE('',(#12363),#2554,.F.) ;
#47582 = ADVANCED_FACE('',(#12364),#2555,.T.) ;
#47583 = ADVANCED_FACE('',(#12365),#2556,.F.) ;
#47584 = ADVANCED_FACE('',(#12366),#2208,.T.) ;
#47585 = ADVANCED_FACE('',(#12367),#2209,.T.) ;
#47586 = ADVANCED_FACE('',(#12368),#10127,.T.) ;
#47587 = ADVANCED_FACE('',(#12369),#10128,.T.) ;
#47588 = ADVANCED_FACE('',(#12370),#2210,.T.) ;
#47589 = ADVANCED_FACE('',(#12371),#10129,.T.) ;
#47590 = ADVANCED_FACE('',(#12372),#10130,.T.) ;
#47591 = ADVANCED_FACE('',(#12373),#10131,.T.) ;
#47592 = ADVANCED_FACE('',(#12374),#10132,.T.) ;
#47593 = ADVANCED_FACE('',(#12375),#10133,.T.) ;
#47594 = ADVANCED_FACE('',(#12376),#2557,.T.) ;
#47595 = ADVANCED_FACE('',(#12377),#2558,.T.) ;
#47596 = ADVANCED_FACE('',(#12378),#2559,.T.) ;
#47597 = ADVANCED_FACE('',(#12379,#737),#2560,.F.) ;
#47598 = ADVANCED_FACE('',(#12380),#2561,.T.) ;
#47599 = ADVANCED_FACE('',(#12381),#2562,.T.) ;
#47600 = ADVANCED_FACE('',(#12382),#2005,.T.) ;
#47601 = ADVANCED_FACE('',(#12383),#2006,.T.) ;
#47602 = ADVANCED_FACE('',(#12384),#2007,.T.) ;
#47603 = ADVANCED_FACE('',(#12385),#2008,.T.) ;
#47604 = ADVANCED_FACE('',(#12386),#2009,.T.) ;
#47605 = ADVANCED_FACE('',(#12387),#2563,.F.) ;
#47606 = ADVANCED_FACE('',(#12388),#2010,.F.) ;
#47607 = ADVANCED_FACE('',(#12389),#2011,.F.) ;
#47608 = ADVANCED_FACE('',(#12390),#2012,.F.) ;
#47609 = ADVANCED_FACE('',(#12391),#2013,.F.) ;
#47610 = ADVANCED_FACE('',(#12392),#2014,.F.) ;
#47611 = ADVANCED_FACE('',(#12393),#2564,.F.) ;
#47612 = ADVANCED_FACE('',(#12394),#2565,.F.) ;
#47613 = ADVANCED_FACE('',(#12395),#2566,.F.) ;
#47614 = ADVANCED_FACE('',(#12396),#2567,.F.) ;
#47615 = ADVANCED_FACE('',(#12397),#2015,.F.) ;
#47616 = ADVANCED_FACE('',(#12398),#2016,.F.) ;
#47617 = ADVANCED_FACE('',(#12399),#2017,.F.) ;
#47618 = ADVANCED_FACE('',(#12400),#2018,.F.) ;
#47619 = ADVANCED_FACE('',(#12401),#2568,.F.) ;
#47620 = ADVANCED_FACE('',(#12402),#2569,.F.) ;
#47621 = ADVANCED_FACE('',(#12403),#2570,.F.) ;
#47622 = ADVANCED_FACE('',(#12404),#2019,.F.) ;
#47623 = ADVANCED_FACE('',(#12405),#2020,.F.) ;
#47624 = ADVANCED_FACE('',(#12406),#2021,.F.) ;
#47625 = ADVANCED_FACE('',(#12407),#2022,.F.) ;
#47626 = ADVANCED_FACE('',(#12408),#2023,.F.) ;
#47627 = ADVANCED_FACE('',(#12409),#2024,.F.) ;
#47628 = ADVANCED_FACE('',(#12410),#2025,.F.) ;
#47629 = ADVANCED_FACE('',(#12411),#2571,.F.) ;
#47630 = ADVANCED_FACE('',(#12412),#2572,.F.) ;
#47631 = ADVANCED_FACE('',(#12413),#2573,.F.) ;
#47632 = ADVANCED_FACE('',(#12414,#738),#2574,.T.) ;
#47633 = ADVANCED_FACE('',(#12415,#739,#740),#2575,.T.) ;
#47634 = ADVANCED_FACE('',(#12416),#2026,.T.) ;
#47635 = ADVANCED_FACE('',(#12417),#2027,.T.) ;
#47636 = ADVANCED_FACE('',(#12418),#45715,.T.) ;
#47637 = ADVANCED_FACE('',(#12419),#10134,.T.) ;
#47638 = ADVANCED_FACE('',(#12420),#97,.F.) ;
#47639 = ADVANCED_FACE('',(#12421),#10135,.T.) ;
#47640 = ADVANCED_FACE('',(#12422),#2028,.F.) ;
#47641 = ADVANCED_FACE('',(#12423),#2576,.F.) ;
#47642 = ADVANCED_FACE('',(#12424),#10136,.T.) ;
#47643 = ADVANCED_FACE('',(#12425),#2577,.T.) ;
#47644 = ADVANCED_FACE('',(#12426),#2029,.F.) ;
#47645 = ADVANCED_FACE('',(#12427),#10137,.T.) ;
#47646 = ADVANCED_FACE('',(#12428),#98,.F.) ;
#47647 = ADVANCED_FACE('',(#12429),#10138,.T.) ;
#47648 = ADVANCED_FACE('',(#12430),#45716,.T.) ;
#47649 = ADVANCED_FACE('',(#12431),#2578,.T.) ;
#47650 = ADVANCED_FACE('',(#12432),#10139,.T.) ;
#47651 = ADVANCED_FACE('',(#12433),#2579,.T.) ;
#47652 = ADVANCED_FACE('',(#12434),#2030,.F.) ;
#47653 = ADVANCED_FACE('',(#12435),#2580,.T.) ;
#47654 = ADVANCED_FACE('',(#12436),#2581,.T.) ;
#47655 = ADVANCED_FACE('',(#12437),#2031,.T.) ;
#47656 = ADVANCED_FACE('',(#12438),#10140,.F.) ;
#47657 = ADVANCED_FACE('',(#12439),#2032,.T.) ;
#47658 = ADVANCED_FACE('',(#12440),#2033,.T.) ;
#47659 = ADVANCED_FACE('',(#12441),#10141,.T.) ;
#47660 = ADVANCED_FACE('',(#12442),#2582,.F.) ;
#47661 = ADVANCED_FACE('',(#12443),#10142,.T.) ;
#47662 = ADVANCED_FACE('',(#12444),#2034,.T.) ;
#47663 = ADVANCED_FACE('',(#12445),#10143,.F.) ;
#47664 = ADVANCED_FACE('',(#12446),#2035,.T.) ;
#47665 = ADVANCED_FACE('',(#12447),#2036,.T.) ;
#47666 = ADVANCED_FACE('',(#12448),#2583,.F.) ;
#47667 = ADVANCED_FACE('',(#12449),#10144,.T.) ;
#47668 = ADVANCED_FACE('',(#12450),#10145,.T.) ;
#47669 = ADVANCED_FACE('',(#12451),#2037,.F.) ;
#47670 = ADVANCED_FACE('',(#12452),#10146,.T.) ;
#47671 = ADVANCED_FACE('',(#12453),#10147,.T.) ;
#47672 = ADVANCED_FACE('',(#12454),#2584,.T.) ;
#47673 = ADVANCED_FACE('',(#12455),#2585,.T.) ;
#47674 = ADVANCED_FACE('',(#12456),#2586,.T.) ;
#47675 = ADVANCED_FACE('',(#12457),#10148,.T.) ;
#47676 = ADVANCED_FACE('',(#12458),#10149,.F.) ;
#47677 = ADVANCED_FACE('',(#12459),#2587,.T.) ;
#47678 = ADVANCED_FACE('',(#12460),#2038,.T.) ;
#47679 = ADVANCED_FACE('',(#12461),#10150,.F.) ;
#47680 = ADVANCED_FACE('',(#12462),#2588,.T.) ;
#47681 = ADVANCED_FACE('',(#12463),#10151,.F.) ;
#47682 = ADVANCED_FACE('',(#12464),#2589,.F.) ;
#47683 = ADVANCED_FACE('',(#12465),#45717,.T.) ;
#47684 = ADVANCED_FACE('',(#12466),#10152,.T.) ;
#47685 = ADVANCED_FACE('',(#12467),#10153,.T.) ;
#47686 = ADVANCED_FACE('',(#12468),#2590,.T.) ;
#47687 = ADVANCED_FACE('',(#12469),#45718,.T.) ;
#47688 = ADVANCED_FACE('',(#12470),#10154,.T.) ;
#47689 = ADVANCED_FACE('',(#12471),#10155,.T.) ;
#47690 = ADVANCED_FACE('',(#12472),#45719,.T.) ;
#47691 = ADVANCED_FACE('',(#12473),#45720,.T.) ;
#47692 = ADVANCED_FACE('',(#12474),#10156,.T.) ;
#47693 = ADVANCED_FACE('',(#12475),#45721,.T.) ;
#47694 = ADVANCED_FACE('',(#12476),#10157,.T.) ;
#47695 = ADVANCED_FACE('',(#12477),#45722,.T.) ;
#47696 = ADVANCED_FACE('',(#12478),#10158,.T.) ;
#47697 = ADVANCED_FACE('',(#12479),#2591,.T.) ;
#47698 = ADVANCED_FACE('',(#12480),#10159,.T.) ;
#47699 = ADVANCED_FACE('',(#12481),#2592,.T.) ;
#47700 = ADVANCED_FACE('',(#12482),#10160,.T.) ;
#47701 = ADVANCED_FACE('',(#12483),#2211,.T.) ;
#47702 = ADVANCED_FACE('',(#12484),#10161,.T.) ;
#47703 = ADVANCED_FACE('',(#12485),#45723,.T.) ;
#47704 = ADVANCED_FACE('',(#12486),#10162,.T.) ;
#47705 = ADVANCED_FACE('',(#12487),#45724,.T.) ;
#47706 = ADVANCED_FACE('',(#12488),#45725,.T.) ;
#47707 = ADVANCED_FACE('',(#12489),#10163,.T.) ;
#47708 = ADVANCED_FACE('',(#12490),#45726,.T.) ;
#47709 = ADVANCED_FACE('',(#12491),#10164,.T.) ;
#47710 = ADVANCED_FACE('',(#12492),#10165,.T.) ;
#47711 = ADVANCED_FACE('',(#12493),#45727,.T.) ;
#47712 = ADVANCED_FACE('',(#12494),#2593,.F.) ;
#47713 = ADVANCED_FACE('',(#12495),#10166,.T.) ;
#47714 = ADVANCED_FACE('',(#12496),#2594,.T.) ;
#47715 = ADVANCED_FACE('',(#12497),#10167,.F.) ;
#47716 = ADVANCED_FACE('',(#12498),#2039,.T.) ;
#47717 = ADVANCED_FACE('',(#12499),#10168,.T.) ;
#47718 = ADVANCED_FACE('',(#12500),#10169,.F.) ;
#47719 = ADVANCED_FACE('',(#12501),#2040,.T.) ;
#47720 = ADVANCED_FACE('',(#12502),#2595,.T.) ;
#47721 = ADVANCED_FACE('',(#12503),#45728,.T.) ;
#47722 = ADVANCED_FACE('',(#12504),#10170,.T.) ;
#47723 = ADVANCED_FACE('',(#12505),#45729,.T.) ;
#47724 = ADVANCED_FACE('',(#12506),#10171,.F.) ;
#47725 = ADVANCED_FACE('',(#12507),#2041,.T.) ;
#47726 = ADVANCED_FACE('',(#12508),#2042,.T.) ;
#47727 = ADVANCED_FACE('',(#12509),#10172,.F.) ;
#47728 = ADVANCED_FACE('',(#12510),#2043,.T.) ;
#47729 = ADVANCED_FACE('',(#12511),#45730,.T.) ;
#47730 = ADVANCED_FACE('',(#12512),#10173,.T.) ;
#47731 = ADVANCED_FACE('',(#12513),#45731,.T.) ;
#47732 = ADVANCED_FACE('',(#12514),#10174,.T.) ;
#47733 = ADVANCED_FACE('',(#12515),#45732,.T.) ;
#47734 = ADVANCED_FACE('',(#12516),#10175,.T.) ;
#47735 = ADVANCED_FACE('',(#12517),#45733,.T.) ;
#47736 = ADVANCED_FACE('',(#12518),#10176,.F.) ;
#47737 = ADVANCED_FACE('',(#12519),#2596,.T.) ;
#47738 = ADVANCED_FACE('',(#12520),#10177,.T.) ;
#47739 = ADVANCED_FACE('',(#12521),#2597,.T.) ;
#47740 = ADVANCED_FACE('',(#12522),#10178,.T.) ;
#47741 = ADVANCED_FACE('',(#12523),#10179,.T.) ;
#47742 = ADVANCED_FACE('',(#12524),#2044,.T.) ;
#47743 = ADVANCED_FACE('',(#12525),#2045,.T.) ;
#47744 = ADVANCED_FACE('',(#12526),#10180,.F.) ;
#47745 = ADVANCED_FACE('',(#12527),#2046,.T.) ;
#47746 = ADVANCED_FACE('',(#12528),#2047,.T.) ;
#47747 = ADVANCED_FACE('',(#12529),#2048,.T.) ;
#47748 = ADVANCED_FACE('',(#12530),#10181,.T.) ;
#47749 = ADVANCED_FACE('',(#12531),#2598,.T.) ;
#47750 = ADVANCED_FACE('',(#12532),#2599,.F.) ;
#47751 = ADVANCED_FACE('',(#12533),#10182,.T.) ;
#47752 = ADVANCED_FACE('',(#12534),#10183,.T.) ;
#47753 = ADVANCED_FACE('',(#12535),#45734,.T.) ;
#47754 = ADVANCED_FACE('',(#12536),#10184,.T.) ;
#47755 = ADVANCED_FACE('',(#12537),#10185,.T.) ;
#47756 = ADVANCED_FACE('',(#12538),#10186,.T.) ;
#47757 = ADVANCED_FACE('',(#12539),#2600,.F.) ;
#47758 = ADVANCED_FACE('',(#12540),#2601,.T.) ;
#47759 = ADVANCED_FACE('',(#12541),#2049,.T.) ;
#47760 = ADVANCED_FACE('',(#12542),#45735,.F.) ;
#47761 = ADVANCED_FACE('',(#12543),#10187,.F.) ;
#47762 = ADVANCED_FACE('',(#12544),#2602,.T.) ;
#47763 = ADVANCED_FACE('',(#12545),#10188,.T.) ;
#47764 = ADVANCED_FACE('',(#12546),#10189,.T.) ;
#47765 = ADVANCED_FACE('',(#12547),#2212,.F.) ;
#47766 = ADVANCED_FACE('',(#12548),#10190,.F.) ;
#47767 = ADVANCED_FACE('',(#12549),#10191,.F.) ;
#47768 = ADVANCED_FACE('',(#12550),#45736,.T.) ;
#47769 = ADVANCED_FACE('',(#12551),#10192,.T.) ;
#47770 = ADVANCED_FACE('',(#12552),#10193,.T.) ;
#47771 = ADVANCED_FACE('',(#12553),#10194,.F.) ;
#47772 = ADVANCED_FACE('',(#12554,#741,#742,#743,#744,#745,#746,#747),#2603,
 .F.) ;
#47773 = ADVANCED_FACE('',(#12555),#2604,.T.) ;
#47774 = ADVANCED_FACE('',(#12556),#2050,.F.) ;
#47775 = ADVANCED_FACE('',(#12557),#10195,.T.) ;
#47776 = ADVANCED_FACE('',(#12558),#45737,.F.) ;
#47777 = ADVANCED_FACE('',(#12559),#45738,.T.) ;
#47778 = ADVANCED_FACE('',(#12560),#10196,.T.) ;
#47779 = ADVANCED_FACE('',(#12561),#10197,.T.) ;
#47780 = ADVANCED_FACE('',(#12562),#10198,.F.) ;
#47781 = ADVANCED_FACE('',(#12563),#2605,.T.) ;
#47782 = ADVANCED_FACE('',(#12564),#2606,.T.) ;
#47783 = ADVANCED_FACE('',(#12565),#2213,.T.) ;
#47784 = ADVANCED_FACE('',(#12566),#10199,.T.) ;
#47785 = ADVANCED_FACE('',(#12567),#45739,.T.) ;
#47786 = ADVANCED_FACE('',(#12568),#10200,.T.) ;
#47787 = ADVANCED_FACE('',(#12569),#45740,.T.) ;
#47788 = ADVANCED_FACE('',(#12570),#10201,.T.) ;
#47789 = ADVANCED_FACE('',(#12571),#10202,.T.) ;
#47790 = ADVANCED_FACE('',(#12572),#45741,.T.) ;
#47791 = ADVANCED_FACE('',(#12573),#10203,.T.) ;
#47792 = ADVANCED_FACE('',(#12574),#2051,.F.) ;
#47793 = ADVANCED_FACE('',(#12575),#45742,.T.) ;
#47794 = ADVANCED_FACE('',(#12576),#99,.F.) ;
#47795 = ADVANCED_FACE('',(#12577),#10204,.T.) ;
#47796 = ADVANCED_FACE('',(#12578),#45743,.T.) ;
#47797 = ADVANCED_FACE('',(#12579),#10205,.T.) ;
#47798 = ADVANCED_FACE('',(#12580),#10206,.T.) ;
#47799 = ADVANCED_FACE('',(#12581),#10207,.F.) ;
#47800 = ADVANCED_FACE('',(#12582),#45744,.F.) ;
#47801 = ADVANCED_FACE('',(#12583),#10208,.F.) ;
#47802 = ADVANCED_FACE('',(#12584),#100,.T.) ;
#47803 = ADVANCED_FACE('',(#12585),#2607,.F.) ;
#47804 = ADVANCED_FACE('',(#12586),#2608,.T.) ;
#47805 = ADVANCED_FACE('',(#12587),#10209,.F.) ;
#47806 = ADVANCED_FACE('',(#12588),#2609,.T.) ;
#47807 = ADVANCED_FACE('',(#12589),#10210,.T.) ;
#47808 = ADVANCED_FACE('',(#12590),#2610,.T.) ;
#47809 = ADVANCED_FACE('',(#12591),#10211,.T.) ;
#47810 = ADVANCED_FACE('',(#12592),#2611,.T.) ;
#47811 = ADVANCED_FACE('',(#12593),#10212,.T.) ;
#47812 = ADVANCED_FACE('',(#12594),#10213,.F.) ;
#47813 = ADVANCED_FACE('',(#12595),#2052,.F.) ;
#47814 = ADVANCED_FACE('',(#12596),#10214,.F.) ;
#47815 = ADVANCED_FACE('',(#12597),#45745,.T.) ;
#47816 = ADVANCED_FACE('',(#12598),#10215,.T.) ;
#47817 = ADVANCED_FACE('',(#12599),#45746,.T.) ;
#47818 = ADVANCED_FACE('',(#12600),#45747,.T.) ;
#47819 = ADVANCED_FACE('',(#12601),#2053,.F.) ;
#47820 = ADVANCED_FACE('',(#12602),#45748,.T.) ;
#47821 = ADVANCED_FACE('',(#12603),#10216,.T.) ;
#47822 = ADVANCED_FACE('',(#12604),#10217,.T.) ;
#47823 = ADVANCED_FACE('',(#12605),#2054,.F.) ;
#47824 = ADVANCED_FACE('',(#12606),#2055,.F.) ;
#47825 = ADVANCED_FACE('',(#12607),#10218,.T.) ;
#47826 = ADVANCED_FACE('',(#12608),#10219,.F.) ;
#47827 = ADVANCED_FACE('',(#12609),#45749,.T.) ;
#47828 = ADVANCED_FACE('',(#12610),#10220,.T.) ;
#47829 = ADVANCED_FACE('',(#12611),#45750,.T.) ;
#47830 = ADVANCED_FACE('',(#12612),#10221,.T.) ;
#47831 = ADVANCED_FACE('',(#12613),#10222,.F.) ;
#47832 = ADVANCED_FACE('',(#12614),#10223,.T.) ;
#47833 = ADVANCED_FACE('',(#12615),#45751,.T.) ;
#47834 = ADVANCED_FACE('',(#12616),#10224,.T.) ;
#47835 = ADVANCED_FACE('',(#12617),#45752,.T.) ;
#47836 = ADVANCED_FACE('',(#12618),#10225,.T.) ;
#47837 = ADVANCED_FACE('',(#12619),#45753,.T.) ;
#47838 = ADVANCED_FACE('',(#12620),#10226,.T.) ;
#47839 = ADVANCED_FACE('',(#12621),#45754,.T.) ;
#47840 = ADVANCED_FACE('',(#12622),#10227,.T.) ;
#47841 = ADVANCED_FACE('',(#12623),#10228,.T.) ;
#47842 = ADVANCED_FACE('',(#12624),#2056,.F.) ;
#47843 = ADVANCED_FACE('',(#12625),#2057,.F.) ;
#47844 = ADVANCED_FACE('',(#12626),#10229,.F.) ;
#47845 = ADVANCED_FACE('',(#12627),#10230,.F.) ;
#47846 = ADVANCED_FACE('',(#12628),#10231,.F.) ;
#47847 = ADVANCED_FACE('',(#12629),#10232,.T.) ;
#47848 = ADVANCED_FACE('',(#12630),#10233,.F.) ;
#47849 = ADVANCED_FACE('',(#12631),#2612,.T.) ;
#47850 = ADVANCED_FACE('',(#12632),#10234,.F.) ;
#47851 = ADVANCED_FACE('',(#12633),#10235,.T.) ;
#47852 = ADVANCED_FACE('',(#12634),#2613,.T.) ;
#47853 = ADVANCED_FACE('',(#12635),#2614,.F.) ;
#47854 = ADVANCED_FACE('',(#12636),#2615,.T.) ;
#47855 = ADVANCED_FACE('',(#12637),#2616,.F.) ;
#47856 = ADVANCED_FACE('',(#12638),#2617,.F.) ;
#47857 = ADVANCED_FACE('',(#12639),#10236,.T.) ;
#47858 = ADVANCED_FACE('',(#12640),#2618,.T.) ;
#47859 = ADVANCED_FACE('',(#12641),#10237,.T.) ;
#47860 = ADVANCED_FACE('',(#12642),#45755,.T.) ;
#47861 = ADVANCED_FACE('',(#12643),#45756,.T.) ;
#47862 = ADVANCED_FACE('',(#12644),#10238,.T.) ;
#47863 = ADVANCED_FACE('',(#12645),#10239,.T.) ;
#47864 = ADVANCED_FACE('',(#12646),#45757,.T.) ;
#47865 = ADVANCED_FACE('',(#12647),#10240,.T.) ;
#47866 = ADVANCED_FACE('',(#12648),#10241,.F.) ;
#47867 = ADVANCED_FACE('',(#12649),#10242,.F.) ;
#47868 = ADVANCED_FACE('',(#12650),#10243,.T.) ;
#47869 = ADVANCED_FACE('',(#12651),#45758,.T.) ;
#47870 = ADVANCED_FACE('',(#12652),#10244,.T.) ;
#47871 = ADVANCED_FACE('',(#12653),#10245,.T.) ;
#47872 = ADVANCED_FACE('',(#12654),#2619,.T.) ;
#47873 = ADVANCED_FACE('',(#12655),#10246,.T.) ;
#47874 = ADVANCED_FACE('',(#12656),#2620,.T.) ;
#47875 = ADVANCED_FACE('',(#12657),#10247,.T.) ;
#47876 = ADVANCED_FACE('',(#12658),#2058,.F.) ;
#47877 = ADVANCED_FACE('',(#12659),#10248,.T.) ;
#47878 = ADVANCED_FACE('',(#12660),#45759,.T.) ;
#47879 = ADVANCED_FACE('',(#12661),#10249,.T.) ;
#47880 = ADVANCED_FACE('',(#12662),#45760,.T.) ;
#47881 = ADVANCED_FACE('',(#12663),#10250,.T.) ;
#47882 = ADVANCED_FACE('',(#12664),#45761,.T.) ;
#47883 = ADVANCED_FACE('',(#12665),#10251,.T.) ;
#47884 = ADVANCED_FACE('',(#12666),#45762,.T.) ;
#47885 = ADVANCED_FACE('',(#12667),#10252,.T.) ;
#47886 = ADVANCED_FACE('',(#12668),#45763,.T.) ;
#47887 = ADVANCED_FACE('',(#12669),#10253,.T.) ;
#47888 = ADVANCED_FACE('',(#12670),#2059,.F.) ;
#47889 = ADVANCED_FACE('',(#12671),#10254,.T.) ;
#47890 = ADVANCED_FACE('',(#12672),#2060,.F.) ;
#47891 = ADVANCED_FACE('',(#12673),#2061,.F.) ;
#47892 = ADVANCED_FACE('',(#12674),#2062,.F.) ;
#47893 = ADVANCED_FACE('',(#12675),#45764,.T.) ;
#47894 = ADVANCED_FACE('',(#12676),#10255,.T.) ;
#47895 = ADVANCED_FACE('',(#12677),#45765,.T.) ;
#47896 = ADVANCED_FACE('',(#12678),#10256,.T.) ;
#47897 = ADVANCED_FACE('',(#12679),#45766,.T.) ;
#47898 = ADVANCED_FACE('',(#12680),#45767,.T.) ;
#47899 = ADVANCED_FACE('',(#12681),#10257,.T.) ;
#47900 = ADVANCED_FACE('',(#12682),#45768,.T.) ;
#47901 = ADVANCED_FACE('',(#12683),#10258,.T.) ;
#47902 = ADVANCED_FACE('',(#12684),#45769,.T.) ;
#47903 = ADVANCED_FACE('',(#12685),#2621,.T.) ;
#47904 = ADVANCED_FACE('',(#12686),#10259,.T.) ;
#47905 = ADVANCED_FACE('',(#12687),#2622,.T.) ;
#47906 = ADVANCED_FACE('',(#12688),#10260,.T.) ;
#47907 = ADVANCED_FACE('',(#12689),#10261,.F.) ;
#47908 = ADVANCED_FACE('',(#12690),#2623,.T.) ;
#47909 = ADVANCED_FACE('',(#12691),#10262,.T.) ;
#47910 = ADVANCED_FACE('',(#12692),#10263,.T.) ;
#47911 = ADVANCED_FACE('',(#12693),#10264,.T.) ;
#47912 = ADVANCED_FACE('',(#12694),#10265,.T.) ;
#47913 = ADVANCED_FACE('',(#12695),#45770,.T.) ;
#47914 = ADVANCED_FACE('',(#12696),#10266,.T.) ;
#47915 = ADVANCED_FACE('',(#12697),#45771,.T.) ;
#47916 = ADVANCED_FACE('',(#12698),#10267,.T.) ;
#47917 = ADVANCED_FACE('',(#12699),#45772,.T.) ;
#47918 = ADVANCED_FACE('',(#12700),#10268,.T.) ;
#47919 = ADVANCED_FACE('',(#12701),#45773,.T.) ;
#47920 = ADVANCED_FACE('',(#12702),#10269,.T.) ;
#47921 = ADVANCED_FACE('',(#12703),#45774,.T.) ;
#47922 = ADVANCED_FACE('',(#12704),#10270,.T.) ;
#47923 = ADVANCED_FACE('',(#12705),#10271,.T.) ;
#47924 = ADVANCED_FACE('',(#12706),#45775,.T.) ;
#47925 = ADVANCED_FACE('',(#12707),#10272,.T.) ;
#47926 = ADVANCED_FACE('',(#12708),#45776,.T.) ;
#47927 = ADVANCED_FACE('',(#12709),#10273,.T.) ;
#47928 = ADVANCED_FACE('',(#12710),#45777,.T.) ;
#47929 = ADVANCED_FACE('',(#12711),#10274,.T.) ;
#47930 = ADVANCED_FACE('',(#12712),#2624,.F.) ;
#47931 = ADVANCED_FACE('',(#12713),#2625,.T.) ;
#47932 = ADVANCED_FACE('',(#12714),#10275,.T.) ;
#47933 = ADVANCED_FACE('',(#12715,#748,#749),#2626,.T.) ;
#47934 = ADVANCED_FACE('',(#12716),#10276,.T.) ;
#47935 = ADVANCED_FACE('',(#12717),#2627,.T.) ;
#47936 = ADVANCED_FACE('',(#12718,#750),#2628,.T.) ;
#47937 = ADVANCED_FACE('',(#12719),#10277,.T.) ;
#47938 = ADVANCED_FACE('',(#12720),#2629,.F.) ;
#47939 = ADVANCED_FACE('',(#12721),#2630,.T.) ;
#47940 = ADVANCED_FACE('',(#12722),#2063,.F.) ;
#47941 = ADVANCED_FACE('',(#12723),#2064,.F.) ;
#47942 = ADVANCED_FACE('',(#12724),#10278,.T.) ;
#47943 = ADVANCED_FACE('',(#12725),#2065,.F.) ;
#47944 = ADVANCED_FACE('',(#12726),#45778,.T.) ;
#47945 = ADVANCED_FACE('',(#12727),#10279,.T.) ;
#47946 = ADVANCED_FACE('',(#12728),#10280,.F.) ;
#47947 = ADVANCED_FACE('',(#12729),#10281,.T.) ;
#47948 = ADVANCED_FACE('',(#12730),#10282,.F.) ;
#47949 = ADVANCED_FACE('',(#12731),#10283,.T.) ;
#47950 = ADVANCED_FACE('',(#12732),#2066,.F.) ;
#47951 = ADVANCED_FACE('',(#12733),#2067,.F.) ;
#47952 = ADVANCED_FACE('',(#12734),#10284,.T.) ;
#47953 = ADVANCED_FACE('',(#12735),#2631,.F.) ;
#47954 = ADVANCED_FACE('',(#12736),#10285,.T.) ;
#47955 = ADVANCED_FACE('',(#12737),#2632,.T.) ;
#47956 = ADVANCED_FACE('',(#12738),#10286,.F.) ;
#47957 = ADVANCED_FACE('',(#12739),#10287,.T.) ;
#47958 = ADVANCED_FACE('',(#12740),#10288,.T.) ;
#47959 = ADVANCED_FACE('',(#12741),#2633,.F.) ;
#47960 = ADVANCED_FACE('',(#12742),#2634,.T.) ;
#47961 = ADVANCED_FACE('',(#12743),#2635,.F.) ;
#47962 = ADVANCED_FACE('',(#12744),#2068,.F.) ;
#47963 = ADVANCED_FACE('',(#12745),#10289,.T.) ;
#47964 = ADVANCED_FACE('',(#12746),#2069,.F.) ;
#47965 = ADVANCED_FACE('',(#12747),#2070,.F.) ;
#47966 = ADVANCED_FACE('',(#12748),#2071,.F.) ;
#47967 = ADVANCED_FACE('',(#12749),#2072,.F.) ;
#47968 = ADVANCED_FACE('',(#12750),#10290,.F.) ;
#47969 = ADVANCED_FACE('',(#12751),#10291,.F.) ;
#47970 = ADVANCED_FACE('',(#12752),#2073,.F.) ;
#47971 = ADVANCED_FACE('',(#12753),#10292,.T.) ;
#47972 = ADVANCED_FACE('',(#12754),#2074,.F.) ;
#47973 = ADVANCED_FACE('',(#12755),#2075,.F.) ;
#47974 = ADVANCED_FACE('',(#12756,#751,#752,#753),#2636,.T.) ;
#47975 = ADVANCED_FACE('',(#12757),#10293,.T.) ;
#47976 = ADVANCED_FACE('',(#12758),#2637,.T.) ;
#47977 = ADVANCED_FACE('',(#12759),#10294,.T.) ;
#47978 = ADVANCED_FACE('',(#12760),#2076,.F.) ;
#47979 = ADVANCED_FACE('',(#12761),#2077,.T.) ;
#47980 = ADVANCED_FACE('',(#12762),#10295,.F.) ;
#47981 = ADVANCED_FACE('',(#12763),#10296,.T.) ;
#47982 = ADVANCED_FACE('',(#12764),#2638,.T.) ;
#47983 = ADVANCED_FACE('',(#12765),#2078,.F.) ;
#47984 = ADVANCED_FACE('',(#12766),#2079,.F.) ;
#47985 = ADVANCED_FACE('',(#12767),#10297,.T.) ;
#47986 = ADVANCED_FACE('',(#12768),#2639,.T.) ;
#47987 = ADVANCED_FACE('',(#12769),#2640,.F.) ;
#47988 = ADVANCED_FACE('',(#12770),#2641,.T.) ;
#47989 = ADVANCED_FACE('',(#12771),#10298,.T.) ;
#47990 = ADVANCED_FACE('',(#12772),#10299,.F.) ;
#47991 = ADVANCED_FACE('',(#12773),#2642,.T.) ;
#47992 = ADVANCED_FACE('',(#12774),#10300,.F.) ;
#47993 = ADVANCED_FACE('',(#12775),#2643,.F.) ;
#47994 = ADVANCED_FACE('',(#12776),#10301,.T.) ;
#47995 = ADVANCED_FACE('',(#12777),#2644,.F.) ;
#47996 = ADVANCED_FACE('',(#12778),#10302,.F.) ;
#47997 = ADVANCED_FACE('',(#12779),#2645,.F.) ;
#47998 = ADVANCED_FACE('',(#12780),#2080,.F.) ;
#47999 = ADVANCED_FACE('',(#12781),#10303,.F.) ;
#48000 = ADVANCED_FACE('',(#12782),#10304,.F.) ;
#48001 = ADVANCED_FACE('',(#12783),#2646,.T.) ;
#48002 = ADVANCED_FACE('',(#12784),#2647,.T.) ;
#48003 = ADVANCED_FACE('',(#12785),#2648,.T.) ;
#48004 = ADVANCED_FACE('',(#12786,#754),#2649,.F.) ;
#48005 = ADVANCED_FACE('',(#12787),#45779,.T.) ;
#48006 = ADVANCED_FACE('',(#12788),#10305,.T.) ;
#48007 = ADVANCED_FACE('',(#12789),#45780,.T.) ;
#48008 = ADVANCED_FACE('',(#12790),#10306,.T.) ;
#48009 = ADVANCED_FACE('',(#12791),#2650,.T.) ;
#48010 = ADVANCED_FACE('',(#12792),#2651,.T.) ;
#48011 = ADVANCED_FACE('',(#12793),#2652,.T.) ;
#48012 = ADVANCED_FACE('',(#12794),#2653,.T.) ;
#48013 = ADVANCED_FACE('',(#12795,#755),#2654,.F.) ;
#48014 = ADVANCED_FACE('',(#12796),#2655,.F.) ;
#48015 = ADVANCED_FACE('',(#12797,#756),#2656,.F.) ;
#48016 = ADVANCED_FACE('',(#12798),#2657,.F.) ;
#48017 = ADVANCED_FACE('',(#12799),#10307,.F.) ;
#48018 = ADVANCED_FACE('',(#12800),#2081,.T.) ;
#48019 = ADVANCED_FACE('',(#12801),#10308,.F.) ;
#48020 = ADVANCED_FACE('',(#12802),#2082,.T.) ;
#48021 = ADVANCED_FACE('',(#12803),#10309,.F.) ;
#48022 = ADVANCED_FACE('',(#12804),#10310,.F.) ;
#48023 = ADVANCED_FACE('',(#12805),#10311,.F.) ;
#48024 = ADVANCED_FACE('',(#12806),#2658,.F.) ;
#48025 = ADVANCED_FACE('',(#12807),#2659,.F.) ;
#48026 = ADVANCED_FACE('',(#12808),#2660,.F.) ;
#48027 = ADVANCED_FACE('',(#12809),#2661,.F.) ;
#48028 = ADVANCED_FACE('',(#12810),#2662,.T.) ;
#48029 = ADVANCED_FACE('',(#12811),#2083,.T.) ;
#48030 = ADVANCED_FACE('',(#12812),#10312,.F.) ;
#48031 = ADVANCED_FACE('',(#12813),#10313,.F.) ;
#48032 = ADVANCED_FACE('',(#12814),#10314,.F.) ;
#48033 = ADVANCED_FACE('',(#12815),#10315,.F.) ;
#48034 = ADVANCED_FACE('',(#12816),#2084,.T.) ;
#48035 = ADVANCED_FACE('',(#12817),#10316,.F.) ;
#48036 = ADVANCED_FACE('',(#12818),#2663,.F.) ;
#48037 = ADVANCED_FACE('',(#12819),#2085,.F.) ;
#48038 = ADVANCED_FACE('',(#12820),#2664,.F.) ;
#48039 = ADVANCED_FACE('',(#12821),#2086,.F.) ;
#48040 = ADVANCED_FACE('',(#12822),#2665,.T.) ;
#48041 = ADVANCED_FACE('',(#12823),#10317,.F.) ;
#48042 = ADVANCED_FACE('',(#12824),#10318,.F.) ;
#48043 = ADVANCED_FACE('',(#12825),#10319,.F.) ;
#48044 = ADVANCED_FACE('',(#12826),#10320,.F.) ;
#48045 = ADVANCED_FACE('',(#12827),#10321,.F.) ;
#48046 = ADVANCED_FACE('',(#12828),#10322,.F.) ;
#48047 = ADVANCED_FACE('',(#12829),#10323,.F.) ;
#48048 = ADVANCED_FACE('',(#12830),#2666,.F.) ;
#48049 = ADVANCED_FACE('',(#12831),#2667,.F.) ;
#48050 = ADVANCED_FACE('',(#12832),#2668,.F.) ;
#48051 = ADVANCED_FACE('',(#12833),#2669,.F.) ;
#48052 = ADVANCED_FACE('',(#12834),#2670,.F.) ;
#48053 = ADVANCED_FACE('',(#12835),#10324,.F.) ;
#48054 = ADVANCED_FACE('',(#12836),#10325,.F.) ;
#48055 = ADVANCED_FACE('',(#12837),#10326,.F.) ;
#48056 = ADVANCED_FACE('',(#12838),#10327,.F.) ;
#48057 = ADVANCED_FACE('',(#12839),#2671,.F.) ;
#48058 = ADVANCED_FACE('',(#12840),#2672,.F.) ;
#48059 = ADVANCED_FACE('',(#12841),#2673,.F.) ;
#48060 = ADVANCED_FACE('',(#12842),#10328,.F.) ;
#48061 = ADVANCED_FACE('',(#12843),#10329,.F.) ;
#48062 = ADVANCED_FACE('',(#12844),#10330,.F.) ;
#48063 = ADVANCED_FACE('',(#12845),#10331,.F.) ;
#48064 = ADVANCED_FACE('',(#12846),#10332,.F.) ;
#48065 = ADVANCED_FACE('',(#12847),#10333,.F.) ;
#48066 = ADVANCED_FACE('',(#12848),#10334,.F.) ;
#48067 = ADVANCED_FACE('',(#12849),#2674,.F.) ;
#48068 = ADVANCED_FACE('',(#12850),#2675,.F.) ;
#48069 = ADVANCED_FACE('',(#12851),#2676,.F.) ;
#48070 = ADVANCED_FACE('',(#12852),#2677,.F.) ;
#48071 = ADVANCED_FACE('',(#12853),#2678,.F.) ;
#48072 = ADVANCED_FACE('',(#12854),#10335,.F.) ;
#48073 = ADVANCED_FACE('',(#12855),#10336,.F.) ;
#48074 = ADVANCED_FACE('',(#12856),#10337,.F.) ;
#48075 = ADVANCED_FACE('',(#12857),#10338,.F.) ;
#48076 = ADVANCED_FACE('',(#12858),#2679,.F.) ;
#48077 = ADVANCED_FACE('',(#12859),#2680,.F.) ;
#48078 = ADVANCED_FACE('',(#12860),#2681,.F.) ;
#48079 = ADVANCED_FACE('',(#12861),#10339,.F.) ;
#48080 = ADVANCED_FACE('',(#12862),#10340,.F.) ;
#48081 = ADVANCED_FACE('',(#12863),#10341,.F.) ;
#48082 = ADVANCED_FACE('',(#12864),#45781,.F.) ;
#48083 = ADVANCED_FACE('',(#12865),#10342,.F.) ;
#48084 = ADVANCED_FACE('',(#12866),#10343,.F.) ;
#48085 = ADVANCED_FACE('',(#12867),#10344,.F.) ;
#48086 = ADVANCED_FACE('',(#12868),#45782,.F.) ;
#48087 = ADVANCED_FACE('',(#12869),#10345,.F.) ;
#48088 = ADVANCED_FACE('',(#12870),#10346,.F.) ;
#48089 = ADVANCED_FACE('',(#12871),#10347,.F.) ;
#48090 = ADVANCED_FACE('',(#12872),#2682,.F.) ;
#48091 = ADVANCED_FACE('',(#12873),#10348,.T.) ;
#48092 = ADVANCED_FACE('',(#12874),#2683,.F.) ;
#48093 = ADVANCED_FACE('',(#12875),#2684,.F.) ;
#48094 = ADVANCED_FACE('',(#12876),#2685,.F.) ;
#48095 = ADVANCED_FACE('',(#12877),#2686,.F.) ;
#48096 = ADVANCED_FACE('',(#12878),#2687,.T.) ;
#48097 = ADVANCED_FACE('',(#12879),#10349,.F.) ;
#48098 = ADVANCED_FACE('',(#12880),#10350,.F.) ;
#48099 = ADVANCED_FACE('',(#12881),#45783,.F.) ;
#48100 = ADVANCED_FACE('',(#12882),#10351,.F.) ;
#48101 = ADVANCED_FACE('',(#12883),#10352,.F.) ;
#48102 = ADVANCED_FACE('',(#12884),#10353,.F.) ;
#48103 = ADVANCED_FACE('',(#12885),#45784,.F.) ;
#48104 = ADVANCED_FACE('',(#12886),#10354,.F.) ;
#48105 = ADVANCED_FACE('',(#12887),#10355,.F.) ;
#48106 = ADVANCED_FACE('',(#12888),#10356,.F.) ;
#48107 = ADVANCED_FACE('',(#12889),#10357,.F.) ;
#48108 = ADVANCED_FACE('',(#12890),#10358,.T.) ;
#48109 = ADVANCED_FACE('',(#12891),#2688,.F.) ;
#48110 = ADVANCED_FACE('',(#12892),#2689,.F.) ;
#48111 = ADVANCED_FACE('',(#12893),#2690,.F.) ;
#48112 = ADVANCED_FACE('',(#12894),#2691,.F.) ;
#48113 = ADVANCED_FACE('',(#12895),#2692,.F.) ;
#48114 = ADVANCED_FACE('',(#12896),#2693,.T.) ;
#48115 = ADVANCED_FACE('',(#12897),#2087,.F.) ;
#48116 = ADVANCED_FACE('',(#12898),#10359,.T.) ;
#48117 = ADVANCED_FACE('',(#12899),#10360,.T.) ;
#48118 = ADVANCED_FACE('',(#12900),#10361,.T.) ;
#48119 = ADVANCED_FACE('',(#12901),#10362,.T.) ;
#48120 = ADVANCED_FACE('',(#12902),#10363,.T.) ;
#48121 = ADVANCED_FACE('',(#12903),#2088,.F.) ;
#48122 = ADVANCED_FACE('',(#12904),#2089,.F.) ;
#48123 = ADVANCED_FACE('',(#12905),#2694,.F.) ;
#48124 = ADVANCED_FACE('',(#12906),#2090,.F.) ;
#48125 = ADVANCED_FACE('',(#12907),#2091,.F.) ;
#48126 = ADVANCED_FACE('',(#12908),#10364,.T.) ;
#48127 = ADVANCED_FACE('',(#12909),#10365,.T.) ;
#48128 = ADVANCED_FACE('',(#12910),#10366,.T.) ;
#48129 = ADVANCED_FACE('',(#12911),#10367,.T.) ;
#48130 = ADVANCED_FACE('',(#12912),#2092,.F.) ;
#48131 = ADVANCED_FACE('',(#12913),#10368,.T.) ;
#48132 = ADVANCED_FACE('',(#12914),#2695,.F.) ;
#48133 = ADVANCED_FACE('',(#12915),#2696,.F.) ;
#48134 = ADVANCED_FACE('',(#12916),#10369,.T.) ;
#48135 = ADVANCED_FACE('',(#12917),#10370,.T.) ;
#48136 = ADVANCED_FACE('',(#12918),#10371,.T.) ;
#48137 = ADVANCED_FACE('',(#12919),#10372,.T.) ;
#48138 = ADVANCED_FACE('',(#12920),#10373,.T.) ;
#48139 = ADVANCED_FACE('',(#12921),#10374,.T.) ;
#48140 = ADVANCED_FACE('',(#12922),#10375,.T.) ;
#48141 = ADVANCED_FACE('',(#12923),#2697,.F.) ;
#48142 = ADVANCED_FACE('',(#12924),#2698,.F.) ;
#48143 = ADVANCED_FACE('',(#12925),#2699,.F.) ;
#48144 = ADVANCED_FACE('',(#12926,#757,#758,#759),#2700,.T.) ;
#48145 = ADVANCED_FACE('',(#12927),#10376,.T.) ;
#48146 = ADVANCED_FACE('',(#12928),#10377,.T.) ;
#48147 = ADVANCED_FACE('',(#12929),#10378,.T.) ;
#48148 = ADVANCED_FACE('',(#12930),#10379,.T.) ;
#48149 = ADVANCED_FACE('',(#12931),#2701,.F.) ;
#48150 = ADVANCED_FACE('',(#12932),#10380,.T.) ;
#48151 = ADVANCED_FACE('',(#12933),#10381,.T.) ;
#48152 = ADVANCED_FACE('',(#12934),#10382,.T.) ;
#48153 = ADVANCED_FACE('',(#12935),#10383,.T.) ;
#48154 = ADVANCED_FACE('',(#12936),#10384,.T.) ;
#48155 = ADVANCED_FACE('',(#12937),#10385,.T.) ;
#48156 = ADVANCED_FACE('',(#12938),#10386,.T.) ;
#48157 = ADVANCED_FACE('',(#12939),#2702,.F.) ;
#48158 = ADVANCED_FACE('',(#12940),#2703,.F.) ;
#48159 = ADVANCED_FACE('',(#12941),#10387,.T.) ;
#48160 = ADVANCED_FACE('',(#12942),#10388,.T.) ;
#48161 = ADVANCED_FACE('',(#12943),#10389,.T.) ;
#48162 = ADVANCED_FACE('',(#12944),#10390,.T.) ;
#48163 = ADVANCED_FACE('',(#12945),#10391,.T.) ;
#48164 = ADVANCED_FACE('',(#12946),#10392,.T.) ;
#48165 = ADVANCED_FACE('',(#12947),#10393,.T.) ;
#48166 = ADVANCED_FACE('',(#12948),#10394,.T.) ;
#48167 = ADVANCED_FACE('',(#12949),#10395,.T.) ;
#48168 = ADVANCED_FACE('',(#12950),#10396,.T.) ;
#48169 = ADVANCED_FACE('',(#12951),#45785,.T.) ;
#48170 = ADVANCED_FACE('',(#12952),#10397,.T.) ;
#48171 = ADVANCED_FACE('',(#12953),#45786,.T.) ;
#48172 = ADVANCED_FACE('',(#12954),#10398,.T.) ;
#48173 = ADVANCED_FACE('',(#12955),#2704,.F.) ;
#48174 = ADVANCED_FACE('',(#12956),#10399,.F.) ;
#48175 = ADVANCED_FACE('',(#12957),#2705,.F.) ;
#48176 = ADVANCED_FACE('',(#12958),#2706,.F.) ;
#48177 = ADVANCED_FACE('',(#12959),#10400,.T.) ;
#48178 = ADVANCED_FACE('',(#12960),#10401,.T.) ;
#48179 = ADVANCED_FACE('',(#12961),#10402,.T.) ;
#48180 = ADVANCED_FACE('',(#12962),#10403,.T.) ;
#48181 = ADVANCED_FACE('',(#12963),#10404,.T.) ;
#48182 = ADVANCED_FACE('',(#12964),#10405,.T.) ;
#48183 = ADVANCED_FACE('',(#12965),#45787,.T.) ;
#48184 = ADVANCED_FACE('',(#12966),#10406,.T.) ;
#48185 = ADVANCED_FACE('',(#12967),#10407,.T.) ;
#48186 = ADVANCED_FACE('',(#12968),#45788,.T.) ;
#48187 = ADVANCED_FACE('',(#12969),#10408,.T.) ;
#48188 = ADVANCED_FACE('',(#12970),#2707,.F.) ;
#48189 = ADVANCED_FACE('',(#12971),#2708,.F.) ;
#48190 = ADVANCED_FACE('',(#12972),#2709,.F.) ;
#48191 = ADVANCED_FACE('',(#12973),#10409,.F.) ;
#48192 = ADVANCED_FACE('',(#12974),#2710,.F.) ;
#48193 = ADVANCED_FACE('',(#12975),#2711,.F.) ;
#48194 = ADVANCED_FACE('',(#12976),#2712,.F.) ;
#48195 = ADVANCED_FACE('',(#12977),#2713,.F.) ;
#48196 = ADVANCED_FACE('',(#12978),#2714,.F.) ;
#48197 = ADVANCED_FACE('',(#12979),#2715,.F.) ;
#48198 = ADVANCED_FACE('',(#12980),#2716,.F.) ;
#48199 = ADVANCED_FACE('',(#12981),#2717,.F.) ;
#48200 = ADVANCED_FACE('',(#12982),#2718,.T.) ;
#48201 = ADVANCED_FACE('',(#12983),#2719,.T.) ;
#48202 = ADVANCED_FACE('',(#12984),#10410,.F.) ;
#48203 = ADVANCED_FACE('',(#12985),#2720,.T.) ;
#48204 = ADVANCED_FACE('',(#12986),#10411,.T.) ;
#48205 = ADVANCED_FACE('',(#12987),#2721,.T.) ;
#48206 = ADVANCED_FACE('',(#12988),#2722,.T.) ;
#48207 = ADVANCED_FACE('',(#12989),#2723,.T.) ;
#48208 = ADVANCED_FACE('',(#12990),#2724,.F.) ;
#48209 = ADVANCED_FACE('',(#12991),#10412,.T.) ;
#48210 = ADVANCED_FACE('',(#12992),#2725,.T.) ;
#48211 = ADVANCED_FACE('',(#12993),#2726,.T.) ;
#48212 = ADVANCED_FACE('',(#12994),#2727,.T.) ;
#48213 = ADVANCED_FACE('',(#12995),#2728,.T.) ;
#48214 = ADVANCED_FACE('',(#12996),#2729,.F.) ;
#48215 = ADVANCED_FACE('',(#12997),#2730,.F.) ;
#48216 = ADVANCED_FACE('',(#12998),#2731,.F.) ;
#48217 = ADVANCED_FACE('',(#12999),#2732,.T.) ;
#48218 = ADVANCED_FACE('',(#13000),#2733,.T.) ;
#48219 = ADVANCED_FACE('',(#13001),#10413,.T.) ;
#48220 = ADVANCED_FACE('',(#13002),#2734,.T.) ;
#48221 = ADVANCED_FACE('',(#13003),#2735,.T.) ;
#48222 = ADVANCED_FACE('',(#13004),#2736,.F.) ;
#48223 = ADVANCED_FACE('',(#13005),#10414,.F.) ;
#48224 = ADVANCED_FACE('',(#13006),#2737,.T.) ;
#48225 = ADVANCED_FACE('',(#13007),#2738,.T.) ;
#48226 = ADVANCED_FACE('',(#13008),#2739,.T.) ;
#48227 = ADVANCED_FACE('',(#13009),#2740,.T.) ;
#48228 = ADVANCED_FACE('',(#13010),#2741,.T.) ;
#48229 = ADVANCED_FACE('',(#13011),#10415,.T.) ;
#48230 = ADVANCED_FACE('',(#13012),#2742,.F.) ;
#48231 = ADVANCED_FACE('',(#13013),#10416,.T.) ;
#48232 = ADVANCED_FACE('',(#13014),#2743,.T.) ;
#48233 = ADVANCED_FACE('',(#13015),#2744,.F.) ;
#48234 = ADVANCED_FACE('',(#13016),#2745,.F.) ;
#48235 = ADVANCED_FACE('',(#13017),#2746,.F.) ;
#48236 = ADVANCED_FACE('',(#13018),#2747,.T.) ;
#48237 = ADVANCED_FACE('',(#13019),#10417,.T.) ;
#48238 = ADVANCED_FACE('',(#13020),#2214,.T.) ;
#48239 = ADVANCED_FACE('',(#13021),#45789,.T.) ;
#48240 = ADVANCED_FACE('',(#13022),#2093,.T.) ;
#48241 = ADVANCED_FACE('',(#13023),#10418,.T.) ;
#48242 = ADVANCED_FACE('',(#13024),#2094,.F.) ;
#48243 = ADVANCED_FACE('',(#13025),#45790,.T.) ;
#48244 = ADVANCED_FACE('',(#13026),#10419,.T.) ;
#48245 = ADVANCED_FACE('',(#13027),#10420,.F.) ;
#48246 = ADVANCED_FACE('',(#13028),#2215,.T.) ;
#48247 = ADVANCED_FACE('',(#13029),#2095,.F.) ;
#48248 = ADVANCED_FACE('',(#13030),#10421,.T.) ;
#48249 = ADVANCED_FACE('',(#13031),#45791,.T.) ;
#48250 = ADVANCED_FACE('',(#13032),#2096,.F.) ;
#48251 = ADVANCED_FACE('',(#13033),#10422,.T.) ;
#48252 = ADVANCED_FACE('',(#13034),#45792,.T.) ;
#48253 = ADVANCED_FACE('',(#13035),#2097,.F.) ;
#48254 = ADVANCED_FACE('',(#13036),#2098,.F.) ;
#48255 = ADVANCED_FACE('',(#13037),#45793,.T.) ;
#48256 = ADVANCED_FACE('',(#13038),#10423,.T.) ;
#48257 = ADVANCED_FACE('',(#13039),#2099,.F.) ;
#48258 = ADVANCED_FACE('',(#13040),#10424,.T.) ;
#48259 = ADVANCED_FACE('',(#13041),#45794,.T.) ;
#48260 = ADVANCED_FACE('',(#13042),#2100,.F.) ;
#48261 = ADVANCED_FACE('',(#13043),#10425,.T.) ;
#48262 = ADVANCED_FACE('',(#13044),#45795,.T.) ;
#48263 = ADVANCED_FACE('',(#13045),#101,.F.) ;
#48264 = ADVANCED_FACE('',(#13046),#10426,.T.) ;
#48265 = ADVANCED_FACE('',(#13047),#10427,.T.) ;
#48266 = ADVANCED_FACE('',(#13048),#45796,.T.) ;
#48267 = ADVANCED_FACE('',(#13049),#10428,.T.) ;
#48268 = ADVANCED_FACE('',(#13050),#2101,.F.) ;
#48269 = ADVANCED_FACE('',(#13051),#102,.F.) ;
#48270 = ADVANCED_FACE('',(#13052),#2102,.F.) ;
#48271 = ADVANCED_FACE('',(#13053),#10429,.T.) ;
#48272 = ADVANCED_FACE('',(#13054),#10430,.T.) ;
#48273 = ADVANCED_FACE('',(#13055),#2103,.F.) ;
#48274 = ADVANCED_FACE('',(#13056),#10431,.T.) ;
#48275 = ADVANCED_FACE('',(#13057),#2748,.F.) ;
#48276 = ADVANCED_FACE('',(#13058),#10432,.F.) ;
#48277 = ADVANCED_FACE('',(#13059),#2749,.T.) ;
#48278 = ADVANCED_FACE('',(#13060),#10433,.T.) ;
#48279 = ADVANCED_FACE('',(#13061),#2750,.T.) ;
#48280 = ADVANCED_FACE('',(#13062),#2751,.T.) ;
#48281 = ADVANCED_FACE('',(#13063),#10434,.T.) ;
#48282 = ADVANCED_FACE('',(#13064),#10435,.F.) ;
#48283 = ADVANCED_FACE('',(#13065),#10436,.F.) ;
#48284 = ADVANCED_FACE('',(#13066),#2752,.T.) ;
#48285 = ADVANCED_FACE('',(#13067),#10437,.F.) ;
#48286 = ADVANCED_FACE('',(#13068),#2753,.T.) ;
#48287 = ADVANCED_FACE('',(#13069),#2754,.T.) ;
#48288 = ADVANCED_FACE('',(#13070),#10438,.F.) ;
#48289 = ADVANCED_FACE('',(#13071),#2755,.T.) ;
#48290 = ADVANCED_FACE('',(#13072),#10439,.F.) ;
#48291 = ADVANCED_FACE('',(#13073),#2756,.T.) ;
#48292 = ADVANCED_FACE('',(#13074),#2757,.T.) ;
#48293 = ADVANCED_FACE('',(#13075),#2104,.T.) ;
#48294 = ADVANCED_FACE('',(#13076),#2758,.T.) ;
#48295 = ADVANCED_FACE('',(#13077),#2105,.T.) ;
#48296 = ADVANCED_FACE('',(#13078),#10440,.F.) ;
#48297 = ADVANCED_FACE('',(#13079,#760),#2759,.T.) ;
#48298 = ADVANCED_FACE('',(#13080),#10441,.F.) ;
#48299 = ADVANCED_FACE('',(#13081),#10442,.F.) ;
#48300 = ADVANCED_FACE('',(#13082),#2760,.T.) ;
#48301 = ADVANCED_FACE('',(#13083),#10443,.F.) ;
#48302 = ADVANCED_FACE('',(#13084),#2761,.T.) ;
#48303 = ADVANCED_FACE('',(#13085),#10444,.F.) ;
#48304 = ADVANCED_FACE('',(#13086),#2762,.T.) ;
#48305 = ADVANCED_FACE('',(#13087),#10445,.F.) ;
#48306 = ADVANCED_FACE('',(#13088),#2763,.T.) ;
#48307 = ADVANCED_FACE('',(#13089),#10446,.F.) ;
#48308 = ADVANCED_FACE('',(#13090),#2764,.T.) ;
#48309 = ADVANCED_FACE('',(#13091),#2765,.T.) ;
#48310 = ADVANCED_FACE('',(#13092),#10447,.F.) ;
#48311 = ADVANCED_FACE('',(#13093),#2766,.T.) ;
#48312 = ADVANCED_FACE('',(#13094),#10448,.F.) ;
#48313 = ADVANCED_FACE('',(#13095),#2767,.T.) ;
#48314 = ADVANCED_FACE('',(#13096),#10449,.F.) ;
#48315 = ADVANCED_FACE('',(#13097),#2768,.T.) ;
#48316 = ADVANCED_FACE('',(#13098),#10450,.F.) ;
#48317 = ADVANCED_FACE('',(#13099),#2769,.T.) ;
#48318 = ADVANCED_FACE('',(#13100),#2106,.T.) ;
#48319 = ADVANCED_FACE('',(#13101),#10451,.F.) ;
#48320 = ADVANCED_FACE('',(#13102),#2770,.T.) ;
#48321 = ADVANCED_FACE('',(#13103),#10452,.F.) ;
#48322 = ADVANCED_FACE('',(#13104),#2771,.T.) ;
#48323 = ADVANCED_FACE('',(#13105),#2772,.T.) ;
#48324 = ADVANCED_FACE('',(#13106),#2773,.T.) ;
#48325 = ADVANCED_FACE('',(#13107),#10453,.F.) ;
#48326 = ADVANCED_FACE('',(#13108),#2774,.T.) ;
#48327 = ADVANCED_FACE('',(#13109),#10454,.F.) ;
#48328 = ADVANCED_FACE('',(#13110),#2775,.T.) ;
#48329 = ADVANCED_FACE('',(#13111),#10455,.F.) ;
#48330 = ADVANCED_FACE('',(#13112),#10456,.F.) ;
#48331 = ADVANCED_FACE('',(#13113),#2776,.T.) ;
#48332 = ADVANCED_FACE('',(#13114),#10457,.F.) ;
#48333 = ADVANCED_FACE('',(#13115),#2777,.T.) ;
#48334 = ADVANCED_FACE('',(#13116),#2778,.T.) ;
#48335 = ADVANCED_FACE('',(#13117),#10458,.F.) ;
#48336 = ADVANCED_FACE('',(#13118),#2779,.T.) ;
#48337 = ADVANCED_FACE('',(#13119),#10459,.F.) ;
#48338 = ADVANCED_FACE('',(#13120),#2780,.T.) ;
#48339 = ADVANCED_FACE('',(#13121),#2781,.T.) ;
#48340 = ADVANCED_FACE('',(#13122),#10460,.F.) ;
#48341 = ADVANCED_FACE('',(#13123),#2782,.T.) ;
#48342 = ADVANCED_FACE('',(#13124),#10461,.F.) ;
#48343 = ADVANCED_FACE('',(#13125),#2783,.T.) ;
#48344 = ADVANCED_FACE('',(#13126),#2784,.F.) ;
#48345 = ADVANCED_FACE('',(#13127),#2785,.T.) ;
#48346 = ADVANCED_FACE('',(#13128),#2107,.T.) ;
#48347 = ADVANCED_FACE('',(#13129),#2786,.T.) ;
#48348 = ADVANCED_FACE('',(#13130),#10462,.F.) ;
#48349 = ADVANCED_FACE('',(#13131),#2787,.T.) ;
#48350 = ADVANCED_FACE('',(#13132),#10463,.F.) ;
#48351 = ADVANCED_FACE('',(#13133),#2788,.F.) ;
#48352 = ADVANCED_FACE('',(#13134),#2108,.T.) ;
#48353 = ADVANCED_FACE('',(#13135),#2789,.T.) ;
#48354 = ADVANCED_FACE('',(#13136),#2790,.T.) ;
#48355 = ADVANCED_FACE('',(#13137),#10464,.F.) ;
#48356 = ADVANCED_FACE('',(#13138),#2791,.T.) ;
#48357 = ADVANCED_FACE('',(#13139),#10465,.F.) ;
#48358 = ADVANCED_FACE('',(#13140),#2792,.T.) ;
#48359 = ADVANCED_FACE('',(#13141),#2793,.F.) ;
#48360 = ADVANCED_FACE('',(#13142),#10466,.F.) ;
#48361 = ADVANCED_FACE('',(#13143),#2794,.T.) ;
#48362 = ADVANCED_FACE('',(#13144),#2795,.T.) ;
#48363 = ADVANCED_FACE('',(#13145),#2796,.T.) ;
#48364 = ADVANCED_FACE('',(#13146),#2797,.T.) ;
#48365 = ADVANCED_FACE('',(#13147),#2798,.T.) ;
#48366 = ADVANCED_FACE('',(#13148),#10467,.F.) ;
#48367 = ADVANCED_FACE('',(#13149),#2799,.F.) ;
#48368 = ADVANCED_FACE('',(#13150),#10468,.F.) ;
#48369 = ADVANCED_FACE('',(#13151),#2800,.T.) ;
#48370 = ADVANCED_FACE('',(#13152),#2801,.T.) ;
#48371 = ADVANCED_FACE('',(#13153),#10469,.F.) ;
#48372 = ADVANCED_FACE('',(#13154),#2802,.T.) ;
#48373 = ADVANCED_FACE('',(#13155),#10470,.F.) ;
#48374 = ADVANCED_FACE('',(#13156),#2803,.T.) ;
#48375 = ADVANCED_FACE('',(#13157),#2804,.F.) ;
#48376 = ADVANCED_FACE('',(#13158),#10471,.F.) ;
#48377 = ADVANCED_FACE('',(#13159),#2805,.T.) ;
#48378 = ADVANCED_FACE('',(#13160),#10472,.F.) ;
#48379 = ADVANCED_FACE('',(#13161),#2806,.T.) ;
#48380 = ADVANCED_FACE('',(#13162),#10473,.F.) ;
#48381 = ADVANCED_FACE('',(#13163),#2807,.T.) ;
#48382 = ADVANCED_FACE('',(#13164),#2808,.F.) ;
#48383 = ADVANCED_FACE('',(#13165),#2809,.F.) ;
#48384 = ADVANCED_FACE('',(#13166),#10474,.F.) ;
#48385 = ADVANCED_FACE('',(#13167),#2810,.T.) ;
#48386 = ADVANCED_FACE('',(#13168),#2811,.F.) ;
#48387 = ADVANCED_FACE('',(#13169),#2812,.T.) ;
#48388 = ADVANCED_FACE('',(#13170),#2813,.T.) ;
#48389 = ADVANCED_FACE('',(#13171),#2814,.T.) ;
#48390 = ADVANCED_FACE('',(#13172),#2815,.T.) ;
#48391 = ADVANCED_FACE('',(#13173),#2816,.T.) ;
#48392 = ADVANCED_FACE('',(#13174),#2817,.T.) ;
#48393 = ADVANCED_FACE('',(#13175),#2818,.T.) ;
#48394 = ADVANCED_FACE('',(#13176),#10475,.F.) ;
#48395 = ADVANCED_FACE('',(#13177),#2819,.T.) ;
#48396 = ADVANCED_FACE('',(#13178),#10476,.F.) ;
#48397 = ADVANCED_FACE('',(#13179),#2820,.T.) ;
#48398 = ADVANCED_FACE('',(#13180),#2821,.F.) ;
#48399 = ADVANCED_FACE('',(#13181),#10477,.F.) ;
#48400 = ADVANCED_FACE('',(#13182),#2822,.T.) ;
#48401 = ADVANCED_FACE('',(#13183),#10478,.T.) ;
#48402 = ADVANCED_FACE('',(#13184),#2823,.T.) ;
#48403 = ADVANCED_FACE('',(#13185),#2824,.T.) ;
#48404 = ADVANCED_FACE('',(#13186),#2825,.F.) ;
#48405 = ADVANCED_FACE('',(#13187),#2826,.T.) ;
#48406 = ADVANCED_FACE('',(#13188),#2827,.T.) ;
#48407 = ADVANCED_FACE('',(#13189),#10479,.T.) ;
#48408 = ADVANCED_FACE('',(#13190),#2828,.T.) ;
#48409 = ADVANCED_FACE('',(#13191),#10480,.T.) ;
#48410 = ADVANCED_FACE('',(#13192),#2829,.T.) ;
#48411 = ADVANCED_FACE('',(#13193),#2830,.T.) ;
#48412 = ADVANCED_FACE('',(#13194),#10481,.T.) ;
#48413 = ADVANCED_FACE('',(#13195),#10482,.F.) ;
#48414 = ADVANCED_FACE('',(#13196),#2831,.T.) ;
#48415 = ADVANCED_FACE('',(#13197),#10483,.F.) ;
#48416 = ADVANCED_FACE('',(#13198),#2832,.F.) ;
#48417 = ADVANCED_FACE('',(#13199),#10484,.F.) ;
#48418 = ADVANCED_FACE('',(#13200),#2833,.F.) ;
#48419 = ADVANCED_FACE('',(#13201),#2834,.F.) ;
#48420 = ADVANCED_FACE('',(#13202),#10485,.F.) ;
#48421 = ADVANCED_FACE('',(#13203),#2835,.F.) ;
#48422 = ADVANCED_FACE('',(#13204),#2836,.F.) ;
#48423 = ADVANCED_FACE('',(#13205),#2837,.F.) ;
#48424 = ADVANCED_FACE('',(#13206),#2838,.F.) ;
#48425 = ADVANCED_FACE('',(#13207),#2839,.F.) ;
#48426 = ADVANCED_FACE('',(#13208),#2840,.T.) ;
#48427 = ADVANCED_FACE('',(#13209),#2841,.T.) ;
#48428 = ADVANCED_FACE('',(#13210),#2842,.T.) ;
#48429 = ADVANCED_FACE('',(#13211),#2843,.T.) ;
#48430 = ADVANCED_FACE('',(#13212),#2844,.T.) ;
#48431 = ADVANCED_FACE('',(#13213),#2845,.T.) ;
#48432 = ADVANCED_FACE('',(#13214),#2846,.T.) ;
#48433 = ADVANCED_FACE('',(#13215),#2847,.T.) ;
#48434 = ADVANCED_FACE('',(#13216),#2848,.F.) ;
#48435 = ADVANCED_FACE('',(#13217),#2849,.T.) ;
#48436 = ADVANCED_FACE('',(#13218),#2850,.T.) ;
#48437 = ADVANCED_FACE('',(#13219),#2851,.T.) ;
#48438 = ADVANCED_FACE('',(#13220),#2852,.T.) ;
#48439 = ADVANCED_FACE('',(#13221),#2853,.T.) ;
#48440 = ADVANCED_FACE('',(#13222),#2854,.F.) ;
#48441 = ADVANCED_FACE('',(#13223),#10486,.T.) ;
#48442 = ADVANCED_FACE('',(#13224),#10487,.T.) ;
#48443 = ADVANCED_FACE('',(#13225),#10488,.T.) ;
#48444 = ADVANCED_FACE('',(#13226),#10489,.T.) ;
#48445 = ADVANCED_FACE('',(#13227,#761),#10490,.T.) ;
#48446 = ADVANCED_FACE('',(#13228),#10491,.T.) ;
#48447 = ADVANCED_FACE('',(#13229),#2855,.T.) ;
#48448 = ADVANCED_FACE('',(#13230),#2109,.F.) ;
#48449 = ADVANCED_FACE('',(#13231),#2110,.F.) ;
#48450 = ADVANCED_FACE('',(#13232),#2856,.T.) ;
#48451 = ADVANCED_FACE('',(#13233),#2857,.F.) ;
#48452 = ADVANCED_FACE('',(#13234),#45797,.F.) ;
#48453 = ADVANCED_FACE('',(#13235,#762),#2858,.F.) ;
#48454 = ADVANCED_FACE('',(#13236),#45798,.F.) ;
#48455 = ADVANCED_FACE('',(#13237,#763),#2859,.T.) ;
#48456 = ADVANCED_FACE('',(#13238,#764),#2860,.T.) ;
#48457 = ADVANCED_FACE('',(#13239,#765),#2861,.F.) ;
#48458 = ADVANCED_FACE('',(#13240),#2111,.F.) ;
#48459 = ADVANCED_FACE('',(#13241),#2112,.F.) ;
#48460 = ADVANCED_FACE('',(#13242),#45799,.T.) ;
#48461 = ADVANCED_FACE('',(#13243),#10492,.T.) ;
#48462 = ADVANCED_FACE('',(#13244),#45800,.T.) ;
#48463 = ADVANCED_FACE('',(#13245),#10493,.T.) ;
#48464 = ADVANCED_FACE('',(#13246),#45801,.T.) ;
#48465 = ADVANCED_FACE('',(#13247),#10494,.T.) ;
#48466 = ADVANCED_FACE('',(#13248),#45802,.T.) ;
#48467 = ADVANCED_FACE('',(#13249),#10495,.T.) ;
#48468 = ADVANCED_FACE('',(#13250),#45803,.T.) ;
#48469 = ADVANCED_FACE('',(#13251),#10496,.T.) ;
#48470 = ADVANCED_FACE('',(#13252),#45804,.T.) ;
#48471 = ADVANCED_FACE('',(#13253),#10497,.T.) ;
#48472 = ADVANCED_FACE('',(#13254),#45805,.T.) ;
#48473 = ADVANCED_FACE('',(#13255),#10498,.T.) ;
#48474 = ADVANCED_FACE('',(#13256),#45806,.T.) ;
#48475 = ADVANCED_FACE('',(#13257),#10499,.T.) ;
#48476 = ADVANCED_FACE('',(#13258),#45807,.T.) ;
#48477 = ADVANCED_FACE('',(#13259),#10500,.T.) ;
#48478 = ADVANCED_FACE('',(#13260),#45808,.T.) ;
#48479 = ADVANCED_FACE('',(#13261),#10501,.T.) ;
#48480 = ADVANCED_FACE('',(#13262),#45809,.T.) ;
#48481 = ADVANCED_FACE('',(#13263),#10502,.T.) ;
#48482 = ADVANCED_FACE('',(#13264),#45810,.T.) ;
#48483 = ADVANCED_FACE('',(#13265),#10503,.T.) ;
#48484 = ADVANCED_FACE('',(#13266),#45811,.T.) ;
#48485 = ADVANCED_FACE('',(#13267),#10504,.T.) ;
#48486 = ADVANCED_FACE('',(#13268),#45812,.T.) ;
#48487 = ADVANCED_FACE('',(#13269),#10505,.T.) ;
#48488 = ADVANCED_FACE('',(#13270),#45813,.T.) ;
#48489 = ADVANCED_FACE('',(#13271),#10506,.T.) ;
#48490 = ADVANCED_FACE('',(#13272),#45814,.T.) ;
#48491 = ADVANCED_FACE('',(#13273),#10507,.T.) ;
#48492 = ADVANCED_FACE('',(#13274),#45815,.T.) ;
#48493 = ADVANCED_FACE('',(#13275),#10508,.T.) ;
#48494 = ADVANCED_FACE('',(#13276),#45816,.T.) ;
#48495 = ADVANCED_FACE('',(#13277),#10509,.T.) ;
#48496 = ADVANCED_FACE('',(#13278),#45817,.T.) ;
#48497 = ADVANCED_FACE('',(#13279),#10510,.T.) ;
#48498 = ADVANCED_FACE('',(#13280),#45818,.T.) ;
#48499 = ADVANCED_FACE('',(#13281),#10511,.T.) ;
#48500 = ADVANCED_FACE('',(#13282),#45819,.T.) ;
#48501 = ADVANCED_FACE('',(#13283),#10512,.T.) ;
#48502 = ADVANCED_FACE('',(#13284),#45820,.T.) ;
#48503 = ADVANCED_FACE('',(#13285),#10513,.T.) ;
#48504 = ADVANCED_FACE('',(#13286),#45821,.T.) ;
#48505 = ADVANCED_FACE('',(#13287),#10514,.T.) ;
#48506 = ADVANCED_FACE('',(#13288),#45822,.T.) ;
#48507 = ADVANCED_FACE('',(#13289),#10515,.T.) ;
#48508 = ADVANCED_FACE('',(#13290),#45823,.T.) ;
#48509 = ADVANCED_FACE('',(#13291),#10516,.T.) ;
#48510 = ADVANCED_FACE('',(#13292),#45824,.T.) ;
#48511 = ADVANCED_FACE('',(#13293),#10517,.T.) ;
#48512 = ADVANCED_FACE('',(#13294),#45825,.T.) ;
#48513 = ADVANCED_FACE('',(#13295),#10518,.T.) ;
#48514 = ADVANCED_FACE('',(#13296),#45826,.T.) ;
#48515 = ADVANCED_FACE('',(#13297),#10519,.T.) ;
#48516 = ADVANCED_FACE('',(#13298),#45827,.T.) ;
#48517 = ADVANCED_FACE('',(#13299),#10520,.T.) ;
#48518 = ADVANCED_FACE('',(#13300),#45828,.T.) ;
#48519 = ADVANCED_FACE('',(#13301),#10521,.T.) ;
#48520 = ADVANCED_FACE('',(#13302),#45829,.T.) ;
#48521 = ADVANCED_FACE('',(#13303),#10522,.T.) ;
#48522 = ADVANCED_FACE('',(#13304),#45830,.T.) ;
#48523 = ADVANCED_FACE('',(#13305),#10523,.T.) ;
#48524 = ADVANCED_FACE('',(#13306),#45831,.T.) ;
#48525 = ADVANCED_FACE('',(#13307),#10524,.T.) ;
#48526 = ADVANCED_FACE('',(#13308),#45832,.T.) ;
#48527 = ADVANCED_FACE('',(#13309),#10525,.T.) ;
#48528 = ADVANCED_FACE('',(#13310),#45833,.T.) ;
#48529 = ADVANCED_FACE('',(#13311),#10526,.T.) ;
#48530 = ADVANCED_FACE('',(#13312),#45834,.T.) ;
#48531 = ADVANCED_FACE('',(#13313),#10527,.T.) ;
#48532 = ADVANCED_FACE('',(#13314),#45835,.T.) ;
#48533 = ADVANCED_FACE('',(#13315),#10528,.T.) ;
#48534 = ADVANCED_FACE('',(#13316),#45836,.T.) ;
#48535 = ADVANCED_FACE('',(#13317),#10529,.T.) ;
#48536 = ADVANCED_FACE('',(#13318),#45837,.T.) ;
#48537 = ADVANCED_FACE('',(#13319),#10530,.T.) ;
#48538 = ADVANCED_FACE('',(#13320),#45838,.T.) ;
#48539 = ADVANCED_FACE('',(#13321),#10531,.T.) ;
#48540 = ADVANCED_FACE('',(#13322),#2862,.T.) ;
#48541 = ADVANCED_FACE('',(#13323),#10532,.T.) ;
#48542 = ADVANCED_FACE('',(#13324),#2863,.T.) ;
#48543 = ADVANCED_FACE('',(#13325),#10533,.T.) ;
#48544 = ADVANCED_FACE('',(#13326),#2864,.T.) ;
#48545 = ADVANCED_FACE('',(#13327),#10534,.T.) ;
#48546 = ADVANCED_FACE('',(#13328),#2865,.T.) ;
#48547 = ADVANCED_FACE('',(#13329),#10535,.T.) ;
#48548 = ADVANCED_FACE('',(#13330),#2866,.T.) ;
#48549 = ADVANCED_FACE('',(#13331),#10536,.T.) ;
#48550 = ADVANCED_FACE('',(#13332),#2867,.T.) ;
#48551 = ADVANCED_FACE('',(#13333),#10537,.T.) ;
#48552 = ADVANCED_FACE('',(#13334),#2868,.T.) ;
#48553 = ADVANCED_FACE('',(#13335),#10538,.T.) ;
#48554 = ADVANCED_FACE('',(#13336),#2869,.T.) ;
#48555 = ADVANCED_FACE('',(#13337),#10539,.T.) ;
#48556 = ADVANCED_FACE('',(#13338),#2870,.T.) ;
#48557 = ADVANCED_FACE('',(#13339),#10540,.T.) ;
#48558 = ADVANCED_FACE('',(#13340),#2871,.T.) ;
#48559 = ADVANCED_FACE('',(#13341),#10541,.T.) ;
#48560 = ADVANCED_FACE('',(#13342),#2872,.T.) ;
#48561 = ADVANCED_FACE('',(#13343),#10542,.T.) ;
#48562 = ADVANCED_FACE('',(#13344),#2873,.T.) ;
#48563 = ADVANCED_FACE('',(#13345),#10543,.T.) ;
#48564 = ADVANCED_FACE('',(#13346),#2874,.T.) ;
#48565 = ADVANCED_FACE('',(#13347),#10544,.T.) ;
#48566 = ADVANCED_FACE('',(#13348),#2875,.T.) ;
#48567 = ADVANCED_FACE('',(#13349),#10545,.T.) ;
#48568 = ADVANCED_FACE('',(#13350),#2876,.T.) ;
#48569 = ADVANCED_FACE('',(#13351),#10546,.T.) ;
#48570 = ADVANCED_FACE('',(#13352),#2877,.T.) ;
#48571 = ADVANCED_FACE('',(#13353),#10547,.T.) ;
#48572 = ADVANCED_FACE('',(#13354),#2878,.T.) ;
#48573 = ADVANCED_FACE('',(#13355),#10548,.T.) ;
#48574 = ADVANCED_FACE('',(#13356),#2879,.T.) ;
#48575 = ADVANCED_FACE('',(#13357),#10549,.T.) ;
#48576 = ADVANCED_FACE('',(#13358),#2880,.T.) ;
#48577 = ADVANCED_FACE('',(#13359),#10550,.T.) ;
#48578 = ADVANCED_FACE('',(#13360),#2881,.T.) ;
#48579 = ADVANCED_FACE('',(#13361),#10551,.T.) ;
#48580 = ADVANCED_FACE('',(#13362),#2882,.F.) ;
#48581 = ADVANCED_FACE('',(#13363),#2883,.F.) ;
#48582 = ADVANCED_FACE('',(#13364),#2884,.F.) ;
#48583 = ADVANCED_FACE('',(#13365),#2885,.F.) ;
#48584 = ADVANCED_FACE('',(#13366),#2886,.F.) ;
#48585 = ADVANCED_FACE('',(#13367),#2887,.F.) ;
#48586 = ADVANCED_FACE('',(#13368),#2888,.F.) ;
#48587 = ADVANCED_FACE('',(#13369),#2889,.F.) ;
#48588 = ADVANCED_FACE('',(#13370),#2890,.F.) ;
#48589 = ADVANCED_FACE('',(#13371),#2891,.F.) ;
#48590 = ADVANCED_FACE('',(#13372),#2892,.F.) ;
#48591 = ADVANCED_FACE('',(#13373),#2893,.F.) ;
#48592 = ADVANCED_FACE('',(#13374),#2894,.F.) ;
#48593 = ADVANCED_FACE('',(#13375),#2895,.F.) ;
#48594 = ADVANCED_FACE('',(#13376),#2896,.F.) ;
#48595 = ADVANCED_FACE('',(#13377),#2897,.F.) ;
#48596 = ADVANCED_FACE('',(#13378),#2898,.F.) ;
#48597 = ADVANCED_FACE('',(#13379),#2899,.F.) ;
#48598 = ADVANCED_FACE('',(#13380),#2900,.F.) ;
#48599 = ADVANCED_FACE('',(#13381),#45839,.F.) ;
#48600 = ADVANCED_FACE('',(#13382),#2901,.F.) ;
#48601 = ADVANCED_FACE('',(#13383),#45840,.F.) ;
#48602 = ADVANCED_FACE('',(#13384),#2902,.T.) ;
#48603 = ADVANCED_FACE('',(#13385),#2903,.T.) ;
#48604 = ADVANCED_FACE('',(#13386),#2904,.T.) ;
#48605 = ADVANCED_FACE('',(#13387),#2905,.T.) ;
#48606 = ADVANCED_FACE('',(#13388),#2906,.T.) ;
#48607 = ADVANCED_FACE('',(#13389),#2907,.T.) ;
#48608 = ADVANCED_FACE('',(#13390),#2908,.T.) ;
#48609 = ADVANCED_FACE('',(#13391),#2909,.T.) ;
#48610 = ADVANCED_FACE('',(#13392),#2910,.T.) ;
#48611 = ADVANCED_FACE('',(#13393),#2911,.T.) ;
#48612 = ADVANCED_FACE('',(#13394),#2912,.T.) ;
#48613 = ADVANCED_FACE('',(#13395),#2913,.T.) ;
#48614 = ADVANCED_FACE('',(#13396),#2914,.T.) ;
#48615 = ADVANCED_FACE('',(#13397),#2915,.T.) ;
#48616 = ADVANCED_FACE('',(#13398),#2916,.T.) ;
#48617 = ADVANCED_FACE('',(#13399),#2917,.T.) ;
#48618 = ADVANCED_FACE('',(#13400),#2918,.T.) ;
#48619 = ADVANCED_FACE('',(#13401),#2919,.T.) ;
#48620 = ADVANCED_FACE('',(#13402),#2920,.T.) ;
#48621 = ADVANCED_FACE('',(#13403),#2921,.T.) ;
#48622 = ADVANCED_FACE('',(#13404),#45841,.T.) ;
#48623 = ADVANCED_FACE('',(#13405),#10552,.T.) ;
#48624 = ADVANCED_FACE('',(#13406),#10553,.T.) ;
#48625 = ADVANCED_FACE('',(#13407),#10554,.T.) ;
#48626 = ADVANCED_FACE('',(#13408),#45842,.T.) ;
#48627 = ADVANCED_FACE('',(#13409),#10555,.T.) ;
#48628 = ADVANCED_FACE('',(#13410),#10556,.T.) ;
#48629 = ADVANCED_FACE('',(#13411),#10557,.T.) ;
#48630 = ADVANCED_FACE('',(#13412),#45843,.T.) ;
#48631 = ADVANCED_FACE('',(#13413),#10558,.T.) ;
#48632 = ADVANCED_FACE('',(#13414),#10559,.T.) ;
#48633 = ADVANCED_FACE('',(#13415),#10560,.T.) ;
#48634 = ADVANCED_FACE('',(#13416),#45844,.T.) ;
#48635 = ADVANCED_FACE('',(#13417),#10561,.T.) ;
#48636 = ADVANCED_FACE('',(#13418),#10562,.T.) ;
#48637 = ADVANCED_FACE('',(#13419),#10563,.T.) ;
#48638 = ADVANCED_FACE('',(#13420),#45845,.T.) ;
#48639 = ADVANCED_FACE('',(#13421),#10564,.T.) ;
#48640 = ADVANCED_FACE('',(#13422),#10565,.T.) ;
#48641 = ADVANCED_FACE('',(#13423),#10566,.T.) ;
#48642 = ADVANCED_FACE('',(#13424),#45846,.T.) ;
#48643 = ADVANCED_FACE('',(#13425),#10567,.T.) ;
#48644 = ADVANCED_FACE('',(#13426),#10568,.T.) ;
#48645 = ADVANCED_FACE('',(#13427),#10569,.T.) ;
#48646 = ADVANCED_FACE('',(#13428),#45847,.T.) ;
#48647 = ADVANCED_FACE('',(#13429),#10570,.T.) ;
#48648 = ADVANCED_FACE('',(#13430),#10571,.T.) ;
#48649 = ADVANCED_FACE('',(#13431),#10572,.T.) ;
#48650 = ADVANCED_FACE('',(#13432),#45848,.T.) ;
#48651 = ADVANCED_FACE('',(#13433),#10573,.T.) ;
#48652 = ADVANCED_FACE('',(#13434),#10574,.T.) ;
#48653 = ADVANCED_FACE('',(#13435),#10575,.T.) ;
#48654 = ADVANCED_FACE('',(#13436),#45849,.T.) ;
#48655 = ADVANCED_FACE('',(#13437),#10576,.T.) ;
#48656 = ADVANCED_FACE('',(#13438),#10577,.T.) ;
#48657 = ADVANCED_FACE('',(#13439),#10578,.T.) ;
#48658 = ADVANCED_FACE('',(#13440),#45850,.T.) ;
#48659 = ADVANCED_FACE('',(#13441),#10579,.T.) ;
#48660 = ADVANCED_FACE('',(#13442),#10580,.T.) ;
#48661 = ADVANCED_FACE('',(#13443),#10581,.T.) ;
#48662 = ADVANCED_FACE('',(#13444),#45851,.T.) ;
#48663 = ADVANCED_FACE('',(#13445),#10582,.T.) ;
#48664 = ADVANCED_FACE('',(#13446),#45852,.T.) ;
#48665 = ADVANCED_FACE('',(#13447),#45853,.T.) ;
#48666 = ADVANCED_FACE('',(#13448),#45854,.T.) ;
#48667 = ADVANCED_FACE('',(#13449),#10583,.T.) ;
#48668 = ADVANCED_FACE('',(#13450),#45855,.T.) ;
#48669 = ADVANCED_FACE('',(#13451),#45856,.T.) ;
#48670 = ADVANCED_FACE('',(#13452),#45857,.T.) ;
#48671 = ADVANCED_FACE('',(#13453),#10584,.T.) ;
#48672 = ADVANCED_FACE('',(#13454),#45858,.T.) ;
#48673 = ADVANCED_FACE('',(#13455),#45859,.T.) ;
#48674 = ADVANCED_FACE('',(#13456),#45860,.T.) ;
#48675 = ADVANCED_FACE('',(#13457),#10585,.T.) ;
#48676 = ADVANCED_FACE('',(#13458),#45861,.T.) ;
#48677 = ADVANCED_FACE('',(#13459),#45862,.T.) ;
#48678 = ADVANCED_FACE('',(#13460),#45863,.T.) ;
#48679 = ADVANCED_FACE('',(#13461),#10586,.T.) ;
#48680 = ADVANCED_FACE('',(#13462),#45864,.T.) ;
#48681 = ADVANCED_FACE('',(#13463),#45865,.T.) ;
#48682 = ADVANCED_FACE('',(#13464),#45866,.T.) ;
#48683 = ADVANCED_FACE('',(#13465),#10587,.T.) ;
#48684 = ADVANCED_FACE('',(#13466),#45867,.T.) ;
#48685 = ADVANCED_FACE('',(#13467),#45868,.T.) ;
#48686 = ADVANCED_FACE('',(#13468),#45869,.T.) ;
#48687 = ADVANCED_FACE('',(#13469),#10588,.T.) ;
#48688 = ADVANCED_FACE('',(#13470),#45870,.T.) ;
#48689 = ADVANCED_FACE('',(#13471),#45871,.T.) ;
#48690 = ADVANCED_FACE('',(#13472),#45872,.T.) ;
#48691 = ADVANCED_FACE('',(#13473),#10589,.T.) ;
#48692 = ADVANCED_FACE('',(#13474),#45873,.T.) ;
#48693 = ADVANCED_FACE('',(#13475),#45874,.T.) ;
#48694 = ADVANCED_FACE('',(#13476),#45875,.T.) ;
#48695 = ADVANCED_FACE('',(#13477),#10590,.T.) ;
#48696 = ADVANCED_FACE('',(#13478),#45876,.T.) ;
#48697 = ADVANCED_FACE('',(#13479),#45877,.T.) ;
#48698 = ADVANCED_FACE('',(#13480),#45878,.T.) ;
#48699 = ADVANCED_FACE('',(#13481),#10591,.T.) ;
#48700 = ADVANCED_FACE('',(#13482),#45879,.T.) ;
#48701 = ADVANCED_FACE('',(#13483),#45880,.T.) ;
#48702 = ADVANCED_FACE('',(#13484),#10592,.T.) ;
#48703 = ADVANCED_FACE('',(#13485),#2922,.T.) ;
#48704 = ADVANCED_FACE('',(#13486),#10593,.T.) ;
#48705 = ADVANCED_FACE('',(#13487),#2923,.T.) ;
#48706 = ADVANCED_FACE('',(#13488),#2924,.T.) ;
#48707 = ADVANCED_FACE('',(#13489),#2925,.T.) ;
#48708 = ADVANCED_FACE('',(#13490),#10594,.T.) ;
#48709 = ADVANCED_FACE('',(#13491),#2926,.T.) ;
#48710 = ADVANCED_FACE('',(#13492),#2927,.T.) ;
#48711 = ADVANCED_FACE('',(#13493),#10595,.T.) ;
#48712 = ADVANCED_FACE('',(#13494),#2928,.T.) ;
#48713 = ADVANCED_FACE('',(#13495),#2929,.T.) ;
#48714 = ADVANCED_FACE('',(#13496),#10596,.T.) ;
#48715 = ADVANCED_FACE('',(#13497),#2930,.T.) ;
#48716 = ADVANCED_FACE('',(#13498),#2931,.T.) ;
#48717 = ADVANCED_FACE('',(#13499),#10597,.T.) ;
#48718 = ADVANCED_FACE('',(#13500),#2932,.T.) ;
#48719 = ADVANCED_FACE('',(#13501),#2933,.T.) ;
#48720 = ADVANCED_FACE('',(#13502),#10598,.T.) ;
#48721 = ADVANCED_FACE('',(#13503),#2934,.T.) ;
#48722 = ADVANCED_FACE('',(#13504),#2935,.T.) ;
#48723 = ADVANCED_FACE('',(#13505),#10599,.T.) ;
#48724 = ADVANCED_FACE('',(#13506),#2936,.T.) ;
#48725 = ADVANCED_FACE('',(#13507),#2937,.T.) ;
#48726 = ADVANCED_FACE('',(#13508),#10600,.T.) ;
#48727 = ADVANCED_FACE('',(#13509),#2938,.T.) ;
#48728 = ADVANCED_FACE('',(#13510),#2939,.T.) ;
#48729 = ADVANCED_FACE('',(#13511),#10601,.T.) ;
#48730 = ADVANCED_FACE('',(#13512),#2940,.T.) ;
#48731 = ADVANCED_FACE('',(#13513),#2941,.T.) ;
#48732 = ADVANCED_FACE('',(#13514),#10602,.T.) ;
#48733 = ADVANCED_FACE('',(#13515),#10603,.T.) ;
#48734 = ADVANCED_FACE('',(#13516),#10604,.T.) ;
#48735 = ADVANCED_FACE('',(#13517),#10605,.T.) ;
#48736 = ADVANCED_FACE('',(#13518),#10606,.T.) ;
#48737 = ADVANCED_FACE('',(#13519),#10607,.T.) ;
#48738 = ADVANCED_FACE('',(#13520),#10608,.T.) ;
#48739 = ADVANCED_FACE('',(#13521),#10609,.T.) ;
#48740 = ADVANCED_FACE('',(#13522),#10610,.T.) ;
#48741 = ADVANCED_FACE('',(#13523),#10611,.T.) ;
#48742 = ADVANCED_FACE('',(#13524),#10612,.F.) ;
#48743 = ADVANCED_FACE('',(#13525),#45881,.F.) ;
#48744 = ADVANCED_FACE('',(#13526,#766),#2942,.F.) ;
#48745 = ADVANCED_FACE('',(#13527),#45882,.F.) ;
#48746 = ADVANCED_FACE('',(#13528,#767),#2943,.T.) ;
#48747 = ADVANCED_FACE('',(#13529,#768),#2944,.T.) ;
#48748 = ADVANCED_FACE('',(#13530,#769),#2945,.F.) ;
#48749 = ADVANCED_FACE('',(#13531),#2113,.F.) ;
#48750 = ADVANCED_FACE('',(#13532),#2114,.F.) ;
#48751 = ADVANCED_FACE('',(#13533),#45883,.T.) ;
#48752 = ADVANCED_FACE('',(#13534),#10613,.T.) ;
#48753 = ADVANCED_FACE('',(#13535),#45884,.T.) ;
#48754 = ADVANCED_FACE('',(#13536),#10614,.T.) ;
#48755 = ADVANCED_FACE('',(#13537),#45885,.T.) ;
#48756 = ADVANCED_FACE('',(#13538),#10615,.T.) ;
#48757 = ADVANCED_FACE('',(#13539),#45886,.T.) ;
#48758 = ADVANCED_FACE('',(#13540),#10616,.T.) ;
#48759 = ADVANCED_FACE('',(#13541),#45887,.T.) ;
#48760 = ADVANCED_FACE('',(#13542),#10617,.T.) ;
#48761 = ADVANCED_FACE('',(#13543),#45888,.T.) ;
#48762 = ADVANCED_FACE('',(#13544),#10618,.T.) ;
#48763 = ADVANCED_FACE('',(#13545),#45889,.T.) ;
#48764 = ADVANCED_FACE('',(#13546),#10619,.T.) ;
#48765 = ADVANCED_FACE('',(#13547),#45890,.T.) ;
#48766 = ADVANCED_FACE('',(#13548),#10620,.T.) ;
#48767 = ADVANCED_FACE('',(#13549),#45891,.T.) ;
#48768 = ADVANCED_FACE('',(#13550),#10621,.T.) ;
#48769 = ADVANCED_FACE('',(#13551),#45892,.T.) ;
#48770 = ADVANCED_FACE('',(#13552),#10622,.T.) ;
#48771 = ADVANCED_FACE('',(#13553),#45893,.T.) ;
#48772 = ADVANCED_FACE('',(#13554),#10623,.T.) ;
#48773 = ADVANCED_FACE('',(#13555),#45894,.T.) ;
#48774 = ADVANCED_FACE('',(#13556),#10624,.T.) ;
#48775 = ADVANCED_FACE('',(#13557),#45895,.T.) ;
#48776 = ADVANCED_FACE('',(#13558),#10625,.T.) ;
#48777 = ADVANCED_FACE('',(#13559),#45896,.T.) ;
#48778 = ADVANCED_FACE('',(#13560),#10626,.T.) ;
#48779 = ADVANCED_FACE('',(#13561),#45897,.T.) ;
#48780 = ADVANCED_FACE('',(#13562),#10627,.T.) ;
#48781 = ADVANCED_FACE('',(#13563),#45898,.T.) ;
#48782 = ADVANCED_FACE('',(#13564),#10628,.T.) ;
#48783 = ADVANCED_FACE('',(#13565),#45899,.T.) ;
#48784 = ADVANCED_FACE('',(#13566),#10629,.T.) ;
#48785 = ADVANCED_FACE('',(#13567),#45900,.T.) ;
#48786 = ADVANCED_FACE('',(#13568),#10630,.T.) ;
#48787 = ADVANCED_FACE('',(#13569),#45901,.T.) ;
#48788 = ADVANCED_FACE('',(#13570),#10631,.T.) ;
#48789 = ADVANCED_FACE('',(#13571),#45902,.T.) ;
#48790 = ADVANCED_FACE('',(#13572),#10632,.T.) ;
#48791 = ADVANCED_FACE('',(#13573),#45903,.T.) ;
#48792 = ADVANCED_FACE('',(#13574),#10633,.T.) ;
#48793 = ADVANCED_FACE('',(#13575),#45904,.T.) ;
#48794 = ADVANCED_FACE('',(#13576),#10634,.T.) ;
#48795 = ADVANCED_FACE('',(#13577),#45905,.T.) ;
#48796 = ADVANCED_FACE('',(#13578),#10635,.T.) ;
#48797 = ADVANCED_FACE('',(#13579),#45906,.T.) ;
#48798 = ADVANCED_FACE('',(#13580),#10636,.T.) ;
#48799 = ADVANCED_FACE('',(#13581),#45907,.T.) ;
#48800 = ADVANCED_FACE('',(#13582),#10637,.T.) ;
#48801 = ADVANCED_FACE('',(#13583),#45908,.T.) ;
#48802 = ADVANCED_FACE('',(#13584),#10638,.T.) ;
#48803 = ADVANCED_FACE('',(#13585),#45909,.T.) ;
#48804 = ADVANCED_FACE('',(#13586),#10639,.T.) ;
#48805 = ADVANCED_FACE('',(#13587),#45910,.T.) ;
#48806 = ADVANCED_FACE('',(#13588),#10640,.T.) ;
#48807 = ADVANCED_FACE('',(#13589),#45911,.T.) ;
#48808 = ADVANCED_FACE('',(#13590),#10641,.T.) ;
#48809 = ADVANCED_FACE('',(#13591),#45912,.T.) ;
#48810 = ADVANCED_FACE('',(#13592),#10642,.T.) ;
#48811 = ADVANCED_FACE('',(#13593),#45913,.T.) ;
#48812 = ADVANCED_FACE('',(#13594),#10643,.T.) ;
#48813 = ADVANCED_FACE('',(#13595),#45914,.T.) ;
#48814 = ADVANCED_FACE('',(#13596),#10644,.T.) ;
#48815 = ADVANCED_FACE('',(#13597),#45915,.T.) ;
#48816 = ADVANCED_FACE('',(#13598),#10645,.T.) ;
#48817 = ADVANCED_FACE('',(#13599),#45916,.T.) ;
#48818 = ADVANCED_FACE('',(#13600),#10646,.T.) ;
#48819 = ADVANCED_FACE('',(#13601),#45917,.T.) ;
#48820 = ADVANCED_FACE('',(#13602),#10647,.T.) ;
#48821 = ADVANCED_FACE('',(#13603),#45918,.T.) ;
#48822 = ADVANCED_FACE('',(#13604),#10648,.T.) ;
#48823 = ADVANCED_FACE('',(#13605),#45919,.T.) ;
#48824 = ADVANCED_FACE('',(#13606),#10649,.T.) ;
#48825 = ADVANCED_FACE('',(#13607),#45920,.T.) ;
#48826 = ADVANCED_FACE('',(#13608),#10650,.T.) ;
#48827 = ADVANCED_FACE('',(#13609),#45921,.T.) ;
#48828 = ADVANCED_FACE('',(#13610),#10651,.T.) ;
#48829 = ADVANCED_FACE('',(#13611),#45922,.T.) ;
#48830 = ADVANCED_FACE('',(#13612),#10652,.T.) ;
#48831 = ADVANCED_FACE('',(#13613),#2946,.T.) ;
#48832 = ADVANCED_FACE('',(#13614),#10653,.T.) ;
#48833 = ADVANCED_FACE('',(#13615),#2947,.T.) ;
#48834 = ADVANCED_FACE('',(#13616),#10654,.T.) ;
#48835 = ADVANCED_FACE('',(#13617),#2948,.T.) ;
#48836 = ADVANCED_FACE('',(#13618),#10655,.T.) ;
#48837 = ADVANCED_FACE('',(#13619),#2949,.T.) ;
#48838 = ADVANCED_FACE('',(#13620),#10656,.T.) ;
#48839 = ADVANCED_FACE('',(#13621),#2950,.T.) ;
#48840 = ADVANCED_FACE('',(#13622),#10657,.T.) ;
#48841 = ADVANCED_FACE('',(#13623),#2951,.T.) ;
#48842 = ADVANCED_FACE('',(#13624),#10658,.T.) ;
#48843 = ADVANCED_FACE('',(#13625),#2952,.T.) ;
#48844 = ADVANCED_FACE('',(#13626),#10659,.T.) ;
#48845 = ADVANCED_FACE('',(#13627),#2953,.T.) ;
#48846 = ADVANCED_FACE('',(#13628),#10660,.T.) ;
#48847 = ADVANCED_FACE('',(#13629),#2954,.T.) ;
#48848 = ADVANCED_FACE('',(#13630),#10661,.T.) ;
#48849 = ADVANCED_FACE('',(#13631),#2955,.T.) ;
#48850 = ADVANCED_FACE('',(#13632),#10662,.T.) ;
#48851 = ADVANCED_FACE('',(#13633),#2956,.T.) ;
#48852 = ADVANCED_FACE('',(#13634),#10663,.T.) ;
#48853 = ADVANCED_FACE('',(#13635),#2957,.T.) ;
#48854 = ADVANCED_FACE('',(#13636),#10664,.T.) ;
#48855 = ADVANCED_FACE('',(#13637),#2958,.T.) ;
#48856 = ADVANCED_FACE('',(#13638),#10665,.T.) ;
#48857 = ADVANCED_FACE('',(#13639),#2959,.T.) ;
#48858 = ADVANCED_FACE('',(#13640),#10666,.T.) ;
#48859 = ADVANCED_FACE('',(#13641),#2960,.T.) ;
#48860 = ADVANCED_FACE('',(#13642),#10667,.T.) ;
#48861 = ADVANCED_FACE('',(#13643),#2961,.T.) ;
#48862 = ADVANCED_FACE('',(#13644),#10668,.T.) ;
#48863 = ADVANCED_FACE('',(#13645),#2962,.T.) ;
#48864 = ADVANCED_FACE('',(#13646),#10669,.T.) ;
#48865 = ADVANCED_FACE('',(#13647),#2963,.T.) ;
#48866 = ADVANCED_FACE('',(#13648),#10670,.T.) ;
#48867 = ADVANCED_FACE('',(#13649),#2964,.T.) ;
#48868 = ADVANCED_FACE('',(#13650),#10671,.T.) ;
#48869 = ADVANCED_FACE('',(#13651),#2965,.T.) ;
#48870 = ADVANCED_FACE('',(#13652),#10672,.T.) ;
#48871 = ADVANCED_FACE('',(#13653),#2966,.F.) ;
#48872 = ADVANCED_FACE('',(#13654),#2967,.F.) ;
#48873 = ADVANCED_FACE('',(#13655),#2968,.F.) ;
#48874 = ADVANCED_FACE('',(#13656),#2969,.F.) ;
#48875 = ADVANCED_FACE('',(#13657),#2970,.F.) ;
#48876 = ADVANCED_FACE('',(#13658),#2971,.F.) ;
#48877 = ADVANCED_FACE('',(#13659),#2972,.F.) ;
#48878 = ADVANCED_FACE('',(#13660),#2973,.F.) ;
#48879 = ADVANCED_FACE('',(#13661),#2974,.F.) ;
#48880 = ADVANCED_FACE('',(#13662),#2975,.F.) ;
#48881 = ADVANCED_FACE('',(#13663),#2976,.F.) ;
#48882 = ADVANCED_FACE('',(#13664),#2977,.F.) ;
#48883 = ADVANCED_FACE('',(#13665),#2978,.F.) ;
#48884 = ADVANCED_FACE('',(#13666),#2979,.F.) ;
#48885 = ADVANCED_FACE('',(#13667),#2980,.F.) ;
#48886 = ADVANCED_FACE('',(#13668),#2981,.F.) ;
#48887 = ADVANCED_FACE('',(#13669),#2982,.F.) ;
#48888 = ADVANCED_FACE('',(#13670),#2983,.F.) ;
#48889 = ADVANCED_FACE('',(#13671),#2984,.F.) ;
#48890 = ADVANCED_FACE('',(#13672),#45923,.F.) ;
#48891 = ADVANCED_FACE('',(#13673),#2985,.F.) ;
#48892 = ADVANCED_FACE('',(#13674),#45924,.F.) ;
#48893 = ADVANCED_FACE('',(#13675),#2986,.T.) ;
#48894 = ADVANCED_FACE('',(#13676),#2987,.T.) ;
#48895 = ADVANCED_FACE('',(#13677),#2988,.T.) ;
#48896 = ADVANCED_FACE('',(#13678),#2989,.T.) ;
#48897 = ADVANCED_FACE('',(#13679),#2990,.T.) ;
#48898 = ADVANCED_FACE('',(#13680),#2991,.T.) ;
#48899 = ADVANCED_FACE('',(#13681),#2992,.T.) ;
#48900 = ADVANCED_FACE('',(#13682),#2993,.T.) ;
#48901 = ADVANCED_FACE('',(#13683),#2994,.T.) ;
#48902 = ADVANCED_FACE('',(#13684),#2995,.T.) ;
#48903 = ADVANCED_FACE('',(#13685),#2996,.T.) ;
#48904 = ADVANCED_FACE('',(#13686),#2997,.T.) ;
#48905 = ADVANCED_FACE('',(#13687),#2998,.T.) ;
#48906 = ADVANCED_FACE('',(#13688),#2999,.T.) ;
#48907 = ADVANCED_FACE('',(#13689),#3000,.T.) ;
#48908 = ADVANCED_FACE('',(#13690),#3001,.T.) ;
#48909 = ADVANCED_FACE('',(#13691),#3002,.T.) ;
#48910 = ADVANCED_FACE('',(#13692),#3003,.T.) ;
#48911 = ADVANCED_FACE('',(#13693),#3004,.T.) ;
#48912 = ADVANCED_FACE('',(#13694),#3005,.T.) ;
#48913 = ADVANCED_FACE('',(#13695),#45925,.T.) ;
#48914 = ADVANCED_FACE('',(#13696),#10673,.T.) ;
#48915 = ADVANCED_FACE('',(#13697),#10674,.T.) ;
#48916 = ADVANCED_FACE('',(#13698),#10675,.T.) ;
#48917 = ADVANCED_FACE('',(#13699),#45926,.T.) ;
#48918 = ADVANCED_FACE('',(#13700),#10676,.T.) ;
#48919 = ADVANCED_FACE('',(#13701),#10677,.T.) ;
#48920 = ADVANCED_FACE('',(#13702),#10678,.T.) ;
#48921 = ADVANCED_FACE('',(#13703),#45927,.T.) ;
#48922 = ADVANCED_FACE('',(#13704),#10679,.T.) ;
#48923 = ADVANCED_FACE('',(#13705),#10680,.T.) ;
#48924 = ADVANCED_FACE('',(#13706),#10681,.T.) ;
#48925 = ADVANCED_FACE('',(#13707),#45928,.T.) ;
#48926 = ADVANCED_FACE('',(#13708),#10682,.T.) ;
#48927 = ADVANCED_FACE('',(#13709),#10683,.T.) ;
#48928 = ADVANCED_FACE('',(#13710),#10684,.T.) ;
#48929 = ADVANCED_FACE('',(#13711),#45929,.T.) ;
#48930 = ADVANCED_FACE('',(#13712),#10685,.T.) ;
#48931 = ADVANCED_FACE('',(#13713),#10686,.T.) ;
#48932 = ADVANCED_FACE('',(#13714),#10687,.T.) ;
#48933 = ADVANCED_FACE('',(#13715),#45930,.T.) ;
#48934 = ADVANCED_FACE('',(#13716),#10688,.T.) ;
#48935 = ADVANCED_FACE('',(#13717),#10689,.T.) ;
#48936 = ADVANCED_FACE('',(#13718),#10690,.T.) ;
#48937 = ADVANCED_FACE('',(#13719),#45931,.T.) ;
#48938 = ADVANCED_FACE('',(#13720),#10691,.T.) ;
#48939 = ADVANCED_FACE('',(#13721),#10692,.T.) ;
#48940 = ADVANCED_FACE('',(#13722),#10693,.T.) ;
#48941 = ADVANCED_FACE('',(#13723),#45932,.T.) ;
#48942 = ADVANCED_FACE('',(#13724),#10694,.T.) ;
#48943 = ADVANCED_FACE('',(#13725),#10695,.T.) ;
#48944 = ADVANCED_FACE('',(#13726),#10696,.T.) ;
#48945 = ADVANCED_FACE('',(#13727),#45933,.T.) ;
#48946 = ADVANCED_FACE('',(#13728),#10697,.T.) ;
#48947 = ADVANCED_FACE('',(#13729),#10698,.T.) ;
#48948 = ADVANCED_FACE('',(#13730),#10699,.T.) ;
#48949 = ADVANCED_FACE('',(#13731),#45934,.T.) ;
#48950 = ADVANCED_FACE('',(#13732),#10700,.T.) ;
#48951 = ADVANCED_FACE('',(#13733),#10701,.T.) ;
#48952 = ADVANCED_FACE('',(#13734),#10702,.T.) ;
#48953 = ADVANCED_FACE('',(#13735),#45935,.T.) ;
#48954 = ADVANCED_FACE('',(#13736),#10703,.T.) ;
#48955 = ADVANCED_FACE('',(#13737),#45936,.T.) ;
#48956 = ADVANCED_FACE('',(#13738),#45937,.T.) ;
#48957 = ADVANCED_FACE('',(#13739),#45938,.T.) ;
#48958 = ADVANCED_FACE('',(#13740),#10704,.T.) ;
#48959 = ADVANCED_FACE('',(#13741),#45939,.T.) ;
#48960 = ADVANCED_FACE('',(#13742),#45940,.T.) ;
#48961 = ADVANCED_FACE('',(#13743),#45941,.T.) ;
#48962 = ADVANCED_FACE('',(#13744),#10705,.T.) ;
#48963 = ADVANCED_FACE('',(#13745),#45942,.T.) ;
#48964 = ADVANCED_FACE('',(#13746),#45943,.T.) ;
#48965 = ADVANCED_FACE('',(#13747),#45944,.T.) ;
#48966 = ADVANCED_FACE('',(#13748),#10706,.T.) ;
#48967 = ADVANCED_FACE('',(#13749),#45945,.T.) ;
#48968 = ADVANCED_FACE('',(#13750),#45946,.T.) ;
#48969 = ADVANCED_FACE('',(#13751),#45947,.T.) ;
#48970 = ADVANCED_FACE('',(#13752),#10707,.T.) ;
#48971 = ADVANCED_FACE('',(#13753),#45948,.T.) ;
#48972 = ADVANCED_FACE('',(#13754),#45949,.T.) ;
#48973 = ADVANCED_FACE('',(#13755),#45950,.T.) ;
#48974 = ADVANCED_FACE('',(#13756),#10708,.T.) ;
#48975 = ADVANCED_FACE('',(#13757),#45951,.T.) ;
#48976 = ADVANCED_FACE('',(#13758),#45952,.T.) ;
#48977 = ADVANCED_FACE('',(#13759),#45953,.T.) ;
#48978 = ADVANCED_FACE('',(#13760),#10709,.T.) ;
#48979 = ADVANCED_FACE('',(#13761),#45954,.T.) ;
#48980 = ADVANCED_FACE('',(#13762),#45955,.T.) ;
#48981 = ADVANCED_FACE('',(#13763),#45956,.T.) ;
#48982 = ADVANCED_FACE('',(#13764),#10710,.T.) ;
#48983 = ADVANCED_FACE('',(#13765),#45957,.T.) ;
#48984 = ADVANCED_FACE('',(#13766),#45958,.T.) ;
#48985 = ADVANCED_FACE('',(#13767),#45959,.T.) ;
#48986 = ADVANCED_FACE('',(#13768),#10711,.T.) ;
#48987 = ADVANCED_FACE('',(#13769),#45960,.T.) ;
#48988 = ADVANCED_FACE('',(#13770),#45961,.T.) ;
#48989 = ADVANCED_FACE('',(#13771),#45962,.T.) ;
#48990 = ADVANCED_FACE('',(#13772),#10712,.T.) ;
#48991 = ADVANCED_FACE('',(#13773),#45963,.T.) ;
#48992 = ADVANCED_FACE('',(#13774),#45964,.T.) ;
#48993 = ADVANCED_FACE('',(#13775),#10713,.T.) ;
#48994 = ADVANCED_FACE('',(#13776),#3006,.T.) ;
#48995 = ADVANCED_FACE('',(#13777),#10714,.T.) ;
#48996 = ADVANCED_FACE('',(#13778),#3007,.T.) ;
#48997 = ADVANCED_FACE('',(#13779),#3008,.T.) ;
#48998 = ADVANCED_FACE('',(#13780),#3009,.T.) ;
#48999 = ADVANCED_FACE('',(#13781),#10715,.T.) ;
#49000 = ADVANCED_FACE('',(#13782),#3010,.T.) ;
#49001 = ADVANCED_FACE('',(#13783),#3011,.T.) ;
#49002 = ADVANCED_FACE('',(#13784),#10716,.T.) ;
#49003 = ADVANCED_FACE('',(#13785),#3012,.T.) ;
#49004 = ADVANCED_FACE('',(#13786),#3013,.T.) ;
#49005 = ADVANCED_FACE('',(#13787),#10717,.T.) ;
#49006 = ADVANCED_FACE('',(#13788),#3014,.T.) ;
#49007 = ADVANCED_FACE('',(#13789),#3015,.T.) ;
#49008 = ADVANCED_FACE('',(#13790),#10718,.T.) ;
#49009 = ADVANCED_FACE('',(#13791),#3016,.T.) ;
#49010 = ADVANCED_FACE('',(#13792),#3017,.T.) ;
#49011 = ADVANCED_FACE('',(#13793),#10719,.T.) ;
#49012 = ADVANCED_FACE('',(#13794),#3018,.T.) ;
#49013 = ADVANCED_FACE('',(#13795),#3019,.T.) ;
#49014 = ADVANCED_FACE('',(#13796),#10720,.T.) ;
#49015 = ADVANCED_FACE('',(#13797),#3020,.T.) ;
#49016 = ADVANCED_FACE('',(#13798),#3021,.T.) ;
#49017 = ADVANCED_FACE('',(#13799),#10721,.T.) ;
#49018 = ADVANCED_FACE('',(#13800),#3022,.T.) ;
#49019 = ADVANCED_FACE('',(#13801),#3023,.T.) ;
#49020 = ADVANCED_FACE('',(#13802),#10722,.T.) ;
#49021 = ADVANCED_FACE('',(#13803),#3024,.T.) ;
#49022 = ADVANCED_FACE('',(#13804),#3025,.T.) ;
#49023 = ADVANCED_FACE('',(#13805),#10723,.T.) ;
#49024 = ADVANCED_FACE('',(#13806),#10724,.T.) ;
#49025 = ADVANCED_FACE('',(#13807),#10725,.T.) ;
#49026 = ADVANCED_FACE('',(#13808),#10726,.T.) ;
#49027 = ADVANCED_FACE('',(#13809),#10727,.T.) ;
#49028 = ADVANCED_FACE('',(#13810),#10728,.T.) ;
#49029 = ADVANCED_FACE('',(#13811),#10729,.T.) ;
#49030 = ADVANCED_FACE('',(#13812),#10730,.T.) ;
#49031 = ADVANCED_FACE('',(#13813),#10731,.T.) ;
#49032 = ADVANCED_FACE('',(#13814),#10732,.T.) ;
#49033 = ADVANCED_FACE('',(#13815),#10733,.F.) ;
#49034 = ADVANCED_FACE('',(#13816),#10734,.T.) ;
#49035 = ADVANCED_FACE('',(#13817),#10735,.T.) ;
#49036 = ADVANCED_FACE('',(#13818),#10736,.T.) ;
#49037 = ADVANCED_FACE('',(#13819),#10737,.T.) ;
#49038 = ADVANCED_FACE('',(#13820),#10738,.T.) ;
#49039 = ADVANCED_FACE('',(#13821),#10739,.T.) ;
#49040 = ADVANCED_FACE('',(#13822),#10740,.T.) ;
#49041 = ADVANCED_FACE('',(#13823),#10741,.T.) ;
#49042 = ADVANCED_FACE('',(#13824),#10742,.T.) ;
#49043 = ADVANCED_FACE('',(#13825),#10743,.T.) ;
#49044 = ADVANCED_FACE('',(#13826,#770,#771,#772),#10744,.T.) ;
#49045 = ADVANCED_FACE('',(#13827),#10745,.T.) ;
#49046 = ADVANCED_FACE('',(#13828),#10746,.T.) ;
#49047 = ADVANCED_FACE('',(#13829),#3026,.T.) ;
#49048 = ADVANCED_FACE('',(#13830),#2115,.F.) ;
#49049 = ADVANCED_FACE('',(#13831),#3027,.F.) ;
#49050 = ADVANCED_FACE('',(#13832),#2116,.F.) ;
#49051 = ADVANCED_FACE('',(#13833),#3028,.T.) ;
#49052 = ADVANCED_FACE('',(#13834),#2117,.F.) ;
#49053 = ADVANCED_FACE('',(#13835),#3029,.F.) ;
#49054 = ADVANCED_FACE('',(#13836),#2118,.F.) ;
#49055 = ADVANCED_FACE('',(#13837),#3030,.F.) ;
#49056 = ADVANCED_FACE('',(#13838),#3031,.T.) ;
#49057 = CLOSED_SHELL('',(#45965,#45966,#45967,#45968,#45969,#45970,#45971,
#45972,#45973,#45974,#45975,#45976,#45977,#45978,#45979,#45980,#45981,#45982,
#45983,#45984,#45985,#45986,#45987,#45988,#45989,#45990,#45991,#45992,#45993,
#45994,#45995,#45996,#45997,#45998,#45999,#46000,#46001,#46002,#46003,#46004,
#46005,#46006,#46007,#46008,#46009,#46010,#46011,#46012,#46013,#46014,#46015,
#46016,#46017,#46018,#46019,#46020,#46021,#46022,#46023,#46024,#46025,#46026,
#46027,#46028,#46029,#46030,#46031,#46032,#46033,#46034,#46035,#46036,#46037,
#46038,#46039,#46040,#46041,#46042,#46043,#46044,#46045,#46046,#46047,#46048,
#46049,#46050,#46051,#46052,#46053,#46054,#46055,#46056,#46057,#46058,#46059,
#46060,#46061,#46062,#46063,#46064,#46065,#46066,#46067,#46068,#46069,#46070,
#46071,#46072,#46073,#46074,#46075,#46076,#46077,#46078,#46079,#46080,#46081,
#46082,#46083,#46084,#46085,#46086,#46087,#46088,#46089,#46090,#46091,#46092,
#46093,#46094,#46095,#46096,#46097,#46098,#46099,#46100,#46101,#46102,#46103,
#46104,#46105,#46106,#46107,#46108,#46109,#46110,#46111,#46112,#46113,#46114,
#46115,#46116,#46117,#46118,#46119,#46120,#46121,#46122,#46123,#46124,#46125,
#46126,#46127,#46128,#46129,#46130,#46131,#46132,#46133,#46134,#46135,#46136,
#46137,#46138,#46139,#46140,#46141,#46142,#46143,#46144,#46145,#46146,#46147,
#46148,#46149,#46150,#46151,#46152,#46153,#46154,#46155,#46156,#46157,#46158,
#46159,#46160,#46161,#46162,#46163,#46164,#46165,#46166,#46167,#46168,#46169,
#46170,#46171,#46172,#46173,#46174,#46175,#46176,#46177,#46178,#46179,#46180,
#46181,#46182,#46183,#46184,#46185,#46186,#46187,#46188,#46189,#46190,#46191,
#46192,#46193,#46194,#46195,#46196,#46197,#46198,#46199,#46200,#46201,#46202,
#46203,#46204,#46205,#46206,#46207,#46208,#46209,#46210,#46211,#46212,#46213,
#46214,#46215,#46216,#46217,#46218,#46219,#46220,#46221,#46222,#46223)) ;
#49058 = CLOSED_SHELL('',(#46224,#46225,#46226,#46227,#46228,#46229,#46230,
#46231,#46232,#46233,#46234,#46235,#46236,#46237,#46238,#46239,#46240,#46241,
#46242,#46243,#46244,#46245,#46246,#46247,#46248,#46249,#46250,#46251,#46252,
#46253,#46254,#46255,#46256,#46257,#46258,#46259,#46260,#46261,#46262,#46263,
#46264,#46265,#46266,#46267,#46268,#46269,#46270,#46271,#46272,#46273,#46274,
#46275,#46276,#46277,#46278,#46279,#46280,#46281,#46282,#46283,#46284,#46285,
#46286,#46287,#46288,#46289,#46290,#46291,#46292,#46293,#46294,#46295,#46296,
#46297,#46298,#46299,#46300,#46301,#46302,#46303,#46304,#46305,#46306,#46307,
#46308,#46309,#46310,#46311,#46312,#46313,#46314,#46315,#46316,#46317,#46318,
#46319,#46320,#46321,#46322,#46323,#46324,#46325,#46326,#46327,#46328,#46329,
#46330,#46331,#46332,#46333,#46334,#46335,#46336,#46337,#46338,#46339,#46340,
#46341,#46342,#46343,#46344,#46345,#46346,#46347,#46348,#46349,#46350,#46351,
#46352,#46353,#46354,#46355,#46356,#46357,#46358,#46359,#46360,#46361,#46362,
#46363,#46364,#46365,#46366,#46367,#46368,#46369,#46370,#46371,#46372,#46373,
#46374,#46375,#46376,#46377,#46378,#46379,#46380,#46381,#46382,#46383,#46384,
#46385,#46386,#46387,#46388,#46389,#46390,#46391,#46392,#46393,#46394,#46395,
#46396,#46397,#46398,#46399,#46400,#46401,#46402,#46403,#46404,#46405,#46406,
#46407,#46408,#46409,#46410,#46411,#46412,#46413,#46414,#46415,#46416,#46417,
#46418,#46419,#46420,#46421,#46422,#46423,#46424,#46425)) ;
#49059 = CLOSED_SHELL('',(#46426,#46427,#46428,#46429,#46430,#46431,#46432,
#46433,#46434,#46435,#46436,#46437,#46438,#46439,#46440,#46441,#46442,#46443,
#46444,#46445,#46446,#46447,#46448,#46449,#46450,#46451,#46452,#46453,#46454,
#46455,#46456,#46457,#46458,#46459,#46460,#46461,#46462,#46463,#46464,#46465,
#46466,#46467,#46468,#46469,#46470,#46471,#46472,#46473,#46474,#46475,#46476,
#46477,#46478,#46479,#46480,#46481,#46482,#46483,#46484,#46485,#46486,#46487,
#46488,#46489,#46490,#46491,#46492,#46493,#46494,#46495,#46496,#46497,#46498,
#46499,#46500,#46501,#46502,#46503,#46504,#46505,#46506,#46507,#46508,#46509,
#46510,#46511,#46512,#46513,#46514,#46515,#46516,#46517,#46518,#46519,#46520,
#46521,#46522,#46523,#46524,#46525,#46526,#46527,#46528,#46529,#46530,#46531,
#46532,#46533,#46534,#46535,#46536,#46537,#46538,#46539,#46540,#46541,#46542,
#46543,#46544,#46545,#46546,#46547,#46548,#46549,#46550,#46551,#46552,#46553,
#46554,#46555,#46556,#46557,#46558,#46559,#46560,#46561,#46562,#46563,#46564,
#46565,#46566,#46567,#46568,#46569,#46570,#46571,#46572,#46573,#46574,#46575,
#46576,#46577,#46578,#46579,#46580,#46581,#46582,#46583,#46584,#46585,#46586,
#46587,#46588,#46589,#46590,#46591,#46592,#46593,#46594,#46595,#46596,#46597,
#46598,#46599,#46600,#46601,#46602,#46603,#46604,#46605,#46606,#46607,#46608,
#46609,#46610,#46611,#46612,#46613,#46614,#46615,#46616,#46617,#46618,#46619,
#46620,#46621,#46622,#46623,#46624,#46625,#46626,#46627,#46628,#46629,#46630,
#46631,#46632,#46633,#46634,#46635,#46636,#46637,#46638,#46639,#46640,#46641,
#46642,#46643,#46644,#46645,#46646,#46647,#46648,#46649,#46650,#46651,#46652,
#46653,#46654,#46655,#46656,#46657,#46658,#46659,#46660,#46661,#46662,#46663,
#46664,#46665,#46666,#46667,#46668,#46669,#46670,#46671,#46672,#46673,#46674,
#46675,#46676,#46677,#46678,#46679,#46680,#46681,#46682,#46683,#46684,#46685,
#46686,#46687,#46688,#46689,#46690,#46691,#46692,#46693,#46694,#46695,#46696,
#46697,#46698,#46699,#46700,#46701,#46702,#46703,#46704,#46705,#46706,#46707,
#46708,#46709,#46710,#46711,#46712,#46713,#46714,#46715,#46716,#46717,#46718,
#46719,#46720,#46721,#46722,#46723,#46724,#46725,#46726,#46727,#46728,#46729,
#46730,#46731,#46732,#46733,#46734,#46735,#46736,#46737,#46738,#46739,#46740,
#46741,#46742,#46743,#46744,#46745,#46746,#46747,#46748,#46749,#46750,#46751,
#46752,#46753,#46754,#46755,#46756,#46757,#46758,#46759,#46760,#46761,#46762,
#46763,#46764,#46765,#46766,#46767,#46768,#46769,#46770,#46771,#46772,#46773,
#46774,#46775,#46776,#46777,#46778,#46779,#46780,#46781,#46782,#46783,#46784,
#46785,#46786,#46787,#46788,#46789,#46790,#46791,#46792,#46793,#46794,#46795,
#46796,#46797,#46798,#46799,#46800,#46801,#46802,#46803,#46804,#46805,#46806,
#46807,#46808,#46809,#46810,#46811,#46812,#46813,#46814,#46815,#46816,#46817,
#46818,#46819,#46820,#46821,#46822,#46823,#46824,#46825,#46826,#46827,#46828,
#46829,#46830,#46831,#46832,#46833,#46834,#46835,#46836,#46837,#46838,#46839,
#46840,#46841,#46842,#46843,#46844,#46845,#46846,#46847,#46848,#46849,#46850,
#46851,#46852,#46853,#46854,#46855,#46856,#46857,#46858,#46859,#46860,#46861,
#46862,#46863,#46864,#46865,#46866,#46867,#46868,#46869,#46870,#46871,#46872,
#46873,#46874,#46875,#46876,#46877,#46878,#46879,#46880,#46881,#46882,#46883,
#46884,#46885,#46886,#46887,#46888,#46889,#46890,#46891,#46892,#46893,#46894,
#46895,#46896,#46897,#46898,#46899,#46900,#46901,#46902,#46903,#46904,#46905,
#46906,#46907,#46908,#46909,#46910,#46911,#46912,#46913,#46914,#46915,#46916,
#46917,#46918,#46919,#46920,#46921,#46922,#46923,#46924,#46925,#46926,#46927,
#46928,#46929,#46930,#46931,#46932,#46933,#46934,#46935,#46936,#46937,#46938,
#46939,#46940,#46941,#46942,#46943,#46944,#46945,#46946,#46947,#46948,#46949,
#46950,#46951,#46952,#46953,#46954,#46955,#46956,#46957,#46958,#46959,#46960,
#46961,#46962,#46963,#46964,#46965,#46966,#46967,#46968,#46969,#46970,#46971,
#46972,#46973,#46974,#46975,#46976,#46977,#46978,#46979,#46980,#46981,#46982,
#46983,#46984,#46985,#46986,#46987,#46988,#46989,#46990,#46991,#46992,#46993,
#46994,#46995,#46996,#46997,#46998,#46999,#47000,#47001,#47002,#47003,#47004,
#47005,#47006,#47007,#47008,#47009,#47010,#47011,#47012,#47013,#47014,#47015,
#47016,#47017,#47018,#47019,#47020,#47021,#47022,#47023,#47024,#47025,#47026,
#47027,#47028,#47029,#47030,#47031,#47032,#47033,#47034,#47035,#47036,#47037,
#47038,#47039,#47040,#47041,#47042,#47043,#47044,#47045,#47046,#47047,#47048,
#47049,#47050,#47051,#47052,#47053,#47054,#47055,#47056,#47057,#47058,#47059,
#47060,#47061,#47062,#47063,#47064,#47065,#47066,#47067,#47068,#47069,#47070,
#47071,#47072,#47073,#47074,#47075,#47076,#47077,#47078,#47079,#47080,#47081,
#47082,#47083,#47084,#47085,#47086,#47087,#47088,#47089,#47090,#47091,#47092,
#47093,#47094,#47095,#47096,#47097,#47098,#47099,#47100,#47101,#47102,#47103,
#47104,#47105,#47106,#47107,#47108,#47109,#47110,#47111,#47112,#47113,#47114,
#47115,#47116,#47117,#47118,#47119,#47120,#47121,#47122,#47123,#47124,#47125,
#47126,#47127,#47128,#47129,#47130,#47131,#47132,#47133,#47134,#47135,#47136,
#47137,#47138,#47139,#47140,#47141,#47142,#47143,#47144,#47145,#47146,#47147,
#47148,#47149,#47150,#47151,#47152,#47153,#47154,#47155,#47156,#47157,#47158,
#47159,#47160,#47161,#47162,#47163,#47164,#47165,#47166,#47167,#47168,#47169,
#47170,#47171,#47172,#47173,#47174,#47175,#47176,#47177,#47178)) ;
#49060 = CLOSED_SHELL('',(#47179,#47180,#47181,#47182,#47183,#47184,#47185,
#47186,#47187,#47188,#47189,#47190,#47191,#47192,#47193)) ;
#49061 = CLOSED_SHELL('',(#47194,#47195,#47196,#47197,#47198,#47199,#47200,
#47201,#47202,#47203,#47204,#47205,#47206,#47207,#47208,#47209,#47210,#47211,
#47212,#47213,#47214,#47215,#47216,#47217,#47218,#47219,#47220,#47221,#47222,
#47223,#47224,#47225,#47226,#47227,#47228,#47229,#47230,#47231,#47232,#47233,
#47234,#47235,#47236,#47237,#47238,#47239,#47240,#47241,#47242,#47243,#47244,
#47245,#47246,#47247,#47248,#47249,#47250,#47251,#47252,#47253,#47254,#47255,
#47256,#47257,#47258,#47259,#47260,#47261,#47262,#47263,#47264,#47265,#47266,
#47267,#47268,#47269,#47270,#47271,#47272,#47273,#47274,#47275,#47276,#47277,
#47278,#47279,#47280,#47281,#47282,#47283,#47284,#47285,#47286,#47287,#47288,
#47289,#47290,#47291,#47292,#47293,#47294,#47295,#47296,#47297,#47298,#47299,
#47300,#47301,#47302,#47303,#47304,#47305,#47306,#47307,#47308,#47309,#47310,
#47311,#47312,#47313,#47314)) ;
#49062 = CLOSED_SHELL('',(#47315,#47316,#47317,#47318,#47319,#47320)) ;
#49063 = CLOSED_SHELL('',(#47321,#47322,#47323,#47324)) ;
#49064 = CLOSED_SHELL('',(#47325,#47326,#47327,#47328)) ;
#49065 = CLOSED_SHELL('',(#47329,#47330,#47331,#47332,#47333)) ;
#49066 = CLOSED_SHELL('',(#47334,#47335,#47336,#47337,#47338,#47339,#47340,
#47341,#47342,#47343,#47344,#47345,#47346,#47347,#47348,#47349,#47350,#47351,
#47352,#47353,#47354,#47355,#47356,#47357,#47358,#47359,#47360,#47361,#47362,
#47363,#47364,#47365,#47366,#47367,#47368,#47369,#47370,#47371,#47372,#47373,
#47374,#47375,#47376,#47377,#47378,#47379,#47380,#47381,#47382,#47383,#47384,
#47385,#47386,#47387,#47388,#47389,#47390,#47391,#47392,#47393,#47394,#47395,
#47396,#47397,#47398,#47399,#47400,#47401,#47402,#47403,#47404,#47405,#47406,
#47407,#47408,#47409,#47410,#47411)) ;
#49067 = CLOSED_SHELL('',(#47412,#47413,#47414,#47415,#47416,#47417,#47418,
#47419,#47420,#47421,#47422,#47423,#47424,#47425,#47426,#47427,#47428,#47429,
#47430,#47431,#47432)) ;
#49068 = CLOSED_SHELL('',(#47433,#47434,#47435,#47436,#47437,#47438,#47439,
#47440,#47441,#47442,#47443,#47444,#47445,#47446,#47447,#47448,#47449,#47450,
#47451,#47452,#47453,#47454,#47455,#47456,#47457,#47458,#47459,#47460,#47461,
#47462,#47463,#47464,#47465,#47466,#47467,#47468,#47469,#47470,#47471,#47472,
#47473,#47474)) ;
#49069 = CLOSED_SHELL('',(#47475,#47476,#47477,#47478,#47479,#47480,#47481,
#47482,#47483,#47484,#47485,#47486,#47487,#47488,#47489,#47490,#47491,#47492,
#47493,#47494,#47495,#47496,#47497,#47498,#47499,#47500,#47501,#47502,#47503,
#47504,#47505,#47506,#47507,#47508,#47509,#47510,#47511,#47512,#47513,#47514,
#47515,#47516)) ;
#49070 = CLOSED_SHELL('',(#47517,#47518,#47519,#47520,#47521,#47522,#47523,
#47524,#47525,#47526,#47527,#47528,#47529,#47530,#47531,#47532,#47533,#47534,
#47535,#47536,#47537,#47538,#47539,#47540,#47541,#47542,#47543,#47544,#47545,
#47546,#47547,#47548,#47549,#47550,#47551,#47552,#47553,#47554,#47555,#47556,
#47557,#47558)) ;
#49071 = CLOSED_SHELL('',(#47559,#47560,#47561,#47562,#47563,#47564,#47565,
#47566,#47567,#47568,#47569,#47570,#47571,#47572,#47573,#47574,#47575,#47576,
#47577,#47578,#47579,#47580,#47581,#47582,#47583,#47584,#47585,#47586,#47587,
#47588,#47589,#47590,#47591,#47592,#47593,#47594,#47595,#47596,#47597,#47598,
#47599)) ;
#49072 = CLOSED_SHELL('',(#47600,#47601,#47602,#47603,#47604,#47605,#47606,
#47607,#47608,#47609,#47610,#47611,#47612,#47613,#47614,#47615,#47616,#47617,
#47618,#47619,#47620,#47621,#47622,#47623,#47624,#47625,#47626,#47627,#47628,
#47629,#47630,#47631,#47632,#47633,#47634,#47635,#47636,#47637,#47638,#47639,
#47640,#47641,#47642,#47643,#47644,#47645,#47646,#47647,#47648,#47649,#47650,
#47651,#47652,#47653,#47654,#47655,#47656,#47657,#47658,#47659,#47660,#47661,
#47662,#47663,#47664,#47665,#47666,#47667,#47668,#47669,#47670,#47671,#47672,
#47673,#47674,#47675,#47676,#47677,#47678,#47679,#47680,#47681,#47682,#47683,
#47684,#47685,#47686,#47687,#47688,#47689,#47690,#47691,#47692,#47693,#47694,
#47695,#47696,#47697,#47698,#47699,#47700,#47701,#47702,#47703,#47704,#47705,
#47706,#47707,#47708,#47709,#47710,#47711,#47712,#47713,#47714,#47715,#47716,
#47717,#47718,#47719,#47720,#47721,#47722,#47723,#47724,#47725,#47726,#47727,
#47728,#47729,#47730,#47731,#47732,#47733,#47734,#47735,#47736,#47737,#47738,
#47739,#47740,#47741,#47742,#47743,#47744,#47745,#47746,#47747,#47748,#47749,
#47750,#47751,#47752,#47753,#47754,#47755,#47756,#47757,#47758,#47759,#47760,
#47761,#47762,#47763,#47764,#47765,#47766,#47767,#47768,#47769,#47770,#47771,
#47772,#47773,#47774,#47775,#47776,#47777,#47778,#47779,#47780,#47781,#47782,
#47783,#47784,#47785,#47786,#47787,#47788,#47789,#47790,#47791,#47792,#47793,
#47794,#47795,#47796,#47797,#47798,#47799,#47800,#47801,#47802,#47803,#47804,
#47805,#47806,#47807,#47808,#47809,#47810,#47811,#47812,#47813,#47814,#47815,
#47816,#47817,#47818,#47819,#47820,#47821,#47822,#47823,#47824,#47825,#47826,
#47827,#47828,#47829,#47830,#47831,#47832,#47833,#47834,#47835,#47836,#47837,
#47838,#47839,#47840,#47841,#47842,#47843,#47844,#47845,#47846,#47847,#47848,
#47849,#47850,#47851,#47852,#47853,#47854,#47855,#47856,#47857,#47858,#47859,
#47860,#47861,#47862,#47863,#47864,#47865,#47866,#47867,#47868,#47869,#47870,
#47871,#47872,#47873,#47874,#47875,#47876,#47877,#47878,#47879,#47880,#47881,
#47882,#47883,#47884,#47885,#47886,#47887,#47888,#47889,#47890,#47891,#47892,
#47893,#47894,#47895,#47896,#47897,#47898,#47899,#47900,#47901,#47902,#47903,
#47904,#47905,#47906,#47907,#47908,#47909,#47910,#47911,#47912,#47913,#47914,
#47915,#47916,#47917,#47918,#47919,#47920,#47921,#47922,#47923,#47924,#47925,
#47926,#47927,#47928,#47929,#47930,#47931,#47932,#47933,#47934,#47935,#47936,
#47937,#47938,#47939,#47940,#47941,#47942,#47943,#47944,#47945,#47946,#47947,
#47948,#47949,#47950,#47951,#47952,#47953,#47954,#47955,#47956,#47957,#47958,
#47959,#47960,#47961,#47962,#47963,#47964,#47965,#47966,#47967,#47968,#47969,
#47970,#47971,#47972,#47973,#47974,#47975,#47976,#47977,#47978,#47979,#47980,
#47981,#47982,#47983,#47984,#47985,#47986,#47987,#47988,#47989,#47990,#47991,
#47992,#47993,#47994,#47995,#47996,#47997,#47998,#47999,#48000,#48001,#48002,
#48003,#48004,#48005,#48006,#48007,#48008,#48009,#48010,#48011,#48012,#48013,
#48014,#48015,#48016,#48017,#48018,#48019,#48020,#48021,#48022,#48023,#48024,
#48025,#48026,#48027,#48028,#48029,#48030,#48031,#48032,#48033,#48034,#48035,
#48036,#48037,#48038,#48039,#48040,#48041,#48042,#48043,#48044,#48045,#48046,
#48047,#48048,#48049,#48050,#48051,#48052,#48053,#48054,#48055,#48056,#48057,
#48058,#48059,#48060,#48061,#48062,#48063,#48064,#48065,#48066,#48067,#48068,
#48069,#48070,#48071,#48072,#48073,#48074,#48075,#48076,#48077,#48078,#48079,
#48080,#48081,#48082,#48083,#48084,#48085,#48086,#48087,#48088,#48089,#48090,
#48091,#48092,#48093,#48094,#48095,#48096,#48097,#48098,#48099,#48100,#48101,
#48102,#48103,#48104,#48105,#48106,#48107,#48108,#48109,#48110,#48111,#48112,
#48113,#48114,#48115,#48116,#48117,#48118,#48119,#48120,#48121,#48122,#48123,
#48124,#48125,#48126,#48127,#48128,#48129,#48130,#48131,#48132,#48133,#48134,
#48135,#48136,#48137,#48138,#48139,#48140,#48141,#48142,#48143,#48144,#48145,
#48146,#48147,#48148,#48149,#48150,#48151,#48152,#48153,#48154,#48155,#48156,
#48157,#48158,#48159,#48160,#48161,#48162,#48163,#48164,#48165,#48166,#48167,
#48168,#48169,#48170,#48171,#48172,#48173,#48174,#48175,#48176,#48177,#48178,
#48179,#48180,#48181,#48182,#48183,#48184,#48185,#48186,#48187,#48188,#48189,
#48190,#48191,#48192,#48193,#48194,#48195,#48196,#48197,#48198,#48199,#48200,
#48201,#48202,#48203,#48204,#48205,#48206,#48207,#48208,#48209,#48210,#48211,
#48212,#48213,#48214,#48215,#48216,#48217,#48218,#48219,#48220,#48221,#48222,
#48223,#48224,#48225,#48226,#48227,#48228,#48229,#48230,#48231,#48232,#48233,
#48234,#48235,#48236,#48237,#48238,#48239,#48240,#48241,#48242,#48243,#48244,
#48245,#48246,#48247,#48248,#48249,#48250,#48251,#48252,#48253,#48254,#48255,
#48256,#48257,#48258,#48259,#48260,#48261,#48262,#48263,#48264,#48265,#48266,
#48267,#48268,#48269,#48270,#48271,#48272,#48273,#48274,#48275,#48276,#48277,
#48278,#48279,#48280,#48281,#48282,#48283,#48284,#48285,#48286,#48287,#48288,
#48289,#48290,#48291,#48292,#48293,#48294,#48295,#48296,#48297,#48298,#48299,
#48300,#48301,#48302,#48303,#48304,#48305,#48306,#48307,#48308,#48309,#48310,
#48311,#48312,#48313,#48314,#48315,#48316,#48317,#48318,#48319,#48320,#48321,
#48322,#48323,#48324,#48325,#48326,#48327,#48328,#48329,#48330,#48331,#48332,
#48333,#48334,#48335,#48336,#48337,#48338,#48339,#48340,#48341,#48342,#48343,
#48344,#48345,#48346,#48347,#48348,#48349,#48350,#48351,#48352,#48353,#48354,
#48355,#48356,#48357,#48358,#48359,#48360,#48361,#48362,#48363,#48364,#48365,
#48366,#48367,#48368,#48369,#48370,#48371,#48372,#48373,#48374,#48375,#48376,
#48377,#48378,#48379,#48380,#48381,#48382,#48383,#48384,#48385,#48386,#48387,
#48388,#48389,#48390,#48391,#48392,#48393,#48394,#48395,#48396,#48397,#48398,
#48399,#48400,#48401,#48402,#48403,#48404,#48405,#48406,#48407,#48408,#48409,
#48410,#48411,#48412,#48413,#48414,#48415,#48416,#48417,#48418,#48419,#48420,
#48421,#48422,#48423,#48424,#48425)) ;
#49073 = CLOSED_SHELL('',(#48426,#48427,#48428,#48429,#48430,#48431,#48432,
#48433,#48434,#48435,#48436,#48437,#48438,#48439,#48440)) ;
#49074 = CLOSED_SHELL('',(#48441,#48442,#48443,#48444,#48445,#48446,#48447,
#48448,#48449,#48450,#48451)) ;
#49075 = CLOSED_SHELL('',(#48452,#48453,#48454,#48455,#48456,#48457,#48458,
#48459,#48460,#48461,#48462,#48463,#48464,#48465,#48466,#48467,#48468,#48469,
#48470,#48471,#48472,#48473,#48474,#48475,#48476,#48477,#48478,#48479,#48480,
#48481,#48482,#48483,#48484,#48485,#48486,#48487,#48488,#48489,#48490,#48491,
#48492,#48493,#48494,#48495,#48496,#48497,#48498,#48499,#48500,#48501,#48502,
#48503,#48504,#48505,#48506,#48507,#48508,#48509,#48510,#48511,#48512,#48513,
#48514,#48515,#48516,#48517,#48518,#48519,#48520,#48521,#48522,#48523,#48524,
#48525,#48526,#48527,#48528,#48529,#48530,#48531,#48532,#48533,#48534,#48535,
#48536,#48537,#48538,#48539,#48540,#48541,#48542,#48543,#48544,#48545,#48546,
#48547,#48548,#48549,#48550,#48551,#48552,#48553,#48554,#48555,#48556,#48557,
#48558,#48559,#48560,#48561,#48562,#48563,#48564,#48565,#48566,#48567,#48568,
#48569,#48570,#48571,#48572,#48573,#48574,#48575,#48576,#48577,#48578,#48579,
#48580,#48581,#48582,#48583,#48584,#48585,#48586,#48587,#48588,#48589,#48590,
#48591,#48592,#48593,#48594,#48595,#48596,#48597,#48598,#48599,#48600,#48601,
#48602,#48603,#48604,#48605,#48606,#48607,#48608,#48609,#48610,#48611,#48612,
#48613,#48614,#48615,#48616,#48617,#48618,#48619,#48620,#48621,#48622,#48623,
#48624,#48625,#48626,#48627,#48628,#48629,#48630,#48631,#48632,#48633,#48634,
#48635,#48636,#48637,#48638,#48639,#48640,#48641,#48642,#48643,#48644,#48645,
#48646,#48647,#48648,#48649,#48650,#48651,#48652,#48653,#48654,#48655,#48656,
#48657,#48658,#48659,#48660,#48661,#48662,#48663,#48664,#48665,#48666,#48667,
#48668,#48669,#48670,#48671,#48672,#48673,#48674,#48675,#48676,#48677,#48678,
#48679,#48680,#48681,#48682,#48683,#48684,#48685,#48686,#48687,#48688,#48689,
#48690,#48691,#48692,#48693,#48694,#48695,#48696,#48697,#48698,#48699,#48700,
#48701,#48702,#48703,#48704,#48705,#48706,#48707,#48708,#48709,#48710,#48711,
#48712,#48713,#48714,#48715,#48716,#48717,#48718,#48719,#48720,#48721,#48722,
#48723,#48724,#48725,#48726,#48727,#48728,#48729,#48730,#48731,#48732,#48733,
#48734,#48735,#48736,#48737,#48738,#48739,#48740,#48741,#48742)) ;
#49076 = CLOSED_SHELL('',(#48743,#48744,#48745,#48746,#48747,#48748,#48749,
#48750,#48751,#48752,#48753,#48754,#48755,#48756,#48757,#48758,#48759,#48760,
#48761,#48762,#48763,#48764,#48765,#48766,#48767,#48768,#48769,#48770,#48771,
#48772,#48773,#48774,#48775,#48776,#48777,#48778,#48779,#48780,#48781,#48782,
#48783,#48784,#48785,#48786,#48787,#48788,#48789,#48790,#48791,#48792,#48793,
#48794,#48795,#48796,#48797,#48798,#48799,#48800,#48801,#48802,#48803,#48804,
#48805,#48806,#48807,#48808,#48809,#48810,#48811,#48812,#48813,#48814,#48815,
#48816,#48817,#48818,#48819,#48820,#48821,#48822,#48823,#48824,#48825,#48826,
#48827,#48828,#48829,#48830,#48831,#48832,#48833,#48834,#48835,#48836,#48837,
#48838,#48839,#48840,#48841,#48842,#48843,#48844,#48845,#48846,#48847,#48848,
#48849,#48850,#48851,#48852,#48853,#48854,#48855,#48856,#48857,#48858,#48859,
#48860,#48861,#48862,#48863,#48864,#48865,#48866,#48867,#48868,#48869,#48870,
#48871,#48872,#48873,#48874,#48875,#48876,#48877,#48878,#48879,#48880,#48881,
#48882,#48883,#48884,#48885,#48886,#48887,#48888,#48889,#48890,#48891,#48892,
#48893,#48894,#48895,#48896,#48897,#48898,#48899,#48900,#48901,#48902,#48903,
#48904,#48905,#48906,#48907,#48908,#48909,#48910,#48911,#48912,#48913,#48914,
#48915,#48916,#48917,#48918,#48919,#48920,#48921,#48922,#48923,#48924,#48925,
#48926,#48927,#48928,#48929,#48930,#48931,#48932,#48933,#48934,#48935,#48936,
#48937,#48938,#48939,#48940,#48941,#48942,#48943,#48944,#48945,#48946,#48947,
#48948,#48949,#48950,#48951,#48952,#48953,#48954,#48955,#48956,#48957,#48958,
#48959,#48960,#48961,#48962,#48963,#48964,#48965,#48966,#48967,#48968,#48969,
#48970,#48971,#48972,#48973,#48974,#48975,#48976,#48977,#48978,#48979,#48980,
#48981,#48982,#48983,#48984,#48985,#48986,#48987,#48988,#48989,#48990,#48991,
#48992,#48993,#48994,#48995,#48996,#48997,#48998,#48999,#49000,#49001,#49002,
#49003,#49004,#49005,#49006,#49007,#49008,#49009,#49010,#49011,#49012,#49013,
#49014,#49015,#49016,#49017,#49018,#49019,#49020,#49021,#49022,#49023,#49024,
#49025,#49026,#49027,#49028,#49029,#49030,#49031,#49032,#49033)) ;
#49077 = CLOSED_SHELL('',(#49034,#49035,#49036,#49037,#49038,#49039,#49040,
#49041,#49042,#49043,#49044,#49045,#49046,#49047,#49048,#49049,#49050,#49051,
#49052,#49053,#49054,#49055,#49056)) ;
#49078 = DERIVED_UNIT_ELEMENT(#49120,1.) ;
#49079 = DERIVED_UNIT_ELEMENT(#117172,-3.) ;
#49080 = DERIVED_UNIT_ELEMENT(#49120,1.) ;
#49081 = DERIVED_UNIT_ELEMENT(#117172,-3.) ;
#49082 = DERIVED_UNIT_ELEMENT(#49120,1.) ;
#49083 = DERIVED_UNIT_ELEMENT(#117172,-3.) ;
#49084 = DERIVED_UNIT_ELEMENT(#49120,1.) ;
#49085 = DERIVED_UNIT_ELEMENT(#117172,-3.) ;
#49086 = DERIVED_UNIT_ELEMENT(#49120,1.) ;
#49087 = DERIVED_UNIT_ELEMENT(#117172,-3.) ;
#49088 = DERIVED_UNIT_ELEMENT(#49120,1.) ;
#49089 = DERIVED_UNIT_ELEMENT(#117172,-3.) ;
#49090 = DERIVED_UNIT_ELEMENT(#49120,1.) ;
#49091 = DERIVED_UNIT_ELEMENT(#117172,-3.) ;
#49092 = DERIVED_UNIT_ELEMENT(#49120,1.) ;
#49093 = DERIVED_UNIT_ELEMENT(#117172,-3.) ;
#49094 = DERIVED_UNIT_ELEMENT(#49120,1.) ;
#49095 = DERIVED_UNIT_ELEMENT(#117172,-3.) ;
#49096 = DERIVED_UNIT_ELEMENT(#49120,1.) ;
#49097 = DERIVED_UNIT_ELEMENT(#117172,-3.) ;
#49098 = DERIVED_UNIT_ELEMENT(#49120,1.) ;
#49099 = DERIVED_UNIT_ELEMENT(#117172,-3.) ;
#49100 = DERIVED_UNIT_ELEMENT(#49120,1.) ;
#49101 = DERIVED_UNIT_ELEMENT(#117172,-3.) ;
#49102 = DERIVED_UNIT_ELEMENT(#49120,1.) ;
#49103 = DERIVED_UNIT_ELEMENT(#117172,-3.) ;
#49104 = DERIVED_UNIT_ELEMENT(#49120,1.) ;
#49105 = DERIVED_UNIT_ELEMENT(#117172,-3.) ;
#49106 = DERIVED_UNIT_ELEMENT(#49120,1.) ;
#49107 = DERIVED_UNIT_ELEMENT(#117172,-3.) ;
#49108 = DERIVED_UNIT_ELEMENT(#49120,1.) ;
#49109 = DERIVED_UNIT_ELEMENT(#117172,-3.) ;
#49110 = DERIVED_UNIT_ELEMENT(#49120,1.) ;
#49111 = DERIVED_UNIT_ELEMENT(#117172,-3.) ;
#49112 = DERIVED_UNIT_ELEMENT(#49120,1.) ;
#49113 = DERIVED_UNIT_ELEMENT(#117172,-3.) ;
#49114 = DERIVED_UNIT_ELEMENT(#49120,1.) ;
#49115 = DERIVED_UNIT_ELEMENT(#117172,-3.) ;
#49116 = DERIVED_UNIT_ELEMENT(#49120,1.) ;
#49117 = DERIVED_UNIT_ELEMENT(#117172,-3.) ;
#49118 = DERIVED_UNIT_ELEMENT(#49120,1.) ;
#49119 = DERIVED_UNIT_ELEMENT(#117172,-3.) ;
#49120 = (
MASS_UNIT()
NAMED_UNIT(*)
SI_UNIT(.KILO.,.GRAM.)
) ;
#49121 = DERIVED_UNIT((#49078,#49079)) ;
#49122 = DERIVED_UNIT((#49080,#49081)) ;
#49123 = DERIVED_UNIT((#49082,#49083)) ;
#49124 = DERIVED_UNIT((#49084,#49085)) ;
#49125 = DERIVED_UNIT((#49086,#49087)) ;
#49126 = DERIVED_UNIT((#49088,#49089)) ;
#49127 = DERIVED_UNIT((#49090,#49091)) ;
#49128 = DERIVED_UNIT((#49092,#49093)) ;
#49129 = DERIVED_UNIT((#49094,#49095)) ;
#49130 = DERIVED_UNIT((#49096,#49097)) ;
#49131 = DERIVED_UNIT((#49098,#49099)) ;
#49132 = DERIVED_UNIT((#49100,#49101)) ;
#49133 = DERIVED_UNIT((#49102,#49103)) ;
#49134 = DERIVED_UNIT((#49104,#49105)) ;
#49135 = DERIVED_UNIT((#49106,#49107)) ;
#49136 = DERIVED_UNIT((#49108,#49109)) ;
#49137 = DERIVED_UNIT((#49110,#49111)) ;
#49138 = DERIVED_UNIT((#49112,#49113)) ;
#49139 = DERIVED_UNIT((#49114,#49115)) ;
#49140 = DERIVED_UNIT((#49116,#49117)) ;
#49141 = DERIVED_UNIT((#49118,#49119)) ;
#49142 = MEASURE_REPRESENTATION_ITEM('density measure',
POSITIVE_RATIO_MEASURE(7850.),#49121) ;
#49143 = MEASURE_REPRESENTATION_ITEM('density measure',
POSITIVE_RATIO_MEASURE(7850.),#49122) ;
#49144 = MEASURE_REPRESENTATION_ITEM('density measure',
POSITIVE_RATIO_MEASURE(7850.),#49123) ;
#49145 = MEASURE_REPRESENTATION_ITEM('density measure',
POSITIVE_RATIO_MEASURE(7850.),#49124) ;
#49146 = MEASURE_REPRESENTATION_ITEM('density measure',
POSITIVE_RATIO_MEASURE(7850.),#49125) ;
#49147 = MEASURE_REPRESENTATION_ITEM('density measure',
POSITIVE_RATIO_MEASURE(7850.),#49126) ;
#49148 = MEASURE_REPRESENTATION_ITEM('density measure',
POSITIVE_RATIO_MEASURE(7850.),#49127) ;
#49149 = MEASURE_REPRESENTATION_ITEM('density measure',
POSITIVE_RATIO_MEASURE(7850.),#49128) ;
#49150 = MEASURE_REPRESENTATION_ITEM('density measure',
POSITIVE_RATIO_MEASURE(7850.),#49129) ;
#49151 = MEASURE_REPRESENTATION_ITEM('density measure',
POSITIVE_RATIO_MEASURE(7850.),#49130) ;
#49152 = MEASURE_REPRESENTATION_ITEM('density measure',
POSITIVE_RATIO_MEASURE(7850.),#49131) ;
#49153 = MEASURE_REPRESENTATION_ITEM('density measure',
POSITIVE_RATIO_MEASURE(7850.),#49132) ;
#49154 = MEASURE_REPRESENTATION_ITEM('density measure',
POSITIVE_RATIO_MEASURE(7850.),#49133) ;
#49155 = MEASURE_REPRESENTATION_ITEM('density measure',
POSITIVE_RATIO_MEASURE(7850.),#49134) ;
#49156 = MEASURE_REPRESENTATION_ITEM('density measure',
POSITIVE_RATIO_MEASURE(7850.),#49135) ;
#49157 = MEASURE_REPRESENTATION_ITEM('density measure',
POSITIVE_RATIO_MEASURE(7850.),#49136) ;
#49158 = MEASURE_REPRESENTATION_ITEM('density measure',
POSITIVE_RATIO_MEASURE(7850.),#49137) ;
#49159 = MEASURE_REPRESENTATION_ITEM('density measure',
POSITIVE_RATIO_MEASURE(7850.),#49138) ;
#49160 = MEASURE_REPRESENTATION_ITEM('density measure',
POSITIVE_RATIO_MEASURE(7850.),#49139) ;
#49161 = MEASURE_REPRESENTATION_ITEM('density measure',
POSITIVE_RATIO_MEASURE(7850.),#49140) ;
#49162 = MEASURE_REPRESENTATION_ITEM('density measure',
POSITIVE_RATIO_MEASURE(7850.),#49141) ;
#49163 = PROPERTY_DEFINITION_REPRESENTATION(#49268,#49205) ;
#49164 = PROPERTY_DEFINITION_REPRESENTATION(#49269,#49206) ;
#49165 = PROPERTY_DEFINITION_REPRESENTATION(#49270,#49207) ;
#49166 = PROPERTY_DEFINITION_REPRESENTATION(#49271,#49208) ;
#49167 = PROPERTY_DEFINITION_REPRESENTATION(#49272,#49209) ;
#49168 = PROPERTY_DEFINITION_REPRESENTATION(#49273,#49210) ;
#49169 = PROPERTY_DEFINITION_REPRESENTATION(#49274,#49211) ;
#49170 = PROPERTY_DEFINITION_REPRESENTATION(#49275,#49212) ;
#49171 = PROPERTY_DEFINITION_REPRESENTATION(#49276,#49213) ;
#49172 = PROPERTY_DEFINITION_REPRESENTATION(#49277,#49214) ;
#49173 = PROPERTY_DEFINITION_REPRESENTATION(#49278,#49215) ;
#49174 = PROPERTY_DEFINITION_REPRESENTATION(#49279,#49216) ;
#49175 = PROPERTY_DEFINITION_REPRESENTATION(#49280,#49217) ;
#49176 = PROPERTY_DEFINITION_REPRESENTATION(#49281,#49218) ;
#49177 = PROPERTY_DEFINITION_REPRESENTATION(#49282,#49219) ;
#49178 = PROPERTY_DEFINITION_REPRESENTATION(#49283,#49220) ;
#49179 = PROPERTY_DEFINITION_REPRESENTATION(#49284,#49221) ;
#49180 = PROPERTY_DEFINITION_REPRESENTATION(#49285,#49222) ;
#49181 = PROPERTY_DEFINITION_REPRESENTATION(#49286,#49223) ;
#49182 = PROPERTY_DEFINITION_REPRESENTATION(#49287,#49224) ;
#49183 = PROPERTY_DEFINITION_REPRESENTATION(#49288,#49225) ;
#49184 = PROPERTY_DEFINITION_REPRESENTATION(#49289,#49226) ;
#49185 = PROPERTY_DEFINITION_REPRESENTATION(#49290,#49227) ;
#49186 = PROPERTY_DEFINITION_REPRESENTATION(#49291,#49228) ;
#49187 = PROPERTY_DEFINITION_REPRESENTATION(#49292,#49229) ;
#49188 = PROPERTY_DEFINITION_REPRESENTATION(#49293,#49230) ;
#49189 = PROPERTY_DEFINITION_REPRESENTATION(#49294,#49231) ;
#49190 = PROPERTY_DEFINITION_REPRESENTATION(#49295,#49232) ;
#49191 = PROPERTY_DEFINITION_REPRESENTATION(#49296,#49233) ;
#49192 = PROPERTY_DEFINITION_REPRESENTATION(#49297,#49234) ;
#49193 = PROPERTY_DEFINITION_REPRESENTATION(#49298,#49235) ;
#49194 = PROPERTY_DEFINITION_REPRESENTATION(#49299,#49236) ;
#49195 = PROPERTY_DEFINITION_REPRESENTATION(#49300,#49237) ;
#49196 = PROPERTY_DEFINITION_REPRESENTATION(#49301,#49238) ;
#49197 = PROPERTY_DEFINITION_REPRESENTATION(#49302,#49239) ;
#49198 = PROPERTY_DEFINITION_REPRESENTATION(#49303,#49240) ;
#49199 = PROPERTY_DEFINITION_REPRESENTATION(#49304,#49241) ;
#49200 = PROPERTY_DEFINITION_REPRESENTATION(#49305,#49242) ;
#49201 = PROPERTY_DEFINITION_REPRESENTATION(#49306,#49243) ;
#49202 = PROPERTY_DEFINITION_REPRESENTATION(#49307,#49244) ;
#49203 = PROPERTY_DEFINITION_REPRESENTATION(#49308,#49245) ;
#49204 = PROPERTY_DEFINITION_REPRESENTATION(#49309,#49246) ;
#49205 = REPRESENTATION('material name',(#49247),#117149) ;
#49206 = REPRESENTATION('density',(#49142),#117149) ;
#49207 = REPRESENTATION('material name',(#49248),#117150) ;
#49208 = REPRESENTATION('density',(#49143),#117150) ;
#49209 = REPRESENTATION('material name',(#49249),#117151) ;
#49210 = REPRESENTATION('density',(#49144),#117151) ;
#49211 = REPRESENTATION('material name',(#49250),#117152) ;
#49212 = REPRESENTATION('density',(#49145),#117152) ;
#49213 = REPRESENTATION('material name',(#49251),#117153) ;
#49214 = REPRESENTATION('density',(#49146),#117153) ;
#49215 = REPRESENTATION('material name',(#49252),#117154) ;
#49216 = REPRESENTATION('density',(#49147),#117154) ;
#49217 = REPRESENTATION('material name',(#49253),#117155) ;
#49218 = REPRESENTATION('density',(#49148),#117155) ;
#49219 = REPRESENTATION('material name',(#49254),#117156) ;
#49220 = REPRESENTATION('density',(#49149),#117156) ;
#49221 = REPRESENTATION('material name',(#49255),#117157) ;
#49222 = REPRESENTATION('density',(#49150),#117157) ;
#49223 = REPRESENTATION('material name',(#49256),#117158) ;
#49224 = REPRESENTATION('density',(#49151),#117158) ;
#49225 = REPRESENTATION('material name',(#49257),#117159) ;
#49226 = REPRESENTATION('density',(#49152),#117159) ;
#49227 = REPRESENTATION('material name',(#49258),#117160) ;
#49228 = REPRESENTATION('density',(#49153),#117160) ;
#49229 = REPRESENTATION('material name',(#49259),#117161) ;
#49230 = REPRESENTATION('density',(#49154),#117161) ;
#49231 = REPRESENTATION('material name',(#49260),#117162) ;
#49232 = REPRESENTATION('density',(#49155),#117162) ;
#49233 = REPRESENTATION('material name',(#49261),#117163) ;
#49234 = REPRESENTATION('density',(#49156),#117163) ;
#49235 = REPRESENTATION('material name',(#49262),#117164) ;
#49236 = REPRESENTATION('density',(#49157),#117164) ;
#49237 = REPRESENTATION('material name',(#49263),#117165) ;
#49238 = REPRESENTATION('density',(#49158),#117165) ;
#49239 = REPRESENTATION('material name',(#49264),#117166) ;
#49240 = REPRESENTATION('density',(#49159),#117166) ;
#49241 = REPRESENTATION('material name',(#49265),#117167) ;
#49242 = REPRESENTATION('density',(#49160),#117167) ;
#49243 = REPRESENTATION('material name',(#49266),#117168) ;
#49244 = REPRESENTATION('density',(#49161),#117168) ;
#49245 = REPRESENTATION('material name',(#49267),#117169) ;
#49246 = REPRESENTATION('density',(#49162),#117169) ;
#49247 = DESCRIPTIVE_REPRESENTATION_ITEM('Steel','Steel') ;
#49248 = DESCRIPTIVE_REPRESENTATION_ITEM('Steel','Steel') ;
#49249 = DESCRIPTIVE_REPRESENTATION_ITEM('Steel','Steel') ;
#49250 = DESCRIPTIVE_REPRESENTATION_ITEM('Steel','Steel') ;
#49251 = DESCRIPTIVE_REPRESENTATION_ITEM('Steel','Steel') ;
#49252 = DESCRIPTIVE_REPRESENTATION_ITEM('Steel','Steel') ;
#49253 = DESCRIPTIVE_REPRESENTATION_ITEM('Steel','Steel') ;
#49254 = DESCRIPTIVE_REPRESENTATION_ITEM('Steel','Steel') ;
#49255 = DESCRIPTIVE_REPRESENTATION_ITEM('Steel','Steel') ;
#49256 = DESCRIPTIVE_REPRESENTATION_ITEM('Steel','Steel') ;
#49257 = DESCRIPTIVE_REPRESENTATION_ITEM('Steel','Steel') ;
#49258 = DESCRIPTIVE_REPRESENTATION_ITEM('Steel','Steel') ;
#49259 = DESCRIPTIVE_REPRESENTATION_ITEM('Steel','Steel') ;
#49260 = DESCRIPTIVE_REPRESENTATION_ITEM('Steel','Steel') ;
#49261 = DESCRIPTIVE_REPRESENTATION_ITEM('Steel','Steel') ;
#49262 = DESCRIPTIVE_REPRESENTATION_ITEM('Steel','Steel') ;
#49263 = DESCRIPTIVE_REPRESENTATION_ITEM('Steel','Steel') ;
#49264 = DESCRIPTIVE_REPRESENTATION_ITEM('Steel','Steel') ;
#49265 = DESCRIPTIVE_REPRESENTATION_ITEM('Steel','Steel') ;
#49266 = DESCRIPTIVE_REPRESENTATION_ITEM('Steel','Steel') ;
#49267 = DESCRIPTIVE_REPRESENTATION_ITEM('Steel','Steel') ;
#49268 = PROPERTY_DEFINITION('material property','material name',#117264) ;
#49269 = PROPERTY_DEFINITION('material property','density of part',#117264) ;
#49270 = PROPERTY_DEFINITION('material property','material name',#117265) ;
#49271 = PROPERTY_DEFINITION('material property','density of part',#117265) ;
#49272 = PROPERTY_DEFINITION('material property','material name',#117266) ;
#49273 = PROPERTY_DEFINITION('material property','density of part',#117266) ;
#49274 = PROPERTY_DEFINITION('material property','material name',#117267) ;
#49275 = PROPERTY_DEFINITION('material property','density of part',#117267) ;
#49276 = PROPERTY_DEFINITION('material property','material name',#117268) ;
#49277 = PROPERTY_DEFINITION('material property','density of part',#117268) ;
#49278 = PROPERTY_DEFINITION('material property','material name',#117269) ;
#49279 = PROPERTY_DEFINITION('material property','density of part',#117269) ;
#49280 = PROPERTY_DEFINITION('material property','material name',#117270) ;
#49281 = PROPERTY_DEFINITION('material property','density of part',#117270) ;
#49282 = PROPERTY_DEFINITION('material property','material name',#117271) ;
#49283 = PROPERTY_DEFINITION('material property','density of part',#117271) ;
#49284 = PROPERTY_DEFINITION('material property','material name',#117272) ;
#49285 = PROPERTY_DEFINITION('material property','density of part',#117272) ;
#49286 = PROPERTY_DEFINITION('material property','material name',#117273) ;
#49287 = PROPERTY_DEFINITION('material property','density of part',#117273) ;
#49288 = PROPERTY_DEFINITION('material property','material name',#117274) ;
#49289 = PROPERTY_DEFINITION('material property','density of part',#117274) ;
#49290 = PROPERTY_DEFINITION('material property','material name',#117275) ;
#49291 = PROPERTY_DEFINITION('material property','density of part',#117275) ;
#49292 = PROPERTY_DEFINITION('material property','material name',#117276) ;
#49293 = PROPERTY_DEFINITION('material property','density of part',#117276) ;
#49294 = PROPERTY_DEFINITION('material property','material name',#117277) ;
#49295 = PROPERTY_DEFINITION('material property','density of part',#117277) ;
#49296 = PROPERTY_DEFINITION('material property','material name',#117278) ;
#49297 = PROPERTY_DEFINITION('material property','density of part',#117278) ;
#49298 = PROPERTY_DEFINITION('material property','material name',#117279) ;
#49299 = PROPERTY_DEFINITION('material property','density of part',#117279) ;
#49300 = PROPERTY_DEFINITION('material property','material name',#117280) ;
#49301 = PROPERTY_DEFINITION('material property','density of part',#117280) ;
#49302 = PROPERTY_DEFINITION('material property','material name',#117281) ;
#49303 = PROPERTY_DEFINITION('material property','density of part',#117281) ;
#49304 = PROPERTY_DEFINITION('material property','material name',#117282) ;
#49305 = PROPERTY_DEFINITION('material property','density of part',#117282) ;
#49306 = PROPERTY_DEFINITION('material property','material name',#117283) ;
#49307 = PROPERTY_DEFINITION('material property','density of part',#117283) ;
#49308 = PROPERTY_DEFINITION('material property','material name',#117284) ;
#49309 = PROPERTY_DEFINITION('material property','density of part',#117284) ;
#49310 = AXIS2_PLACEMENT_3D('',#69885,#55097,#55098) ;
#49311 = AXIS2_PLACEMENT_3D('',#69886,#55099,#55100) ;
#49312 = AXIS2_PLACEMENT_3D('',#69887,#55101,#55102) ;
#49313 = AXIS2_PLACEMENT_3D('',#69889,#55103,#55104) ;
#49314 = AXIS2_PLACEMENT_3D('',#69891,#55105,#55106) ;
#49315 = AXIS2_PLACEMENT_3D('',#69892,#55107,#55108) ;
#49316 = AXIS2_PLACEMENT_3D('',#69893,#55109,#55110) ;
#49317 = AXIS2_PLACEMENT_3D('',#69897,#55112,#55113) ;
#49318 = AXIS2_PLACEMENT_3D('',#69901,#55115,#55116) ;
#49319 = AXIS2_PLACEMENT_3D('',#69905,#55118,#55119) ;
#49320 = AXIS2_PLACEMENT_3D('',#69909,#55121,#55122) ;
#49321 = AXIS2_PLACEMENT_3D('',#69913,#55124,#55125) ;
#49322 = AXIS2_PLACEMENT_3D('',#69917,#55127,#55128) ;
#49323 = AXIS2_PLACEMENT_3D('',#69921,#55130,#55131) ;
#49324 = AXIS2_PLACEMENT_3D('',#69925,#55133,#55134) ;
#49325 = AXIS2_PLACEMENT_3D('',#69929,#55136,#55137) ;
#49326 = AXIS2_PLACEMENT_3D('',#69933,#55139,#55140) ;
#49327 = AXIS2_PLACEMENT_3D('',#69937,#55142,#55143) ;
#49328 = AXIS2_PLACEMENT_3D('',#69941,#55145,#55146) ;
#49329 = AXIS2_PLACEMENT_3D('',#69945,#55148,#55149) ;
#49330 = AXIS2_PLACEMENT_3D('',#69949,#55151,#55152) ;
#49331 = AXIS2_PLACEMENT_3D('',#69953,#55154,#55155) ;
#49332 = AXIS2_PLACEMENT_3D('',#69957,#55157,#55158) ;
#49333 = AXIS2_PLACEMENT_3D('',#69961,#55160,#55161) ;
#49334 = AXIS2_PLACEMENT_3D('',#69965,#55163,#55164) ;
#49335 = AXIS2_PLACEMENT_3D('',#69969,#55166,#55167) ;
#49336 = AXIS2_PLACEMENT_3D('',#69973,#55169,#55170) ;
#49337 = AXIS2_PLACEMENT_3D('',#69977,#55172,#55173) ;
#49338 = AXIS2_PLACEMENT_3D('',#69981,#55175,#55176) ;
#49339 = AXIS2_PLACEMENT_3D('',#69985,#55178,#55179) ;
#49340 = AXIS2_PLACEMENT_3D('',#69989,#55181,#55182) ;
#49341 = AXIS2_PLACEMENT_3D('',#69993,#55184,#55185) ;
#49342 = AXIS2_PLACEMENT_3D('',#69997,#55187,#55188) ;
#49343 = AXIS2_PLACEMENT_3D('',#70001,#55190,#55191) ;
#49344 = AXIS2_PLACEMENT_3D('',#70005,#55193,#55194) ;
#49345 = AXIS2_PLACEMENT_3D('',#70009,#55196,#55197) ;
#49346 = AXIS2_PLACEMENT_3D('',#70013,#55199,#55200) ;
#49347 = AXIS2_PLACEMENT_3D('',#70017,#55202,#55203) ;
#49348 = AXIS2_PLACEMENT_3D('',#70021,#55205,#55206) ;
#49349 = AXIS2_PLACEMENT_3D('',#70025,#55208,#55209) ;
#49350 = AXIS2_PLACEMENT_3D('',#70029,#55211,#55212) ;
#49351 = AXIS2_PLACEMENT_3D('',#70033,#55214,#55215) ;
#49352 = AXIS2_PLACEMENT_3D('',#70037,#55217,#55218) ;
#49353 = AXIS2_PLACEMENT_3D('',#70041,#55220,#55221) ;
#49354 = AXIS2_PLACEMENT_3D('',#70045,#55223,#55224) ;
#49355 = AXIS2_PLACEMENT_3D('',#70049,#55226,#55227) ;
#49356 = AXIS2_PLACEMENT_3D('',#70053,#55229,#55230) ;
#49357 = AXIS2_PLACEMENT_3D('',#70056,#55232,#55233) ;
#49358 = AXIS2_PLACEMENT_3D('',#70057,#55234,#55235) ;
#49359 = AXIS2_PLACEMENT_3D('',#70058,#55236,#55237) ;
#49360 = AXIS2_PLACEMENT_3D('',#70061,#55238,#55239) ;
#49361 = AXIS2_PLACEMENT_3D('',#70065,#55241,#55242) ;
#49362 = AXIS2_PLACEMENT_3D('',#70067,#55244,#55245) ;
#49363 = AXIS2_PLACEMENT_3D('',#70070,#55246,#55247) ;
#49364 = AXIS2_PLACEMENT_3D('',#70074,#55249,#55250) ;
#49365 = AXIS2_PLACEMENT_3D('',#70076,#55252,#55253) ;
#49366 = AXIS2_PLACEMENT_3D('',#70079,#55254,#55255) ;
#49367 = AXIS2_PLACEMENT_3D('',#70080,#55256,#55257) ;
#49368 = AXIS2_PLACEMENT_3D('',#70081,#55258,#55259) ;
#49369 = AXIS2_PLACEMENT_3D('',#70082,#55260,#55261) ;
#49370 = AXIS2_PLACEMENT_3D('',#70084,#55262,#55263) ;
#49371 = AXIS2_PLACEMENT_3D('',#70087,#55266,#55267) ;
#49372 = AXIS2_PLACEMENT_3D('',#70090,#55268,#55269) ;
#49373 = AXIS2_PLACEMENT_3D('',#70093,#55271,#55272) ;
#49374 = AXIS2_PLACEMENT_3D('',#70095,#55274,#55275) ;
#49375 = AXIS2_PLACEMENT_3D('',#70098,#55276,#55277) ;
#49376 = AXIS2_PLACEMENT_3D('',#70102,#55279,#55280) ;
#49377 = AXIS2_PLACEMENT_3D('',#70104,#55282,#55283) ;
#49378 = AXIS2_PLACEMENT_3D('',#70107,#55284,#55285) ;
#49379 = AXIS2_PLACEMENT_3D('',#70108,#55286,#55287) ;
#49380 = AXIS2_PLACEMENT_3D('',#70109,#55288,#55289) ;
#49381 = AXIS2_PLACEMENT_3D('',#70110,#55290,#55291) ;
#49382 = AXIS2_PLACEMENT_3D('',#70112,#55292,#55293) ;
#49383 = AXIS2_PLACEMENT_3D('',#70115,#55296,#55297) ;
#49384 = AXIS2_PLACEMENT_3D('',#70118,#55298,#55299) ;
#49385 = AXIS2_PLACEMENT_3D('',#70121,#55301,#55302) ;
#49386 = AXIS2_PLACEMENT_3D('',#70123,#55304,#55305) ;
#49387 = AXIS2_PLACEMENT_3D('',#70126,#55306,#55307) ;
#49388 = AXIS2_PLACEMENT_3D('',#70130,#55309,#55310) ;
#49389 = AXIS2_PLACEMENT_3D('',#70132,#55312,#55313) ;
#49390 = AXIS2_PLACEMENT_3D('',#70135,#55314,#55315) ;
#49391 = AXIS2_PLACEMENT_3D('',#70136,#55316,#55317) ;
#49392 = AXIS2_PLACEMENT_3D('',#70137,#55318,#55319) ;
#49393 = AXIS2_PLACEMENT_3D('',#70138,#55320,#55321) ;
#49394 = AXIS2_PLACEMENT_3D('',#70140,#55322,#55323) ;
#49395 = AXIS2_PLACEMENT_3D('',#70143,#55326,#55327) ;
#49396 = AXIS2_PLACEMENT_3D('',#70146,#55328,#55329) ;
#49397 = AXIS2_PLACEMENT_3D('',#70149,#55331,#55332) ;
#49398 = AXIS2_PLACEMENT_3D('',#70151,#55334,#55335) ;
#49399 = AXIS2_PLACEMENT_3D('',#70154,#55336,#55337) ;
#49400 = AXIS2_PLACEMENT_3D('',#70156,#55338,#55339) ;
#49401 = AXIS2_PLACEMENT_3D('',#70158,#55340,#55341) ;
#49402 = AXIS2_PLACEMENT_3D('',#70159,#55342,#55343) ;
#49403 = AXIS2_PLACEMENT_3D('',#70160,#55344,#55345) ;
#49404 = AXIS2_PLACEMENT_3D('',#70162,#55346,#55347) ;
#49405 = AXIS2_PLACEMENT_3D('',#70165,#55350,#55351) ;
#49406 = AXIS2_PLACEMENT_3D('',#70167,#55352,#55353) ;
#49407 = AXIS2_PLACEMENT_3D('',#70170,#55356,#55357) ;
#49408 = AXIS2_PLACEMENT_3D('',#70171,#55358,#55359) ;
#49409 = AXIS2_PLACEMENT_3D('',#70172,#55360,#55361) ;
#49410 = AXIS2_PLACEMENT_3D('',#70173,#55362,#55363) ;
#49411 = AXIS2_PLACEMENT_3D('',#70174,#55364,#55365) ;
#49412 = AXIS2_PLACEMENT_3D('',#70175,#55366,#55367) ;
#49413 = AXIS2_PLACEMENT_3D('',#70176,#55368,#55369) ;
#49414 = AXIS2_PLACEMENT_3D('',#70177,#55370,#55371) ;
#49415 = AXIS2_PLACEMENT_3D('',#70178,#55372,#55373) ;
#49416 = AXIS2_PLACEMENT_3D('',#70179,#55374,#55375) ;
#49417 = AXIS2_PLACEMENT_3D('',#70180,#55376,#55377) ;
#49418 = AXIS2_PLACEMENT_3D('',#70181,#55378,#55379) ;
#49419 = AXIS2_PLACEMENT_3D('',#70182,#55380,#55381) ;
#49420 = AXIS2_PLACEMENT_3D('',#70183,#55382,#55383) ;
#49421 = AXIS2_PLACEMENT_3D('',#70184,#55384,#55385) ;
#49422 = AXIS2_PLACEMENT_3D('',#70185,#55386,#55387) ;
#49423 = AXIS2_PLACEMENT_3D('',#70186,#55388,#55389) ;
#49424 = AXIS2_PLACEMENT_3D('',#70192,#55393,#55394) ;
#49425 = AXIS2_PLACEMENT_3D('',#70195,#55396,#55397) ;
#49426 = AXIS2_PLACEMENT_3D('',#70196,#55398,#55399) ;
#49427 = AXIS2_PLACEMENT_3D('',#70200,#55402,#55403) ;
#49428 = AXIS2_PLACEMENT_3D('',#70203,#55405,#55406) ;
#49429 = AXIS2_PLACEMENT_3D('',#70204,#55407,#55408) ;
#49430 = AXIS2_PLACEMENT_3D('',#70208,#55411,#55412) ;
#49431 = AXIS2_PLACEMENT_3D('',#70211,#55414,#55415) ;
#49432 = AXIS2_PLACEMENT_3D('',#70212,#55416,#55417) ;
#49433 = AXIS2_PLACEMENT_3D('',#70216,#55420,#55421) ;
#49434 = AXIS2_PLACEMENT_3D('',#70219,#55423,#55424) ;
#49435 = AXIS2_PLACEMENT_3D('',#70220,#55425,#55426) ;
#49436 = AXIS2_PLACEMENT_3D('',#70224,#55429,#55430) ;
#49437 = AXIS2_PLACEMENT_3D('',#70227,#55432,#55433) ;
#49438 = AXIS2_PLACEMENT_3D('',#70228,#55434,#55435) ;
#49439 = AXIS2_PLACEMENT_3D('',#70232,#55438,#55439) ;
#49440 = AXIS2_PLACEMENT_3D('',#70235,#55441,#55442) ;
#49441 = AXIS2_PLACEMENT_3D('',#70236,#55443,#55444) ;
#49442 = AXIS2_PLACEMENT_3D('',#70237,#55445,#55446) ;
#49443 = AXIS2_PLACEMENT_3D('',#70239,#55447,#55448) ;
#49444 = AXIS2_PLACEMENT_3D('',#70241,#55449,#55450) ;
#49445 = AXIS2_PLACEMENT_3D('',#70242,#55451,#55452) ;
#49446 = AXIS2_PLACEMENT_3D('',#70243,#55453,#55454) ;
#49447 = AXIS2_PLACEMENT_3D('',#70245,#55455,#55456) ;
#49448 = AXIS2_PLACEMENT_3D('',#70247,#55457,#55458) ;
#49449 = AXIS2_PLACEMENT_3D('',#70248,#55459,#55460) ;
#49450 = AXIS2_PLACEMENT_3D('',#70249,#55461,#55462) ;
#49451 = AXIS2_PLACEMENT_3D('',#70251,#55463,#55464) ;
#49452 = AXIS2_PLACEMENT_3D('',#70253,#55465,#55466) ;
#49453 = AXIS2_PLACEMENT_3D('',#70254,#55467,#55468) ;
#49454 = AXIS2_PLACEMENT_3D('',#70255,#55469,#55470) ;
#49455 = AXIS2_PLACEMENT_3D('',#70256,#55471,#55472) ;
#49456 = AXIS2_PLACEMENT_3D('',#70257,#55473,#55474) ;
#49457 = AXIS2_PLACEMENT_3D('',#70259,#55475,#55476) ;
#49458 = AXIS2_PLACEMENT_3D('',#70261,#55477,#55478) ;
#49459 = AXIS2_PLACEMENT_3D('',#70262,#55479,#55480) ;
#49460 = AXIS2_PLACEMENT_3D('',#70263,#55481,#55482) ;
#49461 = AXIS2_PLACEMENT_3D('',#70265,#55483,#55484) ;
#49462 = AXIS2_PLACEMENT_3D('',#70267,#55485,#55486) ;
#49463 = AXIS2_PLACEMENT_3D('',#70268,#55487,#55488) ;
#49464 = AXIS2_PLACEMENT_3D('',#70535,#55489,#55490) ;
#49465 = AXIS2_PLACEMENT_3D('',#70537,#55491,#55492) ;
#49466 = AXIS2_PLACEMENT_3D('',#70539,#55493,#55494) ;
#49467 = AXIS2_PLACEMENT_3D('',#70540,#55495,#55496) ;
#49468 = AXIS2_PLACEMENT_3D('',#70541,#55497,#55498) ;
#49469 = AXIS2_PLACEMENT_3D('',#70543,#55499,#55500) ;
#49470 = AXIS2_PLACEMENT_3D('',#70545,#55501,#55502) ;
#49471 = AXIS2_PLACEMENT_3D('',#70546,#55503,#55504) ;
#49472 = AXIS2_PLACEMENT_3D('',#70547,#55505,#55506) ;
#49473 = AXIS2_PLACEMENT_3D('',#70548,#55507,#55508) ;
#49474 = AXIS2_PLACEMENT_3D('',#70549,#55509,#55510) ;
#49475 = AXIS2_PLACEMENT_3D('',#70551,#55511,#55512) ;
#49476 = AXIS2_PLACEMENT_3D('',#70553,#55513,#55514) ;
#49477 = AXIS2_PLACEMENT_3D('',#70554,#55515,#55516) ;
#49478 = AXIS2_PLACEMENT_3D('',#70555,#55517,#55518) ;
#49479 = AXIS2_PLACEMENT_3D('',#70557,#55519,#55520) ;
#49480 = AXIS2_PLACEMENT_3D('',#70559,#55521,#55522) ;
#49481 = AXIS2_PLACEMENT_3D('',#70560,#55523,#55524) ;
#49482 = AXIS2_PLACEMENT_3D('',#70754,#55525,#55526) ;
#49483 = AXIS2_PLACEMENT_3D('',#70756,#55527,#55528) ;
#49484 = AXIS2_PLACEMENT_3D('',#70758,#55529,#55530) ;
#49485 = AXIS2_PLACEMENT_3D('',#70759,#55531,#55532) ;
#49486 = AXIS2_PLACEMENT_3D('',#70760,#55533,#55534) ;
#49487 = AXIS2_PLACEMENT_3D('',#70762,#55535,#55536) ;
#49488 = AXIS2_PLACEMENT_3D('',#70764,#55537,#55538) ;
#49489 = AXIS2_PLACEMENT_3D('',#70765,#55539,#55540) ;
#49490 = AXIS2_PLACEMENT_3D('',#70766,#55541,#55542) ;
#49491 = AXIS2_PLACEMENT_3D('',#70767,#55543,#55544) ;
#49492 = AXIS2_PLACEMENT_3D('',#70768,#55545,#55546) ;
#49493 = AXIS2_PLACEMENT_3D('',#70770,#55547,#55548) ;
#49494 = AXIS2_PLACEMENT_3D('',#70772,#55549,#55550) ;
#49495 = AXIS2_PLACEMENT_3D('',#70773,#55551,#55552) ;
#49496 = AXIS2_PLACEMENT_3D('',#70774,#55553,#55554) ;
#49497 = AXIS2_PLACEMENT_3D('',#70776,#55555,#55556) ;
#49498 = AXIS2_PLACEMENT_3D('',#70778,#55557,#55558) ;
#49499 = AXIS2_PLACEMENT_3D('',#70779,#55559,#55560) ;
#49500 = AXIS2_PLACEMENT_3D('',#70973,#55561,#55562) ;
#49501 = AXIS2_PLACEMENT_3D('',#70975,#55563,#55564) ;
#49502 = AXIS2_PLACEMENT_3D('',#70977,#55565,#55566) ;
#49503 = AXIS2_PLACEMENT_3D('',#70978,#55567,#55568) ;
#49504 = AXIS2_PLACEMENT_3D('',#70979,#55569,#55570) ;
#49505 = AXIS2_PLACEMENT_3D('',#70981,#55571,#55572) ;
#49506 = AXIS2_PLACEMENT_3D('',#70983,#55573,#55574) ;
#49507 = AXIS2_PLACEMENT_3D('',#70984,#55575,#55576) ;
#49508 = AXIS2_PLACEMENT_3D('',#70985,#55577,#55578) ;
#49509 = AXIS2_PLACEMENT_3D('',#70986,#55579,#55580) ;
#49510 = AXIS2_PLACEMENT_3D('',#70987,#55581,#55582) ;
#49511 = AXIS2_PLACEMENT_3D('',#70989,#55583,#55584) ;
#49512 = AXIS2_PLACEMENT_3D('',#70991,#55585,#55586) ;
#49513 = AXIS2_PLACEMENT_3D('',#70992,#55587,#55588) ;
#49514 = AXIS2_PLACEMENT_3D('',#70993,#55589,#55590) ;
#49515 = AXIS2_PLACEMENT_3D('',#70995,#55591,#55592) ;
#49516 = AXIS2_PLACEMENT_3D('',#70997,#55593,#55594) ;
#49517 = AXIS2_PLACEMENT_3D('',#70998,#55595,#55596) ;
#49518 = AXIS2_PLACEMENT_3D('',#71197,#55597,#55598) ;
#49519 = AXIS2_PLACEMENT_3D('',#71199,#55599,#55600) ;
#49520 = AXIS2_PLACEMENT_3D('',#71201,#55601,#55602) ;
#49521 = AXIS2_PLACEMENT_3D('',#71202,#55603,#55604) ;
#49522 = AXIS2_PLACEMENT_3D('',#71203,#55605,#55606) ;
#49523 = AXIS2_PLACEMENT_3D('',#71205,#55607,#55608) ;
#49524 = AXIS2_PLACEMENT_3D('',#71207,#55609,#55610) ;
#49525 = AXIS2_PLACEMENT_3D('',#71208,#55611,#55612) ;
#49526 = AXIS2_PLACEMENT_3D('',#71209,#55613,#55614) ;
#49527 = AXIS2_PLACEMENT_3D('',#71210,#55615,#55616) ;
#49528 = AXIS2_PLACEMENT_3D('',#71211,#55617,#55618) ;
#49529 = AXIS2_PLACEMENT_3D('',#71213,#55619,#55620) ;
#49530 = AXIS2_PLACEMENT_3D('',#71215,#55621,#55622) ;
#49531 = AXIS2_PLACEMENT_3D('',#71216,#55623,#55624) ;
#49532 = AXIS2_PLACEMENT_3D('',#71217,#55625,#55626) ;
#49533 = AXIS2_PLACEMENT_3D('',#71219,#55627,#55628) ;
#49534 = AXIS2_PLACEMENT_3D('',#71221,#55629,#55630) ;
#49535 = AXIS2_PLACEMENT_3D('',#71222,#55631,#55632) ;
#49536 = AXIS2_PLACEMENT_3D('',#71425,#55633,#55634) ;
#49537 = AXIS2_PLACEMENT_3D('',#71427,#55635,#55636) ;
#49538 = AXIS2_PLACEMENT_3D('',#71429,#55637,#55638) ;
#49539 = AXIS2_PLACEMENT_3D('',#71430,#55639,#55640) ;
#49540 = AXIS2_PLACEMENT_3D('',#71431,#55641,#55642) ;
#49541 = AXIS2_PLACEMENT_3D('',#71433,#55643,#55644) ;
#49542 = AXIS2_PLACEMENT_3D('',#71435,#55645,#55646) ;
#49543 = AXIS2_PLACEMENT_3D('',#71436,#55647,#55648) ;
#49544 = AXIS2_PLACEMENT_3D('',#71437,#55649,#55650) ;
#49545 = AXIS2_PLACEMENT_3D('',#71438,#55651,#55652) ;
#49546 = AXIS2_PLACEMENT_3D('',#71439,#55653,#55654) ;
#49547 = AXIS2_PLACEMENT_3D('',#71441,#55655,#55656) ;
#49548 = AXIS2_PLACEMENT_3D('',#71443,#55657,#55658) ;
#49549 = AXIS2_PLACEMENT_3D('',#71444,#55659,#55660) ;
#49550 = AXIS2_PLACEMENT_3D('',#71445,#55661,#55662) ;
#49551 = AXIS2_PLACEMENT_3D('',#71447,#55663,#55664) ;
#49552 = AXIS2_PLACEMENT_3D('',#71449,#55665,#55666) ;
#49553 = AXIS2_PLACEMENT_3D('',#71450,#55667,#55668) ;
#49554 = AXIS2_PLACEMENT_3D('',#71644,#55669,#55670) ;
#49555 = AXIS2_PLACEMENT_3D('',#71646,#55671,#55672) ;
#49556 = AXIS2_PLACEMENT_3D('',#71648,#55673,#55674) ;
#49557 = AXIS2_PLACEMENT_3D('',#71649,#55675,#55676) ;
#49558 = AXIS2_PLACEMENT_3D('',#71650,#55677,#55678) ;
#49559 = AXIS2_PLACEMENT_3D('',#71652,#55679,#55680) ;
#49560 = AXIS2_PLACEMENT_3D('',#71654,#55681,#55682) ;
#49561 = AXIS2_PLACEMENT_3D('',#71655,#55683,#55684) ;
#49562 = AXIS2_PLACEMENT_3D('',#71656,#55685,#55686) ;
#49563 = AXIS2_PLACEMENT_3D('',#71657,#55687,#55688) ;
#49564 = AXIS2_PLACEMENT_3D('',#71658,#55689,#55690) ;
#49565 = AXIS2_PLACEMENT_3D('',#71660,#55691,#55692) ;
#49566 = AXIS2_PLACEMENT_3D('',#71662,#55693,#55694) ;
#49567 = AXIS2_PLACEMENT_3D('',#71663,#55695,#55696) ;
#49568 = AXIS2_PLACEMENT_3D('',#71664,#55697,#55698) ;
#49569 = AXIS2_PLACEMENT_3D('',#71666,#55699,#55700) ;
#49570 = AXIS2_PLACEMENT_3D('',#71668,#55701,#55702) ;
#49571 = AXIS2_PLACEMENT_3D('',#71669,#55703,#55704) ;
#49572 = AXIS2_PLACEMENT_3D('',#71863,#55705,#55706) ;
#49573 = AXIS2_PLACEMENT_3D('',#71865,#55707,#55708) ;
#49574 = AXIS2_PLACEMENT_3D('',#71867,#55709,#55710) ;
#49575 = AXIS2_PLACEMENT_3D('',#71868,#55711,#55712) ;
#49576 = AXIS2_PLACEMENT_3D('',#71869,#55713,#55714) ;
#49577 = AXIS2_PLACEMENT_3D('',#71871,#55715,#55716) ;
#49578 = AXIS2_PLACEMENT_3D('',#71873,#55717,#55718) ;
#49579 = AXIS2_PLACEMENT_3D('',#71874,#55719,#55720) ;
#49580 = AXIS2_PLACEMENT_3D('',#71875,#55721,#55722) ;
#49581 = AXIS2_PLACEMENT_3D('',#71876,#55723,#55724) ;
#49582 = AXIS2_PLACEMENT_3D('',#71877,#55725,#55726) ;
#49583 = AXIS2_PLACEMENT_3D('',#71879,#55727,#55728) ;
#49584 = AXIS2_PLACEMENT_3D('',#71881,#55729,#55730) ;
#49585 = AXIS2_PLACEMENT_3D('',#71882,#55731,#55732) ;
#49586 = AXIS2_PLACEMENT_3D('',#71883,#55733,#55734) ;
#49587 = AXIS2_PLACEMENT_3D('',#71885,#55735,#55736) ;
#49588 = AXIS2_PLACEMENT_3D('',#71887,#55737,#55738) ;
#49589 = AXIS2_PLACEMENT_3D('',#71888,#55739,#55740) ;
#49590 = AXIS2_PLACEMENT_3D('',#72070,#55741,#55742) ;
#49591 = AXIS2_PLACEMENT_3D('',#72072,#55743,#55744) ;
#49592 = AXIS2_PLACEMENT_3D('',#72074,#55745,#55746) ;
#49593 = AXIS2_PLACEMENT_3D('',#72075,#55747,#55748) ;
#49594 = AXIS2_PLACEMENT_3D('',#72076,#55749,#55750) ;
#49595 = AXIS2_PLACEMENT_3D('',#72078,#55751,#55752) ;
#49596 = AXIS2_PLACEMENT_3D('',#72080,#55753,#55754) ;
#49597 = AXIS2_PLACEMENT_3D('',#72081,#55755,#55756) ;
#49598 = AXIS2_PLACEMENT_3D('',#72082,#55757,#55758) ;
#49599 = AXIS2_PLACEMENT_3D('',#72083,#55759,#55760) ;
#49600 = AXIS2_PLACEMENT_3D('',#72084,#55761,#55762) ;
#49601 = AXIS2_PLACEMENT_3D('',#72086,#55763,#55764) ;
#49602 = AXIS2_PLACEMENT_3D('',#72088,#55765,#55766) ;
#49603 = AXIS2_PLACEMENT_3D('',#72089,#55767,#55768) ;
#49604 = AXIS2_PLACEMENT_3D('',#72090,#55769,#55770) ;
#49605 = AXIS2_PLACEMENT_3D('',#72092,#55771,#55772) ;
#49606 = AXIS2_PLACEMENT_3D('',#72094,#55773,#55774) ;
#49607 = AXIS2_PLACEMENT_3D('',#72095,#55775,#55776) ;
#49608 = AXIS2_PLACEMENT_3D('',#72201,#55777,#55778) ;
#49609 = AXIS2_PLACEMENT_3D('',#72203,#55779,#55780) ;
#49610 = AXIS2_PLACEMENT_3D('',#72205,#55781,#55782) ;
#49611 = AXIS2_PLACEMENT_3D('',#72206,#55783,#55784) ;
#49612 = AXIS2_PLACEMENT_3D('',#72207,#55785,#55786) ;
#49613 = AXIS2_PLACEMENT_3D('',#72209,#55787,#55788) ;
#49614 = AXIS2_PLACEMENT_3D('',#72211,#55789,#55790) ;
#49615 = AXIS2_PLACEMENT_3D('',#72212,#55791,#55792) ;
#49616 = AXIS2_PLACEMENT_3D('',#72213,#55793,#55794) ;
#49617 = AXIS2_PLACEMENT_3D('',#72214,#55795,#55796) ;
#49618 = AXIS2_PLACEMENT_3D('',#72215,#55797,#55798) ;
#49619 = AXIS2_PLACEMENT_3D('',#72217,#55799,#55800) ;
#49620 = AXIS2_PLACEMENT_3D('',#72219,#55801,#55802) ;
#49621 = AXIS2_PLACEMENT_3D('',#72220,#55803,#55804) ;
#49622 = AXIS2_PLACEMENT_3D('',#72399,#55805,#55806) ;
#49623 = AXIS2_PLACEMENT_3D('',#72400,#55807,#55808) ;
#49624 = AXIS2_PLACEMENT_3D('',#72401,#55809,#55810) ;
#49625 = AXIS2_PLACEMENT_3D('',#72418,#55812,#55813) ;
#49626 = AXIS2_PLACEMENT_3D('',#72629,#55815,#55816) ;
#49627 = AXIS2_PLACEMENT_3D('',#72644,#55818,#55819) ;
#49628 = AXIS2_PLACEMENT_3D('',#72653,#55820,#55821) ;
#49629 = AXIS2_PLACEMENT_3D('',#72660,#55822,#55823) ;
#49630 = AXIS2_PLACEMENT_3D('',#72677,#55825,#55826) ;
#49631 = AXIS2_PLACEMENT_3D('',#72678,#55827,#55828) ;
#49632 = AXIS2_PLACEMENT_3D('',#72679,#55829,#55830) ;
#49633 = AXIS2_PLACEMENT_3D('',#72696,#55832,#55833) ;
#49634 = AXIS2_PLACEMENT_3D('',#72705,#55834,#55835) ;
#49635 = AXIS2_PLACEMENT_3D('',#72712,#55836,#55837) ;
#49636 = AXIS2_PLACEMENT_3D('',#72727,#55839,#55840) ;
#49637 = AXIS2_PLACEMENT_3D('',#72736,#55841,#55842) ;
#49638 = AXIS2_PLACEMENT_3D('',#72939,#55843,#55844) ;
#49639 = AXIS2_PLACEMENT_3D('',#72954,#55846,#55847) ;
#49640 = AXIS2_PLACEMENT_3D('',#72971,#55849,#55850) ;
#49641 = AXIS2_PLACEMENT_3D('',#72972,#55851,#55852) ;
#49642 = AXIS2_PLACEMENT_3D('',#72973,#55853,#55854) ;
#49643 = AXIS2_PLACEMENT_3D('',#72990,#55856,#55857) ;
#49644 = AXIS2_PLACEMENT_3D('',#72999,#55858,#55859) ;
#49645 = AXIS2_PLACEMENT_3D('',#73006,#55860,#55861) ;
#49646 = AXIS2_PLACEMENT_3D('',#73021,#55863,#55864) ;
#49647 = AXIS2_PLACEMENT_3D('',#73030,#55865,#55866) ;
#49648 = AXIS2_PLACEMENT_3D('',#73230,#55867,#55868) ;
#49649 = AXIS2_PLACEMENT_3D('',#73245,#55870,#55871) ;
#49650 = AXIS2_PLACEMENT_3D('',#73262,#55873,#55874) ;
#49651 = AXIS2_PLACEMENT_3D('',#73263,#55875,#55876) ;
#49652 = AXIS2_PLACEMENT_3D('',#73264,#55877,#55878) ;
#49653 = AXIS2_PLACEMENT_3D('',#73281,#55880,#55881) ;
#49654 = AXIS2_PLACEMENT_3D('',#73290,#55882,#55883) ;
#49655 = AXIS2_PLACEMENT_3D('',#73297,#55884,#55885) ;
#49656 = AXIS2_PLACEMENT_3D('',#73312,#55887,#55888) ;
#49657 = AXIS2_PLACEMENT_3D('',#73321,#55889,#55890) ;
#49658 = AXIS2_PLACEMENT_3D('',#73433,#55891,#55892) ;
#49659 = AXIS2_PLACEMENT_3D('',#73448,#55894,#55895) ;
#49660 = AXIS2_PLACEMENT_3D('',#73465,#55897,#55898) ;
#49661 = AXIS2_PLACEMENT_3D('',#73466,#55899,#55900) ;
#49662 = AXIS2_PLACEMENT_3D('',#73467,#55901,#55902) ;
#49663 = AXIS2_PLACEMENT_3D('',#73484,#55904,#55905) ;
#49664 = AXIS2_PLACEMENT_3D('',#73493,#55906,#55907) ;
#49665 = AXIS2_PLACEMENT_3D('',#73500,#55908,#55909) ;
#49666 = AXIS2_PLACEMENT_3D('',#73515,#55911,#55912) ;
#49667 = AXIS2_PLACEMENT_3D('',#73524,#55913,#55914) ;
#49668 = AXIS2_PLACEMENT_3D('',#73709,#55915,#55916) ;
#49669 = AXIS2_PLACEMENT_3D('',#73724,#55918,#55919) ;
#49670 = AXIS2_PLACEMENT_3D('',#73741,#55921,#55922) ;
#49671 = AXIS2_PLACEMENT_3D('',#73742,#55923,#55924) ;
#49672 = AXIS2_PLACEMENT_3D('',#73743,#55925,#55926) ;
#49673 = AXIS2_PLACEMENT_3D('',#73760,#55928,#55929) ;
#49674 = AXIS2_PLACEMENT_3D('',#73769,#55930,#55931) ;
#49675 = AXIS2_PLACEMENT_3D('',#73776,#55932,#55933) ;
#49676 = AXIS2_PLACEMENT_3D('',#73791,#55935,#55936) ;
#49677 = AXIS2_PLACEMENT_3D('',#73800,#55937,#55938) ;
#49678 = AXIS2_PLACEMENT_3D('',#74000,#55939,#55940) ;
#49679 = AXIS2_PLACEMENT_3D('',#74015,#55942,#55943) ;
#49680 = AXIS2_PLACEMENT_3D('',#74032,#55945,#55946) ;
#49681 = AXIS2_PLACEMENT_3D('',#74033,#55947,#55948) ;
#49682 = AXIS2_PLACEMENT_3D('',#74034,#55949,#55950) ;
#49683 = AXIS2_PLACEMENT_3D('',#74051,#55952,#55953) ;
#49684 = AXIS2_PLACEMENT_3D('',#74060,#55954,#55955) ;
#49685 = AXIS2_PLACEMENT_3D('',#74067,#55956,#55957) ;
#49686 = AXIS2_PLACEMENT_3D('',#74082,#55959,#55960) ;
#49687 = AXIS2_PLACEMENT_3D('',#74091,#55961,#55962) ;
#49688 = AXIS2_PLACEMENT_3D('',#74294,#55963,#55964) ;
#49689 = AXIS2_PLACEMENT_3D('',#74309,#55966,#55967) ;
#49690 = AXIS2_PLACEMENT_3D('',#74326,#55969,#55970) ;
#49691 = AXIS2_PLACEMENT_3D('',#74327,#55971,#55972) ;
#49692 = AXIS2_PLACEMENT_3D('',#74328,#55973,#55974) ;
#49693 = AXIS2_PLACEMENT_3D('',#74345,#55976,#55977) ;
#49694 = AXIS2_PLACEMENT_3D('',#74354,#55978,#55979) ;
#49695 = AXIS2_PLACEMENT_3D('',#74361,#55980,#55981) ;
#49696 = AXIS2_PLACEMENT_3D('',#74376,#55983,#55984) ;
#49697 = AXIS2_PLACEMENT_3D('',#74385,#55985,#55986) ;
#49698 = AXIS2_PLACEMENT_3D('',#74570,#55987,#55988) ;
#49699 = AXIS2_PLACEMENT_3D('',#74585,#55990,#55991) ;
#49700 = AXIS2_PLACEMENT_3D('',#74602,#55993,#55994) ;
#49701 = AXIS2_PLACEMENT_3D('',#74603,#55995,#55996) ;
#49702 = AXIS2_PLACEMENT_3D('',#74604,#55997,#55998) ;
#49703 = AXIS2_PLACEMENT_3D('',#74621,#56000,#56001) ;
#49704 = AXIS2_PLACEMENT_3D('',#74630,#56002,#56003) ;
#49705 = AXIS2_PLACEMENT_3D('',#74637,#56004,#56005) ;
#49706 = AXIS2_PLACEMENT_3D('',#74652,#56007,#56008) ;
#49707 = AXIS2_PLACEMENT_3D('',#74661,#56009,#56010) ;
#49708 = AXIS2_PLACEMENT_3D('',#74773,#56011,#56012) ;
#49709 = AXIS2_PLACEMENT_3D('',#74788,#56014,#56015) ;
#49710 = AXIS2_PLACEMENT_3D('',#74805,#56017,#56018) ;
#49711 = AXIS2_PLACEMENT_3D('',#74806,#56019,#56020) ;
#49712 = AXIS2_PLACEMENT_3D('',#74807,#56021,#56022) ;
#49713 = AXIS2_PLACEMENT_3D('',#74824,#56024,#56025) ;
#49714 = AXIS2_PLACEMENT_3D('',#74833,#56026,#56027) ;
#49715 = AXIS2_PLACEMENT_3D('',#74840,#56028,#56029) ;
#49716 = AXIS2_PLACEMENT_3D('',#74855,#56031,#56032) ;
#49717 = AXIS2_PLACEMENT_3D('',#74864,#56033,#56034) ;
#49718 = AXIS2_PLACEMENT_3D('',#75052,#56035,#56036) ;
#49719 = AXIS2_PLACEMENT_3D('',#75067,#56038,#56039) ;
#49720 = AXIS2_PLACEMENT_3D('',#75084,#56041,#56042) ;
#49721 = AXIS2_PLACEMENT_3D('',#75093,#56043,#56044) ;
#49722 = AXIS2_PLACEMENT_3D('',#75100,#56045,#56046) ;
#49723 = AXIS2_PLACEMENT_3D('',#75101,#56047,#56048) ;
#49724 = AXIS2_PLACEMENT_3D('',#75102,#56049,#56050) ;
#49725 = AXIS2_PLACEMENT_3D('',#75103,#56051,#56052) ;
#49726 = AXIS2_PLACEMENT_3D('',#75104,#56053,#56054) ;
#49727 = AXIS2_PLACEMENT_3D('',#75105,#56055,#56056) ;
#49728 = AXIS2_PLACEMENT_3D('',#75106,#56057,#56058) ;
#49729 = AXIS2_PLACEMENT_3D('',#75107,#56059,#56060) ;
#49730 = AXIS2_PLACEMENT_3D('',#75108,#56061,#56062) ;
#49731 = AXIS2_PLACEMENT_3D('',#75109,#56063,#56064) ;
#49732 = AXIS2_PLACEMENT_3D('',#75110,#56065,#56066) ;
#49733 = AXIS2_PLACEMENT_3D('',#75111,#56067,#56068) ;
#49734 = AXIS2_PLACEMENT_3D('',#75112,#56069,#56070) ;
#49735 = AXIS2_PLACEMENT_3D('',#75113,#56071,#56072) ;
#49736 = AXIS2_PLACEMENT_3D('',#75114,#56073,#56074) ;
#49737 = AXIS2_PLACEMENT_3D('',#75115,#56075,#56076) ;
#49738 = AXIS2_PLACEMENT_3D('',#75116,#56077,#56078) ;
#49739 = AXIS2_PLACEMENT_3D('',#75117,#56079,#56080) ;
#49740 = AXIS2_PLACEMENT_3D('',#75118,#56081,#56082) ;
#49741 = AXIS2_PLACEMENT_3D('',#75119,#56083,#56084) ;
#49742 = AXIS2_PLACEMENT_3D('',#75120,#56085,#56086) ;
#49743 = AXIS2_PLACEMENT_3D('',#75121,#56087,#56088) ;
#49744 = AXIS2_PLACEMENT_3D('',#75122,#56089,#56090) ;
#49745 = AXIS2_PLACEMENT_3D('',#75123,#56091,#56092) ;
#49746 = AXIS2_PLACEMENT_3D('',#75124,#56093,#56094) ;
#49747 = AXIS2_PLACEMENT_3D('',#75125,#56095,#56096) ;
#49748 = AXIS2_PLACEMENT_3D('',#75126,#56097,#56098) ;
#49749 = AXIS2_PLACEMENT_3D('',#75127,#56099,#56100) ;
#49750 = AXIS2_PLACEMENT_3D('',#75128,#56101,#56102) ;
#49751 = AXIS2_PLACEMENT_3D('',#75129,#56103,#56104) ;
#49752 = AXIS2_PLACEMENT_3D('',#75130,#56105,#56106) ;
#49753 = AXIS2_PLACEMENT_3D('',#75131,#56107,#56108) ;
#49754 = AXIS2_PLACEMENT_3D('',#75132,#56109,#56110) ;
#49755 = AXIS2_PLACEMENT_3D('',#75133,#56111,#56112) ;
#49756 = AXIS2_PLACEMENT_3D('',#75134,#56113,#56114) ;
#49757 = AXIS2_PLACEMENT_3D('',#75135,#56115,#56116) ;
#49758 = AXIS2_PLACEMENT_3D('',#75136,#56117,#56118) ;
#49759 = AXIS2_PLACEMENT_3D('',#75137,#56119,#56120) ;
#49760 = AXIS2_PLACEMENT_3D('',#75138,#56121,#56122) ;
#49761 = AXIS2_PLACEMENT_3D('',#75139,#56123,#56124) ;
#49762 = AXIS2_PLACEMENT_3D('',#75140,#56125,#56126) ;
#49763 = AXIS2_PLACEMENT_3D('',#75143,#56128,#56129) ;
#49764 = AXIS2_PLACEMENT_3D('',#75144,#56130,#56131) ;
#49765 = AXIS2_PLACEMENT_3D('',#75146,#56132,#56133) ;
#49766 = AXIS2_PLACEMENT_3D('',#75148,#56134,#56135) ;
#49767 = AXIS2_PLACEMENT_3D('',#75149,#56136,#56137) ;
#49768 = AXIS2_PLACEMENT_3D('',#75150,#56138,#56139) ;
#49769 = AXIS2_PLACEMENT_3D('',#75152,#56140,#56141) ;
#49770 = AXIS2_PLACEMENT_3D('',#75156,#56143,#56144) ;
#49771 = AXIS2_PLACEMENT_3D('',#75160,#56146,#56147) ;
#49772 = AXIS2_PLACEMENT_3D('',#75164,#56149,#56150) ;
#49773 = AXIS2_PLACEMENT_3D('',#75168,#56152,#56153) ;
#49774 = AXIS2_PLACEMENT_3D('',#75172,#56155,#56156) ;
#49775 = AXIS2_PLACEMENT_3D('',#75176,#56158,#56159) ;
#49776 = AXIS2_PLACEMENT_3D('',#75180,#56161,#56162) ;
#49777 = AXIS2_PLACEMENT_3D('',#75184,#56164,#56165) ;
#49778 = AXIS2_PLACEMENT_3D('',#75188,#56167,#56168) ;
#49779 = AXIS2_PLACEMENT_3D('',#75192,#56170,#56171) ;
#49780 = AXIS2_PLACEMENT_3D('',#75196,#56173,#56174) ;
#49781 = AXIS2_PLACEMENT_3D('',#75198,#56176,#56177) ;
#49782 = AXIS2_PLACEMENT_3D('',#75201,#56179,#56180) ;
#49783 = AXIS2_PLACEMENT_3D('',#75202,#56181,#56182) ;
#49784 = AXIS2_PLACEMENT_3D('',#75204,#56184,#56185) ;
#49785 = AXIS2_PLACEMENT_3D('',#75205,#56186,#56187) ;
#49786 = AXIS2_PLACEMENT_3D('',#75206,#56188,#56189) ;
#49787 = AXIS2_PLACEMENT_3D('',#75207,#56190,#56191) ;
#49788 = AXIS2_PLACEMENT_3D('',#75208,#56192,#56193) ;
#49789 = AXIS2_PLACEMENT_3D('',#75209,#56194,#56195) ;
#49790 = AXIS2_PLACEMENT_3D('',#75211,#56196,#56197) ;
#49791 = AXIS2_PLACEMENT_3D('',#75213,#56198,#56199) ;
#49792 = AXIS2_PLACEMENT_3D('',#75214,#56200,#56201) ;
#49793 = AXIS2_PLACEMENT_3D('',#75215,#56202,#56203) ;
#49794 = AXIS2_PLACEMENT_3D('',#75218,#56206,#56207) ;
#49795 = AXIS2_PLACEMENT_3D('',#75221,#56209,#56210) ;
#49796 = AXIS2_PLACEMENT_3D('',#75222,#56211,#56212) ;
#49797 = AXIS2_PLACEMENT_3D('',#75224,#56214,#56215) ;
#49798 = AXIS2_PLACEMENT_3D('',#75225,#56216,#56217) ;
#49799 = AXIS2_PLACEMENT_3D('',#75227,#56218,#56219) ;
#49800 = AXIS2_PLACEMENT_3D('',#75228,#56220,#56221) ;
#49801 = AXIS2_PLACEMENT_3D('',#75229,#56222,#56223) ;
#49802 = AXIS2_PLACEMENT_3D('',#75231,#56225,#56226) ;
#49803 = AXIS2_PLACEMENT_3D('',#75232,#56227,#56228) ;
#49804 = AXIS2_PLACEMENT_3D('',#75233,#56229,#56230) ;
#49805 = AXIS2_PLACEMENT_3D('',#75234,#56231,#56232) ;
#49806 = AXIS2_PLACEMENT_3D('',#75235,#56233,#56234) ;
#49807 = AXIS2_PLACEMENT_3D('',#75236,#56235,#56236) ;
#49808 = AXIS2_PLACEMENT_3D('',#75237,#56237,#56238) ;
#49809 = AXIS2_PLACEMENT_3D('',#75238,#56239,#56240) ;
#49810 = AXIS2_PLACEMENT_3D('',#75239,#56241,#56242) ;
#49811 = AXIS2_PLACEMENT_3D('',#75240,#56243,#56244) ;
#49812 = AXIS2_PLACEMENT_3D('',#75241,#56245,#56246) ;
#49813 = AXIS2_PLACEMENT_3D('',#75242,#56247,#56248) ;
#49814 = AXIS2_PLACEMENT_3D('',#75243,#56249,#56250) ;
#49815 = AXIS2_PLACEMENT_3D('',#75244,#56251,#56252) ;
#49816 = AXIS2_PLACEMENT_3D('',#75245,#56253,#56254) ;
#49817 = AXIS2_PLACEMENT_3D('',#75246,#56255,#56256) ;
#49818 = AXIS2_PLACEMENT_3D('',#75247,#56257,#56258) ;
#49819 = AXIS2_PLACEMENT_3D('',#75248,#56259,#56260) ;
#49820 = AXIS2_PLACEMENT_3D('',#75250,#56261,#56262) ;
#49821 = AXIS2_PLACEMENT_3D('',#75251,#56263,#56264) ;
#49822 = AXIS2_PLACEMENT_3D('',#75252,#56265,#56266) ;
#49823 = AXIS2_PLACEMENT_3D('',#75254,#56268,#56269) ;
#49824 = AXIS2_PLACEMENT_3D('',#75256,#56270,#56271) ;
#49825 = AXIS2_PLACEMENT_3D('',#75258,#56272,#56273) ;
#49826 = AXIS2_PLACEMENT_3D('',#75259,#56274,#56275) ;
#49827 = AXIS2_PLACEMENT_3D('',#75260,#56276,#56277) ;
#49828 = AXIS2_PLACEMENT_3D('',#75262,#56279,#56280) ;
#49829 = AXIS2_PLACEMENT_3D('',#75265,#56283,#56284) ;
#49830 = AXIS2_PLACEMENT_3D('',#75267,#56285,#56286) ;
#49831 = AXIS2_PLACEMENT_3D('',#75269,#56287,#56288) ;
#49832 = AXIS2_PLACEMENT_3D('',#75270,#56289,#56290) ;
#49833 = AXIS2_PLACEMENT_3D('',#75271,#56291,#56292) ;
#49834 = AXIS2_PLACEMENT_3D('',#75273,#56294,#56295) ;
#49835 = AXIS2_PLACEMENT_3D('',#75275,#56296,#56297) ;
#49836 = AXIS2_PLACEMENT_3D('',#75276,#56298,#56299) ;
#49837 = AXIS2_PLACEMENT_3D('',#75277,#56300,#56301) ;
#49838 = AXIS2_PLACEMENT_3D('',#75279,#56303,#56304) ;
#49839 = AXIS2_PLACEMENT_3D('',#75281,#56306,#56307) ;
#49840 = AXIS2_PLACEMENT_3D('',#75284,#56310,#56311) ;
#49841 = AXIS2_PLACEMENT_3D('',#75286,#56313,#56314) ;
#49842 = AXIS2_PLACEMENT_3D('',#75287,#56315,#56316) ;
#49843 = AXIS2_PLACEMENT_3D('',#75288,#56317,#56318) ;
#49844 = AXIS2_PLACEMENT_3D('',#75289,#56319,#56320) ;
#49845 = AXIS2_PLACEMENT_3D('',#75290,#56321,#56322) ;
#49846 = AXIS2_PLACEMENT_3D('',#75291,#56323,#56324) ;
#49847 = AXIS2_PLACEMENT_3D('',#75292,#56325,#56326) ;
#49848 = AXIS2_PLACEMENT_3D('',#75293,#56327,#56328) ;
#49849 = AXIS2_PLACEMENT_3D('',#75294,#56329,#56330) ;
#49850 = AXIS2_PLACEMENT_3D('',#75295,#56331,#56332) ;
#49851 = AXIS2_PLACEMENT_3D('',#75296,#56333,#56334) ;
#49852 = AXIS2_PLACEMENT_3D('',#75297,#56335,#56336) ;
#49853 = AXIS2_PLACEMENT_3D('',#75298,#56337,#56338) ;
#49854 = AXIS2_PLACEMENT_3D('',#75299,#56339,#56340) ;
#49855 = AXIS2_PLACEMENT_3D('',#75300,#56341,#56342) ;
#49856 = AXIS2_PLACEMENT_3D('',#75301,#56343,#56344) ;
#49857 = AXIS2_PLACEMENT_3D('',#75302,#56345,#56346) ;
#49858 = AXIS2_PLACEMENT_3D('',#75303,#56347,#56348) ;
#49859 = AXIS2_PLACEMENT_3D('',#75304,#56349,#56350) ;
#49860 = AXIS2_PLACEMENT_3D('',#75305,#56351,#56352) ;
#49861 = AXIS2_PLACEMENT_3D('',#75306,#56353,#56354) ;
#49862 = AXIS2_PLACEMENT_3D('',#75307,#56355,#56356) ;
#49863 = AXIS2_PLACEMENT_3D('',#75308,#56357,#56358) ;
#49864 = AXIS2_PLACEMENT_3D('',#75309,#56359,#56360) ;
#49865 = AXIS2_PLACEMENT_3D('',#75310,#56361,#56362) ;
#49866 = AXIS2_PLACEMENT_3D('',#75311,#56363,#56364) ;
#49867 = AXIS2_PLACEMENT_3D('',#75338,#56365,#56366) ;
#49868 = AXIS2_PLACEMENT_3D('',#75379,#56367,#56368) ;
#49869 = AXIS2_PLACEMENT_3D('',#75381,#56369,#56370) ;
#49870 = AXIS2_PLACEMENT_3D('',#75383,#56371,#56372) ;
#49871 = AXIS2_PLACEMENT_3D('',#75384,#56373,#56374) ;
#49872 = AXIS2_PLACEMENT_3D('',#75385,#56375,#56376) ;
#49873 = AXIS2_PLACEMENT_3D('',#75388,#56377,#56378) ;
#49874 = AXIS2_PLACEMENT_3D('',#75498,#56381,#56382) ;
#49875 = AXIS2_PLACEMENT_3D('',#75538,#56387,#56388) ;
#49876 = AXIS2_PLACEMENT_3D('',#75539,#56389,#56390) ;
#49877 = AXIS2_PLACEMENT_3D('',#75561,#56391,#56392) ;
#49878 = AXIS2_PLACEMENT_3D('',#75563,#56393,#56394) ;
#49879 = AXIS2_PLACEMENT_3D('',#75564,#56395,#56396) ;
#49880 = AXIS2_PLACEMENT_3D('',#75587,#56397,#56398) ;
#49881 = AXIS2_PLACEMENT_3D('',#75594,#56399,#56400) ;
#49882 = AXIS2_PLACEMENT_3D('',#75637,#56401,#56402) ;
#49883 = AXIS2_PLACEMENT_3D('',#75644,#56403,#56404) ;
#49884 = AXIS2_PLACEMENT_3D('',#75647,#56405,#56406) ;
#49885 = AXIS2_PLACEMENT_3D('',#75671,#56409,#56410) ;
#49886 = AXIS2_PLACEMENT_3D('',#75673,#56411,#56412) ;
#49887 = AXIS2_PLACEMENT_3D('',#75674,#56413,#56414) ;
#49888 = AXIS2_PLACEMENT_3D('',#75697,#56415,#56416) ;
#49889 = AXIS2_PLACEMENT_3D('',#75744,#56417,#56418) ;
#49890 = AXIS2_PLACEMENT_3D('',#75751,#56419,#56420) ;
#49891 = AXIS2_PLACEMENT_3D('',#75754,#56421,#56422) ;
#49892 = AXIS2_PLACEMENT_3D('',#75777,#56425,#56426) ;
#49893 = AXIS2_PLACEMENT_3D('',#75778,#56427,#56428) ;
#49894 = AXIS2_PLACEMENT_3D('',#75790,#56430,#56431) ;
#49895 = AXIS2_PLACEMENT_3D('',#75792,#56433,#56434) ;
#49896 = AXIS2_PLACEMENT_3D('',#75833,#56439,#56440) ;
#49897 = AXIS2_PLACEMENT_3D('',#75838,#56442,#56443) ;
#49898 = AXIS2_PLACEMENT_3D('',#75844,#56446,#56447) ;
#49899 = AXIS2_PLACEMENT_3D('',#75846,#56448,#56449) ;
#49900 = AXIS2_PLACEMENT_3D('',#75848,#56450,#56451) ;
#49901 = AXIS2_PLACEMENT_3D('',#75850,#56452,#56453) ;
#49902 = AXIS2_PLACEMENT_3D('',#75852,#56454,#56455) ;
#49903 = AXIS2_PLACEMENT_3D('',#75860,#56456,#56457) ;
#49904 = AXIS2_PLACEMENT_3D('',#75884,#56459,#56460) ;
#49905 = AXIS2_PLACEMENT_3D('',#75886,#56461,#56462) ;
#49906 = AXIS2_PLACEMENT_3D('',#75888,#56463,#56464) ;
#49907 = AXIS2_PLACEMENT_3D('',#75891,#56466,#56467) ;
#49908 = AXIS2_PLACEMENT_3D('',#75896,#56469,#56470) ;
#49909 = AXIS2_PLACEMENT_3D('',#75898,#56471,#56472) ;
#49910 = AXIS2_PLACEMENT_3D('',#75915,#56474,#56475) ;
#49911 = AXIS2_PLACEMENT_3D('',#75931,#56476,#56477) ;
#49912 = AXIS2_PLACEMENT_3D('',#75933,#56478,#56479) ;
#49913 = AXIS2_PLACEMENT_3D('',#75951,#56481,#56482) ;
#49914 = AXIS2_PLACEMENT_3D('',#75953,#56483,#56484) ;
#49915 = AXIS2_PLACEMENT_3D('',#75957,#56486,#56487) ;
#49916 = AXIS2_PLACEMENT_3D('',#75960,#56489,#56490) ;
#49917 = AXIS2_PLACEMENT_3D('',#75961,#56491,#56492) ;
#49918 = AXIS2_PLACEMENT_3D('',#75963,#56493,#56494) ;
#49919 = AXIS2_PLACEMENT_3D('',#75966,#56496,#56497) ;
#49920 = AXIS2_PLACEMENT_3D('',#75988,#56498,#56499) ;
#49921 = AXIS2_PLACEMENT_3D('',#75989,#56500,#56501) ;
#49922 = AXIS2_PLACEMENT_3D('',#76011,#56502,#56503) ;
#49923 = AXIS2_PLACEMENT_3D('',#76053,#56504,#56505) ;
#49924 = AXIS2_PLACEMENT_3D('',#76054,#56506,#56507) ;
#49925 = AXIS2_PLACEMENT_3D('',#76056,#56508,#56509) ;
#49926 = AXIS2_PLACEMENT_3D('',#76089,#56511,#56512) ;
#49927 = AXIS2_PLACEMENT_3D('',#76111,#56513,#56514) ;
#49928 = AXIS2_PLACEMENT_3D('',#76198,#56519,#56520) ;
#49929 = AXIS2_PLACEMENT_3D('',#76199,#56521,#56522) ;
#49930 = AXIS2_PLACEMENT_3D('',#76203,#56525,#56526) ;
#49931 = AXIS2_PLACEMENT_3D('',#76205,#56527,#56528) ;
#49932 = AXIS2_PLACEMENT_3D('',#76206,#56529,#56530) ;
#49933 = AXIS2_PLACEMENT_3D('',#76207,#56531,#56532) ;
#49934 = AXIS2_PLACEMENT_3D('',#76209,#56533,#56534) ;
#49935 = AXIS2_PLACEMENT_3D('',#76211,#56536,#56537) ;
#49936 = AXIS2_PLACEMENT_3D('',#76213,#56538,#56539) ;
#49937 = AXIS2_PLACEMENT_3D('',#76216,#56541,#56542) ;
#49938 = AXIS2_PLACEMENT_3D('',#76217,#56543,#56544) ;
#49939 = AXIS2_PLACEMENT_3D('',#76235,#56545,#56546) ;
#49940 = AXIS2_PLACEMENT_3D('',#76236,#56547,#56548) ;
#49941 = AXIS2_PLACEMENT_3D('',#76274,#56550,#56551) ;
#49942 = AXIS2_PLACEMENT_3D('',#76275,#56552,#56553) ;
#49943 = AXIS2_PLACEMENT_3D('',#76297,#56554,#56555) ;
#49944 = AXIS2_PLACEMENT_3D('',#76298,#56556,#56557) ;
#49945 = AXIS2_PLACEMENT_3D('',#76320,#56558,#56559) ;
#49946 = AXIS2_PLACEMENT_3D('',#76321,#56560,#56561) ;
#49947 = AXIS2_PLACEMENT_3D('',#76348,#56562,#56563) ;
#49948 = AXIS2_PLACEMENT_3D('',#76384,#56564,#56565) ;
#49949 = AXIS2_PLACEMENT_3D('',#76431,#56566,#56567) ;
#49950 = AXIS2_PLACEMENT_3D('',#76439,#56568,#56569) ;
#49951 = AXIS2_PLACEMENT_3D('',#76441,#56570,#56571) ;
#49952 = AXIS2_PLACEMENT_3D('',#76464,#56573,#56574) ;
#49953 = AXIS2_PLACEMENT_3D('',#76465,#56575,#56576) ;
#49954 = AXIS2_PLACEMENT_3D('',#76492,#56577,#56578) ;
#49955 = AXIS2_PLACEMENT_3D('',#76524,#56579,#56580) ;
#49956 = AXIS2_PLACEMENT_3D('',#76525,#56581,#56582) ;
#49957 = AXIS2_PLACEMENT_3D('',#76547,#56583,#56584) ;
#49958 = AXIS2_PLACEMENT_3D('',#76548,#56585,#56586) ;
#49959 = AXIS2_PLACEMENT_3D('',#76570,#56587,#56588) ;
#49960 = AXIS2_PLACEMENT_3D('',#76571,#56589,#56590) ;
#49961 = AXIS2_PLACEMENT_3D('',#76593,#56591,#56592) ;
#49962 = AXIS2_PLACEMENT_3D('',#76594,#56593,#56594) ;
#49963 = AXIS2_PLACEMENT_3D('',#76616,#56595,#56596) ;
#49964 = AXIS2_PLACEMENT_3D('',#76617,#56597,#56598) ;
#49965 = AXIS2_PLACEMENT_3D('',#76618,#56599,#56600) ;
#49966 = AXIS2_PLACEMENT_3D('',#76621,#56602,#56603) ;
#49967 = AXIS2_PLACEMENT_3D('',#76622,#56604,#56605) ;
#49968 = AXIS2_PLACEMENT_3D('',#76650,#56607,#56608) ;
#49969 = AXIS2_PLACEMENT_3D('',#76651,#56609,#56610) ;
#49970 = AXIS2_PLACEMENT_3D('',#76681,#56613,#56614) ;
#49971 = AXIS2_PLACEMENT_3D('',#76684,#56616,#56617) ;
#49972 = AXIS2_PLACEMENT_3D('',#76707,#56619,#56620) ;
#49973 = AXIS2_PLACEMENT_3D('',#76723,#56622,#56623) ;
#49974 = AXIS2_PLACEMENT_3D('',#76727,#56626,#56627) ;
#49975 = AXIS2_PLACEMENT_3D('',#76760,#56629,#56630) ;
#49976 = AXIS2_PLACEMENT_3D('',#76777,#56632,#56633) ;
#49977 = AXIS2_PLACEMENT_3D('',#76781,#56636,#56637) ;
#49978 = AXIS2_PLACEMENT_3D('',#76785,#56640,#56641) ;
#49979 = AXIS2_PLACEMENT_3D('',#76788,#56643,#56644) ;
#49980 = AXIS2_PLACEMENT_3D('',#76789,#56645,#56646) ;
#49981 = AXIS2_PLACEMENT_3D('',#76793,#56649,#56650) ;
#49982 = AXIS2_PLACEMENT_3D('',#76810,#56651,#56652) ;
#49983 = AXIS2_PLACEMENT_3D('',#76851,#56653,#56654) ;
#49984 = AXIS2_PLACEMENT_3D('',#76858,#56655,#56656) ;
#49985 = AXIS2_PLACEMENT_3D('',#76859,#56657,#56658) ;
#49986 = AXIS2_PLACEMENT_3D('',#76862,#56659,#56660) ;
#49987 = AXIS2_PLACEMENT_3D('',#76864,#56661,#56662) ;
#49988 = AXIS2_PLACEMENT_3D('',#76865,#56663,#56664) ;
#49989 = AXIS2_PLACEMENT_3D('',#76914,#56667,#56668) ;
#49990 = AXIS2_PLACEMENT_3D('',#76922,#56669,#56670) ;
#49991 = AXIS2_PLACEMENT_3D('',#76923,#56671,#56672) ;
#49992 = AXIS2_PLACEMENT_3D('',#76926,#56673,#56674) ;
#49993 = AXIS2_PLACEMENT_3D('',#76928,#56675,#56676) ;
#49994 = AXIS2_PLACEMENT_3D('',#76930,#56677,#56678) ;
#49995 = AXIS2_PLACEMENT_3D('',#76931,#56679,#56680) ;
#49996 = AXIS2_PLACEMENT_3D('',#76968,#56683,#56684) ;
#49997 = AXIS2_PLACEMENT_3D('',#76970,#56685,#56686) ;
#49998 = AXIS2_PLACEMENT_3D('',#76972,#56687,#56688) ;
#49999 = AXIS2_PLACEMENT_3D('',#76973,#56689,#56690) ;
#50000 = AXIS2_PLACEMENT_3D('',#76994,#56691,#56692) ;
#50001 = AXIS2_PLACEMENT_3D('',#76995,#56693,#56694) ;
#50002 = AXIS2_PLACEMENT_3D('',#76996,#56695,#56696) ;
#50003 = AXIS2_PLACEMENT_3D('',#76999,#56699,#56700) ;
#50004 = AXIS2_PLACEMENT_3D('',#77038,#56702,#56703) ;
#50005 = AXIS2_PLACEMENT_3D('',#77039,#56704,#56705) ;
#50006 = AXIS2_PLACEMENT_3D('',#77075,#56706,#56707) ;
#50007 = AXIS2_PLACEMENT_3D('',#77076,#56708,#56709) ;
#50008 = AXIS2_PLACEMENT_3D('',#77097,#56710,#56711) ;
#50009 = AXIS2_PLACEMENT_3D('',#77119,#56712,#56713) ;
#50010 = AXIS2_PLACEMENT_3D('',#77121,#56714,#56715) ;
#50011 = AXIS2_PLACEMENT_3D('',#77122,#56716,#56717) ;
#50012 = AXIS2_PLACEMENT_3D('',#77145,#56718,#56719) ;
#50013 = AXIS2_PLACEMENT_3D('',#77146,#56720,#56721) ;
#50014 = AXIS2_PLACEMENT_3D('',#77147,#56722,#56723) ;
#50015 = AXIS2_PLACEMENT_3D('',#77148,#56724,#56725) ;
#50016 = AXIS2_PLACEMENT_3D('',#77163,#56728,#56729) ;
#50017 = AXIS2_PLACEMENT_3D('',#77186,#56731,#56732) ;
#50018 = AXIS2_PLACEMENT_3D('',#77187,#56733,#56734) ;
#50019 = AXIS2_PLACEMENT_3D('',#77209,#56735,#56736) ;
#50020 = AXIS2_PLACEMENT_3D('',#77210,#56737,#56738) ;
#50021 = AXIS2_PLACEMENT_3D('',#77211,#56739,#56740) ;
#50022 = AXIS2_PLACEMENT_3D('',#77246,#56742,#56743) ;
#50023 = AXIS2_PLACEMENT_3D('',#77247,#56744,#56745) ;
#50024 = AXIS2_PLACEMENT_3D('',#77252,#56748,#56749) ;
#50025 = AXIS2_PLACEMENT_3D('',#77271,#56752,#56753) ;
#50026 = AXIS2_PLACEMENT_3D('',#77275,#56755,#56756) ;
#50027 = AXIS2_PLACEMENT_3D('',#77277,#56758,#56759) ;
#50028 = AXIS2_PLACEMENT_3D('',#77304,#56760,#56761) ;
#50029 = AXIS2_PLACEMENT_3D('',#77311,#56762,#56763) ;
#50030 = AXIS2_PLACEMENT_3D('',#77333,#56764,#56765) ;
#50031 = AXIS2_PLACEMENT_3D('',#77334,#56766,#56767) ;
#50032 = AXIS2_PLACEMENT_3D('',#77356,#56768,#56769) ;
#50033 = AXIS2_PLACEMENT_3D('',#77357,#56770,#56771) ;
#50034 = AXIS2_PLACEMENT_3D('',#77358,#56772,#56773) ;
#50035 = AXIS2_PLACEMENT_3D('',#77360,#56774,#56775) ;
#50036 = AXIS2_PLACEMENT_3D('',#77394,#56777,#56778) ;
#50037 = AXIS2_PLACEMENT_3D('',#77428,#56779,#56780) ;
#50038 = AXIS2_PLACEMENT_3D('',#77430,#56781,#56782) ;
#50039 = AXIS2_PLACEMENT_3D('',#77462,#56783,#56784) ;
#50040 = AXIS2_PLACEMENT_3D('',#77473,#56785,#56786) ;
#50041 = AXIS2_PLACEMENT_3D('',#77476,#56789,#56790) ;
#50042 = AXIS2_PLACEMENT_3D('',#77509,#56791,#56792) ;
#50043 = AXIS2_PLACEMENT_3D('',#77518,#56793,#56794) ;
#50044 = AXIS2_PLACEMENT_3D('',#77550,#56795,#56796) ;
#50045 = AXIS2_PLACEMENT_3D('',#77576,#56797,#56798) ;
#50046 = AXIS2_PLACEMENT_3D('',#77577,#56799,#56800) ;
#50047 = AXIS2_PLACEMENT_3D('',#77578,#56801,#56802) ;
#50048 = AXIS2_PLACEMENT_3D('',#77580,#56803,#56804) ;
#50049 = AXIS2_PLACEMENT_3D('',#77618,#56806,#56807) ;
#50050 = AXIS2_PLACEMENT_3D('',#77647,#56808,#56809) ;
#50051 = AXIS2_PLACEMENT_3D('',#77674,#56810,#56811) ;
#50052 = AXIS2_PLACEMENT_3D('',#77675,#56812,#56813) ;
#50053 = AXIS2_PLACEMENT_3D('',#77676,#56814,#56815) ;
#50054 = AXIS2_PLACEMENT_3D('',#77677,#56816,#56817) ;
#50055 = AXIS2_PLACEMENT_3D('',#77708,#56822,#56823) ;
#50056 = AXIS2_PLACEMENT_3D('',#77709,#56824,#56825) ;
#50057 = AXIS2_PLACEMENT_3D('',#77712,#56826,#56827) ;
#50058 = AXIS2_PLACEMENT_3D('',#77714,#56828,#56829) ;
#50059 = AXIS2_PLACEMENT_3D('',#77715,#56830,#56831) ;
#50060 = AXIS2_PLACEMENT_3D('',#77743,#56832,#56833) ;
#50061 = AXIS2_PLACEMENT_3D('',#77745,#56834,#56835) ;
#50062 = AXIS2_PLACEMENT_3D('',#77747,#56836,#56837) ;
#50063 = AXIS2_PLACEMENT_3D('',#77763,#56840,#56841) ;
#50064 = AXIS2_PLACEMENT_3D('',#77766,#56842,#56843) ;
#50065 = AXIS2_PLACEMENT_3D('',#77768,#56844,#56845) ;
#50066 = AXIS2_PLACEMENT_3D('',#77770,#56846,#56847) ;
#50067 = AXIS2_PLACEMENT_3D('',#77772,#56848,#56849) ;
#50068 = AXIS2_PLACEMENT_3D('',#77773,#56850,#56851) ;
#50069 = AXIS2_PLACEMENT_3D('',#77774,#56852,#56853) ;
#50070 = AXIS2_PLACEMENT_3D('',#77803,#56856,#56857) ;
#50071 = AXIS2_PLACEMENT_3D('',#77832,#56858,#56859) ;
#50072 = AXIS2_PLACEMENT_3D('',#77834,#56860,#56861) ;
#50073 = AXIS2_PLACEMENT_3D('',#77835,#56862,#56863) ;
#50074 = AXIS2_PLACEMENT_3D('',#77836,#56864,#56865) ;
#50075 = AXIS2_PLACEMENT_3D('',#77839,#56866,#56867) ;
#50076 = AXIS2_PLACEMENT_3D('',#77886,#56870,#56871) ;
#50077 = AXIS2_PLACEMENT_3D('',#77959,#56872,#56873) ;
#50078 = AXIS2_PLACEMENT_3D('',#77968,#56874,#56875) ;
#50079 = AXIS2_PLACEMENT_3D('',#77978,#56876,#56877) ;
#50080 = AXIS2_PLACEMENT_3D('',#78026,#56880,#56881) ;
#50081 = AXIS2_PLACEMENT_3D('',#78052,#56882,#56883) ;
#50082 = AXIS2_PLACEMENT_3D('',#78054,#56884,#56885) ;
#50083 = AXIS2_PLACEMENT_3D('',#78055,#56886,#56887) ;
#50084 = AXIS2_PLACEMENT_3D('',#78056,#56888,#56889) ;
#50085 = AXIS2_PLACEMENT_3D('',#78059,#56890,#56891) ;
#50086 = AXIS2_PLACEMENT_3D('',#78100,#56894,#56895) ;
#50087 = AXIS2_PLACEMENT_3D('',#78135,#56896,#56897) ;
#50088 = AXIS2_PLACEMENT_3D('',#78169,#56903,#56904) ;
#50089 = AXIS2_PLACEMENT_3D('',#78179,#56906,#56907) ;
#50090 = AXIS2_PLACEMENT_3D('',#78182,#56908,#56909) ;
#50091 = AXIS2_PLACEMENT_3D('',#78214,#56912,#56913) ;
#50092 = AXIS2_PLACEMENT_3D('',#78222,#56914,#56915) ;
#50093 = AXIS2_PLACEMENT_3D('',#78223,#56916,#56917) ;
#50094 = AXIS2_PLACEMENT_3D('',#78266,#56920,#56921) ;
#50095 = AXIS2_PLACEMENT_3D('',#78267,#56922,#56923) ;
#50096 = AXIS2_PLACEMENT_3D('',#78304,#56924,#56925) ;
#50097 = AXIS2_PLACEMENT_3D('',#78313,#56926,#56927) ;
#50098 = AXIS2_PLACEMENT_3D('',#78314,#56928,#56929) ;
#50099 = AXIS2_PLACEMENT_3D('',#78317,#56930,#56931) ;
#50100 = AXIS2_PLACEMENT_3D('',#78319,#56932,#56933) ;
#50101 = AXIS2_PLACEMENT_3D('',#78320,#56934,#56935) ;
#50102 = AXIS2_PLACEMENT_3D('',#78363,#56938,#56939) ;
#50103 = AXIS2_PLACEMENT_3D('',#78365,#56940,#56941) ;
#50104 = AXIS2_PLACEMENT_3D('',#78366,#56942,#56943) ;
#50105 = AXIS2_PLACEMENT_3D('',#78393,#56944,#56945) ;
#50106 = AXIS2_PLACEMENT_3D('',#78400,#56946,#56947) ;
#50107 = AXIS2_PLACEMENT_3D('',#78401,#56948,#56949) ;
#50108 = AXIS2_PLACEMENT_3D('',#78404,#56950,#56951) ;
#50109 = AXIS2_PLACEMENT_3D('',#78406,#56952,#56953) ;
#50110 = AXIS2_PLACEMENT_3D('',#78407,#56954,#56955) ;
#50111 = AXIS2_PLACEMENT_3D('',#78418,#56958,#56959) ;
#50112 = AXIS2_PLACEMENT_3D('',#78421,#56960,#56961) ;
#50113 = AXIS2_PLACEMENT_3D('',#78423,#56962,#56963) ;
#50114 = AXIS2_PLACEMENT_3D('',#78424,#56964,#56965) ;
#50115 = AXIS2_PLACEMENT_3D('',#78489,#56966,#56967) ;
#50116 = AXIS2_PLACEMENT_3D('',#78498,#56968,#56969) ;
#50117 = AXIS2_PLACEMENT_3D('',#78499,#56970,#56971) ;
#50118 = AXIS2_PLACEMENT_3D('',#78502,#56972,#56973) ;
#50119 = AXIS2_PLACEMENT_3D('',#78504,#56974,#56975) ;
#50120 = AXIS2_PLACEMENT_3D('',#78506,#56976,#56977) ;
#50121 = AXIS2_PLACEMENT_3D('',#78507,#56978,#56979) ;
#50122 = AXIS2_PLACEMENT_3D('',#78524,#56982,#56983) ;
#50123 = AXIS2_PLACEMENT_3D('',#78551,#56986,#56987) ;
#50124 = AXIS2_PLACEMENT_3D('',#78572,#56988,#56989) ;
#50125 = AXIS2_PLACEMENT_3D('',#78573,#56990,#56991) ;
#50126 = AXIS2_PLACEMENT_3D('',#78587,#56995,#56996) ;
#50127 = AXIS2_PLACEMENT_3D('',#78614,#56999,#57000) ;
#50128 = AXIS2_PLACEMENT_3D('',#78630,#57002,#57003) ;
#50129 = AXIS2_PLACEMENT_3D('',#78631,#57004,#57005) ;
#50130 = AXIS2_PLACEMENT_3D('',#78640,#57006,#57007) ;
#50131 = AXIS2_PLACEMENT_3D('',#78691,#57008,#57009) ;
#50132 = AXIS2_PLACEMENT_3D('',#78693,#57010,#57011) ;
#50133 = AXIS2_PLACEMENT_3D('',#78720,#57012,#57013) ;
#50134 = AXIS2_PLACEMENT_3D('',#78721,#57014,#57015) ;
#50135 = AXIS2_PLACEMENT_3D('',#78766,#57020,#57021) ;
#50136 = AXIS2_PLACEMENT_3D('',#78770,#57024,#57025) ;
#50137 = AXIS2_PLACEMENT_3D('',#78771,#57026,#57027) ;
#50138 = AXIS2_PLACEMENT_3D('',#78773,#57028,#57029) ;
#50139 = AXIS2_PLACEMENT_3D('',#78774,#57030,#57031) ;
#50140 = AXIS2_PLACEMENT_3D('',#78775,#57032,#57033) ;
#50141 = AXIS2_PLACEMENT_3D('',#78808,#57034,#57035) ;
#50142 = AXIS2_PLACEMENT_3D('',#78829,#57036,#57037) ;
#50143 = AXIS2_PLACEMENT_3D('',#78850,#57038,#57039) ;
#50144 = AXIS2_PLACEMENT_3D('',#78876,#57040,#57041) ;
#50145 = AXIS2_PLACEMENT_3D('',#78898,#57042,#57043) ;
#50146 = AXIS2_PLACEMENT_3D('',#78899,#57044,#57045) ;
#50147 = AXIS2_PLACEMENT_3D('',#78900,#57046,#57047) ;
#50148 = AXIS2_PLACEMENT_3D('',#78902,#57048,#57049) ;
#50149 = AXIS2_PLACEMENT_3D('',#78940,#57051,#57052) ;
#50150 = AXIS2_PLACEMENT_3D('',#78974,#57053,#57054) ;
#50151 = AXIS2_PLACEMENT_3D('',#79010,#57055,#57056) ;
#50152 = AXIS2_PLACEMENT_3D('',#79041,#57057,#57058) ;
#50153 = AXIS2_PLACEMENT_3D('',#79042,#57059,#57060) ;
#50154 = AXIS2_PLACEMENT_3D('',#79043,#57061,#57062) ;
#50155 = AXIS2_PLACEMENT_3D('',#79100,#57067,#57068) ;
#50156 = AXIS2_PLACEMENT_3D('',#79134,#57075,#57076) ;
#50157 = AXIS2_PLACEMENT_3D('',#79173,#57079,#57080) ;
#50158 = AXIS2_PLACEMENT_3D('',#79188,#57081,#57082) ;
#50159 = AXIS2_PLACEMENT_3D('',#79190,#57084,#57085) ;
#50160 = AXIS2_PLACEMENT_3D('',#79191,#57086,#57087) ;
#50161 = AXIS2_PLACEMENT_3D('',#79193,#57089,#57090) ;
#50162 = AXIS2_PLACEMENT_3D('',#79195,#57092,#57093) ;
#50163 = AXIS2_PLACEMENT_3D('',#79196,#57094,#57095) ;
#50164 = AXIS2_PLACEMENT_3D('',#79197,#57096,#57097) ;
#50165 = AXIS2_PLACEMENT_3D('',#79541,#57098,#57099) ;
#50166 = AXIS2_PLACEMENT_3D('',#79545,#57101,#57102) ;
#50167 = AXIS2_PLACEMENT_3D('',#79547,#57104,#57105) ;
#50168 = AXIS2_PLACEMENT_3D('',#79552,#57108,#57109) ;
#50169 = AXIS2_PLACEMENT_3D('',#79553,#57110,#57111) ;
#50170 = AXIS2_PLACEMENT_3D('',#79726,#57114,#57115) ;
#50171 = AXIS2_PLACEMENT_3D('',#79732,#57119,#57120) ;
#50172 = AXIS2_PLACEMENT_3D('',#79736,#57123,#57124) ;
#50173 = AXIS2_PLACEMENT_3D('',#79758,#57128,#57129) ;
#50174 = AXIS2_PLACEMENT_3D('',#79872,#57138,#57139) ;
#50175 = AXIS2_PLACEMENT_3D('',#79874,#57140,#57141) ;
#50176 = AXIS2_PLACEMENT_3D('',#79899,#57143,#57144) ;
#50177 = AXIS2_PLACEMENT_3D('',#79901,#57145,#57146) ;
#50178 = AXIS2_PLACEMENT_3D('',#79903,#57148,#57149) ;
#50179 = AXIS2_PLACEMENT_3D('',#80157,#57151,#57152) ;
#50180 = AXIS2_PLACEMENT_3D('',#80263,#57153,#57154) ;
#50181 = AXIS2_PLACEMENT_3D('',#80267,#57156,#57157) ;
#50182 = AXIS2_PLACEMENT_3D('',#80268,#57158,#57159) ;
#50183 = AXIS2_PLACEMENT_3D('',#80331,#57160,#57161) ;
#50184 = AXIS2_PLACEMENT_3D('',#80333,#57162,#57163) ;
#50185 = AXIS2_PLACEMENT_3D('',#80335,#57165,#57166) ;
#50186 = AXIS2_PLACEMENT_3D('',#80338,#57168,#57169) ;
#50187 = AXIS2_PLACEMENT_3D('',#80339,#57170,#57171) ;
#50188 = AXIS2_PLACEMENT_3D('',#80342,#57173,#57174) ;
#50189 = AXIS2_PLACEMENT_3D('',#80343,#57175,#57176) ;
#50190 = AXIS2_PLACEMENT_3D('',#80868,#57181,#57182) ;
#50191 = AXIS2_PLACEMENT_3D('',#80872,#57185,#57186) ;
#50192 = AXIS2_PLACEMENT_3D('',#80876,#57189,#57190) ;
#50193 = AXIS2_PLACEMENT_3D('',#80980,#57197,#57198) ;
#50194 = AXIS2_PLACEMENT_3D('',#81071,#57201,#57202) ;
#50195 = AXIS2_PLACEMENT_3D('',#81091,#57204,#57205) ;
#50196 = AXIS2_PLACEMENT_3D('',#81092,#57206,#57207) ;
#50197 = AXIS2_PLACEMENT_3D('',#81118,#57209,#57210) ;
#50198 = AXIS2_PLACEMENT_3D('',#81227,#57211,#57212) ;
#50199 = AXIS2_PLACEMENT_3D('',#81516,#57214,#57215) ;
#50200 = AXIS2_PLACEMENT_3D('',#81517,#57216,#57217) ;
#50201 = AXIS2_PLACEMENT_3D('',#81522,#57219,#57220) ;
#50202 = AXIS2_PLACEMENT_3D('',#81525,#57222,#57223) ;
#50203 = AXIS2_PLACEMENT_3D('',#81526,#57224,#57225) ;
#50204 = AXIS2_PLACEMENT_3D('',#81531,#57228,#57229) ;
#50205 = AXIS2_PLACEMENT_3D('',#81532,#57230,#57231) ;
#50206 = AXIS2_PLACEMENT_3D('',#81535,#57234,#57235) ;
#50207 = AXIS2_PLACEMENT_3D('',#81541,#57239,#57240) ;
#50208 = AXIS2_PLACEMENT_3D('',#81545,#57243,#57244) ;
#50209 = AXIS2_PLACEMENT_3D('',#81546,#57245,#57246) ;
#50210 = AXIS2_PLACEMENT_3D('',#81551,#57248,#57249) ;
#50211 = AXIS2_PLACEMENT_3D('',#81554,#57251,#57252) ;
#50212 = AXIS2_PLACEMENT_3D('',#81555,#57253,#57254) ;
#50213 = AXIS2_PLACEMENT_3D('',#81560,#57257,#57258) ;
#50214 = AXIS2_PLACEMENT_3D('',#81561,#57259,#57260) ;
#50215 = AXIS2_PLACEMENT_3D('',#81566,#57263,#57264) ;
#50216 = AXIS2_PLACEMENT_3D('',#81567,#57265,#57266) ;
#50217 = AXIS2_PLACEMENT_3D('',#81570,#57269,#57270) ;
#50218 = AXIS2_PLACEMENT_3D('',#81576,#57274,#57275) ;
#50219 = AXIS2_PLACEMENT_3D('',#81580,#57278,#57279) ;
#50220 = AXIS2_PLACEMENT_3D('',#81581,#57280,#57281) ;
#50221 = AXIS2_PLACEMENT_3D('',#81586,#57283,#57284) ;
#50222 = AXIS2_PLACEMENT_3D('',#81589,#57286,#57287) ;
#50223 = AXIS2_PLACEMENT_3D('',#81590,#57288,#57289) ;
#50224 = AXIS2_PLACEMENT_3D('',#81595,#57292,#57293) ;
#50225 = AXIS2_PLACEMENT_3D('',#81596,#57294,#57295) ;
#50226 = AXIS2_PLACEMENT_3D('',#81599,#57298,#57299) ;
#50227 = AXIS2_PLACEMENT_3D('',#81605,#57303,#57304) ;
#50228 = AXIS2_PLACEMENT_3D('',#81609,#57307,#57308) ;
#50229 = AXIS2_PLACEMENT_3D('',#81610,#57309,#57310) ;
#50230 = AXIS2_PLACEMENT_3D('',#81634,#57312,#57313) ;
#50231 = AXIS2_PLACEMENT_3D('',#81791,#57314,#57315) ;
#50232 = AXIS2_PLACEMENT_3D('',#81793,#57316,#57317) ;
#50233 = AXIS2_PLACEMENT_3D('',#81796,#57319,#57320) ;
#50234 = AXIS2_PLACEMENT_3D('',#82250,#57321,#57322) ;
#50235 = AXIS2_PLACEMENT_3D('',#82254,#57324,#57325) ;
#50236 = AXIS2_PLACEMENT_3D('',#82257,#57327,#57328) ;
#50237 = AXIS2_PLACEMENT_3D('',#82258,#57329,#57330) ;
#50238 = AXIS2_PLACEMENT_3D('',#82262,#57332,#57333) ;
#50239 = AXIS2_PLACEMENT_3D('',#82264,#57335,#57336) ;
#50240 = AXIS2_PLACEMENT_3D('',#82268,#57338,#57339) ;
#50241 = AXIS2_PLACEMENT_3D('',#82270,#57341,#57342) ;
#50242 = AXIS2_PLACEMENT_3D('',#82304,#57345,#57346) ;
#50243 = AXIS2_PLACEMENT_3D('',#82326,#57347,#57348) ;
#50244 = AXIS2_PLACEMENT_3D('',#82500,#57350,#57351) ;
#50245 = AXIS2_PLACEMENT_3D('',#82547,#57358,#57359) ;
#50246 = AXIS2_PLACEMENT_3D('',#82549,#57361,#57362) ;
#50247 = AXIS2_PLACEMENT_3D('',#82551,#57364,#57365) ;
#50248 = AXIS2_PLACEMENT_3D('',#82553,#57367,#57368) ;
#50249 = AXIS2_PLACEMENT_3D('',#82554,#57369,#57370) ;
#50250 = AXIS2_PLACEMENT_3D('',#82563,#57374,#57375) ;
#50251 = AXIS2_PLACEMENT_3D('',#82567,#57377,#57378) ;
#50252 = AXIS2_PLACEMENT_3D('',#82573,#57381,#57382) ;
#50253 = AXIS2_PLACEMENT_3D('',#82574,#57383,#57384) ;
#50254 = AXIS2_PLACEMENT_3D('',#82580,#57387,#57388) ;
#50255 = AXIS2_PLACEMENT_3D('',#82584,#57390,#57391) ;
#50256 = AXIS2_PLACEMENT_3D('',#82592,#57395,#57396) ;
#50257 = AXIS2_PLACEMENT_3D('',#82596,#57398,#57399) ;
#50258 = AXIS2_PLACEMENT_3D('',#82600,#57401,#57402) ;
#50259 = AXIS2_PLACEMENT_3D('',#82604,#57404,#57405) ;
#50260 = AXIS2_PLACEMENT_3D('',#82608,#57407,#57408) ;
#50261 = AXIS2_PLACEMENT_3D('',#82612,#57410,#57411) ;
#50262 = AXIS2_PLACEMENT_3D('',#82616,#57413,#57414) ;
#50263 = AXIS2_PLACEMENT_3D('',#82620,#57416,#57417) ;
#50264 = AXIS2_PLACEMENT_3D('',#82624,#57419,#57420) ;
#50265 = AXIS2_PLACEMENT_3D('',#82628,#57422,#57423) ;
#50266 = AXIS2_PLACEMENT_3D('',#82632,#57425,#57426) ;
#50267 = AXIS2_PLACEMENT_3D('',#82636,#57428,#57429) ;
#50268 = AXIS2_PLACEMENT_3D('',#82638,#57430,#57431) ;
#50269 = AXIS2_PLACEMENT_3D('',#82642,#57433,#57434) ;
#50270 = AXIS2_PLACEMENT_3D('',#82644,#57435,#57436) ;
#50271 = AXIS2_PLACEMENT_3D('',#82648,#57438,#57439) ;
#50272 = AXIS2_PLACEMENT_3D('',#82651,#57441,#57442) ;
#50273 = AXIS2_PLACEMENT_3D('',#82666,#57449,#57450) ;
#50274 = AXIS2_PLACEMENT_3D('',#82670,#57452,#57453) ;
#50275 = AXIS2_PLACEMENT_3D('',#82674,#57455,#57456) ;
#50276 = AXIS2_PLACEMENT_3D('',#82680,#57459,#57460) ;
#50277 = AXIS2_PLACEMENT_3D('',#82684,#57462,#57463) ;
#50278 = AXIS2_PLACEMENT_3D('',#82690,#57466,#57467) ;
#50279 = AXIS2_PLACEMENT_3D('',#82704,#57474,#57475) ;
#50280 = AXIS2_PLACEMENT_3D('',#82708,#57477,#57478) ;
#50281 = AXIS2_PLACEMENT_3D('',#82712,#57480,#57481) ;
#50282 = AXIS2_PLACEMENT_3D('',#82716,#57483,#57484) ;
#50283 = AXIS2_PLACEMENT_3D('',#82720,#57486,#57487) ;
#50284 = AXIS2_PLACEMENT_3D('',#82723,#57489,#57490) ;
#50285 = AXIS2_PLACEMENT_3D('',#82726,#57491,#57492) ;
#50286 = AXIS2_PLACEMENT_3D('',#82732,#57495,#57496) ;
#50287 = AXIS2_PLACEMENT_3D('',#82736,#57498,#57499) ;
#50288 = AXIS2_PLACEMENT_3D('',#82742,#57502,#57503) ;
#50289 = AXIS2_PLACEMENT_3D('',#82746,#57505,#57506) ;
#50290 = AXIS2_PLACEMENT_3D('',#82750,#57508,#57509) ;
#50291 = AXIS2_PLACEMENT_3D('',#82754,#57511,#57512) ;
#50292 = AXIS2_PLACEMENT_3D('',#82760,#57515,#57516) ;
#50293 = AXIS2_PLACEMENT_3D('',#82764,#57518,#57519) ;
#50294 = AXIS2_PLACEMENT_3D('',#82770,#57522,#57523) ;
#50295 = AXIS2_PLACEMENT_3D('',#82774,#57525,#57526) ;
#50296 = AXIS2_PLACEMENT_3D('',#82778,#57528,#57529) ;
#50297 = AXIS2_PLACEMENT_3D('',#82794,#57537,#57538) ;
#50298 = AXIS2_PLACEMENT_3D('',#82798,#57540,#57541) ;
#50299 = AXIS2_PLACEMENT_3D('',#82802,#57543,#57544) ;
#50300 = AXIS2_PLACEMENT_3D('',#82806,#57546,#57547) ;
#50301 = AXIS2_PLACEMENT_3D('',#82809,#57549,#57550) ;
#50302 = AXIS2_PLACEMENT_3D('',#82814,#57552,#57553) ;
#50303 = AXIS2_PLACEMENT_3D('',#82818,#57555,#57556) ;
#50304 = AXIS2_PLACEMENT_3D('',#82822,#57558,#57559) ;
#50305 = AXIS2_PLACEMENT_3D('',#82826,#57561,#57562) ;
#50306 = AXIS2_PLACEMENT_3D('',#82830,#57564,#57565) ;
#50307 = AXIS2_PLACEMENT_3D('',#82841,#57571,#57572) ;
#50308 = AXIS2_PLACEMENT_3D('',#82843,#57573,#57574) ;
#50309 = AXIS2_PLACEMENT_3D('',#82852,#57578,#57579) ;
#50310 = AXIS2_PLACEMENT_3D('',#82856,#57581,#57582) ;
#50311 = AXIS2_PLACEMENT_3D('',#82860,#57584,#57585) ;
#50312 = AXIS2_PLACEMENT_3D('',#82864,#57587,#57588) ;
#50313 = AXIS2_PLACEMENT_3D('',#82873,#57593,#57594) ;
#50314 = AXIS2_PLACEMENT_3D('',#82875,#57595,#57596) ;
#50315 = AXIS2_PLACEMENT_3D('',#82878,#57597,#57598) ;
#50316 = AXIS2_PLACEMENT_3D('',#82882,#57600,#57601) ;
#50317 = AXIS2_PLACEMENT_3D('',#82886,#57603,#57604) ;
#50318 = AXIS2_PLACEMENT_3D('',#82890,#57606,#57607) ;
#50319 = AXIS2_PLACEMENT_3D('',#82894,#57609,#57610) ;
#50320 = AXIS2_PLACEMENT_3D('',#82898,#57612,#57613) ;
#50321 = AXIS2_PLACEMENT_3D('',#82902,#57615,#57616) ;
#50322 = AXIS2_PLACEMENT_3D('',#82908,#57619,#57620) ;
#50323 = AXIS2_PLACEMENT_3D('',#82912,#57622,#57623) ;
#50324 = AXIS2_PLACEMENT_3D('',#82918,#57626,#57627) ;
#50325 = AXIS2_PLACEMENT_3D('',#82928,#57633,#57634) ;
#50326 = AXIS2_PLACEMENT_3D('',#82929,#57635,#57636) ;
#50327 = AXIS2_PLACEMENT_3D('',#82930,#57637,#57638) ;
#50328 = AXIS2_PLACEMENT_3D('',#82931,#57639,#57640) ;
#50329 = AXIS2_PLACEMENT_3D('',#82932,#57641,#57642) ;
#50330 = AXIS2_PLACEMENT_3D('',#82933,#57643,#57644) ;
#50331 = AXIS2_PLACEMENT_3D('',#82935,#57646,#57647) ;
#50332 = AXIS2_PLACEMENT_3D('',#82936,#57648,#57649) ;
#50333 = AXIS2_PLACEMENT_3D('',#82937,#57650,#57651) ;
#50334 = AXIS2_PLACEMENT_3D('',#82938,#57652,#57653) ;
#50335 = AXIS2_PLACEMENT_3D('',#82939,#57654,#57655) ;
#50336 = AXIS2_PLACEMENT_3D('',#82940,#57656,#57657) ;
#50337 = AXIS2_PLACEMENT_3D('',#82941,#57658,#57659) ;
#50338 = AXIS2_PLACEMENT_3D('',#82944,#57661,#57662) ;
#50339 = AXIS2_PLACEMENT_3D('',#82945,#57663,#57664) ;
#50340 = AXIS2_PLACEMENT_3D('',#82947,#57666,#57667) ;
#50341 = AXIS2_PLACEMENT_3D('',#82949,#57669,#57670) ;
#50342 = AXIS2_PLACEMENT_3D('',#82950,#57671,#57672) ;
#50343 = AXIS2_PLACEMENT_3D('',#82951,#57673,#57674) ;
#50344 = AXIS2_PLACEMENT_3D('',#82952,#57675,#57676) ;
#50345 = AXIS2_PLACEMENT_3D('',#82953,#57677,#57678) ;
#50346 = AXIS2_PLACEMENT_3D('',#82954,#57679,#57680) ;
#50347 = AXIS2_PLACEMENT_3D('',#82956,#57682,#57683) ;
#50348 = AXIS2_PLACEMENT_3D('',#82957,#57684,#57685) ;
#50349 = AXIS2_PLACEMENT_3D('',#83011,#57689,#57690) ;
#50350 = AXIS2_PLACEMENT_3D('',#83014,#57691,#57692) ;
#50351 = AXIS2_PLACEMENT_3D('',#83016,#57693,#57694) ;
#50352 = AXIS2_PLACEMENT_3D('',#83017,#57695,#57696) ;
#50353 = AXIS2_PLACEMENT_3D('',#83018,#57697,#57698) ;
#50354 = AXIS2_PLACEMENT_3D('',#83019,#57699,#57700) ;
#50355 = AXIS2_PLACEMENT_3D('',#83021,#57701,#57702) ;
#50356 = AXIS2_PLACEMENT_3D('',#83022,#57703,#57704) ;
#50357 = AXIS2_PLACEMENT_3D('',#83025,#57706,#57707) ;
#50358 = AXIS2_PLACEMENT_3D('',#83026,#57708,#57709) ;
#50359 = AXIS2_PLACEMENT_3D('',#83028,#57710,#57711) ;
#50360 = AXIS2_PLACEMENT_3D('',#83029,#57712,#57713) ;
#50361 = AXIS2_PLACEMENT_3D('',#83030,#57714,#57715) ;
#50362 = AXIS2_PLACEMENT_3D('',#83032,#57716,#57717) ;
#50363 = AXIS2_PLACEMENT_3D('',#83034,#57719,#57720) ;
#50364 = AXIS2_PLACEMENT_3D('',#83036,#57721,#57722) ;
#50365 = AXIS2_PLACEMENT_3D('',#83037,#57723,#57724) ;
#50366 = AXIS2_PLACEMENT_3D('',#83038,#57725,#57726) ;
#50367 = AXIS2_PLACEMENT_3D('',#83043,#57728,#57729) ;
#50368 = AXIS2_PLACEMENT_3D('',#83055,#57735,#57736) ;
#50369 = AXIS2_PLACEMENT_3D('',#83059,#57738,#57739) ;
#50370 = AXIS2_PLACEMENT_3D('',#83063,#57741,#57742) ;
#50371 = AXIS2_PLACEMENT_3D('',#83069,#57745,#57746) ;
#50372 = AXIS2_PLACEMENT_3D('',#83073,#57748,#57749) ;
#50373 = AXIS2_PLACEMENT_3D('',#83081,#57753,#57754) ;
#50374 = AXIS2_PLACEMENT_3D('',#83085,#57756,#57757) ;
#50375 = AXIS2_PLACEMENT_3D('',#83091,#57760,#57761) ;
#50376 = AXIS2_PLACEMENT_3D('',#83095,#57763,#57764) ;
#50377 = AXIS2_PLACEMENT_3D('',#83099,#57766,#57767) ;
#50378 = AXIS2_PLACEMENT_3D('',#83101,#57768,#57769) ;
#50379 = AXIS2_PLACEMENT_3D('',#83105,#57771,#57772) ;
#50380 = AXIS2_PLACEMENT_3D('',#83107,#57773,#57774) ;
#50381 = AXIS2_PLACEMENT_3D('',#83111,#57776,#57777) ;
#50382 = AXIS2_PLACEMENT_3D('',#83115,#57779,#57780) ;
#50383 = AXIS2_PLACEMENT_3D('',#83119,#57782,#57783) ;
#50384 = AXIS2_PLACEMENT_3D('',#83123,#57785,#57786) ;
#50385 = AXIS2_PLACEMENT_3D('',#83127,#57788,#57789) ;
#50386 = AXIS2_PLACEMENT_3D('',#83131,#57791,#57792) ;
#50387 = AXIS2_PLACEMENT_3D('',#83135,#57794,#57795) ;
#50388 = AXIS2_PLACEMENT_3D('',#83157,#57799,#57800) ;
#50389 = AXIS2_PLACEMENT_3D('',#83161,#57802,#57803) ;
#50390 = AXIS2_PLACEMENT_3D('',#83164,#57805,#57806) ;
#50391 = AXIS2_PLACEMENT_3D('',#83171,#57809,#57810) ;
#50392 = AXIS2_PLACEMENT_3D('',#83175,#57812,#57813) ;
#50393 = AXIS2_PLACEMENT_3D('',#83181,#57816,#57817) ;
#50394 = AXIS2_PLACEMENT_3D('',#83185,#57819,#57820) ;
#50395 = AXIS2_PLACEMENT_3D('',#83189,#57822,#57823) ;
#50396 = AXIS2_PLACEMENT_3D('',#83192,#57825,#57826) ;
#50397 = AXIS2_PLACEMENT_3D('',#83194,#57827,#57828) ;
#50398 = AXIS2_PLACEMENT_3D('',#83196,#57829,#57830) ;
#50399 = AXIS2_PLACEMENT_3D('',#83203,#57833,#57834) ;
#50400 = AXIS2_PLACEMENT_3D('',#83207,#57836,#57837) ;
#50401 = AXIS2_PLACEMENT_3D('',#83211,#57839,#57840) ;
#50402 = AXIS2_PLACEMENT_3D('',#83215,#57842,#57843) ;
#50403 = AXIS2_PLACEMENT_3D('',#83219,#57845,#57846) ;
#50404 = AXIS2_PLACEMENT_3D('',#83223,#57848,#57849) ;
#50405 = AXIS2_PLACEMENT_3D('',#83230,#57853,#57854) ;
#50406 = AXIS2_PLACEMENT_3D('',#83235,#57856,#57857) ;
#50407 = AXIS2_PLACEMENT_3D('',#83239,#57859,#57860) ;
#50408 = AXIS2_PLACEMENT_3D('',#83243,#57862,#57863) ;
#50409 = AXIS2_PLACEMENT_3D('',#83247,#57865,#57866) ;
#50410 = AXIS2_PLACEMENT_3D('',#83251,#57868,#57869) ;
#50411 = AXIS2_PLACEMENT_3D('',#83258,#57873,#57874) ;
#50412 = AXIS2_PLACEMENT_3D('',#83261,#57875,#57876) ;
#50413 = AXIS2_PLACEMENT_3D('',#83265,#57878,#57879) ;
#50414 = AXIS2_PLACEMENT_3D('',#83269,#57881,#57882) ;
#50415 = AXIS2_PLACEMENT_3D('',#83273,#57884,#57885) ;
#50416 = AXIS2_PLACEMENT_3D('',#83292,#57891,#57892) ;
#50417 = AXIS2_PLACEMENT_3D('',#83296,#57894,#57895) ;
#50418 = AXIS2_PLACEMENT_3D('',#83300,#57897,#57898) ;
#50419 = AXIS2_PLACEMENT_3D('',#83304,#57900,#57901) ;
#50420 = AXIS2_PLACEMENT_3D('',#83328,#57906,#57907) ;
#50421 = AXIS2_PLACEMENT_3D('',#83332,#57909,#57910) ;
#50422 = AXIS2_PLACEMENT_3D('',#83336,#57912,#57913) ;
#50423 = AXIS2_PLACEMENT_3D('',#83340,#57915,#57916) ;
#50424 = AXIS2_PLACEMENT_3D('',#83353,#57919,#57920) ;
#50425 = AXIS2_PLACEMENT_3D('',#83357,#57922,#57923) ;
#50426 = AXIS2_PLACEMENT_3D('',#83361,#57925,#57926) ;
#50427 = AXIS2_PLACEMENT_3D('',#83365,#57928,#57929) ;
#50428 = AXIS2_PLACEMENT_3D('',#83371,#57932,#57933) ;
#50429 = AXIS2_PLACEMENT_3D('',#83375,#57935,#57936) ;
#50430 = AXIS2_PLACEMENT_3D('',#83381,#57939,#57940) ;
#50431 = AXIS2_PLACEMENT_3D('',#83385,#57942,#57943) ;
#50432 = AXIS2_PLACEMENT_3D('',#83389,#57945,#57946) ;
#50433 = AXIS2_PLACEMENT_3D('',#83393,#57948,#57949) ;
#50434 = AXIS2_PLACEMENT_3D('',#83399,#57952,#57953) ;
#50435 = AXIS2_PLACEMENT_3D('',#83403,#57955,#57956) ;
#50436 = AXIS2_PLACEMENT_3D('',#83426,#57959,#57960) ;
#50437 = AXIS2_PLACEMENT_3D('',#83429,#57961,#57962) ;
#50438 = AXIS2_PLACEMENT_3D('',#83430,#57963,#57964) ;
#50439 = AXIS2_PLACEMENT_3D('',#83432,#57965,#57966) ;
#50440 = AXIS2_PLACEMENT_3D('',#83433,#57967,#57968) ;
#50441 = AXIS2_PLACEMENT_3D('',#83434,#57969,#57970) ;
#50442 = AXIS2_PLACEMENT_3D('',#83437,#57971,#57972) ;
#50443 = AXIS2_PLACEMENT_3D('',#83440,#57975,#57976) ;
#50444 = AXIS2_PLACEMENT_3D('',#83443,#57977,#57978) ;
#50445 = AXIS2_PLACEMENT_3D('',#83444,#57979,#57980) ;
#50446 = AXIS2_PLACEMENT_3D('',#83445,#57981,#57982) ;
#50447 = AXIS2_PLACEMENT_3D('',#83446,#57983,#57984) ;
#50448 = AXIS2_PLACEMENT_3D('',#83449,#57985,#57986) ;
#50449 = AXIS2_PLACEMENT_3D('',#83452,#57989,#57990) ;
#50450 = AXIS2_PLACEMENT_3D('',#83455,#57991,#57992) ;
#50451 = AXIS2_PLACEMENT_3D('',#83456,#57993,#57994) ;
#50452 = AXIS2_PLACEMENT_3D('',#83457,#57995,#57996) ;
#50453 = AXIS2_PLACEMENT_3D('',#83458,#57997,#57998) ;
#50454 = AXIS2_PLACEMENT_3D('',#83461,#57999,#58000) ;
#50455 = AXIS2_PLACEMENT_3D('',#83464,#58003,#58004) ;
#50456 = AXIS2_PLACEMENT_3D('',#83467,#58005,#58006) ;
#50457 = AXIS2_PLACEMENT_3D('',#83468,#58007,#58008) ;
#50458 = AXIS2_PLACEMENT_3D('',#83469,#58009,#58010) ;
#50459 = AXIS2_PLACEMENT_3D('',#83470,#58011,#58012) ;
#50460 = AXIS2_PLACEMENT_3D('',#83473,#58013,#58014) ;
#50461 = AXIS2_PLACEMENT_3D('',#83476,#58017,#58018) ;
#50462 = AXIS2_PLACEMENT_3D('',#83479,#58019,#58020) ;
#50463 = AXIS2_PLACEMENT_3D('',#83480,#58021,#58022) ;
#50464 = AXIS2_PLACEMENT_3D('',#83481,#58023,#58024) ;
#50465 = AXIS2_PLACEMENT_3D('',#83482,#58025,#58026) ;
#50466 = AXIS2_PLACEMENT_3D('',#83485,#58027,#58028) ;
#50467 = AXIS2_PLACEMENT_3D('',#83488,#58031,#58032) ;
#50468 = AXIS2_PLACEMENT_3D('',#83491,#58033,#58034) ;
#50469 = AXIS2_PLACEMENT_3D('',#83492,#58035,#58036) ;
#50470 = AXIS2_PLACEMENT_3D('',#83493,#58037,#58038) ;
#50471 = AXIS2_PLACEMENT_3D('',#83494,#58039,#58040) ;
#50472 = AXIS2_PLACEMENT_3D('',#83497,#58041,#58042) ;
#50473 = AXIS2_PLACEMENT_3D('',#83500,#58045,#58046) ;
#50474 = AXIS2_PLACEMENT_3D('',#83502,#58047,#58048) ;
#50475 = AXIS2_PLACEMENT_3D('',#83503,#58049,#58050) ;
#50476 = AXIS2_PLACEMENT_3D('',#83504,#58051,#58052) ;
#50477 = AXIS2_PLACEMENT_3D('',#83505,#58053,#58054) ;
#50478 = AXIS2_PLACEMENT_3D('',#83511,#58057,#58058) ;
#50479 = AXIS2_PLACEMENT_3D('',#83517,#58062,#58063) ;
#50480 = AXIS2_PLACEMENT_3D('',#83520,#58065,#58066) ;
#50481 = AXIS2_PLACEMENT_3D('',#83521,#58067,#58068) ;
#50482 = AXIS2_PLACEMENT_3D('',#83525,#58071,#58072) ;
#50483 = AXIS2_PLACEMENT_3D('',#83528,#58074,#58075) ;
#50484 = AXIS2_PLACEMENT_3D('',#83529,#58076,#58077) ;
#50485 = AXIS2_PLACEMENT_3D('',#83533,#58080,#58081) ;
#50486 = AXIS2_PLACEMENT_3D('',#83536,#58083,#58084) ;
#50487 = AXIS2_PLACEMENT_3D('',#83537,#58085,#58086) ;
#50488 = AXIS2_PLACEMENT_3D('',#83541,#58089,#58090) ;
#50489 = AXIS2_PLACEMENT_3D('',#83544,#58092,#58093) ;
#50490 = AXIS2_PLACEMENT_3D('',#83545,#58094,#58095) ;
#50491 = AXIS2_PLACEMENT_3D('',#83549,#58098,#58099) ;
#50492 = AXIS2_PLACEMENT_3D('',#83552,#58101,#58102) ;
#50493 = AXIS2_PLACEMENT_3D('',#83553,#58103,#58104) ;
#50494 = AXIS2_PLACEMENT_3D('',#83561,#58108,#58109) ;
#50495 = AXIS2_PLACEMENT_3D('',#83563,#58111,#58112) ;
#50496 = AXIS2_PLACEMENT_3D('',#83565,#58113,#58114) ;
#50497 = AXIS2_PLACEMENT_3D('',#83566,#58115,#58116) ;
#50498 = AXIS2_PLACEMENT_3D('',#83567,#58117,#58118) ;
#50499 = AXIS2_PLACEMENT_3D('',#83570,#58120,#58121) ;
#50500 = AXIS2_PLACEMENT_3D('',#83687,#58123,#58124) ;
#50501 = AXIS2_PLACEMENT_3D('',#83689,#58125,#58126) ;
#50502 = AXIS2_PLACEMENT_3D('',#83690,#58127,#58128) ;
#50503 = AXIS2_PLACEMENT_3D('',#83691,#58129,#58130) ;
#50504 = AXIS2_PLACEMENT_3D('',#83693,#58131,#58132) ;
#50505 = AXIS2_PLACEMENT_3D('',#83694,#58133,#58134) ;
#50506 = AXIS2_PLACEMENT_3D('',#83697,#58135,#58136) ;
#50507 = AXIS2_PLACEMENT_3D('',#83698,#58137,#58138) ;
#50508 = AXIS2_PLACEMENT_3D('',#83699,#58139,#58140) ;
#50509 = AXIS2_PLACEMENT_3D('',#83700,#58141,#58142) ;
#50510 = AXIS2_PLACEMENT_3D('',#83703,#58144,#58145) ;
#50511 = AXIS2_PLACEMENT_3D('',#83704,#58146,#58147) ;
#50512 = AXIS2_PLACEMENT_3D('',#83706,#58148,#58149) ;
#50513 = AXIS2_PLACEMENT_3D('',#83708,#58150,#58151) ;
#50514 = AXIS2_PLACEMENT_3D('',#83710,#58152,#58153) ;
#50515 = AXIS2_PLACEMENT_3D('',#83711,#58154,#58155) ;
#50516 = AXIS2_PLACEMENT_3D('',#83712,#58156,#58157) ;
#50517 = AXIS2_PLACEMENT_3D('',#83716,#58159,#58160) ;
#50518 = AXIS2_PLACEMENT_3D('',#83717,#58161,#58162) ;
#50519 = AXIS2_PLACEMENT_3D('',#83718,#58163,#58164) ;
#50520 = AXIS2_PLACEMENT_3D('',#83725,#58167,#58168) ;
#50521 = AXIS2_PLACEMENT_3D('',#83729,#58170,#58171) ;
#50522 = AXIS2_PLACEMENT_3D('',#83731,#58173,#58174) ;
#50523 = AXIS2_PLACEMENT_3D('',#83733,#58175,#58176) ;
#50524 = AXIS2_PLACEMENT_3D('',#83734,#58177,#58178) ;
#50525 = AXIS2_PLACEMENT_3D('',#83735,#58179,#58180) ;
#50526 = AXIS2_PLACEMENT_3D('',#83753,#58184,#58185) ;
#50527 = AXIS2_PLACEMENT_3D('',#83755,#58186,#58187) ;
#50528 = AXIS2_PLACEMENT_3D('',#83757,#58188,#58189) ;
#50529 = AXIS2_PLACEMENT_3D('',#83759,#58190,#58191) ;
#50530 = AXIS2_PLACEMENT_3D('',#83760,#58192,#58193) ;
#50531 = AXIS2_PLACEMENT_3D('',#83761,#58194,#58195) ;
#50532 = AXIS2_PLACEMENT_3D('',#83765,#58197,#58198) ;
#50533 = AXIS2_PLACEMENT_3D('',#83766,#58199,#58200) ;
#50534 = AXIS2_PLACEMENT_3D('',#83767,#58201,#58202) ;
#50535 = AXIS2_PLACEMENT_3D('',#83774,#58205,#58206) ;
#50536 = AXIS2_PLACEMENT_3D('',#83778,#58208,#58209) ;
#50537 = AXIS2_PLACEMENT_3D('',#83780,#58211,#58212) ;
#50538 = AXIS2_PLACEMENT_3D('',#83782,#58213,#58214) ;
#50539 = AXIS2_PLACEMENT_3D('',#83783,#58215,#58216) ;
#50540 = AXIS2_PLACEMENT_3D('',#83784,#58217,#58218) ;
#50541 = AXIS2_PLACEMENT_3D('',#83802,#58222,#58223) ;
#50542 = AXIS2_PLACEMENT_3D('',#83804,#58224,#58225) ;
#50543 = AXIS2_PLACEMENT_3D('',#83806,#58226,#58227) ;
#50544 = AXIS2_PLACEMENT_3D('',#83807,#58228,#58229) ;
#50545 = AXIS2_PLACEMENT_3D('',#83808,#58230,#58231) ;
#50546 = AXIS2_PLACEMENT_3D('',#83810,#58232,#58233) ;
#50547 = AXIS2_PLACEMENT_3D('',#83812,#58235,#58236) ;
#50548 = AXIS2_PLACEMENT_3D('',#83814,#58237,#58238) ;
#50549 = AXIS2_PLACEMENT_3D('',#83815,#58239,#58240) ;
#50550 = AXIS2_PLACEMENT_3D('',#83816,#58241,#58242) ;
#50551 = AXIS2_PLACEMENT_3D('',#83818,#58243,#58244) ;
#50552 = AXIS2_PLACEMENT_3D('',#83820,#58246,#58247) ;
#50553 = AXIS2_PLACEMENT_3D('',#83822,#58248,#58249) ;
#50554 = AXIS2_PLACEMENT_3D('',#83823,#58250,#58251) ;
#50555 = AXIS2_PLACEMENT_3D('',#83824,#58252,#58253) ;
#50556 = AXIS2_PLACEMENT_3D('',#83828,#58255,#58256) ;
#50557 = AXIS2_PLACEMENT_3D('',#83890,#58266,#58267) ;
#50558 = AXIS2_PLACEMENT_3D('',#83892,#58269,#58270) ;
#50559 = AXIS2_PLACEMENT_3D('',#83893,#58271,#58272) ;
#50560 = AXIS2_PLACEMENT_3D('',#83894,#58273,#58274) ;
#50561 = AXIS2_PLACEMENT_3D('',#83898,#58276,#58277) ;
#50562 = AXIS2_PLACEMENT_3D('',#83937,#58278,#58279) ;
#50563 = AXIS2_PLACEMENT_3D('',#83942,#58282,#58283) ;
#50564 = AXIS2_PLACEMENT_3D('',#83981,#58284,#58285) ;
#50565 = AXIS2_PLACEMENT_3D('',#83985,#58287,#58288) ;
#50566 = AXIS2_PLACEMENT_3D('',#84000,#58291,#58292) ;
#50567 = AXIS2_PLACEMENT_3D('',#84001,#58293,#58294) ;
#50568 = AXIS2_PLACEMENT_3D('',#84002,#58295,#58296) ;
#50569 = AXIS2_PLACEMENT_3D('',#84016,#58297,#58298) ;
#50570 = AXIS2_PLACEMENT_3D('',#84038,#58299,#58300) ;
#50571 = AXIS2_PLACEMENT_3D('',#84039,#58301,#58302) ;
#50572 = AXIS2_PLACEMENT_3D('',#84061,#58303,#58304) ;
#50573 = AXIS2_PLACEMENT_3D('',#84081,#58305,#58306) ;
#50574 = AXIS2_PLACEMENT_3D('',#84083,#58307,#58308) ;
#50575 = AXIS2_PLACEMENT_3D('',#84110,#58310,#58311) ;
#50576 = AXIS2_PLACEMENT_3D('',#84116,#58312,#58313) ;
#50577 = AXIS2_PLACEMENT_3D('',#84117,#58314,#58315) ;
#50578 = AXIS2_PLACEMENT_3D('',#84118,#58316,#58317) ;
#50579 = AXIS2_PLACEMENT_3D('',#84119,#58318,#58319) ;
#50580 = AXIS2_PLACEMENT_3D('',#84121,#58320,#58321) ;
#50581 = AXIS2_PLACEMENT_3D('',#84123,#58322,#58323) ;
#50582 = AXIS2_PLACEMENT_3D('',#84124,#58324,#58325) ;
#50583 = AXIS2_PLACEMENT_3D('',#84125,#58326,#58327) ;
#50584 = AXIS2_PLACEMENT_3D('',#84127,#58328,#58329) ;
#50585 = AXIS2_PLACEMENT_3D('',#84129,#58331,#58332) ;
#50586 = AXIS2_PLACEMENT_3D('',#84131,#58333,#58334) ;
#50587 = AXIS2_PLACEMENT_3D('',#84132,#58335,#58336) ;
#50588 = AXIS2_PLACEMENT_3D('',#84133,#58337,#58338) ;
#50589 = AXIS2_PLACEMENT_3D('',#84135,#58339,#58340) ;
#50590 = AXIS2_PLACEMENT_3D('',#84137,#58342,#58343) ;
#50591 = AXIS2_PLACEMENT_3D('',#84150,#58344,#58345) ;
#50592 = AXIS2_PLACEMENT_3D('',#84156,#58346,#58347) ;
#50593 = AXIS2_PLACEMENT_3D('',#84158,#58348,#58349) ;
#50594 = AXIS2_PLACEMENT_3D('',#84160,#58350,#58351) ;
#50595 = AXIS2_PLACEMENT_3D('',#84161,#58352,#58353) ;
#50596 = AXIS2_PLACEMENT_3D('',#84162,#58354,#58355) ;
#50597 = AXIS2_PLACEMENT_3D('',#84164,#58356,#58357) ;
#50598 = AXIS2_PLACEMENT_3D('',#84166,#58359,#58360) ;
#50599 = AXIS2_PLACEMENT_3D('',#84168,#58361,#58362) ;
#50600 = AXIS2_PLACEMENT_3D('',#84169,#58363,#58364) ;
#50601 = AXIS2_PLACEMENT_3D('',#84170,#58365,#58366) ;
#50602 = AXIS2_PLACEMENT_3D('',#84173,#58367,#58368) ;
#50603 = AXIS2_PLACEMENT_3D('',#84174,#58369,#58370) ;
#50604 = AXIS2_PLACEMENT_3D('',#84175,#58371,#58372) ;
#50605 = AXIS2_PLACEMENT_3D('',#84176,#58373,#58374) ;
#50606 = AXIS2_PLACEMENT_3D('',#84179,#58377,#58378) ;
#50607 = AXIS2_PLACEMENT_3D('',#84181,#58379,#58380) ;
#50608 = AXIS2_PLACEMENT_3D('',#84183,#58381,#58382) ;
#50609 = AXIS2_PLACEMENT_3D('',#84184,#58383,#58384) ;
#50610 = AXIS2_PLACEMENT_3D('',#84185,#58385,#58386) ;
#50611 = AXIS2_PLACEMENT_3D('',#84188,#58387,#58388) ;
#50612 = AXIS2_PLACEMENT_3D('',#84189,#58389,#58390) ;
#50613 = AXIS2_PLACEMENT_3D('',#84190,#58391,#58392) ;
#50614 = AXIS2_PLACEMENT_3D('',#84191,#58393,#58394) ;
#50615 = AXIS2_PLACEMENT_3D('',#84193,#58396,#58397) ;
#50616 = AXIS2_PLACEMENT_3D('',#84195,#58399,#58400) ;
#50617 = AXIS2_PLACEMENT_3D('',#84198,#58401,#58402) ;
#50618 = AXIS2_PLACEMENT_3D('',#84199,#58403,#58404) ;
#50619 = AXIS2_PLACEMENT_3D('',#84200,#58405,#58406) ;
#50620 = AXIS2_PLACEMENT_3D('',#84201,#58407,#58408) ;
#50621 = AXIS2_PLACEMENT_3D('',#84204,#58411,#58412) ;
#50622 = AXIS2_PLACEMENT_3D('',#84207,#58413,#58414) ;
#50623 = AXIS2_PLACEMENT_3D('',#84210,#58417,#58418) ;
#50624 = AXIS2_PLACEMENT_3D('',#84211,#58419,#58420) ;
#50625 = AXIS2_PLACEMENT_3D('',#84212,#58421,#58422) ;
#50626 = AXIS2_PLACEMENT_3D('',#84213,#58423,#58424) ;
#50627 = AXIS2_PLACEMENT_3D('',#84215,#58425,#58426) ;
#50628 = AXIS2_PLACEMENT_3D('',#84217,#58428,#58429) ;
#50629 = AXIS2_PLACEMENT_3D('',#84219,#58430,#58431) ;
#50630 = AXIS2_PLACEMENT_3D('',#84220,#58432,#58433) ;
#50631 = AXIS2_PLACEMENT_3D('',#84221,#58434,#58435) ;
#50632 = AXIS2_PLACEMENT_3D('',#84224,#58437,#58438) ;
#50633 = AXIS2_PLACEMENT_3D('',#84225,#58439,#58440) ;
#50634 = AXIS2_PLACEMENT_3D('',#84227,#58442,#58443) ;
#50635 = AXIS2_PLACEMENT_3D('',#84230,#58445,#58446) ;
#50636 = AXIS2_PLACEMENT_3D('',#84231,#58447,#58448) ;
#50637 = AXIS2_PLACEMENT_3D('',#84235,#58450,#58451) ;
#50638 = AXIS2_PLACEMENT_3D('',#84237,#58453,#58454) ;
#50639 = AXIS2_PLACEMENT_3D('',#84239,#58456,#58457) ;
#50640 = AXIS2_PLACEMENT_3D('',#84242,#58458,#58459) ;
#50641 = AXIS2_PLACEMENT_3D('',#84243,#58460,#58461) ;
#50642 = AXIS2_PLACEMENT_3D('',#84244,#58462,#58463) ;
#50643 = AXIS2_PLACEMENT_3D('',#84245,#58464,#58465) ;
#50644 = AXIS2_PLACEMENT_3D('',#84248,#58466,#58467) ;
#50645 = AXIS2_PLACEMENT_3D('',#84271,#58470,#58471) ;
#50646 = AXIS2_PLACEMENT_3D('',#84272,#58472,#58473) ;
#50647 = AXIS2_PLACEMENT_3D('',#84273,#58474,#58475) ;
#50648 = AXIS2_PLACEMENT_3D('',#84276,#58477,#58478) ;
#50649 = AXIS2_PLACEMENT_3D('',#84277,#58479,#58480) ;
#50650 = AXIS2_PLACEMENT_3D('',#84301,#58482,#58483) ;
#50651 = AXIS2_PLACEMENT_3D('',#84302,#58484,#58485) ;
#50652 = AXIS2_PLACEMENT_3D('',#84303,#58486,#58487) ;
#50653 = AXIS2_PLACEMENT_3D('',#84304,#58488,#58489) ;
#50654 = AXIS2_PLACEMENT_3D('',#84307,#58490,#58491) ;
#50655 = AXIS2_PLACEMENT_3D('',#84310,#58494,#58495) ;
#50656 = AXIS2_PLACEMENT_3D('',#84311,#58496,#58497) ;
#50657 = AXIS2_PLACEMENT_3D('',#84312,#58498,#58499) ;
#50658 = AXIS2_PLACEMENT_3D('',#84313,#58500,#58501) ;
#50659 = AXIS2_PLACEMENT_3D('',#84317,#58504,#58505) ;
#50660 = AXIS2_PLACEMENT_3D('',#84318,#58506,#58507) ;
#50661 = AXIS2_PLACEMENT_3D('',#84319,#58508,#58509) ;
#50662 = AXIS2_PLACEMENT_3D('',#84321,#58510,#58511) ;
#50663 = AXIS2_PLACEMENT_3D('',#84323,#58512,#58513) ;
#50664 = AXIS2_PLACEMENT_3D('',#84325,#58515,#58516) ;
#50665 = AXIS2_PLACEMENT_3D('',#84327,#58517,#58518) ;
#50666 = AXIS2_PLACEMENT_3D('',#84328,#58519,#58520) ;
#50667 = AXIS2_PLACEMENT_3D('',#84329,#58521,#58522) ;
#50668 = AXIS2_PLACEMENT_3D('',#84331,#58523,#58524) ;
#50669 = AXIS2_PLACEMENT_3D('',#84333,#58526,#58527) ;
#50670 = AXIS2_PLACEMENT_3D('',#84335,#58528,#58529) ;
#50671 = AXIS2_PLACEMENT_3D('',#84336,#58530,#58531) ;
#50672 = AXIS2_PLACEMENT_3D('',#84337,#58532,#58533) ;
#50673 = AXIS2_PLACEMENT_3D('',#84339,#58534,#58535) ;
#50674 = AXIS2_PLACEMENT_3D('',#84341,#58537,#58538) ;
#50675 = AXIS2_PLACEMENT_3D('',#84342,#58539,#58540) ;
#50676 = AXIS2_PLACEMENT_3D('',#84343,#58541,#58542) ;
#50677 = AXIS2_PLACEMENT_3D('',#84345,#58543,#58544) ;
#50678 = AXIS2_PLACEMENT_3D('',#84347,#58546,#58547) ;
#50679 = AXIS2_PLACEMENT_3D('',#84353,#58551,#58552) ;
#50680 = AXIS2_PLACEMENT_3D('',#84356,#58554,#58555) ;
#50681 = AXIS2_PLACEMENT_3D('',#84357,#58556,#58557) ;
#50682 = AXIS2_PLACEMENT_3D('',#84361,#58560,#58561) ;
#50683 = AXIS2_PLACEMENT_3D('',#84364,#58563,#58564) ;
#50684 = AXIS2_PLACEMENT_3D('',#84365,#58565,#58566) ;
#50685 = AXIS2_PLACEMENT_3D('',#84369,#58569,#58570) ;
#50686 = AXIS2_PLACEMENT_3D('',#84372,#58572,#58573) ;
#50687 = AXIS2_PLACEMENT_3D('',#84373,#58574,#58575) ;
#50688 = AXIS2_PLACEMENT_3D('',#84377,#58578,#58579) ;
#50689 = AXIS2_PLACEMENT_3D('',#84380,#58581,#58582) ;
#50690 = AXIS2_PLACEMENT_3D('',#84381,#58583,#58584) ;
#50691 = AXIS2_PLACEMENT_3D('',#84385,#58587,#58588) ;
#50692 = AXIS2_PLACEMENT_3D('',#84388,#58590,#58591) ;
#50693 = AXIS2_PLACEMENT_3D('',#84389,#58592,#58593) ;
#50694 = AXIS2_PLACEMENT_3D('',#84393,#58596,#58597) ;
#50695 = AXIS2_PLACEMENT_3D('',#84395,#58598,#58599) ;
#50696 = AXIS2_PLACEMENT_3D('',#84398,#58601,#58602) ;
#50697 = AXIS2_PLACEMENT_3D('',#84399,#58603,#58604) ;
#50698 = AXIS2_PLACEMENT_3D('',#84401,#58605,#58606) ;
#50699 = AXIS2_PLACEMENT_3D('',#84402,#58607,#58608) ;
#50700 = AXIS2_PLACEMENT_3D('',#84403,#58609,#58610) ;
#50701 = AXIS2_PLACEMENT_3D('',#84405,#58611,#58612) ;
#50702 = AXIS2_PLACEMENT_3D('',#84407,#58614,#58615) ;
#50703 = AXIS2_PLACEMENT_3D('',#84409,#58616,#58617) ;
#50704 = AXIS2_PLACEMENT_3D('',#84410,#58618,#58619) ;
#50705 = AXIS2_PLACEMENT_3D('',#84411,#58620,#58621) ;
#50706 = AXIS2_PLACEMENT_3D('',#84413,#58622,#58623) ;
#50707 = AXIS2_PLACEMENT_3D('',#84415,#58625,#58626) ;
#50708 = AXIS2_PLACEMENT_3D('',#84417,#58627,#58628) ;
#50709 = AXIS2_PLACEMENT_3D('',#84418,#58629,#58630) ;
#50710 = AXIS2_PLACEMENT_3D('',#84419,#58631,#58632) ;
#50711 = AXIS2_PLACEMENT_3D('',#84421,#58633,#58634) ;
#50712 = AXIS2_PLACEMENT_3D('',#84423,#58636,#58637) ;
#50713 = AXIS2_PLACEMENT_3D('',#84425,#58638,#58639) ;
#50714 = AXIS2_PLACEMENT_3D('',#84426,#58640,#58641) ;
#50715 = AXIS2_PLACEMENT_3D('',#84427,#58642,#58643) ;
#50716 = AXIS2_PLACEMENT_3D('',#84429,#58644,#58645) ;
#50717 = AXIS2_PLACEMENT_3D('',#84431,#58647,#58648) ;
#50718 = AXIS2_PLACEMENT_3D('',#84433,#58649,#58650) ;
#50719 = AXIS2_PLACEMENT_3D('',#84436,#58652,#58653) ;
#50720 = AXIS2_PLACEMENT_3D('',#84437,#58654,#58655) ;
#50721 = AXIS2_PLACEMENT_3D('',#84439,#58656,#58657) ;
#50722 = AXIS2_PLACEMENT_3D('',#84440,#58658,#58659) ;
#50723 = AXIS2_PLACEMENT_3D('',#84441,#58660,#58661) ;
#50724 = AXIS2_PLACEMENT_3D('',#84443,#58662,#58663) ;
#50725 = AXIS2_PLACEMENT_3D('',#84445,#58665,#58666) ;
#50726 = AXIS2_PLACEMENT_3D('',#84447,#58667,#58668) ;
#50727 = AXIS2_PLACEMENT_3D('',#84448,#58669,#58670) ;
#50728 = AXIS2_PLACEMENT_3D('',#84449,#58671,#58672) ;
#50729 = AXIS2_PLACEMENT_3D('',#84451,#58673,#58674) ;
#50730 = AXIS2_PLACEMENT_3D('',#84453,#58676,#58677) ;
#50731 = AXIS2_PLACEMENT_3D('',#84454,#58678,#58679) ;
#50732 = AXIS2_PLACEMENT_3D('',#84455,#58680,#58681) ;
#50733 = AXIS2_PLACEMENT_3D('',#84456,#58682,#58683) ;
#50734 = AXIS2_PLACEMENT_3D('',#84457,#58684,#58685) ;
#50735 = AXIS2_PLACEMENT_3D('',#84461,#58687,#58688) ;
#50736 = AXIS2_PLACEMENT_3D('',#84463,#58690,#58691) ;
#50737 = AXIS2_PLACEMENT_3D('',#84467,#58694,#58695) ;
#50738 = AXIS2_PLACEMENT_3D('',#84470,#58697,#58698) ;
#50739 = AXIS2_PLACEMENT_3D('',#84471,#58699,#58700) ;
#50740 = AXIS2_PLACEMENT_3D('',#84475,#58703,#58704) ;
#50741 = AXIS2_PLACEMENT_3D('',#84478,#58706,#58707) ;
#50742 = AXIS2_PLACEMENT_3D('',#84479,#58708,#58709) ;
#50743 = AXIS2_PLACEMENT_3D('',#84483,#58712,#58713) ;
#50744 = AXIS2_PLACEMENT_3D('',#84486,#58715,#58716) ;
#50745 = AXIS2_PLACEMENT_3D('',#84487,#58717,#58718) ;
#50746 = AXIS2_PLACEMENT_3D('',#84491,#58721,#58722) ;
#50747 = AXIS2_PLACEMENT_3D('',#84493,#58723,#58724) ;
#50748 = AXIS2_PLACEMENT_3D('',#84495,#58725,#58726) ;
#50749 = AXIS2_PLACEMENT_3D('',#84496,#58727,#58728) ;
#50750 = AXIS2_PLACEMENT_3D('',#84497,#58729,#58730) ;
#50751 = AXIS2_PLACEMENT_3D('',#84500,#58731,#58732) ;
#50752 = AXIS2_PLACEMENT_3D('',#84501,#58733,#58734) ;
#50753 = AXIS2_PLACEMENT_3D('',#84502,#58735,#58736) ;
#50754 = AXIS2_PLACEMENT_3D('',#84503,#58737,#58738) ;
#50755 = AXIS2_PLACEMENT_3D('',#84505,#58739,#58740) ;
#50756 = AXIS2_PLACEMENT_3D('',#84507,#58742,#58743) ;
#50757 = AXIS2_PLACEMENT_3D('',#84509,#58744,#58745) ;
#50758 = AXIS2_PLACEMENT_3D('',#84510,#58746,#58747) ;
#50759 = AXIS2_PLACEMENT_3D('',#84511,#58748,#58749) ;
#50760 = AXIS2_PLACEMENT_3D('',#84513,#58750,#58751) ;
#50761 = AXIS2_PLACEMENT_3D('',#84515,#58753,#58754) ;
#50762 = AXIS2_PLACEMENT_3D('',#84517,#58755,#58756) ;
#50763 = AXIS2_PLACEMENT_3D('',#84518,#58757,#58758) ;
#50764 = AXIS2_PLACEMENT_3D('',#84519,#58759,#58760) ;
#50765 = AXIS2_PLACEMENT_3D('',#84521,#58761,#58762) ;
#50766 = AXIS2_PLACEMENT_3D('',#84523,#58764,#58765) ;
#50767 = AXIS2_PLACEMENT_3D('',#84525,#58766,#58767) ;
#50768 = AXIS2_PLACEMENT_3D('',#84526,#58768,#58769) ;
#50769 = AXIS2_PLACEMENT_3D('',#84527,#58770,#58771) ;
#50770 = AXIS2_PLACEMENT_3D('',#84529,#58772,#58773) ;
#50771 = AXIS2_PLACEMENT_3D('',#84531,#58775,#58776) ;
#50772 = AXIS2_PLACEMENT_3D('',#84533,#58777,#58778) ;
#50773 = AXIS2_PLACEMENT_3D('',#84534,#58779,#58780) ;
#50774 = AXIS2_PLACEMENT_3D('',#84535,#58781,#58782) ;
#50775 = AXIS2_PLACEMENT_3D('',#84537,#58784,#58785) ;
#50776 = AXIS2_PLACEMENT_3D('',#84539,#58786,#58787) ;
#50777 = AXIS2_PLACEMENT_3D('',#84541,#58789,#58790) ;
#50778 = AXIS2_PLACEMENT_3D('',#84544,#58791,#58792) ;
#50779 = AXIS2_PLACEMENT_3D('',#84567,#58795,#58796) ;
#50780 = AXIS2_PLACEMENT_3D('',#84568,#58797,#58798) ;
#50781 = AXIS2_PLACEMENT_3D('',#84569,#58799,#58800) ;
#50782 = AXIS2_PLACEMENT_3D('',#84572,#58801,#58802) ;
#50783 = AXIS2_PLACEMENT_3D('',#84595,#58805,#58806) ;
#50784 = AXIS2_PLACEMENT_3D('',#84596,#58807,#58808) ;
#50785 = AXIS2_PLACEMENT_3D('',#84597,#58809,#58810) ;
#50786 = AXIS2_PLACEMENT_3D('',#84599,#58811,#58812) ;
#50787 = AXIS2_PLACEMENT_3D('',#84601,#58814,#58815) ;
#50788 = AXIS2_PLACEMENT_3D('',#84605,#58818,#58819) ;
#50789 = AXIS2_PLACEMENT_3D('',#84607,#58820,#58821) ;
#50790 = AXIS2_PLACEMENT_3D('',#84609,#58822,#58823) ;
#50791 = AXIS2_PLACEMENT_3D('',#84610,#58824,#58825) ;
#50792 = AXIS2_PLACEMENT_3D('',#84611,#58826,#58827) ;
#50793 = AXIS2_PLACEMENT_3D('',#84613,#58828,#58829) ;
#50794 = AXIS2_PLACEMENT_3D('',#84615,#58831,#58832) ;
#50795 = AXIS2_PLACEMENT_3D('',#84617,#58833,#58834) ;
#50796 = AXIS2_PLACEMENT_3D('',#84620,#58836,#58837) ;
#50797 = AXIS2_PLACEMENT_3D('',#84621,#58838,#58839) ;
#50798 = AXIS2_PLACEMENT_3D('',#84623,#58840,#58841) ;
#50799 = AXIS2_PLACEMENT_3D('',#84624,#58842,#58843) ;
#50800 = AXIS2_PLACEMENT_3D('',#84625,#58844,#58845) ;
#50801 = AXIS2_PLACEMENT_3D('',#84627,#58846,#58847) ;
#50802 = AXIS2_PLACEMENT_3D('',#84629,#58849,#58850) ;
#50803 = AXIS2_PLACEMENT_3D('',#84631,#58851,#58852) ;
#50804 = AXIS2_PLACEMENT_3D('',#84632,#58853,#58854) ;
#50805 = AXIS2_PLACEMENT_3D('',#84633,#58855,#58856) ;
#50806 = AXIS2_PLACEMENT_3D('',#84635,#58857,#58858) ;
#50807 = AXIS2_PLACEMENT_3D('',#84637,#58860,#58861) ;
#50808 = AXIS2_PLACEMENT_3D('',#84638,#58862,#58863) ;
#50809 = AXIS2_PLACEMENT_3D('',#84639,#58864,#58865) ;
#50810 = AXIS2_PLACEMENT_3D('',#84641,#58866,#58867) ;
#50811 = AXIS2_PLACEMENT_3D('',#84644,#58869,#58870) ;
#50812 = AXIS2_PLACEMENT_3D('',#84645,#58871,#58872) ;
#50813 = AXIS2_PLACEMENT_3D('',#84647,#58873,#58874) ;
#50814 = AXIS2_PLACEMENT_3D('',#84648,#58875,#58876) ;
#50815 = AXIS2_PLACEMENT_3D('',#84649,#58877,#58878) ;
#50816 = AXIS2_PLACEMENT_3D('',#84650,#58879,#58880) ;
#50817 = AXIS2_PLACEMENT_3D('',#84651,#58881,#58882) ;
#50818 = AXIS2_PLACEMENT_3D('',#84657,#58886,#58887) ;
#50819 = AXIS2_PLACEMENT_3D('',#84660,#58889,#58890) ;
#50820 = AXIS2_PLACEMENT_3D('',#84661,#58891,#58892) ;
#50821 = AXIS2_PLACEMENT_3D('',#84665,#58895,#58896) ;
#50822 = AXIS2_PLACEMENT_3D('',#84668,#58898,#58899) ;
#50823 = AXIS2_PLACEMENT_3D('',#84669,#58900,#58901) ;
#50824 = AXIS2_PLACEMENT_3D('',#84673,#58904,#58905) ;
#50825 = AXIS2_PLACEMENT_3D('',#84676,#58907,#58908) ;
#50826 = AXIS2_PLACEMENT_3D('',#84677,#58909,#58910) ;
#50827 = AXIS2_PLACEMENT_3D('',#84681,#58913,#58914) ;
#50828 = AXIS2_PLACEMENT_3D('',#84684,#58916,#58917) ;
#50829 = AXIS2_PLACEMENT_3D('',#84685,#58918,#58919) ;
#50830 = AXIS2_PLACEMENT_3D('',#84689,#58922,#58923) ;
#50831 = AXIS2_PLACEMENT_3D('',#84691,#58924,#58925) ;
#50832 = AXIS2_PLACEMENT_3D('',#84693,#58926,#58927) ;
#50833 = AXIS2_PLACEMENT_3D('',#84694,#58928,#58929) ;
#50834 = AXIS2_PLACEMENT_3D('',#84695,#58930,#58931) ;
#50835 = AXIS2_PLACEMENT_3D('',#84697,#58932,#58933) ;
#50836 = AXIS2_PLACEMENT_3D('',#84699,#58935,#58936) ;
#50837 = AXIS2_PLACEMENT_3D('',#84701,#58937,#58938) ;
#50838 = AXIS2_PLACEMENT_3D('',#84704,#58940,#58941) ;
#50839 = AXIS2_PLACEMENT_3D('',#84705,#58942,#58943) ;
#50840 = AXIS2_PLACEMENT_3D('',#84707,#58944,#58945) ;
#50841 = AXIS2_PLACEMENT_3D('',#84708,#58946,#58947) ;
#50842 = AXIS2_PLACEMENT_3D('',#84709,#58948,#58949) ;
#50843 = AXIS2_PLACEMENT_3D('',#84711,#58950,#58951) ;
#50844 = AXIS2_PLACEMENT_3D('',#84713,#58953,#58954) ;
#50845 = AXIS2_PLACEMENT_3D('',#84715,#58955,#58956) ;
#50846 = AXIS2_PLACEMENT_3D('',#84716,#58957,#58958) ;
#50847 = AXIS2_PLACEMENT_3D('',#84717,#58959,#58960) ;
#50848 = AXIS2_PLACEMENT_3D('',#84719,#58961,#58962) ;
#50849 = AXIS2_PLACEMENT_3D('',#84721,#58964,#58965) ;
#50850 = AXIS2_PLACEMENT_3D('',#84722,#58966,#58967) ;
#50851 = AXIS2_PLACEMENT_3D('',#84723,#58968,#58969) ;
#50852 = AXIS2_PLACEMENT_3D('',#84725,#58970,#58971) ;
#50853 = AXIS2_PLACEMENT_3D('',#84728,#58973,#58974) ;
#50854 = AXIS2_PLACEMENT_3D('',#84729,#58975,#58976) ;
#50855 = AXIS2_PLACEMENT_3D('',#84731,#58977,#58978) ;
#50856 = AXIS2_PLACEMENT_3D('',#84732,#58979,#58980) ;
#50857 = AXIS2_PLACEMENT_3D('',#84733,#58981,#58982) ;
#50858 = AXIS2_PLACEMENT_3D('',#84734,#58983,#58984) ;
#50859 = AXIS2_PLACEMENT_3D('',#84735,#58985,#58986) ;
#50860 = AXIS2_PLACEMENT_3D('',#84741,#58990,#58991) ;
#50861 = AXIS2_PLACEMENT_3D('',#84744,#58993,#58994) ;
#50862 = AXIS2_PLACEMENT_3D('',#84745,#58995,#58996) ;
#50863 = AXIS2_PLACEMENT_3D('',#84749,#58999,#59000) ;
#50864 = AXIS2_PLACEMENT_3D('',#84752,#59002,#59003) ;
#50865 = AXIS2_PLACEMENT_3D('',#84753,#59004,#59005) ;
#50866 = AXIS2_PLACEMENT_3D('',#84757,#59008,#59009) ;
#50867 = AXIS2_PLACEMENT_3D('',#84760,#59011,#59012) ;
#50868 = AXIS2_PLACEMENT_3D('',#84761,#59013,#59014) ;
#50869 = AXIS2_PLACEMENT_3D('',#84765,#59017,#59018) ;
#50870 = AXIS2_PLACEMENT_3D('',#84768,#59020,#59021) ;
#50871 = AXIS2_PLACEMENT_3D('',#84769,#59022,#59023) ;
#50872 = AXIS2_PLACEMENT_3D('',#84773,#59026,#59027) ;
#50873 = AXIS2_PLACEMENT_3D('',#84774,#59028,#59029) ;
#50874 = AXIS2_PLACEMENT_3D('',#84775,#59030,#59031) ;
#50875 = AXIS2_PLACEMENT_3D('',#84777,#59032,#59033) ;
#50876 = AXIS2_PLACEMENT_3D('',#84779,#59035,#59036) ;
#50877 = AXIS2_PLACEMENT_3D('',#84780,#59037,#59038) ;
#50878 = AXIS2_PLACEMENT_3D('',#84782,#59039,#59040) ;
#50879 = AXIS2_PLACEMENT_3D('',#84783,#59041,#59042) ;
#50880 = AXIS2_PLACEMENT_3D('',#84784,#59043,#59044) ;
#50881 = AXIS2_PLACEMENT_3D('',#84785,#59045,#59046) ;
#50882 = AXIS2_PLACEMENT_3D('',#84787,#59048,#59049) ;
#50883 = AXIS2_PLACEMENT_3D('',#84789,#59051,#59052) ;
#50884 = AXIS2_PLACEMENT_3D('',#84791,#59053,#59054) ;
#50885 = AXIS2_PLACEMENT_3D('',#84792,#59055,#59056) ;
#50886 = AXIS2_PLACEMENT_3D('',#84793,#59057,#59058) ;
#50887 = AXIS2_PLACEMENT_3D('',#84794,#59059,#59060) ;
#50888 = AXIS2_PLACEMENT_3D('',#84797,#59062,#59063) ;
#50889 = AXIS2_PLACEMENT_3D('',#84798,#59064,#59065) ;
#50890 = AXIS2_PLACEMENT_3D('',#84800,#59066,#59067) ;
#50891 = AXIS2_PLACEMENT_3D('',#84801,#59068,#59069) ;
#50892 = AXIS2_PLACEMENT_3D('',#84802,#59070,#59071) ;
#50893 = AXIS2_PLACEMENT_3D('',#84804,#59072,#59073) ;
#50894 = AXIS2_PLACEMENT_3D('',#84806,#59075,#59076) ;
#50895 = AXIS2_PLACEMENT_3D('',#84808,#59077,#59078) ;
#50896 = AXIS2_PLACEMENT_3D('',#84809,#59079,#59080) ;
#50897 = AXIS2_PLACEMENT_3D('',#84810,#59081,#59082) ;
#50898 = AXIS2_PLACEMENT_3D('',#84812,#59083,#59084) ;
#50899 = AXIS2_PLACEMENT_3D('',#84814,#59086,#59087) ;
#50900 = AXIS2_PLACEMENT_3D('',#84816,#59088,#59089) ;
#50901 = AXIS2_PLACEMENT_3D('',#84817,#59090,#59091) ;
#50902 = AXIS2_PLACEMENT_3D('',#84818,#59092,#59093) ;
#50903 = AXIS2_PLACEMENT_3D('',#84820,#59094,#59095) ;
#50904 = AXIS2_PLACEMENT_3D('',#84822,#59097,#59098) ;
#50905 = AXIS2_PLACEMENT_3D('',#84824,#59099,#59100) ;
#50906 = AXIS2_PLACEMENT_3D('',#84825,#59101,#59102) ;
#50907 = AXIS2_PLACEMENT_3D('',#84826,#59103,#59104) ;
#50908 = AXIS2_PLACEMENT_3D('',#84828,#59106,#59107) ;
#50909 = AXIS2_PLACEMENT_3D('',#84832,#59110,#59111) ;
#50910 = AXIS2_PLACEMENT_3D('',#84835,#59113,#59114) ;
#50911 = AXIS2_PLACEMENT_3D('',#84836,#59115,#59116) ;
#50912 = AXIS2_PLACEMENT_3D('',#84840,#59119,#59120) ;
#50913 = AXIS2_PLACEMENT_3D('',#84843,#59122,#59123) ;
#50914 = AXIS2_PLACEMENT_3D('',#84844,#59124,#59125) ;
#50915 = AXIS2_PLACEMENT_3D('',#84848,#59128,#59129) ;
#50916 = AXIS2_PLACEMENT_3D('',#84851,#59131,#59132) ;
#50917 = AXIS2_PLACEMENT_3D('',#84852,#59133,#59134) ;
#50918 = AXIS2_PLACEMENT_3D('',#84856,#59137,#59138) ;
#50919 = AXIS2_PLACEMENT_3D('',#84859,#59140,#59141) ;
#50920 = AXIS2_PLACEMENT_3D('',#84860,#59142,#59143) ;
#50921 = AXIS2_PLACEMENT_3D('',#84862,#59145,#59146) ;
#50922 = AXIS2_PLACEMENT_3D('',#84864,#59148,#59149) ;
#50923 = AXIS2_PLACEMENT_3D('',#84866,#59150,#59151) ;
#50924 = AXIS2_PLACEMENT_3D('',#84868,#59152,#59153) ;
#50925 = AXIS2_PLACEMENT_3D('',#84869,#59154,#59155) ;
#50926 = AXIS2_PLACEMENT_3D('',#84870,#59156,#59157) ;
#50927 = AXIS2_PLACEMENT_3D('',#84878,#59162,#59163) ;
#50928 = AXIS2_PLACEMENT_3D('',#84880,#59164,#59165) ;
#50929 = AXIS2_PLACEMENT_3D('',#84881,#59166,#59167) ;
#50930 = AXIS2_PLACEMENT_3D('',#84882,#59168,#59169) ;
#50931 = AXIS2_PLACEMENT_3D('',#84884,#59171,#59172) ;
#50932 = AXIS2_PLACEMENT_3D('',#84885,#59173,#59174) ;
#50933 = AXIS2_PLACEMENT_3D('',#84887,#59175,#59176) ;
#50934 = AXIS2_PLACEMENT_3D('',#84888,#59177,#59178) ;
#50935 = AXIS2_PLACEMENT_3D('',#84889,#59179,#59180) ;
#50936 = AXIS2_PLACEMENT_3D('',#84891,#59181,#59182) ;
#50937 = AXIS2_PLACEMENT_3D('',#84892,#59183,#59184) ;
#50938 = AXIS2_PLACEMENT_3D('',#84893,#59185,#59186) ;
#50939 = AXIS2_PLACEMENT_3D('',#84894,#59187,#59188) ;
#50940 = AXIS2_PLACEMENT_3D('',#84896,#59190,#59191) ;
#50941 = AXIS2_PLACEMENT_3D('',#84898,#59193,#59194) ;
#50942 = AXIS2_PLACEMENT_3D('',#84899,#59195,#59196) ;
#50943 = AXIS2_PLACEMENT_3D('',#84901,#59197,#59198) ;
#50944 = AXIS2_PLACEMENT_3D('',#84902,#59199,#59200) ;
#50945 = AXIS2_PLACEMENT_3D('',#84903,#59201,#59202) ;
#50946 = AXIS2_PLACEMENT_3D('',#84904,#59203,#59204) ;
#50947 = AXIS2_PLACEMENT_3D('',#84905,#59205,#59206) ;
#50948 = AXIS2_PLACEMENT_3D('',#84907,#59208,#59209) ;
#50949 = AXIS2_PLACEMENT_3D('',#84909,#59211,#59212) ;
#50950 = AXIS2_PLACEMENT_3D('',#84911,#59214,#59215) ;
#50951 = AXIS2_PLACEMENT_3D('',#84913,#59217,#59218) ;
#50952 = AXIS2_PLACEMENT_3D('',#84914,#59219,#59220) ;
#50953 = AXIS2_PLACEMENT_3D('',#84916,#59221,#59222) ;
#50954 = AXIS2_PLACEMENT_3D('',#84918,#59223,#59224) ;
#50955 = AXIS2_PLACEMENT_3D('',#84919,#59225,#59226) ;
#50956 = AXIS2_PLACEMENT_3D('',#84920,#59227,#59228) ;
#50957 = AXIS2_PLACEMENT_3D('',#84922,#59229,#59230) ;
#50958 = AXIS2_PLACEMENT_3D('',#84924,#59231,#59232) ;
#50959 = AXIS2_PLACEMENT_3D('',#84925,#59233,#59234) ;
#50960 = AXIS2_PLACEMENT_3D('',#84926,#59235,#59236) ;
#50961 = AXIS2_PLACEMENT_3D('',#84933,#59241,#59242) ;
#50962 = AXIS2_PLACEMENT_3D('',#84934,#59243,#59244) ;
#50963 = AXIS2_PLACEMENT_3D('',#84935,#59245,#59246) ;
#50964 = AXIS2_PLACEMENT_3D('',#84936,#59247,#59248) ;
#50965 = AXIS2_PLACEMENT_3D('',#84937,#59249,#59250) ;
#50966 = AXIS2_PLACEMENT_3D('',#84938,#59251,#59252) ;
#50967 = AXIS2_PLACEMENT_3D('',#84939,#59253,#59254) ;
#50968 = AXIS2_PLACEMENT_3D('',#84940,#59255,#59256) ;
#50969 = AXIS2_PLACEMENT_3D('',#84941,#59257,#59258) ;
#50970 = AXIS2_PLACEMENT_3D('',#84942,#59259,#59260) ;
#50971 = AXIS2_PLACEMENT_3D('',#84943,#59261,#59262) ;
#50972 = AXIS2_PLACEMENT_3D('',#84944,#59263,#59264) ;
#50973 = AXIS2_PLACEMENT_3D('',#84945,#59265,#59266) ;
#50974 = AXIS2_PLACEMENT_3D('',#84946,#59267,#59268) ;
#50975 = AXIS2_PLACEMENT_3D('',#84947,#59269,#59270) ;
#50976 = AXIS2_PLACEMENT_3D('',#84949,#59271,#59272) ;
#50977 = AXIS2_PLACEMENT_3D('',#84950,#59273,#59274) ;
#50978 = AXIS2_PLACEMENT_3D('',#84951,#59275,#59276) ;
#50979 = AXIS2_PLACEMENT_3D('',#84952,#59277,#59278) ;
#50980 = AXIS2_PLACEMENT_3D('',#84953,#59279,#59280) ;
#50981 = AXIS2_PLACEMENT_3D('',#84955,#59281,#59282) ;
#50982 = AXIS2_PLACEMENT_3D('',#84956,#59283,#59284) ;
#50983 = AXIS2_PLACEMENT_3D('',#84957,#59285,#59286) ;
#50984 = AXIS2_PLACEMENT_3D('',#84958,#59287,#59288) ;
#50985 = AXIS2_PLACEMENT_3D('',#84960,#59290,#59291) ;
#50986 = AXIS2_PLACEMENT_3D('',#84961,#59292,#59293) ;
#50987 = AXIS2_PLACEMENT_3D('',#84963,#59294,#59295) ;
#50988 = AXIS2_PLACEMENT_3D('',#84964,#59296,#59297) ;
#50989 = AXIS2_PLACEMENT_3D('',#84965,#59298,#59299) ;
#50990 = AXIS2_PLACEMENT_3D('',#84967,#59300,#59301) ;
#50991 = AXIS2_PLACEMENT_3D('',#84968,#59302,#59303) ;
#50992 = AXIS2_PLACEMENT_3D('',#84969,#59304,#59305) ;
#50993 = AXIS2_PLACEMENT_3D('',#84970,#59306,#59307) ;
#50994 = AXIS2_PLACEMENT_3D('',#84972,#59309,#59310) ;
#50995 = AXIS2_PLACEMENT_3D('',#84974,#59312,#59313) ;
#50996 = AXIS2_PLACEMENT_3D('',#84975,#59314,#59315) ;
#50997 = AXIS2_PLACEMENT_3D('',#84977,#59317,#59318) ;
#50998 = AXIS2_PLACEMENT_3D('',#84979,#59320,#59321) ;
#50999 = AXIS2_PLACEMENT_3D('',#84981,#59323,#59324) ;
#51000 = AXIS2_PLACEMENT_3D('',#84982,#59325,#59326) ;
#51001 = AXIS2_PLACEMENT_3D('',#84983,#59327,#59328) ;
#51002 = AXIS2_PLACEMENT_3D('',#84984,#59329,#59330) ;
#51003 = AXIS2_PLACEMENT_3D('',#84986,#59332,#59333) ;
#51004 = AXIS2_PLACEMENT_3D('',#84987,#59334,#59335) ;
#51005 = AXIS2_PLACEMENT_3D('',#84989,#59336,#59337) ;
#51006 = AXIS2_PLACEMENT_3D('',#84991,#59338,#59339) ;
#51007 = AXIS2_PLACEMENT_3D('',#84992,#59340,#59341) ;
#51008 = AXIS2_PLACEMENT_3D('',#84993,#59342,#59343) ;
#51009 = AXIS2_PLACEMENT_3D('',#84995,#59344,#59345) ;
#51010 = AXIS2_PLACEMENT_3D('',#84997,#59346,#59347) ;
#51011 = AXIS2_PLACEMENT_3D('',#84998,#59348,#59349) ;
#51012 = AXIS2_PLACEMENT_3D('',#84999,#59350,#59351) ;
#51013 = AXIS2_PLACEMENT_3D('',#85006,#59356,#59357) ;
#51014 = AXIS2_PLACEMENT_3D('',#85007,#59358,#59359) ;
#51015 = AXIS2_PLACEMENT_3D('',#85008,#59360,#59361) ;
#51016 = AXIS2_PLACEMENT_3D('',#85009,#59362,#59363) ;
#51017 = AXIS2_PLACEMENT_3D('',#85010,#59364,#59365) ;
#51018 = AXIS2_PLACEMENT_3D('',#85011,#59366,#59367) ;
#51019 = AXIS2_PLACEMENT_3D('',#85012,#59368,#59369) ;
#51020 = AXIS2_PLACEMENT_3D('',#85013,#59370,#59371) ;
#51021 = AXIS2_PLACEMENT_3D('',#85014,#59372,#59373) ;
#51022 = AXIS2_PLACEMENT_3D('',#85015,#59374,#59375) ;
#51023 = AXIS2_PLACEMENT_3D('',#85016,#59376,#59377) ;
#51024 = AXIS2_PLACEMENT_3D('',#85017,#59378,#59379) ;
#51025 = AXIS2_PLACEMENT_3D('',#85019,#59380,#59381) ;
#51026 = AXIS2_PLACEMENT_3D('',#85020,#59382,#59383) ;
#51027 = AXIS2_PLACEMENT_3D('',#85021,#59384,#59385) ;
#51028 = AXIS2_PLACEMENT_3D('',#85022,#59386,#59387) ;
#51029 = AXIS2_PLACEMENT_3D('',#85023,#59388,#59389) ;
#51030 = AXIS2_PLACEMENT_3D('',#85024,#59390,#59391) ;
#51031 = AXIS2_PLACEMENT_3D('',#85025,#59392,#59393) ;
#51032 = AXIS2_PLACEMENT_3D('',#85026,#59394,#59395) ;
#51033 = AXIS2_PLACEMENT_3D('',#85027,#59396,#59397) ;
#51034 = AXIS2_PLACEMENT_3D('',#85029,#59398,#59399) ;
#51035 = AXIS2_PLACEMENT_3D('',#85030,#59400,#59401) ;
#51036 = AXIS2_PLACEMENT_3D('',#85031,#59402,#59403) ;
#51037 = AXIS2_PLACEMENT_3D('',#85032,#59404,#59405) ;
#51038 = AXIS2_PLACEMENT_3D('',#85034,#59406,#59407) ;
#51039 = AXIS2_PLACEMENT_3D('',#85035,#59408,#59409) ;
#51040 = AXIS2_PLACEMENT_3D('',#85036,#59410,#59411) ;
#51041 = AXIS2_PLACEMENT_3D('',#85037,#59412,#59413) ;
#51042 = AXIS2_PLACEMENT_3D('',#85039,#59415,#59416) ;
#51043 = AXIS2_PLACEMENT_3D('',#85041,#59417,#59418) ;
#51044 = AXIS2_PLACEMENT_3D('',#85042,#59419,#59420) ;
#51045 = AXIS2_PLACEMENT_3D('',#85043,#59421,#59422) ;
#51046 = AXIS2_PLACEMENT_3D('',#85044,#59423,#59424) ;
#51047 = AXIS2_PLACEMENT_3D('',#85046,#59426,#59427) ;
#51048 = AXIS2_PLACEMENT_3D('',#85048,#59429,#59430) ;
#51049 = AXIS2_PLACEMENT_3D('',#85049,#59431,#59432) ;
#51050 = AXIS2_PLACEMENT_3D('',#85051,#59434,#59435) ;
#51051 = AXIS2_PLACEMENT_3D('',#85053,#59437,#59438) ;
#51052 = AXIS2_PLACEMENT_3D('',#85055,#59440,#59441) ;
#51053 = AXIS2_PLACEMENT_3D('',#85056,#59442,#59443) ;
#51054 = AXIS2_PLACEMENT_3D('',#85057,#59444,#59445) ;
#51055 = AXIS2_PLACEMENT_3D('',#85059,#59447,#59448) ;
#51056 = AXIS2_PLACEMENT_3D('',#85060,#59449,#59450) ;
#51057 = AXIS2_PLACEMENT_3D('',#85062,#59451,#59452) ;
#51058 = AXIS2_PLACEMENT_3D('',#85064,#59453,#59454) ;
#51059 = AXIS2_PLACEMENT_3D('',#85065,#59455,#59456) ;
#51060 = AXIS2_PLACEMENT_3D('',#85066,#59457,#59458) ;
#51061 = AXIS2_PLACEMENT_3D('',#85068,#59459,#59460) ;
#51062 = AXIS2_PLACEMENT_3D('',#85070,#59461,#59462) ;
#51063 = AXIS2_PLACEMENT_3D('',#85071,#59463,#59464) ;
#51064 = AXIS2_PLACEMENT_3D('',#85072,#59465,#59466) ;
#51065 = AXIS2_PLACEMENT_3D('',#85073,#59467,#59468) ;
#51066 = AXIS2_PLACEMENT_3D('',#85074,#59469,#59470) ;
#51067 = AXIS2_PLACEMENT_3D('',#85075,#59471,#59472) ;
#51068 = AXIS2_PLACEMENT_3D('',#85076,#59473,#59474) ;
#51069 = AXIS2_PLACEMENT_3D('',#85077,#59475,#59476) ;
#51070 = AXIS2_PLACEMENT_3D('',#85078,#59477,#59478) ;
#51071 = AXIS2_PLACEMENT_3D('',#85079,#59479,#59480) ;
#51072 = AXIS2_PLACEMENT_3D('',#85080,#59481,#59482) ;
#51073 = AXIS2_PLACEMENT_3D('',#85082,#59483,#59484) ;
#51074 = AXIS2_PLACEMENT_3D('',#85083,#59485,#59486) ;
#51075 = AXIS2_PLACEMENT_3D('',#85084,#59487,#59488) ;
#51076 = AXIS2_PLACEMENT_3D('',#85086,#59489,#59490) ;
#51077 = AXIS2_PLACEMENT_3D('',#85088,#59492,#59493) ;
#51078 = AXIS2_PLACEMENT_3D('',#85090,#59494,#59495) ;
#51079 = AXIS2_PLACEMENT_3D('',#85091,#59496,#59497) ;
#51080 = AXIS2_PLACEMENT_3D('',#85092,#59498,#59499) ;
#51081 = AXIS2_PLACEMENT_3D('',#85094,#59501,#59502) ;
#51082 = AXIS2_PLACEMENT_3D('',#85095,#59503,#59504) ;
#51083 = AXIS2_PLACEMENT_3D('',#85096,#59505,#59506) ;
#51084 = AXIS2_PLACEMENT_3D('',#85097,#59507,#59508) ;
#51085 = AXIS2_PLACEMENT_3D('',#85098,#59509,#59510) ;
#51086 = AXIS2_PLACEMENT_3D('',#85099,#59511,#59512) ;
#51087 = AXIS2_PLACEMENT_3D('',#85100,#59513,#59514) ;
#51088 = AXIS2_PLACEMENT_3D('',#85101,#59515,#59516) ;
#51089 = AXIS2_PLACEMENT_3D('',#85102,#59517,#59518) ;
#51090 = AXIS2_PLACEMENT_3D('',#85103,#59519,#59520) ;
#51091 = AXIS2_PLACEMENT_3D('',#85104,#59521,#59522) ;
#51092 = AXIS2_PLACEMENT_3D('',#85106,#59523,#59524) ;
#51093 = AXIS2_PLACEMENT_3D('',#85107,#59525,#59526) ;
#51094 = AXIS2_PLACEMENT_3D('',#85108,#59527,#59528) ;
#51095 = AXIS2_PLACEMENT_3D('',#85110,#59529,#59530) ;
#51096 = AXIS2_PLACEMENT_3D('',#85112,#59532,#59533) ;
#51097 = AXIS2_PLACEMENT_3D('',#85114,#59534,#59535) ;
#51098 = AXIS2_PLACEMENT_3D('',#85115,#59536,#59537) ;
#51099 = AXIS2_PLACEMENT_3D('',#85116,#59538,#59539) ;
#51100 = AXIS2_PLACEMENT_3D('',#85118,#59540,#59541) ;
#51101 = AXIS2_PLACEMENT_3D('',#85120,#59543,#59544) ;
#51102 = AXIS2_PLACEMENT_3D('',#85122,#59545,#59546) ;
#51103 = AXIS2_PLACEMENT_3D('',#85123,#59547,#59548) ;
#51104 = AXIS2_PLACEMENT_3D('',#85124,#59549,#59550) ;
#51105 = AXIS2_PLACEMENT_3D('',#85126,#59551,#59552) ;
#51106 = AXIS2_PLACEMENT_3D('',#85127,#59553,#59554) ;
#51107 = AXIS2_PLACEMENT_3D('',#85128,#59555,#59556) ;
#51108 = AXIS2_PLACEMENT_3D('',#85130,#59557,#59558) ;
#51109 = AXIS2_PLACEMENT_3D('',#85132,#59560,#59561) ;
#51110 = AXIS2_PLACEMENT_3D('',#85134,#59562,#59563) ;
#51111 = AXIS2_PLACEMENT_3D('',#85135,#59564,#59565) ;
#51112 = AXIS2_PLACEMENT_3D('',#85136,#59566,#59567) ;
#51113 = AXIS2_PLACEMENT_3D('',#85138,#59568,#59569) ;
#51114 = AXIS2_PLACEMENT_3D('',#85139,#59570,#59571) ;
#51115 = AXIS2_PLACEMENT_3D('',#85140,#59572,#59573) ;
#51116 = AXIS2_PLACEMENT_3D('',#85142,#59574,#59575) ;
#51117 = AXIS2_PLACEMENT_3D('',#85144,#59577,#59578) ;
#51118 = AXIS2_PLACEMENT_3D('',#85146,#59579,#59580) ;
#51119 = AXIS2_PLACEMENT_3D('',#85147,#59581,#59582) ;
#51120 = AXIS2_PLACEMENT_3D('',#85148,#59583,#59584) ;
#51121 = AXIS2_PLACEMENT_3D('',#85150,#59585,#59586) ;
#51122 = AXIS2_PLACEMENT_3D('',#85152,#59588,#59589) ;
#51123 = AXIS2_PLACEMENT_3D('',#85154,#59590,#59591) ;
#51124 = AXIS2_PLACEMENT_3D('',#85155,#59592,#59593) ;
#51125 = AXIS2_PLACEMENT_3D('',#85156,#59594,#59595) ;
#51126 = AXIS2_PLACEMENT_3D('',#85158,#59596,#59597) ;
#51127 = AXIS2_PLACEMENT_3D('',#85160,#59599,#59600) ;
#51128 = AXIS2_PLACEMENT_3D('',#85162,#59601,#59602) ;
#51129 = AXIS2_PLACEMENT_3D('',#85163,#59603,#59604) ;
#51130 = AXIS2_PLACEMENT_3D('',#85164,#59605,#59606) ;
#51131 = AXIS2_PLACEMENT_3D('',#85166,#59607,#59608) ;
#51132 = AXIS2_PLACEMENT_3D('',#85168,#59610,#59611) ;
#51133 = AXIS2_PLACEMENT_3D('',#85170,#59612,#59613) ;
#51134 = AXIS2_PLACEMENT_3D('',#85171,#59614,#59615) ;
#51135 = AXIS2_PLACEMENT_3D('',#85172,#59616,#59617) ;
#51136 = AXIS2_PLACEMENT_3D('',#85174,#59618,#59619) ;
#51137 = AXIS2_PLACEMENT_3D('',#85176,#59621,#59622) ;
#51138 = AXIS2_PLACEMENT_3D('',#85178,#59623,#59624) ;
#51139 = AXIS2_PLACEMENT_3D('',#85179,#59625,#59626) ;
#51140 = AXIS2_PLACEMENT_3D('',#85180,#59627,#59628) ;
#51141 = AXIS2_PLACEMENT_3D('',#85182,#59629,#59630) ;
#51142 = AXIS2_PLACEMENT_3D('',#85184,#59632,#59633) ;
#51143 = AXIS2_PLACEMENT_3D('',#85186,#59634,#59635) ;
#51144 = AXIS2_PLACEMENT_3D('',#85187,#59636,#59637) ;
#51145 = AXIS2_PLACEMENT_3D('',#85188,#59638,#59639) ;
#51146 = AXIS2_PLACEMENT_3D('',#85190,#59640,#59641) ;
#51147 = AXIS2_PLACEMENT_3D('',#85192,#59643,#59644) ;
#51148 = AXIS2_PLACEMENT_3D('',#85194,#59645,#59646) ;
#51149 = AXIS2_PLACEMENT_3D('',#85195,#59647,#59648) ;
#51150 = AXIS2_PLACEMENT_3D('',#85196,#59649,#59650) ;
#51151 = AXIS2_PLACEMENT_3D('',#85198,#59652,#59653) ;
#51152 = AXIS2_PLACEMENT_3D('',#85201,#59654,#59655) ;
#51153 = AXIS2_PLACEMENT_3D('',#85202,#59656,#59657) ;
#51154 = AXIS2_PLACEMENT_3D('',#85203,#59658,#59659) ;
#51155 = AXIS2_PLACEMENT_3D('',#85204,#59660,#59661) ;
#51156 = AXIS2_PLACEMENT_3D('',#85207,#59664,#59665) ;
#51157 = AXIS2_PLACEMENT_3D('',#85209,#59667,#59668) ;
#51158 = AXIS2_PLACEMENT_3D('',#85212,#59669,#59670) ;
#51159 = AXIS2_PLACEMENT_3D('',#85215,#59673,#59674) ;
#51160 = AXIS2_PLACEMENT_3D('',#85216,#59675,#59676) ;
#51161 = AXIS2_PLACEMENT_3D('',#85217,#59677,#59678) ;
#51162 = AXIS2_PLACEMENT_3D('',#85218,#59679,#59680) ;
#51163 = AXIS2_PLACEMENT_3D('',#85220,#59681,#59682) ;
#51164 = AXIS2_PLACEMENT_3D('',#85221,#59683,#59684) ;
#51165 = AXIS2_PLACEMENT_3D('',#85222,#59685,#59686) ;
#51166 = AXIS2_PLACEMENT_3D('',#85228,#59690,#59691) ;
#51167 = AXIS2_PLACEMENT_3D('',#85231,#59693,#59694) ;
#51168 = AXIS2_PLACEMENT_3D('',#85232,#59695,#59696) ;
#51169 = AXIS2_PLACEMENT_3D('',#85236,#59699,#59700) ;
#51170 = AXIS2_PLACEMENT_3D('',#85239,#59702,#59703) ;
#51171 = AXIS2_PLACEMENT_3D('',#85240,#59704,#59705) ;
#51172 = AXIS2_PLACEMENT_3D('',#85243,#59707,#59708) ;
#51173 = AXIS2_PLACEMENT_3D('',#85244,#59709,#59710) ;
#51174 = AXIS2_PLACEMENT_3D('',#85248,#59713,#59714) ;
#51175 = AXIS2_PLACEMENT_3D('',#85251,#59716,#59717) ;
#51176 = AXIS2_PLACEMENT_3D('',#85252,#59718,#59719) ;
#51177 = AXIS2_PLACEMENT_3D('',#85255,#59721,#59722) ;
#51178 = AXIS2_PLACEMENT_3D('',#85256,#59723,#59724) ;
#51179 = AXIS2_PLACEMENT_3D('',#85260,#59727,#59728) ;
#51180 = AXIS2_PLACEMENT_3D('',#85263,#59730,#59731) ;
#51181 = AXIS2_PLACEMENT_3D('',#85264,#59732,#59733) ;
#51182 = AXIS2_PLACEMENT_3D('',#85268,#59736,#59737) ;
#51183 = AXIS2_PLACEMENT_3D('',#85271,#59739,#59740) ;
#51184 = AXIS2_PLACEMENT_3D('',#85272,#59741,#59742) ;
#51185 = AXIS2_PLACEMENT_3D('',#85276,#59745,#59746) ;
#51186 = AXIS2_PLACEMENT_3D('',#85279,#59748,#59749) ;
#51187 = AXIS2_PLACEMENT_3D('',#85280,#59750,#59751) ;
#51188 = AXIS2_PLACEMENT_3D('',#85284,#59754,#59755) ;
#51189 = AXIS2_PLACEMENT_3D('',#85287,#59757,#59758) ;
#51190 = AXIS2_PLACEMENT_3D('',#85288,#59759,#59760) ;
#51191 = AXIS2_PLACEMENT_3D('',#85292,#59763,#59764) ;
#51192 = AXIS2_PLACEMENT_3D('',#85295,#59766,#59767) ;
#51193 = AXIS2_PLACEMENT_3D('',#85296,#59768,#59769) ;
#51194 = AXIS2_PLACEMENT_3D('',#85300,#59772,#59773) ;
#51195 = AXIS2_PLACEMENT_3D('',#85303,#59775,#59776) ;
#51196 = AXIS2_PLACEMENT_3D('',#85304,#59777,#59778) ;
#51197 = AXIS2_PLACEMENT_3D('',#85308,#59781,#59782) ;
#51198 = AXIS2_PLACEMENT_3D('',#85311,#59784,#59785) ;
#51199 = AXIS2_PLACEMENT_3D('',#85312,#59786,#59787) ;
#51200 = AXIS2_PLACEMENT_3D('',#85314,#59789,#59790) ;
#51201 = AXIS2_PLACEMENT_3D('',#85315,#59791,#59792) ;
#51202 = AXIS2_PLACEMENT_3D('',#85316,#59793,#59794) ;
#51203 = AXIS2_PLACEMENT_3D('',#85319,#59795,#59796) ;
#51204 = AXIS2_PLACEMENT_3D('',#85323,#59798,#59799) ;
#51205 = AXIS2_PLACEMENT_3D('',#85325,#59801,#59802) ;
#51206 = AXIS2_PLACEMENT_3D('',#85327,#59803,#59804) ;
#51207 = AXIS2_PLACEMENT_3D('',#85328,#59805,#59806) ;
#51208 = AXIS2_PLACEMENT_3D('',#85329,#59807,#59808) ;
#51209 = AXIS2_PLACEMENT_3D('',#85330,#59809,#59810) ;
#51210 = AXIS2_PLACEMENT_3D('',#85331,#59811,#59812) ;
#51211 = AXIS2_PLACEMENT_3D('',#85332,#59813,#59814) ;
#51212 = AXIS2_PLACEMENT_3D('',#85335,#59816,#59817) ;
#51213 = AXIS2_PLACEMENT_3D('',#85336,#59818,#59819) ;
#51214 = AXIS2_PLACEMENT_3D('',#85340,#59822,#59823) ;
#51215 = AXIS2_PLACEMENT_3D('',#85347,#59827,#59828) ;
#51216 = AXIS2_PLACEMENT_3D('',#85348,#59829,#59830) ;
#51217 = AXIS2_PLACEMENT_3D('',#85351,#59832,#59833) ;
#51218 = AXIS2_PLACEMENT_3D('',#85352,#59834,#59835) ;
#51219 = AXIS2_PLACEMENT_3D('',#85354,#59836,#59837) ;
#51220 = AXIS2_PLACEMENT_3D('',#85355,#59838,#59839) ;
#51221 = AXIS2_PLACEMENT_3D('',#85356,#59840,#59841) ;
#51222 = AXIS2_PLACEMENT_3D('',#85357,#59842,#59843) ;
#51223 = AXIS2_PLACEMENT_3D('',#85358,#59844,#59845) ;
#51224 = AXIS2_PLACEMENT_3D('',#85361,#59848,#59849) ;
#51225 = AXIS2_PLACEMENT_3D('',#85363,#59850,#59851) ;
#51226 = AXIS2_PLACEMENT_3D('',#85365,#59852,#59853) ;
#51227 = AXIS2_PLACEMENT_3D('',#85366,#59854,#59855) ;
#51228 = AXIS2_PLACEMENT_3D('',#85367,#59856,#59857) ;
#51229 = AXIS2_PLACEMENT_3D('',#85370,#59858,#59859) ;
#51230 = AXIS2_PLACEMENT_3D('',#85371,#59860,#59861) ;
#51231 = AXIS2_PLACEMENT_3D('',#85372,#59862,#59863) ;
#51232 = AXIS2_PLACEMENT_3D('',#85373,#59864,#59865) ;
#51233 = AXIS2_PLACEMENT_3D('',#85375,#59867,#59868) ;
#51234 = AXIS2_PLACEMENT_3D('',#85378,#59869,#59870) ;
#51235 = AXIS2_PLACEMENT_3D('',#85379,#59871,#59872) ;
#51236 = AXIS2_PLACEMENT_3D('',#85380,#59873,#59874) ;
#51237 = AXIS2_PLACEMENT_3D('',#85381,#59875,#59876) ;
#51238 = AXIS2_PLACEMENT_3D('',#85383,#59878,#59879) ;
#51239 = AXIS2_PLACEMENT_3D('',#85386,#59880,#59881) ;
#51240 = AXIS2_PLACEMENT_3D('',#85387,#59882,#59883) ;
#51241 = AXIS2_PLACEMENT_3D('',#85388,#59884,#59885) ;
#51242 = AXIS2_PLACEMENT_3D('',#85389,#59886,#59887) ;
#51243 = AXIS2_PLACEMENT_3D('',#85391,#59889,#59890) ;
#51244 = AXIS2_PLACEMENT_3D('',#85394,#59891,#59892) ;
#51245 = AXIS2_PLACEMENT_3D('',#85395,#59893,#59894) ;
#51246 = AXIS2_PLACEMENT_3D('',#85396,#59895,#59896) ;
#51247 = AXIS2_PLACEMENT_3D('',#85397,#59897,#59898) ;
#51248 = AXIS2_PLACEMENT_3D('',#85399,#59900,#59901) ;
#51249 = AXIS2_PLACEMENT_3D('',#85401,#59902,#59903) ;
#51250 = AXIS2_PLACEMENT_3D('',#85403,#59904,#59905) ;
#51251 = AXIS2_PLACEMENT_3D('',#85404,#59906,#59907) ;
#51252 = AXIS2_PLACEMENT_3D('',#85405,#59908,#59909) ;
#51253 = AXIS2_PLACEMENT_3D('',#85407,#59911,#59912) ;
#51254 = AXIS2_PLACEMENT_3D('',#85410,#59915,#59916) ;
#51255 = AXIS2_PLACEMENT_3D('',#85412,#59918,#59919) ;
#51256 = AXIS2_PLACEMENT_3D('',#85415,#59922,#59923) ;
#51257 = AXIS2_PLACEMENT_3D('',#85418,#59926,#59927) ;
#51258 = AXIS2_PLACEMENT_3D('',#85421,#59930,#59931) ;
#51259 = AXIS2_PLACEMENT_3D('',#85424,#59934,#59935) ;
#51260 = AXIS2_PLACEMENT_3D('',#85427,#59938,#59939) ;
#51261 = AXIS2_PLACEMENT_3D('',#85429,#59941,#59942) ;
#51262 = AXIS2_PLACEMENT_3D('',#85430,#59943,#59944) ;
#51263 = AXIS2_PLACEMENT_3D('',#85431,#59945,#59946) ;
#51264 = AXIS2_PLACEMENT_3D('',#85433,#59947,#59948) ;
#51265 = AXIS2_PLACEMENT_3D('',#85435,#59949,#59950) ;
#51266 = AXIS2_PLACEMENT_3D('',#85436,#59951,#59952) ;
#51267 = AXIS2_PLACEMENT_3D('',#85437,#59953,#59954) ;
#51268 = AXIS2_PLACEMENT_3D('',#85439,#59955,#59956) ;
#51269 = AXIS2_PLACEMENT_3D('',#85441,#59957,#59958) ;
#51270 = AXIS2_PLACEMENT_3D('',#85442,#59959,#59960) ;
#51271 = AXIS2_PLACEMENT_3D('',#85443,#59961,#59962) ;
#51272 = AXIS2_PLACEMENT_3D('',#85445,#59964,#59965) ;
#51273 = AXIS2_PLACEMENT_3D('',#85448,#59968,#59969) ;
#51274 = AXIS2_PLACEMENT_3D('',#85450,#59970,#59971) ;
#51275 = AXIS2_PLACEMENT_3D('',#85452,#59972,#59973) ;
#51276 = AXIS2_PLACEMENT_3D('',#85453,#59974,#59975) ;
#51277 = AXIS2_PLACEMENT_3D('',#85454,#59976,#59977) ;
#51278 = AXIS2_PLACEMENT_3D('',#85455,#59978,#59979) ;
#51279 = AXIS2_PLACEMENT_3D('',#85456,#59980,#59981) ;
#51280 = AXIS2_PLACEMENT_3D('',#85457,#59982,#59983) ;
#51281 = AXIS2_PLACEMENT_3D('',#85459,#59985,#59986) ;
#51282 = AXIS2_PLACEMENT_3D('',#85461,#59987,#59988) ;
#51283 = AXIS2_PLACEMENT_3D('',#85462,#59989,#59990) ;
#51284 = AXIS2_PLACEMENT_3D('',#85463,#59991,#59992) ;
#51285 = AXIS2_PLACEMENT_3D('',#85464,#59993,#59994) ;
#51286 = AXIS2_PLACEMENT_3D('',#85466,#59996,#59997) ;
#51287 = AXIS2_PLACEMENT_3D('',#85467,#59998,#59999) ;
#51288 = AXIS2_PLACEMENT_3D('',#85468,#60000,#60001) ;
#51289 = AXIS2_PLACEMENT_3D('',#85469,#60002,#60003) ;
#51290 = AXIS2_PLACEMENT_3D('',#85470,#60004,#60005) ;
#51291 = AXIS2_PLACEMENT_3D('',#85471,#60006,#60007) ;
#51292 = AXIS2_PLACEMENT_3D('',#85472,#60008,#60009) ;
#51293 = AXIS2_PLACEMENT_3D('',#85473,#60010,#60011) ;
#51294 = AXIS2_PLACEMENT_3D('',#85474,#60012,#60013) ;
#51295 = AXIS2_PLACEMENT_3D('',#85475,#60014,#60015) ;
#51296 = AXIS2_PLACEMENT_3D('',#85476,#60016,#60017) ;
#51297 = AXIS2_PLACEMENT_3D('',#85477,#60018,#60019) ;
#51298 = AXIS2_PLACEMENT_3D('',#85478,#60020,#60021) ;
#51299 = AXIS2_PLACEMENT_3D('',#85479,#60022,#60023) ;
#51300 = AXIS2_PLACEMENT_3D('',#85481,#60025,#60026) ;
#51301 = AXIS2_PLACEMENT_3D('',#85484,#60029,#60030) ;
#51302 = AXIS2_PLACEMENT_3D('',#85486,#60032,#60033) ;
#51303 = AXIS2_PLACEMENT_3D('',#85489,#60036,#60037) ;
#51304 = AXIS2_PLACEMENT_3D('',#85490,#60038,#60039) ;
#51305 = AXIS2_PLACEMENT_3D('',#85491,#60040,#60041) ;
#51306 = AXIS2_PLACEMENT_3D('',#85494,#60042,#60043) ;
#51307 = AXIS2_PLACEMENT_3D('',#85498,#60045,#60046) ;
#51308 = AXIS2_PLACEMENT_3D('',#85500,#60048,#60049) ;
#51309 = AXIS2_PLACEMENT_3D('',#85501,#60050,#60051) ;
#51310 = AXIS2_PLACEMENT_3D('',#85502,#60052,#60053) ;
#51311 = AXIS2_PLACEMENT_3D('',#85503,#60054,#60055) ;
#51312 = AXIS2_PLACEMENT_3D('',#85504,#60056,#60057) ;
#51313 = AXIS2_PLACEMENT_3D('',#85505,#60058,#60059) ;
#51314 = AXIS2_PLACEMENT_3D('',#85509,#60062,#60063) ;
#51315 = AXIS2_PLACEMENT_3D('',#85512,#60064,#60065) ;
#51316 = AXIS2_PLACEMENT_3D('',#85516,#60067,#60068) ;
#51317 = AXIS2_PLACEMENT_3D('',#85518,#60070,#60071) ;
#51318 = AXIS2_PLACEMENT_3D('',#85519,#60072,#60073) ;
#51319 = AXIS2_PLACEMENT_3D('',#85520,#60074,#60075) ;
#51320 = AXIS2_PLACEMENT_3D('',#85521,#60076,#60077) ;
#51321 = AXIS2_PLACEMENT_3D('',#85522,#60078,#60079) ;
#51322 = AXIS2_PLACEMENT_3D('',#85523,#60080,#60081) ;
#51323 = AXIS2_PLACEMENT_3D('',#85525,#60083,#60084) ;
#51324 = AXIS2_PLACEMENT_3D('',#85527,#60086,#60087) ;
#51325 = AXIS2_PLACEMENT_3D('',#85528,#60088,#60089) ;
#51326 = AXIS2_PLACEMENT_3D('',#85529,#60090,#60091) ;
#51327 = AXIS2_PLACEMENT_3D('',#85530,#60092,#60093) ;
#51328 = AXIS2_PLACEMENT_3D('',#85531,#60094,#60095) ;
#51329 = AXIS2_PLACEMENT_3D('',#85532,#60096,#60097) ;
#51330 = AXIS2_PLACEMENT_3D('',#85533,#60098,#60099) ;
#51331 = AXIS2_PLACEMENT_3D('',#85534,#60100,#60101) ;
#51332 = AXIS2_PLACEMENT_3D('',#85535,#60102,#60103) ;
#51333 = AXIS2_PLACEMENT_3D('',#85536,#60104,#60105) ;
#51334 = AXIS2_PLACEMENT_3D('',#85537,#60106,#60107) ;
#51335 = AXIS2_PLACEMENT_3D('',#85538,#60108,#60109) ;
#51336 = AXIS2_PLACEMENT_3D('',#85539,#60110,#60111) ;
#51337 = AXIS2_PLACEMENT_3D('',#85540,#60112,#60113) ;
#51338 = AXIS2_PLACEMENT_3D('',#85541,#60114,#60115) ;
#51339 = AXIS2_PLACEMENT_3D('',#85542,#60116,#60117) ;
#51340 = AXIS2_PLACEMENT_3D('',#85543,#60118,#60119) ;
#51341 = AXIS2_PLACEMENT_3D('',#85544,#60120,#60121) ;
#51342 = AXIS2_PLACEMENT_3D('',#85547,#60122,#60123) ;
#51343 = AXIS2_PLACEMENT_3D('',#85551,#60125,#60126) ;
#51344 = AXIS2_PLACEMENT_3D('',#85553,#60128,#60129) ;
#51345 = AXIS2_PLACEMENT_3D('',#85554,#60130,#60131) ;
#51346 = AXIS2_PLACEMENT_3D('',#85555,#60132,#60133) ;
#51347 = AXIS2_PLACEMENT_3D('',#85556,#60134,#60135) ;
#51348 = AXIS2_PLACEMENT_3D('',#85557,#60136,#60137) ;
#51349 = AXIS2_PLACEMENT_3D('',#85558,#60138,#60139) ;
#51350 = AXIS2_PLACEMENT_3D('',#85559,#60140,#60141) ;
#51351 = AXIS2_PLACEMENT_3D('',#85562,#60143,#60144) ;
#51352 = AXIS2_PLACEMENT_3D('',#85563,#60145,#60146) ;
#51353 = AXIS2_PLACEMENT_3D('',#85567,#60149,#60150) ;
#51354 = AXIS2_PLACEMENT_3D('',#85574,#60154,#60155) ;
#51355 = AXIS2_PLACEMENT_3D('',#85575,#60156,#60157) ;
#51356 = AXIS2_PLACEMENT_3D('',#85578,#60159,#60160) ;
#51357 = AXIS2_PLACEMENT_3D('',#85579,#60161,#60162) ;
#51358 = AXIS2_PLACEMENT_3D('',#85581,#60163,#60164) ;
#51359 = AXIS2_PLACEMENT_3D('',#85582,#60165,#60166) ;
#51360 = AXIS2_PLACEMENT_3D('',#85583,#60167,#60168) ;
#51361 = AXIS2_PLACEMENT_3D('',#85584,#60169,#60170) ;
#51362 = AXIS2_PLACEMENT_3D('',#85585,#60171,#60172) ;
#51363 = AXIS2_PLACEMENT_3D('',#85588,#60175,#60176) ;
#51364 = AXIS2_PLACEMENT_3D('',#85591,#60177,#60178) ;
#51365 = AXIS2_PLACEMENT_3D('',#85592,#60179,#60180) ;
#51366 = AXIS2_PLACEMENT_3D('',#85593,#60181,#60182) ;
#51367 = AXIS2_PLACEMENT_3D('',#85594,#60183,#60184) ;
#51368 = AXIS2_PLACEMENT_3D('',#85597,#60185,#60186) ;
#51369 = AXIS2_PLACEMENT_3D('',#85598,#60187,#60188) ;
#51370 = AXIS2_PLACEMENT_3D('',#85599,#60189,#60190) ;
#51371 = AXIS2_PLACEMENT_3D('',#85600,#60191,#60192) ;
#51372 = AXIS2_PLACEMENT_3D('',#85603,#60193,#60194) ;
#51373 = AXIS2_PLACEMENT_3D('',#85604,#60195,#60196) ;
#51374 = AXIS2_PLACEMENT_3D('',#85605,#60197,#60198) ;
#51375 = AXIS2_PLACEMENT_3D('',#85606,#60199,#60200) ;
#51376 = AXIS2_PLACEMENT_3D('',#85609,#60201,#60202) ;
#51377 = AXIS2_PLACEMENT_3D('',#85610,#60203,#60204) ;
#51378 = AXIS2_PLACEMENT_3D('',#85611,#60205,#60206) ;
#51379 = AXIS2_PLACEMENT_3D('',#85612,#60207,#60208) ;
#51380 = AXIS2_PLACEMENT_3D('',#85614,#60210,#60211) ;
#51381 = AXIS2_PLACEMENT_3D('',#85615,#60212,#60213) ;
#51382 = AXIS2_PLACEMENT_3D('',#85617,#60215,#60216) ;
#51383 = AXIS2_PLACEMENT_3D('',#85620,#60219,#60220) ;
#51384 = AXIS2_PLACEMENT_3D('',#85622,#60222,#60223) ;
#51385 = AXIS2_PLACEMENT_3D('',#85625,#60226,#60227) ;
#51386 = AXIS2_PLACEMENT_3D('',#85627,#60229,#60230) ;
#51387 = AXIS2_PLACEMENT_3D('',#85630,#60233,#60234) ;
#51388 = AXIS2_PLACEMENT_3D('',#85632,#60236,#60237) ;
#51389 = AXIS2_PLACEMENT_3D('',#85635,#60240,#60241) ;
#51390 = AXIS2_PLACEMENT_3D('',#85637,#60243,#60244) ;
#51391 = AXIS2_PLACEMENT_3D('',#85638,#60245,#60246) ;
#51392 = AXIS2_PLACEMENT_3D('',#85639,#60247,#60248) ;
#51393 = AXIS2_PLACEMENT_3D('',#85640,#60249,#60250) ;
#51394 = AXIS2_PLACEMENT_3D('',#85641,#60251,#60252) ;
#51395 = AXIS2_PLACEMENT_3D('',#85642,#60253,#60254) ;
#51396 = AXIS2_PLACEMENT_3D('',#85644,#60256,#60257) ;
#51397 = AXIS2_PLACEMENT_3D('',#85645,#60258,#60259) ;
#51398 = AXIS2_PLACEMENT_3D('',#85647,#60261,#60262) ;
#51399 = AXIS2_PLACEMENT_3D('',#85648,#60263,#60264) ;
#51400 = AXIS2_PLACEMENT_3D('',#85650,#60265,#60266) ;
#51401 = AXIS2_PLACEMENT_3D('',#85652,#60267,#60268) ;
#51402 = AXIS2_PLACEMENT_3D('',#85653,#60269,#60270) ;
#51403 = AXIS2_PLACEMENT_3D('',#85654,#60271,#60272) ;
#51404 = AXIS2_PLACEMENT_3D('',#85657,#60273,#60274) ;
#51405 = AXIS2_PLACEMENT_3D('',#85658,#60275,#60276) ;
#51406 = AXIS2_PLACEMENT_3D('',#85659,#60277,#60278) ;
#51407 = AXIS2_PLACEMENT_3D('',#85660,#60279,#60280) ;
#51408 = AXIS2_PLACEMENT_3D('',#85662,#60281,#60282) ;
#51409 = AXIS2_PLACEMENT_3D('',#85664,#60283,#60284) ;
#51410 = AXIS2_PLACEMENT_3D('',#85665,#60285,#60286) ;
#51411 = AXIS2_PLACEMENT_3D('',#85666,#60287,#60288) ;
#51412 = AXIS2_PLACEMENT_3D('',#85669,#60289,#60290) ;
#51413 = AXIS2_PLACEMENT_3D('',#85670,#60291,#60292) ;
#51414 = AXIS2_PLACEMENT_3D('',#85671,#60293,#60294) ;
#51415 = AXIS2_PLACEMENT_3D('',#85672,#60295,#60296) ;
#51416 = AXIS2_PLACEMENT_3D('',#85674,#60297,#60298) ;
#51417 = AXIS2_PLACEMENT_3D('',#85676,#60299,#60300) ;
#51418 = AXIS2_PLACEMENT_3D('',#85677,#60301,#60302) ;
#51419 = AXIS2_PLACEMENT_3D('',#85678,#60303,#60304) ;
#51420 = AXIS2_PLACEMENT_3D('',#85681,#60305,#60306) ;
#51421 = AXIS2_PLACEMENT_3D('',#85682,#60307,#60308) ;
#51422 = AXIS2_PLACEMENT_3D('',#85683,#60309,#60310) ;
#51423 = AXIS2_PLACEMENT_3D('',#85684,#60311,#60312) ;
#51424 = AXIS2_PLACEMENT_3D('',#85686,#60313,#60314) ;
#51425 = AXIS2_PLACEMENT_3D('',#85688,#60315,#60316) ;
#51426 = AXIS2_PLACEMENT_3D('',#85689,#60317,#60318) ;
#51427 = AXIS2_PLACEMENT_3D('',#85690,#60319,#60320) ;
#51428 = AXIS2_PLACEMENT_3D('',#85692,#60322,#60323) ;
#51429 = AXIS2_PLACEMENT_3D('',#85695,#60324,#60325) ;
#51430 = AXIS2_PLACEMENT_3D('',#85696,#60326,#60327) ;
#51431 = AXIS2_PLACEMENT_3D('',#85697,#60328,#60329) ;
#51432 = AXIS2_PLACEMENT_3D('',#85698,#60330,#60331) ;
#51433 = AXIS2_PLACEMENT_3D('',#85700,#60333,#60334) ;
#51434 = AXIS2_PLACEMENT_3D('',#85702,#60336,#60337) ;
#51435 = AXIS2_PLACEMENT_3D('',#85705,#60340,#60341) ;
#51436 = AXIS2_PLACEMENT_3D('',#85707,#60343,#60344) ;
#51437 = AXIS2_PLACEMENT_3D('',#85709,#60346,#60347) ;
#51438 = AXIS2_PLACEMENT_3D('',#85712,#60350,#60351) ;
#51439 = AXIS2_PLACEMENT_3D('',#85715,#60354,#60355) ;
#51440 = AXIS2_PLACEMENT_3D('',#85717,#60357,#60358) ;
#51441 = AXIS2_PLACEMENT_3D('',#85719,#60360,#60361) ;
#51442 = AXIS2_PLACEMENT_3D('',#85721,#60363,#60364) ;
#51443 = AXIS2_PLACEMENT_3D('',#85724,#60367,#60368) ;
#51444 = AXIS2_PLACEMENT_3D('',#85725,#60369,#60370) ;
#51445 = AXIS2_PLACEMENT_3D('',#85726,#60371,#60372) ;
#51446 = AXIS2_PLACEMENT_3D('',#85727,#60373,#60374) ;
#51447 = AXIS2_PLACEMENT_3D('',#85728,#60375,#60376) ;
#51448 = AXIS2_PLACEMENT_3D('',#85730,#60377,#60378) ;
#51449 = AXIS2_PLACEMENT_3D('',#85731,#60379,#60380) ;
#51450 = AXIS2_PLACEMENT_3D('',#85732,#60381,#60382) ;
#51451 = AXIS2_PLACEMENT_3D('',#85736,#60384,#60385) ;
#51452 = AXIS2_PLACEMENT_3D('',#85737,#60386,#60387) ;
#51453 = AXIS2_PLACEMENT_3D('',#85738,#60388,#60389) ;
#51454 = AXIS2_PLACEMENT_3D('',#85739,#60390,#60391) ;
#51455 = AXIS2_PLACEMENT_3D('',#85740,#60392,#60393) ;
#51456 = AXIS2_PLACEMENT_3D('',#85743,#60394,#60395) ;
#51457 = AXIS2_PLACEMENT_3D('',#85747,#60397,#60398) ;
#51458 = AXIS2_PLACEMENT_3D('',#85749,#60400,#60401) ;
#51459 = AXIS2_PLACEMENT_3D('',#85750,#60402,#60403) ;
#51460 = AXIS2_PLACEMENT_3D('',#85751,#60404,#60405) ;
#51461 = AXIS2_PLACEMENT_3D('',#85752,#60406,#60407) ;
#51462 = AXIS2_PLACEMENT_3D('',#85753,#60408,#60409) ;
#51463 = AXIS2_PLACEMENT_3D('',#85754,#60410,#60411) ;
#51464 = AXIS2_PLACEMENT_3D('',#85755,#60412,#60413) ;
#51465 = AXIS2_PLACEMENT_3D('',#85759,#60416,#60417) ;
#51466 = AXIS2_PLACEMENT_3D('',#85763,#60419,#60420) ;
#51467 = AXIS2_PLACEMENT_3D('',#85767,#60423,#60424) ;
#51468 = AXIS2_PLACEMENT_3D('',#85771,#60427,#60428) ;
#51469 = AXIS2_PLACEMENT_3D('',#85773,#60429,#60430) ;
#51470 = AXIS2_PLACEMENT_3D('',#85775,#60432,#60433) ;
#51471 = AXIS2_PLACEMENT_3D('',#85777,#60434,#60435) ;
#51472 = AXIS2_PLACEMENT_3D('',#85778,#60436,#60437) ;
#51473 = AXIS2_PLACEMENT_3D('',#85779,#60438,#60439) ;
#51474 = AXIS2_PLACEMENT_3D('',#85780,#60440,#60441) ;
#51475 = AXIS2_PLACEMENT_3D('',#85781,#60442,#60443) ;
#51476 = AXIS2_PLACEMENT_3D('',#85782,#60444,#60445) ;
#51477 = AXIS2_PLACEMENT_3D('',#85783,#60446,#60447) ;
#51478 = AXIS2_PLACEMENT_3D('',#85784,#60448,#60449) ;
#51479 = AXIS2_PLACEMENT_3D('',#85785,#60450,#60451) ;
#51480 = AXIS2_PLACEMENT_3D('',#85786,#60452,#60453) ;
#51481 = AXIS2_PLACEMENT_3D('',#85787,#60454,#60455) ;
#51482 = AXIS2_PLACEMENT_3D('',#85788,#60456,#60457) ;
#51483 = AXIS2_PLACEMENT_3D('',#85789,#60458,#60459) ;
#51484 = AXIS2_PLACEMENT_3D('',#85790,#60460,#60461) ;
#51485 = AXIS2_PLACEMENT_3D('',#85791,#60462,#60463) ;
#51486 = AXIS2_PLACEMENT_3D('',#85792,#60464,#60465) ;
#51487 = AXIS2_PLACEMENT_3D('',#85793,#60466,#60467) ;
#51488 = AXIS2_PLACEMENT_3D('',#85794,#60468,#60469) ;
#51489 = AXIS2_PLACEMENT_3D('',#85795,#60470,#60471) ;
#51490 = AXIS2_PLACEMENT_3D('',#85796,#60472,#60473) ;
#51491 = AXIS2_PLACEMENT_3D('',#85797,#60474,#60475) ;
#51492 = AXIS2_PLACEMENT_3D('',#85798,#60476,#60477) ;
#51493 = AXIS2_PLACEMENT_3D('',#85799,#60478,#60479) ;
#51494 = AXIS2_PLACEMENT_3D('',#85800,#60480,#60481) ;
#51495 = AXIS2_PLACEMENT_3D('',#85801,#60482,#60483) ;
#51496 = AXIS2_PLACEMENT_3D('',#85802,#60484,#60485) ;
#51497 = AXIS2_PLACEMENT_3D('',#85803,#60486,#60487) ;
#51498 = AXIS2_PLACEMENT_3D('',#85804,#60488,#60489) ;
#51499 = AXIS2_PLACEMENT_3D('',#85805,#60490,#60491) ;
#51500 = AXIS2_PLACEMENT_3D('',#85807,#60493,#60494) ;
#51501 = AXIS2_PLACEMENT_3D('',#85809,#60495,#60496) ;
#51502 = AXIS2_PLACEMENT_3D('',#85811,#60497,#60498) ;
#51503 = AXIS2_PLACEMENT_3D('',#85812,#60499,#60500) ;
#51504 = AXIS2_PLACEMENT_3D('',#85813,#60501,#60502) ;
#51505 = AXIS2_PLACEMENT_3D('',#85815,#60504,#60505) ;
#51506 = AXIS2_PLACEMENT_3D('',#85817,#60506,#60507) ;
#51507 = AXIS2_PLACEMENT_3D('',#85819,#60508,#60509) ;
#51508 = AXIS2_PLACEMENT_3D('',#85820,#60510,#60511) ;
#51509 = AXIS2_PLACEMENT_3D('',#85821,#60512,#60513) ;
#51510 = AXIS2_PLACEMENT_3D('',#85823,#60515,#60516) ;
#51511 = AXIS2_PLACEMENT_3D('',#85824,#60517,#60518) ;
#51512 = AXIS2_PLACEMENT_3D('',#85825,#60519,#60520) ;
#51513 = AXIS2_PLACEMENT_3D('',#85826,#60521,#60522) ;
#51514 = AXIS2_PLACEMENT_3D('',#85827,#60523,#60524) ;
#51515 = AXIS2_PLACEMENT_3D('',#85828,#60525,#60526) ;
#51516 = AXIS2_PLACEMENT_3D('',#85829,#60527,#60528) ;
#51517 = AXIS2_PLACEMENT_3D('',#85830,#60529,#60530) ;
#51518 = AXIS2_PLACEMENT_3D('',#85831,#60531,#60532) ;
#51519 = AXIS2_PLACEMENT_3D('',#85832,#60533,#60534) ;
#51520 = AXIS2_PLACEMENT_3D('',#85833,#60535,#60536) ;
#51521 = AXIS2_PLACEMENT_3D('',#85834,#60537,#60538) ;
#51522 = AXIS2_PLACEMENT_3D('',#85835,#60539,#60540) ;
#51523 = AXIS2_PLACEMENT_3D('',#85836,#60541,#60542) ;
#51524 = AXIS2_PLACEMENT_3D('',#85837,#60543,#60544) ;
#51525 = AXIS2_PLACEMENT_3D('',#85838,#60545,#60546) ;
#51526 = AXIS2_PLACEMENT_3D('',#85839,#60547,#60548) ;
#51527 = AXIS2_PLACEMENT_3D('',#85840,#60549,#60550) ;
#51528 = AXIS2_PLACEMENT_3D('',#85841,#60551,#60552) ;
#51529 = AXIS2_PLACEMENT_3D('',#85842,#60553,#60554) ;
#51530 = AXIS2_PLACEMENT_3D('',#85843,#60555,#60556) ;
#51531 = AXIS2_PLACEMENT_3D('',#85844,#60557,#60558) ;
#51532 = AXIS2_PLACEMENT_3D('',#85845,#60559,#60560) ;
#51533 = AXIS2_PLACEMENT_3D('',#85846,#60561,#60562) ;
#51534 = AXIS2_PLACEMENT_3D('',#85847,#60563,#60564) ;
#51535 = AXIS2_PLACEMENT_3D('',#85848,#60565,#60566) ;
#51536 = AXIS2_PLACEMENT_3D('',#85849,#60567,#60568) ;
#51537 = AXIS2_PLACEMENT_3D('',#85850,#60569,#60570) ;
#51538 = AXIS2_PLACEMENT_3D('',#85851,#60571,#60572) ;
#51539 = AXIS2_PLACEMENT_3D('',#85852,#60573,#60574) ;
#51540 = AXIS2_PLACEMENT_3D('',#85853,#60575,#60576) ;
#51541 = AXIS2_PLACEMENT_3D('',#85854,#60577,#60578) ;
#51542 = AXIS2_PLACEMENT_3D('',#85855,#60579,#60580) ;
#51543 = AXIS2_PLACEMENT_3D('',#85856,#60581,#60582) ;
#51544 = AXIS2_PLACEMENT_3D('',#85857,#60583,#60584) ;
#51545 = AXIS2_PLACEMENT_3D('',#85858,#60585,#60586) ;
#51546 = AXIS2_PLACEMENT_3D('',#85859,#60587,#60588) ;
#51547 = AXIS2_PLACEMENT_3D('',#85860,#60589,#60590) ;
#51548 = AXIS2_PLACEMENT_3D('',#85861,#60591,#60592) ;
#51549 = AXIS2_PLACEMENT_3D('',#85862,#60593,#60594) ;
#51550 = AXIS2_PLACEMENT_3D('',#85863,#60595,#60596) ;
#51551 = AXIS2_PLACEMENT_3D('',#85864,#60597,#60598) ;
#51552 = AXIS2_PLACEMENT_3D('',#85865,#60599,#60600) ;
#51553 = AXIS2_PLACEMENT_3D('',#85866,#60601,#60602) ;
#51554 = AXIS2_PLACEMENT_3D('',#85867,#60603,#60604) ;
#51555 = AXIS2_PLACEMENT_3D('',#85868,#60605,#60606) ;
#51556 = AXIS2_PLACEMENT_3D('',#85869,#60607,#60608) ;
#51557 = AXIS2_PLACEMENT_3D('',#85870,#60609,#60610) ;
#51558 = AXIS2_PLACEMENT_3D('',#85871,#60611,#60612) ;
#51559 = AXIS2_PLACEMENT_3D('',#85872,#60613,#60614) ;
#51560 = AXIS2_PLACEMENT_3D('',#85874,#60615,#60616) ;
#51561 = AXIS2_PLACEMENT_3D('',#85875,#60617,#60618) ;
#51562 = AXIS2_PLACEMENT_3D('',#85876,#60619,#60620) ;
#51563 = AXIS2_PLACEMENT_3D('',#85878,#60621,#60622) ;
#51564 = AXIS2_PLACEMENT_3D('',#85880,#60624,#60625) ;
#51565 = AXIS2_PLACEMENT_3D('',#85882,#60626,#60627) ;
#51566 = AXIS2_PLACEMENT_3D('',#85883,#60628,#60629) ;
#51567 = AXIS2_PLACEMENT_3D('',#85884,#60630,#60631) ;
#51568 = AXIS2_PLACEMENT_3D('',#85886,#60633,#60634) ;
#51569 = AXIS2_PLACEMENT_3D('',#85888,#60635,#60636) ;
#51570 = AXIS2_PLACEMENT_3D('',#85889,#60637,#60638) ;
#51571 = AXIS2_PLACEMENT_3D('',#85890,#60639,#60640) ;
#51572 = AXIS2_PLACEMENT_3D('',#85892,#60641,#60642) ;
#51573 = AXIS2_PLACEMENT_3D('',#85893,#60643,#60644) ;
#51574 = AXIS2_PLACEMENT_3D('',#85896,#60645,#60646) ;
#51575 = AXIS2_PLACEMENT_3D('',#85897,#60647,#60648) ;
#51576 = AXIS2_PLACEMENT_3D('',#85898,#60649,#60650) ;
#51577 = AXIS2_PLACEMENT_3D('',#85899,#60651,#60652) ;
#51578 = AXIS2_PLACEMENT_3D('',#85901,#60653,#60654) ;
#51579 = AXIS2_PLACEMENT_3D('',#85903,#60656,#60657) ;
#51580 = AXIS2_PLACEMENT_3D('',#85905,#60658,#60659) ;
#51581 = AXIS2_PLACEMENT_3D('',#85907,#60660,#60661) ;
#51582 = AXIS2_PLACEMENT_3D('',#85908,#60662,#60663) ;
#51583 = AXIS2_PLACEMENT_3D('',#85909,#60664,#60665) ;
#51584 = AXIS2_PLACEMENT_3D('',#85911,#60666,#60667) ;
#51585 = AXIS2_PLACEMENT_3D('',#85913,#60668,#60669) ;
#51586 = AXIS2_PLACEMENT_3D('',#85915,#60670,#60671) ;
#51587 = AXIS2_PLACEMENT_3D('',#85916,#60672,#60673) ;
#51588 = AXIS2_PLACEMENT_3D('',#85917,#60674,#60675) ;
#51589 = AXIS2_PLACEMENT_3D('',#85921,#60677,#60678) ;
#51590 = AXIS2_PLACEMENT_3D('',#85922,#60679,#60680) ;
#51591 = AXIS2_PLACEMENT_3D('',#85923,#60681,#60682) ;
#51592 = AXIS2_PLACEMENT_3D('',#85925,#60683,#60684) ;
#51593 = AXIS2_PLACEMENT_3D('',#85926,#60685,#60686) ;
#51594 = AXIS2_PLACEMENT_3D('',#85927,#60687,#60688) ;
#51595 = AXIS2_PLACEMENT_3D('',#85929,#60689,#60690) ;
#51596 = AXIS2_PLACEMENT_3D('',#85930,#60691,#60692) ;
#51597 = AXIS2_PLACEMENT_3D('',#85932,#60693,#60694) ;
#51598 = AXIS2_PLACEMENT_3D('',#85933,#60695,#60696) ;
#51599 = AXIS2_PLACEMENT_3D('',#85934,#60697,#60698) ;
#51600 = AXIS2_PLACEMENT_3D('',#85936,#60699,#60700) ;
#51601 = AXIS2_PLACEMENT_3D('',#85938,#60702,#60703) ;
#51602 = AXIS2_PLACEMENT_3D('',#85940,#60704,#60705) ;
#51603 = AXIS2_PLACEMENT_3D('',#85942,#60706,#60707) ;
#51604 = AXIS2_PLACEMENT_3D('',#85944,#60708,#60709) ;
#51605 = AXIS2_PLACEMENT_3D('',#85945,#60710,#60711) ;
#51606 = AXIS2_PLACEMENT_3D('',#85946,#60712,#60713) ;
#51607 = AXIS2_PLACEMENT_3D('',#85950,#60715,#60716) ;
#51608 = AXIS2_PLACEMENT_3D('',#85951,#60717,#60718) ;
#51609 = AXIS2_PLACEMENT_3D('',#85952,#60719,#60720) ;
#51610 = AXIS2_PLACEMENT_3D('',#85954,#60721,#60722) ;
#51611 = AXIS2_PLACEMENT_3D('',#85955,#60723,#60724) ;
#51612 = AXIS2_PLACEMENT_3D('',#85956,#60725,#60726) ;
#51613 = AXIS2_PLACEMENT_3D('',#85958,#60727,#60728) ;
#51614 = AXIS2_PLACEMENT_3D('',#85959,#60729,#60730) ;
#51615 = AXIS2_PLACEMENT_3D('',#85960,#60731,#60732) ;
#51616 = AXIS2_PLACEMENT_3D('',#85961,#60733,#60734) ;
#51617 = AXIS2_PLACEMENT_3D('',#85962,#60735,#60736) ;
#51618 = AXIS2_PLACEMENT_3D('',#85963,#60737,#60738) ;
#51619 = AXIS2_PLACEMENT_3D('',#85964,#60739,#60740) ;
#51620 = AXIS2_PLACEMENT_3D('',#85965,#60741,#60742) ;
#51621 = AXIS2_PLACEMENT_3D('',#85966,#60743,#60744) ;
#51622 = AXIS2_PLACEMENT_3D('',#85967,#60745,#60746) ;
#51623 = AXIS2_PLACEMENT_3D('',#85968,#60747,#60748) ;
#51624 = AXIS2_PLACEMENT_3D('',#85971,#60751,#60752) ;
#51625 = AXIS2_PLACEMENT_3D('',#85973,#60754,#60755) ;
#51626 = AXIS2_PLACEMENT_3D('',#85974,#60756,#60757) ;
#51627 = AXIS2_PLACEMENT_3D('',#85975,#60758,#60759) ;
#51628 = AXIS2_PLACEMENT_3D('',#85976,#60760,#60761) ;
#51629 = AXIS2_PLACEMENT_3D('',#85977,#60762,#60763) ;
#51630 = AXIS2_PLACEMENT_3D('',#85978,#60764,#60765) ;
#51631 = AXIS2_PLACEMENT_3D('',#86009,#60766,#60767) ;
#51632 = AXIS2_PLACEMENT_3D('',#86011,#60768,#60769) ;
#51633 = AXIS2_PLACEMENT_3D('',#86012,#60770,#60771) ;
#51634 = AXIS2_PLACEMENT_3D('',#86040,#60772,#60773) ;
#51635 = AXIS2_PLACEMENT_3D('',#86041,#60774,#60775) ;
#51636 = AXIS2_PLACEMENT_3D('',#86043,#60776,#60777) ;
#51637 = AXIS2_PLACEMENT_3D('',#86044,#60778,#60779) ;
#51638 = AXIS2_PLACEMENT_3D('',#86045,#60780,#60781) ;
#51639 = AXIS2_PLACEMENT_3D('',#86072,#60782,#60783) ;
#51640 = AXIS2_PLACEMENT_3D('',#86073,#60784,#60785) ;
#51641 = AXIS2_PLACEMENT_3D('',#86075,#60786,#60787) ;
#51642 = AXIS2_PLACEMENT_3D('',#86077,#60788,#60789) ;
#51643 = AXIS2_PLACEMENT_3D('',#86078,#60790,#60791) ;
#51644 = AXIS2_PLACEMENT_3D('',#86106,#60792,#60793) ;
#51645 = AXIS2_PLACEMENT_3D('',#86107,#60794,#60795) ;
#51646 = AXIS2_PLACEMENT_3D('',#86108,#60796,#60797) ;
#51647 = AXIS2_PLACEMENT_3D('',#86109,#60798,#60799) ;
#51648 = AXIS2_PLACEMENT_3D('',#86112,#60801,#60802) ;
#51649 = AXIS2_PLACEMENT_3D('',#86143,#60803,#60804) ;
#51650 = AXIS2_PLACEMENT_3D('',#86144,#60805,#60806) ;
#51651 = AXIS2_PLACEMENT_3D('',#86145,#60807,#60808) ;
#51652 = AXIS2_PLACEMENT_3D('',#86146,#60809,#60810) ;
#51653 = AXIS2_PLACEMENT_3D('',#86173,#60811,#60812) ;
#51654 = AXIS2_PLACEMENT_3D('',#86174,#60813,#60814) ;
#51655 = AXIS2_PLACEMENT_3D('',#86175,#60815,#60816) ;
#51656 = AXIS2_PLACEMENT_3D('',#86177,#60818,#60819) ;
#51657 = AXIS2_PLACEMENT_3D('',#86178,#60820,#60821) ;
#51658 = AXIS2_PLACEMENT_3D('',#86181,#60823,#60824) ;
#51659 = AXIS2_PLACEMENT_3D('',#86212,#60825,#60826) ;
#51660 = AXIS2_PLACEMENT_3D('',#86213,#60827,#60828) ;
#51661 = AXIS2_PLACEMENT_3D('',#86214,#60829,#60830) ;
#51662 = AXIS2_PLACEMENT_3D('',#86215,#60831,#60832) ;
#51663 = AXIS2_PLACEMENT_3D('',#86242,#60833,#60834) ;
#51664 = AXIS2_PLACEMENT_3D('',#86243,#60835,#60836) ;
#51665 = AXIS2_PLACEMENT_3D('',#86244,#60837,#60838) ;
#51666 = AXIS2_PLACEMENT_3D('',#86246,#60840,#60841) ;
#51667 = AXIS2_PLACEMENT_3D('',#86247,#60842,#60843) ;
#51668 = AXIS2_PLACEMENT_3D('',#86249,#60844,#60845) ;
#51669 = AXIS2_PLACEMENT_3D('',#86251,#60847,#60848) ;
#51670 = AXIS2_PLACEMENT_3D('',#86254,#60850,#60851) ;
#51671 = AXIS2_PLACEMENT_3D('',#86255,#60852,#60853) ;
#51672 = AXIS2_PLACEMENT_3D('',#86257,#60855,#60856) ;
#51673 = AXIS2_PLACEMENT_3D('',#86258,#60857,#60858) ;
#51674 = AXIS2_PLACEMENT_3D('',#86259,#60859,#60860) ;
#51675 = AXIS2_PLACEMENT_3D('',#86262,#60862,#60863) ;
#51676 = AXIS2_PLACEMENT_3D('',#86263,#60864,#60865) ;
#51677 = AXIS2_PLACEMENT_3D('',#86265,#60867,#60868) ;
#51678 = AXIS2_PLACEMENT_3D('',#86266,#60869,#60870) ;
#51679 = AXIS2_PLACEMENT_3D('',#86267,#60871,#60872) ;
#51680 = AXIS2_PLACEMENT_3D('',#86270,#60874,#60875) ;
#51681 = AXIS2_PLACEMENT_3D('',#86271,#60876,#60877) ;
#51682 = AXIS2_PLACEMENT_3D('',#86273,#60879,#60880) ;
#51683 = AXIS2_PLACEMENT_3D('',#86274,#60881,#60882) ;
#51684 = AXIS2_PLACEMENT_3D('',#86275,#60883,#60884) ;
#51685 = AXIS2_PLACEMENT_3D('',#86279,#60887,#60888) ;
#51686 = AXIS2_PLACEMENT_3D('',#86281,#60890,#60891) ;
#51687 = AXIS2_PLACEMENT_3D('',#86282,#60892,#60893) ;
#51688 = AXIS2_PLACEMENT_3D('',#86285,#60896,#60897) ;
#51689 = AXIS2_PLACEMENT_3D('',#86286,#60898,#60899) ;
#51690 = AXIS2_PLACEMENT_3D('',#86287,#60900,#60901) ;
#51691 = AXIS2_PLACEMENT_3D('',#86290,#60904,#60905) ;
#51692 = AXIS2_PLACEMENT_3D('',#86291,#60906,#60907) ;
#51693 = AXIS2_PLACEMENT_3D('',#86292,#60908,#60909) ;
#51694 = AXIS2_PLACEMENT_3D('',#86294,#60911,#60912) ;
#51695 = AXIS2_PLACEMENT_3D('',#86295,#60913,#60914) ;
#51696 = AXIS2_PLACEMENT_3D('',#86296,#60915,#60916) ;
#51697 = AXIS2_PLACEMENT_3D('',#86297,#60917,#60918) ;
#51698 = AXIS2_PLACEMENT_3D('',#86298,#60919,#60920) ;
#51699 = AXIS2_PLACEMENT_3D('',#86299,#60921,#60922) ;
#51700 = AXIS2_PLACEMENT_3D('',#86300,#60923,#60924) ;
#51701 = AXIS2_PLACEMENT_3D('',#86301,#60925,#60926) ;
#51702 = AXIS2_PLACEMENT_3D('',#86307,#60927,#60928) ;
#51703 = AXIS2_PLACEMENT_3D('',#86314,#60930,#60931) ;
#51704 = AXIS2_PLACEMENT_3D('',#86396,#60933,#60934) ;
#51705 = AXIS2_PLACEMENT_3D('',#86422,#60935,#60936) ;
#51706 = AXIS2_PLACEMENT_3D('',#86453,#60937,#60938) ;
#51707 = AXIS2_PLACEMENT_3D('',#86539,#60939,#60940) ;
#51708 = AXIS2_PLACEMENT_3D('',#86541,#60942,#60943) ;
#51709 = AXIS2_PLACEMENT_3D('',#86542,#60944,#60945) ;
#51710 = AXIS2_PLACEMENT_3D('',#86543,#60946,#60947) ;
#51711 = AXIS2_PLACEMENT_3D('',#86548,#60949,#60950) ;
#51712 = AXIS2_PLACEMENT_3D('',#86551,#60952,#60953) ;
#51713 = AXIS2_PLACEMENT_3D('',#86552,#60954,#60955) ;
#51714 = AXIS2_PLACEMENT_3D('',#86556,#60957,#60958) ;
#51715 = AXIS2_PLACEMENT_3D('',#86558,#60960,#60961) ;
#51716 = AXIS2_PLACEMENT_3D('',#86562,#60963,#60964) ;
#51717 = AXIS2_PLACEMENT_3D('',#86564,#60966,#60967) ;
#51718 = AXIS2_PLACEMENT_3D('',#86567,#60968,#60969) ;
#51719 = AXIS2_PLACEMENT_3D('',#86569,#60970,#60971) ;
#51720 = AXIS2_PLACEMENT_3D('',#86570,#60972,#60973) ;
#51721 = AXIS2_PLACEMENT_3D('',#86571,#60974,#60975) ;
#51722 = AXIS2_PLACEMENT_3D('',#86574,#60976,#60977) ;
#51723 = AXIS2_PLACEMENT_3D('',#86577,#60980,#60981) ;
#51724 = AXIS2_PLACEMENT_3D('',#86580,#60982,#60983) ;
#51725 = AXIS2_PLACEMENT_3D('',#86583,#60986,#60987) ;
#51726 = AXIS2_PLACEMENT_3D('',#86586,#60990,#60991) ;
#51727 = AXIS2_PLACEMENT_3D('',#86592,#60995,#60996) ;
#51728 = AXIS2_PLACEMENT_3D('',#86597,#61000,#61001) ;
#51729 = AXIS2_PLACEMENT_3D('',#86601,#61004,#61005) ;
#51730 = AXIS2_PLACEMENT_3D('',#86605,#61008,#61009) ;
#51731 = AXIS2_PLACEMENT_3D('',#86607,#61011,#61012) ;
#51732 = AXIS2_PLACEMENT_3D('',#86609,#61014,#61015) ;
#51733 = AXIS2_PLACEMENT_3D('',#86610,#61016,#61017) ;
#51734 = AXIS2_PLACEMENT_3D('',#86611,#61018,#61019) ;
#51735 = AXIS2_PLACEMENT_3D('',#86612,#61020,#61021) ;
#51736 = AXIS2_PLACEMENT_3D('',#86628,#61023,#61024) ;
#51737 = AXIS2_PLACEMENT_3D('',#86630,#61026,#61027) ;
#51738 = AXIS2_PLACEMENT_3D('',#86632,#61028,#61029) ;
#51739 = AXIS2_PLACEMENT_3D('',#86636,#61031,#61032) ;
#51740 = AXIS2_PLACEMENT_3D('',#86638,#61034,#61035) ;
#51741 = AXIS2_PLACEMENT_3D('',#86653,#61037,#61038) ;
#51742 = AXIS2_PLACEMENT_3D('',#86655,#61040,#61041) ;
#51743 = AXIS2_PLACEMENT_3D('',#86656,#61042,#61043) ;
#51744 = AXIS2_PLACEMENT_3D('',#86657,#61044,#61045) ;
#51745 = AXIS2_PLACEMENT_3D('',#86658,#61046,#61047) ;
#51746 = AXIS2_PLACEMENT_3D('',#86659,#61048,#61049) ;
#51747 = AXIS2_PLACEMENT_3D('',#86663,#61051,#61052) ;
#51748 = AXIS2_PLACEMENT_3D('',#86675,#61058,#61059) ;
#51749 = AXIS2_PLACEMENT_3D('',#86679,#61061,#61062) ;
#51750 = AXIS2_PLACEMENT_3D('',#86683,#61064,#61065) ;
#51751 = AXIS2_PLACEMENT_3D('',#86687,#61067,#61068) ;
#51752 = AXIS2_PLACEMENT_3D('',#86706,#61078,#61079) ;
#51753 = AXIS2_PLACEMENT_3D('',#86711,#61081,#61082) ;
#51754 = AXIS2_PLACEMENT_3D('',#86714,#61084,#61085) ;
#51755 = AXIS2_PLACEMENT_3D('',#86923,#61102,#61103) ;
#51756 = AXIS2_PLACEMENT_3D('',#86926,#61105,#61106) ;
#51757 = AXIS2_PLACEMENT_3D('',#86927,#61107,#61108) ;
#51758 = AXIS2_PLACEMENT_3D('',#86931,#61111,#61112) ;
#51759 = AXIS2_PLACEMENT_3D('',#86934,#61114,#61115) ;
#51760 = AXIS2_PLACEMENT_3D('',#86935,#61116,#61117) ;
#51761 = AXIS2_PLACEMENT_3D('',#86937,#61118,#61119) ;
#51762 = AXIS2_PLACEMENT_3D('',#86957,#61129,#61130) ;
#51763 = AXIS2_PLACEMENT_3D('',#86961,#61132,#61133) ;
#51764 = AXIS2_PLACEMENT_3D('',#86965,#61135,#61136) ;
#51765 = AXIS2_PLACEMENT_3D('',#86969,#61138,#61139) ;
#51766 = AXIS2_PLACEMENT_3D('',#86980,#61145,#61146) ;
#51767 = AXIS2_PLACEMENT_3D('',#86983,#61147,#61148) ;
#51768 = AXIS2_PLACEMENT_3D('',#86987,#61150,#61151) ;
#51769 = AXIS2_PLACEMENT_3D('',#86997,#61157,#61158) ;
#51770 = AXIS2_PLACEMENT_3D('',#86999,#61159,#61160) ;
#51771 = AXIS2_PLACEMENT_3D('',#87002,#61162,#61163) ;
#51772 = AXIS2_PLACEMENT_3D('',#87003,#61164,#61165) ;
#51773 = AXIS2_PLACEMENT_3D('',#87005,#61166,#61167) ;
#51774 = AXIS2_PLACEMENT_3D('',#87007,#61168,#61169) ;
#51775 = AXIS2_PLACEMENT_3D('',#87009,#61171,#61172) ;
#51776 = AXIS2_PLACEMENT_3D('',#87012,#61175,#61176) ;
#51777 = AXIS2_PLACEMENT_3D('',#87014,#61177,#61178) ;
#51778 = AXIS2_PLACEMENT_3D('',#87016,#61179,#61180) ;
#51779 = AXIS2_PLACEMENT_3D('',#87017,#61181,#61182) ;
#51780 = AXIS2_PLACEMENT_3D('',#87018,#61183,#61184) ;
#51781 = AXIS2_PLACEMENT_3D('',#87020,#61185,#61186) ;
#51782 = AXIS2_PLACEMENT_3D('',#87022,#61187,#61188) ;
#51783 = AXIS2_PLACEMENT_3D('',#87023,#61189,#61190) ;
#51784 = AXIS2_PLACEMENT_3D('',#87024,#61191,#61192) ;
#51785 = AXIS2_PLACEMENT_3D('',#87027,#61195,#61196) ;
#51786 = AXIS2_PLACEMENT_3D('',#87033,#61200,#61201) ;
#51787 = AXIS2_PLACEMENT_3D('',#87034,#61202,#61203) ;
#51788 = AXIS2_PLACEMENT_3D('',#87035,#61204,#61205) ;
#51789 = AXIS2_PLACEMENT_3D('',#87038,#61207,#61208) ;
#51790 = AXIS2_PLACEMENT_3D('',#87039,#61209,#61210) ;
#51791 = AXIS2_PLACEMENT_3D('',#87041,#61211,#61212) ;
#51792 = AXIS2_PLACEMENT_3D('',#87043,#61213,#61214) ;
#51793 = AXIS2_PLACEMENT_3D('',#87044,#61215,#61216) ;
#51794 = AXIS2_PLACEMENT_3D('',#87045,#61217,#61218) ;
#51795 = AXIS2_PLACEMENT_3D('',#87047,#61219,#61220) ;
#51796 = AXIS2_PLACEMENT_3D('',#87048,#61221,#61222) ;
#51797 = AXIS2_PLACEMENT_3D('',#87049,#61223,#61224) ;
#51798 = AXIS2_PLACEMENT_3D('',#87052,#61227,#61228) ;
#51799 = AXIS2_PLACEMENT_3D('',#87054,#61230,#61231) ;
#51800 = AXIS2_PLACEMENT_3D('',#87055,#61232,#61233) ;
#51801 = AXIS2_PLACEMENT_3D('',#87057,#61234,#61235) ;
#51802 = AXIS2_PLACEMENT_3D('',#87058,#61236,#61237) ;
#51803 = AXIS2_PLACEMENT_3D('',#87059,#61238,#61239) ;
#51804 = AXIS2_PLACEMENT_3D('',#87060,#61240,#61241) ;
#51805 = AXIS2_PLACEMENT_3D('',#87062,#61242,#61243) ;
#51806 = AXIS2_PLACEMENT_3D('',#87063,#61244,#61245) ;
#51807 = AXIS2_PLACEMENT_3D('',#87064,#61246,#61247) ;
#51808 = AXIS2_PLACEMENT_3D('',#87066,#61249,#61250) ;
#51809 = AXIS2_PLACEMENT_3D('',#87069,#61252,#61253) ;
#51810 = AXIS2_PLACEMENT_3D('',#87070,#61254,#61255) ;
#51811 = AXIS2_PLACEMENT_3D('',#87074,#61258,#61259) ;
#51812 = AXIS2_PLACEMENT_3D('',#87075,#61260,#61261) ;
#51813 = AXIS2_PLACEMENT_3D('',#87103,#61262,#61263) ;
#51814 = AXIS2_PLACEMENT_3D('',#87105,#61264,#61265) ;
#51815 = AXIS2_PLACEMENT_3D('',#87106,#61266,#61267) ;
#51816 = AXIS2_PLACEMENT_3D('',#87108,#61268,#61269) ;
#51817 = AXIS2_PLACEMENT_3D('',#87109,#61270,#61271) ;
#51818 = AXIS2_PLACEMENT_3D('',#87110,#61272,#61273) ;
#51819 = AXIS2_PLACEMENT_3D('',#87114,#61275,#61276) ;
#51820 = AXIS2_PLACEMENT_3D('',#87142,#61278,#61279) ;
#51821 = AXIS2_PLACEMENT_3D('',#87143,#61280,#61281) ;
#51822 = AXIS2_PLACEMENT_3D('',#87145,#61282,#61283) ;
#51823 = AXIS2_PLACEMENT_3D('',#87146,#61284,#61285) ;
#51824 = AXIS2_PLACEMENT_3D('',#87147,#61286,#61287) ;
#51825 = AXIS2_PLACEMENT_3D('',#87153,#61291,#61292) ;
#51826 = AXIS2_PLACEMENT_3D('',#87154,#61293,#61294) ;
#51827 = AXIS2_PLACEMENT_3D('',#87155,#61295,#61296) ;
#51828 = AXIS2_PLACEMENT_3D('',#87158,#61298,#61299) ;
#51829 = AXIS2_PLACEMENT_3D('',#87169,#61300,#61301) ;
#51830 = AXIS2_PLACEMENT_3D('',#87170,#61302,#61303) ;
#51831 = AXIS2_PLACEMENT_3D('',#87180,#61304,#61305) ;
#51832 = AXIS2_PLACEMENT_3D('',#87181,#61306,#61307) ;
#51833 = AXIS2_PLACEMENT_3D('',#87183,#61309,#61310) ;
#51834 = AXIS2_PLACEMENT_3D('',#87185,#61312,#61313) ;
#51835 = AXIS2_PLACEMENT_3D('',#87186,#61314,#61315) ;
#51836 = AXIS2_PLACEMENT_3D('',#87188,#61316,#61317) ;
#51837 = AXIS2_PLACEMENT_3D('',#87190,#61318,#61319) ;
#51838 = AXIS2_PLACEMENT_3D('',#87192,#61321,#61322) ;
#51839 = AXIS2_PLACEMENT_3D('',#87194,#61323,#61324) ;
#51840 = AXIS2_PLACEMENT_3D('',#87195,#61325,#61326) ;
#51841 = AXIS2_PLACEMENT_3D('',#87196,#61327,#61328) ;
#51842 = AXIS2_PLACEMENT_3D('',#87198,#61329,#61330) ;
#51843 = AXIS2_PLACEMENT_3D('',#87200,#61332,#61333) ;
#51844 = AXIS2_PLACEMENT_3D('',#87201,#61334,#61335) ;
#51845 = AXIS2_PLACEMENT_3D('',#87202,#61336,#61337) ;
#51846 = AXIS2_PLACEMENT_3D('',#87205,#61340,#61341) ;
#51847 = AXIS2_PLACEMENT_3D('',#87207,#61343,#61344) ;
#51848 = AXIS2_PLACEMENT_3D('',#87216,#61345,#61346) ;
#51849 = AXIS2_PLACEMENT_3D('',#87221,#61347,#61348) ;
#51850 = AXIS2_PLACEMENT_3D('',#87230,#61351,#61352) ;
#51851 = AXIS2_PLACEMENT_3D('',#87231,#61353,#61354) ;
#51852 = AXIS2_PLACEMENT_3D('',#87232,#61355,#61356) ;
#51853 = AXIS2_PLACEMENT_3D('',#87234,#61358,#61359) ;
#51854 = AXIS2_PLACEMENT_3D('',#87241,#61360,#61361) ;
#51855 = AXIS2_PLACEMENT_3D('',#87243,#61363,#61364) ;
#51856 = AXIS2_PLACEMENT_3D('',#87246,#61366,#61367) ;
#51857 = AXIS2_PLACEMENT_3D('',#87247,#61368,#61369) ;
#51858 = AXIS2_PLACEMENT_3D('',#87248,#61370,#61371) ;
#51859 = AXIS2_PLACEMENT_3D('',#87249,#61372,#61373) ;
#51860 = AXIS2_PLACEMENT_3D('',#87250,#61374,#61375) ;
#51861 = AXIS2_PLACEMENT_3D('',#87252,#61377,#61378) ;
#51862 = AXIS2_PLACEMENT_3D('',#87255,#61380,#61381) ;
#51863 = AXIS2_PLACEMENT_3D('',#87256,#61382,#61383) ;
#51864 = AXIS2_PLACEMENT_3D('',#87258,#61385,#61386) ;
#51865 = AXIS2_PLACEMENT_3D('',#87260,#61388,#61389) ;
#51866 = AXIS2_PLACEMENT_3D('',#87261,#61390,#61391) ;
#51867 = AXIS2_PLACEMENT_3D('',#87262,#61392,#61393) ;
#51868 = AXIS2_PLACEMENT_3D('',#87265,#61394,#61395) ;
#51869 = AXIS2_PLACEMENT_3D('',#87266,#61396,#61397) ;
#51870 = AXIS2_PLACEMENT_3D('',#87267,#61398,#61399) ;
#51871 = AXIS2_PLACEMENT_3D('',#87268,#61400,#61401) ;
#51872 = AXIS2_PLACEMENT_3D('',#87271,#61402,#61403) ;
#51873 = AXIS2_PLACEMENT_3D('',#87274,#61406,#61407) ;
#51874 = AXIS2_PLACEMENT_3D('',#87275,#61408,#61409) ;
#51875 = AXIS2_PLACEMENT_3D('',#87276,#61410,#61411) ;
#51876 = AXIS2_PLACEMENT_3D('',#87277,#61412,#61413) ;
#51877 = AXIS2_PLACEMENT_3D('',#87278,#61414,#61415) ;
#51878 = AXIS2_PLACEMENT_3D('',#87281,#61416,#61417) ;
#51879 = AXIS2_PLACEMENT_3D('',#87282,#61418,#61419) ;
#51880 = AXIS2_PLACEMENT_3D('',#87283,#61420,#61421) ;
#51881 = AXIS2_PLACEMENT_3D('',#87284,#61422,#61423) ;
#51882 = AXIS2_PLACEMENT_3D('',#87287,#61424,#61425) ;
#51883 = AXIS2_PLACEMENT_3D('',#87290,#61428,#61429) ;
#51884 = AXIS2_PLACEMENT_3D('',#87291,#61430,#61431) ;
#51885 = AXIS2_PLACEMENT_3D('',#87292,#61432,#61433) ;
#51886 = AXIS2_PLACEMENT_3D('',#87293,#61434,#61435) ;
#51887 = AXIS2_PLACEMENT_3D('',#87294,#61436,#61437) ;
#51888 = AXIS2_PLACEMENT_3D('',#87297,#61438,#61439) ;
#51889 = AXIS2_PLACEMENT_3D('',#87298,#61440,#61441) ;
#51890 = AXIS2_PLACEMENT_3D('',#87299,#61442,#61443) ;
#51891 = AXIS2_PLACEMENT_3D('',#87300,#61444,#61445) ;
#51892 = AXIS2_PLACEMENT_3D('',#87303,#61446,#61447) ;
#51893 = AXIS2_PLACEMENT_3D('',#87306,#61450,#61451) ;
#51894 = AXIS2_PLACEMENT_3D('',#87307,#61452,#61453) ;
#51895 = AXIS2_PLACEMENT_3D('',#87308,#61454,#61455) ;
#51896 = AXIS2_PLACEMENT_3D('',#87309,#61456,#61457) ;
#51897 = AXIS2_PLACEMENT_3D('',#87310,#61458,#61459) ;
#51898 = AXIS2_PLACEMENT_3D('',#87313,#61460,#61461) ;
#51899 = AXIS2_PLACEMENT_3D('',#87314,#61462,#61463) ;
#51900 = AXIS2_PLACEMENT_3D('',#87315,#61464,#61465) ;
#51901 = AXIS2_PLACEMENT_3D('',#87316,#61466,#61467) ;
#51902 = AXIS2_PLACEMENT_3D('',#87319,#61468,#61469) ;
#51903 = AXIS2_PLACEMENT_3D('',#87322,#61472,#61473) ;
#51904 = AXIS2_PLACEMENT_3D('',#87323,#61474,#61475) ;
#51905 = AXIS2_PLACEMENT_3D('',#87324,#61476,#61477) ;
#51906 = AXIS2_PLACEMENT_3D('',#87325,#61478,#61479) ;
#51907 = AXIS2_PLACEMENT_3D('',#87326,#61480,#61481) ;
#51908 = AXIS2_PLACEMENT_3D('',#87329,#61482,#61483) ;
#51909 = AXIS2_PLACEMENT_3D('',#87330,#61484,#61485) ;
#51910 = AXIS2_PLACEMENT_3D('',#87331,#61486,#61487) ;
#51911 = AXIS2_PLACEMENT_3D('',#87332,#61488,#61489) ;
#51912 = AXIS2_PLACEMENT_3D('',#87335,#61490,#61491) ;
#51913 = AXIS2_PLACEMENT_3D('',#87338,#61494,#61495) ;
#51914 = AXIS2_PLACEMENT_3D('',#87339,#61496,#61497) ;
#51915 = AXIS2_PLACEMENT_3D('',#87340,#61498,#61499) ;
#51916 = AXIS2_PLACEMENT_3D('',#87341,#61500,#61501) ;
#51917 = AXIS2_PLACEMENT_3D('',#87342,#61502,#61503) ;
#51918 = AXIS2_PLACEMENT_3D('',#87345,#61504,#61505) ;
#51919 = AXIS2_PLACEMENT_3D('',#87346,#61506,#61507) ;
#51920 = AXIS2_PLACEMENT_3D('',#87347,#61508,#61509) ;
#51921 = AXIS2_PLACEMENT_3D('',#87348,#61510,#61511) ;
#51922 = AXIS2_PLACEMENT_3D('',#87351,#61512,#61513) ;
#51923 = AXIS2_PLACEMENT_3D('',#87354,#61516,#61517) ;
#51924 = AXIS2_PLACEMENT_3D('',#87355,#61518,#61519) ;
#51925 = AXIS2_PLACEMENT_3D('',#87356,#61520,#61521) ;
#51926 = AXIS2_PLACEMENT_3D('',#87357,#61522,#61523) ;
#51927 = AXIS2_PLACEMENT_3D('',#87358,#61524,#61525) ;
#51928 = AXIS2_PLACEMENT_3D('',#87361,#61526,#61527) ;
#51929 = AXIS2_PLACEMENT_3D('',#87362,#61528,#61529) ;
#51930 = AXIS2_PLACEMENT_3D('',#87363,#61530,#61531) ;
#51931 = AXIS2_PLACEMENT_3D('',#87364,#61532,#61533) ;
#51932 = AXIS2_PLACEMENT_3D('',#87367,#61534,#61535) ;
#51933 = AXIS2_PLACEMENT_3D('',#87370,#61538,#61539) ;
#51934 = AXIS2_PLACEMENT_3D('',#87371,#61540,#61541) ;
#51935 = AXIS2_PLACEMENT_3D('',#87372,#61542,#61543) ;
#51936 = AXIS2_PLACEMENT_3D('',#87373,#61544,#61545) ;
#51937 = AXIS2_PLACEMENT_3D('',#87374,#61546,#61547) ;
#51938 = AXIS2_PLACEMENT_3D('',#87377,#61548,#61549) ;
#51939 = AXIS2_PLACEMENT_3D('',#87378,#61550,#61551) ;
#51940 = AXIS2_PLACEMENT_3D('',#87379,#61552,#61553) ;
#51941 = AXIS2_PLACEMENT_3D('',#87380,#61554,#61555) ;
#51942 = AXIS2_PLACEMENT_3D('',#87383,#61556,#61557) ;
#51943 = AXIS2_PLACEMENT_3D('',#87386,#61560,#61561) ;
#51944 = AXIS2_PLACEMENT_3D('',#87387,#61562,#61563) ;
#51945 = AXIS2_PLACEMENT_3D('',#87388,#61564,#61565) ;
#51946 = AXIS2_PLACEMENT_3D('',#87389,#61566,#61567) ;
#51947 = AXIS2_PLACEMENT_3D('',#87390,#61568,#61569) ;
#51948 = AXIS2_PLACEMENT_3D('',#87392,#61571,#61572) ;
#51949 = AXIS2_PLACEMENT_3D('',#87394,#61574,#61575) ;
#51950 = AXIS2_PLACEMENT_3D('',#87395,#61576,#61577) ;
#51951 = AXIS2_PLACEMENT_3D('',#87397,#61579,#61580) ;
#51952 = AXIS2_PLACEMENT_3D('',#87399,#61582,#61583) ;
#51953 = AXIS2_PLACEMENT_3D('',#87400,#61584,#61585) ;
#51954 = AXIS2_PLACEMENT_3D('',#87402,#61587,#61588) ;
#51955 = AXIS2_PLACEMENT_3D('',#87404,#61590,#61591) ;
#51956 = AXIS2_PLACEMENT_3D('',#87405,#61592,#61593) ;
#51957 = AXIS2_PLACEMENT_3D('',#87407,#61595,#61596) ;
#51958 = AXIS2_PLACEMENT_3D('',#87409,#61598,#61599) ;
#51959 = AXIS2_PLACEMENT_3D('',#87410,#61600,#61601) ;
#51960 = AXIS2_PLACEMENT_3D('',#87419,#61606,#61607) ;
#51961 = AXIS2_PLACEMENT_3D('',#87422,#61610,#61611) ;
#51962 = AXIS2_PLACEMENT_3D('',#87424,#61613,#61614) ;
#51963 = AXIS2_PLACEMENT_3D('',#87426,#61616,#61617) ;
#51964 = AXIS2_PLACEMENT_3D('',#87428,#61619,#61620) ;
#51965 = AXIS2_PLACEMENT_3D('',#87430,#61622,#61623) ;
#51966 = AXIS2_PLACEMENT_3D('',#87431,#61624,#61625) ;
#51967 = AXIS2_PLACEMENT_3D('',#87433,#61627,#61628) ;
#51968 = AXIS2_PLACEMENT_3D('',#87434,#61629,#61630) ;
#51969 = AXIS2_PLACEMENT_3D('',#87436,#61632,#61633) ;
#51970 = AXIS2_PLACEMENT_3D('',#87438,#61635,#61636) ;
#51971 = AXIS2_PLACEMENT_3D('',#87440,#61638,#61639) ;
#51972 = AXIS2_PLACEMENT_3D('',#87442,#61641,#61642) ;
#51973 = AXIS2_PLACEMENT_3D('',#87444,#61644,#61645) ;
#51974 = AXIS2_PLACEMENT_3D('',#87445,#61646,#61647) ;
#51975 = AXIS2_PLACEMENT_3D('',#87446,#61648,#61649) ;
#51976 = AXIS2_PLACEMENT_3D('',#87455,#61654,#61655) ;
#51977 = AXIS2_PLACEMENT_3D('',#87461,#61659,#61660) ;
#51978 = AXIS2_PLACEMENT_3D('',#87467,#61664,#61665) ;
#51979 = AXIS2_PLACEMENT_3D('',#87470,#61668,#61669) ;
#51980 = AXIS2_PLACEMENT_3D('',#87471,#61670,#61671) ;
#51981 = AXIS2_PLACEMENT_3D('',#87472,#61672,#61673) ;
#51982 = AXIS2_PLACEMENT_3D('',#87473,#61674,#61675) ;
#51983 = AXIS2_PLACEMENT_3D('',#87476,#61676,#61677) ;
#51984 = AXIS2_PLACEMENT_3D('',#87478,#61678,#61679) ;
#51985 = AXIS2_PLACEMENT_3D('',#87480,#61680,#61681) ;
#51986 = AXIS2_PLACEMENT_3D('',#87481,#61682,#61683) ;
#51987 = AXIS2_PLACEMENT_3D('',#87482,#61684,#61685) ;
#51988 = AXIS2_PLACEMENT_3D('',#87483,#61686,#61687) ;
#51989 = AXIS2_PLACEMENT_3D('',#87486,#61689,#61690) ;
#51990 = AXIS2_PLACEMENT_3D('',#87487,#61691,#61692) ;
#51991 = AXIS2_PLACEMENT_3D('',#87489,#61693,#61694) ;
#51992 = AXIS2_PLACEMENT_3D('',#87491,#61696,#61697) ;
#51993 = AXIS2_PLACEMENT_3D('',#87492,#61698,#61699) ;
#51994 = AXIS2_PLACEMENT_3D('',#87493,#61700,#61701) ;
#51995 = AXIS2_PLACEMENT_3D('',#87496,#61702,#61703) ;
#51996 = AXIS2_PLACEMENT_3D('',#87498,#61704,#61705) ;
#51997 = AXIS2_PLACEMENT_3D('',#87500,#61706,#61707) ;
#51998 = AXIS2_PLACEMENT_3D('',#87501,#61708,#61709) ;
#51999 = AXIS2_PLACEMENT_3D('',#87502,#61710,#61711) ;
#52000 = AXIS2_PLACEMENT_3D('',#87503,#61712,#61713) ;
#52001 = AXIS2_PLACEMENT_3D('',#87506,#61715,#61716) ;
#52002 = AXIS2_PLACEMENT_3D('',#87507,#61717,#61718) ;
#52003 = AXIS2_PLACEMENT_3D('',#87509,#61719,#61720) ;
#52004 = AXIS2_PLACEMENT_3D('',#87511,#61722,#61723) ;
#52005 = AXIS2_PLACEMENT_3D('',#87512,#61724,#61725) ;
#52006 = AXIS2_PLACEMENT_3D('',#87513,#61726,#61727) ;
#52007 = AXIS2_PLACEMENT_3D('',#87515,#61728,#61729) ;
#52008 = AXIS2_PLACEMENT_3D('',#87517,#61730,#61731) ;
#52009 = AXIS2_PLACEMENT_3D('',#87518,#61732,#61733) ;
#52010 = AXIS2_PLACEMENT_3D('',#87519,#61734,#61735) ;
#52011 = AXIS2_PLACEMENT_3D('',#87522,#61737,#61738) ;
#52012 = AXIS2_PLACEMENT_3D('',#87523,#61739,#61740) ;
#52013 = AXIS2_PLACEMENT_3D('',#87525,#61741,#61742) ;
#52014 = AXIS2_PLACEMENT_3D('',#87526,#61743,#61744) ;
#52015 = AXIS2_PLACEMENT_3D('',#87528,#61745,#61746) ;
#52016 = AXIS2_PLACEMENT_3D('',#87530,#61748,#61749) ;
#52017 = AXIS2_PLACEMENT_3D('',#87531,#61750,#61751) ;
#52018 = AXIS2_PLACEMENT_3D('',#87532,#61752,#61753) ;
#52019 = AXIS2_PLACEMENT_3D('',#87535,#61754,#61755) ;
#52020 = AXIS2_PLACEMENT_3D('',#87537,#61756,#61757) ;
#52021 = AXIS2_PLACEMENT_3D('',#87539,#61758,#61759) ;
#52022 = AXIS2_PLACEMENT_3D('',#87540,#61760,#61761) ;
#52023 = AXIS2_PLACEMENT_3D('',#87563,#61762,#61763) ;
#52024 = AXIS2_PLACEMENT_3D('',#87565,#61764,#61765) ;
#52025 = AXIS2_PLACEMENT_3D('',#87566,#61766,#61767) ;
#52026 = AXIS2_PLACEMENT_3D('',#87567,#61768,#61769) ;
#52027 = AXIS2_PLACEMENT_3D('',#87570,#61772,#61773) ;
#52028 = AXIS2_PLACEMENT_3D('',#87573,#61774,#61775) ;
#52029 = AXIS2_PLACEMENT_3D('',#87575,#61776,#61777) ;
#52030 = AXIS2_PLACEMENT_3D('',#87576,#61778,#61779) ;
#52031 = AXIS2_PLACEMENT_3D('',#87604,#61780,#61781) ;
#52032 = AXIS2_PLACEMENT_3D('',#87606,#61782,#61783) ;
#52033 = AXIS2_PLACEMENT_3D('',#87608,#61784,#61785) ;
#52034 = AXIS2_PLACEMENT_3D('',#87610,#61786,#61787) ;
#52035 = AXIS2_PLACEMENT_3D('',#87611,#61788,#61789) ;
#52036 = AXIS2_PLACEMENT_3D('',#87612,#61790,#61791) ;
#52037 = AXIS2_PLACEMENT_3D('',#87615,#61794,#61795) ;
#52038 = AXIS2_PLACEMENT_3D('',#87618,#61796,#61797) ;
#52039 = AXIS2_PLACEMENT_3D('',#87620,#61798,#61799) ;
#52040 = AXIS2_PLACEMENT_3D('',#87622,#61800,#61801) ;
#52041 = AXIS2_PLACEMENT_3D('',#87623,#61802,#61803) ;
#52042 = AXIS2_PLACEMENT_3D('',#87646,#61804,#61805) ;
#52043 = AXIS2_PLACEMENT_3D('',#87648,#61806,#61807) ;
#52044 = AXIS2_PLACEMENT_3D('',#87649,#61808,#61809) ;
#52045 = AXIS2_PLACEMENT_3D('',#87650,#61810,#61811) ;
#52046 = AXIS2_PLACEMENT_3D('',#87653,#61814,#61815) ;
#52047 = AXIS2_PLACEMENT_3D('',#87656,#61818,#61819) ;
#52048 = AXIS2_PLACEMENT_3D('',#87659,#61820,#61821) ;
#52049 = AXIS2_PLACEMENT_3D('',#87661,#61822,#61823) ;
#52050 = AXIS2_PLACEMENT_3D('',#87663,#61824,#61825) ;
#52051 = AXIS2_PLACEMENT_3D('',#87664,#61826,#61827) ;
#52052 = AXIS2_PLACEMENT_3D('',#87687,#61828,#61829) ;
#52053 = AXIS2_PLACEMENT_3D('',#87689,#61830,#61831) ;
#52054 = AXIS2_PLACEMENT_3D('',#87690,#61832,#61833) ;
#52055 = AXIS2_PLACEMENT_3D('',#87691,#61834,#61835) ;
#52056 = AXIS2_PLACEMENT_3D('',#87694,#61838,#61839) ;
#52057 = AXIS2_PLACEMENT_3D('',#87697,#61840,#61841) ;
#52058 = AXIS2_PLACEMENT_3D('',#87699,#61842,#61843) ;
#52059 = AXIS2_PLACEMENT_3D('',#87700,#61844,#61845) ;
#52060 = AXIS2_PLACEMENT_3D('',#87728,#61846,#61847) ;
#52061 = AXIS2_PLACEMENT_3D('',#87730,#61848,#61849) ;
#52062 = AXIS2_PLACEMENT_3D('',#87732,#61850,#61851) ;
#52063 = AXIS2_PLACEMENT_3D('',#87734,#61852,#61853) ;
#52064 = AXIS2_PLACEMENT_3D('',#87735,#61854,#61855) ;
#52065 = AXIS2_PLACEMENT_3D('',#87736,#61856,#61857) ;
#52066 = AXIS2_PLACEMENT_3D('',#87739,#61860,#61861) ;
#52067 = AXIS2_PLACEMENT_3D('',#87742,#61864,#61865) ;
#52068 = AXIS2_PLACEMENT_3D('',#87745,#61866,#61867) ;
#52069 = AXIS2_PLACEMENT_3D('',#87747,#61868,#61869) ;
#52070 = AXIS2_PLACEMENT_3D('',#87749,#61870,#61871) ;
#52071 = AXIS2_PLACEMENT_3D('',#87750,#61872,#61873) ;
#52072 = AXIS2_PLACEMENT_3D('',#87773,#61874,#61875) ;
#52073 = AXIS2_PLACEMENT_3D('',#87775,#61876,#61877) ;
#52074 = AXIS2_PLACEMENT_3D('',#87776,#61878,#61879) ;
#52075 = AXIS2_PLACEMENT_3D('',#87777,#61880,#61881) ;
#52076 = AXIS2_PLACEMENT_3D('',#87780,#61884,#61885) ;
#52077 = AXIS2_PLACEMENT_3D('',#87783,#61886,#61887) ;
#52078 = AXIS2_PLACEMENT_3D('',#87785,#61888,#61889) ;
#52079 = AXIS2_PLACEMENT_3D('',#87787,#61890,#61891) ;
#52080 = AXIS2_PLACEMENT_3D('',#87788,#61892,#61893) ;
#52081 = AXIS2_PLACEMENT_3D('',#87811,#61894,#61895) ;
#52082 = AXIS2_PLACEMENT_3D('',#87813,#61896,#61897) ;
#52083 = AXIS2_PLACEMENT_3D('',#87814,#61898,#61899) ;
#52084 = AXIS2_PLACEMENT_3D('',#87815,#61900,#61901) ;
#52085 = AXIS2_PLACEMENT_3D('',#87818,#61904,#61905) ;
#52086 = AXIS2_PLACEMENT_3D('',#87821,#61908,#61909) ;
#52087 = AXIS2_PLACEMENT_3D('',#87824,#61910,#61911) ;
#52088 = AXIS2_PLACEMENT_3D('',#87826,#61912,#61913) ;
#52089 = AXIS2_PLACEMENT_3D('',#87827,#61914,#61915) ;
#52090 = AXIS2_PLACEMENT_3D('',#87855,#61916,#61917) ;
#52091 = AXIS2_PLACEMENT_3D('',#87857,#61918,#61919) ;
#52092 = AXIS2_PLACEMENT_3D('',#87859,#61920,#61921) ;
#52093 = AXIS2_PLACEMENT_3D('',#87861,#61922,#61923) ;
#52094 = AXIS2_PLACEMENT_3D('',#87862,#61924,#61925) ;
#52095 = AXIS2_PLACEMENT_3D('',#87863,#61926,#61927) ;
#52096 = AXIS2_PLACEMENT_3D('',#87866,#61930,#61931) ;
#52097 = AXIS2_PLACEMENT_3D('',#87869,#61932,#61933) ;
#52098 = AXIS2_PLACEMENT_3D('',#87871,#61934,#61935) ;
#52099 = AXIS2_PLACEMENT_3D('',#87873,#61936,#61937) ;
#52100 = AXIS2_PLACEMENT_3D('',#87874,#61938,#61939) ;
#52101 = AXIS2_PLACEMENT_3D('',#87897,#61940,#61941) ;
#52102 = AXIS2_PLACEMENT_3D('',#87899,#61942,#61943) ;
#52103 = AXIS2_PLACEMENT_3D('',#87900,#61944,#61945) ;
#52104 = AXIS2_PLACEMENT_3D('',#87901,#61946,#61947) ;
#52105 = AXIS2_PLACEMENT_3D('',#87904,#61950,#61951) ;
#52106 = AXIS2_PLACEMENT_3D('',#87907,#61954,#61955) ;
#52107 = AXIS2_PLACEMENT_3D('',#87910,#61956,#61957) ;
#52108 = AXIS2_PLACEMENT_3D('',#87912,#61958,#61959) ;
#52109 = AXIS2_PLACEMENT_3D('',#87914,#61960,#61961) ;
#52110 = AXIS2_PLACEMENT_3D('',#87915,#61962,#61963) ;
#52111 = AXIS2_PLACEMENT_3D('',#87938,#61964,#61965) ;
#52112 = AXIS2_PLACEMENT_3D('',#87940,#61966,#61967) ;
#52113 = AXIS2_PLACEMENT_3D('',#87941,#61968,#61969) ;
#52114 = AXIS2_PLACEMENT_3D('',#87942,#61970,#61971) ;
#52115 = AXIS2_PLACEMENT_3D('',#87945,#61974,#61975) ;
#52116 = AXIS2_PLACEMENT_3D('',#87948,#61976,#61977) ;
#52117 = AXIS2_PLACEMENT_3D('',#87950,#61978,#61979) ;
#52118 = AXIS2_PLACEMENT_3D('',#87951,#61980,#61981) ;
#52119 = AXIS2_PLACEMENT_3D('',#87979,#61982,#61983) ;
#52120 = AXIS2_PLACEMENT_3D('',#87981,#61984,#61985) ;
#52121 = AXIS2_PLACEMENT_3D('',#87983,#61986,#61987) ;
#52122 = AXIS2_PLACEMENT_3D('',#87985,#61988,#61989) ;
#52123 = AXIS2_PLACEMENT_3D('',#87986,#61990,#61991) ;
#52124 = AXIS2_PLACEMENT_3D('',#87987,#61992,#61993) ;
#52125 = AXIS2_PLACEMENT_3D('',#87990,#61996,#61997) ;
#52126 = AXIS2_PLACEMENT_3D('',#87993,#62000,#62001) ;
#52127 = AXIS2_PLACEMENT_3D('',#87996,#62002,#62003) ;
#52128 = AXIS2_PLACEMENT_3D('',#87998,#62004,#62005) ;
#52129 = AXIS2_PLACEMENT_3D('',#88000,#62006,#62007) ;
#52130 = AXIS2_PLACEMENT_3D('',#88001,#62008,#62009) ;
#52131 = AXIS2_PLACEMENT_3D('',#88024,#62010,#62011) ;
#52132 = AXIS2_PLACEMENT_3D('',#88026,#62012,#62013) ;
#52133 = AXIS2_PLACEMENT_3D('',#88027,#62014,#62015) ;
#52134 = AXIS2_PLACEMENT_3D('',#88028,#62016,#62017) ;
#52135 = AXIS2_PLACEMENT_3D('',#88031,#62020,#62021) ;
#52136 = AXIS2_PLACEMENT_3D('',#88034,#62024,#62025) ;
#52137 = AXIS2_PLACEMENT_3D('',#88037,#62028,#62029) ;
#52138 = AXIS2_PLACEMENT_3D('',#88040,#62032,#62033) ;
#52139 = AXIS2_PLACEMENT_3D('',#88043,#62036,#62037) ;
#52140 = AXIS2_PLACEMENT_3D('',#88046,#62040,#62041) ;
#52141 = AXIS2_PLACEMENT_3D('',#88049,#62044,#62045) ;
#52142 = AXIS2_PLACEMENT_3D('',#88052,#62048,#62049) ;
#52143 = AXIS2_PLACEMENT_3D('',#88054,#62051,#62052) ;
#52144 = AXIS2_PLACEMENT_3D('',#88056,#62054,#62055) ;
#52145 = AXIS2_PLACEMENT_3D('',#88058,#62057,#62058) ;
#52146 = AXIS2_PLACEMENT_3D('',#88060,#62060,#62061) ;
#52147 = AXIS2_PLACEMENT_3D('',#88062,#62063,#62064) ;
#52148 = AXIS2_PLACEMENT_3D('',#88064,#62066,#62067) ;
#52149 = AXIS2_PLACEMENT_3D('',#88066,#62069,#62070) ;
#52150 = AXIS2_PLACEMENT_3D('',#88068,#62072,#62073) ;
#52151 = AXIS2_PLACEMENT_3D('',#88070,#62075,#62076) ;
#52152 = AXIS2_PLACEMENT_3D('',#88072,#62078,#62079) ;
#52153 = AXIS2_PLACEMENT_3D('',#88074,#62081,#62082) ;
#52154 = AXIS2_PLACEMENT_3D('',#88076,#62083,#62084) ;
#52155 = AXIS2_PLACEMENT_3D('',#88077,#62085,#62086) ;
#52156 = AXIS2_PLACEMENT_3D('',#88080,#62089,#62090) ;
#52157 = AXIS2_PLACEMENT_3D('',#88083,#62093,#62094) ;
#52158 = AXIS2_PLACEMENT_3D('',#88085,#62096,#62097) ;
#52159 = AXIS2_PLACEMENT_3D('',#88088,#62100,#62101) ;
#52160 = AXIS2_PLACEMENT_3D('',#88091,#62104,#62105) ;
#52161 = AXIS2_PLACEMENT_3D('',#88094,#62108,#62109) ;
#52162 = AXIS2_PLACEMENT_3D('',#88097,#62112,#62113) ;
#52163 = AXIS2_PLACEMENT_3D('',#88098,#62114,#62115) ;
#52164 = AXIS2_PLACEMENT_3D('',#88099,#62116,#62117) ;
#52165 = AXIS2_PLACEMENT_3D('',#88100,#62118,#62119) ;
#52166 = AXIS2_PLACEMENT_3D('',#88101,#62120,#62121) ;
#52167 = AXIS2_PLACEMENT_3D('',#88102,#62122,#62123) ;
#52168 = AXIS2_PLACEMENT_3D('',#88103,#62124,#62125) ;
#52169 = AXIS2_PLACEMENT_3D('',#88105,#62126,#62127) ;
#52170 = AXIS2_PLACEMENT_3D('',#88106,#62128,#62129) ;
#52171 = AXIS2_PLACEMENT_3D('',#88107,#62130,#62131) ;
#52172 = AXIS2_PLACEMENT_3D('',#88111,#62133,#62134) ;
#52173 = AXIS2_PLACEMENT_3D('',#88112,#62135,#62136) ;
#52174 = AXIS2_PLACEMENT_3D('',#88113,#62137,#62138) ;
#52175 = AXIS2_PLACEMENT_3D('',#88115,#62139,#62140) ;
#52176 = AXIS2_PLACEMENT_3D('',#88116,#62141,#62142) ;
#52177 = AXIS2_PLACEMENT_3D('',#88117,#62143,#62144) ;
#52178 = AXIS2_PLACEMENT_3D('',#88118,#62145,#62146) ;
#52179 = AXIS2_PLACEMENT_3D('',#88119,#62147,#62148) ;
#52180 = AXIS2_PLACEMENT_3D('',#88120,#62149,#62150) ;
#52181 = AXIS2_PLACEMENT_3D('',#88123,#62151,#62152) ;
#52182 = AXIS2_PLACEMENT_3D('',#88125,#62153,#62154) ;
#52183 = AXIS2_PLACEMENT_3D('',#88126,#62155,#62156) ;
#52184 = AXIS2_PLACEMENT_3D('',#88127,#62157,#62158) ;
#52185 = AXIS2_PLACEMENT_3D('',#88130,#62159,#62160) ;
#52186 = AXIS2_PLACEMENT_3D('',#88132,#62161,#62162) ;
#52187 = AXIS2_PLACEMENT_3D('',#88133,#62163,#62164) ;
#52188 = AXIS2_PLACEMENT_3D('',#88134,#62165,#62166) ;
#52189 = AXIS2_PLACEMENT_3D('',#88137,#62167,#62168) ;
#52190 = AXIS2_PLACEMENT_3D('',#88139,#62169,#62170) ;
#52191 = AXIS2_PLACEMENT_3D('',#88140,#62171,#62172) ;
#52192 = AXIS2_PLACEMENT_3D('',#88141,#62173,#62174) ;
#52193 = AXIS2_PLACEMENT_3D('',#88146,#62177,#62178) ;
#52194 = AXIS2_PLACEMENT_3D('',#88147,#62179,#62180) ;
#52195 = AXIS2_PLACEMENT_3D('',#88150,#62183,#62184) ;
#52196 = AXIS2_PLACEMENT_3D('',#88153,#62185,#62186) ;
#52197 = AXIS2_PLACEMENT_3D('',#88155,#62187,#62188) ;
#52198 = AXIS2_PLACEMENT_3D('',#88156,#62189,#62190) ;
#52199 = AXIS2_PLACEMENT_3D('',#88157,#62191,#62192) ;
#52200 = AXIS2_PLACEMENT_3D('',#88160,#62193,#62194) ;
#52201 = AXIS2_PLACEMENT_3D('',#88162,#62195,#62196) ;
#52202 = AXIS2_PLACEMENT_3D('',#88163,#62197,#62198) ;
#52203 = AXIS2_PLACEMENT_3D('',#88164,#62199,#62200) ;
#52204 = AXIS2_PLACEMENT_3D('',#88167,#62203,#62204) ;
#52205 = AXIS2_PLACEMENT_3D('',#88170,#62207,#62208) ;
#52206 = AXIS2_PLACEMENT_3D('',#88173,#62209,#62210) ;
#52207 = AXIS2_PLACEMENT_3D('',#88176,#62213,#62214) ;
#52208 = AXIS2_PLACEMENT_3D('',#88179,#62217,#62218) ;
#52209 = AXIS2_PLACEMENT_3D('',#88184,#62221,#62222) ;
#52210 = AXIS2_PLACEMENT_3D('',#88185,#62223,#62224) ;
#52211 = AXIS2_PLACEMENT_3D('',#88188,#62227,#62228) ;
#52212 = AXIS2_PLACEMENT_3D('',#88191,#62231,#62232) ;
#52213 = AXIS2_PLACEMENT_3D('',#88194,#62235,#62236) ;
#52214 = AXIS2_PLACEMENT_3D('',#88196,#62238,#62239) ;
#52215 = AXIS2_PLACEMENT_3D('',#88198,#62241,#62242) ;
#52216 = AXIS2_PLACEMENT_3D('',#88199,#62243,#62244) ;
#52217 = AXIS2_PLACEMENT_3D('',#88200,#62245,#62246) ;
#52218 = AXIS2_PLACEMENT_3D('',#88201,#62247,#62248) ;
#52219 = AXIS2_PLACEMENT_3D('',#88202,#62249,#62250) ;
#52220 = AXIS2_PLACEMENT_3D('',#88203,#62251,#62252) ;
#52221 = AXIS2_PLACEMENT_3D('',#88205,#62253,#62254) ;
#52222 = AXIS2_PLACEMENT_3D('',#88207,#62255,#62256) ;
#52223 = AXIS2_PLACEMENT_3D('',#88209,#62257,#62258) ;
#52224 = AXIS2_PLACEMENT_3D('',#88210,#62259,#62260) ;
#52225 = AXIS2_PLACEMENT_3D('',#88211,#62261,#62262) ;
#52226 = AXIS2_PLACEMENT_3D('',#88215,#62264,#62265) ;
#52227 = AXIS2_PLACEMENT_3D('',#88216,#62266,#62267) ;
#52228 = AXIS2_PLACEMENT_3D('',#88217,#62268,#62269) ;
#52229 = AXIS2_PLACEMENT_3D('',#88218,#62270,#62271) ;
#52230 = AXIS2_PLACEMENT_3D('',#88223,#62273,#62274) ;
#52231 = AXIS2_PLACEMENT_3D('',#88226,#62276,#62277) ;
#52232 = AXIS2_PLACEMENT_3D('',#88227,#62278,#62279) ;
#52233 = AXIS2_PLACEMENT_3D('',#88231,#62281,#62282) ;
#52234 = AXIS2_PLACEMENT_3D('',#88233,#62284,#62285) ;
#52235 = AXIS2_PLACEMENT_3D('',#88237,#62287,#62288) ;
#52236 = AXIS2_PLACEMENT_3D('',#88239,#62290,#62291) ;
#52237 = AXIS2_PLACEMENT_3D('',#88243,#62293,#62294) ;
#52238 = AXIS2_PLACEMENT_3D('',#88245,#62296,#62297) ;
#52239 = AXIS2_PLACEMENT_3D('',#88249,#62299,#62300) ;
#52240 = AXIS2_PLACEMENT_3D('',#88251,#62302,#62303) ;
#52241 = AXIS2_PLACEMENT_3D('',#88256,#62305,#62306) ;
#52242 = AXIS2_PLACEMENT_3D('',#88259,#62308,#62309) ;
#52243 = AXIS2_PLACEMENT_3D('',#88260,#62310,#62311) ;
#52244 = AXIS2_PLACEMENT_3D('',#88265,#62314,#62315) ;
#52245 = AXIS2_PLACEMENT_3D('',#88266,#62316,#62317) ;
#52246 = AXIS2_PLACEMENT_3D('',#88269,#62320,#62321) ;
#52247 = AXIS2_PLACEMENT_3D('',#88274,#62324,#62325) ;
#52248 = AXIS2_PLACEMENT_3D('',#88275,#62326,#62327) ;
#52249 = AXIS2_PLACEMENT_3D('',#88280,#62330,#62331) ;
#52250 = AXIS2_PLACEMENT_3D('',#88281,#62332,#62333) ;
#52251 = AXIS2_PLACEMENT_3D('',#88286,#62336,#62337) ;
#52252 = AXIS2_PLACEMENT_3D('',#88287,#62338,#62339) ;
#52253 = AXIS2_PLACEMENT_3D('',#88290,#62342,#62343) ;
#52254 = AXIS2_PLACEMENT_3D('',#88296,#62347,#62348) ;
#52255 = AXIS2_PLACEMENT_3D('',#88300,#62351,#62352) ;
#52256 = AXIS2_PLACEMENT_3D('',#88304,#62355,#62356) ;
#52257 = AXIS2_PLACEMENT_3D('',#88308,#62359,#62360) ;
#52258 = AXIS2_PLACEMENT_3D('',#88312,#62363,#62364) ;
#52259 = AXIS2_PLACEMENT_3D('',#88316,#62367,#62368) ;
#52260 = AXIS2_PLACEMENT_3D('',#88318,#62369,#62370) ;
#52261 = AXIS2_PLACEMENT_3D('',#88319,#62371,#62372) ;
#52262 = AXIS2_PLACEMENT_3D('',#88324,#62374,#62375) ;
#52263 = AXIS2_PLACEMENT_3D('',#88327,#62377,#62378) ;
#52264 = AXIS2_PLACEMENT_3D('',#88328,#62379,#62380) ;
#52265 = AXIS2_PLACEMENT_3D('',#88332,#62382,#62383) ;
#52266 = AXIS2_PLACEMENT_3D('',#88334,#62385,#62386) ;
#52267 = AXIS2_PLACEMENT_3D('',#88338,#62388,#62389) ;
#52268 = AXIS2_PLACEMENT_3D('',#88340,#62391,#62392) ;
#52269 = AXIS2_PLACEMENT_3D('',#88343,#62394,#62395) ;
#52270 = AXIS2_PLACEMENT_3D('',#88345,#62397,#62398) ;
#52271 = AXIS2_PLACEMENT_3D('',#88348,#62400,#62401) ;
#52272 = AXIS2_PLACEMENT_3D('',#88349,#62402,#62403) ;
#52273 = AXIS2_PLACEMENT_3D('',#88352,#62405,#62406) ;
#52274 = AXIS2_PLACEMENT_3D('',#88353,#62407,#62408) ;
#52275 = AXIS2_PLACEMENT_3D('',#88356,#62410,#62411) ;
#52276 = AXIS2_PLACEMENT_3D('',#88357,#62412,#62413) ;
#52277 = AXIS2_PLACEMENT_3D('',#88360,#62415,#62416) ;
#52278 = AXIS2_PLACEMENT_3D('',#88361,#62417,#62418) ;
#52279 = AXIS2_PLACEMENT_3D('',#88364,#62420,#62421) ;
#52280 = AXIS2_PLACEMENT_3D('',#88365,#62422,#62423) ;
#52281 = AXIS2_PLACEMENT_3D('',#88368,#62425,#62426) ;
#52282 = AXIS2_PLACEMENT_3D('',#88369,#62427,#62428) ;
#52283 = AXIS2_PLACEMENT_3D('',#88374,#62431,#62432) ;
#52284 = AXIS2_PLACEMENT_3D('',#88375,#62433,#62434) ;
#52285 = AXIS2_PLACEMENT_3D('',#88378,#62437,#62438) ;
#52286 = AXIS2_PLACEMENT_3D('',#88380,#62440,#62441) ;
#52287 = AXIS2_PLACEMENT_3D('',#88382,#62443,#62444) ;
#52288 = AXIS2_PLACEMENT_3D('',#88384,#62446,#62447) ;
#52289 = AXIS2_PLACEMENT_3D('',#88385,#62448,#62449) ;
#52290 = AXIS2_PLACEMENT_3D('',#88386,#62450,#62451) ;
#52291 = AXIS2_PLACEMENT_3D('',#88387,#62452,#62453) ;
#52292 = AXIS2_PLACEMENT_3D('',#88389,#62455,#62456) ;
#52293 = AXIS2_PLACEMENT_3D('',#88391,#62458,#62459) ;
#52294 = AXIS2_PLACEMENT_3D('',#88392,#62460,#62461) ;
#52295 = AXIS2_PLACEMENT_3D('',#88393,#62462,#62463) ;
#52296 = AXIS2_PLACEMENT_3D('',#88398,#62465,#62466) ;
#52297 = AXIS2_PLACEMENT_3D('',#88401,#62468,#62469) ;
#52298 = AXIS2_PLACEMENT_3D('',#88402,#62470,#62471) ;
#52299 = AXIS2_PLACEMENT_3D('',#88406,#62473,#62474) ;
#52300 = AXIS2_PLACEMENT_3D('',#88408,#62476,#62477) ;
#52301 = AXIS2_PLACEMENT_3D('',#88412,#62479,#62480) ;
#52302 = AXIS2_PLACEMENT_3D('',#88414,#62482,#62483) ;
#52303 = AXIS2_PLACEMENT_3D('',#88418,#62485,#62486) ;
#52304 = AXIS2_PLACEMENT_3D('',#88420,#62488,#62489) ;
#52305 = AXIS2_PLACEMENT_3D('',#88424,#62491,#62492) ;
#52306 = AXIS2_PLACEMENT_3D('',#88426,#62494,#62495) ;
#52307 = AXIS2_PLACEMENT_3D('',#88431,#62498,#62499) ;
#52308 = AXIS2_PLACEMENT_3D('',#88432,#62500,#62501) ;
#52309 = AXIS2_PLACEMENT_3D('',#88437,#62504,#62505) ;
#52310 = AXIS2_PLACEMENT_3D('',#88438,#62506,#62507) ;
#52311 = AXIS2_PLACEMENT_3D('',#88443,#62510,#62511) ;
#52312 = AXIS2_PLACEMENT_3D('',#88444,#62512,#62513) ;
#52313 = AXIS2_PLACEMENT_3D('',#88449,#62516,#62517) ;
#52314 = AXIS2_PLACEMENT_3D('',#88450,#62518,#62519) ;
#52315 = AXIS2_PLACEMENT_3D('',#88455,#62522,#62523) ;
#52316 = AXIS2_PLACEMENT_3D('',#88456,#62524,#62525) ;
#52317 = AXIS2_PLACEMENT_3D('',#88461,#62528,#62529) ;
#52318 = AXIS2_PLACEMENT_3D('',#88462,#62530,#62531) ;
#52319 = AXIS2_PLACEMENT_3D('',#88465,#62534,#62535) ;
#52320 = AXIS2_PLACEMENT_3D('',#88471,#62539,#62540) ;
#52321 = AXIS2_PLACEMENT_3D('',#88475,#62543,#62544) ;
#52322 = AXIS2_PLACEMENT_3D('',#88479,#62547,#62548) ;
#52323 = AXIS2_PLACEMENT_3D('',#88483,#62551,#62552) ;
#52324 = AXIS2_PLACEMENT_3D('',#88487,#62555,#62556) ;
#52325 = AXIS2_PLACEMENT_3D('',#88491,#62559,#62560) ;
#52326 = AXIS2_PLACEMENT_3D('',#88492,#62561,#62562) ;
#52327 = AXIS2_PLACEMENT_3D('',#88494,#62563,#62564) ;
#52328 = AXIS2_PLACEMENT_3D('',#88496,#62565,#62566) ;
#52329 = AXIS2_PLACEMENT_3D('',#88498,#62567,#62568) ;
#52330 = AXIS2_PLACEMENT_3D('',#88499,#62569,#62570) ;
#52331 = AXIS2_PLACEMENT_3D('',#88500,#62571,#62572) ;
#52332 = AXIS2_PLACEMENT_3D('',#88504,#62574,#62575) ;
#52333 = AXIS2_PLACEMENT_3D('',#88505,#62576,#62577) ;
#52334 = AXIS2_PLACEMENT_3D('',#88506,#62578,#62579) ;
#52335 = AXIS2_PLACEMENT_3D('',#88507,#62580,#62581) ;
#52336 = AXIS2_PLACEMENT_3D('',#88511,#62583,#62584) ;
#52337 = AXIS2_PLACEMENT_3D('',#88512,#62585,#62586) ;
#52338 = AXIS2_PLACEMENT_3D('',#88513,#62587,#62588) ;
#52339 = AXIS2_PLACEMENT_3D('',#88516,#62590,#62591) ;
#52340 = AXIS2_PLACEMENT_3D('',#88517,#62592,#62593) ;
#52341 = AXIS2_PLACEMENT_3D('',#88520,#62595,#62596) ;
#52342 = AXIS2_PLACEMENT_3D('',#88521,#62597,#62598) ;
#52343 = AXIS2_PLACEMENT_3D('',#88524,#62600,#62601) ;
#52344 = AXIS2_PLACEMENT_3D('',#88525,#62602,#62603) ;
#52345 = AXIS2_PLACEMENT_3D('',#88529,#62605,#62606) ;
#52346 = AXIS2_PLACEMENT_3D('',#88531,#62608,#62609) ;
#52347 = AXIS2_PLACEMENT_3D('',#88536,#62611,#62612) ;
#52348 = AXIS2_PLACEMENT_3D('',#88539,#62614,#62615) ;
#52349 = AXIS2_PLACEMENT_3D('',#88540,#62616,#62617) ;
#52350 = AXIS2_PLACEMENT_3D('',#88545,#62620,#62621) ;
#52351 = AXIS2_PLACEMENT_3D('',#88546,#62622,#62623) ;
#52352 = AXIS2_PLACEMENT_3D('',#88549,#62626,#62627) ;
#52353 = AXIS2_PLACEMENT_3D('',#88554,#62630,#62631) ;
#52354 = AXIS2_PLACEMENT_3D('',#88555,#62632,#62633) ;
#52355 = AXIS2_PLACEMENT_3D('',#88559,#62636,#62637) ;
#52356 = AXIS2_PLACEMENT_3D('',#88560,#62638,#62639) ;
#52357 = AXIS2_PLACEMENT_3D('',#88563,#62641,#62642) ;
#52358 = AXIS2_PLACEMENT_3D('',#88564,#62643,#62644) ;
#52359 = AXIS2_PLACEMENT_3D('',#88566,#62646,#62647) ;
#52360 = AXIS2_PLACEMENT_3D('',#88568,#62649,#62650) ;
#52361 = AXIS2_PLACEMENT_3D('',#88570,#62652,#62653) ;
#52362 = AXIS2_PLACEMENT_3D('',#88572,#62655,#62656) ;
#52363 = AXIS2_PLACEMENT_3D('',#88574,#62657,#62658) ;
#52364 = AXIS2_PLACEMENT_3D('',#88575,#62659,#62660) ;
#52365 = AXIS2_PLACEMENT_3D('',#88576,#62661,#62662) ;
#52366 = AXIS2_PLACEMENT_3D('',#88577,#62663,#62664) ;
#52367 = AXIS2_PLACEMENT_3D('',#88579,#62666,#62667) ;
#52368 = AXIS2_PLACEMENT_3D('',#88581,#62669,#62670) ;
#52369 = AXIS2_PLACEMENT_3D('',#88582,#62671,#62672) ;
#52370 = AXIS2_PLACEMENT_3D('',#88583,#62673,#62674) ;
#52371 = AXIS2_PLACEMENT_3D('',#88588,#62676,#62677) ;
#52372 = AXIS2_PLACEMENT_3D('',#88591,#62679,#62680) ;
#52373 = AXIS2_PLACEMENT_3D('',#88592,#62681,#62682) ;
#52374 = AXIS2_PLACEMENT_3D('',#88596,#62684,#62685) ;
#52375 = AXIS2_PLACEMENT_3D('',#88598,#62687,#62688) ;
#52376 = AXIS2_PLACEMENT_3D('',#88602,#62690,#62691) ;
#52377 = AXIS2_PLACEMENT_3D('',#88604,#62693,#62694) ;
#52378 = AXIS2_PLACEMENT_3D('',#88608,#62696,#62697) ;
#52379 = AXIS2_PLACEMENT_3D('',#88610,#62699,#62700) ;
#52380 = AXIS2_PLACEMENT_3D('',#88614,#62702,#62703) ;
#52381 = AXIS2_PLACEMENT_3D('',#88616,#62705,#62706) ;
#52382 = AXIS2_PLACEMENT_3D('',#88621,#62709,#62710) ;
#52383 = AXIS2_PLACEMENT_3D('',#88622,#62711,#62712) ;
#52384 = AXIS2_PLACEMENT_3D('',#88627,#62715,#62716) ;
#52385 = AXIS2_PLACEMENT_3D('',#88628,#62717,#62718) ;
#52386 = AXIS2_PLACEMENT_3D('',#88633,#62721,#62722) ;
#52387 = AXIS2_PLACEMENT_3D('',#88634,#62723,#62724) ;
#52388 = AXIS2_PLACEMENT_3D('',#88639,#62727,#62728) ;
#52389 = AXIS2_PLACEMENT_3D('',#88640,#62729,#62730) ;
#52390 = AXIS2_PLACEMENT_3D('',#88645,#62733,#62734) ;
#52391 = AXIS2_PLACEMENT_3D('',#88646,#62735,#62736) ;
#52392 = AXIS2_PLACEMENT_3D('',#88651,#62739,#62740) ;
#52393 = AXIS2_PLACEMENT_3D('',#88652,#62741,#62742) ;
#52394 = AXIS2_PLACEMENT_3D('',#88655,#62745,#62746) ;
#52395 = AXIS2_PLACEMENT_3D('',#88661,#62750,#62751) ;
#52396 = AXIS2_PLACEMENT_3D('',#88665,#62754,#62755) ;
#52397 = AXIS2_PLACEMENT_3D('',#88669,#62758,#62759) ;
#52398 = AXIS2_PLACEMENT_3D('',#88673,#62762,#62763) ;
#52399 = AXIS2_PLACEMENT_3D('',#88677,#62766,#62767) ;
#52400 = AXIS2_PLACEMENT_3D('',#88681,#62770,#62771) ;
#52401 = AXIS2_PLACEMENT_3D('',#88682,#62772,#62773) ;
#52402 = AXIS2_PLACEMENT_3D('',#88684,#62774,#62775) ;
#52403 = AXIS2_PLACEMENT_3D('',#88686,#62776,#62777) ;
#52404 = AXIS2_PLACEMENT_3D('',#88688,#62778,#62779) ;
#52405 = AXIS2_PLACEMENT_3D('',#88689,#62780,#62781) ;
#52406 = AXIS2_PLACEMENT_3D('',#88690,#62782,#62783) ;
#52407 = AXIS2_PLACEMENT_3D('',#88694,#62785,#62786) ;
#52408 = AXIS2_PLACEMENT_3D('',#88695,#62787,#62788) ;
#52409 = AXIS2_PLACEMENT_3D('',#88696,#62789,#62790) ;
#52410 = AXIS2_PLACEMENT_3D('',#88697,#62791,#62792) ;
#52411 = AXIS2_PLACEMENT_3D('',#88701,#62794,#62795) ;
#52412 = AXIS2_PLACEMENT_3D('',#88702,#62796,#62797) ;
#52413 = AXIS2_PLACEMENT_3D('',#88703,#62798,#62799) ;
#52414 = AXIS2_PLACEMENT_3D('',#88706,#62801,#62802) ;
#52415 = AXIS2_PLACEMENT_3D('',#88707,#62803,#62804) ;
#52416 = AXIS2_PLACEMENT_3D('',#88710,#62806,#62807) ;
#52417 = AXIS2_PLACEMENT_3D('',#88711,#62808,#62809) ;
#52418 = AXIS2_PLACEMENT_3D('',#88714,#62811,#62812) ;
#52419 = AXIS2_PLACEMENT_3D('',#88715,#62813,#62814) ;
#52420 = AXIS2_PLACEMENT_3D('',#88719,#62816,#62817) ;
#52421 = AXIS2_PLACEMENT_3D('',#88721,#62819,#62820) ;
#52422 = AXIS2_PLACEMENT_3D('',#88726,#62822,#62823) ;
#52423 = AXIS2_PLACEMENT_3D('',#88729,#62825,#62826) ;
#52424 = AXIS2_PLACEMENT_3D('',#88730,#62827,#62828) ;
#52425 = AXIS2_PLACEMENT_3D('',#88735,#62831,#62832) ;
#52426 = AXIS2_PLACEMENT_3D('',#88736,#62833,#62834) ;
#52427 = AXIS2_PLACEMENT_3D('',#88739,#62837,#62838) ;
#52428 = AXIS2_PLACEMENT_3D('',#88744,#62841,#62842) ;
#52429 = AXIS2_PLACEMENT_3D('',#88745,#62843,#62844) ;
#52430 = AXIS2_PLACEMENT_3D('',#88749,#62847,#62848) ;
#52431 = AXIS2_PLACEMENT_3D('',#88750,#62849,#62850) ;
#52432 = AXIS2_PLACEMENT_3D('',#88753,#62852,#62853) ;
#52433 = AXIS2_PLACEMENT_3D('',#88754,#62854,#62855) ;
#52434 = AXIS2_PLACEMENT_3D('',#88756,#62857,#62858) ;
#52435 = AXIS2_PLACEMENT_3D('',#88758,#62860,#62861) ;
#52436 = AXIS2_PLACEMENT_3D('',#88760,#62863,#62864) ;
#52437 = AXIS2_PLACEMENT_3D('',#88762,#62866,#62867) ;
#52438 = AXIS2_PLACEMENT_3D('',#88764,#62868,#62869) ;
#52439 = AXIS2_PLACEMENT_3D('',#88765,#62870,#62871) ;
#52440 = AXIS2_PLACEMENT_3D('',#88766,#62872,#62873) ;
#52441 = AXIS2_PLACEMENT_3D('',#88767,#62874,#62875) ;
#52442 = AXIS2_PLACEMENT_3D('',#88769,#62877,#62878) ;
#52443 = AXIS2_PLACEMENT_3D('',#88771,#62880,#62881) ;
#52444 = AXIS2_PLACEMENT_3D('',#88772,#62882,#62883) ;
#52445 = AXIS2_PLACEMENT_3D('',#88773,#62884,#62885) ;
#52446 = AXIS2_PLACEMENT_3D('',#88776,#62886,#62887) ;
#52447 = AXIS2_PLACEMENT_3D('',#88778,#62888,#62889) ;
#52448 = AXIS2_PLACEMENT_3D('',#88779,#62890,#62891) ;
#52449 = AXIS2_PLACEMENT_3D('',#88780,#62892,#62893) ;
#52450 = AXIS2_PLACEMENT_3D('',#88783,#62894,#62895) ;
#52451 = AXIS2_PLACEMENT_3D('',#88785,#62896,#62897) ;
#52452 = AXIS2_PLACEMENT_3D('',#88786,#62898,#62899) ;
#52453 = AXIS2_PLACEMENT_3D('',#88787,#62900,#62901) ;
#52454 = AXIS2_PLACEMENT_3D('',#88790,#62904,#62905) ;
#52455 = AXIS2_PLACEMENT_3D('',#88793,#62906,#62907) ;
#52456 = AXIS2_PLACEMENT_3D('',#88795,#62908,#62909) ;
#52457 = AXIS2_PLACEMENT_3D('',#88796,#62910,#62911) ;
#52458 = AXIS2_PLACEMENT_3D('',#88797,#62912,#62913) ;
#52459 = AXIS2_PLACEMENT_3D('',#88800,#62916,#62917) ;
#52460 = AXIS2_PLACEMENT_3D('',#88803,#62918,#62919) ;
#52461 = AXIS2_PLACEMENT_3D('',#88805,#62920,#62921) ;
#52462 = AXIS2_PLACEMENT_3D('',#88807,#62922,#62923) ;
#52463 = AXIS2_PLACEMENT_3D('',#88808,#62924,#62925) ;
#52464 = AXIS2_PLACEMENT_3D('',#88841,#62926,#62927) ;
#52465 = AXIS2_PLACEMENT_3D('',#88843,#62928,#62929) ;
#52466 = AXIS2_PLACEMENT_3D('',#88845,#62930,#62931) ;
#52467 = AXIS2_PLACEMENT_3D('',#88846,#62932,#62933) ;
#52468 = AXIS2_PLACEMENT_3D('',#88847,#62934,#62935) ;
#52469 = AXIS2_PLACEMENT_3D('',#88850,#62938,#62939) ;
#52470 = AXIS2_PLACEMENT_3D('',#88853,#62942,#62943) ;
#52471 = AXIS2_PLACEMENT_3D('',#88856,#62944,#62945) ;
#52472 = AXIS2_PLACEMENT_3D('',#88858,#62946,#62947) ;
#52473 = AXIS2_PLACEMENT_3D('',#88859,#62948,#62949) ;
#52474 = AXIS2_PLACEMENT_3D('',#88860,#62950,#62951) ;
#52475 = AXIS2_PLACEMENT_3D('',#88863,#62954,#62955) ;
#52476 = AXIS2_PLACEMENT_3D('',#88866,#62958,#62959) ;
#52477 = AXIS2_PLACEMENT_3D('',#88869,#62960,#62961) ;
#52478 = AXIS2_PLACEMENT_3D('',#88871,#62962,#62963) ;
#52479 = AXIS2_PLACEMENT_3D('',#88873,#62964,#62965) ;
#52480 = AXIS2_PLACEMENT_3D('',#88874,#62966,#62967) ;
#52481 = AXIS2_PLACEMENT_3D('',#88902,#62968,#62969) ;
#52482 = AXIS2_PLACEMENT_3D('',#88904,#62970,#62971) ;
#52483 = AXIS2_PLACEMENT_3D('',#88906,#62972,#62973) ;
#52484 = AXIS2_PLACEMENT_3D('',#88907,#62974,#62975) ;
#52485 = AXIS2_PLACEMENT_3D('',#88908,#62976,#62977) ;
#52486 = AXIS2_PLACEMENT_3D('',#88911,#62980,#62981) ;
#52487 = AXIS2_PLACEMENT_3D('',#88914,#62984,#62985) ;
#52488 = AXIS2_PLACEMENT_3D('',#88917,#62988,#62989) ;
#52489 = AXIS2_PLACEMENT_3D('',#88920,#62992,#62993) ;
#52490 = AXIS2_PLACEMENT_3D('',#88923,#62996,#62997) ;
#52491 = AXIS2_PLACEMENT_3D('',#88926,#63000,#63001) ;
#52492 = AXIS2_PLACEMENT_3D('',#88927,#63002,#63003) ;
#52493 = AXIS2_PLACEMENT_3D('',#88928,#63004,#63005) ;
#52494 = AXIS2_PLACEMENT_3D('',#88929,#63006,#63007) ;
#52495 = AXIS2_PLACEMENT_3D('',#88930,#63008,#63009) ;
#52496 = AXIS2_PLACEMENT_3D('',#88931,#63010,#63011) ;
#52497 = AXIS2_PLACEMENT_3D('',#88934,#63012,#63013) ;
#52498 = AXIS2_PLACEMENT_3D('',#88936,#63014,#63015) ;
#52499 = AXIS2_PLACEMENT_3D('',#88937,#63016,#63017) ;
#52500 = AXIS2_PLACEMENT_3D('',#88938,#63018,#63019) ;
#52501 = AXIS2_PLACEMENT_3D('',#88941,#63020,#63021) ;
#52502 = AXIS2_PLACEMENT_3D('',#88943,#63022,#63023) ;
#52503 = AXIS2_PLACEMENT_3D('',#88944,#63024,#63025) ;
#52504 = AXIS2_PLACEMENT_3D('',#88945,#63026,#63027) ;
#52505 = AXIS2_PLACEMENT_3D('',#88948,#63030,#63031) ;
#52506 = AXIS2_PLACEMENT_3D('',#88953,#63034,#63035) ;
#52507 = AXIS2_PLACEMENT_3D('',#88954,#63036,#63037) ;
#52508 = AXIS2_PLACEMENT_3D('',#88957,#63038,#63039) ;
#52509 = AXIS2_PLACEMENT_3D('',#88959,#63040,#63041) ;
#52510 = AXIS2_PLACEMENT_3D('',#88960,#63042,#63043) ;
#52511 = AXIS2_PLACEMENT_3D('',#88961,#63044,#63045) ;
#52512 = AXIS2_PLACEMENT_3D('',#88964,#63048,#63049) ;
#52513 = AXIS2_PLACEMENT_3D('',#88968,#63052,#63053) ;
#52514 = AXIS2_PLACEMENT_3D('',#88969,#63054,#63055) ;
#52515 = AXIS2_PLACEMENT_3D('',#88972,#63056,#63057) ;
#52516 = AXIS2_PLACEMENT_3D('',#88975,#63060,#63061) ;
#52517 = AXIS2_PLACEMENT_3D('',#88978,#63062,#63063) ;
#52518 = AXIS2_PLACEMENT_3D('',#88981,#63066,#63067) ;
#52519 = AXIS2_PLACEMENT_3D('',#88984,#63068,#63069) ;
#52520 = AXIS2_PLACEMENT_3D('',#88987,#63072,#63073) ;
#52521 = AXIS2_PLACEMENT_3D('',#88989,#63075,#63076) ;
#52522 = AXIS2_PLACEMENT_3D('',#88994,#63080,#63081) ;
#52523 = AXIS2_PLACEMENT_3D('',#88996,#63083,#63084) ;
#52524 = AXIS2_PLACEMENT_3D('',#88997,#63085,#63086) ;
#52525 = AXIS2_PLACEMENT_3D('',#88998,#63087,#63088) ;
#52526 = AXIS2_PLACEMENT_3D('',#88999,#63089,#63090) ;
#52527 = AXIS2_PLACEMENT_3D('',#89165,#63091,#63092) ;
#52528 = AXIS2_PLACEMENT_3D('',#89259,#63093,#63094) ;
#52529 = AXIS2_PLACEMENT_3D('',#89557,#63095,#63096) ;
#52530 = AXIS2_PLACEMENT_3D('',#89637,#63097,#63098) ;
#52531 = AXIS2_PLACEMENT_3D('',#89873,#63099,#63100) ;
#52532 = AXIS2_PLACEMENT_3D('',#89874,#63101,#63102) ;
#52533 = AXIS2_PLACEMENT_3D('',#89998,#63112,#63113) ;
#52534 = AXIS2_PLACEMENT_3D('',#90004,#63117,#63118) ;
#52535 = AXIS2_PLACEMENT_3D('',#90007,#63121,#63122) ;
#52536 = AXIS2_PLACEMENT_3D('',#90016,#63127,#63128) ;
#52537 = AXIS2_PLACEMENT_3D('',#90114,#63136,#63137) ;
#52538 = AXIS2_PLACEMENT_3D('',#90120,#63141,#63142) ;
#52539 = AXIS2_PLACEMENT_3D('',#90126,#63146,#63147) ;
#52540 = AXIS2_PLACEMENT_3D('',#90293,#63158,#63159) ;
#52541 = AXIS2_PLACEMENT_3D('',#90299,#63163,#63164) ;
#52542 = AXIS2_PLACEMENT_3D('',#90305,#63168,#63169) ;
#52543 = AXIS2_PLACEMENT_3D('',#90308,#63172,#63173) ;
#52544 = AXIS2_PLACEMENT_3D('',#90309,#63174,#63175) ;
#52545 = AXIS2_PLACEMENT_3D('',#90316,#63178,#63179) ;
#52546 = AXIS2_PLACEMENT_3D('',#90320,#63181,#63182) ;
#52547 = AXIS2_PLACEMENT_3D('',#90324,#63184,#63185) ;
#52548 = AXIS2_PLACEMENT_3D('',#90328,#63187,#63188) ;
#52549 = AXIS2_PLACEMENT_3D('',#90330,#63189,#63190) ;
#52550 = AXIS2_PLACEMENT_3D('',#90334,#63192,#63193) ;
#52551 = AXIS2_PLACEMENT_3D('',#90338,#63195,#63196) ;
#52552 = AXIS2_PLACEMENT_3D('',#90342,#63198,#63199) ;
#52553 = AXIS2_PLACEMENT_3D('',#90345,#63201,#63202) ;
#52554 = AXIS2_PLACEMENT_3D('',#90350,#63204,#63205) ;
#52555 = AXIS2_PLACEMENT_3D('',#90364,#63208,#63209) ;
#52556 = AXIS2_PLACEMENT_3D('',#90368,#63211,#63212) ;
#52557 = AXIS2_PLACEMENT_3D('',#90397,#63215,#63216) ;
#52558 = AXIS2_PLACEMENT_3D('',#90400,#63217,#63218) ;
#52559 = AXIS2_PLACEMENT_3D('',#90402,#63219,#63220) ;
#52560 = AXIS2_PLACEMENT_3D('',#90412,#63221,#63222) ;
#52561 = AXIS2_PLACEMENT_3D('',#90413,#63223,#63224) ;
#52562 = AXIS2_PLACEMENT_3D('',#90416,#63225,#63226) ;
#52563 = AXIS2_PLACEMENT_3D('',#90430,#63229,#63230) ;
#52564 = AXIS2_PLACEMENT_3D('',#90431,#63231,#63232) ;
#52565 = AXIS2_PLACEMENT_3D('',#90432,#63233,#63234) ;
#52566 = AXIS2_PLACEMENT_3D('',#90433,#63235,#63236) ;
#52567 = AXIS2_PLACEMENT_3D('',#90436,#63237,#63238) ;
#52568 = AXIS2_PLACEMENT_3D('',#90506,#63241,#63242) ;
#52569 = AXIS2_PLACEMENT_3D('',#90507,#63243,#63244) ;
#52570 = AXIS2_PLACEMENT_3D('',#90517,#63250,#63251) ;
#52571 = AXIS2_PLACEMENT_3D('',#90520,#63253,#63254) ;
#52572 = AXIS2_PLACEMENT_3D('',#90521,#63255,#63256) ;
#52573 = AXIS2_PLACEMENT_3D('',#90559,#63259,#63260) ;
#52574 = AXIS2_PLACEMENT_3D('',#90561,#63261,#63262) ;
#52575 = AXIS2_PLACEMENT_3D('',#90563,#63263,#63264) ;
#52576 = AXIS2_PLACEMENT_3D('',#90591,#63265,#63266) ;
#52577 = AXIS2_PLACEMENT_3D('',#90594,#63267,#63268) ;
#52578 = AXIS2_PLACEMENT_3D('',#90608,#63271,#63272) ;
#52579 = AXIS2_PLACEMENT_3D('',#90609,#63273,#63274) ;
#52580 = AXIS2_PLACEMENT_3D('',#90610,#63275,#63276) ;
#52581 = AXIS2_PLACEMENT_3D('',#90611,#63277,#63278) ;
#52582 = AXIS2_PLACEMENT_3D('',#90614,#63279,#63280) ;
#52583 = AXIS2_PLACEMENT_3D('',#90617,#63283,#63284) ;
#52584 = AXIS2_PLACEMENT_3D('',#90626,#63285,#63286) ;
#52585 = AXIS2_PLACEMENT_3D('',#90627,#63287,#63288) ;
#52586 = AXIS2_PLACEMENT_3D('',#90628,#63289,#63290) ;
#52587 = AXIS2_PLACEMENT_3D('',#90634,#63294,#63295) ;
#52588 = AXIS2_PLACEMENT_3D('',#90637,#63297,#63298) ;
#52589 = AXIS2_PLACEMENT_3D('',#90638,#63299,#63300) ;
#52590 = AXIS2_PLACEMENT_3D('',#90752,#63304,#63305) ;
#52591 = AXIS2_PLACEMENT_3D('',#90753,#63306,#63307) ;
#52592 = AXIS2_PLACEMENT_3D('',#90755,#63309,#63310) ;
#52593 = AXIS2_PLACEMENT_3D('',#90773,#63311,#63312) ;
#52594 = AXIS2_PLACEMENT_3D('',#90783,#63314,#63315) ;
#52595 = AXIS2_PLACEMENT_3D('',#90793,#63320,#63321) ;
#52596 = AXIS2_PLACEMENT_3D('',#90797,#63323,#63324) ;
#52597 = AXIS2_PLACEMENT_3D('',#90826,#63326,#63327) ;
#52598 = AXIS2_PLACEMENT_3D('',#90828,#63328,#63329) ;
#52599 = AXIS2_PLACEMENT_3D('',#90830,#63330,#63331) ;
#52600 = AXIS2_PLACEMENT_3D('',#90832,#63332,#63333) ;
#52601 = AXIS2_PLACEMENT_3D('',#90833,#63334,#63335) ;
#52602 = AXIS2_PLACEMENT_3D('',#90834,#63336,#63337) ;
#52603 = AXIS2_PLACEMENT_3D('',#90837,#63338,#63339) ;
#52604 = AXIS2_PLACEMENT_3D('',#90862,#63342,#63343) ;
#52605 = AXIS2_PLACEMENT_3D('',#90863,#63344,#63345) ;
#52606 = AXIS2_PLACEMENT_3D('',#90864,#63346,#63347) ;
#52607 = AXIS2_PLACEMENT_3D('',#90902,#63348,#63349) ;
#52608 = AXIS2_PLACEMENT_3D('',#90906,#63351,#63352) ;
#52609 = AXIS2_PLACEMENT_3D('',#90908,#63354,#63355) ;
#52610 = AXIS2_PLACEMENT_3D('',#90913,#63358,#63359) ;
#52611 = AXIS2_PLACEMENT_3D('',#90914,#63360,#63361) ;
#52612 = AXIS2_PLACEMENT_3D('',#90917,#63363,#63364) ;
#52613 = AXIS2_PLACEMENT_3D('',#90945,#63365,#63366) ;
#52614 = AXIS2_PLACEMENT_3D('',#90947,#63367,#63368) ;
#52615 = AXIS2_PLACEMENT_3D('',#90949,#63369,#63370) ;
#52616 = AXIS2_PLACEMENT_3D('',#90951,#63371,#63372) ;
#52617 = AXIS2_PLACEMENT_3D('',#90952,#63373,#63374) ;
#52618 = AXIS2_PLACEMENT_3D('',#90953,#63375,#63376) ;
#52619 = AXIS2_PLACEMENT_3D('',#90956,#63377,#63378) ;
#52620 = AXIS2_PLACEMENT_3D('',#90981,#63381,#63382) ;
#52621 = AXIS2_PLACEMENT_3D('',#90982,#63383,#63384) ;
#52622 = AXIS2_PLACEMENT_3D('',#90983,#63385,#63386) ;
#52623 = AXIS2_PLACEMENT_3D('',#91030,#63387,#63388) ;
#52624 = AXIS2_PLACEMENT_3D('',#91036,#63391,#63392) ;
#52625 = AXIS2_PLACEMENT_3D('',#91040,#63394,#63395) ;
#52626 = AXIS2_PLACEMENT_3D('',#91049,#63400,#63401) ;
#52627 = AXIS2_PLACEMENT_3D('',#91053,#63404,#63405) ;
#52628 = AXIS2_PLACEMENT_3D('',#91056,#63407,#63408) ;
#52629 = AXIS2_PLACEMENT_3D('',#91057,#63409,#63410) ;
#52630 = AXIS2_PLACEMENT_3D('',#91061,#63412,#63413) ;
#52631 = AXIS2_PLACEMENT_3D('',#91085,#63415,#63416) ;
#52632 = AXIS2_PLACEMENT_3D('',#91087,#63417,#63418) ;
#52633 = AXIS2_PLACEMENT_3D('',#91088,#63419,#63420) ;
#52634 = AXIS2_PLACEMENT_3D('',#91089,#63421,#63422) ;
#52635 = AXIS2_PLACEMENT_3D('',#91093,#63424,#63425) ;
#52636 = AXIS2_PLACEMENT_3D('',#91095,#63427,#63428) ;
#52637 = AXIS2_PLACEMENT_3D('',#91112,#63431,#63432) ;
#52638 = AXIS2_PLACEMENT_3D('',#91114,#63434,#63435) ;
#52639 = AXIS2_PLACEMENT_3D('',#91124,#63440,#63441) ;
#52640 = AXIS2_PLACEMENT_3D('',#91128,#63443,#63444) ;
#52641 = AXIS2_PLACEMENT_3D('',#91130,#63446,#63447) ;
#52642 = AXIS2_PLACEMENT_3D('',#91132,#63449,#63450) ;
#52643 = AXIS2_PLACEMENT_3D('',#91134,#63451,#63452) ;
#52644 = AXIS2_PLACEMENT_3D('',#91136,#63454,#63455) ;
#52645 = AXIS2_PLACEMENT_3D('',#91138,#63456,#63457) ;
#52646 = AXIS2_PLACEMENT_3D('',#91140,#63459,#63460) ;
#52647 = AXIS2_PLACEMENT_3D('',#91144,#63462,#63463) ;
#52648 = AXIS2_PLACEMENT_3D('',#91146,#63465,#63466) ;
#52649 = AXIS2_PLACEMENT_3D('',#91182,#63468,#63469) ;
#52650 = AXIS2_PLACEMENT_3D('',#91184,#63470,#63471) ;
#52651 = AXIS2_PLACEMENT_3D('',#91186,#63472,#63473) ;
#52652 = AXIS2_PLACEMENT_3D('',#91187,#63474,#63475) ;
#52653 = AXIS2_PLACEMENT_3D('',#91188,#63476,#63477) ;
#52654 = AXIS2_PLACEMENT_3D('',#91191,#63480,#63481) ;
#52655 = AXIS2_PLACEMENT_3D('',#91195,#63483,#63484) ;
#52656 = AXIS2_PLACEMENT_3D('',#91199,#63487,#63488) ;
#52657 = AXIS2_PLACEMENT_3D('',#91202,#63490,#63491) ;
#52658 = AXIS2_PLACEMENT_3D('',#91203,#63492,#63493) ;
#52659 = AXIS2_PLACEMENT_3D('',#91213,#63499,#63500) ;
#52660 = AXIS2_PLACEMENT_3D('',#91215,#63501,#63502) ;
#52661 = AXIS2_PLACEMENT_3D('',#91217,#63503,#63504) ;
#52662 = AXIS2_PLACEMENT_3D('',#91219,#63505,#63506) ;
#52663 = AXIS2_PLACEMENT_3D('',#91220,#63507,#63508) ;
#52664 = AXIS2_PLACEMENT_3D('',#91221,#63509,#63510) ;
#52665 = AXIS2_PLACEMENT_3D('',#91223,#63512,#63513) ;
#52666 = AXIS2_PLACEMENT_3D('',#91227,#63515,#63516) ;
#52667 = AXIS2_PLACEMENT_3D('',#91229,#63518,#63519) ;
#52668 = AXIS2_PLACEMENT_3D('',#91236,#63523,#63524) ;
#52669 = AXIS2_PLACEMENT_3D('',#91237,#63525,#63526) ;
#52670 = AXIS2_PLACEMENT_3D('',#91239,#63527,#63528) ;
#52671 = AXIS2_PLACEMENT_3D('',#91241,#63529,#63530) ;
#52672 = AXIS2_PLACEMENT_3D('',#91242,#63531,#63532) ;
#52673 = AXIS2_PLACEMENT_3D('',#91243,#63533,#63534) ;
#52674 = AXIS2_PLACEMENT_3D('',#91244,#63535,#63536) ;
#52675 = AXIS2_PLACEMENT_3D('',#91245,#63537,#63538) ;
#52676 = AXIS2_PLACEMENT_3D('',#91247,#63539,#63540) ;
#52677 = AXIS2_PLACEMENT_3D('',#91249,#63542,#63543) ;
#52678 = AXIS2_PLACEMENT_3D('',#91251,#63544,#63545) ;
#52679 = AXIS2_PLACEMENT_3D('',#91253,#63546,#63547) ;
#52680 = AXIS2_PLACEMENT_3D('',#91254,#63548,#63549) ;
#52681 = AXIS2_PLACEMENT_3D('',#91255,#63550,#63551) ;
#52682 = AXIS2_PLACEMENT_3D('',#91257,#63552,#63553) ;
#52683 = AXIS2_PLACEMENT_3D('',#91258,#63554,#63555) ;
#52684 = AXIS2_PLACEMENT_3D('',#91259,#63556,#63557) ;
#52685 = AXIS2_PLACEMENT_3D('',#91261,#63559,#63560) ;
#52686 = AXIS2_PLACEMENT_3D('',#91263,#63561,#63562) ;
#52687 = AXIS2_PLACEMENT_3D('',#91265,#63563,#63564) ;
#52688 = AXIS2_PLACEMENT_3D('',#91266,#63565,#63566) ;
#52689 = AXIS2_PLACEMENT_3D('',#91267,#63567,#63568) ;
#52690 = AXIS2_PLACEMENT_3D('',#91270,#63569,#63570) ;
#52691 = AXIS2_PLACEMENT_3D('',#91273,#63573,#63574) ;
#52692 = AXIS2_PLACEMENT_3D('',#91275,#63575,#63576) ;
#52693 = AXIS2_PLACEMENT_3D('',#91276,#63577,#63578) ;
#52694 = AXIS2_PLACEMENT_3D('',#91277,#63579,#63580) ;
#52695 = AXIS2_PLACEMENT_3D('',#91278,#63581,#63582) ;
#52696 = AXIS2_PLACEMENT_3D('',#91280,#63584,#63585) ;
#52697 = AXIS2_PLACEMENT_3D('',#91292,#63592,#63593) ;
#52698 = AXIS2_PLACEMENT_3D('',#91295,#63595,#63596) ;
#52699 = AXIS2_PLACEMENT_3D('',#91296,#63597,#63598) ;
#52700 = AXIS2_PLACEMENT_3D('',#91300,#63600,#63601) ;
#52701 = AXIS2_PLACEMENT_3D('',#91307,#63605,#63606) ;
#52702 = AXIS2_PLACEMENT_3D('',#91308,#63607,#63608) ;
#52703 = AXIS2_PLACEMENT_3D('',#91319,#63609,#63610) ;
#52704 = AXIS2_PLACEMENT_3D('',#91322,#63611,#63612) ;
#52705 = AXIS2_PLACEMENT_3D('',#91324,#63613,#63614) ;
#52706 = AXIS2_PLACEMENT_3D('',#91325,#63615,#63616) ;
#52707 = AXIS2_PLACEMENT_3D('',#91326,#63617,#63618) ;
#52708 = AXIS2_PLACEMENT_3D('',#91329,#63619,#63620) ;
#52709 = AXIS2_PLACEMENT_3D('',#91332,#63623,#63624) ;
#52710 = AXIS2_PLACEMENT_3D('',#91352,#63625,#63626) ;
#52711 = AXIS2_PLACEMENT_3D('',#91354,#63627,#63628) ;
#52712 = AXIS2_PLACEMENT_3D('',#91355,#63629,#63630) ;
#52713 = AXIS2_PLACEMENT_3D('',#91356,#63631,#63632) ;
#52714 = AXIS2_PLACEMENT_3D('',#91359,#63633,#63634) ;
#52715 = AXIS2_PLACEMENT_3D('',#91362,#63637,#63638) ;
#52716 = AXIS2_PLACEMENT_3D('',#91365,#63639,#63640) ;
#52717 = AXIS2_PLACEMENT_3D('',#91366,#63641,#63642) ;
#52718 = AXIS2_PLACEMENT_3D('',#91367,#63643,#63644) ;
#52719 = AXIS2_PLACEMENT_3D('',#91368,#63645,#63646) ;
#52720 = AXIS2_PLACEMENT_3D('',#91371,#63647,#63648) ;
#52721 = AXIS2_PLACEMENT_3D('',#91372,#63649,#63650) ;
#52722 = AXIS2_PLACEMENT_3D('',#91373,#63651,#63652) ;
#52723 = AXIS2_PLACEMENT_3D('',#91374,#63653,#63654) ;
#52724 = AXIS2_PLACEMENT_3D('',#91377,#63655,#63656) ;
#52725 = AXIS2_PLACEMENT_3D('',#91380,#63659,#63660) ;
#52726 = AXIS2_PLACEMENT_3D('',#91383,#63661,#63662) ;
#52727 = AXIS2_PLACEMENT_3D('',#91384,#63663,#63664) ;
#52728 = AXIS2_PLACEMENT_3D('',#91385,#63665,#63666) ;
#52729 = AXIS2_PLACEMENT_3D('',#91386,#63667,#63668) ;
#52730 = AXIS2_PLACEMENT_3D('',#91389,#63671,#63672) ;
#52731 = AXIS2_PLACEMENT_3D('',#91392,#63673,#63674) ;
#52732 = AXIS2_PLACEMENT_3D('',#91395,#63677,#63678) ;
#52733 = AXIS2_PLACEMENT_3D('',#91404,#63679,#63680) ;
#52734 = AXIS2_PLACEMENT_3D('',#91405,#63681,#63682) ;
#52735 = AXIS2_PLACEMENT_3D('',#91406,#63683,#63684) ;
#52736 = AXIS2_PLACEMENT_3D('',#91410,#63686,#63687) ;
#52737 = AXIS2_PLACEMENT_3D('',#91414,#63689,#63690) ;
#52738 = AXIS2_PLACEMENT_3D('',#91422,#63694,#63695) ;
#52739 = AXIS2_PLACEMENT_3D('',#91424,#63696,#63697) ;
#52740 = AXIS2_PLACEMENT_3D('',#91425,#63698,#63699) ;
#52741 = AXIS2_PLACEMENT_3D('',#91426,#63700,#63701) ;
#52742 = AXIS2_PLACEMENT_3D('',#91429,#63703,#63704) ;
#52743 = AXIS2_PLACEMENT_3D('',#91430,#63705,#63706) ;
#52744 = AXIS2_PLACEMENT_3D('',#91434,#63709,#63710) ;
#52745 = AXIS2_PLACEMENT_3D('',#91437,#63711,#63712) ;
#52746 = AXIS2_PLACEMENT_3D('',#91441,#63714,#63715) ;
#52747 = AXIS2_PLACEMENT_3D('',#91444,#63717,#63718) ;
#52748 = AXIS2_PLACEMENT_3D('',#91512,#63719,#63720) ;
#52749 = AXIS2_PLACEMENT_3D('',#91514,#63721,#63722) ;
#52750 = AXIS2_PLACEMENT_3D('',#91517,#63724,#63725) ;
#52751 = AXIS2_PLACEMENT_3D('',#91518,#63726,#63727) ;
#52752 = AXIS2_PLACEMENT_3D('',#91522,#63729,#63730) ;
#52753 = AXIS2_PLACEMENT_3D('',#91572,#63732,#63733) ;
#52754 = AXIS2_PLACEMENT_3D('',#91578,#63737,#63738) ;
#52755 = AXIS2_PLACEMENT_3D('',#91581,#63739,#63740) ;
#52756 = AXIS2_PLACEMENT_3D('',#91582,#63741,#63742) ;
#52757 = AXIS2_PLACEMENT_3D('',#91584,#63743,#63744) ;
#52758 = AXIS2_PLACEMENT_3D('',#91585,#63745,#63746) ;
#52759 = AXIS2_PLACEMENT_3D('',#91586,#63747,#63748) ;
#52760 = AXIS2_PLACEMENT_3D('',#91588,#63749,#63750) ;
#52761 = AXIS2_PLACEMENT_3D('',#91590,#63752,#63753) ;
#52762 = AXIS2_PLACEMENT_3D('',#91591,#63754,#63755) ;
#52763 = AXIS2_PLACEMENT_3D('',#91592,#63756,#63757) ;
#52764 = AXIS2_PLACEMENT_3D('',#91594,#63758,#63759) ;
#52765 = AXIS2_PLACEMENT_3D('',#91622,#63761,#63762) ;
#52766 = AXIS2_PLACEMENT_3D('',#91649,#63763,#63764) ;
#52767 = AXIS2_PLACEMENT_3D('',#91650,#63765,#63766) ;
#52768 = AXIS2_PLACEMENT_3D('',#91651,#63767,#63768) ;
#52769 = AXIS2_PLACEMENT_3D('',#91652,#63769,#63770) ;
#52770 = AXIS2_PLACEMENT_3D('',#91655,#63771,#63772) ;
#52771 = AXIS2_PLACEMENT_3D('',#91695,#63775,#63776) ;
#52772 = AXIS2_PLACEMENT_3D('',#91697,#63777,#63778) ;
#52773 = AXIS2_PLACEMENT_3D('',#91704,#63779,#63780) ;
#52774 = AXIS2_PLACEMENT_3D('',#91706,#63781,#63782) ;
#52775 = AXIS2_PLACEMENT_3D('',#91708,#63783,#63784) ;
#52776 = AXIS2_PLACEMENT_3D('',#91709,#63785,#63786) ;
#52777 = AXIS2_PLACEMENT_3D('',#91710,#63787,#63788) ;
#52778 = AXIS2_PLACEMENT_3D('',#91712,#63789,#63790) ;
#52779 = AXIS2_PLACEMENT_3D('',#91714,#63792,#63793) ;
#52780 = AXIS2_PLACEMENT_3D('',#91716,#63794,#63795) ;
#52781 = AXIS2_PLACEMENT_3D('',#91717,#63796,#63797) ;
#52782 = AXIS2_PLACEMENT_3D('',#91718,#63798,#63799) ;
#52783 = AXIS2_PLACEMENT_3D('',#91720,#63800,#63801) ;
#52784 = AXIS2_PLACEMENT_3D('',#91722,#63803,#63804) ;
#52785 = AXIS2_PLACEMENT_3D('',#91725,#63805,#63806) ;
#52786 = AXIS2_PLACEMENT_3D('',#91726,#63807,#63808) ;
#52787 = AXIS2_PLACEMENT_3D('',#91727,#63809,#63810) ;
#52788 = AXIS2_PLACEMENT_3D('',#91728,#63811,#63812) ;
#52789 = AXIS2_PLACEMENT_3D('',#91731,#63813,#63814) ;
#52790 = AXIS2_PLACEMENT_3D('',#91734,#63817,#63818) ;
#52791 = AXIS2_PLACEMENT_3D('',#91735,#63819,#63820) ;
#52792 = AXIS2_PLACEMENT_3D('',#91736,#63821,#63822) ;
#52793 = AXIS2_PLACEMENT_3D('',#91737,#63823,#63824) ;
#52794 = AXIS2_PLACEMENT_3D('',#91740,#63826,#63827) ;
#52795 = AXIS2_PLACEMENT_3D('',#91741,#63828,#63829) ;
#52796 = AXIS2_PLACEMENT_3D('',#91745,#63832,#63833) ;
#52797 = AXIS2_PLACEMENT_3D('',#91748,#63835,#63836) ;
#52798 = AXIS2_PLACEMENT_3D('',#91749,#63837,#63838) ;
#52799 = AXIS2_PLACEMENT_3D('',#91757,#63843,#63844) ;
#52800 = AXIS2_PLACEMENT_3D('',#91760,#63846,#63847) ;
#52801 = AXIS2_PLACEMENT_3D('',#91761,#63848,#63849) ;
#52802 = AXIS2_PLACEMENT_3D('',#91763,#63850,#63851) ;
#52803 = AXIS2_PLACEMENT_3D('',#91791,#63853,#63854) ;
#52804 = AXIS2_PLACEMENT_3D('',#91853,#63855,#63856) ;
#52805 = AXIS2_PLACEMENT_3D('',#91854,#63857,#63858) ;
#52806 = AXIS2_PLACEMENT_3D('',#91855,#63859,#63860) ;
#52807 = AXIS2_PLACEMENT_3D('',#91856,#63861,#63862) ;
#52808 = AXIS2_PLACEMENT_3D('',#91859,#63863,#63864) ;
#52809 = AXIS2_PLACEMENT_3D('',#91884,#63867,#63868) ;
#52810 = AXIS2_PLACEMENT_3D('',#91885,#63869,#63870) ;
#52811 = AXIS2_PLACEMENT_3D('',#91886,#63871,#63872) ;
#52812 = AXIS2_PLACEMENT_3D('',#91909,#63873,#63874) ;
#52813 = AXIS2_PLACEMENT_3D('',#91910,#63875,#63876) ;
#52814 = AXIS2_PLACEMENT_3D('',#91911,#63877,#63878) ;
#52815 = AXIS2_PLACEMENT_3D('',#91929,#63879,#63880) ;
#52816 = AXIS2_PLACEMENT_3D('',#91941,#63881,#63882) ;
#52817 = AXIS2_PLACEMENT_3D('',#91942,#63883,#63884) ;
#52818 = AXIS2_PLACEMENT_3D('',#91951,#63886,#63887) ;
#52819 = AXIS2_PLACEMENT_3D('',#91953,#63889,#63890) ;
#52820 = AXIS2_PLACEMENT_3D('',#91971,#63895,#63896) ;
#52821 = AXIS2_PLACEMENT_3D('',#91972,#63897,#63898) ;
#52822 = AXIS2_PLACEMENT_3D('',#91974,#63900,#63901) ;
#52823 = AXIS2_PLACEMENT_3D('',#91977,#63903,#63904) ;
#52824 = AXIS2_PLACEMENT_3D('',#91978,#63905,#63906) ;
#52825 = AXIS2_PLACEMENT_3D('',#91980,#63907,#63908) ;
#52826 = AXIS2_PLACEMENT_3D('',#91997,#63910,#63911) ;
#52827 = AXIS2_PLACEMENT_3D('',#91999,#63912,#63913) ;
#52828 = AXIS2_PLACEMENT_3D('',#92014,#63914,#63915) ;
#52829 = AXIS2_PLACEMENT_3D('',#92017,#63917,#63918) ;
#52830 = AXIS2_PLACEMENT_3D('',#92018,#63919,#63920) ;
#52831 = AXIS2_PLACEMENT_3D('',#92020,#63922,#63923) ;
#52832 = AXIS2_PLACEMENT_3D('',#92024,#63925,#63926) ;
#52833 = AXIS2_PLACEMENT_3D('',#92026,#63928,#63929) ;
#52834 = AXIS2_PLACEMENT_3D('',#92030,#63932,#63933) ;
#52835 = AXIS2_PLACEMENT_3D('',#92053,#63934,#63935) ;
#52836 = AXIS2_PLACEMENT_3D('',#92055,#63936,#63937) ;
#52837 = AXIS2_PLACEMENT_3D('',#92056,#63938,#63939) ;
#52838 = AXIS2_PLACEMENT_3D('',#92057,#63940,#63941) ;
#52839 = AXIS2_PLACEMENT_3D('',#92060,#63942,#63943) ;
#52840 = AXIS2_PLACEMENT_3D('',#92061,#63944,#63945) ;
#52841 = AXIS2_PLACEMENT_3D('',#92062,#63946,#63947) ;
#52842 = AXIS2_PLACEMENT_3D('',#92063,#63948,#63949) ;
#52843 = AXIS2_PLACEMENT_3D('',#92090,#63952,#63953) ;
#52844 = AXIS2_PLACEMENT_3D('',#92100,#63959,#63960) ;
#52845 = AXIS2_PLACEMENT_3D('',#92103,#63962,#63963) ;
#52846 = AXIS2_PLACEMENT_3D('',#92104,#63964,#63965) ;
#52847 = AXIS2_PLACEMENT_3D('',#92108,#63967,#63968) ;
#52848 = AXIS2_PLACEMENT_3D('',#92110,#63970,#63971) ;
#52849 = AXIS2_PLACEMENT_3D('',#92113,#63972,#63973) ;
#52850 = AXIS2_PLACEMENT_3D('',#92115,#63974,#63975) ;
#52851 = AXIS2_PLACEMENT_3D('',#92116,#63976,#63977) ;
#52852 = AXIS2_PLACEMENT_3D('',#92117,#63978,#63979) ;
#52853 = AXIS2_PLACEMENT_3D('',#92120,#63982,#63983) ;
#52854 = AXIS2_PLACEMENT_3D('',#92123,#63986,#63987) ;
#52855 = AXIS2_PLACEMENT_3D('',#92126,#63988,#63989) ;
#52856 = AXIS2_PLACEMENT_3D('',#92128,#63990,#63991) ;
#52857 = AXIS2_PLACEMENT_3D('',#92130,#63992,#63993) ;
#52858 = AXIS2_PLACEMENT_3D('',#92131,#63994,#63995) ;
#52859 = AXIS2_PLACEMENT_3D('',#92132,#63996,#63997) ;
#52860 = AXIS2_PLACEMENT_3D('',#92135,#64000,#64001) ;
#52861 = AXIS2_PLACEMENT_3D('',#92138,#64004,#64005) ;
#52862 = AXIS2_PLACEMENT_3D('',#92141,#64008,#64009) ;
#52863 = AXIS2_PLACEMENT_3D('',#92145,#64011,#64012) ;
#52864 = AXIS2_PLACEMENT_3D('',#92149,#64014,#64015) ;
#52865 = AXIS2_PLACEMENT_3D('',#92153,#64017,#64018) ;
#52866 = AXIS2_PLACEMENT_3D('',#92157,#64020,#64021) ;
#52867 = AXIS2_PLACEMENT_3D('',#92169,#64027,#64028) ;
#52868 = AXIS2_PLACEMENT_3D('',#92173,#64030,#64031) ;
#52869 = AXIS2_PLACEMENT_3D('',#92177,#64033,#64034) ;
#52870 = AXIS2_PLACEMENT_3D('',#92181,#64036,#64037) ;
#52871 = AXIS2_PLACEMENT_3D('',#92185,#64039,#64040) ;
#52872 = AXIS2_PLACEMENT_3D('',#92189,#64042,#64043) ;
#52873 = AXIS2_PLACEMENT_3D('',#92197,#64047,#64048) ;
#52874 = AXIS2_PLACEMENT_3D('',#92201,#64050,#64051) ;
#52875 = AXIS2_PLACEMENT_3D('',#92205,#64053,#64054) ;
#52876 = AXIS2_PLACEMENT_3D('',#92209,#64056,#64057) ;
#52877 = AXIS2_PLACEMENT_3D('',#92213,#64059,#64060) ;
#52878 = AXIS2_PLACEMENT_3D('',#92249,#64071,#64072) ;
#52879 = AXIS2_PLACEMENT_3D('',#92253,#64074,#64075) ;
#52880 = AXIS2_PLACEMENT_3D('',#92259,#64078,#64079) ;
#52881 = AXIS2_PLACEMENT_3D('',#92265,#64082,#64083) ;
#52882 = AXIS2_PLACEMENT_3D('',#92282,#64088,#64089) ;
#52883 = AXIS2_PLACEMENT_3D('',#92284,#64090,#64091) ;
#52884 = AXIS2_PLACEMENT_3D('',#92286,#64092,#64093) ;
#52885 = AXIS2_PLACEMENT_3D('',#92288,#64094,#64095) ;
#52886 = AXIS2_PLACEMENT_3D('',#92292,#64097,#64098) ;
#52887 = AXIS2_PLACEMENT_3D('',#92298,#64101,#64102) ;
#52888 = AXIS2_PLACEMENT_3D('',#92302,#64104,#64105) ;
#52889 = AXIS2_PLACEMENT_3D('',#92308,#64108,#64109) ;
#52890 = AXIS2_PLACEMENT_3D('',#92312,#64111,#64112) ;
#52891 = AXIS2_PLACEMENT_3D('',#92320,#64116,#64117) ;
#52892 = AXIS2_PLACEMENT_3D('',#92324,#64119,#64120) ;
#52893 = AXIS2_PLACEMENT_3D('',#92328,#64122,#64123) ;
#52894 = AXIS2_PLACEMENT_3D('',#92332,#64125,#64126) ;
#52895 = AXIS2_PLACEMENT_3D('',#92337,#64129,#64130) ;
#52896 = AXIS2_PLACEMENT_3D('',#92339,#64131,#64132) ;
#52897 = AXIS2_PLACEMENT_3D('',#92343,#64134,#64135) ;
#52898 = AXIS2_PLACEMENT_3D('',#92349,#64138,#64139) ;
#52899 = AXIS2_PLACEMENT_3D('',#92353,#64141,#64142) ;
#52900 = AXIS2_PLACEMENT_3D('',#92355,#64143,#64144) ;
#52901 = AXIS2_PLACEMENT_3D('',#92361,#64147,#64148) ;
#52902 = AXIS2_PLACEMENT_3D('',#92365,#64150,#64151) ;
#52903 = AXIS2_PLACEMENT_3D('',#92369,#64153,#64154) ;
#52904 = AXIS2_PLACEMENT_3D('',#92373,#64156,#64157) ;
#52905 = AXIS2_PLACEMENT_3D('',#92376,#64159,#64160) ;
#52906 = AXIS2_PLACEMENT_3D('',#92379,#64161,#64162) ;
#52907 = AXIS2_PLACEMENT_3D('',#92383,#64164,#64165) ;
#52908 = AXIS2_PLACEMENT_3D('',#92389,#64168,#64169) ;
#52909 = AXIS2_PLACEMENT_3D('',#92393,#64171,#64172) ;
#52910 = AXIS2_PLACEMENT_3D('',#92397,#64174,#64175) ;
#52911 = AXIS2_PLACEMENT_3D('',#92401,#64177,#64178) ;
#52912 = AXIS2_PLACEMENT_3D('',#92406,#64181,#64182) ;
#52913 = AXIS2_PLACEMENT_3D('',#92420,#64185,#64186) ;
#52914 = AXIS2_PLACEMENT_3D('',#92424,#64188,#64189) ;
#52915 = AXIS2_PLACEMENT_3D('',#92428,#64191,#64192) ;
#52916 = AXIS2_PLACEMENT_3D('',#92432,#64194,#64195) ;
#52917 = AXIS2_PLACEMENT_3D('',#92455,#64200,#64201) ;
#52918 = AXIS2_PLACEMENT_3D('',#92459,#64203,#64204) ;
#52919 = AXIS2_PLACEMENT_3D('',#92463,#64206,#64207) ;
#52920 = AXIS2_PLACEMENT_3D('',#92467,#64209,#64210) ;
#52921 = AXIS2_PLACEMENT_3D('',#92473,#64213,#64214) ;
#52922 = AXIS2_PLACEMENT_3D('',#92477,#64216,#64217) ;
#52923 = AXIS2_PLACEMENT_3D('',#92483,#64220,#64221) ;
#52924 = AXIS2_PLACEMENT_3D('',#92487,#64223,#64224) ;
#52925 = AXIS2_PLACEMENT_3D('',#92491,#64226,#64227) ;
#52926 = AXIS2_PLACEMENT_3D('',#92495,#64229,#64230) ;
#52927 = AXIS2_PLACEMENT_3D('',#92499,#64233,#64234) ;
#52928 = AXIS2_PLACEMENT_3D('',#92567,#64235,#64236) ;
#52929 = AXIS2_PLACEMENT_3D('',#92576,#64237,#64238) ;
#52930 = AXIS2_PLACEMENT_3D('',#92577,#64239,#64240) ;
#52931 = AXIS2_PLACEMENT_3D('',#92580,#64243,#64244) ;
#52932 = AXIS2_PLACEMENT_3D('',#92601,#64245,#64246) ;
#52933 = AXIS2_PLACEMENT_3D('',#92602,#64247,#64248) ;
#52934 = AXIS2_PLACEMENT_3D('',#92604,#64249,#64250) ;
#52935 = AXIS2_PLACEMENT_3D('',#92605,#64251,#64252) ;
#52936 = AXIS2_PLACEMENT_3D('',#92606,#64253,#64254) ;
#52937 = AXIS2_PLACEMENT_3D('',#92608,#64255,#64256) ;
#52938 = AXIS2_PLACEMENT_3D('',#92610,#64258,#64259) ;
#52939 = AXIS2_PLACEMENT_3D('',#92612,#64261,#64262) ;
#52940 = AXIS2_PLACEMENT_3D('',#92616,#64264,#64265) ;
#52941 = AXIS2_PLACEMENT_3D('',#92618,#64267,#64268) ;
#52942 = AXIS2_PLACEMENT_3D('',#92625,#64273,#64274) ;
#52943 = AXIS2_PLACEMENT_3D('',#92632,#64279,#64280) ;
#52944 = AXIS2_PLACEMENT_3D('',#92635,#64281,#64282) ;
#52945 = AXIS2_PLACEMENT_3D('',#92637,#64283,#64284) ;
#52946 = AXIS2_PLACEMENT_3D('',#92638,#64285,#64286) ;
#52947 = AXIS2_PLACEMENT_3D('',#92639,#64287,#64288) ;
#52948 = AXIS2_PLACEMENT_3D('',#92643,#64290,#64291) ;
#52949 = AXIS2_PLACEMENT_3D('',#92645,#64293,#64294) ;
#52950 = AXIS2_PLACEMENT_3D('',#92648,#64295,#64296) ;
#52951 = AXIS2_PLACEMENT_3D('',#92649,#64297,#64298) ;
#52952 = AXIS2_PLACEMENT_3D('',#92650,#64299,#64300) ;
#52953 = AXIS2_PLACEMENT_3D('',#92651,#64301,#64302) ;
#52954 = AXIS2_PLACEMENT_3D('',#92654,#64303,#64304) ;
#52955 = AXIS2_PLACEMENT_3D('',#92657,#64307,#64308) ;
#52956 = AXIS2_PLACEMENT_3D('',#92660,#64309,#64310) ;
#52957 = AXIS2_PLACEMENT_3D('',#92661,#64311,#64312) ;
#52958 = AXIS2_PLACEMENT_3D('',#92662,#64313,#64314) ;
#52959 = AXIS2_PLACEMENT_3D('',#92663,#64315,#64316) ;
#52960 = AXIS2_PLACEMENT_3D('',#92666,#64319,#64320) ;
#52961 = AXIS2_PLACEMENT_3D('',#92686,#64322,#64323) ;
#52962 = AXIS2_PLACEMENT_3D('',#92688,#64325,#64326) ;
#52963 = AXIS2_PLACEMENT_3D('',#92691,#64327,#64328) ;
#52964 = AXIS2_PLACEMENT_3D('',#92692,#64329,#64330) ;
#52965 = AXIS2_PLACEMENT_3D('',#92693,#64331,#64332) ;
#52966 = AXIS2_PLACEMENT_3D('',#92694,#64333,#64334) ;
#52967 = AXIS2_PLACEMENT_3D('',#92747,#64337,#64338) ;
#52968 = AXIS2_PLACEMENT_3D('',#92749,#64339,#64340) ;
#52969 = AXIS2_PLACEMENT_3D('',#92751,#64341,#64342) ;
#52970 = AXIS2_PLACEMENT_3D('',#92752,#64343,#64344) ;
#52971 = AXIS2_PLACEMENT_3D('',#92753,#64345,#64346) ;
#52972 = AXIS2_PLACEMENT_3D('',#92755,#64347,#64348) ;
#52973 = AXIS2_PLACEMENT_3D('',#92756,#64349,#64350) ;
#52974 = AXIS2_PLACEMENT_3D('',#92767,#64351,#64352) ;
#52975 = AXIS2_PLACEMENT_3D('',#92768,#64353,#64354) ;
#52976 = AXIS2_PLACEMENT_3D('',#92769,#64355,#64356) ;
#52977 = AXIS2_PLACEMENT_3D('',#92771,#64357,#64358) ;
#52978 = AXIS2_PLACEMENT_3D('',#92773,#64360,#64361) ;
#52979 = AXIS2_PLACEMENT_3D('',#92775,#64362,#64363) ;
#52980 = AXIS2_PLACEMENT_3D('',#92776,#64364,#64365) ;
#52981 = AXIS2_PLACEMENT_3D('',#92777,#64366,#64367) ;
#52982 = AXIS2_PLACEMENT_3D('',#92779,#64369,#64370) ;
#52983 = AXIS2_PLACEMENT_3D('',#92782,#64373,#64374) ;
#52984 = AXIS2_PLACEMENT_3D('',#92784,#64375,#64376) ;
#52985 = AXIS2_PLACEMENT_3D('',#92786,#64378,#64379) ;
#52986 = AXIS2_PLACEMENT_3D('',#92788,#64380,#64381) ;
#52987 = AXIS2_PLACEMENT_3D('',#92789,#64382,#64383) ;
#52988 = AXIS2_PLACEMENT_3D('',#92790,#64384,#64385) ;
#52989 = AXIS2_PLACEMENT_3D('',#92792,#64386,#64387) ;
#52990 = AXIS2_PLACEMENT_3D('',#92839,#64389,#64390) ;
#52991 = AXIS2_PLACEMENT_3D('',#92844,#64393,#64394) ;
#52992 = AXIS2_PLACEMENT_3D('',#92845,#64395,#64396) ;
#52993 = AXIS2_PLACEMENT_3D('',#92852,#64400,#64401) ;
#52994 = AXIS2_PLACEMENT_3D('',#92853,#64402,#64403) ;
#52995 = AXIS2_PLACEMENT_3D('',#92856,#64405,#64406) ;
#52996 = AXIS2_PLACEMENT_3D('',#92857,#64407,#64408) ;
#52997 = AXIS2_PLACEMENT_3D('',#92861,#64411,#64412) ;
#52998 = AXIS2_PLACEMENT_3D('',#92864,#64414,#64415) ;
#52999 = AXIS2_PLACEMENT_3D('',#92865,#64416,#64417) ;
#53000 = AXIS2_PLACEMENT_3D('',#92871,#64420,#64421) ;
#53001 = AXIS2_PLACEMENT_3D('',#92875,#64423,#64424) ;
#53002 = AXIS2_PLACEMENT_3D('',#92879,#64426,#64427) ;
#53003 = AXIS2_PLACEMENT_3D('',#92881,#64429,#64430) ;
#53004 = AXIS2_PLACEMENT_3D('',#92884,#64432,#64433) ;
#53005 = AXIS2_PLACEMENT_3D('',#92885,#64434,#64435) ;
#53006 = AXIS2_PLACEMENT_3D('',#92889,#64438,#64439) ;
#53007 = AXIS2_PLACEMENT_3D('',#92892,#64441,#64442) ;
#53008 = AXIS2_PLACEMENT_3D('',#92893,#64443,#64444) ;
#53009 = AXIS2_PLACEMENT_3D('',#92895,#64445,#64446) ;
#53010 = AXIS2_PLACEMENT_3D('',#92901,#64447,#64448) ;
#53011 = AXIS2_PLACEMENT_3D('',#92934,#64449,#64450) ;
#53012 = AXIS2_PLACEMENT_3D('',#92962,#64451,#64452) ;
#53013 = AXIS2_PLACEMENT_3D('',#92969,#64453,#64454) ;
#53014 = AXIS2_PLACEMENT_3D('',#92972,#64455,#64456) ;
#53015 = AXIS2_PLACEMENT_3D('',#92975,#64459,#64460) ;
#53016 = AXIS2_PLACEMENT_3D('',#92978,#64461,#64462) ;
#53017 = AXIS2_PLACEMENT_3D('',#92980,#64463,#64464) ;
#53018 = AXIS2_PLACEMENT_3D('',#92982,#64465,#64466) ;
#53019 = AXIS2_PLACEMENT_3D('',#92983,#64467,#64468) ;
#53020 = AXIS2_PLACEMENT_3D('',#92984,#64469,#64470) ;
#53021 = AXIS2_PLACEMENT_3D('',#92987,#64471,#64472) ;
#53022 = AXIS2_PLACEMENT_3D('',#92990,#64475,#64476) ;
#53023 = AXIS2_PLACEMENT_3D('',#92991,#64477,#64478) ;
#53024 = AXIS2_PLACEMENT_3D('',#92992,#64479,#64480) ;
#53025 = AXIS2_PLACEMENT_3D('',#92993,#64481,#64482) ;
#53026 = AXIS2_PLACEMENT_3D('',#92996,#64483,#64484) ;
#53027 = AXIS2_PLACEMENT_3D('',#92998,#64485,#64486) ;
#53028 = AXIS2_PLACEMENT_3D('',#93000,#64487,#64488) ;
#53029 = AXIS2_PLACEMENT_3D('',#93001,#64489,#64490) ;
#53030 = AXIS2_PLACEMENT_3D('',#93060,#64491,#64492) ;
#53031 = AXIS2_PLACEMENT_3D('',#93068,#64493,#64494) ;
#53032 = AXIS2_PLACEMENT_3D('',#93069,#64495,#64496) ;
#53033 = AXIS2_PLACEMENT_3D('',#93072,#64497,#64498) ;
#53034 = AXIS2_PLACEMENT_3D('',#93073,#64499,#64500) ;
#53035 = AXIS2_PLACEMENT_3D('',#93074,#64501,#64502) ;
#53036 = AXIS2_PLACEMENT_3D('',#93075,#64503,#64504) ;
#53037 = AXIS2_PLACEMENT_3D('',#93078,#64507,#64508) ;
#53038 = AXIS2_PLACEMENT_3D('',#93081,#64509,#64510) ;
#53039 = AXIS2_PLACEMENT_3D('',#93110,#64513,#64514) ;
#53040 = AXIS2_PLACEMENT_3D('',#93142,#64515,#64516) ;
#53041 = AXIS2_PLACEMENT_3D('',#93143,#64517,#64518) ;
#53042 = AXIS2_PLACEMENT_3D('',#93144,#64519,#64520) ;
#53043 = AXIS2_PLACEMENT_3D('',#93146,#64522,#64523) ;
#53044 = AXIS2_PLACEMENT_3D('',#93149,#64524,#64525) ;
#53045 = AXIS2_PLACEMENT_3D('',#93152,#64528,#64529) ;
#53046 = AXIS2_PLACEMENT_3D('',#93154,#64530,#64531) ;
#53047 = AXIS2_PLACEMENT_3D('',#93155,#64532,#64533) ;
#53048 = AXIS2_PLACEMENT_3D('',#93156,#64534,#64535) ;
#53049 = AXIS2_PLACEMENT_3D('',#93158,#64536,#64537) ;
#53050 = AXIS2_PLACEMENT_3D('',#93160,#64539,#64540) ;
#53051 = AXIS2_PLACEMENT_3D('',#93162,#64541,#64542) ;
#53052 = AXIS2_PLACEMENT_3D('',#93163,#64543,#64544) ;
#53053 = AXIS2_PLACEMENT_3D('',#93164,#64545,#64546) ;
#53054 = AXIS2_PLACEMENT_3D('',#93166,#64548,#64549) ;
#53055 = AXIS2_PLACEMENT_3D('',#93169,#64550,#64551) ;
#53056 = AXIS2_PLACEMENT_3D('',#93172,#64554,#64555) ;
#53057 = AXIS2_PLACEMENT_3D('',#93175,#64556,#64557) ;
#53058 = AXIS2_PLACEMENT_3D('',#93178,#64560,#64561) ;
#53059 = AXIS2_PLACEMENT_3D('',#93181,#64562,#64563) ;
#53060 = AXIS2_PLACEMENT_3D('',#93182,#64564,#64565) ;
#53061 = AXIS2_PLACEMENT_3D('',#93183,#64566,#64567) ;
#53062 = AXIS2_PLACEMENT_3D('',#93184,#64568,#64569) ;
#53063 = AXIS2_PLACEMENT_3D('',#93187,#64570,#64571) ;
#53064 = AXIS2_PLACEMENT_3D('',#93190,#64574,#64575) ;
#53065 = AXIS2_PLACEMENT_3D('',#93193,#64576,#64577) ;
#53066 = AXIS2_PLACEMENT_3D('',#93194,#64578,#64579) ;
#53067 = AXIS2_PLACEMENT_3D('',#93195,#64580,#64581) ;
#53068 = AXIS2_PLACEMENT_3D('',#93196,#64582,#64583) ;
#53069 = AXIS2_PLACEMENT_3D('',#93199,#64584,#64585) ;
#53070 = AXIS2_PLACEMENT_3D('',#93202,#64588,#64589) ;
#53071 = AXIS2_PLACEMENT_3D('',#93205,#64590,#64591) ;
#53072 = AXIS2_PLACEMENT_3D('',#93206,#64592,#64593) ;
#53073 = AXIS2_PLACEMENT_3D('',#93207,#64594,#64595) ;
#53074 = AXIS2_PLACEMENT_3D('',#93208,#64596,#64597) ;
#53075 = AXIS2_PLACEMENT_3D('',#93211,#64598,#64599) ;
#53076 = AXIS2_PLACEMENT_3D('',#93214,#64602,#64603) ;
#53077 = AXIS2_PLACEMENT_3D('',#93217,#64604,#64605) ;
#53078 = AXIS2_PLACEMENT_3D('',#93218,#64606,#64607) ;
#53079 = AXIS2_PLACEMENT_3D('',#93219,#64608,#64609) ;
#53080 = AXIS2_PLACEMENT_3D('',#93220,#64610,#64611) ;
#53081 = AXIS2_PLACEMENT_3D('',#93223,#64614,#64615) ;
#53082 = AXIS2_PLACEMENT_3D('',#93226,#64616,#64617) ;
#53083 = AXIS2_PLACEMENT_3D('',#93260,#64620,#64621) ;
#53084 = AXIS2_PLACEMENT_3D('',#93286,#64622,#64623) ;
#53085 = AXIS2_PLACEMENT_3D('',#93287,#64624,#64625) ;
#53086 = AXIS2_PLACEMENT_3D('',#93290,#64626,#64627) ;
#53087 = AXIS2_PLACEMENT_3D('',#93293,#64630,#64631) ;
#53088 = AXIS2_PLACEMENT_3D('',#93295,#64632,#64633) ;
#53089 = AXIS2_PLACEMENT_3D('',#93297,#64635,#64636) ;
#53090 = AXIS2_PLACEMENT_3D('',#93304,#64638,#64639) ;
#53091 = AXIS2_PLACEMENT_3D('',#93308,#64641,#64642) ;
#53092 = AXIS2_PLACEMENT_3D('',#93310,#64644,#64645) ;
#53093 = AXIS2_PLACEMENT_3D('',#93313,#64648,#64649) ;
#53094 = AXIS2_PLACEMENT_3D('',#93315,#64651,#64652) ;
#53095 = AXIS2_PLACEMENT_3D('',#93317,#64654,#64655) ;
#53096 = AXIS2_PLACEMENT_3D('',#93321,#64657,#64658) ;
#53097 = AXIS2_PLACEMENT_3D('',#93323,#64660,#64661) ;
#53098 = AXIS2_PLACEMENT_3D('',#93328,#64665,#64666) ;
#53099 = AXIS2_PLACEMENT_3D('',#93330,#64668,#64669) ;
#53100 = AXIS2_PLACEMENT_3D('',#93335,#64673,#64674) ;
#53101 = AXIS2_PLACEMENT_3D('',#93337,#64676,#64677) ;
#53102 = AXIS2_PLACEMENT_3D('',#93340,#64679,#64680) ;
#53103 = AXIS2_PLACEMENT_3D('',#93341,#64681,#64682) ;
#53104 = AXIS2_PLACEMENT_3D('',#93344,#64683,#64684) ;
#53105 = AXIS2_PLACEMENT_3D('',#93348,#64686,#64687) ;
#53106 = AXIS2_PLACEMENT_3D('',#93350,#64689,#64690) ;
#53107 = AXIS2_PLACEMENT_3D('',#93356,#64694,#64695) ;
#53108 = AXIS2_PLACEMENT_3D('',#93358,#64696,#64697) ;
#53109 = AXIS2_PLACEMENT_3D('',#93360,#64698,#64699) ;
#53110 = AXIS2_PLACEMENT_3D('',#93362,#64701,#64702) ;
#53111 = AXIS2_PLACEMENT_3D('',#93365,#64703,#64704) ;
#53112 = AXIS2_PLACEMENT_3D('',#93367,#64705,#64706) ;
#53113 = AXIS2_PLACEMENT_3D('',#93369,#64707,#64708) ;
#53114 = AXIS2_PLACEMENT_3D('',#93370,#64709,#64710) ;
#53115 = AXIS2_PLACEMENT_3D('',#93371,#64711,#64712) ;
#53116 = AXIS2_PLACEMENT_3D('',#93374,#64713,#64714) ;
#53117 = AXIS2_PLACEMENT_3D('',#93376,#64715,#64716) ;
#53118 = AXIS2_PLACEMENT_3D('',#93378,#64717,#64718) ;
#53119 = AXIS2_PLACEMENT_3D('',#93379,#64719,#64720) ;
#53120 = AXIS2_PLACEMENT_3D('',#93380,#64721,#64722) ;
#53121 = AXIS2_PLACEMENT_3D('',#93383,#64725,#64726) ;
#53122 = AXIS2_PLACEMENT_3D('',#93386,#64727,#64728) ;
#53123 = AXIS2_PLACEMENT_3D('',#93390,#64730,#64731) ;
#53124 = AXIS2_PLACEMENT_3D('',#93392,#64733,#64734) ;
#53125 = AXIS2_PLACEMENT_3D('',#93395,#64735,#64736) ;
#53126 = AXIS2_PLACEMENT_3D('',#93396,#64737,#64738) ;
#53127 = AXIS2_PLACEMENT_3D('',#93397,#64739,#64740) ;
#53128 = AXIS2_PLACEMENT_3D('',#93398,#64741,#64742) ;
#53129 = AXIS2_PLACEMENT_3D('',#93401,#64745,#64746) ;
#53130 = AXIS2_PLACEMENT_3D('',#93404,#64747,#64748) ;
#53131 = AXIS2_PLACEMENT_3D('',#93407,#64751,#64752) ;
#53132 = AXIS2_PLACEMENT_3D('',#93410,#64753,#64754) ;
#53133 = AXIS2_PLACEMENT_3D('',#93413,#64757,#64758) ;
#53134 = AXIS2_PLACEMENT_3D('',#93416,#64759,#64760) ;
#53135 = AXIS2_PLACEMENT_3D('',#93419,#64763,#64764) ;
#53136 = AXIS2_PLACEMENT_3D('',#93422,#64765,#64766) ;
#53137 = AXIS2_PLACEMENT_3D('',#93423,#64767,#64768) ;
#53138 = AXIS2_PLACEMENT_3D('',#93424,#64769,#64770) ;
#53139 = AXIS2_PLACEMENT_3D('',#93425,#64771,#64772) ;
#53140 = AXIS2_PLACEMENT_3D('',#93428,#64773,#64774) ;
#53141 = AXIS2_PLACEMENT_3D('',#93431,#64777,#64778) ;
#53142 = AXIS2_PLACEMENT_3D('',#93435,#64780,#64781) ;
#53143 = AXIS2_PLACEMENT_3D('',#93437,#64783,#64784) ;
#53144 = AXIS2_PLACEMENT_3D('',#93443,#64787,#64788) ;
#53145 = AXIS2_PLACEMENT_3D('',#93449,#64791,#64792) ;
#53146 = AXIS2_PLACEMENT_3D('',#93453,#64794,#64795) ;
#53147 = AXIS2_PLACEMENT_3D('',#93457,#64797,#64798) ;
#53148 = AXIS2_PLACEMENT_3D('',#93459,#64800,#64801) ;
#53149 = AXIS2_PLACEMENT_3D('',#93462,#64803,#64804) ;
#53150 = AXIS2_PLACEMENT_3D('',#93463,#64805,#64806) ;
#53151 = AXIS2_PLACEMENT_3D('',#93475,#64814,#64815) ;
#53152 = AXIS2_PLACEMENT_3D('',#93477,#64816,#64817) ;
#53153 = AXIS2_PLACEMENT_3D('',#93480,#64819,#64820) ;
#53154 = AXIS2_PLACEMENT_3D('',#93517,#64821,#64822) ;
#53155 = AXIS2_PLACEMENT_3D('',#93518,#64823,#64824) ;
#53156 = AXIS2_PLACEMENT_3D('',#93519,#64825,#64826) ;
#53157 = AXIS2_PLACEMENT_3D('',#93521,#64828,#64829) ;
#53158 = AXIS2_PLACEMENT_3D('',#93523,#64830,#64831) ;
#53159 = AXIS2_PLACEMENT_3D('',#93524,#64832,#64833) ;
#53160 = AXIS2_PLACEMENT_3D('',#93525,#64834,#64835) ;
#53161 = AXIS2_PLACEMENT_3D('',#93527,#64836,#64837) ;
#53162 = AXIS2_PLACEMENT_3D('',#93529,#64839,#64840) ;
#53163 = AXIS2_PLACEMENT_3D('',#93531,#64841,#64842) ;
#53164 = AXIS2_PLACEMENT_3D('',#93532,#64843,#64844) ;
#53165 = AXIS2_PLACEMENT_3D('',#93533,#64845,#64846) ;
#53166 = AXIS2_PLACEMENT_3D('',#93535,#64847,#64848) ;
#53167 = AXIS2_PLACEMENT_3D('',#93537,#64850,#64851) ;
#53168 = AXIS2_PLACEMENT_3D('',#93539,#64852,#64853) ;
#53169 = AXIS2_PLACEMENT_3D('',#93540,#64854,#64855) ;
#53170 = AXIS2_PLACEMENT_3D('',#93541,#64856,#64857) ;
#53171 = AXIS2_PLACEMENT_3D('',#93543,#64858,#64859) ;
#53172 = AXIS2_PLACEMENT_3D('',#93545,#64861,#64862) ;
#53173 = AXIS2_PLACEMENT_3D('',#93547,#64863,#64864) ;
#53174 = AXIS2_PLACEMENT_3D('',#93548,#64865,#64866) ;
#53175 = AXIS2_PLACEMENT_3D('',#93549,#64867,#64868) ;
#53176 = AXIS2_PLACEMENT_3D('',#93551,#64869,#64870) ;
#53177 = AXIS2_PLACEMENT_3D('',#93553,#64872,#64873) ;
#53178 = AXIS2_PLACEMENT_3D('',#93555,#64874,#64875) ;
#53179 = AXIS2_PLACEMENT_3D('',#93556,#64876,#64877) ;
#53180 = AXIS2_PLACEMENT_3D('',#93557,#64878,#64879) ;
#53181 = AXIS2_PLACEMENT_3D('',#93559,#64880,#64881) ;
#53182 = AXIS2_PLACEMENT_3D('',#93586,#64883,#64884) ;
#53183 = AXIS2_PLACEMENT_3D('',#93587,#64885,#64886) ;
#53184 = AXIS2_PLACEMENT_3D('',#93588,#64887,#64888) ;
#53185 = AXIS2_PLACEMENT_3D('',#93590,#64889,#64890) ;
#53186 = AXIS2_PLACEMENT_3D('',#93621,#64892,#64893) ;
#53187 = AXIS2_PLACEMENT_3D('',#93622,#64894,#64895) ;
#53188 = AXIS2_PLACEMENT_3D('',#93652,#64896,#64897) ;
#53189 = AXIS2_PLACEMENT_3D('',#93653,#64898,#64899) ;
#53190 = AXIS2_PLACEMENT_3D('',#93678,#64900,#64901) ;
#53191 = AXIS2_PLACEMENT_3D('',#93683,#64902,#64903) ;
#53192 = AXIS2_PLACEMENT_3D('',#93684,#64904,#64905) ;
#53193 = AXIS2_PLACEMENT_3D('',#93685,#64906,#64907) ;
#53194 = AXIS2_PLACEMENT_3D('',#93686,#64908,#64909) ;
#53195 = AXIS2_PLACEMENT_3D('',#93687,#64910,#64911) ;
#53196 = AXIS2_PLACEMENT_3D('',#93689,#64912,#64913) ;
#53197 = AXIS2_PLACEMENT_3D('',#93690,#64914,#64915) ;
#53198 = AXIS2_PLACEMENT_3D('',#93691,#64916,#64917) ;
#53199 = AXIS2_PLACEMENT_3D('',#93693,#64918,#64919) ;
#53200 = AXIS2_PLACEMENT_3D('',#93695,#64921,#64922) ;
#53201 = AXIS2_PLACEMENT_3D('',#93697,#64923,#64924) ;
#53202 = AXIS2_PLACEMENT_3D('',#93698,#64925,#64926) ;
#53203 = AXIS2_PLACEMENT_3D('',#93699,#64927,#64928) ;
#53204 = AXIS2_PLACEMENT_3D('',#93701,#64929,#64930) ;
#53205 = AXIS2_PLACEMENT_3D('',#93702,#64931,#64932) ;
#53206 = AXIS2_PLACEMENT_3D('',#93703,#64933,#64934) ;
#53207 = AXIS2_PLACEMENT_3D('',#93704,#64935,#64936) ;
#53208 = AXIS2_PLACEMENT_3D('',#93706,#64938,#64939) ;
#53209 = AXIS2_PLACEMENT_3D('',#93707,#64940,#64941) ;
#53210 = AXIS2_PLACEMENT_3D('',#93708,#64942,#64943) ;
#53211 = AXIS2_PLACEMENT_3D('',#93709,#64944,#64945) ;
#53212 = AXIS2_PLACEMENT_3D('',#93710,#64946,#64947) ;
#53213 = AXIS2_PLACEMENT_3D('',#93711,#64948,#64949) ;
#53214 = AXIS2_PLACEMENT_3D('',#93712,#64950,#64951) ;
#53215 = AXIS2_PLACEMENT_3D('',#93716,#64954,#64955) ;
#53216 = AXIS2_PLACEMENT_3D('',#93717,#64956,#64957) ;
#53217 = AXIS2_PLACEMENT_3D('',#93718,#64958,#64959) ;
#53218 = AXIS2_PLACEMENT_3D('',#93720,#64961,#64962) ;
#53219 = AXIS2_PLACEMENT_3D('',#93722,#64964,#64965) ;
#53220 = AXIS2_PLACEMENT_3D('',#93724,#64967,#64968) ;
#53221 = AXIS2_PLACEMENT_3D('',#93726,#64970,#64971) ;
#53222 = AXIS2_PLACEMENT_3D('',#93727,#64972,#64973) ;
#53223 = AXIS2_PLACEMENT_3D('',#93729,#64974,#64975) ;
#53224 = AXIS2_PLACEMENT_3D('',#93731,#64977,#64978) ;
#53225 = AXIS2_PLACEMENT_3D('',#93732,#64979,#64980) ;
#53226 = AXIS2_PLACEMENT_3D('',#93733,#64981,#64982) ;
#53227 = AXIS2_PLACEMENT_3D('',#93736,#64984,#64985) ;
#53228 = AXIS2_PLACEMENT_3D('',#93737,#64986,#64987) ;
#53229 = AXIS2_PLACEMENT_3D('',#93739,#64988,#64989) ;
#53230 = AXIS2_PLACEMENT_3D('',#93740,#64990,#64991) ;
#53231 = AXIS2_PLACEMENT_3D('',#93741,#64992,#64993) ;
#53232 = AXIS2_PLACEMENT_3D('',#93743,#64995,#64996) ;
#53233 = AXIS2_PLACEMENT_3D('',#93745,#64997,#64998) ;
#53234 = AXIS2_PLACEMENT_3D('',#93746,#64999,#65000) ;
#53235 = AXIS2_PLACEMENT_3D('',#93747,#65001,#65002) ;
#53236 = AXIS2_PLACEMENT_3D('',#93749,#65003,#65004) ;
#53237 = AXIS2_PLACEMENT_3D('',#93751,#65006,#65007) ;
#53238 = AXIS2_PLACEMENT_3D('',#93752,#65008,#65009) ;
#53239 = AXIS2_PLACEMENT_3D('',#93753,#65010,#65011) ;
#53240 = AXIS2_PLACEMENT_3D('',#93754,#65012,#65013) ;
#53241 = AXIS2_PLACEMENT_3D('',#93755,#65014,#65015) ;
#53242 = AXIS2_PLACEMENT_3D('',#93756,#65016,#65017) ;
#53243 = AXIS2_PLACEMENT_3D('',#93757,#65018,#65019) ;
#53244 = AXIS2_PLACEMENT_3D('',#93758,#65020,#65021) ;
#53245 = AXIS2_PLACEMENT_3D('',#93760,#65022,#65023) ;
#53246 = AXIS2_PLACEMENT_3D('',#93762,#65025,#65026) ;
#53247 = AXIS2_PLACEMENT_3D('',#93764,#65027,#65028) ;
#53248 = AXIS2_PLACEMENT_3D('',#93765,#65029,#65030) ;
#53249 = AXIS2_PLACEMENT_3D('',#93766,#65031,#65032) ;
#53250 = AXIS2_PLACEMENT_3D('',#93769,#65034,#65035) ;
#53251 = AXIS2_PLACEMENT_3D('',#93770,#65036,#65037) ;
#53252 = AXIS2_PLACEMENT_3D('',#93773,#65038,#65039) ;
#53253 = AXIS2_PLACEMENT_3D('',#93777,#65041,#65042) ;
#53254 = AXIS2_PLACEMENT_3D('',#93779,#65044,#65045) ;
#53255 = AXIS2_PLACEMENT_3D('',#93781,#65046,#65047) ;
#53256 = AXIS2_PLACEMENT_3D('',#93782,#65048,#65049) ;
#53257 = AXIS2_PLACEMENT_3D('',#93783,#65050,#65051) ;
#53258 = AXIS2_PLACEMENT_3D('',#93784,#65052,#65053) ;
#53259 = AXIS2_PLACEMENT_3D('',#93786,#65054,#65055) ;
#53260 = AXIS2_PLACEMENT_3D('',#93788,#65057,#65058) ;
#53261 = AXIS2_PLACEMENT_3D('',#93790,#65059,#65060) ;
#53262 = AXIS2_PLACEMENT_3D('',#93791,#65061,#65062) ;
#53263 = AXIS2_PLACEMENT_3D('',#93792,#65063,#65064) ;
#53264 = AXIS2_PLACEMENT_3D('',#93794,#65065,#65066) ;
#53265 = AXIS2_PLACEMENT_3D('',#93796,#65068,#65069) ;
#53266 = AXIS2_PLACEMENT_3D('',#93798,#65070,#65071) ;
#53267 = AXIS2_PLACEMENT_3D('',#93799,#65072,#65073) ;
#53268 = AXIS2_PLACEMENT_3D('',#93800,#65074,#65075) ;
#53269 = AXIS2_PLACEMENT_3D('',#93802,#65077,#65078) ;
#53270 = AXIS2_PLACEMENT_3D('',#93803,#65079,#65080) ;
#53271 = AXIS2_PLACEMENT_3D('',#93805,#65082,#65083) ;
#53272 = AXIS2_PLACEMENT_3D('',#93806,#65084,#65085) ;
#53273 = AXIS2_PLACEMENT_3D('',#93810,#65087,#65088) ;
#53274 = AXIS2_PLACEMENT_3D('',#93814,#65090,#65091) ;
#53275 = AXIS2_PLACEMENT_3D('',#93817,#65093,#65094) ;
#53276 = AXIS2_PLACEMENT_3D('',#93903,#65105,#65106) ;
#53277 = AXIS2_PLACEMENT_3D('',#93906,#65108,#65109) ;
#53278 = AXIS2_PLACEMENT_3D('',#93907,#65110,#65111) ;
#53279 = AXIS2_PLACEMENT_3D('',#93912,#65114,#65115) ;
#53280 = AXIS2_PLACEMENT_3D('',#93913,#65116,#65117) ;
#53281 = AXIS2_PLACEMENT_3D('',#93919,#65121,#65122) ;
#53282 = AXIS2_PLACEMENT_3D('',#93921,#65123,#65124) ;
#53283 = AXIS2_PLACEMENT_3D('',#93922,#65125,#65126) ;
#53284 = AXIS2_PLACEMENT_3D('',#93925,#65128,#65129) ;
#53285 = AXIS2_PLACEMENT_3D('',#93926,#65130,#65131) ;
#53286 = AXIS2_PLACEMENT_3D('',#93934,#65136,#65137) ;
#53287 = AXIS2_PLACEMENT_3D('',#93969,#65140,#65141) ;
#53288 = AXIS2_PLACEMENT_3D('',#93971,#65142,#65143) ;
#53289 = AXIS2_PLACEMENT_3D('',#93973,#65144,#65145) ;
#53290 = AXIS2_PLACEMENT_3D('',#93974,#65146,#65147) ;
#53291 = AXIS2_PLACEMENT_3D('',#94007,#65148,#65149) ;
#53292 = AXIS2_PLACEMENT_3D('',#94009,#65150,#65151) ;
#53293 = AXIS2_PLACEMENT_3D('',#94011,#65152,#65153) ;
#53294 = AXIS2_PLACEMENT_3D('',#94012,#65154,#65155) ;
#53295 = AXIS2_PLACEMENT_3D('',#94013,#65156,#65157) ;
#53296 = AXIS2_PLACEMENT_3D('',#94017,#65159,#65160) ;
#53297 = AXIS2_PLACEMENT_3D('',#94046,#65162,#65163) ;
#53298 = AXIS2_PLACEMENT_3D('',#94080,#65164,#65165) ;
#53299 = AXIS2_PLACEMENT_3D('',#94083,#65166,#65167) ;
#53300 = AXIS2_PLACEMENT_3D('',#94084,#65168,#65169) ;
#53301 = AXIS2_PLACEMENT_3D('',#94085,#65170,#65171) ;
#53302 = AXIS2_PLACEMENT_3D('',#94086,#65172,#65173) ;
#53303 = AXIS2_PLACEMENT_3D('',#94089,#65176,#65177) ;
#53304 = AXIS2_PLACEMENT_3D('',#94092,#65178,#65179) ;
#53305 = AXIS2_PLACEMENT_3D('',#94095,#65182,#65183) ;
#53306 = AXIS2_PLACEMENT_3D('',#94098,#65186,#65187) ;
#53307 = AXIS2_PLACEMENT_3D('',#94101,#65188,#65189) ;
#53308 = AXIS2_PLACEMENT_3D('',#94104,#65192,#65193) ;
#53309 = AXIS2_PLACEMENT_3D('',#94106,#65194,#65195) ;
#53310 = AXIS2_PLACEMENT_3D('',#94130,#65198,#65199) ;
#53311 = AXIS2_PLACEMENT_3D('',#94131,#65200,#65201) ;
#53312 = AXIS2_PLACEMENT_3D('',#94156,#65202,#65203) ;
#53313 = AXIS2_PLACEMENT_3D('',#94160,#65205,#65206) ;
#53314 = AXIS2_PLACEMENT_3D('',#94162,#65208,#65209) ;
#53315 = AXIS2_PLACEMENT_3D('',#94164,#65211,#65212) ;
#53316 = AXIS2_PLACEMENT_3D('',#94166,#65214,#65215) ;
#53317 = AXIS2_PLACEMENT_3D('',#94170,#65217,#65218) ;
#53318 = AXIS2_PLACEMENT_3D('',#94172,#65220,#65221) ;
#53319 = AXIS2_PLACEMENT_3D('',#94174,#65222,#65223) ;
#53320 = AXIS2_PLACEMENT_3D('',#94176,#65224,#65225) ;
#53321 = AXIS2_PLACEMENT_3D('',#94192,#65227,#65228) ;
#53322 = AXIS2_PLACEMENT_3D('',#94196,#65230,#65231) ;
#53323 = AXIS2_PLACEMENT_3D('',#94197,#65232,#65233) ;
#53324 = AXIS2_PLACEMENT_3D('',#94198,#65234,#65235) ;
#53325 = AXIS2_PLACEMENT_3D('',#94202,#65237,#65238) ;
#53326 = AXIS2_PLACEMENT_3D('',#94205,#65240,#65241) ;
#53327 = AXIS2_PLACEMENT_3D('',#94206,#65242,#65243) ;
#53328 = AXIS2_PLACEMENT_3D('',#94215,#65249,#65250) ;
#53329 = AXIS2_PLACEMENT_3D('',#94219,#65253,#65254) ;
#53330 = AXIS2_PLACEMENT_3D('',#94247,#65257,#65258) ;
#53331 = AXIS2_PLACEMENT_3D('',#94248,#65259,#65260) ;
#53332 = AXIS2_PLACEMENT_3D('',#94249,#65261,#65262) ;
#53333 = AXIS2_PLACEMENT_3D('',#94250,#65263,#65264) ;
#53334 = AXIS2_PLACEMENT_3D('',#94279,#65265,#65266) ;
#53335 = AXIS2_PLACEMENT_3D('',#94316,#65267,#65268) ;
#53336 = AXIS2_PLACEMENT_3D('',#94374,#65269,#65270) ;
#53337 = AXIS2_PLACEMENT_3D('',#94375,#65271,#65272) ;
#53338 = AXIS2_PLACEMENT_3D('',#94429,#65273,#65274) ;
#53339 = AXIS2_PLACEMENT_3D('',#94431,#65276,#65277) ;
#53340 = AXIS2_PLACEMENT_3D('',#94447,#65280,#65281) ;
#53341 = AXIS2_PLACEMENT_3D('',#94477,#65283,#65284) ;
#53342 = AXIS2_PLACEMENT_3D('',#94479,#65285,#65286) ;
#53343 = AXIS2_PLACEMENT_3D('',#94480,#65287,#65288) ;
#53344 = AXIS2_PLACEMENT_3D('',#94481,#65289,#65290) ;
#53345 = AXIS2_PLACEMENT_3D('',#94484,#65291,#65292) ;
#53346 = AXIS2_PLACEMENT_3D('',#94516,#65295,#65296) ;
#53347 = AXIS2_PLACEMENT_3D('',#94517,#65297,#65298) ;
#53348 = AXIS2_PLACEMENT_3D('',#94518,#65299,#65300) ;
#53349 = AXIS2_PLACEMENT_3D('',#94540,#65301,#65302) ;
#53350 = AXIS2_PLACEMENT_3D('',#94559,#65303,#65304) ;
#53351 = AXIS2_PLACEMENT_3D('',#94563,#65306,#65307) ;
#53352 = AXIS2_PLACEMENT_3D('',#94570,#65311,#65312) ;
#53353 = AXIS2_PLACEMENT_3D('',#94578,#65316,#65317) ;
#53354 = AXIS2_PLACEMENT_3D('',#94586,#65321,#65322) ;
#53355 = AXIS2_PLACEMENT_3D('',#94602,#65330,#65331) ;
#53356 = AXIS2_PLACEMENT_3D('',#94616,#65338,#65339) ;
#53357 = AXIS2_PLACEMENT_3D('',#94626,#65345,#65346) ;
#53358 = AXIS2_PLACEMENT_3D('',#94627,#65347,#65348) ;
#53359 = AXIS2_PLACEMENT_3D('',#94629,#65350,#65351) ;
#53360 = AXIS2_PLACEMENT_3D('',#94631,#65352,#65353) ;
#53361 = AXIS2_PLACEMENT_3D('',#94633,#65355,#65356) ;
#53362 = AXIS2_PLACEMENT_3D('',#94634,#65357,#65358) ;
#53363 = AXIS2_PLACEMENT_3D('',#94668,#65359,#65360) ;
#53364 = AXIS2_PLACEMENT_3D('',#94669,#65361,#65362) ;
#53365 = AXIS2_PLACEMENT_3D('',#94670,#65363,#65364) ;
#53366 = AXIS2_PLACEMENT_3D('',#94683,#65366,#65367) ;
#53367 = AXIS2_PLACEMENT_3D('',#94685,#65368,#65369) ;
#53368 = AXIS2_PLACEMENT_3D('',#94687,#65371,#65372) ;
#53369 = AXIS2_PLACEMENT_3D('',#94735,#65374,#65375) ;
#53370 = AXIS2_PLACEMENT_3D('',#94777,#65376,#65377) ;
#53371 = AXIS2_PLACEMENT_3D('',#94779,#65379,#65380) ;
#53372 = AXIS2_PLACEMENT_3D('',#94781,#65382,#65383) ;
#53373 = AXIS2_PLACEMENT_3D('',#94784,#65385,#65386) ;
#53374 = AXIS2_PLACEMENT_3D('',#94785,#65387,#65388) ;
#53375 = AXIS2_PLACEMENT_3D('',#94789,#65391,#65392) ;
#53376 = AXIS2_PLACEMENT_3D('',#94792,#65395,#65396) ;
#53377 = AXIS2_PLACEMENT_3D('',#94799,#65398,#65399) ;
#53378 = AXIS2_PLACEMENT_3D('',#94807,#65401,#65402) ;
#53379 = AXIS2_PLACEMENT_3D('',#94823,#65404,#65405) ;
#53380 = AXIS2_PLACEMENT_3D('',#94824,#65406,#65407) ;
#53381 = AXIS2_PLACEMENT_3D('',#94825,#65408,#65409) ;
#53382 = AXIS2_PLACEMENT_3D('',#94827,#65411,#65412) ;
#53383 = AXIS2_PLACEMENT_3D('',#94829,#65414,#65415) ;
#53384 = AXIS2_PLACEMENT_3D('',#94830,#65416,#65417) ;
#53385 = AXIS2_PLACEMENT_3D('',#94840,#65423,#65424) ;
#53386 = AXIS2_PLACEMENT_3D('',#94842,#65425,#65426) ;
#53387 = AXIS2_PLACEMENT_3D('',#94844,#65428,#65429) ;
#53388 = AXIS2_PLACEMENT_3D('',#94887,#65433,#65434) ;
#53389 = AXIS2_PLACEMENT_3D('',#94889,#65435,#65436) ;
#53390 = AXIS2_PLACEMENT_3D('',#94892,#65438,#65439) ;
#53391 = AXIS2_PLACEMENT_3D('',#94893,#65440,#65441) ;
#53392 = AXIS2_PLACEMENT_3D('',#94896,#65443,#65444) ;
#53393 = AXIS2_PLACEMENT_3D('',#94897,#65445,#65446) ;
#53394 = AXIS2_PLACEMENT_3D('',#94901,#65449,#65450) ;
#53395 = AXIS2_PLACEMENT_3D('',#94905,#65453,#65454) ;
#53396 = AXIS2_PLACEMENT_3D('',#94907,#65456,#65457) ;
#53397 = AXIS2_PLACEMENT_3D('',#94913,#65460,#65461) ;
#53398 = AXIS2_PLACEMENT_3D('',#94916,#65463,#65464) ;
#53399 = AXIS2_PLACEMENT_3D('',#94920,#65467,#65468) ;
#53400 = AXIS2_PLACEMENT_3D('',#94921,#65469,#65470) ;
#53401 = AXIS2_PLACEMENT_3D('',#94922,#65471,#65472) ;
#53402 = AXIS2_PLACEMENT_3D('',#94923,#65473,#65474) ;
#53403 = AXIS2_PLACEMENT_3D('',#94924,#65475,#65476) ;
#53404 = AXIS2_PLACEMENT_3D('',#94925,#65477,#65478) ;
#53405 = AXIS2_PLACEMENT_3D('',#94926,#65479,#65480) ;
#53406 = AXIS2_PLACEMENT_3D('',#94927,#65481,#65482) ;
#53407 = AXIS2_PLACEMENT_3D('',#94928,#65483,#65484) ;
#53408 = AXIS2_PLACEMENT_3D('',#94930,#65486,#65487) ;
#53409 = AXIS2_PLACEMENT_3D('',#94936,#65491,#65492) ;
#53410 = AXIS2_PLACEMENT_3D('',#94942,#65496,#65497) ;
#53411 = AXIS2_PLACEMENT_3D('',#94945,#65500,#65501) ;
#53412 = AXIS2_PLACEMENT_3D('',#94947,#65503,#65504) ;
#53413 = AXIS2_PLACEMENT_3D('',#94949,#65506,#65507) ;
#53414 = AXIS2_PLACEMENT_3D('',#94951,#65509,#65510) ;
#53415 = AXIS2_PLACEMENT_3D('',#94952,#65511,#65512) ;
#53416 = AXIS2_PLACEMENT_3D('',#94973,#65515,#65516) ;
#53417 = AXIS2_PLACEMENT_3D('',#95156,#65517,#65518) ;
#53418 = AXIS2_PLACEMENT_3D('',#95268,#65521,#65522) ;
#53419 = AXIS2_PLACEMENT_3D('',#95273,#65525,#65526) ;
#53420 = AXIS2_PLACEMENT_3D('',#95274,#65527,#65528) ;
#53421 = AXIS2_PLACEMENT_3D('',#95279,#65531,#65532) ;
#53422 = AXIS2_PLACEMENT_3D('',#95280,#65533,#65534) ;
#53423 = AXIS2_PLACEMENT_3D('',#95283,#65537,#65538) ;
#53424 = AXIS2_PLACEMENT_3D('',#95289,#65542,#65543) ;
#53425 = AXIS2_PLACEMENT_3D('',#95293,#65546,#65547) ;
#53426 = AXIS2_PLACEMENT_3D('',#95297,#65550,#65551) ;
#53427 = AXIS2_PLACEMENT_3D('',#95301,#65554,#65555) ;
#53428 = AXIS2_PLACEMENT_3D('',#95536,#65556,#65557) ;
#53429 = AXIS2_PLACEMENT_3D('',#95540,#65559,#65560) ;
#53430 = AXIS2_PLACEMENT_3D('',#95542,#65562,#65563) ;
#53431 = AXIS2_PLACEMENT_3D('',#95546,#65565,#65566) ;
#53432 = AXIS2_PLACEMENT_3D('',#95548,#65568,#65569) ;
#53433 = AXIS2_PLACEMENT_3D('',#95553,#65572,#65573) ;
#53434 = AXIS2_PLACEMENT_3D('',#95554,#65574,#65575) ;
#53435 = AXIS2_PLACEMENT_3D('',#95782,#65578,#65579) ;
#53436 = AXIS2_PLACEMENT_3D('',#95785,#65582,#65583) ;
#53437 = AXIS2_PLACEMENT_3D('',#95964,#65588,#65589) ;
#53438 = AXIS2_PLACEMENT_3D('',#96075,#65593,#65594) ;
#53439 = AXIS2_PLACEMENT_3D('',#96076,#65595,#65596) ;
#53440 = AXIS2_PLACEMENT_3D('',#96081,#65598,#65599) ;
#53441 = AXIS2_PLACEMENT_3D('',#96084,#65601,#65602) ;
#53442 = AXIS2_PLACEMENT_3D('',#96085,#65603,#65604) ;
#53443 = AXIS2_PLACEMENT_3D('',#96089,#65606,#65607) ;
#53444 = AXIS2_PLACEMENT_3D('',#96091,#65609,#65610) ;
#53445 = AXIS2_PLACEMENT_3D('',#96095,#65612,#65613) ;
#53446 = AXIS2_PLACEMENT_3D('',#96097,#65615,#65616) ;
#53447 = AXIS2_PLACEMENT_3D('',#96102,#65619,#65620) ;
#53448 = AXIS2_PLACEMENT_3D('',#96103,#65621,#65622) ;
#53449 = AXIS2_PLACEMENT_3D('',#96108,#65625,#65626) ;
#53450 = AXIS2_PLACEMENT_3D('',#96109,#65627,#65628) ;
#53451 = AXIS2_PLACEMENT_3D('',#96114,#65631,#65632) ;
#53452 = AXIS2_PLACEMENT_3D('',#96115,#65633,#65634) ;
#53453 = AXIS2_PLACEMENT_3D('',#96118,#65637,#65638) ;
#53454 = AXIS2_PLACEMENT_3D('',#96124,#65642,#65643) ;
#53455 = AXIS2_PLACEMENT_3D('',#96128,#65646,#65647) ;
#53456 = AXIS2_PLACEMENT_3D('',#96132,#65650,#65651) ;
#53457 = AXIS2_PLACEMENT_3D('',#96136,#65654,#65655) ;
#53458 = AXIS2_PLACEMENT_3D('',#96137,#65656,#65657) ;
#53459 = AXIS2_PLACEMENT_3D('',#96142,#65659,#65660) ;
#53460 = AXIS2_PLACEMENT_3D('',#96145,#65662,#65663) ;
#53461 = AXIS2_PLACEMENT_3D('',#96146,#65664,#65665) ;
#53462 = AXIS2_PLACEMENT_3D('',#96151,#65668,#65669) ;
#53463 = AXIS2_PLACEMENT_3D('',#96152,#65670,#65671) ;
#53464 = AXIS2_PLACEMENT_3D('',#96157,#65674,#65675) ;
#53465 = AXIS2_PLACEMENT_3D('',#96158,#65676,#65677) ;
#53466 = AXIS2_PLACEMENT_3D('',#96161,#65680,#65681) ;
#53467 = AXIS2_PLACEMENT_3D('',#96167,#65685,#65686) ;
#53468 = AXIS2_PLACEMENT_3D('',#96171,#65689,#65690) ;
#53469 = AXIS2_PLACEMENT_3D('',#96172,#65691,#65692) ;
#53470 = AXIS2_PLACEMENT_3D('',#96177,#65694,#65695) ;
#53471 = AXIS2_PLACEMENT_3D('',#96180,#65697,#65698) ;
#53472 = AXIS2_PLACEMENT_3D('',#96181,#65699,#65700) ;
#53473 = AXIS2_PLACEMENT_3D('',#96185,#65702,#65703) ;
#53474 = AXIS2_PLACEMENT_3D('',#96187,#65705,#65706) ;
#53475 = AXIS2_PLACEMENT_3D('',#96191,#65708,#65709) ;
#53476 = AXIS2_PLACEMENT_3D('',#96193,#65711,#65712) ;
#53477 = AXIS2_PLACEMENT_3D('',#96198,#65715,#65716) ;
#53478 = AXIS2_PLACEMENT_3D('',#96199,#65717,#65718) ;
#53479 = AXIS2_PLACEMENT_3D('',#96204,#65721,#65722) ;
#53480 = AXIS2_PLACEMENT_3D('',#96205,#65723,#65724) ;
#53481 = AXIS2_PLACEMENT_3D('',#96210,#65727,#65728) ;
#53482 = AXIS2_PLACEMENT_3D('',#96211,#65729,#65730) ;
#53483 = AXIS2_PLACEMENT_3D('',#96214,#65733,#65734) ;
#53484 = AXIS2_PLACEMENT_3D('',#96220,#65738,#65739) ;
#53485 = AXIS2_PLACEMENT_3D('',#96224,#65742,#65743) ;
#53486 = AXIS2_PLACEMENT_3D('',#96228,#65746,#65747) ;
#53487 = AXIS2_PLACEMENT_3D('',#96232,#65750,#65751) ;
#53488 = AXIS2_PLACEMENT_3D('',#96233,#65752,#65753) ;
#53489 = AXIS2_PLACEMENT_3D('',#96238,#65755,#65756) ;
#53490 = AXIS2_PLACEMENT_3D('',#96241,#65758,#65759) ;
#53491 = AXIS2_PLACEMENT_3D('',#96242,#65760,#65761) ;
#53492 = AXIS2_PLACEMENT_3D('',#96247,#65764,#65765) ;
#53493 = AXIS2_PLACEMENT_3D('',#96248,#65766,#65767) ;
#53494 = AXIS2_PLACEMENT_3D('',#96253,#65770,#65771) ;
#53495 = AXIS2_PLACEMENT_3D('',#96254,#65772,#65773) ;
#53496 = AXIS2_PLACEMENT_3D('',#96257,#65776,#65777) ;
#53497 = AXIS2_PLACEMENT_3D('',#96263,#65781,#65782) ;
#53498 = AXIS2_PLACEMENT_3D('',#96267,#65785,#65786) ;
#53499 = AXIS2_PLACEMENT_3D('',#96268,#65787,#65788) ;
#53500 = AXIS2_PLACEMENT_3D('',#96273,#65790,#65791) ;
#53501 = AXIS2_PLACEMENT_3D('',#96276,#65793,#65794) ;
#53502 = AXIS2_PLACEMENT_3D('',#96277,#65795,#65796) ;
#53503 = AXIS2_PLACEMENT_3D('',#96281,#65798,#65799) ;
#53504 = AXIS2_PLACEMENT_3D('',#96283,#65801,#65802) ;
#53505 = AXIS2_PLACEMENT_3D('',#96287,#65804,#65805) ;
#53506 = AXIS2_PLACEMENT_3D('',#96289,#65807,#65808) ;
#53507 = AXIS2_PLACEMENT_3D('',#96292,#65809,#65810) ;
#53508 = AXIS2_PLACEMENT_3D('',#96293,#65811,#65812) ;
#53509 = AXIS2_PLACEMENT_3D('',#96294,#65813,#65814) ;
#53510 = AXIS2_PLACEMENT_3D('',#96295,#65815,#65816) ;
#53511 = AXIS2_PLACEMENT_3D('',#96300,#65819,#65820) ;
#53512 = AXIS2_PLACEMENT_3D('',#96301,#65821,#65822) ;
#53513 = AXIS2_PLACEMENT_3D('',#96306,#65825,#65826) ;
#53514 = AXIS2_PLACEMENT_3D('',#96307,#65827,#65828) ;
#53515 = AXIS2_PLACEMENT_3D('',#96311,#65830,#65831) ;
#53516 = AXIS2_PLACEMENT_3D('',#96313,#65833,#65834) ;
#53517 = AXIS2_PLACEMENT_3D('',#96316,#65835,#65836) ;
#53518 = AXIS2_PLACEMENT_3D('',#96317,#65837,#65838) ;
#53519 = AXIS2_PLACEMENT_3D('',#96318,#65839,#65840) ;
#53520 = AXIS2_PLACEMENT_3D('',#96319,#65841,#65842) ;
#53521 = AXIS2_PLACEMENT_3D('',#96324,#65845,#65846) ;
#53522 = AXIS2_PLACEMENT_3D('',#96325,#65847,#65848) ;
#53523 = AXIS2_PLACEMENT_3D('',#96330,#65851,#65852) ;
#53524 = AXIS2_PLACEMENT_3D('',#96331,#65853,#65854) ;
#53525 = AXIS2_PLACEMENT_3D('',#96334,#65857,#65858) ;
#53526 = AXIS2_PLACEMENT_3D('',#96340,#65862,#65863) ;
#53527 = AXIS2_PLACEMENT_3D('',#96343,#65865,#65866) ;
#53528 = AXIS2_PLACEMENT_3D('',#96344,#65867,#65868) ;
#53529 = AXIS2_PLACEMENT_3D('',#96348,#65871,#65872) ;
#53530 = AXIS2_PLACEMENT_3D('',#96352,#65875,#65876) ;
#53531 = AXIS2_PLACEMENT_3D('',#96356,#65879,#65880) ;
#53532 = AXIS2_PLACEMENT_3D('',#96360,#65883,#65884) ;
#53533 = AXIS2_PLACEMENT_3D('',#96361,#65885,#65886) ;
#53534 = AXIS2_PLACEMENT_3D('',#96366,#65888,#65889) ;
#53535 = AXIS2_PLACEMENT_3D('',#96369,#65891,#65892) ;
#53536 = AXIS2_PLACEMENT_3D('',#96370,#65893,#65894) ;
#53537 = AXIS2_PLACEMENT_3D('',#96374,#65896,#65897) ;
#53538 = AXIS2_PLACEMENT_3D('',#96376,#65899,#65900) ;
#53539 = AXIS2_PLACEMENT_3D('',#96379,#65901,#65902) ;
#53540 = AXIS2_PLACEMENT_3D('',#96380,#65903,#65904) ;
#53541 = AXIS2_PLACEMENT_3D('',#96381,#65905,#65906) ;
#53542 = AXIS2_PLACEMENT_3D('',#96382,#65907,#65908) ;
#53543 = AXIS2_PLACEMENT_3D('',#96387,#65911,#65912) ;
#53544 = AXIS2_PLACEMENT_3D('',#96388,#65913,#65914) ;
#53545 = AXIS2_PLACEMENT_3D('',#96392,#65916,#65917) ;
#53546 = AXIS2_PLACEMENT_3D('',#96394,#65919,#65920) ;
#53547 = AXIS2_PLACEMENT_3D('',#96398,#65922,#65923) ;
#53548 = AXIS2_PLACEMENT_3D('',#96400,#65925,#65926) ;
#53549 = AXIS2_PLACEMENT_3D('',#96403,#65927,#65928) ;
#53550 = AXIS2_PLACEMENT_3D('',#96404,#65929,#65930) ;
#53551 = AXIS2_PLACEMENT_3D('',#96405,#65931,#65932) ;
#53552 = AXIS2_PLACEMENT_3D('',#96406,#65933,#65934) ;
#53553 = AXIS2_PLACEMENT_3D('',#96411,#65937,#65938) ;
#53554 = AXIS2_PLACEMENT_3D('',#96412,#65939,#65940) ;
#53555 = AXIS2_PLACEMENT_3D('',#96417,#65943,#65944) ;
#53556 = AXIS2_PLACEMENT_3D('',#96418,#65945,#65946) ;
#53557 = AXIS2_PLACEMENT_3D('',#96423,#65949,#65950) ;
#53558 = AXIS2_PLACEMENT_3D('',#96424,#65951,#65952) ;
#53559 = AXIS2_PLACEMENT_3D('',#96427,#65955,#65956) ;
#53560 = AXIS2_PLACEMENT_3D('',#96431,#65958,#65959) ;
#53561 = AXIS2_PLACEMENT_3D('',#96433,#65961,#65962) ;
#53562 = AXIS2_PLACEMENT_3D('',#96437,#65965,#65966) ;
#53563 = AXIS2_PLACEMENT_3D('',#96441,#65969,#65970) ;
#53564 = AXIS2_PLACEMENT_3D('',#96445,#65973,#65974) ;
#53565 = AXIS2_PLACEMENT_3D('',#96449,#65977,#65978) ;
#53566 = AXIS2_PLACEMENT_3D('',#96453,#65981,#65982) ;
#53567 = AXIS2_PLACEMENT_3D('',#96757,#65983,#65984) ;
#53568 = AXIS2_PLACEMENT_3D('',#96774,#65986,#65987) ;
#53569 = AXIS2_PLACEMENT_3D('',#96775,#65988,#65989) ;
#53570 = AXIS2_PLACEMENT_3D('',#96776,#65990,#65991) ;
#53571 = AXIS2_PLACEMENT_3D('',#96777,#65992,#65993) ;
#53572 = AXIS2_PLACEMENT_3D('',#96778,#65994,#65995) ;
#53573 = AXIS2_PLACEMENT_3D('',#96779,#65996,#65997) ;
#53574 = AXIS2_PLACEMENT_3D('',#96780,#65998,#65999) ;
#53575 = AXIS2_PLACEMENT_3D('',#96902,#66001,#66002) ;
#53576 = AXIS2_PLACEMENT_3D('',#97048,#66004,#66005) ;
#53577 = AXIS2_PLACEMENT_3D('',#97049,#66006,#66007) ;
#53578 = AXIS2_PLACEMENT_3D('',#97050,#66008,#66009) ;
#53579 = AXIS2_PLACEMENT_3D('',#97052,#66010,#66011) ;
#53580 = AXIS2_PLACEMENT_3D('',#97055,#66013,#66014) ;
#53581 = AXIS2_PLACEMENT_3D('',#97056,#66015,#66016) ;
#53582 = AXIS2_PLACEMENT_3D('',#97072,#66018,#66019) ;
#53583 = AXIS2_PLACEMENT_3D('',#97187,#66021,#66022) ;
#53584 = AXIS2_PLACEMENT_3D('',#97188,#66023,#66024) ;
#53585 = AXIS2_PLACEMENT_3D('',#97190,#66026,#66027) ;
#53586 = AXIS2_PLACEMENT_3D('',#97192,#66029,#66030) ;
#53587 = AXIS2_PLACEMENT_3D('',#97196,#66032,#66033) ;
#53588 = AXIS2_PLACEMENT_3D('',#97199,#66035,#66036) ;
#53589 = AXIS2_PLACEMENT_3D('',#97200,#66037,#66038) ;
#53590 = AXIS2_PLACEMENT_3D('',#97204,#66040,#66041) ;
#53591 = AXIS2_PLACEMENT_3D('',#97206,#66043,#66044) ;
#53592 = AXIS2_PLACEMENT_3D('',#97209,#66046,#66047) ;
#53593 = AXIS2_PLACEMENT_3D('',#97210,#66048,#66049) ;
#53594 = AXIS2_PLACEMENT_3D('',#97213,#66051,#66052) ;
#53595 = AXIS2_PLACEMENT_3D('',#97214,#66053,#66054) ;
#53596 = AXIS2_PLACEMENT_3D('',#97217,#66056,#66057) ;
#53597 = AXIS2_PLACEMENT_3D('',#97218,#66058,#66059) ;
#53598 = AXIS2_PLACEMENT_3D('',#97221,#66061,#66062) ;
#53599 = AXIS2_PLACEMENT_3D('',#97222,#66063,#66064) ;
#53600 = AXIS2_PLACEMENT_3D('',#97225,#66067,#66068) ;
#53601 = AXIS2_PLACEMENT_3D('',#97227,#66070,#66071) ;
#53602 = AXIS2_PLACEMENT_3D('',#97229,#66073,#66074) ;
#53603 = AXIS2_PLACEMENT_3D('',#97230,#66075,#66076) ;
#53604 = AXIS2_PLACEMENT_3D('',#97235,#66078,#66079) ;
#53605 = AXIS2_PLACEMENT_3D('',#97238,#66081,#66082) ;
#53606 = AXIS2_PLACEMENT_3D('',#97240,#66083,#66084) ;
#53607 = AXIS2_PLACEMENT_3D('',#97244,#66086,#66087) ;
#53608 = AXIS2_PLACEMENT_3D('',#97298,#66090,#66091) ;
#53609 = AXIS2_PLACEMENT_3D('',#97321,#66103,#66104) ;
#53610 = AXIS2_PLACEMENT_3D('',#97322,#66105,#66106) ;
#53611 = AXIS2_PLACEMENT_3D('',#97323,#66107,#66108) ;
#53612 = AXIS2_PLACEMENT_3D('',#97324,#66109,#66110) ;
#53613 = AXIS2_PLACEMENT_3D('',#97325,#66111,#66112) ;
#53614 = AXIS2_PLACEMENT_3D('',#97326,#66113,#66114) ;
#53615 = AXIS2_PLACEMENT_3D('',#97329,#66116,#66117) ;
#53616 = AXIS2_PLACEMENT_3D('',#97330,#66118,#66119) ;
#53617 = AXIS2_PLACEMENT_3D('',#97332,#66121,#66122) ;
#53618 = AXIS2_PLACEMENT_3D('',#97334,#66124,#66125) ;
#53619 = AXIS2_PLACEMENT_3D('',#97336,#66126,#66127) ;
#53620 = AXIS2_PLACEMENT_3D('',#97339,#66129,#66130) ;
#53621 = AXIS2_PLACEMENT_3D('',#97340,#66131,#66132) ;
#53622 = AXIS2_PLACEMENT_3D('',#97341,#66133,#66134) ;
#53623 = AXIS2_PLACEMENT_3D('',#97343,#66136,#66137) ;
#53624 = AXIS2_PLACEMENT_3D('',#97344,#66138,#66139) ;
#53625 = AXIS2_PLACEMENT_3D('',#97345,#66140,#66141) ;
#53626 = AXIS2_PLACEMENT_3D('',#97346,#66142,#66143) ;
#53627 = AXIS2_PLACEMENT_3D('',#97347,#66144,#66145) ;
#53628 = AXIS2_PLACEMENT_3D('',#97348,#66146,#66147) ;
#53629 = AXIS2_PLACEMENT_3D('',#97349,#66148,#66149) ;
#53630 = AXIS2_PLACEMENT_3D('',#97350,#66150,#66151) ;
#53631 = AXIS2_PLACEMENT_3D('',#97351,#66152,#66153) ;
#53632 = AXIS2_PLACEMENT_3D('',#97353,#66155,#66156) ;
#53633 = AXIS2_PLACEMENT_3D('',#97355,#66158,#66159) ;
#53634 = AXIS2_PLACEMENT_3D('',#97357,#66161,#66162) ;
#53635 = AXIS2_PLACEMENT_3D('',#97358,#66163,#66164) ;
#53636 = AXIS2_PLACEMENT_3D('',#97359,#66165,#66166) ;
#53637 = AXIS2_PLACEMENT_3D('',#97360,#66167,#66168) ;
#53638 = AXIS2_PLACEMENT_3D('',#97362,#66169,#66170) ;
#53639 = AXIS2_PLACEMENT_3D('',#97364,#66172,#66173) ;
#53640 = AXIS2_PLACEMENT_3D('',#97365,#66174,#66175) ;
#53641 = AXIS2_PLACEMENT_3D('',#97366,#66176,#66177) ;
#53642 = AXIS2_PLACEMENT_3D('',#97368,#66179,#66180) ;
#53643 = AXIS2_PLACEMENT_3D('',#97372,#66182,#66183) ;
#53644 = AXIS2_PLACEMENT_3D('',#97373,#66184,#66185) ;
#53645 = AXIS2_PLACEMENT_3D('',#97374,#66186,#66187) ;
#53646 = AXIS2_PLACEMENT_3D('',#97375,#66188,#66189) ;
#53647 = AXIS2_PLACEMENT_3D('',#97377,#66191,#66192) ;
#53648 = AXIS2_PLACEMENT_3D('',#97378,#66193,#66194) ;
#53649 = AXIS2_PLACEMENT_3D('',#97379,#66195,#66196) ;
#53650 = AXIS2_PLACEMENT_3D('',#97380,#66197,#66198) ;
#53651 = AXIS2_PLACEMENT_3D('',#97381,#66199,#66200) ;
#53652 = AXIS2_PLACEMENT_3D('',#97382,#66201,#66202) ;
#53653 = AXIS2_PLACEMENT_3D('',#97383,#66203,#66204) ;
#53654 = AXIS2_PLACEMENT_3D('',#97384,#66205,#66206) ;
#53655 = AXIS2_PLACEMENT_3D('',#97385,#66207,#66208) ;
#53656 = AXIS2_PLACEMENT_3D('',#97386,#66209,#66210) ;
#53657 = AXIS2_PLACEMENT_3D('',#97387,#66211,#66212) ;
#53658 = AXIS2_PLACEMENT_3D('',#97388,#66213,#66214) ;
#53659 = AXIS2_PLACEMENT_3D('',#97389,#66215,#66216) ;
#53660 = AXIS2_PLACEMENT_3D('',#97391,#66217,#66218) ;
#53661 = AXIS2_PLACEMENT_3D('',#97392,#66219,#66220) ;
#53662 = AXIS2_PLACEMENT_3D('',#97393,#66221,#66222) ;
#53663 = AXIS2_PLACEMENT_3D('',#97395,#66223,#66224) ;
#53664 = AXIS2_PLACEMENT_3D('',#97397,#66226,#66227) ;
#53665 = AXIS2_PLACEMENT_3D('',#97400,#66230,#66231) ;
#53666 = AXIS2_PLACEMENT_3D('',#97402,#66233,#66234) ;
#53667 = AXIS2_PLACEMENT_3D('',#97404,#66236,#66237) ;
#53668 = AXIS2_PLACEMENT_3D('',#97405,#66238,#66239) ;
#53669 = AXIS2_PLACEMENT_3D('',#97407,#66240,#66241) ;
#53670 = AXIS2_PLACEMENT_3D('',#97410,#66243,#66244) ;
#53671 = AXIS2_PLACEMENT_3D('',#97411,#66245,#66246) ;
#53672 = AXIS2_PLACEMENT_3D('',#97414,#66248,#66249) ;
#53673 = AXIS2_PLACEMENT_3D('',#97415,#66250,#66251) ;
#53674 = AXIS2_PLACEMENT_3D('',#97416,#66252,#66253) ;
#53675 = AXIS2_PLACEMENT_3D('',#97417,#66254,#66255) ;
#53676 = AXIS2_PLACEMENT_3D('',#97418,#66256,#66257) ;
#53677 = AXIS2_PLACEMENT_3D('',#97419,#66258,#66259) ;
#53678 = AXIS2_PLACEMENT_3D('',#97420,#66260,#66261) ;
#53679 = AXIS2_PLACEMENT_3D('',#97421,#66262,#66263) ;
#53680 = AXIS2_PLACEMENT_3D('',#97422,#66264,#66265) ;
#53681 = AXIS2_PLACEMENT_3D('',#97423,#66266,#66267) ;
#53682 = AXIS2_PLACEMENT_3D('',#97424,#66268,#66269) ;
#53683 = AXIS2_PLACEMENT_3D('',#97426,#66270,#66271) ;
#53684 = AXIS2_PLACEMENT_3D('',#97427,#66272,#66273) ;
#53685 = AXIS2_PLACEMENT_3D('',#97428,#66274,#66275) ;
#53686 = AXIS2_PLACEMENT_3D('',#97430,#66277,#66278) ;
#53687 = AXIS2_PLACEMENT_3D('',#97432,#66280,#66281) ;
#53688 = AXIS2_PLACEMENT_3D('',#97433,#66282,#66283) ;
#53689 = AXIS2_PLACEMENT_3D('',#97434,#66284,#66285) ;
#53690 = AXIS2_PLACEMENT_3D('',#97435,#66286,#66287) ;
#53691 = AXIS2_PLACEMENT_3D('',#97436,#66288,#66289) ;
#53692 = AXIS2_PLACEMENT_3D('',#97438,#66291,#66292) ;
#53693 = AXIS2_PLACEMENT_3D('',#97440,#66294,#66295) ;
#53694 = AXIS2_PLACEMENT_3D('',#97442,#66297,#66298) ;
#53695 = AXIS2_PLACEMENT_3D('',#97444,#66300,#66301) ;
#53696 = AXIS2_PLACEMENT_3D('',#97445,#66302,#66303) ;
#53697 = AXIS2_PLACEMENT_3D('',#97446,#66304,#66305) ;
#53698 = AXIS2_PLACEMENT_3D('',#97448,#66307,#66308) ;
#53699 = AXIS2_PLACEMENT_3D('',#97449,#66309,#66310) ;
#53700 = AXIS2_PLACEMENT_3D('',#97450,#66311,#66312) ;
#53701 = AXIS2_PLACEMENT_3D('',#97451,#66313,#66314) ;
#53702 = AXIS2_PLACEMENT_3D('',#97452,#66315,#66316) ;
#53703 = AXIS2_PLACEMENT_3D('',#97456,#66319,#66320) ;
#53704 = AXIS2_PLACEMENT_3D('',#97460,#66322,#66323) ;
#53705 = AXIS2_PLACEMENT_3D('',#97464,#66325,#66326) ;
#53706 = AXIS2_PLACEMENT_3D('',#97468,#66329,#66330) ;
#53707 = AXIS2_PLACEMENT_3D('',#97470,#66332,#66333) ;
#53708 = AXIS2_PLACEMENT_3D('',#97473,#66335,#66336) ;
#53709 = AXIS2_PLACEMENT_3D('',#97474,#66337,#66338) ;
#53710 = AXIS2_PLACEMENT_3D('',#97478,#66341,#66342) ;
#53711 = AXIS2_PLACEMENT_3D('',#97481,#66344,#66345) ;
#53712 = AXIS2_PLACEMENT_3D('',#97482,#66346,#66347) ;
#53713 = AXIS2_PLACEMENT_3D('',#97486,#66350,#66351) ;
#53714 = AXIS2_PLACEMENT_3D('',#97490,#66354,#66355) ;
#53715 = AXIS2_PLACEMENT_3D('',#97494,#66358,#66359) ;
#53716 = AXIS2_PLACEMENT_3D('',#97497,#66361,#66362) ;
#53717 = AXIS2_PLACEMENT_3D('',#97498,#66363,#66364) ;
#53718 = AXIS2_PLACEMENT_3D('',#97501,#66366,#66367) ;
#53719 = AXIS2_PLACEMENT_3D('',#97502,#66368,#66369) ;
#53720 = AXIS2_PLACEMENT_3D('',#97506,#66372,#66373) ;
#53721 = AXIS2_PLACEMENT_3D('',#97508,#66375,#66376) ;
#53722 = AXIS2_PLACEMENT_3D('',#97509,#66377,#66378) ;
#53723 = AXIS2_PLACEMENT_3D('',#97515,#66382,#66383) ;
#53724 = AXIS2_PLACEMENT_3D('',#97519,#66386,#66387) ;
#53725 = AXIS2_PLACEMENT_3D('',#97523,#66390,#66391) ;
#53726 = AXIS2_PLACEMENT_3D('',#97525,#66393,#66394) ;
#53727 = AXIS2_PLACEMENT_3D('',#97526,#66395,#66396) ;
#53728 = AXIS2_PLACEMENT_3D('',#97533,#66401,#66402) ;
#53729 = AXIS2_PLACEMENT_3D('',#97537,#66404,#66405) ;
#53730 = AXIS2_PLACEMENT_3D('',#97539,#66407,#66408) ;
#53731 = AXIS2_PLACEMENT_3D('',#97541,#66410,#66411) ;
#53732 = AXIS2_PLACEMENT_3D('',#97543,#66413,#66414) ;
#53733 = AXIS2_PLACEMENT_3D('',#97544,#66415,#66416) ;
#53734 = AXIS2_PLACEMENT_3D('',#97547,#66418,#66419) ;
#53735 = AXIS2_PLACEMENT_3D('',#97548,#66420,#66421) ;
#53736 = AXIS2_PLACEMENT_3D('',#97549,#66422,#66423) ;
#53737 = AXIS2_PLACEMENT_3D('',#97550,#66424,#66425) ;
#53738 = AXIS2_PLACEMENT_3D('',#97552,#66427,#66428) ;
#53739 = AXIS2_PLACEMENT_3D('',#97556,#66432,#66433) ;
#53740 = AXIS2_PLACEMENT_3D('',#97557,#66434,#66435) ;
#53741 = AXIS2_PLACEMENT_3D('',#97560,#66437,#66438) ;
#53742 = AXIS2_PLACEMENT_3D('',#97561,#66439,#66440) ;
#53743 = AXIS2_PLACEMENT_3D('',#97563,#66442,#66443) ;
#53744 = AXIS2_PLACEMENT_3D('',#97565,#66445,#66446) ;
#53745 = AXIS2_PLACEMENT_3D('',#97566,#66447,#66448) ;
#53746 = AXIS2_PLACEMENT_3D('',#97568,#66450,#66451) ;
#53747 = AXIS2_PLACEMENT_3D('',#97569,#66452,#66453) ;
#53748 = AXIS2_PLACEMENT_3D('',#97570,#66454,#66455) ;
#53749 = AXIS2_PLACEMENT_3D('',#97571,#66456,#66457) ;
#53750 = AXIS2_PLACEMENT_3D('',#97591,#66459,#66460) ;
#53751 = AXIS2_PLACEMENT_3D('',#97592,#66461,#66462) ;
#53752 = AXIS2_PLACEMENT_3D('',#97594,#66463,#66464) ;
#53753 = AXIS2_PLACEMENT_3D('',#97596,#66465,#66466) ;
#53754 = AXIS2_PLACEMENT_3D('',#97597,#66467,#66468) ;
#53755 = AXIS2_PLACEMENT_3D('',#97598,#66469,#66470) ;
#53756 = AXIS2_PLACEMENT_3D('',#97616,#66471,#66472) ;
#53757 = AXIS2_PLACEMENT_3D('',#97695,#66473,#66474) ;
#53758 = AXIS2_PLACEMENT_3D('',#97696,#66475,#66476) ;
#53759 = AXIS2_PLACEMENT_3D('',#97724,#66478,#66479) ;
#53760 = AXIS2_PLACEMENT_3D('',#97729,#66480,#66481) ;
#53761 = AXIS2_PLACEMENT_3D('',#97730,#66482,#66483) ;
#53762 = AXIS2_PLACEMENT_3D('',#97732,#66484,#66485) ;
#53763 = AXIS2_PLACEMENT_3D('',#97733,#66486,#66487) ;
#53764 = AXIS2_PLACEMENT_3D('',#97734,#66488,#66489) ;
#53765 = AXIS2_PLACEMENT_3D('',#97736,#66491,#66492) ;
#53766 = AXIS2_PLACEMENT_3D('',#97737,#66493,#66494) ;
#53767 = AXIS2_PLACEMENT_3D('',#97739,#66495,#66496) ;
#53768 = AXIS2_PLACEMENT_3D('',#97740,#66497,#66498) ;
#53769 = AXIS2_PLACEMENT_3D('',#97762,#66499,#66500) ;
#53770 = AXIS2_PLACEMENT_3D('',#97763,#66501,#66502) ;
#53771 = AXIS2_PLACEMENT_3D('',#97764,#66503,#66504) ;
#53772 = AXIS2_PLACEMENT_3D('',#97766,#66506,#66507) ;
#53773 = AXIS2_PLACEMENT_3D('',#97769,#66508,#66509) ;
#53774 = AXIS2_PLACEMENT_3D('',#97770,#66510,#66511) ;
#53775 = AXIS2_PLACEMENT_3D('',#97808,#66512,#66513) ;
#53776 = AXIS2_PLACEMENT_3D('',#97814,#66514,#66515) ;
#53777 = AXIS2_PLACEMENT_3D('',#97815,#66516,#66517) ;
#53778 = AXIS2_PLACEMENT_3D('',#97819,#66519,#66520) ;
#53779 = AXIS2_PLACEMENT_3D('',#97836,#66521,#66522) ;
#53780 = AXIS2_PLACEMENT_3D('',#97837,#66523,#66524) ;
#53781 = AXIS2_PLACEMENT_3D('',#97868,#66525,#66526) ;
#53782 = AXIS2_PLACEMENT_3D('',#97895,#66527,#66528) ;
#53783 = AXIS2_PLACEMENT_3D('',#97896,#66529,#66530) ;
#53784 = AXIS2_PLACEMENT_3D('',#97897,#66531,#66532) ;
#53785 = AXIS2_PLACEMENT_3D('',#97899,#66533,#66534) ;
#53786 = AXIS2_PLACEMENT_3D('',#97900,#66535,#66536) ;
#53787 = AXIS2_PLACEMENT_3D('',#97901,#66537,#66538) ;
#53788 = AXIS2_PLACEMENT_3D('',#97924,#66540,#66541) ;
#53789 = AXIS2_PLACEMENT_3D('',#97930,#66542,#66543) ;
#53790 = AXIS2_PLACEMENT_3D('',#97931,#66544,#66545) ;
#53791 = AXIS2_PLACEMENT_3D('',#97935,#66547,#66548) ;
#53792 = AXIS2_PLACEMENT_3D('',#97952,#66549,#66550) ;
#53793 = AXIS2_PLACEMENT_3D('',#97953,#66551,#66552) ;
#53794 = AXIS2_PLACEMENT_3D('',#97984,#66553,#66554) ;
#53795 = AXIS2_PLACEMENT_3D('',#97985,#66555,#66556) ;
#53796 = AXIS2_PLACEMENT_3D('',#97987,#66557,#66558) ;
#53797 = AXIS2_PLACEMENT_3D('',#97990,#66560,#66561) ;
#53798 = AXIS2_PLACEMENT_3D('',#97991,#66562,#66563) ;
#53799 = AXIS2_PLACEMENT_3D('',#97992,#66564,#66565) ;
#53800 = AXIS2_PLACEMENT_3D('',#98002,#66566,#66567) ;
#53801 = AXIS2_PLACEMENT_3D('',#98003,#66568,#66569) ;
#53802 = AXIS2_PLACEMENT_3D('',#98005,#66571,#66572) ;
#53803 = AXIS2_PLACEMENT_3D('',#98007,#66573,#66574) ;
#53804 = AXIS2_PLACEMENT_3D('',#98010,#66576,#66577) ;
#53805 = AXIS2_PLACEMENT_3D('',#98011,#66578,#66579) ;
#53806 = AXIS2_PLACEMENT_3D('',#98012,#66580,#66581) ;
#53807 = AXIS2_PLACEMENT_3D('',#98013,#66582,#66583) ;
#53808 = AXIS2_PLACEMENT_3D('',#98016,#66584,#66585) ;
#53809 = AXIS2_PLACEMENT_3D('',#98020,#66587,#66588) ;
#53810 = AXIS2_PLACEMENT_3D('',#98042,#66590,#66591) ;
#53811 = AXIS2_PLACEMENT_3D('',#98043,#66592,#66593) ;
#53812 = AXIS2_PLACEMENT_3D('',#98053,#66594,#66595) ;
#53813 = AXIS2_PLACEMENT_3D('',#98076,#66596,#66597) ;
#53814 = AXIS2_PLACEMENT_3D('',#98077,#66598,#66599) ;
#53815 = AXIS2_PLACEMENT_3D('',#98078,#66600,#66601) ;
#53816 = AXIS2_PLACEMENT_3D('',#98079,#66602,#66603) ;
#53817 = AXIS2_PLACEMENT_3D('',#98082,#66604,#66605) ;
#53818 = AXIS2_PLACEMENT_3D('',#98085,#66608,#66609) ;
#53819 = AXIS2_PLACEMENT_3D('',#98089,#66611,#66612) ;
#53820 = AXIS2_PLACEMENT_3D('',#98113,#66614,#66615) ;
#53821 = AXIS2_PLACEMENT_3D('',#98114,#66616,#66617) ;
#53822 = AXIS2_PLACEMENT_3D('',#98115,#66618,#66619) ;
#53823 = AXIS2_PLACEMENT_3D('',#98116,#66620,#66621) ;
#53824 = AXIS2_PLACEMENT_3D('',#98119,#66624,#66625) ;
#53825 = AXIS2_PLACEMENT_3D('',#98122,#66628,#66629) ;
#53826 = AXIS2_PLACEMENT_3D('',#98124,#66631,#66632) ;
#53827 = AXIS2_PLACEMENT_3D('',#98126,#66634,#66635) ;
#53828 = AXIS2_PLACEMENT_3D('',#98128,#66637,#66638) ;
#53829 = AXIS2_PLACEMENT_3D('',#98129,#66639,#66640) ;
#53830 = AXIS2_PLACEMENT_3D('',#98130,#66641,#66642) ;
#53831 = AXIS2_PLACEMENT_3D('',#98131,#66643,#66644) ;
#53832 = AXIS2_PLACEMENT_3D('',#98132,#66645,#66646) ;
#53833 = AXIS2_PLACEMENT_3D('',#98135,#66649,#66650) ;
#53834 = AXIS2_PLACEMENT_3D('',#98138,#66653,#66654) ;
#53835 = AXIS2_PLACEMENT_3D('',#98144,#66658,#66659) ;
#53836 = AXIS2_PLACEMENT_3D('',#98146,#66660,#66661) ;
#53837 = AXIS2_PLACEMENT_3D('',#98148,#66663,#66664) ;
#53838 = AXIS2_PLACEMENT_3D('',#98152,#66667,#66668) ;
#53839 = AXIS2_PLACEMENT_3D('',#98156,#66671,#66672) ;
#53840 = AXIS2_PLACEMENT_3D('',#98158,#66673,#66674) ;
#53841 = AXIS2_PLACEMENT_3D('',#98160,#66676,#66677) ;
#53842 = AXIS2_PLACEMENT_3D('',#98164,#66680,#66681) ;
#53843 = AXIS2_PLACEMENT_3D('',#98166,#66682,#66683) ;
#53844 = AXIS2_PLACEMENT_3D('',#98168,#66685,#66686) ;
#53845 = AXIS2_PLACEMENT_3D('',#98172,#66689,#66690) ;
#53846 = AXIS2_PLACEMENT_3D('',#98196,#66694,#66695) ;
#53847 = AXIS2_PLACEMENT_3D('',#98218,#66698,#66699) ;
#53848 = AXIS2_PLACEMENT_3D('',#98220,#66701,#66702) ;
#53849 = AXIS2_PLACEMENT_3D('',#98223,#66704,#66705) ;
#53850 = AXIS2_PLACEMENT_3D('',#98224,#66706,#66707) ;
#53851 = AXIS2_PLACEMENT_3D('',#98225,#66708,#66709) ;
#53852 = AXIS2_PLACEMENT_3D('',#98228,#66711,#66712) ;
#53853 = AXIS2_PLACEMENT_3D('',#98229,#66713,#66714) ;
#53854 = AXIS2_PLACEMENT_3D('',#98235,#66718,#66719) ;
#53855 = AXIS2_PLACEMENT_3D('',#98237,#66720,#66721) ;
#53856 = AXIS2_PLACEMENT_3D('',#98239,#66723,#66724) ;
#53857 = AXIS2_PLACEMENT_3D('',#98243,#66727,#66728) ;
#53858 = AXIS2_PLACEMENT_3D('',#98245,#66729,#66730) ;
#53859 = AXIS2_PLACEMENT_3D('',#98247,#66732,#66733) ;
#53860 = AXIS2_PLACEMENT_3D('',#98251,#66736,#66737) ;
#53861 = AXIS2_PLACEMENT_3D('',#98254,#66738,#66739) ;
#53862 = AXIS2_PLACEMENT_3D('',#98257,#66742,#66743) ;
#53863 = AXIS2_PLACEMENT_3D('',#98261,#66746,#66747) ;
#53864 = AXIS2_PLACEMENT_3D('',#98263,#66748,#66749) ;
#53865 = AXIS2_PLACEMENT_3D('',#98265,#66751,#66752) ;
#53866 = AXIS2_PLACEMENT_3D('',#98269,#66755,#66756) ;
#53867 = AXIS2_PLACEMENT_3D('',#98273,#66759,#66760) ;
#53868 = AXIS2_PLACEMENT_3D('',#98275,#66761,#66762) ;
#53869 = AXIS2_PLACEMENT_3D('',#98277,#66764,#66765) ;
#53870 = AXIS2_PLACEMENT_3D('',#98281,#66768,#66769) ;
#53871 = AXIS2_PLACEMENT_3D('',#98284,#66771,#66772) ;
#53872 = AXIS2_PLACEMENT_3D('',#98285,#66773,#66774) ;
#53873 = AXIS2_PLACEMENT_3D('',#98291,#66778,#66779) ;
#53874 = AXIS2_PLACEMENT_3D('',#98293,#66780,#66781) ;
#53875 = AXIS2_PLACEMENT_3D('',#98295,#66783,#66784) ;
#53876 = AXIS2_PLACEMENT_3D('',#98299,#66787,#66788) ;
#53877 = AXIS2_PLACEMENT_3D('',#98301,#66789,#66790) ;
#53878 = AXIS2_PLACEMENT_3D('',#98303,#66792,#66793) ;
#53879 = AXIS2_PLACEMENT_3D('',#98327,#66797,#66798) ;
#53880 = AXIS2_PLACEMENT_3D('',#98330,#66799,#66800) ;
#53881 = AXIS2_PLACEMENT_3D('',#98333,#66803,#66804) ;
#53882 = AXIS2_PLACEMENT_3D('',#98337,#66807,#66808) ;
#53883 = AXIS2_PLACEMENT_3D('',#98339,#66809,#66810) ;
#53884 = AXIS2_PLACEMENT_3D('',#98341,#66812,#66813) ;
#53885 = AXIS2_PLACEMENT_3D('',#98345,#66816,#66817) ;
#53886 = AXIS2_PLACEMENT_3D('',#98347,#66819,#66820) ;
#53887 = AXIS2_PLACEMENT_3D('',#98351,#66823,#66824) ;
#53888 = AXIS2_PLACEMENT_3D('',#98354,#66825,#66826) ;
#53889 = AXIS2_PLACEMENT_3D('',#98357,#66829,#66830) ;
#53890 = AXIS2_PLACEMENT_3D('',#98362,#66834,#66835) ;
#53891 = AXIS2_PLACEMENT_3D('',#98364,#66836,#66837) ;
#53892 = AXIS2_PLACEMENT_3D('',#98366,#66839,#66840) ;
#53893 = AXIS2_PLACEMENT_3D('',#98370,#66843,#66844) ;
#53894 = AXIS2_PLACEMENT_3D('',#98371,#66845,#66846) ;
#53895 = AXIS2_PLACEMENT_3D('',#98372,#66847,#66848) ;
#53896 = AXIS2_PLACEMENT_3D('',#98375,#66849,#66850) ;
#53897 = AXIS2_PLACEMENT_3D('',#98378,#66853,#66854) ;
#53898 = AXIS2_PLACEMENT_3D('',#98382,#66857,#66858) ;
#53899 = AXIS2_PLACEMENT_3D('',#98384,#66859,#66860) ;
#53900 = AXIS2_PLACEMENT_3D('',#98386,#66862,#66863) ;
#53901 = AXIS2_PLACEMENT_3D('',#98390,#66866,#66867) ;
#53902 = AXIS2_PLACEMENT_3D('',#98394,#66870,#66871) ;
#53903 = AXIS2_PLACEMENT_3D('',#98396,#66872,#66873) ;
#53904 = AXIS2_PLACEMENT_3D('',#98398,#66875,#66876) ;
#53905 = AXIS2_PLACEMENT_3D('',#98402,#66879,#66880) ;
#53906 = AXIS2_PLACEMENT_3D('',#98404,#66881,#66882) ;
#53907 = AXIS2_PLACEMENT_3D('',#98406,#66884,#66885) ;
#53908 = AXIS2_PLACEMENT_3D('',#98410,#66888,#66889) ;
#53909 = AXIS2_PLACEMENT_3D('',#98414,#66892,#66893) ;
#53910 = AXIS2_PLACEMENT_3D('',#98416,#66894,#66895) ;
#53911 = AXIS2_PLACEMENT_3D('',#98418,#66897,#66898) ;
#53912 = AXIS2_PLACEMENT_3D('',#98422,#66901,#66902) ;
#53913 = AXIS2_PLACEMENT_3D('',#98424,#66903,#66904) ;
#53914 = AXIS2_PLACEMENT_3D('',#98426,#66906,#66907) ;
#53915 = AXIS2_PLACEMENT_3D('',#98428,#66909,#66910) ;
#53916 = AXIS2_PLACEMENT_3D('',#98429,#66911,#66912) ;
#53917 = AXIS2_PLACEMENT_3D('',#98453,#66916,#66917) ;
#53918 = AXIS2_PLACEMENT_3D('',#98457,#66920,#66921) ;
#53919 = AXIS2_PLACEMENT_3D('',#98459,#66922,#66923) ;
#53920 = AXIS2_PLACEMENT_3D('',#98461,#66925,#66926) ;
#53921 = AXIS2_PLACEMENT_3D('',#98465,#66929,#66930) ;
#53922 = AXIS2_PLACEMENT_3D('',#98466,#66931,#66932) ;
#53923 = AXIS2_PLACEMENT_3D('',#98467,#66933,#66934) ;
#53924 = AXIS2_PLACEMENT_3D('',#98488,#66936,#66937) ;
#53925 = AXIS2_PLACEMENT_3D('',#98492,#66940,#66941) ;
#53926 = AXIS2_PLACEMENT_3D('',#98496,#66944,#66945) ;
#53927 = AXIS2_PLACEMENT_3D('',#98498,#66946,#66947) ;
#53928 = AXIS2_PLACEMENT_3D('',#98500,#66949,#66950) ;
#53929 = AXIS2_PLACEMENT_3D('',#98504,#66953,#66954) ;
#53930 = AXIS2_PLACEMENT_3D('',#98506,#66955,#66956) ;
#53931 = AXIS2_PLACEMENT_3D('',#98508,#66958,#66959) ;
#53932 = AXIS2_PLACEMENT_3D('',#98510,#66961,#66962) ;
#53933 = AXIS2_PLACEMENT_3D('',#98511,#66963,#66964) ;
#53934 = AXIS2_PLACEMENT_3D('',#98513,#66965,#66966) ;
#53935 = AXIS2_PLACEMENT_3D('',#98515,#66968,#66969) ;
#53936 = AXIS2_PLACEMENT_3D('',#98519,#66972,#66973) ;
#53937 = AXIS2_PLACEMENT_3D('',#98523,#66976,#66977) ;
#53938 = AXIS2_PLACEMENT_3D('',#98527,#66980,#66981) ;
#53939 = AXIS2_PLACEMENT_3D('',#98531,#66984,#66985) ;
#53940 = AXIS2_PLACEMENT_3D('',#98535,#66988,#66989) ;
#53941 = AXIS2_PLACEMENT_3D('',#98537,#66990,#66991) ;
#53942 = AXIS2_PLACEMENT_3D('',#98539,#66993,#66994) ;
#53943 = AXIS2_PLACEMENT_3D('',#98541,#66995,#66996) ;
#53944 = AXIS2_PLACEMENT_3D('',#98543,#66998,#66999) ;
#53945 = AXIS2_PLACEMENT_3D('',#98545,#67000,#67001) ;
#53946 = AXIS2_PLACEMENT_3D('',#98547,#67003,#67004) ;
#53947 = AXIS2_PLACEMENT_3D('',#98551,#67007,#67008) ;
#53948 = AXIS2_PLACEMENT_3D('',#98555,#67011,#67012) ;
#53949 = AXIS2_PLACEMENT_3D('',#98557,#67013,#67014) ;
#53950 = AXIS2_PLACEMENT_3D('',#98559,#67016,#67017) ;
#53951 = AXIS2_PLACEMENT_3D('',#98563,#67020,#67021) ;
#53952 = AXIS2_PLACEMENT_3D('',#98565,#67022,#67023) ;
#53953 = AXIS2_PLACEMENT_3D('',#98567,#67025,#67026) ;
#53954 = AXIS2_PLACEMENT_3D('',#98569,#67028,#67029) ;
#53955 = AXIS2_PLACEMENT_3D('',#98570,#67030,#67031) ;
#53956 = AXIS2_PLACEMENT_3D('',#98572,#67032,#67033) ;
#53957 = AXIS2_PLACEMENT_3D('',#98574,#67035,#67036) ;
#53958 = AXIS2_PLACEMENT_3D('',#98578,#67039,#67040) ;
#53959 = AXIS2_PLACEMENT_3D('',#98580,#67041,#67042) ;
#53960 = AXIS2_PLACEMENT_3D('',#98582,#67044,#67045) ;
#53961 = AXIS2_PLACEMENT_3D('',#98586,#67048,#67049) ;
#53962 = AXIS2_PLACEMENT_3D('',#98588,#67050,#67051) ;
#53963 = AXIS2_PLACEMENT_3D('',#98590,#67053,#67054) ;
#53964 = AXIS2_PLACEMENT_3D('',#98592,#67056,#67057) ;
#53965 = AXIS2_PLACEMENT_3D('',#98593,#67058,#67059) ;
#53966 = AXIS2_PLACEMENT_3D('',#98594,#67060,#67061) ;
#53967 = AXIS2_PLACEMENT_3D('',#98596,#67062,#67063) ;
#53968 = AXIS2_PLACEMENT_3D('',#98598,#67065,#67066) ;
#53969 = AXIS2_PLACEMENT_3D('',#98602,#67069,#67070) ;
#53970 = AXIS2_PLACEMENT_3D('',#98603,#67071,#67072) ;
#53971 = AXIS2_PLACEMENT_3D('',#98606,#67075,#67076) ;
#53972 = AXIS2_PLACEMENT_3D('',#98609,#67079,#67080) ;
#53973 = AXIS2_PLACEMENT_3D('',#98611,#67082,#67083) ;
#53974 = AXIS2_PLACEMENT_3D('',#98614,#67086,#67087) ;
#53975 = AXIS2_PLACEMENT_3D('',#98615,#67088,#67089) ;
#53976 = AXIS2_PLACEMENT_3D('',#98617,#67091,#67092) ;
#53977 = AXIS2_PLACEMENT_3D('',#98619,#67094,#67095) ;
#53978 = AXIS2_PLACEMENT_3D('',#98621,#67097,#67098) ;
#53979 = AXIS2_PLACEMENT_3D('',#98623,#67100,#67101) ;
#53980 = AXIS2_PLACEMENT_3D('',#98625,#67103,#67104) ;
#53981 = AXIS2_PLACEMENT_3D('',#98626,#67105,#67106) ;
#53982 = AXIS2_PLACEMENT_3D('',#98628,#67107,#67108) ;
#53983 = AXIS2_PLACEMENT_3D('',#98629,#67109,#67110) ;
#53984 = AXIS2_PLACEMENT_3D('',#98630,#67111,#67112) ;
#53985 = AXIS2_PLACEMENT_3D('',#98632,#67114,#67115) ;
#53986 = AXIS2_PLACEMENT_3D('',#98633,#67116,#67117) ;
#53987 = AXIS2_PLACEMENT_3D('',#98635,#67119,#67120) ;
#53988 = AXIS2_PLACEMENT_3D('',#98637,#67122,#67123) ;
#53989 = AXIS2_PLACEMENT_3D('',#98638,#67124,#67125) ;
#53990 = AXIS2_PLACEMENT_3D('',#98640,#67127,#67128) ;
#53991 = AXIS2_PLACEMENT_3D('',#98641,#67129,#67130) ;
#53992 = AXIS2_PLACEMENT_3D('',#98643,#67132,#67133) ;
#53993 = AXIS2_PLACEMENT_3D('',#98644,#67134,#67135) ;
#53994 = AXIS2_PLACEMENT_3D('',#98646,#67137,#67138) ;
#53995 = AXIS2_PLACEMENT_3D('',#98647,#67139,#67140) ;
#53996 = AXIS2_PLACEMENT_3D('',#98648,#67141,#67142) ;
#53997 = AXIS2_PLACEMENT_3D('',#98650,#67144,#67145) ;
#53998 = AXIS2_PLACEMENT_3D('',#98651,#67146,#67147) ;
#53999 = AXIS2_PLACEMENT_3D('',#98653,#67149,#67150) ;
#54000 = AXIS2_PLACEMENT_3D('',#98655,#67152,#67153) ;
#54001 = AXIS2_PLACEMENT_3D('',#98657,#67155,#67156) ;
#54002 = AXIS2_PLACEMENT_3D('',#98659,#67158,#67159) ;
#54003 = AXIS2_PLACEMENT_3D('',#98661,#67161,#67162) ;
#54004 = AXIS2_PLACEMENT_3D('',#98662,#67163,#67164) ;
#54005 = AXIS2_PLACEMENT_3D('',#98664,#67166,#67167) ;
#54006 = AXIS2_PLACEMENT_3D('',#98665,#67168,#67169) ;
#54007 = AXIS2_PLACEMENT_3D('',#98668,#67172,#67173) ;
#54008 = AXIS2_PLACEMENT_3D('',#98669,#67174,#67175) ;
#54009 = AXIS2_PLACEMENT_3D('',#98670,#67176,#67177) ;
#54010 = AXIS2_PLACEMENT_3D('',#98671,#67178,#67179) ;
#54011 = AXIS2_PLACEMENT_3D('',#98672,#67180,#67181) ;
#54012 = AXIS2_PLACEMENT_3D('',#98673,#67182,#67183) ;
#54013 = AXIS2_PLACEMENT_3D('',#98682,#67188,#67189) ;
#54014 = AXIS2_PLACEMENT_3D('',#98688,#67193,#67194) ;
#54015 = AXIS2_PLACEMENT_3D('',#98694,#67198,#67199) ;
#54016 = AXIS2_PLACEMENT_3D('',#98700,#67203,#67204) ;
#54017 = AXIS2_PLACEMENT_3D('',#98706,#67208,#67209) ;
#54018 = AXIS2_PLACEMENT_3D('',#98712,#67213,#67214) ;
#54019 = AXIS2_PLACEMENT_3D('',#98718,#67218,#67219) ;
#54020 = AXIS2_PLACEMENT_3D('',#98720,#67221,#67222) ;
#54021 = AXIS2_PLACEMENT_3D('',#98722,#67224,#67225) ;
#54022 = AXIS2_PLACEMENT_3D('',#98731,#67230,#67231) ;
#54023 = AXIS2_PLACEMENT_3D('',#98738,#67236,#67237) ;
#54024 = AXIS2_PLACEMENT_3D('',#98744,#67241,#67242) ;
#54025 = AXIS2_PLACEMENT_3D('',#98747,#67245,#67246) ;
#54026 = AXIS2_PLACEMENT_3D('',#98748,#67247,#67248) ;
#54027 = AXIS2_PLACEMENT_3D('',#98749,#67249,#67250) ;
#54028 = AXIS2_PLACEMENT_3D('',#98750,#67251,#67252) ;
#54029 = AXIS2_PLACEMENT_3D('',#98836,#67254,#67255) ;
#54030 = AXIS2_PLACEMENT_3D('',#98887,#67256,#67257) ;
#54031 = AXIS2_PLACEMENT_3D('',#99175,#67259,#67260) ;
#54032 = AXIS2_PLACEMENT_3D('',#99298,#67262,#67263) ;
#54033 = AXIS2_PLACEMENT_3D('',#99534,#67265,#67266) ;
#54034 = AXIS2_PLACEMENT_3D('',#99537,#67267,#67268) ;
#54035 = AXIS2_PLACEMENT_3D('',#100195,#67269,#67270) ;
#54036 = AXIS2_PLACEMENT_3D('',#100950,#67271,#67272) ;
#54037 = AXIS2_PLACEMENT_3D('',#100951,#67273,#67274) ;
#54038 = AXIS2_PLACEMENT_3D('',#101050,#67275,#67276) ;
#54039 = AXIS2_PLACEMENT_3D('',#101141,#67277,#67278) ;
#54040 = AXIS2_PLACEMENT_3D('',#101743,#67279,#67280) ;
#54041 = AXIS2_PLACEMENT_3D('',#101744,#67281,#67282) ;
#54042 = AXIS2_PLACEMENT_3D('',#101745,#67283,#67284) ;
#54043 = AXIS2_PLACEMENT_3D('',#101746,#67285,#67286) ;
#54044 = AXIS2_PLACEMENT_3D('',#101748,#67287,#67288) ;
#54045 = AXIS2_PLACEMENT_3D('',#101750,#67289,#67290) ;
#54046 = AXIS2_PLACEMENT_3D('',#101751,#67291,#67292) ;
#54047 = AXIS2_PLACEMENT_3D('',#101752,#67293,#67294) ;
#54048 = AXIS2_PLACEMENT_3D('',#101770,#67295,#67296) ;
#54049 = AXIS2_PLACEMENT_3D('',#101772,#67297,#67298) ;
#54050 = AXIS2_PLACEMENT_3D('',#101774,#67299,#67300) ;
#54051 = AXIS2_PLACEMENT_3D('',#101775,#67301,#67302) ;
#54052 = AXIS2_PLACEMENT_3D('',#101776,#67303,#67304) ;
#54053 = AXIS2_PLACEMENT_3D('',#101794,#67305,#67306) ;
#54054 = AXIS2_PLACEMENT_3D('',#101796,#67307,#67308) ;
#54055 = AXIS2_PLACEMENT_3D('',#101797,#67309,#67310) ;
#54056 = AXIS2_PLACEMENT_3D('',#101799,#67311,#67312) ;
#54057 = AXIS2_PLACEMENT_3D('',#102014,#67313,#67314) ;
#54058 = AXIS2_PLACEMENT_3D('',#102017,#67315,#67316) ;
#54059 = AXIS2_PLACEMENT_3D('',#102034,#67317,#67318) ;
#54060 = AXIS2_PLACEMENT_3D('',#102049,#67319,#67320) ;
#54061 = AXIS2_PLACEMENT_3D('',#102070,#67323,#67324) ;
#54062 = AXIS2_PLACEMENT_3D('',#102072,#67325,#67326) ;
#54063 = AXIS2_PLACEMENT_3D('',#102090,#67327,#67328) ;
#54064 = AXIS2_PLACEMENT_3D('',#102091,#67329,#67330) ;
#54065 = AXIS2_PLACEMENT_3D('',#102110,#67333,#67334) ;
#54066 = AXIS2_PLACEMENT_3D('',#102112,#67335,#67336) ;
#54067 = AXIS2_PLACEMENT_3D('',#102128,#67337,#67338) ;
#54068 = AXIS2_PLACEMENT_3D('',#102129,#67339,#67340) ;
#54069 = AXIS2_PLACEMENT_3D('',#102150,#67343,#67344) ;
#54070 = AXIS2_PLACEMENT_3D('',#102152,#67345,#67346) ;
#54071 = AXIS2_PLACEMENT_3D('',#102170,#67347,#67348) ;
#54072 = AXIS2_PLACEMENT_3D('',#102171,#67349,#67350) ;
#54073 = AXIS2_PLACEMENT_3D('',#102190,#67353,#67354) ;
#54074 = AXIS2_PLACEMENT_3D('',#102192,#67355,#67356) ;
#54075 = AXIS2_PLACEMENT_3D('',#102208,#67357,#67358) ;
#54076 = AXIS2_PLACEMENT_3D('',#102209,#67359,#67360) ;
#54077 = AXIS2_PLACEMENT_3D('',#102230,#67363,#67364) ;
#54078 = AXIS2_PLACEMENT_3D('',#102232,#67365,#67366) ;
#54079 = AXIS2_PLACEMENT_3D('',#102250,#67367,#67368) ;
#54080 = AXIS2_PLACEMENT_3D('',#102251,#67369,#67370) ;
#54081 = AXIS2_PLACEMENT_3D('',#102270,#67373,#67374) ;
#54082 = AXIS2_PLACEMENT_3D('',#102272,#67375,#67376) ;
#54083 = AXIS2_PLACEMENT_3D('',#102288,#67377,#67378) ;
#54084 = AXIS2_PLACEMENT_3D('',#102289,#67379,#67380) ;
#54085 = AXIS2_PLACEMENT_3D('',#102310,#67383,#67384) ;
#54086 = AXIS2_PLACEMENT_3D('',#102312,#67385,#67386) ;
#54087 = AXIS2_PLACEMENT_3D('',#102330,#67387,#67388) ;
#54088 = AXIS2_PLACEMENT_3D('',#102331,#67389,#67390) ;
#54089 = AXIS2_PLACEMENT_3D('',#102350,#67393,#67394) ;
#54090 = AXIS2_PLACEMENT_3D('',#102352,#67395,#67396) ;
#54091 = AXIS2_PLACEMENT_3D('',#102368,#67397,#67398) ;
#54092 = AXIS2_PLACEMENT_3D('',#102369,#67399,#67400) ;
#54093 = AXIS2_PLACEMENT_3D('',#102390,#67403,#67404) ;
#54094 = AXIS2_PLACEMENT_3D('',#102392,#67405,#67406) ;
#54095 = AXIS2_PLACEMENT_3D('',#102410,#67407,#67408) ;
#54096 = AXIS2_PLACEMENT_3D('',#102411,#67409,#67410) ;
#54097 = AXIS2_PLACEMENT_3D('',#102430,#67413,#67414) ;
#54098 = AXIS2_PLACEMENT_3D('',#102432,#67415,#67416) ;
#54099 = AXIS2_PLACEMENT_3D('',#102448,#67417,#67418) ;
#54100 = AXIS2_PLACEMENT_3D('',#102449,#67419,#67420) ;
#54101 = AXIS2_PLACEMENT_3D('',#102470,#67423,#67424) ;
#54102 = AXIS2_PLACEMENT_3D('',#102472,#67425,#67426) ;
#54103 = AXIS2_PLACEMENT_3D('',#102490,#67427,#67428) ;
#54104 = AXIS2_PLACEMENT_3D('',#102491,#67429,#67430) ;
#54105 = AXIS2_PLACEMENT_3D('',#102510,#67433,#67434) ;
#54106 = AXIS2_PLACEMENT_3D('',#102512,#67435,#67436) ;
#54107 = AXIS2_PLACEMENT_3D('',#102528,#67437,#67438) ;
#54108 = AXIS2_PLACEMENT_3D('',#102529,#67439,#67440) ;
#54109 = AXIS2_PLACEMENT_3D('',#102550,#67443,#67444) ;
#54110 = AXIS2_PLACEMENT_3D('',#102552,#67445,#67446) ;
#54111 = AXIS2_PLACEMENT_3D('',#102570,#67447,#67448) ;
#54112 = AXIS2_PLACEMENT_3D('',#102571,#67449,#67450) ;
#54113 = AXIS2_PLACEMENT_3D('',#102590,#67453,#67454) ;
#54114 = AXIS2_PLACEMENT_3D('',#102592,#67455,#67456) ;
#54115 = AXIS2_PLACEMENT_3D('',#102608,#67457,#67458) ;
#54116 = AXIS2_PLACEMENT_3D('',#102609,#67459,#67460) ;
#54117 = AXIS2_PLACEMENT_3D('',#102630,#67463,#67464) ;
#54118 = AXIS2_PLACEMENT_3D('',#102632,#67465,#67466) ;
#54119 = AXIS2_PLACEMENT_3D('',#102650,#67467,#67468) ;
#54120 = AXIS2_PLACEMENT_3D('',#102651,#67469,#67470) ;
#54121 = AXIS2_PLACEMENT_3D('',#102670,#67473,#67474) ;
#54122 = AXIS2_PLACEMENT_3D('',#102672,#67475,#67476) ;
#54123 = AXIS2_PLACEMENT_3D('',#102688,#67477,#67478) ;
#54124 = AXIS2_PLACEMENT_3D('',#102689,#67479,#67480) ;
#54125 = AXIS2_PLACEMENT_3D('',#102710,#67483,#67484) ;
#54126 = AXIS2_PLACEMENT_3D('',#102712,#67485,#67486) ;
#54127 = AXIS2_PLACEMENT_3D('',#102730,#67487,#67488) ;
#54128 = AXIS2_PLACEMENT_3D('',#102731,#67489,#67490) ;
#54129 = AXIS2_PLACEMENT_3D('',#102750,#67493,#67494) ;
#54130 = AXIS2_PLACEMENT_3D('',#102752,#67495,#67496) ;
#54131 = AXIS2_PLACEMENT_3D('',#102768,#67497,#67498) ;
#54132 = AXIS2_PLACEMENT_3D('',#102769,#67499,#67500) ;
#54133 = AXIS2_PLACEMENT_3D('',#102790,#67503,#67504) ;
#54134 = AXIS2_PLACEMENT_3D('',#102792,#67505,#67506) ;
#54135 = AXIS2_PLACEMENT_3D('',#102810,#67507,#67508) ;
#54136 = AXIS2_PLACEMENT_3D('',#102811,#67509,#67510) ;
#54137 = AXIS2_PLACEMENT_3D('',#102830,#67513,#67514) ;
#54138 = AXIS2_PLACEMENT_3D('',#102832,#67515,#67516) ;
#54139 = AXIS2_PLACEMENT_3D('',#102848,#67517,#67518) ;
#54140 = AXIS2_PLACEMENT_3D('',#102849,#67519,#67520) ;
#54141 = AXIS2_PLACEMENT_3D('',#102870,#67523,#67524) ;
#54142 = AXIS2_PLACEMENT_3D('',#102872,#67525,#67526) ;
#54143 = AXIS2_PLACEMENT_3D('',#102874,#67527,#67528) ;
#54144 = AXIS2_PLACEMENT_3D('',#102891,#67529,#67530) ;
#54145 = AXIS2_PLACEMENT_3D('',#102910,#67533,#67534) ;
#54146 = AXIS2_PLACEMENT_3D('',#102912,#67535,#67536) ;
#54147 = AXIS2_PLACEMENT_3D('',#102914,#67537,#67538) ;
#54148 = AXIS2_PLACEMENT_3D('',#102929,#67539,#67540) ;
#54149 = AXIS2_PLACEMENT_3D('',#102950,#67543,#67544) ;
#54150 = AXIS2_PLACEMENT_3D('',#102952,#67545,#67546) ;
#54151 = AXIS2_PLACEMENT_3D('',#102954,#67547,#67548) ;
#54152 = AXIS2_PLACEMENT_3D('',#102971,#67549,#67550) ;
#54153 = AXIS2_PLACEMENT_3D('',#102990,#67553,#67554) ;
#54154 = AXIS2_PLACEMENT_3D('',#102992,#67555,#67556) ;
#54155 = AXIS2_PLACEMENT_3D('',#102994,#67557,#67558) ;
#54156 = AXIS2_PLACEMENT_3D('',#103009,#67559,#67560) ;
#54157 = AXIS2_PLACEMENT_3D('',#103030,#67563,#67564) ;
#54158 = AXIS2_PLACEMENT_3D('',#103032,#67565,#67566) ;
#54159 = AXIS2_PLACEMENT_3D('',#103034,#67567,#67568) ;
#54160 = AXIS2_PLACEMENT_3D('',#103051,#67569,#67570) ;
#54161 = AXIS2_PLACEMENT_3D('',#103070,#67573,#67574) ;
#54162 = AXIS2_PLACEMENT_3D('',#103072,#67575,#67576) ;
#54163 = AXIS2_PLACEMENT_3D('',#103074,#67577,#67578) ;
#54164 = AXIS2_PLACEMENT_3D('',#103089,#67579,#67580) ;
#54165 = AXIS2_PLACEMENT_3D('',#103110,#67583,#67584) ;
#54166 = AXIS2_PLACEMENT_3D('',#103112,#67585,#67586) ;
#54167 = AXIS2_PLACEMENT_3D('',#103114,#67587,#67588) ;
#54168 = AXIS2_PLACEMENT_3D('',#103131,#67589,#67590) ;
#54169 = AXIS2_PLACEMENT_3D('',#103150,#67593,#67594) ;
#54170 = AXIS2_PLACEMENT_3D('',#103152,#67595,#67596) ;
#54171 = AXIS2_PLACEMENT_3D('',#103154,#67597,#67598) ;
#54172 = AXIS2_PLACEMENT_3D('',#103169,#67599,#67600) ;
#54173 = AXIS2_PLACEMENT_3D('',#103190,#67603,#67604) ;
#54174 = AXIS2_PLACEMENT_3D('',#103192,#67605,#67606) ;
#54175 = AXIS2_PLACEMENT_3D('',#103194,#67607,#67608) ;
#54176 = AXIS2_PLACEMENT_3D('',#103211,#67609,#67610) ;
#54177 = AXIS2_PLACEMENT_3D('',#103230,#67613,#67614) ;
#54178 = AXIS2_PLACEMENT_3D('',#103232,#67615,#67616) ;
#54179 = AXIS2_PLACEMENT_3D('',#103234,#67617,#67618) ;
#54180 = AXIS2_PLACEMENT_3D('',#103249,#67619,#67620) ;
#54181 = AXIS2_PLACEMENT_3D('',#103270,#67623,#67624) ;
#54182 = AXIS2_PLACEMENT_3D('',#103272,#67625,#67626) ;
#54183 = AXIS2_PLACEMENT_3D('',#103274,#67627,#67628) ;
#54184 = AXIS2_PLACEMENT_3D('',#103291,#67629,#67630) ;
#54185 = AXIS2_PLACEMENT_3D('',#103310,#67633,#67634) ;
#54186 = AXIS2_PLACEMENT_3D('',#103312,#67635,#67636) ;
#54187 = AXIS2_PLACEMENT_3D('',#103314,#67637,#67638) ;
#54188 = AXIS2_PLACEMENT_3D('',#103329,#67639,#67640) ;
#54189 = AXIS2_PLACEMENT_3D('',#103350,#67643,#67644) ;
#54190 = AXIS2_PLACEMENT_3D('',#103352,#67645,#67646) ;
#54191 = AXIS2_PLACEMENT_3D('',#103354,#67647,#67648) ;
#54192 = AXIS2_PLACEMENT_3D('',#103371,#67649,#67650) ;
#54193 = AXIS2_PLACEMENT_3D('',#103390,#67653,#67654) ;
#54194 = AXIS2_PLACEMENT_3D('',#103392,#67655,#67656) ;
#54195 = AXIS2_PLACEMENT_3D('',#103394,#67657,#67658) ;
#54196 = AXIS2_PLACEMENT_3D('',#103409,#67659,#67660) ;
#54197 = AXIS2_PLACEMENT_3D('',#103430,#67663,#67664) ;
#54198 = AXIS2_PLACEMENT_3D('',#103432,#67665,#67666) ;
#54199 = AXIS2_PLACEMENT_3D('',#103434,#67667,#67668) ;
#54200 = AXIS2_PLACEMENT_3D('',#103451,#67669,#67670) ;
#54201 = AXIS2_PLACEMENT_3D('',#103470,#67673,#67674) ;
#54202 = AXIS2_PLACEMENT_3D('',#103472,#67675,#67676) ;
#54203 = AXIS2_PLACEMENT_3D('',#103474,#67677,#67678) ;
#54204 = AXIS2_PLACEMENT_3D('',#103489,#67679,#67680) ;
#54205 = AXIS2_PLACEMENT_3D('',#103510,#67683,#67684) ;
#54206 = AXIS2_PLACEMENT_3D('',#103512,#67685,#67686) ;
#54207 = AXIS2_PLACEMENT_3D('',#103514,#67687,#67688) ;
#54208 = AXIS2_PLACEMENT_3D('',#103531,#67689,#67690) ;
#54209 = AXIS2_PLACEMENT_3D('',#103550,#67693,#67694) ;
#54210 = AXIS2_PLACEMENT_3D('',#103552,#67695,#67696) ;
#54211 = AXIS2_PLACEMENT_3D('',#103554,#67697,#67698) ;
#54212 = AXIS2_PLACEMENT_3D('',#103569,#67699,#67700) ;
#54213 = AXIS2_PLACEMENT_3D('',#103590,#67703,#67704) ;
#54214 = AXIS2_PLACEMENT_3D('',#103592,#67705,#67706) ;
#54215 = AXIS2_PLACEMENT_3D('',#103594,#67707,#67708) ;
#54216 = AXIS2_PLACEMENT_3D('',#103611,#67709,#67710) ;
#54217 = AXIS2_PLACEMENT_3D('',#103614,#67713,#67714) ;
#54218 = AXIS2_PLACEMENT_3D('',#103620,#67718,#67719) ;
#54219 = AXIS2_PLACEMENT_3D('',#103623,#67721,#67722) ;
#54220 = AXIS2_PLACEMENT_3D('',#103624,#67723,#67724) ;
#54221 = AXIS2_PLACEMENT_3D('',#103628,#67727,#67728) ;
#54222 = AXIS2_PLACEMENT_3D('',#103631,#67730,#67731) ;
#54223 = AXIS2_PLACEMENT_3D('',#103632,#67732,#67733) ;
#54224 = AXIS2_PLACEMENT_3D('',#103636,#67736,#67737) ;
#54225 = AXIS2_PLACEMENT_3D('',#103639,#67739,#67740) ;
#54226 = AXIS2_PLACEMENT_3D('',#103640,#67741,#67742) ;
#54227 = AXIS2_PLACEMENT_3D('',#103644,#67745,#67746) ;
#54228 = AXIS2_PLACEMENT_3D('',#103647,#67748,#67749) ;
#54229 = AXIS2_PLACEMENT_3D('',#103648,#67750,#67751) ;
#54230 = AXIS2_PLACEMENT_3D('',#103652,#67754,#67755) ;
#54231 = AXIS2_PLACEMENT_3D('',#103655,#67757,#67758) ;
#54232 = AXIS2_PLACEMENT_3D('',#103656,#67759,#67760) ;
#54233 = AXIS2_PLACEMENT_3D('',#103660,#67763,#67764) ;
#54234 = AXIS2_PLACEMENT_3D('',#103663,#67766,#67767) ;
#54235 = AXIS2_PLACEMENT_3D('',#103664,#67768,#67769) ;
#54236 = AXIS2_PLACEMENT_3D('',#103668,#67772,#67773) ;
#54237 = AXIS2_PLACEMENT_3D('',#103671,#67775,#67776) ;
#54238 = AXIS2_PLACEMENT_3D('',#103672,#67777,#67778) ;
#54239 = AXIS2_PLACEMENT_3D('',#103676,#67781,#67782) ;
#54240 = AXIS2_PLACEMENT_3D('',#103679,#67784,#67785) ;
#54241 = AXIS2_PLACEMENT_3D('',#103680,#67786,#67787) ;
#54242 = AXIS2_PLACEMENT_3D('',#103684,#67790,#67791) ;
#54243 = AXIS2_PLACEMENT_3D('',#103687,#67793,#67794) ;
#54244 = AXIS2_PLACEMENT_3D('',#103688,#67795,#67796) ;
#54245 = AXIS2_PLACEMENT_3D('',#103692,#67799,#67800) ;
#54246 = AXIS2_PLACEMENT_3D('',#103695,#67802,#67803) ;
#54247 = AXIS2_PLACEMENT_3D('',#103696,#67804,#67805) ;
#54248 = AXIS2_PLACEMENT_3D('',#103700,#67808,#67809) ;
#54249 = AXIS2_PLACEMENT_3D('',#103703,#67811,#67812) ;
#54250 = AXIS2_PLACEMENT_3D('',#103704,#67813,#67814) ;
#54251 = AXIS2_PLACEMENT_3D('',#103708,#67817,#67818) ;
#54252 = AXIS2_PLACEMENT_3D('',#103711,#67820,#67821) ;
#54253 = AXIS2_PLACEMENT_3D('',#103712,#67822,#67823) ;
#54254 = AXIS2_PLACEMENT_3D('',#103716,#67826,#67827) ;
#54255 = AXIS2_PLACEMENT_3D('',#103719,#67829,#67830) ;
#54256 = AXIS2_PLACEMENT_3D('',#103720,#67831,#67832) ;
#54257 = AXIS2_PLACEMENT_3D('',#103724,#67835,#67836) ;
#54258 = AXIS2_PLACEMENT_3D('',#103727,#67838,#67839) ;
#54259 = AXIS2_PLACEMENT_3D('',#103728,#67840,#67841) ;
#54260 = AXIS2_PLACEMENT_3D('',#103732,#67844,#67845) ;
#54261 = AXIS2_PLACEMENT_3D('',#103735,#67847,#67848) ;
#54262 = AXIS2_PLACEMENT_3D('',#103736,#67849,#67850) ;
#54263 = AXIS2_PLACEMENT_3D('',#103740,#67853,#67854) ;
#54264 = AXIS2_PLACEMENT_3D('',#103743,#67856,#67857) ;
#54265 = AXIS2_PLACEMENT_3D('',#103744,#67858,#67859) ;
#54266 = AXIS2_PLACEMENT_3D('',#103748,#67862,#67863) ;
#54267 = AXIS2_PLACEMENT_3D('',#103751,#67865,#67866) ;
#54268 = AXIS2_PLACEMENT_3D('',#103752,#67867,#67868) ;
#54269 = AXIS2_PLACEMENT_3D('',#103756,#67871,#67872) ;
#54270 = AXIS2_PLACEMENT_3D('',#103759,#67874,#67875) ;
#54271 = AXIS2_PLACEMENT_3D('',#103760,#67876,#67877) ;
#54272 = AXIS2_PLACEMENT_3D('',#103764,#67880,#67881) ;
#54273 = AXIS2_PLACEMENT_3D('',#103767,#67883,#67884) ;
#54274 = AXIS2_PLACEMENT_3D('',#103768,#67885,#67886) ;
#54275 = AXIS2_PLACEMENT_3D('',#103772,#67889,#67890) ;
#54276 = AXIS2_PLACEMENT_3D('',#103775,#67892,#67893) ;
#54277 = AXIS2_PLACEMENT_3D('',#103776,#67894,#67895) ;
#54278 = AXIS2_PLACEMENT_3D('',#103777,#67896,#67897) ;
#54279 = AXIS2_PLACEMENT_3D('',#103778,#67898,#67899) ;
#54280 = AXIS2_PLACEMENT_3D('',#103779,#67900,#67901) ;
#54281 = AXIS2_PLACEMENT_3D('',#103780,#67902,#67903) ;
#54282 = AXIS2_PLACEMENT_3D('',#103781,#67904,#67905) ;
#54283 = AXIS2_PLACEMENT_3D('',#103782,#67906,#67907) ;
#54284 = AXIS2_PLACEMENT_3D('',#103783,#67908,#67909) ;
#54285 = AXIS2_PLACEMENT_3D('',#103784,#67910,#67911) ;
#54286 = AXIS2_PLACEMENT_3D('',#103785,#67912,#67913) ;
#54287 = AXIS2_PLACEMENT_3D('',#103786,#67914,#67915) ;
#54288 = AXIS2_PLACEMENT_3D('',#103787,#67916,#67917) ;
#54289 = AXIS2_PLACEMENT_3D('',#103788,#67918,#67919) ;
#54290 = AXIS2_PLACEMENT_3D('',#103789,#67920,#67921) ;
#54291 = AXIS2_PLACEMENT_3D('',#103790,#67922,#67923) ;
#54292 = AXIS2_PLACEMENT_3D('',#103791,#67924,#67925) ;
#54293 = AXIS2_PLACEMENT_3D('',#103792,#67926,#67927) ;
#54294 = AXIS2_PLACEMENT_3D('',#103793,#67928,#67929) ;
#54295 = AXIS2_PLACEMENT_3D('',#103794,#67930,#67931) ;
#54296 = AXIS2_PLACEMENT_3D('',#103795,#67932,#67933) ;
#54297 = AXIS2_PLACEMENT_3D('',#103796,#67934,#67935) ;
#54298 = AXIS2_PLACEMENT_3D('',#103797,#67936,#67937) ;
#54299 = AXIS2_PLACEMENT_3D('',#103798,#67938,#67939) ;
#54300 = AXIS2_PLACEMENT_3D('',#103799,#67940,#67941) ;
#54301 = AXIS2_PLACEMENT_3D('',#103800,#67942,#67943) ;
#54302 = AXIS2_PLACEMENT_3D('',#103801,#67944,#67945) ;
#54303 = AXIS2_PLACEMENT_3D('',#103802,#67946,#67947) ;
#54304 = AXIS2_PLACEMENT_3D('',#103803,#67948,#67949) ;
#54305 = AXIS2_PLACEMENT_3D('',#103804,#67950,#67951) ;
#54306 = AXIS2_PLACEMENT_3D('',#103805,#67952,#67953) ;
#54307 = AXIS2_PLACEMENT_3D('',#103806,#67954,#67955) ;
#54308 = AXIS2_PLACEMENT_3D('',#103807,#67956,#67957) ;
#54309 = AXIS2_PLACEMENT_3D('',#103808,#67958,#67959) ;
#54310 = AXIS2_PLACEMENT_3D('',#103809,#67960,#67961) ;
#54311 = AXIS2_PLACEMENT_3D('',#103810,#67962,#67963) ;
#54312 = AXIS2_PLACEMENT_3D('',#103811,#67964,#67965) ;
#54313 = AXIS2_PLACEMENT_3D('',#103812,#67966,#67967) ;
#54314 = AXIS2_PLACEMENT_3D('',#103814,#67968,#67969) ;
#54315 = AXIS2_PLACEMENT_3D('',#103815,#67970,#67971) ;
#54316 = AXIS2_PLACEMENT_3D('',#103816,#67972,#67973) ;
#54317 = AXIS2_PLACEMENT_3D('',#103817,#67974,#67975) ;
#54318 = AXIS2_PLACEMENT_3D('',#103818,#67976,#67977) ;
#54319 = AXIS2_PLACEMENT_3D('',#103819,#67978,#67979) ;
#54320 = AXIS2_PLACEMENT_3D('',#103820,#67980,#67981) ;
#54321 = AXIS2_PLACEMENT_3D('',#103822,#67982,#67983) ;
#54322 = AXIS2_PLACEMENT_3D('',#103824,#67984,#67985) ;
#54323 = AXIS2_PLACEMENT_3D('',#103826,#67986,#67987) ;
#54324 = AXIS2_PLACEMENT_3D('',#103828,#67988,#67989) ;
#54325 = AXIS2_PLACEMENT_3D('',#103830,#67990,#67991) ;
#54326 = AXIS2_PLACEMENT_3D('',#103832,#67992,#67993) ;
#54327 = AXIS2_PLACEMENT_3D('',#103834,#67994,#67995) ;
#54328 = AXIS2_PLACEMENT_3D('',#103836,#67996,#67997) ;
#54329 = AXIS2_PLACEMENT_3D('',#103838,#67998,#67999) ;
#54330 = AXIS2_PLACEMENT_3D('',#103840,#68000,#68001) ;
#54331 = AXIS2_PLACEMENT_3D('',#103842,#68002,#68003) ;
#54332 = AXIS2_PLACEMENT_3D('',#103844,#68004,#68005) ;
#54333 = AXIS2_PLACEMENT_3D('',#103846,#68006,#68007) ;
#54334 = AXIS2_PLACEMENT_3D('',#103848,#68008,#68009) ;
#54335 = AXIS2_PLACEMENT_3D('',#103850,#68010,#68011) ;
#54336 = AXIS2_PLACEMENT_3D('',#103852,#68012,#68013) ;
#54337 = AXIS2_PLACEMENT_3D('',#103854,#68014,#68015) ;
#54338 = AXIS2_PLACEMENT_3D('',#103856,#68016,#68017) ;
#54339 = AXIS2_PLACEMENT_3D('',#103858,#68018,#68019) ;
#54340 = AXIS2_PLACEMENT_3D('',#103860,#68020,#68021) ;
#54341 = AXIS2_PLACEMENT_3D('',#103862,#68022,#68023) ;
#54342 = AXIS2_PLACEMENT_3D('',#103864,#68024,#68025) ;
#54343 = AXIS2_PLACEMENT_3D('',#103866,#68026,#68027) ;
#54344 = AXIS2_PLACEMENT_3D('',#103868,#68028,#68029) ;
#54345 = AXIS2_PLACEMENT_3D('',#103870,#68030,#68031) ;
#54346 = AXIS2_PLACEMENT_3D('',#103872,#68032,#68033) ;
#54347 = AXIS2_PLACEMENT_3D('',#103874,#68034,#68035) ;
#54348 = AXIS2_PLACEMENT_3D('',#103876,#68036,#68037) ;
#54349 = AXIS2_PLACEMENT_3D('',#103878,#68038,#68039) ;
#54350 = AXIS2_PLACEMENT_3D('',#103880,#68040,#68041) ;
#54351 = AXIS2_PLACEMENT_3D('',#103882,#68042,#68043) ;
#54352 = AXIS2_PLACEMENT_3D('',#103884,#68044,#68045) ;
#54353 = AXIS2_PLACEMENT_3D('',#103886,#68046,#68047) ;
#54354 = AXIS2_PLACEMENT_3D('',#103888,#68048,#68049) ;
#54355 = AXIS2_PLACEMENT_3D('',#103890,#68050,#68051) ;
#54356 = AXIS2_PLACEMENT_3D('',#103892,#68052,#68053) ;
#54357 = AXIS2_PLACEMENT_3D('',#103894,#68054,#68055) ;
#54358 = AXIS2_PLACEMENT_3D('',#103896,#68056,#68057) ;
#54359 = AXIS2_PLACEMENT_3D('',#103898,#68058,#68059) ;
#54360 = AXIS2_PLACEMENT_3D('',#103900,#68060,#68061) ;
#54361 = AXIS2_PLACEMENT_3D('',#103902,#68062,#68063) ;
#54362 = AXIS2_PLACEMENT_3D('',#103903,#68064,#68065) ;
#54363 = AXIS2_PLACEMENT_3D('',#103904,#68066,#68067) ;
#54364 = AXIS2_PLACEMENT_3D('',#103908,#68069,#68070) ;
#54365 = AXIS2_PLACEMENT_3D('',#103910,#68072,#68073) ;
#54366 = AXIS2_PLACEMENT_3D('',#103914,#68075,#68076) ;
#54367 = AXIS2_PLACEMENT_3D('',#103916,#68078,#68079) ;
#54368 = AXIS2_PLACEMENT_3D('',#103920,#68081,#68082) ;
#54369 = AXIS2_PLACEMENT_3D('',#103922,#68084,#68085) ;
#54370 = AXIS2_PLACEMENT_3D('',#103926,#68087,#68088) ;
#54371 = AXIS2_PLACEMENT_3D('',#103928,#68090,#68091) ;
#54372 = AXIS2_PLACEMENT_3D('',#103932,#68093,#68094) ;
#54373 = AXIS2_PLACEMENT_3D('',#103934,#68096,#68097) ;
#54374 = AXIS2_PLACEMENT_3D('',#103938,#68099,#68100) ;
#54375 = AXIS2_PLACEMENT_3D('',#103940,#68102,#68103) ;
#54376 = AXIS2_PLACEMENT_3D('',#103944,#68105,#68106) ;
#54377 = AXIS2_PLACEMENT_3D('',#103946,#68108,#68109) ;
#54378 = AXIS2_PLACEMENT_3D('',#103950,#68111,#68112) ;
#54379 = AXIS2_PLACEMENT_3D('',#103952,#68114,#68115) ;
#54380 = AXIS2_PLACEMENT_3D('',#103956,#68117,#68118) ;
#54381 = AXIS2_PLACEMENT_3D('',#103958,#68120,#68121) ;
#54382 = AXIS2_PLACEMENT_3D('',#103962,#68123,#68124) ;
#54383 = AXIS2_PLACEMENT_3D('',#103964,#68126,#68127) ;
#54384 = AXIS2_PLACEMENT_3D('',#103968,#68129,#68130) ;
#54385 = AXIS2_PLACEMENT_3D('',#103970,#68132,#68133) ;
#54386 = AXIS2_PLACEMENT_3D('',#103974,#68135,#68136) ;
#54387 = AXIS2_PLACEMENT_3D('',#103976,#68138,#68139) ;
#54388 = AXIS2_PLACEMENT_3D('',#103980,#68141,#68142) ;
#54389 = AXIS2_PLACEMENT_3D('',#103982,#68144,#68145) ;
#54390 = AXIS2_PLACEMENT_3D('',#103986,#68147,#68148) ;
#54391 = AXIS2_PLACEMENT_3D('',#103988,#68150,#68151) ;
#54392 = AXIS2_PLACEMENT_3D('',#103992,#68153,#68154) ;
#54393 = AXIS2_PLACEMENT_3D('',#103994,#68156,#68157) ;
#54394 = AXIS2_PLACEMENT_3D('',#103998,#68159,#68160) ;
#54395 = AXIS2_PLACEMENT_3D('',#104000,#68162,#68163) ;
#54396 = AXIS2_PLACEMENT_3D('',#104004,#68165,#68166) ;
#54397 = AXIS2_PLACEMENT_3D('',#104006,#68168,#68169) ;
#54398 = AXIS2_PLACEMENT_3D('',#104010,#68171,#68172) ;
#54399 = AXIS2_PLACEMENT_3D('',#104012,#68174,#68175) ;
#54400 = AXIS2_PLACEMENT_3D('',#104016,#68177,#68178) ;
#54401 = AXIS2_PLACEMENT_3D('',#104018,#68180,#68181) ;
#54402 = AXIS2_PLACEMENT_3D('',#104022,#68183,#68184) ;
#54403 = AXIS2_PLACEMENT_3D('',#104024,#68186,#68187) ;
#54404 = AXIS2_PLACEMENT_3D('',#104041,#68188,#68189) ;
#54405 = AXIS2_PLACEMENT_3D('',#104056,#68190,#68191) ;
#54406 = AXIS2_PLACEMENT_3D('',#104075,#68193,#68194) ;
#54407 = AXIS2_PLACEMENT_3D('',#104094,#68196,#68197) ;
#54408 = AXIS2_PLACEMENT_3D('',#104127,#68199,#68200) ;
#54409 = AXIS2_PLACEMENT_3D('',#104142,#68201,#68202) ;
#54410 = AXIS2_PLACEMENT_3D('',#104159,#68203,#68204) ;
#54411 = AXIS2_PLACEMENT_3D('',#104193,#68206,#68207) ;
#54412 = AXIS2_PLACEMENT_3D('',#104224,#68208,#68209) ;
#54413 = AXIS2_PLACEMENT_3D('',#104239,#68210,#68211) ;
#54414 = AXIS2_PLACEMENT_3D('',#104256,#68212,#68213) ;
#54415 = AXIS2_PLACEMENT_3D('',#104290,#68215,#68216) ;
#54416 = AXIS2_PLACEMENT_3D('',#104321,#68217,#68218) ;
#54417 = AXIS2_PLACEMENT_3D('',#104336,#68219,#68220) ;
#54418 = AXIS2_PLACEMENT_3D('',#104353,#68221,#68222) ;
#54419 = AXIS2_PLACEMENT_3D('',#104387,#68224,#68225) ;
#54420 = AXIS2_PLACEMENT_3D('',#104418,#68226,#68227) ;
#54421 = AXIS2_PLACEMENT_3D('',#104433,#68228,#68229) ;
#54422 = AXIS2_PLACEMENT_3D('',#104450,#68230,#68231) ;
#54423 = AXIS2_PLACEMENT_3D('',#104484,#68233,#68234) ;
#54424 = AXIS2_PLACEMENT_3D('',#104515,#68235,#68236) ;
#54425 = AXIS2_PLACEMENT_3D('',#104530,#68237,#68238) ;
#54426 = AXIS2_PLACEMENT_3D('',#104547,#68239,#68240) ;
#54427 = AXIS2_PLACEMENT_3D('',#104581,#68242,#68243) ;
#54428 = AXIS2_PLACEMENT_3D('',#104612,#68244,#68245) ;
#54429 = AXIS2_PLACEMENT_3D('',#104627,#68246,#68247) ;
#54430 = AXIS2_PLACEMENT_3D('',#104644,#68248,#68249) ;
#54431 = AXIS2_PLACEMENT_3D('',#104678,#68251,#68252) ;
#54432 = AXIS2_PLACEMENT_3D('',#104709,#68253,#68254) ;
#54433 = AXIS2_PLACEMENT_3D('',#104724,#68255,#68256) ;
#54434 = AXIS2_PLACEMENT_3D('',#104741,#68257,#68258) ;
#54435 = AXIS2_PLACEMENT_3D('',#104775,#68260,#68261) ;
#54436 = AXIS2_PLACEMENT_3D('',#104806,#68262,#68263) ;
#54437 = AXIS2_PLACEMENT_3D('',#104821,#68264,#68265) ;
#54438 = AXIS2_PLACEMENT_3D('',#104838,#68266,#68267) ;
#54439 = AXIS2_PLACEMENT_3D('',#104872,#68269,#68270) ;
#54440 = AXIS2_PLACEMENT_3D('',#104903,#68271,#68272) ;
#54441 = AXIS2_PLACEMENT_3D('',#104918,#68273,#68274) ;
#54442 = AXIS2_PLACEMENT_3D('',#104935,#68275,#68276) ;
#54443 = AXIS2_PLACEMENT_3D('',#104966,#68277,#68278) ;
#54444 = AXIS2_PLACEMENT_3D('',#104997,#68279,#68280) ;
#54445 = AXIS2_PLACEMENT_3D('',#105012,#68281,#68282) ;
#54446 = AXIS2_PLACEMENT_3D('',#105029,#68283,#68284) ;
#54447 = AXIS2_PLACEMENT_3D('',#105030,#68285,#68286) ;
#54448 = AXIS2_PLACEMENT_3D('',#105031,#68287,#68288) ;
#54449 = AXIS2_PLACEMENT_3D('',#105033,#68289,#68290) ;
#54450 = AXIS2_PLACEMENT_3D('',#105048,#68291,#68292) ;
#54451 = AXIS2_PLACEMENT_3D('',#105067,#68294,#68295) ;
#54452 = AXIS2_PLACEMENT_3D('',#105068,#68296,#68297) ;
#54453 = AXIS2_PLACEMENT_3D('',#105069,#68298,#68299) ;
#54454 = AXIS2_PLACEMENT_3D('',#105070,#68300,#68301) ;
#54455 = AXIS2_PLACEMENT_3D('',#105072,#68302,#68303) ;
#54456 = AXIS2_PLACEMENT_3D('',#105087,#68304,#68305) ;
#54457 = AXIS2_PLACEMENT_3D('',#105106,#68307,#68308) ;
#54458 = AXIS2_PLACEMENT_3D('',#105107,#68309,#68310) ;
#54459 = AXIS2_PLACEMENT_3D('',#105108,#68311,#68312) ;
#54460 = AXIS2_PLACEMENT_3D('',#105109,#68313,#68314) ;
#54461 = AXIS2_PLACEMENT_3D('',#105111,#68315,#68316) ;
#54462 = AXIS2_PLACEMENT_3D('',#105126,#68317,#68318) ;
#54463 = AXIS2_PLACEMENT_3D('',#105145,#68320,#68321) ;
#54464 = AXIS2_PLACEMENT_3D('',#105146,#68322,#68323) ;
#54465 = AXIS2_PLACEMENT_3D('',#105147,#68324,#68325) ;
#54466 = AXIS2_PLACEMENT_3D('',#105148,#68326,#68327) ;
#54467 = AXIS2_PLACEMENT_3D('',#105150,#68328,#68329) ;
#54468 = AXIS2_PLACEMENT_3D('',#105165,#68330,#68331) ;
#54469 = AXIS2_PLACEMENT_3D('',#105184,#68333,#68334) ;
#54470 = AXIS2_PLACEMENT_3D('',#105185,#68335,#68336) ;
#54471 = AXIS2_PLACEMENT_3D('',#105186,#68337,#68338) ;
#54472 = AXIS2_PLACEMENT_3D('',#105187,#68339,#68340) ;
#54473 = AXIS2_PLACEMENT_3D('',#105189,#68341,#68342) ;
#54474 = AXIS2_PLACEMENT_3D('',#105204,#68343,#68344) ;
#54475 = AXIS2_PLACEMENT_3D('',#105223,#68346,#68347) ;
#54476 = AXIS2_PLACEMENT_3D('',#105224,#68348,#68349) ;
#54477 = AXIS2_PLACEMENT_3D('',#105225,#68350,#68351) ;
#54478 = AXIS2_PLACEMENT_3D('',#105226,#68352,#68353) ;
#54479 = AXIS2_PLACEMENT_3D('',#105228,#68354,#68355) ;
#54480 = AXIS2_PLACEMENT_3D('',#105243,#68356,#68357) ;
#54481 = AXIS2_PLACEMENT_3D('',#105262,#68359,#68360) ;
#54482 = AXIS2_PLACEMENT_3D('',#105263,#68361,#68362) ;
#54483 = AXIS2_PLACEMENT_3D('',#105264,#68363,#68364) ;
#54484 = AXIS2_PLACEMENT_3D('',#105265,#68365,#68366) ;
#54485 = AXIS2_PLACEMENT_3D('',#105267,#68367,#68368) ;
#54486 = AXIS2_PLACEMENT_3D('',#105282,#68369,#68370) ;
#54487 = AXIS2_PLACEMENT_3D('',#105301,#68372,#68373) ;
#54488 = AXIS2_PLACEMENT_3D('',#105302,#68374,#68375) ;
#54489 = AXIS2_PLACEMENT_3D('',#105303,#68376,#68377) ;
#54490 = AXIS2_PLACEMENT_3D('',#105304,#68378,#68379) ;
#54491 = AXIS2_PLACEMENT_3D('',#105306,#68380,#68381) ;
#54492 = AXIS2_PLACEMENT_3D('',#105321,#68382,#68383) ;
#54493 = AXIS2_PLACEMENT_3D('',#105340,#68385,#68386) ;
#54494 = AXIS2_PLACEMENT_3D('',#105341,#68387,#68388) ;
#54495 = AXIS2_PLACEMENT_3D('',#105342,#68389,#68390) ;
#54496 = AXIS2_PLACEMENT_3D('',#105343,#68391,#68392) ;
#54497 = AXIS2_PLACEMENT_3D('',#105345,#68393,#68394) ;
#54498 = AXIS2_PLACEMENT_3D('',#105360,#68395,#68396) ;
#54499 = AXIS2_PLACEMENT_3D('',#105379,#68398,#68399) ;
#54500 = AXIS2_PLACEMENT_3D('',#105380,#68400,#68401) ;
#54501 = AXIS2_PLACEMENT_3D('',#105381,#68402,#68403) ;
#54502 = AXIS2_PLACEMENT_3D('',#105382,#68404,#68405) ;
#54503 = AXIS2_PLACEMENT_3D('',#105383,#68406,#68407) ;
#54504 = AXIS2_PLACEMENT_3D('',#105386,#68410,#68411) ;
#54505 = AXIS2_PLACEMENT_3D('',#105388,#68413,#68414) ;
#54506 = AXIS2_PLACEMENT_3D('',#105390,#68416,#68417) ;
#54507 = AXIS2_PLACEMENT_3D('',#105391,#68418,#68419) ;
#54508 = AXIS2_PLACEMENT_3D('',#105394,#68422,#68423) ;
#54509 = AXIS2_PLACEMENT_3D('',#105397,#68426,#68427) ;
#54510 = AXIS2_PLACEMENT_3D('',#105398,#68428,#68429) ;
#54511 = AXIS2_PLACEMENT_3D('',#105401,#68432,#68433) ;
#54512 = AXIS2_PLACEMENT_3D('',#105404,#68436,#68437) ;
#54513 = AXIS2_PLACEMENT_3D('',#105405,#68438,#68439) ;
#54514 = AXIS2_PLACEMENT_3D('',#105408,#68442,#68443) ;
#54515 = AXIS2_PLACEMENT_3D('',#105411,#68446,#68447) ;
#54516 = AXIS2_PLACEMENT_3D('',#105412,#68448,#68449) ;
#54517 = AXIS2_PLACEMENT_3D('',#105415,#68452,#68453) ;
#54518 = AXIS2_PLACEMENT_3D('',#105418,#68456,#68457) ;
#54519 = AXIS2_PLACEMENT_3D('',#105419,#68458,#68459) ;
#54520 = AXIS2_PLACEMENT_3D('',#105422,#68462,#68463) ;
#54521 = AXIS2_PLACEMENT_3D('',#105425,#68466,#68467) ;
#54522 = AXIS2_PLACEMENT_3D('',#105426,#68468,#68469) ;
#54523 = AXIS2_PLACEMENT_3D('',#105429,#68472,#68473) ;
#54524 = AXIS2_PLACEMENT_3D('',#105432,#68476,#68477) ;
#54525 = AXIS2_PLACEMENT_3D('',#105433,#68478,#68479) ;
#54526 = AXIS2_PLACEMENT_3D('',#105436,#68482,#68483) ;
#54527 = AXIS2_PLACEMENT_3D('',#105439,#68486,#68487) ;
#54528 = AXIS2_PLACEMENT_3D('',#105440,#68488,#68489) ;
#54529 = AXIS2_PLACEMENT_3D('',#105443,#68492,#68493) ;
#54530 = AXIS2_PLACEMENT_3D('',#105446,#68496,#68497) ;
#54531 = AXIS2_PLACEMENT_3D('',#105447,#68498,#68499) ;
#54532 = AXIS2_PLACEMENT_3D('',#105450,#68502,#68503) ;
#54533 = AXIS2_PLACEMENT_3D('',#105452,#68505,#68506) ;
#54534 = AXIS2_PLACEMENT_3D('',#105453,#68507,#68508) ;
#54535 = AXIS2_PLACEMENT_3D('',#105454,#68509,#68510) ;
#54536 = AXIS2_PLACEMENT_3D('',#105455,#68511,#68512) ;
#54537 = AXIS2_PLACEMENT_3D('',#105456,#68513,#68514) ;
#54538 = AXIS2_PLACEMENT_3D('',#105457,#68515,#68516) ;
#54539 = AXIS2_PLACEMENT_3D('',#105458,#68517,#68518) ;
#54540 = AXIS2_PLACEMENT_3D('',#105459,#68519,#68520) ;
#54541 = AXIS2_PLACEMENT_3D('',#105460,#68521,#68522) ;
#54542 = AXIS2_PLACEMENT_3D('',#105461,#68523,#68524) ;
#54543 = AXIS2_PLACEMENT_3D('',#105462,#68525,#68526) ;
#54544 = AXIS2_PLACEMENT_3D('',#105464,#68528,#68529) ;
#54545 = AXIS2_PLACEMENT_3D('',#105465,#68530,#68531) ;
#54546 = AXIS2_PLACEMENT_3D('',#105467,#68532,#68533) ;
#54547 = AXIS2_PLACEMENT_3D('',#105469,#68534,#68535) ;
#54548 = AXIS2_PLACEMENT_3D('',#105470,#68536,#68537) ;
#54549 = AXIS2_PLACEMENT_3D('',#105471,#68538,#68539) ;
#54550 = AXIS2_PLACEMENT_3D('',#105490,#68540,#68541) ;
#54551 = AXIS2_PLACEMENT_3D('',#105492,#68542,#68543) ;
#54552 = AXIS2_PLACEMENT_3D('',#105494,#68544,#68545) ;
#54553 = AXIS2_PLACEMENT_3D('',#105495,#68546,#68547) ;
#54554 = AXIS2_PLACEMENT_3D('',#105496,#68548,#68549) ;
#54555 = AXIS2_PLACEMENT_3D('',#105515,#68550,#68551) ;
#54556 = AXIS2_PLACEMENT_3D('',#105517,#68552,#68553) ;
#54557 = AXIS2_PLACEMENT_3D('',#105518,#68554,#68555) ;
#54558 = AXIS2_PLACEMENT_3D('',#105520,#68556,#68557) ;
#54559 = AXIS2_PLACEMENT_3D('',#105747,#68558,#68559) ;
#54560 = AXIS2_PLACEMENT_3D('',#105750,#68560,#68561) ;
#54561 = AXIS2_PLACEMENT_3D('',#105767,#68562,#68563) ;
#54562 = AXIS2_PLACEMENT_3D('',#105782,#68564,#68565) ;
#54563 = AXIS2_PLACEMENT_3D('',#105803,#68568,#68569) ;
#54564 = AXIS2_PLACEMENT_3D('',#105805,#68570,#68571) ;
#54565 = AXIS2_PLACEMENT_3D('',#105823,#68572,#68573) ;
#54566 = AXIS2_PLACEMENT_3D('',#105824,#68574,#68575) ;
#54567 = AXIS2_PLACEMENT_3D('',#105843,#68578,#68579) ;
#54568 = AXIS2_PLACEMENT_3D('',#105845,#68580,#68581) ;
#54569 = AXIS2_PLACEMENT_3D('',#105861,#68582,#68583) ;
#54570 = AXIS2_PLACEMENT_3D('',#105862,#68584,#68585) ;
#54571 = AXIS2_PLACEMENT_3D('',#105883,#68588,#68589) ;
#54572 = AXIS2_PLACEMENT_3D('',#105885,#68590,#68591) ;
#54573 = AXIS2_PLACEMENT_3D('',#105903,#68592,#68593) ;
#54574 = AXIS2_PLACEMENT_3D('',#105904,#68594,#68595) ;
#54575 = AXIS2_PLACEMENT_3D('',#105923,#68598,#68599) ;
#54576 = AXIS2_PLACEMENT_3D('',#105925,#68600,#68601) ;
#54577 = AXIS2_PLACEMENT_3D('',#105941,#68602,#68603) ;
#54578 = AXIS2_PLACEMENT_3D('',#105942,#68604,#68605) ;
#54579 = AXIS2_PLACEMENT_3D('',#105963,#68608,#68609) ;
#54580 = AXIS2_PLACEMENT_3D('',#105965,#68610,#68611) ;
#54581 = AXIS2_PLACEMENT_3D('',#105983,#68612,#68613) ;
#54582 = AXIS2_PLACEMENT_3D('',#105984,#68614,#68615) ;
#54583 = AXIS2_PLACEMENT_3D('',#106003,#68618,#68619) ;
#54584 = AXIS2_PLACEMENT_3D('',#106005,#68620,#68621) ;
#54585 = AXIS2_PLACEMENT_3D('',#106021,#68622,#68623) ;
#54586 = AXIS2_PLACEMENT_3D('',#106022,#68624,#68625) ;
#54587 = AXIS2_PLACEMENT_3D('',#106043,#68628,#68629) ;
#54588 = AXIS2_PLACEMENT_3D('',#106045,#68630,#68631) ;
#54589 = AXIS2_PLACEMENT_3D('',#106063,#68632,#68633) ;
#54590 = AXIS2_PLACEMENT_3D('',#106064,#68634,#68635) ;
#54591 = AXIS2_PLACEMENT_3D('',#106083,#68638,#68639) ;
#54592 = AXIS2_PLACEMENT_3D('',#106085,#68640,#68641) ;
#54593 = AXIS2_PLACEMENT_3D('',#106101,#68642,#68643) ;
#54594 = AXIS2_PLACEMENT_3D('',#106102,#68644,#68645) ;
#54595 = AXIS2_PLACEMENT_3D('',#106123,#68648,#68649) ;
#54596 = AXIS2_PLACEMENT_3D('',#106125,#68650,#68651) ;
#54597 = AXIS2_PLACEMENT_3D('',#106143,#68652,#68653) ;
#54598 = AXIS2_PLACEMENT_3D('',#106144,#68654,#68655) ;
#54599 = AXIS2_PLACEMENT_3D('',#106163,#68658,#68659) ;
#54600 = AXIS2_PLACEMENT_3D('',#106165,#68660,#68661) ;
#54601 = AXIS2_PLACEMENT_3D('',#106181,#68662,#68663) ;
#54602 = AXIS2_PLACEMENT_3D('',#106182,#68664,#68665) ;
#54603 = AXIS2_PLACEMENT_3D('',#106203,#68668,#68669) ;
#54604 = AXIS2_PLACEMENT_3D('',#106205,#68670,#68671) ;
#54605 = AXIS2_PLACEMENT_3D('',#106223,#68672,#68673) ;
#54606 = AXIS2_PLACEMENT_3D('',#106224,#68674,#68675) ;
#54607 = AXIS2_PLACEMENT_3D('',#106243,#68678,#68679) ;
#54608 = AXIS2_PLACEMENT_3D('',#106245,#68680,#68681) ;
#54609 = AXIS2_PLACEMENT_3D('',#106261,#68682,#68683) ;
#54610 = AXIS2_PLACEMENT_3D('',#106262,#68684,#68685) ;
#54611 = AXIS2_PLACEMENT_3D('',#106283,#68688,#68689) ;
#54612 = AXIS2_PLACEMENT_3D('',#106285,#68690,#68691) ;
#54613 = AXIS2_PLACEMENT_3D('',#106303,#68692,#68693) ;
#54614 = AXIS2_PLACEMENT_3D('',#106304,#68694,#68695) ;
#54615 = AXIS2_PLACEMENT_3D('',#106323,#68698,#68699) ;
#54616 = AXIS2_PLACEMENT_3D('',#106325,#68700,#68701) ;
#54617 = AXIS2_PLACEMENT_3D('',#106341,#68702,#68703) ;
#54618 = AXIS2_PLACEMENT_3D('',#106342,#68704,#68705) ;
#54619 = AXIS2_PLACEMENT_3D('',#106363,#68708,#68709) ;
#54620 = AXIS2_PLACEMENT_3D('',#106365,#68710,#68711) ;
#54621 = AXIS2_PLACEMENT_3D('',#106383,#68712,#68713) ;
#54622 = AXIS2_PLACEMENT_3D('',#106384,#68714,#68715) ;
#54623 = AXIS2_PLACEMENT_3D('',#106403,#68718,#68719) ;
#54624 = AXIS2_PLACEMENT_3D('',#106405,#68720,#68721) ;
#54625 = AXIS2_PLACEMENT_3D('',#106421,#68722,#68723) ;
#54626 = AXIS2_PLACEMENT_3D('',#106422,#68724,#68725) ;
#54627 = AXIS2_PLACEMENT_3D('',#106443,#68728,#68729) ;
#54628 = AXIS2_PLACEMENT_3D('',#106445,#68730,#68731) ;
#54629 = AXIS2_PLACEMENT_3D('',#106463,#68732,#68733) ;
#54630 = AXIS2_PLACEMENT_3D('',#106464,#68734,#68735) ;
#54631 = AXIS2_PLACEMENT_3D('',#106483,#68738,#68739) ;
#54632 = AXIS2_PLACEMENT_3D('',#106485,#68740,#68741) ;
#54633 = AXIS2_PLACEMENT_3D('',#106501,#68742,#68743) ;
#54634 = AXIS2_PLACEMENT_3D('',#106502,#68744,#68745) ;
#54635 = AXIS2_PLACEMENT_3D('',#106523,#68748,#68749) ;
#54636 = AXIS2_PLACEMENT_3D('',#106525,#68750,#68751) ;
#54637 = AXIS2_PLACEMENT_3D('',#106543,#68752,#68753) ;
#54638 = AXIS2_PLACEMENT_3D('',#106544,#68754,#68755) ;
#54639 = AXIS2_PLACEMENT_3D('',#106563,#68758,#68759) ;
#54640 = AXIS2_PLACEMENT_3D('',#106565,#68760,#68761) ;
#54641 = AXIS2_PLACEMENT_3D('',#106581,#68762,#68763) ;
#54642 = AXIS2_PLACEMENT_3D('',#106582,#68764,#68765) ;
#54643 = AXIS2_PLACEMENT_3D('',#106603,#68768,#68769) ;
#54644 = AXIS2_PLACEMENT_3D('',#106605,#68770,#68771) ;
#54645 = AXIS2_PLACEMENT_3D('',#106607,#68772,#68773) ;
#54646 = AXIS2_PLACEMENT_3D('',#106624,#68774,#68775) ;
#54647 = AXIS2_PLACEMENT_3D('',#106643,#68778,#68779) ;
#54648 = AXIS2_PLACEMENT_3D('',#106645,#68780,#68781) ;
#54649 = AXIS2_PLACEMENT_3D('',#106647,#68782,#68783) ;
#54650 = AXIS2_PLACEMENT_3D('',#106662,#68784,#68785) ;
#54651 = AXIS2_PLACEMENT_3D('',#106683,#68788,#68789) ;
#54652 = AXIS2_PLACEMENT_3D('',#106685,#68790,#68791) ;
#54653 = AXIS2_PLACEMENT_3D('',#106687,#68792,#68793) ;
#54654 = AXIS2_PLACEMENT_3D('',#106704,#68794,#68795) ;
#54655 = AXIS2_PLACEMENT_3D('',#106723,#68798,#68799) ;
#54656 = AXIS2_PLACEMENT_3D('',#106725,#68800,#68801) ;
#54657 = AXIS2_PLACEMENT_3D('',#106727,#68802,#68803) ;
#54658 = AXIS2_PLACEMENT_3D('',#106742,#68804,#68805) ;
#54659 = AXIS2_PLACEMENT_3D('',#106763,#68808,#68809) ;
#54660 = AXIS2_PLACEMENT_3D('',#106765,#68810,#68811) ;
#54661 = AXIS2_PLACEMENT_3D('',#106767,#68812,#68813) ;
#54662 = AXIS2_PLACEMENT_3D('',#106784,#68814,#68815) ;
#54663 = AXIS2_PLACEMENT_3D('',#106803,#68818,#68819) ;
#54664 = AXIS2_PLACEMENT_3D('',#106805,#68820,#68821) ;
#54665 = AXIS2_PLACEMENT_3D('',#106807,#68822,#68823) ;
#54666 = AXIS2_PLACEMENT_3D('',#106822,#68824,#68825) ;
#54667 = AXIS2_PLACEMENT_3D('',#106843,#68828,#68829) ;
#54668 = AXIS2_PLACEMENT_3D('',#106845,#68830,#68831) ;
#54669 = AXIS2_PLACEMENT_3D('',#106847,#68832,#68833) ;
#54670 = AXIS2_PLACEMENT_3D('',#106864,#68834,#68835) ;
#54671 = AXIS2_PLACEMENT_3D('',#106883,#68838,#68839) ;
#54672 = AXIS2_PLACEMENT_3D('',#106885,#68840,#68841) ;
#54673 = AXIS2_PLACEMENT_3D('',#106887,#68842,#68843) ;
#54674 = AXIS2_PLACEMENT_3D('',#106902,#68844,#68845) ;
#54675 = AXIS2_PLACEMENT_3D('',#106923,#68848,#68849) ;
#54676 = AXIS2_PLACEMENT_3D('',#106925,#68850,#68851) ;
#54677 = AXIS2_PLACEMENT_3D('',#106927,#68852,#68853) ;
#54678 = AXIS2_PLACEMENT_3D('',#106944,#68854,#68855) ;
#54679 = AXIS2_PLACEMENT_3D('',#106963,#68858,#68859) ;
#54680 = AXIS2_PLACEMENT_3D('',#106965,#68860,#68861) ;
#54681 = AXIS2_PLACEMENT_3D('',#106967,#68862,#68863) ;
#54682 = AXIS2_PLACEMENT_3D('',#106982,#68864,#68865) ;
#54683 = AXIS2_PLACEMENT_3D('',#107003,#68868,#68869) ;
#54684 = AXIS2_PLACEMENT_3D('',#107005,#68870,#68871) ;
#54685 = AXIS2_PLACEMENT_3D('',#107007,#68872,#68873) ;
#54686 = AXIS2_PLACEMENT_3D('',#107024,#68874,#68875) ;
#54687 = AXIS2_PLACEMENT_3D('',#107043,#68878,#68879) ;
#54688 = AXIS2_PLACEMENT_3D('',#107045,#68880,#68881) ;
#54689 = AXIS2_PLACEMENT_3D('',#107047,#68882,#68883) ;
#54690 = AXIS2_PLACEMENT_3D('',#107062,#68884,#68885) ;
#54691 = AXIS2_PLACEMENT_3D('',#107083,#68888,#68889) ;
#54692 = AXIS2_PLACEMENT_3D('',#107085,#68890,#68891) ;
#54693 = AXIS2_PLACEMENT_3D('',#107087,#68892,#68893) ;
#54694 = AXIS2_PLACEMENT_3D('',#107104,#68894,#68895) ;
#54695 = AXIS2_PLACEMENT_3D('',#107123,#68898,#68899) ;
#54696 = AXIS2_PLACEMENT_3D('',#107125,#68900,#68901) ;
#54697 = AXIS2_PLACEMENT_3D('',#107127,#68902,#68903) ;
#54698 = AXIS2_PLACEMENT_3D('',#107142,#68904,#68905) ;
#54699 = AXIS2_PLACEMENT_3D('',#107163,#68908,#68909) ;
#54700 = AXIS2_PLACEMENT_3D('',#107165,#68910,#68911) ;
#54701 = AXIS2_PLACEMENT_3D('',#107167,#68912,#68913) ;
#54702 = AXIS2_PLACEMENT_3D('',#107184,#68914,#68915) ;
#54703 = AXIS2_PLACEMENT_3D('',#107203,#68918,#68919) ;
#54704 = AXIS2_PLACEMENT_3D('',#107205,#68920,#68921) ;
#54705 = AXIS2_PLACEMENT_3D('',#107207,#68922,#68923) ;
#54706 = AXIS2_PLACEMENT_3D('',#107222,#68924,#68925) ;
#54707 = AXIS2_PLACEMENT_3D('',#107243,#68928,#68929) ;
#54708 = AXIS2_PLACEMENT_3D('',#107245,#68930,#68931) ;
#54709 = AXIS2_PLACEMENT_3D('',#107247,#68932,#68933) ;
#54710 = AXIS2_PLACEMENT_3D('',#107264,#68934,#68935) ;
#54711 = AXIS2_PLACEMENT_3D('',#107283,#68938,#68939) ;
#54712 = AXIS2_PLACEMENT_3D('',#107285,#68940,#68941) ;
#54713 = AXIS2_PLACEMENT_3D('',#107287,#68942,#68943) ;
#54714 = AXIS2_PLACEMENT_3D('',#107302,#68944,#68945) ;
#54715 = AXIS2_PLACEMENT_3D('',#107323,#68948,#68949) ;
#54716 = AXIS2_PLACEMENT_3D('',#107325,#68950,#68951) ;
#54717 = AXIS2_PLACEMENT_3D('',#107327,#68952,#68953) ;
#54718 = AXIS2_PLACEMENT_3D('',#107344,#68954,#68955) ;
#54719 = AXIS2_PLACEMENT_3D('',#107347,#68958,#68959) ;
#54720 = AXIS2_PLACEMENT_3D('',#107353,#68963,#68964) ;
#54721 = AXIS2_PLACEMENT_3D('',#107356,#68966,#68967) ;
#54722 = AXIS2_PLACEMENT_3D('',#107357,#68968,#68969) ;
#54723 = AXIS2_PLACEMENT_3D('',#107361,#68972,#68973) ;
#54724 = AXIS2_PLACEMENT_3D('',#107364,#68975,#68976) ;
#54725 = AXIS2_PLACEMENT_3D('',#107365,#68977,#68978) ;
#54726 = AXIS2_PLACEMENT_3D('',#107369,#68981,#68982) ;
#54727 = AXIS2_PLACEMENT_3D('',#107372,#68984,#68985) ;
#54728 = AXIS2_PLACEMENT_3D('',#107373,#68986,#68987) ;
#54729 = AXIS2_PLACEMENT_3D('',#107377,#68990,#68991) ;
#54730 = AXIS2_PLACEMENT_3D('',#107380,#68993,#68994) ;
#54731 = AXIS2_PLACEMENT_3D('',#107381,#68995,#68996) ;
#54732 = AXIS2_PLACEMENT_3D('',#107385,#68999,#69000) ;
#54733 = AXIS2_PLACEMENT_3D('',#107388,#69002,#69003) ;
#54734 = AXIS2_PLACEMENT_3D('',#107389,#69004,#69005) ;
#54735 = AXIS2_PLACEMENT_3D('',#107393,#69008,#69009) ;
#54736 = AXIS2_PLACEMENT_3D('',#107396,#69011,#69012) ;
#54737 = AXIS2_PLACEMENT_3D('',#107397,#69013,#69014) ;
#54738 = AXIS2_PLACEMENT_3D('',#107401,#69017,#69018) ;
#54739 = AXIS2_PLACEMENT_3D('',#107404,#69020,#69021) ;
#54740 = AXIS2_PLACEMENT_3D('',#107405,#69022,#69023) ;
#54741 = AXIS2_PLACEMENT_3D('',#107409,#69026,#69027) ;
#54742 = AXIS2_PLACEMENT_3D('',#107412,#69029,#69030) ;
#54743 = AXIS2_PLACEMENT_3D('',#107413,#69031,#69032) ;
#54744 = AXIS2_PLACEMENT_3D('',#107417,#69035,#69036) ;
#54745 = AXIS2_PLACEMENT_3D('',#107420,#69038,#69039) ;
#54746 = AXIS2_PLACEMENT_3D('',#107421,#69040,#69041) ;
#54747 = AXIS2_PLACEMENT_3D('',#107425,#69044,#69045) ;
#54748 = AXIS2_PLACEMENT_3D('',#107428,#69047,#69048) ;
#54749 = AXIS2_PLACEMENT_3D('',#107429,#69049,#69050) ;
#54750 = AXIS2_PLACEMENT_3D('',#107433,#69053,#69054) ;
#54751 = AXIS2_PLACEMENT_3D('',#107436,#69056,#69057) ;
#54752 = AXIS2_PLACEMENT_3D('',#107437,#69058,#69059) ;
#54753 = AXIS2_PLACEMENT_3D('',#107441,#69062,#69063) ;
#54754 = AXIS2_PLACEMENT_3D('',#107444,#69065,#69066) ;
#54755 = AXIS2_PLACEMENT_3D('',#107445,#69067,#69068) ;
#54756 = AXIS2_PLACEMENT_3D('',#107449,#69071,#69072) ;
#54757 = AXIS2_PLACEMENT_3D('',#107452,#69074,#69075) ;
#54758 = AXIS2_PLACEMENT_3D('',#107453,#69076,#69077) ;
#54759 = AXIS2_PLACEMENT_3D('',#107457,#69080,#69081) ;
#54760 = AXIS2_PLACEMENT_3D('',#107460,#69083,#69084) ;
#54761 = AXIS2_PLACEMENT_3D('',#107461,#69085,#69086) ;
#54762 = AXIS2_PLACEMENT_3D('',#107465,#69089,#69090) ;
#54763 = AXIS2_PLACEMENT_3D('',#107468,#69092,#69093) ;
#54764 = AXIS2_PLACEMENT_3D('',#107469,#69094,#69095) ;
#54765 = AXIS2_PLACEMENT_3D('',#107473,#69098,#69099) ;
#54766 = AXIS2_PLACEMENT_3D('',#107476,#69101,#69102) ;
#54767 = AXIS2_PLACEMENT_3D('',#107477,#69103,#69104) ;
#54768 = AXIS2_PLACEMENT_3D('',#107481,#69107,#69108) ;
#54769 = AXIS2_PLACEMENT_3D('',#107484,#69110,#69111) ;
#54770 = AXIS2_PLACEMENT_3D('',#107485,#69112,#69113) ;
#54771 = AXIS2_PLACEMENT_3D('',#107489,#69116,#69117) ;
#54772 = AXIS2_PLACEMENT_3D('',#107492,#69119,#69120) ;
#54773 = AXIS2_PLACEMENT_3D('',#107493,#69121,#69122) ;
#54774 = AXIS2_PLACEMENT_3D('',#107497,#69125,#69126) ;
#54775 = AXIS2_PLACEMENT_3D('',#107500,#69128,#69129) ;
#54776 = AXIS2_PLACEMENT_3D('',#107501,#69130,#69131) ;
#54777 = AXIS2_PLACEMENT_3D('',#107505,#69134,#69135) ;
#54778 = AXIS2_PLACEMENT_3D('',#107508,#69137,#69138) ;
#54779 = AXIS2_PLACEMENT_3D('',#107509,#69139,#69140) ;
#54780 = AXIS2_PLACEMENT_3D('',#107510,#69141,#69142) ;
#54781 = AXIS2_PLACEMENT_3D('',#107511,#69143,#69144) ;
#54782 = AXIS2_PLACEMENT_3D('',#107512,#69145,#69146) ;
#54783 = AXIS2_PLACEMENT_3D('',#107513,#69147,#69148) ;
#54784 = AXIS2_PLACEMENT_3D('',#107514,#69149,#69150) ;
#54785 = AXIS2_PLACEMENT_3D('',#107515,#69151,#69152) ;
#54786 = AXIS2_PLACEMENT_3D('',#107516,#69153,#69154) ;
#54787 = AXIS2_PLACEMENT_3D('',#107517,#69155,#69156) ;
#54788 = AXIS2_PLACEMENT_3D('',#107518,#69157,#69158) ;
#54789 = AXIS2_PLACEMENT_3D('',#107519,#69159,#69160) ;
#54790 = AXIS2_PLACEMENT_3D('',#107520,#69161,#69162) ;
#54791 = AXIS2_PLACEMENT_3D('',#107521,#69163,#69164) ;
#54792 = AXIS2_PLACEMENT_3D('',#107522,#69165,#69166) ;
#54793 = AXIS2_PLACEMENT_3D('',#107523,#69167,#69168) ;
#54794 = AXIS2_PLACEMENT_3D('',#107524,#69169,#69170) ;
#54795 = AXIS2_PLACEMENT_3D('',#107525,#69171,#69172) ;
#54796 = AXIS2_PLACEMENT_3D('',#107526,#69173,#69174) ;
#54797 = AXIS2_PLACEMENT_3D('',#107527,#69175,#69176) ;
#54798 = AXIS2_PLACEMENT_3D('',#107528,#69177,#69178) ;
#54799 = AXIS2_PLACEMENT_3D('',#107529,#69179,#69180) ;
#54800 = AXIS2_PLACEMENT_3D('',#107530,#69181,#69182) ;
#54801 = AXIS2_PLACEMENT_3D('',#107531,#69183,#69184) ;
#54802 = AXIS2_PLACEMENT_3D('',#107532,#69185,#69186) ;
#54803 = AXIS2_PLACEMENT_3D('',#107533,#69187,#69188) ;
#54804 = AXIS2_PLACEMENT_3D('',#107534,#69189,#69190) ;
#54805 = AXIS2_PLACEMENT_3D('',#107535,#69191,#69192) ;
#54806 = AXIS2_PLACEMENT_3D('',#107536,#69193,#69194) ;
#54807 = AXIS2_PLACEMENT_3D('',#107537,#69195,#69196) ;
#54808 = AXIS2_PLACEMENT_3D('',#107538,#69197,#69198) ;
#54809 = AXIS2_PLACEMENT_3D('',#107539,#69199,#69200) ;
#54810 = AXIS2_PLACEMENT_3D('',#107540,#69201,#69202) ;
#54811 = AXIS2_PLACEMENT_3D('',#107541,#69203,#69204) ;
#54812 = AXIS2_PLACEMENT_3D('',#107542,#69205,#69206) ;
#54813 = AXIS2_PLACEMENT_3D('',#107543,#69207,#69208) ;
#54814 = AXIS2_PLACEMENT_3D('',#107544,#69209,#69210) ;
#54815 = AXIS2_PLACEMENT_3D('',#107545,#69211,#69212) ;
#54816 = AXIS2_PLACEMENT_3D('',#107547,#69213,#69214) ;
#54817 = AXIS2_PLACEMENT_3D('',#107548,#69215,#69216) ;
#54818 = AXIS2_PLACEMENT_3D('',#107549,#69217,#69218) ;
#54819 = AXIS2_PLACEMENT_3D('',#107550,#69219,#69220) ;
#54820 = AXIS2_PLACEMENT_3D('',#107551,#69221,#69222) ;
#54821 = AXIS2_PLACEMENT_3D('',#107552,#69223,#69224) ;
#54822 = AXIS2_PLACEMENT_3D('',#107553,#69225,#69226) ;
#54823 = AXIS2_PLACEMENT_3D('',#107555,#69227,#69228) ;
#54824 = AXIS2_PLACEMENT_3D('',#107557,#69229,#69230) ;
#54825 = AXIS2_PLACEMENT_3D('',#107559,#69231,#69232) ;
#54826 = AXIS2_PLACEMENT_3D('',#107561,#69233,#69234) ;
#54827 = AXIS2_PLACEMENT_3D('',#107563,#69235,#69236) ;
#54828 = AXIS2_PLACEMENT_3D('',#107565,#69237,#69238) ;
#54829 = AXIS2_PLACEMENT_3D('',#107567,#69239,#69240) ;
#54830 = AXIS2_PLACEMENT_3D('',#107569,#69241,#69242) ;
#54831 = AXIS2_PLACEMENT_3D('',#107571,#69243,#69244) ;
#54832 = AXIS2_PLACEMENT_3D('',#107573,#69245,#69246) ;
#54833 = AXIS2_PLACEMENT_3D('',#107575,#69247,#69248) ;
#54834 = AXIS2_PLACEMENT_3D('',#107577,#69249,#69250) ;
#54835 = AXIS2_PLACEMENT_3D('',#107579,#69251,#69252) ;
#54836 = AXIS2_PLACEMENT_3D('',#107581,#69253,#69254) ;
#54837 = AXIS2_PLACEMENT_3D('',#107583,#69255,#69256) ;
#54838 = AXIS2_PLACEMENT_3D('',#107585,#69257,#69258) ;
#54839 = AXIS2_PLACEMENT_3D('',#107587,#69259,#69260) ;
#54840 = AXIS2_PLACEMENT_3D('',#107589,#69261,#69262) ;
#54841 = AXIS2_PLACEMENT_3D('',#107591,#69263,#69264) ;
#54842 = AXIS2_PLACEMENT_3D('',#107593,#69265,#69266) ;
#54843 = AXIS2_PLACEMENT_3D('',#107595,#69267,#69268) ;
#54844 = AXIS2_PLACEMENT_3D('',#107597,#69269,#69270) ;
#54845 = AXIS2_PLACEMENT_3D('',#107599,#69271,#69272) ;
#54846 = AXIS2_PLACEMENT_3D('',#107601,#69273,#69274) ;
#54847 = AXIS2_PLACEMENT_3D('',#107603,#69275,#69276) ;
#54848 = AXIS2_PLACEMENT_3D('',#107605,#69277,#69278) ;
#54849 = AXIS2_PLACEMENT_3D('',#107607,#69279,#69280) ;
#54850 = AXIS2_PLACEMENT_3D('',#107609,#69281,#69282) ;
#54851 = AXIS2_PLACEMENT_3D('',#107611,#69283,#69284) ;
#54852 = AXIS2_PLACEMENT_3D('',#107613,#69285,#69286) ;
#54853 = AXIS2_PLACEMENT_3D('',#107615,#69287,#69288) ;
#54854 = AXIS2_PLACEMENT_3D('',#107617,#69289,#69290) ;
#54855 = AXIS2_PLACEMENT_3D('',#107619,#69291,#69292) ;
#54856 = AXIS2_PLACEMENT_3D('',#107621,#69293,#69294) ;
#54857 = AXIS2_PLACEMENT_3D('',#107623,#69295,#69296) ;
#54858 = AXIS2_PLACEMENT_3D('',#107625,#69297,#69298) ;
#54859 = AXIS2_PLACEMENT_3D('',#107627,#69299,#69300) ;
#54860 = AXIS2_PLACEMENT_3D('',#107629,#69301,#69302) ;
#54861 = AXIS2_PLACEMENT_3D('',#107631,#69303,#69304) ;
#54862 = AXIS2_PLACEMENT_3D('',#107633,#69305,#69306) ;
#54863 = AXIS2_PLACEMENT_3D('',#107635,#69307,#69308) ;
#54864 = AXIS2_PLACEMENT_3D('',#107636,#69309,#69310) ;
#54865 = AXIS2_PLACEMENT_3D('',#107637,#69311,#69312) ;
#54866 = AXIS2_PLACEMENT_3D('',#107641,#69314,#69315) ;
#54867 = AXIS2_PLACEMENT_3D('',#107643,#69317,#69318) ;
#54868 = AXIS2_PLACEMENT_3D('',#107647,#69320,#69321) ;
#54869 = AXIS2_PLACEMENT_3D('',#107649,#69323,#69324) ;
#54870 = AXIS2_PLACEMENT_3D('',#107653,#69326,#69327) ;
#54871 = AXIS2_PLACEMENT_3D('',#107655,#69329,#69330) ;
#54872 = AXIS2_PLACEMENT_3D('',#107659,#69332,#69333) ;
#54873 = AXIS2_PLACEMENT_3D('',#107661,#69335,#69336) ;
#54874 = AXIS2_PLACEMENT_3D('',#107665,#69338,#69339) ;
#54875 = AXIS2_PLACEMENT_3D('',#107667,#69341,#69342) ;
#54876 = AXIS2_PLACEMENT_3D('',#107671,#69344,#69345) ;
#54877 = AXIS2_PLACEMENT_3D('',#107673,#69347,#69348) ;
#54878 = AXIS2_PLACEMENT_3D('',#107677,#69350,#69351) ;
#54879 = AXIS2_PLACEMENT_3D('',#107679,#69353,#69354) ;
#54880 = AXIS2_PLACEMENT_3D('',#107683,#69356,#69357) ;
#54881 = AXIS2_PLACEMENT_3D('',#107685,#69359,#69360) ;
#54882 = AXIS2_PLACEMENT_3D('',#107689,#69362,#69363) ;
#54883 = AXIS2_PLACEMENT_3D('',#107691,#69365,#69366) ;
#54884 = AXIS2_PLACEMENT_3D('',#107695,#69368,#69369) ;
#54885 = AXIS2_PLACEMENT_3D('',#107697,#69371,#69372) ;
#54886 = AXIS2_PLACEMENT_3D('',#107701,#69374,#69375) ;
#54887 = AXIS2_PLACEMENT_3D('',#107703,#69377,#69378) ;
#54888 = AXIS2_PLACEMENT_3D('',#107707,#69380,#69381) ;
#54889 = AXIS2_PLACEMENT_3D('',#107709,#69383,#69384) ;
#54890 = AXIS2_PLACEMENT_3D('',#107713,#69386,#69387) ;
#54891 = AXIS2_PLACEMENT_3D('',#107715,#69389,#69390) ;
#54892 = AXIS2_PLACEMENT_3D('',#107719,#69392,#69393) ;
#54893 = AXIS2_PLACEMENT_3D('',#107721,#69395,#69396) ;
#54894 = AXIS2_PLACEMENT_3D('',#107725,#69398,#69399) ;
#54895 = AXIS2_PLACEMENT_3D('',#107727,#69401,#69402) ;
#54896 = AXIS2_PLACEMENT_3D('',#107731,#69404,#69405) ;
#54897 = AXIS2_PLACEMENT_3D('',#107733,#69407,#69408) ;
#54898 = AXIS2_PLACEMENT_3D('',#107737,#69410,#69411) ;
#54899 = AXIS2_PLACEMENT_3D('',#107739,#69413,#69414) ;
#54900 = AXIS2_PLACEMENT_3D('',#107743,#69416,#69417) ;
#54901 = AXIS2_PLACEMENT_3D('',#107745,#69419,#69420) ;
#54902 = AXIS2_PLACEMENT_3D('',#107749,#69422,#69423) ;
#54903 = AXIS2_PLACEMENT_3D('',#107751,#69425,#69426) ;
#54904 = AXIS2_PLACEMENT_3D('',#107755,#69428,#69429) ;
#54905 = AXIS2_PLACEMENT_3D('',#107757,#69431,#69432) ;
#54906 = AXIS2_PLACEMENT_3D('',#107774,#69433,#69434) ;
#54907 = AXIS2_PLACEMENT_3D('',#107789,#69435,#69436) ;
#54908 = AXIS2_PLACEMENT_3D('',#107808,#69438,#69439) ;
#54909 = AXIS2_PLACEMENT_3D('',#107827,#69441,#69442) ;
#54910 = AXIS2_PLACEMENT_3D('',#107860,#69444,#69445) ;
#54911 = AXIS2_PLACEMENT_3D('',#107875,#69446,#69447) ;
#54912 = AXIS2_PLACEMENT_3D('',#107892,#69448,#69449) ;
#54913 = AXIS2_PLACEMENT_3D('',#107926,#69451,#69452) ;
#54914 = AXIS2_PLACEMENT_3D('',#107957,#69453,#69454) ;
#54915 = AXIS2_PLACEMENT_3D('',#107972,#69455,#69456) ;
#54916 = AXIS2_PLACEMENT_3D('',#107989,#69457,#69458) ;
#54917 = AXIS2_PLACEMENT_3D('',#108023,#69460,#69461) ;
#54918 = AXIS2_PLACEMENT_3D('',#108054,#69462,#69463) ;
#54919 = AXIS2_PLACEMENT_3D('',#108069,#69464,#69465) ;
#54920 = AXIS2_PLACEMENT_3D('',#108086,#69466,#69467) ;
#54921 = AXIS2_PLACEMENT_3D('',#108120,#69469,#69470) ;
#54922 = AXIS2_PLACEMENT_3D('',#108151,#69471,#69472) ;
#54923 = AXIS2_PLACEMENT_3D('',#108166,#69473,#69474) ;
#54924 = AXIS2_PLACEMENT_3D('',#108183,#69475,#69476) ;
#54925 = AXIS2_PLACEMENT_3D('',#108217,#69478,#69479) ;
#54926 = AXIS2_PLACEMENT_3D('',#108248,#69480,#69481) ;
#54927 = AXIS2_PLACEMENT_3D('',#108263,#69482,#69483) ;
#54928 = AXIS2_PLACEMENT_3D('',#108280,#69484,#69485) ;
#54929 = AXIS2_PLACEMENT_3D('',#108314,#69487,#69488) ;
#54930 = AXIS2_PLACEMENT_3D('',#108345,#69489,#69490) ;
#54931 = AXIS2_PLACEMENT_3D('',#108360,#69491,#69492) ;
#54932 = AXIS2_PLACEMENT_3D('',#108377,#69493,#69494) ;
#54933 = AXIS2_PLACEMENT_3D('',#108411,#69496,#69497) ;
#54934 = AXIS2_PLACEMENT_3D('',#108442,#69498,#69499) ;
#54935 = AXIS2_PLACEMENT_3D('',#108457,#69500,#69501) ;
#54936 = AXIS2_PLACEMENT_3D('',#108474,#69502,#69503) ;
#54937 = AXIS2_PLACEMENT_3D('',#108508,#69505,#69506) ;
#54938 = AXIS2_PLACEMENT_3D('',#108539,#69507,#69508) ;
#54939 = AXIS2_PLACEMENT_3D('',#108554,#69509,#69510) ;
#54940 = AXIS2_PLACEMENT_3D('',#108571,#69511,#69512) ;
#54941 = AXIS2_PLACEMENT_3D('',#108605,#69514,#69515) ;
#54942 = AXIS2_PLACEMENT_3D('',#108636,#69516,#69517) ;
#54943 = AXIS2_PLACEMENT_3D('',#108651,#69518,#69519) ;
#54944 = AXIS2_PLACEMENT_3D('',#108668,#69520,#69521) ;
#54945 = AXIS2_PLACEMENT_3D('',#108699,#69522,#69523) ;
#54946 = AXIS2_PLACEMENT_3D('',#108730,#69524,#69525) ;
#54947 = AXIS2_PLACEMENT_3D('',#108745,#69526,#69527) ;
#54948 = AXIS2_PLACEMENT_3D('',#108762,#69528,#69529) ;
#54949 = AXIS2_PLACEMENT_3D('',#108763,#69530,#69531) ;
#54950 = AXIS2_PLACEMENT_3D('',#108764,#69532,#69533) ;
#54951 = AXIS2_PLACEMENT_3D('',#108766,#69534,#69535) ;
#54952 = AXIS2_PLACEMENT_3D('',#108781,#69536,#69537) ;
#54953 = AXIS2_PLACEMENT_3D('',#108800,#69539,#69540) ;
#54954 = AXIS2_PLACEMENT_3D('',#108801,#69541,#69542) ;
#54955 = AXIS2_PLACEMENT_3D('',#108802,#69543,#69544) ;
#54956 = AXIS2_PLACEMENT_3D('',#108803,#69545,#69546) ;
#54957 = AXIS2_PLACEMENT_3D('',#108805,#69547,#69548) ;
#54958 = AXIS2_PLACEMENT_3D('',#108820,#69549,#69550) ;
#54959 = AXIS2_PLACEMENT_3D('',#108839,#69552,#69553) ;
#54960 = AXIS2_PLACEMENT_3D('',#108840,#69554,#69555) ;
#54961 = AXIS2_PLACEMENT_3D('',#108841,#69556,#69557) ;
#54962 = AXIS2_PLACEMENT_3D('',#108842,#69558,#69559) ;
#54963 = AXIS2_PLACEMENT_3D('',#108844,#69560,#69561) ;
#54964 = AXIS2_PLACEMENT_3D('',#108859,#69562,#69563) ;
#54965 = AXIS2_PLACEMENT_3D('',#108878,#69565,#69566) ;
#54966 = AXIS2_PLACEMENT_3D('',#108879,#69567,#69568) ;
#54967 = AXIS2_PLACEMENT_3D('',#108880,#69569,#69570) ;
#54968 = AXIS2_PLACEMENT_3D('',#108881,#69571,#69572) ;
#54969 = AXIS2_PLACEMENT_3D('',#108883,#69573,#69574) ;
#54970 = AXIS2_PLACEMENT_3D('',#108898,#69575,#69576) ;
#54971 = AXIS2_PLACEMENT_3D('',#108917,#69578,#69579) ;
#54972 = AXIS2_PLACEMENT_3D('',#108918,#69580,#69581) ;
#54973 = AXIS2_PLACEMENT_3D('',#108919,#69582,#69583) ;
#54974 = AXIS2_PLACEMENT_3D('',#108920,#69584,#69585) ;
#54975 = AXIS2_PLACEMENT_3D('',#108922,#69586,#69587) ;
#54976 = AXIS2_PLACEMENT_3D('',#108937,#69588,#69589) ;
#54977 = AXIS2_PLACEMENT_3D('',#108956,#69591,#69592) ;
#54978 = AXIS2_PLACEMENT_3D('',#108957,#69593,#69594) ;
#54979 = AXIS2_PLACEMENT_3D('',#108958,#69595,#69596) ;
#54980 = AXIS2_PLACEMENT_3D('',#108959,#69597,#69598) ;
#54981 = AXIS2_PLACEMENT_3D('',#108961,#69599,#69600) ;
#54982 = AXIS2_PLACEMENT_3D('',#108976,#69601,#69602) ;
#54983 = AXIS2_PLACEMENT_3D('',#108995,#69604,#69605) ;
#54984 = AXIS2_PLACEMENT_3D('',#108996,#69606,#69607) ;
#54985 = AXIS2_PLACEMENT_3D('',#108997,#69608,#69609) ;
#54986 = AXIS2_PLACEMENT_3D('',#108998,#69610,#69611) ;
#54987 = AXIS2_PLACEMENT_3D('',#109000,#69612,#69613) ;
#54988 = AXIS2_PLACEMENT_3D('',#109015,#69614,#69615) ;
#54989 = AXIS2_PLACEMENT_3D('',#109034,#69617,#69618) ;
#54990 = AXIS2_PLACEMENT_3D('',#109035,#69619,#69620) ;
#54991 = AXIS2_PLACEMENT_3D('',#109036,#69621,#69622) ;
#54992 = AXIS2_PLACEMENT_3D('',#109037,#69623,#69624) ;
#54993 = AXIS2_PLACEMENT_3D('',#109039,#69625,#69626) ;
#54994 = AXIS2_PLACEMENT_3D('',#109054,#69627,#69628) ;
#54995 = AXIS2_PLACEMENT_3D('',#109073,#69630,#69631) ;
#54996 = AXIS2_PLACEMENT_3D('',#109074,#69632,#69633) ;
#54997 = AXIS2_PLACEMENT_3D('',#109075,#69634,#69635) ;
#54998 = AXIS2_PLACEMENT_3D('',#109076,#69636,#69637) ;
#54999 = AXIS2_PLACEMENT_3D('',#109078,#69638,#69639) ;
#55000 = AXIS2_PLACEMENT_3D('',#109093,#69640,#69641) ;
#55001 = AXIS2_PLACEMENT_3D('',#109112,#69643,#69644) ;
#55002 = AXIS2_PLACEMENT_3D('',#109113,#69645,#69646) ;
#55003 = AXIS2_PLACEMENT_3D('',#109114,#69647,#69648) ;
#55004 = AXIS2_PLACEMENT_3D('',#109115,#69649,#69650) ;
#55005 = AXIS2_PLACEMENT_3D('',#109116,#69651,#69652) ;
#55006 = AXIS2_PLACEMENT_3D('',#109119,#69655,#69656) ;
#55007 = AXIS2_PLACEMENT_3D('',#109121,#69658,#69659) ;
#55008 = AXIS2_PLACEMENT_3D('',#109123,#69661,#69662) ;
#55009 = AXIS2_PLACEMENT_3D('',#109124,#69663,#69664) ;
#55010 = AXIS2_PLACEMENT_3D('',#109127,#69667,#69668) ;
#55011 = AXIS2_PLACEMENT_3D('',#109130,#69671,#69672) ;
#55012 = AXIS2_PLACEMENT_3D('',#109131,#69673,#69674) ;
#55013 = AXIS2_PLACEMENT_3D('',#109134,#69677,#69678) ;
#55014 = AXIS2_PLACEMENT_3D('',#109137,#69681,#69682) ;
#55015 = AXIS2_PLACEMENT_3D('',#109138,#69683,#69684) ;
#55016 = AXIS2_PLACEMENT_3D('',#109141,#69687,#69688) ;
#55017 = AXIS2_PLACEMENT_3D('',#109144,#69691,#69692) ;
#55018 = AXIS2_PLACEMENT_3D('',#109145,#69693,#69694) ;
#55019 = AXIS2_PLACEMENT_3D('',#109148,#69697,#69698) ;
#55020 = AXIS2_PLACEMENT_3D('',#109151,#69701,#69702) ;
#55021 = AXIS2_PLACEMENT_3D('',#109152,#69703,#69704) ;
#55022 = AXIS2_PLACEMENT_3D('',#109155,#69707,#69708) ;
#55023 = AXIS2_PLACEMENT_3D('',#109158,#69711,#69712) ;
#55024 = AXIS2_PLACEMENT_3D('',#109159,#69713,#69714) ;
#55025 = AXIS2_PLACEMENT_3D('',#109162,#69717,#69718) ;
#55026 = AXIS2_PLACEMENT_3D('',#109165,#69721,#69722) ;
#55027 = AXIS2_PLACEMENT_3D('',#109166,#69723,#69724) ;
#55028 = AXIS2_PLACEMENT_3D('',#109169,#69727,#69728) ;
#55029 = AXIS2_PLACEMENT_3D('',#109172,#69731,#69732) ;
#55030 = AXIS2_PLACEMENT_3D('',#109173,#69733,#69734) ;
#55031 = AXIS2_PLACEMENT_3D('',#109176,#69737,#69738) ;
#55032 = AXIS2_PLACEMENT_3D('',#109179,#69741,#69742) ;
#55033 = AXIS2_PLACEMENT_3D('',#109180,#69743,#69744) ;
#55034 = AXIS2_PLACEMENT_3D('',#109183,#69747,#69748) ;
#55035 = AXIS2_PLACEMENT_3D('',#109185,#69750,#69751) ;
#55036 = AXIS2_PLACEMENT_3D('',#109186,#69752,#69753) ;
#55037 = AXIS2_PLACEMENT_3D('',#109187,#69754,#69755) ;
#55038 = AXIS2_PLACEMENT_3D('',#109188,#69756,#69757) ;
#55039 = AXIS2_PLACEMENT_3D('',#109189,#69758,#69759) ;
#55040 = AXIS2_PLACEMENT_3D('',#109190,#69760,#69761) ;
#55041 = AXIS2_PLACEMENT_3D('',#109191,#69762,#69763) ;
#55042 = AXIS2_PLACEMENT_3D('',#109192,#69764,#69765) ;
#55043 = AXIS2_PLACEMENT_3D('',#109193,#69766,#69767) ;
#55044 = AXIS2_PLACEMENT_3D('',#109194,#69768,#69769) ;
#55045 = AXIS2_PLACEMENT_3D('',#109195,#69770,#69771) ;
#55046 = AXIS2_PLACEMENT_3D('',#109197,#69773,#69774) ;
#55047 = AXIS2_PLACEMENT_3D('',#109198,#69775,#69776) ;
#55048 = AXIS2_PLACEMENT_3D('',#109284,#69778,#69779) ;
#55049 = AXIS2_PLACEMENT_3D('',#109333,#69780,#69781) ;
#55050 = AXIS2_PLACEMENT_3D('',#109621,#69783,#69784) ;
#55051 = AXIS2_PLACEMENT_3D('',#109744,#69786,#69787) ;
#55052 = AXIS2_PLACEMENT_3D('',#109980,#69789,#69790) ;
#55053 = AXIS2_PLACEMENT_3D('',#110080,#69792,#69793) ;
#55054 = AXIS2_PLACEMENT_3D('',#110141,#69794,#69795) ;
#55055 = AXIS2_PLACEMENT_3D('',#110476,#69797,#69798) ;
#55056 = AXIS2_PLACEMENT_3D('',#110810,#69800,#69801) ;
#55057 = AXIS2_PLACEMENT_3D('',#111141,#69803,#69804) ;
#55058 = AXIS2_PLACEMENT_3D('',#111469,#69806,#69807) ;
#55059 = AXIS2_PLACEMENT_3D('',#111809,#69809,#69810) ;
#55060 = AXIS2_PLACEMENT_3D('',#111811,#69811,#69812) ;
#55061 = AXIS2_PLACEMENT_3D('',#111814,#69813,#69814) ;
#55062 = AXIS2_PLACEMENT_3D('',#112477,#69815,#69816) ;
#55063 = AXIS2_PLACEMENT_3D('',#113233,#69817,#69818) ;
#55064 = AXIS2_PLACEMENT_3D('',#114269,#69819,#69820) ;
#55065 = AXIS2_PLACEMENT_3D('',#115394,#69821,#69822) ;
#55066 = AXIS2_PLACEMENT_3D('',#115395,#69823,#69824) ;
#55067 = AXIS2_PLACEMENT_3D('',#115506,#69825,#69826) ;
#55068 = AXIS2_PLACEMENT_3D('',#115597,#69827,#69828) ;
#55069 = AXIS2_PLACEMENT_3D('',#115696,#69829,#69830) ;
#55070 = AXIS2_PLACEMENT_3D('',#115787,#69831,#69832) ;
#55071 = AXIS2_PLACEMENT_3D('',#116183,#69833,#69834) ;
#55072 = AXIS2_PLACEMENT_3D('',#116393,#69835,#69836) ;
#55073 = AXIS2_PLACEMENT_3D('',#116841,#69837,#69838) ;
#55074 = AXIS2_PLACEMENT_3D('',#117102,#69839,#69840) ;
#55075 = AXIS2_PLACEMENT_3D('',#117103,#69841,#69842) ;
#55076 = AXIS2_PLACEMENT_3D('',#117104,#69843,#69844) ;
#55077 = AXIS2_PLACEMENT_3D('',#117105,#69845,#69846) ;
#55078 = AXIS2_PLACEMENT_3D('',#117106,#69847,#69848) ;
#55079 = AXIS2_PLACEMENT_3D('',#117107,#69849,#69850) ;
#55080 = AXIS2_PLACEMENT_3D('',#117108,#69851,#69852) ;
#55081 = AXIS2_PLACEMENT_3D('',#117109,#69853,#69854) ;
#55082 = AXIS2_PLACEMENT_3D('',#117110,#69855,#69856) ;
#55083 = AXIS2_PLACEMENT_3D('',#117111,#69857,#69858) ;
#55084 = AXIS2_PLACEMENT_3D('',#117112,#69859,#69860) ;
#55085 = AXIS2_PLACEMENT_3D('',#117113,#69861,#69862) ;
#55086 = AXIS2_PLACEMENT_3D('',#117114,#69863,#69864) ;
#55087 = AXIS2_PLACEMENT_3D('',#117115,#69865,#69866) ;
#55088 = AXIS2_PLACEMENT_3D('',#117116,#69867,#69868) ;
#55089 = AXIS2_PLACEMENT_3D('',#117117,#69869,#69870) ;
#55090 = AXIS2_PLACEMENT_3D('',#117118,#69871,#69872) ;
#55091 = AXIS2_PLACEMENT_3D('',#117119,#69873,#69874) ;
#55092 = AXIS2_PLACEMENT_3D('',#117120,#69875,#69876) ;
#55093 = AXIS2_PLACEMENT_3D('',#117121,#69877,#69878) ;
#55094 = AXIS2_PLACEMENT_3D('',#117122,#69879,#69880) ;
#55095 = AXIS2_PLACEMENT_3D('',#117123,#69881,#69882) ;
#55096 = AXIS2_PLACEMENT_3D('',#117124,#69883,#69884) ;
#55097 = DIRECTION('axis',(0.,0.,1.)) ;
#55098 = DIRECTION('refdir',(1.,0.,0.)) ;
#55099 = DIRECTION('axis',(0.,0.,1.)) ;
#55100 = DIRECTION('refdir',(1.,0.,0.)) ;
#55101 = DIRECTION('center_axis',(0.,0.,1.)) ;
#55102 = DIRECTION('ref_axis',(1.,0.,0.)) ;
#55103 = DIRECTION('center_axis',(0.,0.,-1.)) ;
#55104 = DIRECTION('ref_axis',(1.,0.,0.)) ;
#55105 = DIRECTION('center_axis',(0.,-1.,0.)) ;
#55106 = DIRECTION('ref_axis',(-1.,0.,0.)) ;
#55107 = DIRECTION('center_axis',(0.,0.,1.)) ;
#55108 = DIRECTION('ref_axis',(1.,0.,0.)) ;
#55109 = DIRECTION('center_axis',(0.,0.,1.)) ;
#55110 = DIRECTION('ref_axis',(1.,0.,0.)) ;
#55111 = DIRECTION('',(0.,0.,-1.)) ;
#55112 = DIRECTION('center_axis',(0.,0.,-1.)) ;
#55113 = DIRECTION('ref_axis',(-1.,-5.9211894646675E-15,0.)) ;
#55114 = DIRECTION('',(0.,0.,1.)) ;
#55115 = DIRECTION('center_axis',(0.,0.,-1.)) ;
#55116 = DIRECTION('ref_axis',(-0.987688340595137,-0.156434465040233,0.)) ;
#55117 = DIRECTION('',(0.,0.,-1.)) ;
#55118 = DIRECTION('center_axis',(0.,0.,-1.)) ;
#55119 = DIRECTION('ref_axis',(-0.951056516295152,-0.309016994374953,0.)) ;
#55120 = DIRECTION('',(0.,0.,1.)) ;
#55121 = DIRECTION('center_axis',(0.,0.,-1.)) ;
#55122 = DIRECTION('ref_axis',(-0.89100652418837,-0.453990499739543,0.)) ;
#55123 = DIRECTION('',(0.,0.,-1.)) ;
#55124 = DIRECTION('center_axis',(0.,0.,-1.)) ;
#55125 = DIRECTION('ref_axis',(-0.809016994374946,-0.587785252292475,0.)) ;
#55126 = DIRECTION('',(0.,0.,1.)) ;
#55127 = DIRECTION('center_axis',(0.,0.,-1.)) ;
#55128 = DIRECTION('ref_axis',(-0.707106781186549,-0.707106781186546,0.)) ;
#55129 = DIRECTION('',(0.,0.,-1.)) ;
#55130 = DIRECTION('center_axis',(0.,0.,-1.)) ;
#55131 = DIRECTION('ref_axis',(-0.587785252292474,-0.809016994374947,0.)) ;
#55132 = DIRECTION('',(0.,0.,1.)) ;
#55133 = DIRECTION('center_axis',(0.,0.,-1.)) ;
#55134 = DIRECTION('ref_axis',(-0.453990499739548,-0.891006524188367,0.)) ;
#55135 = DIRECTION('',(0.,0.,-1.)) ;
#55136 = DIRECTION('center_axis',(0.,0.,-1.)) ;
#55137 = DIRECTION('ref_axis',(-0.309016994374946,-0.951056516295154,0.)) ;
#55138 = DIRECTION('',(0.,0.,1.)) ;
#55139 = DIRECTION('center_axis',(0.,0.,-1.)) ;
#55140 = DIRECTION('ref_axis',(-0.156434465040232,-0.987688340595138,0.)) ;
#55141 = DIRECTION('',(0.,0.,-1.)) ;
#55142 = DIRECTION('center_axis',(0.,0.,-1.)) ;
#55143 = DIRECTION('ref_axis',(0.,-1.,0.)) ;
#55144 = DIRECTION('',(0.,0.,1.)) ;
#55145 = DIRECTION('center_axis',(0.,0.,-1.)) ;
#55146 = DIRECTION('ref_axis',(0.156434465040235,-0.987688340595137,0.)) ;
#55147 = DIRECTION('',(0.,0.,-1.)) ;
#55148 = DIRECTION('center_axis',(0.,0.,-1.)) ;
#55149 = DIRECTION('ref_axis',(0.309016994374953,-0.951056516295152,0.)) ;
#55150 = DIRECTION('',(0.,0.,1.)) ;
#55151 = DIRECTION('center_axis',(0.,0.,-1.)) ;
#55152 = DIRECTION('ref_axis',(0.453990499739551,-0.891006524188366,0.)) ;
#55153 = DIRECTION('',(0.,0.,-1.)) ;
#55154 = DIRECTION('center_axis',(0.,0.,-1.)) ;
#55155 = DIRECTION('ref_axis',(0.587785252292479,-0.809016994374943,0.)) ;
#55156 = DIRECTION('',(0.,0.,1.)) ;
#55157 = DIRECTION('center_axis',(0.,0.,-1.)) ;
#55158 = DIRECTION('ref_axis',(0.70710678118655,-0.707106781186545,0.)) ;
#55159 = DIRECTION('',(0.,0.,-1.)) ;
#55160 = DIRECTION('center_axis',(0.,0.,-1.)) ;
#55161 = DIRECTION('ref_axis',(0.809016994374954,-0.587785252292464,0.)) ;
#55162 = DIRECTION('',(0.,0.,1.)) ;
#55163 = DIRECTION('center_axis',(0.,0.,-1.)) ;
#55164 = DIRECTION('ref_axis',(0.891006524188373,-0.453990499739537,0.)) ;
#55165 = DIRECTION('',(0.,0.,-1.)) ;
#55166 = DIRECTION('center_axis',(0.,0.,-1.)) ;
#55167 = DIRECTION('ref_axis',(0.951056516295156,-0.309016994374941,0.)) ;
#55168 = DIRECTION('',(0.,0.,1.)) ;
#55169 = DIRECTION('center_axis',(0.,0.,-1.)) ;
#55170 = DIRECTION('ref_axis',(0.987688340595139,-0.156434465040226,0.)) ;
#55171 = DIRECTION('',(0.,0.,-1.)) ;
#55172 = DIRECTION('center_axis',(0.,0.,-1.)) ;
#55173 = DIRECTION('ref_axis',(1.,0.,0.)) ;
#55174 = DIRECTION('',(0.,0.,1.)) ;
#55175 = DIRECTION('center_axis',(0.,0.,-1.)) ;
#55176 = DIRECTION('ref_axis',(0.987688340595137,0.156434465040233,0.)) ;
#55177 = DIRECTION('',(0.,0.,-1.)) ;
#55178 = DIRECTION('center_axis',(0.,0.,-1.)) ;
#55179 = DIRECTION('ref_axis',(0.951056516295154,0.309016994374947,0.)) ;
#55180 = DIRECTION('',(0.,0.,1.)) ;
#55181 = DIRECTION('center_axis',(0.,0.,-1.)) ;
#55182 = DIRECTION('ref_axis',(0.891006524188367,0.453990499739548,0.)) ;
#55183 = DIRECTION('',(0.,0.,-1.)) ;
#55184 = DIRECTION('center_axis',(0.,0.,-1.)) ;
#55185 = DIRECTION('ref_axis',(0.809016994374945,0.587785252292477,0.)) ;
#55186 = DIRECTION('',(0.,0.,1.)) ;
#55187 = DIRECTION('center_axis',(0.,0.,-1.)) ;
#55188 = DIRECTION('ref_axis',(0.707106781186547,0.707106781186547,0.)) ;
#55189 = DIRECTION('',(0.,0.,-1.)) ;
#55190 = DIRECTION('center_axis',(0.,0.,-1.)) ;
#55191 = DIRECTION('ref_axis',(0.587785252292479,0.809016994374943,0.)) ;
#55192 = DIRECTION('',(0.,0.,1.)) ;
#55193 = DIRECTION('center_axis',(0.,0.,-1.)) ;
#55194 = DIRECTION('ref_axis',(0.453990499739548,0.891006524188367,0.)) ;
#55195 = DIRECTION('',(0.,0.,-1.)) ;
#55196 = DIRECTION('center_axis',(0.,0.,-1.)) ;
#55197 = DIRECTION('ref_axis',(0.30901699437495,0.951056516295153,0.)) ;
#55198 = DIRECTION('',(0.,0.,1.)) ;
#55199 = DIRECTION('center_axis',(0.,0.,-1.)) ;
#55200 = DIRECTION('ref_axis',(0.156434465040232,0.987688340595138,0.)) ;
#55201 = DIRECTION('',(0.,0.,-1.)) ;
#55202 = DIRECTION('center_axis',(0.,0.,-1.)) ;
#55203 = DIRECTION('ref_axis',(4.44089209850062E-15,1.,0.)) ;
#55204 = DIRECTION('',(0.,0.,1.)) ;
#55205 = DIRECTION('center_axis',(0.,0.,-1.)) ;
#55206 = DIRECTION('ref_axis',(-0.156434465040226,0.987688340595139,0.)) ;
#55207 = DIRECTION('',(0.,0.,-1.)) ;
#55208 = DIRECTION('center_axis',(0.,0.,-1.)) ;
#55209 = DIRECTION('ref_axis',(-0.309016994374939,0.951056516295156,0.)) ;
#55210 = DIRECTION('',(0.,0.,1.)) ;
#55211 = DIRECTION('center_axis',(0.,0.,-1.)) ;
#55212 = DIRECTION('ref_axis',(-0.453990499739542,0.89100652418837,0.)) ;
#55213 = DIRECTION('',(0.,0.,-1.)) ;
#55214 = DIRECTION('center_axis',(0.,0.,-1.)) ;
#55215 = DIRECTION('ref_axis',(-0.587785252292473,0.809016994374948,0.)) ;
#55216 = DIRECTION('',(0.,0.,1.)) ;
#55217 = DIRECTION('center_axis',(0.,0.,-1.)) ;
#55218 = DIRECTION('ref_axis',(-0.707106781186542,0.707106781186554,0.)) ;
#55219 = DIRECTION('',(0.,0.,-1.)) ;
#55220 = DIRECTION('center_axis',(0.,0.,-1.)) ;
#55221 = DIRECTION('ref_axis',(-0.809016994374941,0.587785252292481,0.)) ;
#55222 = DIRECTION('',(0.,0.,1.)) ;
#55223 = DIRECTION('center_axis',(0.,0.,-1.)) ;
#55224 = DIRECTION('ref_axis',(-0.891006524188364,0.453990499739554,0.)) ;
#55225 = DIRECTION('',(0.,0.,-1.)) ;
#55226 = DIRECTION('center_axis',(0.,0.,-1.)) ;
#55227 = DIRECTION('ref_axis',(-0.95105651629515,0.309016994374958,0.)) ;
#55228 = DIRECTION('',(0.,0.,1.)) ;
#55229 = DIRECTION('center_axis',(0.,0.,-1.)) ;
#55230 = DIRECTION('ref_axis',(-0.987688340595137,0.156434465040233,0.)) ;
#55231 = DIRECTION('',(0.,0.,-1.)) ;
#55232 = DIRECTION('center_axis',(0.,0.,-1.)) ;
#55233 = DIRECTION('ref_axis',(-1.,-5.9211894646675E-15,0.)) ;
#55234 = DIRECTION('center_axis',(0.,0.,-1.)) ;
#55235 = DIRECTION('ref_axis',(1.,0.,0.)) ;
#55236 = DIRECTION('center_axis',(0.,1.,0.)) ;
#55237 = DIRECTION('ref_axis',(0.70710678118654,0.,0.707106781186555)) ;
#55238 = DIRECTION('center_axis',(0.,-1.,0.)) ;
#55239 = DIRECTION('ref_axis',(1.,0.,0.)) ;
#55240 = DIRECTION('',(0.,1.,0.)) ;
#55241 = DIRECTION('center_axis',(0.,1.,0.)) ;
#55242 = DIRECTION('ref_axis',(0.,0.,1.)) ;
#55243 = DIRECTION('',(0.,-1.,0.)) ;
#55244 = DIRECTION('center_axis',(-1.26882631385732E-15,1.,0.)) ;
#55245 = DIRECTION('ref_axis',(0.70710678118654,8.97195690676432E-16,0.707106781186555)) ;
#55246 = DIRECTION('center_axis',(0.,-1.,0.)) ;
#55247 = DIRECTION('ref_axis',(1.,0.,0.)) ;
#55248 = DIRECTION('',(-1.26882631385732E-15,1.,0.)) ;
#55249 = DIRECTION('center_axis',(0.,1.,0.)) ;
#55250 = DIRECTION('ref_axis',(0.,0.,1.)) ;
#55251 = DIRECTION('',(1.26882631385732E-15,-1.,0.)) ;
#55252 = DIRECTION('center_axis',(0.,0.,-1.)) ;
#55253 = DIRECTION('ref_axis',(-1.,0.,0.)) ;
#55254 = DIRECTION('center_axis',(1.,0.,0.)) ;
#55255 = DIRECTION('ref_axis',(0.,0.,1.)) ;
#55256 = DIRECTION('center_axis',(0.,0.,1.)) ;
#55257 = DIRECTION('ref_axis',(-0.707106781186543,0.707106781186552,0.)) ;
#55258 = DIRECTION('center_axis',(0.,0.,-1.)) ;
#55259 = DIRECTION('ref_axis',(-0.707106781186543,0.707106781186552,0.)) ;
#55260 = DIRECTION('center_axis',(1.,0.,0.)) ;
#55261 = DIRECTION('ref_axis',(0.,-0.707106781186602,0.707106781186493)) ;
#55262 = DIRECTION('center_axis',(1.,0.,0.)) ;
#55263 = DIRECTION('ref_axis',(0.,0.,1.)) ;
#55264 = DIRECTION('',(-1.,0.,0.)) ;
#55265 = DIRECTION('',(1.,0.,0.)) ;
#55266 = DIRECTION('center_axis',(1.,2.96059473233375E-14,0.)) ;
#55267 = DIRECTION('ref_axis',(2.09345661157853E-14,-0.707106781186602,0.707106781186493)) ;
#55268 = DIRECTION('center_axis',(-1.,-4.44089209850072E-14,0.)) ;
#55269 = DIRECTION('ref_axis',(4.44089209850072E-14,-1.,0.)) ;
#55270 = DIRECTION('',(1.,2.96059473233375E-14,0.)) ;
#55271 = DIRECTION('center_axis',(1.,4.44089209850072E-14,0.)) ;
#55272 = DIRECTION('ref_axis',(0.,0.,1.)) ;
#55273 = DIRECTION('',(-1.,-2.96059473233375E-14,0.)) ;
#55274 = DIRECTION('center_axis',(1.,0.,0.)) ;
#55275 = DIRECTION('ref_axis',(0.,-0.707106781186602,0.707106781186493)) ;
#55276 = DIRECTION('center_axis',(-1.,0.,0.)) ;
#55277 = DIRECTION('ref_axis',(0.,-1.,0.)) ;
#55278 = DIRECTION('',(1.,0.,0.)) ;
#55279 = DIRECTION('center_axis',(1.,0.,0.)) ;
#55280 = DIRECTION('ref_axis',(0.,0.,1.)) ;
#55281 = DIRECTION('',(-1.,0.,0.)) ;
#55282 = DIRECTION('center_axis',(0.,0.,-1.)) ;
#55283 = DIRECTION('ref_axis',(-1.,0.,0.)) ;
#55284 = DIRECTION('center_axis',(0.,-1.,0.)) ;
#55285 = DIRECTION('ref_axis',(0.,0.,1.)) ;
#55286 = DIRECTION('center_axis',(0.,0.,1.)) ;
#55287 = DIRECTION('ref_axis',(0.707106781186548,0.707106781186548,0.)) ;
#55288 = DIRECTION('center_axis',(0.,0.,-1.)) ;
#55289 = DIRECTION('ref_axis',(0.707106781186547,0.707106781186547,0.)) ;
#55290 = DIRECTION('center_axis',(0.,-1.,0.)) ;
#55291 = DIRECTION('ref_axis',(-0.70710678118654,0.,0.707106781186555)) ;
#55292 = DIRECTION('center_axis',(0.,-1.,0.)) ;
#55293 = DIRECTION('ref_axis',(0.,0.,1.)) ;
#55294 = DIRECTION('',(0.,1.,0.)) ;
#55295 = DIRECTION('',(0.,-1.,0.)) ;
#55296 = DIRECTION('center_axis',(-7.40148683083432E-15,-1.,0.)) ;
#55297 = DIRECTION('ref_axis',(-0.70710678118654,5.23364152894582E-15,0.707106781186555)) ;
#55298 = DIRECTION('center_axis',(0.,1.,0.)) ;
#55299 = DIRECTION('ref_axis',(-1.,0.,0.)) ;
#55300 = DIRECTION('',(-7.40148683083432E-15,-1.,0.)) ;
#55301 = DIRECTION('center_axis',(0.,-1.,0.)) ;
#55302 = DIRECTION('ref_axis',(0.,0.,1.)) ;
#55303 = DIRECTION('',(7.40148683083432E-15,1.,0.)) ;
#55304 = DIRECTION('center_axis',(0.,-1.,0.)) ;
#55305 = DIRECTION('ref_axis',(-0.70710678118654,0.,0.707106781186555)) ;
#55306 = DIRECTION('center_axis',(0.,1.,0.)) ;
#55307 = DIRECTION('ref_axis',(-1.,0.,0.)) ;
#55308 = DIRECTION('',(0.,-1.,0.)) ;
#55309 = DIRECTION('center_axis',(0.,-1.,0.)) ;
#55310 = DIRECTION('ref_axis',(0.,0.,1.)) ;
#55311 = DIRECTION('',(0.,1.,0.)) ;
#55312 = DIRECTION('center_axis',(0.,0.,-1.)) ;
#55313 = DIRECTION('ref_axis',(-1.,0.,0.)) ;
#55314 = DIRECTION('center_axis',(-1.,0.,0.)) ;
#55315 = DIRECTION('ref_axis',(0.,0.,1.)) ;
#55316 = DIRECTION('center_axis',(0.,0.,1.)) ;
#55317 = DIRECTION('ref_axis',(0.707106781186548,-0.707106781186548,0.)) ;
#55318 = DIRECTION('center_axis',(0.,0.,-1.)) ;
#55319 = DIRECTION('ref_axis',(0.707106781186547,-0.707106781186547,0.)) ;
#55320 = DIRECTION('center_axis',(-1.,0.,0.)) ;
#55321 = DIRECTION('ref_axis',(0.,0.707106781186477,0.707106781186618)) ;
#55322 = DIRECTION('center_axis',(-1.,0.,0.)) ;
#55323 = DIRECTION('ref_axis',(0.,0.,1.)) ;
#55324 = DIRECTION('',(1.,0.,0.)) ;
#55325 = DIRECTION('',(-1.,0.,0.)) ;
#55326 = DIRECTION('center_axis',(-1.,0.,0.)) ;
#55327 = DIRECTION('ref_axis',(0.,0.707106781186477,0.707106781186618)) ;
#55328 = DIRECTION('center_axis',(1.,0.,0.)) ;
#55329 = DIRECTION('ref_axis',(0.,1.,0.)) ;
#55330 = DIRECTION('',(-1.,0.,0.)) ;
#55331 = DIRECTION('center_axis',(-1.,0.,0.)) ;
#55332 = DIRECTION('ref_axis',(0.,0.,1.)) ;
#55333 = DIRECTION('',(1.,0.,0.)) ;
#55334 = DIRECTION('center_axis',(0.,0.,-1.)) ;
#55335 = DIRECTION('ref_axis',(-1.,0.,0.)) ;
#55336 = DIRECTION('center_axis',(1.,0.,0.)) ;
#55337 = DIRECTION('ref_axis',(0.,1.,0.)) ;
#55338 = DIRECTION('center_axis',(0.,0.,-1.)) ;
#55339 = DIRECTION('ref_axis',(-0.707106781186547,-0.707106781186547,0.)) ;
#55340 = DIRECTION('center_axis',(0.,1.,0.)) ;
#55341 = DIRECTION('ref_axis',(0.,0.,1.)) ;
#55342 = DIRECTION('center_axis',(0.,0.,1.)) ;
#55343 = DIRECTION('ref_axis',(-0.707106781186548,-0.707106781186548,0.)) ;
#55344 = DIRECTION('center_axis',(-1.26882631385732E-15,1.,0.)) ;
#55345 = DIRECTION('ref_axis',(0.70710678118654,8.97195690676432E-16,0.707106781186555)) ;
#55346 = DIRECTION('center_axis',(0.,1.,0.)) ;
#55347 = DIRECTION('ref_axis',(0.,0.,1.)) ;
#55348 = DIRECTION('',(1.26882631385732E-15,-1.,0.)) ;
#55349 = DIRECTION('',(-1.26882631385732E-15,1.,0.)) ;
#55350 = DIRECTION('center_axis',(-1.,0.,0.)) ;
#55351 = DIRECTION('ref_axis',(0.,0.707106781186477,0.707106781186618)) ;
#55352 = DIRECTION('center_axis',(1.,0.,0.)) ;
#55353 = DIRECTION('ref_axis',(0.,1.,0.)) ;
#55354 = DIRECTION('',(-1.,0.,0.)) ;
#55355 = DIRECTION('',(1.,0.,0.)) ;
#55356 = DIRECTION('center_axis',(0.408248290463862,-0.816496580927723,0.40824829046387)) ;
#55357 = DIRECTION('ref_axis',(0.577350269189623,0.577350269189623,0.577350269189632)) ;
#55358 = DIRECTION('center_axis',(0.,0.,-1.)) ;
#55359 = DIRECTION('ref_axis',(0.707106781186636,0.707106781186459,0.)) ;
#55360 = DIRECTION('center_axis',(-0.40824829046386,-0.81649658092772,0.408248290463878)) ;
#55361 = DIRECTION('ref_axis',(-0.577350269189623,0.577350269189623,0.577350269189632)) ;
#55362 = DIRECTION('center_axis',(0.,0.,-1.)) ;
#55363 = DIRECTION('ref_axis',(-0.707106781186636,0.707106781186459,0.)) ;
#55364 = DIRECTION('center_axis',(-0.408248290463862,-0.816496580927723,0.40824829046387)) ;
#55365 = DIRECTION('ref_axis',(-0.577350269189623,0.577350269189623,0.577350269189632)) ;
#55366 = DIRECTION('center_axis',(0.,0.,-1.)) ;
#55367 = DIRECTION('ref_axis',(-0.707106781186636,0.707106781186459,0.)) ;
#55368 = DIRECTION('center_axis',(0.408248290463862,-0.816496580927723,-0.40824829046387)) ;
#55369 = DIRECTION('ref_axis',(-0.577350269189623,-0.577350269189623,0.577350269189632)) ;
#55370 = DIRECTION('center_axis',(0.,0.,-1.)) ;
#55371 = DIRECTION('ref_axis',(-0.707106781186481,-0.707106781186614,0.)) ;
#55372 = DIRECTION('center_axis',(0.40824829046386,-0.81649658092772,-0.408248290463878)) ;
#55373 = DIRECTION('ref_axis',(-0.577350269189623,-0.577350269189623,0.577350269189632)) ;
#55374 = DIRECTION('center_axis',(0.,0.,-1.)) ;
#55375 = DIRECTION('ref_axis',(-0.707106781186614,-0.707106781186481,0.)) ;
#55376 = DIRECTION('center_axis',(0.408248290463928,-0.408248290463857,-0.816496580927697)) ;
#55377 = DIRECTION('ref_axis',(0.577350269189706,-0.577350269189493,0.577350269189679)) ;
#55378 = DIRECTION('center_axis',(0.,0.,-1.)) ;
#55379 = DIRECTION('ref_axis',(0.707106781186636,-0.707106781186459,0.)) ;
#55380 = DIRECTION('center_axis',(0.40824829046386,-0.40824829046386,-0.816496580927729)) ;
#55381 = DIRECTION('ref_axis',(0.577350269189626,-0.577350269189626,0.577350269189626)) ;
#55382 = DIRECTION('center_axis',(0.,0.,-1.)) ;
#55383 = DIRECTION('ref_axis',(0.707106781186481,-0.707106781186614,0.)) ;
#55384 = DIRECTION('center_axis',(0.408248290463862,-0.816496580927723,0.40824829046387)) ;
#55385 = DIRECTION('ref_axis',(0.577350269189623,0.577350269189623,0.577350269189632)) ;
#55386 = DIRECTION('center_axis',(0.,0.,-1.)) ;
#55387 = DIRECTION('ref_axis',(0.707106781186636,0.707106781186459,0.)) ;
#55388 = DIRECTION('center_axis',(-1.,0.,0.)) ;
#55389 = DIRECTION('ref_axis',(0.,1.,0.)) ;
#55390 = DIRECTION('',(0.,0.,1.)) ;
#55391 = DIRECTION('',(0.,-1.,0.)) ;
#55392 = DIRECTION('',(0.,0.,-1.)) ;
#55393 = DIRECTION('center_axis',(0.,0.,-1.)) ;
#55394 = DIRECTION('ref_axis',(-0.707106781186579,-0.707106781186516,0.)) ;
#55395 = DIRECTION('',(0.,0.,-1.)) ;
#55396 = DIRECTION('center_axis',(0.,0.,1.)) ;
#55397 = DIRECTION('ref_axis',(4.44089209850072E-14,-1.,0.)) ;
#55398 = DIRECTION('center_axis',(2.96059473233375E-14,-1.,0.)) ;
#55399 = DIRECTION('ref_axis',(-1.,-2.96059473233375E-14,0.)) ;
#55400 = DIRECTION('',(0.,0.,1.)) ;
#55401 = DIRECTION('',(1.,2.96059473233375E-14,0.)) ;
#55402 = DIRECTION('center_axis',(0.,0.,-1.)) ;
#55403 = DIRECTION('ref_axis',(0.70710678118661,-0.707106781186485,0.)) ;
#55404 = DIRECTION('',(0.,0.,-1.)) ;
#55405 = DIRECTION('center_axis',(0.,0.,1.)) ;
#55406 = DIRECTION('ref_axis',(1.,0.,0.)) ;
#55407 = DIRECTION('center_axis',(1.,1.26882631385732E-15,0.)) ;
#55408 = DIRECTION('ref_axis',(1.26882631385732E-15,-1.,0.)) ;
#55409 = DIRECTION('',(0.,0.,1.)) ;
#55410 = DIRECTION('',(-1.26882631385732E-15,1.,0.)) ;
#55411 = DIRECTION('center_axis',(0.,0.,-1.)) ;
#55412 = DIRECTION('ref_axis',(-0.707106781186554,0.707106781186541,0.)) ;
#55413 = DIRECTION('',(0.,0.,-1.)) ;
#55414 = DIRECTION('center_axis',(0.,0.,-1.)) ;
#55415 = DIRECTION('ref_axis',(-0.707106781186539,0.707106781186556,0.)) ;
#55416 = DIRECTION('center_axis',(0.,-1.,0.)) ;
#55417 = DIRECTION('ref_axis',(-1.,0.,0.)) ;
#55418 = DIRECTION('',(0.,0.,1.)) ;
#55419 = DIRECTION('',(1.,0.,0.)) ;
#55420 = DIRECTION('center_axis',(0.,0.,-1.)) ;
#55421 = DIRECTION('ref_axis',(0.707106781186485,-0.70710678118661,0.)) ;
#55422 = DIRECTION('',(0.,0.,-1.)) ;
#55423 = DIRECTION('center_axis',(0.,0.,1.)) ;
#55424 = DIRECTION('ref_axis',(1.,0.,0.)) ;
#55425 = DIRECTION('center_axis',(1.,0.,0.)) ;
#55426 = DIRECTION('ref_axis',(0.,-1.,0.)) ;
#55427 = DIRECTION('',(0.,0.,1.)) ;
#55428 = DIRECTION('',(0.,1.,0.)) ;
#55429 = DIRECTION('center_axis',(0.,0.,-1.)) ;
#55430 = DIRECTION('ref_axis',(0.70710678118661,0.707106781186485,0.)) ;
#55431 = DIRECTION('',(0.,0.,-1.)) ;
#55432 = DIRECTION('center_axis',(0.,0.,1.)) ;
#55433 = DIRECTION('ref_axis',(0.,1.,0.)) ;
#55434 = DIRECTION('center_axis',(0.,1.,0.)) ;
#55435 = DIRECTION('ref_axis',(1.,0.,0.)) ;
#55436 = DIRECTION('',(0.,0.,1.)) ;
#55437 = DIRECTION('',(-1.,0.,0.)) ;
#55438 = DIRECTION('center_axis',(0.,0.,-1.)) ;
#55439 = DIRECTION('ref_axis',(-0.707106781186548,-0.707106781186548,0.)) ;
#55440 = DIRECTION('',(0.,0.,-1.)) ;
#55441 = DIRECTION('center_axis',(0.,0.,-1.)) ;
#55442 = DIRECTION('ref_axis',(-0.707106781186564,-0.707106781186531,0.)) ;
#55443 = DIRECTION('center_axis',(0.,0.,-1.)) ;
#55444 = DIRECTION('ref_axis',(1.,0.,0.)) ;
#55445 = DIRECTION('center_axis',(0.,0.,1.)) ;
#55446 = DIRECTION('ref_axis',(1.,0.,0.)) ;
#55447 = DIRECTION('center_axis',(-1.31682711760943E-11,1.79856020404298E-11,
-1.)) ;
#55448 = DIRECTION('ref_axis',(0.806857664468129,0.590745892316684,4.62568615494041E-26)) ;
#55449 = DIRECTION('center_axis',(-0.317035052983307,0.433015558388784,0.843792807135212)) ;
#55450 = DIRECTION('ref_axis',(-0.365456287528658,0.765207700889935,-0.529998940003196)) ;
#55451 = DIRECTION('center_axis',(0.902369376537521,0.4309634651421,-4.58229759167643E-13)) ;
#55452 = DIRECTION('ref_axis',(-0.4309634651421,0.902369376537521,2.6214339396372E-29)) ;
#55453 = DIRECTION('center_axis',(0.,0.,1.)) ;
#55454 = DIRECTION('ref_axis',(1.,0.,0.)) ;
#55455 = DIRECTION('center_axis',(2.16808315015822E-11,4.00706478615926E-12,
-1.)) ;
#55456 = DIRECTION('ref_axis',(-0.181742644394422,0.98334612990977,-7.78466561773078E-27)) ;
#55457 = DIRECTION('center_axis',(-0.983346129909754,-0.181742644394508,-2.43498486700547E-13)) ;
#55458 = DIRECTION('ref_axis',(-0.154117454211813,0.83387585041345,-0.5299989400032)) ;
#55459 = DIRECTION('center_axis',(0.00196658646623397,0.536665474150936,0.843792807146412)) ;
#55460 = DIRECTION('ref_axis',(-0.999993285952489,0.00366443037087552,-1.17624957867241E-19)) ;
#55461 = DIRECTION('center_axis',(0.,0.,1.)) ;
#55462 = DIRECTION('ref_axis',(-0.928035724969788,0.372491198795086,0.)) ;
#55463 = DIRECTION('center_axis',(1.9734015444057E-11,1.07018918516592E-11,
-1.)) ;
#55464 = DIRECTION('ref_axis',(-0.476718191734985,0.879056178903787,-9.54822769938885E-27)) ;
#55465 = DIRECTION('center_axis',(-0.879056178903635,-0.476718191735265,-3.46485113656339E-13)) ;
#55466 = DIRECTION('ref_axis',(-0.404256218079704,0.745438148835541,-0.52999894000322)) ;
#55467 = DIRECTION('center_axis',(-0.163968416933248,0.511006904900617,0.843792807146574)) ;
#55468 = DIRECTION('ref_axis',(-0.952182502115841,-0.305529839237374,-1.20183483998926E-16)) ;
#55469 = DIRECTION('center_axis',(0.,0.,-1.)) ;
#55470 = DIRECTION('ref_axis',(-1.,0.,0.)) ;
#55471 = DIRECTION('center_axis',(8.28544638211486E-16,4.22164579210903E-16,
1.)) ;
#55472 = DIRECTION('ref_axis',(-0.453990499739544,0.891006524188369,1.49459261390817E-31)) ;
#55473 = DIRECTION('center_axis',(0.,0.,1.)) ;
#55474 = DIRECTION('ref_axis',(1.,0.,0.)) ;
#55475 = DIRECTION('center_axis',(-6.99415838648067E-12,2.1260400847229E-11,
-1.)) ;
#55476 = DIRECTION('ref_axis',(0.949917759598147,0.312500000000059,8.11578044958985E-27)) ;
#55477 = DIRECTION('center_axis',(-0.167709086662903,0.509791487647221,0.843792807135216)) ;
#55478 = DIRECTION('ref_axis',(-0.111107399873594,0.840687973798145,-0.529998940003183)) ;
#55479 = DIRECTION('center_axis',(0.991379310344833,0.131023139254877,-1.92356772507714E-13)) ;
#55480 = DIRECTION('ref_axis',(-0.131023139254877,0.991379310344833,2.71194847215894E-32)) ;
#55481 = DIRECTION('center_axis',(0.,0.,1.)) ;
#55482 = DIRECTION('ref_axis',(1.,0.,0.)) ;
#55483 = DIRECTION('center_axis',(-2.9576381803503E-9,2.13233469821874E-9,
-1.)) ;
#55484 = DIRECTION('ref_axis',(0.584816719432152,0.811165460724639,-3.75440385536796E-24)) ;
#55485 = DIRECTION('center_axis',(-0.435327416839363,0.31385305198745,0.843792807451054)) ;
#55486 = DIRECTION('ref_axis',(-0.584031767477094,0.614823566702723,-0.529998940003208)) ;
#55487 = DIRECTION('center_axis',(0.725029240977556,0.688718084362179,-4.33368493355678E-11)) ;
#55488 = DIRECTION('ref_axis',(-0.688718084362179,0.725029240977556,4.25223242774214E-27)) ;
#55489 = DIRECTION('center_axis',(0.,0.,1.)) ;
#55490 = DIRECTION('ref_axis',(1.,0.,0.)) ;
#55491 = DIRECTION('center_axis',(2.1947551897582E-11,-2.90064268900393E-12,
-1.)) ;
#55492 = DIRECTION('ref_axis',(0.13102313925492,0.991379310344828,-1.27623067668808E-26)) ;
#55493 = DIRECTION('center_axis',(-0.991379310344839,0.131023139254833,-1.40543823316144E-13)) ;
#55494 = DIRECTION('ref_axis',(0.111107399873597,0.840687973798168,-0.529998940003147)) ;
#55495 = DIRECTION('center_axis',(0.16770908668058,0.509791487623121,0.843792807146263)) ;
#55496 = DIRECTION('ref_axis',(-0.949917759597208,0.312500000002913,1.29384740635467E-16)) ;
#55497 = DIRECTION('center_axis',(0.,0.,1.)) ;
#55498 = DIRECTION('ref_axis',(-0.997720534269979,0.0674813714741176,0.)) ;
#55499 = DIRECTION('center_axis',(1.55778144178567E-11,1.63991206560649E-11,
-1.)) ;
#55500 = DIRECTION('ref_axis',(-0.725029240977598,0.688718084362135,9.07425119548907E-27)) ;
#55501 = DIRECTION('center_axis',(-0.688718084362041,-0.725029240977687,-3.15160813713268E-13)) ;
#55502 = DIRECTION('ref_axis',(-0.614823566703066,0.584031767476771,-0.529998940003165)) ;
#55503 = DIRECTION('center_axis',(-0.313853049248083,0.435327419404426,0.843792807146614)) ;
#55504 = DIRECTION('ref_axis',(-0.811165460726608,-0.584816719429421,2.43009916984589E-17)) ;
#55505 = DIRECTION('center_axis',(0.,0.,-1.)) ;
#55506 = DIRECTION('ref_axis',(-1.,0.,0.)) ;
#55507 = DIRECTION('center_axis',(0.,0.,1.)) ;
#55508 = DIRECTION('ref_axis',(-0.70710678118654,0.707106781186555,0.)) ;
#55509 = DIRECTION('center_axis',(0.,0.,1.)) ;
#55510 = DIRECTION('ref_axis',(1.,0.,0.)) ;
#55511 = DIRECTION('center_axis',(-8.18284374038753E-14,2.2330315979718E-11,
-1.)) ;
#55512 = DIRECTION('ref_axis',(0.9999932859525,0.00366443036803338,-2.0111893130656E-29)) ;
#55513 = DIRECTION('center_axis',(-0.00196658644184458,0.536665474168601,
0.843792807135234)) ;
#55514 = DIRECTION('ref_axis',(0.154117454211902,0.833875850413451,-0.529998940003172)) ;
#55515 = DIRECTION('center_axis',(0.983346129909768,-0.181742644394433,-2.0434311177167E-13)) ;
#55516 = DIRECTION('ref_axis',(0.181742644394433,0.983346129909768,1.81948992375041E-30)) ;
#55517 = DIRECTION('center_axis',(0.,0.,1.)) ;
#55518 = DIRECTION('ref_axis',(1.,0.,0.)) ;
#55519 = DIRECTION('center_axis',(-3.47159356885201E-9,1.11394131129615E-9,
-1.)) ;
#55520 = DIRECTION('ref_axis',(0.30552983924033,0.952182502114893,-5.05335281096018E-24)) ;
#55521 = DIRECTION('center_axis',(-0.511006903307709,0.163968420330768,0.843792807451035)) ;
#55522 = DIRECTION('ref_axis',(-0.745438148835789,0.404256218079294,-0.529998940003184)) ;
#55523 = DIRECTION('center_axis',(0.476718191734985,0.879056178903787,-4.318892192726E-11)) ;
#55524 = DIRECTION('ref_axis',(-0.879056178903787,0.476718191734985,-2.44707824205826E-27)) ;
#55525 = DIRECTION('center_axis',(0.,0.,1.)) ;
#55526 = DIRECTION('ref_axis',(1.,0.,0.)) ;
#55527 = DIRECTION('center_axis',(2.04816646369444E-11,-9.78185806535746E-12,
-1.)) ;
#55528 = DIRECTION('ref_axis',(0.430963465142067,0.902369376537536,1.52695952366941E-26)) ;
#55529 = DIRECTION('center_axis',(-0.902369376537554,0.430963465142031,1.0484051409526E-14)) ;
#55530 = DIRECTION('ref_axis',(0.365456287528609,0.765207700890011,-0.52999894000312)) ;
#55531 = DIRECTION('center_axis',(0.317035052992538,0.433015558359767,0.843792807146635)) ;
#55532 = DIRECTION('ref_axis',(-0.806857664466093,0.590745892319466,-1.0919610983098E-14)) ;
#55533 = DIRECTION('center_axis',(0.,0.,1.)) ;
#55534 = DIRECTION('ref_axis',(-0.969741506148218,-0.244134002657118,0.)) ;
#55535 = DIRECTION('center_axis',(9.63335300264386E-12,2.01707185088096E-11,
-1.)) ;
#55536 = DIRECTION('ref_axis',(-0.902369376537538,0.430963465142064,-8.19822425960458E-27)) ;
#55537 = DIRECTION('center_axis',(-0.430963465142029,-0.902369376537555,-4.78686444844716E-13)) ;
#55538 = DIRECTION('ref_axis',(-0.76520770088988,0.365456287528832,-0.529998940003155)) ;
#55539 = DIRECTION('center_axis',(-0.433015558360072,0.317035052992619,0.843792807146448)) ;
#55540 = DIRECTION('ref_axis',(-0.590745892319279,-0.806857664466229,4.35385268996785E-16)) ;
#55541 = DIRECTION('center_axis',(0.,0.,-1.)) ;
#55542 = DIRECTION('ref_axis',(-1.,0.,0.)) ;
#55543 = DIRECTION('center_axis',(-4.22164579210917E-16,-8.28544638211483E-16,
1.)) ;
#55544 = DIRECTION('ref_axis',(-0.891006524188363,0.453990499739557,-3.67890034138173E-31)) ;
#55545 = DIRECTION('center_axis',(0.,0.,1.)) ;
#55546 = DIRECTION('ref_axis',(1.,0.,0.)) ;
#55547 = DIRECTION('center_axis',(1.1139654743955E-9,3.47166887305239E-9,
-1.)) ;
#55548 = DIRECTION('ref_axis',(0.95218250211488,-0.30552983924037,3.12386086939447E-24)) ;
#55549 = DIRECTION('center_axis',(0.163968420330646,0.511006903307724,0.843792807451049)) ;
#55550 = DIRECTION('ref_axis',(0.404256218079267,0.745438148835828,-0.529998940003149)) ;
#55551 = DIRECTION('center_axis',(0.879056178903768,-0.476718191735019,-4.35521559523163E-11)) ;
#55552 = DIRECTION('ref_axis',(0.476718191735019,0.879056178903768,1.19542347053691E-27)) ;
#55553 = DIRECTION('center_axis',(0.,0.,1.)) ;
#55554 = DIRECTION('ref_axis',(1.,0.,0.)) ;
#55555 = DIRECTION('center_axis',(-2.2505433560128E-11,-8.24701478889645E-14,
-1.)) ;
#55556 = DIRECTION('ref_axis',(-0.00366443036789935,0.9999932859525,-6.10256549266988E-30)) ;
#55557 = DIRECTION('center_axis',(-0.536665474168608,-0.00196658644177862,
0.843792807135229)) ;
#55558 = DIRECTION('ref_axis',(-0.833875850413441,0.154117454211901,-0.529998940003188)) ;
#55559 = DIRECTION('center_axis',(0.181742644394586,0.98334612990974,1.24050620488944E-13)) ;
#55560 = DIRECTION('ref_axis',(-0.98334612990974,0.181742644394586,4.16361191750322E-31)) ;
#55561 = DIRECTION('center_axis',(0.,0.,1.)) ;
#55562 = DIRECTION('ref_axis',(1.,0.,0.)) ;
#55563 = DIRECTION('center_axis',(1.63294940199106E-11,-1.55116748461524E-11,
-1.)) ;
#55564 = DIRECTION('ref_axis',(0.688718084362179,0.725029240977556,-3.72638284961352E-26)) ;
#55565 = DIRECTION('center_axis',(-0.725029240977534,0.688718084362202,3.31781870825906E-13)) ;
#55566 = DIRECTION('ref_axis',(0.584031767476678,0.614823566703193,-0.529998940003121)) ;
#55567 = DIRECTION('center_axis',(0.435327419404398,0.313853049248157,0.843792807146601)) ;
#55568 = DIRECTION('ref_axis',(-0.584816719429501,0.81116546072655,-2.76706225236514E-14)) ;
#55569 = DIRECTION('center_axis',(0.,0.,1.)) ;
#55570 = DIRECTION('ref_axis',(-0.846837422818252,-0.531851839626921,0.)) ;
#55571 = DIRECTION('center_axis',(2.95467354287013E-12,2.23563733542085E-11,
-1.)) ;
#55572 = DIRECTION('ref_axis',(-0.99137931034482,0.131023139254975,-2.37981664476678E-27)) ;
#55573 = DIRECTION('center_axis',(-0.13102313925497,-0.991379310344821,-2.30233604581775E-13)) ;
#55574 = DIRECTION('ref_axis',(-0.840687973798143,0.11110739987376,-0.529998940003153)) ;
#55575 = DIRECTION('center_axis',(-0.509791487622676,0.167709086680539,0.84379280714654)) ;
#55576 = DIRECTION('ref_axis',(-0.3125000000031,-0.949917759597147,-6.06868932102577E-15)) ;
#55577 = DIRECTION('center_axis',(0.,0.,-1.)) ;
#55578 = DIRECTION('ref_axis',(-1.,0.,0.)) ;
#55579 = DIRECTION('center_axis',(-4.07310400565444E-16,-2.57165665851294E-15,
1.)) ;
#55580 = DIRECTION('ref_axis',(-0.987688340595137,0.156434465040233,1.02208220263746E-30)) ;
#55581 = DIRECTION('center_axis',(0.,0.,1.)) ;
#55582 = DIRECTION('ref_axis',(1.,0.,0.)) ;
#55583 = DIRECTION('center_axis',(2.13219594596649E-9,2.95744572512378E-9,
-1.)) ;
#55584 = DIRECTION('ref_axis',(0.811165460724706,-0.584816719432059,2.16408345829625E-24)) ;
#55585 = DIRECTION('center_axis',(0.31385305198712,0.435327416839625,0.843792807451041)) ;
#55586 = DIRECTION('ref_axis',(0.614823566702783,0.584031767477069,-0.529998940003167)) ;
#55587 = DIRECTION('center_axis',(0.688718084362157,-0.725029240977577,-4.29727203305136E-11)) ;
#55588 = DIRECTION('ref_axis',(0.725029240977577,0.688718084362157,-2.82507373973619E-28)) ;
#55589 = DIRECTION('center_axis',(0.,0.,1.)) ;
#55590 = DIRECTION('ref_axis',(-0.846837422818128,0.531851839627119,0.)) ;
#55591 = DIRECTION('center_axis',(-2.13516241724208E-11,-7.02416865719327E-12,
-1.)) ;
#55592 = DIRECTION('ref_axis',(-0.312499999999965,0.949917759598178,-2.13901517135901E-26)) ;
#55593 = DIRECTION('center_axis',(-0.509791487647294,-0.167709086662617,0.843792807135229)) ;
#55594 = DIRECTION('ref_axis',(-0.840687973798133,-0.111107399873593,-0.529998940003203)) ;
#55595 = DIRECTION('center_axis',(-0.131023139254975,0.99137931034482,1.00333650532032E-13)) ;
#55596 = DIRECTION('ref_axis',(-0.99137931034482,-0.131023139254975,-1.54140930935766E-30)) ;
#55597 = DIRECTION('center_axis',(0.,0.,1.)) ;
#55598 = DIRECTION('ref_axis',(1.,0.,0.)) ;
#55599 = DIRECTION('center_axis',(1.06076376456186E-11,-1.95602130936441E-11,
-1.)) ;
#55600 = DIRECTION('ref_axis',(0.879056178903777,0.476718191735003,-1.06012529608883E-27)) ;
#55601 = DIRECTION('center_axis',(-0.476718191735159,0.879056178903692,-5.28038199040795E-14)) ;
#55602 = DIRECTION('ref_axis',(0.745438148835549,0.404256218079769,-0.529998940003159)) ;
#55603 = DIRECTION('center_axis',(0.511006904900899,0.163968416933291,0.843792807146396)) ;
#55604 = DIRECTION('ref_axis',(-0.305529839237293,0.952182502115867,-3.36895286441765E-16)) ;
#55605 = DIRECTION('center_axis',(0.,0.,1.)) ;
#55606 = DIRECTION('ref_axis',(1.,0.,0.)) ;
#55607 = DIRECTION('center_axis',(-4.09946443533915E-12,2.21807738113741E-11,
-1.)) ;
#55608 = DIRECTION('ref_axis',(-0.983346129909772,-0.181742644394414,7.99870886518743E-27)) ;
#55609 = DIRECTION('center_axis',(0.181742644394235,-0.983346129909805,3.51119831505045E-13)) ;
#55610 = DIRECTION('ref_axis',(-0.833875850413454,-0.154117454211895,-0.529998940003169)) ;
#55611 = DIRECTION('center_axis',(-0.536665474150717,0.00196658646630492,
0.843792807146551)) ;
#55612 = DIRECTION('ref_axis',(-0.00366443037100923,-0.999993285952489,-4.49392882749049E-18)) ;
#55613 = DIRECTION('center_axis',(0.,0.,-1.)) ;
#55614 = DIRECTION('ref_axis',(-1.,0.,0.)) ;
#55615 = DIRECTION('center_axis',(4.07310400565444E-16,-2.57165665851294E-15,
1.)) ;
#55616 = DIRECTION('ref_axis',(-0.987688340595137,-0.156434465040233,-1.02208220263746E-30)) ;
#55617 = DIRECTION('center_axis',(0.,0.,1.)) ;
#55618 = DIRECTION('ref_axis',(1.,0.,0.)) ;
#55619 = DIRECTION('center_axis',(1.7935464781828E-11,1.31315628682055E-11,
-1.)) ;
#55620 = DIRECTION('ref_axis',(0.590745892316729,-0.806857664468097,-2.56130688849362E-26)) ;
#55621 = DIRECTION('center_axis',(0.433015558388759,0.317035052983428,0.84379280713518)) ;
#55622 = DIRECTION('ref_axis',(0.765207700889972,0.365456287528543,-0.529998940003221)) ;
#55623 = DIRECTION('center_axis',(0.430963465142209,-0.902369376537469,2.13644511040471E-13)) ;
#55624 = DIRECTION('ref_axis',(0.902369376537469,0.430963465142209,1.03035559199192E-29)) ;
#55625 = DIRECTION('center_axis',(0.,0.,1.)) ;
#55626 = DIRECTION('ref_axis',(-0.969741506148105,0.244134002657569,0.)) ;
#55627 = DIRECTION('center_axis',(-1.81360138162381E-11,-1.32783960997652E-11,
-1.)) ;
#55628 = DIRECTION('ref_axis',(-0.590745892316613,0.806857664468181,4.5131152795346E-26)) ;
#55629 = DIRECTION('center_axis',(-0.433015558388868,-0.317035052983152,0.843792807135227)) ;
#55630 = DIRECTION('ref_axis',(-0.765207700889916,-0.365456287528693,-0.529998940003199)) ;
#55631 = DIRECTION('center_axis',(-0.430963465142191,0.902369376537477,-1.55470811146141E-13)) ;
#55632 = DIRECTION('ref_axis',(-0.902369376537477,-0.430963465142191,-2.56005574118538E-30)) ;
#55633 = DIRECTION('center_axis',(0.,0.,1.)) ;
#55634 = DIRECTION('ref_axis',(1.,0.,0.)) ;
#55635 = DIRECTION('center_axis',(4.10254442364617E-12,-2.21974385550383E-11,
-1.)) ;
#55636 = DIRECTION('ref_axis',(0.98334612990977,0.181742644394422,1.01873606893427E-26)) ;
#55637 = DIRECTION('center_axis',(-0.181742644394422,0.98334612990977,6.10504213176762E-14)) ;
#55638 = DIRECTION('ref_axis',(0.833875850413441,0.154117454211901,-0.529998940003189)) ;
#55639 = DIRECTION('center_axis',(0.536665474150816,-0.00196658646632877,
0.843792807146488)) ;
#55640 = DIRECTION('ref_axis',(0.00366443037105299,0.999993285952489,-2.34126876451944E-18)) ;
#55641 = DIRECTION('center_axis',(0.,0.,1.)) ;
#55642 = DIRECTION('ref_axis',(1.,0.,0.)) ;
#55643 = DIRECTION('center_axis',(-1.06507252826682E-11,1.96396655966931E-11,
-1.)) ;
#55644 = DIRECTION('ref_axis',(-0.879056178903767,-0.476718191735022,-5.02209139854702E-27)) ;
#55645 = DIRECTION('center_axis',(0.476718191735315,-0.879056178903608,-3.76403016459087E-13)) ;
#55646 = DIRECTION('ref_axis',(-0.745438148835569,-0.404256218079756,-0.529998940003141)) ;
#55647 = DIRECTION('center_axis',(-0.51100690490078,-0.163968416933259,0.843792807146473)) ;
#55648 = DIRECTION('ref_axis',(0.305529839237304,-0.952182502115864,-1.10174364593412E-16)) ;
#55649 = DIRECTION('center_axis',(0.,0.,-1.)) ;
#55650 = DIRECTION('ref_axis',(-1.,0.,0.)) ;
#55651 = DIRECTION('center_axis',(4.22164579210906E-16,-8.28544638211488E-16,
1.)) ;
#55652 = DIRECTION('ref_axis',(-0.891006524188369,-0.453990499739545,8.13162959031963E-31)) ;
#55653 = DIRECTION('center_axis',(0.,0.,1.)) ;
#55654 = DIRECTION('ref_axis',(1.,0.,0.)) ;
#55655 = DIRECTION('center_axis',(2.14643118094183E-11,7.06124016807633E-12,
-1.)) ;
#55656 = DIRECTION('ref_axis',(0.312500000000018,-0.94991775959816,2.99169651445016E-27)) ;
#55657 = DIRECTION('center_axis',(0.509791487647313,0.167709086662475,0.843792807135246)) ;
#55658 = DIRECTION('ref_axis',(0.840687973798138,0.111107399873593,-0.529998940003195)) ;
#55659 = DIRECTION('center_axis',(0.131023139254964,-0.991379310344822,-5.71828291818378E-13)) ;
#55660 = DIRECTION('ref_axis',(0.991379310344822,0.131023139254964,4.17162583323648E-30)) ;
#55661 = DIRECTION('center_axis',(0.,0.,1.)) ;
#55662 = DIRECTION('ref_axis',(-0.997720534324265,-0.0674813706714934,0.)) ;
#55663 = DIRECTION('center_axis',(-2.13215299884117E-9,-2.95738615564921E-9,
-1.)) ;
#55664 = DIRECTION('ref_axis',(-0.811165460724706,0.584816719432059,1.39233222030208E-24)) ;
#55665 = DIRECTION('center_axis',(-0.313853051987107,-0.435327416839706,0.843792807451004)) ;
#55666 = DIRECTION('ref_axis',(-0.614823566702853,-0.584031767476959,-0.529998940003206)) ;
#55667 = DIRECTION('center_axis',(-0.688718084362157,0.725029240977577,-4.33310958927125E-11)) ;
#55668 = DIRECTION('ref_axis',(-0.725029240977577,-0.688718084362157,1.5461825750629E-27)) ;
#55669 = DIRECTION('center_axis',(0.,0.,1.)) ;
#55670 = DIRECTION('ref_axis',(1.,0.,0.)) ;
#55671 = DIRECTION('center_axis',(-2.94653190735649E-12,-2.22947701210221E-11,
-1.)) ;
#55672 = DIRECTION('ref_axis',(0.991379310344822,-0.131023139254964,-6.81534253461201E-28)) ;
#55673 = DIRECTION('center_axis',(0.131023139254789,0.991379310344845,-5.43252859013157E-13)) ;
#55674 = DIRECTION('ref_axis',(0.840687973798117,-0.111107399873768,-0.529998940003192)) ;
#55675 = DIRECTION('center_axis',(0.509791487622542,-0.167709086680493,0.84379280714663)) ;
#55676 = DIRECTION('ref_axis',(0.312500000003087,0.949917759597151,1.58736934972717E-16)) ;
#55677 = DIRECTION('center_axis',(0.,0.,1.)) ;
#55678 = DIRECTION('ref_axis',(1.,0.,0.)) ;
#55679 = DIRECTION('center_axis',(-1.62352932768802E-11,1.54221918961996E-11,
-1.)) ;
#55680 = DIRECTION('ref_axis',(-0.688718084362202,-0.725029240977533,1.19191244840782E-26)) ;
#55681 = DIRECTION('center_axis',(0.725029240977534,-0.688718084362202,2.10320299617929E-13)) ;
#55682 = DIRECTION('ref_axis',(-0.58403176747671,-0.614823566703132,-0.529998940003157)) ;
#55683 = DIRECTION('center_axis',(-0.435327419404505,-0.313853049248141,0.843792807146552)) ;
#55684 = DIRECTION('ref_axis',(0.584816719429358,-0.811165460726653,-5.01043326805999E-14)) ;
#55685 = DIRECTION('center_axis',(0.,0.,-1.)) ;
#55686 = DIRECTION('ref_axis',(-1.,0.,0.)) ;
#55687 = DIRECTION('center_axis',(1.44658084518888E-15,-1.70959554431413E-15,
1.)) ;
#55688 = DIRECTION('ref_axis',(-0.707106781186548,-0.707106781186548,-1.85979477303204E-16)) ;
#55689 = DIRECTION('center_axis',(0.,0.,1.)) ;
#55690 = DIRECTION('ref_axis',(1.,0.,0.)) ;
#55691 = DIRECTION('center_axis',(2.24206992470253E-11,8.21596428150777E-14,
-1.)) ;
#55692 = DIRECTION('ref_axis',(0.00366443036794375,-0.9999932859525,-1.73167550995323E-28)) ;
#55693 = DIRECTION('center_axis',(0.536665474168609,0.00196658644184461,0.843792807135228)) ;
#55694 = DIRECTION('ref_axis',(0.833875850413446,-0.154117454211902,-0.529998940003181)) ;
#55695 = DIRECTION('center_axis',(-0.181742644394406,-0.983346129909773,8.68769869850415E-14)) ;
#55696 = DIRECTION('ref_axis',(0.983346129909773,-0.181742644394406,-7.34270832319073E-31)) ;
#55697 = DIRECTION('center_axis',(0.,0.,1.)) ;
#55698 = DIRECTION('ref_axis',(-0.928035725269356,-0.372491198048733,0.)) ;
#55699 = DIRECTION('center_axis',(-1.11393785942449E-9,-3.4715828111092E-9,
-1.)) ;
#55700 = DIRECTION('ref_axis',(-0.952182502114923,0.305529839240235,-3.60849389683753E-24)) ;
#55701 = DIRECTION('center_axis',(-0.163968420330871,-0.511006903307736,0.843792807450998)) ;
#55702 = DIRECTION('ref_axis',(-0.404256218079276,-0.745438148835749,-0.529998940003254)) ;
#55703 = DIRECTION('center_axis',(-0.879056178903768,0.476718191735019,-4.37732160119147E-11)) ;
#55704 = DIRECTION('ref_axis',(-0.476718191735019,-0.879056178903768,9.78614700219985E-28)) ;
#55705 = DIRECTION('center_axis',(0.,0.,1.)) ;
#55706 = DIRECTION('ref_axis',(1.,0.,0.)) ;
#55707 = DIRECTION('center_axis',(-9.62361496574279E-12,-2.01503285987642E-11,
-1.)) ;
#55708 = DIRECTION('ref_axis',(0.902369376537538,-0.430963465142064,9.56718048253853E-27)) ;
#55709 = DIRECTION('center_axis',(0.430963465142353,0.9023693765374,1.31562059760998E-13)) ;
#55710 = DIRECTION('ref_axis',(0.765207700889898,-0.36545628752882,-0.529998940003137)) ;
#55711 = DIRECTION('center_axis',(0.43301555835997,-0.317035052992614,0.843792807146502)) ;
#55712 = DIRECTION('ref_axis',(0.590745892319364,0.806857664466167,1.44988079538749E-16)) ;
#55713 = DIRECTION('center_axis',(0.,0.,1.)) ;
#55714 = DIRECTION('ref_axis',(1.,0.,0.)) ;
#55715 = DIRECTION('center_axis',(-2.0282863014037E-11,9.68691220559095E-12,
-1.)) ;
#55716 = DIRECTION('ref_axis',(-0.430963465142136,-0.902369376537504,2.16449102858497E-26)) ;
#55717 = DIRECTION('center_axis',(0.902369376537521,-0.4309634651421,-8.69409141277904E-14)) ;
#55718 = DIRECTION('ref_axis',(-0.365456287528697,-0.765207700889925,-0.529998940003183)) ;
#55719 = DIRECTION('center_axis',(-0.317035052992546,-0.433015558360071,0.843792807146476)) ;
#55720 = DIRECTION('ref_axis',(0.806857664466293,-0.590745892319192,-1.37211078002745E-16)) ;
#55721 = DIRECTION('center_axis',(0.,0.,-1.)) ;
#55722 = DIRECTION('ref_axis',(-1.,0.,0.)) ;
#55723 = DIRECTION('center_axis',(-9.94253565853781E-16,5.06597495053088E-16,
1.)) ;
#55724 = DIRECTION('ref_axis',(-0.453990499739548,-0.891006524188367,-3.14592610423102E-31)) ;
#55725 = DIRECTION('center_axis',(0.,0.,1.)) ;
#55726 = DIRECTION('ref_axis',(1.,0.,0.)) ;
#55727 = DIRECTION('center_axis',(3.47146985480851E-9,-1.11390161477595E-9,
-1.)) ;
#55728 = DIRECTION('ref_axis',(-0.305529839240301,-0.952182502114902,-1.48325462235839E-24)) ;
#55729 = DIRECTION('center_axis',(0.511006903307789,-0.1639684203306,0.843792807451018)) ;
#55730 = DIRECTION('ref_axis',(0.745438148835797,-0.404256218079275,-0.529998940003187)) ;
#55731 = DIRECTION('center_axis',(-0.476718191734966,-0.879056178903797,-4.38641204088889E-11)) ;
#55732 = DIRECTION('ref_axis',(0.879056178903797,-0.476718191734966,-1.80827304522098E-27)) ;
#55733 = DIRECTION('center_axis',(0.,0.,1.)) ;
#55734 = DIRECTION('ref_axis',(1.,0.,0.)) ;
#55735 = DIRECTION('center_axis',(8.22631445047335E-14,-2.24489440180613E-11,
-1.)) ;
#55736 = DIRECTION('ref_axis',(-0.9999932859525,-0.00366443036785559,1.09795538423137E-28)) ;
#55737 = DIRECTION('center_axis',(0.0019665864417164,-0.536665474168584,0.843792807135245)) ;
#55738 = DIRECTION('ref_axis',(-0.154117454211859,-0.833875850413457,-0.529998940003176)) ;
#55739 = DIRECTION('center_axis',(-0.98334612990977,0.181742644394422,-1.2520130905831E-13)) ;
#55740 = DIRECTION('ref_axis',(-0.181742644394422,-0.98334612990977,3.55276238107094E-31)) ;
#55741 = DIRECTION('center_axis',(0.,0.,1.)) ;
#55742 = DIRECTION('ref_axis',(1.,0.,0.)) ;
#55743 = DIRECTION('center_axis',(-1.53521617614545E-11,-1.61615709562502E-11,
-1.)) ;
#55744 = DIRECTION('ref_axis',(0.725029240977556,-0.688718084362179,4.97396118593888E-26)) ;
#55745 = DIRECTION('center_axis',(0.688718084362295,0.725029240977446,1.16091691217673E-13)) ;
#55746 = DIRECTION('ref_axis',(0.614823566703032,-0.584031767476833,-0.529998940003137)) ;
#55747 = DIRECTION('center_axis',(0.313853049248137,-0.435327419404485,0.843792807146564)) ;
#55748 = DIRECTION('ref_axis',(0.811165460726592,0.584816719429442,5.74276711858885E-15)) ;
#55749 = DIRECTION('center_axis',(0.,0.,1.)) ;
#55750 = DIRECTION('ref_axis',(1.,0.,0.)) ;
#55751 = DIRECTION('center_axis',(-2.20203557186253E-11,2.91026462188401E-12,
-1.)) ;
#55752 = DIRECTION('ref_axis',(-0.13102313925492,-0.991379310344828,-4.30145676726048E-27)) ;
#55753 = DIRECTION('center_axis',(0.991379310344833,-0.131023139254877,-7.01280755869045E-14)) ;
#55754 = DIRECTION('ref_axis',(-0.111107399873598,-0.840687973798168,-0.529998940003147)) ;
#55755 = DIRECTION('center_axis',(-0.167709086680666,-0.50979148762307,0.843792807146277)) ;
#55756 = DIRECTION('ref_axis',(0.949917759597151,-0.312500000003087,-4.01412734958935E-16)) ;
#55757 = DIRECTION('center_axis',(0.,0.,-1.)) ;
#55758 = DIRECTION('ref_axis',(-1.,0.,0.)) ;
#55759 = DIRECTION('center_axis',(-2.57165665851294E-15,4.0731040056544E-16,
1.)) ;
#55760 = DIRECTION('ref_axis',(-0.156434465040232,-0.987688340595138,-1.98479792514679E-30)) ;
#55761 = DIRECTION('center_axis',(0.,0.,1.)) ;
#55762 = DIRECTION('ref_axis',(1.,0.,0.)) ;
#55763 = DIRECTION('center_axis',(2.95735407977765E-9,-2.13212987346573E-9,
-1.)) ;
#55764 = DIRECTION('ref_axis',(-0.584816719432093,-0.811165460724681,2.97218307444548E-24)) ;
#55765 = DIRECTION('center_axis',(0.435327416839734,-0.313853051987051,0.84379280745101)) ;
#55766 = DIRECTION('ref_axis',(0.584031767477118,-0.614823566702701,-0.529998940003206)) ;
#55767 = DIRECTION('center_axis',(-0.725029240977556,-0.688718084362179,-4.39928696743698E-11)) ;
#55768 = DIRECTION('ref_axis',(0.688718084362179,-0.725029240977556,-1.08729406708994E-27)) ;
#55769 = DIRECTION('center_axis',(0.,0.,1.)) ;
#55770 = DIRECTION('ref_axis',(1.,0.,0.)) ;
#55771 = DIRECTION('center_axis',(7.01181148690086E-12,-2.13140616267525E-11,
-1.)) ;
#55772 = DIRECTION('ref_axis',(-0.949917759598147,-0.312500000000059,-1.64248236045399E-27)) ;
#55773 = DIRECTION('center_axis',(0.167709086662834,-0.50979148764727,0.8437928071352)) ;
#55774 = DIRECTION('ref_axis',(0.111107399873592,-0.840687973798123,-0.529998940003219)) ;
#55775 = DIRECTION('center_axis',(-0.991379310344825,-0.131023139254943,-2.99498663741709E-13)) ;
#55776 = DIRECTION('ref_axis',(0.131023139254943,-0.991379310344825,-1.19589846978882E-30)) ;
#55777 = DIRECTION('center_axis',(0.,0.,1.)) ;
#55778 = DIRECTION('ref_axis',(1.,0.,0.)) ;
#55779 = DIRECTION('center_axis',(-1.9257300425779E-11,-1.04433660293747E-11,
-1.)) ;
#55780 = DIRECTION('ref_axis',(0.476718191735025,-0.879056178903765,1.65334232004212E-26)) ;
#55781 = DIRECTION('center_axis',(0.879056178903672,0.476718191735196,-1.47927408302731E-13)) ;
#55782 = DIRECTION('ref_axis',(0.404256218079741,-0.745438148835528,-0.52999894000321)) ;
#55783 = DIRECTION('center_axis',(0.163968416933482,-0.511006904901325,0.8437928071461)) ;
#55784 = DIRECTION('ref_axis',(0.952182502115837,0.305529839237387,7.9536453947219E-16)) ;
#55785 = DIRECTION('center_axis',(0.,0.,1.)) ;
#55786 = DIRECTION('ref_axis',(1.,0.,0.)) ;
#55787 = DIRECTION('center_axis',(-2.17530453907752E-11,-4.02041140215211E-12,
-1.)) ;
#55788 = DIRECTION('ref_axis',(0.181742644394422,-0.98334612990977,1.13897981748785E-26)) ;
#55789 = DIRECTION('center_axis',(0.983346129909754,0.181742644394508,-1.0017383267518E-13)) ;
#55790 = DIRECTION('ref_axis',(0.15411745421188,-0.833875850413392,-0.529998940003271)) ;
#55791 = DIRECTION('center_axis',(-0.00196658646623659,-0.536665474151653,
0.843792807145956)) ;
#55792 = DIRECTION('ref_axis',(0.999993285952489,-0.00366443037087552,-6.21826829040495E-18)) ;
#55793 = DIRECTION('center_axis',(0.,0.,-1.)) ;
#55794 = DIRECTION('ref_axis',(-1.,0.,0.)) ;
#55795 = DIRECTION('center_axis',(5.51069283967058E-16,8.72808001211679E-17,
1.)) ;
#55796 = DIRECTION('ref_axis',(0.156434465040235,-0.987688340595137,9.09125219431195E-32)) ;
#55797 = DIRECTION('center_axis',(0.,0.,1.)) ;
#55798 = DIRECTION('ref_axis',(1.,0.,0.)) ;
#55799 = DIRECTION('center_axis',(1.29546955665479E-11,-1.76938943540163E-11,
-1.)) ;
#55800 = DIRECTION('ref_axis',(-0.806857664468129,-0.590745892316684,3.0891578375814E-26)) ;
#55801 = DIRECTION('center_axis',(0.317035052983624,-0.433015558388607,0.843792807135184)) ;
#55802 = DIRECTION('ref_axis',(0.365456287528694,-0.765207700889918,-0.529998940003195)) ;
#55803 = DIRECTION('center_axis',(-0.902369376537504,-0.430963465142136,-4.698644991465E-13)) ;
#55804 = DIRECTION('ref_axis',(0.430963465142136,-0.902369376537503,1.34307188058981E-30)) ;
#55805 = DIRECTION('center_axis',(0.,0.,-1.)) ;
#55806 = DIRECTION('ref_axis',(-1.,0.,0.)) ;
#55807 = DIRECTION('center_axis',(-3.31417855284593E-16,-1.68865831684365E-16,
1.)) ;
#55808 = DIRECTION('ref_axis',(0.453990499739554,-0.891006524188364,2.22675583611484E-31)) ;
#55809 = DIRECTION('center_axis',(0.,0.,-1.)) ;
#55810 = DIRECTION('ref_axis',(-0.24413400265269,-0.969741506149333,0.)) ;
#55811 = DIRECTION('',(0.,0.,-1.)) ;
#55812 = DIRECTION('center_axis',(0.,0.,1.)) ;
#55813 = DIRECTION('ref_axis',(0.767508312901273,-0.641038992283185,0.)) ;
#55814 = DIRECTION('',(0.,0.,1.)) ;
#55815 = DIRECTION('center_axis',(0.,0.,1.)) ;
#55816 = DIRECTION('ref_axis',(0.928035724967976,-0.3724911987996,0.)) ;
#55817 = DIRECTION('',(0.,0.,1.)) ;
#55818 = DIRECTION('center_axis',(0.,0.,1.)) ;
#55819 = DIRECTION('ref_axis',(1.,0.,0.)) ;
#55820 = DIRECTION('center_axis',(0.,0.,1.)) ;
#55821 = DIRECTION('ref_axis',(0.309016994374953,-0.951056516295152,0.)) ;
#55822 = DIRECTION('center_axis',(0.,0.,-1.)) ;
#55823 = DIRECTION('ref_axis',(-0.531851839622895,-0.846837422820781,0.)) ;
#55824 = DIRECTION('',(0.,0.,-1.)) ;
#55825 = DIRECTION('center_axis',(0.,0.,-1.)) ;
#55826 = DIRECTION('ref_axis',(-1.,0.,0.)) ;
#55827 = DIRECTION('center_axis',(1.44658084518887E-15,1.44658084518888E-15,
1.)) ;
#55828 = DIRECTION('ref_axis',(0.707106781186548,-0.707106781186547,5.66547588605294E-30)) ;
#55829 = DIRECTION('center_axis',(0.,0.,-1.)) ;
#55830 = DIRECTION('ref_axis',(0.0674813714788309,-0.99772053426966,0.)) ;
#55831 = DIRECTION('',(0.,0.,-1.)) ;
#55832 = DIRECTION('center_axis',(0.,0.,1.)) ;
#55833 = DIRECTION('ref_axis',(1.,0.,0.)) ;
#55834 = DIRECTION('center_axis',(0.,0.,1.)) ;
#55835 = DIRECTION('ref_axis',(0.587785252292479,-0.809016994374943,0.)) ;
#55836 = DIRECTION('center_axis',(0.,0.,1.)) ;
#55837 = DIRECTION('ref_axis',(0.531851839622895,-0.846837422820781,0.)) ;
#55838 = DIRECTION('',(0.,0.,1.)) ;
#55839 = DIRECTION('center_axis',(0.,0.,1.)) ;
#55840 = DIRECTION('ref_axis',(1.,0.,0.)) ;
#55841 = DIRECTION('center_axis',(0.,0.,1.)) ;
#55842 = DIRECTION('ref_axis',(0.,-1.,0.)) ;
#55843 = DIRECTION('center_axis',(0.,0.,1.)) ;
#55844 = DIRECTION('ref_axis',(0.99772053426966,-0.0674813714788309,0.)) ;
#55845 = DIRECTION('',(0.,0.,1.)) ;
#55846 = DIRECTION('center_axis',(0.,0.,-1.)) ;
#55847 = DIRECTION('ref_axis',(-0.767508312901297,-0.641038992283156,0.)) ;
#55848 = DIRECTION('',(0.,0.,-1.)) ;
#55849 = DIRECTION('center_axis',(0.,0.,-1.)) ;
#55850 = DIRECTION('ref_axis',(-1.,0.,0.)) ;
#55851 = DIRECTION('center_axis',(5.06597495053079E-16,9.94253565853788E-16,
1.)) ;
#55852 = DIRECTION('ref_axis',(0.891006524188372,-0.453990499739539,-6.76446233908251E-32)) ;
#55853 = DIRECTION('center_axis',(0.,0.,-1.)) ;
#55854 = DIRECTION('ref_axis',(0.37249119879969,-0.92803572496794,0.)) ;
#55855 = DIRECTION('',(0.,0.,-1.)) ;
#55856 = DIRECTION('center_axis',(0.,0.,1.)) ;
#55857 = DIRECTION('ref_axis',(1.,0.,0.)) ;
#55858 = DIRECTION('center_axis',(0.,0.,1.)) ;
#55859 = DIRECTION('ref_axis',(0.809016994374954,-0.587785252292464,0.)) ;
#55860 = DIRECTION('center_axis',(0.,0.,1.)) ;
#55861 = DIRECTION('ref_axis',(0.24413400265269,-0.969741506149333,0.)) ;
#55862 = DIRECTION('',(0.,0.,1.)) ;
#55863 = DIRECTION('center_axis',(0.,0.,1.)) ;
#55864 = DIRECTION('ref_axis',(1.,0.,0.)) ;
#55865 = DIRECTION('center_axis',(0.,0.,1.)) ;
#55866 = DIRECTION('ref_axis',(-0.309016994374946,-0.951056516295154,0.)) ;
#55867 = DIRECTION('center_axis',(0.,0.,1.)) ;
#55868 = DIRECTION('ref_axis',(0.969741506149316,0.244134002652757,0.)) ;
#55869 = DIRECTION('',(0.,0.,1.)) ;
#55870 = DIRECTION('center_axis',(0.,0.,-1.)) ;
#55871 = DIRECTION('ref_axis',(-0.928035724967896,-0.372491198799799,0.)) ;
#55872 = DIRECTION('',(0.,0.,-1.)) ;
#55873 = DIRECTION('center_axis',(0.,0.,-1.)) ;
#55874 = DIRECTION('ref_axis',(-1.,0.,0.)) ;
#55875 = DIRECTION('center_axis',(1.25502561241578E-16,-3.96473122685091E-16,
1.)) ;
#55876 = DIRECTION('ref_axis',(0.987688340595138,-0.156434465040227,-1.85979477303204E-16)) ;
#55877 = DIRECTION('center_axis',(0.,0.,-1.)) ;
#55878 = DIRECTION('ref_axis',(0.641038992283168,-0.767508312901288,0.)) ;
#55879 = DIRECTION('',(0.,0.,-1.)) ;
#55880 = DIRECTION('center_axis',(0.,0.,1.)) ;
#55881 = DIRECTION('ref_axis',(1.,0.,0.)) ;
#55882 = DIRECTION('center_axis',(0.,0.,1.)) ;
#55883 = DIRECTION('ref_axis',(0.951056516295156,-0.309016994374941,0.)) ;
#55884 = DIRECTION('center_axis',(0.,0.,1.)) ;
#55885 = DIRECTION('ref_axis',(-0.0674813714788309,-0.99772053426966,0.)) ;
#55886 = DIRECTION('',(0.,0.,1.)) ;
#55887 = DIRECTION('center_axis',(0.,0.,1.)) ;
#55888 = DIRECTION('ref_axis',(1.,0.,0.)) ;
#55889 = DIRECTION('center_axis',(0.,0.,1.)) ;
#55890 = DIRECTION('ref_axis',(-0.587785252292474,-0.809016994374947,0.)) ;
#55891 = DIRECTION('center_axis',(0.,0.,1.)) ;
#55892 = DIRECTION('ref_axis',(0.846837422820716,0.531851839622999,0.)) ;
#55893 = DIRECTION('',(0.,0.,1.)) ;
#55894 = DIRECTION('center_axis',(0.,0.,-1.)) ;
#55895 = DIRECTION('ref_axis',(-0.997720534269675,-0.0674813714786051,0.)) ;
#55896 = DIRECTION('',(0.,0.,-1.)) ;
#55897 = DIRECTION('center_axis',(0.,0.,-1.)) ;
#55898 = DIRECTION('ref_axis',(-1.,0.,0.)) ;
#55899 = DIRECTION('center_axis',(-4.07310400565444E-16,2.57165665851294E-15,
1.)) ;
#55900 = DIRECTION('ref_axis',(0.987688340595137,0.156434465040233,-1.02208220263746E-30)) ;
#55901 = DIRECTION('center_axis',(0.,0.,-1.)) ;
#55902 = DIRECTION('ref_axis',(0.846837422820716,-0.531851839622999,0.)) ;
#55903 = DIRECTION('',(0.,0.,-1.)) ;
#55904 = DIRECTION('center_axis',(0.,0.,1.)) ;
#55905 = DIRECTION('ref_axis',(1.,0.,0.)) ;
#55906 = DIRECTION('center_axis',(0.,0.,1.)) ;
#55907 = DIRECTION('ref_axis',(1.,0.,0.)) ;
#55908 = DIRECTION('center_axis',(0.,0.,1.)) ;
#55909 = DIRECTION('ref_axis',(-0.37249119879969,-0.92803572496794,0.)) ;
#55910 = DIRECTION('',(0.,0.,1.)) ;
#55911 = DIRECTION('center_axis',(0.,0.,1.)) ;
#55912 = DIRECTION('ref_axis',(1.,0.,0.)) ;
#55913 = DIRECTION('center_axis',(0.,0.,1.)) ;
#55914 = DIRECTION('ref_axis',(-0.809016994374946,-0.587785252292475,0.)) ;
#55915 = DIRECTION('center_axis',(0.,0.,1.)) ;
#55916 = DIRECTION('ref_axis',(0.641038992283213,0.76750831290125,0.)) ;
#55917 = DIRECTION('',(0.,0.,1.)) ;
#55918 = DIRECTION('center_axis',(0.,0.,-1.)) ;
#55919 = DIRECTION('ref_axis',(-0.969741506149309,0.244134002652785,0.)) ;
#55920 = DIRECTION('',(0.,0.,-1.)) ;
#55921 = DIRECTION('center_axis',(0.,0.,-1.)) ;
#55922 = DIRECTION('ref_axis',(-1.,0.,0.)) ;
#55923 = DIRECTION('center_axis',(-5.06597495053093E-16,9.94253565853781E-16,
1.)) ;
#55924 = DIRECTION('ref_axis',(0.891006524188366,0.453990499739551,6.90961123949975E-31)) ;
#55925 = DIRECTION('center_axis',(0.,0.,-1.)) ;
#55926 = DIRECTION('ref_axis',(0.969741506149316,-0.244134002652757,0.)) ;
#55927 = DIRECTION('',(0.,0.,-1.)) ;
#55928 = DIRECTION('center_axis',(0.,0.,1.)) ;
#55929 = DIRECTION('ref_axis',(1.,0.,0.)) ;
#55930 = DIRECTION('center_axis',(0.,0.,1.)) ;
#55931 = DIRECTION('ref_axis',(0.951056516295154,0.309016994374947,0.)) ;
#55932 = DIRECTION('center_axis',(0.,0.,1.)) ;
#55933 = DIRECTION('ref_axis',(-0.641038992283066,-0.767508312901373,0.)) ;
#55934 = DIRECTION('',(0.,0.,1.)) ;
#55935 = DIRECTION('center_axis',(0.,0.,1.)) ;
#55936 = DIRECTION('ref_axis',(1.,0.,0.)) ;
#55937 = DIRECTION('center_axis',(0.,0.,1.)) ;
#55938 = DIRECTION('ref_axis',(-0.951056516295152,-0.309016994374953,0.)) ;
#55939 = DIRECTION('center_axis',(0.,0.,1.)) ;
#55940 = DIRECTION('ref_axis',(0.37249119879961,0.928035724967972,0.)) ;
#55941 = DIRECTION('',(0.,0.,1.)) ;
#55942 = DIRECTION('center_axis',(0.,0.,-1.)) ;
#55943 = DIRECTION('ref_axis',(-0.846837422820716,0.531851839622999,0.)) ;
#55944 = DIRECTION('',(0.,0.,-1.)) ;
#55945 = DIRECTION('center_axis',(0.,0.,-1.)) ;
#55946 = DIRECTION('ref_axis',(-1.,0.,0.)) ;
#55947 = DIRECTION('center_axis',(0.,0.,1.)) ;
#55948 = DIRECTION('ref_axis',(0.707106781186546,0.707106781186549,0.)) ;
#55949 = DIRECTION('center_axis',(0.,0.,-1.)) ;
#55950 = DIRECTION('ref_axis',(0.99772053426966,0.0674813714788348,0.)) ;
#55951 = DIRECTION('',(0.,0.,-1.)) ;
#55952 = DIRECTION('center_axis',(0.,0.,1.)) ;
#55953 = DIRECTION('ref_axis',(1.,0.,0.)) ;
#55954 = DIRECTION('center_axis',(0.,0.,1.)) ;
#55955 = DIRECTION('ref_axis',(0.809016994374945,0.587785252292477,0.)) ;
#55956 = DIRECTION('center_axis',(0.,0.,1.)) ;
#55957 = DIRECTION('ref_axis',(-0.846837422820716,-0.531851839622999,0.)) ;
#55958 = DIRECTION('',(0.,0.,1.)) ;
#55959 = DIRECTION('center_axis',(0.,0.,1.)) ;
#55960 = DIRECTION('ref_axis',(-1.,0.,0.)) ;
#55961 = DIRECTION('center_axis',(0.,0.,1.)) ;
#55962 = DIRECTION('ref_axis',(-1.,-5.9211894646675E-15,0.)) ;
#55963 = DIRECTION('center_axis',(0.,0.,1.)) ;
#55964 = DIRECTION('ref_axis',(0.0674813714788309,0.99772053426966,0.)) ;
#55965 = DIRECTION('',(0.,0.,1.)) ;
#55966 = DIRECTION('center_axis',(0.,0.,-1.)) ;
#55967 = DIRECTION('ref_axis',(-0.641038992283134,0.767508312901316,0.)) ;
#55968 = DIRECTION('',(0.,0.,-1.)) ;
#55969 = DIRECTION('center_axis',(0.,0.,-1.)) ;
#55970 = DIRECTION('ref_axis',(-1.,0.,0.)) ;
#55971 = DIRECTION('center_axis',(9.94253565853781E-16,-5.06597495053088E-16,
1.)) ;
#55972 = DIRECTION('ref_axis',(0.453990499739548,0.891006524188367,-3.14592610423102E-31)) ;
#55973 = DIRECTION('center_axis',(0.,0.,-1.)) ;
#55974 = DIRECTION('ref_axis',(0.928035724967976,0.3724911987996,0.)) ;
#55975 = DIRECTION('',(0.,0.,-1.)) ;
#55976 = DIRECTION('center_axis',(0.,0.,1.)) ;
#55977 = DIRECTION('ref_axis',(1.,0.,0.)) ;
#55978 = DIRECTION('center_axis',(0.,0.,1.)) ;
#55979 = DIRECTION('ref_axis',(0.587785252292479,0.809016994374943,0.)) ;
#55980 = DIRECTION('center_axis',(0.,0.,1.)) ;
#55981 = DIRECTION('ref_axis',(-0.96974150614937,-0.24413400265254,0.)) ;
#55982 = DIRECTION('',(0.,0.,1.)) ;
#55983 = DIRECTION('center_axis',(0.,0.,1.)) ;
#55984 = DIRECTION('ref_axis',(1.,0.,0.)) ;
#55985 = DIRECTION('center_axis',(0.,0.,1.)) ;
#55986 = DIRECTION('ref_axis',(-0.95105651629515,0.309016994374958,0.)) ;
#55987 = DIRECTION('center_axis',(0.,0.,1.)) ;
#55988 = DIRECTION('ref_axis',(-0.244134002652526,0.969741506149374,0.)) ;
#55989 = DIRECTION('',(0.,0.,1.)) ;
#55990 = DIRECTION('center_axis',(0.,0.,-1.)) ;
#55991 = DIRECTION('ref_axis',(-0.37249119879956,0.928035724967992,0.)) ;
#55992 = DIRECTION('',(0.,0.,-1.)) ;
#55993 = DIRECTION('center_axis',(0.,0.,-1.)) ;
#55994 = DIRECTION('ref_axis',(-1.,0.,0.)) ;
#55995 = DIRECTION('center_axis',(2.57165665851294E-15,-4.0731040056544E-16,
1.)) ;
#55996 = DIRECTION('ref_axis',(0.156434465040232,0.987688340595138,-1.98479792514679E-30)) ;
#55997 = DIRECTION('center_axis',(0.,0.,-1.)) ;
#55998 = DIRECTION('ref_axis',(0.767508312901183,0.641038992283292,0.)) ;
#55999 = DIRECTION('',(0.,0.,-1.)) ;
#56000 = DIRECTION('center_axis',(0.,0.,1.)) ;
#56001 = DIRECTION('ref_axis',(1.,0.,0.)) ;
#56002 = DIRECTION('center_axis',(0.,0.,1.)) ;
#56003 = DIRECTION('ref_axis',(0.30901699437495,0.951056516295153,0.)) ;
#56004 = DIRECTION('center_axis',(0.,0.,1.)) ;
#56005 = DIRECTION('ref_axis',(-0.99772053426966,0.0674813714788309,0.)) ;
#56006 = DIRECTION('',(0.,0.,1.)) ;
#56007 = DIRECTION('center_axis',(0.,0.,1.)) ;
#56008 = DIRECTION('ref_axis',(1.,0.,0.)) ;
#56009 = DIRECTION('center_axis',(0.,0.,1.)) ;
#56010 = DIRECTION('ref_axis',(-0.809016994374941,0.587785252292481,0.)) ;
#56011 = DIRECTION('center_axis',(0.,0.,1.)) ;
#56012 = DIRECTION('ref_axis',(-0.531851839622895,0.846837422820781,0.)) ;
#56013 = DIRECTION('',(0.,0.,1.)) ;
#56014 = DIRECTION('center_axis',(0.,0.,-1.)) ;
#56015 = DIRECTION('ref_axis',(-0.0674813714788309,0.99772053426966,0.)) ;
#56016 = DIRECTION('',(0.,0.,-1.)) ;
#56017 = DIRECTION('center_axis',(0.,0.,-1.)) ;
#56018 = DIRECTION('ref_axis',(-1.,0.,0.)) ;
#56019 = DIRECTION('center_axis',(-1.83689761322353E-16,-2.90936000403874E-17,
1.)) ;
#56020 = DIRECTION('ref_axis',(-0.156434465040225,0.987688340595139,-9.33979109190074E-33)) ;
#56021 = DIRECTION('center_axis',(0.,0.,-1.)) ;
#56022 = DIRECTION('ref_axis',(0.531851839622895,0.846837422820781,0.)) ;
#56023 = DIRECTION('',(0.,0.,-1.)) ;
#56024 = DIRECTION('center_axis',(0.,0.,1.)) ;
#56025 = DIRECTION('ref_axis',(1.,0.,0.)) ;
#56026 = DIRECTION('center_axis',(0.,0.,1.)) ;
#56027 = DIRECTION('ref_axis',(4.44089209850062E-15,1.,0.)) ;
#56028 = DIRECTION('center_axis',(0.,0.,1.)) ;
#56029 = DIRECTION('ref_axis',(-0.928035724967976,0.3724911987996,0.)) ;
#56030 = DIRECTION('',(0.,0.,1.)) ;
#56031 = DIRECTION('center_axis',(0.,0.,1.)) ;
#56032 = DIRECTION('ref_axis',(1.,0.,0.)) ;
#56033 = DIRECTION('center_axis',(0.,0.,1.)) ;
#56034 = DIRECTION('ref_axis',(-0.587785252292473,0.809016994374948,0.)) ;
#56035 = DIRECTION('center_axis',(0.,0.,1.)) ;
#56036 = DIRECTION('ref_axis',(-0.767508312901273,0.641038992283185,0.)) ;
#56037 = DIRECTION('',(0.,0.,1.)) ;
#56038 = DIRECTION('center_axis',(0.,0.,-1.)) ;
#56039 = DIRECTION('ref_axis',(0.244134002652635,0.969741506149347,0.)) ;
#56040 = DIRECTION('',(0.,0.,-1.)) ;
#56041 = DIRECTION('center_axis',(0.,0.,1.)) ;
#56042 = DIRECTION('ref_axis',(1.,0.,0.)) ;
#56043 = DIRECTION('center_axis',(0.,0.,1.)) ;
#56044 = DIRECTION('ref_axis',(-0.309016994374939,0.951056516295156,0.)) ;
#56045 = DIRECTION('center_axis',(0.,0.,-1.)) ;
#56046 = DIRECTION('ref_axis',(-0.809016994374947,-0.587785252292473,0.)) ;
#56047 = DIRECTION('center_axis',(0.,0.,-1.)) ;
#56048 = DIRECTION('ref_axis',(-0.809016994374947,-0.587785252292473,0.)) ;
#56049 = DIRECTION('center_axis',(0.,0.,-1.)) ;
#56050 = DIRECTION('ref_axis',(-0.587785252292473,-0.809016994374948,0.)) ;
#56051 = DIRECTION('center_axis',(0.,0.,-1.)) ;
#56052 = DIRECTION('ref_axis',(-0.587785252292473,-0.809016994374948,0.)) ;
#56053 = DIRECTION('center_axis',(0.,0.,-1.)) ;
#56054 = DIRECTION('ref_axis',(-0.309016994374947,-0.951056516295154,0.)) ;
#56055 = DIRECTION('center_axis',(0.,0.,-1.)) ;
#56056 = DIRECTION('ref_axis',(-0.309016994374947,-0.951056516295154,0.)) ;
#56057 = DIRECTION('center_axis',(0.,0.,-1.)) ;
#56058 = DIRECTION('ref_axis',(0.,-1.,0.)) ;
#56059 = DIRECTION('center_axis',(0.,0.,-1.)) ;
#56060 = DIRECTION('ref_axis',(0.,-1.,0.)) ;
#56061 = DIRECTION('center_axis',(0.,0.,-1.)) ;
#56062 = DIRECTION('ref_axis',(0.309016994374947,-0.951056516295154,0.)) ;
#56063 = DIRECTION('center_axis',(0.,0.,-1.)) ;
#56064 = DIRECTION('ref_axis',(0.309016994374947,-0.951056516295154,0.)) ;
#56065 = DIRECTION('center_axis',(0.,0.,-1.)) ;
#56066 = DIRECTION('ref_axis',(0.587785252292473,-0.809016994374947,0.)) ;
#56067 = DIRECTION('center_axis',(0.,0.,-1.)) ;
#56068 = DIRECTION('ref_axis',(0.587785252292473,-0.809016994374947,0.)) ;
#56069 = DIRECTION('center_axis',(0.,0.,-1.)) ;
#56070 = DIRECTION('ref_axis',(0.809016994374947,-0.587785252292473,0.)) ;
#56071 = DIRECTION('center_axis',(0.,0.,-1.)) ;
#56072 = DIRECTION('ref_axis',(0.809016994374947,-0.587785252292473,0.)) ;
#56073 = DIRECTION('center_axis',(0.,0.,-1.)) ;
#56074 = DIRECTION('ref_axis',(0.951056516295154,-0.309016994374947,0.)) ;
#56075 = DIRECTION('center_axis',(0.,0.,-1.)) ;
#56076 = DIRECTION('ref_axis',(0.951056516295154,-0.309016994374947,0.)) ;
#56077 = DIRECTION('center_axis',(0.,0.,-1.)) ;
#56078 = DIRECTION('ref_axis',(1.,0.,0.)) ;
#56079 = DIRECTION('center_axis',(0.,0.,-1.)) ;
#56080 = DIRECTION('ref_axis',(1.,0.,0.)) ;
#56081 = DIRECTION('center_axis',(0.,0.,-1.)) ;
#56082 = DIRECTION('ref_axis',(0.951056516295154,0.309016994374948,0.)) ;
#56083 = DIRECTION('center_axis',(0.,0.,-1.)) ;
#56084 = DIRECTION('ref_axis',(0.951056516295154,0.309016994374948,0.)) ;
#56085 = DIRECTION('center_axis',(0.,0.,-1.)) ;
#56086 = DIRECTION('ref_axis',(0.809016994374947,0.587785252292473,0.)) ;
#56087 = DIRECTION('center_axis',(0.,0.,-1.)) ;
#56088 = DIRECTION('ref_axis',(0.809016994374947,0.587785252292473,0.)) ;
#56089 = DIRECTION('center_axis',(0.,0.,-1.)) ;
#56090 = DIRECTION('ref_axis',(0.587785252292473,0.809016994374947,0.)) ;
#56091 = DIRECTION('center_axis',(0.,0.,-1.)) ;
#56092 = DIRECTION('ref_axis',(0.587785252292473,0.809016994374947,0.)) ;
#56093 = DIRECTION('center_axis',(0.,0.,-1.)) ;
#56094 = DIRECTION('ref_axis',(0.309016994374947,0.951056516295154,0.)) ;
#56095 = DIRECTION('center_axis',(0.,0.,-1.)) ;
#56096 = DIRECTION('ref_axis',(0.309016994374947,0.951056516295154,0.)) ;
#56097 = DIRECTION('center_axis',(0.,0.,-1.)) ;
#56098 = DIRECTION('ref_axis',(-1.73472347597682E-16,1.,0.)) ;
#56099 = DIRECTION('center_axis',(0.,0.,-1.)) ;
#56100 = DIRECTION('ref_axis',(-1.73472347597682E-16,1.,0.)) ;
#56101 = DIRECTION('center_axis',(0.,0.,-1.)) ;
#56102 = DIRECTION('ref_axis',(-0.309016994374948,0.951056516295154,0.)) ;
#56103 = DIRECTION('center_axis',(0.,0.,-1.)) ;
#56104 = DIRECTION('ref_axis',(-0.309016994374948,0.951056516295154,0.)) ;
#56105 = DIRECTION('center_axis',(0.,0.,-1.)) ;
#56106 = DIRECTION('ref_axis',(-0.587785252292473,0.809016994374947,0.)) ;
#56107 = DIRECTION('center_axis',(0.,0.,-1.)) ;
#56108 = DIRECTION('ref_axis',(-0.587785252292473,0.809016994374947,0.)) ;
#56109 = DIRECTION('center_axis',(0.,0.,-1.)) ;
#56110 = DIRECTION('ref_axis',(-0.809016994374948,0.587785252292473,0.)) ;
#56111 = DIRECTION('center_axis',(0.,0.,-1.)) ;
#56112 = DIRECTION('ref_axis',(-0.809016994374948,0.587785252292473,0.)) ;
#56113 = DIRECTION('center_axis',(0.,0.,-1.)) ;
#56114 = DIRECTION('ref_axis',(-0.951056516295154,0.309016994374947,0.)) ;
#56115 = DIRECTION('center_axis',(0.,0.,-1.)) ;
#56116 = DIRECTION('ref_axis',(-0.951056516295154,0.309016994374947,0.)) ;
#56117 = DIRECTION('center_axis',(0.,0.,-1.)) ;
#56118 = DIRECTION('ref_axis',(-1.,-5.78241158658939E-17,0.)) ;
#56119 = DIRECTION('center_axis',(0.,0.,-1.)) ;
#56120 = DIRECTION('ref_axis',(-1.,-5.78241158658939E-17,0.)) ;
#56121 = DIRECTION('center_axis',(0.,0.,-1.)) ;
#56122 = DIRECTION('ref_axis',(-0.951056516295154,-0.309016994374947,0.)) ;
#56123 = DIRECTION('center_axis',(0.,0.,-1.)) ;
#56124 = DIRECTION('ref_axis',(-0.951056516295154,-0.309016994374947,0.)) ;
#56125 = DIRECTION('center_axis',(0.,0.,1.)) ;
#56126 = DIRECTION('ref_axis',(1.,0.,0.)) ;
#56127 = DIRECTION('',(0.52999894000318,6.49061505426385E-17,-0.847998304005088)) ;
#56128 = DIRECTION('center_axis',(0.,-1.67304619266744E-15,-1.)) ;
#56129 = DIRECTION('ref_axis',(1.,0.,0.)) ;
#56130 = DIRECTION('center_axis',(0.,0.,-1.)) ;
#56131 = DIRECTION('ref_axis',(-1.,0.,0.)) ;
#56132 = DIRECTION('center_axis',(0.,-1.,0.)) ;
#56133 = DIRECTION('ref_axis',(-1.,0.,0.)) ;
#56134 = DIRECTION('center_axis',(0.,0.,1.)) ;
#56135 = DIRECTION('ref_axis',(-0.707106781186564,-0.707106781186531,0.)) ;
#56136 = DIRECTION('center_axis',(-1.,0.,0.)) ;
#56137 = DIRECTION('ref_axis',(0.,0.,-1.)) ;
#56138 = DIRECTION('center_axis',(0.,0.,-1.)) ;
#56139 = DIRECTION('ref_axis',(1.,0.,0.)) ;
#56140 = DIRECTION('center_axis',(0.,0.,1.)) ;
#56141 = DIRECTION('ref_axis',(1.,0.,0.)) ;
#56142 = DIRECTION('',(1.26882631385732E-15,-1.,0.)) ;
#56143 = DIRECTION('center_axis',(0.,0.,-1.)) ;
#56144 = DIRECTION('ref_axis',(0.707106781186548,0.707106781186548,0.)) ;
#56145 = DIRECTION('',(1.,0.,0.)) ;
#56146 = DIRECTION('center_axis',(0.,0.,-1.)) ;
#56147 = DIRECTION('ref_axis',(-0.707106781186548,0.707106781186548,0.)) ;
#56148 = DIRECTION('',(0.,1.,0.)) ;
#56149 = DIRECTION('center_axis',(0.,0.,1.)) ;
#56150 = DIRECTION('ref_axis',(0.707106781186564,-0.707106781186531,0.)) ;
#56151 = DIRECTION('',(1.,0.,0.)) ;
#56152 = DIRECTION('center_axis',(0.,0.,-1.)) ;
#56153 = DIRECTION('ref_axis',(-0.707106781186548,0.707106781186548,0.)) ;
#56154 = DIRECTION('',(7.40148683083432E-15,1.,0.)) ;
#56155 = DIRECTION('center_axis',(0.,0.,-1.)) ;
#56156 = DIRECTION('ref_axis',(-0.707106781186548,-0.707106781186548,0.)) ;
#56157 = DIRECTION('',(-1.,0.,0.)) ;
#56158 = DIRECTION('center_axis',(0.,0.,1.)) ;
#56159 = DIRECTION('ref_axis',(0.707106781186531,0.707106781186564,0.)) ;
#56160 = DIRECTION('',(0.,1.,0.)) ;
#56161 = DIRECTION('center_axis',(0.,0.,-1.)) ;
#56162 = DIRECTION('ref_axis',(-0.707106781186548,-0.707106781186548,0.)) ;
#56163 = DIRECTION('',(-1.,-2.96059473233375E-14,0.)) ;
#56164 = DIRECTION('center_axis',(0.,0.,-1.)) ;
#56165 = DIRECTION('ref_axis',(0.70710678118661,-0.707106781186485,0.)) ;
#56166 = DIRECTION('',(1.26882631385732E-15,-1.,0.)) ;
#56167 = DIRECTION('center_axis',(0.,0.,1.)) ;
#56168 = DIRECTION('ref_axis',(-0.707106781186539,0.707106781186556,0.)) ;
#56169 = DIRECTION('',(-1.,0.,0.)) ;
#56170 = DIRECTION('center_axis',(0.,0.,-1.)) ;
#56171 = DIRECTION('ref_axis',(0.707106781186548,-0.707106781186548,0.)) ;
#56172 = DIRECTION('',(0.,-1.,0.)) ;
#56173 = DIRECTION('center_axis',(0.,0.,-1.)) ;
#56174 = DIRECTION('ref_axis',(0.707106781186548,0.707106781186548,0.)) ;
#56175 = DIRECTION('',(1.,0.,0.)) ;
#56176 = DIRECTION('center_axis',(-1.26882631385732E-15,1.,0.)) ;
#56177 = DIRECTION('ref_axis',(-0.70710678118654,-8.97195690676432E-16,-0.707106781186555)) ;
#56178 = DIRECTION('',(-1.26882631385732E-15,1.,0.)) ;
#56179 = DIRECTION('center_axis',(0.,-1.,0.)) ;
#56180 = DIRECTION('ref_axis',(-1.,0.,0.)) ;
#56181 = DIRECTION('center_axis',(1.,1.26882631385732E-15,0.)) ;
#56182 = DIRECTION('ref_axis',(1.26882631385732E-15,-1.,0.)) ;
#56183 = DIRECTION('',(0.,0.,1.)) ;
#56184 = DIRECTION('center_axis',(0.,0.,-1.)) ;
#56185 = DIRECTION('ref_axis',(-1.,0.,0.)) ;
#56186 = DIRECTION('center_axis',(-1.,0.,0.)) ;
#56187 = DIRECTION('ref_axis',(0.,1.,0.)) ;
#56188 = DIRECTION('center_axis',(0.,1.,0.)) ;
#56189 = DIRECTION('ref_axis',(-4.44089209850062E-14,0.,-1.)) ;
#56190 = DIRECTION('center_axis',(1.,0.,0.)) ;
#56191 = DIRECTION('ref_axis',(0.,0.707106781186602,-0.707106781186493)) ;
#56192 = DIRECTION('center_axis',(-1.,0.,0.)) ;
#56193 = DIRECTION('ref_axis',(0.,1.,0.)) ;
#56194 = DIRECTION('center_axis',(0.,0.,-1.)) ;
#56195 = DIRECTION('ref_axis',(-1.,0.,0.)) ;
#56196 = DIRECTION('center_axis',(1.,0.,0.)) ;
#56197 = DIRECTION('ref_axis',(0.,-1.,0.)) ;
#56198 = DIRECTION('center_axis',(0.,-1.,0.)) ;
#56199 = DIRECTION('ref_axis',(4.44089209850062E-14,0.,-1.)) ;
#56200 = DIRECTION('center_axis',(0.,0.,-1.)) ;
#56201 = DIRECTION('ref_axis',(0.707106781186564,-0.707106781186531,0.)) ;
#56202 = DIRECTION('center_axis',(0.,0.,-1.)) ;
#56203 = DIRECTION('ref_axis',(0.707106781186548,-0.707106781186548,0.)) ;
#56204 = DIRECTION('',(0.,0.,-1.)) ;
#56205 = DIRECTION('',(0.,0.,1.)) ;
#56206 = DIRECTION('center_axis',(-1.,0.,0.)) ;
#56207 = DIRECTION('ref_axis',(0.,-0.707106781186477,-0.707106781186618)) ;
#56208 = DIRECTION('',(-1.,0.,0.)) ;
#56209 = DIRECTION('center_axis',(1.,0.,0.)) ;
#56210 = DIRECTION('ref_axis',(0.,-1.,0.)) ;
#56211 = DIRECTION('center_axis',(0.,1.,0.)) ;
#56212 = DIRECTION('ref_axis',(1.,0.,0.)) ;
#56213 = DIRECTION('',(0.,0.,1.)) ;
#56214 = DIRECTION('center_axis',(0.,0.,-1.)) ;
#56215 = DIRECTION('ref_axis',(-1.,0.,0.)) ;
#56216 = DIRECTION('center_axis',(0.,1.,0.)) ;
#56217 = DIRECTION('ref_axis',(1.,0.,0.)) ;
#56218 = DIRECTION('center_axis',(1.,0.,0.)) ;
#56219 = DIRECTION('ref_axis',(0.,0.,-1.)) ;
#56220 = DIRECTION('center_axis',(0.,0.,-1.)) ;
#56221 = DIRECTION('ref_axis',(0.707106781186531,0.707106781186564,0.)) ;
#56222 = DIRECTION('center_axis',(0.,0.,-1.)) ;
#56223 = DIRECTION('ref_axis',(0.707106781186548,0.707106781186548,0.)) ;
#56224 = DIRECTION('',(0.,0.,1.)) ;
#56225 = DIRECTION('center_axis',(0.,-1.,0.)) ;
#56226 = DIRECTION('ref_axis',(0.70710678118654,0.,-0.707106781186555)) ;
#56227 = DIRECTION('center_axis',(0.,1.,0.)) ;
#56228 = DIRECTION('ref_axis',(1.,0.,0.)) ;
#56229 = DIRECTION('center_axis',(0.,0.,1.)) ;
#56230 = DIRECTION('ref_axis',(1.,0.,0.)) ;
#56231 = DIRECTION('center_axis',(0.,-1.,0.)) ;
#56232 = DIRECTION('ref_axis',(-1.,0.,0.)) ;
#56233 = DIRECTION('center_axis',(0.,0.,-1.)) ;
#56234 = DIRECTION('ref_axis',(-1.,0.,0.)) ;
#56235 = DIRECTION('center_axis',(0.,1.,0.)) ;
#56236 = DIRECTION('ref_axis',(0.,0.,-1.)) ;
#56237 = DIRECTION('center_axis',(0.,0.,-1.)) ;
#56238 = DIRECTION('ref_axis',(-1.,0.,0.)) ;
#56239 = DIRECTION('center_axis',(0.,-1.,0.)) ;
#56240 = DIRECTION('ref_axis',(-1.,0.,0.)) ;
#56241 = DIRECTION('center_axis',(-1.,0.,0.)) ;
#56242 = DIRECTION('ref_axis',(0.,0.,-1.)) ;
#56243 = DIRECTION('center_axis',(0.,1.,0.)) ;
#56244 = DIRECTION('ref_axis',(-0.70710678118654,0.,-0.707106781186555)) ;
#56245 = DIRECTION('center_axis',(0.,0.,1.)) ;
#56246 = DIRECTION('ref_axis',(1.,0.,0.)) ;
#56247 = DIRECTION('center_axis',(0.,1.,0.)) ;
#56248 = DIRECTION('ref_axis',(0.,0.,-1.)) ;
#56249 = DIRECTION('center_axis',(-1.,-4.44089209850072E-14,0.)) ;
#56250 = DIRECTION('ref_axis',(-4.44089209850072E-14,1.,0.)) ;
#56251 = DIRECTION('center_axis',(-1.26882631385732E-15,1.,0.)) ;
#56252 = DIRECTION('ref_axis',(-0.70710678118654,-8.97195690676432E-16,-0.707106781186555)) ;
#56253 = DIRECTION('center_axis',(-1.,0.,0.)) ;
#56254 = DIRECTION('ref_axis',(0.,-0.707106781186477,-0.707106781186618)) ;
#56255 = DIRECTION('center_axis',(0.,0.,-1.)) ;
#56256 = DIRECTION('ref_axis',(-1.,0.,0.)) ;
#56257 = DIRECTION('center_axis',(1.,4.44089209850072E-14,0.)) ;
#56258 = DIRECTION('ref_axis',(0.,0.,-1.)) ;
#56259 = DIRECTION('center_axis',(0.,0.,-1.)) ;
#56260 = DIRECTION('ref_axis',(-1.,0.,0.)) ;
#56261 = DIRECTION('center_axis',(0.,0.,1.)) ;
#56262 = DIRECTION('ref_axis',(0.,1.,0.)) ;
#56263 = DIRECTION('center_axis',(-1.,0.,0.)) ;
#56264 = DIRECTION('ref_axis',(0.,0.,-1.)) ;
#56265 = DIRECTION('center_axis',(0.,0.,-1.)) ;
#56266 = DIRECTION('ref_axis',(0.70710678118661,0.707106781186485,0.)) ;
#56267 = DIRECTION('',(0.,0.,-1.)) ;
#56268 = DIRECTION('center_axis',(0.,0.,-1.)) ;
#56269 = DIRECTION('ref_axis',(-1.,0.,0.)) ;
#56270 = DIRECTION('center_axis',(1.,0.,0.)) ;
#56271 = DIRECTION('ref_axis',(0.,-1.,0.)) ;
#56272 = DIRECTION('center_axis',(0.,0.,1.)) ;
#56273 = DIRECTION('ref_axis',(-1.,0.,0.)) ;
#56274 = DIRECTION('center_axis',(0.,-1.,0.)) ;
#56275 = DIRECTION('ref_axis',(0.,0.,-1.)) ;
#56276 = DIRECTION('center_axis',(-1.,0.,0.)) ;
#56277 = DIRECTION('ref_axis',(0.,-0.707106781186477,-0.707106781186618)) ;
#56278 = DIRECTION('',(-1.,0.,0.)) ;
#56279 = DIRECTION('center_axis',(0.,0.,-1.)) ;
#56280 = DIRECTION('ref_axis',(-0.70710678118661,0.707106781186485,0.)) ;
#56281 = DIRECTION('',(0.,0.,-1.)) ;
#56282 = DIRECTION('',(0.,0.,1.)) ;
#56283 = DIRECTION('center_axis',(0.,0.,-1.)) ;
#56284 = DIRECTION('ref_axis',(-1.,0.,0.)) ;
#56285 = DIRECTION('center_axis',(0.,1.,0.)) ;
#56286 = DIRECTION('ref_axis',(1.,0.,0.)) ;
#56287 = DIRECTION('center_axis',(0.,0.,1.)) ;
#56288 = DIRECTION('ref_axis',(0.,-1.,0.)) ;
#56289 = DIRECTION('center_axis',(1.,0.,0.)) ;
#56290 = DIRECTION('ref_axis',(0.,0.,-1.)) ;
#56291 = DIRECTION('center_axis',(0.,-1.,0.)) ;
#56292 = DIRECTION('ref_axis',(0.70710678118654,0.,-0.707106781186555)) ;
#56293 = DIRECTION('',(0.,-1.,0.)) ;
#56294 = DIRECTION('center_axis',(0.,0.,-1.)) ;
#56295 = DIRECTION('ref_axis',(-1.,0.,0.)) ;
#56296 = DIRECTION('center_axis',(0.,0.,1.)) ;
#56297 = DIRECTION('ref_axis',(-1.,0.,0.)) ;
#56298 = DIRECTION('center_axis',(0.,-1.,0.)) ;
#56299 = DIRECTION('ref_axis',(0.,0.,-1.)) ;
#56300 = DIRECTION('center_axis',(0.,0.,-1.)) ;
#56301 = DIRECTION('ref_axis',(-0.70710678118661,0.707106781186485,0.)) ;
#56302 = DIRECTION('',(0.,0.,-1.)) ;
#56303 = DIRECTION('center_axis',(-7.40148683083432E-15,-1.,0.)) ;
#56304 = DIRECTION('ref_axis',(0.70710678118654,-5.23364152894582E-15,-0.707106781186555)) ;
#56305 = DIRECTION('',(-7.40148683083432E-15,-1.,0.)) ;
#56306 = DIRECTION('center_axis',(0.,0.,-1.)) ;
#56307 = DIRECTION('ref_axis',(-0.707106781186485,-0.70710678118661,0.)) ;
#56308 = DIRECTION('',(0.,0.,-1.)) ;
#56309 = DIRECTION('',(0.,0.,1.)) ;
#56310 = DIRECTION('center_axis',(1.,0.,0.)) ;
#56311 = DIRECTION('ref_axis',(0.,0.707106781186602,-0.707106781186493)) ;
#56312 = DIRECTION('',(1.,0.,0.)) ;
#56313 = DIRECTION('center_axis',(1.,2.96059473233375E-14,0.)) ;
#56314 = DIRECTION('ref_axis',(-2.09345661157853E-14,0.707106781186602,-0.707106781186493)) ;
#56315 = DIRECTION('center_axis',(0.,0.,-1.)) ;
#56316 = DIRECTION('ref_axis',(0.951056516295153,0.309016994374948,0.)) ;
#56317 = DIRECTION('center_axis',(0.,0.,-1.)) ;
#56318 = DIRECTION('ref_axis',(0.809016994374947,0.587785252292473,0.)) ;
#56319 = DIRECTION('center_axis',(0.,0.,-1.)) ;
#56320 = DIRECTION('ref_axis',(0.587785252292473,0.809016994374948,0.)) ;
#56321 = DIRECTION('center_axis',(0.,0.,-1.)) ;
#56322 = DIRECTION('ref_axis',(0.309016994374947,0.951056516295154,0.)) ;
#56323 = DIRECTION('center_axis',(0.,0.,-1.)) ;
#56324 = DIRECTION('ref_axis',(-2.22044604925031E-16,1.,0.)) ;
#56325 = DIRECTION('center_axis',(0.,0.,-1.)) ;
#56326 = DIRECTION('ref_axis',(-0.309016994374948,0.951056516295153,0.)) ;
#56327 = DIRECTION('center_axis',(0.,0.,-1.)) ;
#56328 = DIRECTION('ref_axis',(-0.587785252292473,0.809016994374947,0.)) ;
#56329 = DIRECTION('center_axis',(0.,0.,-1.)) ;
#56330 = DIRECTION('ref_axis',(-0.809016994374947,0.587785252292473,0.)) ;
#56331 = DIRECTION('center_axis',(0.,0.,-1.)) ;
#56332 = DIRECTION('ref_axis',(-0.951056516295154,0.309016994374947,0.)) ;
#56333 = DIRECTION('center_axis',(0.,0.,-1.)) ;
#56334 = DIRECTION('ref_axis',(-1.,-1.11022302462516E-16,0.)) ;
#56335 = DIRECTION('center_axis',(0.,0.,-1.)) ;
#56336 = DIRECTION('ref_axis',(-0.951056516295154,-0.309016994374948,0.)) ;
#56337 = DIRECTION('center_axis',(0.,0.,-1.)) ;
#56338 = DIRECTION('ref_axis',(-0.809016994374947,-0.587785252292473,0.)) ;
#56339 = DIRECTION('center_axis',(0.,0.,-1.)) ;
#56340 = DIRECTION('ref_axis',(-0.587785252292473,-0.809016994374947,0.)) ;
#56341 = DIRECTION('center_axis',(0.,0.,-1.)) ;
#56342 = DIRECTION('ref_axis',(-0.309016994374947,-0.951056516295154,0.)) ;
#56343 = DIRECTION('center_axis',(0.,0.,-1.)) ;
#56344 = DIRECTION('ref_axis',(5.55111512312578E-17,-1.,0.)) ;
#56345 = DIRECTION('center_axis',(0.,0.,-1.)) ;
#56346 = DIRECTION('ref_axis',(0.309016994374948,-0.951056516295154,0.)) ;
#56347 = DIRECTION('center_axis',(0.,0.,-1.)) ;
#56348 = DIRECTION('ref_axis',(0.587785252292473,-0.809016994374947,0.)) ;
#56349 = DIRECTION('center_axis',(0.,0.,-1.)) ;
#56350 = DIRECTION('ref_axis',(0.809016994374947,-0.587785252292473,0.)) ;
#56351 = DIRECTION('center_axis',(0.,0.,-1.)) ;
#56352 = DIRECTION('ref_axis',(0.951056516295154,-0.309016994374947,0.)) ;
#56353 = DIRECTION('center_axis',(0.,0.,-1.)) ;
#56354 = DIRECTION('ref_axis',(1.,0.,0.)) ;
#56355 = DIRECTION('center_axis',(-1.,0.,0.)) ;
#56356 = DIRECTION('ref_axis',(0.,1.,0.)) ;
#56357 = DIRECTION('center_axis',(-1.,7.40148683083432E-15,0.)) ;
#56358 = DIRECTION('ref_axis',(7.40148683083432E-15,1.,0.)) ;
#56359 = DIRECTION('center_axis',(0.,-1.,0.)) ;
#56360 = DIRECTION('ref_axis',(-1.,0.,0.)) ;
#56361 = DIRECTION('center_axis',(0.,1.,0.)) ;
#56362 = DIRECTION('ref_axis',(1.,0.,0.)) ;
#56363 = DIRECTION('axis',(0.,0.,1.)) ;
#56364 = DIRECTION('refdir',(1.,0.,0.)) ;
#56365 = DIRECTION('center_axis',(-0.587427618878729,0.654887367420063,-0.47544855512672)) ;
#56366 = DIRECTION('ref_axis',(-0.744407146074326,-0.667725992360247,-1.89646896053702E-16)) ;
#56367 = DIRECTION('center_axis',(-0.995319431851992,0.096639684280469,0.)) ;
#56368 = DIRECTION('ref_axis',(-0.096639684280469,-0.995319431851992,0.)) ;
#56369 = DIRECTION('center_axis',(0.,0.,-1.)) ;
#56370 = DIRECTION('ref_axis',(0.318773588672553,0.947830891649361,0.)) ;
#56371 = DIRECTION('center_axis',(0.947791521574129,-0.318890626441414,-5.85612796687415E-15)) ;
#56372 = DIRECTION('ref_axis',(1.99840144432528E-12,5.9211894646675E-12,1.)) ;
#56373 = DIRECTION('center_axis',(0.,0.,1.)) ;
#56374 = DIRECTION('ref_axis',(0.096762587722359,0.995307490988224,0.)) ;
#56375 = DIRECTION('center_axis',(-0.995319431851989,0.0966396842804928,-7.19611906216879E-49)) ;
#56376 = DIRECTION('ref_axis',(-0.0683345760864578,-0.703797119709225,0.707106781186606)) ;
#56377 = DIRECTION('center_axis',(-0.995319431851992,0.096639684280469,0.)) ;
#56378 = DIRECTION('ref_axis',(-0.096639684280469,-0.995319431851992,0.)) ;
#56379 = DIRECTION('',(0.995319431851989,-0.0966396842804928,7.19611906216879E-49)) ;
#56380 = DIRECTION('',(-0.995319431851989,0.0966396842804928,-7.19611906216879E-49)) ;
#56381 = DIRECTION('center_axis',(0.0966396842804928,0.995319431851989,0.)) ;
#56382 = DIRECTION('ref_axis',(-0.995319431851989,0.0966396842804928,-5.45822738711604E-33)) ;
#56383 = DIRECTION('',(0.,0.,1.)) ;
#56384 = DIRECTION('',(0.995319431851989,-0.0966396842804928,0.)) ;
#56385 = DIRECTION('',(0.,0.,-1.)) ;
#56386 = DIRECTION('',(0.,0.,-1.)) ;
#56387 = DIRECTION('center_axis',(-0.116360000472909,0.99320710342302,0.)) ;
#56388 = DIRECTION('ref_axis',(0.993207103423019,0.116360000472909,0.)) ;
#56389 = DIRECTION('center_axis',(0.,0.,1.)) ;
#56390 = DIRECTION('ref_axis',(-0.476528951337224,-0.879158778911662,0.)) ;
#56391 = DIRECTION('center_axis',(0.,0.,-1.)) ;
#56392 = DIRECTION('ref_axis',(0.505066256142945,0.863080573820167,0.)) ;
#56393 = DIRECTION('center_axis',(-0.0271755831899855,0.9996306756389,0.)) ;
#56394 = DIRECTION('ref_axis',(0.9996306756389,0.0271755831899855,0.)) ;
#56395 = DIRECTION('center_axis',(0.,0.,1.)) ;
#56396 = DIRECTION('ref_axis',(-0.509318332147653,-0.860578198967609,0.)) ;
#56397 = DIRECTION('center_axis',(-0.686781523075192,0.726863907181062,0.)) ;
#56398 = DIRECTION('ref_axis',(-0.726863907181062,-0.686781523075192,0.)) ;
#56399 = DIRECTION('center_axis',(0.515397663572033,-0.856951135353988,0.)) ;
#56400 = DIRECTION('ref_axis',(0.,0.,1.)) ;
#56401 = DIRECTION('center_axis',(1.,0.,0.)) ;
#56402 = DIRECTION('ref_axis',(0.,1.,0.)) ;
#56403 = DIRECTION('center_axis',(-1.,0.,-7.18398817372806E-49)) ;
#56404 = DIRECTION('ref_axis',(-5.07984675360707E-49,0.707106781186547,0.707106781186547)) ;
#56405 = DIRECTION('center_axis',(1.,0.,0.)) ;
#56406 = DIRECTION('ref_axis',(0.,1.,0.)) ;
#56407 = DIRECTION('',(1.,0.,7.18398817372806E-49)) ;
#56408 = DIRECTION('',(-1.,0.,-7.18398817372806E-49)) ;
#56409 = DIRECTION('center_axis',(0.,0.,-1.)) ;
#56410 = DIRECTION('ref_axis',(0.95026155010241,-0.311453024382434,0.)) ;
#56411 = DIRECTION('center_axis',(0.805994027221583,-0.591923667446348,0.)) ;
#56412 = DIRECTION('ref_axis',(0.591923667446348,0.805994027221583,0.)) ;
#56413 = DIRECTION('center_axis',(0.,0.,1.)) ;
#56414 = DIRECTION('ref_axis',(0.950261550112609,-0.311453024351316,0.)) ;
#56415 = DIRECTION('center_axis',(0.583094656822871,-0.81240422277621,0.)) ;
#56416 = DIRECTION('ref_axis',(0.81240422277621,0.583094656822871,0.)) ;
#56417 = DIRECTION('center_axis',(-1.,0.,0.)) ;
#56418 = DIRECTION('ref_axis',(0.,-1.,0.)) ;
#56419 = DIRECTION('center_axis',(1.,0.,7.18398817372806E-49)) ;
#56420 = DIRECTION('ref_axis',(-5.07984675360707E-49,-0.707106781186547,0.707106781186547)) ;
#56421 = DIRECTION('center_axis',(-1.,0.,0.)) ;
#56422 = DIRECTION('ref_axis',(0.,-1.,0.)) ;
#56423 = DIRECTION('',(-1.,0.,-7.18398817372806E-49)) ;
#56424 = DIRECTION('',(1.,0.,7.18398817372806E-49)) ;
#56425 = DIRECTION('center_axis',(0.,0.,-1.)) ;
#56426 = DIRECTION('ref_axis',(0.87045897764999,-0.49224096561393,0.)) ;
#56427 = DIRECTION('center_axis',(0.,0.,1.)) ;
#56428 = DIRECTION('ref_axis',(0.870458977657674,-0.492240965600342,0.)) ;
#56429 = DIRECTION('',(0.,0.,-1.)) ;
#56430 = DIRECTION('center_axis',(0.,0.,1.)) ;
#56431 = DIRECTION('ref_axis',(0.950261550099627,-0.311453024390925,0.)) ;
#56432 = DIRECTION('',(0.,0.,1.)) ;
#56433 = DIRECTION('center_axis',(0.,1.,0.)) ;
#56434 = DIRECTION('ref_axis',(-1.,0.,7.51759117411176E-34)) ;
#56435 = DIRECTION('',(0.,0.,1.)) ;
#56436 = DIRECTION('',(1.,0.,0.)) ;
#56437 = DIRECTION('',(0.,0.,-1.)) ;
#56438 = DIRECTION('',(0.,0.,1.)) ;
#56439 = DIRECTION('center_axis',(-7.18398817372806E-49,4.73470448533E-50,
1.)) ;
#56440 = DIRECTION('ref_axis',(-1.,-8.69145204082858E-115,-7.18398817372806E-49)) ;
#56441 = DIRECTION('',(0.,1.,-4.73470448533E-50)) ;
#56442 = DIRECTION('center_axis',(7.18398817372806E-49,-4.73470448533E-50,
-1.)) ;
#56443 = DIRECTION('ref_axis',(-0.988714441989024,-0.149812390016092,-7.03198111894656E-49)) ;
#56444 = DIRECTION('',(0.52991926423319,0.848048096156435,3.40540801481717E-49)) ;
#56445 = DIRECTION('',(0.,1.,-4.73470448533E-50)) ;
#56446 = DIRECTION('center_axis',(0.,0.,-1.)) ;
#56447 = DIRECTION('ref_axis',(-0.999999996867551,-7.91511064151848E-5,0.)) ;
#56448 = DIRECTION('center_axis',(0.,0.,-1.)) ;
#56449 = DIRECTION('ref_axis',(0.695780933920748,0.718254058110618,0.)) ;
#56450 = DIRECTION('center_axis',(0.,0.,-1.)) ;
#56451 = DIRECTION('ref_axis',(0.719657715388816,0.694329008958541,0.)) ;
#56452 = DIRECTION('center_axis',(0.,0.,-1.)) ;
#56453 = DIRECTION('ref_axis',(0.588307081130752,0.808637606280721,0.)) ;
#56454 = DIRECTION('center_axis',(0.,0.,-1.)) ;
#56455 = DIRECTION('ref_axis',(-0.864233277861794,-0.503091285390891,0.)) ;
#56456 = DIRECTION('center_axis',(0.,0.,-1.)) ;
#56457 = DIRECTION('ref_axis',(0.951152389067781,-0.308721772427299,0.)) ;
#56458 = DIRECTION('',(-1.,0.,-7.18398817372806E-49)) ;
#56459 = DIRECTION('center_axis',(0.,0.,1.)) ;
#56460 = DIRECTION('ref_axis',(-0.508512638759206,-0.86105452569634,0.)) ;
#56461 = DIRECTION('center_axis',(0.,0.,1.)) ;
#56462 = DIRECTION('ref_axis',(-0.575679505271721,-0.817675429012091,0.)) ;
#56463 = DIRECTION('center_axis',(0.,0.,1.)) ;
#56464 = DIRECTION('ref_axis',(-0.999001972402703,0.0446660848464377,0.)) ;
#56465 = DIRECTION('',(0.801695394071906,-0.597732795757345,6.04237904485494E-49)) ;
#56466 = DIRECTION('center_axis',(7.18398817372806E-49,-4.73470448533E-50,
-1.)) ;
#56467 = DIRECTION('ref_axis',(-0.564686561222103,0.825305451075634,-4.44745931978026E-49)) ;
#56468 = DIRECTION('',(1.,0.,7.18398817372806E-49)) ;
#56469 = DIRECTION('center_axis',(0.,0.,1.)) ;
#56470 = DIRECTION('ref_axis',(0.87103386621213,-0.491222967614045,0.)) ;
#56471 = DIRECTION('center_axis',(0.,0.,1.)) ;
#56472 = DIRECTION('ref_axis',(-0.557169735681217,-0.830398630563011,0.)) ;
#56473 = DIRECTION('',(-0.995319431851989,0.0966396842804928,-7.19611906216879E-49)) ;
#56474 = DIRECTION('center_axis',(0.,0.,-1.)) ;
#56475 = DIRECTION('ref_axis',(-0.686121032649195,0.727487407833567,0.)) ;
#56476 = DIRECTION('center_axis',(0.,0.,-1.)) ;
#56477 = DIRECTION('ref_axis',(0.559966405429213,0.828515313552312,0.)) ;
#56478 = DIRECTION('center_axis',(0.,0.,-1.)) ;
#56479 = DIRECTION('ref_axis',(0.502348696023835,0.864665130326852,0.)) ;
#56480 = DIRECTION('',(0.995319431851989,-0.0966396842804928,7.19611906216879E-49)) ;
#56481 = DIRECTION('center_axis',(0.,0.,1.)) ;
#56482 = DIRECTION('ref_axis',(0.710148456608062,0.704051965111374,0.)) ;
#56483 = DIRECTION('center_axis',(0.,0.,1.)) ;
#56484 = DIRECTION('ref_axis',(-0.980153473557896,-0.198240178249495,0.)) ;
#56485 = DIRECTION('',(0.,-1.,4.73470448533E-50)) ;
#56486 = DIRECTION('center_axis',(7.18398817372806E-49,-4.73470448533E-50,
-1.)) ;
#56487 = DIRECTION('ref_axis',(0.382998231470488,-0.923749075610081,3.1888226546038E-49)) ;
#56488 = DIRECTION('',(-0.992304006159154,0.123825519827269,-7.18732796940279E-49)) ;
#56489 = DIRECTION('center_axis',(-7.18398817372806E-49,4.73470448533E-50,
1.)) ;
#56490 = DIRECTION('ref_axis',(0.600000000000003,0.799999999999998,3.93161654541046E-49)) ;
#56491 = DIRECTION('center_axis',(-1.,0.,-7.18398817372806E-49)) ;
#56492 = DIRECTION('ref_axis',(-5.07984675360707E-49,0.707106781186547,0.707106781186547)) ;
#56493 = DIRECTION('center_axis',(-1.,0.,0.)) ;
#56494 = DIRECTION('ref_axis',(0.,0.,1.)) ;
#56495 = DIRECTION('',(-1.,0.,-7.18398817372806E-49)) ;
#56496 = DIRECTION('center_axis',(1.,0.,0.)) ;
#56497 = DIRECTION('ref_axis',(0.,1.,0.)) ;
#56498 = DIRECTION('center_axis',(0.,0.,-1.)) ;
#56499 = DIRECTION('ref_axis',(0.871033866206537,-0.491222967623962,0.)) ;
#56500 = DIRECTION('center_axis',(0.517399992172763,-0.855743681308617,0.)) ;
#56501 = DIRECTION('ref_axis',(0.855743681308617,0.517399992172763,0.)) ;
#56502 = DIRECTION('center_axis',(0.248948925328251,-0.968516614507933,0.)) ;
#56503 = DIRECTION('ref_axis',(0.968516614507933,0.248948925328251,0.)) ;
#56504 = DIRECTION('center_axis',(-0.995319431851992,0.096639684280469,0.)) ;
#56505 = DIRECTION('ref_axis',(-0.096639684280469,-0.995319431851992,0.)) ;
#56506 = DIRECTION('center_axis',(0.995319431851989,-0.0966396842804928,7.19611906216879E-49)) ;
#56507 = DIRECTION('ref_axis',(-0.0683345760864578,-0.703797119709225,0.707106781186606)) ;
#56508 = DIRECTION('center_axis',(-0.995319431851992,0.096639684280469,0.)) ;
#56509 = DIRECTION('ref_axis',(-0.096639684280469,-0.995319431851992,0.)) ;
#56510 = DIRECTION('',(0.995319431851989,-0.0966396842804928,7.19611906216879E-49)) ;
#56511 = DIRECTION('center_axis',(-0.164953742105299,0.986301304351494,0.)) ;
#56512 = DIRECTION('ref_axis',(-0.986301304351494,-0.164953742105299,0.)) ;
#56513 = DIRECTION('center_axis',(-0.45978265173531,0.888031482078899,0.)) ;
#56514 = DIRECTION('ref_axis',(-0.888031482078899,-0.45978265173531,0.)) ;
#56515 = DIRECTION('',(0.,0.,-1.)) ;
#56516 = DIRECTION('',(0.,0.,1.)) ;
#56517 = DIRECTION('',(0.,0.,1.)) ;
#56518 = DIRECTION('',(0.,0.,-1.)) ;
#56519 = DIRECTION('center_axis',(0.,0.,1.)) ;
#56520 = DIRECTION('ref_axis',(0.871033866207808,-0.491222967621709,0.)) ;
#56521 = DIRECTION('center_axis',(0.,1.,0.)) ;
#56522 = DIRECTION('ref_axis',(-1.,0.,0.)) ;
#56523 = DIRECTION('',(0.,0.,1.)) ;
#56524 = DIRECTION('',(1.,0.,0.)) ;
#56525 = DIRECTION('center_axis',(7.18398817372806E-49,-4.73470448533E-50,
-1.)) ;
#56526 = DIRECTION('ref_axis',(-1.,0.,0.)) ;
#56527 = DIRECTION('center_axis',(0.,-1.,4.73470448533E-50)) ;
#56528 = DIRECTION('ref_axis',(1.,0.,0.)) ;
#56529 = DIRECTION('center_axis',(7.18398817372806E-49,-4.73470448533E-50,
-1.)) ;
#56530 = DIRECTION('ref_axis',(0.600000000000003,0.799999999999998,3.93161654541046E-49)) ;
#56531 = DIRECTION('center_axis',(0.,0.,1.)) ;
#56532 = DIRECTION('ref_axis',(-1.,0.,0.)) ;
#56533 = DIRECTION('center_axis',(-1.09763027743844E-32,-3.07546720254364E-67,
1.)) ;
#56534 = DIRECTION('ref_axis',(-1.,1.74482680966927E-115,-1.09763027743844E-32)) ;
#56535 = DIRECTION('',(0.,0.,1.)) ;
#56536 = DIRECTION('center_axis',(0.,-1.,4.73470448533E-50)) ;
#56537 = DIRECTION('ref_axis',(-0.707106781186495,3.34794164849145E-50,0.7071067811866)) ;
#56538 = DIRECTION('center_axis',(-0.0703834704923706,-0.997519963951429,
0.000297657167785072)) ;
#56539 = DIRECTION('ref_axis',(0.997396008926277,-0.0703794229952271,-0.0157460533719646)) ;
#56540 = DIRECTION('',(0.,-1.,4.73470448533E-50)) ;
#56541 = DIRECTION('center_axis',(0.0703834704969201,-0.997519963951109,-0.000297657163792654)) ;
#56542 = DIRECTION('ref_axis',(0.997396008921092,0.0703794229994621,-0.0157460536814624)) ;
#56543 = DIRECTION('center_axis',(-7.18398817372806E-49,4.73470448533E-50,
1.)) ;
#56544 = DIRECTION('ref_axis',(1.,0.,0.)) ;
#56545 = DIRECTION('center_axis',(-7.18398817372806E-49,4.73470448533E-50,
1.)) ;
#56546 = DIRECTION('ref_axis',(-0.564686561222103,0.825305451075634,-4.44745931978026E-49)) ;
#56547 = DIRECTION('center_axis',(-0.801695394071906,0.597732795757345,-6.04237904485494E-49)) ;
#56548 = DIRECTION('ref_axis',(0.422660913217549,0.566884249594181,0.707106781186654)) ;
#56549 = DIRECTION('',(-0.801695394071906,0.597732795757345,-6.04237904485494E-49)) ;
#56550 = DIRECTION('center_axis',(0.0446052839668792,0.999004688999123,0.)) ;
#56551 = DIRECTION('ref_axis',(0.,0.,1.)) ;
#56552 = DIRECTION('center_axis',(0.,0.,-1.)) ;
#56553 = DIRECTION('ref_axis',(-0.996530462288612,0.083228827522952,0.)) ;
#56554 = DIRECTION('center_axis',(-0.0271755831899875,0.9996306756389,0.)) ;
#56555 = DIRECTION('ref_axis',(0.,0.,1.)) ;
#56556 = DIRECTION('center_axis',(0.,0.,-1.)) ;
#56557 = DIRECTION('ref_axis',(0.566808378068744,0.823849660163236,0.)) ;
#56558 = DIRECTION('center_axis',(-0.116360000473519,0.993207103422948,0.)) ;
#56559 = DIRECTION('ref_axis',(0.,0.,1.)) ;
#56560 = DIRECTION('center_axis',(0.,0.,-1.)) ;
#56561 = DIRECTION('ref_axis',(0.509318333459063,0.860578198191473,0.)) ;
#56562 = DIRECTION('center_axis',(-0.488003536614868,0.872841651304165,0.)) ;
#56563 = DIRECTION('ref_axis',(0.,0.,1.)) ;
#56564 = DIRECTION('center_axis',(-0.707983649981725,0.70622882365318,0.)) ;
#56565 = DIRECTION('ref_axis',(0.,0.,1.)) ;
#56566 = DIRECTION('center_axis',(1.,0.,0.)) ;
#56567 = DIRECTION('ref_axis',(0.,0.,1.)) ;
#56568 = DIRECTION('center_axis',(1.,0.,7.18398817372806E-49)) ;
#56569 = DIRECTION('ref_axis',(-5.07984675360707E-49,-0.707106781186547,0.707106781186547)) ;
#56570 = DIRECTION('center_axis',(1.,0.,0.)) ;
#56571 = DIRECTION('ref_axis',(0.,0.,1.)) ;
#56572 = DIRECTION('',(1.,0.,7.18398817372806E-49)) ;
#56573 = DIRECTION('center_axis',(0.809381734448945,-0.587282902816366,0.)) ;
#56574 = DIRECTION('ref_axis',(0.,0.,1.)) ;
#56575 = DIRECTION('center_axis',(0.,0.,1.)) ;
#56576 = DIRECTION('ref_axis',(0.95115238906757,-0.308721772427949,0.)) ;
#56577 = DIRECTION('center_axis',(0.548205483813554,-0.83634367787217,0.)) ;
#56578 = DIRECTION('ref_axis',(0.,0.,1.)) ;
#56579 = DIRECTION('center_axis',(0.503089999549594,-0.864234026380118,0.)) ;
#56580 = DIRECTION('ref_axis',(0.,0.,1.)) ;
#56581 = DIRECTION('center_axis',(0.,0.,1.)) ;
#56582 = DIRECTION('ref_axis',(-0.836344700122326,-0.548203924262949,0.)) ;
#56583 = DIRECTION('center_axis',(0.231127698080859,-0.972923423081099,0.)) ;
#56584 = DIRECTION('ref_axis',(0.,0.,1.)) ;
#56585 = DIRECTION('center_axis',(0.,0.,1.)) ;
#56586 = DIRECTION('ref_axis',(-0.588703310582201,-0.808349189465516,0.)) ;
#56587 = DIRECTION('center_axis',(0.199440361015477,-0.9799099664755,0.)) ;
#56588 = DIRECTION('ref_axis',(0.,0.,1.)) ;
#56589 = DIRECTION('center_axis',(0.,0.,1.)) ;
#56590 = DIRECTION('ref_axis',(0.731503731905511,0.681837436789965,0.)) ;
#56591 = DIRECTION('center_axis',(0.195410291837853,-0.980721580186673,0.)) ;
#56592 = DIRECTION('ref_axis',(0.,0.,1.)) ;
#56593 = DIRECTION('center_axis',(0.,0.,1.)) ;
#56594 = DIRECTION('ref_axis',(0.710838965198327,0.703354793511619,0.)) ;
#56595 = DIRECTION('center_axis',(0.,-1.,0.)) ;
#56596 = DIRECTION('ref_axis',(0.,0.,1.)) ;
#56597 = DIRECTION('center_axis',(0.,0.,1.)) ;
#56598 = DIRECTION('ref_axis',(-0.980737044055406,-0.195332666027636,0.)) ;
#56599 = DIRECTION('center_axis',(0.,-1.,4.73470448533E-50)) ;
#56600 = DIRECTION('ref_axis',(-0.707106781186495,3.34794164849145E-50,0.7071067811866)) ;
#56601 = DIRECTION('',(0.,-1.,4.73470448533E-50)) ;
#56602 = DIRECTION('center_axis',(-0.27563735581696,-0.96126169593833,0.)) ;
#56603 = DIRECTION('ref_axis',(-0.96126169593833,0.27563735581696,-1.7177296129898E-49)) ;
#56604 = DIRECTION('center_axis',(-0.52991926423319,-0.848048096156435,-3.40540801481717E-49)) ;
#56605 = DIRECTION('ref_axis',(-0.599660559564581,0.37470950522069,0.707106781186519)) ;
#56606 = DIRECTION('',(-0.52991926423319,-0.848048096156435,-3.40540801481717E-49)) ;
#56607 = DIRECTION('center_axis',(-7.18398817372806E-49,4.73470448533E-50,
1.)) ;
#56608 = DIRECTION('ref_axis',(1.,0.,0.)) ;
#56609 = DIRECTION('center_axis',(-7.18398817372806E-49,4.73470448533E-50,
1.)) ;
#56610 = DIRECTION('ref_axis',(-0.988714441989024,-0.149812390016092,-7.03198111894657E-49)) ;
#56611 = DIRECTION('',(0.,0.,-1.)) ;
#56612 = DIRECTION('',(0.,0.,-1.)) ;
#56613 = DIRECTION('center_axis',(0.,0.,-1.)) ;
#56614 = DIRECTION('ref_axis',(-0.850596491898227,-0.525818987837477,0.)) ;
#56615 = DIRECTION('',(0.,0.,1.)) ;
#56616 = DIRECTION('center_axis',(0.,0.,-1.)) ;
#56617 = DIRECTION('ref_axis',(-0.864233152292046,-0.5030915011003,0.)) ;
#56618 = DIRECTION('',(0.,0.,1.)) ;
#56619 = DIRECTION('center_axis',(0.,0.,-1.)) ;
#56620 = DIRECTION('ref_axis',(0.58870331058208,0.808349189465604,0.)) ;
#56621 = DIRECTION('',(0.,0.,1.)) ;
#56622 = DIRECTION('center_axis',(0.,0.,-1.)) ;
#56623 = DIRECTION('ref_axis',(-0.0605458183509709,0.99816541909656,0.)) ;
#56624 = DIRECTION('',(0.,0.,1.)) ;
#56625 = DIRECTION('',(-1.69617406539954E-14,0.,1.)) ;
#56626 = DIRECTION('center_axis',(0.,0.,-1.)) ;
#56627 = DIRECTION('ref_axis',(0.73297616972146,0.680254316135118,0.)) ;
#56628 = DIRECTION('',(0.,0.,1.)) ;
#56629 = DIRECTION('center_axis',(0.,0.,1.)) ;
#56630 = DIRECTION('ref_axis',(0.0630245162323191,-0.998011979063218,0.)) ;
#56631 = DIRECTION('',(0.,0.,-1.)) ;
#56632 = DIRECTION('center_axis',(-1.,0.,0.)) ;
#56633 = DIRECTION('ref_axis',(0.,-1.,0.)) ;
#56634 = DIRECTION('',(0.,0.,1.)) ;
#56635 = DIRECTION('',(0.,-1.,0.)) ;
#56636 = DIRECTION('center_axis',(-0.848048096156435,0.52991926423319,0.)) ;
#56637 = DIRECTION('ref_axis',(-0.52991926423319,-0.848048096156435,0.)) ;
#56638 = DIRECTION('',(0.,0.,1.)) ;
#56639 = DIRECTION('',(-0.52991926423319,-0.848048096156435,0.)) ;
#56640 = DIRECTION('center_axis',(0.,0.,1.)) ;
#56641 = DIRECTION('ref_axis',(-1.,0.,0.)) ;
#56642 = DIRECTION('',(0.,0.,1.)) ;
#56643 = DIRECTION('center_axis',(-1.09763027743844E-32,-3.07546720254364E-67,
1.)) ;
#56644 = DIRECTION('ref_axis',(-1.,1.74482680966927E-115,-1.09763027743844E-32)) ;
#56645 = DIRECTION('center_axis',(-1.,0.,0.)) ;
#56646 = DIRECTION('ref_axis',(0.,-1.,0.)) ;
#56647 = DIRECTION('',(0.,0.,1.)) ;
#56648 = DIRECTION('',(0.,-1.,0.)) ;
#56649 = DIRECTION('center_axis',(-7.18398817372806E-49,4.73470448533E-50,
1.)) ;
#56650 = DIRECTION('ref_axis',(1.,0.,0.)) ;
#56651 = DIRECTION('center_axis',(-7.18398817372806E-49,4.73470448533E-50,
1.)) ;
#56652 = DIRECTION('ref_axis',(0.382998231470488,-0.923749075610081,3.1888226546038E-49)) ;
#56653 = DIRECTION('center_axis',(0.995319431851992,-0.096639684280469,0.)) ;
#56654 = DIRECTION('ref_axis',(0.096639684280469,0.995319431851992,0.)) ;
#56655 = DIRECTION('center_axis',(-0.205129249961233,0.978734893017686,-3.0494635128401E-13)) ;
#56656 = DIRECTION('ref_axis',(-7.40148683083438E-14,2.96059473233375E-13,
1.)) ;
#56657 = DIRECTION('center_axis',(-0.823739491888484,0.435623967792083,0.362884290357663)) ;
#56658 = DIRECTION('ref_axis',(-0.566968473112313,-0.632911145682689,-0.527228823346485)) ;
#56659 = DIRECTION('center_axis',(-0.205129249960219,0.978734893017899,6.14991217244375E-10)) ;
#56660 = DIRECTION('ref_axis',(-0.978734893017899,-0.205129249960219,-7.97116905459272E-27)) ;
#56661 = DIRECTION('center_axis',(0.,0.,1.)) ;
#56662 = DIRECTION('ref_axis',(-0.096639684280469,-0.995319431851992,0.)) ;
#56663 = DIRECTION('center_axis',(0.995319431884589,-0.0966396839447406,0.)) ;
#56664 = DIRECTION('ref_axis',(0.,0.,-1.)) ;
#56665 = DIRECTION('',(0.,0.,-1.)) ;
#56666 = DIRECTION('',(0.,0.,1.)) ;
#56667 = DIRECTION('center_axis',(-0.103428412047358,0.99463690037187,0.)) ;
#56668 = DIRECTION('ref_axis',(-0.99463690037187,-0.103428412047358,0.)) ;
#56669 = DIRECTION('center_axis',(-0.995319431851992,0.096639684280469,0.)) ;
#56670 = DIRECTION('ref_axis',(0.,0.,1.)) ;
#56671 = DIRECTION('center_axis',(-0.369434341203981,-0.833228591457252,0.411398082053555)) ;
#56672 = DIRECTION('ref_axis',(0.556714224316335,-0.552928670244287,-0.619950931982319)) ;
#56673 = DIRECTION('center_axis',(-0.995319431851991,0.096639684280469,-2.15264418689913E-8)) ;
#56674 = DIRECTION('ref_axis',(-0.0966396842804691,-0.995319431851992,-1.81350378306141E-24)) ;
#56675 = DIRECTION('center_axis',(0.,0.,1.)) ;
#56676 = DIRECTION('ref_axis',(0.99463690037187,0.103428412047358,0.)) ;
#56677 = DIRECTION('center_axis',(0.,0.,1.)) ;
#56678 = DIRECTION('ref_axis',(0.99463690037187,0.103428412047358,0.)) ;
#56679 = DIRECTION('center_axis',(-0.103428467957002,0.994636894558043,0.)) ;
#56680 = DIRECTION('ref_axis',(0.,0.,-1.)) ;
#56681 = DIRECTION('',(0.,0.,-1.)) ;
#56682 = DIRECTION('',(0.,0.,1.)) ;
#56683 = DIRECTION('center_axis',(0.0757934708266429,0.997123537872841,0.)) ;
#56684 = DIRECTION('ref_axis',(0.997123537872841,-0.0757934708266429,0.)) ;
#56685 = DIRECTION('center_axis',(0.,0.,1.)) ;
#56686 = DIRECTION('ref_axis',(-0.556954524428844,-0.830542989687012,0.)) ;
#56687 = DIRECTION('center_axis',(0.0327072745977339,-0.999464973967767,0.)) ;
#56688 = DIRECTION('ref_axis',(0.,0.,-1.)) ;
#56689 = DIRECTION('center_axis',(0.,0.,-1.)) ;
#56690 = DIRECTION('ref_axis',(0.548199354674537,0.836347695360262,0.)) ;
#56691 = DIRECTION('center_axis',(0.,0.,-1.)) ;
#56692 = DIRECTION('ref_axis',(0.499475161905295,0.866328207228461,0.)) ;
#56693 = DIRECTION('center_axis',(0.,0.,1.)) ;
#56694 = DIRECTION('ref_axis',(-0.498945449405617,-0.866633393377746,0.)) ;
#56695 = DIRECTION('center_axis',(-0.995319431851989,0.0966396842804928,-1.09249274412357E-32)) ;
#56696 = DIRECTION('ref_axis',(-0.0683345760864603,-0.703797119709251,-0.70710678118658)) ;
#56697 = DIRECTION('',(0.995319431851989,-0.0966396842804928,1.09249274412357E-32)) ;
#56698 = DIRECTION('',(-0.995319431851989,0.0966396842804928,-1.09249274412357E-32)) ;
#56699 = DIRECTION('center_axis',(-0.995319431851989,0.0966396842804928,-7.19611906216879E-49)) ;
#56700 = DIRECTION('ref_axis',(0.0683345760864578,0.703797119709225,0.707106781186606)) ;
#56701 = DIRECTION('',(-0.995319431851989,0.0966396842804928,-7.19611906216879E-49)) ;
#56702 = DIRECTION('center_axis',(0.,0.,1.)) ;
#56703 = DIRECTION('ref_axis',(-0.543457078351713,-0.839436956530638,0.)) ;
#56704 = DIRECTION('center_axis',(0.0757934708213221,0.997123537873245,0.)) ;
#56705 = DIRECTION('ref_axis',(-0.997123537873245,0.0757934708213221,0.)) ;
#56706 = DIRECTION('center_axis',(-0.032707310967753,0.999464972777565,0.)) ;
#56707 = DIRECTION('ref_axis',(-0.999464972777565,-0.032707310967753,0.)) ;
#56708 = DIRECTION('center_axis',(0.,0.,1.)) ;
#56709 = DIRECTION('ref_axis',(-0.568977005763106,-0.822353431872726,0.)) ;
#56710 = DIRECTION('center_axis',(0.,0.,1.)) ;
#56711 = DIRECTION('ref_axis',(-0.501869373976784,-0.864943426741975,0.)) ;
#56712 = DIRECTION('center_axis',(0.,0.,-1.)) ;
#56713 = DIRECTION('ref_axis',(0.711895385472461,0.702285526081106,0.)) ;
#56714 = DIRECTION('center_axis',(-0.198321321731455,0.980137058449832,0.)) ;
#56715 = DIRECTION('ref_axis',(0.,0.,-1.)) ;
#56716 = DIRECTION('center_axis',(0.,0.,1.)) ;
#56717 = DIRECTION('ref_axis',(0.7258408460618,0.687862679746684,0.)) ;
#56718 = DIRECTION('center_axis',(-2.96059473233386E-13,1.,0.)) ;
#56719 = DIRECTION('ref_axis',(0.,0.,-1.)) ;
#56720 = DIRECTION('center_axis',(0.,0.,1.)) ;
#56721 = DIRECTION('ref_axis',(-0.980153473557867,-0.198240178249636,0.)) ;
#56722 = DIRECTION('center_axis',(0.,0.,-1.)) ;
#56723 = DIRECTION('ref_axis',(-0.99999999657314,-8.2787195019415E-5,0.)) ;
#56724 = DIRECTION('center_axis',(0.,1.,3.07546720254364E-67)) ;
#56725 = DIRECTION('ref_axis',(-0.707106781186574,2.17468371423535E-67,-0.707106781186521)) ;
#56726 = DIRECTION('',(0.,-1.,-3.07546720254364E-67)) ;
#56727 = DIRECTION('',(0.,1.,3.07546720254364E-67)) ;
#56728 = DIRECTION('center_axis',(0.992304006159154,-0.123825519827269,7.18732796940279E-49)) ;
#56729 = DIRECTION('ref_axis',(-0.087557864753804,-0.701664891753657,0.707106781186606)) ;
#56730 = DIRECTION('',(0.992304006159154,-0.123825519827269,7.18732796940279E-49)) ;
#56731 = DIRECTION('center_axis',(0.,0.,-1.)) ;
#56732 = DIRECTION('ref_axis',(0.695398896812718,0.718623944989071,0.)) ;
#56733 = DIRECTION('center_axis',(0.198321321723131,-0.980137058451516,0.)) ;
#56734 = DIRECTION('ref_axis',(0.980137058451516,0.198321321723131,0.)) ;
#56735 = DIRECTION('center_axis',(0.,0.,-1.)) ;
#56736 = DIRECTION('ref_axis',(-0.99999999657314,-8.27871951115587E-5,0.)) ;
#56737 = DIRECTION('center_axis',(2.96059473233364E-13,-1.,0.)) ;
#56738 = DIRECTION('ref_axis',(1.,2.96059473233364E-13,0.)) ;
#56739 = DIRECTION('center_axis',(0.,1.,-4.73470448533E-50)) ;
#56740 = DIRECTION('ref_axis',(0.707106781186547,3.34794164849121E-50,0.707106781186547)) ;
#56741 = DIRECTION('',(0.,1.,-4.73470448533E-50)) ;
#56742 = DIRECTION('center_axis',(0.,0.,1.)) ;
#56743 = DIRECTION('ref_axis',(-0.250389541446926,-0.968145173790583,0.)) ;
#56744 = DIRECTION('center_axis',(-1.09763027743844E-32,-3.07546720254364E-67,
1.)) ;
#56745 = DIRECTION('ref_axis',(-1.,1.74482680966927E-115,-1.09763027743844E-32)) ;
#56746 = DIRECTION('',(-0.707106781186472,0.707106781186623,-1.01994663078385E-65)) ;
#56747 = DIRECTION('',(0.992304006159154,-0.123825519827269,1.08918292158375E-32)) ;
#56748 = DIRECTION('center_axis',(-1.09763027743844E-32,-3.07546720254364E-67,
1.)) ;
#56749 = DIRECTION('ref_axis',(-1.,3.3757259187808E-99,-1.09763027743844E-32)) ;
#56750 = DIRECTION('',(0.,0.,1.)) ;
#56751 = DIRECTION('',(0.,0.,1.)) ;
#56752 = DIRECTION('center_axis',(0.,0.,-1.)) ;
#56753 = DIRECTION('ref_axis',(-0.996836376575686,0.0794810564566027,0.)) ;
#56754 = DIRECTION('',(0.,0.,1.)) ;
#56755 = DIRECTION('center_axis',(0.,0.,1.)) ;
#56756 = DIRECTION('ref_axis',(0.988785171592188,0.149344850729469,0.)) ;
#56757 = DIRECTION('',(0.,0.,1.)) ;
#56758 = DIRECTION('center_axis',(0.0966396842804928,0.995319431851989,0.)) ;
#56759 = DIRECTION('ref_axis',(-0.995319431851989,0.0966396842804928,-5.45822738711604E-33)) ;
#56760 = DIRECTION('center_axis',(0.248948925327991,-0.968516614508,0.)) ;
#56761 = DIRECTION('ref_axis',(-0.968516614508,-0.248948925327991,0.)) ;
#56762 = DIRECTION('center_axis',(0.995319431851992,-0.096639684280469,0.)) ;
#56763 = DIRECTION('ref_axis',(0.,0.,-1.)) ;
#56764 = DIRECTION('center_axis',(0.517399992172731,-0.855743681308637,0.)) ;
#56765 = DIRECTION('ref_axis',(-0.855743681308637,-0.517399992172731,0.)) ;
#56766 = DIRECTION('center_axis',(0.,0.,-1.)) ;
#56767 = DIRECTION('ref_axis',(0.560035503521478,0.828468608213639,0.)) ;
#56768 = DIRECTION('center_axis',(1.,0.,0.)) ;
#56769 = DIRECTION('ref_axis',(0.,-1.,0.)) ;
#56770 = DIRECTION('center_axis',(0.,0.,-1.)) ;
#56771 = DIRECTION('ref_axis',(0.871033866220507,-0.491222967599191,0.)) ;
#56772 = DIRECTION('center_axis',(-1.,0.,0.)) ;
#56773 = DIRECTION('ref_axis',(0.,-0.707106781186574,-0.707106781186521)) ;
#56774 = DIRECTION('center_axis',(1.,0.,0.)) ;
#56775 = DIRECTION('ref_axis',(0.,-1.,0.)) ;
#56776 = DIRECTION('',(-1.,0.,0.)) ;
#56777 = DIRECTION('center_axis',(-0.45978265173519,0.888031482078962,0.)) ;
#56778 = DIRECTION('ref_axis',(0.888031482078962,0.45978265173519,0.)) ;
#56779 = DIRECTION('center_axis',(0.,0.,-1.)) ;
#56780 = DIRECTION('ref_axis',(0.707405248487832,-0.706808187850048,0.)) ;
#56781 = DIRECTION('center_axis',(-0.164953742105275,0.986301304351498,0.)) ;
#56782 = DIRECTION('ref_axis',(0.986301304351498,0.164953742105275,0.)) ;
#56783 = DIRECTION('center_axis',(-0.995319431851992,0.096639684280469,0.)) ;
#56784 = DIRECTION('ref_axis',(0.096639684280469,0.995319431851992,0.)) ;
#56785 = DIRECTION('center_axis',(0.995319431851989,-0.0966396842804928,0.)) ;
#56786 = DIRECTION('ref_axis',(0.0683345760864603,0.703797119709251,-0.70710678118658)) ;
#56787 = DIRECTION('',(-0.995319431851989,0.0966396842804928,0.)) ;
#56788 = DIRECTION('',(0.995319431851989,-0.0966396842804928,0.)) ;
#56789 = DIRECTION('center_axis',(0.,0.,1.)) ;
#56790 = DIRECTION('ref_axis',(-1.,0.,0.)) ;
#56791 = DIRECTION('center_axis',(0.583094656822871,-0.81240422277621,0.)) ;
#56792 = DIRECTION('ref_axis',(-0.81240422277621,-0.583094656822871,0.)) ;
#56793 = DIRECTION('center_axis',(1.,0.,0.)) ;
#56794 = DIRECTION('ref_axis',(0.,0.,-1.)) ;
#56795 = DIRECTION('center_axis',(0.805994027221688,-0.591923667446204,0.)) ;
#56796 = DIRECTION('ref_axis',(-0.591923667446204,-0.805994027221688,0.)) ;
#56797 = DIRECTION('center_axis',(1.,0.,0.)) ;
#56798 = DIRECTION('ref_axis',(0.,-1.,0.)) ;
#56799 = DIRECTION('center_axis',(0.,0.,-1.)) ;
#56800 = DIRECTION('ref_axis',(0.950261550112188,-0.311453024352601,0.)) ;
#56801 = DIRECTION('center_axis',(-1.,0.,0.)) ;
#56802 = DIRECTION('ref_axis',(0.,-0.707106781186574,-0.707106781186521)) ;
#56803 = DIRECTION('center_axis',(1.,0.,0.)) ;
#56804 = DIRECTION('ref_axis',(0.,-1.,0.)) ;
#56805 = DIRECTION('',(-1.,0.,0.)) ;
#56806 = DIRECTION('center_axis',(-0.686781523075266,0.726863907180992,0.)) ;
#56807 = DIRECTION('ref_axis',(0.726863907180992,0.686781523075266,0.)) ;
#56808 = DIRECTION('center_axis',(-0.515397663572599,0.856951135353648,0.)) ;
#56809 = DIRECTION('ref_axis',(0.856951135353648,0.515397663572599,0.)) ;
#56810 = DIRECTION('center_axis',(-1.,0.,0.)) ;
#56811 = DIRECTION('ref_axis',(0.,1.,0.)) ;
#56812 = DIRECTION('center_axis',(0.,0.,-1.)) ;
#56813 = DIRECTION('ref_axis',(0.870458977666652,-0.492240965584466,0.)) ;
#56814 = DIRECTION('center_axis',(0.,0.,1.)) ;
#56815 = DIRECTION('ref_axis',(0.870458977653571,-0.492240965607597,0.)) ;
#56816 = DIRECTION('center_axis',(1.,0.,0.)) ;
#56817 = DIRECTION('ref_axis',(0.,0.707106781186574,-0.707106781186521)) ;
#56818 = DIRECTION('',(-1.,0.,0.)) ;
#56819 = DIRECTION('',(1.,0.,0.)) ;
#56820 = DIRECTION('',(0.,0.,-1.)) ;
#56821 = DIRECTION('',(0.,0.,1.)) ;
#56822 = DIRECTION('center_axis',(0.,0.,1.)) ;
#56823 = DIRECTION('ref_axis',(-1.,0.,0.)) ;
#56824 = DIRECTION('center_axis',(-0.9039126820276,0.356838437056911,0.235813895070778)) ;
#56825 = DIRECTION('ref_axis',(0.427717036450173,0.754121910522067,0.49835557667275)) ;
#56826 = DIRECTION('center_axis',(-1.,0.,-2.96059473233375E-13)) ;
#56827 = DIRECTION('ref_axis',(0.,1.,0.)) ;
#56828 = DIRECTION('center_axis',(0.,0.,-1.)) ;
#56829 = DIRECTION('ref_axis',(0.858256747734086,0.513220571459202,0.)) ;
#56830 = DIRECTION('center_axis',(0.513220571458668,-0.858256747734405,0.)) ;
#56831 = DIRECTION('ref_axis',(0.,0.,1.)) ;
#56832 = DIRECTION('center_axis',(0.513220571458983,-0.858256747734216,-5.08190081266363E-13)) ;
#56833 = DIRECTION('ref_axis',(-0.858256747734216,-0.513220571458983,-2.16500831402799E-29)) ;
#56834 = DIRECTION('center_axis',(0.,0.,1.)) ;
#56835 = DIRECTION('ref_axis',(-0.557171124810912,-0.830397698501714,0.)) ;
#56836 = DIRECTION('center_axis',(-1.,0.,0.)) ;
#56837 = DIRECTION('ref_axis',(0.,0.,-1.)) ;
#56838 = DIRECTION('',(0.,0.,1.)) ;
#56839 = DIRECTION('',(0.,0.,-1.)) ;
#56840 = DIRECTION('center_axis',(-0.198151110421921,-0.949811551695269,0.242062293025544)) ;
#56841 = DIRECTION('ref_axis',(-0.601638685605581,0.312822659451454,0.734964540448387)) ;
#56842 = DIRECTION('center_axis',(0.,0.,-1.)) ;
#56843 = DIRECTION('ref_axis',(0.,1.,0.)) ;
#56844 = DIRECTION('center_axis',(1.,-2.81256499571696E-12,0.)) ;
#56845 = DIRECTION('ref_axis',(0.,0.,1.)) ;
#56846 = DIRECTION('center_axis',(0.57437040532927,-0.818595527401592,2.78906268328281E-12)) ;
#56847 = DIRECTION('ref_axis',(-0.818595527401592,-0.57437040532927,1.14085547468979E-28)) ;
#56848 = DIRECTION('center_axis',(0.,0.,-1.)) ;
#56849 = DIRECTION('ref_axis',(0.,1.,0.)) ;
#56850 = DIRECTION('center_axis',(0.,0.,-1.)) ;
#56851 = DIRECTION('ref_axis',(0.,1.,0.)) ;
#56852 = DIRECTION('center_axis',(-1.,0.,0.)) ;
#56853 = DIRECTION('ref_axis',(0.,0.707106781186561,0.707106781186534)) ;
#56854 = DIRECTION('',(1.,0.,0.)) ;
#56855 = DIRECTION('',(-1.,0.,0.)) ;
#56856 = DIRECTION('center_axis',(0.805994027221583,-0.591923667446348,0.)) ;
#56857 = DIRECTION('ref_axis',(0.,0.,1.)) ;
#56858 = DIRECTION('center_axis',(0.,0.,1.)) ;
#56859 = DIRECTION('ref_axis',(0.95026155011525,-0.311453024343258,0.)) ;
#56860 = DIRECTION('center_axis',(1.,0.,0.)) ;
#56861 = DIRECTION('ref_axis',(0.,0.,1.)) ;
#56862 = DIRECTION('center_axis',(0.,0.,-1.)) ;
#56863 = DIRECTION('ref_axis',(0.95026155010268,-0.311453024381611,0.)) ;
#56864 = DIRECTION('center_axis',(1.,0.,0.)) ;
#56865 = DIRECTION('ref_axis',(0.,-0.707106781186561,0.707106781186534)) ;
#56866 = DIRECTION('center_axis',(1.,0.,0.)) ;
#56867 = DIRECTION('ref_axis',(0.,0.,1.)) ;
#56868 = DIRECTION('',(-1.,0.,0.)) ;
#56869 = DIRECTION('',(1.,0.,0.)) ;
#56870 = DIRECTION('center_axis',(-0.686781523075266,0.726863907180992,0.)) ;
#56871 = DIRECTION('ref_axis',(0.,0.,1.)) ;
#56872 = DIRECTION('center_axis',(0.,0.,-1.)) ;
#56873 = DIRECTION('ref_axis',(0.327194307029667,0.944957081272677,0.)) ;
#56874 = DIRECTION('center_axis',(1.,0.,0.)) ;
#56875 = DIRECTION('ref_axis',(0.,-1.,0.)) ;
#56876 = DIRECTION('center_axis',(0.574370405327453,-0.818595527402866,5.3993661000774E-13)) ;
#56877 = DIRECTION('ref_axis',(5.18104078158406E-13,-2.96059473233376E-13,
-1.)) ;
#56878 = DIRECTION('',(0.,0.,-1.)) ;
#56879 = DIRECTION('',(0.,0.,1.)) ;
#56880 = DIRECTION('center_axis',(-0.805994027221724,0.591923667446156,0.)) ;
#56881 = DIRECTION('ref_axis',(0.591923667446156,0.805994027221724,0.)) ;
#56882 = DIRECTION('center_axis',(0.,0.,1.)) ;
#56883 = DIRECTION('ref_axis',(0.95026155010112,-0.311453024386369,0.)) ;
#56884 = DIRECTION('center_axis',(-1.,0.,0.)) ;
#56885 = DIRECTION('ref_axis',(0.,1.,0.)) ;
#56886 = DIRECTION('center_axis',(0.,0.,-1.)) ;
#56887 = DIRECTION('ref_axis',(0.950261550111873,-0.311453024353561,0.)) ;
#56888 = DIRECTION('center_axis',(1.,0.,0.)) ;
#56889 = DIRECTION('ref_axis',(0.,0.707106781186561,-0.707106781186534)) ;
#56890 = DIRECTION('center_axis',(-1.,0.,0.)) ;
#56891 = DIRECTION('ref_axis',(0.,1.,0.)) ;
#56892 = DIRECTION('',(-1.,0.,0.)) ;
#56893 = DIRECTION('',(1.,0.,0.)) ;
#56894 = DIRECTION('center_axis',(0.686781523075266,-0.726863907180992,0.)) ;
#56895 = DIRECTION('ref_axis',(-0.726863907180992,-0.686781523075266,0.)) ;
#56896 = DIRECTION('center_axis',(-1.,0.,0.)) ;
#56897 = DIRECTION('ref_axis',(0.,-0.707106781186561,-0.707106781186534)) ;
#56898 = DIRECTION('',(1.,0.,0.)) ;
#56899 = DIRECTION('',(-1.,0.,0.)) ;
#56900 = DIRECTION('',(0.,0.,1.)) ;
#56901 = DIRECTION('',(0.,0.,-1.)) ;
#56902 = DIRECTION('',(0.,0.,1.)) ;
#56903 = DIRECTION('center_axis',(0.,1.,0.)) ;
#56904 = DIRECTION('ref_axis',(-1.,0.,7.51759117411176E-34)) ;
#56905 = DIRECTION('',(0.,0.,-1.)) ;
#56906 = DIRECTION('center_axis',(0.,0.,1.)) ;
#56907 = DIRECTION('ref_axis',(-1.,0.,0.)) ;
#56908 = DIRECTION('center_axis',(0.,0.,1.)) ;
#56909 = DIRECTION('ref_axis',(0.721343829160339,0.692577129374266,0.)) ;
#56910 = DIRECTION('',(-0.995319431851989,0.0966396842804928,0.)) ;
#56911 = DIRECTION('',(1.,0.,0.)) ;
#56912 = DIRECTION('center_axis',(0.,0.,1.)) ;
#56913 = DIRECTION('ref_axis',(0.951152389067664,-0.308721772427659,0.)) ;
#56914 = DIRECTION('center_axis',(0.,0.,1.)) ;
#56915 = DIRECTION('ref_axis',(-0.836344563545471,-0.548204132625737,0.)) ;
#56916 = DIRECTION('center_axis',(0.,0.,1.)) ;
#56917 = DIRECTION('ref_axis',(-0.58830708113082,-0.808637606280671,0.)) ;
#56918 = DIRECTION('',(-1.,0.,0.)) ;
#56919 = DIRECTION('',(0.995319431851989,-0.0966396842804928,0.)) ;
#56920 = DIRECTION('center_axis',(0.,-1.,0.)) ;
#56921 = DIRECTION('ref_axis',(1.,0.,0.)) ;
#56922 = DIRECTION('center_axis',(0.,0.,1.)) ;
#56923 = DIRECTION('ref_axis',(-1.,0.,0.)) ;
#56924 = DIRECTION('center_axis',(-1.,0.,0.)) ;
#56925 = DIRECTION('ref_axis',(0.,1.,0.)) ;
#56926 = DIRECTION('center_axis',(-0.467163988180043,0.884170689486887,4.00075432832064E-13)) ;
#56927 = DIRECTION('ref_axis',(-2.96059473233375E-13,2.96059473233375E-13,
-1.)) ;
#56928 = DIRECTION('center_axis',(-0.245569634402396,-0.928738932586164,-0.277740075895048)) ;
#56929 = DIRECTION('ref_axis',(0.615184564295696,-0.37073439967014,0.695775794889083)) ;
#56930 = DIRECTION('center_axis',(-0.467163988180506,0.884170689486642,1.72376051565199E-12)) ;
#56931 = DIRECTION('ref_axis',(0.884170689486642,0.467163988180506,2.87117640726933E-30)) ;
#56932 = DIRECTION('center_axis',(0.,0.,-1.)) ;
#56933 = DIRECTION('ref_axis',(0.,-1.,0.)) ;
#56934 = DIRECTION('center_axis',(-1.,6.66133814775069E-13,0.)) ;
#56935 = DIRECTION('ref_axis',(0.,0.,1.)) ;
#56936 = DIRECTION('',(0.,0.,1.)) ;
#56937 = DIRECTION('',(0.,0.,-1.)) ;
#56938 = DIRECTION('center_axis',(-0.520123256650074,0.854091211693295,-5.05723588454344E-13)) ;
#56939 = DIRECTION('ref_axis',(0.854091211693295,0.520123256650074,1.77749193559808E-29)) ;
#56940 = DIRECTION('center_axis',(0.,0.,1.)) ;
#56941 = DIRECTION('ref_axis',(-0.553419070298074,-0.832902955109666,0.)) ;
#56942 = DIRECTION('center_axis',(1.,0.,0.)) ;
#56943 = DIRECTION('ref_axis',(0.,0.,-1.)) ;
#56944 = DIRECTION('center_axis',(0.160503998606273,-0.987035190067405,-1.18796823198059E-14)) ;
#56945 = DIRECTION('ref_axis',(-0.987035190067405,-0.160503998606273,-9.21627772871048E-32)) ;
#56946 = DIRECTION('center_axis',(-0.995319431851992,0.096639684280469,0.)) ;
#56947 = DIRECTION('ref_axis',(0.,0.,-1.)) ;
#56948 = DIRECTION('center_axis',(-0.905234052991426,0.354988520804968,-0.233526142865029)) ;
#56949 = DIRECTION('ref_axis',(-0.424913296220226,-0.756266514397689,0.497503416969204)) ;
#56950 = DIRECTION('center_axis',(1.,0.,-7.40148683083437E-14)) ;
#56951 = DIRECTION('ref_axis',(0.,-1.,0.)) ;
#56952 = DIRECTION('center_axis',(0.,0.,-1.)) ;
#56953 = DIRECTION('ref_axis',(-0.854091211693295,-0.520123256650074,0.)) ;
#56954 = DIRECTION('center_axis',(-0.520123256651582,0.854091211692377,-2.528617942269E-13)) ;
#56955 = DIRECTION('ref_axis',(5.49867212303732E-29,2.96059473233375E-13,
1.)) ;
#56956 = DIRECTION('',(0.,0.,1.)) ;
#56957 = DIRECTION('',(8.45884209238215E-14,0.,-1.)) ;
#56958 = DIRECTION('center_axis',(-0.815753560152279,0.437411293584229,0.378440866376576)) ;
#56959 = DIRECTION('ref_axis',(0.578399627505853,0.616908799770245,0.533739078264957)) ;
#56960 = DIRECTION('center_axis',(0.,0.,-1.)) ;
#56961 = DIRECTION('ref_axis',(0.987035190067405,0.160503998606273,0.)) ;
#56962 = DIRECTION('center_axis',(0.160504422009498,-0.987035121216767,0.)) ;
#56963 = DIRECTION('ref_axis',(0.,0.,1.)) ;
#56964 = DIRECTION('center_axis',(-0.995319431851971,0.096639684280467,2.05513535042918E-7)) ;
#56965 = DIRECTION('ref_axis',(0.096639684280469,0.995319431851992,-7.31253112867355E-24)) ;
#56966 = DIRECTION('center_axis',(0.995319431851992,-0.096639684280469,0.)) ;
#56967 = DIRECTION('ref_axis',(-0.096639684280469,-0.995319431851992,0.)) ;
#56968 = DIRECTION('center_axis',(0.2434402440985,-0.969915897154626,-2.69134591984373E-13)) ;
#56969 = DIRECTION('ref_axis',(7.40148683083438E-14,2.96059473233375E-13,
-1.)) ;
#56970 = DIRECTION('center_axis',(-0.324142602044054,-0.870147708379737,0.371179928257984)) ;
#56971 = DIRECTION('ref_axis',(-0.572356119989909,0.492790995860895,0.655412470363911)) ;
#56972 = DIRECTION('center_axis',(0.243440244098866,-0.969915897154534,1.80181976079286E-14)) ;
#56973 = DIRECTION('ref_axis',(-0.969915897154534,-0.243440244098866,7.08310863902769E-31)) ;
#56974 = DIRECTION('center_axis',(0.,0.,-1.)) ;
#56975 = DIRECTION('ref_axis',(0.0966396842805139,0.995319431851987,0.)) ;
#56976 = DIRECTION('center_axis',(0.,0.,-1.)) ;
#56977 = DIRECTION('ref_axis',(0.0966396842805139,0.995319431851987,0.)) ;
#56978 = DIRECTION('center_axis',(0.995319431851956,-0.0966396842808356,0.)) ;
#56979 = DIRECTION('ref_axis',(0.,0.,1.)) ;
#56980 = DIRECTION('',(0.,0.,1.)) ;
#56981 = DIRECTION('',(0.,0.,-1.)) ;
#56982 = DIRECTION('center_axis',(-0.995319431851989,0.0966396842804928,0.)) ;
#56983 = DIRECTION('ref_axis',(0.068334576086459,0.703797119709238,0.707106781186593)) ;
#56984 = DIRECTION('',(0.995319431851989,-0.0966396842804928,0.)) ;
#56985 = DIRECTION('',(-0.995319431851989,0.0966396842804928,0.)) ;
#56986 = DIRECTION('center_axis',(0.,0.,1.)) ;
#56987 = DIRECTION('ref_axis',(-0.56271407713106,-0.826651599767725,0.)) ;
#56988 = DIRECTION('center_axis',(0.,0.,1.)) ;
#56989 = DIRECTION('ref_axis',(-0.562088660145462,-0.827076984407062,0.)) ;
#56990 = DIRECTION('center_axis',(-0.995319431851989,0.0966396842804928,0.)) ;
#56991 = DIRECTION('ref_axis',(-0.068334576086459,-0.703797119709238,-0.707106781186593)) ;
#56992 = DIRECTION('',(-0.995319431851989,0.0966396842804928,0.)) ;
#56993 = DIRECTION('',(0.,0.,-1.)) ;
#56994 = DIRECTION('',(0.,0.,1.)) ;
#56995 = DIRECTION('center_axis',(1.,0.,0.)) ;
#56996 = DIRECTION('ref_axis',(0.,-0.707106781186561,0.707106781186534)) ;
#56997 = DIRECTION('',(-1.,0.,0.)) ;
#56998 = DIRECTION('',(1.,0.,0.)) ;
#56999 = DIRECTION('center_axis',(1.,0.,0.)) ;
#57000 = DIRECTION('ref_axis',(0.,0.707106781186561,-0.707106781186534)) ;
#57001 = DIRECTION('',(1.,0.,0.)) ;
#57002 = DIRECTION('center_axis',(0.,1.,0.)) ;
#57003 = DIRECTION('ref_axis',(-1.,0.,0.)) ;
#57004 = DIRECTION('center_axis',(0.,0.,1.)) ;
#57005 = DIRECTION('ref_axis',(-1.,0.,0.)) ;
#57006 = DIRECTION('center_axis',(-0.0966396842804928,-0.995319431851989,
0.)) ;
#57007 = DIRECTION('ref_axis',(0.995319431851989,-0.0966396842804928,5.45822738711604E-33)) ;
#57008 = DIRECTION('center_axis',(0.,0.,1.)) ;
#57009 = DIRECTION('ref_axis',(-0.999001662609301,0.0446730131494725,0.)) ;
#57010 = DIRECTION('center_axis',(0.0446052839665837,0.999004688999136,0.)) ;
#57011 = DIRECTION('ref_axis',(0.999004688999136,-0.0446052839665837,0.)) ;
#57012 = DIRECTION('center_axis',(0.,0.,-1.)) ;
#57013 = DIRECTION('ref_axis',(0.575679505269549,0.81767542901362,0.)) ;
#57014 = DIRECTION('center_axis',(0.,0.,1.)) ;
#57015 = DIRECTION('ref_axis',(-0.56680837807234,-0.823849660160762,0.)) ;
#57016 = DIRECTION('',(0.,0.,1.)) ;
#57017 = DIRECTION('',(0.,0.,1.)) ;
#57018 = DIRECTION('',(0.,0.,1.)) ;
#57019 = DIRECTION('',(0.,0.,1.)) ;
#57020 = DIRECTION('center_axis',(0.597732795757345,0.801695394071906,0.)) ;
#57021 = DIRECTION('ref_axis',(-0.801695394071906,0.597732795757345,-4.49124931094878E-33)) ;
#57022 = DIRECTION('',(0.801695394071906,-0.597732795757345,4.49124931094878E-33)) ;
#57023 = DIRECTION('',(0.,0.,1.)) ;
#57024 = DIRECTION('center_axis',(-0.338065775749409,-0.859650876406611,-0.383029896953615)) ;
#57025 = DIRECTION('ref_axis',(-0.568856539673029,0.510881953775375,-0.644516769818974)) ;
#57026 = DIRECTION('center_axis',(-0.202660578497202,0.979249043871464,4.76011490716992E-8)) ;
#57027 = DIRECTION('ref_axis',(-0.979249043871465,-0.202660578497202,-8.65153100789119E-24)) ;
#57028 = DIRECTION('center_axis',(0.,0.,-1.)) ;
#57029 = DIRECTION('ref_axis',(0.0966396842805423,0.995319431851984,0.)) ;
#57030 = DIRECTION('center_axis',(0.,0.,-1.)) ;
#57031 = DIRECTION('ref_axis',(0.0966396842805423,0.995319431851984,0.)) ;
#57032 = DIRECTION('center_axis',(-0.995319429345644,0.0966397100940514,0.)) ;
#57033 = DIRECTION('ref_axis',(0.,0.,-1.)) ;
#57034 = DIRECTION('center_axis',(-0.23112769823868,0.972923423043607,0.)) ;
#57035 = DIRECTION('ref_axis',(0.,0.,-1.)) ;
#57036 = DIRECTION('center_axis',(-0.503089999562018,0.864234026372885,0.)) ;
#57037 = DIRECTION('ref_axis',(0.,0.,-1.)) ;
#57038 = DIRECTION('center_axis',(-0.548205483816164,0.836343677870459,0.)) ;
#57039 = DIRECTION('ref_axis',(0.,0.,-1.)) ;
#57040 = DIRECTION('center_axis',(-0.809381734448836,0.587282902816516,0.)) ;
#57041 = DIRECTION('ref_axis',(0.,0.,-1.)) ;
#57042 = DIRECTION('center_axis',(-1.,0.,0.)) ;
#57043 = DIRECTION('ref_axis',(0.,0.,-1.)) ;
#57044 = DIRECTION('center_axis',(0.,0.,-1.)) ;
#57045 = DIRECTION('ref_axis',(0.951152389067135,-0.308721772429289,0.)) ;
#57046 = DIRECTION('center_axis',(-1.,0.,0.)) ;
#57047 = DIRECTION('ref_axis',(0.,-0.707106781186561,-0.707106781186534)) ;
#57048 = DIRECTION('center_axis',(-1.,0.,0.)) ;
#57049 = DIRECTION('ref_axis',(0.,0.,-1.)) ;
#57050 = DIRECTION('',(-1.,0.,0.)) ;
#57051 = DIRECTION('center_axis',(0.707983649981651,-0.706228823653254,0.)) ;
#57052 = DIRECTION('ref_axis',(0.,0.,-1.)) ;
#57053 = DIRECTION('center_axis',(0.488003536616536,-0.872841651303232,0.)) ;
#57054 = DIRECTION('ref_axis',(0.,0.,-1.)) ;
#57055 = DIRECTION('center_axis',(0.124324416828667,-0.992241623487048,0.)) ;
#57056 = DIRECTION('ref_axis',(0.,0.,-1.)) ;
#57057 = DIRECTION('center_axis',(0.995319431851992,-0.096639684280469,0.)) ;
#57058 = DIRECTION('ref_axis',(0.,0.,-1.)) ;
#57059 = DIRECTION('center_axis',(0.995319431851989,-0.0966396842804928,0.)) ;
#57060 = DIRECTION('ref_axis',(0.068334576086459,0.703797119709238,-0.707106781186593)) ;
#57061 = DIRECTION('center_axis',(0.,-1.,0.)) ;
#57062 = DIRECTION('ref_axis',(1.,0.,0.)) ;
#57063 = DIRECTION('',(0.,0.,1.)) ;
#57064 = DIRECTION('',(-7.24452218352468E-15,0.,-1.)) ;
#57065 = DIRECTION('',(0.,0.,1.)) ;
#57066 = DIRECTION('',(0.,0.,1.)) ;
#57067 = DIRECTION('center_axis',(0.707106781186623,0.707106781186472,0.)) ;
#57068 = DIRECTION('ref_axis',(-0.707106781186472,0.707106781186623,-1.01994663078385E-65)) ;
#57069 = DIRECTION('',(-0.707106781186472,0.707106781186623,-1.01994663078385E-65)) ;
#57070 = DIRECTION('',(0.,0.,-1.)) ;
#57071 = DIRECTION('',(0.,0.,-1.)) ;
#57072 = DIRECTION('',(0.,0.,1.)) ;
#57073 = DIRECTION('',(0.,0.,-1.)) ;
#57074 = DIRECTION('',(0.,0.,1.)) ;
#57075 = DIRECTION('center_axis',(-0.0966396842804928,-0.995319431851989,
0.)) ;
#57076 = DIRECTION('ref_axis',(0.995319431851989,-0.0966396842804928,5.45822738711604E-33)) ;
#57077 = DIRECTION('',(0.,0.,-1.)) ;
#57078 = DIRECTION('',(0.,0.,-1.)) ;
#57079 = DIRECTION('center_axis',(0.,-1.,0.)) ;
#57080 = DIRECTION('ref_axis',(1.,0.,0.)) ;
#57081 = DIRECTION('center_axis',(1.,0.,0.)) ;
#57082 = DIRECTION('ref_axis',(0.,1.,-7.30021430143246E-35)) ;
#57083 = DIRECTION('',(0.,0.,1.)) ;
#57084 = DIRECTION('center_axis',(-7.18398817372806E-49,4.73470448533E-50,
1.)) ;
#57085 = DIRECTION('ref_axis',(-1.,-8.69145204082858E-115,-7.18398817372806E-49)) ;
#57086 = DIRECTION('center_axis',(-1.09763027743844E-32,-3.07546720254364E-67,
1.)) ;
#57087 = DIRECTION('ref_axis',(-1.,1.74482680966927E-115,-1.09763027743844E-32)) ;
#57088 = DIRECTION('',(-0.992304006159154,0.123825519827269,-1.05251895471164E-32)) ;
#57089 = DIRECTION('center_axis',(-0.123825519827269,-0.992304006159154,0.)) ;
#57090 = DIRECTION('ref_axis',(0.992304006159154,-0.123825519827269,1.05251895471164E-32)) ;
#57091 = DIRECTION('',(0.,0.,1.)) ;
#57092 = DIRECTION('center_axis',(0.,0.,1.)) ;
#57093 = DIRECTION('ref_axis',(-1.,0.,0.)) ;
#57094 = DIRECTION('center_axis',(0.,0.,1.)) ;
#57095 = DIRECTION('ref_axis',(-1.,0.,0.)) ;
#57096 = DIRECTION('axis',(0.,0.,1.)) ;
#57097 = DIRECTION('refdir',(1.,0.,0.)) ;
#57098 = DIRECTION('center_axis',(1.,0.,0.)) ;
#57099 = DIRECTION('ref_axis',(0.,0.707106781186574,-0.707106781186521)) ;
#57100 = DIRECTION('',(1.,0.,0.)) ;
#57101 = DIRECTION('center_axis',(0.707106781186574,0.707106781186521,0.)) ;
#57102 = DIRECTION('ref_axis',(-0.707106781186521,0.707106781186574,0.)) ;
#57103 = DIRECTION('',(-1.,0.,0.)) ;
#57104 = DIRECTION('center_axis',(0.,1.,0.)) ;
#57105 = DIRECTION('ref_axis',(-0.707106781186574,0.,-0.707106781186521)) ;
#57106 = DIRECTION('',(0.,-1.,0.)) ;
#57107 = DIRECTION('',(0.,1.,0.)) ;
#57108 = DIRECTION('center_axis',(-0.707106781186574,0.707106781186521,0.)) ;
#57109 = DIRECTION('ref_axis',(-0.707106781186521,-0.707106781186574,0.)) ;
#57110 = DIRECTION('center_axis',(-1.,0.,0.)) ;
#57111 = DIRECTION('ref_axis',(0.,-0.707106781186574,-0.707106781186521)) ;
#57112 = DIRECTION('',(1.,0.,0.)) ;
#57113 = DIRECTION('',(-1.,0.,0.)) ;
#57114 = DIRECTION('center_axis',(0.,1.,0.)) ;
#57115 = DIRECTION('ref_axis',(1.,0.,0.)) ;
#57116 = DIRECTION('',(0.,0.,-1.)) ;
#57117 = DIRECTION('',(1.,0.,1.51760508056877E-16)) ;
#57118 = DIRECTION('',(0.,0.,-1.)) ;
#57119 = DIRECTION('center_axis',(-1.,0.,0.)) ;
#57120 = DIRECTION('ref_axis',(0.,1.,0.)) ;
#57121 = DIRECTION('',(0.,0.,-1.)) ;
#57122 = DIRECTION('',(0.,1.,5.60383084497428E-34)) ;
#57123 = DIRECTION('center_axis',(0.,-1.,0.)) ;
#57124 = DIRECTION('ref_axis',(-1.,0.,0.)) ;
#57125 = DIRECTION('',(0.,0.,-1.)) ;
#57126 = DIRECTION('',(-1.,0.,-1.51760508056877E-16)) ;
#57127 = DIRECTION('',(0.,0.,-1.)) ;
#57128 = DIRECTION('center_axis',(0.,0.,1.)) ;
#57129 = DIRECTION('ref_axis',(-1.,0.,0.)) ;
#57130 = DIRECTION('',(1.,0.,0.)) ;
#57131 = DIRECTION('',(0.536696284465946,-0.843775502275604,0.)) ;
#57132 = DIRECTION('',(1.,0.,0.)) ;
#57133 = DIRECTION('',(-0.538514312398237,0.842616363087173,0.)) ;
#57134 = DIRECTION('',(-1.,0.,0.)) ;
#57135 = DIRECTION('',(0.,-1.,0.)) ;
#57136 = DIRECTION('',(1.,0.,0.)) ;
#57137 = DIRECTION('',(0.,1.,0.)) ;
#57138 = DIRECTION('center_axis',(-0.538514312398237,0.842616363087172,0.)) ;
#57139 = DIRECTION('ref_axis',(-0.595819744277688,-0.380787122062806,-0.707106781186545)) ;
#57140 = DIRECTION('center_axis',(0.480356996202705,0.877073062064452,0.)) ;
#57141 = DIRECTION('ref_axis',(0.877073062064452,-0.480356996202705,0.)) ;
#57142 = DIRECTION('',(0.538514312398237,-0.842616363087173,0.)) ;
#57143 = DIRECTION('center_axis',(1.,0.,0.)) ;
#57144 = DIRECTION('ref_axis',(0.,0.707106781186574,-0.707106781186521)) ;
#57145 = DIRECTION('center_axis',(0.876554700080465,-0.481302251986053,0.)) ;
#57146 = DIRECTION('ref_axis',(-0.481302251986053,-0.876554700080465,0.)) ;
#57147 = DIRECTION('',(-1.,0.,0.)) ;
#57148 = DIRECTION('center_axis',(0.536696284465946,-0.843775502275604,0.)) ;
#57149 = DIRECTION('ref_axis',(0.596639379458124,0.379501582183469,-0.707106781186596)) ;
#57150 = DIRECTION('',(-0.536696284465946,0.843775502275604,0.)) ;
#57151 = DIRECTION('center_axis',(0.999980832705611,-0.00587550485991174,
-0.00195260442350964)) ;
#57152 = DIRECTION('ref_axis',(-0.00195251174417658,2.1509854887887E-5,-0.99999809361579)) ;
#57153 = DIRECTION('center_axis',(1.,0.,0.)) ;
#57154 = DIRECTION('ref_axis',(0.,0.707106781186574,-0.707106781186521)) ;
#57155 = DIRECTION('',(-1.,0.,0.)) ;
#57156 = DIRECTION('center_axis',(-0.999999985503101,-0.000120403056781265,
-0.000120403083049754)) ;
#57157 = DIRECTION('ref_axis',(0.000120401111956324,1.63776238757342E-5,-0.999999992617673)) ;
#57158 = DIRECTION('center_axis',(0.707106781186574,0.707106781186521,0.)) ;
#57159 = DIRECTION('ref_axis',(-0.707106781186521,0.707106781186574,0.)) ;
#57160 = DIRECTION('center_axis',(0.,1.,0.)) ;
#57161 = DIRECTION('ref_axis',(-0.707106781186574,0.,-0.707106781186521)) ;
#57162 = DIRECTION('center_axis',(0.707106781186574,0.707106781186521,0.)) ;
#57163 = DIRECTION('ref_axis',(0.707106781186521,-0.707106781186574,0.)) ;
#57164 = DIRECTION('',(0.,-1.,0.)) ;
#57165 = DIRECTION('center_axis',(1.,0.,0.)) ;
#57166 = DIRECTION('ref_axis',(0.,0.707106781186574,-0.707106781186521)) ;
#57167 = DIRECTION('',(-1.,0.,0.)) ;
#57168 = DIRECTION('center_axis',(0.707106781186574,-0.707106781186521,0.)) ;
#57169 = DIRECTION('ref_axis',(-0.707106781186521,-0.707106781186574,0.)) ;
#57170 = DIRECTION('center_axis',(0.,-1.,0.)) ;
#57171 = DIRECTION('ref_axis',(0.707106781186574,0.,-0.707106781186521)) ;
#57172 = DIRECTION('',(0.,1.,0.)) ;
#57173 = DIRECTION('center_axis',(-0.707106781186574,-0.707106781186521,0.)) ;
#57174 = DIRECTION('ref_axis',(-0.707106781186521,0.707106781186574,0.)) ;
#57175 = DIRECTION('center_axis',(-1.,0.,0.)) ;
#57176 = DIRECTION('ref_axis',(0.,-0.707106781186574,-0.707106781186521)) ;
#57177 = DIRECTION('',(1.,0.,0.)) ;
#57178 = DIRECTION('',(0.,0.,-1.)) ;
#57179 = DIRECTION('',(0.,0.,-1.)) ;
#57180 = DIRECTION('',(0.,0.,-1.)) ;
#57181 = DIRECTION('center_axis',(-0.842616363087172,-0.538514312398237,0.)) ;
#57182 = DIRECTION('ref_axis',(-0.538514312398237,0.842616363087172,0.)) ;
#57183 = DIRECTION('',(0.,0.,-1.)) ;
#57184 = DIRECTION('',(-0.538514312398237,0.842616363087173,-8.17252056454565E-17)) ;
#57185 = DIRECTION('center_axis',(0.,1.,0.)) ;
#57186 = DIRECTION('ref_axis',(1.,0.,0.)) ;
#57187 = DIRECTION('',(0.,0.,-1.)) ;
#57188 = DIRECTION('',(1.,0.,1.51760508056877E-16)) ;
#57189 = DIRECTION('center_axis',(0.843775502275604,0.536696284465946,0.)) ;
#57190 = DIRECTION('ref_axis',(0.536696284465946,-0.843775502275604,0.)) ;
#57191 = DIRECTION('',(0.,0.,-1.)) ;
#57192 = DIRECTION('',(0.536696284465946,-0.843775502275604,8.14493008027904E-17)) ;
#57193 = DIRECTION('',(0.,0.,-1.)) ;
#57194 = DIRECTION('',(0.,0.,-1.)) ;
#57195 = DIRECTION('',(0.,0.,-1.)) ;
#57196 = DIRECTION('',(0.,0.,-1.)) ;
#57197 = DIRECTION('center_axis',(0.,1.,0.)) ;
#57198 = DIRECTION('ref_axis',(1.,0.,0.)) ;
#57199 = DIRECTION('',(0.,0.,-1.)) ;
#57200 = DIRECTION('',(1.,0.,1.51760508056877E-16)) ;
#57201 = DIRECTION('center_axis',(-1.,0.,-1.51760508056877E-16)) ;
#57202 = DIRECTION('ref_axis',(-1.07310884363333E-16,0.707106781186547,0.707106781186547)) ;
#57203 = DIRECTION('',(1.,0.,1.51760508056877E-16)) ;
#57204 = DIRECTION('center_axis',(-0.707106781186574,0.707106781186521,0.)) ;
#57205 = DIRECTION('ref_axis',(0.707106781186521,0.707106781186574,2.14621768726675E-16)) ;
#57206 = DIRECTION('center_axis',(1.,0.,1.51760508056877E-16)) ;
#57207 = DIRECTION('ref_axis',(-1.07310884363333E-16,-0.707106781186547,0.707106781186547)) ;
#57208 = DIRECTION('',(-1.,0.,-1.51760508056877E-16)) ;
#57209 = DIRECTION('center_axis',(-0.707106781186574,-0.707106781186521,0.)) ;
#57210 = DIRECTION('ref_axis',(-0.707106781186521,0.707106781186574,-2.14621768726675E-16)) ;
#57211 = DIRECTION('center_axis',(0.,1.,5.60383084497428E-34)) ;
#57212 = DIRECTION('ref_axis',(0.707106781186547,-3.96250679110365E-34,0.707106781186547)) ;
#57213 = DIRECTION('',(0.,-1.,-5.60383084497428E-34)) ;
#57214 = DIRECTION('center_axis',(-1.51760508056877E-16,-5.60383084497428E-34,
1.)) ;
#57215 = DIRECTION('ref_axis',(1.,1.81422958079369E-66,1.51760508056877E-16)) ;
#57216 = DIRECTION('center_axis',(0.707106781186552,0.707106781186543,0.)) ;
#57217 = DIRECTION('ref_axis',(-0.500000000000041,0.500000000000047,-0.707106781186485)) ;
#57218 = DIRECTION('',(0.707106781186552,0.707106781186543,0.)) ;
#57219 = DIRECTION('center_axis',(1.,-5.23364152894628E-14,-7.40148683083437E-14)) ;
#57220 = DIRECTION('ref_axis',(-5.23364152894683E-14,-1.,-7.40148683083368E-14)) ;
#57221 = DIRECTION('',(-0.707106781186552,-0.707106781186543,0.)) ;
#57222 = DIRECTION('center_axis',(-0.38268343236509,0.923879532511287,0.)) ;
#57223 = DIRECTION('ref_axis',(0.923879532511287,0.38268343236509,0.)) ;
#57224 = DIRECTION('center_axis',(0.707106781186552,-0.707106781186543,0.)) ;
#57225 = DIRECTION('ref_axis',(0.499999999999936,0.499999999999943,-0.707106781186633)) ;
#57226 = DIRECTION('',(-0.707106781186552,0.707106781186543,0.)) ;
#57227 = DIRECTION('',(0.707106781186552,-0.707106781186543,0.)) ;
#57228 = DIRECTION('center_axis',(-0.38268343236508,-0.923879532511291,0.)) ;
#57229 = DIRECTION('ref_axis',(-0.923879532511291,0.38268343236508,0.)) ;
#57230 = DIRECTION('center_axis',(-1.,0.,0.)) ;
#57231 = DIRECTION('ref_axis',(0.,-0.707106781186574,-0.707106781186521)) ;
#57232 = DIRECTION('',(1.,0.,0.)) ;
#57233 = DIRECTION('',(-1.,0.,0.)) ;
#57234 = DIRECTION('center_axis',(0.,-1.,0.)) ;
#57235 = DIRECTION('ref_axis',(-1.,0.,-1.77819390572528E-34)) ;
#57236 = DIRECTION('',(0.,0.,-1.)) ;
#57237 = DIRECTION('',(-1.,0.,-1.51760508056877E-16)) ;
#57238 = DIRECTION('',(0.,0.,-1.)) ;
#57239 = DIRECTION('center_axis',(-0.707106781186543,0.707106781186552,0.)) ;
#57240 = DIRECTION('ref_axis',(0.707106781186552,0.707106781186543,1.25737296900294E-34)) ;
#57241 = DIRECTION('',(0.,0.,-1.)) ;
#57242 = DIRECTION('',(0.707106781186552,0.707106781186543,1.07310884363334E-16)) ;
#57243 = DIRECTION('center_axis',(0.,0.,-1.)) ;
#57244 = DIRECTION('ref_axis',(-1.,0.,0.)) ;
#57245 = DIRECTION('center_axis',(0.,1.,0.)) ;
#57246 = DIRECTION('ref_axis',(-0.707106781186521,0.,-0.707106781186574)) ;
#57247 = DIRECTION('',(0.,1.,0.)) ;
#57248 = DIRECTION('center_axis',(0.7071067811866,0.707106781186495,0.)) ;
#57249 = DIRECTION('ref_axis',(0.707106781186495,-0.7071067811866,0.)) ;
#57250 = DIRECTION('',(0.,-1.,0.)) ;
#57251 = DIRECTION('center_axis',(-0.707106781186495,0.7071067811866,0.)) ;
#57252 = DIRECTION('ref_axis',(0.7071067811866,0.707106781186495,0.)) ;
#57253 = DIRECTION('center_axis',(1.,0.,0.)) ;
#57254 = DIRECTION('ref_axis',(0.,0.707106781186574,-0.707106781186521)) ;
#57255 = DIRECTION('',(-1.,0.,0.)) ;
#57256 = DIRECTION('',(1.,0.,0.)) ;
#57257 = DIRECTION('center_axis',(0.707106781186574,-0.707106781186521,0.)) ;
#57258 = DIRECTION('ref_axis',(-0.707106781186521,-0.707106781186574,0.)) ;
#57259 = DIRECTION('center_axis',(0.,-1.,0.)) ;
#57260 = DIRECTION('ref_axis',(0.707106781186574,0.,-0.707106781186521)) ;
#57261 = DIRECTION('',(0.,1.,0.)) ;
#57262 = DIRECTION('',(0.,-1.,0.)) ;
#57263 = DIRECTION('center_axis',(-0.707106781186469,-0.707106781186626,0.)) ;
#57264 = DIRECTION('ref_axis',(-0.707106781186626,0.707106781186469,0.)) ;
#57265 = DIRECTION('center_axis',(-1.,0.,0.)) ;
#57266 = DIRECTION('ref_axis',(0.,-0.707106781186574,-0.707106781186521)) ;
#57267 = DIRECTION('',(1.,0.,0.)) ;
#57268 = DIRECTION('',(-1.,0.,0.)) ;
#57269 = DIRECTION('center_axis',(0.,-1.,0.)) ;
#57270 = DIRECTION('ref_axis',(-1.,0.,0.)) ;
#57271 = DIRECTION('',(0.,0.,-1.)) ;
#57272 = DIRECTION('',(-1.,0.,-1.51760508056877E-16)) ;
#57273 = DIRECTION('',(0.,0.,-1.)) ;
#57274 = DIRECTION('center_axis',(-1.,0.,0.)) ;
#57275 = DIRECTION('ref_axis',(0.,1.,0.)) ;
#57276 = DIRECTION('',(0.,0.,-1.)) ;
#57277 = DIRECTION('',(0.,1.,5.60383084497428E-34)) ;
#57278 = DIRECTION('center_axis',(0.,0.,-1.)) ;
#57279 = DIRECTION('ref_axis',(-1.,0.,0.)) ;
#57280 = DIRECTION('center_axis',(-0.707106781186552,0.707106781186543,0.)) ;
#57281 = DIRECTION('ref_axis',(-0.499999999999936,-0.499999999999943,-0.707106781186633)) ;
#57282 = DIRECTION('',(-0.707106781186552,0.707106781186543,0.)) ;
#57283 = DIRECTION('center_axis',(0.38268343236508,0.923879532511291,0.)) ;
#57284 = DIRECTION('ref_axis',(0.923879532511291,-0.38268343236508,0.)) ;
#57285 = DIRECTION('',(0.707106781186552,-0.707106781186543,0.)) ;
#57286 = DIRECTION('center_axis',(-1.,5.23364152894628E-14,-7.40148683083437E-14)) ;
#57287 = DIRECTION('ref_axis',(5.23364152894683E-14,1.,-7.40148683083368E-14)) ;
#57288 = DIRECTION('center_axis',(1.,0.,0.)) ;
#57289 = DIRECTION('ref_axis',(0.,0.707106781186574,-0.707106781186521)) ;
#57290 = DIRECTION('',(-1.,0.,0.)) ;
#57291 = DIRECTION('',(1.,0.,0.)) ;
#57292 = DIRECTION('center_axis',(0.38268343236509,-0.923879532511287,0.)) ;
#57293 = DIRECTION('ref_axis',(-0.923879532511287,-0.38268343236509,0.)) ;
#57294 = DIRECTION('center_axis',(-0.707106781186552,-0.707106781186543,0.)) ;
#57295 = DIRECTION('ref_axis',(0.500000000000041,-0.500000000000047,-0.707106781186485)) ;
#57296 = DIRECTION('',(0.707106781186552,0.707106781186543,0.)) ;
#57297 = DIRECTION('',(-0.707106781186552,-0.707106781186543,0.)) ;
#57298 = DIRECTION('center_axis',(0.707106781186543,-0.707106781186552,0.)) ;
#57299 = DIRECTION('ref_axis',(-0.707106781186552,-0.707106781186543,-1.25737296900294E-34)) ;
#57300 = DIRECTION('',(0.,0.,-1.)) ;
#57301 = DIRECTION('',(-0.707106781186552,-0.707106781186543,-1.07310884363334E-16)) ;
#57302 = DIRECTION('',(0.,0.,-1.)) ;
#57303 = DIRECTION('center_axis',(-0.707106781186543,-0.707106781186552,0.)) ;
#57304 = DIRECTION('ref_axis',(-0.707106781186552,0.707106781186543,-1.25737296900294E-34)) ;
#57305 = DIRECTION('',(0.,0.,-1.)) ;
#57306 = DIRECTION('',(-0.707106781186552,0.707106781186543,-1.07310884363334E-16)) ;
#57307 = DIRECTION('center_axis',(0.,0.,-1.)) ;
#57308 = DIRECTION('ref_axis',(-1.,0.,0.)) ;
#57309 = DIRECTION('center_axis',(-0.538514312398237,0.842616363087172,-8.17252056454566E-17)) ;
#57310 = DIRECTION('ref_axis',(0.595819744277703,0.380787122062815,0.707106781186527)) ;
#57311 = DIRECTION('',(0.538514312398237,-0.842616363087173,8.17252056454565E-17)) ;
#57312 = DIRECTION('center_axis',(0.48035699620269,0.87707306206446,0.)) ;
#57313 = DIRECTION('ref_axis',(-0.87707306206446,0.48035699620269,-1.73030634072448E-16)) ;
#57314 = DIRECTION('center_axis',(0.536696284465946,-0.843775502275604,8.14493008027904E-17)) ;
#57315 = DIRECTION('ref_axis',(-0.596639379458102,-0.379501582183455,0.707106781186622)) ;
#57316 = DIRECTION('center_axis',(-0.538364893193227,0.842709511753463,-0.00198004476873555)) ;
#57317 = DIRECTION('ref_axis',(-0.0010804597739936,0.00165936097387972,0.999998039561996)) ;
#57318 = DIRECTION('',(-0.536696284465946,0.843775502275604,-8.14493008027904E-17)) ;
#57319 = DIRECTION('center_axis',(0.87655470008041,-0.481302251986153,0.)) ;
#57320 = DIRECTION('ref_axis',(0.481302251986153,0.87655470008041,-1.69226926461802E-16)) ;
#57321 = DIRECTION('center_axis',(0.,1.,5.60383084497428E-34)) ;
#57322 = DIRECTION('ref_axis',(0.707106781186547,-3.96250679110365E-34,0.707106781186547)) ;
#57323 = DIRECTION('',(0.,1.,5.60383084497428E-34)) ;
#57324 = DIRECTION('center_axis',(-0.707106781186574,-0.707106781186521,0.)) ;
#57325 = DIRECTION('ref_axis',(0.707106781186521,-0.707106781186574,-7.92501358220702E-34)) ;
#57326 = DIRECTION('',(0.,-1.,-5.60383084497428E-34)) ;
#57327 = DIRECTION('center_axis',(0.707106781186574,0.707106781186521,0.)) ;
#57328 = DIRECTION('ref_axis',(0.707106781186521,-0.707106781186574,-7.92501358220702E-34)) ;
#57329 = DIRECTION('center_axis',(-1.,0.,-1.51760508056877E-16)) ;
#57330 = DIRECTION('ref_axis',(-1.07310884363333E-16,0.707106781186547,0.707106781186547)) ;
#57331 = DIRECTION('',(1.,0.,1.51760508056877E-16)) ;
#57332 = DIRECTION('center_axis',(-0.707106781186574,-0.707106781186521,0.)) ;
#57333 = DIRECTION('ref_axis',(0.707106781186521,-0.707106781186574,2.14621768726675E-16)) ;
#57334 = DIRECTION('',(-1.,0.,-1.51760508056877E-16)) ;
#57335 = DIRECTION('center_axis',(0.,-1.,-5.60383084497428E-34)) ;
#57336 = DIRECTION('ref_axis',(-0.707106781186547,-3.96250679110365E-34,0.707106781186547)) ;
#57337 = DIRECTION('',(0.,1.,5.60383084497428E-34)) ;
#57338 = DIRECTION('center_axis',(0.707106781186574,-0.707106781186521,0.)) ;
#57339 = DIRECTION('ref_axis',(0.707106781186521,0.707106781186574,7.92501358220702E-34)) ;
#57340 = DIRECTION('',(0.,-1.,-5.60383084497428E-34)) ;
#57341 = DIRECTION('center_axis',(1.,0.,1.51760508056877E-16)) ;
#57342 = DIRECTION('ref_axis',(-1.07310884363333E-16,-0.707106781186547,0.707106781186547)) ;
#57343 = DIRECTION('',(1.,0.,1.51760508056877E-16)) ;
#57344 = DIRECTION('',(-1.,0.,-1.51760508056877E-16)) ;
#57345 = DIRECTION('center_axis',(-0.999999927776723,-0.000360666211120845,
0.000119860056843106)) ;
#57346 = DIRECTION('ref_axis',(0.000119860035380113,8.11099348877999E-8,0.999999992816783)) ;
#57347 = DIRECTION('center_axis',(1.,0.,1.51760508056877E-16)) ;
#57348 = DIRECTION('ref_axis',(-1.07310884363333E-16,-0.707106781186547,0.707106781186547)) ;
#57349 = DIRECTION('',(-1.,0.,-1.51760508056877E-16)) ;
#57350 = DIRECTION('center_axis',(1.,0.,1.51760508056877E-16)) ;
#57351 = DIRECTION('ref_axis',(-1.07310884363333E-16,-0.707106781186547,0.707106781186547)) ;
#57352 = DIRECTION('',(-1.,0.,-1.51760508056877E-16)) ;
#57353 = DIRECTION('',(0.,0.,-1.)) ;
#57354 = DIRECTION('',(0.,0.,-1.)) ;
#57355 = DIRECTION('',(0.,0.,-1.)) ;
#57356 = DIRECTION('',(0.,0.,-1.)) ;
#57357 = DIRECTION('',(0.,0.,-1.)) ;
#57358 = DIRECTION('center_axis',(0.,-1.,0.)) ;
#57359 = DIRECTION('ref_axis',(-1.,0.,0.)) ;
#57360 = DIRECTION('',(0.,0.,-1.)) ;
#57361 = DIRECTION('center_axis',(1.,0.,0.)) ;
#57362 = DIRECTION('ref_axis',(0.,-1.,0.)) ;
#57363 = DIRECTION('',(0.,0.,-1.)) ;
#57364 = DIRECTION('center_axis',(0.,1.,0.)) ;
#57365 = DIRECTION('ref_axis',(1.,0.,0.)) ;
#57366 = DIRECTION('',(0.,0.,-1.)) ;
#57367 = DIRECTION('center_axis',(-1.,0.,0.)) ;
#57368 = DIRECTION('ref_axis',(0.,1.,0.)) ;
#57369 = DIRECTION('center_axis',(-1.51760508056877E-16,-5.60383084497428E-34,
1.)) ;
#57370 = DIRECTION('ref_axis',(1.,1.81422958079369E-66,1.51760508056877E-16)) ;
#57371 = DIRECTION('',(0.,-1.,-5.60383084497428E-34)) ;
#57372 = DIRECTION('',(1.,0.,1.51760508056877E-16)) ;
#57373 = DIRECTION('',(0.,1.,5.60383084497428E-34)) ;
#57374 = DIRECTION('center_axis',(-1.51760508056877E-16,-5.60383084497428E-34,
1.)) ;
#57375 = DIRECTION('ref_axis',(1.99707445226891E-15,-1.,3.02516650419242E-31)) ;
#57376 = DIRECTION('',(1.,-3.19495806435525E-17,1.51760508056877E-16)) ;
#57377 = DIRECTION('center_axis',(-1.51760508056877E-16,-5.60383084497428E-34,
1.)) ;
#57378 = DIRECTION('ref_axis',(1.75742551799664E-15,-1.,2.66147406398793E-31)) ;
#57379 = DIRECTION('',(0.,-1.,-5.60383084497428E-34)) ;
#57380 = DIRECTION('',(1.,0.,1.51760508056877E-16)) ;
#57381 = DIRECTION('center_axis',(-1.51760508056877E-16,-5.60383084497428E-34,
1.)) ;
#57382 = DIRECTION('ref_axis',(1.,2.24153233798966E-35,1.51760508056877E-16)) ;
#57383 = DIRECTION('center_axis',(-1.51760508056877E-16,-5.60383084497428E-34,
1.)) ;
#57384 = DIRECTION('ref_axis',(1.,2.24153233798966E-35,1.51760508056877E-16)) ;
#57385 = DIRECTION('',(1.,0.,1.51760508056877E-16)) ;
#57386 = DIRECTION('',(0.,1.,5.60383084497428E-34)) ;
#57387 = DIRECTION('center_axis',(-1.51760508056877E-16,-5.60383084497428E-34,
1.)) ;
#57388 = DIRECTION('ref_axis',(9.58595737089076E-16,-1.,1.44916592997297E-31)) ;
#57389 = DIRECTION('',(1.,-3.19495806435525E-17,1.51760508056877E-16)) ;
#57390 = DIRECTION('center_axis',(-1.51760508056877E-16,-5.60383084497428E-34,
1.)) ;
#57391 = DIRECTION('ref_axis',(1.35801062754286E-15,-1.,2.05531999698045E-31)) ;
#57392 = DIRECTION('',(0.,-1.,-5.60383084497428E-34)) ;
#57393 = DIRECTION('',(1.,0.,1.51760508056877E-16)) ;
#57394 = DIRECTION('',(-2.22044604925031E-16,1.,-3.31372189702139E-32)) ;
#57395 = DIRECTION('center_axis',(1.51760508056877E-16,5.60383084497428E-34,
-1.)) ;
#57396 = DIRECTION('ref_axis',(-0.70710678118657,-0.707106781186525,-1.07310884363337E-16)) ;
#57397 = DIRECTION('',(-1.,0.,-1.51760508056877E-16)) ;
#57398 = DIRECTION('center_axis',(1.51760508056877E-16,5.60383084497428E-34,
-1.)) ;
#57399 = DIRECTION('ref_axis',(0.707106781186573,-0.707106781186522,1.07310884363337E-16)) ;
#57400 = DIRECTION('',(2.33146835171284E-14,-1.,3.53768783266021E-30)) ;
#57401 = DIRECTION('center_axis',(-1.51760508056877E-16,-5.60383084497428E-34,
1.)) ;
#57402 = DIRECTION('ref_axis',(-0.707106781186485,0.70710678118661,-1.07310884363324E-16)) ;
#57403 = DIRECTION('',(-1.,0.,-1.51760508056877E-16)) ;
#57404 = DIRECTION('center_axis',(-1.51760508056877E-16,-5.60383084497428E-34,
1.)) ;
#57405 = DIRECTION('ref_axis',(0.70710678118661,0.707106781186485,1.07310884363343E-16)) ;
#57406 = DIRECTION('',(2.22044604925032E-15,1.,3.37536403631613E-31)) ;
#57407 = DIRECTION('center_axis',(1.51760508056877E-16,5.60383084497428E-34,
-1.)) ;
#57408 = DIRECTION('ref_axis',(-0.707106781186548,-0.707106781186548,-1.07310884363333E-16)) ;
#57409 = DIRECTION('',(-1.,0.,-1.51760508056877E-16)) ;
#57410 = DIRECTION('center_axis',(-1.51760508056877E-16,-5.60383084497428E-34,
1.)) ;
#57411 = DIRECTION('ref_axis',(0.707106781186547,0.707106781186547,1.07310884363333E-16)) ;
#57412 = DIRECTION('',(5.25359141716359E-35,1.,5.60383084497428E-34)) ;
#57413 = DIRECTION('center_axis',(1.51760508056877E-16,5.60383084497428E-34,
-1.)) ;
#57414 = DIRECTION('ref_axis',(-0.953716950748229,-0.300705799504266,-1.44736568988007E-16)) ;
#57415 = DIRECTION('',(-0.573576436351042,0.819152044288994,-8.70462513900874E-17)) ;
#57416 = DIRECTION('center_axis',(1.51760508056877E-16,5.60383084497428E-34,
-1.)) ;
#57417 = DIRECTION('ref_axis',(-0.53729960834682,-0.843391445812888,-8.15408615414745E-17)) ;
#57418 = DIRECTION('',(-0.984807753012209,0.173648177666924,-1.49454924935485E-16)) ;
#57419 = DIRECTION('center_axis',(1.51760508056877E-16,5.60383084497428E-34,
-1.)) ;
#57420 = DIRECTION('ref_axis',(0.642787609686539,-0.766044443118978,9.75497742186947E-17)) ;
#57421 = DIRECTION('',(5.23472275150178E-15,-1.,7.93863801220309E-31)) ;
#57422 = DIRECTION('center_axis',(-1.51760508056877E-16,-5.60383084497428E-34,
1.)) ;
#57423 = DIRECTION('ref_axis',(-0.923879532511313,0.382683432365025,-1.40208427237267E-16)) ;
#57424 = DIRECTION('',(-0.707106781186521,-0.707106781186574,-1.0731088436333E-16)) ;
#57425 = DIRECTION('center_axis',(1.51760508056877E-16,5.60383084497428E-34,
-1.)) ;
#57426 = DIRECTION('ref_axis',(0.923879532511288,-0.382683432365087,1.40208427237263E-16)) ;
#57427 = DIRECTION('',(6.83214169000096E-16,-1.,1.03124546314615E-31)) ;
#57428 = DIRECTION('center_axis',(1.51760508056877E-16,5.60383084497428E-34,
-1.)) ;
#57429 = DIRECTION('ref_axis',(0.718421208107098,0.695608343640254,1.09027967541169E-16)) ;
#57430 = DIRECTION('center_axis',(-1.51760508056877E-16,-5.60383084497428E-34,
1.)) ;
#57431 = DIRECTION('ref_axis',(-0.718421208107092,-0.69560834364026,-1.09027967541168E-16)) ;
#57432 = DIRECTION('',(0.,-1.,-5.60383084497428E-34)) ;
#57433 = DIRECTION('center_axis',(-1.51760508056877E-16,-5.60383084497428E-34,
1.)) ;
#57434 = DIRECTION('ref_axis',(-0.718421208107087,0.695608343640265,-1.09027967541167E-16)) ;
#57435 = DIRECTION('center_axis',(1.51760508056877E-16,5.60383084497428E-34,
-1.)) ;
#57436 = DIRECTION('ref_axis',(0.718421208107084,-0.695608343640269,1.09027967541166E-16)) ;
#57437 = DIRECTION('',(6.83214169000096E-16,-1.,1.03124546314615E-31)) ;
#57438 = DIRECTION('center_axis',(1.51760508056877E-16,5.60383084497428E-34,
-1.)) ;
#57439 = DIRECTION('ref_axis',(0.923879532511263,0.382683432365148,1.40208427237259E-16)) ;
#57440 = DIRECTION('',(0.707106781186615,-0.70710678118648,1.07310884363344E-16)) ;
#57441 = DIRECTION('center_axis',(-1.51760508056877E-16,-5.60383084497428E-34,
1.)) ;
#57442 = DIRECTION('ref_axis',(-0.923879532511263,-0.382683432365148,-1.40208427237259E-16)) ;
#57443 = DIRECTION('',(-0.707106781186552,-0.707106781186543,-1.07310884363334E-16)) ;
#57444 = DIRECTION('',(-0.707106781186552,0.707106781186543,-1.07310884363334E-16)) ;
#57445 = DIRECTION('',(1.,0.,1.51760508056877E-16)) ;
#57446 = DIRECTION('',(0.707106781186552,-0.707106781186543,1.07310884363334E-16)) ;
#57447 = DIRECTION('',(-1.,0.,-1.51760508056877E-16)) ;
#57448 = DIRECTION('',(0.707106781186552,0.707106781186543,1.07310884363334E-16)) ;
#57449 = DIRECTION('center_axis',(-1.51760508056877E-16,-5.60383084497428E-34,
1.)) ;
#57450 = DIRECTION('ref_axis',(0.707106781186485,-0.70710678118661,1.07310884363324E-16)) ;
#57451 = DIRECTION('',(1.,0.,1.51760508056877E-16)) ;
#57452 = DIRECTION('center_axis',(-1.51760508056877E-16,-5.60383084497428E-34,
1.)) ;
#57453 = DIRECTION('ref_axis',(-0.707106781186359,-0.707106781186736,-1.07310884363305E-16)) ;
#57454 = DIRECTION('',(0.,-1.,-5.60383084497428E-34)) ;
#57455 = DIRECTION('center_axis',(-1.51760508056877E-16,-5.60383084497428E-34,
1.)) ;
#57456 = DIRECTION('ref_axis',(-0.707106781186485,0.70710678118661,-1.07310884363324E-16)) ;
#57457 = DIRECTION('',(-1.,0.,-1.51760508056877E-16)) ;
#57458 = DIRECTION('',(0.,-1.,-5.60383084497428E-34)) ;
#57459 = DIRECTION('center_axis',(-1.51760508056877E-16,-5.60383084497428E-34,
1.)) ;
#57460 = DIRECTION('ref_axis',(-0.707106781186485,0.70710678118661,-1.07310884363324E-16)) ;
#57461 = DIRECTION('',(-1.,0.,-1.51760508056877E-16)) ;
#57462 = DIRECTION('center_axis',(-1.51760508056877E-16,-5.60383084497428E-34,
1.)) ;
#57463 = DIRECTION('ref_axis',(0.70710678118661,0.707106781186485,1.07310884363343E-16)) ;
#57464 = DIRECTION('',(0.,1.,5.60383084497428E-34)) ;
#57465 = DIRECTION('',(-1.,0.,-1.51760508056877E-16)) ;
#57466 = DIRECTION('center_axis',(-1.51760508056877E-16,-5.60383084497428E-34,
1.)) ;
#57467 = DIRECTION('ref_axis',(0.707106781186359,0.707106781186736,1.07310884363305E-16)) ;
#57468 = DIRECTION('',(0.,1.,5.60383084497428E-34)) ;
#57469 = DIRECTION('',(-7.105427357601E-15,-1.,-1.07888364883526E-30)) ;
#57470 = DIRECTION('',(1.,0.,1.51760508056877E-16)) ;
#57471 = DIRECTION('',(-3.17206578464329E-15,1.,-4.80833931982806E-31)) ;
#57472 = DIRECTION('',(-1.,3.55271367880051E-14,-1.51760508056877E-16)) ;
#57473 = DIRECTION('',(-7.105427357601E-15,-1.,-1.07888364883526E-30)) ;
#57474 = DIRECTION('center_axis',(-1.51760508056877E-16,-5.60383084497428E-34,
1.)) ;
#57475 = DIRECTION('ref_axis',(0.707106781186485,-0.70710678118661,1.07310884363324E-16)) ;
#57476 = DIRECTION('',(1.,-7.10542735760144E-15,1.51760508056877E-16)) ;
#57477 = DIRECTION('center_axis',(-1.51760508056877E-16,-5.60383084497428E-34,
1.)) ;
#57478 = DIRECTION('ref_axis',(-0.382683432365031,-0.923879532511311,-5.80762321206666E-17)) ;
#57479 = DIRECTION('',(0.707106781186544,-0.707106781186551,1.07310884363333E-16)) ;
#57480 = DIRECTION('center_axis',(-1.51760508056877E-16,-5.60383084497428E-34,
1.)) ;
#57481 = DIRECTION('ref_axis',(-0.92387953251129,-0.382683432365082,-1.40208427237263E-16)) ;
#57482 = DIRECTION('',(-3.73034936274055E-14,-1.,-5.66175752827605E-30)) ;
#57483 = DIRECTION('center_axis',(-1.51760508056877E-16,-5.60383084497428E-34,
1.)) ;
#57484 = DIRECTION('ref_axis',(-0.923879532511297,0.382683432365065,-1.40208427237264E-16)) ;
#57485 = DIRECTION('',(-0.707106781186563,-0.707106781186532,-1.07310884363336E-16)) ;
#57486 = DIRECTION('center_axis',(-1.51760508056877E-16,-5.60383084497428E-34,
1.)) ;
#57487 = DIRECTION('ref_axis',(-0.382683432365031,0.923879532511311,-5.80762321206666E-17)) ;
#57488 = DIRECTION('',(-1.,0.,-1.51760508056877E-16)) ;
#57489 = DIRECTION('center_axis',(-1.51760508056877E-16,-5.60383084497428E-34,
1.)) ;
#57490 = DIRECTION('ref_axis',(0.707106781186359,0.707106781186736,1.07310884363305E-16)) ;
#57491 = DIRECTION('center_axis',(-1.51760508056877E-16,-5.60383084497428E-34,
1.)) ;
#57492 = DIRECTION('ref_axis',(-0.707106781186485,0.70710678118661,-1.07310884363324E-16)) ;
#57493 = DIRECTION('',(-1.,0.,-1.51760508056877E-16)) ;
#57494 = DIRECTION('',(0.,-1.,-5.60383084497428E-34)) ;
#57495 = DIRECTION('center_axis',(-1.51760508056877E-16,-5.60383084497428E-34,
1.)) ;
#57496 = DIRECTION('ref_axis',(-0.707106781186485,0.70710678118661,-1.07310884363324E-16)) ;
#57497 = DIRECTION('',(-1.,0.,-1.51760508056877E-16)) ;
#57498 = DIRECTION('center_axis',(-1.51760508056877E-16,-5.60383084497428E-34,
1.)) ;
#57499 = DIRECTION('ref_axis',(0.70710678118661,0.707106781186485,1.07310884363343E-16)) ;
#57500 = DIRECTION('',(0.,1.,5.60383084497428E-34)) ;
#57501 = DIRECTION('',(-1.,0.,-1.51760508056877E-16)) ;
#57502 = DIRECTION('center_axis',(-1.51760508056877E-16,-5.60383084497428E-34,
1.)) ;
#57503 = DIRECTION('ref_axis',(0.707106781186359,0.707106781186736,1.07310884363305E-16)) ;
#57504 = DIRECTION('',(0.,1.,5.60383084497428E-34)) ;
#57505 = DIRECTION('center_axis',(-1.51760508056877E-16,-5.60383084497428E-34,
1.)) ;
#57506 = DIRECTION('ref_axis',(0.707106781186485,-0.70710678118661,1.07310884363324E-16)) ;
#57507 = DIRECTION('',(1.,0.,1.51760508056877E-16)) ;
#57508 = DIRECTION('center_axis',(-1.51760508056877E-16,-5.60383084497428E-34,
1.)) ;
#57509 = DIRECTION('ref_axis',(-0.707106781186359,-0.707106781186736,-1.07310884363305E-16)) ;
#57510 = DIRECTION('',(0.,-1.,-5.60383084497428E-34)) ;
#57511 = DIRECTION('center_axis',(-1.51760508056877E-16,-5.60383084497428E-34,
1.)) ;
#57512 = DIRECTION('ref_axis',(-0.873151649036935,0.487448661690728,-1.32509937868545E-16)) ;
#57513 = DIRECTION('',(-1.,0.,-1.51760508056877E-16)) ;
#57514 = DIRECTION('',(0.,-1.,-5.60383084497428E-34)) ;
#57515 = DIRECTION('center_axis',(-1.51760508056877E-16,-5.60383084497428E-34,
1.)) ;
#57516 = DIRECTION('ref_axis',(-0.707106781186485,0.70710678118661,-1.07310884363324E-16)) ;
#57517 = DIRECTION('',(-1.,0.,-1.51760508056877E-16)) ;
#57518 = DIRECTION('center_axis',(-1.51760508056877E-16,-5.60383084497428E-34,
1.)) ;
#57519 = DIRECTION('ref_axis',(0.70710678118661,0.707106781186485,1.07310884363343E-16)) ;
#57520 = DIRECTION('',(0.,1.,5.60383084497428E-34)) ;
#57521 = DIRECTION('',(-1.,0.,-1.51760508056877E-16)) ;
#57522 = DIRECTION('center_axis',(-1.51760508056877E-16,-5.60383084497428E-34,
1.)) ;
#57523 = DIRECTION('ref_axis',(0.707106781186359,0.707106781186736,1.07310884363305E-16)) ;
#57524 = DIRECTION('',(0.,1.,5.60383084497428E-34)) ;
#57525 = DIRECTION('center_axis',(-1.51760508056877E-16,-5.60383084497428E-34,
1.)) ;
#57526 = DIRECTION('ref_axis',(0.707106781186485,-0.70710678118661,1.07310884363324E-16)) ;
#57527 = DIRECTION('',(1.,0.,1.51760508056877E-16)) ;
#57528 = DIRECTION('center_axis',(-1.51760508056877E-16,-5.60383084497428E-34,
1.)) ;
#57529 = DIRECTION('ref_axis',(-0.707106781186359,-0.707106781186736,-1.07310884363305E-16)) ;
#57530 = DIRECTION('',(0.,-1.,-5.60383084497428E-34)) ;
#57531 = DIRECTION('',(-7.105427357601E-15,-1.,-1.07888364883526E-30)) ;
#57532 = DIRECTION('',(1.,0.,1.51760508056877E-16)) ;
#57533 = DIRECTION('',(-3.17206578464327E-15,1.,-4.80833931982803E-31)) ;
#57534 = DIRECTION('',(-1.,3.55271367880051E-14,-1.51760508056877E-16)) ;
#57535 = DIRECTION('',(-7.105427357601E-15,-1.,-1.07888364883526E-30)) ;
#57536 = DIRECTION('',(1.,-7.10542735760144E-15,1.51760508056877E-16)) ;
#57537 = DIRECTION('center_axis',(-1.51760508056877E-16,-5.60383084497428E-34,
1.)) ;
#57538 = DIRECTION('ref_axis',(-0.382683432365004,-0.923879532511322,-5.80762321206626E-17)) ;
#57539 = DIRECTION('',(0.707106781186575,-0.70710678118652,1.07310884363338E-16)) ;
#57540 = DIRECTION('center_axis',(-1.51760508056877E-16,-5.60383084497428E-34,
1.)) ;
#57541 = DIRECTION('ref_axis',(-0.92387953251129,-0.382683432365082,-1.40208427237263E-16)) ;
#57542 = DIRECTION('',(-3.73034936274055E-14,-1.,-5.66175752827605E-30)) ;
#57543 = DIRECTION('center_axis',(-1.51760508056877E-16,-5.60383084497428E-34,
1.)) ;
#57544 = DIRECTION('ref_axis',(-0.92387953251129,0.382683432365082,-1.40208427237263E-16)) ;
#57545 = DIRECTION('',(-0.707106781186563,-0.707106781186532,-1.07310884363336E-16)) ;
#57546 = DIRECTION('center_axis',(-1.51760508056877E-16,-5.60383084497428E-34,
1.)) ;
#57547 = DIRECTION('ref_axis',(-0.382683432365031,0.923879532511311,-5.80762321206666E-17)) ;
#57548 = DIRECTION('',(-1.,0.,-1.51760508056877E-16)) ;
#57549 = DIRECTION('center_axis',(-1.51760508056877E-16,-5.60383084497428E-34,
1.)) ;
#57550 = DIRECTION('ref_axis',(1.,2.24153233798966E-35,1.51760508056877E-16)) ;
#57551 = DIRECTION('',(-1.1311821873082E-49,1.,5.60383084497428E-34)) ;
#57552 = DIRECTION('center_axis',(-1.51760508056877E-16,-5.60383084497428E-34,
1.)) ;
#57553 = DIRECTION('ref_axis',(-0.707106781186485,0.70710678118661,-1.07310884363324E-16)) ;
#57554 = DIRECTION('',(-1.,0.,-1.51760508056877E-16)) ;
#57555 = DIRECTION('center_axis',(-1.51760508056877E-16,-5.60383084497428E-34,
1.)) ;
#57556 = DIRECTION('ref_axis',(0.382683432365058,0.9238795325113,5.80762321206707E-17)) ;
#57557 = DIRECTION('',(-0.707106781186555,0.70710678118654,-1.07310884363335E-16)) ;
#57558 = DIRECTION('center_axis',(-1.51760508056877E-16,-5.60383084497428E-34,
1.)) ;
#57559 = DIRECTION('ref_axis',(0.923879532511287,0.38268343236509,1.40208427237263E-16)) ;
#57560 = DIRECTION('',(-1.1311821873082E-49,1.,5.60383084497428E-34)) ;
#57561 = DIRECTION('center_axis',(-1.51760508056877E-16,-5.60383084497428E-34,
1.)) ;
#57562 = DIRECTION('ref_axis',(0.923879532511283,-0.382683432365099,1.40208427237262E-16)) ;
#57563 = DIRECTION('',(0.707106781186555,0.70710678118654,1.07310884363335E-16)) ;
#57564 = DIRECTION('center_axis',(-1.51760508056877E-16,-5.60383084497428E-34,
1.)) ;
#57565 = DIRECTION('ref_axis',(0.382683432365031,-0.923879532511311,5.80762321206666E-17)) ;
#57566 = DIRECTION('',(1.,0.,1.51760508056877E-16)) ;
#57567 = DIRECTION('',(-1.1311821873082E-49,1.,5.60383084497428E-34)) ;
#57568 = DIRECTION('',(-1.,-3.55271367880051E-14,-1.51760508056877E-16)) ;
#57569 = DIRECTION('',(0.,-1.,-5.60383084497428E-34)) ;
#57570 = DIRECTION('',(1.,0.,1.51760508056877E-16)) ;
#57571 = DIRECTION('center_axis',(-1.4923676700635E-16,0.,1.)) ;
#57572 = DIRECTION('ref_axis',(-1.,0.,-1.4923676700635E-16)) ;
#57573 = DIRECTION('center_axis',(-1.4923676700635E-16,0.,1.)) ;
#57574 = DIRECTION('ref_axis',(-1.,0.,-1.4923676700635E-16)) ;
#57575 = DIRECTION('',(1.,1.77635683940026E-14,1.51760508056877E-16)) ;
#57576 = DIRECTION('',(0.,1.,5.60383084497428E-34)) ;
#57577 = DIRECTION('',(-1.,0.,-1.51760508056877E-16)) ;
#57578 = DIRECTION('center_axis',(-1.51760508056877E-16,-5.60383084497428E-34,
1.)) ;
#57579 = DIRECTION('ref_axis',(0.38268343236499,0.923879532511328,5.80762321206604E-17)) ;
#57580 = DIRECTION('',(-0.707106781186555,0.70710678118654,-1.07310884363335E-16)) ;
#57581 = DIRECTION('center_axis',(-1.51760508056877E-16,-5.60383084497428E-34,
1.)) ;
#57582 = DIRECTION('ref_axis',(0.92387953251129,0.382683432365082,1.40208427237263E-16)) ;
#57583 = DIRECTION('',(0.,1.,5.60383084497428E-34)) ;
#57584 = DIRECTION('center_axis',(-1.51760508056877E-16,-5.60383084497428E-34,
1.)) ;
#57585 = DIRECTION('ref_axis',(0.92387953251129,-0.382683432365082,1.40208427237263E-16)) ;
#57586 = DIRECTION('',(0.707106781186555,0.70710678118654,1.07310884363335E-16)) ;
#57587 = DIRECTION('center_axis',(-1.51760508056877E-16,-5.60383084497428E-34,
1.)) ;
#57588 = DIRECTION('ref_axis',(0.382683432365017,-0.923879532511317,5.80762321206645E-17)) ;
#57589 = DIRECTION('',(1.,0.,1.51760508056877E-16)) ;
#57590 = DIRECTION('',(0.,1.,5.60383084497428E-34)) ;
#57591 = DIRECTION('',(-1.,0.,-1.51760508056877E-16)) ;
#57592 = DIRECTION('',(-3.17206578464331E-15,-1.,-4.81954698151804E-31)) ;
#57593 = DIRECTION('center_axis',(-1.4923676700635E-16,0.,1.)) ;
#57594 = DIRECTION('ref_axis',(-1.,0.,-1.4923676700635E-16)) ;
#57595 = DIRECTION('center_axis',(-1.51760508056877E-16,-5.60383084497428E-34,
1.)) ;
#57596 = DIRECTION('ref_axis',(1.,2.80191542248707E-35,1.51760508056877E-16)) ;
#57597 = DIRECTION('center_axis',(-1.51760508056877E-16,-5.60383084497428E-34,
1.)) ;
#57598 = DIRECTION('ref_axis',(-0.707106781186469,0.707106781186626,-1.07310884363322E-16)) ;
#57599 = DIRECTION('',(-1.,0.,-1.51760508056877E-16)) ;
#57600 = DIRECTION('center_axis',(-1.51760508056877E-16,-5.60383084497428E-34,
1.)) ;
#57601 = DIRECTION('ref_axis',(0.707106781186485,0.70710678118661,1.07310884363324E-16)) ;
#57602 = DIRECTION('',(-1.11022302462516E-15,1.,-1.67927627189059E-31)) ;
#57603 = DIRECTION('center_axis',(-1.51760508056877E-16,-5.60383084497428E-34,
1.)) ;
#57604 = DIRECTION('ref_axis',(0.707106781186485,-0.70710678118661,1.07310884363324E-16)) ;
#57605 = DIRECTION('',(1.,0.,1.51760508056877E-16)) ;
#57606 = DIRECTION('center_axis',(-1.51760508056877E-16,-5.60383084497428E-34,
1.)) ;
#57607 = DIRECTION('ref_axis',(-0.707106781186485,-0.70710678118661,-1.07310884363324E-16)) ;
#57608 = DIRECTION('',(-5.55111512312578E-16,-1.,-8.48043882212758E-32)) ;
#57609 = DIRECTION('center_axis',(-1.51760508056877E-16,-5.60383084497428E-34,
1.)) ;
#57610 = DIRECTION('ref_axis',(0.707106781186485,-0.70710678118661,1.07310884363324E-16)) ;
#57611 = DIRECTION('',(1.,0.,1.51760508056877E-16)) ;
#57612 = DIRECTION('center_axis',(-1.51760508056877E-16,-5.60383084497428E-34,
1.)) ;
#57613 = DIRECTION('ref_axis',(-0.707106781186359,-0.707106781186736,-1.07310884363305E-16)) ;
#57614 = DIRECTION('',(0.,-1.,-5.60383084497428E-34)) ;
#57615 = DIRECTION('center_axis',(-1.51760508056877E-16,-5.60383084497428E-34,
1.)) ;
#57616 = DIRECTION('ref_axis',(-0.707106781186485,0.70710678118661,-1.07310884363324E-16)) ;
#57617 = DIRECTION('',(-1.,0.,-1.51760508056877E-16)) ;
#57618 = DIRECTION('',(0.,-1.,-5.60383084497428E-34)) ;
#57619 = DIRECTION('center_axis',(-1.51760508056877E-16,-5.60383084497428E-34,
1.)) ;
#57620 = DIRECTION('ref_axis',(-0.707106781186485,0.70710678118661,-1.07310884363324E-16)) ;
#57621 = DIRECTION('',(-1.,0.,-1.51760508056877E-16)) ;
#57622 = DIRECTION('center_axis',(-1.51760508056877E-16,-5.60383084497428E-34,
1.)) ;
#57623 = DIRECTION('ref_axis',(0.70710678118661,0.707106781186485,1.07310884363343E-16)) ;
#57624 = DIRECTION('',(0.,1.,5.60383084497428E-34)) ;
#57625 = DIRECTION('',(-1.,0.,-1.51760508056877E-16)) ;
#57626 = DIRECTION('center_axis',(-1.51760508056877E-16,-5.60383084497428E-34,
1.)) ;
#57627 = DIRECTION('ref_axis',(0.707106781186359,0.707106781186736,1.07310884363305E-16)) ;
#57628 = DIRECTION('',(0.,1.,5.60383084497428E-34)) ;
#57629 = DIRECTION('',(0.,-1.,-5.60383084497428E-34)) ;
#57630 = DIRECTION('',(-1.,0.,-1.51760508056877E-16)) ;
#57631 = DIRECTION('',(0.,1.,5.60383084497428E-34)) ;
#57632 = DIRECTION('',(1.,0.,1.51760508056877E-16)) ;
#57633 = DIRECTION('center_axis',(0.707106781186552,0.707106781186543,1.07310884363334E-16)) ;
#57634 = DIRECTION('ref_axis',(0.499999999999936,-0.499999999999943,0.707106781186633)) ;
#57635 = DIRECTION('center_axis',(-0.38268343236509,0.923879532511287,0.)) ;
#57636 = DIRECTION('ref_axis',(-0.923879532511287,-0.38268343236509,-1.16152464241352E-16)) ;
#57637 = DIRECTION('center_axis',(-1.,-5.23364152894628E-14,0.)) ;
#57638 = DIRECTION('ref_axis',(5.23364152894628E-14,-1.,-1.51760508056887E-16)) ;
#57639 = DIRECTION('center_axis',(-1.,0.,-1.51760508056877E-16)) ;
#57640 = DIRECTION('ref_axis',(-1.07310884363329E-16,0.707106781186574,0.707106781186521)) ;
#57641 = DIRECTION('center_axis',(-0.38268343236511,-0.923879532511278,0.)) ;
#57642 = DIRECTION('ref_axis',(0.923879532511278,-0.38268343236511,1.64264390233177E-16)) ;
#57643 = DIRECTION('center_axis',(0.707106781186552,-0.707106781186543,1.07310884363334E-16)) ;
#57644 = DIRECTION('ref_axis',(-0.500000000000041,-0.500000000000047,0.707106781186485)) ;
#57645 = DIRECTION('',(0.707106781186552,-0.707106781186543,1.07310884363334E-16)) ;
#57646 = DIRECTION('center_axis',(0.707106781186543,0.707106781186552,0.)) ;
#57647 = DIRECTION('ref_axis',(0.707106781186552,-0.707106781186543,1.25737296900294E-34)) ;
#57648 = DIRECTION('center_axis',(0.,1.,5.60383084497428E-34)) ;
#57649 = DIRECTION('ref_axis',(0.707106781186521,-3.9625067911038E-34,0.707106781186574)) ;
#57650 = DIRECTION('center_axis',(-0.707106781186574,0.707106781186521,0.)) ;
#57651 = DIRECTION('ref_axis',(-0.707106781186521,-0.707106781186574,-7.92501358220702E-34)) ;
#57652 = DIRECTION('center_axis',(-0.707106781186574,-0.707106781186521,0.)) ;
#57653 = DIRECTION('ref_axis',(0.707106781186521,-0.707106781186574,-7.92501358220702E-34)) ;
#57654 = DIRECTION('center_axis',(-1.,0.,-1.51760508056877E-16)) ;
#57655 = DIRECTION('ref_axis',(-1.07310884363329E-16,0.707106781186574,0.707106781186521)) ;
#57656 = DIRECTION('center_axis',(-0.707106781186574,-0.707106781186521,0.)) ;
#57657 = DIRECTION('ref_axis',(0.707106781186521,-0.707106781186574,2.14621768726675E-16)) ;
#57658 = DIRECTION('center_axis',(0.,-1.,-5.60383084497428E-34)) ;
#57659 = DIRECTION('ref_axis',(-0.707106781186574,-3.96250679110351E-34,0.707106781186521)) ;
#57660 = DIRECTION('',(0.,-1.,-5.60383084497428E-34)) ;
#57661 = DIRECTION('center_axis',(0.707106781186574,-0.707106781186521,0.)) ;
#57662 = DIRECTION('ref_axis',(0.707106781186521,0.707106781186574,7.92501358220702E-34)) ;
#57663 = DIRECTION('center_axis',(1.,0.,1.51760508056877E-16)) ;
#57664 = DIRECTION('ref_axis',(-1.07310884363329E-16,-0.707106781186574,0.707106781186521)) ;
#57665 = DIRECTION('',(1.,0.,1.51760508056877E-16)) ;
#57666 = DIRECTION('center_axis',(0.,1.,0.)) ;
#57667 = DIRECTION('ref_axis',(1.,0.,0.)) ;
#57668 = DIRECTION('',(0.,0.,-1.)) ;
#57669 = DIRECTION('center_axis',(-0.707106781186552,0.707106781186543,-1.07310884363334E-16)) ;
#57670 = DIRECTION('ref_axis',(0.499999999999936,0.499999999999943,0.707106781186633)) ;
#57671 = DIRECTION('center_axis',(-1.,-5.23364152894628E-14,7.40148683083464E-14)) ;
#57672 = DIRECTION('ref_axis',(5.23364152894683E-14,-1.,7.41666288163964E-14)) ;
#57673 = DIRECTION('center_axis',(-0.3826834323651,-0.923879532511283,0.)) ;
#57674 = DIRECTION('ref_axis',(0.923879532511282,-0.3826834323651,1.16152464241351E-16)) ;
#57675 = DIRECTION('center_axis',(-0.707106781186552,-0.707106781186543,-1.07310884363334E-16)) ;
#57676 = DIRECTION('ref_axis',(-0.500000000000041,0.500000000000047,0.707106781186485)) ;
#57677 = DIRECTION('center_axis',(0.38268343236508,-0.923879532511291,0.)) ;
#57678 = DIRECTION('ref_axis',(0.923879532511291,0.38268343236508,1.16152464241352E-16)) ;
#57679 = DIRECTION('center_axis',(1.,0.,1.51760508056877E-16)) ;
#57680 = DIRECTION('ref_axis',(-1.07310884363329E-16,-0.707106781186574,0.707106781186521)) ;
#57681 = DIRECTION('',(1.,0.,1.51760508056877E-16)) ;
#57682 = DIRECTION('center_axis',(0.,1.,0.)) ;
#57683 = DIRECTION('ref_axis',(1.,0.,1.77819390572528E-34)) ;
#57684 = DIRECTION('center_axis',(1.,0.,0.)) ;
#57685 = DIRECTION('ref_axis',(0.,-1.,0.)) ;
#57686 = DIRECTION('',(0.,0.,-1.)) ;
#57687 = DIRECTION('',(0.,0.,-1.)) ;
#57688 = DIRECTION('',(0.,0.,-1.)) ;
#57689 = DIRECTION('center_axis',(1.4923676700635E-16,0.,-1.)) ;
#57690 = DIRECTION('ref_axis',(-1.,0.,0.)) ;
#57691 = DIRECTION('center_axis',(-1.4923676700635E-16,0.,1.)) ;
#57692 = DIRECTION('ref_axis',(1.,0.,1.4923676700635E-16)) ;
#57693 = DIRECTION('center_axis',(0.,-1.,0.)) ;
#57694 = DIRECTION('ref_axis',(1.,0.,0.)) ;
#57695 = DIRECTION('center_axis',(1.4923676700635E-16,0.,-1.)) ;
#57696 = DIRECTION('ref_axis',(1.,0.,1.4923676700635E-16)) ;
#57697 = DIRECTION('center_axis',(-1.4923676700635E-16,0.,1.)) ;
#57698 = DIRECTION('ref_axis',(1.,0.,1.4923676700635E-16)) ;
#57699 = DIRECTION('center_axis',(-1.4923676700635E-16,0.,1.)) ;
#57700 = DIRECTION('ref_axis',(1.,0.,1.4923676700635E-16)) ;
#57701 = DIRECTION('center_axis',(-1.4923676700635E-16,0.,1.)) ;
#57702 = DIRECTION('ref_axis',(1.,0.,1.4923676700635E-16)) ;
#57703 = DIRECTION('center_axis',(0.,0.,1.)) ;
#57704 = DIRECTION('ref_axis',(1.,0.,0.)) ;
#57705 = DIRECTION('',(0.,0.,1.)) ;
#57706 = DIRECTION('center_axis',(1.4923676700635E-16,0.,-1.)) ;
#57707 = DIRECTION('ref_axis',(1.,0.,1.4923676700635E-16)) ;
#57708 = DIRECTION('center_axis',(-1.4923676700635E-16,0.,1.)) ;
#57709 = DIRECTION('ref_axis',(1.,0.,0.)) ;
#57710 = DIRECTION('center_axis',(1.4923676700635E-16,0.,-1.)) ;
#57711 = DIRECTION('ref_axis',(1.,0.,1.4923676700635E-16)) ;
#57712 = DIRECTION('center_axis',(0.,-1.,0.)) ;
#57713 = DIRECTION('ref_axis',(-1.,0.,0.)) ;
#57714 = DIRECTION('center_axis',(0.,0.,1.)) ;
#57715 = DIRECTION('ref_axis',(1.,0.,0.)) ;
#57716 = DIRECTION('center_axis',(-1.51760508056877E-16,-5.60383084497428E-34,
1.)) ;
#57717 = DIRECTION('ref_axis',(1.,1.86794361499138E-35,1.51760508056877E-16)) ;
#57718 = DIRECTION('',(0.,0.,-1.)) ;
#57719 = DIRECTION('center_axis',(-1.51760508056877E-16,-5.60383084497428E-34,
1.)) ;
#57720 = DIRECTION('ref_axis',(1.,0.,0.)) ;
#57721 = DIRECTION('center_axis',(1.51760508056877E-16,5.60383084497428E-34,
-1.)) ;
#57722 = DIRECTION('ref_axis',(1.,1.86794361499138E-35,1.51760508056877E-16)) ;
#57723 = DIRECTION('center_axis',(0.,1.,5.60383084497428E-34)) ;
#57724 = DIRECTION('ref_axis',(-1.,0.,0.)) ;
#57725 = DIRECTION('center_axis',(-1.51760508056877E-16,-5.60383084497428E-34,
1.)) ;
#57726 = DIRECTION('ref_axis',(1.,1.81422958079369E-66,1.51760508056877E-16)) ;
#57727 = DIRECTION('',(-1.,0.,-1.51760508056877E-16)) ;
#57728 = DIRECTION('center_axis',(1.51760508056877E-16,5.60383084497428E-34,
-1.)) ;
#57729 = DIRECTION('ref_axis',(-0.707106781186614,0.707106781186481,-1.07310884363344E-16)) ;
#57730 = DIRECTION('',(-1.1311821873082E-49,1.,5.60383084497428E-34)) ;
#57731 = DIRECTION('',(-1.,0.,-1.51760508056877E-16)) ;
#57732 = DIRECTION('',(1.1311821873082E-49,-1.,-5.60383084497428E-34)) ;
#57733 = DIRECTION('',(1.1311821873082E-49,-1.,-5.60383084497428E-34)) ;
#57734 = DIRECTION('',(-1.,0.,-1.51760508056877E-16)) ;
#57735 = DIRECTION('center_axis',(1.51760508056877E-16,5.60383084497428E-34,
-1.)) ;
#57736 = DIRECTION('ref_axis',(0.382683432365032,-0.923879532511311,5.80762321206668E-17)) ;
#57737 = DIRECTION('',(-0.707106781186555,-0.70710678118654,-1.07310884363335E-16)) ;
#57738 = DIRECTION('center_axis',(1.51760508056877E-16,5.60383084497428E-34,
-1.)) ;
#57739 = DIRECTION('ref_axis',(0.923879532511313,-0.382683432365025,1.40208427237267E-16)) ;
#57740 = DIRECTION('',(1.1311821873082E-49,-1.,-5.60383084497428E-34)) ;
#57741 = DIRECTION('center_axis',(1.51760508056877E-16,5.60383084497428E-34,
-1.)) ;
#57742 = DIRECTION('ref_axis',(0.923879532511313,0.382683432365025,1.40208427237267E-16)) ;
#57743 = DIRECTION('',(0.707106781186555,-0.70710678118654,1.07310884363335E-16)) ;
#57744 = DIRECTION('',(-1.,0.,-1.51760508056877E-16)) ;
#57745 = DIRECTION('center_axis',(-1.51760508056877E-16,-5.60383084497428E-34,
1.)) ;
#57746 = DIRECTION('ref_axis',(1.19824467136135E-15,-1.,1.81285837017747E-31)) ;
#57747 = DIRECTION('',(1.,-3.19495806435525E-17,1.51760508056877E-16)) ;
#57748 = DIRECTION('center_axis',(-1.51760508056877E-16,-5.60383084497428E-34,
1.)) ;
#57749 = DIRECTION('ref_axis',(8.7871275899832E-16,-1.,1.32793511657148E-31)) ;
#57750 = DIRECTION('',(0.,1.,5.60383084497428E-34)) ;
#57751 = DIRECTION('',(-1.,0.,-1.51760508056877E-16)) ;
#57752 = DIRECTION('',(0.,1.,5.60383084497428E-34)) ;
#57753 = DIRECTION('center_axis',(-1.51760508056877E-16,-5.60383084497428E-34,
1.)) ;
#57754 = DIRECTION('ref_axis',(1.67754253990588E-15,-1.,2.54024325058643E-31)) ;
#57755 = DIRECTION('',(1.,-3.19495806435525E-17,1.51760508056877E-16)) ;
#57756 = DIRECTION('center_axis',(-1.51760508056877E-16,-5.60383084497428E-34,
1.)) ;
#57757 = DIRECTION('ref_axis',(7.18946802816807E-16,-1.,1.08547348976849E-31)) ;
#57758 = DIRECTION('',(-1.,0.,-1.51760508056877E-16)) ;
#57759 = DIRECTION('',(0.,1.,5.60383084497428E-34)) ;
#57760 = DIRECTION('center_axis',(1.51760508056877E-16,5.60383084497428E-34,
-1.)) ;
#57761 = DIRECTION('ref_axis',(-0.923879532511284,-0.382683432365097,-1.40208427237262E-16)) ;
#57762 = DIRECTION('',(-0.707106781186615,0.70710678118648,-1.07310884363344E-16)) ;
#57763 = DIRECTION('center_axis',(-1.51760508056877E-16,-5.60383084497428E-34,
1.)) ;
#57764 = DIRECTION('ref_axis',(0.923879532511263,0.382683432365148,1.40208427237259E-16)) ;
#57765 = DIRECTION('',(-6.83214169000096E-16,1.,-1.03124546314615E-31)) ;
#57766 = DIRECTION('center_axis',(-1.51760508056877E-16,-5.60383084497428E-34,
1.)) ;
#57767 = DIRECTION('ref_axis',(0.718421208107084,-0.695608343640269,1.09027967541166E-16)) ;
#57768 = DIRECTION('center_axis',(1.51760508056877E-16,5.60383084497428E-34,
-1.)) ;
#57769 = DIRECTION('ref_axis',(-0.718421208107087,0.695608343640265,-1.09027967541167E-16)) ;
#57770 = DIRECTION('',(0.,1.,5.60383084497428E-34)) ;
#57771 = DIRECTION('center_axis',(1.51760508056877E-16,5.60383084497428E-34,
-1.)) ;
#57772 = DIRECTION('ref_axis',(-0.718421208107092,-0.69560834364026,-1.09027967541168E-16)) ;
#57773 = DIRECTION('center_axis',(-1.51760508056877E-16,-5.60383084497428E-34,
1.)) ;
#57774 = DIRECTION('ref_axis',(0.718421208107098,0.695608343640254,1.09027967541169E-16)) ;
#57775 = DIRECTION('',(-6.83214169000096E-16,1.,-1.03124546314615E-31)) ;
#57776 = DIRECTION('center_axis',(-1.51760508056877E-16,-5.60383084497428E-34,
1.)) ;
#57777 = DIRECTION('ref_axis',(0.923879532511288,-0.382683432365087,1.40208427237263E-16)) ;
#57778 = DIRECTION('',(0.707106781186521,0.707106781186574,1.0731088436333E-16)) ;
#57779 = DIRECTION('center_axis',(1.51760508056877E-16,5.60383084497428E-34,
-1.)) ;
#57780 = DIRECTION('ref_axis',(-0.923879532511292,0.382683432365076,-1.40208427237264E-16)) ;
#57781 = DIRECTION('',(-5.23472275150178E-15,1.,-7.93863801220309E-31)) ;
#57782 = DIRECTION('center_axis',(-1.51760508056877E-16,-5.60383084497428E-34,
1.)) ;
#57783 = DIRECTION('ref_axis',(0.642787609686539,-0.766044443118978,9.75497742186947E-17)) ;
#57784 = DIRECTION('',(0.984807753012209,-0.173648177666924,1.49454924935485E-16)) ;
#57785 = DIRECTION('center_axis',(-1.51760508056877E-16,-5.60383084497428E-34,
1.)) ;
#57786 = DIRECTION('ref_axis',(-0.537299608346822,-0.843391445812887,-8.15408615414747E-17)) ;
#57787 = DIRECTION('',(0.573576436351042,-0.819152044288994,8.70462513900874E-17)) ;
#57788 = DIRECTION('center_axis',(-1.51760508056877E-16,-5.60383084497428E-34,
1.)) ;
#57789 = DIRECTION('ref_axis',(-0.953716950748229,-0.300705799504266,-1.44736568988007E-16)) ;
#57790 = DIRECTION('',(-5.25359141716359E-35,-1.,-5.60383084497428E-34)) ;
#57791 = DIRECTION('center_axis',(1.51760508056877E-16,5.60383084497428E-34,
-1.)) ;
#57792 = DIRECTION('ref_axis',(0.707106781186547,0.707106781186547,1.07310884363333E-16)) ;
#57793 = DIRECTION('',(1.,0.,1.51760508056877E-16)) ;
#57794 = DIRECTION('center_axis',(-1.51760508056877E-16,-5.60383084497428E-34,
1.)) ;
#57795 = DIRECTION('ref_axis',(-0.707106781186548,-0.707106781186548,-1.07310884363333E-16)) ;
#57796 = DIRECTION('',(-2.22044604925032E-15,-1.,-3.37536403631613E-31)) ;
#57797 = DIRECTION('',(-1.,0.,-1.51760508056877E-16)) ;
#57798 = DIRECTION('',(-2.33146835171284E-14,1.,-3.53768783266021E-30)) ;
#57799 = DIRECTION('center_axis',(-1.51760508056877E-16,-5.60383084497428E-34,
1.)) ;
#57800 = DIRECTION('ref_axis',(0.707106781186544,-0.707106781186551,1.07310884363333E-16)) ;
#57801 = DIRECTION('',(1.,0.,1.51760508056877E-16)) ;
#57802 = DIRECTION('center_axis',(-1.51760508056877E-16,-5.60383084497428E-34,
1.)) ;
#57803 = DIRECTION('ref_axis',(-0.70710678118657,-0.707106781186525,-1.07310884363337E-16)) ;
#57804 = DIRECTION('',(2.22044604925031E-16,-1.,3.31372189702139E-32)) ;
#57805 = DIRECTION('center_axis',(1.51760508056877E-16,5.60383084497428E-34,
-1.)) ;
#57806 = DIRECTION('ref_axis',(1.,1.86794361499143E-34,1.51760508056877E-16)) ;
#57807 = DIRECTION('',(1.,0.,1.51760508056877E-16)) ;
#57808 = DIRECTION('',(0.,-1.,-5.60383084497428E-34)) ;
#57809 = DIRECTION('center_axis',(1.51760508056877E-16,5.60383084497428E-34,
-1.)) ;
#57810 = DIRECTION('ref_axis',(0.707106781186592,0.707106781186503,1.0731088436334E-16)) ;
#57811 = DIRECTION('',(1.,0.,1.51760508056877E-16)) ;
#57812 = DIRECTION('center_axis',(1.51760508056877E-16,5.60383084497428E-34,
-1.)) ;
#57813 = DIRECTION('ref_axis',(-0.707106781186592,0.707106781186503,-1.0731088436334E-16)) ;
#57814 = DIRECTION('',(0.,1.,5.60383084497428E-34)) ;
#57815 = DIRECTION('',(1.,0.,1.51760508056877E-16)) ;
#57816 = DIRECTION('center_axis',(1.51760508056877E-16,5.60383084497428E-34,
-1.)) ;
#57817 = DIRECTION('ref_axis',(-0.707106781186592,0.707106781186503,-1.0731088436334E-16)) ;
#57818 = DIRECTION('',(0.,1.,5.60383084497428E-34)) ;
#57819 = DIRECTION('center_axis',(1.51760508056877E-16,5.60383084497428E-34,
-1.)) ;
#57820 = DIRECTION('ref_axis',(-0.707106781186592,-0.707106781186503,-1.0731088436334E-16)) ;
#57821 = DIRECTION('',(-1.,0.,-1.51760508056877E-16)) ;
#57822 = DIRECTION('center_axis',(1.51760508056877E-16,5.60383084497428E-34,
-1.)) ;
#57823 = DIRECTION('ref_axis',(0.707106781186592,-0.707106781186503,1.0731088436334E-16)) ;
#57824 = DIRECTION('',(0.,-1.,-5.60383084497428E-34)) ;
#57825 = DIRECTION('center_axis',(1.51760508056877E-16,5.60383084497428E-34,
-1.)) ;
#57826 = DIRECTION('ref_axis',(0.707106781186592,0.707106781186503,1.0731088436334E-16)) ;
#57827 = DIRECTION('center_axis',(1.51760508056877E-16,5.60383084497428E-34,
-1.)) ;
#57828 = DIRECTION('ref_axis',(1.,-2.24153233798967E-35,1.51760508056877E-16)) ;
#57829 = DIRECTION('center_axis',(-1.51760508056877E-16,-5.60383084497428E-34,
1.)) ;
#57830 = DIRECTION('ref_axis',(1.,-8.50440216098095E-50,1.51760508056877E-16)) ;
#57831 = DIRECTION('',(-1.,0.,-1.51760508056877E-16)) ;
#57832 = DIRECTION('',(-7.105427357601E-15,-1.,-1.07888364883526E-30)) ;
#57833 = DIRECTION('center_axis',(1.51760508056877E-16,5.60383084497428E-34,
-1.)) ;
#57834 = DIRECTION('ref_axis',(0.707106781186359,0.707106781186736,1.07310884363305E-16)) ;
#57835 = DIRECTION('',(1.,0.,1.51760508056877E-16)) ;
#57836 = DIRECTION('center_axis',(1.51760508056877E-16,5.60383084497428E-34,
-1.)) ;
#57837 = DIRECTION('ref_axis',(-0.38268343236507,0.923879532511295,-5.80762321206726E-17)) ;
#57838 = DIRECTION('',(0.707106781186563,0.707106781186532,1.07310884363336E-16)) ;
#57839 = DIRECTION('center_axis',(1.51760508056877E-16,5.60383084497428E-34,
-1.)) ;
#57840 = DIRECTION('ref_axis',(-0.923879532511313,0.382683432365025,-1.40208427237267E-16)) ;
#57841 = DIRECTION('',(3.73034936274055E-14,1.,5.66175752827605E-30)) ;
#57842 = DIRECTION('center_axis',(1.51760508056877E-16,5.60383084497428E-34,
-1.)) ;
#57843 = DIRECTION('ref_axis',(-0.923879532511313,-0.382683432365025,-1.40208427237267E-16)) ;
#57844 = DIRECTION('',(-0.707106781186575,0.70710678118652,-1.07310884363338E-16)) ;
#57845 = DIRECTION('center_axis',(1.51760508056877E-16,5.60383084497428E-34,
-1.)) ;
#57846 = DIRECTION('ref_axis',(-0.382683432364994,-0.923879532511326,-5.8076232120661E-17)) ;
#57847 = DIRECTION('',(-1.,7.10542735760144E-15,-1.51760508056877E-16)) ;
#57848 = DIRECTION('center_axis',(1.51760508056877E-16,5.60383084497428E-34,
-1.)) ;
#57849 = DIRECTION('ref_axis',(0.707106781186485,-0.70710678118661,1.07310884363324E-16)) ;
#57850 = DIRECTION('',(-7.105427357601E-15,-1.,-1.07888364883526E-30)) ;
#57851 = DIRECTION('',(1.,-3.55271367880051E-14,1.51760508056877E-16)) ;
#57852 = DIRECTION('',(7.105427357601E-15,1.,1.07888364883526E-30)) ;
#57853 = DIRECTION('center_axis',(-1.51760508056877E-16,-5.60383084497428E-34,
1.)) ;
#57854 = DIRECTION('ref_axis',(1.,-8.50440216098095E-50,1.51760508056877E-16)) ;
#57855 = DIRECTION('',(-1.,0.,-1.51760508056877E-16)) ;
#57856 = DIRECTION('center_axis',(1.51760508056877E-16,5.60383084497428E-34,
-1.)) ;
#57857 = DIRECTION('ref_axis',(-0.382683432365099,0.923879532511283,-5.80762321206769E-17)) ;
#57858 = DIRECTION('',(0.707106781186563,0.707106781186532,1.07310884363336E-16)) ;
#57859 = DIRECTION('center_axis',(1.51760508056877E-16,5.60383084497428E-34,
-1.)) ;
#57860 = DIRECTION('ref_axis',(-0.923879532511297,0.382683432365065,-1.40208427237264E-16)) ;
#57861 = DIRECTION('',(-3.73034936274055E-14,-1.,-5.66175752827605E-30)) ;
#57862 = DIRECTION('center_axis',(1.51760508056877E-16,5.60383084497428E-34,
-1.)) ;
#57863 = DIRECTION('ref_axis',(-0.923879532511297,-0.382683432365065,-1.40208427237264E-16)) ;
#57864 = DIRECTION('',(-0.707106781186544,0.707106781186551,-1.07310884363333E-16)) ;
#57865 = DIRECTION('center_axis',(1.51760508056877E-16,5.60383084497428E-34,
-1.)) ;
#57866 = DIRECTION('ref_axis',(-0.382683432365045,-0.923879532511305,-5.80762321206688E-17)) ;
#57867 = DIRECTION('',(1.,-7.10542735760144E-15,1.51760508056877E-16)) ;
#57868 = DIRECTION('center_axis',(1.51760508056877E-16,5.60383084497428E-34,
-1.)) ;
#57869 = DIRECTION('ref_axis',(0.707106781186548,-0.707106781186548,1.07310884363333E-16)) ;
#57870 = DIRECTION('',(7.105427357601E-15,1.,1.07888364883526E-30)) ;
#57871 = DIRECTION('',(7.105427357601E-15,1.,1.07888364883526E-30)) ;
#57872 = DIRECTION('',(7.105427357601E-15,1.,1.07888364883526E-30)) ;
#57873 = DIRECTION('center_axis',(1.51760508056877E-16,5.60383084497428E-34,
-1.)) ;
#57874 = DIRECTION('ref_axis',(0.707106781186296,0.707106781186799,1.07310884363295E-16)) ;
#57875 = DIRECTION('center_axis',(1.51760508056877E-16,5.60383084497428E-34,
-1.)) ;
#57876 = DIRECTION('ref_axis',(-0.707106781186469,0.707106781186626,-1.07310884363321E-16)) ;
#57877 = DIRECTION('',(5.55111512312578E-16,1.,8.48043882212758E-32)) ;
#57878 = DIRECTION('center_axis',(1.51760508056877E-16,5.60383084497428E-34,
-1.)) ;
#57879 = DIRECTION('ref_axis',(-0.707106781186485,-0.70710678118661,-1.07310884363324E-16)) ;
#57880 = DIRECTION('',(-1.,0.,-1.51760508056877E-16)) ;
#57881 = DIRECTION('center_axis',(1.51760508056877E-16,5.60383084497428E-34,
-1.)) ;
#57882 = DIRECTION('ref_axis',(0.707106781186485,-0.70710678118661,1.07310884363324E-16)) ;
#57883 = DIRECTION('',(1.11022302462516E-15,-1.,1.67927627189059E-31)) ;
#57884 = DIRECTION('center_axis',(1.51760508056877E-16,5.60383084497428E-34,
-1.)) ;
#57885 = DIRECTION('ref_axis',(0.707106781186485,0.70710678118661,1.07310884363324E-16)) ;
#57886 = DIRECTION('',(1.,0.,1.51760508056877E-16)) ;
#57887 = DIRECTION('',(0.,-1.,-5.60383084497428E-34)) ;
#57888 = DIRECTION('',(0.,-1.,-5.60383084497428E-34)) ;
#57889 = DIRECTION('',(0.,-1.,-5.60383084497428E-34)) ;
#57890 = DIRECTION('',(-1.,0.,-1.51760508056877E-16)) ;
#57891 = DIRECTION('center_axis',(1.51760508056877E-16,5.60383084497428E-34,
-1.)) ;
#57892 = DIRECTION('ref_axis',(0.382683432364994,-0.923879532511326,5.8076232120661E-17)) ;
#57893 = DIRECTION('',(-0.707106781186555,-0.70710678118654,-1.07310884363335E-16)) ;
#57894 = DIRECTION('center_axis',(1.51760508056877E-16,5.60383084497428E-34,
-1.)) ;
#57895 = DIRECTION('ref_axis',(0.923879532511313,-0.382683432365025,1.40208427237267E-16)) ;
#57896 = DIRECTION('',(0.,-1.,-5.60383084497428E-34)) ;
#57897 = DIRECTION('center_axis',(1.51760508056877E-16,5.60383084497428E-34,
-1.)) ;
#57898 = DIRECTION('ref_axis',(0.923879532511313,0.382683432365025,1.40208427237267E-16)) ;
#57899 = DIRECTION('',(0.707106781186555,-0.70710678118654,1.07310884363335E-16)) ;
#57900 = DIRECTION('center_axis',(1.51760508056877E-16,5.60383084497428E-34,
-1.)) ;
#57901 = DIRECTION('ref_axis',(0.382683432364994,0.923879532511326,5.8076232120661E-17)) ;
#57902 = DIRECTION('',(1.,0.,1.51760508056877E-16)) ;
#57903 = DIRECTION('',(-1.,0.,-1.51760508056877E-16)) ;
#57904 = DIRECTION('',(0.,1.,5.60383084497428E-34)) ;
#57905 = DIRECTION('',(1.,0.,1.51760508056877E-16)) ;
#57906 = DIRECTION('center_axis',(1.51760508056877E-16,5.60383084497428E-34,
-1.)) ;
#57907 = DIRECTION('ref_axis',(-0.87315164903695,0.487448661690701,-1.32509937868548E-16)) ;
#57908 = DIRECTION('',(0.,1.,5.60383084497428E-34)) ;
#57909 = DIRECTION('center_axis',(1.51760508056877E-16,5.60383084497428E-34,
-1.)) ;
#57910 = DIRECTION('ref_axis',(-0.707106781186359,-0.707106781186736,-1.07310884363305E-16)) ;
#57911 = DIRECTION('',(-1.,0.,-1.51760508056877E-16)) ;
#57912 = DIRECTION('center_axis',(1.51760508056877E-16,5.60383084497428E-34,
-1.)) ;
#57913 = DIRECTION('ref_axis',(0.873151649036935,-0.487448661690728,1.32509937868545E-16)) ;
#57914 = DIRECTION('',(0.,-1.,-5.60383084497428E-34)) ;
#57915 = DIRECTION('center_axis',(1.51760508056877E-16,5.60383084497428E-34,
-1.)) ;
#57916 = DIRECTION('ref_axis',(0.873151649036842,0.487448661690894,1.32509937868531E-16)) ;
#57917 = DIRECTION('',(1.,0.,1.51760508056877E-16)) ;
#57918 = DIRECTION('',(0.,-1.,-5.60383084497428E-34)) ;
#57919 = DIRECTION('center_axis',(1.51760508056877E-16,5.60383084497428E-34,
-1.)) ;
#57920 = DIRECTION('ref_axis',(-0.87315164903695,0.487448661690701,-1.32509937868548E-16)) ;
#57921 = DIRECTION('',(0.,1.,5.60383084497428E-34)) ;
#57922 = DIRECTION('center_axis',(1.51760508056877E-16,5.60383084497428E-34,
-1.)) ;
#57923 = DIRECTION('ref_axis',(-0.873151649036905,-0.487448661690782,-1.32509937868541E-16)) ;
#57924 = DIRECTION('',(-1.,0.,-1.51760508056877E-16)) ;
#57925 = DIRECTION('center_axis',(1.51760508056877E-16,5.60383084497428E-34,
-1.)) ;
#57926 = DIRECTION('ref_axis',(0.873151649036766,-0.48744866169103,1.3250993786852E-16)) ;
#57927 = DIRECTION('',(0.,-1.,-5.60383084497428E-34)) ;
#57928 = DIRECTION('center_axis',(1.51760508056877E-16,5.60383084497428E-34,
-1.)) ;
#57929 = DIRECTION('ref_axis',(0.873151649036827,0.487448661690921,1.32509937868529E-16)) ;
#57930 = DIRECTION('',(1.,0.,1.51760508056877E-16)) ;
#57931 = DIRECTION('',(0.,-1.,-5.60383084497428E-34)) ;
#57932 = DIRECTION('center_axis',(1.51760508056877E-16,5.60383084497428E-34,
-1.)) ;
#57933 = DIRECTION('ref_axis',(0.707106781186592,0.707106781186503,1.0731088436334E-16)) ;
#57934 = DIRECTION('',(1.,0.,1.51760508056877E-16)) ;
#57935 = DIRECTION('center_axis',(1.51760508056877E-16,5.60383084497428E-34,
-1.)) ;
#57936 = DIRECTION('ref_axis',(-0.707106781186636,0.707106781186459,-1.07310884363347E-16)) ;
#57937 = DIRECTION('',(0.,1.,5.60383084497428E-34)) ;
#57938 = DIRECTION('',(1.,0.,1.51760508056877E-16)) ;
#57939 = DIRECTION('center_axis',(1.51760508056877E-16,5.60383084497428E-34,
-1.)) ;
#57940 = DIRECTION('ref_axis',(-0.87315164903695,0.487448661690701,-1.32509937868548E-16)) ;
#57941 = DIRECTION('',(0.,1.,5.60383084497428E-34)) ;
#57942 = DIRECTION('center_axis',(1.51760508056877E-16,5.60383084497428E-34,
-1.)) ;
#57943 = DIRECTION('ref_axis',(-0.873151649036905,-0.487448661690782,-1.32509937868541E-16)) ;
#57944 = DIRECTION('',(-1.,0.,-1.51760508056877E-16)) ;
#57945 = DIRECTION('center_axis',(1.51760508056877E-16,5.60383084497428E-34,
-1.)) ;
#57946 = DIRECTION('ref_axis',(0.873151649036766,-0.48744866169103,1.3250993786852E-16)) ;
#57947 = DIRECTION('',(0.,-1.,-5.60383084497428E-34)) ;
#57948 = DIRECTION('center_axis',(1.51760508056877E-16,5.60383084497428E-34,
-1.)) ;
#57949 = DIRECTION('ref_axis',(0.873151649036935,0.487448661690728,1.32509937868545E-16)) ;
#57950 = DIRECTION('',(1.,0.,1.51760508056877E-16)) ;
#57951 = DIRECTION('',(0.,-1.,-5.60383084497428E-34)) ;
#57952 = DIRECTION('center_axis',(1.51760508056877E-16,5.60383084497428E-34,
-1.)) ;
#57953 = DIRECTION('ref_axis',(0.707106781186592,0.707106781186503,1.0731088436334E-16)) ;
#57954 = DIRECTION('',(1.,0.,1.51760508056877E-16)) ;
#57955 = DIRECTION('center_axis',(1.51760508056877E-16,5.60383084497428E-34,
-1.)) ;
#57956 = DIRECTION('ref_axis',(-0.707106781186592,0.707106781186503,-1.0731088436334E-16)) ;
#57957 = DIRECTION('',(0.,1.,5.60383084497428E-34)) ;
#57958 = DIRECTION('',(1.,0.,1.51760508056877E-16)) ;
#57959 = DIRECTION('center_axis',(-1.,-2.22044604925031E-16,0.)) ;
#57960 = DIRECTION('ref_axis',(0.,0.,1.)) ;
#57961 = DIRECTION('center_axis',(0.,0.,1.)) ;
#57962 = DIRECTION('ref_axis',(-1.,0.,0.)) ;
#57963 = DIRECTION('center_axis',(-1.,0.,-1.11022302462517E-14)) ;
#57964 = DIRECTION('ref_axis',(-1.11022302462517E-14,0.,1.)) ;
#57965 = DIRECTION('center_axis',(0.,1.,0.)) ;
#57966 = DIRECTION('ref_axis',(-0.707106781186548,0.,-0.707106781186548)) ;
#57967 = DIRECTION('center_axis',(-1.,-2.22044604925031E-16,0.)) ;
#57968 = DIRECTION('ref_axis',(-1.47241706008224E-16,0.663117692312033,0.748515147570685)) ;
#57969 = DIRECTION('center_axis',(0.,0.,1.)) ;
#57970 = DIRECTION('ref_axis',(-0.707106781186391,-0.707106781186704,0.)) ;
#57971 = DIRECTION('center_axis',(0.,0.,1.)) ;
#57972 = DIRECTION('ref_axis',(-1.,0.,0.)) ;
#57973 = DIRECTION('',(0.,0.,1.)) ;
#57974 = DIRECTION('',(0.,0.,-1.)) ;
#57975 = DIRECTION('center_axis',(0.,1.,0.)) ;
#57976 = DIRECTION('ref_axis',(0.,0.,1.)) ;
#57977 = DIRECTION('center_axis',(-1.,0.,-4.44089209850043E-14)) ;
#57978 = DIRECTION('ref_axis',(4.44089209850043E-14,0.,-1.)) ;
#57979 = DIRECTION('center_axis',(0.,1.,0.)) ;
#57980 = DIRECTION('ref_axis',(-0.707106781186549,0.,-0.707106781186546)) ;
#57981 = DIRECTION('center_axis',(0.,-1.,0.)) ;
#57982 = DIRECTION('ref_axis',(-0.707106781186549,0.,-0.707106781186546)) ;
#57983 = DIRECTION('center_axis',(-1.,0.,-1.51760508056877E-16)) ;
#57984 = DIRECTION('ref_axis',(1.07310884363305E-16,-0.707106781186736,-0.707106781186359)) ;
#57985 = DIRECTION('center_axis',(-1.,0.,0.)) ;
#57986 = DIRECTION('ref_axis',(0.,0.,-1.)) ;
#57987 = DIRECTION('',(-1.,0.,-1.51760508056877E-16)) ;
#57988 = DIRECTION('',(1.,0.,1.51760508056877E-16)) ;
#57989 = DIRECTION('center_axis',(0.,1.,0.)) ;
#57990 = DIRECTION('ref_axis',(0.,0.,1.)) ;
#57991 = DIRECTION('center_axis',(0.,0.,-1.)) ;
#57992 = DIRECTION('ref_axis',(1.,0.,0.)) ;
#57993 = DIRECTION('center_axis',(0.,1.,0.)) ;
#57994 = DIRECTION('ref_axis',(0.707106781186548,0.,-0.707106781186548)) ;
#57995 = DIRECTION('center_axis',(0.,-1.,0.)) ;
#57996 = DIRECTION('ref_axis',(0.707106781186548,0.,-0.707106781186548)) ;
#57997 = DIRECTION('center_axis',(-8.7076315656875E-16,0.,1.)) ;
#57998 = DIRECTION('ref_axis',(0.707106781186391,-0.707106781186704,6.1572253281703E-16)) ;
#57999 = DIRECTION('center_axis',(0.,0.,-1.)) ;
#58000 = DIRECTION('ref_axis',(1.,0.,0.)) ;
#58001 = DIRECTION('',(8.7076315656875E-16,0.,-1.)) ;
#58002 = DIRECTION('',(-8.7076315656875E-16,0.,1.)) ;
#58003 = DIRECTION('center_axis',(0.,1.,0.)) ;
#58004 = DIRECTION('ref_axis',(0.,0.,1.)) ;
#58005 = DIRECTION('center_axis',(0.,0.,1.)) ;
#58006 = DIRECTION('ref_axis',(-1.,0.,0.)) ;
#58007 = DIRECTION('center_axis',(0.,-1.,0.)) ;
#58008 = DIRECTION('ref_axis',(0.,0.,1.)) ;
#58009 = DIRECTION('center_axis',(0.,1.,0.)) ;
#58010 = DIRECTION('ref_axis',(0.,0.,1.)) ;
#58011 = DIRECTION('center_axis',(0.,0.,-1.)) ;
#58012 = DIRECTION('ref_axis',(-0.707106781186359,-0.707106781186736,0.)) ;
#58013 = DIRECTION('center_axis',(0.,0.,1.)) ;
#58014 = DIRECTION('ref_axis',(-1.,0.,0.)) ;
#58015 = DIRECTION('',(0.,0.,1.)) ;
#58016 = DIRECTION('',(0.,0.,-1.)) ;
#58017 = DIRECTION('center_axis',(0.,1.,0.)) ;
#58018 = DIRECTION('ref_axis',(0.,0.,1.)) ;
#58019 = DIRECTION('center_axis',(-1.,0.,0.)) ;
#58020 = DIRECTION('ref_axis',(0.,0.,-1.)) ;
#58021 = DIRECTION('center_axis',(0.,1.,0.)) ;
#58022 = DIRECTION('ref_axis',(-0.707106781186548,0.,-0.707106781186548)) ;
#58023 = DIRECTION('center_axis',(0.,-1.,0.)) ;
#58024 = DIRECTION('ref_axis',(-0.707106781186548,0.,-0.707106781186548)) ;
#58025 = DIRECTION('center_axis',(-1.,0.,-1.51760508056877E-16)) ;
#58026 = DIRECTION('ref_axis',(1.07310884363305E-16,-0.707106781186736,-0.707106781186359)) ;
#58027 = DIRECTION('center_axis',(-1.,0.,0.)) ;
#58028 = DIRECTION('ref_axis',(0.,0.,-1.)) ;
#58029 = DIRECTION('',(-1.,0.,-1.51760508056877E-16)) ;
#58030 = DIRECTION('',(1.,0.,1.51760508056877E-16)) ;
#58031 = DIRECTION('center_axis',(0.,1.,0.)) ;
#58032 = DIRECTION('ref_axis',(0.,0.,1.)) ;
#58033 = DIRECTION('center_axis',(0.,0.,-1.)) ;
#58034 = DIRECTION('ref_axis',(1.,0.,0.)) ;
#58035 = DIRECTION('center_axis',(0.,1.,0.)) ;
#58036 = DIRECTION('ref_axis',(0.707106781186549,0.,-0.707106781186546)) ;
#58037 = DIRECTION('center_axis',(0.,-1.,0.)) ;
#58038 = DIRECTION('ref_axis',(0.707106781186549,0.,-0.707106781186547)) ;
#58039 = DIRECTION('center_axis',(0.,0.,-1.)) ;
#58040 = DIRECTION('ref_axis',(0.707106781186359,-0.707106781186736,0.)) ;
#58041 = DIRECTION('center_axis',(0.,0.,-1.)) ;
#58042 = DIRECTION('ref_axis',(1.,0.,0.)) ;
#58043 = DIRECTION('',(0.,0.,-1.)) ;
#58044 = DIRECTION('',(0.,0.,1.)) ;
#58045 = DIRECTION('center_axis',(1.,0.,0.)) ;
#58046 = DIRECTION('ref_axis',(0.,0.,-1.)) ;
#58047 = DIRECTION('center_axis',(1.,0.,0.)) ;
#58048 = DIRECTION('ref_axis',(0.,0.663117692312022,0.748515147570694)) ;
#58049 = DIRECTION('center_axis',(0.,1.,0.)) ;
#58050 = DIRECTION('ref_axis',(0.707106781186548,0.,-0.707106781186548)) ;
#58051 = DIRECTION('center_axis',(1.,0.,0.)) ;
#58052 = DIRECTION('ref_axis',(0.,1.,0.)) ;
#58053 = DIRECTION('center_axis',(1.,0.,0.)) ;
#58054 = DIRECTION('ref_axis',(0.,1.,0.)) ;
#58055 = DIRECTION('',(0.,-1.,-5.60383084497428E-34)) ;
#58056 = DIRECTION('',(0.,0.,-1.)) ;
#58057 = DIRECTION('center_axis',(-1.,0.,0.)) ;
#58058 = DIRECTION('ref_axis',(0.,0.707106781186538,0.707106781186557)) ;
#58059 = DIRECTION('',(0.,1.,5.60383084497428E-34)) ;
#58060 = DIRECTION('',(0.,0.,1.)) ;
#58061 = DIRECTION('',(0.,-1.,-5.60383084497428E-34)) ;
#58062 = DIRECTION('center_axis',(0.,-1.,-5.60383084497428E-34)) ;
#58063 = DIRECTION('ref_axis',(0.707106781186549,3.96250679110365E-34,-0.707106781186546)) ;
#58064 = DIRECTION('',(0.,1.,5.60383084497428E-34)) ;
#58065 = DIRECTION('center_axis',(0.,1.,0.)) ;
#58066 = DIRECTION('ref_axis',(0.707106781186549,0.,-0.707106781186547)) ;
#58067 = DIRECTION('center_axis',(-1.51760508056877E-16,-5.60383084497428E-34,
1.)) ;
#58068 = DIRECTION('ref_axis',(1.,1.81422958079369E-66,1.51760508056877E-16)) ;
#58069 = DIRECTION('',(0.,-1.,-5.60383084497428E-34)) ;
#58070 = DIRECTION('',(-1.,0.,-1.51760508056877E-16)) ;
#58071 = DIRECTION('center_axis',(0.,1.,5.60383084497428E-34)) ;
#58072 = DIRECTION('ref_axis',(-0.707106781186546,3.96250679110366E-34,-0.707106781186549)) ;
#58073 = DIRECTION('',(0.,1.,5.60383084497428E-34)) ;
#58074 = DIRECTION('center_axis',(0.,1.,0.)) ;
#58075 = DIRECTION('ref_axis',(-0.810015401063436,0.,-0.586408603313459)) ;
#58076 = DIRECTION('center_axis',(1.,0.,0.)) ;
#58077 = DIRECTION('ref_axis',(0.,0.,1.)) ;
#58078 = DIRECTION('',(0.,1.,0.)) ;
#58079 = DIRECTION('',(0.,0.,1.)) ;
#58080 = DIRECTION('center_axis',(0.,-1.,0.)) ;
#58081 = DIRECTION('ref_axis',(-1.,0.,0.)) ;
#58082 = DIRECTION('',(0.,1.,0.)) ;
#58083 = DIRECTION('center_axis',(0.,-1.,0.)) ;
#58084 = DIRECTION('ref_axis',(0.,0.,1.)) ;
#58085 = DIRECTION('center_axis',(-1.,0.,-8.7076315656875E-16)) ;
#58086 = DIRECTION('ref_axis',(8.7076315656875E-16,0.,-1.)) ;
#58087 = DIRECTION('',(4.87960943544713E-49,-1.,-5.60383084497428E-34)) ;
#58088 = DIRECTION('',(8.7076315656875E-16,0.,-1.)) ;
#58089 = DIRECTION('center_axis',(4.87960943544713E-49,-1.,-5.60383084497428E-34)) ;
#58090 = DIRECTION('ref_axis',(0.707106781186548,3.96250679110366E-34,-0.707106781186548)) ;
#58091 = DIRECTION('',(-4.87960943544713E-49,1.,5.60383084497428E-34)) ;
#58092 = DIRECTION('center_axis',(0.,1.,0.)) ;
#58093 = DIRECTION('ref_axis',(0.810015401063433,0.,-0.586408603313462)) ;
#58094 = DIRECTION('center_axis',(-1.51760508056877E-16,-5.60383084497428E-34,
1.)) ;
#58095 = DIRECTION('ref_axis',(1.,1.81422958079369E-66,1.51760508056877E-16)) ;
#58096 = DIRECTION('',(2.22044604925031E-16,-1.,3.31372189702139E-32)) ;
#58097 = DIRECTION('',(-1.,0.,-1.51760508056877E-16)) ;
#58098 = DIRECTION('center_axis',(-2.22044604925031E-16,1.,-3.31372189702139E-32)) ;
#58099 = DIRECTION('ref_axis',(-0.707106781186546,-1.57009245868377E-16,-0.707106781186549)) ;
#58100 = DIRECTION('',(-2.22044604925031E-16,1.,-3.31372189702139E-32)) ;
#58101 = DIRECTION('center_axis',(0.,1.,0.)) ;
#58102 = DIRECTION('ref_axis',(-0.707106781186549,0.,-0.707106781186546)) ;
#58103 = DIRECTION('center_axis',(-1.,-2.22044604925031E-16,0.)) ;
#58104 = DIRECTION('ref_axis',(2.22044604925031E-16,-1.,3.31372189702139E-32)) ;
#58105 = DIRECTION('',(-2.22044604925031E-16,1.,-3.31372189702139E-32)) ;
#58106 = DIRECTION('',(0.,0.,-1.)) ;
#58107 = DIRECTION('',(2.22044604925031E-16,-1.,3.31372189702139E-32)) ;
#58108 = DIRECTION('center_axis',(1.,2.22044604925031E-16,0.)) ;
#58109 = DIRECTION('ref_axis',(-1.57009245868375E-16,0.707106781186538,0.707106781186557)) ;
#58110 = DIRECTION('',(0.,0.,1.)) ;
#58111 = DIRECTION('center_axis',(-1.51760508056877E-16,-5.60383084497428E-34,
1.)) ;
#58112 = DIRECTION('ref_axis',(1.,0.,0.)) ;
#58113 = DIRECTION('center_axis',(0.,1.,5.60383084497428E-34)) ;
#58114 = DIRECTION('ref_axis',(-1.,0.,0.)) ;
#58115 = DIRECTION('center_axis',(-1.51760508056877E-16,-5.60383084497428E-34,
1.)) ;
#58116 = DIRECTION('ref_axis',(1.,1.86794361499143E-34,1.51760508056877E-16)) ;
#58117 = DIRECTION('center_axis',(0.,0.,1.)) ;
#58118 = DIRECTION('ref_axis',(1.,0.,0.)) ;
#58119 = DIRECTION('',(0.,0.,-1.)) ;
#58120 = DIRECTION('center_axis',(-1.4923676700635E-16,0.,1.)) ;
#58121 = DIRECTION('ref_axis',(1.,0.,1.4923676700635E-16)) ;
#58122 = DIRECTION('',(0.000396813558216815,-0.999999921269497,0.)) ;
#58123 = DIRECTION('center_axis',(-1.4923676700635E-16,0.,1.)) ;
#58124 = DIRECTION('ref_axis',(1.,0.,0.)) ;
#58125 = DIRECTION('center_axis',(0.,-1.,0.)) ;
#58126 = DIRECTION('ref_axis',(-1.,0.,0.)) ;
#58127 = DIRECTION('center_axis',(-1.4923676700635E-16,0.,1.)) ;
#58128 = DIRECTION('ref_axis',(1.,0.,1.4923676700635E-16)) ;
#58129 = DIRECTION('center_axis',(-1.4923676700635E-16,0.,1.)) ;
#58130 = DIRECTION('ref_axis',(1.,0.,1.4923676700635E-16)) ;
#58131 = DIRECTION('center_axis',(1.4923676700635E-16,0.,-1.)) ;
#58132 = DIRECTION('ref_axis',(1.,0.,1.4923676700635E-16)) ;
#58133 = DIRECTION('center_axis',(1.4923676700635E-16,0.,-1.)) ;
#58134 = DIRECTION('ref_axis',(-1.,0.,0.)) ;
#58135 = DIRECTION('center_axis',(-1.4923676700635E-16,0.,1.)) ;
#58136 = DIRECTION('ref_axis',(1.,0.,1.4923676700635E-16)) ;
#58137 = DIRECTION('center_axis',(0.,-1.,0.)) ;
#58138 = DIRECTION('ref_axis',(1.,0.,0.)) ;
#58139 = DIRECTION('center_axis',(-1.4923676700635E-16,0.,1.)) ;
#58140 = DIRECTION('ref_axis',(1.,0.,1.4923676700635E-16)) ;
#58141 = DIRECTION('center_axis',(0.,0.,1.)) ;
#58142 = DIRECTION('ref_axis',(1.,0.,0.)) ;
#58143 = DIRECTION('',(0.,0.,1.)) ;
#58144 = DIRECTION('center_axis',(1.4923676700635E-16,0.,-1.)) ;
#58145 = DIRECTION('ref_axis',(1.,0.,1.4923676700635E-16)) ;
#58146 = DIRECTION('center_axis',(0.,-0.97854978498675,-0.206010481049838)) ;
#58147 = DIRECTION('ref_axis',(0.,0.206010481049828,-0.978549784986752)) ;
#58148 = DIRECTION('center_axis',(0.,0.97854978498675,0.206010481049838)) ;
#58149 = DIRECTION('ref_axis',(-1.,9.47139866158082E-17,-4.49891436425098E-16)) ;
#58150 = DIRECTION('center_axis',(-1.,0.,0.)) ;
#58151 = DIRECTION('ref_axis',(0.,-0.206010481049841,0.978549784986749)) ;
#58152 = DIRECTION('center_axis',(0.,-0.97854978498675,-0.206010481049838)) ;
#58153 = DIRECTION('ref_axis',(-1.,9.47139866158082E-17,-4.49891436425098E-16)) ;
#58154 = DIRECTION('center_axis',(0.,-0.97854978498675,-0.206010481049838)) ;
#58155 = DIRECTION('ref_axis',(-1.,9.47139866158082E-17,-4.49891436425098E-16)) ;
#58156 = DIRECTION('center_axis',(0.,-0.97854978498675,-0.206010481049839)) ;
#58157 = DIRECTION('ref_axis',(-1.,0.,0.)) ;
#58158 = DIRECTION('',(0.,-0.97854978498675,-0.206010481049839)) ;
#58159 = DIRECTION('center_axis',(0.,0.97854978498675,0.206010481049838)) ;
#58160 = DIRECTION('ref_axis',(-1.,-9.47139866158082E-17,4.49891436425098E-16)) ;
#58161 = DIRECTION('center_axis',(0.,0.97854978498675,0.206010481049838)) ;
#58162 = DIRECTION('ref_axis',(-1.,-9.47139866158082E-17,4.49891436425098E-16)) ;
#58163 = DIRECTION('center_axis',(0.,0.97854978498675,0.206010481049838)) ;
#58164 = DIRECTION('ref_axis',(0.,-0.206010481049838,0.97854978498675)) ;
#58165 = DIRECTION('',(-1.,3.19495806435525E-17,-1.51760508056877E-16)) ;
#58166 = DIRECTION('',(0.,-0.206010481049838,0.97854978498675)) ;
#58167 = DIRECTION('center_axis',(0.,0.97854978498675,0.206010481049838)) ;
#58168 = DIRECTION('ref_axis',(2.85896974219543E-17,0.206010481049838,-0.97854978498675)) ;
#58169 = DIRECTION('',(-1.,0.,-1.4923676700635E-16)) ;
#58170 = DIRECTION('center_axis',(0.,0.97854978498675,0.206010481049838)) ;
#58171 = DIRECTION('ref_axis',(-1.42948487109771E-17,0.206010481049838,-0.97854978498675)) ;
#58172 = DIRECTION('',(0.,0.206010481049838,-0.97854978498675)) ;
#58173 = DIRECTION('center_axis',(0.,0.97854978498675,0.206010481049838)) ;
#58174 = DIRECTION('ref_axis',(0.,-0.206010481049828,0.978549784986752)) ;
#58175 = DIRECTION('center_axis',(0.,-0.97854978498675,-0.206010481049838)) ;
#58176 = DIRECTION('ref_axis',(-1.,-9.47139866158082E-17,4.49891436425098E-16)) ;
#58177 = DIRECTION('center_axis',(-1.,0.,0.)) ;
#58178 = DIRECTION('ref_axis',(0.,0.206010481049841,-0.978549784986749)) ;
#58179 = DIRECTION('center_axis',(0.,0.97854978498675,0.206010481049838)) ;
#58180 = DIRECTION('ref_axis',(0.,-0.206010481049838,0.97854978498675)) ;
#58181 = DIRECTION('',(0.,-0.206010481049838,0.97854978498675)) ;
#58182 = DIRECTION('',(0.,0.206010481049838,-0.97854978498675)) ;
#58183 = DIRECTION('',(-1.,0.,0.)) ;
#58184 = DIRECTION('center_axis',(0.,-0.97854978498675,-0.206010481049838)) ;
#58185 = DIRECTION('ref_axis',(0.,0.206010481049829,-0.978549784986752)) ;
#58186 = DIRECTION('center_axis',(0.,0.97854978498675,0.206010481049838)) ;
#58187 = DIRECTION('ref_axis',(-1.,-3.89103363082382E-16,1.84824097464135E-15)) ;
#58188 = DIRECTION('center_axis',(-1.,0.,0.)) ;
#58189 = DIRECTION('ref_axis',(0.,-0.206010481049842,0.978549784986749)) ;
#58190 = DIRECTION('center_axis',(0.,-0.97854978498675,-0.206010481049838)) ;
#58191 = DIRECTION('ref_axis',(-1.,-3.89103363082383E-16,1.84824097464135E-15)) ;
#58192 = DIRECTION('center_axis',(0.,-0.97854978498675,-0.206010481049838)) ;
#58193 = DIRECTION('ref_axis',(-1.,-3.89103363082383E-16,1.84824097464135E-15)) ;
#58194 = DIRECTION('center_axis',(0.,-0.97854978498675,-0.206010481049839)) ;
#58195 = DIRECTION('ref_axis',(-1.,0.,0.)) ;
#58196 = DIRECTION('',(0.,-0.97854978498675,-0.206010481049839)) ;
#58197 = DIRECTION('center_axis',(0.,0.97854978498675,0.206010481049838)) ;
#58198 = DIRECTION('ref_axis',(-1.,-9.47139866158086E-17,4.498914364251E-16)) ;
#58199 = DIRECTION('center_axis',(0.,0.97854978498675,0.206010481049838)) ;
#58200 = DIRECTION('ref_axis',(-1.,-9.47139866158086E-17,4.498914364251E-16)) ;
#58201 = DIRECTION('center_axis',(0.,0.97854978498675,0.206010481049838)) ;
#58202 = DIRECTION('ref_axis',(0.,-0.206010481049838,0.97854978498675)) ;
#58203 = DIRECTION('',(-1.,3.19495806435525E-17,-1.51760508056877E-16)) ;
#58204 = DIRECTION('',(0.,-0.206010481049838,0.97854978498675)) ;
#58205 = DIRECTION('center_axis',(0.,0.97854978498675,0.206010481049838)) ;
#58206 = DIRECTION('ref_axis',(1.42948487109771E-17,0.206010481049838,-0.97854978498675)) ;
#58207 = DIRECTION('',(-1.,0.,-1.4923676700635E-16)) ;
#58208 = DIRECTION('center_axis',(0.,0.97854978498675,0.206010481049838)) ;
#58209 = DIRECTION('ref_axis',(-1.42948487109771E-17,0.206010481049838,-0.97854978498675)) ;
#58210 = DIRECTION('',(0.,0.206010481049838,-0.97854978498675)) ;
#58211 = DIRECTION('center_axis',(0.,0.97854978498675,0.206010481049838)) ;
#58212 = DIRECTION('ref_axis',(0.,-0.206010481049829,0.978549784986752)) ;
#58213 = DIRECTION('center_axis',(0.,-0.97854978498675,-0.206010481049838)) ;
#58214 = DIRECTION('ref_axis',(-1.,-9.47139866158086E-17,4.498914364251E-16)) ;
#58215 = DIRECTION('center_axis',(-1.,0.,0.)) ;
#58216 = DIRECTION('ref_axis',(0.,0.206010481049842,-0.978549784986749)) ;
#58217 = DIRECTION('center_axis',(0.,0.97854978498675,0.206010481049838)) ;
#58218 = DIRECTION('ref_axis',(0.,-0.206010481049838,0.97854978498675)) ;
#58219 = DIRECTION('',(-1.,0.,0.)) ;
#58220 = DIRECTION('',(0.,-0.206010481049838,0.97854978498675)) ;
#58221 = DIRECTION('',(0.,0.206010481049838,-0.97854978498675)) ;
#58222 = DIRECTION('center_axis',(0.,-1.,0.)) ;
#58223 = DIRECTION('ref_axis',(0.,0.,-1.)) ;
#58224 = DIRECTION('center_axis',(1.,0.,0.)) ;
#58225 = DIRECTION('ref_axis',(0.,0.,-1.)) ;
#58226 = DIRECTION('center_axis',(0.,-1.,0.)) ;
#58227 = DIRECTION('ref_axis',(0.810015401063433,0.,-0.586408603313462)) ;
#58228 = DIRECTION('center_axis',(0.,0.,-1.)) ;
#58229 = DIRECTION('ref_axis',(0.,1.,0.)) ;
#58230 = DIRECTION('center_axis',(8.7076315656875E-16,0.,-1.)) ;
#58231 = DIRECTION('ref_axis',(0.707106781186391,0.707106781186704,6.1572253281703E-16)) ;
#58232 = DIRECTION('center_axis',(0.,0.,-1.)) ;
#58233 = DIRECTION('ref_axis',(0.,1.,0.)) ;
#58234 = DIRECTION('',(-8.7076315656875E-16,0.,1.)) ;
#58235 = DIRECTION('center_axis',(0.,-1.,0.)) ;
#58236 = DIRECTION('ref_axis',(0.,0.,1.)) ;
#58237 = DIRECTION('center_axis',(0.,0.,1.)) ;
#58238 = DIRECTION('ref_axis',(0.,1.,0.)) ;
#58239 = DIRECTION('center_axis',(0.,1.,0.)) ;
#58240 = DIRECTION('ref_axis',(0.,0.,1.)) ;
#58241 = DIRECTION('center_axis',(0.,0.,1.)) ;
#58242 = DIRECTION('ref_axis',(-0.707106781186359,0.707106781186736,0.)) ;
#58243 = DIRECTION('center_axis',(0.,0.,1.)) ;
#58244 = DIRECTION('ref_axis',(0.,1.,0.)) ;
#58245 = DIRECTION('',(0.,0.,-1.)) ;
#58246 = DIRECTION('center_axis',(0.,-1.,0.)) ;
#58247 = DIRECTION('ref_axis',(0.,0.,-1.)) ;
#58248 = DIRECTION('center_axis',(-1.,0.,0.)) ;
#58249 = DIRECTION('ref_axis',(0.,1.,0.)) ;
#58250 = DIRECTION('center_axis',(0.,-1.,0.)) ;
#58251 = DIRECTION('ref_axis',(-0.810015401063435,0.,-0.586408603313459)) ;
#58252 = DIRECTION('center_axis',(0.,1.,0.)) ;
#58253 = DIRECTION('ref_axis',(-1.,0.,-1.4923676700635E-16)) ;
#58254 = DIRECTION('',(1.,0.,1.51760508056877E-16)) ;
#58255 = DIRECTION('center_axis',(0.,-1.,0.)) ;
#58256 = DIRECTION('ref_axis',(-0.707106781186549,0.,-0.707106781186546)) ;
#58257 = DIRECTION('',(0.,0.,-1.)) ;
#58258 = DIRECTION('',(-1.,0.,-1.51760508056877E-16)) ;
#58259 = DIRECTION('',(0.,0.,1.)) ;
#58260 = DIRECTION('',(0.,0.,-1.)) ;
#58261 = DIRECTION('',(-1.,0.,-1.51760508056877E-16)) ;
#58262 = DIRECTION('',(0.,0.,1.)) ;
#58263 = DIRECTION('',(0.,0.,-1.)) ;
#58264 = DIRECTION('',(-1.,0.,-1.51760508056877E-16)) ;
#58265 = DIRECTION('',(0.,0.,1.)) ;
#58266 = DIRECTION('center_axis',(0.,-1.,0.)) ;
#58267 = DIRECTION('ref_axis',(0.707106781186549,0.,-0.707106781186546)) ;
#58268 = DIRECTION('',(1.,0.,1.51760508056877E-16)) ;
#58269 = DIRECTION('center_axis',(1.,0.,1.51760508056877E-16)) ;
#58270 = DIRECTION('ref_axis',(1.07310884363343E-16,0.707106781186485,-0.70710678118661)) ;
#58271 = DIRECTION('center_axis',(-1.,0.,-4.44089209850043E-14)) ;
#58272 = DIRECTION('ref_axis',(0.,1.,0.)) ;
#58273 = DIRECTION('center_axis',(0.,1.,0.)) ;
#58274 = DIRECTION('ref_axis',(-1.,0.,-1.4923676700635E-16)) ;
#58275 = DIRECTION('',(1.,0.,1.51760508056877E-16)) ;
#58276 = DIRECTION('center_axis',(0.,-1.,0.)) ;
#58277 = DIRECTION('ref_axis',(-3.36349381434756E-17,0.,-1.)) ;
#58278 = DIRECTION('center_axis',(0.,-1.,0.)) ;
#58279 = DIRECTION('ref_axis',(0.,0.,-1.)) ;
#58280 = DIRECTION('',(0.,0.,-1.)) ;
#58281 = DIRECTION('',(0.,0.,-1.)) ;
#58282 = DIRECTION('center_axis',(0.,-1.,0.)) ;
#58283 = DIRECTION('ref_axis',(0.,0.,-1.)) ;
#58284 = DIRECTION('center_axis',(0.,-1.,0.)) ;
#58285 = DIRECTION('ref_axis',(3.36349381434756E-17,0.,-1.)) ;
#58286 = DIRECTION('',(1.,0.,1.51760508056877E-16)) ;
#58287 = DIRECTION('center_axis',(0.,-1.,0.)) ;
#58288 = DIRECTION('ref_axis',(1.,0.,3.92523114670939E-16)) ;
#58289 = DIRECTION('',(1.,0.,1.51760508056877E-16)) ;
#58290 = DIRECTION('',(1.,0.,1.51760508056877E-16)) ;
#58291 = DIRECTION('center_axis',(1.,0.,1.51760508056877E-16)) ;
#58292 = DIRECTION('ref_axis',(1.07310884363343E-16,0.707106781186485,-0.70710678118661)) ;
#58293 = DIRECTION('center_axis',(-1.,0.,0.)) ;
#58294 = DIRECTION('ref_axis',(0.,1.,0.)) ;
#58295 = DIRECTION('center_axis',(-1.,0.,-1.51760508056877E-16)) ;
#58296 = DIRECTION('ref_axis',(-1.07310884363324E-16,0.70710678118661,0.707106781186485)) ;
#58297 = DIRECTION('center_axis',(-1.,0.,0.)) ;
#58298 = DIRECTION('ref_axis',(0.,0.,1.)) ;
#58299 = DIRECTION('center_axis',(-0.996538840142805,0.,0.0831284553377041)) ;
#58300 = DIRECTION('ref_axis',(0.0828427124744576,0.0828427124744687,0.993113372168428)) ;
#58301 = DIRECTION('center_axis',(0.554700196225257,0.832050294337825,-2.46336371845354E-14)) ;
#58302 = DIRECTION('ref_axis',(0.832050294337825,-0.554700196225257,1.77197583952116E-30)) ;
#58303 = DIRECTION('center_axis',(-1.,1.11022302462518E-14,-2.26623325918295E-15)) ;
#58304 = DIRECTION('ref_axis',(-3.546880840987E-30,0.19999999999989,0.979795897113294)) ;
#58305 = DIRECTION('center_axis',(-1.,0.,-1.51760508056877E-16)) ;
#58306 = DIRECTION('ref_axis',(-9.59817728648186E-17,0.774596669241454,0.632455532033712)) ;
#58307 = DIRECTION('center_axis',(-1.,0.,0.)) ;
#58308 = DIRECTION('ref_axis',(0.,0.199999999999984,0.979795897113275)) ;
#58309 = DIRECTION('',(-1.,0.,-1.51760508056877E-16)) ;
#58310 = DIRECTION('center_axis',(-1.,0.,6.66133814775093E-14)) ;
#58311 = DIRECTION('ref_axis',(6.66133814775093E-14,0.,1.)) ;
#58312 = DIRECTION('center_axis',(-1.,0.,-1.51760508056877E-16)) ;
#58313 = DIRECTION('ref_axis',(-1.07310884363324E-16,0.70710678118661,0.707106781186485)) ;
#58314 = DIRECTION('center_axis',(2.22044604925031E-16,-1.,3.31372189702139E-32)) ;
#58315 = DIRECTION('ref_axis',(-0.707106781186548,-1.57009245868377E-16,-0.707106781186548)) ;
#58316 = DIRECTION('center_axis',(0.,1.,0.)) ;
#58317 = DIRECTION('ref_axis',(0.,0.,-1.)) ;
#58318 = DIRECTION('center_axis',(1.51760508056877E-16,5.60383084497428E-34,
-1.)) ;
#58319 = DIRECTION('ref_axis',(-1.,0.,0.)) ;
#58320 = DIRECTION('center_axis',(1.,0.,0.)) ;
#58321 = DIRECTION('ref_axis',(0.,-1.,4.44089209849993E-14)) ;
#58322 = DIRECTION('center_axis',(-1.51760508056877E-16,-5.60383084497428E-34,
1.)) ;
#58323 = DIRECTION('ref_axis',(-0.707106781186614,0.707106781186481,-1.07310884363344E-16)) ;
#58324 = DIRECTION('center_axis',(0.,1.,0.)) ;
#58325 = DIRECTION('ref_axis',(1.,0.,0.)) ;
#58326 = DIRECTION('center_axis',(-1.,0.,-1.51760508056877E-16)) ;
#58327 = DIRECTION('ref_axis',(1.07310884363343E-16,-0.707106781186485,-0.70710678118661)) ;
#58328 = DIRECTION('center_axis',(1.,0.,0.)) ;
#58329 = DIRECTION('ref_axis',(0.,-1.,0.)) ;
#58330 = DIRECTION('',(-1.,0.,-1.51760508056877E-16)) ;
#58331 = DIRECTION('center_axis',(1.51760508056877E-16,5.60383084497428E-34,
-1.)) ;
#58332 = DIRECTION('ref_axis',(-1.,0.,0.)) ;
#58333 = DIRECTION('center_axis',(0.707106781186592,-0.707106781186503,0.)) ;
#58334 = DIRECTION('ref_axis',(-0.707106781186503,-0.707106781186592,-4.44089209850158E-14)) ;
#58335 = DIRECTION('center_axis',(-1.51760508056877E-16,-5.60383084497428E-34,
1.)) ;
#58336 = DIRECTION('ref_axis',(0.382683432364956,0.923879532511342,5.80762321206553E-17)) ;
#58337 = DIRECTION('center_axis',(0.707106781186555,-0.70710678118654,1.07310884363335E-16)) ;
#58338 = DIRECTION('ref_axis',(-0.499999999999962,-0.499999999999972,-0.707106781186594)) ;
#58339 = DIRECTION('center_axis',(0.707106781186437,-0.707106781186659,0.)) ;
#58340 = DIRECTION('ref_axis',(-0.707106781186659,-0.707106781186437,0.)) ;
#58341 = DIRECTION('',(-0.707106781186555,0.70710678118654,-1.07310884363335E-16)) ;
#58342 = DIRECTION('center_axis',(-1.,0.,-1.51760508056877E-16)) ;
#58343 = DIRECTION('ref_axis',(-1.07310884363324E-16,0.70710678118661,0.707106781186485)) ;
#58344 = DIRECTION('center_axis',(0.,-0.206010481049838,0.97854978498675)) ;
#58345 = DIRECTION('ref_axis',(0.707106781186543,-0.691939188692773,-0.145671408145844)) ;
#58346 = DIRECTION('center_axis',(-0.816496580927833,-0.40824829046381,0.408248290463703)) ;
#58347 = DIRECTION('ref_axis',(0.577350269189448,-0.577350269189946,0.577350269189484)) ;
#58348 = DIRECTION('center_axis',(-3.55271367880058E-13,-1.,0.)) ;
#58349 = DIRECTION('ref_axis',(0.,0.,1.)) ;
#58350 = DIRECTION('center_axis',(1.,0.,0.)) ;
#58351 = DIRECTION('ref_axis',(0.,-1.,0.)) ;
#58352 = DIRECTION('center_axis',(0.,0.,1.)) ;
#58353 = DIRECTION('ref_axis',(1.,0.,0.)) ;
#58354 = DIRECTION('center_axis',(1.,0.,1.51760508056877E-16)) ;
#58355 = DIRECTION('ref_axis',(-1.07310884363343E-16,-0.707106781186485,0.70710678118661)) ;
#58356 = DIRECTION('center_axis',(1.,0.,0.)) ;
#58357 = DIRECTION('ref_axis',(0.,0.,1.)) ;
#58358 = DIRECTION('',(1.,0.,1.51760508056877E-16)) ;
#58359 = DIRECTION('center_axis',(-1.51760508056877E-16,-5.60383084497428E-34,
1.)) ;
#58360 = DIRECTION('ref_axis',(1.,0.,0.)) ;
#58361 = DIRECTION('center_axis',(0.,1.,0.)) ;
#58362 = DIRECTION('ref_axis',(0.707106781186548,0.,0.707106781186548)) ;
#58363 = DIRECTION('center_axis',(0.,0.,1.)) ;
#58364 = DIRECTION('ref_axis',(0.,1.,0.)) ;
#58365 = DIRECTION('center_axis',(-0.81649658092775,-0.408248290463875,-0.408248290463804)) ;
#58366 = DIRECTION('ref_axis',(0.577350269189602,-0.577350269189744,-0.577350269189531)) ;
#58367 = DIRECTION('center_axis',(0.,0.,-1.)) ;
#58368 = DIRECTION('ref_axis',(1.,0.,0.)) ;
#58369 = DIRECTION('center_axis',(1.,0.,1.51760508056877E-16)) ;
#58370 = DIRECTION('ref_axis',(1.07310884363347E-16,-0.707106781186459,-0.707106781186636)) ;
#58371 = DIRECTION('center_axis',(0.,-1.,-5.60383084497428E-34)) ;
#58372 = DIRECTION('ref_axis',(0.707106781186547,3.96250679110365E-34,-0.707106781186547)) ;
#58373 = DIRECTION('center_axis',(0.,0.,1.)) ;
#58374 = DIRECTION('ref_axis',(0.70710678118661,-0.707106781186485,0.)) ;
#58375 = DIRECTION('',(0.,0.,1.)) ;
#58376 = DIRECTION('',(0.,0.,-1.)) ;
#58377 = DIRECTION('center_axis',(0.,0.,1.)) ;
#58378 = DIRECTION('ref_axis',(1.,0.,0.)) ;
#58379 = DIRECTION('center_axis',(-1.,0.,0.)) ;
#58380 = DIRECTION('ref_axis',(0.,-1.,0.)) ;
#58381 = DIRECTION('center_axis',(0.,0.,-1.)) ;
#58382 = DIRECTION('ref_axis',(1.,0.,0.)) ;
#58383 = DIRECTION('center_axis',(0.,-1.,0.)) ;
#58384 = DIRECTION('ref_axis',(0.,0.,1.)) ;
#58385 = DIRECTION('center_axis',(0.,0.,-1.)) ;
#58386 = DIRECTION('ref_axis',(-1.,0.,0.)) ;
#58387 = DIRECTION('center_axis',(4.44089209850072E-14,0.,-1.)) ;
#58388 = DIRECTION('ref_axis',(0.,1.,0.)) ;
#58389 = DIRECTION('center_axis',(1.,0.,0.)) ;
#58390 = DIRECTION('ref_axis',(0.,0.,1.)) ;
#58391 = DIRECTION('center_axis',(0.,-1.,0.)) ;
#58392 = DIRECTION('ref_axis',(1.,0.,0.)) ;
#58393 = DIRECTION('center_axis',(1.,0.,1.51760508056877E-16)) ;
#58394 = DIRECTION('ref_axis',(-1.07310884363343E-16,-0.707106781186485,0.70710678118661)) ;
#58395 = DIRECTION('',(1.,0.,1.51760508056877E-16)) ;
#58396 = DIRECTION('center_axis',(0.,1.,5.60383084497428E-34)) ;
#58397 = DIRECTION('ref_axis',(0.707106781186548,-3.96250679110365E-34,0.707106781186548)) ;
#58398 = DIRECTION('',(0.,1.,5.60383084497428E-34)) ;
#58399 = DIRECTION('center_axis',(0.,-1.,0.)) ;
#58400 = DIRECTION('ref_axis',(0.,0.,-1.)) ;
#58401 = DIRECTION('center_axis',(0.,0.,1.)) ;
#58402 = DIRECTION('ref_axis',(0.,1.,0.)) ;
#58403 = DIRECTION('center_axis',(0.,1.,0.)) ;
#58404 = DIRECTION('ref_axis',(0.707106781186548,0.,-0.707106781186548)) ;
#58405 = DIRECTION('center_axis',(0.,-1.,0.)) ;
#58406 = DIRECTION('ref_axis',(0.707106781186548,0.,-0.707106781186548)) ;
#58407 = DIRECTION('center_axis',(0.,0.,1.)) ;
#58408 = DIRECTION('ref_axis',(-0.70710678118661,0.707106781186485,0.)) ;
#58409 = DIRECTION('',(0.,0.,-1.)) ;
#58410 = DIRECTION('',(0.,0.,1.)) ;
#58411 = DIRECTION('center_axis',(0.,0.,1.)) ;
#58412 = DIRECTION('ref_axis',(0.70710678118661,0.707106781186485,0.)) ;
#58413 = DIRECTION('center_axis',(0.,0.,-1.)) ;
#58414 = DIRECTION('ref_axis',(0.,1.,0.)) ;
#58415 = DIRECTION('',(0.,0.,1.)) ;
#58416 = DIRECTION('',(0.,0.,-1.)) ;
#58417 = DIRECTION('center_axis',(0.,-1.,0.)) ;
#58418 = DIRECTION('ref_axis',(0.,0.,-1.)) ;
#58419 = DIRECTION('center_axis',(0.,1.,0.)) ;
#58420 = DIRECTION('ref_axis',(-0.707106781186548,0.,-0.707106781186548)) ;
#58421 = DIRECTION('center_axis',(0.,-1.,0.)) ;
#58422 = DIRECTION('ref_axis',(-0.707106781186548,0.,-0.707106781186548)) ;
#58423 = DIRECTION('center_axis',(0.,-1.,-5.60383084497428E-34)) ;
#58424 = DIRECTION('ref_axis',(-0.707106781186548,-3.96250679110365E-34,0.707106781186548)) ;
#58425 = DIRECTION('center_axis',(0.,1.,0.)) ;
#58426 = DIRECTION('ref_axis',(-1.,0.,0.)) ;
#58427 = DIRECTION('',(0.,-1.,-5.60383084497428E-34)) ;
#58428 = DIRECTION('center_axis',(-0.81649658092775,0.408248290463875,-0.408248290463804)) ;
#58429 = DIRECTION('ref_axis',(-0.577350269189602,-0.577350269189744,0.577350269189531)) ;
#58430 = DIRECTION('center_axis',(0.,0.,1.)) ;
#58431 = DIRECTION('ref_axis',(-0.707106781186636,-0.707106781186459,0.)) ;
#58432 = DIRECTION('center_axis',(-1.,0.,-1.51760508056877E-16)) ;
#58433 = DIRECTION('ref_axis',(-1.07310884363347E-16,-0.707106781186459,0.707106781186636)) ;
#58434 = DIRECTION('center_axis',(-1.,0.,-1.51760508056877E-16)) ;
#58435 = DIRECTION('ref_axis',(1.07310884363343E-16,-0.707106781186485,-0.70710678118661)) ;
#58436 = DIRECTION('',(-1.,0.,-1.51760508056877E-16)) ;
#58437 = DIRECTION('center_axis',(1.,0.,0.)) ;
#58438 = DIRECTION('ref_axis',(0.,-1.,0.)) ;
#58439 = DIRECTION('center_axis',(0.,1.,0.)) ;
#58440 = DIRECTION('ref_axis',(-1.,0.,-1.4923676700635E-16)) ;
#58441 = DIRECTION('',(0.,0.,1.)) ;
#58442 = DIRECTION('center_axis',(1.,0.,1.51760508056877E-16)) ;
#58443 = DIRECTION('ref_axis',(-1.07310884363343E-16,-0.707106781186485,0.70710678118661)) ;
#58444 = DIRECTION('',(1.,0.,1.51760508056877E-16)) ;
#58445 = DIRECTION('center_axis',(-1.,0.,0.)) ;
#58446 = DIRECTION('ref_axis',(0.,-1.,0.)) ;
#58447 = DIRECTION('center_axis',(0.,0.,1.)) ;
#58448 = DIRECTION('ref_axis',(-0.70710678118661,-0.707106781186485,0.)) ;
#58449 = DIRECTION('',(0.,0.,-1.)) ;
#58450 = DIRECTION('center_axis',(0.,0.,-1.)) ;
#58451 = DIRECTION('ref_axis',(-0.707106781186636,-0.707106781186459,0.)) ;
#58452 = DIRECTION('',(0.,0.,1.)) ;
#58453 = DIRECTION('center_axis',(1.,0.,0.)) ;
#58454 = DIRECTION('ref_axis',(0.,1.,0.)) ;
#58455 = DIRECTION('',(0.,1.,5.60383084497428E-34)) ;
#58456 = DIRECTION('center_axis',(1.,0.,0.)) ;
#58457 = DIRECTION('ref_axis',(0.,0.,-1.)) ;
#58458 = DIRECTION('center_axis',(0.,0.,1.)) ;
#58459 = DIRECTION('ref_axis',(-1.,0.,0.)) ;
#58460 = DIRECTION('center_axis',(-1.,0.,0.)) ;
#58461 = DIRECTION('ref_axis',(0.,0.707106781186481,-0.707106781186614)) ;
#58462 = DIRECTION('center_axis',(1.,0.,0.)) ;
#58463 = DIRECTION('ref_axis',(0.,0.707106781186481,-0.707106781186614)) ;
#58464 = DIRECTION('center_axis',(0.,0.,1.)) ;
#58465 = DIRECTION('ref_axis',(-0.707106781186359,-0.707106781186736,0.)) ;
#58466 = DIRECTION('center_axis',(0.,0.,1.)) ;
#58467 = DIRECTION('ref_axis',(-1.,0.,0.)) ;
#58468 = DIRECTION('',(0.,0.,-1.)) ;
#58469 = DIRECTION('',(0.,0.,1.)) ;
#58470 = DIRECTION('center_axis',(0.894427190999916,-0.447213595499958,0.)) ;
#58471 = DIRECTION('ref_axis',(0.447213595499958,0.894427190999916,0.)) ;
#58472 = DIRECTION('center_axis',(-0.447213595500021,0.894427190999884,0.)) ;
#58473 = DIRECTION('ref_axis',(0.894427190999884,0.447213595500021,0.)) ;
#58474 = DIRECTION('center_axis',(0.,1.,5.60383084497428E-34)) ;
#58475 = DIRECTION('ref_axis',(0.707106781186548,-3.96250679110365E-34,0.707106781186548)) ;
#58476 = DIRECTION('',(0.,1.,5.60383084497428E-34)) ;
#58477 = DIRECTION('center_axis',(-0.70710678118661,-0.707106781186485,0.)) ;
#58478 = DIRECTION('ref_axis',(0.707106781186485,-0.70710678118661,2.45326946669362E-16)) ;
#58479 = DIRECTION('center_axis',(-1.,0.,0.)) ;
#58480 = DIRECTION('ref_axis',(0.,-1.,0.)) ;
#58481 = DIRECTION('',(0.,0.,1.)) ;
#58482 = DIRECTION('center_axis',(0.,4.44089209850151E-14,-1.)) ;
#58483 = DIRECTION('ref_axis',(-1.,0.,0.)) ;
#58484 = DIRECTION('center_axis',(-0.447213595500021,-0.894427190999884,0.)) ;
#58485 = DIRECTION('ref_axis',(0.894427190999884,-0.447213595500021,0.)) ;
#58486 = DIRECTION('center_axis',(0.894427190999916,0.447213595499958,0.)) ;
#58487 = DIRECTION('ref_axis',(0.447213595499958,-0.894427190999916,0.)) ;
#58488 = DIRECTION('center_axis',(0.,0.,1.)) ;
#58489 = DIRECTION('ref_axis',(-0.707106781186673,0.707106781186422,0.)) ;
#58490 = DIRECTION('center_axis',(0.,0.,-1.)) ;
#58491 = DIRECTION('ref_axis',(-1.,0.,0.)) ;
#58492 = DIRECTION('',(0.,0.,1.)) ;
#58493 = DIRECTION('',(0.,0.,-1.)) ;
#58494 = DIRECTION('center_axis',(1.,0.,0.)) ;
#58495 = DIRECTION('ref_axis',(0.,0.,-1.)) ;
#58496 = DIRECTION('center_axis',(-1.,0.,0.)) ;
#58497 = DIRECTION('ref_axis',(0.,-0.707106781186481,-0.707106781186614)) ;
#58498 = DIRECTION('center_axis',(1.,0.,0.)) ;
#58499 = DIRECTION('ref_axis',(0.,-0.707106781186481,-0.707106781186614)) ;
#58500 = DIRECTION('center_axis',(-1.,0.,0.)) ;
#58501 = DIRECTION('ref_axis',(0.,-1.,0.)) ;
#58502 = DIRECTION('',(0.,1.,5.60383084497428E-34)) ;
#58503 = DIRECTION('',(0.,0.,-1.)) ;
#58504 = DIRECTION('center_axis',(0.,1.,5.60383084497428E-34)) ;
#58505 = DIRECTION('ref_axis',(0.707106781186548,-3.96250679110365E-34,0.707106781186548)) ;
#58506 = DIRECTION('center_axis',(-0.70710678118661,0.707106781186485,0.)) ;
#58507 = DIRECTION('ref_axis',(0.707106781186485,0.70710678118661,1.83995210002018E-16)) ;
#58508 = DIRECTION('center_axis',(1.,0.,1.51760508056877E-16)) ;
#58509 = DIRECTION('ref_axis',(1.07310884363343E-16,0.707106781186485,-0.70710678118661)) ;
#58510 = DIRECTION('center_axis',(-1.,0.,0.)) ;
#58511 = DIRECTION('ref_axis',(0.,1.,0.)) ;
#58512 = DIRECTION('center_axis',(-1.,0.,-2.01858731750028E-16)) ;
#58513 = DIRECTION('ref_axis',(1.42735678062174E-16,0.707106781186485,-0.70710678118661)) ;
#58514 = DIRECTION('',(1.,0.,1.51760508056877E-16)) ;
#58515 = DIRECTION('center_axis',(1.51760508056877E-16,5.60383084497428E-34,
-1.)) ;
#58516 = DIRECTION('ref_axis',(-1.,0.,0.)) ;
#58517 = DIRECTION('center_axis',(-0.707106781186614,-0.707106781186481,0.)) ;
#58518 = DIRECTION('ref_axis',(-0.707106781186481,0.707106781186614,0.)) ;
#58519 = DIRECTION('center_axis',(-1.51760508056877E-16,-5.60383084497428E-34,
1.)) ;
#58520 = DIRECTION('ref_axis',(0.382683432365032,-0.923879532511311,5.80762321206668E-17)) ;
#58521 = DIRECTION('center_axis',(-0.707106781186555,-0.70710678118654,-1.07310884363335E-16)) ;
#58522 = DIRECTION('ref_axis',(-0.499999999999977,0.499999999999988,-0.707106781186572)) ;
#58523 = DIRECTION('center_axis',(-0.707106781186459,-0.707106781186636,0.)) ;
#58524 = DIRECTION('ref_axis',(-0.707106781186636,0.707106781186459,0.)) ;
#58525 = DIRECTION('',(0.707106781186555,0.70710678118654,1.07310884363335E-16)) ;
#58526 = DIRECTION('center_axis',(1.51760508056877E-16,5.60383084497428E-34,
-1.)) ;
#58527 = DIRECTION('ref_axis',(-1.,0.,0.)) ;
#58528 = DIRECTION('center_axis',(0.,-1.,0.)) ;
#58529 = DIRECTION('ref_axis',(-1.,0.,0.)) ;
#58530 = DIRECTION('center_axis',(-1.51760508056877E-16,-5.60383084497428E-34,
1.)) ;
#58531 = DIRECTION('ref_axis',(0.923879532511313,-0.382683432365025,1.40208427237267E-16)) ;
#58532 = DIRECTION('center_axis',(-1.1311821873082E-49,1.,5.60383084497428E-34)) ;
#58533 = DIRECTION('ref_axis',(-0.707106781186548,3.96250679110365E-34,-0.707106781186548)) ;
#58534 = DIRECTION('center_axis',(0.,-1.,0.)) ;
#58535 = DIRECTION('ref_axis',(-1.,0.,0.)) ;
#58536 = DIRECTION('',(-1.1311821873082E-49,1.,5.60383084497428E-34)) ;
#58537 = DIRECTION('center_axis',(1.51760508056877E-16,5.60383084497428E-34,
-1.)) ;
#58538 = DIRECTION('ref_axis',(-1.,0.,0.)) ;
#58539 = DIRECTION('center_axis',(-1.51760508056877E-16,-5.60383084497428E-34,
1.)) ;
#58540 = DIRECTION('ref_axis',(0.923879532511313,0.382683432365025,1.40208427237267E-16)) ;
#58541 = DIRECTION('center_axis',(1.1311821873082E-49,-1.,-5.60383084497428E-34)) ;
#58542 = DIRECTION('ref_axis',(0.707106781186548,3.96250679110365E-34,-0.707106781186548)) ;
#58543 = DIRECTION('center_axis',(0.,-1.,0.)) ;
#58544 = DIRECTION('ref_axis',(0.707106781186548,0.,-0.707106781186548)) ;
#58545 = DIRECTION('',(1.1311821873082E-49,-1.,-5.60383084497428E-34)) ;
#58546 = DIRECTION('center_axis',(-1.,0.,-2.01858731750028E-16)) ;
#58547 = DIRECTION('ref_axis',(0.,-1.,0.)) ;
#58548 = DIRECTION('',(2.01858731750028E-16,0.,-1.)) ;
#58549 = DIRECTION('',(-1.1311821873082E-49,1.,5.60383084497428E-34)) ;
#58550 = DIRECTION('',(2.01858731750028E-16,0.,-1.)) ;
#58551 = DIRECTION('center_axis',(-2.01858731750028E-16,0.,1.)) ;
#58552 = DIRECTION('ref_axis',(-0.70710678118661,0.707106781186485,-1.42735678062174E-16)) ;
#58553 = DIRECTION('',(-2.01858731750028E-16,0.,1.)) ;
#58554 = DIRECTION('center_axis',(0.,0.,-1.)) ;
#58555 = DIRECTION('ref_axis',(0.,1.,0.)) ;
#58556 = DIRECTION('center_axis',(0.,1.,0.)) ;
#58557 = DIRECTION('ref_axis',(-1.,0.,-1.4923676700635E-16)) ;
#58558 = DIRECTION('',(2.01858731750028E-16,0.,-1.)) ;
#58559 = DIRECTION('',(1.,0.,1.51760508056877E-16)) ;
#58560 = DIRECTION('center_axis',(2.01858731750028E-16,0.,-1.)) ;
#58561 = DIRECTION('ref_axis',(0.382683432365058,0.9238795325113,7.72479923189582E-17)) ;
#58562 = DIRECTION('',(-2.01858731750028E-16,0.,1.)) ;
#58563 = DIRECTION('center_axis',(0.,0.,-1.)) ;
#58564 = DIRECTION('ref_axis',(0.707106781186481,0.707106781186614,0.)) ;
#58565 = DIRECTION('center_axis',(-0.70710678118654,-0.707106781186555,-1.4273567806216E-16)) ;
#58566 = DIRECTION('ref_axis',(-2.01858731750028E-16,-3.26018819696323E-31,
1.)) ;
#58567 = DIRECTION('',(2.01858731750028E-16,-3.48630559684206E-32,-1.)) ;
#58568 = DIRECTION('',(0.707106781186555,-0.70710678118654,1.07310884363335E-16)) ;
#58569 = DIRECTION('center_axis',(-2.01858731750028E-16,3.48630559684206E-32,
1.)) ;
#58570 = DIRECTION('ref_axis',(0.923879532511304,0.382683432365048,1.86493150722541E-16)) ;
#58571 = DIRECTION('',(-2.01858731750028E-16,3.48630559684206E-32,1.)) ;
#58572 = DIRECTION('center_axis',(0.,6.28036983473606E-14,-1.)) ;
#58573 = DIRECTION('ref_axis',(1.,0.,0.)) ;
#58574 = DIRECTION('center_axis',(1.,0.,2.01858731750028E-16)) ;
#58575 = DIRECTION('ref_axis',(0.,1.,0.)) ;
#58576 = DIRECTION('',(2.01858731750028E-16,3.48630559684206E-32,-1.)) ;
#58577 = DIRECTION('',(1.1311821873082E-49,-1.,-5.60383084497428E-34)) ;
#58578 = DIRECTION('center_axis',(2.01858731750028E-16,3.48630559684206E-32,
-1.)) ;
#58579 = DIRECTION('ref_axis',(0.923879532511304,-0.382683432365048,1.86493150722541E-16)) ;
#58580 = DIRECTION('',(-2.01858731750028E-16,-3.48630559684206E-32,1.)) ;
#58581 = DIRECTION('center_axis',(0.,0.,-1.)) ;
#58582 = DIRECTION('ref_axis',(0.707106781186592,-0.707106781186503,0.)) ;
#58583 = DIRECTION('center_axis',(-0.70710678118654,0.707106781186555,-1.4273567806216E-16)) ;
#58584 = DIRECTION('ref_axis',(-2.01858731750028E-16,3.26018819696323E-31,
1.)) ;
#58585 = DIRECTION('',(2.01858731750028E-16,0.,-1.)) ;
#58586 = DIRECTION('',(-0.707106781186555,-0.70710678118654,-1.07310884363335E-16)) ;
#58587 = DIRECTION('center_axis',(-2.01858731750028E-16,0.,1.)) ;
#58588 = DIRECTION('ref_axis',(0.382683432365017,-0.923879532511317,7.72479923189499E-17)) ;
#58589 = DIRECTION('',(-2.01858731750028E-16,0.,1.)) ;
#58590 = DIRECTION('center_axis',(0.,0.,-1.)) ;
#58591 = DIRECTION('ref_axis',(0.,-1.,0.)) ;
#58592 = DIRECTION('center_axis',(0.,-1.,0.)) ;
#58593 = DIRECTION('ref_axis',(1.,0.,1.4923676700635E-16)) ;
#58594 = DIRECTION('',(-2.01858731750028E-16,0.,1.)) ;
#58595 = DIRECTION('',(-1.,0.,-1.51760508056877E-16)) ;
#58596 = DIRECTION('center_axis',(-1.,0.,-1.51760508056877E-16)) ;
#58597 = DIRECTION('ref_axis',(1.07310884363343E-16,-0.707106781186485,-0.70710678118661)) ;
#58598 = DIRECTION('center_axis',(-1.,0.,0.)) ;
#58599 = DIRECTION('ref_axis',(0.,0.,-1.)) ;
#58600 = DIRECTION('',(-1.,0.,-1.51760508056877E-16)) ;
#58601 = DIRECTION('center_axis',(1.,0.,0.)) ;
#58602 = DIRECTION('ref_axis',(0.,-1.,4.44089209849993E-14)) ;
#58603 = DIRECTION('center_axis',(1.51760508056877E-16,5.60383084497428E-34,
-1.)) ;
#58604 = DIRECTION('ref_axis',(-1.,0.,0.)) ;
#58605 = DIRECTION('center_axis',(0.,1.,0.)) ;
#58606 = DIRECTION('ref_axis',(0.,0.,-1.)) ;
#58607 = DIRECTION('center_axis',(-1.51760508056877E-16,-5.60383084497428E-34,
1.)) ;
#58608 = DIRECTION('ref_axis',(0.707106781186592,0.707106781186503,1.0731088436334E-16)) ;
#58609 = DIRECTION('center_axis',(0.,1.,5.60383084497428E-34)) ;
#58610 = DIRECTION('ref_axis',(-0.707106781186579,3.96250679110348E-34,-0.707106781186516)) ;
#58611 = DIRECTION('center_axis',(0.,1.,0.)) ;
#58612 = DIRECTION('ref_axis',(0.,0.,-1.)) ;
#58613 = DIRECTION('',(0.,1.,5.60383084497428E-34)) ;
#58614 = DIRECTION('center_axis',(1.51760508056877E-16,5.60383084497428E-34,
-1.)) ;
#58615 = DIRECTION('ref_axis',(-1.,0.,0.)) ;
#58616 = DIRECTION('center_axis',(1.,0.,0.)) ;
#58617 = DIRECTION('ref_axis',(0.,0.,-1.)) ;
#58618 = DIRECTION('center_axis',(-1.51760508056877E-16,-5.60383084497428E-34,
1.)) ;
#58619 = DIRECTION('ref_axis',(0.707106781186592,-0.707106781186503,1.0731088436334E-16)) ;
#58620 = DIRECTION('center_axis',(1.,0.,1.51760508056877E-16)) ;
#58621 = DIRECTION('ref_axis',(1.07310884363343E-16,0.707106781186485,-0.70710678118661)) ;
#58622 = DIRECTION('center_axis',(1.,0.,0.)) ;
#58623 = DIRECTION('ref_axis',(0.,0.,-1.)) ;
#58624 = DIRECTION('',(1.,0.,1.51760508056877E-16)) ;
#58625 = DIRECTION('center_axis',(1.51760508056877E-16,5.60383084497428E-34,
-1.)) ;
#58626 = DIRECTION('ref_axis',(-1.,0.,0.)) ;
#58627 = DIRECTION('center_axis',(0.,-1.,0.)) ;
#58628 = DIRECTION('ref_axis',(0.,0.,-1.)) ;
#58629 = DIRECTION('center_axis',(-1.51760508056877E-16,-5.60383084497428E-34,
1.)) ;
#58630 = DIRECTION('ref_axis',(-0.707106781186592,-0.707106781186503,-1.0731088436334E-16)) ;
#58631 = DIRECTION('center_axis',(0.,-1.,-5.60383084497428E-34)) ;
#58632 = DIRECTION('ref_axis',(0.707106781186579,3.96250679110348E-34,-0.707106781186516)) ;
#58633 = DIRECTION('center_axis',(0.,-1.,0.)) ;
#58634 = DIRECTION('ref_axis',(0.,0.,-1.)) ;
#58635 = DIRECTION('',(0.,-1.,-5.60383084497428E-34)) ;
#58636 = DIRECTION('center_axis',(1.51760508056877E-16,5.60383084497428E-34,
-1.)) ;
#58637 = DIRECTION('ref_axis',(-1.,0.,0.)) ;
#58638 = DIRECTION('center_axis',(-1.,0.,0.)) ;
#58639 = DIRECTION('ref_axis',(0.,0.,-1.)) ;
#58640 = DIRECTION('center_axis',(-1.51760508056877E-16,-5.60383084497428E-34,
1.)) ;
#58641 = DIRECTION('ref_axis',(-0.707106781186592,0.707106781186503,-1.0731088436334E-16)) ;
#58642 = DIRECTION('center_axis',(-1.,0.,-1.51760508056877E-16)) ;
#58643 = DIRECTION('ref_axis',(1.07310884363343E-16,-0.707106781186485,-0.70710678118661)) ;
#58644 = DIRECTION('center_axis',(-1.,0.,0.)) ;
#58645 = DIRECTION('ref_axis',(0.,0.,-1.)) ;
#58646 = DIRECTION('',(-1.,0.,-1.51760508056877E-16)) ;
#58647 = DIRECTION('center_axis',(0.,-1.,-5.60383084497428E-34)) ;
#58648 = DIRECTION('ref_axis',(0.707106781186579,3.96250679110348E-34,-0.707106781186516)) ;
#58649 = DIRECTION('center_axis',(0.,-1.,0.)) ;
#58650 = DIRECTION('ref_axis',(0.,0.,-1.)) ;
#58651 = DIRECTION('',(0.,-1.,-5.60383084497428E-34)) ;
#58652 = DIRECTION('center_axis',(0.,1.,0.)) ;
#58653 = DIRECTION('ref_axis',(1.,0.,0.)) ;
#58654 = DIRECTION('center_axis',(1.51760508056877E-16,5.60383084497428E-34,
-1.)) ;
#58655 = DIRECTION('ref_axis',(-1.,0.,0.)) ;
#58656 = DIRECTION('center_axis',(-1.,0.,0.)) ;
#58657 = DIRECTION('ref_axis',(0.,0.,-1.)) ;
#58658 = DIRECTION('center_axis',(-1.51760508056877E-16,-5.60383084497428E-34,
1.)) ;
#58659 = DIRECTION('ref_axis',(-0.707106781186592,0.707106781186503,-1.0731088436334E-16)) ;
#58660 = DIRECTION('center_axis',(-1.,0.,-1.51760508056877E-16)) ;
#58661 = DIRECTION('ref_axis',(1.07310884363343E-16,-0.707106781186485,-0.70710678118661)) ;
#58662 = DIRECTION('center_axis',(-1.,0.,0.)) ;
#58663 = DIRECTION('ref_axis',(0.,0.,-1.)) ;
#58664 = DIRECTION('',(-1.,0.,-1.51760508056877E-16)) ;
#58665 = DIRECTION('center_axis',(1.51760508056877E-16,5.60383084497428E-34,
-1.)) ;
#58666 = DIRECTION('ref_axis',(-1.,0.,0.)) ;
#58667 = DIRECTION('center_axis',(0.,1.,0.)) ;
#58668 = DIRECTION('ref_axis',(0.,0.,-1.)) ;
#58669 = DIRECTION('center_axis',(-1.51760508056877E-16,-5.60383084497428E-34,
1.)) ;
#58670 = DIRECTION('ref_axis',(0.707106781186592,0.707106781186503,1.0731088436334E-16)) ;
#58671 = DIRECTION('center_axis',(0.,1.,5.60383084497428E-34)) ;
#58672 = DIRECTION('ref_axis',(-0.707106781186579,3.96250679110348E-34,-0.707106781186516)) ;
#58673 = DIRECTION('center_axis',(0.,1.,0.)) ;
#58674 = DIRECTION('ref_axis',(0.,0.,-1.)) ;
#58675 = DIRECTION('',(0.,1.,5.60383084497428E-34)) ;
#58676 = DIRECTION('center_axis',(-0.408248290463679,-0.816496580927927,0.408248290463644)) ;
#58677 = DIRECTION('ref_axis',(0.577350269189721,-0.577350269189436,-0.577350269189721)) ;
#58678 = DIRECTION('center_axis',(0.,0.,-1.)) ;
#58679 = DIRECTION('ref_axis',(0.707106781186636,-0.707106781186459,0.)) ;
#58680 = DIRECTION('center_axis',(-0.816496580927726,0.408248290463863,0.408248290463863)) ;
#58681 = DIRECTION('ref_axis',(-0.577350269189614,-0.577350269189756,-0.577350269189507)) ;
#58682 = DIRECTION('center_axis',(0.,0.,-1.)) ;
#58683 = DIRECTION('ref_axis',(-0.707106781186681,-0.707106781186414,0.)) ;
#58684 = DIRECTION('center_axis',(0.,0.,1.)) ;
#58685 = DIRECTION('ref_axis',(0.70710678118661,-0.707106781186485,0.)) ;
#58686 = DIRECTION('',(0.,0.,1.)) ;
#58687 = DIRECTION('center_axis',(-4.44089209850072E-14,0.,-1.)) ;
#58688 = DIRECTION('ref_axis',(0.,-1.,0.)) ;
#58689 = DIRECTION('',(0.,0.,-1.)) ;
#58690 = DIRECTION('center_axis',(0.,-1.,0.)) ;
#58691 = DIRECTION('ref_axis',(1.,0.,1.4923676700635E-16)) ;
#58692 = DIRECTION('',(0.,0.,-1.)) ;
#58693 = DIRECTION('',(-1.,0.,-1.51760508056877E-16)) ;
#58694 = DIRECTION('center_axis',(0.,0.,1.)) ;
#58695 = DIRECTION('ref_axis',(-0.707106781186359,-0.707106781186736,0.)) ;
#58696 = DIRECTION('',(0.,0.,1.)) ;
#58697 = DIRECTION('center_axis',(0.,0.,-1.)) ;
#58698 = DIRECTION('ref_axis',(-1.,0.,0.)) ;
#58699 = DIRECTION('center_axis',(-1.,0.,0.)) ;
#58700 = DIRECTION('ref_axis',(0.,-1.,0.)) ;
#58701 = DIRECTION('',(0.,0.,-1.)) ;
#58702 = DIRECTION('',(0.,1.,5.60383084497428E-34)) ;
#58703 = DIRECTION('center_axis',(0.,0.,1.)) ;
#58704 = DIRECTION('ref_axis',(-0.70710678118661,0.707106781186485,0.)) ;
#58705 = DIRECTION('',(0.,0.,1.)) ;
#58706 = DIRECTION('center_axis',(4.44089209850072E-14,0.,-1.)) ;
#58707 = DIRECTION('ref_axis',(0.,1.,0.)) ;
#58708 = DIRECTION('center_axis',(0.,1.,0.)) ;
#58709 = DIRECTION('ref_axis',(-1.,0.,-1.4923676700635E-16)) ;
#58710 = DIRECTION('',(0.,0.,-1.)) ;
#58711 = DIRECTION('',(1.,0.,1.51760508056877E-16)) ;
#58712 = DIRECTION('center_axis',(0.,0.,1.)) ;
#58713 = DIRECTION('ref_axis',(0.70710678118661,-0.707106781186485,0.)) ;
#58714 = DIRECTION('',(0.,0.,1.)) ;
#58715 = DIRECTION('center_axis',(0.,0.,1.)) ;
#58716 = DIRECTION('ref_axis',(1.,0.,0.)) ;
#58717 = DIRECTION('center_axis',(-1.,0.,0.)) ;
#58718 = DIRECTION('ref_axis',(0.,-1.,0.)) ;
#58719 = DIRECTION('',(0.,0.,-1.)) ;
#58720 = DIRECTION('',(0.,1.,5.60383084497428E-34)) ;
#58721 = DIRECTION('center_axis',(0.,0.,-1.)) ;
#58722 = DIRECTION('ref_axis',(-1.,0.,0.)) ;
#58723 = DIRECTION('center_axis',(-1.,0.,0.)) ;
#58724 = DIRECTION('ref_axis',(0.,1.,0.)) ;
#58725 = DIRECTION('center_axis',(0.,4.44089209849993E-14,1.)) ;
#58726 = DIRECTION('ref_axis',(1.,0.,0.)) ;
#58727 = DIRECTION('center_axis',(0.,1.,0.)) ;
#58728 = DIRECTION('ref_axis',(0.,0.,-1.)) ;
#58729 = DIRECTION('center_axis',(0.,0.,1.)) ;
#58730 = DIRECTION('ref_axis',(1.,0.,0.)) ;
#58731 = DIRECTION('center_axis',(4.44089209850072E-14,0.,1.)) ;
#58732 = DIRECTION('ref_axis',(0.,1.,0.)) ;
#58733 = DIRECTION('center_axis',(-1.,0.,0.)) ;
#58734 = DIRECTION('ref_axis',(0.,0.,-1.)) ;
#58735 = DIRECTION('center_axis',(0.,-1.,0.)) ;
#58736 = DIRECTION('ref_axis',(-1.,0.,0.)) ;
#58737 = DIRECTION('center_axis',(-1.,0.,-1.51760508056877E-16)) ;
#58738 = DIRECTION('ref_axis',(1.07310884363343E-16,-0.707106781186485,-0.70710678118661)) ;
#58739 = DIRECTION('center_axis',(1.,0.,0.)) ;
#58740 = DIRECTION('ref_axis',(0.,-1.,0.)) ;
#58741 = DIRECTION('',(-1.,0.,-1.51760508056877E-16)) ;
#58742 = DIRECTION('center_axis',(1.51760508056877E-16,5.60383084497428E-34,
-1.)) ;
#58743 = DIRECTION('ref_axis',(-1.,0.,0.)) ;
#58744 = DIRECTION('center_axis',(0.707106781186592,0.707106781186503,0.)) ;
#58745 = DIRECTION('ref_axis',(0.707106781186503,-0.707106781186592,0.)) ;
#58746 = DIRECTION('center_axis',(-1.51760508056877E-16,-5.60383084497428E-34,
1.)) ;
#58747 = DIRECTION('ref_axis',(-0.38268343236507,0.923879532511295,-5.80762321206726E-17)) ;
#58748 = DIRECTION('center_axis',(0.707106781186563,0.707106781186532,1.07310884363336E-16)) ;
#58749 = DIRECTION('ref_axis',(0.499999999999956,-0.499999999999978,-0.707106781186594)) ;
#58750 = DIRECTION('center_axis',(0.707106781186503,0.707106781186592,0.)) ;
#58751 = DIRECTION('ref_axis',(0.707106781186592,-0.707106781186503,0.)) ;
#58752 = DIRECTION('',(-0.707106781186563,-0.707106781186532,-1.07310884363336E-16)) ;
#58753 = DIRECTION('center_axis',(1.51760508056877E-16,5.60383084497428E-34,
-1.)) ;
#58754 = DIRECTION('ref_axis',(-1.,0.,0.)) ;
#58755 = DIRECTION('center_axis',(0.,1.,0.)) ;
#58756 = DIRECTION('ref_axis',(1.,0.,0.)) ;
#58757 = DIRECTION('center_axis',(-1.51760508056877E-16,-5.60383084497428E-34,
1.)) ;
#58758 = DIRECTION('ref_axis',(-0.923879532511313,0.382683432365025,-1.40208427237267E-16)) ;
#58759 = DIRECTION('center_axis',(-3.73034936274055E-14,-1.,-5.66175752827605E-30)) ;
#58760 = DIRECTION('ref_axis',(0.707106781186579,-2.63775533058888E-14,-0.707106781186516)) ;
#58761 = DIRECTION('center_axis',(0.,1.,0.)) ;
#58762 = DIRECTION('ref_axis',(1.,0.,0.)) ;
#58763 = DIRECTION('',(-3.73034936274055E-14,-1.,-5.66175752827605E-30)) ;
#58764 = DIRECTION('center_axis',(1.51760508056877E-16,5.60383084497428E-34,
-1.)) ;
#58765 = DIRECTION('ref_axis',(-1.,0.,0.)) ;
#58766 = DIRECTION('center_axis',(-0.707106781186636,0.707106781186459,0.)) ;
#58767 = DIRECTION('ref_axis',(0.707106781186459,0.707106781186636,0.)) ;
#58768 = DIRECTION('center_axis',(-1.51760508056877E-16,-5.60383084497428E-34,
1.)) ;
#58769 = DIRECTION('ref_axis',(-0.923879532511313,-0.382683432365025,-1.40208427237267E-16)) ;
#58770 = DIRECTION('center_axis',(-0.707106781186575,0.70710678118652,-1.07310884363338E-16)) ;
#58771 = DIRECTION('ref_axis',(0.499999999999948,0.499999999999986,-0.707106781186594)) ;
#58772 = DIRECTION('center_axis',(-0.707106781186503,0.707106781186592,0.)) ;
#58773 = DIRECTION('ref_axis',(0.707106781186592,0.707106781186503,0.)) ;
#58774 = DIRECTION('',(0.707106781186575,-0.70710678118652,1.07310884363338E-16)) ;
#58775 = DIRECTION('center_axis',(1.51760508056877E-16,5.60383084497428E-34,
-1.)) ;
#58776 = DIRECTION('ref_axis',(-1.,0.,0.)) ;
#58777 = DIRECTION('center_axis',(-1.,0.,0.)) ;
#58778 = DIRECTION('ref_axis',(0.,1.,0.)) ;
#58779 = DIRECTION('center_axis',(-1.51760508056877E-16,-5.60383084497428E-34,
1.)) ;
#58780 = DIRECTION('ref_axis',(-0.382683432364994,-0.923879532511326,-5.8076232120661E-17)) ;
#58781 = DIRECTION('center_axis',(1.,-7.10542735760144E-15,1.51760508056877E-16)) ;
#58782 = DIRECTION('ref_axis',(5.13160675215303E-15,0.707106781186736,-0.707106781186359)) ;
#58783 = DIRECTION('',(1.,-7.10542735760144E-15,1.51760508056877E-16)) ;
#58784 = DIRECTION('center_axis',(7.105427357601E-15,1.,1.07888364883526E-30)) ;
#58785 = DIRECTION('ref_axis',(-0.707106781186516,5.02429586778786E-15,-0.707106781186579)) ;
#58786 = DIRECTION('center_axis',(0.,-1.,0.)) ;
#58787 = DIRECTION('ref_axis',(-0.707106781186516,0.,-0.707106781186579)) ;
#58788 = DIRECTION('',(7.105427357601E-15,1.,1.07888364883526E-30)) ;
#58789 = DIRECTION('center_axis',(0.,0.,1.)) ;
#58790 = DIRECTION('ref_axis',(0.707106781186296,0.707106781186799,0.)) ;
#58791 = DIRECTION('center_axis',(0.,-4.44089209849835E-14,1.)) ;
#58792 = DIRECTION('ref_axis',(1.,0.,0.)) ;
#58793 = DIRECTION('',(0.,0.,-1.)) ;
#58794 = DIRECTION('',(0.,0.,1.)) ;
#58795 = DIRECTION('center_axis',(-0.894427190999916,0.447213595499958,0.)) ;
#58796 = DIRECTION('ref_axis',(-0.447213595499958,-0.894427190999916,0.)) ;
#58797 = DIRECTION('center_axis',(0.447213595500021,-0.894427190999884,0.)) ;
#58798 = DIRECTION('ref_axis',(-0.894427190999884,-0.447213595500021,0.)) ;
#58799 = DIRECTION('center_axis',(0.,0.,1.)) ;
#58800 = DIRECTION('ref_axis',(0.707106781186548,-0.707106781186548,0.)) ;
#58801 = DIRECTION('center_axis',(4.44089209850072E-14,0.,1.)) ;
#58802 = DIRECTION('ref_axis',(0.,-1.,0.)) ;
#58803 = DIRECTION('',(0.,0.,-1.)) ;
#58804 = DIRECTION('',(0.,0.,1.)) ;
#58805 = DIRECTION('center_axis',(0.447213595500021,0.894427190999884,0.)) ;
#58806 = DIRECTION('ref_axis',(-0.894427190999884,0.447213595500021,0.)) ;
#58807 = DIRECTION('center_axis',(-0.894427190999916,-0.447213595499958,0.)) ;
#58808 = DIRECTION('ref_axis',(-0.447213595499958,0.894427190999916,0.)) ;
#58809 = DIRECTION('center_axis',(7.105427357601E-15,1.,1.07888364883526E-30)) ;
#58810 = DIRECTION('ref_axis',(-0.707106781186516,5.02429586778786E-15,-0.707106781186579)) ;
#58811 = DIRECTION('center_axis',(3.55271367880051E-14,1.,0.)) ;
#58812 = DIRECTION('ref_axis',(-0.707106781186516,2.51214793389393E-14,-0.707106781186579)) ;
#58813 = DIRECTION('',(7.105427357601E-15,1.,1.07888364883526E-30)) ;
#58814 = DIRECTION('center_axis',(1.,-7.105427357601E-15,0.)) ;
#58815 = DIRECTION('ref_axis',(7.105427357601E-15,1.,1.06039100704685E-30)) ;
#58816 = DIRECTION('',(0.,0.,1.)) ;
#58817 = DIRECTION('',(-7.105427357601E-15,-1.,-1.07888364883526E-30)) ;
#58818 = DIRECTION('center_axis',(1.51760508056877E-16,5.60383084497428E-34,
-1.)) ;
#58819 = DIRECTION('ref_axis',(-1.,0.,0.)) ;
#58820 = DIRECTION('center_axis',(-1.,0.,0.)) ;
#58821 = DIRECTION('ref_axis',(0.,0.,-1.)) ;
#58822 = DIRECTION('center_axis',(0.,0.,1.)) ;
#58823 = DIRECTION('ref_axis',(0.,1.,0.)) ;
#58824 = DIRECTION('center_axis',(0.,1.,0.)) ;
#58825 = DIRECTION('ref_axis',(0.707106781186548,0.,-0.707106781186548)) ;
#58826 = DIRECTION('center_axis',(-1.,0.,-1.51760508056877E-16)) ;
#58827 = DIRECTION('ref_axis',(1.07310884363343E-16,-0.707106781186485,-0.70710678118661)) ;
#58828 = DIRECTION('center_axis',(-1.,0.,0.)) ;
#58829 = DIRECTION('ref_axis',(0.,0.,-1.)) ;
#58830 = DIRECTION('',(-1.,0.,-1.51760508056877E-16)) ;
#58831 = DIRECTION('center_axis',(0.,-1.,-5.60383084497428E-34)) ;
#58832 = DIRECTION('ref_axis',(0.707106781186548,3.96250679110365E-34,-0.707106781186548)) ;
#58833 = DIRECTION('center_axis',(0.,-1.,0.)) ;
#58834 = DIRECTION('ref_axis',(0.,0.,-1.)) ;
#58835 = DIRECTION('',(0.,-1.,-5.60383084497428E-34)) ;
#58836 = DIRECTION('center_axis',(0.,1.,0.)) ;
#58837 = DIRECTION('ref_axis',(1.,0.,0.)) ;
#58838 = DIRECTION('center_axis',(1.51760508056877E-16,5.60383084497428E-34,
-1.)) ;
#58839 = DIRECTION('ref_axis',(-1.,0.,0.)) ;
#58840 = DIRECTION('center_axis',(-1.,0.,0.)) ;
#58841 = DIRECTION('ref_axis',(0.,0.,-1.)) ;
#58842 = DIRECTION('center_axis',(-1.51760508056877E-16,-5.60383084497428E-34,
1.)) ;
#58843 = DIRECTION('ref_axis',(-0.707106781186592,0.707106781186503,-1.0731088436334E-16)) ;
#58844 = DIRECTION('center_axis',(-1.,0.,-1.51760508056877E-16)) ;
#58845 = DIRECTION('ref_axis',(1.07310884363343E-16,-0.707106781186485,-0.70710678118661)) ;
#58846 = DIRECTION('center_axis',(-1.,0.,0.)) ;
#58847 = DIRECTION('ref_axis',(0.,0.,-1.)) ;
#58848 = DIRECTION('',(-1.,0.,-1.51760508056877E-16)) ;
#58849 = DIRECTION('center_axis',(1.51760508056877E-16,5.60383084497428E-34,
-1.)) ;
#58850 = DIRECTION('ref_axis',(-1.,0.,0.)) ;
#58851 = DIRECTION('center_axis',(0.,1.,0.)) ;
#58852 = DIRECTION('ref_axis',(0.,0.,-1.)) ;
#58853 = DIRECTION('center_axis',(-1.51760508056877E-16,-5.60383084497428E-34,
1.)) ;
#58854 = DIRECTION('ref_axis',(0.707106781186592,0.707106781186503,1.0731088436334E-16)) ;
#58855 = DIRECTION('center_axis',(0.,1.,5.60383084497428E-34)) ;
#58856 = DIRECTION('ref_axis',(-0.707106781186548,3.96250679110365E-34,-0.707106781186548)) ;
#58857 = DIRECTION('center_axis',(0.,1.,0.)) ;
#58858 = DIRECTION('ref_axis',(0.,0.,-1.)) ;
#58859 = DIRECTION('',(0.,1.,5.60383084497428E-34)) ;
#58860 = DIRECTION('center_axis',(-0.408248290463679,-0.816496580927927,0.408248290463644)) ;
#58861 = DIRECTION('ref_axis',(0.577350269189732,-0.577350269189448,-0.577350269189697)) ;
#58862 = DIRECTION('center_axis',(0.,0.,-1.)) ;
#58863 = DIRECTION('ref_axis',(0.707106781186636,-0.707106781186459,0.)) ;
#58864 = DIRECTION('center_axis',(-1.,0.,-1.51760508056877E-16)) ;
#58865 = DIRECTION('ref_axis',(1.07310884363343E-16,-0.707106781186485,-0.70710678118661)) ;
#58866 = DIRECTION('center_axis',(-1.,0.,0.)) ;
#58867 = DIRECTION('ref_axis',(0.,0.,-1.)) ;
#58868 = DIRECTION('',(-1.,0.,-1.51760508056877E-16)) ;
#58869 = DIRECTION('center_axis',(1.,0.,0.)) ;
#58870 = DIRECTION('ref_axis',(0.,-1.,0.)) ;
#58871 = DIRECTION('center_axis',(1.51760508056877E-16,5.60383084497428E-34,
-1.)) ;
#58872 = DIRECTION('ref_axis',(-1.,0.,0.)) ;
#58873 = DIRECTION('center_axis',(0.,1.,0.)) ;
#58874 = DIRECTION('ref_axis',(-0.707106781186548,0.,-0.707106781186548)) ;
#58875 = DIRECTION('center_axis',(0.,0.,-1.)) ;
#58876 = DIRECTION('ref_axis',(0.,1.,0.)) ;
#58877 = DIRECTION('center_axis',(-0.816496580927726,0.408248290463863,0.408248290463863)) ;
#58878 = DIRECTION('ref_axis',(-0.577350269189614,-0.577350269189756,-0.577350269189507)) ;
#58879 = DIRECTION('center_axis',(0.,0.,-1.)) ;
#58880 = DIRECTION('ref_axis',(-0.707106781186681,-0.707106781186414,0.)) ;
#58881 = DIRECTION('center_axis',(0.,1.,0.)) ;
#58882 = DIRECTION('ref_axis',(-1.,0.,-1.4923676700635E-16)) ;
#58883 = DIRECTION('',(0.,0.,-1.)) ;
#58884 = DIRECTION('',(1.,0.,1.51760508056877E-16)) ;
#58885 = DIRECTION('',(0.,0.,1.)) ;
#58886 = DIRECTION('center_axis',(0.,0.,1.)) ;
#58887 = DIRECTION('ref_axis',(0.70710678118661,-0.707106781186485,0.)) ;
#58888 = DIRECTION('',(0.,0.,1.)) ;
#58889 = DIRECTION('center_axis',(0.,0.,1.)) ;
#58890 = DIRECTION('ref_axis',(1.,0.,0.)) ;
#58891 = DIRECTION('center_axis',(-1.,0.,0.)) ;
#58892 = DIRECTION('ref_axis',(0.,-1.,0.)) ;
#58893 = DIRECTION('',(0.,0.,-1.)) ;
#58894 = DIRECTION('',(0.,1.,5.60383084497428E-34)) ;
#58895 = DIRECTION('center_axis',(0.,0.,1.)) ;
#58896 = DIRECTION('ref_axis',(-0.70710678118661,0.707106781186485,0.)) ;
#58897 = DIRECTION('',(0.,0.,1.)) ;
#58898 = DIRECTION('center_axis',(0.,0.,-1.)) ;
#58899 = DIRECTION('ref_axis',(0.,1.,0.)) ;
#58900 = DIRECTION('center_axis',(0.,1.,0.)) ;
#58901 = DIRECTION('ref_axis',(-1.,0.,-1.4923676700635E-16)) ;
#58902 = DIRECTION('',(0.,0.,-1.)) ;
#58903 = DIRECTION('',(1.,0.,1.51760508056877E-16)) ;
#58904 = DIRECTION('center_axis',(0.,0.,1.)) ;
#58905 = DIRECTION('ref_axis',(0.70710678118661,0.707106781186485,0.)) ;
#58906 = DIRECTION('',(0.,0.,1.)) ;
#58907 = DIRECTION('center_axis',(0.,0.,-1.)) ;
#58908 = DIRECTION('ref_axis',(1.,0.,0.)) ;
#58909 = DIRECTION('center_axis',(1.,0.,0.)) ;
#58910 = DIRECTION('ref_axis',(0.,1.,0.)) ;
#58911 = DIRECTION('',(0.,0.,-1.)) ;
#58912 = DIRECTION('',(0.,-1.,-5.60383084497428E-34)) ;
#58913 = DIRECTION('center_axis',(0.,0.,1.)) ;
#58914 = DIRECTION('ref_axis',(-0.707106781186673,-0.707106781186422,0.)) ;
#58915 = DIRECTION('',(0.,0.,1.)) ;
#58916 = DIRECTION('center_axis',(0.,0.,1.)) ;
#58917 = DIRECTION('ref_axis',(0.,-1.,0.)) ;
#58918 = DIRECTION('center_axis',(0.,1.,0.)) ;
#58919 = DIRECTION('ref_axis',(-1.,0.,-1.4923676700635E-16)) ;
#58920 = DIRECTION('',(0.,0.,-1.)) ;
#58921 = DIRECTION('',(1.,0.,1.51760508056877E-16)) ;
#58922 = DIRECTION('center_axis',(1.51760508056877E-16,5.60383084497428E-34,
-1.)) ;
#58923 = DIRECTION('ref_axis',(-1.,0.,0.)) ;
#58924 = DIRECTION('center_axis',(-1.,0.,0.)) ;
#58925 = DIRECTION('ref_axis',(0.,0.,-1.)) ;
#58926 = DIRECTION('center_axis',(0.,0.,1.)) ;
#58927 = DIRECTION('ref_axis',(0.,1.,0.)) ;
#58928 = DIRECTION('center_axis',(0.,1.,0.)) ;
#58929 = DIRECTION('ref_axis',(0.707106781186548,0.,-0.707106781186548)) ;
#58930 = DIRECTION('center_axis',(-1.,0.,-1.51760508056877E-16)) ;
#58931 = DIRECTION('ref_axis',(1.07310884363343E-16,-0.707106781186485,-0.70710678118661)) ;
#58932 = DIRECTION('center_axis',(-1.,0.,0.)) ;
#58933 = DIRECTION('ref_axis',(0.,0.,-1.)) ;
#58934 = DIRECTION('',(-1.,0.,-1.51760508056877E-16)) ;
#58935 = DIRECTION('center_axis',(0.,-1.,-5.60383084497428E-34)) ;
#58936 = DIRECTION('ref_axis',(0.707106781186548,3.96250679110365E-34,-0.707106781186548)) ;
#58937 = DIRECTION('center_axis',(0.,-1.,0.)) ;
#58938 = DIRECTION('ref_axis',(0.,0.,-1.)) ;
#58939 = DIRECTION('',(0.,-1.,-5.60383084497428E-34)) ;
#58940 = DIRECTION('center_axis',(0.,1.,0.)) ;
#58941 = DIRECTION('ref_axis',(1.,0.,0.)) ;
#58942 = DIRECTION('center_axis',(1.51760508056877E-16,5.60383084497428E-34,
-1.)) ;
#58943 = DIRECTION('ref_axis',(-1.,0.,0.)) ;
#58944 = DIRECTION('center_axis',(-1.,0.,0.)) ;
#58945 = DIRECTION('ref_axis',(0.,0.,-1.)) ;
#58946 = DIRECTION('center_axis',(-1.51760508056877E-16,-5.60383084497428E-34,
1.)) ;
#58947 = DIRECTION('ref_axis',(-0.707106781186636,0.707106781186459,-1.07310884363347E-16)) ;
#58948 = DIRECTION('center_axis',(-1.,0.,-1.51760508056877E-16)) ;
#58949 = DIRECTION('ref_axis',(1.07310884363343E-16,-0.707106781186485,-0.70710678118661)) ;
#58950 = DIRECTION('center_axis',(-1.,0.,0.)) ;
#58951 = DIRECTION('ref_axis',(0.,0.,-1.)) ;
#58952 = DIRECTION('',(-1.,0.,-1.51760508056877E-16)) ;
#58953 = DIRECTION('center_axis',(1.51760508056877E-16,5.60383084497428E-34,
-1.)) ;
#58954 = DIRECTION('ref_axis',(-1.,0.,0.)) ;
#58955 = DIRECTION('center_axis',(0.,1.,0.)) ;
#58956 = DIRECTION('ref_axis',(0.,0.,-1.)) ;
#58957 = DIRECTION('center_axis',(-1.51760508056877E-16,-5.60383084497428E-34,
1.)) ;
#58958 = DIRECTION('ref_axis',(0.707106781186592,0.707106781186503,1.0731088436334E-16)) ;
#58959 = DIRECTION('center_axis',(0.,1.,5.60383084497428E-34)) ;
#58960 = DIRECTION('ref_axis',(-0.707106781186548,3.96250679110365E-34,-0.707106781186548)) ;
#58961 = DIRECTION('center_axis',(0.,1.,0.)) ;
#58962 = DIRECTION('ref_axis',(0.,0.,-1.)) ;
#58963 = DIRECTION('',(0.,1.,5.60383084497428E-34)) ;
#58964 = DIRECTION('center_axis',(-0.40824829046362,-0.816496580927951,0.408248290463656)) ;
#58965 = DIRECTION('ref_axis',(0.577350269189721,-0.577350269189436,-0.577350269189721)) ;
#58966 = DIRECTION('center_axis',(0.,0.,-1.)) ;
#58967 = DIRECTION('ref_axis',(0.707106781186636,-0.707106781186459,0.)) ;
#58968 = DIRECTION('center_axis',(-1.,0.,-1.51760508056877E-16)) ;
#58969 = DIRECTION('ref_axis',(1.07310884363343E-16,-0.707106781186485,-0.70710678118661)) ;
#58970 = DIRECTION('center_axis',(-1.,0.,0.)) ;
#58971 = DIRECTION('ref_axis',(0.,0.,-1.)) ;
#58972 = DIRECTION('',(-1.,0.,-1.51760508056877E-16)) ;
#58973 = DIRECTION('center_axis',(1.,0.,0.)) ;
#58974 = DIRECTION('ref_axis',(0.,-1.,0.)) ;
#58975 = DIRECTION('center_axis',(1.51760508056877E-16,5.60383084497428E-34,
-1.)) ;
#58976 = DIRECTION('ref_axis',(-1.,0.,0.)) ;
#58977 = DIRECTION('center_axis',(0.,1.,0.)) ;
#58978 = DIRECTION('ref_axis',(-0.707106781186548,0.,-0.707106781186548)) ;
#58979 = DIRECTION('center_axis',(0.,0.,-1.)) ;
#58980 = DIRECTION('ref_axis',(0.,1.,0.)) ;
#58981 = DIRECTION('center_axis',(-0.81649658092775,0.408248290463875,0.408248290463804)) ;
#58982 = DIRECTION('ref_axis',(-0.577350269189602,-0.577350269189744,-0.577350269189531)) ;
#58983 = DIRECTION('center_axis',(0.,0.,-1.)) ;
#58984 = DIRECTION('ref_axis',(-0.707106781186636,-0.707106781186459,0.)) ;
#58985 = DIRECTION('center_axis',(0.,1.,0.)) ;
#58986 = DIRECTION('ref_axis',(-1.,0.,-1.4923676700635E-16)) ;
#58987 = DIRECTION('',(0.,0.,-1.)) ;
#58988 = DIRECTION('',(1.,0.,1.51760508056877E-16)) ;
#58989 = DIRECTION('',(0.,0.,1.)) ;
#58990 = DIRECTION('center_axis',(0.,0.,1.)) ;
#58991 = DIRECTION('ref_axis',(0.70710678118661,-0.707106781186485,0.)) ;
#58992 = DIRECTION('',(0.,0.,1.)) ;
#58993 = DIRECTION('center_axis',(0.,0.,1.)) ;
#58994 = DIRECTION('ref_axis',(1.,0.,0.)) ;
#58995 = DIRECTION('center_axis',(-1.,0.,0.)) ;
#58996 = DIRECTION('ref_axis',(0.,-1.,0.)) ;
#58997 = DIRECTION('',(0.,0.,-1.)) ;
#58998 = DIRECTION('',(0.,1.,5.60383084497428E-34)) ;
#58999 = DIRECTION('center_axis',(0.,0.,1.)) ;
#59000 = DIRECTION('ref_axis',(-0.707106781186673,0.707106781186422,0.)) ;
#59001 = DIRECTION('',(0.,0.,1.)) ;
#59002 = DIRECTION('center_axis',(0.,0.,-1.)) ;
#59003 = DIRECTION('ref_axis',(0.,1.,0.)) ;
#59004 = DIRECTION('center_axis',(0.,1.,0.)) ;
#59005 = DIRECTION('ref_axis',(-1.,0.,-1.4923676700635E-16)) ;
#59006 = DIRECTION('',(0.,0.,-1.)) ;
#59007 = DIRECTION('',(1.,0.,1.51760508056877E-16)) ;
#59008 = DIRECTION('center_axis',(0.,0.,1.)) ;
#59009 = DIRECTION('ref_axis',(0.70710678118661,0.707106781186485,0.)) ;
#59010 = DIRECTION('',(0.,0.,1.)) ;
#59011 = DIRECTION('center_axis',(0.,0.,-1.)) ;
#59012 = DIRECTION('ref_axis',(1.,0.,0.)) ;
#59013 = DIRECTION('center_axis',(1.,0.,0.)) ;
#59014 = DIRECTION('ref_axis',(0.,1.,0.)) ;
#59015 = DIRECTION('',(0.,0.,-1.)) ;
#59016 = DIRECTION('',(0.,-1.,-5.60383084497428E-34)) ;
#59017 = DIRECTION('center_axis',(0.,0.,1.)) ;
#59018 = DIRECTION('ref_axis',(-0.70710678118661,-0.707106781186485,0.)) ;
#59019 = DIRECTION('',(0.,0.,1.)) ;
#59020 = DIRECTION('center_axis',(0.,0.,1.)) ;
#59021 = DIRECTION('ref_axis',(0.,-1.,0.)) ;
#59022 = DIRECTION('center_axis',(0.,1.,0.)) ;
#59023 = DIRECTION('ref_axis',(-1.,0.,-1.4923676700635E-16)) ;
#59024 = DIRECTION('',(0.,0.,-1.)) ;
#59025 = DIRECTION('',(1.,0.,1.51760508056877E-16)) ;
#59026 = DIRECTION('center_axis',(0.,1.,5.60383084497428E-34)) ;
#59027 = DIRECTION('ref_axis',(-0.707106781186548,3.96250679110365E-34,-0.707106781186548)) ;
#59028 = DIRECTION('center_axis',(0.,1.,0.)) ;
#59029 = DIRECTION('ref_axis',(0.,0.,-1.)) ;
#59030 = DIRECTION('center_axis',(-1.,0.,-1.51760508056877E-16)) ;
#59031 = DIRECTION('ref_axis',(1.07310884363343E-16,-0.707106781186485,-0.70710678118661)) ;
#59032 = DIRECTION('center_axis',(-1.,0.,0.)) ;
#59033 = DIRECTION('ref_axis',(0.,0.,-1.)) ;
#59034 = DIRECTION('',(-1.,0.,-1.51760508056877E-16)) ;
#59035 = DIRECTION('center_axis',(1.,0.,0.)) ;
#59036 = DIRECTION('ref_axis',(0.,-1.,0.)) ;
#59037 = DIRECTION('center_axis',(1.51760508056877E-16,5.60383084497428E-34,
-1.)) ;
#59038 = DIRECTION('ref_axis',(-1.,0.,0.)) ;
#59039 = DIRECTION('center_axis',(0.,1.,0.)) ;
#59040 = DIRECTION('ref_axis',(-0.707106781186548,0.,-0.707106781186548)) ;
#59041 = DIRECTION('center_axis',(0.,0.,-1.)) ;
#59042 = DIRECTION('ref_axis',(0.,1.,0.)) ;
#59043 = DIRECTION('center_axis',(-0.816496580927773,0.408248290463851,0.40824829046378)) ;
#59044 = DIRECTION('ref_axis',(-0.577350269189543,-0.577350269189756,-0.577350269189578)) ;
#59045 = DIRECTION('center_axis',(0.,1.,0.)) ;
#59046 = DIRECTION('ref_axis',(-1.,0.,-1.4923676700635E-16)) ;
#59047 = DIRECTION('',(0.,0.,-1.)) ;
#59048 = DIRECTION('center_axis',(0.,-1.,-5.60383084497428E-34)) ;
#59049 = DIRECTION('ref_axis',(0.707106781186548,3.96250679110365E-34,-0.707106781186548)) ;
#59050 = DIRECTION('',(0.,-1.,-5.60383084497428E-34)) ;
#59051 = DIRECTION('center_axis',(1.51760508056877E-16,5.60383084497428E-34,
-1.)) ;
#59052 = DIRECTION('ref_axis',(-1.,0.,0.)) ;
#59053 = DIRECTION('center_axis',(0.,0.,1.)) ;
#59054 = DIRECTION('ref_axis',(0.,1.,0.)) ;
#59055 = DIRECTION('center_axis',(0.,1.,0.)) ;
#59056 = DIRECTION('ref_axis',(0.707106781186548,0.,-0.707106781186548)) ;
#59057 = DIRECTION('center_axis',(-1.,0.,0.)) ;
#59058 = DIRECTION('ref_axis',(0.,-1.,0.)) ;
#59059 = DIRECTION('center_axis',(1.,0.,1.51760508056877E-16)) ;
#59060 = DIRECTION('ref_axis',(1.07310884363343E-16,0.707106781186485,-0.70710678118661)) ;
#59061 = DIRECTION('',(1.,0.,1.51760508056877E-16)) ;
#59062 = DIRECTION('center_axis',(-1.,0.,0.)) ;
#59063 = DIRECTION('ref_axis',(0.,1.,0.)) ;
#59064 = DIRECTION('center_axis',(1.51760508056877E-16,5.60383084497428E-34,
-1.)) ;
#59065 = DIRECTION('ref_axis',(-1.,0.,0.)) ;
#59066 = DIRECTION('center_axis',(-0.707106781186636,-0.707106781186459,0.)) ;
#59067 = DIRECTION('ref_axis',(-0.707106781186459,0.707106781186636,0.)) ;
#59068 = DIRECTION('center_axis',(-1.51760508056877E-16,-5.60383084497428E-34,
1.)) ;
#59069 = DIRECTION('ref_axis',(0.382683432364994,-0.923879532511326,5.8076232120661E-17)) ;
#59070 = DIRECTION('center_axis',(-0.707106781186555,-0.70710678118654,-1.07310884363335E-16)) ;
#59071 = DIRECTION('ref_axis',(-0.499999999999931,0.499999999999941,-0.707106781186638)) ;
#59072 = DIRECTION('center_axis',(-0.707106781186592,-0.707106781186503,0.)) ;
#59073 = DIRECTION('ref_axis',(-0.707106781186503,0.707106781186592,0.)) ;
#59074 = DIRECTION('',(0.707106781186555,0.70710678118654,1.07310884363335E-16)) ;
#59075 = DIRECTION('center_axis',(1.51760508056877E-16,5.60383084497428E-34,
-1.)) ;
#59076 = DIRECTION('ref_axis',(-1.,0.,0.)) ;
#59077 = DIRECTION('center_axis',(0.,-1.,0.)) ;
#59078 = DIRECTION('ref_axis',(-1.,0.,0.)) ;
#59079 = DIRECTION('center_axis',(-1.51760508056877E-16,-5.60383084497428E-34,
1.)) ;
#59080 = DIRECTION('ref_axis',(0.923879532511313,-0.382683432365025,1.40208427237267E-16)) ;
#59081 = DIRECTION('center_axis',(0.,1.,5.60383084497428E-34)) ;
#59082 = DIRECTION('ref_axis',(-0.707106781186548,3.96250679110365E-34,-0.707106781186548)) ;
#59083 = DIRECTION('center_axis',(0.,-1.,0.)) ;
#59084 = DIRECTION('ref_axis',(-1.,0.,0.)) ;
#59085 = DIRECTION('',(0.,1.,5.60383084497428E-34)) ;
#59086 = DIRECTION('center_axis',(1.51760508056877E-16,5.60383084497428E-34,
-1.)) ;
#59087 = DIRECTION('ref_axis',(-1.,0.,0.)) ;
#59088 = DIRECTION('center_axis',(0.707106781186459,-0.707106781186636,0.)) ;
#59089 = DIRECTION('ref_axis',(-0.707106781186636,-0.707106781186459,0.)) ;
#59090 = DIRECTION('center_axis',(-1.51760508056877E-16,-5.60383084497428E-34,
1.)) ;
#59091 = DIRECTION('ref_axis',(0.923879532511313,0.382683432365025,1.40208427237267E-16)) ;
#59092 = DIRECTION('center_axis',(0.707106781186555,-0.70710678118654,1.07310884363335E-16)) ;
#59093 = DIRECTION('ref_axis',(-0.499999999999962,-0.499999999999972,-0.707106781186594)) ;
#59094 = DIRECTION('center_axis',(0.707106781186503,-0.707106781186592,0.)) ;
#59095 = DIRECTION('ref_axis',(-0.707106781186592,-0.707106781186503,0.)) ;
#59096 = DIRECTION('',(-0.707106781186555,0.70710678118654,-1.07310884363335E-16)) ;
#59097 = DIRECTION('center_axis',(1.51760508056877E-16,5.60383084497428E-34,
-1.)) ;
#59098 = DIRECTION('ref_axis',(-1.,0.,0.)) ;
#59099 = DIRECTION('center_axis',(1.,0.,0.)) ;
#59100 = DIRECTION('ref_axis',(0.,-1.,0.)) ;
#59101 = DIRECTION('center_axis',(-1.51760508056877E-16,-5.60383084497428E-34,
1.)) ;
#59102 = DIRECTION('ref_axis',(0.382683432364994,0.923879532511326,5.8076232120661E-17)) ;
#59103 = DIRECTION('center_axis',(-1.,0.,-1.51760508056877E-16)) ;
#59104 = DIRECTION('ref_axis',(1.07310884363343E-16,-0.707106781186485,-0.70710678118661)) ;
#59105 = DIRECTION('',(-1.,0.,-1.51760508056877E-16)) ;
#59106 = DIRECTION('center_axis',(0.,1.,0.)) ;
#59107 = DIRECTION('ref_axis',(-1.,0.,-1.4923676700635E-16)) ;
#59108 = DIRECTION('',(0.,0.,-1.)) ;
#59109 = DIRECTION('',(1.,0.,1.51760508056877E-16)) ;
#59110 = DIRECTION('center_axis',(0.,0.,-1.)) ;
#59111 = DIRECTION('ref_axis',(0.382683432365017,0.923879532511317,0.)) ;
#59112 = DIRECTION('',(0.,0.,1.)) ;
#59113 = DIRECTION('center_axis',(-4.44089209850105E-14,4.44089209849993E-14,
-1.)) ;
#59114 = DIRECTION('ref_axis',(0.707106781186459,0.707106781186636,-6.25253024584262E-29)) ;
#59115 = DIRECTION('center_axis',(-0.70710678118654,-0.707106781186555,0.)) ;
#59116 = DIRECTION('ref_axis',(0.,0.,1.)) ;
#59117 = DIRECTION('',(0.,0.,-1.)) ;
#59118 = DIRECTION('',(0.707106781186555,-0.70710678118654,1.07310884363335E-16)) ;
#59119 = DIRECTION('center_axis',(0.,0.,1.)) ;
#59120 = DIRECTION('ref_axis',(0.923879532511311,0.382683432365031,0.)) ;
#59121 = DIRECTION('',(0.,0.,1.)) ;
#59122 = DIRECTION('center_axis',(0.,-6.28036983473606E-14,-1.)) ;
#59123 = DIRECTION('ref_axis',(1.,0.,0.)) ;
#59124 = DIRECTION('center_axis',(1.,0.,0.)) ;
#59125 = DIRECTION('ref_axis',(0.,1.,0.)) ;
#59126 = DIRECTION('',(0.,0.,-1.)) ;
#59127 = DIRECTION('',(0.,-1.,-5.60383084497428E-34)) ;
#59128 = DIRECTION('center_axis',(0.,0.,-1.)) ;
#59129 = DIRECTION('ref_axis',(0.923879532511311,-0.382683432365031,0.)) ;
#59130 = DIRECTION('',(0.,0.,1.)) ;
#59131 = DIRECTION('center_axis',(4.44089209850072E-14,4.44089209850128E-14,
-1.)) ;
#59132 = DIRECTION('ref_axis',(0.707106781186592,-0.707106781186503,-9.0726912223815E-30)) ;
#59133 = DIRECTION('center_axis',(-0.70710678118654,0.707106781186555,0.)) ;
#59134 = DIRECTION('ref_axis',(0.,0.,1.)) ;
#59135 = DIRECTION('',(0.,0.,-1.)) ;
#59136 = DIRECTION('',(-0.707106781186555,-0.70710678118654,-1.07310884363335E-16)) ;
#59137 = DIRECTION('center_axis',(0.,0.,1.)) ;
#59138 = DIRECTION('ref_axis',(0.382683432365017,-0.923879532511317,0.)) ;
#59139 = DIRECTION('',(0.,0.,1.)) ;
#59140 = DIRECTION('center_axis',(0.,0.,-1.)) ;
#59141 = DIRECTION('ref_axis',(0.,-1.,0.)) ;
#59142 = DIRECTION('center_axis',(0.,-1.,0.)) ;
#59143 = DIRECTION('ref_axis',(1.,0.,1.4923676700635E-16)) ;
#59144 = DIRECTION('',(-1.,0.,-1.51760508056877E-16)) ;
#59145 = DIRECTION('center_axis',(0.,0.,1.)) ;
#59146 = DIRECTION('ref_axis',(-0.707106781186673,0.707106781186422,0.)) ;
#59147 = DIRECTION('',(0.,0.,-1.)) ;
#59148 = DIRECTION('center_axis',(1.51760508056877E-16,5.60383084497428E-34,
-1.)) ;
#59149 = DIRECTION('ref_axis',(-1.,0.,0.)) ;
#59150 = DIRECTION('center_axis',(-1.,0.,0.)) ;
#59151 = DIRECTION('ref_axis',(0.,1.,4.44089209849993E-14)) ;
#59152 = DIRECTION('center_axis',(0.,0.,1.)) ;
#59153 = DIRECTION('ref_axis',(0.,-1.,0.)) ;
#59154 = DIRECTION('center_axis',(0.,-1.,0.)) ;
#59155 = DIRECTION('ref_axis',(-0.707106781186548,0.,-0.707106781186548)) ;
#59156 = DIRECTION('center_axis',(0.,-1.,0.)) ;
#59157 = DIRECTION('ref_axis',(1.,0.,1.4923676700635E-16)) ;
#59158 = DIRECTION('',(1.,0.,1.51760508056877E-16)) ;
#59159 = DIRECTION('',(0.,0.,-1.)) ;
#59160 = DIRECTION('',(-1.,0.,-1.51760508056877E-16)) ;
#59161 = DIRECTION('',(0.,0.,1.)) ;
#59162 = DIRECTION('center_axis',(0.,0.,1.)) ;
#59163 = DIRECTION('ref_axis',(1.,0.,0.)) ;
#59164 = DIRECTION('center_axis',(0.,0.,-1.)) ;
#59165 = DIRECTION('ref_axis',(1.,0.,0.)) ;
#59166 = DIRECTION('center_axis',(0.,-1.,0.)) ;
#59167 = DIRECTION('ref_axis',(0.,0.,1.)) ;
#59168 = DIRECTION('center_axis',(0.,0.,1.)) ;
#59169 = DIRECTION('ref_axis',(0.707106781186359,0.707106781186736,0.)) ;
#59170 = DIRECTION('',(0.,0.,1.)) ;
#59171 = DIRECTION('center_axis',(0.,0.,1.)) ;
#59172 = DIRECTION('ref_axis',(1.,0.,0.)) ;
#59173 = DIRECTION('center_axis',(1.,0.,0.)) ;
#59174 = DIRECTION('ref_axis',(0.,1.,0.)) ;
#59175 = DIRECTION('center_axis',(0.,0.,-1.)) ;
#59176 = DIRECTION('ref_axis',(-1.,0.,0.)) ;
#59177 = DIRECTION('center_axis',(0.,1.,0.)) ;
#59178 = DIRECTION('ref_axis',(0.,0.,1.)) ;
#59179 = DIRECTION('center_axis',(0.,0.,1.)) ;
#59180 = DIRECTION('ref_axis',(1.,0.,0.)) ;
#59181 = DIRECTION('center_axis',(0.,1.,0.)) ;
#59182 = DIRECTION('ref_axis',(-1.,0.,0.)) ;
#59183 = DIRECTION('center_axis',(4.44089209850072E-14,0.,-1.)) ;
#59184 = DIRECTION('ref_axis',(0.,-1.,0.)) ;
#59185 = DIRECTION('center_axis',(-1.,0.,0.)) ;
#59186 = DIRECTION('ref_axis',(0.,0.,1.)) ;
#59187 = DIRECTION('center_axis',(0.,-1.,-5.60383084497428E-34)) ;
#59188 = DIRECTION('ref_axis',(-0.707106781186548,-3.96250679110365E-34,0.707106781186548)) ;
#59189 = DIRECTION('',(0.,-1.,-5.60383084497428E-34)) ;
#59190 = DIRECTION('center_axis',(0.,0.,1.)) ;
#59191 = DIRECTION('ref_axis',(0.70710678118661,-0.707106781186485,0.)) ;
#59192 = DIRECTION('',(0.,0.,-1.)) ;
#59193 = DIRECTION('center_axis',(-1.,0.,-1.51760508056877E-16)) ;
#59194 = DIRECTION('ref_axis',(-1.07310884363343E-16,0.707106781186485,0.70710678118661)) ;
#59195 = DIRECTION('center_axis',(0.,0.,1.)) ;
#59196 = DIRECTION('ref_axis',(1.,0.,0.)) ;
#59197 = DIRECTION('center_axis',(0.,0.,1.)) ;
#59198 = DIRECTION('ref_axis',(0.,-1.,0.)) ;
#59199 = DIRECTION('center_axis',(1.,0.,0.)) ;
#59200 = DIRECTION('ref_axis',(0.,0.,-1.)) ;
#59201 = DIRECTION('center_axis',(0.,1.,0.)) ;
#59202 = DIRECTION('ref_axis',(1.,0.,0.)) ;
#59203 = DIRECTION('center_axis',(1.,0.,1.51760508056877E-16)) ;
#59204 = DIRECTION('ref_axis',(1.07310884363343E-16,0.707106781186485,-0.70710678118661)) ;
#59205 = DIRECTION('center_axis',(0.,-1.,-5.60383084497428E-34)) ;
#59206 = DIRECTION('ref_axis',(0.707106781186548,3.96250679110365E-34,-0.707106781186548)) ;
#59207 = DIRECTION('',(0.,-1.,-5.60383084497428E-34)) ;
#59208 = DIRECTION('center_axis',(0.,0.,1.)) ;
#59209 = DIRECTION('ref_axis',(-0.707106781186359,-0.707106781186736,0.)) ;
#59210 = DIRECTION('',(0.,0.,1.)) ;
#59211 = DIRECTION('center_axis',(0.,1.,5.60383084497428E-34)) ;
#59212 = DIRECTION('ref_axis',(0.707106781186548,-3.96250679110365E-34,0.707106781186548)) ;
#59213 = DIRECTION('',(0.,1.,5.60383084497428E-34)) ;
#59214 = DIRECTION('center_axis',(1.,0.,0.)) ;
#59215 = DIRECTION('ref_axis',(0.,1.,0.)) ;
#59216 = DIRECTION('',(0.,1.,5.60383084497428E-34)) ;
#59217 = DIRECTION('center_axis',(0.,1.,5.60383084497428E-34)) ;
#59218 = DIRECTION('ref_axis',(-0.707106781186548,3.96250679110365E-34,-0.707106781186548)) ;
#59219 = DIRECTION('center_axis',(-1.51760508056877E-16,-5.60383084497428E-34,
1.)) ;
#59220 = DIRECTION('ref_axis',(1.,0.,0.)) ;
#59221 = DIRECTION('center_axis',(-1.,0.,0.)) ;
#59222 = DIRECTION('ref_axis',(0.,1.,0.)) ;
#59223 = DIRECTION('center_axis',(0.,-1.,0.)) ;
#59224 = DIRECTION('ref_axis',(0.707106781186548,0.,-0.707106781186548)) ;
#59225 = DIRECTION('center_axis',(0.,0.,-1.)) ;
#59226 = DIRECTION('ref_axis',(0.,-1.,0.)) ;
#59227 = DIRECTION('center_axis',(1.51760508056877E-16,5.60383084497428E-34,
-1.)) ;
#59228 = DIRECTION('ref_axis',(-1.,0.,0.)) ;
#59229 = DIRECTION('center_axis',(-1.,0.,0.)) ;
#59230 = DIRECTION('ref_axis',(0.,1.,0.)) ;
#59231 = DIRECTION('center_axis',(0.,0.,1.)) ;
#59232 = DIRECTION('ref_axis',(0.,-1.,0.)) ;
#59233 = DIRECTION('center_axis',(0.,-1.,0.)) ;
#59234 = DIRECTION('ref_axis',(-0.707106781186548,0.,-0.707106781186548)) ;
#59235 = DIRECTION('center_axis',(0.,-1.,0.)) ;
#59236 = DIRECTION('ref_axis',(1.,0.,1.4923676700635E-16)) ;
#59237 = DIRECTION('',(1.,0.,1.51760508056877E-16)) ;
#59238 = DIRECTION('',(0.,0.,-1.)) ;
#59239 = DIRECTION('',(-1.,0.,-1.51760508056877E-16)) ;
#59240 = DIRECTION('',(0.,0.,1.)) ;
#59241 = DIRECTION('center_axis',(0.,0.,-1.)) ;
#59242 = DIRECTION('ref_axis',(-1.,0.,0.)) ;
#59243 = DIRECTION('center_axis',(1.,0.,0.)) ;
#59244 = DIRECTION('ref_axis',(0.,0.,1.)) ;
#59245 = DIRECTION('center_axis',(0.,-1.,0.)) ;
#59246 = DIRECTION('ref_axis',(1.,0.,0.)) ;
#59247 = DIRECTION('center_axis',(0.,0.,1.)) ;
#59248 = DIRECTION('ref_axis',(1.,0.,0.)) ;
#59249 = DIRECTION('center_axis',(-1.,0.,0.)) ;
#59250 = DIRECTION('ref_axis',(0.,-1.,0.)) ;
#59251 = DIRECTION('center_axis',(0.,-1.,0.)) ;
#59252 = DIRECTION('ref_axis',(0.,0.,1.)) ;
#59253 = DIRECTION('center_axis',(1.,0.,1.51760508056877E-16)) ;
#59254 = DIRECTION('ref_axis',(-1.07310884363343E-16,-0.707106781186485,0.70710678118661)) ;
#59255 = DIRECTION('center_axis',(-0.816496580927844,-0.40824829046378,0.408248290463709)) ;
#59256 = DIRECTION('ref_axis',(0.577350269189507,-0.577350269189934,0.577350269189436)) ;
#59257 = DIRECTION('center_axis',(-3.55271367880058E-13,-1.,0.)) ;
#59258 = DIRECTION('ref_axis',(0.,0.,1.)) ;
#59259 = DIRECTION('center_axis',(1.,0.,0.)) ;
#59260 = DIRECTION('ref_axis',(0.,-1.,0.)) ;
#59261 = DIRECTION('center_axis',(-0.816496580927762,0.408248290463881,-0.408248290463774)) ;
#59262 = DIRECTION('ref_axis',(-0.577350269189602,-0.577350269189744,0.577350269189531)) ;
#59263 = DIRECTION('center_axis',(-1.,-8.88178419699986E-14,0.)) ;
#59264 = DIRECTION('ref_axis',(0.,0.,1.)) ;
#59265 = DIRECTION('center_axis',(0.,-1.,0.)) ;
#59266 = DIRECTION('ref_axis',(-1.,0.,0.)) ;
#59267 = DIRECTION('center_axis',(0.,-1.,-5.60383084497428E-34)) ;
#59268 = DIRECTION('ref_axis',(-0.707106781186548,-3.96250679110365E-34,0.707106781186548)) ;
#59269 = DIRECTION('center_axis',(0.,0.,1.)) ;
#59270 = DIRECTION('ref_axis',(1.,0.,0.)) ;
#59271 = DIRECTION('center_axis',(0.,-1.,0.)) ;
#59272 = DIRECTION('ref_axis',(1.,0.,0.)) ;
#59273 = DIRECTION('center_axis',(0.,0.,-1.)) ;
#59274 = DIRECTION('ref_axis',(0.,1.,0.)) ;
#59275 = DIRECTION('center_axis',(1.,0.,0.)) ;
#59276 = DIRECTION('ref_axis',(0.,0.,1.)) ;
#59277 = DIRECTION('center_axis',(0.,0.,1.)) ;
#59278 = DIRECTION('ref_axis',(1.,0.,0.)) ;
#59279 = DIRECTION('center_axis',(-1.,0.,0.)) ;
#59280 = DIRECTION('ref_axis',(0.,-1.,0.)) ;
#59281 = DIRECTION('center_axis',(0.,0.,-1.)) ;
#59282 = DIRECTION('ref_axis',(1.,0.,0.)) ;
#59283 = DIRECTION('center_axis',(0.,-1.,0.)) ;
#59284 = DIRECTION('ref_axis',(0.,0.,1.)) ;
#59285 = DIRECTION('center_axis',(1.,0.,1.51760508056877E-16)) ;
#59286 = DIRECTION('ref_axis',(-1.07310884363343E-16,-0.707106781186485,0.70710678118661)) ;
#59287 = DIRECTION('center_axis',(0.,0.,1.)) ;
#59288 = DIRECTION('ref_axis',(0.707106781186359,0.707106781186736,0.)) ;
#59289 = DIRECTION('',(0.,0.,1.)) ;
#59290 = DIRECTION('center_axis',(0.,0.,1.)) ;
#59291 = DIRECTION('ref_axis',(1.,0.,0.)) ;
#59292 = DIRECTION('center_axis',(1.,0.,0.)) ;
#59293 = DIRECTION('ref_axis',(0.,1.,0.)) ;
#59294 = DIRECTION('center_axis',(0.,0.,-1.)) ;
#59295 = DIRECTION('ref_axis',(-1.,0.,0.)) ;
#59296 = DIRECTION('center_axis',(0.,1.,0.)) ;
#59297 = DIRECTION('ref_axis',(0.,0.,1.)) ;
#59298 = DIRECTION('center_axis',(0.,0.,1.)) ;
#59299 = DIRECTION('ref_axis',(1.,0.,0.)) ;
#59300 = DIRECTION('center_axis',(0.,1.,0.)) ;
#59301 = DIRECTION('ref_axis',(-1.,0.,0.)) ;
#59302 = DIRECTION('center_axis',(-4.44089209850072E-14,0.,-1.)) ;
#59303 = DIRECTION('ref_axis',(0.,-1.,0.)) ;
#59304 = DIRECTION('center_axis',(-1.,0.,0.)) ;
#59305 = DIRECTION('ref_axis',(0.,0.,1.)) ;
#59306 = DIRECTION('center_axis',(0.,-1.,-5.60383084497428E-34)) ;
#59307 = DIRECTION('ref_axis',(-0.707106781186548,-3.96250679110365E-34,0.707106781186548)) ;
#59308 = DIRECTION('',(0.,-1.,-5.60383084497428E-34)) ;
#59309 = DIRECTION('center_axis',(0.,0.,1.)) ;
#59310 = DIRECTION('ref_axis',(0.70710678118661,-0.707106781186485,0.)) ;
#59311 = DIRECTION('',(0.,0.,-1.)) ;
#59312 = DIRECTION('center_axis',(-1.,0.,-1.51760508056877E-16)) ;
#59313 = DIRECTION('ref_axis',(-1.07310884363343E-16,0.707106781186485,0.70710678118661)) ;
#59314 = DIRECTION('center_axis',(0.,0.,1.)) ;
#59315 = DIRECTION('ref_axis',(-0.707106781186359,-0.707106781186736,0.)) ;
#59316 = DIRECTION('',(0.,0.,1.)) ;
#59317 = DIRECTION('center_axis',(0.,1.,5.60383084497428E-34)) ;
#59318 = DIRECTION('ref_axis',(0.707106781186548,-3.96250679110365E-34,0.707106781186548)) ;
#59319 = DIRECTION('',(0.,1.,5.60383084497428E-34)) ;
#59320 = DIRECTION('center_axis',(0.,0.,1.)) ;
#59321 = DIRECTION('ref_axis',(-0.707106781186673,0.707106781186422,0.)) ;
#59322 = DIRECTION('',(0.,0.,-1.)) ;
#59323 = DIRECTION('center_axis',(1.,0.,1.51760508056877E-16)) ;
#59324 = DIRECTION('ref_axis',(-1.07310884363343E-16,-0.707106781186485,0.70710678118661)) ;
#59325 = DIRECTION('center_axis',(0.,1.,5.60383084497428E-34)) ;
#59326 = DIRECTION('ref_axis',(0.707106781186548,-3.96250679110365E-34,0.707106781186548)) ;
#59327 = DIRECTION('center_axis',(1.,0.,1.51760508056877E-16)) ;
#59328 = DIRECTION('ref_axis',(1.07310884363343E-16,0.707106781186485,-0.70710678118661)) ;
#59329 = DIRECTION('center_axis',(1.,0.,0.)) ;
#59330 = DIRECTION('ref_axis',(0.,1.,0.)) ;
#59331 = DIRECTION('',(0.,1.,5.60383084497428E-34)) ;
#59332 = DIRECTION('center_axis',(0.,1.,5.60383084497428E-34)) ;
#59333 = DIRECTION('ref_axis',(-0.707106781186548,3.96250679110365E-34,-0.707106781186548)) ;
#59334 = DIRECTION('center_axis',(-1.51760508056877E-16,-5.60383084497428E-34,
1.)) ;
#59335 = DIRECTION('ref_axis',(1.,0.,0.)) ;
#59336 = DIRECTION('center_axis',(-1.,0.,0.)) ;
#59337 = DIRECTION('ref_axis',(0.,1.,0.)) ;
#59338 = DIRECTION('center_axis',(0.,-1.,0.)) ;
#59339 = DIRECTION('ref_axis',(0.707106781186548,0.,-0.707106781186548)) ;
#59340 = DIRECTION('center_axis',(0.,0.,-1.)) ;
#59341 = DIRECTION('ref_axis',(0.,-1.,0.)) ;
#59342 = DIRECTION('center_axis',(1.51760508056877E-16,5.60383084497428E-34,
-1.)) ;
#59343 = DIRECTION('ref_axis',(-1.,0.,0.)) ;
#59344 = DIRECTION('center_axis',(-1.,0.,0.)) ;
#59345 = DIRECTION('ref_axis',(0.,1.,0.)) ;
#59346 = DIRECTION('center_axis',(0.,0.,1.)) ;
#59347 = DIRECTION('ref_axis',(0.,-1.,0.)) ;
#59348 = DIRECTION('center_axis',(0.,-1.,0.)) ;
#59349 = DIRECTION('ref_axis',(-0.707106781186548,0.,-0.707106781186548)) ;
#59350 = DIRECTION('center_axis',(0.,-1.,0.)) ;
#59351 = DIRECTION('ref_axis',(1.,0.,1.4923676700635E-16)) ;
#59352 = DIRECTION('',(1.,0.,1.51760508056877E-16)) ;
#59353 = DIRECTION('',(0.,0.,-1.)) ;
#59354 = DIRECTION('',(-1.,0.,-1.51760508056877E-16)) ;
#59355 = DIRECTION('',(0.,0.,1.)) ;
#59356 = DIRECTION('center_axis',(0.,0.,1.)) ;
#59357 = DIRECTION('ref_axis',(1.,0.,0.)) ;
#59358 = DIRECTION('center_axis',(0.,-1.,0.)) ;
#59359 = DIRECTION('ref_axis',(1.,0.,0.)) ;
#59360 = DIRECTION('center_axis',(1.,0.,0.)) ;
#59361 = DIRECTION('ref_axis',(0.,0.,1.)) ;
#59362 = DIRECTION('center_axis',(-0.816496580927809,-0.408248290463869,0.408248290463691)) ;
#59363 = DIRECTION('ref_axis',(0.577350269189507,-0.577350269189792,0.577350269189578)) ;
#59364 = DIRECTION('center_axis',(-3.55271367880058E-13,-1.,0.)) ;
#59365 = DIRECTION('ref_axis',(0.,0.,1.)) ;
#59366 = DIRECTION('center_axis',(1.,0.,0.)) ;
#59367 = DIRECTION('ref_axis',(0.,-1.,0.)) ;
#59368 = DIRECTION('center_axis',(0.,1.,5.60383084497428E-34)) ;
#59369 = DIRECTION('ref_axis',(0.707106781186548,-3.96250679110365E-34,0.707106781186548)) ;
#59370 = DIRECTION('center_axis',(0.,0.,1.)) ;
#59371 = DIRECTION('ref_axis',(1.,0.,0.)) ;
#59372 = DIRECTION('center_axis',(-1.,0.,0.)) ;
#59373 = DIRECTION('ref_axis',(0.,-1.,0.)) ;
#59374 = DIRECTION('center_axis',(0.,-1.,0.)) ;
#59375 = DIRECTION('ref_axis',(0.,0.,1.)) ;
#59376 = DIRECTION('center_axis',(1.,0.,1.51760508056877E-16)) ;
#59377 = DIRECTION('ref_axis',(-1.07310884363343E-16,-0.707106781186485,0.70710678118661)) ;
#59378 = DIRECTION('center_axis',(0.,0.,1.)) ;
#59379 = DIRECTION('ref_axis',(1.,0.,0.)) ;
#59380 = DIRECTION('center_axis',(0.,-1.,0.)) ;
#59381 = DIRECTION('ref_axis',(1.,0.,0.)) ;
#59382 = DIRECTION('center_axis',(0.,0.,-1.)) ;
#59383 = DIRECTION('ref_axis',(0.,1.,0.)) ;
#59384 = DIRECTION('center_axis',(1.,0.,0.)) ;
#59385 = DIRECTION('ref_axis',(0.,0.,1.)) ;
#59386 = DIRECTION('center_axis',(-0.81649658092775,0.408248290463875,-0.408248290463804)) ;
#59387 = DIRECTION('ref_axis',(-0.577350269189555,-0.577350269189768,0.577350269189555)) ;
#59388 = DIRECTION('center_axis',(-1.,0.,0.)) ;
#59389 = DIRECTION('ref_axis',(0.,0.,1.)) ;
#59390 = DIRECTION('center_axis',(0.,-1.,0.)) ;
#59391 = DIRECTION('ref_axis',(-1.,0.,0.)) ;
#59392 = DIRECTION('center_axis',(0.,-1.,-5.60383084497428E-34)) ;
#59393 = DIRECTION('ref_axis',(-0.707106781186548,-3.96250679110365E-34,0.707106781186548)) ;
#59394 = DIRECTION('center_axis',(0.,0.,1.)) ;
#59395 = DIRECTION('ref_axis',(1.,0.,0.)) ;
#59396 = DIRECTION('center_axis',(1.,0.,0.)) ;
#59397 = DIRECTION('ref_axis',(0.,1.,0.)) ;
#59398 = DIRECTION('center_axis',(0.,0.,-1.)) ;
#59399 = DIRECTION('ref_axis',(-1.,0.,0.)) ;
#59400 = DIRECTION('center_axis',(0.,1.,0.)) ;
#59401 = DIRECTION('ref_axis',(0.,0.,1.)) ;
#59402 = DIRECTION('center_axis',(0.,0.,1.)) ;
#59403 = DIRECTION('ref_axis',(1.,0.,0.)) ;
#59404 = DIRECTION('center_axis',(-1.,0.,0.)) ;
#59405 = DIRECTION('ref_axis',(0.,-1.,0.)) ;
#59406 = DIRECTION('center_axis',(0.,0.,-1.)) ;
#59407 = DIRECTION('ref_axis',(1.,0.,0.)) ;
#59408 = DIRECTION('center_axis',(0.,-1.,0.)) ;
#59409 = DIRECTION('ref_axis',(0.,0.,1.)) ;
#59410 = DIRECTION('center_axis',(1.,0.,1.51760508056877E-16)) ;
#59411 = DIRECTION('ref_axis',(-1.07310884363343E-16,-0.707106781186485,0.70710678118661)) ;
#59412 = DIRECTION('center_axis',(0.,0.,1.)) ;
#59413 = DIRECTION('ref_axis',(0.707106781186359,0.707106781186736,0.)) ;
#59414 = DIRECTION('',(0.,0.,1.)) ;
#59415 = DIRECTION('center_axis',(0.,0.,1.)) ;
#59416 = DIRECTION('ref_axis',(1.,0.,0.)) ;
#59417 = DIRECTION('center_axis',(0.,1.,0.)) ;
#59418 = DIRECTION('ref_axis',(-1.,0.,0.)) ;
#59419 = DIRECTION('center_axis',(0.,0.,-1.)) ;
#59420 = DIRECTION('ref_axis',(0.,-1.,0.)) ;
#59421 = DIRECTION('center_axis',(-1.,0.,0.)) ;
#59422 = DIRECTION('ref_axis',(0.,0.,1.)) ;
#59423 = DIRECTION('center_axis',(0.,-1.,-5.60383084497428E-34)) ;
#59424 = DIRECTION('ref_axis',(-0.707106781186548,-3.96250679110365E-34,0.707106781186548)) ;
#59425 = DIRECTION('',(0.,-1.,-5.60383084497428E-34)) ;
#59426 = DIRECTION('center_axis',(0.,0.,1.)) ;
#59427 = DIRECTION('ref_axis',(0.707106781186548,-0.707106781186548,0.)) ;
#59428 = DIRECTION('',(0.,0.,-1.)) ;
#59429 = DIRECTION('center_axis',(-1.,0.,-1.51760508056877E-16)) ;
#59430 = DIRECTION('ref_axis',(-1.07310884363343E-16,0.707106781186485,0.70710678118661)) ;
#59431 = DIRECTION('center_axis',(0.,0.,1.)) ;
#59432 = DIRECTION('ref_axis',(-0.707106781186359,-0.707106781186736,0.)) ;
#59433 = DIRECTION('',(0.,0.,1.)) ;
#59434 = DIRECTION('center_axis',(0.,1.,5.60383084497428E-34)) ;
#59435 = DIRECTION('ref_axis',(0.707106781186548,-3.96250679110365E-34,0.707106781186548)) ;
#59436 = DIRECTION('',(0.,1.,5.60383084497428E-34)) ;
#59437 = DIRECTION('center_axis',(0.,0.,1.)) ;
#59438 = DIRECTION('ref_axis',(-0.70710678118661,0.707106781186485,0.)) ;
#59439 = DIRECTION('',(0.,0.,-1.)) ;
#59440 = DIRECTION('center_axis',(1.,0.,1.51760508056877E-16)) ;
#59441 = DIRECTION('ref_axis',(-1.07310884363343E-16,-0.707106781186485,0.70710678118661)) ;
#59442 = DIRECTION('center_axis',(1.,0.,1.51760508056877E-16)) ;
#59443 = DIRECTION('ref_axis',(1.07310884363343E-16,0.707106781186485,-0.70710678118661)) ;
#59444 = DIRECTION('center_axis',(1.,0.,0.)) ;
#59445 = DIRECTION('ref_axis',(0.,1.,0.)) ;
#59446 = DIRECTION('',(0.,1.,5.60383084497428E-34)) ;
#59447 = DIRECTION('center_axis',(0.,1.,5.60383084497428E-34)) ;
#59448 = DIRECTION('ref_axis',(-0.707106781186548,3.96250679110365E-34,-0.707106781186548)) ;
#59449 = DIRECTION('center_axis',(0.,0.,1.)) ;
#59450 = DIRECTION('ref_axis',(1.,0.,0.)) ;
#59451 = DIRECTION('center_axis',(-1.,0.,0.)) ;
#59452 = DIRECTION('ref_axis',(0.,-1.,0.)) ;
#59453 = DIRECTION('center_axis',(0.,0.,-1.)) ;
#59454 = DIRECTION('ref_axis',(1.,0.,0.)) ;
#59455 = DIRECTION('center_axis',(0.,-1.,0.)) ;
#59456 = DIRECTION('ref_axis',(0.,0.,1.)) ;
#59457 = DIRECTION('center_axis',(0.,0.,1.)) ;
#59458 = DIRECTION('ref_axis',(1.,0.,0.)) ;
#59459 = DIRECTION('center_axis',(0.,-1.,0.)) ;
#59460 = DIRECTION('ref_axis',(1.,0.,0.)) ;
#59461 = DIRECTION('center_axis',(-4.44089209850092E-14,0.,-1.)) ;
#59462 = DIRECTION('ref_axis',(0.,1.,0.)) ;
#59463 = DIRECTION('center_axis',(1.,0.,0.)) ;
#59464 = DIRECTION('ref_axis',(0.,0.,1.)) ;
#59465 = DIRECTION('center_axis',(0.,0.,1.)) ;
#59466 = DIRECTION('ref_axis',(-0.707106781186359,0.707106781186736,0.)) ;
#59467 = DIRECTION('center_axis',(0.,0.,1.)) ;
#59468 = DIRECTION('ref_axis',(0.,1.,0.)) ;
#59469 = DIRECTION('center_axis',(0.,0.,-1.)) ;
#59470 = DIRECTION('ref_axis',(-1.,0.,0.)) ;
#59471 = DIRECTION('center_axis',(1.,2.22044604925031E-16,0.)) ;
#59472 = DIRECTION('ref_axis',(0.,0.,-1.)) ;
#59473 = DIRECTION('center_axis',(0.,1.,0.)) ;
#59474 = DIRECTION('ref_axis',(-1.,0.,0.)) ;
#59475 = DIRECTION('center_axis',(-1.,-2.22044604925031E-16,0.)) ;
#59476 = DIRECTION('ref_axis',(-1.57009245868375E-16,0.707106781186538,0.707106781186557)) ;
#59477 = DIRECTION('center_axis',(2.22044604925031E-16,-1.,3.31372189702139E-32)) ;
#59478 = DIRECTION('ref_axis',(-0.707106781186548,-1.57009245868377E-16,0.707106781186548)) ;
#59479 = DIRECTION('center_axis',(0.,1.,0.)) ;
#59480 = DIRECTION('ref_axis',(-1.,0.,0.)) ;
#59481 = DIRECTION('center_axis',(1.51760508056877E-16,5.60383084497428E-34,
-1.)) ;
#59482 = DIRECTION('ref_axis',(-1.,0.,0.)) ;
#59483 = DIRECTION('center_axis',(-1.,0.,0.)) ;
#59484 = DIRECTION('ref_axis',(0.,-1.,0.)) ;
#59485 = DIRECTION('center_axis',(-1.51760508056877E-16,-5.60383084497428E-34,
1.)) ;
#59486 = DIRECTION('ref_axis',(-0.70710678118657,-0.707106781186525,-1.07310884363337E-16)) ;
#59487 = DIRECTION('center_axis',(1.,0.,1.51760508056877E-16)) ;
#59488 = DIRECTION('ref_axis',(-1.07310884363343E-16,-0.707106781186485,0.70710678118661)) ;
#59489 = DIRECTION('center_axis',(-1.,0.,0.)) ;
#59490 = DIRECTION('ref_axis',(0.,-1.,0.)) ;
#59491 = DIRECTION('',(1.,0.,1.51760508056877E-16)) ;
#59492 = DIRECTION('center_axis',(1.51760508056877E-16,5.60383084497428E-34,
-1.)) ;
#59493 = DIRECTION('ref_axis',(-1.,0.,0.)) ;
#59494 = DIRECTION('center_axis',(0.,-1.,0.)) ;
#59495 = DIRECTION('ref_axis',(1.,0.,0.)) ;
#59496 = DIRECTION('center_axis',(-1.51760508056877E-16,-5.60383084497428E-34,
1.)) ;
#59497 = DIRECTION('ref_axis',(0.707106781186574,-0.707106781186522,1.07310884363337E-16)) ;
#59498 = DIRECTION('center_axis',(-2.33146835171284E-14,1.,-3.53768783266021E-30)) ;
#59499 = DIRECTION('ref_axis',(0.707106781186579,1.64859708161805E-14,0.707106781186516)) ;
#59500 = DIRECTION('',(-2.33146835171284E-14,1.,-3.53768783266021E-30)) ;
#59501 = DIRECTION('center_axis',(0.,-1.,0.)) ;
#59502 = DIRECTION('ref_axis',(0.,0.,-1.)) ;
#59503 = DIRECTION('center_axis',(0.,-1.,0.)) ;
#59504 = DIRECTION('ref_axis',(0.,0.,-1.)) ;
#59505 = DIRECTION('center_axis',(0.,0.,-1.)) ;
#59506 = DIRECTION('ref_axis',(0.,1.,0.)) ;
#59507 = DIRECTION('center_axis',(0.,0.,1.)) ;
#59508 = DIRECTION('ref_axis',(0.70710678118661,0.707106781186485,0.)) ;
#59509 = DIRECTION('center_axis',(0.,0.,-1.)) ;
#59510 = DIRECTION('ref_axis',(0.,1.,0.)) ;
#59511 = DIRECTION('center_axis',(-1.,0.,0.)) ;
#59512 = DIRECTION('ref_axis',(0.,0.,1.)) ;
#59513 = DIRECTION('center_axis',(0.,1.,0.)) ;
#59514 = DIRECTION('ref_axis',(0.,0.,1.)) ;
#59515 = DIRECTION('center_axis',(1.,0.,0.)) ;
#59516 = DIRECTION('ref_axis',(0.,0.707106781186538,0.707106781186557)) ;
#59517 = DIRECTION('center_axis',(0.,1.,5.60383084497428E-34)) ;
#59518 = DIRECTION('ref_axis',(0.707106781186516,-3.96250679110383E-34,0.707106781186579)) ;
#59519 = DIRECTION('center_axis',(0.,1.,0.)) ;
#59520 = DIRECTION('ref_axis',(0.,0.,1.)) ;
#59521 = DIRECTION('center_axis',(-1.51760508056877E-16,-5.60383084497428E-34,
1.)) ;
#59522 = DIRECTION('ref_axis',(1.,0.,0.)) ;
#59523 = DIRECTION('center_axis',(-0.707106781186548,0.707106781186548,0.)) ;
#59524 = DIRECTION('ref_axis',(0.,0.,1.)) ;
#59525 = DIRECTION('center_axis',(1.51760508056877E-16,5.60383084497428E-34,
-1.)) ;
#59526 = DIRECTION('ref_axis',(-0.923879532511263,-0.382683432365147,-1.40208427237259E-16)) ;
#59527 = DIRECTION('center_axis',(-0.707106781186615,0.70710678118648,-1.07310884363344E-16)) ;
#59528 = DIRECTION('ref_axis',(0.499999999999866,0.499999999999961,0.70710678118667)) ;
#59529 = DIRECTION('center_axis',(-0.707106781186548,0.707106781186548,0.)) ;
#59530 = DIRECTION('ref_axis',(0.,0.,1.)) ;
#59531 = DIRECTION('',(-0.707106781186615,0.70710678118648,-1.07310884363344E-16)) ;
#59532 = DIRECTION('center_axis',(1.51760508056877E-16,5.60383084497428E-34,
-1.)) ;
#59533 = DIRECTION('ref_axis',(-1.,0.,0.)) ;
#59534 = DIRECTION('center_axis',(0.,1.,0.)) ;
#59535 = DIRECTION('ref_axis',(0.,0.,1.)) ;
#59536 = DIRECTION('center_axis',(-1.51760508056877E-16,-5.60383084497428E-34,
1.)) ;
#59537 = DIRECTION('ref_axis',(0.923879532511263,0.382683432365147,1.40208427237259E-16)) ;
#59538 = DIRECTION('center_axis',(-6.83214169000096E-16,1.,-1.03124546314615E-31)) ;
#59539 = DIRECTION('ref_axis',(0.707106781186453,4.83105371902635E-16,0.707106781186642)) ;
#59540 = DIRECTION('center_axis',(0.,1.,0.)) ;
#59541 = DIRECTION('ref_axis',(0.,0.,1.)) ;
#59542 = DIRECTION('',(-6.83214169000096E-16,1.,-1.03124546314615E-31)) ;
#59543 = DIRECTION('center_axis',(1.51760508056877E-16,5.60383084497428E-34,
-1.)) ;
#59544 = DIRECTION('ref_axis',(-1.,0.,0.)) ;
#59545 = DIRECTION('center_axis',(0.999479573214818,0.0322580645161017,0.)) ;
#59546 = DIRECTION('ref_axis',(0.,0.,1.)) ;
#59547 = DIRECTION('center_axis',(-1.51760508056877E-16,-5.60383084497428E-34,
1.)) ;
#59548 = DIRECTION('ref_axis',(0.718421208107084,-0.695608343640269,1.09027967541166E-16)) ;
#59549 = DIRECTION('center_axis',(1.51760508056877E-16,5.60383084497428E-34,
-1.)) ;
#59550 = DIRECTION('ref_axis',(-1.,0.,0.)) ;
#59551 = DIRECTION('center_axis',(0.,1.,0.)) ;
#59552 = DIRECTION('ref_axis',(0.,0.,1.)) ;
#59553 = DIRECTION('center_axis',(1.51760508056877E-16,5.60383084497428E-34,
-1.)) ;
#59554 = DIRECTION('ref_axis',(-0.718421208107087,0.695608343640265,-1.09027967541167E-16)) ;
#59555 = DIRECTION('center_axis',(0.,1.,5.60383084497428E-34)) ;
#59556 = DIRECTION('ref_axis',(0.707106781186548,-3.96250679110365E-34,0.707106781186548)) ;
#59557 = DIRECTION('center_axis',(0.,1.,0.)) ;
#59558 = DIRECTION('ref_axis',(0.,0.,1.)) ;
#59559 = DIRECTION('',(0.,1.,5.60383084497428E-34)) ;
#59560 = DIRECTION('center_axis',(1.51760508056877E-16,5.60383084497428E-34,
-1.)) ;
#59561 = DIRECTION('ref_axis',(-1.,0.,0.)) ;
#59562 = DIRECTION('center_axis',(-0.999479573214819,0.0322580645160902,0.)) ;
#59563 = DIRECTION('ref_axis',(0.,0.,1.)) ;
#59564 = DIRECTION('center_axis',(1.51760508056877E-16,5.60383084497428E-34,
-1.)) ;
#59565 = DIRECTION('ref_axis',(-0.718421208107092,-0.69560834364026,-1.09027967541168E-16)) ;
#59566 = DIRECTION('center_axis',(1.51760508056877E-16,5.60383084497428E-34,
-1.)) ;
#59567 = DIRECTION('ref_axis',(-1.,0.,0.)) ;
#59568 = DIRECTION('center_axis',(0.,1.,0.)) ;
#59569 = DIRECTION('ref_axis',(0.,0.,1.)) ;
#59570 = DIRECTION('center_axis',(-1.51760508056877E-16,-5.60383084497428E-34,
1.)) ;
#59571 = DIRECTION('ref_axis',(0.718421208107098,0.695608343640254,1.09027967541169E-16)) ;
#59572 = DIRECTION('center_axis',(-6.83214169000096E-16,1.,-1.03124546314615E-31)) ;
#59573 = DIRECTION('ref_axis',(0.707106781186579,4.83105371902721E-16,0.707106781186516)) ;
#59574 = DIRECTION('center_axis',(0.,1.,0.)) ;
#59575 = DIRECTION('ref_axis',(0.,0.,1.)) ;
#59576 = DIRECTION('',(-6.83214169000096E-16,1.,-1.03124546314615E-31)) ;
#59577 = DIRECTION('center_axis',(1.51760508056877E-16,5.60383084497428E-34,
-1.)) ;
#59578 = DIRECTION('ref_axis',(-1.,0.,0.)) ;
#59579 = DIRECTION('center_axis',(0.707106781186548,0.707106781186548,0.)) ;
#59580 = DIRECTION('ref_axis',(0.,0.,1.)) ;
#59581 = DIRECTION('center_axis',(-1.51760508056877E-16,-5.60383084497428E-34,
1.)) ;
#59582 = DIRECTION('ref_axis',(0.923879532511288,-0.382683432365087,1.40208427237263E-16)) ;
#59583 = DIRECTION('center_axis',(0.707106781186521,0.707106781186574,1.0731088436333E-16)) ;
#59584 = DIRECTION('ref_axis',(0.499999999999964,-0.499999999999927,0.707106781186625)) ;
#59585 = DIRECTION('center_axis',(0.707106781186548,0.707106781186548,0.)) ;
#59586 = DIRECTION('ref_axis',(0.,0.,1.)) ;
#59587 = DIRECTION('',(0.707106781186521,0.707106781186574,1.0731088436333E-16)) ;
#59588 = DIRECTION('center_axis',(-1.51760508056877E-16,-5.60383084497428E-34,
1.)) ;
#59589 = DIRECTION('ref_axis',(1.,0.,0.)) ;
#59590 = DIRECTION('center_axis',(0.,1.,0.)) ;
#59591 = DIRECTION('ref_axis',(0.,0.,1.)) ;
#59592 = DIRECTION('center_axis',(1.51760508056877E-16,5.60383084497428E-34,
-1.)) ;
#59593 = DIRECTION('ref_axis',(-0.923879532511313,0.382683432365025,-1.40208427237267E-16)) ;
#59594 = DIRECTION('center_axis',(-5.23472275150178E-15,1.,-7.93863801220309E-31)) ;
#59595 = DIRECTION('ref_axis',(0.707106781186516,3.70150795521825E-15,0.707106781186579)) ;
#59596 = DIRECTION('center_axis',(0.,1.,0.)) ;
#59597 = DIRECTION('ref_axis',(0.,0.,1.)) ;
#59598 = DIRECTION('',(-5.23472275150178E-15,1.,-7.93863801220309E-31)) ;
#59599 = DIRECTION('center_axis',(-1.51760508056877E-16,-5.60383084497428E-34,
1.)) ;
#59600 = DIRECTION('ref_axis',(1.,0.,0.)) ;
#59601 = DIRECTION('center_axis',(0.984807753012208,-0.173648177666931,0.)) ;
#59602 = DIRECTION('ref_axis',(0.,0.,1.)) ;
#59603 = DIRECTION('center_axis',(-1.51760508056877E-16,-5.60383084497428E-34,
1.)) ;
#59604 = DIRECTION('ref_axis',(0.642787609686539,-0.766044443118978,9.75497742186947E-17)) ;
#59605 = DIRECTION('center_axis',(0.984807753012209,-0.173648177666924,1.49454924935485E-16)) ;
#59606 = DIRECTION('ref_axis',(-0.122787803968973,-0.696364240320047,0.70710678118652)) ;
#59607 = DIRECTION('center_axis',(0.984807753012208,-0.173648177666931,0.)) ;
#59608 = DIRECTION('ref_axis',(0.,0.,1.)) ;
#59609 = DIRECTION('',(0.984807753012209,-0.173648177666924,1.49454924935485E-16)) ;
#59610 = DIRECTION('center_axis',(1.51760508056877E-16,5.60383084497428E-34,
-1.)) ;
#59611 = DIRECTION('ref_axis',(-1.,0.,0.)) ;
#59612 = DIRECTION('center_axis',(0.573576436350949,-0.81915204428906,0.)) ;
#59613 = DIRECTION('ref_axis',(0.,0.,1.)) ;
#59614 = DIRECTION('center_axis',(-1.51760508056877E-16,-5.60383084497428E-34,
1.)) ;
#59615 = DIRECTION('ref_axis',(-0.53729960834682,-0.843391445812888,-8.15408615414744E-17)) ;
#59616 = DIRECTION('center_axis',(0.573576436351042,-0.819152044288994,8.70462513900874E-17)) ;
#59617 = DIRECTION('ref_axis',(-0.579227965339658,-0.405579787672697,0.707106781186442)) ;
#59618 = DIRECTION('center_axis',(0.573576436351033,-0.819152044289001,0.)) ;
#59619 = DIRECTION('ref_axis',(0.,0.,1.)) ;
#59620 = DIRECTION('',(0.573576436351042,-0.819152044288994,8.70462513900874E-17)) ;
#59621 = DIRECTION('center_axis',(1.51760508056877E-16,5.60383084497428E-34,
-1.)) ;
#59622 = DIRECTION('ref_axis',(-1.,0.,0.)) ;
#59623 = DIRECTION('center_axis',(0.,-1.,0.)) ;
#59624 = DIRECTION('ref_axis',(0.,0.,1.)) ;
#59625 = DIRECTION('center_axis',(-1.51760508056877E-16,-5.60383084497428E-34,
1.)) ;
#59626 = DIRECTION('ref_axis',(-0.953716950748229,-0.300705799504266,-1.44736568988007E-16)) ;
#59627 = DIRECTION('center_axis',(-5.25359141716359E-35,-1.,-5.60383084497428E-34)) ;
#59628 = DIRECTION('ref_axis',(-0.707106781186548,-3.59102177943767E-34,0.707106781186548)) ;
#59629 = DIRECTION('center_axis',(0.,-1.,0.)) ;
#59630 = DIRECTION('ref_axis',(0.,0.,1.)) ;
#59631 = DIRECTION('',(-5.25359141716359E-35,-1.,-5.60383084497428E-34)) ;
#59632 = DIRECTION('center_axis',(-1.51760508056877E-16,-5.60383084497428E-34,
1.)) ;
#59633 = DIRECTION('ref_axis',(1.,0.,0.)) ;
#59634 = DIRECTION('center_axis',(1.,0.,0.)) ;
#59635 = DIRECTION('ref_axis',(0.,0.,1.)) ;
#59636 = DIRECTION('center_axis',(1.51760508056877E-16,5.60383084497428E-34,
-1.)) ;
#59637 = DIRECTION('ref_axis',(0.707106781186547,0.707106781186547,1.07310884363333E-16)) ;
#59638 = DIRECTION('center_axis',(1.,0.,1.51760508056877E-16)) ;
#59639 = DIRECTION('ref_axis',(-1.07310884363343E-16,-0.707106781186485,0.70710678118661)) ;
#59640 = DIRECTION('center_axis',(1.,0.,0.)) ;
#59641 = DIRECTION('ref_axis',(0.,0.,1.)) ;
#59642 = DIRECTION('',(1.,0.,1.51760508056877E-16)) ;
#59643 = DIRECTION('center_axis',(1.51760508056877E-16,5.60383084497428E-34,
-1.)) ;
#59644 = DIRECTION('ref_axis',(-1.,0.,0.)) ;
#59645 = DIRECTION('center_axis',(0.,-1.,0.)) ;
#59646 = DIRECTION('ref_axis',(0.,0.,1.)) ;
#59647 = DIRECTION('center_axis',(-1.51760508056877E-16,-5.60383084497428E-34,
1.)) ;
#59648 = DIRECTION('ref_axis',(-0.707106781186547,-0.707106781186547,-1.07310884363333E-16)) ;
#59649 = DIRECTION('center_axis',(-2.22044604925032E-15,-1.,-3.37536403631613E-31)) ;
#59650 = DIRECTION('ref_axis',(-0.707106781186548,1.57009245868378E-15,0.707106781186548)) ;
#59651 = DIRECTION('',(-2.22044604925032E-15,-1.,-3.37536403631613E-31)) ;
#59652 = DIRECTION('center_axis',(0.,-1.,0.)) ;
#59653 = DIRECTION('ref_axis',(0.,0.,-1.)) ;
#59654 = DIRECTION('center_axis',(0.,0.,1.)) ;
#59655 = DIRECTION('ref_axis',(0.,1.,0.)) ;
#59656 = DIRECTION('center_axis',(0.,1.,0.)) ;
#59657 = DIRECTION('ref_axis',(0.707106781186548,0.,-0.707106781186548)) ;
#59658 = DIRECTION('center_axis',(0.,-1.,0.)) ;
#59659 = DIRECTION('ref_axis',(0.707106781186548,0.,-0.707106781186548)) ;
#59660 = DIRECTION('center_axis',(-2.01858731750028E-16,0.,1.)) ;
#59661 = DIRECTION('ref_axis',(-0.707106781186579,0.707106781186516,-1.42735678062167E-16)) ;
#59662 = DIRECTION('',(2.01858731750028E-16,0.,-1.)) ;
#59663 = DIRECTION('',(-2.01858731750028E-16,0.,1.)) ;
#59664 = DIRECTION('center_axis',(1.,0.,1.51760508056877E-16)) ;
#59665 = DIRECTION('ref_axis',(-1.07310884363343E-16,-0.707106781186485,0.70710678118661)) ;
#59666 = DIRECTION('',(1.,0.,1.51760508056877E-16)) ;
#59667 = DIRECTION('center_axis',(-2.01858731750028E-16,0.,1.)) ;
#59668 = DIRECTION('ref_axis',(0.70710678118661,0.707106781186485,1.42735678062174E-16)) ;
#59669 = DIRECTION('center_axis',(0.,0.,-1.)) ;
#59670 = DIRECTION('ref_axis',(0.,1.,0.)) ;
#59671 = DIRECTION('',(-2.01858731750028E-16,0.,1.)) ;
#59672 = DIRECTION('',(2.01858731750028E-16,0.,-1.)) ;
#59673 = DIRECTION('center_axis',(0.,-1.,0.)) ;
#59674 = DIRECTION('ref_axis',(0.,0.,-1.)) ;
#59675 = DIRECTION('center_axis',(0.,1.,0.)) ;
#59676 = DIRECTION('ref_axis',(-0.707106781186548,0.,-0.707106781186548)) ;
#59677 = DIRECTION('center_axis',(0.,-1.,0.)) ;
#59678 = DIRECTION('ref_axis',(-0.707106781186548,0.,-0.707106781186548)) ;
#59679 = DIRECTION('center_axis',(-1.,0.,-1.51760508056877E-16)) ;
#59680 = DIRECTION('ref_axis',(-1.07310884363335E-16,0.70710678118654,0.707106781186555)) ;
#59681 = DIRECTION('center_axis',(-0.863778900898434,-0.503871025524085,0.)) ;
#59682 = DIRECTION('ref_axis',(-0.503871025524085,0.863778900898434,0.)) ;
#59683 = DIRECTION('center_axis',(-0.863778900898434,-0.503871025524085,0.)) ;
#59684 = DIRECTION('ref_axis',(-0.503871025524085,0.863778900898434,0.)) ;
#59685 = DIRECTION('center_axis',(0.70710678118648,0.707106781186615,0.)) ;
#59686 = DIRECTION('ref_axis',(-0.707106781186615,0.70710678118648,-1.05526329952557E-16)) ;
#59687 = DIRECTION('',(0.,0.,1.)) ;
#59688 = DIRECTION('',(0.707106781186615,-0.70710678118648,1.07310884363344E-16)) ;
#59689 = DIRECTION('',(0.,0.,-1.)) ;
#59690 = DIRECTION('center_axis',(0.,0.,1.)) ;
#59691 = DIRECTION('ref_axis',(0.923879532511284,0.382683432365097,0.)) ;
#59692 = DIRECTION('',(0.,0.,-1.)) ;
#59693 = DIRECTION('center_axis',(1.51760508056877E-16,5.60383084497428E-34,
-1.)) ;
#59694 = DIRECTION('ref_axis',(0.923879532511263,0.382683432365147,1.40208427237259E-16)) ;
#59695 = DIRECTION('center_axis',(1.,6.83214169000096E-16,0.)) ;
#59696 = DIRECTION('ref_axis',(-6.83214169000096E-16,1.,-1.01960673754504E-31)) ;
#59697 = DIRECTION('',(0.,0.,1.)) ;
#59698 = DIRECTION('',(6.83214169000096E-16,-1.,1.03124546314615E-31)) ;
#59699 = DIRECTION('center_axis',(0.,0.,-1.)) ;
#59700 = DIRECTION('ref_axis',(-1.,0.,0.)) ;
#59701 = DIRECTION('',(0.,0.,-1.)) ;
#59702 = DIRECTION('center_axis',(1.51760508056877E-16,5.60383084497428E-34,
-1.)) ;
#59703 = DIRECTION('ref_axis',(0.718421208107084,-0.695608343640269,1.09027967541166E-16)) ;
#59704 = DIRECTION('center_axis',(0.,0.,1.)) ;
#59705 = DIRECTION('ref_axis',(0.,1.,0.)) ;
#59706 = DIRECTION('',(0.,0.,1.)) ;
#59707 = DIRECTION('center_axis',(-1.51760508056877E-16,-5.60383084497428E-34,
1.)) ;
#59708 = DIRECTION('ref_axis',(-0.718421208107087,0.695608343640265,-1.09027967541167E-16)) ;
#59709 = DIRECTION('center_axis',(1.,0.,0.)) ;
#59710 = DIRECTION('ref_axis',(0.,1.,0.)) ;
#59711 = DIRECTION('',(0.,0.,1.)) ;
#59712 = DIRECTION('',(0.,-1.,-5.60383084497428E-34)) ;
#59713 = DIRECTION('center_axis',(0.,0.,1.)) ;
#59714 = DIRECTION('ref_axis',(-1.,0.,0.)) ;
#59715 = DIRECTION('',(0.,0.,1.)) ;
#59716 = DIRECTION('center_axis',(-1.51760508056877E-16,-5.60383084497428E-34,
1.)) ;
#59717 = DIRECTION('ref_axis',(-0.718421208107092,-0.69560834364026,-1.09027967541168E-16)) ;
#59718 = DIRECTION('center_axis',(0.,0.,1.)) ;
#59719 = DIRECTION('ref_axis',(-1.,0.,0.)) ;
#59720 = DIRECTION('',(0.,0.,-1.)) ;
#59721 = DIRECTION('center_axis',(1.51760508056877E-16,5.60383084497428E-34,
-1.)) ;
#59722 = DIRECTION('ref_axis',(0.718421208107098,0.695608343640254,1.09027967541169E-16)) ;
#59723 = DIRECTION('center_axis',(1.,6.83214169000096E-16,0.)) ;
#59724 = DIRECTION('ref_axis',(-6.83214169000096E-16,1.,-1.01960673754504E-31)) ;
#59725 = DIRECTION('',(0.,0.,1.)) ;
#59726 = DIRECTION('',(6.83214169000096E-16,-1.,1.03124546314615E-31)) ;
#59727 = DIRECTION('center_axis',(0.,0.,1.)) ;
#59728 = DIRECTION('ref_axis',(0.923879532511284,-0.382683432365097,0.)) ;
#59729 = DIRECTION('',(0.,0.,-1.)) ;
#59730 = DIRECTION('center_axis',(1.51760508056877E-16,5.60383084497428E-34,
-1.)) ;
#59731 = DIRECTION('ref_axis',(0.923879532511288,-0.382683432365087,1.40208427237263E-16)) ;
#59732 = DIRECTION('center_axis',(0.707106781186574,-0.707106781186521,0.)) ;
#59733 = DIRECTION('ref_axis',(0.707106781186521,0.707106781186574,1.05526329952543E-16)) ;
#59734 = DIRECTION('',(0.,0.,1.)) ;
#59735 = DIRECTION('',(-0.707106781186521,-0.707106781186574,-1.0731088436333E-16)) ;
#59736 = DIRECTION('center_axis',(0.,0.,1.)) ;
#59737 = DIRECTION('ref_axis',(-0.923879532511311,0.382683432365031,0.)) ;
#59738 = DIRECTION('',(0.,0.,-1.)) ;
#59739 = DIRECTION('center_axis',(-1.51760508056877E-16,-5.60383084497428E-34,
1.)) ;
#59740 = DIRECTION('ref_axis',(-0.923879532511292,0.382683432365076,-1.40208427237264E-16)) ;
#59741 = DIRECTION('center_axis',(1.,5.23472275150178E-15,0.)) ;
#59742 = DIRECTION('ref_axis',(-5.23472275150178E-15,1.,-7.81213099608712E-31)) ;
#59743 = DIRECTION('',(0.,0.,1.)) ;
#59744 = DIRECTION('',(5.23472275150178E-15,-1.,7.93863801220309E-31)) ;
#59745 = DIRECTION('center_axis',(0.,0.,1.)) ;
#59746 = DIRECTION('ref_axis',(-0.17364817766693,-0.984807753012208,0.)) ;
#59747 = DIRECTION('',(0.,0.,1.)) ;
#59748 = DIRECTION('center_axis',(1.51760508056877E-16,5.60383084497428E-34,
-1.)) ;
#59749 = DIRECTION('ref_axis',(0.642787609686539,-0.766044443118978,9.75497742186947E-17)) ;
#59750 = DIRECTION('center_axis',(-0.173648177666924,-0.984807753012209,0.)) ;
#59751 = DIRECTION('ref_axis',(0.984807753012209,-0.173648177666924,1.4696952518233E-16)) ;
#59752 = DIRECTION('',(0.,0.,1.)) ;
#59753 = DIRECTION('',(-0.984807753012209,0.173648177666924,-1.49454924935485E-16)) ;
#59754 = DIRECTION('center_axis',(0.,0.,1.)) ;
#59755 = DIRECTION('ref_axis',(-0.537299608346821,-0.843391445812888,0.)) ;
#59756 = DIRECTION('',(0.,0.,-1.)) ;
#59757 = DIRECTION('center_axis',(1.51760508056877E-16,5.60383084497428E-34,
-1.)) ;
#59758 = DIRECTION('ref_axis',(-0.537299608346822,-0.843391445812887,-8.15408615414747E-17)) ;
#59759 = DIRECTION('center_axis',(-0.819152044288994,-0.573576436351042,0.)) ;
#59760 = DIRECTION('ref_axis',(0.573576436351042,-0.819152044288994,8.61198118612814E-17)) ;
#59761 = DIRECTION('',(0.,0.,1.)) ;
#59762 = DIRECTION('',(-0.573576436351042,0.819152044288994,-8.70462513900874E-17)) ;
#59763 = DIRECTION('center_axis',(0.,0.,1.)) ;
#59764 = DIRECTION('ref_axis',(-0.953716950748228,-0.300705799504269,0.)) ;
#59765 = DIRECTION('',(0.,0.,-1.)) ;
#59766 = DIRECTION('center_axis',(1.51760508056877E-16,5.60383084497428E-34,
-1.)) ;
#59767 = DIRECTION('ref_axis',(-0.953716950748229,-0.300705799504266,-1.44736568988007E-16)) ;
#59768 = DIRECTION('center_axis',(-1.,5.25359141716359E-35,0.)) ;
#59769 = DIRECTION('ref_axis',(-5.25359141716359E-35,-1.,3.52030637124432E-19)) ;
#59770 = DIRECTION('',(0.,0.,1.)) ;
#59771 = DIRECTION('',(5.25359141716359E-35,1.,5.60383084497428E-34)) ;
#59772 = DIRECTION('center_axis',(0.,0.,1.)) ;
#59773 = DIRECTION('ref_axis',(0.707106781186537,0.707106781186558,0.)) ;
#59774 = DIRECTION('',(0.,0.,-1.)) ;
#59775 = DIRECTION('center_axis',(-1.51760508056877E-16,-5.60383084497428E-34,
1.)) ;
#59776 = DIRECTION('ref_axis',(0.707106781186547,0.707106781186547,1.07310884363333E-16)) ;
#59777 = DIRECTION('center_axis',(0.,-1.,0.)) ;
#59778 = DIRECTION('ref_axis',(1.,0.,2.24978329294248E-16)) ;
#59779 = DIRECTION('',(-2.01858731750028E-16,0.,1.)) ;
#59780 = DIRECTION('',(-1.,0.,-1.51760508056877E-16)) ;
#59781 = DIRECTION('center_axis',(2.01858731750028E-16,0.,-1.)) ;
#59782 = DIRECTION('ref_axis',(-0.707106781186537,-0.707106781186558,-1.42735678062159E-16)) ;
#59783 = DIRECTION('',(2.01858731750028E-16,0.,-1.)) ;
#59784 = DIRECTION('center_axis',(1.51760508056877E-16,5.60383084497428E-34,
-1.)) ;
#59785 = DIRECTION('ref_axis',(-0.707106781186547,-0.707106781186547,-1.07310884363333E-16)) ;
#59786 = DIRECTION('center_axis',(1.,-2.22044604925032E-15,2.01858731750028E-16)) ;
#59787 = DIRECTION('ref_axis',(2.22044604925032E-15,1.,1.18383464030937E-18)) ;
#59788 = DIRECTION('',(2.22044604925032E-15,1.,3.37536403631613E-31)) ;
#59789 = DIRECTION('center_axis',(2.22044604925032E-15,1.,3.37536403631613E-31)) ;
#59790 = DIRECTION('ref_axis',(-0.707106781186548,1.57009245868378E-15,-0.707106781186548)) ;
#59791 = DIRECTION('center_axis',(0.,-1.,0.)) ;
#59792 = DIRECTION('ref_axis',(-1.,0.,0.)) ;
#59793 = DIRECTION('center_axis',(0.,0.,1.)) ;
#59794 = DIRECTION('ref_axis',(-0.707106781186359,0.707106781186736,0.)) ;
#59795 = DIRECTION('center_axis',(-1.4923676700635E-16,0.,1.)) ;
#59796 = DIRECTION('ref_axis',(-0.707106781186359,0.707106781186736,-1.05526329952519E-16)) ;
#59797 = DIRECTION('',(0.,0.,1.)) ;
#59798 = DIRECTION('center_axis',(0.,0.,-1.)) ;
#59799 = DIRECTION('ref_axis',(-1.,0.,0.)) ;
#59800 = DIRECTION('',(0.,0.,-1.)) ;
#59801 = DIRECTION('center_axis',(0.,-1.,0.)) ;
#59802 = DIRECTION('ref_axis',(0.,0.,-1.)) ;
#59803 = DIRECTION('center_axis',(-1.,-9.23705556487986E-12,0.)) ;
#59804 = DIRECTION('ref_axis',(0.,0.,1.)) ;
#59805 = DIRECTION('center_axis',(0.,-1.,0.)) ;
#59806 = DIRECTION('ref_axis',(-0.707106781186881,0.,0.707106781186214)) ;
#59807 = DIRECTION('center_axis',(0.,1.,0.)) ;
#59808 = DIRECTION('ref_axis',(-0.707106781186881,0.,0.707106781186215)) ;
#59809 = DIRECTION('center_axis',(1.,0.,1.51760508056877E-16)) ;
#59810 = DIRECTION('ref_axis',(-1.07310884363305E-16,0.707106781186736,0.707106781186359)) ;
#59811 = DIRECTION('center_axis',(0.70710678118661,0.707106781186485,0.)) ;
#59812 = DIRECTION('ref_axis',(-0.707106781186485,0.70710678118661,-2.45326946669362E-16)) ;
#59813 = DIRECTION('center_axis',(3.17206578464329E-15,-1.,4.80833931982806E-31)) ;
#59814 = DIRECTION('ref_axis',(-0.707106781186551,-2.24298922669111E-15,0.707106781186544)) ;
#59815 = DIRECTION('',(3.17206578464329E-15,-1.,4.80833931982806E-31)) ;
#59816 = DIRECTION('center_axis',(-3.55271367880051E-14,-1.,0.)) ;
#59817 = DIRECTION('ref_axis',(-0.707106781186879,2.51214793389522E-14,0.707106781186216)) ;
#59818 = DIRECTION('center_axis',(-1.,-3.17206578464329E-15,0.)) ;
#59819 = DIRECTION('ref_axis',(3.17206578464329E-15,-1.,4.73388842431626E-31)) ;
#59820 = DIRECTION('',(-3.17206578464329E-15,1.,-4.73388842431626E-31)) ;
#59821 = DIRECTION('',(0.,0.,-1.)) ;
#59822 = DIRECTION('center_axis',(-1.4923676700635E-16,0.,1.)) ;
#59823 = DIRECTION('ref_axis',(1.,0.,1.4923676700635E-16)) ;
#59824 = DIRECTION('',(1.,0.,1.4923676700635E-16)) ;
#59825 = DIRECTION('',(-7.105427357601E-15,-1.,-1.06039100704685E-30)) ;
#59826 = DIRECTION('',(-1.,3.55271367880051E-14,-1.4923676700635E-16)) ;
#59827 = DIRECTION('center_axis',(-1.4923676700635E-16,0.,1.)) ;
#59828 = DIRECTION('ref_axis',(-0.70710678118661,-0.707106781186485,-1.05526329952556E-16)) ;
#59829 = DIRECTION('center_axis',(0.,0.,1.)) ;
#59830 = DIRECTION('ref_axis',(-0.70710678118661,-0.707106781186485,0.)) ;
#59831 = DIRECTION('',(0.,0.,1.)) ;
#59832 = DIRECTION('center_axis',(0.,0.,-1.)) ;
#59833 = DIRECTION('ref_axis',(0.,-1.,0.)) ;
#59834 = DIRECTION('center_axis',(3.55271367880051E-14,1.,0.)) ;
#59835 = DIRECTION('ref_axis',(0.,0.,1.)) ;
#59836 = DIRECTION('center_axis',(-1.,4.25984888819251E-25,9.5923269327607E-12)) ;
#59837 = DIRECTION('ref_axis',(-3.39809272400367E-40,-1.,4.44089209849993E-14)) ;
#59838 = DIRECTION('center_axis',(3.55271367880051E-14,1.,0.)) ;
#59839 = DIRECTION('ref_axis',(-0.707106781186879,2.51214793389522E-14,0.707106781186216)) ;
#59840 = DIRECTION('center_axis',(-1.,3.55271367880051E-14,-1.51760508056877E-16)) ;
#59841 = DIRECTION('ref_axis',(-2.52287902233105E-14,-0.707106781186736,0.707106781186359)) ;
#59842 = DIRECTION('center_axis',(0.70710678118661,-0.707106781186485,0.)) ;
#59843 = DIRECTION('ref_axis',(-0.707106781186485,-0.70710678118661,0.)) ;
#59844 = DIRECTION('center_axis',(-3.55271367880051E-14,-1.,0.)) ;
#59845 = DIRECTION('ref_axis',(1.,-3.55271367880051E-14,1.4923676700635E-16)) ;
#59846 = DIRECTION('',(0.,0.,1.)) ;
#59847 = DIRECTION('',(0.,0.,-1.)) ;
#59848 = DIRECTION('center_axis',(0.,0.,1.)) ;
#59849 = DIRECTION('ref_axis',(1.,0.,0.)) ;
#59850 = DIRECTION('center_axis',(-1.,0.,0.)) ;
#59851 = DIRECTION('ref_axis',(0.,-1.,0.)) ;
#59852 = DIRECTION('center_axis',(0.,4.44089209849835E-14,-1.)) ;
#59853 = DIRECTION('ref_axis',(1.,0.,0.)) ;
#59854 = DIRECTION('center_axis',(0.,-1.,0.)) ;
#59855 = DIRECTION('ref_axis',(0.,0.,1.)) ;
#59856 = DIRECTION('center_axis',(0.,0.,-1.)) ;
#59857 = DIRECTION('ref_axis',(-1.,0.,0.)) ;
#59858 = DIRECTION('center_axis',(0.,0.,-1.)) ;
#59859 = DIRECTION('ref_axis',(0.,1.,0.)) ;
#59860 = DIRECTION('center_axis',(1.,0.,0.)) ;
#59861 = DIRECTION('ref_axis',(0.,0.,1.)) ;
#59862 = DIRECTION('center_axis',(-0.707106781186592,-0.707106781186503,0.)) ;
#59863 = DIRECTION('ref_axis',(0.707106781186503,-0.707106781186592,0.)) ;
#59864 = DIRECTION('center_axis',(1.,0.,1.51760508056877E-16)) ;
#59865 = DIRECTION('ref_axis',(-1.07310884363343E-16,-0.707106781186485,0.70710678118661)) ;
#59866 = DIRECTION('',(1.,0.,1.51760508056877E-16)) ;
#59867 = DIRECTION('center_axis',(0.,0.,-1.)) ;
#59868 = DIRECTION('ref_axis',(-1.,0.,0.)) ;
#59869 = DIRECTION('center_axis',(4.44089209850072E-14,4.44089209850072E-14,
-1.)) ;
#59870 = DIRECTION('ref_axis',(-0.707106781186547,0.707106781186547,-2.2709071609452E-30)) ;
#59871 = DIRECTION('center_axis',(0.707106781186548,0.707106781186548,0.)) ;
#59872 = DIRECTION('ref_axis',(0.,0.,1.)) ;
#59873 = DIRECTION('center_axis',(0.,-1.,0.)) ;
#59874 = DIRECTION('ref_axis',(1.,0.,0.)) ;
#59875 = DIRECTION('center_axis',(-0.707106781186563,-0.707106781186532,-1.07310884363336E-16)) ;
#59876 = DIRECTION('ref_axis',(0.499999999999956,-0.499999999999978,0.707106781186594)) ;
#59877 = DIRECTION('',(0.707106781186563,0.707106781186532,1.07310884363336E-16)) ;
#59878 = DIRECTION('center_axis',(0.,0.,-1.)) ;
#59879 = DIRECTION('ref_axis',(-1.,0.,0.)) ;
#59880 = DIRECTION('center_axis',(0.,-6.28036983473606E-14,-1.)) ;
#59881 = DIRECTION('ref_axis',(-1.,0.,0.)) ;
#59882 = DIRECTION('center_axis',(0.,1.,0.)) ;
#59883 = DIRECTION('ref_axis',(0.,0.,1.)) ;
#59884 = DIRECTION('center_axis',(0.707106781186548,-0.707106781186548,0.)) ;
#59885 = DIRECTION('ref_axis',(0.707106781186547,0.707106781186547,0.)) ;
#59886 = DIRECTION('center_axis',(3.73034936274055E-14,1.,5.66175752827605E-30)) ;
#59887 = DIRECTION('ref_axis',(0.707106781186516,-2.63775533058864E-14,0.707106781186579)) ;
#59888 = DIRECTION('',(3.73034936274055E-14,1.,5.66175752827605E-30)) ;
#59889 = DIRECTION('center_axis',(0.,0.,-1.)) ;
#59890 = DIRECTION('ref_axis',(-1.,0.,0.)) ;
#59891 = DIRECTION('center_axis',(-4.44089209849937E-14,4.44089209849993E-14,
-1.)) ;
#59892 = DIRECTION('ref_axis',(-0.707106781186592,-0.707106781186503,-5.90838107042161E-30)) ;
#59893 = DIRECTION('center_axis',(-0.707106781186592,0.707106781186503,0.)) ;
#59894 = DIRECTION('ref_axis',(0.,0.,1.)) ;
#59895 = DIRECTION('center_axis',(1.,0.,0.)) ;
#59896 = DIRECTION('ref_axis',(0.,1.,0.)) ;
#59897 = DIRECTION('center_axis',(0.707106781186544,-0.707106781186551,1.07310884363333E-16)) ;
#59898 = DIRECTION('ref_axis',(0.499999999999969,0.499999999999965,0.707106781186594)) ;
#59899 = DIRECTION('',(-0.707106781186544,0.707106781186551,-1.07310884363333E-16)) ;
#59900 = DIRECTION('center_axis',(0.,0.,1.)) ;
#59901 = DIRECTION('ref_axis',(1.,0.,0.)) ;
#59902 = DIRECTION('center_axis',(0.,1.,0.)) ;
#59903 = DIRECTION('ref_axis',(-1.,0.,0.)) ;
#59904 = DIRECTION('center_axis',(-4.44089209850072E-14,0.,-1.)) ;
#59905 = DIRECTION('ref_axis',(0.,-1.,0.)) ;
#59906 = DIRECTION('center_axis',(-1.,0.,0.)) ;
#59907 = DIRECTION('ref_axis',(0.,0.,1.)) ;
#59908 = DIRECTION('center_axis',(-7.105427357601E-15,-1.,-1.07888364883526E-30)) ;
#59909 = DIRECTION('ref_axis',(-0.707106781186579,5.0242958677883E-15,0.707106781186516)) ;
#59910 = DIRECTION('',(-7.105427357601E-15,-1.,-1.07888364883526E-30)) ;
#59911 = DIRECTION('center_axis',(0.,0.,1.)) ;
#59912 = DIRECTION('ref_axis',(0.707106781186548,-0.707106781186548,0.)) ;
#59913 = DIRECTION('',(0.,0.,1.)) ;
#59914 = DIRECTION('',(0.,0.,-1.)) ;
#59915 = DIRECTION('center_axis',(-1.,7.10542735760144E-15,-1.51760508056877E-16)) ;
#59916 = DIRECTION('ref_axis',(4.91698498342642E-15,0.707106781186736,0.707106781186359)) ;
#59917 = DIRECTION('',(-1.,7.10542735760144E-15,-1.51760508056877E-16)) ;
#59918 = DIRECTION('center_axis',(0.,0.,-1.)) ;
#59919 = DIRECTION('ref_axis',(-0.382683432365045,-0.923879532511305,0.)) ;
#59920 = DIRECTION('',(0.,0.,1.)) ;
#59921 = DIRECTION('',(0.,0.,-1.)) ;
#59922 = DIRECTION('center_axis',(0.,0.,1.)) ;
#59923 = DIRECTION('ref_axis',(-0.923879532511297,-0.382683432365065,0.)) ;
#59924 = DIRECTION('',(0.,0.,1.)) ;
#59925 = DIRECTION('',(0.,0.,-1.)) ;
#59926 = DIRECTION('center_axis',(0.,0.,-1.)) ;
#59927 = DIRECTION('ref_axis',(-0.923879532511297,0.382683432365065,0.)) ;
#59928 = DIRECTION('',(0.,0.,1.)) ;
#59929 = DIRECTION('',(0.,0.,-1.)) ;
#59930 = DIRECTION('center_axis',(0.,0.,1.)) ;
#59931 = DIRECTION('ref_axis',(-0.382683432365099,0.923879532511283,0.)) ;
#59932 = DIRECTION('',(0.,0.,1.)) ;
#59933 = DIRECTION('',(0.,0.,-1.)) ;
#59934 = DIRECTION('center_axis',(0.,0.,1.)) ;
#59935 = DIRECTION('ref_axis',(0.707106781186296,0.707106781186799,0.)) ;
#59936 = DIRECTION('',(0.,0.,1.)) ;
#59937 = DIRECTION('',(0.,0.,-1.)) ;
#59938 = DIRECTION('center_axis',(-7.105427357601E-15,-1.,-1.07888364883526E-30)) ;
#59939 = DIRECTION('ref_axis',(-0.707106781186579,5.0242958677883E-15,0.707106781186516)) ;
#59940 = DIRECTION('',(-7.105427357601E-15,-1.,-1.07888364883526E-30)) ;
#59941 = DIRECTION('center_axis',(-7.10542735760144E-15,-1.,0.)) ;
#59942 = DIRECTION('ref_axis',(1.,-7.10542735760144E-15,1.4923676700635E-16)) ;
#59943 = DIRECTION('center_axis',(1.,-7.105427357601E-15,0.)) ;
#59944 = DIRECTION('ref_axis',(7.105427357601E-15,1.,1.06039100704685E-30)) ;
#59945 = DIRECTION('center_axis',(-0.81649658092775,0.408248290463875,-0.408248290463804)) ;
#59946 = DIRECTION('ref_axis',(-0.577350269189602,-0.577350269189744,0.577350269189531)) ;
#59947 = DIRECTION('center_axis',(-1.,-8.88178419699986E-14,0.)) ;
#59948 = DIRECTION('ref_axis',(0.,0.,1.)) ;
#59949 = DIRECTION('center_axis',(0.,-1.,0.)) ;
#59950 = DIRECTION('ref_axis',(-1.,0.,0.)) ;
#59951 = DIRECTION('center_axis',(-4.44089209850033E-14,0.,1.)) ;
#59952 = DIRECTION('ref_axis',(0.,-1.,0.)) ;
#59953 = DIRECTION('center_axis',(0.,0.,1.)) ;
#59954 = DIRECTION('ref_axis',(1.,0.,0.)) ;
#59955 = DIRECTION('center_axis',(-1.,0.,0.)) ;
#59956 = DIRECTION('ref_axis',(0.,-1.,0.)) ;
#59957 = DIRECTION('center_axis',(0.,0.,-1.)) ;
#59958 = DIRECTION('ref_axis',(1.,0.,0.)) ;
#59959 = DIRECTION('center_axis',(0.,-1.,0.)) ;
#59960 = DIRECTION('ref_axis',(0.,0.,1.)) ;
#59961 = DIRECTION('center_axis',(1.,0.,1.51760508056877E-16)) ;
#59962 = DIRECTION('ref_axis',(-1.07310884363343E-16,-0.707106781186485,0.70710678118661)) ;
#59963 = DIRECTION('',(1.,0.,1.51760508056877E-16)) ;
#59964 = DIRECTION('center_axis',(0.,0.,1.)) ;
#59965 = DIRECTION('ref_axis',(0.707106781186359,0.707106781186736,0.)) ;
#59966 = DIRECTION('',(0.,0.,1.)) ;
#59967 = DIRECTION('',(0.,0.,-1.)) ;
#59968 = DIRECTION('center_axis',(0.,0.,1.)) ;
#59969 = DIRECTION('ref_axis',(1.,0.,0.)) ;
#59970 = DIRECTION('center_axis',(-1.,0.,0.)) ;
#59971 = DIRECTION('ref_axis',(0.,-1.,0.)) ;
#59972 = DIRECTION('center_axis',(0.,0.,-1.)) ;
#59973 = DIRECTION('ref_axis',(1.,0.,0.)) ;
#59974 = DIRECTION('center_axis',(0.,-1.,0.)) ;
#59975 = DIRECTION('ref_axis',(0.,0.,1.)) ;
#59976 = DIRECTION('center_axis',(0.,0.,1.)) ;
#59977 = DIRECTION('ref_axis',(1.,0.,0.)) ;
#59978 = DIRECTION('center_axis',(0.,1.,0.)) ;
#59979 = DIRECTION('ref_axis',(-1.,0.,0.)) ;
#59980 = DIRECTION('center_axis',(-1.,0.,0.)) ;
#59981 = DIRECTION('ref_axis',(0.,0.,1.)) ;
#59982 = DIRECTION('center_axis',(0.,-1.,-5.60383084497428E-34)) ;
#59983 = DIRECTION('ref_axis',(-0.707106781186516,-3.96250679110383E-34,0.707106781186579)) ;
#59984 = DIRECTION('',(0.,-1.,-5.60383084497428E-34)) ;
#59985 = DIRECTION('center_axis',(0.,0.,-1.)) ;
#59986 = DIRECTION('ref_axis',(-1.,0.,0.)) ;
#59987 = DIRECTION('center_axis',(4.44089209850072E-14,0.,-1.)) ;
#59988 = DIRECTION('ref_axis',(0.,1.,0.)) ;
#59989 = DIRECTION('center_axis',(1.,0.,0.)) ;
#59990 = DIRECTION('ref_axis',(0.,0.,1.)) ;
#59991 = DIRECTION('center_axis',(0.,-1.,0.)) ;
#59992 = DIRECTION('ref_axis',(1.,0.,0.)) ;
#59993 = DIRECTION('center_axis',(1.,0.,1.51760508056877E-16)) ;
#59994 = DIRECTION('ref_axis',(-1.07310884363343E-16,-0.707106781186485,0.70710678118661)) ;
#59995 = DIRECTION('',(1.,0.,1.51760508056877E-16)) ;
#59996 = DIRECTION('center_axis',(0.,0.,1.)) ;
#59997 = DIRECTION('ref_axis',(1.,0.,0.)) ;
#59998 = DIRECTION('center_axis',(1.,0.,0.)) ;
#59999 = DIRECTION('ref_axis',(0.,1.,0.)) ;
#60000 = DIRECTION('center_axis',(0.,1.,0.)) ;
#60001 = DIRECTION('ref_axis',(0.,0.,1.)) ;
#60002 = DIRECTION('center_axis',(-1.,0.,-1.51760508056877E-16)) ;
#60003 = DIRECTION('ref_axis',(-1.07310884363343E-16,0.707106781186485,0.70710678118661)) ;
#60004 = DIRECTION('center_axis',(-0.816496580927844,-0.40824829046378,0.408248290463709)) ;
#60005 = DIRECTION('ref_axis',(0.577350269189507,-0.577350269189934,0.577350269189436)) ;
#60006 = DIRECTION('center_axis',(-3.55271367880058E-13,-1.,0.)) ;
#60007 = DIRECTION('ref_axis',(0.,0.,1.)) ;
#60008 = DIRECTION('center_axis',(1.,0.,0.)) ;
#60009 = DIRECTION('ref_axis',(0.,-1.,0.)) ;
#60010 = DIRECTION('center_axis',(0.,0.,1.)) ;
#60011 = DIRECTION('ref_axis',(1.,0.,0.)) ;
#60012 = DIRECTION('center_axis',(0.,-1.,0.)) ;
#60013 = DIRECTION('ref_axis',(1.,0.,0.)) ;
#60014 = DIRECTION('center_axis',(1.,0.,0.)) ;
#60015 = DIRECTION('ref_axis',(0.,0.,1.)) ;
#60016 = DIRECTION('center_axis',(0.,1.,5.60383084497428E-34)) ;
#60017 = DIRECTION('ref_axis',(0.707106781186516,-3.96250679110383E-34,0.707106781186579)) ;
#60018 = DIRECTION('center_axis',(1.,0.,1.51760508056877E-16)) ;
#60019 = DIRECTION('ref_axis',(-1.07310884363343E-16,-0.707106781186485,0.70710678118661)) ;
#60020 = DIRECTION('center_axis',(0.,1.,5.60383084497428E-34)) ;
#60021 = DIRECTION('ref_axis',(0.707106781186516,-3.96250679110383E-34,0.707106781186579)) ;
#60022 = DIRECTION('center_axis',(0.,0.,1.)) ;
#60023 = DIRECTION('ref_axis',(-0.70710678118661,0.707106781186485,0.)) ;
#60024 = DIRECTION('',(0.,0.,1.)) ;
#60025 = DIRECTION('center_axis',(0.,0.,1.)) ;
#60026 = DIRECTION('ref_axis',(0.70710678118661,0.707106781186485,0.)) ;
#60027 = DIRECTION('',(0.,0.,1.)) ;
#60028 = DIRECTION('',(0.,0.,-1.)) ;
#60029 = DIRECTION('center_axis',(0.,-1.,-5.60383084497428E-34)) ;
#60030 = DIRECTION('ref_axis',(-0.707106781186516,-3.96250679110383E-34,0.707106781186579)) ;
#60031 = DIRECTION('',(0.,-1.,-5.60383084497428E-34)) ;
#60032 = DIRECTION('center_axis',(0.,0.,1.)) ;
#60033 = DIRECTION('ref_axis',(-0.707106781186673,-0.707106781186422,0.)) ;
#60034 = DIRECTION('',(0.,0.,1.)) ;
#60035 = DIRECTION('',(0.,0.,-1.)) ;
#60036 = DIRECTION('center_axis',(1.,0.,0.)) ;
#60037 = DIRECTION('ref_axis',(0.,1.,0.)) ;
#60038 = DIRECTION('center_axis',(0.,1.,0.)) ;
#60039 = DIRECTION('ref_axis',(-1.,0.,-1.4923676700635E-16)) ;
#60040 = DIRECTION('center_axis',(0.,0.,1.)) ;
#60041 = DIRECTION('ref_axis',(0.70710678118661,0.707106781186485,0.)) ;
#60042 = DIRECTION('center_axis',(-1.4923676700635E-16,0.,1.)) ;
#60043 = DIRECTION('ref_axis',(0.70710678118661,0.707106781186485,1.05526329952556E-16)) ;
#60044 = DIRECTION('',(0.,0.,1.)) ;
#60045 = DIRECTION('center_axis',(0.,0.,-1.)) ;
#60046 = DIRECTION('ref_axis',(0.,1.,0.)) ;
#60047 = DIRECTION('',(0.,0.,-1.)) ;
#60048 = DIRECTION('center_axis',(1.77635683940026E-14,-1.,0.)) ;
#60049 = DIRECTION('ref_axis',(0.,0.,-1.)) ;
#60050 = DIRECTION('center_axis',(1.,3.94430452610435E-27,-8.88178419700105E-14)) ;
#60051 = DIRECTION('ref_axis',(9.19251792611137E-43,1.,4.44089209849993E-14)) ;
#60052 = DIRECTION('center_axis',(-1.77635683940026E-14,1.,0.)) ;
#60053 = DIRECTION('ref_axis',(0.707106781186549,1.25607396694703E-14,0.707106781186547)) ;
#60054 = DIRECTION('center_axis',(1.77635683940026E-14,-1.,0.)) ;
#60055 = DIRECTION('ref_axis',(0.707106781186548,1.25607396694703E-14,0.707106781186547)) ;
#60056 = DIRECTION('center_axis',(1.,1.77635683940026E-14,1.51760508056877E-16)) ;
#60057 = DIRECTION('ref_axis',(-1.26680505538369E-14,0.707106781186736,0.707106781186359)) ;
#60058 = DIRECTION('center_axis',(-1.77635683940026E-14,1.,0.)) ;
#60059 = DIRECTION('ref_axis',(-1.,-1.77635683940026E-14,-1.4923676700635E-16)) ;
#60060 = DIRECTION('',(1.,1.77635683940026E-14,1.4923676700635E-16)) ;
#60061 = DIRECTION('',(0.,0.,1.)) ;
#60062 = DIRECTION('center_axis',(0.,0.,1.)) ;
#60063 = DIRECTION('ref_axis',(0.707106781186359,-0.707106781186736,0.)) ;
#60064 = DIRECTION('center_axis',(-1.4923676700635E-16,0.,1.)) ;
#60065 = DIRECTION('ref_axis',(0.707106781186359,-0.707106781186736,1.05526329952519E-16)) ;
#60066 = DIRECTION('',(0.,0.,1.)) ;
#60067 = DIRECTION('center_axis',(0.,0.,-1.)) ;
#60068 = DIRECTION('ref_axis',(1.,0.,0.)) ;
#60069 = DIRECTION('',(0.,0.,-1.)) ;
#60070 = DIRECTION('center_axis',(0.,1.,0.)) ;
#60071 = DIRECTION('ref_axis',(0.,0.,1.)) ;
#60072 = DIRECTION('center_axis',(1.,0.,0.)) ;
#60073 = DIRECTION('ref_axis',(0.,0.,1.)) ;
#60074 = DIRECTION('center_axis',(0.,1.,0.)) ;
#60075 = DIRECTION('ref_axis',(0.707106781186547,0.,0.707106781186547)) ;
#60076 = DIRECTION('center_axis',(0.,-1.,0.)) ;
#60077 = DIRECTION('ref_axis',(0.707106781186548,0.,0.707106781186548)) ;
#60078 = DIRECTION('center_axis',(-1.,0.,-1.51760508056877E-16)) ;
#60079 = DIRECTION('ref_axis',(-1.07310884363343E-16,-0.707106781186485,0.70710678118661)) ;
#60080 = DIRECTION('center_axis',(3.17206578464331E-15,1.,4.81954698151804E-31)) ;
#60081 = DIRECTION('ref_axis',(0.707106781186548,-2.24298922669111E-15,0.707106781186548)) ;
#60082 = DIRECTION('',(3.17206578464331E-15,1.,4.81954698151804E-31)) ;
#60083 = DIRECTION('center_axis',(1.,-3.17206578464331E-15,0.)) ;
#60084 = DIRECTION('ref_axis',(3.17206578464331E-15,1.,4.73388842431629E-31)) ;
#60085 = DIRECTION('',(-3.17206578464331E-15,-1.,-4.73388842431629E-31)) ;
#60086 = DIRECTION('center_axis',(0.,0.,-1.)) ;
#60087 = DIRECTION('ref_axis',(-1.,0.,0.)) ;
#60088 = DIRECTION('center_axis',(-1.,0.,0.)) ;
#60089 = DIRECTION('ref_axis',(0.,0.,1.)) ;
#60090 = DIRECTION('center_axis',(0.707106781186592,0.707106781186503,0.)) ;
#60091 = DIRECTION('ref_axis',(-0.707106781186503,0.707106781186592,0.)) ;
#60092 = DIRECTION('center_axis',(-1.,0.,-1.51760508056877E-16)) ;
#60093 = DIRECTION('ref_axis',(-1.07310884363343E-16,0.707106781186485,0.70710678118661)) ;
#60094 = DIRECTION('center_axis',(0.,0.,-1.)) ;
#60095 = DIRECTION('ref_axis',(-1.,0.,0.)) ;
#60096 = DIRECTION('center_axis',(-0.707106781186548,-0.707106781186548,0.)) ;
#60097 = DIRECTION('ref_axis',(0.,0.,1.)) ;
#60098 = DIRECTION('center_axis',(0.,1.,0.)) ;
#60099 = DIRECTION('ref_axis',(-1.,0.,0.)) ;
#60100 = DIRECTION('center_axis',(0.707106781186555,0.70710678118654,1.07310884363335E-16)) ;
#60101 = DIRECTION('ref_axis',(-0.499999999999931,0.499999999999941,0.707106781186638)) ;
#60102 = DIRECTION('center_axis',(0.,0.,-1.)) ;
#60103 = DIRECTION('ref_axis',(-1.,0.,0.)) ;
#60104 = DIRECTION('center_axis',(0.,-1.,0.)) ;
#60105 = DIRECTION('ref_axis',(0.,0.,1.)) ;
#60106 = DIRECTION('center_axis',(-0.707106781186503,0.707106781186592,0.)) ;
#60107 = DIRECTION('ref_axis',(-0.707106781186592,-0.707106781186503,0.)) ;
#60108 = DIRECTION('center_axis',(0.,-1.,-5.60383084497428E-34)) ;
#60109 = DIRECTION('ref_axis',(-0.707106781186548,-3.96250679110365E-34,0.707106781186548)) ;
#60110 = DIRECTION('center_axis',(0.,0.,-1.)) ;
#60111 = DIRECTION('ref_axis',(-1.,0.,0.)) ;
#60112 = DIRECTION('center_axis',(0.707106781186548,-0.707106781186548,0.)) ;
#60113 = DIRECTION('ref_axis',(0.,0.,1.)) ;
#60114 = DIRECTION('center_axis',(-1.,0.,0.)) ;
#60115 = DIRECTION('ref_axis',(0.,-1.,0.)) ;
#60116 = DIRECTION('center_axis',(-0.707106781186555,0.70710678118654,-1.07310884363335E-16)) ;
#60117 = DIRECTION('ref_axis',(-0.499999999999962,-0.499999999999972,0.707106781186594)) ;
#60118 = DIRECTION('center_axis',(1.,0.,1.51760508056877E-16)) ;
#60119 = DIRECTION('ref_axis',(-1.07310884363343E-16,-0.707106781186485,0.70710678118661)) ;
#60120 = DIRECTION('center_axis',(0.,0.,1.)) ;
#60121 = DIRECTION('ref_axis',(-0.707106781186359,0.707106781186736,0.)) ;
#60122 = DIRECTION('center_axis',(-1.4923676700635E-16,0.,1.)) ;
#60123 = DIRECTION('ref_axis',(-0.707106781186359,0.707106781186736,-1.05526329952519E-16)) ;
#60124 = DIRECTION('',(0.,0.,1.)) ;
#60125 = DIRECTION('center_axis',(0.,0.,-1.)) ;
#60126 = DIRECTION('ref_axis',(-1.,0.,0.)) ;
#60127 = DIRECTION('',(0.,0.,-1.)) ;
#60128 = DIRECTION('center_axis',(0.,-1.,0.)) ;
#60129 = DIRECTION('ref_axis',(0.,0.,-1.)) ;
#60130 = DIRECTION('center_axis',(-1.,-9.23705556487986E-12,0.)) ;
#60131 = DIRECTION('ref_axis',(0.,0.,1.)) ;
#60132 = DIRECTION('center_axis',(0.,-1.,0.)) ;
#60133 = DIRECTION('ref_axis',(-0.707106781186543,0.,0.707106781186552)) ;
#60134 = DIRECTION('center_axis',(0.,1.,0.)) ;
#60135 = DIRECTION('ref_axis',(-0.707106781186543,0.,0.707106781186552)) ;
#60136 = DIRECTION('center_axis',(1.,0.,1.51760508056877E-16)) ;
#60137 = DIRECTION('ref_axis',(-1.07310884363343E-16,0.707106781186485,0.70710678118661)) ;
#60138 = DIRECTION('center_axis',(0.70710678118661,0.707106781186485,0.)) ;
#60139 = DIRECTION('ref_axis',(-0.707106781186485,0.70710678118661,-2.45326946669362E-16)) ;
#60140 = DIRECTION('center_axis',(3.17206578464327E-15,-1.,4.80833931982803E-31)) ;
#60141 = DIRECTION('ref_axis',(-0.707106781186551,-2.24298922669109E-15,0.707106781186544)) ;
#60142 = DIRECTION('',(3.17206578464327E-15,-1.,4.80833931982803E-31)) ;
#60143 = DIRECTION('center_axis',(-3.55271367880051E-14,-1.,0.)) ;
#60144 = DIRECTION('ref_axis',(-0.707106781186548,2.51214793389405E-14,0.707106781186547)) ;
#60145 = DIRECTION('center_axis',(-1.,-3.17206578464327E-15,0.)) ;
#60146 = DIRECTION('ref_axis',(3.17206578464327E-15,-1.,4.73388842431623E-31)) ;
#60147 = DIRECTION('',(-3.17206578464327E-15,1.,-4.73388842431623E-31)) ;
#60148 = DIRECTION('',(0.,0.,-1.)) ;
#60149 = DIRECTION('center_axis',(-1.4923676700635E-16,0.,1.)) ;
#60150 = DIRECTION('ref_axis',(1.,0.,1.4923676700635E-16)) ;
#60151 = DIRECTION('',(1.,0.,1.4923676700635E-16)) ;
#60152 = DIRECTION('',(-3.17206578464323E-15,-1.,-4.73388842431617E-31)) ;
#60153 = DIRECTION('',(-1.,3.55271367880051E-14,-1.4923676700635E-16)) ;
#60154 = DIRECTION('center_axis',(-1.4923676700635E-16,0.,1.)) ;
#60155 = DIRECTION('ref_axis',(-0.707106781186359,-0.707106781186736,-1.05526329952519E-16)) ;
#60156 = DIRECTION('center_axis',(0.,0.,1.)) ;
#60157 = DIRECTION('ref_axis',(-0.707106781186359,-0.707106781186736,0.)) ;
#60158 = DIRECTION('',(0.,0.,1.)) ;
#60159 = DIRECTION('center_axis',(0.,0.,-1.)) ;
#60160 = DIRECTION('ref_axis',(0.,-1.,0.)) ;
#60161 = DIRECTION('center_axis',(3.55271367880051E-14,1.,0.)) ;
#60162 = DIRECTION('ref_axis',(0.,0.,1.)) ;
#60163 = DIRECTION('center_axis',(-1.,4.25984888819251E-25,9.5923269327607E-12)) ;
#60164 = DIRECTION('ref_axis',(-3.39809272400367E-40,-1.,4.44089209849993E-14)) ;
#60165 = DIRECTION('center_axis',(3.55271367880051E-14,1.,0.)) ;
#60166 = DIRECTION('ref_axis',(-0.707106781186548,2.51214793389405E-14,0.707106781186547)) ;
#60167 = DIRECTION('center_axis',(-1.,3.55271367880051E-14,-1.51760508056877E-16)) ;
#60168 = DIRECTION('ref_axis',(-2.52287902233016E-14,-0.707106781186485,0.70710678118661)) ;
#60169 = DIRECTION('center_axis',(0.70710678118661,-0.707106781186485,0.)) ;
#60170 = DIRECTION('ref_axis',(-0.707106781186485,-0.70710678118661,-1.22663473334685E-16)) ;
#60171 = DIRECTION('center_axis',(-3.55271367880051E-14,-1.,0.)) ;
#60172 = DIRECTION('ref_axis',(1.,-3.55271367880051E-14,1.4923676700635E-16)) ;
#60173 = DIRECTION('',(0.,0.,1.)) ;
#60174 = DIRECTION('',(0.,0.,-1.)) ;
#60175 = DIRECTION('center_axis',(0.,0.,-1.)) ;
#60176 = DIRECTION('ref_axis',(-1.,0.,0.)) ;
#60177 = DIRECTION('center_axis',(-4.44089209849993E-14,4.44089209849993E-14,
-1.)) ;
#60178 = DIRECTION('ref_axis',(-0.707106781186547,-0.707106781186547,-2.16129177030881E-30)) ;
#60179 = DIRECTION('center_axis',(-0.707106781186503,0.707106781186592,0.)) ;
#60180 = DIRECTION('ref_axis',(0.,0.,1.)) ;
#60181 = DIRECTION('center_axis',(1.,0.,0.)) ;
#60182 = DIRECTION('ref_axis',(0.,1.,0.)) ;
#60183 = DIRECTION('center_axis',(-8.88178419700144E-14,0.,-1.)) ;
#60184 = DIRECTION('ref_axis',(-1.,0.,8.28966525053497E-14)) ;
#60185 = DIRECTION('center_axis',(0.,-6.28036983473606E-14,-1.)) ;
#60186 = DIRECTION('ref_axis',(-1.,0.,0.)) ;
#60187 = DIRECTION('center_axis',(0.,1.,0.)) ;
#60188 = DIRECTION('ref_axis',(0.,0.,1.)) ;
#60189 = DIRECTION('center_axis',(0.707106781186503,-0.707106781186592,-6.28036983473484E-14)) ;
#60190 = DIRECTION('ref_axis',(0.707106781186592,0.707106781186503,2.27272335701132E-30)) ;
#60191 = DIRECTION('center_axis',(0.,0.,-1.)) ;
#60192 = DIRECTION('ref_axis',(-1.,0.,0.)) ;
#60193 = DIRECTION('center_axis',(4.44089209850072E-14,4.44089209850072E-14,
-1.)) ;
#60194 = DIRECTION('ref_axis',(-0.707106781186547,0.707106781186547,-2.2709071609452E-30)) ;
#60195 = DIRECTION('center_axis',(0.707106781186548,0.707106781186548,0.)) ;
#60196 = DIRECTION('ref_axis',(0.,0.,1.)) ;
#60197 = DIRECTION('center_axis',(0.,-1.,0.)) ;
#60198 = DIRECTION('ref_axis',(1.,0.,0.)) ;
#60199 = DIRECTION('center_axis',(0.,0.,-1.)) ;
#60200 = DIRECTION('ref_axis',(-1.,0.,0.)) ;
#60201 = DIRECTION('center_axis',(0.,0.,-1.)) ;
#60202 = DIRECTION('ref_axis',(0.,1.,0.)) ;
#60203 = DIRECTION('center_axis',(1.,0.,0.)) ;
#60204 = DIRECTION('ref_axis',(0.,0.,1.)) ;
#60205 = DIRECTION('center_axis',(-0.707106781186548,-0.707106781186548,0.)) ;
#60206 = DIRECTION('ref_axis',(0.707106781186547,-0.707106781186547,0.)) ;
#60207 = DIRECTION('center_axis',(1.,0.,1.51760508056877E-16)) ;
#60208 = DIRECTION('ref_axis',(-1.07310884363343E-16,-0.707106781186485,0.70710678118661)) ;
#60209 = DIRECTION('',(1.,0.,1.51760508056877E-16)) ;
#60210 = DIRECTION('center_axis',(-7.105427357601E-15,-1.,-1.07888364883526E-30)) ;
#60211 = DIRECTION('ref_axis',(-0.707106781186453,5.02429586778741E-15,0.707106781186642)) ;
#60212 = DIRECTION('center_axis',(-0.707106781186563,-0.707106781186532,-1.07310884363336E-16)) ;
#60213 = DIRECTION('ref_axis',(0.499999999999956,-0.499999999999978,0.707106781186594)) ;
#60214 = DIRECTION('',(0.707106781186563,0.707106781186532,1.07310884363336E-16)) ;
#60215 = DIRECTION('center_axis',(0.,0.,1.)) ;
#60216 = DIRECTION('ref_axis',(-0.382683432365099,0.923879532511283,0.)) ;
#60217 = DIRECTION('',(0.,0.,1.)) ;
#60218 = DIRECTION('',(0.,0.,-1.)) ;
#60219 = DIRECTION('center_axis',(3.73034936274055E-14,1.,5.66175752827605E-30)) ;
#60220 = DIRECTION('ref_axis',(0.707106781186516,-2.63775533058864E-14,0.707106781186579)) ;
#60221 = DIRECTION('',(3.73034936274055E-14,1.,5.66175752827605E-30)) ;
#60222 = DIRECTION('center_axis',(0.,0.,-1.)) ;
#60223 = DIRECTION('ref_axis',(-0.923879532511297,0.382683432365065,0.)) ;
#60224 = DIRECTION('',(0.,0.,1.)) ;
#60225 = DIRECTION('',(0.,0.,-1.)) ;
#60226 = DIRECTION('center_axis',(0.707106781186575,-0.70710678118652,1.07310884363338E-16)) ;
#60227 = DIRECTION('ref_axis',(0.499999999999948,0.499999999999987,0.707106781186594)) ;
#60228 = DIRECTION('',(-0.707106781186575,0.70710678118652,-1.07310884363338E-16)) ;
#60229 = DIRECTION('center_axis',(0.,0.,1.)) ;
#60230 = DIRECTION('ref_axis',(-0.923879532511297,-0.382683432365065,0.)) ;
#60231 = DIRECTION('',(0.,0.,1.)) ;
#60232 = DIRECTION('',(0.,0.,-1.)) ;
#60233 = DIRECTION('center_axis',(-1.,7.10542735760144E-15,-1.51760508056877E-16)) ;
#60234 = DIRECTION('ref_axis',(4.91698498342642E-15,0.707106781186736,0.707106781186359)) ;
#60235 = DIRECTION('',(-1.,7.10542735760144E-15,-1.51760508056877E-16)) ;
#60236 = DIRECTION('center_axis',(0.,0.,-1.)) ;
#60237 = DIRECTION('ref_axis',(-0.382683432364963,-0.923879532511339,0.)) ;
#60238 = DIRECTION('',(0.,0.,1.)) ;
#60239 = DIRECTION('',(0.,0.,-1.)) ;
#60240 = DIRECTION('center_axis',(-7.105427357601E-15,-1.,-1.07888364883526E-30)) ;
#60241 = DIRECTION('ref_axis',(-0.707106781186453,5.02429586778741E-15,0.707106781186642)) ;
#60242 = DIRECTION('',(-7.105427357601E-15,-1.,-1.07888364883526E-30)) ;
#60243 = DIRECTION('center_axis',(0.707106781186532,-0.707106781186563,0.)) ;
#60244 = DIRECTION('ref_axis',(0.,0.,-1.)) ;
#60245 = DIRECTION('center_axis',(-1.,3.73034936274055E-14,0.)) ;
#60246 = DIRECTION('ref_axis',(-3.73034936274055E-14,-1.,-5.56705278699598E-30)) ;
#60247 = DIRECTION('center_axis',(0.70710678118652,0.707106781186575,0.)) ;
#60248 = DIRECTION('ref_axis',(0.,0.,-1.)) ;
#60249 = DIRECTION('center_axis',(-7.10542735760144E-15,-1.,0.)) ;
#60250 = DIRECTION('ref_axis',(1.,-7.10542735760144E-15,1.4923676700635E-16)) ;
#60251 = DIRECTION('center_axis',(1.,-7.105427357601E-15,0.)) ;
#60252 = DIRECTION('ref_axis',(7.105427357601E-15,1.,1.06039100704685E-30)) ;
#60253 = DIRECTION('center_axis',(0.,-1.,-5.60383084497428E-34)) ;
#60254 = DIRECTION('ref_axis',(0.707106781186548,3.96250679110365E-34,-0.707106781186548)) ;
#60255 = DIRECTION('',(0.,-1.,-5.60383084497428E-34)) ;
#60256 = DIRECTION('center_axis',(-1.,0.,0.)) ;
#60257 = DIRECTION('ref_axis',(0.,-1.,0.)) ;
#60258 = DIRECTION('center_axis',(0.,-1.,-5.60383084497428E-34)) ;
#60259 = DIRECTION('ref_axis',(0.707106781186548,3.96250679110365E-34,-0.707106781186548)) ;
#60260 = DIRECTION('',(0.,-1.,-5.60383084497428E-34)) ;
#60261 = DIRECTION('center_axis',(-1.,0.,0.)) ;
#60262 = DIRECTION('ref_axis',(0.,-1.,0.)) ;
#60263 = DIRECTION('center_axis',(0.,0.,1.)) ;
#60264 = DIRECTION('ref_axis',(1.,0.,0.)) ;
#60265 = DIRECTION('center_axis',(0.,1.,0.)) ;
#60266 = DIRECTION('ref_axis',(-1.,0.,0.)) ;
#60267 = DIRECTION('center_axis',(0.,0.,-1.)) ;
#60268 = DIRECTION('ref_axis',(0.,-1.,0.)) ;
#60269 = DIRECTION('center_axis',(-1.,0.,0.)) ;
#60270 = DIRECTION('ref_axis',(0.,0.,1.)) ;
#60271 = DIRECTION('center_axis',(0.,0.,1.)) ;
#60272 = DIRECTION('ref_axis',(1.,0.,0.)) ;
#60273 = DIRECTION('center_axis',(0.,0.,1.)) ;
#60274 = DIRECTION('ref_axis',(1.,0.,0.)) ;
#60275 = DIRECTION('center_axis',(0.,1.,0.)) ;
#60276 = DIRECTION('ref_axis',(0.,0.,-1.)) ;
#60277 = DIRECTION('center_axis',(-1.,0.,0.)) ;
#60278 = DIRECTION('ref_axis',(0.,1.,0.)) ;
#60279 = DIRECTION('center_axis',(0.,0.,1.)) ;
#60280 = DIRECTION('ref_axis',(1.,0.,0.)) ;
#60281 = DIRECTION('center_axis',(-1.,0.,0.)) ;
#60282 = DIRECTION('ref_axis',(0.,-1.,0.)) ;
#60283 = DIRECTION('center_axis',(0.,0.,-1.)) ;
#60284 = DIRECTION('ref_axis',(1.,0.,0.)) ;
#60285 = DIRECTION('center_axis',(0.,-1.,0.)) ;
#60286 = DIRECTION('ref_axis',(0.,0.,1.)) ;
#60287 = DIRECTION('center_axis',(0.,0.,-1.)) ;
#60288 = DIRECTION('ref_axis',(-1.,0.,0.)) ;
#60289 = DIRECTION('center_axis',(0.,0.,-1.)) ;
#60290 = DIRECTION('ref_axis',(-1.,0.,0.)) ;
#60291 = DIRECTION('center_axis',(0.,1.,0.)) ;
#60292 = DIRECTION('ref_axis',(0.,0.,1.)) ;
#60293 = DIRECTION('center_axis',(1.,0.,0.)) ;
#60294 = DIRECTION('ref_axis',(0.,1.,0.)) ;
#60295 = DIRECTION('center_axis',(0.,0.,-1.)) ;
#60296 = DIRECTION('ref_axis',(-1.,0.,0.)) ;
#60297 = DIRECTION('center_axis',(0.,1.,0.)) ;
#60298 = DIRECTION('ref_axis',(1.,0.,0.)) ;
#60299 = DIRECTION('center_axis',(0.,0.,1.)) ;
#60300 = DIRECTION('ref_axis',(0.,-1.,0.)) ;
#60301 = DIRECTION('center_axis',(1.,0.,0.)) ;
#60302 = DIRECTION('ref_axis',(0.,0.,-1.)) ;
#60303 = DIRECTION('center_axis',(0.,0.,1.)) ;
#60304 = DIRECTION('ref_axis',(1.,0.,0.)) ;
#60305 = DIRECTION('center_axis',(0.,0.,1.)) ;
#60306 = DIRECTION('ref_axis',(0.,1.,0.)) ;
#60307 = DIRECTION('center_axis',(-1.,0.,0.)) ;
#60308 = DIRECTION('ref_axis',(0.,0.,-1.)) ;
#60309 = DIRECTION('center_axis',(0.,-1.,0.)) ;
#60310 = DIRECTION('ref_axis',(-1.,0.,0.)) ;
#60311 = DIRECTION('center_axis',(0.,0.,1.)) ;
#60312 = DIRECTION('ref_axis',(1.,0.,0.)) ;
#60313 = DIRECTION('center_axis',(0.,-1.,0.)) ;
#60314 = DIRECTION('ref_axis',(1.,0.,0.)) ;
#60315 = DIRECTION('center_axis',(-4.44089209850092E-14,0.,-1.)) ;
#60316 = DIRECTION('ref_axis',(0.,1.,0.)) ;
#60317 = DIRECTION('center_axis',(1.,0.,0.)) ;
#60318 = DIRECTION('ref_axis',(0.,0.,1.)) ;
#60319 = DIRECTION('center_axis',(5.55111512312578E-16,1.,8.48043882212758E-32)) ;
#60320 = DIRECTION('ref_axis',(0.707106781186579,-3.92523114670961E-16,0.707106781186516)) ;
#60321 = DIRECTION('',(5.55111512312578E-16,1.,8.48043882212758E-32)) ;
#60322 = DIRECTION('center_axis',(0.,0.,1.)) ;
#60323 = DIRECTION('ref_axis',(1.,0.,0.)) ;
#60324 = DIRECTION('center_axis',(0.,0.,1.)) ;
#60325 = DIRECTION('ref_axis',(-1.,0.,0.)) ;
#60326 = DIRECTION('center_axis',(0.,-1.,0.)) ;
#60327 = DIRECTION('ref_axis',(0.,0.,-1.)) ;
#60328 = DIRECTION('center_axis',(1.,0.,0.)) ;
#60329 = DIRECTION('ref_axis',(0.,-1.,0.)) ;
#60330 = DIRECTION('center_axis',(-5.55111512312578E-16,-1.,-8.48043882212758E-32)) ;
#60331 = DIRECTION('ref_axis',(0.707106781186548,-3.92523114670943E-16,-0.707106781186548)) ;
#60332 = DIRECTION('',(-5.55111512312578E-16,-1.,-8.48043882212758E-32)) ;
#60333 = DIRECTION('center_axis',(-1.,0.,-1.51760508056877E-16)) ;
#60334 = DIRECTION('ref_axis',(1.07310884363343E-16,-0.707106781186485,-0.70710678118661)) ;
#60335 = DIRECTION('',(-1.,0.,-1.51760508056877E-16)) ;
#60336 = DIRECTION('center_axis',(0.,0.,1.)) ;
#60337 = DIRECTION('ref_axis',(-0.707106781186579,0.707106781186516,0.)) ;
#60338 = DIRECTION('',(0.,0.,-1.)) ;
#60339 = DIRECTION('',(0.,0.,1.)) ;
#60340 = DIRECTION('center_axis',(1.,0.,1.51760508056877E-16)) ;
#60341 = DIRECTION('ref_axis',(-1.07310884363343E-16,-0.707106781186485,0.70710678118661)) ;
#60342 = DIRECTION('',(1.,0.,1.51760508056877E-16)) ;
#60343 = DIRECTION('center_axis',(-1.11022302462516E-15,1.,-1.67927627189059E-31)) ;
#60344 = DIRECTION('ref_axis',(-0.707106781186548,-7.8504622934189E-16,-0.707106781186548)) ;
#60345 = DIRECTION('',(-1.11022302462516E-15,1.,-1.67927627189059E-31)) ;
#60346 = DIRECTION('center_axis',(0.,0.,1.)) ;
#60347 = DIRECTION('ref_axis',(0.70710678118661,0.707106781186485,0.)) ;
#60348 = DIRECTION('',(0.,0.,-1.)) ;
#60349 = DIRECTION('',(0.,0.,1.)) ;
#60350 = DIRECTION('center_axis',(0.,0.,1.)) ;
#60351 = DIRECTION('ref_axis',(-0.70710678118661,-0.707106781186485,0.)) ;
#60352 = DIRECTION('',(0.,0.,-1.)) ;
#60353 = DIRECTION('',(0.,0.,1.)) ;
#60354 = DIRECTION('center_axis',(1.,0.,1.51760508056877E-16)) ;
#60355 = DIRECTION('ref_axis',(1.07310884363343E-16,0.707106781186485,-0.70710678118661)) ;
#60356 = DIRECTION('',(1.,0.,1.51760508056877E-16)) ;
#60357 = DIRECTION('center_axis',(-1.,0.,-1.51760508056877E-16)) ;
#60358 = DIRECTION('ref_axis',(-1.07310884363343E-16,0.707106781186485,0.70710678118661)) ;
#60359 = DIRECTION('',(-1.,0.,-1.51760508056877E-16)) ;
#60360 = DIRECTION('center_axis',(1.11022302462516E-15,-1.,1.67927627189059E-31)) ;
#60361 = DIRECTION('ref_axis',(-0.707106781186548,-7.8504622934189E-16,0.707106781186548)) ;
#60362 = DIRECTION('',(1.11022302462516E-15,-1.,1.67927627189059E-31)) ;
#60363 = DIRECTION('center_axis',(0.,0.,1.)) ;
#60364 = DIRECTION('ref_axis',(0.70710678118661,-0.707106781186485,0.)) ;
#60365 = DIRECTION('',(0.,0.,-1.)) ;
#60366 = DIRECTION('',(0.,0.,1.)) ;
#60367 = DIRECTION('center_axis',(-1.,5.55111512312578E-16,0.)) ;
#60368 = DIRECTION('ref_axis',(-5.55111512312578E-16,-1.,-8.28430474255348E-32)) ;
#60369 = DIRECTION('center_axis',(0.,1.,0.)) ;
#60370 = DIRECTION('ref_axis',(-1.,0.,-1.4923676700635E-16)) ;
#60371 = DIRECTION('center_axis',(1.,1.11022302462516E-15,0.)) ;
#60372 = DIRECTION('ref_axis',(-1.11022302462516E-15,1.,-1.6568609485107E-31)) ;
#60373 = DIRECTION('center_axis',(0.,-1.,0.)) ;
#60374 = DIRECTION('ref_axis',(1.,0.,1.4923676700635E-16)) ;
#60375 = DIRECTION('center_axis',(-1.51760508056877E-16,-5.60383084497428E-34,
1.)) ;
#60376 = DIRECTION('ref_axis',(1.,0.,0.)) ;
#60377 = DIRECTION('center_axis',(0.,-1.,-5.60383084497428E-34)) ;
#60378 = DIRECTION('ref_axis',(-1.,0.,0.)) ;
#60379 = DIRECTION('center_axis',(-1.51760508056877E-16,-5.60383084497428E-34,
1.)) ;
#60380 = DIRECTION('ref_axis',(1.,-2.24153233798967E-35,1.51760508056877E-16)) ;
#60381 = DIRECTION('center_axis',(-2.01858731750028E-16,0.,1.)) ;
#60382 = DIRECTION('ref_axis',(1.,0.,2.01858731750028E-16)) ;
#60383 = DIRECTION('',(-2.01858731750028E-16,0.,1.)) ;
#60384 = DIRECTION('center_axis',(1.51760508056877E-16,5.60383084497428E-34,
-1.)) ;
#60385 = DIRECTION('ref_axis',(1.,2.24153233798966E-35,1.51760508056877E-16)) ;
#60386 = DIRECTION('center_axis',(1.51760508056877E-16,5.60383084497428E-34,
-1.)) ;
#60387 = DIRECTION('ref_axis',(1.,2.24153233798966E-35,1.51760508056877E-16)) ;
#60388 = DIRECTION('center_axis',(1.51760508056877E-16,5.60383084497428E-34,
-1.)) ;
#60389 = DIRECTION('ref_axis',(-1.,0.,0.)) ;
#60390 = DIRECTION('center_axis',(0.,-1.,-5.60383084497428E-34)) ;
#60391 = DIRECTION('ref_axis',(1.,0.,0.)) ;
#60392 = DIRECTION('center_axis',(0.,0.,1.)) ;
#60393 = DIRECTION('ref_axis',(0.70710678118661,0.707106781186485,0.)) ;
#60394 = DIRECTION('center_axis',(-1.4923676700635E-16,0.,1.)) ;
#60395 = DIRECTION('ref_axis',(0.70710678118661,0.707106781186485,1.05526329952556E-16)) ;
#60396 = DIRECTION('',(0.,0.,1.)) ;
#60397 = DIRECTION('center_axis',(0.,0.,-1.)) ;
#60398 = DIRECTION('ref_axis',(0.,1.,0.)) ;
#60399 = DIRECTION('',(0.,0.,-1.)) ;
#60400 = DIRECTION('center_axis',(0.,-1.,0.)) ;
#60401 = DIRECTION('ref_axis',(0.,0.,-1.)) ;
#60402 = DIRECTION('center_axis',(1.,1.97215226305235E-27,4.44089209850092E-14)) ;
#60403 = DIRECTION('ref_axis',(8.40779078574419E-43,1.,-4.44089209849993E-14)) ;
#60404 = DIRECTION('center_axis',(0.,1.,0.)) ;
#60405 = DIRECTION('ref_axis',(0.707106781186548,0.,0.707106781186548)) ;
#60406 = DIRECTION('center_axis',(0.,-1.,0.)) ;
#60407 = DIRECTION('ref_axis',(0.707106781186547,0.,0.707106781186547)) ;
#60408 = DIRECTION('center_axis',(1.,0.,1.51760508056877E-16)) ;
#60409 = DIRECTION('ref_axis',(-1.07310884363305E-16,0.707106781186736,0.707106781186359)) ;
#60410 = DIRECTION('center_axis',(-0.70710678118661,0.707106781186485,0.)) ;
#60411 = DIRECTION('ref_axis',(0.707106781186485,0.70710678118661,1.83995210002021E-16)) ;
#60412 = DIRECTION('center_axis',(0.,1.,0.)) ;
#60413 = DIRECTION('ref_axis',(-1.,0.,-1.4923676700635E-16)) ;
#60414 = DIRECTION('',(1.,0.,1.4923676700635E-16)) ;
#60415 = DIRECTION('',(0.,0.,1.)) ;
#60416 = DIRECTION('center_axis',(-1.4923676700635E-16,0.,1.)) ;
#60417 = DIRECTION('ref_axis',(1.,0.,1.4923676700635E-16)) ;
#60418 = DIRECTION('',(0.,-1.,0.)) ;
#60419 = DIRECTION('center_axis',(-1.4923676700635E-16,0.,1.)) ;
#60420 = DIRECTION('ref_axis',(0.707106781186642,-0.707106781186453,1.05526329952561E-16)) ;
#60421 = DIRECTION('',(-1.,-3.55271367880051E-14,-1.4923676700635E-16)) ;
#60422 = DIRECTION('',(0.,1.,0.)) ;
#60423 = DIRECTION('center_axis',(1.,0.,0.)) ;
#60424 = DIRECTION('ref_axis',(0.,1.,0.)) ;
#60425 = DIRECTION('',(0.,1.,5.60383084497428E-34)) ;
#60426 = DIRECTION('',(0.,0.,1.)) ;
#60427 = DIRECTION('center_axis',(0.,0.,1.)) ;
#60428 = DIRECTION('ref_axis',(0.707106781186642,-0.707106781186453,0.)) ;
#60429 = DIRECTION('center_axis',(0.,0.,-1.)) ;
#60430 = DIRECTION('ref_axis',(1.,0.,0.)) ;
#60431 = DIRECTION('',(0.,0.,-1.)) ;
#60432 = DIRECTION('center_axis',(-3.55271367880051E-14,1.,0.)) ;
#60433 = DIRECTION('ref_axis',(0.,0.,1.)) ;
#60434 = DIRECTION('center_axis',(1.,4.44089209849835E-14,0.)) ;
#60435 = DIRECTION('ref_axis',(0.,0.,1.)) ;
#60436 = DIRECTION('center_axis',(-3.55271367880051E-14,1.,0.)) ;
#60437 = DIRECTION('ref_axis',(0.707106781186546,2.51214793389404E-14,0.707106781186549)) ;
#60438 = DIRECTION('center_axis',(3.55271367880051E-14,-1.,0.)) ;
#60439 = DIRECTION('ref_axis',(0.707106781186546,2.51214793389404E-14,0.707106781186549)) ;
#60440 = DIRECTION('center_axis',(-1.,-3.55271367880051E-14,-1.51760508056877E-16)) ;
#60441 = DIRECTION('ref_axis',(2.50141684545749E-14,-0.707106781186485,0.70710678118661)) ;
#60442 = DIRECTION('center_axis',(-0.70710678118661,-0.707106781186485,0.)) ;
#60443 = DIRECTION('ref_axis',(0.707106781186485,-0.70710678118661,2.4532694666937E-16)) ;
#60444 = DIRECTION('center_axis',(0.,1.,5.60383084497428E-34)) ;
#60445 = DIRECTION('ref_axis',(0.707106781186548,-3.96250679110365E-34,0.707106781186548)) ;
#60446 = DIRECTION('center_axis',(0.,0.,-1.)) ;
#60447 = DIRECTION('ref_axis',(-1.,0.,0.)) ;
#60448 = DIRECTION('center_axis',(-1.,0.,0.)) ;
#60449 = DIRECTION('ref_axis',(0.,0.,1.)) ;
#60450 = DIRECTION('center_axis',(0.707106781186503,0.707106781186592,0.)) ;
#60451 = DIRECTION('ref_axis',(-0.707106781186592,0.707106781186503,0.)) ;
#60452 = DIRECTION('center_axis',(-1.,0.,-1.51760508056877E-16)) ;
#60453 = DIRECTION('ref_axis',(-1.07310884363343E-16,0.707106781186485,0.70710678118661)) ;
#60454 = DIRECTION('center_axis',(0.70710678118661,-0.707106781186485,0.)) ;
#60455 = DIRECTION('ref_axis',(0.707106781186485,0.70710678118661,2.14621768726686E-16)) ;
#60456 = DIRECTION('center_axis',(0.,0.,-1.)) ;
#60457 = DIRECTION('ref_axis',(-1.,0.,0.)) ;
#60458 = DIRECTION('center_axis',(-0.707106781186481,-0.707106781186614,0.)) ;
#60459 = DIRECTION('ref_axis',(0.,0.,1.)) ;
#60460 = DIRECTION('center_axis',(0.,1.,0.)) ;
#60461 = DIRECTION('ref_axis',(-1.,0.,0.)) ;
#60462 = DIRECTION('center_axis',(0.707106781186555,0.70710678118654,1.07310884363335E-16)) ;
#60463 = DIRECTION('ref_axis',(-0.499999999999977,0.499999999999988,0.707106781186572)) ;
#60464 = DIRECTION('center_axis',(0.,0.,-1.)) ;
#60465 = DIRECTION('ref_axis',(-1.,0.,0.)) ;
#60466 = DIRECTION('center_axis',(0.,-1.,0.)) ;
#60467 = DIRECTION('ref_axis',(0.,0.,1.)) ;
#60468 = DIRECTION('center_axis',(-0.707106781186548,0.707106781186548,0.)) ;
#60469 = DIRECTION('ref_axis',(-0.707106781186547,-0.707106781186547,0.)) ;
#60470 = DIRECTION('center_axis',(1.1311821873082E-49,-1.,-5.60383084497428E-34)) ;
#60471 = DIRECTION('ref_axis',(-0.707106781186548,-3.96250679110365E-34,0.707106781186548)) ;
#60472 = DIRECTION('center_axis',(0.,0.,-1.)) ;
#60473 = DIRECTION('ref_axis',(-1.,0.,0.)) ;
#60474 = DIRECTION('center_axis',(0.70710678118657,-0.707106781186525,0.)) ;
#60475 = DIRECTION('ref_axis',(0.,0.,1.)) ;
#60476 = DIRECTION('center_axis',(-1.,0.,0.)) ;
#60477 = DIRECTION('ref_axis',(0.,-1.,0.)) ;
#60478 = DIRECTION('center_axis',(-0.707106781186555,0.70710678118654,-1.07310884363335E-16)) ;
#60479 = DIRECTION('ref_axis',(-0.499999999999962,-0.499999999999972,0.707106781186594)) ;
#60480 = DIRECTION('center_axis',(0.,0.,-1.)) ;
#60481 = DIRECTION('ref_axis',(-1.,0.,0.)) ;
#60482 = DIRECTION('center_axis',(1.,0.,0.)) ;
#60483 = DIRECTION('ref_axis',(0.,0.,1.)) ;
#60484 = DIRECTION('center_axis',(0.,-1.,0.)) ;
#60485 = DIRECTION('ref_axis',(1.,0.,0.)) ;
#60486 = DIRECTION('center_axis',(1.,0.,1.51760508056877E-16)) ;
#60487 = DIRECTION('ref_axis',(-1.07310884363343E-16,-0.707106781186485,0.70710678118661)) ;
#60488 = DIRECTION('center_axis',(-1.1311821873082E-49,1.,5.60383084497428E-34)) ;
#60489 = DIRECTION('ref_axis',(0.707106781186548,-3.96250679110365E-34,0.707106781186548)) ;
#60490 = DIRECTION('center_axis',(-1.1311821873082E-49,1.,5.60383084497428E-34)) ;
#60491 = DIRECTION('ref_axis',(0.707106781186548,-3.96250679110365E-34,0.707106781186548)) ;
#60492 = DIRECTION('',(-1.1311821873082E-49,1.,5.60383084497428E-34)) ;
#60493 = DIRECTION('center_axis',(1.51760508056877E-16,5.60383084497428E-34,
-1.)) ;
#60494 = DIRECTION('ref_axis',(-1.,0.,0.)) ;
#60495 = DIRECTION('center_axis',(0.,-1.,-5.60383084497428E-34)) ;
#60496 = DIRECTION('ref_axis',(1.,0.,0.)) ;
#60497 = DIRECTION('center_axis',(1.51760508056877E-16,5.60383084497428E-34,
-1.)) ;
#60498 = DIRECTION('ref_axis',(1.,2.24153233798966E-35,1.51760508056877E-16)) ;
#60499 = DIRECTION('center_axis',(1.51760508056877E-16,5.60383084497428E-34,
-1.)) ;
#60500 = DIRECTION('ref_axis',(1.,2.24153233798966E-35,1.51760508056877E-16)) ;
#60501 = DIRECTION('center_axis',(0.,0.,1.)) ;
#60502 = DIRECTION('ref_axis',(1.,0.,0.)) ;
#60503 = DIRECTION('',(0.,0.,1.)) ;
#60504 = DIRECTION('center_axis',(1.51760508056877E-16,5.60383084497428E-34,
-1.)) ;
#60505 = DIRECTION('ref_axis',(-1.,0.,0.)) ;
#60506 = DIRECTION('center_axis',(0.,-1.,-5.60383084497428E-34)) ;
#60507 = DIRECTION('ref_axis',(1.,0.,0.)) ;
#60508 = DIRECTION('center_axis',(1.51760508056877E-16,5.60383084497428E-34,
-1.)) ;
#60509 = DIRECTION('ref_axis',(1.,2.80191542248707E-35,1.51760508056877E-16)) ;
#60510 = DIRECTION('center_axis',(1.51760508056877E-16,5.60383084497428E-34,
-1.)) ;
#60511 = DIRECTION('ref_axis',(1.,2.80191542248707E-35,1.51760508056877E-16)) ;
#60512 = DIRECTION('center_axis',(0.,0.,1.)) ;
#60513 = DIRECTION('ref_axis',(1.,0.,0.)) ;
#60514 = DIRECTION('',(0.,0.,1.)) ;
#60515 = DIRECTION('center_axis',(0.,1.,5.60383084497428E-34)) ;
#60516 = DIRECTION('ref_axis',(0.707106781186548,3.96250679110365E-34,-0.707106781186548)) ;
#60517 = DIRECTION('center_axis',(0.,1.,0.)) ;
#60518 = DIRECTION('ref_axis',(1.,0.,0.)) ;
#60519 = DIRECTION('center_axis',(1.51760508056877E-16,5.60383084497428E-34,
-1.)) ;
#60520 = DIRECTION('ref_axis',(-1.,0.,0.)) ;
#60521 = DIRECTION('center_axis',(-0.707106781186548,0.707106781186548,0.)) ;
#60522 = DIRECTION('ref_axis',(0.707106781186547,0.707106781186547,0.)) ;
#60523 = DIRECTION('center_axis',(-1.51760508056877E-16,-5.60383084497428E-34,
1.)) ;
#60524 = DIRECTION('ref_axis',(-0.923879532511284,-0.382683432365097,-1.40208427237262E-16)) ;
#60525 = DIRECTION('center_axis',(-0.707106781186615,0.70710678118648,-1.07310884363344E-16)) ;
#60526 = DIRECTION('ref_axis',(0.499999999999888,0.499999999999984,-0.707106781186638)) ;
#60527 = DIRECTION('center_axis',(-0.707106781186548,0.707106781186548,0.)) ;
#60528 = DIRECTION('ref_axis',(0.707106781186547,0.707106781186547,0.)) ;
#60529 = DIRECTION('center_axis',(-1.51760508056877E-16,-5.60383084497428E-34,
1.)) ;
#60530 = DIRECTION('ref_axis',(1.,0.,0.)) ;
#60531 = DIRECTION('center_axis',(0.,1.,0.)) ;
#60532 = DIRECTION('ref_axis',(1.,0.,0.)) ;
#60533 = DIRECTION('center_axis',(-6.83214169000096E-16,1.,-1.03124546314615E-31)) ;
#60534 = DIRECTION('ref_axis',(0.707106781186485,4.83105371902657E-16,-0.70710678118661)) ;
#60535 = DIRECTION('center_axis',(0.,1.,0.)) ;
#60536 = DIRECTION('ref_axis',(1.,0.,0.)) ;
#60537 = DIRECTION('center_axis',(-1.51760508056877E-16,-5.60383084497428E-34,
1.)) ;
#60538 = DIRECTION('ref_axis',(1.,0.,0.)) ;
#60539 = DIRECTION('center_axis',(0.999479573214818,0.0322580645161017,0.)) ;
#60540 = DIRECTION('ref_axis',(0.0322580645161017,-0.999479573214818,0.)) ;
#60541 = DIRECTION('center_axis',(1.51760508056877E-16,5.60383084497428E-34,
-1.)) ;
#60542 = DIRECTION('ref_axis',(-1.,0.,0.)) ;
#60543 = DIRECTION('center_axis',(0.,1.,0.)) ;
#60544 = DIRECTION('ref_axis',(1.,0.,0.)) ;
#60545 = DIRECTION('center_axis',(0.,1.,5.60383084497428E-34)) ;
#60546 = DIRECTION('ref_axis',(0.707106781186485,3.962506791104E-34,-0.70710678118661)) ;
#60547 = DIRECTION('center_axis',(0.,1.,0.)) ;
#60548 = DIRECTION('ref_axis',(1.,0.,0.)) ;
#60549 = DIRECTION('center_axis',(1.51760508056877E-16,5.60383084497428E-34,
-1.)) ;
#60550 = DIRECTION('ref_axis',(-1.,0.,0.)) ;
#60551 = DIRECTION('center_axis',(-0.999479573214819,0.0322580645160902,0.)) ;
#60552 = DIRECTION('ref_axis',(0.0322580645160902,0.999479573214818,0.)) ;
#60553 = DIRECTION('center_axis',(-1.51760508056877E-16,-5.60383084497428E-34,
1.)) ;
#60554 = DIRECTION('ref_axis',(1.,0.,0.)) ;
#60555 = DIRECTION('center_axis',(0.,1.,0.)) ;
#60556 = DIRECTION('ref_axis',(1.,0.,0.)) ;
#60557 = DIRECTION('center_axis',(-6.83214169000096E-16,1.,-1.03124546314615E-31)) ;
#60558 = DIRECTION('ref_axis',(0.70710678118661,4.83105371902742E-16,-0.707106781186485)) ;
#60559 = DIRECTION('center_axis',(0.,1.,0.)) ;
#60560 = DIRECTION('ref_axis',(1.,0.,0.)) ;
#60561 = DIRECTION('center_axis',(-1.51760508056877E-16,-5.60383084497428E-34,
1.)) ;
#60562 = DIRECTION('ref_axis',(1.,0.,0.)) ;
#60563 = DIRECTION('center_axis',(0.707106781186548,0.707106781186548,0.)) ;
#60564 = DIRECTION('ref_axis',(0.707106781186547,-0.707106781186547,0.)) ;
#60565 = DIRECTION('center_axis',(0.707106781186521,0.707106781186574,1.0731088436333E-16)) ;
#60566 = DIRECTION('ref_axis',(0.499999999999986,-0.499999999999948,-0.707106781186594)) ;
#60567 = DIRECTION('center_axis',(0.707106781186548,0.707106781186548,0.)) ;
#60568 = DIRECTION('ref_axis',(0.707106781186547,-0.707106781186547,0.)) ;
#60569 = DIRECTION('center_axis',(1.51760508056877E-16,5.60383084497428E-34,
-1.)) ;
#60570 = DIRECTION('ref_axis',(-1.,0.,0.)) ;
#60571 = DIRECTION('center_axis',(0.,1.,0.)) ;
#60572 = DIRECTION('ref_axis',(1.,0.,0.)) ;
#60573 = DIRECTION('center_axis',(-5.23472275150178E-15,1.,-7.93863801220309E-31)) ;
#60574 = DIRECTION('ref_axis',(0.707106781186548,3.70150795521841E-15,-0.707106781186548)) ;
#60575 = DIRECTION('center_axis',(0.,1.,0.)) ;
#60576 = DIRECTION('ref_axis',(1.,0.,0.)) ;
#60577 = DIRECTION('center_axis',(-1.51760508056877E-16,-5.60383084497428E-34,
1.)) ;
#60578 = DIRECTION('ref_axis',(1.,0.,0.)) ;
#60579 = DIRECTION('center_axis',(0.984807753012208,-0.173648177666931,0.)) ;
#60580 = DIRECTION('ref_axis',(-0.173648177666931,-0.984807753012208,0.)) ;
#60581 = DIRECTION('center_axis',(0.984807753012209,-0.173648177666924,1.49454924935485E-16)) ;
#60582 = DIRECTION('ref_axis',(-0.122787803968973,-0.696364240320047,-0.70710678118652)) ;
#60583 = DIRECTION('center_axis',(0.984807753012208,-0.173648177666931,0.)) ;
#60584 = DIRECTION('ref_axis',(-0.173648177666931,-0.984807753012208,4.44089209850038E-14)) ;
#60585 = DIRECTION('center_axis',(-1.51760508056877E-16,-5.60383084497428E-34,
1.)) ;
#60586 = DIRECTION('ref_axis',(1.,0.,0.)) ;
#60587 = DIRECTION('center_axis',(0.573576436350949,-0.81915204428906,0.)) ;
#60588 = DIRECTION('ref_axis',(-0.81915204428906,-0.573576436350949,0.)) ;
#60589 = DIRECTION('center_axis',(0.573576436351042,-0.819152044288994,8.70462513900874E-17)) ;
#60590 = DIRECTION('ref_axis',(-0.579227965339616,-0.405579787672667,-0.707106781186493)) ;
#60591 = DIRECTION('center_axis',(0.573576436351074,-0.819152044288972,0.)) ;
#60592 = DIRECTION('ref_axis',(-0.819152044288972,-0.573576436351074,0.)) ;
#60593 = DIRECTION('center_axis',(-1.51760508056877E-16,-5.60383084497428E-34,
1.)) ;
#60594 = DIRECTION('ref_axis',(1.,0.,0.)) ;
#60595 = DIRECTION('center_axis',(0.,-1.,0.)) ;
#60596 = DIRECTION('ref_axis',(-1.,0.,0.)) ;
#60597 = DIRECTION('center_axis',(-5.25359141716359E-35,-1.,-5.60383084497428E-34)) ;
#60598 = DIRECTION('ref_axis',(-0.707106781186548,4.33399180276964E-34,-0.707106781186548)) ;
#60599 = DIRECTION('center_axis',(0.,-1.,0.)) ;
#60600 = DIRECTION('ref_axis',(-1.,0.,0.)) ;
#60601 = DIRECTION('center_axis',(1.51760508056877E-16,5.60383084497428E-34,
-1.)) ;
#60602 = DIRECTION('ref_axis',(-1.,0.,0.)) ;
#60603 = DIRECTION('center_axis',(1.,0.,0.)) ;
#60604 = DIRECTION('ref_axis',(0.,-1.,0.)) ;
#60605 = DIRECTION('center_axis',(1.,0.,1.51760508056877E-16)) ;
#60606 = DIRECTION('ref_axis',(1.07310884363343E-16,-0.707106781186485,-0.70710678118661)) ;
#60607 = DIRECTION('center_axis',(1.,0.,0.)) ;
#60608 = DIRECTION('ref_axis',(0.,-1.,0.)) ;
#60609 = DIRECTION('center_axis',(-1.51760508056877E-16,-5.60383084497428E-34,
1.)) ;
#60610 = DIRECTION('ref_axis',(1.,0.,0.)) ;
#60611 = DIRECTION('center_axis',(0.,0.,1.)) ;
#60612 = DIRECTION('ref_axis',(-0.923879532511279,-0.382683432365108,0.)) ;
#60613 = DIRECTION('center_axis',(-1.51760508056877E-16,-5.60383084497428E-34,
1.)) ;
#60614 = DIRECTION('ref_axis',(1.,0.,0.)) ;
#60615 = DIRECTION('center_axis',(-1.,0.,0.)) ;
#60616 = DIRECTION('ref_axis',(0.,0.,-1.)) ;
#60617 = DIRECTION('center_axis',(1.51760508056877E-16,5.60383084497428E-34,
-1.)) ;
#60618 = DIRECTION('ref_axis',(-0.70710678118657,-0.707106781186525,-1.07310884363337E-16)) ;
#60619 = DIRECTION('center_axis',(1.,0.,1.51760508056877E-16)) ;
#60620 = DIRECTION('ref_axis',(1.07310884363343E-16,-0.707106781186485,-0.70710678118661)) ;
#60621 = DIRECTION('center_axis',(-1.,0.,0.)) ;
#60622 = DIRECTION('ref_axis',(0.,0.,-1.)) ;
#60623 = DIRECTION('',(-1.,0.,-1.51760508056877E-16)) ;
#60624 = DIRECTION('center_axis',(-1.51760508056877E-16,-5.60383084497428E-34,
1.)) ;
#60625 = DIRECTION('ref_axis',(1.,0.,0.)) ;
#60626 = DIRECTION('center_axis',(0.,-1.,0.)) ;
#60627 = DIRECTION('ref_axis',(0.,0.,-1.)) ;
#60628 = DIRECTION('center_axis',(1.51760508056877E-16,5.60383084497428E-34,
-1.)) ;
#60629 = DIRECTION('ref_axis',(0.707106781186544,-0.707106781186551,1.07310884363333E-16)) ;
#60630 = DIRECTION('center_axis',(2.33146835171284E-14,-1.,3.53768783266021E-30)) ;
#60631 = DIRECTION('ref_axis',(0.707106781186548,1.64859708161797E-14,-0.707106781186548)) ;
#60632 = DIRECTION('',(2.33146835171284E-14,-1.,3.53768783266021E-30)) ;
#60633 = DIRECTION('center_axis',(-1.4923676700635E-16,0.,1.)) ;
#60634 = DIRECTION('ref_axis',(1.,0.,0.)) ;
#60635 = DIRECTION('center_axis',(0.,-1.,0.)) ;
#60636 = DIRECTION('ref_axis',(-1.,0.,0.)) ;
#60637 = DIRECTION('center_axis',(-1.4923676700635E-16,0.,1.)) ;
#60638 = DIRECTION('ref_axis',(1.,0.,1.4923676700635E-16)) ;
#60639 = DIRECTION('center_axis',(-1.4923676700635E-16,0.,1.)) ;
#60640 = DIRECTION('ref_axis',(1.,0.,1.4923676700635E-16)) ;
#60641 = DIRECTION('center_axis',(1.4923676700635E-16,0.,-1.)) ;
#60642 = DIRECTION('ref_axis',(1.,0.,1.4923676700635E-16)) ;
#60643 = DIRECTION('center_axis',(1.4923676700635E-16,0.,-1.)) ;
#60644 = DIRECTION('ref_axis',(-1.,0.,0.)) ;
#60645 = DIRECTION('center_axis',(-1.4923676700635E-16,0.,1.)) ;
#60646 = DIRECTION('ref_axis',(1.,0.,1.4923676700635E-16)) ;
#60647 = DIRECTION('center_axis',(0.,1.,0.)) ;
#60648 = DIRECTION('ref_axis',(1.,0.,0.)) ;
#60649 = DIRECTION('center_axis',(-1.4923676700635E-16,0.,1.)) ;
#60650 = DIRECTION('ref_axis',(1.,0.,1.4923676700635E-16)) ;
#60651 = DIRECTION('center_axis',(0.,0.,-1.)) ;
#60652 = DIRECTION('ref_axis',(1.,0.,0.)) ;
#60653 = DIRECTION('center_axis',(0.,0.,-1.)) ;
#60654 = DIRECTION('ref_axis',(1.,0.,0.)) ;
#60655 = DIRECTION('',(0.,0.,-1.)) ;
#60656 = DIRECTION('center_axis',(0.,0.,1.)) ;
#60657 = DIRECTION('ref_axis',(1.,0.,0.)) ;
#60658 = DIRECTION('center_axis',(0.,-1.,0.)) ;
#60659 = DIRECTION('ref_axis',(-1.,0.,0.)) ;
#60660 = DIRECTION('center_axis',(0.,0.,1.)) ;
#60661 = DIRECTION('ref_axis',(1.,0.,0.)) ;
#60662 = DIRECTION('center_axis',(0.,0.,1.)) ;
#60663 = DIRECTION('ref_axis',(1.,0.,0.)) ;
#60664 = DIRECTION('center_axis',(0.,0.,1.)) ;
#60665 = DIRECTION('ref_axis',(1.,0.,0.)) ;
#60666 = DIRECTION('center_axis',(0.,0.,-1.)) ;
#60667 = DIRECTION('ref_axis',(1.,0.,0.)) ;
#60668 = DIRECTION('center_axis',(0.,-1.,0.)) ;
#60669 = DIRECTION('ref_axis',(-1.,0.,0.)) ;
#60670 = DIRECTION('center_axis',(0.,0.,1.)) ;
#60671 = DIRECTION('ref_axis',(1.,0.,0.)) ;
#60672 = DIRECTION('center_axis',(0.,0.,1.)) ;
#60673 = DIRECTION('ref_axis',(1.,0.,0.)) ;
#60674 = DIRECTION('center_axis',(0.,0.,-1.)) ;
#60675 = DIRECTION('ref_axis',(1.,0.,0.)) ;
#60676 = DIRECTION('',(0.,0.,-1.)) ;
#60677 = DIRECTION('center_axis',(-1.4923676700635E-16,0.,1.)) ;
#60678 = DIRECTION('ref_axis',(1.,0.,1.4923676700635E-16)) ;
#60679 = DIRECTION('center_axis',(-1.4923676700635E-16,0.,1.)) ;
#60680 = DIRECTION('ref_axis',(1.,0.,1.4923676700635E-16)) ;
#60681 = DIRECTION('center_axis',(1.4923676700635E-16,0.,-1.)) ;
#60682 = DIRECTION('ref_axis',(-1.,0.,0.)) ;
#60683 = DIRECTION('center_axis',(0.,1.,0.)) ;
#60684 = DIRECTION('ref_axis',(1.,0.,0.)) ;
#60685 = DIRECTION('center_axis',(1.4923676700635E-16,0.,-1.)) ;
#60686 = DIRECTION('ref_axis',(1.,0.,1.4923676700635E-16)) ;
#60687 = DIRECTION('center_axis',(-1.4923676700635E-16,0.,1.)) ;
#60688 = DIRECTION('ref_axis',(1.,0.,1.4923676700635E-16)) ;
#60689 = DIRECTION('center_axis',(-1.4923676700635E-16,0.,1.)) ;
#60690 = DIRECTION('ref_axis',(1.,0.,1.4923676700635E-16)) ;
#60691 = DIRECTION('center_axis',(-1.4923676700635E-16,0.,1.)) ;
#60692 = DIRECTION('ref_axis',(1.,0.,0.)) ;
#60693 = DIRECTION('center_axis',(1.4923676700635E-16,0.,-1.)) ;
#60694 = DIRECTION('ref_axis',(1.,0.,1.4923676700635E-16)) ;
#60695 = DIRECTION('center_axis',(0.,-1.,0.)) ;
#60696 = DIRECTION('ref_axis',(-1.,0.,0.)) ;
#60697 = DIRECTION('center_axis',(0.,0.,1.)) ;
#60698 = DIRECTION('ref_axis',(1.,0.,0.)) ;
#60699 = DIRECTION('center_axis',(-1.4923676700635E-16,0.,1.)) ;
#60700 = DIRECTION('ref_axis',(1.,0.,1.4923676700635E-16)) ;
#60701 = DIRECTION('',(0.,0.,1.)) ;
#60702 = DIRECTION('center_axis',(0.,0.,1.)) ;
#60703 = DIRECTION('ref_axis',(1.,0.,0.)) ;
#60704 = DIRECTION('center_axis',(0.,0.,-1.)) ;
#60705 = DIRECTION('ref_axis',(1.,0.,0.)) ;
#60706 = DIRECTION('center_axis',(0.,-1.,0.)) ;
#60707 = DIRECTION('ref_axis',(-1.,0.,0.)) ;
#60708 = DIRECTION('center_axis',(0.,0.,1.)) ;
#60709 = DIRECTION('ref_axis',(1.,0.,0.)) ;
#60710 = DIRECTION('center_axis',(0.,0.,1.)) ;
#60711 = DIRECTION('ref_axis',(1.,0.,0.)) ;
#60712 = DIRECTION('center_axis',(0.,0.,-1.)) ;
#60713 = DIRECTION('ref_axis',(1.,0.,0.)) ;
#60714 = DIRECTION('',(0.,0.,-1.)) ;
#60715 = DIRECTION('center_axis',(-1.4923676700635E-16,0.,1.)) ;
#60716 = DIRECTION('ref_axis',(1.,0.,1.4923676700635E-16)) ;
#60717 = DIRECTION('center_axis',(-1.4923676700635E-16,0.,1.)) ;
#60718 = DIRECTION('ref_axis',(1.,0.,1.4923676700635E-16)) ;
#60719 = DIRECTION('center_axis',(-1.4923676700635E-16,0.,1.)) ;
#60720 = DIRECTION('ref_axis',(1.,0.,0.)) ;
#60721 = DIRECTION('center_axis',(0.,-1.,0.)) ;
#60722 = DIRECTION('ref_axis',(-1.,0.,0.)) ;
#60723 = DIRECTION('center_axis',(-1.4923676700635E-16,0.,1.)) ;
#60724 = DIRECTION('ref_axis',(1.,0.,1.4923676700635E-16)) ;
#60725 = DIRECTION('center_axis',(-1.4923676700635E-16,0.,1.)) ;
#60726 = DIRECTION('ref_axis',(1.,0.,1.4923676700635E-16)) ;
#60727 = DIRECTION('center_axis',(1.4923676700635E-16,0.,-1.)) ;
#60728 = DIRECTION('ref_axis',(1.,0.,1.4923676700635E-16)) ;
#60729 = DIRECTION('center_axis',(1.4923676700635E-16,0.,-1.)) ;
#60730 = DIRECTION('ref_axis',(-1.,0.,0.)) ;
#60731 = DIRECTION('center_axis',(0.,1.,0.)) ;
#60732 = DIRECTION('ref_axis',(1.,0.,0.)) ;
#60733 = DIRECTION('center_axis',(-1.4923676700635E-16,0.,1.)) ;
#60734 = DIRECTION('ref_axis',(-1.,0.,0.)) ;
#60735 = DIRECTION('center_axis',(0.,1.,0.)) ;
#60736 = DIRECTION('ref_axis',(1.,0.,0.)) ;
#60737 = DIRECTION('center_axis',(-1.4923676700635E-16,0.,1.)) ;
#60738 = DIRECTION('ref_axis',(-1.,0.,0.)) ;
#60739 = DIRECTION('center_axis',(0.,1.,0.)) ;
#60740 = DIRECTION('ref_axis',(1.,0.,0.)) ;
#60741 = DIRECTION('center_axis',(-1.4923676700635E-16,0.,1.)) ;
#60742 = DIRECTION('ref_axis',(-1.,0.,0.)) ;
#60743 = DIRECTION('center_axis',(0.,1.,0.)) ;
#60744 = DIRECTION('ref_axis',(1.,0.,0.)) ;
#60745 = DIRECTION('center_axis',(-1.4923676700635E-16,0.,1.)) ;
#60746 = DIRECTION('ref_axis',(1.,0.,1.4923676700635E-16)) ;
#60747 = DIRECTION('center_axis',(-2.01858731750028E-16,0.,1.)) ;
#60748 = DIRECTION('ref_axis',(0.707106781186579,-0.707106781186516,1.42735678062167E-16)) ;
#60749 = DIRECTION('',(2.01858731750028E-16,0.,-1.)) ;
#60750 = DIRECTION('',(-2.01858731750028E-16,0.,1.)) ;
#60751 = DIRECTION('center_axis',(0.,-1.,0.)) ;
#60752 = DIRECTION('ref_axis',(1.,0.,2.24978329294248E-16)) ;
#60753 = DIRECTION('',(0.,0.,1.)) ;
#60754 = DIRECTION('center_axis',(0.,0.,1.)) ;
#60755 = DIRECTION('ref_axis',(-0.707106781186574,-0.707106781186521,0.)) ;
#60756 = DIRECTION('center_axis',(0.707106781186551,0.707106781186544,0.)) ;
#60757 = DIRECTION('ref_axis',(0.,0.,-1.)) ;
#60758 = DIRECTION('center_axis',(-1.,3.73034936274055E-14,0.)) ;
#60759 = DIRECTION('ref_axis',(-3.73034936274055E-14,-1.,-5.56705278699598E-30)) ;
#60760 = DIRECTION('center_axis',(0.707106781186532,-0.707106781186563,0.)) ;
#60761 = DIRECTION('ref_axis',(0.,0.,-1.)) ;
#60762 = DIRECTION('center_axis',(0.,1.,0.)) ;
#60763 = DIRECTION('ref_axis',(-1.,0.,-1.4923676700635E-16)) ;
#60764 = DIRECTION('center_axis',(0.,1.,0.)) ;
#60765 = DIRECTION('ref_axis',(-1.,0.,-1.4923676700635E-16)) ;
#60766 = DIRECTION('center_axis',(0.863778900898434,-0.503871025524085,0.)) ;
#60767 = DIRECTION('ref_axis',(0.503871025524085,0.863778900898434,0.)) ;
#60768 = DIRECTION('center_axis',(-0.503871025524087,0.863778900898433,0.)) ;
#60769 = DIRECTION('ref_axis',(0.863778900898433,0.503871025524087,0.)) ;
#60770 = DIRECTION('center_axis',(0.,0.,1.)) ;
#60771 = DIRECTION('ref_axis',(1.,0.,0.)) ;
#60772 = DIRECTION('center_axis',(0.503871025524087,0.863778900898433,0.)) ;
#60773 = DIRECTION('ref_axis',(-0.863778900898433,0.503871025524087,0.)) ;
#60774 = DIRECTION('center_axis',(0.503871025524087,0.863778900898433,0.)) ;
#60775 = DIRECTION('ref_axis',(-0.863778900898433,0.503871025524087,0.)) ;
#60776 = DIRECTION('center_axis',(-0.863778900898434,-0.503871025524085,0.)) ;
#60777 = DIRECTION('ref_axis',(-0.503871025524085,0.863778900898434,0.)) ;
#60778 = DIRECTION('center_axis',(-0.863778900898434,-0.503871025524085,0.)) ;
#60779 = DIRECTION('ref_axis',(-0.503871025524085,0.863778900898434,0.)) ;
#60780 = DIRECTION('center_axis',(-8.88178419700128E-15,8.88178419700113E-15,
1.)) ;
#60781 = DIRECTION('ref_axis',(0.,1.,-8.88178419700113E-15)) ;
#60782 = DIRECTION('center_axis',(0.863778900898434,-0.503871025524085,0.)) ;
#60783 = DIRECTION('ref_axis',(0.503871025524085,0.863778900898434,0.)) ;
#60784 = DIRECTION('center_axis',(0.863778900898434,-0.503871025524085,0.)) ;
#60785 = DIRECTION('ref_axis',(0.503871025524085,0.863778900898434,0.)) ;
#60786 = DIRECTION('center_axis',(-0.503871025524087,0.863778900898433,0.)) ;
#60787 = DIRECTION('ref_axis',(0.863778900898433,0.503871025524087,0.)) ;
#60788 = DIRECTION('center_axis',(-0.503871025524087,0.863778900898433,0.)) ;
#60789 = DIRECTION('ref_axis',(0.863778900898433,0.503871025524087,0.)) ;
#60790 = DIRECTION('center_axis',(0.,0.,1.)) ;
#60791 = DIRECTION('ref_axis',(1.,0.,0.)) ;
#60792 = DIRECTION('center_axis',(0.503871025524087,0.863778900898433,0.)) ;
#60793 = DIRECTION('ref_axis',(-0.863778900898433,0.503871025524087,0.)) ;
#60794 = DIRECTION('center_axis',(0.503871025524087,0.863778900898433,0.)) ;
#60795 = DIRECTION('ref_axis',(-0.863778900898433,0.503871025524087,0.)) ;
#60796 = DIRECTION('center_axis',(0.,-8.88178419700113E-15,1.)) ;
#60797 = DIRECTION('ref_axis',(0.,1.,8.88178419700113E-15)) ;
#60798 = DIRECTION('center_axis',(0.,-1.,-5.60383084497428E-34)) ;
#60799 = DIRECTION('ref_axis',(-0.707106781186545,-3.96250679110367E-34,0.70710678118655)) ;
#60800 = DIRECTION('',(0.,-1.,-5.60383084497428E-34)) ;
#60801 = DIRECTION('center_axis',(0.,1.,0.)) ;
#60802 = DIRECTION('ref_axis',(-1.,0.,0.)) ;
#60803 = DIRECTION('center_axis',(1.,0.,0.)) ;
#60804 = DIRECTION('ref_axis',(0.,0.97854978498675,0.206010481049835)) ;
#60805 = DIRECTION('center_axis',(0.,-0.402044149173841,-0.915620282712808)) ;
#60806 = DIRECTION('ref_axis',(0.,-0.915620282712808,0.402044149173841)) ;
#60807 = DIRECTION('center_axis',(-1.,3.19495806435525E-17,-1.51760508056877E-16)) ;
#60808 = DIRECTION('ref_axis',(-9.77165742124407E-17,0.630075201444312,0.77653412064436)) ;
#60809 = DIRECTION('center_axis',(1.,0.,0.)) ;
#60810 = DIRECTION('ref_axis',(0.,0.97854978498675,0.206010481049835)) ;
#60811 = DIRECTION('center_axis',(0.,-1.,0.)) ;
#60812 = DIRECTION('ref_axis',(1.,0.,7.40148683083442E-15)) ;
#60813 = DIRECTION('center_axis',(0.,-0.402044149173841,-0.915620282712808)) ;
#60814 = DIRECTION('ref_axis',(0.,-0.915620282712808,0.402044149173841)) ;
#60815 = DIRECTION('center_axis',(0.,1.,5.60383084497428E-34)) ;
#60816 = DIRECTION('ref_axis',(0.707106781186545,-3.96250679110367E-34,0.70710678118655)) ;
#60817 = DIRECTION('',(0.,1.,5.60383084497428E-34)) ;
#60818 = DIRECTION('center_axis',(-1.,0.,-1.51760508056877E-16)) ;
#60819 = DIRECTION('ref_axis',(-1.07310884363335E-16,0.70710678118654,0.707106781186555)) ;
#60820 = DIRECTION('center_axis',(0.,-1.,-5.60383084497428E-34)) ;
#60821 = DIRECTION('ref_axis',(-0.70710678118655,-3.96250679110364E-34,0.707106781186545)) ;
#60822 = DIRECTION('',(0.,-1.,-5.60383084497428E-34)) ;
#60823 = DIRECTION('center_axis',(0.,1.,0.)) ;
#60824 = DIRECTION('ref_axis',(-1.,0.,0.)) ;
#60825 = DIRECTION('center_axis',(1.,0.,0.)) ;
#60826 = DIRECTION('ref_axis',(0.,0.978549784986751,0.206010481049832)) ;
#60827 = DIRECTION('center_axis',(0.,-0.402044149173841,-0.915620282712808)) ;
#60828 = DIRECTION('ref_axis',(0.,-0.915620282712808,0.402044149173841)) ;
#60829 = DIRECTION('center_axis',(-1.,3.19495806435525E-17,-1.51760508056877E-16)) ;
#60830 = DIRECTION('ref_axis',(-9.7716574212441E-17,0.63007520144431,0.776534120644362)) ;
#60831 = DIRECTION('center_axis',(1.,0.,0.)) ;
#60832 = DIRECTION('ref_axis',(0.,0.978549784986751,0.206010481049832)) ;
#60833 = DIRECTION('center_axis',(0.,-1.,0.)) ;
#60834 = DIRECTION('ref_axis',(1.,0.,3.70074341541719E-15)) ;
#60835 = DIRECTION('center_axis',(0.,-0.402044149173847,-0.915620282712805)) ;
#60836 = DIRECTION('ref_axis',(0.,-0.915620282712805,0.402044149173847)) ;
#60837 = DIRECTION('center_axis',(0.,1.,5.60383084497428E-34)) ;
#60838 = DIRECTION('ref_axis',(0.707106781186547,-3.96250679110365E-34,0.707106781186547)) ;
#60839 = DIRECTION('',(0.,1.,5.60383084497428E-34)) ;
#60840 = DIRECTION('center_axis',(-1.,0.,-1.51760508056877E-16)) ;
#60841 = DIRECTION('ref_axis',(-1.07310884363335E-16,0.70710678118654,0.707106781186555)) ;
#60842 = DIRECTION('center_axis',(0.,0.206010481049838,-0.97854978498675)) ;
#60843 = DIRECTION('ref_axis',(-0.707106781186557,-0.691939188692759,-0.145671408145841)) ;
#60844 = DIRECTION('center_axis',(0.,0.206010481049834,-0.978549784986751)) ;
#60845 = DIRECTION('ref_axis',(0.,-0.978549784986751,-0.206010481049834)) ;
#60846 = DIRECTION('',(0.,-0.206010481049838,0.97854978498675)) ;
#60847 = DIRECTION('center_axis',(0.,-0.206010481049838,0.97854978498675)) ;
#60848 = DIRECTION('ref_axis',(0.707106781186556,-0.691939188692761,-0.145671408145841)) ;
#60849 = DIRECTION('',(0.,0.206010481049838,-0.97854978498675)) ;
#60850 = DIRECTION('center_axis',(0.,0.206010481049843,-0.978549784986749)) ;
#60851 = DIRECTION('ref_axis',(1.,0.,0.)) ;
#60852 = DIRECTION('center_axis',(-1.,0.,0.)) ;
#60853 = DIRECTION('ref_axis',(0.,-1.,0.)) ;
#60854 = DIRECTION('',(0.,0.,1.)) ;
#60855 = DIRECTION('center_axis',(0.,0.,1.)) ;
#60856 = DIRECTION('ref_axis',(-0.707106781186523,0.707106781186573,0.)) ;
#60857 = DIRECTION('center_axis',(0.,-0.994505452921406,-0.104684784518042)) ;
#60858 = DIRECTION('ref_axis',(0.,0.104684784518042,-0.994505452921406)) ;
#60859 = DIRECTION('center_axis',(0.,0.,1.)) ;
#60860 = DIRECTION('ref_axis',(0.707106781186523,0.707106781186573,0.)) ;
#60861 = DIRECTION('',(0.,0.,-1.)) ;
#60862 = DIRECTION('center_axis',(0.,-0.994505452921406,-0.104684784518042)) ;
#60863 = DIRECTION('ref_axis',(0.,0.104684784518042,-0.994505452921406)) ;
#60864 = DIRECTION('center_axis',(1.,0.,0.)) ;
#60865 = DIRECTION('ref_axis',(0.,1.,0.)) ;
#60866 = DIRECTION('',(0.,-0.206010481049838,0.97854978498675)) ;
#60867 = DIRECTION('center_axis',(0.,0.206010481049838,-0.97854978498675)) ;
#60868 = DIRECTION('ref_axis',(-0.707106781186556,-0.691939188692761,-0.145671408145841)) ;
#60869 = DIRECTION('center_axis',(0.,0.206010481049834,-0.978549784986751)) ;
#60870 = DIRECTION('ref_axis',(0.,-0.978549784986751,-0.206010481049834)) ;
#60871 = DIRECTION('center_axis',(0.,-0.206010481049838,0.97854978498675)) ;
#60872 = DIRECTION('ref_axis',(0.707106781186543,-0.691939188692773,-0.145671408145844)) ;
#60873 = DIRECTION('',(0.,0.206010481049838,-0.97854978498675)) ;
#60874 = DIRECTION('center_axis',(0.,0.206010481049843,-0.978549784986749)) ;
#60875 = DIRECTION('ref_axis',(1.,0.,0.)) ;
#60876 = DIRECTION('center_axis',(-1.,0.,0.)) ;
#60877 = DIRECTION('ref_axis',(0.,-1.,0.)) ;
#60878 = DIRECTION('',(0.,0.,1.)) ;
#60879 = DIRECTION('center_axis',(0.,0.,1.)) ;
#60880 = DIRECTION('ref_axis',(-0.70710678118651,0.707106781186585,0.)) ;
#60881 = DIRECTION('center_axis',(0.,-0.994505452921406,-0.104684784518042)) ;
#60882 = DIRECTION('ref_axis',(0.,0.104684784518042,-0.994505452921406)) ;
#60883 = DIRECTION('center_axis',(0.,-1.,0.)) ;
#60884 = DIRECTION('ref_axis',(1.,0.,1.4923676700635E-16)) ;
#60885 = DIRECTION('',(0.,0.,1.)) ;
#60886 = DIRECTION('',(-1.,0.,-1.4923676700635E-16)) ;
#60887 = DIRECTION('center_axis',(-1.,0.,0.)) ;
#60888 = DIRECTION('ref_axis',(0.,-1.,0.)) ;
#60889 = DIRECTION('',(0.,1.,0.)) ;
#60890 = DIRECTION('center_axis',(-1.4923676700635E-16,0.,1.)) ;
#60891 = DIRECTION('ref_axis',(1.,0.,1.4923676700635E-16)) ;
#60892 = DIRECTION('center_axis',(3.55271367880051E-14,-1.,0.)) ;
#60893 = DIRECTION('ref_axis',(1.,3.55271367880051E-14,1.4923676700635E-16)) ;
#60894 = DIRECTION('',(-2.01858731750028E-16,-7.1714627747365E-30,1.)) ;
#60895 = DIRECTION('',(0.,0.,1.)) ;
#60896 = DIRECTION('center_axis',(-1.,0.,0.)) ;
#60897 = DIRECTION('ref_axis',(0.,-1.,0.)) ;
#60898 = DIRECTION('center_axis',(-1.,0.,-2.01858731750028E-16)) ;
#60899 = DIRECTION('ref_axis',(0.,-1.,0.)) ;
#60900 = DIRECTION('center_axis',(0.,1.,0.)) ;
#60901 = DIRECTION('ref_axis',(-1.,0.,-1.4923676700635E-16)) ;
#60902 = DIRECTION('',(0.,0.,1.)) ;
#60903 = DIRECTION('',(0.,0.,1.)) ;
#60904 = DIRECTION('center_axis',(1.,-7.105427357601E-15,0.)) ;
#60905 = DIRECTION('ref_axis',(7.105427357601E-15,1.,1.06039100704685E-30)) ;
#60906 = DIRECTION('center_axis',(1.,-7.105427357601E-15,0.)) ;
#60907 = DIRECTION('ref_axis',(7.105427357601E-15,1.,1.06039100704685E-30)) ;
#60908 = DIRECTION('center_axis',(0.,1.,0.)) ;
#60909 = DIRECTION('ref_axis',(-1.,0.,-1.4923676700635E-16)) ;
#60910 = DIRECTION('',(0.,0.,1.)) ;
#60911 = DIRECTION('center_axis',(1.,-3.17206578464323E-15,0.)) ;
#60912 = DIRECTION('ref_axis',(3.17206578464323E-15,1.,4.73388842431617E-31)) ;
#60913 = DIRECTION('center_axis',(0.,1.,0.)) ;
#60914 = DIRECTION('ref_axis',(-1.,0.,-1.4923676700635E-16)) ;
#60915 = DIRECTION('center_axis',(-1.,0.,0.)) ;
#60916 = DIRECTION('ref_axis',(0.,-1.,0.)) ;
#60917 = DIRECTION('center_axis',(1.,0.,0.)) ;
#60918 = DIRECTION('ref_axis',(0.,1.,0.)) ;
#60919 = DIRECTION('center_axis',(0.,1.,0.)) ;
#60920 = DIRECTION('ref_axis',(-1.,0.,-1.4923676700635E-16)) ;
#60921 = DIRECTION('center_axis',(0.,1.,0.)) ;
#60922 = DIRECTION('ref_axis',(-1.,0.,-1.4923676700635E-16)) ;
#60923 = DIRECTION('center_axis',(-1.,-2.33146835171284E-14,-2.01858731750028E-16)) ;
#60924 = DIRECTION('ref_axis',(2.33146835171284E-14,-1.,3.47940799187248E-30)) ;
#60925 = DIRECTION('center_axis',(0.,0.206010481049838,-0.97854978498675)) ;
#60926 = DIRECTION('ref_axis',(-0.707106781186557,-0.691939188692759,-0.145671408145841)) ;
#60927 = DIRECTION('center_axis',(0.,0.206010481049838,-0.97854978498675)) ;
#60928 = DIRECTION('ref_axis',(-0.707106781186556,-0.691939188692761,-0.145671408145841)) ;
#60929 = DIRECTION('',(0.,-0.206010481049838,0.97854978498675)) ;
#60930 = DIRECTION('center_axis',(0.,-0.206010481049838,0.97854978498675)) ;
#60931 = DIRECTION('ref_axis',(0.707106781186556,-0.691939188692761,-0.145671408145841)) ;
#60932 = DIRECTION('',(0.,0.206010481049838,-0.97854978498675)) ;
#60933 = DIRECTION('center_axis',(1.,0.,0.)) ;
#60934 = DIRECTION('ref_axis',(0.,1.,0.)) ;
#60935 = DIRECTION('center_axis',(-1.,0.,0.)) ;
#60936 = DIRECTION('ref_axis',(0.,-1.,0.)) ;
#60937 = DIRECTION('center_axis',(0.,-0.994505452921406,-0.104684784518042)) ;
#60938 = DIRECTION('ref_axis',(0.,0.104684784518042,-0.994505452921406)) ;
#60939 = DIRECTION('center_axis',(0.,0.,1.)) ;
#60940 = DIRECTION('ref_axis',(0.707106781186523,0.707106781186573,0.)) ;
#60941 = DIRECTION('',(0.,0.,-1.)) ;
#60942 = DIRECTION('center_axis',(1.,0.,0.)) ;
#60943 = DIRECTION('ref_axis',(0.,1.,0.)) ;
#60944 = DIRECTION('axis',(0.,0.,1.)) ;
#60945 = DIRECTION('refdir',(1.,0.,0.)) ;
#60946 = DIRECTION('center_axis',(-5.22457893941245E-15,-1.,-1.37458674256137E-32)) ;
#60947 = DIRECTION('ref_axis',(-0.707106781186548,3.69433519690296E-15,0.707106781186548)) ;
#60948 = DIRECTION('',(-5.22457893941245E-15,-1.,-1.37458674256137E-32)) ;
#60949 = DIRECTION('center_axis',(0.707106781186512,0.707106781186583,0.)) ;
#60950 = DIRECTION('ref_axis',(-0.707106781186583,0.707106781186512,6.13317366673383E-17)) ;
#60951 = DIRECTION('',(5.22457893941245E-15,1.,1.37458674256137E-32)) ;
#60952 = DIRECTION('center_axis',(-0.382683432365083,-0.92387953251129,0.)) ;
#60953 = DIRECTION('ref_axis',(-0.92387953251129,0.382683432365083,3.59196825968159E-32)) ;
#60954 = DIRECTION('center_axis',(-0.707106781186555,-0.70710678118654,-1.78455441078682E-18)) ;
#60955 = DIRECTION('ref_axis',(-0.499999999999962,0.499999999999972,0.707106781186594)) ;
#60956 = DIRECTION('',(0.707106781186555,0.70710678118654,1.78455441078682E-18)) ;
#60957 = DIRECTION('center_axis',(-0.923879532511372,-0.382683432364885,0.)) ;
#60958 = DIRECTION('ref_axis',(-0.382683432364885,0.923879532511372,4.66326540387932E-18)) ;
#60959 = DIRECTION('',(-0.707106781186555,-0.70710678118654,-1.78455441078682E-18)) ;
#60960 = DIRECTION('center_axis',(-1.,0.,-2.52374105052742E-18)) ;
#60961 = DIRECTION('ref_axis',(-1.78455441078696E-18,0.707106781186485,0.70710678118661)) ;
#60962 = DIRECTION('',(1.,0.,2.52374105052742E-18)) ;
#60963 = DIRECTION('center_axis',(-0.70710678118661,0.707106781186485,0.)) ;
#60964 = DIRECTION('ref_axis',(0.707106781186485,0.70710678118661,3.56910882157392E-18)) ;
#60965 = DIRECTION('',(-1.,0.,-2.52374105052742E-18)) ;
#60966 = DIRECTION('center_axis',(-0.816496580927762,-0.40824829046381,0.408248290463845)) ;
#60967 = DIRECTION('ref_axis',(0.577350269189543,-0.577350269189685,0.577350269189649)) ;
#60968 = DIRECTION('center_axis',(0.,-1.,0.)) ;
#60969 = DIRECTION('ref_axis',(0.,0.,1.)) ;
#60970 = DIRECTION('center_axis',(1.,0.,0.)) ;
#60971 = DIRECTION('ref_axis',(0.,-1.,0.)) ;
#60972 = DIRECTION('center_axis',(0.,0.,1.)) ;
#60973 = DIRECTION('ref_axis',(1.,0.,0.)) ;
#60974 = DIRECTION('center_axis',(1.,0.,2.52374105052742E-18)) ;
#60975 = DIRECTION('ref_axis',(-1.78455441078632E-18,-0.707106781186736,0.707106781186359)) ;
#60976 = DIRECTION('center_axis',(0.707106781186512,0.707106781186583,0.)) ;
#60977 = DIRECTION('ref_axis',(0.707106781186583,-0.707106781186512,-1.83995210001996E-16)) ;
#60978 = DIRECTION('',(1.,0.,2.52374105052742E-18)) ;
#60979 = DIRECTION('',(-1.,0.,-2.52374105052742E-18)) ;
#60980 = DIRECTION('center_axis',(0.,0.,-1.)) ;
#60981 = DIRECTION('ref_axis',(0.707106781186359,-0.707106781186736,0.)) ;
#60982 = DIRECTION('center_axis',(0.,0.,1.)) ;
#60983 = DIRECTION('ref_axis',(0.707106781186359,-0.707106781186736,0.)) ;
#60984 = DIRECTION('',(0.,0.,1.)) ;
#60985 = DIRECTION('',(0.,0.,-1.)) ;
#60986 = DIRECTION('center_axis',(-1.41426179436738E-51,1.,5.60383084497445E-34)) ;
#60987 = DIRECTION('ref_axis',(0.707106781186548,-3.96250679110377E-34,0.707106781186548)) ;
#60988 = DIRECTION('',(1.41426179436738E-51,-1.,-5.60383084497445E-34)) ;
#60989 = DIRECTION('',(-1.41426179436738E-51,1.,5.60383084497445E-34)) ;
#60990 = DIRECTION('center_axis',(-1.,5.22457893941245E-15,0.)) ;
#60991 = DIRECTION('ref_axis',(5.22457893941245E-15,1.,1.37458674256137E-32)) ;
#60992 = DIRECTION('',(0.,0.,-1.)) ;
#60993 = DIRECTION('',(5.22457893941245E-15,1.,1.37458674256137E-32)) ;
#60994 = DIRECTION('',(0.,0.,-1.)) ;
#60995 = DIRECTION('center_axis',(-0.707106781186512,-0.707106781186583,0.)) ;
#60996 = DIRECTION('ref_axis',(-0.707106781186583,0.707106781186512,-1.78455441078689E-18)) ;
#60997 = DIRECTION('',(-0.707106781186583,0.707106781186512,-1.78455441078689E-18)) ;
#60998 = DIRECTION('',(0.,0.,-1.)) ;
#60999 = DIRECTION('',(0.707106781186583,-0.707106781186512,1.78455441078689E-18)) ;
#61000 = DIRECTION('center_axis',(-0.70710678118654,0.707106781186555,0.)) ;
#61001 = DIRECTION('ref_axis',(0.707106781186555,0.70710678118654,1.78455441078682E-18)) ;
#61002 = DIRECTION('',(0.,0.,-1.)) ;
#61003 = DIRECTION('',(0.707106781186555,0.70710678118654,1.78455441078682E-18)) ;
#61004 = DIRECTION('center_axis',(0.,1.,0.)) ;
#61005 = DIRECTION('ref_axis',(1.,0.,2.52374105052742E-18)) ;
#61006 = DIRECTION('',(0.,0.,-1.)) ;
#61007 = DIRECTION('',(1.,0.,2.52374105052742E-18)) ;
#61008 = DIRECTION('center_axis',(1.,1.41426179436738E-51,0.)) ;
#61009 = DIRECTION('ref_axis',(1.41426179436738E-51,-1.,-5.60383084497445E-34)) ;
#61010 = DIRECTION('',(1.41426179436738E-51,-1.,-5.60383084497445E-34)) ;
#61011 = DIRECTION('center_axis',(0.,-1.,0.)) ;
#61012 = DIRECTION('ref_axis',(-1.,0.,-2.52374105052742E-18)) ;
#61013 = DIRECTION('',(-1.,0.,-2.52374105052742E-18)) ;
#61014 = DIRECTION('center_axis',(0.,0.,-1.)) ;
#61015 = DIRECTION('ref_axis',(-1.,0.,0.)) ;
#61016 = DIRECTION('center_axis',(2.52374105052742E-18,5.60383084497445E-34,
-1.)) ;
#61017 = DIRECTION('ref_axis',(1.,3.40207761657885E-68,2.52374105052742E-18)) ;
#61018 = DIRECTION('axis',(0.,0.,1.)) ;
#61019 = DIRECTION('refdir',(1.,0.,0.)) ;
#61020 = DIRECTION('center_axis',(-1.,0.,-2.52374105052742E-18)) ;
#61021 = DIRECTION('ref_axis',(-1.78455441078632E-18,-0.707106781186736,0.707106781186359)) ;
#61022 = DIRECTION('',(1.,0.,2.52374105052742E-18)) ;
#61023 = DIRECTION('center_axis',(-1.,0.,0.)) ;
#61024 = DIRECTION('ref_axis',(0.,-1.,0.)) ;
#61025 = DIRECTION('',(-1.,0.,-2.52374105052742E-18)) ;
#61026 = DIRECTION('center_axis',(0.,0.,-1.)) ;
#61027 = DIRECTION('ref_axis',(0.707106781186359,-0.707106781186736,0.)) ;
#61028 = DIRECTION('center_axis',(0.,0.,-1.)) ;
#61029 = DIRECTION('ref_axis',(1.,0.,0.)) ;
#61030 = DIRECTION('',(0.,0.,-1.)) ;
#61031 = DIRECTION('center_axis',(0.,0.,1.)) ;
#61032 = DIRECTION('ref_axis',(0.,-1.,0.)) ;
#61033 = DIRECTION('',(0.,0.,1.)) ;
#61034 = DIRECTION('center_axis',(-1.,0.,-2.52374105052742E-18)) ;
#61035 = DIRECTION('ref_axis',(1.78455441078632E-18,-0.707106781186736,-0.707106781186359)) ;
#61036 = DIRECTION('',(1.,0.,2.52374105052742E-18)) ;
#61037 = DIRECTION('center_axis',(-1.,0.,0.)) ;
#61038 = DIRECTION('ref_axis',(0.,0.,-1.)) ;
#61039 = DIRECTION('',(-1.,0.,-2.52374105052742E-18)) ;
#61040 = DIRECTION('center_axis',(-0.81649658092775,-0.408248290463875,-0.408248290463804)) ;
#61041 = DIRECTION('ref_axis',(0.57735026918959,-0.577350269189732,-0.577350269189555)) ;
#61042 = DIRECTION('center_axis',(3.36764187079272E-15,-1.,7.93867294829711E-33)) ;
#61043 = DIRECTION('ref_axis',(0.707106781186547,2.38128240344528E-15,-0.707106781186547)) ;
#61044 = DIRECTION('center_axis',(-0.81649658092775,-0.408248290463875,0.408248290463804)) ;
#61045 = DIRECTION('ref_axis',(0.577350269189602,-0.577350269189744,0.577350269189531)) ;
#61046 = DIRECTION('center_axis',(3.36764187079272E-15,-1.,7.93867294829711E-33)) ;
#61047 = DIRECTION('ref_axis',(0.707106781186547,2.38128240344528E-15,0.707106781186547)) ;
#61048 = DIRECTION('center_axis',(2.52374105052742E-18,5.60383084497445E-34,
-1.)) ;
#61049 = DIRECTION('ref_axis',(1.,3.40207761657885E-68,2.52374105052742E-18)) ;
#61050 = DIRECTION('',(3.36764187079272E-15,-1.,7.93867294829711E-33)) ;
#61051 = DIRECTION('center_axis',(-2.52374105052742E-18,-5.60383084497445E-34,
1.)) ;
#61052 = DIRECTION('ref_axis',(-0.707106781186548,0.707106781186548,-1.7845544107868E-18)) ;
#61053 = DIRECTION('',(1.41426179436738E-51,-1.,-5.60383084497445E-34)) ;
#61054 = DIRECTION('',(-1.,0.,-2.52374105052742E-18)) ;
#61055 = DIRECTION('',(-0.212265141871518,-0.977212110826644,-5.35702252137179E-19)) ;
#61056 = DIRECTION('',(1.41426179436738E-51,-1.,-5.60383084497445E-34)) ;
#61057 = DIRECTION('',(-1.,0.,-2.52374105052742E-18)) ;
#61058 = DIRECTION('center_axis',(2.52374105052742E-18,5.60383084497445E-34,
-1.)) ;
#61059 = DIRECTION('ref_axis',(0.422618261740848,-0.906307787036581,1.06657905585792E-18)) ;
#61060 = DIRECTION('',(-0.642787609686526,-0.766044443118989,-1.62222947733628E-18)) ;
#61061 = DIRECTION('center_axis',(2.52374105052742E-18,5.60383084497445E-34,
-1.)) ;
#61062 = DIRECTION('ref_axis',(0.939692620785894,-0.342020143325708,2.37154084195506E-18)) ;
#61063 = DIRECTION('',(-1.0449157878825E-14,-1.,-2.69313517667302E-32)) ;
#61064 = DIRECTION('center_axis',(2.52374105052742E-18,5.60383084497445E-34,
-1.)) ;
#61065 = DIRECTION('ref_axis',(0.939692620785894,0.342020143325708,2.37154084195506E-18)) ;
#61066 = DIRECTION('',(0.642787609686559,-0.766044443118961,1.62222947733637E-18)) ;
#61067 = DIRECTION('center_axis',(2.52374105052742E-18,5.60383084497445E-34,
-1.)) ;
#61068 = DIRECTION('ref_axis',(0.422618261740652,0.906307787036672,1.06657905585743E-18)) ;
#61069 = DIRECTION('',(1.,0.,2.52374105052742E-18)) ;
#61070 = DIRECTION('',(1.41426179436738E-51,-1.,-5.60383084497445E-34)) ;
#61071 = DIRECTION('',(1.,-5.00382208281761E-15,2.52374105052742E-18)) ;
#61072 = DIRECTION('',(1.41426179436738E-51,-1.,-5.60383084497445E-34)) ;
#61073 = DIRECTION('',(1.,0.,2.52374105052742E-18)) ;
#61074 = DIRECTION('',(7.65671051465623E-16,1.,2.49273854828173E-33)) ;
#61075 = DIRECTION('',(-1.,0.,-2.52374105052742E-18)) ;
#61076 = DIRECTION('',(-1.41426179436738E-51,1.,5.60383084497445E-34)) ;
#61077 = DIRECTION('',(0.445803505996966,-0.895130847441207,1.12509260855359E-18)) ;
#61078 = DIRECTION('center_axis',(2.52374105052742E-18,5.60383084497445E-34,
-1.)) ;
#61079 = DIRECTION('ref_axis',(1.,-1.41426179436738E-51,2.52374105052742E-18)) ;
#61080 = DIRECTION('',(1.41426179436738E-51,-1.,-5.60383084497445E-34)) ;
#61081 = DIRECTION('center_axis',(-2.52374105052742E-18,-5.60383084497445E-34,
1.)) ;
#61082 = DIRECTION('ref_axis',(1.73732004304105E-19,1.,5.60821539088498E-34)) ;
#61083 = DIRECTION('',(-1.41426179436738E-51,1.,5.60383084497445E-34)) ;
#61084 = DIRECTION('center_axis',(-2.52374105052742E-18,-5.60383084497445E-34,
1.)) ;
#61085 = DIRECTION('ref_axis',(1.73732004304105E-19,-1.,-5.59944629906392E-34)) ;
#61086 = DIRECTION('',(1.,0.,2.52374105052742E-18)) ;
#61087 = DIRECTION('',(1.41426179436738E-51,-1.,-5.60383084497445E-34)) ;
#61088 = DIRECTION('',(-1.,0.,-2.52374105052742E-18)) ;
#61089 = DIRECTION('',(-1.41426179436738E-51,1.,5.60383084497445E-34)) ;
#61090 = DIRECTION('',(-1.,0.,-2.52374105052742E-18)) ;
#61091 = DIRECTION('',(-1.41426179436738E-51,1.,5.60383084497445E-34)) ;
#61092 = DIRECTION('',(1.,0.,2.52374105052742E-18)) ;
#61093 = DIRECTION('',(1.41426179436738E-51,-1.,-5.60383084497445E-34)) ;
#61094 = DIRECTION('',(-1.,0.,-2.52374105052742E-18)) ;
#61095 = DIRECTION('',(-1.41426179436738E-51,1.,5.60383084497445E-34)) ;
#61096 = DIRECTION('',(1.,0.,2.52374105052742E-18)) ;
#61097 = DIRECTION('',(1.41426179436738E-51,-1.,-5.60383084497445E-34)) ;
#61098 = DIRECTION('',(-1.,0.,-2.52374105052742E-18)) ;
#61099 = DIRECTION('',(-1.41426179436738E-51,1.,5.60383084497445E-34)) ;
#61100 = DIRECTION('',(1.,0.,2.52374105052742E-18)) ;
#61101 = DIRECTION('',(1.41426179436738E-51,-1.,-5.60383084497445E-34)) ;
#61102 = DIRECTION('center_axis',(3.36764187079272E-15,-1.,7.93867294829711E-33)) ;
#61103 = DIRECTION('ref_axis',(0.707106781186548,2.38128240344528E-15,0.707106781186548)) ;
#61104 = DIRECTION('',(-3.36764187079272E-15,1.,-7.93867294829711E-33)) ;
#61105 = DIRECTION('center_axis',(0.,1.,0.)) ;
#61106 = DIRECTION('ref_axis',(0.,0.,1.)) ;
#61107 = DIRECTION('center_axis',(1.,3.36764187079272E-15,0.)) ;
#61108 = DIRECTION('ref_axis',(3.36764187079272E-15,-1.,7.93867294829711E-33)) ;
#61109 = DIRECTION('',(3.36764187079272E-15,-1.,7.93867294829711E-33)) ;
#61110 = DIRECTION('',(0.,0.,-1.)) ;
#61111 = DIRECTION('center_axis',(3.36764187079272E-15,-1.,7.93867294829711E-33)) ;
#61112 = DIRECTION('ref_axis',(0.707106781186548,2.38128240344528E-15,-0.707106781186548)) ;
#61113 = DIRECTION('',(-3.36764187079272E-15,1.,-7.93867294829711E-33)) ;
#61114 = DIRECTION('center_axis',(0.,1.,0.)) ;
#61115 = DIRECTION('ref_axis',(1.,0.,0.)) ;
#61116 = DIRECTION('center_axis',(2.52374105052742E-18,5.60383084497445E-34,
-1.)) ;
#61117 = DIRECTION('ref_axis',(1.,3.40207761657885E-68,2.52374105052742E-18)) ;
#61118 = DIRECTION('center_axis',(-2.52374105052742E-18,-5.60383084497445E-34,
1.)) ;
#61119 = DIRECTION('ref_axis',(1.,-1.41426179436738E-51,2.52374105052742E-18)) ;
#61120 = DIRECTION('',(-0.445803505996966,0.895130847441207,-1.12509260855359E-18)) ;
#61121 = DIRECTION('',(-1.41426179436738E-51,1.,5.60383084497445E-34)) ;
#61122 = DIRECTION('',(-1.,0.,-2.52374105052742E-18)) ;
#61123 = DIRECTION('',(7.65671051465623E-16,1.,2.49273854828173E-33)) ;
#61124 = DIRECTION('',(1.,0.,2.52374105052742E-18)) ;
#61125 = DIRECTION('',(1.41426179436738E-51,-1.,-5.60383084497445E-34)) ;
#61126 = DIRECTION('',(1.,-5.00382208281761E-15,2.52374105052742E-18)) ;
#61127 = DIRECTION('',(-1.41426179436738E-51,1.,5.60383084497445E-34)) ;
#61128 = DIRECTION('',(-1.,0.,-2.52374105052742E-18)) ;
#61129 = DIRECTION('center_axis',(-2.52374105052742E-18,-5.60383084497445E-34,
1.)) ;
#61130 = DIRECTION('ref_axis',(0.422618261740652,0.906307787036672,1.06657905585743E-18)) ;
#61131 = DIRECTION('',(-0.642787609686559,0.766044443118961,-1.62222947733637E-18)) ;
#61132 = DIRECTION('center_axis',(-2.52374105052742E-18,-5.60383084497445E-34,
1.)) ;
#61133 = DIRECTION('ref_axis',(0.939692620785894,0.342020143325708,2.37154084195506E-18)) ;
#61134 = DIRECTION('',(1.0449157878825E-14,1.,2.69313517667302E-32)) ;
#61135 = DIRECTION('center_axis',(-2.52374105052742E-18,-5.60383084497445E-34,
1.)) ;
#61136 = DIRECTION('ref_axis',(0.939692620785894,-0.342020143325708,2.37154084195506E-18)) ;
#61137 = DIRECTION('',(0.642787609686526,0.766044443118989,1.62222947733628E-18)) ;
#61138 = DIRECTION('center_axis',(-2.52374105052742E-18,-5.60383084497445E-34,
1.)) ;
#61139 = DIRECTION('ref_axis',(0.422618261740848,-0.906307787036581,1.06657905585792E-18)) ;
#61140 = DIRECTION('',(1.,0.,2.52374105052742E-18)) ;
#61141 = DIRECTION('',(-1.41426179436738E-51,1.,5.60383084497445E-34)) ;
#61142 = DIRECTION('',(0.212265141871518,0.977212110826644,5.35702252137179E-19)) ;
#61143 = DIRECTION('',(-1.,0.,-2.52374105052742E-18)) ;
#61144 = DIRECTION('',(1.41426179436738E-51,-1.,-5.60383084497445E-34)) ;
#61145 = DIRECTION('center_axis',(2.52374105052742E-18,5.60383084497445E-34,
-1.)) ;
#61146 = DIRECTION('ref_axis',(-0.707106781186548,0.707106781186548,-1.7845544107868E-18)) ;
#61147 = DIRECTION('center_axis',(-2.52374105052742E-18,-5.60383084497445E-34,
1.)) ;
#61148 = DIRECTION('ref_axis',(-1.,-3.40207761657885E-68,-2.52374105052742E-18)) ;
#61149 = DIRECTION('',(1.41426179436738E-51,-1.,-5.60383084497445E-34)) ;
#61150 = DIRECTION('center_axis',(-2.52374105052742E-18,-5.60383084497445E-34,
1.)) ;
#61151 = DIRECTION('ref_axis',(1.,3.40207761657885E-68,2.52374105052742E-18)) ;
#61152 = DIRECTION('',(-1.41426179436738E-51,1.,5.60383084497445E-34)) ;
#61153 = DIRECTION('',(-1.41426179436738E-51,1.,5.60383084497445E-34)) ;
#61154 = DIRECTION('',(-1.,0.,-2.52374105052742E-18)) ;
#61155 = DIRECTION('',(1.41426179436738E-51,-1.,-5.60383084497445E-34)) ;
#61156 = DIRECTION('',(1.,0.,2.52374105052742E-18)) ;
#61157 = DIRECTION('center_axis',(1.41426179436738E-51,-1.,-5.60383084497445E-34)) ;
#61158 = DIRECTION('ref_axis',(0.707106781186548,3.96250679110377E-34,-0.707106781186548)) ;
#61159 = DIRECTION('center_axis',(-5.00382208281761E-15,-1.,0.)) ;
#61160 = DIRECTION('ref_axis',(0.707106781186548,-3.53823652661133E-15,-0.707106781186548)) ;
#61161 = DIRECTION('',(1.41426179436738E-51,-1.,-5.60383084497445E-34)) ;
#61162 = DIRECTION('center_axis',(0.70710678118661,-0.707106781186485,0.)) ;
#61163 = DIRECTION('ref_axis',(0.707106781186485,0.70710678118661,-6.13317366673295E-17)) ;
#61164 = DIRECTION('center_axis',(-1.41426179436738E-51,1.,5.60383084497445E-34)) ;
#61165 = DIRECTION('ref_axis',(0.707106781186548,-3.96250679110377E-34,0.707106781186548)) ;
#61166 = DIRECTION('center_axis',(-5.00382208281761E-15,-1.,0.)) ;
#61167 = DIRECTION('ref_axis',(0.707106781186548,-3.53823652661133E-15,0.707106781186548)) ;
#61168 = DIRECTION('center_axis',(0.70710678118661,-0.707106781186485,0.)) ;
#61169 = DIRECTION('ref_axis',(0.707106781186485,0.70710678118661,6.13317366673295E-17)) ;
#61170 = DIRECTION('',(-1.41426179436738E-51,1.,5.60383084497445E-34)) ;
#61171 = DIRECTION('center_axis',(1.,1.41426179436738E-51,0.)) ;
#61172 = DIRECTION('ref_axis',(1.41426179436738E-51,-1.,-5.60383084497445E-34)) ;
#61173 = DIRECTION('',(0.,0.,-1.)) ;
#61174 = DIRECTION('',(0.,0.,-1.)) ;
#61175 = DIRECTION('center_axis',(2.52374105052742E-18,5.60383084497445E-34,
-1.)) ;
#61176 = DIRECTION('ref_axis',(-1.,0.,0.)) ;
#61177 = DIRECTION('center_axis',(0.,1.,0.)) ;
#61178 = DIRECTION('ref_axis',(1.,0.,0.)) ;
#61179 = DIRECTION('center_axis',(0.64278760968649,-0.76604444311902,2.28364033349672E-13)) ;
#61180 = DIRECTION('ref_axis',(3.55271367880058E-13,6.95559915454618E-29,
-1.)) ;
#61181 = DIRECTION('center_axis',(2.52374105052742E-18,5.60383084497445E-34,
-1.)) ;
#61182 = DIRECTION('ref_axis',(0.939692620785894,0.342020143325708,2.37154084195506E-18)) ;
#61183 = DIRECTION('center_axis',(2.52374105052742E-18,5.60383084497445E-34,
-1.)) ;
#61184 = DIRECTION('ref_axis',(-1.,0.,0.)) ;
#61185 = DIRECTION('center_axis',(0.,1.,0.)) ;
#61186 = DIRECTION('ref_axis',(1.77635683940029E-13,0.,1.)) ;
#61187 = DIRECTION('center_axis',(-2.52374105052742E-18,-5.60383084497445E-34,
1.)) ;
#61188 = DIRECTION('ref_axis',(0.939692620785894,0.342020143325708,2.37154084195506E-18)) ;
#61189 = DIRECTION('center_axis',(0.64278760968649,-0.76604444311902,-2.28364033349672E-13)) ;
#61190 = DIRECTION('ref_axis',(0.76604444311902,0.64278760968649,-2.26813531225949E-29)) ;
#61191 = DIRECTION('center_axis',(0.,0.,-1.)) ;
#61192 = DIRECTION('ref_axis',(0.939692620785895,0.342020143325706,0.)) ;
#61193 = DIRECTION('',(0.,0.,-1.)) ;
#61194 = DIRECTION('',(0.,0.,1.)) ;
#61195 = DIRECTION('center_axis',(1.,-1.0449157878825E-14,0.)) ;
#61196 = DIRECTION('ref_axis',(-1.0449157878825E-14,-1.,-2.69313517667302E-32)) ;
#61197 = DIRECTION('',(1.0449157878825E-14,1.,2.69313517667302E-32)) ;
#61198 = DIRECTION('',(0.,0.,1.)) ;
#61199 = DIRECTION('',(-1.0449157878825E-14,-1.,-2.69313517667302E-32)) ;
#61200 = DIRECTION('center_axis',(-1.0449157878825E-14,-1.,-2.69313517667302E-32)) ;
#61201 = DIRECTION('ref_axis',(0.707106781186485,-7.38867039380535E-15,0.70710678118661)) ;
#61202 = DIRECTION('center_axis',(0.,-1.,0.)) ;
#61203 = DIRECTION('ref_axis',(1.,0.,0.)) ;
#61204 = DIRECTION('center_axis',(0.642787609686559,-0.766044443118961,1.62222947733637E-18)) ;
#61205 = DIRECTION('ref_axis',(0.541675220419852,0.454519477672194,0.707106781186336)) ;
#61206 = DIRECTION('',(-0.642787609686559,0.766044443118961,-1.62222947733637E-18)) ;
#61207 = DIRECTION('center_axis',(-0.64278760968649,0.76604444311902,0.)) ;
#61208 = DIRECTION('ref_axis',(0.,0.,1.)) ;
#61209 = DIRECTION('center_axis',(2.52374105052742E-18,5.60383084497445E-34,
-1.)) ;
#61210 = DIRECTION('ref_axis',(-1.,0.,0.)) ;
#61211 = DIRECTION('center_axis',(-0.64278760968649,0.76604444311902,0.)) ;
#61212 = DIRECTION('ref_axis',(0.76604444311902,0.64278760968649,0.)) ;
#61213 = DIRECTION('center_axis',(1.,0.,0.)) ;
#61214 = DIRECTION('ref_axis',(0.,0.,-1.)) ;
#61215 = DIRECTION('center_axis',(2.52374105052742E-18,5.60383084497445E-34,
-1.)) ;
#61216 = DIRECTION('ref_axis',(0.422618261740652,0.906307787036672,1.06657905585743E-18)) ;
#61217 = DIRECTION('center_axis',(2.52374105052742E-18,5.60383084497445E-34,
-1.)) ;
#61218 = DIRECTION('ref_axis',(-1.,0.,0.)) ;
#61219 = DIRECTION('center_axis',(-2.52374105052742E-18,-5.60383084497445E-34,
1.)) ;
#61220 = DIRECTION('ref_axis',(0.422618261740652,0.906307787036672,1.06657905585743E-18)) ;
#61221 = DIRECTION('center_axis',(1.,0.,0.)) ;
#61222 = DIRECTION('ref_axis',(0.,1.,0.)) ;
#61223 = DIRECTION('center_axis',(0.,0.,-1.)) ;
#61224 = DIRECTION('ref_axis',(0.422618261740691,0.906307787036654,0.)) ;
#61225 = DIRECTION('',(0.,0.,-1.)) ;
#61226 = DIRECTION('',(0.,0.,1.)) ;
#61227 = DIRECTION('center_axis',(0.642787609686559,-0.766044443118961,1.62222947733637E-18)) ;
#61228 = DIRECTION('ref_axis',(0.541675220419655,0.454519477672028,-0.707106781186594)) ;
#61229 = DIRECTION('',(0.642787609686559,-0.766044443118961,1.62222947733637E-18)) ;
#61230 = DIRECTION('center_axis',(0.766044443118961,0.642787609686559,0.)) ;
#61231 = DIRECTION('ref_axis',(0.642787609686559,-0.766044443118961,1.62222947733637E-18)) ;
#61232 = DIRECTION('center_axis',(2.52374105052742E-18,5.60383084497445E-34,
-1.)) ;
#61233 = DIRECTION('ref_axis',(-1.,0.,0.)) ;
#61234 = DIRECTION('center_axis',(0.64278760968649,0.76604444311902,1.14182016674836E-13)) ;
#61235 = DIRECTION('ref_axis',(0.76604444311902,-0.64278760968649,1.13406765612974E-29)) ;
#61236 = DIRECTION('center_axis',(0.,-1.,0.)) ;
#61237 = DIRECTION('ref_axis',(1.77635683940029E-13,0.,-1.)) ;
#61238 = DIRECTION('center_axis',(2.52374105052742E-18,5.60383084497445E-34,
-1.)) ;
#61239 = DIRECTION('ref_axis',(0.939692620785894,-0.342020143325708,2.37154084195506E-18)) ;
#61240 = DIRECTION('center_axis',(2.52374105052742E-18,5.60383084497445E-34,
-1.)) ;
#61241 = DIRECTION('ref_axis',(-1.,0.,0.)) ;
#61242 = DIRECTION('center_axis',(0.64278760968649,0.76604444311902,-1.14182016674836E-13)) ;
#61243 = DIRECTION('ref_axis',(1.77635683940029E-13,-3.47779957727309E-29,
1.)) ;
#61244 = DIRECTION('center_axis',(-2.52374105052742E-18,-5.60383084497445E-34,
1.)) ;
#61245 = DIRECTION('ref_axis',(0.939692620785894,-0.342020143325708,2.37154084195506E-18)) ;
#61246 = DIRECTION('center_axis',(0.,0.,-1.)) ;
#61247 = DIRECTION('ref_axis',(0.939692620785895,-0.342020143325706,0.)) ;
#61248 = DIRECTION('',(0.,0.,-1.)) ;
#61249 = DIRECTION('center_axis',(-0.642787609686526,-0.76604444311899,-1.62222947733628E-18)) ;
#61250 = DIRECTION('ref_axis',(0.541675220419675,-0.454519477672004,-0.707106781186594)) ;
#61251 = DIRECTION('',(-0.642787609686526,-0.766044443118989,-1.62222947733628E-18)) ;
#61252 = DIRECTION('center_axis',(-0.642787609686402,-0.766044443119093,0.)) ;
#61253 = DIRECTION('ref_axis',(0.,0.,-1.)) ;
#61254 = DIRECTION('center_axis',(0.76604444311899,-0.642787609686526,0.)) ;
#61255 = DIRECTION('ref_axis',(-0.642787609686526,-0.766044443118989,-1.62222947733628E-18)) ;
#61256 = DIRECTION('',(0.642787609686526,0.766044443118989,1.62222947733628E-18)) ;
#61257 = DIRECTION('',(0.,0.,1.)) ;
#61258 = DIRECTION('center_axis',(-0.642787609686526,-0.76604444311899,-1.62222947733628E-18)) ;
#61259 = DIRECTION('ref_axis',(0.541675220419675,-0.454519477672004,0.707106781186594)) ;
#61260 = DIRECTION('center_axis',(-0.642787609686402,-0.766044443119093,0.)) ;
#61261 = DIRECTION('ref_axis',(0.766044443119093,-0.642787609686402,0.)) ;
#61262 = DIRECTION('center_axis',(0.,0.,-1.)) ;
#61263 = DIRECTION('ref_axis',(-1.,0.,0.)) ;
#61264 = DIRECTION('center_axis',(-0.316227766016905,-0.948683298050491,0.)) ;
#61265 = DIRECTION('ref_axis',(0.948683298050491,-0.316227766016905,0.)) ;
#61266 = DIRECTION('center_axis',(-0.316227766016905,-0.948683298050491,0.)) ;
#61267 = DIRECTION('ref_axis',(0.948683298050491,-0.316227766016905,0.)) ;
#61268 = DIRECTION('center_axis',(0.948683298050519,0.316227766016821,0.)) ;
#61269 = DIRECTION('ref_axis',(0.316227766016821,-0.948683298050519,0.)) ;
#61270 = DIRECTION('center_axis',(0.948683298050519,0.316227766016821,0.)) ;
#61271 = DIRECTION('ref_axis',(0.316227766016821,-0.948683298050519,0.)) ;
#61272 = DIRECTION('center_axis',(0.,0.,-1.)) ;
#61273 = DIRECTION('ref_axis',(-0.70710678118661,0.707106781186485,0.)) ;
#61274 = DIRECTION('',(0.,0.,-1.)) ;
#61275 = DIRECTION('center_axis',(0.,0.,-1.)) ;
#61276 = DIRECTION('ref_axis',(-1.,0.,0.)) ;
#61277 = DIRECTION('',(0.,0.,1.)) ;
#61278 = DIRECTION('center_axis',(0.948683298050519,0.316227766016821,0.)) ;
#61279 = DIRECTION('ref_axis',(0.316227766016821,-0.948683298050519,0.)) ;
#61280 = DIRECTION('center_axis',(0.948683298050519,0.316227766016821,0.)) ;
#61281 = DIRECTION('ref_axis',(0.316227766016821,-0.948683298050519,0.)) ;
#61282 = DIRECTION('center_axis',(-0.316227766016889,-0.948683298050497,0.)) ;
#61283 = DIRECTION('ref_axis',(0.948683298050497,-0.316227766016889,0.)) ;
#61284 = DIRECTION('center_axis',(-0.316227766016889,-0.948683298050497,0.)) ;
#61285 = DIRECTION('ref_axis',(0.948683298050497,-0.316227766016889,0.)) ;
#61286 = DIRECTION('center_axis',(1.,1.41426179436738E-51,0.)) ;
#61287 = DIRECTION('ref_axis',(1.41426179436738E-51,-1.,-5.60383084497445E-34)) ;
#61288 = DIRECTION('',(-1.41426179436738E-51,1.,5.60383084497445E-34)) ;
#61289 = DIRECTION('',(0.,0.,-1.)) ;
#61290 = DIRECTION('',(1.41426179436738E-51,-1.,-5.60383084497445E-34)) ;
#61291 = DIRECTION('center_axis',(1.41426179436738E-51,-1.,-5.60383084497445E-34)) ;
#61292 = DIRECTION('ref_axis',(0.70710678118661,-3.96250679110342E-34,0.707106781186485)) ;
#61293 = DIRECTION('center_axis',(0.106742421682839,0.994286706847317,0.)) ;
#61294 = DIRECTION('ref_axis',(-0.994286706847317,0.106742421682839,5.24986294729659E-33)) ;
#61295 = DIRECTION('center_axis',(-1.,0.,-2.52374105052742E-18)) ;
#61296 = DIRECTION('ref_axis',(-1.78455441078632E-18,-0.707106781186736,0.707106781186359)) ;
#61297 = DIRECTION('',(1.,0.,2.52374105052742E-18)) ;
#61298 = DIRECTION('center_axis',(1.,0.,0.)) ;
#61299 = DIRECTION('ref_axis',(0.,3.55271367880058E-13,1.)) ;
#61300 = DIRECTION('center_axis',(1.,0.,0.)) ;
#61301 = DIRECTION('ref_axis',(0.,-1.,0.)) ;
#61302 = DIRECTION('center_axis',(2.52374105052742E-18,5.60383084497445E-34,
-1.)) ;
#61303 = DIRECTION('ref_axis',(0.422618261740848,-0.906307787036581,1.06657905585792E-18)) ;
#61304 = DIRECTION('center_axis',(-2.52374105052742E-18,-5.60383084497445E-34,
1.)) ;
#61305 = DIRECTION('ref_axis',(0.422618261740848,-0.906307787036581,1.06657905585792E-18)) ;
#61306 = DIRECTION('center_axis',(0.,0.,-1.)) ;
#61307 = DIRECTION('ref_axis',(0.422618261740767,-0.906307787036618,0.)) ;
#61308 = DIRECTION('',(0.,0.,-1.)) ;
#61309 = DIRECTION('center_axis',(-1.,0.,-2.52374105052742E-18)) ;
#61310 = DIRECTION('ref_axis',(1.78455441078632E-18,-0.707106781186736,-0.707106781186359)) ;
#61311 = DIRECTION('',(-1.,0.,-2.52374105052742E-18)) ;
#61312 = DIRECTION('center_axis',(0.,-1.,0.)) ;
#61313 = DIRECTION('ref_axis',(-1.,0.,-2.52374105052742E-18)) ;
#61314 = DIRECTION('center_axis',(1.41426179436738E-51,-1.,-5.60383084497445E-34)) ;
#61315 = DIRECTION('ref_axis',(0.707106781186548,-3.96250679110377E-34,0.707106781186548)) ;
#61316 = DIRECTION('center_axis',(0.,-1.,0.)) ;
#61317 = DIRECTION('ref_axis',(1.,0.,0.)) ;
#61318 = DIRECTION('center_axis',(0.,1.,0.)) ;
#61319 = DIRECTION('ref_axis',(0.,0.,1.)) ;
#61320 = DIRECTION('',(-1.41426179436738E-51,1.,5.60383084497445E-34)) ;
#61321 = DIRECTION('center_axis',(-2.52374105052742E-18,-5.60383084497445E-34,
1.)) ;
#61322 = DIRECTION('ref_axis',(1.,0.,0.)) ;
#61323 = DIRECTION('center_axis',(0.,-1.,0.)) ;
#61324 = DIRECTION('ref_axis',(0.,0.,1.)) ;
#61325 = DIRECTION('center_axis',(2.52374105052742E-18,5.60383084497445E-34,
-1.)) ;
#61326 = DIRECTION('ref_axis',(1.73732004304105E-19,-1.,-5.59944629906392E-34)) ;
#61327 = DIRECTION('center_axis',(-1.41426179436738E-51,1.,5.60383084497445E-34)) ;
#61328 = DIRECTION('ref_axis',(-0.707106781186548,-3.96250679110377E-34,0.707106781186548)) ;
#61329 = DIRECTION('center_axis',(0.,-1.,0.)) ;
#61330 = DIRECTION('ref_axis',(0.,0.,1.)) ;
#61331 = DIRECTION('',(1.41426179436738E-51,-1.,-5.60383084497445E-34)) ;
#61332 = DIRECTION('center_axis',(-2.52374105052742E-18,-5.60383084497445E-34,
1.)) ;
#61333 = DIRECTION('ref_axis',(1.,0.,0.)) ;
#61334 = DIRECTION('center_axis',(2.52374105052742E-18,5.60383084497445E-34,
-1.)) ;
#61335 = DIRECTION('ref_axis',(1.73732004304105E-19,1.,5.60821539088498E-34)) ;
#61336 = DIRECTION('center_axis',(0.,0.,-1.)) ;
#61337 = DIRECTION('ref_axis',(-1.,0.,0.)) ;
#61338 = DIRECTION('',(0.,0.,-1.)) ;
#61339 = DIRECTION('',(0.,0.,-1.)) ;
#61340 = DIRECTION('center_axis',(1.,1.41426179436738E-51,0.)) ;
#61341 = DIRECTION('ref_axis',(1.41426179436738E-51,-1.,-5.60383084497445E-34)) ;
#61342 = DIRECTION('',(0.,0.,-1.)) ;
#61343 = DIRECTION('center_axis',(2.52374105052742E-18,5.60383084497445E-34,
-1.)) ;
#61344 = DIRECTION('ref_axis',(-1.,0.,0.)) ;
#61345 = DIRECTION('center_axis',(2.52374105052742E-18,5.60383084497445E-34,
-1.)) ;
#61346 = DIRECTION('ref_axis',(-0.707106781186547,0.707106781186547,-1.7845544107868E-18)) ;
#61347 = DIRECTION('center_axis',(0.,1.,0.)) ;
#61348 = DIRECTION('ref_axis',(1.,0.,2.52374105052742E-18)) ;
#61349 = DIRECTION('',(0.,0.,-1.)) ;
#61350 = DIRECTION('',(0.,0.,-1.)) ;
#61351 = DIRECTION('center_axis',(0.,0.,-1.)) ;
#61352 = DIRECTION('ref_axis',(-1.,0.,0.)) ;
#61353 = DIRECTION('center_axis',(-2.52374105052742E-18,-5.60383084497445E-34,
1.)) ;
#61354 = DIRECTION('ref_axis',(-0.707106781186547,0.707106781186547,-1.7845544107868E-18)) ;
#61355 = DIRECTION('center_axis',(0.,-1.,0.)) ;
#61356 = DIRECTION('ref_axis',(-1.,0.,-2.52374105052742E-18)) ;
#61357 = DIRECTION('',(0.,0.,-1.)) ;
#61358 = DIRECTION('center_axis',(-2.52374105052742E-18,-5.60383084497445E-34,
1.)) ;
#61359 = DIRECTION('ref_axis',(1.,0.,0.)) ;
#61360 = DIRECTION('center_axis',(1.,1.41426179436738E-51,0.)) ;
#61361 = DIRECTION('ref_axis',(1.41426179436738E-51,-1.,-5.60383084497445E-34)) ;
#61362 = DIRECTION('',(0.,0.,-1.)) ;
#61363 = DIRECTION('center_axis',(-0.212265141871518,-0.977212110826644,-5.35702252137179E-19)) ;
#61364 = DIRECTION('ref_axis',(0.690993310223154,-0.150094121226878,-0.707106781186533)) ;
#61365 = DIRECTION('',(-0.212265141871518,-0.977212110826644,-5.35702252137179E-19)) ;
#61366 = DIRECTION('center_axis',(0.,1.,0.)) ;
#61367 = DIRECTION('ref_axis',(1.,0.,-4.23798197414957E-16)) ;
#61368 = DIRECTION('center_axis',(-0.106742421682839,-0.994286706847317,0.)) ;
#61369 = DIRECTION('ref_axis',(0.994286706847317,-0.106742421682839,5.01864435613725E-18)) ;
#61370 = DIRECTION('center_axis',(1.41426179436738E-51,-1.,-5.60383084497445E-34)) ;
#61371 = DIRECTION('ref_axis',(0.70710678118661,3.96250679110342E-34,-0.707106781186485)) ;
#61372 = DIRECTION('center_axis',(-1.0449157878825E-14,-1.,-2.69313517667302E-32)) ;
#61373 = DIRECTION('ref_axis',(0.707106781186485,-7.38867039380535E-15,-0.70710678118661)) ;
#61374 = DIRECTION('center_axis',(1.,0.,2.52374105052742E-18)) ;
#61375 = DIRECTION('ref_axis',(1.78455441078632E-18,0.707106781186736,-0.707106781186359)) ;
#61376 = DIRECTION('',(1.,0.,2.52374105052742E-18)) ;
#61377 = DIRECTION('center_axis',(0.,-1.,0.)) ;
#61378 = DIRECTION('ref_axis',(-1.,0.,-2.52374105052742E-18)) ;
#61379 = DIRECTION('',(0.,0.,-1.)) ;
#61380 = DIRECTION('center_axis',(0.,1.,0.)) ;
#61381 = DIRECTION('ref_axis',(1.,0.,4.23798197414957E-16)) ;
#61382 = DIRECTION('center_axis',(0.977212110826644,-0.212265141871518,0.)) ;
#61383 = DIRECTION('ref_axis',(-0.212265141871518,-0.977212110826644,-5.35702252137179E-19)) ;
#61384 = DIRECTION('',(0.212265141871518,0.977212110826644,5.35702252137179E-19)) ;
#61385 = DIRECTION('center_axis',(0.,1.,0.)) ;
#61386 = DIRECTION('ref_axis',(1.,0.,2.52374105052742E-18)) ;
#61387 = DIRECTION('',(-1.,0.,-2.52374105052742E-18)) ;
#61388 = DIRECTION('center_axis',(1.,0.,2.52374105052742E-18)) ;
#61389 = DIRECTION('ref_axis',(-1.78455441078632E-18,0.707106781186736,0.707106781186359)) ;
#61390 = DIRECTION('center_axis',(-0.212265141871518,-0.977212110826644,-5.35702252137179E-19)) ;
#61391 = DIRECTION('ref_axis',(0.690993310223154,-0.150094121226878,0.707106781186533)) ;
#61392 = DIRECTION('center_axis',(1.,1.41426179436738E-51,0.)) ;
#61393 = DIRECTION('ref_axis',(0.,0.,-1.)) ;
#61394 = DIRECTION('center_axis',(0.,1.,0.)) ;
#61395 = DIRECTION('ref_axis',(-1.,0.,0.)) ;
#61396 = DIRECTION('center_axis',(-1.,-1.41426179436738E-51,0.)) ;
#61397 = DIRECTION('ref_axis',(-9.57459760970815E-52,0.677003200386319,0.735980072193997)) ;
#61398 = DIRECTION('center_axis',(1.,1.41426179436738E-51,0.)) ;
#61399 = DIRECTION('ref_axis',(-9.57459760970815E-52,0.677003200386319,0.735980072193997)) ;
#61400 = DIRECTION('center_axis',(1.41426179436738E-51,-1.,0.)) ;
#61401 = DIRECTION('ref_axis',(-0.707106781186568,-1.00003410517026E-51,0.707106781186527)) ;
#61402 = DIRECTION('center_axis',(0.,1.,0.)) ;
#61403 = DIRECTION('ref_axis',(-1.,0.,0.)) ;
#61404 = DIRECTION('',(-1.41426179436738E-51,1.,0.)) ;
#61405 = DIRECTION('',(1.41426179436738E-51,-1.,0.)) ;
#61406 = DIRECTION('center_axis',(1.,1.41426179436738E-51,0.)) ;
#61407 = DIRECTION('ref_axis',(0.,0.,-1.)) ;
#61408 = DIRECTION('center_axis',(-1.,-1.41426179436738E-51,0.)) ;
#61409 = DIRECTION('ref_axis',(9.5745976097084E-52,-0.677003200386337,0.735980072193981)) ;
#61410 = DIRECTION('center_axis',(1.,1.41426179436738E-51,0.)) ;
#61411 = DIRECTION('ref_axis',(9.5745976097084E-52,-0.677003200386337,0.735980072193981)) ;
#61412 = DIRECTION('center_axis',(-1.,-1.41426179436738E-51,0.)) ;
#61413 = DIRECTION('ref_axis',(1.41426179436738E-51,-1.,-5.60383084497445E-34)) ;
#61414 = DIRECTION('center_axis',(-1.,-1.41426179436738E-51,0.)) ;
#61415 = DIRECTION('ref_axis',(0.,0.,1.)) ;
#61416 = DIRECTION('center_axis',(0.,-1.,0.)) ;
#61417 = DIRECTION('ref_axis',(1.,0.,0.)) ;
#61418 = DIRECTION('center_axis',(1.,1.41426179436738E-51,0.)) ;
#61419 = DIRECTION('ref_axis',(9.5745976097084E-52,-0.677003200386337,0.735980072193981)) ;
#61420 = DIRECTION('center_axis',(-1.,-1.41426179436738E-51,0.)) ;
#61421 = DIRECTION('ref_axis',(9.5745976097084E-52,-0.677003200386337,0.735980072193981)) ;
#61422 = DIRECTION('center_axis',(-1.41426179436738E-51,1.,0.)) ;
#61423 = DIRECTION('ref_axis',(0.707106781186568,1.00003410517026E-51,0.707106781186527)) ;
#61424 = DIRECTION('center_axis',(0.,-1.,0.)) ;
#61425 = DIRECTION('ref_axis',(1.,0.,0.)) ;
#61426 = DIRECTION('',(1.41426179436738E-51,-1.,0.)) ;
#61427 = DIRECTION('',(-1.41426179436738E-51,1.,0.)) ;
#61428 = DIRECTION('center_axis',(-1.,-1.41426179436738E-51,0.)) ;
#61429 = DIRECTION('ref_axis',(0.,0.,1.)) ;
#61430 = DIRECTION('center_axis',(1.,1.41426179436738E-51,0.)) ;
#61431 = DIRECTION('ref_axis',(-9.57459760970815E-52,0.677003200386319,0.735980072193997)) ;
#61432 = DIRECTION('center_axis',(-1.,-1.41426179436738E-51,0.)) ;
#61433 = DIRECTION('ref_axis',(-9.57459760970815E-52,0.677003200386319,0.735980072193997)) ;
#61434 = DIRECTION('center_axis',(1.,1.41426179436738E-51,0.)) ;
#61435 = DIRECTION('ref_axis',(-1.41426179436738E-51,1.,5.60383084497445E-34)) ;
#61436 = DIRECTION('center_axis',(-1.,-1.41426179436738E-51,0.)) ;
#61437 = DIRECTION('ref_axis',(0.,0.,1.)) ;
#61438 = DIRECTION('center_axis',(0.,-1.,0.)) ;
#61439 = DIRECTION('ref_axis',(1.,0.,0.)) ;
#61440 = DIRECTION('center_axis',(1.,1.41426179436738E-51,0.)) ;
#61441 = DIRECTION('ref_axis',(9.57459760970815E-52,-0.677003200386319,0.735980072193997)) ;
#61442 = DIRECTION('center_axis',(-1.,-1.41426179436738E-51,0.)) ;
#61443 = DIRECTION('ref_axis',(9.57459760970815E-52,-0.677003200386319,0.735980072193997)) ;
#61444 = DIRECTION('center_axis',(-1.41426179436738E-51,1.,0.)) ;
#61445 = DIRECTION('ref_axis',(0.707106781186547,1.00003410517023E-51,0.707106781186547)) ;
#61446 = DIRECTION('center_axis',(0.,-1.,0.)) ;
#61447 = DIRECTION('ref_axis',(1.,0.,0.)) ;
#61448 = DIRECTION('',(1.41426179436738E-51,-1.,0.)) ;
#61449 = DIRECTION('',(-1.41426179436738E-51,1.,0.)) ;
#61450 = DIRECTION('center_axis',(-1.,-1.41426179436738E-51,0.)) ;
#61451 = DIRECTION('ref_axis',(0.,0.,1.)) ;
#61452 = DIRECTION('center_axis',(1.,1.41426179436738E-51,0.)) ;
#61453 = DIRECTION('ref_axis',(-9.57459760970815E-52,0.677003200386319,0.735980072193997)) ;
#61454 = DIRECTION('center_axis',(-1.,-1.41426179436738E-51,0.)) ;
#61455 = DIRECTION('ref_axis',(-9.57459760970815E-52,0.677003200386319,0.735980072193997)) ;
#61456 = DIRECTION('center_axis',(1.,1.41426179436738E-51,0.)) ;
#61457 = DIRECTION('ref_axis',(-1.41426179436738E-51,1.,5.60383084497445E-34)) ;
#61458 = DIRECTION('center_axis',(1.,1.41426179436738E-51,0.)) ;
#61459 = DIRECTION('ref_axis',(0.,0.,-1.)) ;
#61460 = DIRECTION('center_axis',(0.,1.,0.)) ;
#61461 = DIRECTION('ref_axis',(-1.,0.,0.)) ;
#61462 = DIRECTION('center_axis',(-1.,-1.41426179436738E-51,0.)) ;
#61463 = DIRECTION('ref_axis',(-9.57459760970815E-52,0.677003200386319,0.735980072193997)) ;
#61464 = DIRECTION('center_axis',(1.,1.41426179436738E-51,0.)) ;
#61465 = DIRECTION('ref_axis',(-9.57459760970815E-52,0.677003200386319,0.735980072193997)) ;
#61466 = DIRECTION('center_axis',(1.41426179436738E-51,-1.,0.)) ;
#61467 = DIRECTION('ref_axis',(-0.707106781186547,-1.00003410517023E-51,0.707106781186547)) ;
#61468 = DIRECTION('center_axis',(0.,1.,0.)) ;
#61469 = DIRECTION('ref_axis',(-1.,0.,0.)) ;
#61470 = DIRECTION('',(-1.41426179436738E-51,1.,0.)) ;
#61471 = DIRECTION('',(1.41426179436738E-51,-1.,0.)) ;
#61472 = DIRECTION('center_axis',(1.,1.41426179436738E-51,0.)) ;
#61473 = DIRECTION('ref_axis',(0.,0.,-1.)) ;
#61474 = DIRECTION('center_axis',(-1.,-1.41426179436738E-51,0.)) ;
#61475 = DIRECTION('ref_axis',(9.57459760970815E-52,-0.677003200386319,0.735980072193997)) ;
#61476 = DIRECTION('center_axis',(1.,1.41426179436738E-51,0.)) ;
#61477 = DIRECTION('ref_axis',(9.57459760970815E-52,-0.677003200386319,0.735980072193997)) ;
#61478 = DIRECTION('center_axis',(-1.,-1.41426179436738E-51,0.)) ;
#61479 = DIRECTION('ref_axis',(1.41426179436738E-51,-1.,-5.60383084497445E-34)) ;
#61480 = DIRECTION('center_axis',(-1.,-1.41426179436738E-51,0.)) ;
#61481 = DIRECTION('ref_axis',(0.,0.,1.)) ;
#61482 = DIRECTION('center_axis',(0.,-1.,0.)) ;
#61483 = DIRECTION('ref_axis',(1.,0.,0.)) ;
#61484 = DIRECTION('center_axis',(1.,1.41426179436738E-51,0.)) ;
#61485 = DIRECTION('ref_axis',(9.57459760970815E-52,-0.677003200386319,0.735980072193997)) ;
#61486 = DIRECTION('center_axis',(-1.,-1.41426179436738E-51,0.)) ;
#61487 = DIRECTION('ref_axis',(9.57459760970815E-52,-0.677003200386319,0.735980072193997)) ;
#61488 = DIRECTION('center_axis',(-1.41426179436738E-51,1.,0.)) ;
#61489 = DIRECTION('ref_axis',(0.707106781186568,1.00003410517026E-51,0.707106781186527)) ;
#61490 = DIRECTION('center_axis',(0.,-1.,0.)) ;
#61491 = DIRECTION('ref_axis',(1.,0.,0.)) ;
#61492 = DIRECTION('',(1.41426179436738E-51,-1.,0.)) ;
#61493 = DIRECTION('',(-1.41426179436738E-51,1.,0.)) ;
#61494 = DIRECTION('center_axis',(-1.,-1.41426179436738E-51,0.)) ;
#61495 = DIRECTION('ref_axis',(0.,0.,1.)) ;
#61496 = DIRECTION('center_axis',(1.,1.41426179436738E-51,0.)) ;
#61497 = DIRECTION('ref_axis',(-9.5745976097084E-52,0.677003200386337,0.735980072193981)) ;
#61498 = DIRECTION('center_axis',(-1.,-1.41426179436738E-51,0.)) ;
#61499 = DIRECTION('ref_axis',(-9.5745976097084E-52,0.677003200386337,0.735980072193981)) ;
#61500 = DIRECTION('center_axis',(1.,1.41426179436738E-51,0.)) ;
#61501 = DIRECTION('ref_axis',(-1.41426179436738E-51,1.,5.60383084497445E-34)) ;
#61502 = DIRECTION('center_axis',(1.,1.41426179436738E-51,0.)) ;
#61503 = DIRECTION('ref_axis',(0.,0.,-1.)) ;
#61504 = DIRECTION('center_axis',(0.,1.,0.)) ;
#61505 = DIRECTION('ref_axis',(-1.,0.,0.)) ;
#61506 = DIRECTION('center_axis',(-1.,-1.41426179436738E-51,0.)) ;
#61507 = DIRECTION('ref_axis',(-9.5745976097084E-52,0.677003200386337,0.735980072193981)) ;
#61508 = DIRECTION('center_axis',(1.,1.41426179436738E-51,0.)) ;
#61509 = DIRECTION('ref_axis',(-9.5745976097084E-52,0.677003200386337,0.735980072193981)) ;
#61510 = DIRECTION('center_axis',(1.41426179436738E-51,-1.,0.)) ;
#61511 = DIRECTION('ref_axis',(-0.707106781186568,-1.00003410517026E-51,0.707106781186527)) ;
#61512 = DIRECTION('center_axis',(0.,1.,0.)) ;
#61513 = DIRECTION('ref_axis',(-1.,0.,0.)) ;
#61514 = DIRECTION('',(-1.41426179436738E-51,1.,0.)) ;
#61515 = DIRECTION('',(1.41426179436738E-51,-1.,0.)) ;
#61516 = DIRECTION('center_axis',(1.,1.41426179436738E-51,0.)) ;
#61517 = DIRECTION('ref_axis',(0.,0.,-1.)) ;
#61518 = DIRECTION('center_axis',(-1.,-1.41426179436738E-51,0.)) ;
#61519 = DIRECTION('ref_axis',(9.57459760970815E-52,-0.677003200386319,0.735980072193997)) ;
#61520 = DIRECTION('center_axis',(1.,1.41426179436738E-51,0.)) ;
#61521 = DIRECTION('ref_axis',(9.57459760970815E-52,-0.677003200386319,0.735980072193997)) ;
#61522 = DIRECTION('center_axis',(-1.,-1.41426179436738E-51,0.)) ;
#61523 = DIRECTION('ref_axis',(1.41426179436738E-51,-1.,-5.60383084497445E-34)) ;
#61524 = DIRECTION('center_axis',(-1.,-1.41426179436738E-51,0.)) ;
#61525 = DIRECTION('ref_axis',(0.,0.,1.)) ;
#61526 = DIRECTION('center_axis',(0.,-1.,0.)) ;
#61527 = DIRECTION('ref_axis',(1.,0.,0.)) ;
#61528 = DIRECTION('center_axis',(1.,1.41426179436738E-51,0.)) ;
#61529 = DIRECTION('ref_axis',(9.57459760970817E-52,-0.677003200386321,0.735980072193996)) ;
#61530 = DIRECTION('center_axis',(-1.,-1.41426179436738E-51,0.)) ;
#61531 = DIRECTION('ref_axis',(9.57459760970817E-52,-0.677003200386321,0.735980072193996)) ;
#61532 = DIRECTION('center_axis',(-1.41426179436738E-51,1.,0.)) ;
#61533 = DIRECTION('ref_axis',(0.707106781186568,1.00003410517026E-51,0.707106781186527)) ;
#61534 = DIRECTION('center_axis',(0.,-1.,0.)) ;
#61535 = DIRECTION('ref_axis',(1.,0.,0.)) ;
#61536 = DIRECTION('',(1.41426179436738E-51,-1.,0.)) ;
#61537 = DIRECTION('',(-1.41426179436738E-51,1.,0.)) ;
#61538 = DIRECTION('center_axis',(-1.,-1.41426179436738E-51,0.)) ;
#61539 = DIRECTION('ref_axis',(0.,0.,1.)) ;
#61540 = DIRECTION('center_axis',(1.,1.41426179436738E-51,0.)) ;
#61541 = DIRECTION('ref_axis',(-9.57459760970815E-52,0.677003200386319,0.735980072193997)) ;
#61542 = DIRECTION('center_axis',(-1.,-1.41426179436738E-51,0.)) ;
#61543 = DIRECTION('ref_axis',(-9.57459760970815E-52,0.677003200386319,0.735980072193997)) ;
#61544 = DIRECTION('center_axis',(1.,1.41426179436738E-51,0.)) ;
#61545 = DIRECTION('ref_axis',(-1.41426179436738E-51,1.,5.60383084497445E-34)) ;
#61546 = DIRECTION('center_axis',(1.,1.41426179436738E-51,0.)) ;
#61547 = DIRECTION('ref_axis',(0.,0.,-1.)) ;
#61548 = DIRECTION('center_axis',(0.,1.,0.)) ;
#61549 = DIRECTION('ref_axis',(-1.,0.,0.)) ;
#61550 = DIRECTION('center_axis',(-1.,-1.41426179436738E-51,0.)) ;
#61551 = DIRECTION('ref_axis',(-9.57459760970817E-52,0.677003200386321,0.735980072193996)) ;
#61552 = DIRECTION('center_axis',(1.,1.41426179436738E-51,0.)) ;
#61553 = DIRECTION('ref_axis',(-9.57459760970817E-52,0.677003200386321,0.735980072193996)) ;
#61554 = DIRECTION('center_axis',(1.41426179436738E-51,-1.,0.)) ;
#61555 = DIRECTION('ref_axis',(-0.707106781186568,-1.00003410517026E-51,0.707106781186527)) ;
#61556 = DIRECTION('center_axis',(0.,1.,0.)) ;
#61557 = DIRECTION('ref_axis',(-1.,0.,0.)) ;
#61558 = DIRECTION('',(-1.41426179436738E-51,1.,0.)) ;
#61559 = DIRECTION('',(1.41426179436738E-51,-1.,0.)) ;
#61560 = DIRECTION('center_axis',(1.,1.41426179436738E-51,0.)) ;
#61561 = DIRECTION('ref_axis',(0.,0.,-1.)) ;
#61562 = DIRECTION('center_axis',(-1.,-1.41426179436738E-51,0.)) ;
#61563 = DIRECTION('ref_axis',(9.57459760970815E-52,-0.677003200386319,0.735980072193997)) ;
#61564 = DIRECTION('center_axis',(1.,1.41426179436738E-51,0.)) ;
#61565 = DIRECTION('ref_axis',(9.57459760970815E-52,-0.677003200386319,0.735980072193997)) ;
#61566 = DIRECTION('center_axis',(-1.,-1.41426179436738E-51,0.)) ;
#61567 = DIRECTION('ref_axis',(1.41426179436738E-51,-1.,-5.60383084497445E-34)) ;
#61568 = DIRECTION('center_axis',(1.,0.,0.)) ;
#61569 = DIRECTION('ref_axis',(0.,0.996521728591783,0.083333333333332)) ;
#61570 = DIRECTION('',(1.,0.,0.)) ;
#61571 = DIRECTION('center_axis',(0.,0.,1.)) ;
#61572 = DIRECTION('ref_axis',(1.,0.,0.)) ;
#61573 = DIRECTION('',(-1.,0.,0.)) ;
#61574 = DIRECTION('center_axis',(-1.,0.,0.)) ;
#61575 = DIRECTION('ref_axis',(0.,-0.996521728591783,0.083333333333332)) ;
#61576 = DIRECTION('center_axis',(1.,0.,0.)) ;
#61577 = DIRECTION('ref_axis',(0.,0.996521728591783,0.083333333333332)) ;
#61578 = DIRECTION('',(1.,0.,0.)) ;
#61579 = DIRECTION('center_axis',(0.,0.,1.)) ;
#61580 = DIRECTION('ref_axis',(1.,0.,0.)) ;
#61581 = DIRECTION('',(-1.,0.,0.)) ;
#61582 = DIRECTION('center_axis',(-1.,0.,0.)) ;
#61583 = DIRECTION('ref_axis',(0.,-0.996521728591783,0.083333333333332)) ;
#61584 = DIRECTION('center_axis',(-1.,0.,0.)) ;
#61585 = DIRECTION('ref_axis',(0.,-0.996521728591783,0.083333333333332)) ;
#61586 = DIRECTION('',(-1.,0.,0.)) ;
#61587 = DIRECTION('center_axis',(0.,0.,1.)) ;
#61588 = DIRECTION('ref_axis',(1.,0.,0.)) ;
#61589 = DIRECTION('',(1.,0.,0.)) ;
#61590 = DIRECTION('center_axis',(1.,0.,0.)) ;
#61591 = DIRECTION('ref_axis',(0.,0.996521728591783,0.083333333333332)) ;
#61592 = DIRECTION('center_axis',(1.,0.,0.)) ;
#61593 = DIRECTION('ref_axis',(0.,0.996521728591783,0.083333333333332)) ;
#61594 = DIRECTION('',(1.,0.,0.)) ;
#61595 = DIRECTION('center_axis',(0.,0.,1.)) ;
#61596 = DIRECTION('ref_axis',(1.,0.,0.)) ;
#61597 = DIRECTION('',(-1.,0.,0.)) ;
#61598 = DIRECTION('center_axis',(-1.,0.,0.)) ;
#61599 = DIRECTION('ref_axis',(0.,-0.996521728591783,0.083333333333332)) ;
#61600 = DIRECTION('center_axis',(2.52374105052742E-18,5.60383084497445E-34,
-1.)) ;
#61601 = DIRECTION('ref_axis',(1.,3.40207761657885E-68,2.52374105052742E-18)) ;
#61602 = DIRECTION('',(-1.41426179436738E-51,1.,5.60383084497445E-34)) ;
#61603 = DIRECTION('',(1.,0.,2.52374105052742E-18)) ;
#61604 = DIRECTION('',(1.41426179436738E-51,-1.,-5.60383084497445E-34)) ;
#61605 = DIRECTION('',(-1.,0.,-2.52374105052742E-18)) ;
#61606 = DIRECTION('center_axis',(0.,-1.,0.)) ;
#61607 = DIRECTION('ref_axis',(-1.,0.,-2.52374105052742E-18)) ;
#61608 = DIRECTION('',(0.,0.,-1.)) ;
#61609 = DIRECTION('',(0.,0.,-1.)) ;
#61610 = DIRECTION('center_axis',(1.,1.41426179436738E-51,0.)) ;
#61611 = DIRECTION('ref_axis',(1.41426179436738E-51,-1.,-5.60383084497445E-34)) ;
#61612 = DIRECTION('',(0.,0.,-1.)) ;
#61613 = DIRECTION('center_axis',(0.,0.,-1.)) ;
#61614 = DIRECTION('ref_axis',(1.,0.,0.)) ;
#61615 = DIRECTION('',(0.,0.,1.)) ;
#61616 = DIRECTION('center_axis',(-0.895130847441207,-0.445803505996966,0.)) ;
#61617 = DIRECTION('ref_axis',(-0.445803505996966,0.895130847441207,-1.12509260855359E-18)) ;
#61618 = DIRECTION('',(0.,0.,-1.)) ;
#61619 = DIRECTION('center_axis',(-1.,-1.41426179436738E-51,0.)) ;
#61620 = DIRECTION('ref_axis',(-1.41426179436738E-51,1.,5.60383084497445E-34)) ;
#61621 = DIRECTION('',(0.,0.,-1.)) ;
#61622 = DIRECTION('center_axis',(0.,0.,-1.)) ;
#61623 = DIRECTION('ref_axis',(1.,0.,0.)) ;
#61624 = DIRECTION('center_axis',(0.,1.,0.)) ;
#61625 = DIRECTION('ref_axis',(1.,0.,2.52374105052742E-18)) ;
#61626 = DIRECTION('',(0.,0.,-1.)) ;
#61627 = DIRECTION('center_axis',(-1.,-1.41426179436738E-51,0.)) ;
#61628 = DIRECTION('ref_axis',(-1.41426179436738E-51,1.,5.60383084497445E-34)) ;
#61629 = DIRECTION('center_axis',(5.00382208281761E-15,1.,0.)) ;
#61630 = DIRECTION('ref_axis',(1.,-5.00382208281761E-15,2.52374105052742E-18)) ;
#61631 = DIRECTION('',(0.,0.,-1.)) ;
#61632 = DIRECTION('center_axis',(1.,1.41426179436738E-51,0.)) ;
#61633 = DIRECTION('ref_axis',(1.41426179436738E-51,-1.,-5.60383084497445E-34)) ;
#61634 = DIRECTION('',(0.,0.,-1.)) ;
#61635 = DIRECTION('center_axis',(0.,1.,0.)) ;
#61636 = DIRECTION('ref_axis',(1.,0.,2.52374105052742E-18)) ;
#61637 = DIRECTION('',(0.,0.,-1.)) ;
#61638 = DIRECTION('center_axis',(-1.,7.65671051465623E-16,0.)) ;
#61639 = DIRECTION('ref_axis',(7.65671051465623E-16,1.,2.49273854828173E-33)) ;
#61640 = DIRECTION('',(0.,0.,-1.)) ;
#61641 = DIRECTION('center_axis',(0.,-1.,0.)) ;
#61642 = DIRECTION('ref_axis',(-1.,0.,-2.52374105052742E-18)) ;
#61643 = DIRECTION('',(0.,0.,-1.)) ;
#61644 = DIRECTION('center_axis',(-1.,-1.41426179436738E-51,0.)) ;
#61645 = DIRECTION('ref_axis',(-1.41426179436738E-51,1.,5.60383084497445E-34)) ;
#61646 = DIRECTION('axis',(0.,0.,1.)) ;
#61647 = DIRECTION('refdir',(1.,0.,0.)) ;
#61648 = DIRECTION('center_axis',(0.,-1.,0.)) ;
#61649 = DIRECTION('ref_axis',(-1.,0.,-2.52374105052742E-18)) ;
#61650 = DIRECTION('',(-1.,0.,-2.52374105052742E-18)) ;
#61651 = DIRECTION('',(0.,0.,-1.)) ;
#61652 = DIRECTION('',(-1.,0.,-2.52374105052742E-18)) ;
#61653 = DIRECTION('',(0.,0.,-1.)) ;
#61654 = DIRECTION('center_axis',(1.,1.41426179436738E-51,0.)) ;
#61655 = DIRECTION('ref_axis',(1.41426179436738E-51,-1.,-5.60383084497445E-34)) ;
#61656 = DIRECTION('',(1.41426179436738E-51,-1.,-5.60383084497445E-34)) ;
#61657 = DIRECTION('',(1.41426179436738E-51,-1.,-5.60383084497445E-34)) ;
#61658 = DIRECTION('',(0.,0.,-1.)) ;
#61659 = DIRECTION('center_axis',(0.,1.,0.)) ;
#61660 = DIRECTION('ref_axis',(1.,0.,2.52374105052742E-18)) ;
#61661 = DIRECTION('',(1.,0.,2.52374105052742E-18)) ;
#61662 = DIRECTION('',(1.,0.,2.52374105052742E-18)) ;
#61663 = DIRECTION('',(0.,0.,-1.)) ;
#61664 = DIRECTION('center_axis',(-1.,-1.41426179436738E-51,0.)) ;
#61665 = DIRECTION('ref_axis',(-1.41426179436738E-51,1.,5.60383084497445E-34)) ;
#61666 = DIRECTION('',(-1.41426179436738E-51,1.,5.60383084497445E-34)) ;
#61667 = DIRECTION('',(-1.41426179436738E-51,1.,5.60383084497445E-34)) ;
#61668 = DIRECTION('center_axis',(0.,0.,-1.)) ;
#61669 = DIRECTION('ref_axis',(-1.,0.,0.)) ;
#61670 = DIRECTION('center_axis',(2.52374105052742E-18,5.60383084497445E-34,
-1.)) ;
#61671 = DIRECTION('ref_axis',(1.,3.40207761657885E-68,2.52374105052742E-18)) ;
#61672 = DIRECTION('axis',(0.,0.,1.)) ;
#61673 = DIRECTION('refdir',(1.,0.,0.)) ;
#61674 = DIRECTION('center_axis',(0.,-5.60383084497445E-34,1.)) ;
#61675 = DIRECTION('ref_axis',(-1.,0.,0.)) ;
#61676 = DIRECTION('center_axis',(0.,5.60383084497445E-34,-1.)) ;
#61677 = DIRECTION('ref_axis',(-1.,0.,0.)) ;
#61678 = DIRECTION('center_axis',(0.,1.,5.60383084497445E-34)) ;
#61679 = DIRECTION('ref_axis',(1.,0.,0.)) ;
#61680 = DIRECTION('center_axis',(2.52374105052742E-18,5.60383084497445E-34,
-1.)) ;
#61681 = DIRECTION('ref_axis',(1.,3.40207761657885E-68,2.52374105052742E-18)) ;
#61682 = DIRECTION('center_axis',(2.52374105052742E-18,5.60383084497445E-34,
-1.)) ;
#61683 = DIRECTION('ref_axis',(1.,3.40207761657885E-68,2.52374105052742E-18)) ;
#61684 = DIRECTION('center_axis',(0.,5.60383084497445E-34,-1.)) ;
#61685 = DIRECTION('ref_axis',(-1.,0.,0.)) ;
#61686 = DIRECTION('center_axis',(0.,0.,-1.)) ;
#61687 = DIRECTION('ref_axis',(1.,0.,0.)) ;
#61688 = DIRECTION('',(0.,0.,-1.)) ;
#61689 = DIRECTION('center_axis',(-2.52374105052742E-18,-5.60383084497445E-34,
1.)) ;
#61690 = DIRECTION('ref_axis',(1.,3.40207761657885E-68,2.52374105052742E-18)) ;
#61691 = DIRECTION('center_axis',(0.,0.,-1.)) ;
#61692 = DIRECTION('ref_axis',(1.,0.,0.)) ;
#61693 = DIRECTION('center_axis',(2.52374105052742E-18,5.60383084497445E-34,
-1.)) ;
#61694 = DIRECTION('ref_axis',(1.,3.40207761657885E-68,2.52374105052742E-18)) ;
#61695 = DIRECTION('',(0.,0.,1.)) ;
#61696 = DIRECTION('center_axis',(2.52374105052742E-18,5.60383084497445E-34,
-1.)) ;
#61697 = DIRECTION('ref_axis',(1.,3.40207761657885E-68,2.52374105052742E-18)) ;
#61698 = DIRECTION('axis',(0.,0.,1.)) ;
#61699 = DIRECTION('refdir',(1.,0.,0.)) ;
#61700 = DIRECTION('center_axis',(0.,-5.60383084497445E-34,1.)) ;
#61701 = DIRECTION('ref_axis',(-1.,0.,0.)) ;
#61702 = DIRECTION('center_axis',(0.,5.60383084497445E-34,-1.)) ;
#61703 = DIRECTION('ref_axis',(-1.,0.,0.)) ;
#61704 = DIRECTION('center_axis',(0.,1.,5.60383084497445E-34)) ;
#61705 = DIRECTION('ref_axis',(1.,0.,0.)) ;
#61706 = DIRECTION('center_axis',(2.52374105052742E-18,5.60383084497445E-34,
-1.)) ;
#61707 = DIRECTION('ref_axis',(1.,3.40207761657885E-68,2.52374105052742E-18)) ;
#61708 = DIRECTION('center_axis',(2.52374105052742E-18,5.60383084497445E-34,
-1.)) ;
#61709 = DIRECTION('ref_axis',(1.,3.40207761657885E-68,2.52374105052742E-18)) ;
#61710 = DIRECTION('center_axis',(0.,5.60383084497445E-34,-1.)) ;
#61711 = DIRECTION('ref_axis',(-1.,0.,0.)) ;
#61712 = DIRECTION('center_axis',(0.,0.,-1.)) ;
#61713 = DIRECTION('ref_axis',(1.,0.,0.)) ;
#61714 = DIRECTION('',(0.,0.,-1.)) ;
#61715 = DIRECTION('center_axis',(-2.52374105052742E-18,-5.60383084497445E-34,
1.)) ;
#61716 = DIRECTION('ref_axis',(1.,3.40207761657885E-68,2.52374105052742E-18)) ;
#61717 = DIRECTION('center_axis',(0.,0.,-1.)) ;
#61718 = DIRECTION('ref_axis',(1.,0.,0.)) ;
#61719 = DIRECTION('center_axis',(2.52374105052742E-18,5.60383084497445E-34,
-1.)) ;
#61720 = DIRECTION('ref_axis',(1.,3.40207761657885E-68,2.52374105052742E-18)) ;
#61721 = DIRECTION('',(0.,0.,1.)) ;
#61722 = DIRECTION('center_axis',(2.52374105052742E-18,5.60383084497445E-34,
-1.)) ;
#61723 = DIRECTION('ref_axis',(1.,3.40207761657885E-68,2.52374105052742E-18)) ;
#61724 = DIRECTION('axis',(0.,0.,1.)) ;
#61725 = DIRECTION('refdir',(1.,0.,0.)) ;
#61726 = DIRECTION('center_axis',(-2.52374105052742E-18,-5.60383084497445E-34,
1.)) ;
#61727 = DIRECTION('ref_axis',(1.,0.,0.)) ;
#61728 = DIRECTION('center_axis',(2.52374105052742E-18,5.60383084497445E-34,
-1.)) ;
#61729 = DIRECTION('ref_axis',(1.,1.0086895520954E-34,2.52374105052742E-18)) ;
#61730 = DIRECTION('center_axis',(0.,-1.,-5.60383084497445E-34)) ;
#61731 = DIRECTION('ref_axis',(-1.,0.,0.)) ;
#61732 = DIRECTION('center_axis',(-2.52374105052742E-18,-5.60383084497445E-34,
1.)) ;
#61733 = DIRECTION('ref_axis',(1.,1.0086895520954E-34,2.52374105052742E-18)) ;
#61734 = DIRECTION('center_axis',(0.,0.,-1.)) ;
#61735 = DIRECTION('ref_axis',(1.,0.,0.)) ;
#61736 = DIRECTION('',(0.,0.,-1.)) ;
#61737 = DIRECTION('center_axis',(-2.52374105052742E-18,-5.60383084497445E-34,
1.)) ;
#61738 = DIRECTION('ref_axis',(1.,3.40207761657885E-68,2.52374105052742E-18)) ;
#61739 = DIRECTION('center_axis',(2.52374105052742E-18,5.60383084497445E-34,
-1.)) ;
#61740 = DIRECTION('ref_axis',(1.,3.40207761657885E-68,2.52374105052742E-18)) ;
#61741 = DIRECTION('center_axis',(2.52374105052742E-18,5.60383084497445E-34,
-1.)) ;
#61742 = DIRECTION('ref_axis',(1.,3.40207761657885E-68,2.52374105052742E-18)) ;
#61743 = DIRECTION('center_axis',(0.,0.,-1.)) ;
#61744 = DIRECTION('ref_axis',(1.,0.,0.)) ;
#61745 = DIRECTION('center_axis',(2.52374105052742E-18,5.60383084497445E-34,
-1.)) ;
#61746 = DIRECTION('ref_axis',(1.,3.40207761657885E-68,2.52374105052742E-18)) ;
#61747 = DIRECTION('',(0.,0.,1.)) ;
#61748 = DIRECTION('center_axis',(2.52374105052742E-18,5.60383084497445E-34,
-1.)) ;
#61749 = DIRECTION('ref_axis',(1.,3.40207761657885E-68,2.52374105052742E-18)) ;
#61750 = DIRECTION('axis',(0.,0.,1.)) ;
#61751 = DIRECTION('refdir',(1.,0.,0.)) ;
#61752 = DIRECTION('center_axis',(0.,0.,-1.)) ;
#61753 = DIRECTION('ref_axis',(-1.,0.,0.)) ;
#61754 = DIRECTION('center_axis',(0.,1.,0.)) ;
#61755 = DIRECTION('ref_axis',(-1.,0.,0.)) ;
#61756 = DIRECTION('center_axis',(0.,0.,-1.)) ;
#61757 = DIRECTION('ref_axis',(0.,-1.,0.)) ;
#61758 = DIRECTION('center_axis',(-1.,0.,0.)) ;
#61759 = DIRECTION('ref_axis',(0.,0.,1.)) ;
#61760 = DIRECTION('center_axis',(-2.52374105052742E-18,-5.60383084497445E-34,
1.)) ;
#61761 = DIRECTION('ref_axis',(0.707106781186548,-0.707106781186548,1.7845544107868E-18)) ;
#61762 = DIRECTION('center_axis',(0.,0.,1.)) ;
#61763 = DIRECTION('ref_axis',(0.,-1.,0.)) ;
#61764 = DIRECTION('center_axis',(0.461352736642031,0.887216801234573,0.)) ;
#61765 = DIRECTION('ref_axis',(0.887216801234573,-0.461352736642031,0.)) ;
#61766 = DIRECTION('center_axis',(-0.887216801234586,-0.461352736642007,0.)) ;
#61767 = DIRECTION('ref_axis',(0.461352736642007,-0.887216801234586,0.)) ;
#61768 = DIRECTION('center_axis',(0.,0.,1.)) ;
#61769 = DIRECTION('ref_axis',(0.707106781186547,-0.707106781186547,0.)) ;
#61770 = DIRECTION('',(0.,0.,1.)) ;
#61771 = DIRECTION('',(0.,0.,-1.)) ;
#61772 = DIRECTION('center_axis',(-0.816496580927736,-0.408248290463809,-0.408248290463898)) ;
#61773 = DIRECTION('ref_axis',(-0.577350269189577,0.577350269189695,0.577350269189606)) ;
#61774 = DIRECTION('center_axis',(-1.,0.,0.)) ;
#61775 = DIRECTION('ref_axis',(0.,1.,0.)) ;
#61776 = DIRECTION('center_axis',(0.,0.,1.)) ;
#61777 = DIRECTION('ref_axis',(-1.,0.,0.)) ;
#61778 = DIRECTION('center_axis',(0.,1.,0.)) ;
#61779 = DIRECTION('ref_axis',(0.,0.,1.)) ;
#61780 = DIRECTION('center_axis',(0.,0.,-1.)) ;
#61781 = DIRECTION('ref_axis',(-1.,0.,0.)) ;
#61782 = DIRECTION('center_axis',(0.559857411277938,0.828588968691453,0.)) ;
#61783 = DIRECTION('ref_axis',(0.828588968691453,-0.559857411277938,0.)) ;
#61784 = DIRECTION('center_axis',(0.559857411277938,0.828588968691453,0.)) ;
#61785 = DIRECTION('ref_axis',(0.828588968691453,-0.559857411277938,0.)) ;
#61786 = DIRECTION('center_axis',(-0.82858896869141,-0.559857411278002,0.)) ;
#61787 = DIRECTION('ref_axis',(0.559857411278002,-0.82858896869141,0.)) ;
#61788 = DIRECTION('center_axis',(-0.82858896869141,-0.559857411278002,0.)) ;
#61789 = DIRECTION('ref_axis',(0.559857411278002,-0.82858896869141,0.)) ;
#61790 = DIRECTION('center_axis',(0.,0.,1.)) ;
#61791 = DIRECTION('ref_axis',(-0.707106781186547,0.707106781186547,0.)) ;
#61792 = DIRECTION('',(0.,0.,1.)) ;
#61793 = DIRECTION('',(0.,0.,-1.)) ;
#61794 = DIRECTION('center_axis',(0.,0.,-1.)) ;
#61795 = DIRECTION('ref_axis',(-1.,0.,0.)) ;
#61796 = DIRECTION('center_axis',(-1.,0.,0.)) ;
#61797 = DIRECTION('ref_axis',(0.,-1.,0.)) ;
#61798 = DIRECTION('center_axis',(0.,0.,-1.)) ;
#61799 = DIRECTION('ref_axis',(1.,0.,0.)) ;
#61800 = DIRECTION('center_axis',(0.,-1.,0.)) ;
#61801 = DIRECTION('ref_axis',(0.,0.,1.)) ;
#61802 = DIRECTION('center_axis',(-2.52374105052742E-18,-5.60383084497445E-34,
1.)) ;
#61803 = DIRECTION('ref_axis',(0.707106781186548,0.707106781186548,1.7845544107868E-18)) ;
#61804 = DIRECTION('center_axis',(0.,0.,1.)) ;
#61805 = DIRECTION('ref_axis',(1.,0.,0.)) ;
#61806 = DIRECTION('center_axis',(-0.88721680123456,0.461352736642057,0.)) ;
#61807 = DIRECTION('ref_axis',(0.461352736642057,0.88721680123456,0.)) ;
#61808 = DIRECTION('center_axis',(0.461352736642031,-0.887216801234573,0.)) ;
#61809 = DIRECTION('ref_axis',(0.887216801234573,0.461352736642031,0.)) ;
#61810 = DIRECTION('center_axis',(0.,0.,1.)) ;
#61811 = DIRECTION('ref_axis',(0.707106781186547,0.707106781186547,0.)) ;
#61812 = DIRECTION('',(0.,0.,1.)) ;
#61813 = DIRECTION('',(0.,0.,-1.)) ;
#61814 = DIRECTION('center_axis',(1.41426179436738E-51,-1.,-5.60383084497445E-34)) ;
#61815 = DIRECTION('ref_axis',(-0.707106781186547,-3.96250679110377E-34,0.707106781186547)) ;
#61816 = DIRECTION('',(-1.41426179436738E-51,1.,5.60383084497445E-34)) ;
#61817 = DIRECTION('',(1.41426179436738E-51,-1.,-5.60383084497445E-34)) ;
#61818 = DIRECTION('center_axis',(0.,0.,-1.)) ;
#61819 = DIRECTION('ref_axis',(-1.,0.,0.)) ;
#61820 = DIRECTION('center_axis',(0.,1.,0.)) ;
#61821 = DIRECTION('ref_axis',(-1.,0.,0.)) ;
#61822 = DIRECTION('center_axis',(0.,0.,-1.)) ;
#61823 = DIRECTION('ref_axis',(0.,-1.,0.)) ;
#61824 = DIRECTION('center_axis',(-1.,0.,0.)) ;
#61825 = DIRECTION('ref_axis',(0.,0.,1.)) ;
#61826 = DIRECTION('center_axis',(-2.52374105052742E-18,-5.60383084497445E-34,
1.)) ;
#61827 = DIRECTION('ref_axis',(0.707106781186548,-0.707106781186548,1.7845544107868E-18)) ;
#61828 = DIRECTION('center_axis',(0.,0.,1.)) ;
#61829 = DIRECTION('ref_axis',(0.,-1.,0.)) ;
#61830 = DIRECTION('center_axis',(0.461352736642031,0.887216801234573,0.)) ;
#61831 = DIRECTION('ref_axis',(0.887216801234573,-0.461352736642031,0.)) ;
#61832 = DIRECTION('center_axis',(-0.887216801234586,-0.461352736642007,0.)) ;
#61833 = DIRECTION('ref_axis',(0.461352736642007,-0.887216801234586,0.)) ;
#61834 = DIRECTION('center_axis',(0.,0.,1.)) ;
#61835 = DIRECTION('ref_axis',(0.707106781186547,-0.707106781186547,0.)) ;
#61836 = DIRECTION('',(0.,0.,1.)) ;
#61837 = DIRECTION('',(0.,0.,-1.)) ;
#61838 = DIRECTION('center_axis',(-0.816496580927736,0.408248290463809,-0.408248290463898)) ;
#61839 = DIRECTION('ref_axis',(-0.577350269189577,-0.577350269189695,0.577350269189606)) ;
#61840 = DIRECTION('center_axis',(0.,-1.,0.)) ;
#61841 = DIRECTION('ref_axis',(-1.,0.,0.)) ;
#61842 = DIRECTION('center_axis',(0.,0.,1.)) ;
#61843 = DIRECTION('ref_axis',(0.,-1.,0.)) ;
#61844 = DIRECTION('center_axis',(-1.,0.,0.)) ;
#61845 = DIRECTION('ref_axis',(0.,0.,1.)) ;
#61846 = DIRECTION('center_axis',(0.,0.,-1.)) ;
#61847 = DIRECTION('ref_axis',(0.,-1.,0.)) ;
#61848 = DIRECTION('center_axis',(-0.82858896869141,0.559857411278002,0.)) ;
#61849 = DIRECTION('ref_axis',(0.559857411278002,0.82858896869141,0.)) ;
#61850 = DIRECTION('center_axis',(-0.82858896869141,0.559857411278002,0.)) ;
#61851 = DIRECTION('ref_axis',(0.559857411278002,0.82858896869141,0.)) ;
#61852 = DIRECTION('center_axis',(0.559857411277957,-0.82858896869144,0.)) ;
#61853 = DIRECTION('ref_axis',(0.82858896869144,0.559857411277957,0.)) ;
#61854 = DIRECTION('center_axis',(0.559857411277957,-0.82858896869144,0.)) ;
#61855 = DIRECTION('ref_axis',(0.82858896869144,0.559857411277957,0.)) ;
#61856 = DIRECTION('center_axis',(0.,0.,1.)) ;
#61857 = DIRECTION('ref_axis',(-0.707106781186547,-0.707106781186547,0.)) ;
#61858 = DIRECTION('',(0.,0.,1.)) ;
#61859 = DIRECTION('',(0.,0.,-1.)) ;
#61860 = DIRECTION('center_axis',(1.,0.,2.52374105052742E-18)) ;
#61861 = DIRECTION('ref_axis',(-1.7845544107868E-18,-0.707106781186547,0.707106781186547)) ;
#61862 = DIRECTION('',(-1.,0.,-2.52374105052742E-18)) ;
#61863 = DIRECTION('',(1.,0.,2.52374105052742E-18)) ;
#61864 = DIRECTION('center_axis',(0.,0.,-1.)) ;
#61865 = DIRECTION('ref_axis',(-1.,0.,0.)) ;
#61866 = DIRECTION('center_axis',(1.,0.,0.)) ;
#61867 = DIRECTION('ref_axis',(0.,1.,0.)) ;
#61868 = DIRECTION('center_axis',(0.,0.,-1.)) ;
#61869 = DIRECTION('ref_axis',(-1.,0.,0.)) ;
#61870 = DIRECTION('center_axis',(0.,1.,0.)) ;
#61871 = DIRECTION('ref_axis',(0.,0.,1.)) ;
#61872 = DIRECTION('center_axis',(-2.52374105052742E-18,-5.60383084497445E-34,
1.)) ;
#61873 = DIRECTION('ref_axis',(-0.707106781186548,-0.707106781186548,-1.7845544107868E-18)) ;
#61874 = DIRECTION('center_axis',(0.,0.,1.)) ;
#61875 = DIRECTION('ref_axis',(-1.,0.,0.)) ;
#61876 = DIRECTION('center_axis',(0.88721680123456,-0.461352736642057,0.)) ;
#61877 = DIRECTION('ref_axis',(-0.461352736642057,-0.88721680123456,0.)) ;
#61878 = DIRECTION('center_axis',(-0.461352736642031,0.887216801234573,0.)) ;
#61879 = DIRECTION('ref_axis',(-0.887216801234573,-0.461352736642031,0.)) ;
#61880 = DIRECTION('center_axis',(0.,0.,1.)) ;
#61881 = DIRECTION('ref_axis',(-0.707106781186547,-0.707106781186547,0.)) ;
#61882 = DIRECTION('',(0.,0.,1.)) ;
#61883 = DIRECTION('',(0.,0.,-1.)) ;
#61884 = DIRECTION('center_axis',(0.,0.,-1.)) ;
#61885 = DIRECTION('ref_axis',(-1.,0.,0.)) ;
#61886 = DIRECTION('center_axis',(-1.,0.,0.)) ;
#61887 = DIRECTION('ref_axis',(0.,-1.,0.)) ;
#61888 = DIRECTION('center_axis',(0.,0.,-1.)) ;
#61889 = DIRECTION('ref_axis',(1.,0.,0.)) ;
#61890 = DIRECTION('center_axis',(0.,-1.,0.)) ;
#61891 = DIRECTION('ref_axis',(0.,0.,1.)) ;
#61892 = DIRECTION('center_axis',(-2.52374105052742E-18,-5.60383084497445E-34,
1.)) ;
#61893 = DIRECTION('ref_axis',(0.707106781186548,0.707106781186548,1.7845544107868E-18)) ;
#61894 = DIRECTION('center_axis',(0.,0.,1.)) ;
#61895 = DIRECTION('ref_axis',(1.,0.,0.)) ;
#61896 = DIRECTION('center_axis',(-0.88721680123456,0.461352736642057,0.)) ;
#61897 = DIRECTION('ref_axis',(0.461352736642057,0.88721680123456,0.)) ;
#61898 = DIRECTION('center_axis',(0.461352736642031,-0.887216801234573,0.)) ;
#61899 = DIRECTION('ref_axis',(0.887216801234573,0.461352736642031,0.)) ;
#61900 = DIRECTION('center_axis',(0.,0.,1.)) ;
#61901 = DIRECTION('ref_axis',(0.707106781186547,0.707106781186547,0.)) ;
#61902 = DIRECTION('',(0.,0.,1.)) ;
#61903 = DIRECTION('',(0.,0.,-1.)) ;
#61904 = DIRECTION('center_axis',(1.41426179436738E-51,-1.,-5.60383084497445E-34)) ;
#61905 = DIRECTION('ref_axis',(-0.707106781186547,-3.96250679110377E-34,0.707106781186547)) ;
#61906 = DIRECTION('',(-1.41426179436738E-51,1.,5.60383084497445E-34)) ;
#61907 = DIRECTION('',(1.41426179436738E-51,-1.,-5.60383084497445E-34)) ;
#61908 = DIRECTION('center_axis',(-0.816496580927736,0.408248290463809,0.408248290463898)) ;
#61909 = DIRECTION('ref_axis',(0.577350269189577,0.577350269189695,0.577350269189606)) ;
#61910 = DIRECTION('center_axis',(0.,1.,0.)) ;
#61911 = DIRECTION('ref_axis',(1.,0.,0.)) ;
#61912 = DIRECTION('center_axis',(0.,0.,1.)) ;
#61913 = DIRECTION('ref_axis',(0.,1.,0.)) ;
#61914 = DIRECTION('center_axis',(1.,0.,0.)) ;
#61915 = DIRECTION('ref_axis',(0.,0.,1.)) ;
#61916 = DIRECTION('center_axis',(0.,0.,-1.)) ;
#61917 = DIRECTION('ref_axis',(0.,1.,0.)) ;
#61918 = DIRECTION('center_axis',(0.82858896869141,-0.559857411278002,0.)) ;
#61919 = DIRECTION('ref_axis',(-0.559857411278002,-0.82858896869141,0.)) ;
#61920 = DIRECTION('center_axis',(0.82858896869141,-0.559857411278002,0.)) ;
#61921 = DIRECTION('ref_axis',(-0.559857411278002,-0.82858896869141,0.)) ;
#61922 = DIRECTION('center_axis',(-0.559857411277957,0.82858896869144,0.)) ;
#61923 = DIRECTION('ref_axis',(-0.82858896869144,-0.559857411277957,0.)) ;
#61924 = DIRECTION('center_axis',(-0.559857411277957,0.82858896869144,0.)) ;
#61925 = DIRECTION('ref_axis',(-0.82858896869144,-0.559857411277957,0.)) ;
#61926 = DIRECTION('center_axis',(0.,0.,1.)) ;
#61927 = DIRECTION('ref_axis',(0.707106781186547,0.707106781186547,0.)) ;
#61928 = DIRECTION('',(0.,0.,1.)) ;
#61929 = DIRECTION('',(0.,0.,-1.)) ;
#61930 = DIRECTION('center_axis',(0.,0.,-1.)) ;
#61931 = DIRECTION('ref_axis',(-1.,0.,0.)) ;
#61932 = DIRECTION('center_axis',(0.,-1.,0.)) ;
#61933 = DIRECTION('ref_axis',(1.,0.,0.)) ;
#61934 = DIRECTION('center_axis',(0.,0.,-1.)) ;
#61935 = DIRECTION('ref_axis',(0.,1.,0.)) ;
#61936 = DIRECTION('center_axis',(1.,0.,0.)) ;
#61937 = DIRECTION('ref_axis',(0.,0.,1.)) ;
#61938 = DIRECTION('center_axis',(-2.52374105052742E-18,-5.60383084497445E-34,
1.)) ;
#61939 = DIRECTION('ref_axis',(-0.707106781186548,0.707106781186548,-1.7845544107868E-18)) ;
#61940 = DIRECTION('center_axis',(0.,0.,1.)) ;
#61941 = DIRECTION('ref_axis',(0.,1.,0.)) ;
#61942 = DIRECTION('center_axis',(-0.461352736642031,-0.887216801234573,0.)) ;
#61943 = DIRECTION('ref_axis',(-0.887216801234573,0.461352736642031,0.)) ;
#61944 = DIRECTION('center_axis',(0.887216801234586,0.461352736642007,0.)) ;
#61945 = DIRECTION('ref_axis',(-0.461352736642007,0.887216801234586,0.)) ;
#61946 = DIRECTION('center_axis',(0.,0.,1.)) ;
#61947 = DIRECTION('ref_axis',(-0.707106781186547,0.707106781186547,0.)) ;
#61948 = DIRECTION('',(0.,0.,1.)) ;
#61949 = DIRECTION('',(0.,0.,-1.)) ;
#61950 = DIRECTION('center_axis',(1.,0.,2.52374105052742E-18)) ;
#61951 = DIRECTION('ref_axis',(-1.7845544107868E-18,-0.707106781186547,0.707106781186547)) ;
#61952 = DIRECTION('',(-1.,0.,-2.52374105052742E-18)) ;
#61953 = DIRECTION('',(1.,0.,2.52374105052742E-18)) ;
#61954 = DIRECTION('center_axis',(0.,0.,-1.)) ;
#61955 = DIRECTION('ref_axis',(-1.,0.,0.)) ;
#61956 = DIRECTION('center_axis',(1.,0.,0.)) ;
#61957 = DIRECTION('ref_axis',(0.,1.,0.)) ;
#61958 = DIRECTION('center_axis',(0.,0.,-1.)) ;
#61959 = DIRECTION('ref_axis',(-1.,0.,0.)) ;
#61960 = DIRECTION('center_axis',(0.,1.,0.)) ;
#61961 = DIRECTION('ref_axis',(0.,0.,1.)) ;
#61962 = DIRECTION('center_axis',(-2.52374105052742E-18,-5.60383084497445E-34,
1.)) ;
#61963 = DIRECTION('ref_axis',(-0.707106781186521,-0.707106781186574,-1.78455441078673E-18)) ;
#61964 = DIRECTION('center_axis',(0.,0.,1.)) ;
#61965 = DIRECTION('ref_axis',(-1.,0.,0.)) ;
#61966 = DIRECTION('center_axis',(0.88721680123456,-0.461352736642057,0.)) ;
#61967 = DIRECTION('ref_axis',(-0.461352736642057,-0.88721680123456,0.)) ;
#61968 = DIRECTION('center_axis',(-0.461352736642031,0.887216801234573,0.)) ;
#61969 = DIRECTION('ref_axis',(-0.887216801234573,-0.461352736642031,0.)) ;
#61970 = DIRECTION('center_axis',(0.,0.,1.)) ;
#61971 = DIRECTION('ref_axis',(-0.707106781186495,-0.7071067811866,0.)) ;
#61972 = DIRECTION('',(0.,0.,1.)) ;
#61973 = DIRECTION('',(0.,0.,-1.)) ;
#61974 = DIRECTION('center_axis',(-0.816496580927736,-0.408248290463809,0.408248290463898)) ;
#61975 = DIRECTION('ref_axis',(0.577350269189577,-0.577350269189695,0.577350269189606)) ;
#61976 = DIRECTION('center_axis',(1.,0.,0.)) ;
#61977 = DIRECTION('ref_axis',(0.,-1.,0.)) ;
#61978 = DIRECTION('center_axis',(0.,0.,1.)) ;
#61979 = DIRECTION('ref_axis',(1.,0.,0.)) ;
#61980 = DIRECTION('center_axis',(0.,-1.,0.)) ;
#61981 = DIRECTION('ref_axis',(0.,0.,1.)) ;
#61982 = DIRECTION('center_axis',(0.,0.,-1.)) ;
#61983 = DIRECTION('ref_axis',(1.,0.,0.)) ;
#61984 = DIRECTION('center_axis',(-0.559857411277938,-0.828588968691453,0.)) ;
#61985 = DIRECTION('ref_axis',(-0.828588968691453,0.559857411277938,0.)) ;
#61986 = DIRECTION('center_axis',(-0.559857411277938,-0.828588968691453,0.)) ;
#61987 = DIRECTION('ref_axis',(-0.828588968691453,0.559857411277938,0.)) ;
#61988 = DIRECTION('center_axis',(0.82858896869141,0.559857411278002,0.)) ;
#61989 = DIRECTION('ref_axis',(-0.559857411278002,0.82858896869141,0.)) ;
#61990 = DIRECTION('center_axis',(0.82858896869141,0.559857411278002,0.)) ;
#61991 = DIRECTION('ref_axis',(-0.559857411278002,0.82858896869141,0.)) ;
#61992 = DIRECTION('center_axis',(0.,0.,1.)) ;
#61993 = DIRECTION('ref_axis',(0.707106781186547,-0.707106781186547,0.)) ;
#61994 = DIRECTION('',(0.,0.,1.)) ;
#61995 = DIRECTION('',(0.,0.,-1.)) ;
#61996 = DIRECTION('center_axis',(-1.41426179436738E-51,1.,5.60383084497445E-34)) ;
#61997 = DIRECTION('ref_axis',(0.707106781186547,-3.96250679110377E-34,0.707106781186547)) ;
#61998 = DIRECTION('',(1.41426179436738E-51,-1.,-5.60383084497445E-34)) ;
#61999 = DIRECTION('',(-1.41426179436738E-51,1.,5.60383084497445E-34)) ;
#62000 = DIRECTION('center_axis',(0.,0.,-1.)) ;
#62001 = DIRECTION('ref_axis',(-1.,0.,0.)) ;
#62002 = DIRECTION('center_axis',(0.,-1.,0.)) ;
#62003 = DIRECTION('ref_axis',(1.,0.,0.)) ;
#62004 = DIRECTION('center_axis',(0.,0.,-1.)) ;
#62005 = DIRECTION('ref_axis',(0.,1.,0.)) ;
#62006 = DIRECTION('center_axis',(1.,0.,0.)) ;
#62007 = DIRECTION('ref_axis',(0.,0.,1.)) ;
#62008 = DIRECTION('center_axis',(-2.52374105052742E-18,-5.60383084497445E-34,
1.)) ;
#62009 = DIRECTION('ref_axis',(-0.707106781186548,0.707106781186548,-1.7845544107868E-18)) ;
#62010 = DIRECTION('center_axis',(0.,0.,1.)) ;
#62011 = DIRECTION('ref_axis',(0.,1.,0.)) ;
#62012 = DIRECTION('center_axis',(-0.461352736642031,-0.887216801234573,0.)) ;
#62013 = DIRECTION('ref_axis',(-0.887216801234573,0.461352736642031,0.)) ;
#62014 = DIRECTION('center_axis',(0.887216801234586,0.461352736642007,0.)) ;
#62015 = DIRECTION('ref_axis',(-0.461352736642007,0.887216801234586,0.)) ;
#62016 = DIRECTION('center_axis',(0.,0.,1.)) ;
#62017 = DIRECTION('ref_axis',(-0.707106781186547,0.707106781186547,0.)) ;
#62018 = DIRECTION('',(0.,0.,1.)) ;
#62019 = DIRECTION('',(0.,0.,-1.)) ;
#62020 = DIRECTION('center_axis',(1.,0.,2.52374105052742E-18)) ;
#62021 = DIRECTION('ref_axis',(-1.7845544107868E-18,-0.707106781186547,0.707106781186547)) ;
#62022 = DIRECTION('',(-1.,0.,-2.52374105052742E-18)) ;
#62023 = DIRECTION('',(1.,0.,2.52374105052742E-18)) ;
#62024 = DIRECTION('center_axis',(-1.41426179436738E-51,1.,5.60383084497445E-34)) ;
#62025 = DIRECTION('ref_axis',(0.707106781186495,-3.96250679110407E-34,0.7071067811866)) ;
#62026 = DIRECTION('',(1.41426179436738E-51,-1.,-5.60383084497445E-34)) ;
#62027 = DIRECTION('',(-1.41426179436738E-51,1.,5.60383084497445E-34)) ;
#62028 = DIRECTION('center_axis',(-1.,0.,-2.52374105052742E-18)) ;
#62029 = DIRECTION('ref_axis',(-1.7845544107868E-18,0.707106781186547,0.707106781186547)) ;
#62030 = DIRECTION('',(1.,0.,2.52374105052742E-18)) ;
#62031 = DIRECTION('',(-1.,0.,-2.52374105052742E-18)) ;
#62032 = DIRECTION('center_axis',(-1.41426179436738E-51,1.,5.60383084497445E-34)) ;
#62033 = DIRECTION('ref_axis',(0.707106781186547,-3.96250679110377E-34,0.707106781186547)) ;
#62034 = DIRECTION('',(1.41426179436738E-51,-1.,-5.60383084497445E-34)) ;
#62035 = DIRECTION('',(-1.41426179436738E-51,1.,5.60383084497445E-34)) ;
#62036 = DIRECTION('center_axis',(-1.,0.,-2.52374105052742E-18)) ;
#62037 = DIRECTION('ref_axis',(-1.7845544107868E-18,0.707106781186547,0.707106781186547)) ;
#62038 = DIRECTION('',(1.,0.,2.52374105052742E-18)) ;
#62039 = DIRECTION('',(-1.,0.,-2.52374105052742E-18)) ;
#62040 = DIRECTION('center_axis',(1.41426179436738E-51,-1.,-5.60383084497445E-34)) ;
#62041 = DIRECTION('ref_axis',(-0.707106781186547,-3.96250679110377E-34,0.707106781186547)) ;
#62042 = DIRECTION('',(-1.41426179436738E-51,1.,5.60383084497445E-34)) ;
#62043 = DIRECTION('',(1.41426179436738E-51,-1.,-5.60383084497445E-34)) ;
#62044 = DIRECTION('center_axis',(-1.,0.,-2.52374105052742E-18)) ;
#62045 = DIRECTION('ref_axis',(-1.7845544107868E-18,0.707106781186547,0.707106781186547)) ;
#62046 = DIRECTION('',(1.,0.,2.52374105052742E-18)) ;
#62047 = DIRECTION('',(-1.,0.,-2.52374105052742E-18)) ;
#62048 = DIRECTION('center_axis',(-1.,-1.41426179436738E-51,0.)) ;
#62049 = DIRECTION('ref_axis',(1.41426179436738E-51,-1.,-5.60383084497445E-34)) ;
#62050 = DIRECTION('',(-1.41426179436738E-51,1.,0.)) ;
#62051 = DIRECTION('center_axis',(0.,-1.,0.)) ;
#62052 = DIRECTION('ref_axis',(1.,0.,2.52374105052742E-18)) ;
#62053 = DIRECTION('',(-1.,0.,0.)) ;
#62054 = DIRECTION('center_axis',(1.,0.,0.)) ;
#62055 = DIRECTION('ref_axis',(0.,0.707106781186535,-0.70710678118656)) ;
#62056 = DIRECTION('',(1.,0.,0.)) ;
#62057 = DIRECTION('center_axis',(-1.,-1.41426179436738E-51,0.)) ;
#62058 = DIRECTION('ref_axis',(1.41426179436738E-51,-1.,-5.60383084497445E-34)) ;
#62059 = DIRECTION('',(-1.41426179436738E-51,1.,0.)) ;
#62060 = DIRECTION('center_axis',(1.41426179436738E-51,-1.,0.)) ;
#62061 = DIRECTION('ref_axis',(0.707106781186585,1.00003410517028E-51,-0.70710678118651)) ;
#62062 = DIRECTION('',(1.41426179436738E-51,-1.,0.)) ;
#62063 = DIRECTION('center_axis',(0.,-1.,0.)) ;
#62064 = DIRECTION('ref_axis',(1.,0.,2.52374105052742E-18)) ;
#62065 = DIRECTION('',(-1.,0.,0.)) ;
#62066 = DIRECTION('center_axis',(1.,0.,0.)) ;
#62067 = DIRECTION('ref_axis',(0.,0.707106781186535,-0.70710678118656)) ;
#62068 = DIRECTION('',(1.,0.,0.)) ;
#62069 = DIRECTION('center_axis',(1.,1.41426179436738E-51,0.)) ;
#62070 = DIRECTION('ref_axis',(-1.41426179436738E-51,1.,5.60383084497445E-34)) ;
#62071 = DIRECTION('',(1.41426179436738E-51,-1.,0.)) ;
#62072 = DIRECTION('center_axis',(-1.41426179436738E-51,1.,0.)) ;
#62073 = DIRECTION('ref_axis',(-0.707106781186585,-1.00003410517028E-51,-0.70710678118651)) ;
#62074 = DIRECTION('',(-1.41426179436738E-51,1.,0.)) ;
#62075 = DIRECTION('center_axis',(0.,-1.,0.)) ;
#62076 = DIRECTION('ref_axis',(1.,0.,2.52374105052742E-18)) ;
#62077 = DIRECTION('',(-1.,0.,0.)) ;
#62078 = DIRECTION('center_axis',(1.,0.,0.)) ;
#62079 = DIRECTION('ref_axis',(0.,0.707106781186535,-0.70710678118656)) ;
#62080 = DIRECTION('',(1.,0.,0.)) ;
#62081 = DIRECTION('center_axis',(2.52374105052742E-18,5.60383084497445E-34,
-1.)) ;
#62082 = DIRECTION('ref_axis',(1.,3.40207761657885E-68,2.52374105052742E-18)) ;
#62083 = DIRECTION('center_axis',(2.52374105052742E-18,5.60383084497445E-34,
-1.)) ;
#62084 = DIRECTION('ref_axis',(1.,7.00478855621806E-35,2.52374105052742E-18)) ;
#62085 = DIRECTION('center_axis',(-1.,0.,0.)) ;
#62086 = DIRECTION('ref_axis',(0.,-0.707106781186535,-0.70710678118656)) ;
#62087 = DIRECTION('',(-1.,0.,0.)) ;
#62088 = DIRECTION('',(1.,0.,0.)) ;
#62089 = DIRECTION('center_axis',(-1.41426179436738E-51,1.,0.)) ;
#62090 = DIRECTION('ref_axis',(-0.70710678118656,-1.00003410517025E-51,-0.707106781186535)) ;
#62091 = DIRECTION('',(-1.41426179436738E-51,1.,0.)) ;
#62092 = DIRECTION('',(1.41426179436738E-51,-1.,0.)) ;
#62093 = DIRECTION('center_axis',(1.41426179436738E-51,-1.,0.)) ;
#62094 = DIRECTION('ref_axis',(0.707106781186585,1.00003410517028E-51,-0.70710678118651)) ;
#62095 = DIRECTION('',(1.41426179436738E-51,-1.,0.)) ;
#62096 = DIRECTION('center_axis',(-1.,0.,0.)) ;
#62097 = DIRECTION('ref_axis',(0.,-0.707106781186535,-0.70710678118656)) ;
#62098 = DIRECTION('',(-1.,0.,0.)) ;
#62099 = DIRECTION('',(1.,0.,0.)) ;
#62100 = DIRECTION('center_axis',(1.41426179436738E-51,-1.,0.)) ;
#62101 = DIRECTION('ref_axis',(0.707106781186585,1.00003410517028E-51,-0.70710678118651)) ;
#62102 = DIRECTION('',(1.41426179436738E-51,-1.,0.)) ;
#62103 = DIRECTION('',(-1.41426179436738E-51,1.,0.)) ;
#62104 = DIRECTION('center_axis',(-1.,0.,0.)) ;
#62105 = DIRECTION('ref_axis',(0.,-0.707106781186535,-0.70710678118656)) ;
#62106 = DIRECTION('',(-1.,0.,0.)) ;
#62107 = DIRECTION('',(1.,0.,0.)) ;
#62108 = DIRECTION('center_axis',(-1.41426179436738E-51,1.,0.)) ;
#62109 = DIRECTION('ref_axis',(-0.707106781186585,-1.00003410517028E-51,-0.70710678118651)) ;
#62110 = DIRECTION('',(-1.41426179436738E-51,1.,0.)) ;
#62111 = DIRECTION('',(1.41426179436738E-51,-1.,0.)) ;
#62112 = DIRECTION('center_axis',(0.,1.,0.)) ;
#62113 = DIRECTION('ref_axis',(-1.,0.,-2.52374105052742E-18)) ;
#62114 = DIRECTION('center_axis',(-1.,-1.41426179436738E-51,0.)) ;
#62115 = DIRECTION('ref_axis',(1.41426179436738E-51,-1.,-5.60383084497445E-34)) ;
#62116 = DIRECTION('center_axis',(0.,1.,0.)) ;
#62117 = DIRECTION('ref_axis',(-1.,0.,-2.52374105052742E-18)) ;
#62118 = DIRECTION('center_axis',(1.,1.41426179436738E-51,0.)) ;
#62119 = DIRECTION('ref_axis',(-1.41426179436738E-51,1.,5.60383084497445E-34)) ;
#62120 = DIRECTION('center_axis',(0.,1.,0.)) ;
#62121 = DIRECTION('ref_axis',(-1.,0.,-2.52374105052742E-18)) ;
#62122 = DIRECTION('center_axis',(0.,0.,1.)) ;
#62123 = DIRECTION('ref_axis',(1.,0.,0.)) ;
#62124 = DIRECTION('center_axis',(-2.52374105052742E-18,-5.60383084497445E-34,
1.)) ;
#62125 = DIRECTION('ref_axis',(1.,0.,0.)) ;
#62126 = DIRECTION('center_axis',(0.,-1.,-5.60383084497445E-34)) ;
#62127 = DIRECTION('ref_axis',(-1.,0.,0.)) ;
#62128 = DIRECTION('center_axis',(-2.52374105052742E-18,-5.60383084497445E-34,
1.)) ;
#62129 = DIRECTION('ref_axis',(1.,7.00478855621807E-35,2.52374105052742E-18)) ;
#62130 = DIRECTION('center_axis',(0.,0.,1.)) ;
#62131 = DIRECTION('ref_axis',(1.,0.,0.)) ;
#62132 = DIRECTION('',(0.,0.,-1.)) ;
#62133 = DIRECTION('center_axis',(2.52374105052742E-18,5.60383084497445E-34,
-1.)) ;
#62134 = DIRECTION('ref_axis',(1.,-7.00478855621807E-35,2.52374105052742E-18)) ;
#62135 = DIRECTION('center_axis',(2.52374105052742E-18,5.60383084497445E-34,
-1.)) ;
#62136 = DIRECTION('ref_axis',(1.,-7.00478855621807E-35,2.52374105052742E-18)) ;
#62137 = DIRECTION('center_axis',(2.52374105052742E-18,5.60383084497445E-34,
-1.)) ;
#62138 = DIRECTION('ref_axis',(-1.,0.,0.)) ;
#62139 = DIRECTION('center_axis',(-2.52374105052742E-18,-5.60383084497445E-34,
1.)) ;
#62140 = DIRECTION('ref_axis',(1.,-7.00478855621806E-35,2.52374105052742E-18)) ;
#62141 = DIRECTION('center_axis',(0.,-1.,-5.60383084497445E-34)) ;
#62142 = DIRECTION('ref_axis',(1.,0.,0.)) ;
#62143 = DIRECTION('center_axis',(2.52374105052742E-18,5.60383084497445E-34,
-1.)) ;
#62144 = DIRECTION('ref_axis',(1.,3.40207761657885E-68,2.52374105052742E-18)) ;
#62145 = DIRECTION('center_axis',(1.,1.41426179436738E-51,0.)) ;
#62146 = DIRECTION('ref_axis',(-1.41426179436738E-51,1.,5.60383084497445E-34)) ;
#62147 = DIRECTION('axis',(0.,0.,1.)) ;
#62148 = DIRECTION('refdir',(1.,0.,0.)) ;
#62149 = DIRECTION('center_axis',(-0.81649658092788,0.408248290463869,0.408248290463549)) ;
#62150 = DIRECTION('ref_axis',(0.577350269189413,0.577350269190052,0.577350269189413)) ;
#62151 = DIRECTION('center_axis',(0.,0.,1.)) ;
#62152 = DIRECTION('ref_axis',(0.,1.,0.)) ;
#62153 = DIRECTION('center_axis',(1.,0.,0.)) ;
#62154 = DIRECTION('ref_axis',(0.,0.,1.)) ;
#62155 = DIRECTION('center_axis',(0.,1.,3.55271367880058E-13)) ;
#62156 = DIRECTION('ref_axis',(1.,0.,0.)) ;
#62157 = DIRECTION('center_axis',(-0.816496580927773,0.408248290463798,-0.408248290463833)) ;
#62158 = DIRECTION('ref_axis',(0.577350269189567,0.577350269189673,-0.577350269189638)) ;
#62159 = DIRECTION('center_axis',(0.,1.,0.)) ;
#62160 = DIRECTION('ref_axis',(0.,0.,-1.)) ;
#62161 = DIRECTION('center_axis',(1.,0.,0.)) ;
#62162 = DIRECTION('ref_axis',(0.,1.,0.)) ;
#62163 = DIRECTION('center_axis',(0.,0.,-1.)) ;
#62164 = DIRECTION('ref_axis',(1.,0.,0.)) ;
#62165 = DIRECTION('center_axis',(-0.816496580927773,-0.408248290463798,0.408248290463833)) ;
#62166 = DIRECTION('ref_axis',(-0.577350269189567,0.577350269189673,-0.577350269189638)) ;
#62167 = DIRECTION('center_axis',(0.,1.,0.)) ;
#62168 = DIRECTION('ref_axis',(-1.,0.,0.)) ;
#62169 = DIRECTION('center_axis',(0.,0.,-1.)) ;
#62170 = DIRECTION('ref_axis',(0.,1.,0.)) ;
#62171 = DIRECTION('center_axis',(-1.,0.,0.)) ;
#62172 = DIRECTION('ref_axis',(0.,0.,-1.)) ;
#62173 = DIRECTION('center_axis',(0.,0.,-1.)) ;
#62174 = DIRECTION('ref_axis',(-0.70710678118661,0.707106781186485,0.)) ;
#62175 = DIRECTION('',(0.,0.,-1.)) ;
#62176 = DIRECTION('',(0.,0.,1.)) ;
#62177 = DIRECTION('center_axis',(-0.707106781186548,0.,-0.707106781186548)) ;
#62178 = DIRECTION('ref_axis',(-0.707106781186547,0.,0.707106781186547)) ;
#62179 = DIRECTION('center_axis',(1.,0.,0.)) ;
#62180 = DIRECTION('ref_axis',(0.,0.707106781186485,-0.70710678118661)) ;
#62181 = DIRECTION('',(-1.,0.,0.)) ;
#62182 = DIRECTION('',(1.,0.,0.)) ;
#62183 = DIRECTION('center_axis',(-0.81649658092788,-0.408248290463869,-0.408248290463549)) ;
#62184 = DIRECTION('ref_axis',(0.577350269189413,-0.577350269190052,-0.577350269189413)) ;
#62185 = DIRECTION('center_axis',(0.,0.,-1.)) ;
#62186 = DIRECTION('ref_axis',(0.,-1.,0.)) ;
#62187 = DIRECTION('center_axis',(1.,0.,0.)) ;
#62188 = DIRECTION('ref_axis',(0.,0.,-1.)) ;
#62189 = DIRECTION('center_axis',(0.,-1.,-3.55271367880058E-13)) ;
#62190 = DIRECTION('ref_axis',(1.,0.,0.)) ;
#62191 = DIRECTION('center_axis',(-0.81649658092788,0.408248290463869,0.408248290463549)) ;
#62192 = DIRECTION('ref_axis',(-0.577350269189413,-0.577350269190052,-0.577350269189413)) ;
#62193 = DIRECTION('center_axis',(0.,0.,-1.)) ;
#62194 = DIRECTION('ref_axis',(-1.,0.,0.)) ;
#62195 = DIRECTION('center_axis',(3.55271367880058E-13,-1.,0.)) ;
#62196 = DIRECTION('ref_axis',(0.,0.,-1.)) ;
#62197 = DIRECTION('center_axis',(-1.,0.,0.)) ;
#62198 = DIRECTION('ref_axis',(0.,-1.,0.)) ;
#62199 = DIRECTION('center_axis',(0.,-1.,0.)) ;
#62200 = DIRECTION('ref_axis',(-0.707106781186548,0.,-0.707106781186548)) ;
#62201 = DIRECTION('',(0.,1.,0.)) ;
#62202 = DIRECTION('',(0.,-1.,0.)) ;
#62203 = DIRECTION('center_axis',(1.,0.,0.)) ;
#62204 = DIRECTION('ref_axis',(0.,-0.707106781186736,-0.707106781186359)) ;
#62205 = DIRECTION('',(-1.,0.,0.)) ;
#62206 = DIRECTION('',(1.,0.,0.)) ;
#62207 = DIRECTION('center_axis',(0.,0.,1.)) ;
#62208 = DIRECTION('ref_axis',(-0.70710678118661,-0.707106781186485,0.)) ;
#62209 = DIRECTION('center_axis',(0.,0.,-1.)) ;
#62210 = DIRECTION('ref_axis',(-0.70710678118661,-0.707106781186485,0.)) ;
#62211 = DIRECTION('',(0.,0.,-1.)) ;
#62212 = DIRECTION('',(0.,0.,1.)) ;
#62213 = DIRECTION('center_axis',(0.,1.,0.)) ;
#62214 = DIRECTION('ref_axis',(0.707106781186548,0.,-0.707106781186548)) ;
#62215 = DIRECTION('',(0.,-1.,0.)) ;
#62216 = DIRECTION('',(0.,1.,0.)) ;
#62217 = DIRECTION('center_axis',(0.,0.,-1.)) ;
#62218 = DIRECTION('ref_axis',(0.70710678118661,-0.707106781186485,0.)) ;
#62219 = DIRECTION('',(0.,0.,-1.)) ;
#62220 = DIRECTION('',(0.,0.,1.)) ;
#62221 = DIRECTION('center_axis',(0.,-0.707106781186485,-0.70710678118661)) ;
#62222 = DIRECTION('ref_axis',(0.,-0.70710678118661,0.707106781186485)) ;
#62223 = DIRECTION('center_axis',(0.,0.,1.)) ;
#62224 = DIRECTION('ref_axis',(0.70710678118661,0.707106781186485,0.)) ;
#62225 = DIRECTION('',(0.,0.,-1.)) ;
#62226 = DIRECTION('',(0.,0.,1.)) ;
#62227 = DIRECTION('center_axis',(0.,-1.,0.)) ;
#62228 = DIRECTION('ref_axis',(0.707106781186548,0.,0.707106781186548)) ;
#62229 = DIRECTION('',(0.,1.,0.)) ;
#62230 = DIRECTION('',(0.,-1.,0.)) ;
#62231 = DIRECTION('center_axis',(1.,0.,0.)) ;
#62232 = DIRECTION('ref_axis',(0.,0.707106781186736,0.707106781186359)) ;
#62233 = DIRECTION('',(1.,0.,0.)) ;
#62234 = DIRECTION('',(-1.,0.,0.)) ;
#62235 = DIRECTION('center_axis',(-1.,0.,0.)) ;
#62236 = DIRECTION('ref_axis',(0.,-1.,0.)) ;
#62237 = DIRECTION('',(0.,-1.,0.)) ;
#62238 = DIRECTION('center_axis',(0.,-1.,0.)) ;
#62239 = DIRECTION('ref_axis',(0.,0.,-1.)) ;
#62240 = DIRECTION('',(1.,0.,0.)) ;
#62241 = DIRECTION('center_axis',(0.,1.,0.)) ;
#62242 = DIRECTION('ref_axis',(0.,0.,1.)) ;
#62243 = DIRECTION('center_axis',(0.,0.,-1.)) ;
#62244 = DIRECTION('ref_axis',(0.,1.,0.)) ;
#62245 = DIRECTION('center_axis',(1.,0.,0.)) ;
#62246 = DIRECTION('ref_axis',(0.,0.,-1.)) ;
#62247 = DIRECTION('center_axis',(0.,0.,1.)) ;
#62248 = DIRECTION('ref_axis',(0.,-1.,0.)) ;
#62249 = DIRECTION('axis',(0.,0.,1.)) ;
#62250 = DIRECTION('refdir',(1.,0.,0.)) ;
#62251 = DIRECTION('center_axis',(2.52374105052742E-18,5.60383084497445E-34,
-1.)) ;
#62252 = DIRECTION('ref_axis',(-1.,0.,0.)) ;
#62253 = DIRECTION('center_axis',(-2.52374105052742E-18,-5.60383084497445E-34,
1.)) ;
#62254 = DIRECTION('ref_axis',(1.,-2.80191542248716E-35,2.52374105052742E-18)) ;
#62255 = DIRECTION('center_axis',(0.,-1.,-5.60383084497445E-34)) ;
#62256 = DIRECTION('ref_axis',(1.,0.,0.)) ;
#62257 = DIRECTION('center_axis',(2.52374105052742E-18,5.60383084497445E-34,
-1.)) ;
#62258 = DIRECTION('ref_axis',(1.,-2.80191542248716E-35,2.52374105052742E-18)) ;
#62259 = DIRECTION('center_axis',(2.52374105052742E-18,5.60383084497445E-34,
-1.)) ;
#62260 = DIRECTION('ref_axis',(1.,-2.80191542248716E-35,2.52374105052742E-18)) ;
#62261 = DIRECTION('center_axis',(0.,0.,-1.)) ;
#62262 = DIRECTION('ref_axis',(1.,0.,0.)) ;
#62263 = DIRECTION('',(0.,0.,1.)) ;
#62264 = DIRECTION('center_axis',(-2.52374105052742E-18,-5.60383084497445E-34,
1.)) ;
#62265 = DIRECTION('ref_axis',(1.,5.60383084497445E-35,2.52374105052742E-18)) ;
#62266 = DIRECTION('center_axis',(-2.52374105052742E-18,-5.60383084497445E-34,
1.)) ;
#62267 = DIRECTION('ref_axis',(1.,5.60383084497445E-35,2.52374105052742E-18)) ;
#62268 = DIRECTION('center_axis',(2.52374105052742E-18,5.60383084497445E-34,
-1.)) ;
#62269 = DIRECTION('ref_axis',(1.,3.40207761657885E-68,2.52374105052742E-18)) ;
#62270 = DIRECTION('center_axis',(-1.,0.,-2.52374105052742E-18)) ;
#62271 = DIRECTION('ref_axis',(-1.78455441078696E-18,0.707106781186485,0.70710678118661)) ;
#62272 = DIRECTION('',(1.,0.,2.52374105052742E-18)) ;
#62273 = DIRECTION('center_axis',(-0.70710678118661,-0.707106781186485,0.)) ;
#62274 = DIRECTION('ref_axis',(0.707106781186485,-0.70710678118661,3.56910882157392E-18)) ;
#62275 = DIRECTION('',(-1.,0.,-2.52374105052742E-18)) ;
#62276 = DIRECTION('center_axis',(-0.70710678118661,0.707106781186485,0.)) ;
#62277 = DIRECTION('ref_axis',(-0.707106781186485,-0.70710678118661,-7.92501358220685E-34)) ;
#62278 = DIRECTION('center_axis',(1.41426179436738E-51,-1.,-5.60383084497445E-34)) ;
#62279 = DIRECTION('ref_axis',(-0.707106781186548,-3.96250679110377E-34,0.707106781186548)) ;
#62280 = DIRECTION('',(-1.41426179436738E-51,1.,5.60383084497445E-34)) ;
#62281 = DIRECTION('center_axis',(-0.70710678118661,-0.707106781186485,0.)) ;
#62282 = DIRECTION('ref_axis',(-0.707106781186485,0.70710678118661,7.92501358220685E-34)) ;
#62283 = DIRECTION('',(1.41426179436738E-51,-1.,-5.60383084497445E-34)) ;
#62284 = DIRECTION('center_axis',(-1.,0.,-2.52374105052742E-18)) ;
#62285 = DIRECTION('ref_axis',(-1.78455441078696E-18,0.707106781186485,0.70710678118661)) ;
#62286 = DIRECTION('',(1.,0.,2.52374105052742E-18)) ;
#62287 = DIRECTION('center_axis',(-0.70710678118661,-0.707106781186485,0.)) ;
#62288 = DIRECTION('ref_axis',(0.707106781186485,-0.70710678118661,3.56910882157392E-18)) ;
#62289 = DIRECTION('',(-1.,0.,-2.52374105052742E-18)) ;
#62290 = DIRECTION('center_axis',(1.41426179436738E-51,-1.,-5.60383084497445E-34)) ;
#62291 = DIRECTION('ref_axis',(-0.707106781186548,-3.96250679110377E-34,0.707106781186548)) ;
#62292 = DIRECTION('',(-1.41426179436738E-51,1.,5.60383084497445E-34)) ;
#62293 = DIRECTION('center_axis',(0.70710678118661,-0.707106781186485,0.)) ;
#62294 = DIRECTION('ref_axis',(0.707106781186485,0.70710678118661,7.92501358220685E-34)) ;
#62295 = DIRECTION('',(1.41426179436738E-51,-1.,-5.60383084497445E-34)) ;
#62296 = DIRECTION('center_axis',(1.,0.,2.52374105052742E-18)) ;
#62297 = DIRECTION('ref_axis',(-1.78455441078696E-18,-0.707106781186485,0.70710678118661)) ;
#62298 = DIRECTION('',(-1.,0.,-2.52374105052742E-18)) ;
#62299 = DIRECTION('center_axis',(0.70710678118661,-0.707106781186485,0.)) ;
#62300 = DIRECTION('ref_axis',(-0.707106781186485,-0.70710678118661,-3.56910882157392E-18)) ;
#62301 = DIRECTION('',(1.,0.,2.52374105052742E-18)) ;
#62302 = DIRECTION('center_axis',(1.,0.,2.52374105052742E-18)) ;
#62303 = DIRECTION('ref_axis',(-1.78455441078696E-18,-0.707106781186485,0.70710678118661)) ;
#62304 = DIRECTION('',(-1.,0.,-2.52374105052742E-18)) ;
#62305 = DIRECTION('center_axis',(0.70710678118661,0.707106781186485,0.)) ;
#62306 = DIRECTION('ref_axis',(-0.707106781186485,0.70710678118661,-3.56910882157392E-18)) ;
#62307 = DIRECTION('',(1.,0.,2.52374105052742E-18)) ;
#62308 = DIRECTION('center_axis',(-0.70710678118661,0.707106781186485,0.)) ;
#62309 = DIRECTION('ref_axis',(-0.707106781186485,-0.70710678118661,-3.56910882157392E-18)) ;
#62310 = DIRECTION('center_axis',(-1.41426179436738E-51,1.,5.60383084497445E-34)) ;
#62311 = DIRECTION('ref_axis',(0.707106781186548,-3.96250679110377E-34,0.707106781186548)) ;
#62312 = DIRECTION('',(-1.41426179436738E-51,1.,5.60383084497445E-34)) ;
#62313 = DIRECTION('',(1.41426179436738E-51,-1.,-5.60383084497445E-34)) ;
#62314 = DIRECTION('center_axis',(0.70710678118661,0.707106781186485,0.)) ;
#62315 = DIRECTION('ref_axis',(0.707106781186485,-0.70710678118661,-7.92501358220685E-34)) ;
#62316 = DIRECTION('center_axis',(1.41426179436738E-51,-1.,-5.60383084497445E-34)) ;
#62317 = DIRECTION('ref_axis',(-0.707106781186548,-3.96250679110377E-34,0.707106781186548)) ;
#62318 = DIRECTION('',(-1.41426179436738E-51,1.,5.60383084497445E-34)) ;
#62319 = DIRECTION('',(1.41426179436738E-51,-1.,-5.60383084497445E-34)) ;
#62320 = DIRECTION('center_axis',(1.,0.,2.52374105052742E-18)) ;
#62321 = DIRECTION('ref_axis',(-1.78455441078696E-18,-0.707106781186485,0.70710678118661)) ;
#62322 = DIRECTION('',(1.,0.,2.52374105052742E-18)) ;
#62323 = DIRECTION('',(-1.,0.,-2.52374105052742E-18)) ;
#62324 = DIRECTION('center_axis',(0.70710678118661,0.707106781186485,0.)) ;
#62325 = DIRECTION('ref_axis',(-0.707106781186485,0.70710678118661,-3.56910882157392E-18)) ;
#62326 = DIRECTION('center_axis',(-1.41426179436738E-51,1.,5.60383084497445E-34)) ;
#62327 = DIRECTION('ref_axis',(0.707106781186548,-3.96250679110377E-34,0.707106781186548)) ;
#62328 = DIRECTION('',(-1.41426179436738E-51,1.,5.60383084497445E-34)) ;
#62329 = DIRECTION('',(1.41426179436738E-51,-1.,-5.60383084497445E-34)) ;
#62330 = DIRECTION('center_axis',(-0.70710678118661,0.707106781186485,0.)) ;
#62331 = DIRECTION('ref_axis',(-0.707106781186485,-0.70710678118661,-7.92501358220685E-34)) ;
#62332 = DIRECTION('center_axis',(-1.,0.,-2.52374105052742E-18)) ;
#62333 = DIRECTION('ref_axis',(-1.78455441078696E-18,0.707106781186485,0.70710678118661)) ;
#62334 = DIRECTION('',(-1.,0.,-2.52374105052742E-18)) ;
#62335 = DIRECTION('',(1.,0.,2.52374105052742E-18)) ;
#62336 = DIRECTION('center_axis',(-0.70710678118661,0.707106781186485,0.)) ;
#62337 = DIRECTION('ref_axis',(0.707106781186485,0.70710678118661,3.56910882157392E-18)) ;
#62338 = DIRECTION('center_axis',(-1.41426179436738E-51,1.,5.60383084497445E-34)) ;
#62339 = DIRECTION('ref_axis',(0.707106781186548,-3.96250679110377E-34,0.707106781186548)) ;
#62340 = DIRECTION('',(-1.41426179436738E-51,1.,5.60383084497445E-34)) ;
#62341 = DIRECTION('',(1.41426179436738E-51,-1.,-5.60383084497445E-34)) ;
#62342 = DIRECTION('center_axis',(1.,1.41426179436738E-51,0.)) ;
#62343 = DIRECTION('ref_axis',(1.41426179436738E-51,-1.,-5.60383084497445E-34)) ;
#62344 = DIRECTION('',(0.,0.,-1.)) ;
#62345 = DIRECTION('',(-1.41426179436738E-51,1.,0.)) ;
#62346 = DIRECTION('',(0.,0.,-1.)) ;
#62347 = DIRECTION('center_axis',(0.,-1.,0.)) ;
#62348 = DIRECTION('ref_axis',(-1.,0.,-2.52374105052742E-18)) ;
#62349 = DIRECTION('',(0.,0.,-1.)) ;
#62350 = DIRECTION('',(1.,0.,0.)) ;
#62351 = DIRECTION('center_axis',(1.,1.41426179436738E-51,0.)) ;
#62352 = DIRECTION('ref_axis',(1.41426179436738E-51,-1.,-5.60383084497445E-34)) ;
#62353 = DIRECTION('',(0.,0.,-1.)) ;
#62354 = DIRECTION('',(-1.41426179436738E-51,1.,0.)) ;
#62355 = DIRECTION('center_axis',(0.,1.,0.)) ;
#62356 = DIRECTION('ref_axis',(1.,0.,2.52374105052742E-18)) ;
#62357 = DIRECTION('',(0.,0.,-1.)) ;
#62358 = DIRECTION('',(-1.,0.,0.)) ;
#62359 = DIRECTION('center_axis',(1.,1.41426179436738E-51,0.)) ;
#62360 = DIRECTION('ref_axis',(1.41426179436738E-51,-1.,-5.60383084497445E-34)) ;
#62361 = DIRECTION('',(0.,0.,-1.)) ;
#62362 = DIRECTION('',(-1.41426179436738E-51,1.,0.)) ;
#62363 = DIRECTION('center_axis',(0.,1.,0.)) ;
#62364 = DIRECTION('ref_axis',(1.,0.,2.52374105052742E-18)) ;
#62365 = DIRECTION('',(0.,0.,-1.)) ;
#62366 = DIRECTION('',(-1.,0.,0.)) ;
#62367 = DIRECTION('center_axis',(2.52374105052742E-18,5.60383084497445E-34,
-1.)) ;
#62368 = DIRECTION('ref_axis',(1.,3.40207761657885E-68,2.52374105052742E-18)) ;
#62369 = DIRECTION('center_axis',(2.52374105052742E-18,5.60383084497445E-34,
-1.)) ;
#62370 = DIRECTION('ref_axis',(1.,5.60383084497445E-35,2.52374105052742E-18)) ;
#62371 = DIRECTION('center_axis',(-1.,0.,0.)) ;
#62372 = DIRECTION('ref_axis',(0.,-0.707106781186736,-0.707106781186359)) ;
#62373 = DIRECTION('',(-1.,0.,0.)) ;
#62374 = DIRECTION('center_axis',(-0.707106781186736,0.707106781186359,0.)) ;
#62375 = DIRECTION('ref_axis',(0.707106781186359,0.707106781186736,0.)) ;
#62376 = DIRECTION('',(1.,0.,0.)) ;
#62377 = DIRECTION('center_axis',(-0.707106781186736,0.707106781186359,0.)) ;
#62378 = DIRECTION('ref_axis',(-0.707106781186359,-0.707106781186736,0.)) ;
#62379 = DIRECTION('center_axis',(-1.41426179436738E-51,1.,0.)) ;
#62380 = DIRECTION('ref_axis',(-0.707106781186548,-1.00003410517023E-51,-0.707106781186548)) ;
#62381 = DIRECTION('',(-1.41426179436738E-51,1.,0.)) ;
#62382 = DIRECTION('center_axis',(0.707106781186736,0.707106781186359,0.)) ;
#62383 = DIRECTION('ref_axis',(0.707106781186359,-0.707106781186736,0.)) ;
#62384 = DIRECTION('',(1.41426179436738E-51,-1.,0.)) ;
#62385 = DIRECTION('center_axis',(1.,0.,0.)) ;
#62386 = DIRECTION('ref_axis',(0.,0.707106781186736,-0.707106781186359)) ;
#62387 = DIRECTION('',(1.,0.,0.)) ;
#62388 = DIRECTION('center_axis',(0.707106781186736,0.707106781186359,0.)) ;
#62389 = DIRECTION('ref_axis',(-0.707106781186359,0.707106781186736,0.)) ;
#62390 = DIRECTION('',(-1.,0.,0.)) ;
#62391 = DIRECTION('center_axis',(-1.41426179436738E-51,1.,0.)) ;
#62392 = DIRECTION('ref_axis',(-0.707106781186548,-1.00003410517023E-51,-0.707106781186548)) ;
#62393 = DIRECTION('',(-1.41426179436738E-51,1.,0.)) ;
#62394 = DIRECTION('center_axis',(0.707106781186485,0.70710678118661,0.)) ;
#62395 = DIRECTION('ref_axis',(0.70710678118661,-0.707106781186485,0.)) ;
#62396 = DIRECTION('',(1.41426179436738E-51,-1.,0.)) ;
#62397 = DIRECTION('center_axis',(1.,0.,0.)) ;
#62398 = DIRECTION('ref_axis',(0.,0.707106781186485,-0.70710678118661)) ;
#62399 = DIRECTION('',(1.,0.,0.)) ;
#62400 = DIRECTION('center_axis',(0.707106781186485,-0.70710678118661,0.)) ;
#62401 = DIRECTION('ref_axis',(-0.70710678118661,-0.707106781186485,0.)) ;
#62402 = DIRECTION('center_axis',(1.41426179436738E-51,-1.,0.)) ;
#62403 = DIRECTION('ref_axis',(0.707106781186548,1.00003410517023E-51,-0.707106781186548)) ;
#62404 = DIRECTION('',(1.41426179436738E-51,-1.,0.)) ;
#62405 = DIRECTION('center_axis',(0.707106781186736,-0.707106781186359,0.)) ;
#62406 = DIRECTION('ref_axis',(0.707106781186359,0.707106781186736,0.)) ;
#62407 = DIRECTION('center_axis',(1.,0.,0.)) ;
#62408 = DIRECTION('ref_axis',(0.,0.707106781186736,-0.707106781186359)) ;
#62409 = DIRECTION('',(1.,0.,0.)) ;
#62410 = DIRECTION('center_axis',(0.707106781186736,-0.707106781186359,0.)) ;
#62411 = DIRECTION('ref_axis',(-0.707106781186359,-0.707106781186736,0.)) ;
#62412 = DIRECTION('center_axis',(1.41426179436738E-51,-1.,0.)) ;
#62413 = DIRECTION('ref_axis',(0.707106781186548,1.00003410517023E-51,-0.707106781186548)) ;
#62414 = DIRECTION('',(1.41426179436738E-51,-1.,0.)) ;
#62415 = DIRECTION('center_axis',(-0.707106781186736,-0.707106781186359,0.)) ;
#62416 = DIRECTION('ref_axis',(-0.707106781186359,0.707106781186736,0.)) ;
#62417 = DIRECTION('center_axis',(-1.,0.,0.)) ;
#62418 = DIRECTION('ref_axis',(0.,-0.707106781186736,-0.707106781186359)) ;
#62419 = DIRECTION('',(-1.,0.,0.)) ;
#62420 = DIRECTION('center_axis',(-0.707106781186736,-0.707106781186359,0.)) ;
#62421 = DIRECTION('ref_axis',(0.707106781186359,-0.707106781186736,0.)) ;
#62422 = DIRECTION('center_axis',(1.41426179436738E-51,-1.,0.)) ;
#62423 = DIRECTION('ref_axis',(0.707106781186548,1.00003410517023E-51,-0.707106781186548)) ;
#62424 = DIRECTION('',(1.41426179436738E-51,-1.,0.)) ;
#62425 = DIRECTION('center_axis',(-0.707106781186485,-0.70710678118661,0.)) ;
#62426 = DIRECTION('ref_axis',(-0.70710678118661,0.707106781186485,0.)) ;
#62427 = DIRECTION('center_axis',(-1.,0.,0.)) ;
#62428 = DIRECTION('ref_axis',(0.,-0.707106781186485,-0.70710678118661)) ;
#62429 = DIRECTION('',(1.,0.,0.)) ;
#62430 = DIRECTION('',(-1.,0.,0.)) ;
#62431 = DIRECTION('center_axis',(-0.707106781186485,0.70710678118661,0.)) ;
#62432 = DIRECTION('ref_axis',(0.70710678118661,0.707106781186485,0.)) ;
#62433 = DIRECTION('center_axis',(-1.41426179436738E-51,1.,0.)) ;
#62434 = DIRECTION('ref_axis',(-0.707106781186548,-1.00003410517023E-51,-0.707106781186548)) ;
#62435 = DIRECTION('',(1.41426179436738E-51,-1.,0.)) ;
#62436 = DIRECTION('',(-1.41426179436738E-51,1.,0.)) ;
#62437 = DIRECTION('center_axis',(0.,-1.,0.)) ;
#62438 = DIRECTION('ref_axis',(-1.,0.,-2.52374105052742E-18)) ;
#62439 = DIRECTION('',(0.,0.,-1.)) ;
#62440 = DIRECTION('center_axis',(-1.,-1.41426179436738E-51,0.)) ;
#62441 = DIRECTION('ref_axis',(-1.41426179436738E-51,1.,5.60383084497445E-34)) ;
#62442 = DIRECTION('',(0.,0.,-1.)) ;
#62443 = DIRECTION('center_axis',(0.,-1.,0.)) ;
#62444 = DIRECTION('ref_axis',(-1.,0.,-2.52374105052742E-18)) ;
#62445 = DIRECTION('',(0.,0.,-1.)) ;
#62446 = DIRECTION('center_axis',(0.,0.,-1.)) ;
#62447 = DIRECTION('ref_axis',(-1.,0.,0.)) ;
#62448 = DIRECTION('center_axis',(2.52374105052742E-18,5.60383084497445E-34,
-1.)) ;
#62449 = DIRECTION('ref_axis',(-1.,0.,0.)) ;
#62450 = DIRECTION('center_axis',(0.,-1.,-5.60383084497445E-34)) ;
#62451 = DIRECTION('ref_axis',(1.,0.,0.)) ;
#62452 = DIRECTION('center_axis',(-1.,-1.41426179436738E-51,0.)) ;
#62453 = DIRECTION('ref_axis',(-1.41426179436738E-51,1.,5.60383084497445E-34)) ;
#62454 = DIRECTION('',(0.,0.,-1.)) ;
#62455 = DIRECTION('center_axis',(0.,1.,0.)) ;
#62456 = DIRECTION('ref_axis',(1.,0.,2.52374105052742E-18)) ;
#62457 = DIRECTION('',(0.,0.,-1.)) ;
#62458 = DIRECTION('center_axis',(-1.,-1.41426179436738E-51,0.)) ;
#62459 = DIRECTION('ref_axis',(-1.41426179436738E-51,1.,5.60383084497445E-34)) ;
#62460 = DIRECTION('axis',(0.,0.,1.)) ;
#62461 = DIRECTION('refdir',(1.,0.,0.)) ;
#62462 = DIRECTION('center_axis',(-1.,0.,0.)) ;
#62463 = DIRECTION('ref_axis',(0.,-0.707106781186485,-0.70710678118661)) ;
#62464 = DIRECTION('',(-1.,0.,0.)) ;
#62465 = DIRECTION('center_axis',(-0.70710678118661,0.707106781186485,0.)) ;
#62466 = DIRECTION('ref_axis',(0.707106781186485,0.70710678118661,0.)) ;
#62467 = DIRECTION('',(1.,0.,0.)) ;
#62468 = DIRECTION('center_axis',(-0.70710678118661,0.707106781186485,0.)) ;
#62469 = DIRECTION('ref_axis',(-0.707106781186485,-0.70710678118661,0.)) ;
#62470 = DIRECTION('center_axis',(-1.41426179436738E-51,1.,0.)) ;
#62471 = DIRECTION('ref_axis',(-0.707106781186548,-1.00003410517023E-51,-0.707106781186548)) ;
#62472 = DIRECTION('',(-1.41426179436738E-51,1.,0.)) ;
#62473 = DIRECTION('center_axis',(0.70710678118661,0.707106781186485,0.)) ;
#62474 = DIRECTION('ref_axis',(0.707106781186485,-0.70710678118661,0.)) ;
#62475 = DIRECTION('',(1.41426179436738E-51,-1.,0.)) ;
#62476 = DIRECTION('center_axis',(1.,0.,0.)) ;
#62477 = DIRECTION('ref_axis',(0.,0.707106781186485,-0.70710678118661)) ;
#62478 = DIRECTION('',(1.,0.,0.)) ;
#62479 = DIRECTION('center_axis',(0.70710678118661,0.707106781186485,0.)) ;
#62480 = DIRECTION('ref_axis',(-0.707106781186485,0.70710678118661,0.)) ;
#62481 = DIRECTION('',(-1.,0.,0.)) ;
#62482 = DIRECTION('center_axis',(-1.41426179436738E-51,1.,0.)) ;
#62483 = DIRECTION('ref_axis',(-0.707106781186548,-1.00003410517023E-51,-0.707106781186548)) ;
#62484 = DIRECTION('',(-1.41426179436738E-51,1.,0.)) ;
#62485 = DIRECTION('center_axis',(0.70710678118661,0.707106781186485,0.)) ;
#62486 = DIRECTION('ref_axis',(0.707106781186485,-0.70710678118661,0.)) ;
#62487 = DIRECTION('',(1.41426179436738E-51,-1.,0.)) ;
#62488 = DIRECTION('center_axis',(1.,0.,0.)) ;
#62489 = DIRECTION('ref_axis',(0.,0.707106781186485,-0.70710678118661)) ;
#62490 = DIRECTION('',(1.,0.,0.)) ;
#62491 = DIRECTION('center_axis',(0.70710678118661,-0.707106781186485,0.)) ;
#62492 = DIRECTION('ref_axis',(-0.707106781186485,-0.70710678118661,0.)) ;
#62493 = DIRECTION('',(-1.,0.,0.)) ;
#62494 = DIRECTION('center_axis',(1.41426179436738E-51,-1.,0.)) ;
#62495 = DIRECTION('ref_axis',(0.707106781186548,1.00003410517023E-51,-0.707106781186548)) ;
#62496 = DIRECTION('',(-1.41426179436738E-51,1.,0.)) ;
#62497 = DIRECTION('',(1.41426179436738E-51,-1.,0.)) ;
#62498 = DIRECTION('center_axis',(0.70710678118661,-0.707106781186485,0.)) ;
#62499 = DIRECTION('ref_axis',(0.707106781186485,0.70710678118661,0.)) ;
#62500 = DIRECTION('center_axis',(1.,0.,0.)) ;
#62501 = DIRECTION('ref_axis',(0.,0.707106781186485,-0.70710678118661)) ;
#62502 = DIRECTION('',(-1.,0.,0.)) ;
#62503 = DIRECTION('',(1.,0.,0.)) ;
#62504 = DIRECTION('center_axis',(0.70710678118661,-0.707106781186485,0.)) ;
#62505 = DIRECTION('ref_axis',(-0.707106781186485,-0.70710678118661,0.)) ;
#62506 = DIRECTION('center_axis',(1.41426179436738E-51,-1.,0.)) ;
#62507 = DIRECTION('ref_axis',(0.707106781186548,1.00003410517023E-51,-0.707106781186548)) ;
#62508 = DIRECTION('',(-1.41426179436738E-51,1.,0.)) ;
#62509 = DIRECTION('',(1.41426179436738E-51,-1.,0.)) ;
#62510 = DIRECTION('center_axis',(-0.70710678118661,-0.707106781186485,0.)) ;
#62511 = DIRECTION('ref_axis',(-0.707106781186485,0.70710678118661,0.)) ;
#62512 = DIRECTION('center_axis',(-1.,0.,0.)) ;
#62513 = DIRECTION('ref_axis',(0.,-0.707106781186485,-0.70710678118661)) ;
#62514 = DIRECTION('',(1.,0.,0.)) ;
#62515 = DIRECTION('',(-1.,0.,0.)) ;
#62516 = DIRECTION('center_axis',(-0.70710678118661,-0.707106781186485,0.)) ;
#62517 = DIRECTION('ref_axis',(0.707106781186485,-0.70710678118661,0.)) ;
#62518 = DIRECTION('center_axis',(1.41426179436738E-51,-1.,0.)) ;
#62519 = DIRECTION('ref_axis',(0.707106781186548,1.00003410517023E-51,-0.707106781186548)) ;
#62520 = DIRECTION('',(-1.41426179436738E-51,1.,0.)) ;
#62521 = DIRECTION('',(1.41426179436738E-51,-1.,0.)) ;
#62522 = DIRECTION('center_axis',(-0.70710678118661,-0.707106781186485,0.)) ;
#62523 = DIRECTION('ref_axis',(-0.707106781186485,0.70710678118661,0.)) ;
#62524 = DIRECTION('center_axis',(-1.,0.,0.)) ;
#62525 = DIRECTION('ref_axis',(0.,-0.707106781186485,-0.70710678118661)) ;
#62526 = DIRECTION('',(1.,0.,0.)) ;
#62527 = DIRECTION('',(-1.,0.,0.)) ;
#62528 = DIRECTION('center_axis',(-0.70710678118661,0.707106781186485,0.)) ;
#62529 = DIRECTION('ref_axis',(0.707106781186485,0.70710678118661,0.)) ;
#62530 = DIRECTION('center_axis',(-1.41426179436738E-51,1.,0.)) ;
#62531 = DIRECTION('ref_axis',(-0.707106781186548,-1.00003410517023E-51,-0.707106781186548)) ;
#62532 = DIRECTION('',(1.41426179436738E-51,-1.,0.)) ;
#62533 = DIRECTION('',(-1.41426179436738E-51,1.,0.)) ;
#62534 = DIRECTION('center_axis',(1.,1.41426179436738E-51,0.)) ;
#62535 = DIRECTION('ref_axis',(1.41426179436738E-51,-1.,-5.60383084497445E-34)) ;
#62536 = DIRECTION('',(0.,0.,-1.)) ;
#62537 = DIRECTION('',(1.41426179436738E-51,-1.,-5.60383084497445E-34)) ;
#62538 = DIRECTION('',(0.,0.,-1.)) ;
#62539 = DIRECTION('center_axis',(0.,-1.,0.)) ;
#62540 = DIRECTION('ref_axis',(-1.,0.,-2.52374105052742E-18)) ;
#62541 = DIRECTION('',(0.,0.,-1.)) ;
#62542 = DIRECTION('',(-1.,0.,-2.52374105052742E-18)) ;
#62543 = DIRECTION('center_axis',(1.,1.41426179436738E-51,0.)) ;
#62544 = DIRECTION('ref_axis',(1.41426179436738E-51,-1.,-5.60383084497445E-34)) ;
#62545 = DIRECTION('',(0.,0.,-1.)) ;
#62546 = DIRECTION('',(1.41426179436738E-51,-1.,-5.60383084497445E-34)) ;
#62547 = DIRECTION('center_axis',(0.,-1.,0.)) ;
#62548 = DIRECTION('ref_axis',(-1.,0.,-2.52374105052742E-18)) ;
#62549 = DIRECTION('',(0.,0.,-1.)) ;
#62550 = DIRECTION('',(-1.,0.,-2.52374105052742E-18)) ;
#62551 = DIRECTION('center_axis',(-1.,-1.41426179436738E-51,0.)) ;
#62552 = DIRECTION('ref_axis',(-1.41426179436738E-51,1.,5.60383084497445E-34)) ;
#62553 = DIRECTION('',(0.,0.,-1.)) ;
#62554 = DIRECTION('',(-1.41426179436738E-51,1.,5.60383084497445E-34)) ;
#62555 = DIRECTION('center_axis',(0.,-1.,0.)) ;
#62556 = DIRECTION('ref_axis',(-1.,0.,-2.52374105052742E-18)) ;
#62557 = DIRECTION('',(0.,0.,-1.)) ;
#62558 = DIRECTION('',(-1.,0.,-2.52374105052742E-18)) ;
#62559 = DIRECTION('center_axis',(0.,0.,-1.)) ;
#62560 = DIRECTION('ref_axis',(-1.,0.,0.)) ;
#62561 = DIRECTION('center_axis',(2.52374105052742E-18,5.60383084497445E-34,
-1.)) ;
#62562 = DIRECTION('ref_axis',(-1.,0.,0.)) ;
#62563 = DIRECTION('center_axis',(-2.52374105052742E-18,-5.60383084497445E-34,
1.)) ;
#62564 = DIRECTION('ref_axis',(1.,-2.24153233798974E-35,2.52374105052742E-18)) ;
#62565 = DIRECTION('center_axis',(0.,-1.,-5.60383084497445E-34)) ;
#62566 = DIRECTION('ref_axis',(1.,0.,0.)) ;
#62567 = DIRECTION('center_axis',(2.52374105052742E-18,5.60383084497445E-34,
-1.)) ;
#62568 = DIRECTION('ref_axis',(1.,-2.24153233798974E-35,2.52374105052742E-18)) ;
#62569 = DIRECTION('center_axis',(2.52374105052742E-18,5.60383084497445E-34,
-1.)) ;
#62570 = DIRECTION('ref_axis',(1.,-2.24153233798974E-35,2.52374105052742E-18)) ;
#62571 = DIRECTION('center_axis',(0.,0.,-1.)) ;
#62572 = DIRECTION('ref_axis',(1.,0.,0.)) ;
#62573 = DIRECTION('',(0.,0.,1.)) ;
#62574 = DIRECTION('center_axis',(-2.52374105052742E-18,-5.60383084497445E-34,
1.)) ;
#62575 = DIRECTION('ref_axis',(1.,4.48306467597958E-35,2.52374105052742E-18)) ;
#62576 = DIRECTION('center_axis',(-2.52374105052742E-18,-5.60383084497445E-34,
1.)) ;
#62577 = DIRECTION('ref_axis',(1.,4.48306467597958E-35,2.52374105052742E-18)) ;
#62578 = DIRECTION('center_axis',(2.52374105052742E-18,5.60383084497445E-34,
-1.)) ;
#62579 = DIRECTION('ref_axis',(1.,3.40207761657885E-68,2.52374105052742E-18)) ;
#62580 = DIRECTION('center_axis',(-1.,0.,-2.52374105052742E-18)) ;
#62581 = DIRECTION('ref_axis',(-1.78455441078696E-18,0.707106781186485,0.70710678118661)) ;
#62582 = DIRECTION('',(1.,0.,2.52374105052742E-18)) ;
#62583 = DIRECTION('center_axis',(-0.70710678118661,-0.707106781186485,0.)) ;
#62584 = DIRECTION('ref_axis',(0.707106781186485,-0.70710678118661,3.56910882157392E-18)) ;
#62585 = DIRECTION('center_axis',(-0.70710678118661,0.707106781186485,0.)) ;
#62586 = DIRECTION('ref_axis',(-0.707106781186485,-0.70710678118661,-7.92501358220685E-34)) ;
#62587 = DIRECTION('center_axis',(1.41426179436738E-51,-1.,-5.60383084497445E-34)) ;
#62588 = DIRECTION('ref_axis',(-0.707106781186548,-3.96250679110377E-34,0.707106781186548)) ;
#62589 = DIRECTION('',(-1.41426179436738E-51,1.,5.60383084497445E-34)) ;
#62590 = DIRECTION('center_axis',(-0.70710678118661,-0.707106781186485,0.)) ;
#62591 = DIRECTION('ref_axis',(-0.707106781186485,0.70710678118661,7.92501358220685E-34)) ;
#62592 = DIRECTION('center_axis',(-1.,0.,-2.52374105052742E-18)) ;
#62593 = DIRECTION('ref_axis',(-1.78455441078696E-18,0.707106781186485,0.70710678118661)) ;
#62594 = DIRECTION('',(1.,0.,2.52374105052742E-18)) ;
#62595 = DIRECTION('center_axis',(-0.70710678118661,-0.707106781186485,0.)) ;
#62596 = DIRECTION('ref_axis',(0.707106781186485,-0.70710678118661,3.56910882157392E-18)) ;
#62597 = DIRECTION('center_axis',(1.41426179436738E-51,-1.,-5.60383084497445E-34)) ;
#62598 = DIRECTION('ref_axis',(-0.707106781186548,-3.96250679110377E-34,0.707106781186548)) ;
#62599 = DIRECTION('',(-1.41426179436738E-51,1.,5.60383084497445E-34)) ;
#62600 = DIRECTION('center_axis',(0.70710678118661,-0.707106781186485,0.)) ;
#62601 = DIRECTION('ref_axis',(0.707106781186485,0.70710678118661,7.92501358220685E-34)) ;
#62602 = DIRECTION('center_axis',(1.,0.,2.52374105052742E-18)) ;
#62603 = DIRECTION('ref_axis',(-1.78455441078696E-18,-0.707106781186485,0.70710678118661)) ;
#62604 = DIRECTION('',(-1.,0.,-2.52374105052742E-18)) ;
#62605 = DIRECTION('center_axis',(0.70710678118661,-0.707106781186485,0.)) ;
#62606 = DIRECTION('ref_axis',(-0.707106781186485,-0.70710678118661,-3.56910882157392E-18)) ;
#62607 = DIRECTION('',(1.,0.,2.52374105052742E-18)) ;
#62608 = DIRECTION('center_axis',(1.,0.,2.52374105052742E-18)) ;
#62609 = DIRECTION('ref_axis',(-1.78455441078696E-18,-0.707106781186485,0.70710678118661)) ;
#62610 = DIRECTION('',(-1.,0.,-2.52374105052742E-18)) ;
#62611 = DIRECTION('center_axis',(0.70710678118661,0.707106781186485,0.)) ;
#62612 = DIRECTION('ref_axis',(-0.707106781186485,0.70710678118661,-3.56910882157392E-18)) ;
#62613 = DIRECTION('',(1.,0.,2.52374105052742E-18)) ;
#62614 = DIRECTION('center_axis',(-0.70710678118661,0.707106781186485,0.)) ;
#62615 = DIRECTION('ref_axis',(-0.707106781186485,-0.70710678118661,-3.56910882157392E-18)) ;
#62616 = DIRECTION('center_axis',(-1.41426179436738E-51,1.,5.60383084497445E-34)) ;
#62617 = DIRECTION('ref_axis',(0.707106781186548,-3.96250679110377E-34,0.707106781186548)) ;
#62618 = DIRECTION('',(-1.41426179436738E-51,1.,5.60383084497445E-34)) ;
#62619 = DIRECTION('',(1.41426179436738E-51,-1.,-5.60383084497445E-34)) ;
#62620 = DIRECTION('center_axis',(0.70710678118661,0.707106781186485,0.)) ;
#62621 = DIRECTION('ref_axis',(0.707106781186485,-0.70710678118661,-7.92501358220685E-34)) ;
#62622 = DIRECTION('center_axis',(1.41426179436738E-51,-1.,-5.60383084497445E-34)) ;
#62623 = DIRECTION('ref_axis',(-0.707106781186548,-3.96250679110377E-34,0.707106781186548)) ;
#62624 = DIRECTION('',(-1.41426179436738E-51,1.,5.60383084497445E-34)) ;
#62625 = DIRECTION('',(1.41426179436738E-51,-1.,-5.60383084497445E-34)) ;
#62626 = DIRECTION('center_axis',(1.,0.,2.52374105052742E-18)) ;
#62627 = DIRECTION('ref_axis',(-1.78455441078696E-18,-0.707106781186485,0.70710678118661)) ;
#62628 = DIRECTION('',(1.,0.,2.52374105052742E-18)) ;
#62629 = DIRECTION('',(-1.,0.,-2.52374105052742E-18)) ;
#62630 = DIRECTION('center_axis',(0.70710678118661,0.707106781186485,0.)) ;
#62631 = DIRECTION('ref_axis',(-0.707106781186485,0.70710678118661,-3.56910882157392E-18)) ;
#62632 = DIRECTION('center_axis',(-1.41426179436738E-51,1.,5.60383084497445E-34)) ;
#62633 = DIRECTION('ref_axis',(0.707106781186548,-3.96250679110377E-34,0.707106781186548)) ;
#62634 = DIRECTION('',(-1.41426179436738E-51,1.,5.60383084497445E-34)) ;
#62635 = DIRECTION('',(1.41426179436738E-51,-1.,-5.60383084497445E-34)) ;
#62636 = DIRECTION('center_axis',(-0.70710678118661,0.707106781186485,0.)) ;
#62637 = DIRECTION('ref_axis',(-0.707106781186485,-0.70710678118661,-7.92501358220685E-34)) ;
#62638 = DIRECTION('center_axis',(-1.,0.,-2.52374105052742E-18)) ;
#62639 = DIRECTION('ref_axis',(-1.78455441078696E-18,0.707106781186485,0.70710678118661)) ;
#62640 = DIRECTION('',(1.,0.,2.52374105052742E-18)) ;
#62641 = DIRECTION('center_axis',(-0.70710678118661,0.707106781186485,0.)) ;
#62642 = DIRECTION('ref_axis',(0.707106781186485,0.70710678118661,3.56910882157392E-18)) ;
#62643 = DIRECTION('center_axis',(-1.41426179436738E-51,1.,5.60383084497445E-34)) ;
#62644 = DIRECTION('ref_axis',(0.707106781186548,-3.96250679110377E-34,0.707106781186548)) ;
#62645 = DIRECTION('',(1.41426179436738E-51,-1.,-5.60383084497445E-34)) ;
#62646 = DIRECTION('center_axis',(0.,1.,0.)) ;
#62647 = DIRECTION('ref_axis',(1.,0.,2.52374105052742E-18)) ;
#62648 = DIRECTION('',(0.,0.,-1.)) ;
#62649 = DIRECTION('center_axis',(1.,1.41426179436738E-51,0.)) ;
#62650 = DIRECTION('ref_axis',(1.41426179436738E-51,-1.,-5.60383084497445E-34)) ;
#62651 = DIRECTION('',(0.,0.,-1.)) ;
#62652 = DIRECTION('center_axis',(0.,1.,0.)) ;
#62653 = DIRECTION('ref_axis',(1.,0.,2.52374105052742E-18)) ;
#62654 = DIRECTION('',(0.,0.,-1.)) ;
#62655 = DIRECTION('center_axis',(2.52374105052742E-18,5.60383084497445E-34,
-1.)) ;
#62656 = DIRECTION('ref_axis',(1.,3.40207761657885E-68,2.52374105052742E-18)) ;
#62657 = DIRECTION('center_axis',(2.52374105052742E-18,5.60383084497445E-34,
-1.)) ;
#62658 = DIRECTION('ref_axis',(1.,4.48306467597958E-35,2.52374105052742E-18)) ;
#62659 = DIRECTION('center_axis',(2.52374105052742E-18,5.60383084497445E-34,
-1.)) ;
#62660 = DIRECTION('ref_axis',(-1.,0.,0.)) ;
#62661 = DIRECTION('center_axis',(0.,-1.,-5.60383084497445E-34)) ;
#62662 = DIRECTION('ref_axis',(1.,0.,0.)) ;
#62663 = DIRECTION('center_axis',(-1.,-1.41426179436738E-51,0.)) ;
#62664 = DIRECTION('ref_axis',(-1.41426179436738E-51,1.,5.60383084497445E-34)) ;
#62665 = DIRECTION('',(0.,0.,-1.)) ;
#62666 = DIRECTION('center_axis',(0.,1.,0.)) ;
#62667 = DIRECTION('ref_axis',(1.,0.,2.52374105052742E-18)) ;
#62668 = DIRECTION('',(0.,0.,-1.)) ;
#62669 = DIRECTION('center_axis',(-1.,-1.41426179436738E-51,0.)) ;
#62670 = DIRECTION('ref_axis',(-1.41426179436738E-51,1.,5.60383084497445E-34)) ;
#62671 = DIRECTION('axis',(0.,0.,1.)) ;
#62672 = DIRECTION('refdir',(1.,0.,0.)) ;
#62673 = DIRECTION('center_axis',(-1.,0.,0.)) ;
#62674 = DIRECTION('ref_axis',(0.,-0.707106781186485,-0.70710678118661)) ;
#62675 = DIRECTION('',(-1.,0.,0.)) ;
#62676 = DIRECTION('center_axis',(-0.707106781186626,0.707106781186469,0.)) ;
#62677 = DIRECTION('ref_axis',(0.707106781186469,0.707106781186626,0.)) ;
#62678 = DIRECTION('',(1.,0.,0.)) ;
#62679 = DIRECTION('center_axis',(-0.70710678118661,0.707106781186485,0.)) ;
#62680 = DIRECTION('ref_axis',(-0.707106781186485,-0.70710678118661,0.)) ;
#62681 = DIRECTION('center_axis',(-1.41426179436738E-51,1.,0.)) ;
#62682 = DIRECTION('ref_axis',(-0.707106781186548,-1.00003410517023E-51,-0.707106781186548)) ;
#62683 = DIRECTION('',(-1.41426179436738E-51,1.,0.)) ;
#62684 = DIRECTION('center_axis',(0.707106781186626,0.707106781186469,0.)) ;
#62685 = DIRECTION('ref_axis',(0.707106781186469,-0.707106781186626,0.)) ;
#62686 = DIRECTION('',(1.41426179436738E-51,-1.,0.)) ;
#62687 = DIRECTION('center_axis',(1.,0.,0.)) ;
#62688 = DIRECTION('ref_axis',(0.,0.707106781186485,-0.70710678118661)) ;
#62689 = DIRECTION('',(1.,0.,0.)) ;
#62690 = DIRECTION('center_axis',(0.70710678118661,0.707106781186485,0.)) ;
#62691 = DIRECTION('ref_axis',(-0.707106781186485,0.70710678118661,0.)) ;
#62692 = DIRECTION('',(-1.,0.,0.)) ;
#62693 = DIRECTION('center_axis',(-1.41426179436738E-51,1.,0.)) ;
#62694 = DIRECTION('ref_axis',(-0.707106781186548,-1.00003410517023E-51,-0.707106781186548)) ;
#62695 = DIRECTION('',(-1.41426179436738E-51,1.,0.)) ;
#62696 = DIRECTION('center_axis',(0.70710678118661,0.707106781186485,0.)) ;
#62697 = DIRECTION('ref_axis',(0.707106781186485,-0.70710678118661,0.)) ;
#62698 = DIRECTION('',(1.41426179436738E-51,-1.,0.)) ;
#62699 = DIRECTION('center_axis',(1.,0.,0.)) ;
#62700 = DIRECTION('ref_axis',(0.,0.707106781186485,-0.70710678118661)) ;
#62701 = DIRECTION('',(1.,0.,0.)) ;
#62702 = DIRECTION('center_axis',(0.70710678118661,-0.707106781186485,0.)) ;
#62703 = DIRECTION('ref_axis',(-0.707106781186485,-0.70710678118661,0.)) ;
#62704 = DIRECTION('',(-1.,0.,0.)) ;
#62705 = DIRECTION('center_axis',(1.41426179436738E-51,-1.,0.)) ;
#62706 = DIRECTION('ref_axis',(0.707106781186548,1.00003410517023E-51,-0.707106781186548)) ;
#62707 = DIRECTION('',(-1.41426179436738E-51,1.,0.)) ;
#62708 = DIRECTION('',(1.41426179436738E-51,-1.,0.)) ;
#62709 = DIRECTION('center_axis',(0.70710678118661,-0.707106781186485,0.)) ;
#62710 = DIRECTION('ref_axis',(0.707106781186485,0.70710678118661,0.)) ;
#62711 = DIRECTION('center_axis',(1.,0.,0.)) ;
#62712 = DIRECTION('ref_axis',(0.,0.707106781186485,-0.70710678118661)) ;
#62713 = DIRECTION('',(-1.,0.,0.)) ;
#62714 = DIRECTION('',(1.,0.,0.)) ;
#62715 = DIRECTION('center_axis',(0.707106781186626,-0.707106781186469,0.)) ;
#62716 = DIRECTION('ref_axis',(-0.707106781186469,-0.707106781186626,0.)) ;
#62717 = DIRECTION('center_axis',(1.41426179436738E-51,-1.,0.)) ;
#62718 = DIRECTION('ref_axis',(0.707106781186548,1.00003410517023E-51,-0.707106781186548)) ;
#62719 = DIRECTION('',(-1.41426179436738E-51,1.,0.)) ;
#62720 = DIRECTION('',(1.41426179436738E-51,-1.,0.)) ;
#62721 = DIRECTION('center_axis',(-0.707106781186626,-0.707106781186469,0.)) ;
#62722 = DIRECTION('ref_axis',(-0.707106781186469,0.707106781186626,0.)) ;
#62723 = DIRECTION('center_axis',(-1.,0.,0.)) ;
#62724 = DIRECTION('ref_axis',(0.,-0.707106781186485,-0.70710678118661)) ;
#62725 = DIRECTION('',(1.,0.,0.)) ;
#62726 = DIRECTION('',(-1.,0.,0.)) ;
#62727 = DIRECTION('center_axis',(-0.70710678118661,-0.707106781186485,0.)) ;
#62728 = DIRECTION('ref_axis',(0.707106781186485,-0.70710678118661,0.)) ;
#62729 = DIRECTION('center_axis',(1.41426179436738E-51,-1.,0.)) ;
#62730 = DIRECTION('ref_axis',(0.707106781186548,1.00003410517023E-51,-0.707106781186548)) ;
#62731 = DIRECTION('',(-1.41426179436738E-51,1.,0.)) ;
#62732 = DIRECTION('',(1.41426179436738E-51,-1.,0.)) ;
#62733 = DIRECTION('center_axis',(-0.70710678118661,-0.707106781186485,0.)) ;
#62734 = DIRECTION('ref_axis',(-0.707106781186485,0.70710678118661,0.)) ;
#62735 = DIRECTION('center_axis',(-1.,0.,0.)) ;
#62736 = DIRECTION('ref_axis',(0.,-0.707106781186485,-0.70710678118661)) ;
#62737 = DIRECTION('',(1.,0.,0.)) ;
#62738 = DIRECTION('',(-1.,0.,0.)) ;
#62739 = DIRECTION('center_axis',(-0.70710678118661,0.707106781186485,0.)) ;
#62740 = DIRECTION('ref_axis',(0.707106781186485,0.70710678118661,0.)) ;
#62741 = DIRECTION('center_axis',(-1.41426179436738E-51,1.,0.)) ;
#62742 = DIRECTION('ref_axis',(-0.707106781186548,-1.00003410517023E-51,-0.707106781186548)) ;
#62743 = DIRECTION('',(1.41426179436738E-51,-1.,0.)) ;
#62744 = DIRECTION('',(-1.41426179436738E-51,1.,0.)) ;
#62745 = DIRECTION('center_axis',(1.,1.41426179436738E-51,0.)) ;
#62746 = DIRECTION('ref_axis',(1.41426179436738E-51,-1.,-5.60383084497445E-34)) ;
#62747 = DIRECTION('',(0.,0.,-1.)) ;
#62748 = DIRECTION('',(1.41426179436738E-51,-1.,-5.60383084497445E-34)) ;
#62749 = DIRECTION('',(0.,0.,-1.)) ;
#62750 = DIRECTION('center_axis',(0.,-1.,0.)) ;
#62751 = DIRECTION('ref_axis',(-1.,0.,-2.52374105052742E-18)) ;
#62752 = DIRECTION('',(0.,0.,-1.)) ;
#62753 = DIRECTION('',(-1.,0.,-2.52374105052742E-18)) ;
#62754 = DIRECTION('center_axis',(1.,1.41426179436738E-51,0.)) ;
#62755 = DIRECTION('ref_axis',(1.41426179436738E-51,-1.,-5.60383084497445E-34)) ;
#62756 = DIRECTION('',(0.,0.,-1.)) ;
#62757 = DIRECTION('',(1.41426179436738E-51,-1.,-5.60383084497445E-34)) ;
#62758 = DIRECTION('center_axis',(0.,-1.,0.)) ;
#62759 = DIRECTION('ref_axis',(-1.,0.,-2.52374105052742E-18)) ;
#62760 = DIRECTION('',(0.,0.,-1.)) ;
#62761 = DIRECTION('',(-1.,0.,-2.52374105052742E-18)) ;
#62762 = DIRECTION('center_axis',(-1.,-1.41426179436738E-51,0.)) ;
#62763 = DIRECTION('ref_axis',(-1.41426179436738E-51,1.,5.60383084497445E-34)) ;
#62764 = DIRECTION('',(0.,0.,-1.)) ;
#62765 = DIRECTION('',(-1.41426179436738E-51,1.,5.60383084497445E-34)) ;
#62766 = DIRECTION('center_axis',(0.,-1.,0.)) ;
#62767 = DIRECTION('ref_axis',(-1.,0.,-2.52374105052742E-18)) ;
#62768 = DIRECTION('',(0.,0.,-1.)) ;
#62769 = DIRECTION('',(-1.,0.,-2.52374105052742E-18)) ;
#62770 = DIRECTION('center_axis',(0.,0.,-1.)) ;
#62771 = DIRECTION('ref_axis',(-1.,0.,0.)) ;
#62772 = DIRECTION('center_axis',(2.52374105052742E-18,5.60383084497445E-34,
-1.)) ;
#62773 = DIRECTION('ref_axis',(-1.,0.,0.)) ;
#62774 = DIRECTION('center_axis',(-2.52374105052742E-18,-5.60383084497445E-34,
1.)) ;
#62775 = DIRECTION('ref_axis',(1.,-2.24153233798973E-35,2.52374105052742E-18)) ;
#62776 = DIRECTION('center_axis',(0.,-1.,-5.60383084497445E-34)) ;
#62777 = DIRECTION('ref_axis',(1.,0.,0.)) ;
#62778 = DIRECTION('center_axis',(2.52374105052742E-18,5.60383084497445E-34,
-1.)) ;
#62779 = DIRECTION('ref_axis',(1.,-2.24153233798973E-35,2.52374105052742E-18)) ;
#62780 = DIRECTION('center_axis',(2.52374105052742E-18,5.60383084497445E-34,
-1.)) ;
#62781 = DIRECTION('ref_axis',(1.,-2.24153233798973E-35,2.52374105052742E-18)) ;
#62782 = DIRECTION('center_axis',(0.,0.,-1.)) ;
#62783 = DIRECTION('ref_axis',(1.,0.,0.)) ;
#62784 = DIRECTION('',(0.,0.,1.)) ;
#62785 = DIRECTION('center_axis',(-2.52374105052742E-18,-5.60383084497445E-34,
1.)) ;
#62786 = DIRECTION('ref_axis',(1.,4.48306467597956E-35,2.52374105052742E-18)) ;
#62787 = DIRECTION('center_axis',(-2.52374105052742E-18,-5.60383084497445E-34,
1.)) ;
#62788 = DIRECTION('ref_axis',(1.,4.48306467597956E-35,2.52374105052742E-18)) ;
#62789 = DIRECTION('center_axis',(2.52374105052742E-18,5.60383084497445E-34,
-1.)) ;
#62790 = DIRECTION('ref_axis',(1.,3.40207761657885E-68,2.52374105052742E-18)) ;
#62791 = DIRECTION('center_axis',(-1.,0.,-2.52374105052742E-18)) ;
#62792 = DIRECTION('ref_axis',(-1.78455441078696E-18,0.707106781186485,0.70710678118661)) ;
#62793 = DIRECTION('',(1.,0.,2.52374105052742E-18)) ;
#62794 = DIRECTION('center_axis',(-0.70710678118661,-0.707106781186485,0.)) ;
#62795 = DIRECTION('ref_axis',(0.707106781186485,-0.70710678118661,3.56910882157392E-18)) ;
#62796 = DIRECTION('center_axis',(-0.70710678118661,0.707106781186485,0.)) ;
#62797 = DIRECTION('ref_axis',(-0.707106781186485,-0.70710678118661,-7.92501358220685E-34)) ;
#62798 = DIRECTION('center_axis',(1.41426179436738E-51,-1.,-5.60383084497445E-34)) ;
#62799 = DIRECTION('ref_axis',(-0.707106781186548,-3.96250679110377E-34,0.707106781186548)) ;
#62800 = DIRECTION('',(-1.41426179436738E-51,1.,5.60383084497445E-34)) ;
#62801 = DIRECTION('center_axis',(-0.70710678118661,-0.707106781186485,0.)) ;
#62802 = DIRECTION('ref_axis',(-0.707106781186485,0.70710678118661,7.92501358220685E-34)) ;
#62803 = DIRECTION('center_axis',(-1.,0.,-2.52374105052742E-18)) ;
#62804 = DIRECTION('ref_axis',(-1.78455441078696E-18,0.707106781186485,0.70710678118661)) ;
#62805 = DIRECTION('',(1.,0.,2.52374105052742E-18)) ;
#62806 = DIRECTION('center_axis',(-0.70710678118661,-0.707106781186485,0.)) ;
#62807 = DIRECTION('ref_axis',(0.707106781186485,-0.70710678118661,3.56910882157392E-18)) ;
#62808 = DIRECTION('center_axis',(1.41426179436738E-51,-1.,-5.60383084497445E-34)) ;
#62809 = DIRECTION('ref_axis',(-0.707106781186548,-3.96250679110377E-34,0.707106781186548)) ;
#62810 = DIRECTION('',(-1.41426179436738E-51,1.,5.60383084497445E-34)) ;
#62811 = DIRECTION('center_axis',(0.70710678118661,-0.707106781186485,0.)) ;
#62812 = DIRECTION('ref_axis',(0.707106781186485,0.70710678118661,7.92501358220685E-34)) ;
#62813 = DIRECTION('center_axis',(1.,0.,2.52374105052742E-18)) ;
#62814 = DIRECTION('ref_axis',(-1.78455441078696E-18,-0.707106781186485,0.70710678118661)) ;
#62815 = DIRECTION('',(-1.,0.,-2.52374105052742E-18)) ;
#62816 = DIRECTION('center_axis',(0.70710678118661,-0.707106781186485,0.)) ;
#62817 = DIRECTION('ref_axis',(-0.707106781186485,-0.70710678118661,-3.56910882157392E-18)) ;
#62818 = DIRECTION('',(1.,0.,2.52374105052742E-18)) ;
#62819 = DIRECTION('center_axis',(1.,0.,2.52374105052742E-18)) ;
#62820 = DIRECTION('ref_axis',(-1.78455441078696E-18,-0.707106781186485,0.70710678118661)) ;
#62821 = DIRECTION('',(-1.,0.,-2.52374105052742E-18)) ;
#62822 = DIRECTION('center_axis',(0.70710678118661,0.707106781186485,0.)) ;
#62823 = DIRECTION('ref_axis',(-0.707106781186485,0.70710678118661,-3.56910882157392E-18)) ;
#62824 = DIRECTION('',(1.,0.,2.52374105052742E-18)) ;
#62825 = DIRECTION('center_axis',(-0.70710678118661,0.707106781186485,0.)) ;
#62826 = DIRECTION('ref_axis',(-0.707106781186485,-0.70710678118661,-3.56910882157392E-18)) ;
#62827 = DIRECTION('center_axis',(-1.41426179436738E-51,1.,5.60383084497445E-34)) ;
#62828 = DIRECTION('ref_axis',(0.707106781186548,-3.96250679110377E-34,0.707106781186548)) ;
#62829 = DIRECTION('',(-1.41426179436738E-51,1.,5.60383084497445E-34)) ;
#62830 = DIRECTION('',(1.41426179436738E-51,-1.,-5.60383084497445E-34)) ;
#62831 = DIRECTION('center_axis',(0.70710678118661,0.707106781186485,0.)) ;
#62832 = DIRECTION('ref_axis',(0.707106781186485,-0.70710678118661,-7.92501358220685E-34)) ;
#62833 = DIRECTION('center_axis',(1.41426179436738E-51,-1.,-5.60383084497445E-34)) ;
#62834 = DIRECTION('ref_axis',(-0.707106781186548,-3.96250679110377E-34,0.707106781186548)) ;
#62835 = DIRECTION('',(-1.41426179436738E-51,1.,5.60383084497445E-34)) ;
#62836 = DIRECTION('',(1.41426179436738E-51,-1.,-5.60383084497445E-34)) ;
#62837 = DIRECTION('center_axis',(1.,0.,2.52374105052742E-18)) ;
#62838 = DIRECTION('ref_axis',(-1.78455441078696E-18,-0.707106781186485,0.70710678118661)) ;
#62839 = DIRECTION('',(1.,0.,2.52374105052742E-18)) ;
#62840 = DIRECTION('',(-1.,0.,-2.52374105052742E-18)) ;
#62841 = DIRECTION('center_axis',(0.70710678118661,0.707106781186485,0.)) ;
#62842 = DIRECTION('ref_axis',(-0.707106781186485,0.70710678118661,-3.56910882157392E-18)) ;
#62843 = DIRECTION('center_axis',(-1.41426179436738E-51,1.,5.60383084497445E-34)) ;
#62844 = DIRECTION('ref_axis',(0.707106781186548,-3.96250679110377E-34,0.707106781186548)) ;
#62845 = DIRECTION('',(-1.41426179436738E-51,1.,5.60383084497445E-34)) ;
#62846 = DIRECTION('',(1.41426179436738E-51,-1.,-5.60383084497445E-34)) ;
#62847 = DIRECTION('center_axis',(-0.70710678118661,0.707106781186485,0.)) ;
#62848 = DIRECTION('ref_axis',(-0.707106781186485,-0.70710678118661,-7.92501358220685E-34)) ;
#62849 = DIRECTION('center_axis',(-1.,0.,-2.52374105052742E-18)) ;
#62850 = DIRECTION('ref_axis',(-1.78455441078696E-18,0.707106781186485,0.70710678118661)) ;
#62851 = DIRECTION('',(1.,0.,2.52374105052742E-18)) ;
#62852 = DIRECTION('center_axis',(-0.70710678118661,0.707106781186485,0.)) ;
#62853 = DIRECTION('ref_axis',(0.707106781186485,0.70710678118661,3.56910882157392E-18)) ;
#62854 = DIRECTION('center_axis',(-1.41426179436738E-51,1.,5.60383084497445E-34)) ;
#62855 = DIRECTION('ref_axis',(0.707106781186548,-3.96250679110377E-34,0.707106781186548)) ;
#62856 = DIRECTION('',(1.41426179436738E-51,-1.,-5.60383084497445E-34)) ;
#62857 = DIRECTION('center_axis',(0.,1.,0.)) ;
#62858 = DIRECTION('ref_axis',(1.,0.,2.52374105052742E-18)) ;
#62859 = DIRECTION('',(0.,0.,-1.)) ;
#62860 = DIRECTION('center_axis',(1.,1.41426179436738E-51,0.)) ;
#62861 = DIRECTION('ref_axis',(1.41426179436738E-51,-1.,-5.60383084497445E-34)) ;
#62862 = DIRECTION('',(0.,0.,-1.)) ;
#62863 = DIRECTION('center_axis',(0.,1.,0.)) ;
#62864 = DIRECTION('ref_axis',(1.,0.,2.52374105052742E-18)) ;
#62865 = DIRECTION('',(0.,0.,-1.)) ;
#62866 = DIRECTION('center_axis',(2.52374105052742E-18,5.60383084497445E-34,
-1.)) ;
#62867 = DIRECTION('ref_axis',(1.,3.40207761657885E-68,2.52374105052742E-18)) ;
#62868 = DIRECTION('center_axis',(2.52374105052742E-18,5.60383084497445E-34,
-1.)) ;
#62869 = DIRECTION('ref_axis',(1.,4.48306467597956E-35,2.52374105052742E-18)) ;
#62870 = DIRECTION('center_axis',(2.52374105052742E-18,5.60383084497445E-34,
-1.)) ;
#62871 = DIRECTION('ref_axis',(-1.,0.,0.)) ;
#62872 = DIRECTION('center_axis',(0.,-1.,-5.60383084497445E-34)) ;
#62873 = DIRECTION('ref_axis',(1.,0.,0.)) ;
#62874 = DIRECTION('center_axis',(-1.,-1.41426179436738E-51,0.)) ;
#62875 = DIRECTION('ref_axis',(-1.41426179436738E-51,1.,5.60383084497445E-34)) ;
#62876 = DIRECTION('',(0.,0.,-1.)) ;
#62877 = DIRECTION('center_axis',(0.,1.,0.)) ;
#62878 = DIRECTION('ref_axis',(1.,0.,2.52374105052742E-18)) ;
#62879 = DIRECTION('',(0.,0.,-1.)) ;
#62880 = DIRECTION('center_axis',(-1.,-1.41426179436738E-51,0.)) ;
#62881 = DIRECTION('ref_axis',(-1.41426179436738E-51,1.,5.60383084497445E-34)) ;
#62882 = DIRECTION('axis',(0.,0.,1.)) ;
#62883 = DIRECTION('refdir',(1.,0.,0.)) ;
#62884 = DIRECTION('center_axis',(0.408248290463875,-0.81649658092775,-0.408248290463804)) ;
#62885 = DIRECTION('ref_axis',(0.577350269189578,0.577350269189721,-0.577350269189578)) ;
#62886 = DIRECTION('center_axis',(0.,0.,1.)) ;
#62887 = DIRECTION('ref_axis',(0.,1.,0.)) ;
#62888 = DIRECTION('center_axis',(-1.,0.,0.)) ;
#62889 = DIRECTION('ref_axis',(0.,0.,-1.)) ;
#62890 = DIRECTION('center_axis',(0.,-1.,0.)) ;
#62891 = DIRECTION('ref_axis',(1.,0.,0.)) ;
#62892 = DIRECTION('center_axis',(-0.132437337493908,-0.961810237044439,0.239544191234197)) ;
#62893 = DIRECTION('ref_axis',(0.465369435981278,-0.273717131207721,-0.841730491391326)) ;
#62894 = DIRECTION('center_axis',(0.,-0.808736084303588,0.588171697674497)) ;
#62895 = DIRECTION('ref_axis',(1.,0.,0.)) ;
#62896 = DIRECTION('center_axis',(7.10542735760115E-13,1.,0.)) ;
#62897 = DIRECTION('ref_axis',(0.,0.,-1.)) ;
#62898 = DIRECTION('center_axis',(-1.,0.,0.)) ;
#62899 = DIRECTION('ref_axis',(0.,-0.588171697675046,-0.808736084303189)) ;
#62900 = DIRECTION('center_axis',(1.41426179436738E-51,-1.,-5.60383084497445E-34)) ;
#62901 = DIRECTION('ref_axis',(0.707106781186485,3.96250679110413E-34,-0.70710678118661)) ;
#62902 = DIRECTION('',(-1.41426179436738E-51,1.,5.60383084497445E-34)) ;
#62903 = DIRECTION('',(1.41426179436738E-51,-1.,-5.60383084497445E-34)) ;
#62904 = DIRECTION('center_axis',(-0.408248290463768,-0.816496580927821,-0.408248290463768)) ;
#62905 = DIRECTION('ref_axis',(-0.577350269189673,0.577350269189389,-0.577350269189815)) ;
#62906 = DIRECTION('center_axis',(0.,-1.,0.)) ;
#62907 = DIRECTION('ref_axis',(0.,0.,-1.)) ;
#62908 = DIRECTION('center_axis',(1.,0.,8.88178419700144E-14)) ;
#62909 = DIRECTION('ref_axis',(0.,1.,0.)) ;
#62910 = DIRECTION('center_axis',(0.,0.,1.)) ;
#62911 = DIRECTION('ref_axis',(-1.,0.,0.)) ;
#62912 = DIRECTION('center_axis',(1.,0.,2.52374105052742E-18)) ;
#62913 = DIRECTION('ref_axis',(1.78455441078759E-18,0.707106781186234,-0.707106781186862)) ;
#62914 = DIRECTION('',(-1.,0.,-2.52374105052742E-18)) ;
#62915 = DIRECTION('',(1.,0.,2.52374105052742E-18)) ;
#62916 = DIRECTION('center_axis',(0.,0.,-1.)) ;
#62917 = DIRECTION('ref_axis',(-1.,0.,0.)) ;
#62918 = DIRECTION('center_axis',(0.,0.,-1.)) ;
#62919 = DIRECTION('ref_axis',(1.,0.,0.)) ;
#62920 = DIRECTION('center_axis',(0.,-1.,0.)) ;
#62921 = DIRECTION('ref_axis',(0.,0.,1.)) ;
#62922 = DIRECTION('center_axis',(-2.52374105052742E-18,-5.60383084497445E-34,
1.)) ;
#62923 = DIRECTION('ref_axis',(0.70710678118661,0.707106781186485,1.78455441078696E-18)) ;
#62924 = DIRECTION('center_axis',(-1.,0.,0.)) ;
#62925 = DIRECTION('ref_axis',(0.,-1.,0.)) ;
#62926 = DIRECTION('center_axis',(-2.52374105052742E-18,-5.60383084497445E-34,
1.)) ;
#62927 = DIRECTION('ref_axis',(-5.10157625931022E-17,-1.,-6.89133658777618E-34)) ;
#62928 = DIRECTION('center_axis',(0.,1.,0.)) ;
#62929 = DIRECTION('ref_axis',(-1.,0.,0.)) ;
#62930 = DIRECTION('center_axis',(0.,-0.276379946678477,-0.961048450950316)) ;
#62931 = DIRECTION('ref_axis',(0.,-0.961048450950316,0.276379946678477)) ;
#62932 = DIRECTION('center_axis',(-1.,0.,0.)) ;
#62933 = DIRECTION('ref_axis',(0.,0.,1.)) ;
#62934 = DIRECTION('center_axis',(1.41426179436738E-51,-1.,-5.60383084497445E-34)) ;
#62935 = DIRECTION('ref_axis',(-0.707106781186422,-3.96250679110448E-34,0.707106781186673)) ;
#62936 = DIRECTION('',(-1.41426179436738E-51,1.,5.60383084497445E-34)) ;
#62937 = DIRECTION('',(1.41426179436738E-51,-1.,-5.60383084497445E-34)) ;
#62938 = DIRECTION('center_axis',(-1.14376454575628E-51,0.80873608430319,
-0.588171697675045)) ;
#62939 = DIRECTION('ref_axis',(0.707106781186249,-0.415900195928203,-0.571862769401282)) ;
#62940 = DIRECTION('',(1.14376454575628E-51,-0.80873608430319,0.588171697675045)) ;
#62941 = DIRECTION('',(-1.14376454575628E-51,0.80873608430319,-0.588171697675045)) ;
#62942 = DIRECTION('center_axis',(0.132437337493908,-0.961810237044439,0.239544191234197)) ;
#62943 = DIRECTION('ref_axis',(-0.465369435981306,-0.273717131207737,-0.841730491391305)) ;
#62944 = DIRECTION('center_axis',(8.88082395220738E-13,-0.808736084303066,
0.588171697675215)) ;
#62945 = DIRECTION('ref_axis',(1.19592671626956E-29,-0.588171697675215,-0.808736084303066)) ;
#62946 = DIRECTION('center_axis',(1.,0.,0.)) ;
#62947 = DIRECTION('ref_axis',(0.,0.,-1.)) ;
#62948 = DIRECTION('center_axis',(0.,1.,7.10542735760115E-13)) ;
#62949 = DIRECTION('ref_axis',(-1.,0.,0.)) ;
#62950 = DIRECTION('center_axis',(1.,0.,2.52374105052742E-18)) ;
#62951 = DIRECTION('ref_axis',(2.40003400727798E-18,-0.309244171891167,-0.950982671845994)) ;
#62952 = DIRECTION('',(-1.,0.,-2.52374105052742E-18)) ;
#62953 = DIRECTION('',(1.,0.,2.52374105052742E-18)) ;
#62954 = DIRECTION('center_axis',(-1.41426179436738E-51,1.,5.60383084497445E-34)) ;
#62955 = DIRECTION('ref_axis',(-0.707106781186548,3.96250679110377E-34,-0.707106781186548)) ;
#62956 = DIRECTION('',(1.41426179436738E-51,-1.,-5.60383084497445E-34)) ;
#62957 = DIRECTION('',(-1.41426179436738E-51,1.,5.60383084497445E-34)) ;
#62958 = DIRECTION('center_axis',(0.,0.,1.)) ;
#62959 = DIRECTION('ref_axis',(1.,0.,0.)) ;
#62960 = DIRECTION('center_axis',(-2.52374105052742E-18,-5.60383084497445E-34,
1.)) ;
#62961 = DIRECTION('ref_axis',(-0.707106781186579,0.707106781186516,-1.78455441078688E-18)) ;
#62962 = DIRECTION('center_axis',(0.,-1.,0.)) ;
#62963 = DIRECTION('ref_axis',(1.,0.,0.)) ;
#62964 = DIRECTION('center_axis',(0.,0.,-1.)) ;
#62965 = DIRECTION('ref_axis',(0.,1.,0.)) ;
#62966 = DIRECTION('center_axis',(1.,0.,0.)) ;
#62967 = DIRECTION('ref_axis',(0.,0.,1.)) ;
#62968 = DIRECTION('center_axis',(-2.52374105052742E-18,-5.60383084497445E-34,
1.)) ;
#62969 = DIRECTION('ref_axis',(1.53047287779293E-16,-1.,-1.7413136165696E-34)) ;
#62970 = DIRECTION('center_axis',(1.,0.,0.)) ;
#62971 = DIRECTION('ref_axis',(0.,0.588171697675131,0.808736084303127)) ;
#62972 = DIRECTION('center_axis',(0.,-0.276379946678561,-0.961048450950292)) ;
#62973 = DIRECTION('ref_axis',(0.,-0.961048450950292,0.276379946678561)) ;
#62974 = DIRECTION('center_axis',(0.,1.,0.)) ;
#62975 = DIRECTION('ref_axis',(0.,0.,1.)) ;
#62976 = DIRECTION('center_axis',(-1.41426179436738E-51,1.,5.60383084497445E-34)) ;
#62977 = DIRECTION('ref_axis',(0.707106781186485,-3.96250679110413E-34,0.70710678118661)) ;
#62978 = DIRECTION('',(1.41426179436738E-51,-1.,-5.60383084497445E-34)) ;
#62979 = DIRECTION('',(-1.41426179436738E-51,1.,5.60383084497445E-34)) ;
#62980 = DIRECTION('center_axis',(1.,0.,2.52374105052742E-18)) ;
#62981 = DIRECTION('ref_axis',(-2.40003400727851E-18,0.309244171890519,0.950982671846205)) ;
#62982 = DIRECTION('',(-1.,0.,-2.52374105052742E-18)) ;
#62983 = DIRECTION('',(1.,0.,2.52374105052742E-18)) ;
#62984 = DIRECTION('center_axis',(1.14376454575628E-51,-0.80873608430319,
0.588171697675045)) ;
#62985 = DIRECTION('ref_axis',(-0.707106781186659,-0.415900195927963,-0.571862769400951)) ;
#62986 = DIRECTION('',(-1.14376454575628E-51,0.80873608430319,-0.588171697675045)) ;
#62987 = DIRECTION('',(1.14376454575628E-51,-0.80873608430319,0.588171697675045)) ;
#62988 = DIRECTION('center_axis',(0.,0.,1.)) ;
#62989 = DIRECTION('ref_axis',(-0.707106781186862,0.707106781186234,0.)) ;
#62990 = DIRECTION('',(0.,0.,-1.)) ;
#62991 = DIRECTION('',(0.,0.,1.)) ;
#62992 = DIRECTION('center_axis',(1.,0.,2.52374105052742E-18)) ;
#62993 = DIRECTION('ref_axis',(-1.78455441078775E-18,-0.707106781186171,0.707106781186924)) ;
#62994 = DIRECTION('',(-1.,0.,-2.52374105052742E-18)) ;
#62995 = DIRECTION('',(1.,0.,2.52374105052742E-18)) ;
#62996 = DIRECTION('center_axis',(0.,0.,1.)) ;
#62997 = DIRECTION('ref_axis',(0.707106781186799,0.707106781186296,0.)) ;
#62998 = DIRECTION('',(0.,0.,-1.)) ;
#62999 = DIRECTION('',(0.,0.,1.)) ;
#63000 = DIRECTION('center_axis',(2.52374105052742E-18,5.60383084497445E-34,
-1.)) ;
#63001 = DIRECTION('ref_axis',(1.,3.40207761657885E-68,2.52374105052742E-18)) ;
#63002 = DIRECTION('center_axis',(0.,1.,0.)) ;
#63003 = DIRECTION('ref_axis',(-1.,0.,-2.52374105052742E-18)) ;
#63004 = DIRECTION('center_axis',(1.,1.41426179436738E-51,0.)) ;
#63005 = DIRECTION('ref_axis',(-1.41426179436738E-51,1.,5.60383084497445E-34)) ;
#63006 = DIRECTION('center_axis',(-2.04104045499877E-18,0.588171697675045,
0.80873608430319)) ;
#63007 = DIRECTION('ref_axis',(1.,3.0425809505486E-33,2.52374105052742E-18)) ;
#63008 = DIRECTION('center_axis',(-1.,-1.41426179436738E-51,0.)) ;
#63009 = DIRECTION('ref_axis',(1.41426179436738E-51,-1.,-5.60383084497445E-34)) ;
#63010 = DIRECTION('center_axis',(-0.408248290463887,0.408248290463603,-0.816496580927844)) ;
#63011 = DIRECTION('ref_axis',(-0.577350269189626,0.577350269189768,0.577350269189484)) ;
#63012 = DIRECTION('center_axis',(0.,0.,1.)) ;
#63013 = DIRECTION('ref_axis',(-1.,0.,0.)) ;
#63014 = DIRECTION('center_axis',(0.,1.,0.)) ;
#63015 = DIRECTION('ref_axis',(0.,0.,1.)) ;
#63016 = DIRECTION('center_axis',(-1.,0.,8.88178419700144E-14)) ;
#63017 = DIRECTION('ref_axis',(0.,1.,0.)) ;
#63018 = DIRECTION('center_axis',(0.408248290463875,-0.81649658092775,0.408248290463804)) ;
#63019 = DIRECTION('ref_axis',(0.577350269189578,0.577350269189721,0.577350269189578)) ;
#63020 = DIRECTION('center_axis',(0.,0.,1.)) ;
#63021 = DIRECTION('ref_axis',(0.,1.,0.)) ;
#63022 = DIRECTION('center_axis',(1.,0.,0.)) ;
#63023 = DIRECTION('ref_axis',(0.,0.,1.)) ;
#63024 = DIRECTION('center_axis',(0.,1.,0.)) ;
#63025 = DIRECTION('ref_axis',(1.,0.,0.)) ;
#63026 = DIRECTION('center_axis',(1.,0.,2.52374105052742E-18)) ;
#63027 = DIRECTION('ref_axis',(-1.78455441078759E-18,0.707106781186234,0.707106781186862)) ;
#63028 = DIRECTION('',(-1.,0.,-2.52374105052742E-18)) ;
#63029 = DIRECTION('',(1.,0.,2.52374105052742E-18)) ;
#63030 = DIRECTION('center_axis',(-1.41426179436738E-51,1.,5.60383084497445E-34)) ;
#63031 = DIRECTION('ref_axis',(-0.70710678118661,-3.96250679110342E-34,0.707106781186485)) ;
#63032 = DIRECTION('',(-1.41426179436738E-51,1.,5.60383084497445E-34)) ;
#63033 = DIRECTION('',(1.41426179436738E-51,-1.,-5.60383084497445E-34)) ;
#63034 = DIRECTION('center_axis',(-0.707106781186453,0.707106781186642,0.)) ;
#63035 = DIRECTION('ref_axis',(-0.707106781186642,-0.707106781186453,-7.92501358220861E-34)) ;
#63036 = DIRECTION('center_axis',(0.113208280231592,-0.0586760459202665,-0.991837187708834)) ;
#63037 = DIRECTION('ref_axis',(0.880585961402273,-0.456409214963279,0.127510756714242)) ;
#63038 = DIRECTION('center_axis',(0.,-0.855197831554128,0.518301716093163)) ;
#63039 = DIRECTION('ref_axis',(1.,0.,0.)) ;
#63040 = DIRECTION('center_axis',(-7.10542735760115E-13,-1.,0.)) ;
#63041 = DIRECTION('ref_axis',(0.,0.,1.)) ;
#63042 = DIRECTION('center_axis',(1.,0.,0.)) ;
#63043 = DIRECTION('ref_axis',(0.,-0.518301716093565,-0.855197831553884)) ;
#63044 = DIRECTION('center_axis',(1.41426179436738E-51,-1.,-5.60383084497445E-34)) ;
#63045 = DIRECTION('ref_axis',(0.707106781186485,-3.96250679110413E-34,0.70710678118661)) ;
#63046 = DIRECTION('',(-1.41426179436738E-51,1.,5.60383084497445E-34)) ;
#63047 = DIRECTION('',(1.41426179436738E-51,-1.,-5.60383084497445E-34)) ;
#63048 = DIRECTION('center_axis',(-1.,4.16417273337025E-18,-2.52374105052742E-18)) ;
#63049 = DIRECTION('ref_axis',(-4.68966975891094E-18,-0.963119367356714,0.269074495674346)) ;
#63050 = DIRECTION('',(1.,-4.16417273337025E-18,2.52374105052742E-18)) ;
#63051 = DIRECTION('',(-1.,4.16417273337025E-18,-2.52374105052742E-18)) ;
#63052 = DIRECTION('center_axis',(1.,1.41426179436738E-51,0.)) ;
#63053 = DIRECTION('ref_axis',(1.36210292466788E-51,-0.963119367356714,0.269074495674346)) ;
#63054 = DIRECTION('center_axis',(1.20947361979268E-51,-0.855197831554018,
0.518301716093344)) ;
#63055 = DIRECTION('ref_axis',(0.707106781186597,-0.366494658150203,-0.604716185947835)) ;
#63056 = DIRECTION('center_axis',(0.,0.,1.)) ;
#63057 = DIRECTION('ref_axis',(0.,-1.,0.)) ;
#63058 = DIRECTION('',(1.20947361979268E-51,-0.855197831554018,0.518301716093344)) ;
#63059 = DIRECTION('',(-1.20947361979268E-51,0.855197831554018,-0.518301716093344)) ;
#63060 = DIRECTION('center_axis',(0.,0.,-1.)) ;
#63061 = DIRECTION('ref_axis',(0.707106781186799,0.707106781186296,0.)) ;
#63062 = DIRECTION('center_axis',(0.,0.,1.)) ;
#63063 = DIRECTION('ref_axis',(0.707106781186799,0.707106781186296,0.)) ;
#63064 = DIRECTION('',(0.,0.,1.)) ;
#63065 = DIRECTION('',(0.,0.,-1.)) ;
#63066 = DIRECTION('center_axis',(0.,0.,-1.)) ;
#63067 = DIRECTION('ref_axis',(-0.707106781186862,0.707106781186234,0.)) ;
#63068 = DIRECTION('center_axis',(0.,0.,1.)) ;
#63069 = DIRECTION('ref_axis',(-0.707106781186862,0.707106781186234,0.)) ;
#63070 = DIRECTION('',(0.,0.,1.)) ;
#63071 = DIRECTION('',(0.,0.,-1.)) ;
#63072 = DIRECTION('center_axis',(1.,1.41426179436738E-51,0.)) ;
#63073 = DIRECTION('ref_axis',(1.41426179436738E-51,-1.,-5.60383084497445E-34)) ;
#63074 = DIRECTION('',(1.41426179436738E-51,-1.,-5.60383084497445E-34)) ;
#63075 = DIRECTION('center_axis',(0.,0.,-1.)) ;
#63076 = DIRECTION('ref_axis',(-1.,0.,0.)) ;
#63077 = DIRECTION('',(1.,0.,0.)) ;
#63078 = DIRECTION('',(-1.41426179436738E-51,1.,5.60383084497445E-34)) ;
#63079 = DIRECTION('',(1.,0.,2.52374105052742E-18)) ;
#63080 = DIRECTION('center_axis',(0.,-0.518301716093344,-0.855197831554018)) ;
#63081 = DIRECTION('ref_axis',(-1.,0.,0.)) ;
#63082 = DIRECTION('',(-1.20947361979268E-51,0.855197831554018,-0.518301716093344)) ;
#63083 = DIRECTION('center_axis',(2.52374105052742E-18,5.60383084497445E-34,
-1.)) ;
#63084 = DIRECTION('ref_axis',(1.,3.40207761657885E-68,2.52374105052742E-18)) ;
#63085 = DIRECTION('center_axis',(-1.,-1.41426179436738E-51,0.)) ;
#63086 = DIRECTION('ref_axis',(-1.41426179436738E-51,1.,5.60383084497445E-34)) ;
#63087 = DIRECTION('center_axis',(0.,1.,0.)) ;
#63088 = DIRECTION('ref_axis',(1.,0.,2.52374105052742E-18)) ;
#63089 = DIRECTION('axis',(0.,0.,1.)) ;
#63090 = DIRECTION('refdir',(1.,0.,0.)) ;
#63091 = DIRECTION('center_axis',(1.,0.,0.)) ;
#63092 = DIRECTION('ref_axis',(0.,0.,-1.)) ;
#63093 = DIRECTION('center_axis',(0.245297658020056,0.605609246625242,0.757011558281565)) ;
#63094 = DIRECTION('ref_axis',(3.02873619539704E-17,0.780868809443035,-0.624695047554418)) ;
#63095 = DIRECTION('center_axis',(0.245297658020056,0.605609246625242,0.757011558281565)) ;
#63096 = DIRECTION('ref_axis',(3.02873619539704E-17,0.780868809443035,-0.624695047554418)) ;
#63097 = DIRECTION('center_axis',(0.,-1.,0.)) ;
#63098 = DIRECTION('ref_axis',(-1.,0.,0.)) ;
#63099 = DIRECTION('center_axis',(0.,-1.,0.)) ;
#63100 = DIRECTION('ref_axis',(-1.,0.,0.)) ;
#63101 = DIRECTION('center_axis',(0.,1.,0.)) ;
#63102 = DIRECTION('ref_axis',(-1.,0.,0.)) ;
#63103 = DIRECTION('',(-1.,0.,0.)) ;
#63104 = DIRECTION('',(0.,0.,1.)) ;
#63105 = DIRECTION('',(-1.,0.,0.)) ;
#63106 = DIRECTION('',(0.,0.,1.)) ;
#63107 = DIRECTION('',(0.,0.,1.)) ;
#63108 = DIRECTION('',(0.,0.,1.)) ;
#63109 = DIRECTION('',(0.,0.,1.)) ;
#63110 = DIRECTION('',(0.,0.,1.)) ;
#63111 = DIRECTION('',(0.,0.,1.)) ;
#63112 = DIRECTION('center_axis',(0.,-1.,0.)) ;
#63113 = DIRECTION('ref_axis',(1.,0.,0.)) ;
#63114 = DIRECTION('',(1.,0.,0.)) ;
#63115 = DIRECTION('',(0.,0.,1.)) ;
#63116 = DIRECTION('',(1.,0.,0.)) ;
#63117 = DIRECTION('center_axis',(1.,0.,0.)) ;
#63118 = DIRECTION('ref_axis',(0.,1.,0.)) ;
#63119 = DIRECTION('',(0.,1.,0.)) ;
#63120 = DIRECTION('',(0.,1.,0.)) ;
#63121 = DIRECTION('center_axis',(1.,0.,0.)) ;
#63122 = DIRECTION('ref_axis',(0.,1.,0.)) ;
#63123 = DIRECTION('',(0.,1.,0.)) ;
#63124 = DIRECTION('',(0.,0.,1.)) ;
#63125 = DIRECTION('',(0.,1.,0.)) ;
#63126 = DIRECTION('',(0.,0.,1.)) ;
#63127 = DIRECTION('center_axis',(0.,1.,0.)) ;
#63128 = DIRECTION('ref_axis',(-1.,0.,0.)) ;
#63129 = DIRECTION('',(-1.,0.,0.)) ;
#63130 = DIRECTION('',(0.,0.,1.)) ;
#63131 = DIRECTION('',(-1.,0.,0.)) ;
#63132 = DIRECTION('',(0.,0.,1.)) ;
#63133 = DIRECTION('',(0.,0.,1.)) ;
#63134 = DIRECTION('',(0.,0.,1.)) ;
#63135 = DIRECTION('',(0.,0.,1.)) ;
#63136 = DIRECTION('center_axis',(-0.843775502275604,0.536696284465946,0.)) ;
#63137 = DIRECTION('ref_axis',(-0.536696284465946,-0.843775502275604,0.)) ;
#63138 = DIRECTION('',(-0.536696284465946,-0.843775502275604,0.)) ;
#63139 = DIRECTION('',(0.,0.,1.)) ;
#63140 = DIRECTION('',(-0.536696284465946,-0.843775502275604,0.)) ;
#63141 = DIRECTION('center_axis',(0.,1.,0.)) ;
#63142 = DIRECTION('ref_axis',(-1.,0.,0.)) ;
#63143 = DIRECTION('',(-1.,0.,0.)) ;
#63144 = DIRECTION('',(0.,0.,1.)) ;
#63145 = DIRECTION('',(-1.,0.,0.)) ;
#63146 = DIRECTION('center_axis',(0.842616363087172,-0.538514312398237,0.)) ;
#63147 = DIRECTION('ref_axis',(0.538514312398237,0.842616363087172,0.)) ;
#63148 = DIRECTION('',(0.538514312398237,0.842616363087173,0.)) ;
#63149 = DIRECTION('',(0.,0.,1.)) ;
#63150 = DIRECTION('',(0.538514312398237,0.842616363087172,0.)) ;
#63151 = DIRECTION('',(0.,0.,1.)) ;
#63152 = DIRECTION('',(0.,0.,1.)) ;
#63153 = DIRECTION('',(0.,0.,1.)) ;
#63154 = DIRECTION('',(0.,0.,1.)) ;
#63155 = DIRECTION('',(0.,0.,1.)) ;
#63156 = DIRECTION('',(0.,0.,1.)) ;
#63157 = DIRECTION('',(0.,0.,1.)) ;
#63158 = DIRECTION('center_axis',(0.,-1.,0.)) ;
#63159 = DIRECTION('ref_axis',(1.,0.,0.)) ;
#63160 = DIRECTION('',(1.,0.,0.)) ;
#63161 = DIRECTION('',(0.,0.,1.)) ;
#63162 = DIRECTION('',(1.,0.,0.)) ;
#63163 = DIRECTION('center_axis',(-1.,0.,0.)) ;
#63164 = DIRECTION('ref_axis',(0.,-1.,0.)) ;
#63165 = DIRECTION('',(0.,-1.,0.)) ;
#63166 = DIRECTION('',(0.,0.,1.)) ;
#63167 = DIRECTION('',(0.,-1.,0.)) ;
#63168 = DIRECTION('center_axis',(0.,1.,0.)) ;
#63169 = DIRECTION('ref_axis',(-1.,0.,0.)) ;
#63170 = DIRECTION('',(-1.,0.,0.)) ;
#63171 = DIRECTION('',(-1.,0.,0.)) ;
#63172 = DIRECTION('center_axis',(0.,0.,-1.)) ;
#63173 = DIRECTION('ref_axis',(1.,0.,0.)) ;
#63174 = DIRECTION('center_axis',(0.,0.,-1.)) ;
#63175 = DIRECTION('ref_axis',(1.,0.,0.)) ;
#63176 = DIRECTION('',(9.79313055424617E-16,-1.,0.)) ;
#63177 = DIRECTION('',(-1.,4.33257765707378E-15,0.)) ;
#63178 = DIRECTION('center_axis',(0.,0.,1.)) ;
#63179 = DIRECTION('ref_axis',(1.,0.,0.)) ;
#63180 = DIRECTION('',(-1.,4.33257765707378E-15,0.)) ;
#63181 = DIRECTION('center_axis',(0.,0.,-1.)) ;
#63182 = DIRECTION('ref_axis',(-0.933145676371942,0.359498465460357,0.)) ;
#63183 = DIRECTION('',(0.,1.,0.)) ;
#63184 = DIRECTION('center_axis',(0.,0.,1.)) ;
#63185 = DIRECTION('ref_axis',(0.923879532511298,-0.382683432365064,0.)) ;
#63186 = DIRECTION('',(0.70710678118654,0.707106781186555,0.)) ;
#63187 = DIRECTION('center_axis',(0.,0.,-1.)) ;
#63188 = DIRECTION('ref_axis',(-0.744997757011426,0.66706696968741,0.)) ;
#63189 = DIRECTION('center_axis',(0.,0.,1.)) ;
#63190 = DIRECTION('ref_axis',(0.433012701892204,-0.901387818866005,0.)) ;
#63191 = DIRECTION('',(1.,-3.55271367880048E-14,0.)) ;
#63192 = DIRECTION('center_axis',(0.,0.,-1.)) ;
#63193 = DIRECTION('ref_axis',(-0.707106781186519,0.707106781186576,0.)) ;
#63194 = DIRECTION('',(3.67742382159233E-14,1.,0.)) ;
#63195 = DIRECTION('center_axis',(0.,0.,1.)) ;
#63196 = DIRECTION('ref_axis',(0.683460430828417,-0.729987561189802,0.)) ;
#63197 = DIRECTION('',(0.997835226140326,-0.0657636789837963,0.)) ;
#63198 = DIRECTION('center_axis',(0.,0.,1.)) ;
#63199 = DIRECTION('ref_axis',(-0.624947614806638,-0.780666688637023,0.)) ;
#63200 = DIRECTION('',(0.573576436351043,-0.819152044288994,0.)) ;
#63201 = DIRECTION('center_axis',(0.,0.,1.)) ;
#63202 = DIRECTION('ref_axis',(-0.95371695074823,-0.300705799504264,0.)) ;
#63203 = DIRECTION('',(1.38777878078145E-15,-1.,0.)) ;
#63204 = DIRECTION('center_axis',(0.,0.,1.)) ;
#63205 = DIRECTION('ref_axis',(0.,-1.,0.)) ;
#63206 = DIRECTION('',(0.,1.,0.)) ;
#63207 = DIRECTION('',(-1.,0.,0.)) ;
#63208 = DIRECTION('center_axis',(0.,0.,1.)) ;
#63209 = DIRECTION('ref_axis',(0.409537713826739,-0.912293188045141,0.)) ;
#63210 = DIRECTION('',(0.,0.,1.)) ;
#63211 = DIRECTION('center_axis',(0.,0.,1.)) ;
#63212 = DIRECTION('ref_axis',(0.409537713799064,-0.912293188057565,0.)) ;
#63213 = DIRECTION('',(0.,0.,-1.)) ;
#63214 = DIRECTION('',(0.,0.,-1.)) ;
#63215 = DIRECTION('center_axis',(-4.3325776570738E-15,-1.,0.)) ;
#63216 = DIRECTION('ref_axis',(0.,0.,-1.)) ;
#63217 = DIRECTION('center_axis',(1.,0.,0.)) ;
#63218 = DIRECTION('ref_axis',(0.,-1.,0.)) ;
#63219 = DIRECTION('center_axis',(4.3325776570738E-15,1.,0.)) ;
#63220 = DIRECTION('ref_axis',(0.70710678118654,-3.06359504133418E-15,0.707106781186555)) ;
#63221 = DIRECTION('center_axis',(-4.3325776570738E-15,-1.,0.)) ;
#63222 = DIRECTION('ref_axis',(0.70710678118654,-3.06359504133418E-15,0.707106781186555)) ;
#63223 = DIRECTION('center_axis',(-1.,4.3325776570738E-15,0.)) ;
#63224 = DIRECTION('ref_axis',(-3.06359504133427E-15,-0.707106781186561,-0.707106781186534)) ;
#63225 = DIRECTION('center_axis',(1.,0.,0.)) ;
#63226 = DIRECTION('ref_axis',(0.,-1.,0.)) ;
#63227 = DIRECTION('',(1.,-4.3325776570738E-15,0.)) ;
#63228 = DIRECTION('',(-1.,4.3325776570738E-15,0.)) ;
#63229 = DIRECTION('center_axis',(0.,-1.,0.)) ;
#63230 = DIRECTION('ref_axis',(-1.,0.,0.)) ;
#63231 = DIRECTION('center_axis',(0.,0.,1.)) ;
#63232 = DIRECTION('ref_axis',(-0.707106781186558,-0.707106781186537,0.)) ;
#63233 = DIRECTION('center_axis',(0.,0.,-1.)) ;
#63234 = DIRECTION('ref_axis',(-0.707106781186559,-0.707106781186536,0.)) ;
#63235 = DIRECTION('center_axis',(0.,-1.,0.)) ;
#63236 = DIRECTION('ref_axis',(-0.707106781186534,0.,-0.707106781186561)) ;
#63237 = DIRECTION('center_axis',(0.,-1.,0.)) ;
#63238 = DIRECTION('ref_axis',(-1.,0.,0.)) ;
#63239 = DIRECTION('',(0.,-1.,0.)) ;
#63240 = DIRECTION('',(0.,1.,0.)) ;
#63241 = DIRECTION('center_axis',(-1.,-6.18537818639092E-13,1.57759909874306E-11)) ;
#63242 = DIRECTION('ref_axis',(1.56498614886827E-11,0.0935501748139615,0.99561456638213)) ;
#63243 = DIRECTION('center_axis',(1.,0.,0.)) ;
#63244 = DIRECTION('ref_axis',(0.,-1.,0.)) ;
#63245 = DIRECTION('',(0.,0.,-1.)) ;
#63246 = DIRECTION('',(0.,-1.,0.)) ;
#63247 = DIRECTION('',(0.,0.,-1.)) ;
#63248 = DIRECTION('',(0.,-1.,0.)) ;
#63249 = DIRECTION('',(0.,0.,-1.)) ;
#63250 = DIRECTION('center_axis',(0.,0.,1.)) ;
#63251 = DIRECTION('ref_axis',(-0.707106781186548,-0.707106781186548,0.)) ;
#63252 = DIRECTION('',(0.,0.,1.)) ;
#63253 = DIRECTION('center_axis',(0.,0.,-1.)) ;
#63254 = DIRECTION('ref_axis',(-0.707106781186548,-0.707106781186548,0.)) ;
#63255 = DIRECTION('center_axis',(-4.3325776570738E-15,-1.,0.)) ;
#63256 = DIRECTION('ref_axis',(1.,-4.3325776570738E-15,0.)) ;
#63257 = DIRECTION('',(0.,0.,1.)) ;
#63258 = DIRECTION('',(-1.,4.3325776570738E-15,0.)) ;
#63259 = DIRECTION('center_axis',(1.,0.,0.)) ;
#63260 = DIRECTION('ref_axis',(0.,1.,0.)) ;
#63261 = DIRECTION('center_axis',(0.,1.,2.96059473233375E-13)) ;
#63262 = DIRECTION('ref_axis',(1.,0.,0.)) ;
#63263 = DIRECTION('center_axis',(-0.938080487976382,0.346417375542847,-6.15360874332621E-14)) ;
#63264 = DIRECTION('ref_axis',(0.346417375542847,0.938080487976382,-1.9888398296556E-29)) ;
#63265 = DIRECTION('center_axis',(0.,1.,0.)) ;
#63266 = DIRECTION('ref_axis',(0.707106781186534,0.,-0.707106781186561)) ;
#63267 = DIRECTION('center_axis',(0.,1.,0.)) ;
#63268 = DIRECTION('ref_axis',(1.,0.,0.)) ;
#63269 = DIRECTION('',(0.,1.,0.)) ;
#63270 = DIRECTION('',(0.,-1.,0.)) ;
#63271 = DIRECTION('center_axis',(1.,0.,0.)) ;
#63272 = DIRECTION('ref_axis',(0.,-1.,0.)) ;
#63273 = DIRECTION('center_axis',(0.,0.,1.)) ;
#63274 = DIRECTION('ref_axis',(0.707106781186559,-0.707106781186536,0.)) ;
#63275 = DIRECTION('center_axis',(0.,0.,-1.)) ;
#63276 = DIRECTION('ref_axis',(0.707106781186559,-0.707106781186536,0.)) ;
#63277 = DIRECTION('center_axis',(-1.,4.3325776570738E-15,0.)) ;
#63278 = DIRECTION('ref_axis',(-3.06359504133427E-15,-0.707106781186561,-0.707106781186534)) ;
#63279 = DIRECTION('center_axis',(1.,0.,0.)) ;
#63280 = DIRECTION('ref_axis',(0.,-1.,0.)) ;
#63281 = DIRECTION('',(1.,-4.3325776570738E-15,0.)) ;
#63282 = DIRECTION('',(-1.,4.3325776570738E-15,0.)) ;
#63283 = DIRECTION('center_axis',(-4.3325776570738E-15,-1.,0.)) ;
#63284 = DIRECTION('ref_axis',(0.,0.,-1.)) ;
#63285 = DIRECTION('center_axis',(4.3325776570738E-15,1.,0.)) ;
#63286 = DIRECTION('ref_axis',(-0.707106781186536,3.06359504133416E-15,0.707106781186559)) ;
#63287 = DIRECTION('center_axis',(-4.3325776570738E-15,-1.,0.)) ;
#63288 = DIRECTION('ref_axis',(-0.707106781186536,3.06359504133416E-15,0.707106781186559)) ;
#63289 = DIRECTION('center_axis',(-4.3325776570738E-15,-1.,0.)) ;
#63290 = DIRECTION('ref_axis',(1.,-4.3325776570738E-15,0.)) ;
#63291 = DIRECTION('',(0.,0.,-1.)) ;
#63292 = DIRECTION('',(-1.,4.3325776570738E-15,0.)) ;
#63293 = DIRECTION('',(0.,0.,-1.)) ;
#63294 = DIRECTION('center_axis',(0.,0.,1.)) ;
#63295 = DIRECTION('ref_axis',(0.707106781186563,-0.707106781186532,0.)) ;
#63296 = DIRECTION('',(0.,0.,1.)) ;
#63297 = DIRECTION('center_axis',(0.,0.,-1.)) ;
#63298 = DIRECTION('ref_axis',(0.707106781186563,-0.707106781186532,0.)) ;
#63299 = DIRECTION('center_axis',(1.,0.,0.)) ;
#63300 = DIRECTION('ref_axis',(0.,1.,0.)) ;
#63301 = DIRECTION('',(0.,0.,-1.)) ;
#63302 = DIRECTION('',(0.,1.,0.)) ;
#63303 = DIRECTION('',(-0.693108716251782,-0.720833064901858,0.)) ;
#63304 = DIRECTION('center_axis',(0.,1.,0.)) ;
#63305 = DIRECTION('ref_axis',(0.99998238013875,0.,0.00593627930944729)) ;
#63306 = DIRECTION('center_axis',(0.,0.,-1.)) ;
#63307 = DIRECTION('ref_axis',(1.,0.,0.)) ;
#63308 = DIRECTION('',(-1.,0.,0.)) ;
#63309 = DIRECTION('center_axis',(0.,0.707106781186549,-0.707106781186546)) ;
#63310 = DIRECTION('ref_axis',(-1.,0.,0.)) ;
#63311 = DIRECTION('center_axis',(0.,0.707106781186549,-0.707106781186546)) ;
#63312 = DIRECTION('ref_axis',(0.805613740871385,0.418919145253121,0.418919145253123)) ;
#63313 = DIRECTION('',(0.562259334229024,0.584749707598188,0.58474970759819)) ;
#63314 = DIRECTION('center_axis',(0.,0.707106781186549,-0.707106781186546)) ;
#63315 = DIRECTION('ref_axis',(-0.569728896336401,-0.581123474263131,-0.581123474263133)) ;
#63316 = DIRECTION('',(1.,0.,0.)) ;
#63317 = DIRECTION('',(6.28036983473509E-16,-0.707106781186546,-0.707106781186549)) ;
#63318 = DIRECTION('',(1.,0.,0.)) ;
#63319 = DIRECTION('',(8.05175619837834E-16,-0.707106781186546,-0.707106781186549)) ;
#63320 = DIRECTION('center_axis',(0.,-0.707106781186549,0.707106781186546)) ;
#63321 = DIRECTION('ref_axis',(-8.17756488897798E-17,0.707106781186546,0.707106781186549)) ;
#63322 = DIRECTION('',(-1.,0.,0.)) ;
#63323 = DIRECTION('center_axis',(0.,0.707106781186549,-0.707106781186546)) ;
#63324 = DIRECTION('ref_axis',(0.,-0.707106781186546,-0.707106781186549)) ;
#63325 = DIRECTION('',(-1.,0.,0.)) ;
#63326 = DIRECTION('center_axis',(0.,1.,0.)) ;
#63327 = DIRECTION('ref_axis',(-1.,0.,0.)) ;
#63328 = DIRECTION('center_axis',(-0.282166323991552,0.,-0.95936550157127)) ;
#63329 = DIRECTION('ref_axis',(0.95936550157127,0.,-0.282166323991552)) ;
#63330 = DIRECTION('center_axis',(-0.282166323991552,0.,-0.95936550157127)) ;
#63331 = DIRECTION('ref_axis',(0.95936550157127,0.,-0.282166323991552)) ;
#63332 = DIRECTION('center_axis',(0.959365501571273,0.,0.282166323991543)) ;
#63333 = DIRECTION('ref_axis',(0.282166323991543,0.,-0.959365501571273)) ;
#63334 = DIRECTION('center_axis',(0.959365501571273,0.,0.282166323991543)) ;
#63335 = DIRECTION('ref_axis',(0.282166323991543,0.,-0.959365501571273)) ;
#63336 = DIRECTION('center_axis',(0.,-1.,0.)) ;
#63337 = DIRECTION('ref_axis',(-0.707106781186547,0.,0.707106781186547)) ;
#63338 = DIRECTION('center_axis',(0.,1.,0.)) ;
#63339 = DIRECTION('ref_axis',(-1.,0.,0.)) ;
#63340 = DIRECTION('',(0.,-1.,0.)) ;
#63341 = DIRECTION('',(0.,1.,0.)) ;
#63342 = DIRECTION('center_axis',(-0.613629329650984,0.789594228570653,0.)) ;
#63343 = DIRECTION('ref_axis',(-0.672991217643199,-0.523011864576266,0.523011864576303)) ;
#63344 = DIRECTION('center_axis',(0.,0.,-1.)) ;
#63345 = DIRECTION('ref_axis',(-2.27154580249389E-16,1.,0.)) ;
#63346 = DIRECTION('center_axis',(7.1167068359955E-15,-0.274721127897369,
0.961523947640826)) ;
#63347 = DIRECTION('ref_axis',(-6.67584762217264E-30,0.961523947640826,0.274721127897369)) ;
#63348 = DIRECTION('center_axis',(0.,-0.707106781186546,-0.707106781186549)) ;
#63349 = DIRECTION('ref_axis',(0.707106781186519,0.500000000000021,-0.500000000000019)) ;
#63350 = DIRECTION('',(0.,-0.707106781186546,-0.707106781186549)) ;
#63351 = DIRECTION('center_axis',(0.,0.707106781186529,0.707106781186566)) ;
#63352 = DIRECTION('ref_axis',(1.,0.,0.)) ;
#63353 = DIRECTION('',(0.,0.707106781186546,0.707106781186549)) ;
#63354 = DIRECTION('center_axis',(-1.,0.,0.)) ;
#63355 = DIRECTION('ref_axis',(0.,-1.,0.)) ;
#63356 = DIRECTION('',(0.,0.,1.)) ;
#63357 = DIRECTION('',(0.,-1.,0.)) ;
#63358 = DIRECTION('center_axis',(-1.,0.,0.)) ;
#63359 = DIRECTION('ref_axis',(0.,0.382683432365097,-0.923879532511284)) ;
#63360 = DIRECTION('center_axis',(0.,0.,1.)) ;
#63361 = DIRECTION('ref_axis',(0.707106781186359,-0.707106781186736,0.)) ;
#63362 = DIRECTION('',(0.,0.,-1.)) ;
#63363 = DIRECTION('center_axis',(0.,0.,-1.)) ;
#63364 = DIRECTION('ref_axis',(1.,0.,0.)) ;
#63365 = DIRECTION('center_axis',(0.,1.,0.)) ;
#63366 = DIRECTION('ref_axis',(0.,0.,1.)) ;
#63367 = DIRECTION('center_axis',(-0.959365501571273,0.,0.282166323991543)) ;
#63368 = DIRECTION('ref_axis',(-0.282166323991543,0.,-0.959365501571273)) ;
#63369 = DIRECTION('center_axis',(-0.959365501571273,0.,0.282166323991543)) ;
#63370 = DIRECTION('ref_axis',(-0.282166323991543,0.,-0.959365501571273)) ;
#63371 = DIRECTION('center_axis',(0.282166323991552,0.,-0.95936550157127)) ;
#63372 = DIRECTION('ref_axis',(-0.95936550157127,0.,-0.282166323991552)) ;
#63373 = DIRECTION('center_axis',(0.282166323991552,0.,-0.95936550157127)) ;
#63374 = DIRECTION('ref_axis',(-0.95936550157127,0.,-0.282166323991552)) ;
#63375 = DIRECTION('center_axis',(-8.88178419700125E-16,1.,0.)) ;
#63376 = DIRECTION('ref_axis',(0.707106781186561,6.28036983473522E-16,0.707106781186534)) ;
#63377 = DIRECTION('center_axis',(0.,1.,0.)) ;
#63378 = DIRECTION('ref_axis',(0.,0.,1.)) ;
#63379 = DIRECTION('',(8.88178419700125E-16,-1.,0.)) ;
#63380 = DIRECTION('',(-8.88178419700125E-16,1.,0.)) ;
#63381 = DIRECTION('center_axis',(0.613629329651134,0.789594228570536,0.)) ;
#63382 = DIRECTION('ref_axis',(0.,0.,1.)) ;
#63383 = DIRECTION('center_axis',(-7.1167068359954E-15,-0.27472112789737,
0.961523947640826)) ;
#63384 = DIRECTION('ref_axis',(-1.90123672496938E-31,0.961523947640825,0.27472112789737)) ;
#63385 = DIRECTION('center_axis',(0.,0.,-1.)) ;
#63386 = DIRECTION('ref_axis',(-4.54309160498778E-16,1.,0.)) ;
#63387 = DIRECTION('center_axis',(0.,0.,1.)) ;
#63388 = DIRECTION('ref_axis',(1.,0.,0.)) ;
#63389 = DIRECTION('',(-1.,0.,0.)) ;
#63390 = DIRECTION('',(5.69345140833415E-16,1.,0.)) ;
#63391 = DIRECTION('center_axis',(0.,0.,-1.)) ;
#63392 = DIRECTION('ref_axis',(-0.70710678118657,-0.707106781186525,0.)) ;
#63393 = DIRECTION('',(-1.,0.,0.)) ;
#63394 = DIRECTION('center_axis',(0.,0.,-1.)) ;
#63395 = DIRECTION('ref_axis',(0.707106781186503,-0.707106781186592,0.)) ;
#63396 = DIRECTION('',(1.13869028166683E-15,-1.,0.)) ;
#63397 = DIRECTION('',(-1.,0.,0.)) ;
#63398 = DIRECTION('',(1.,-8.30329439001789E-15,0.)) ;
#63399 = DIRECTION('',(-1.11022302462516E-14,1.,0.)) ;
#63400 = DIRECTION('center_axis',(0.,0.,1.)) ;
#63401 = DIRECTION('ref_axis',(0.,-1.,0.)) ;
#63402 = DIRECTION('',(2.22044604925032E-15,-1.,0.)) ;
#63403 = DIRECTION('',(1.,-8.30329439001789E-15,0.)) ;
#63404 = DIRECTION('center_axis',(1.,-8.30329439001789E-15,0.)) ;
#63405 = DIRECTION('ref_axis',(-5.87131576936922E-15,-0.707106781186469,-0.707106781186626)) ;
#63406 = DIRECTION('',(-1.,8.30329439001789E-15,0.)) ;
#63407 = DIRECTION('center_axis',(0.70710678118661,0.707106781186485,-6.28036983473565E-14)) ;
#63408 = DIRECTION('ref_axis',(-0.707106781186485,0.70710678118661,-6.28036983473666E-14)) ;
#63409 = DIRECTION('center_axis',(0.,0.,-1.)) ;
#63410 = DIRECTION('ref_axis',(-0.707106781186359,-0.707106781186736,0.)) ;
#63411 = DIRECTION('',(0.,0.,-1.)) ;
#63412 = DIRECTION('center_axis',(0.,0.,-1.)) ;
#63413 = DIRECTION('ref_axis',(-8.88178419700617E-14,-1.,0.)) ;
#63414 = DIRECTION('',(0.,0.,1.)) ;
#63415 = DIRECTION('center_axis',(-0.50387102552408,0.,0.863778900898437)) ;
#63416 = DIRECTION('ref_axis',(0.863778900898437,0.,0.50387102552408)) ;
#63417 = DIRECTION('center_axis',(0.86377890089843,0.,-0.503871025524092)) ;
#63418 = DIRECTION('ref_axis',(0.503871025524092,0.,0.86377890089843)) ;
#63419 = DIRECTION('center_axis',(-7.10542735760115E-13,1.,-3.55271367880042E-13)) ;
#63420 = DIRECTION('ref_axis',(7.17464813746296E-42,3.55271367880042E-13,
1.)) ;
#63421 = DIRECTION('center_axis',(1.,0.,-7.16300942304673E-47)) ;
#63422 = DIRECTION('ref_axis',(5.06501253673939E-47,0.707106781186561,0.707106781186534)) ;
#63423 = DIRECTION('',(-1.,0.,7.16300942304673E-47)) ;
#63424 = DIRECTION('center_axis',(1.,3.17373410623533E-15,0.)) ;
#63425 = DIRECTION('ref_axis',(-2.24416890820207E-15,0.707106781186561,0.707106781186534)) ;
#63426 = DIRECTION('',(1.,0.,-7.16300942304673E-47)) ;
#63427 = DIRECTION('center_axis',(0.,0.,-1.)) ;
#63428 = DIRECTION('ref_axis',(0.707106781186521,0.707106781186574,0.)) ;
#63429 = DIRECTION('',(0.,0.,-1.)) ;
#63430 = DIRECTION('',(0.,0.,1.)) ;
#63431 = DIRECTION('center_axis',(-2.46519032881529E-32,1.65309428213318E-45,
1.)) ;
#63432 = DIRECTION('ref_axis',(0.707106781186521,0.707106781186574,1.7431527984206E-32)) ;
#63433 = DIRECTION('',(0.,0.,1.)) ;
#63434 = DIRECTION('center_axis',(-1.,-3.17373410623533E-15,0.)) ;
#63435 = DIRECTION('ref_axis',(-3.17373410623533E-15,1.,0.)) ;
#63436 = DIRECTION('',(0.,0.,-1.)) ;
#63437 = DIRECTION('',(-3.17373410623533E-15,1.,0.)) ;
#63438 = DIRECTION('',(0.,0.,-1.)) ;
#63439 = DIRECTION('',(-3.17373410623533E-15,1.,0.)) ;
#63440 = DIRECTION('center_axis',(-1.,-3.17373410623533E-15,0.)) ;
#63441 = DIRECTION('ref_axis',(-3.17373410623533E-15,1.,6.13317366673399E-17)) ;
#63442 = DIRECTION('',(0.,0.,-1.)) ;
#63443 = DIRECTION('center_axis',(1.,3.17373410623533E-15,0.)) ;
#63444 = DIRECTION('ref_axis',(3.17373410623533E-15,-1.,-6.13317366673399E-17)) ;
#63445 = DIRECTION('',(3.17373410623533E-15,-1.,0.)) ;
#63446 = DIRECTION('center_axis',(0.,1.,0.)) ;
#63447 = DIRECTION('ref_axis',(1.,0.,0.)) ;
#63448 = DIRECTION('',(1.,0.,0.)) ;
#63449 = DIRECTION('center_axis',(2.46519032881529E-32,-1.65309428213318E-45,
-1.)) ;
#63450 = DIRECTION('ref_axis',(1.,3.08616105302236E-93,2.46519032881529E-32)) ;
#63451 = DIRECTION('center_axis',(-2.46519032881529E-32,1.65309428213318E-45,
1.)) ;
#63452 = DIRECTION('ref_axis',(0.447213595500276,0.894427190999757,1.10246663054185E-32)) ;
#63453 = DIRECTION('',(0.800000000000003,0.599999999999996,1.97215226305214E-32)) ;
#63454 = DIRECTION('center_axis',(0.,0.,-1.)) ;
#63455 = DIRECTION('ref_axis',(0.447213595500276,0.894427190999757,0.)) ;
#63456 = DIRECTION('center_axis',(0.,0.,1.)) ;
#63457 = DIRECTION('ref_axis',(1.,0.,0.)) ;
#63458 = DIRECTION('',(0.,0.,1.)) ;
#63459 = DIRECTION('center_axis',(-1.1460366705808E-14,1.,0.)) ;
#63460 = DIRECTION('ref_axis',(0.707106781186534,8.10370301256122E-15,0.707106781186561)) ;
#63461 = DIRECTION('',(-1.1460366705808E-14,1.,0.)) ;
#63462 = DIRECTION('center_axis',(-0.707106781186548,-0.707106781186548,0.)) ;
#63463 = DIRECTION('ref_axis',(0.707106781186547,-0.707106781186547,0.)) ;
#63464 = DIRECTION('',(1.1460366705808E-14,-1.,0.)) ;
#63465 = DIRECTION('center_axis',(0.,0.,-1.)) ;
#63466 = DIRECTION('ref_axis',(1.,0.,0.)) ;
#63467 = DIRECTION('',(-0.707106781186547,0.707106781186547,0.)) ;
#63468 = DIRECTION('center_axis',(0.693108716251755,0.720833064901884,-3.6936252256852E-13)) ;
#63469 = DIRECTION('ref_axis',(-0.720833064901884,0.693108716251755,2.48164876568418E-29)) ;
#63470 = DIRECTION('center_axis',(0.170786723535891,-0.985308020399649,0.)) ;
#63471 = DIRECTION('ref_axis',(-0.985308020399649,-0.170786723535891,0.)) ;
#63472 = DIRECTION('center_axis',(2.22044604925026E-13,2.30926389122032E-13,
-1.)) ;
#63473 = DIRECTION('ref_axis',(-1.,1.34524652575477E-42,-2.22044604925026E-13)) ;
#63474 = DIRECTION('center_axis',(-0.720833064901858,0.693108716251782,0.)) ;
#63475 = DIRECTION('ref_axis',(-0.693108716251782,-0.720833064901858,2.25440992778648E-16)) ;
#63476 = DIRECTION('center_axis',(5.73018335290399E-15,-1.,0.)) ;
#63477 = DIRECTION('ref_axis',(-0.707106781186534,-4.0518515062806E-15,0.707106781186561)) ;
#63478 = DIRECTION('',(-5.73018335290399E-15,1.,0.)) ;
#63479 = DIRECTION('',(5.73018335290399E-15,-1.,0.)) ;
#63480 = DIRECTION('center_axis',(0.720833064901858,-0.693108716251782,0.)) ;
#63481 = DIRECTION('ref_axis',(0.,0.,-1.)) ;
#63482 = DIRECTION('',(0.,0.,1.)) ;
#63483 = DIRECTION('center_axis',(0.720833064901858,-0.693108716251782,0.)) ;
#63484 = DIRECTION('ref_axis',(0.693108716251782,0.720833064901858,9.01763971114601E-17)) ;
#63485 = DIRECTION('',(-0.562259334229024,-0.584749707598188,-0.58474970759819)) ;
#63486 = DIRECTION('',(0.693108716251782,0.720833064901858,0.)) ;
#63487 = DIRECTION('center_axis',(0.,0.,1.)) ;
#63488 = DIRECTION('ref_axis',(-0.927586401609545,0.373608709145084,0.)) ;
#63489 = DIRECTION('',(0.,0.,-1.)) ;
#63490 = DIRECTION('center_axis',(0.,0.,-1.)) ;
#63491 = DIRECTION('ref_axis',(-1.,0.,0.)) ;
#63492 = DIRECTION('center_axis',(-1.,-5.73018335290399E-15,0.)) ;
#63493 = DIRECTION('ref_axis',(-5.73018335290399E-15,1.,0.)) ;
#63494 = DIRECTION('',(-5.73018335290399E-15,1.,0.)) ;
#63495 = DIRECTION('',(0.,0.,1.)) ;
#63496 = DIRECTION('',(5.73018335290399E-15,-1.,0.)) ;
#63497 = DIRECTION('',(0.,0.,1.)) ;
#63498 = DIRECTION('',(5.73018335290399E-15,-1.,1.11561779098947E-30)) ;
#63499 = DIRECTION('center_axis',(-1.,5.69345140833415E-16,0.)) ;
#63500 = DIRECTION('ref_axis',(0.,0.,1.)) ;
#63501 = DIRECTION('center_axis',(0.,1.,0.)) ;
#63502 = DIRECTION('ref_axis',(1.,0.,0.)) ;
#63503 = DIRECTION('center_axis',(1.,-5.69345140833415E-16,0.)) ;
#63504 = DIRECTION('ref_axis',(2.17878952694528E-16,0.382683432365109,-0.923879532511279)) ;
#63505 = DIRECTION('center_axis',(4.71027737605141E-14,-0.707106781186581,
-0.707106781186514)) ;
#63506 = DIRECTION('ref_axis',(-7.31444512085447E-31,0.707106781186514,-0.707106781186581)) ;
#63507 = DIRECTION('center_axis',(-1.,5.69345140833415E-16,0.)) ;
#63508 = DIRECTION('ref_axis',(2.17878952694528E-16,0.382683432365109,-0.923879532511279)) ;
#63509 = DIRECTION('center_axis',(-1.,0.,0.)) ;
#63510 = DIRECTION('ref_axis',(0.,0.382683432365076,-0.923879532511292)) ;
#63511 = DIRECTION('',(1.,0.,0.)) ;
#63512 = DIRECTION('center_axis',(-4.02587809918917E-16,-0.707106781186546,
-0.707106781186549)) ;
#63513 = DIRECTION('ref_axis',(0.707106781186625,0.499999999999946,-0.499999999999944)) ;
#63514 = DIRECTION('',(4.02587809918917E-16,0.707106781186546,0.707106781186549)) ;
#63515 = DIRECTION('center_axis',(0.,0.70710678118657,0.707106781186525)) ;
#63516 = DIRECTION('ref_axis',(1.,0.,0.)) ;
#63517 = DIRECTION('',(-4.02587809918917E-16,-0.707106781186546,-0.707106781186549)) ;
#63518 = DIRECTION('center_axis',(0.,0.707106781186549,-0.707106781186546)) ;
#63519 = DIRECTION('ref_axis',(-1.,0.,0.)) ;
#63520 = DIRECTION('',(1.,0.,0.)) ;
#63521 = DIRECTION('',(8.82074414990881E-16,-0.707106781186546,-0.707106781186549)) ;
#63522 = DIRECTION('',(-1.,0.,0.)) ;
#63523 = DIRECTION('center_axis',(0.,-0.707106781186549,0.707106781186546)) ;
#63524 = DIRECTION('ref_axis',(8.17756488897798E-17,0.707106781186546,0.707106781186549)) ;
#63525 = DIRECTION('center_axis',(-1.,-1.13869028166683E-15,0.)) ;
#63526 = DIRECTION('ref_axis',(0.,0.,1.)) ;
#63527 = DIRECTION('center_axis',(0.,1.,0.)) ;
#63528 = DIRECTION('ref_axis',(0.,0.,-1.)) ;
#63529 = DIRECTION('center_axis',(1.,1.13869028166683E-15,0.)) ;
#63530 = DIRECTION('ref_axis',(-4.35757905389055E-16,0.382683432365109,-0.923879532511279)) ;
#63531 = DIRECTION('center_axis',(-4.7102773760512E-14,-0.707106781186581,
-0.707106781186514)) ;
#63532 = DIRECTION('ref_axis',(-1.,-1.7276484112332E-29,6.66133814775108E-14)) ;
#63533 = DIRECTION('center_axis',(-1.,-1.13869028166683E-15,0.)) ;
#63534 = DIRECTION('ref_axis',(-4.35757905389055E-16,0.382683432365109,-0.923879532511279)) ;
#63535 = DIRECTION('center_axis',(-1.,0.,0.)) ;
#63536 = DIRECTION('ref_axis',(0.,0.382683432365076,-0.923879532511292)) ;
#63537 = DIRECTION('center_axis',(1.13869028166683E-15,-1.,0.)) ;
#63538 = DIRECTION('ref_axis',(-0.707106781186532,-8.05175619837817E-16,-0.707106781186563)) ;
#63539 = DIRECTION('center_axis',(0.,1.,0.)) ;
#63540 = DIRECTION('ref_axis',(0.,0.,-1.)) ;
#63541 = DIRECTION('',(-1.13869028166683E-15,1.,0.)) ;
#63542 = DIRECTION('center_axis',(-8.30329439001789E-15,-1.,0.)) ;
#63543 = DIRECTION('ref_axis',(0.,0.,-1.)) ;
#63544 = DIRECTION('center_axis',(8.30329439001789E-15,1.,0.)) ;
#63545 = DIRECTION('ref_axis',(0.707106781186555,-5.87131576936993E-15,-0.70710678118654)) ;
#63546 = DIRECTION('center_axis',(1.,0.,0.)) ;
#63547 = DIRECTION('ref_axis',(0.,-1.,0.)) ;
#63548 = DIRECTION('center_axis',(-8.30329439001789E-15,-1.,0.)) ;
#63549 = DIRECTION('ref_axis',(0.707106781186555,-5.87131576936993E-15,-0.70710678118654)) ;
#63550 = DIRECTION('center_axis',(-1.,0.,0.)) ;
#63551 = DIRECTION('ref_axis',(0.,0.,1.)) ;
#63552 = DIRECTION('center_axis',(0.,1.,0.)) ;
#63553 = DIRECTION('ref_axis',(1.,0.,0.)) ;
#63554 = DIRECTION('center_axis',(1.,0.,0.)) ;
#63555 = DIRECTION('ref_axis',(0.,0.382683432365097,-0.923879532511284)) ;
#63556 = DIRECTION('center_axis',(0.,-1.,0.)) ;
#63557 = DIRECTION('ref_axis',(0.707106781186547,0.,-0.707106781186547)) ;
#63558 = DIRECTION('',(0.,1.,0.)) ;
#63559 = DIRECTION('center_axis',(8.30329439001789E-15,1.,0.)) ;
#63560 = DIRECTION('ref_axis',(0.,0.,1.)) ;
#63561 = DIRECTION('center_axis',(-8.30329439001789E-15,-1.,0.)) ;
#63562 = DIRECTION('ref_axis',(-0.707106781186571,5.87131576937006E-15,-0.707106781186524)) ;
#63563 = DIRECTION('center_axis',(-1.,0.,0.)) ;
#63564 = DIRECTION('ref_axis',(0.,0.,-1.)) ;
#63565 = DIRECTION('center_axis',(8.30329439001789E-15,1.,0.)) ;
#63566 = DIRECTION('ref_axis',(-0.707106781186571,5.87131576937006E-15,-0.707106781186524)) ;
#63567 = DIRECTION('center_axis',(-8.88178419700125E-16,1.,0.)) ;
#63568 = DIRECTION('ref_axis',(-0.707106781186537,-6.28036983473501E-16,-0.707106781186558)) ;
#63569 = DIRECTION('center_axis',(0.,-1.,0.)) ;
#63570 = DIRECTION('ref_axis',(-1.,0.,0.)) ;
#63571 = DIRECTION('',(8.88178419700125E-16,-1.,0.)) ;
#63572 = DIRECTION('',(-8.88178419700125E-16,1.,0.)) ;
#63573 = DIRECTION('center_axis',(1.,8.88178419700125E-16,0.)) ;
#63574 = DIRECTION('ref_axis',(0.,0.,-1.)) ;
#63575 = DIRECTION('center_axis',(0.,-0.707106781186536,-0.707106781186559)) ;
#63576 = DIRECTION('ref_axis',(-1.,0.,0.)) ;
#63577 = DIRECTION('center_axis',(-1.,-8.88178419700125E-16,0.)) ;
#63578 = DIRECTION('ref_axis',(-3.39891166203452E-16,0.382683432365097,-0.923879532511284)) ;
#63579 = DIRECTION('center_axis',(1.,8.88178419700125E-16,0.)) ;
#63580 = DIRECTION('ref_axis',(-3.39891166203451E-16,0.382683432365097,-0.923879532511284)) ;
#63581 = DIRECTION('center_axis',(-6.28036983473509E-16,0.707106781186546,
0.707106781186549)) ;
#63582 = DIRECTION('ref_axis',(-0.707106781186505,0.500000000000031,-0.500000000000029)) ;
#63583 = DIRECTION('',(-6.28036983473509E-16,0.707106781186546,0.707106781186549)) ;
#63584 = DIRECTION('center_axis',(-8.30329439001789E-15,-1.,0.)) ;
#63585 = DIRECTION('ref_axis',(-1.,8.30329439001789E-15,4.19778536698447E-50)) ;
#63586 = DIRECTION('',(-1.,8.30329439001789E-15,0.)) ;
#63587 = DIRECTION('',(0.,0.,-1.)) ;
#63588 = DIRECTION('',(-1.,8.30329439001789E-15,4.19778536698447E-50)) ;
#63589 = DIRECTION('',(0.,0.,-1.)) ;
#63590 = DIRECTION('',(1.,-9.87859509815899E-15,0.)) ;
#63591 = DIRECTION('',(0.,0.,-1.)) ;
#63592 = DIRECTION('center_axis',(-1.,8.30329439001789E-15,0.)) ;
#63593 = DIRECTION('ref_axis',(-5.87131576936922E-15,-0.707106781186469,-0.707106781186626)) ;
#63594 = DIRECTION('',(1.,-8.30329439001789E-15,0.)) ;
#63595 = DIRECTION('center_axis',(1.,0.,0.)) ;
#63596 = DIRECTION('ref_axis',(0.,-1.,0.)) ;
#63597 = DIRECTION('center_axis',(0.,0.,-1.)) ;
#63598 = DIRECTION('ref_axis',(1.,0.,0.)) ;
#63599 = DIRECTION('',(-1.,0.,0.)) ;
#63600 = DIRECTION('center_axis',(0.,0.,-1.)) ;
#63601 = DIRECTION('ref_axis',(0.998370060467465,-0.0570720804088061,0.)) ;
#63602 = DIRECTION('',(-5.73018335290399E-15,1.,0.)) ;
#63603 = DIRECTION('',(1.,-4.33257765707378E-15,0.)) ;
#63604 = DIRECTION('',(9.79313055424617E-16,-1.,0.)) ;
#63605 = DIRECTION('center_axis',(0.,0.,-1.)) ;
#63606 = DIRECTION('ref_axis',(0.707106781186554,0.707106781186541,0.)) ;
#63607 = DIRECTION('center_axis',(-1.,0.,0.)) ;
#63608 = DIRECTION('ref_axis',(0.,0.382683432365084,-0.923879532511289)) ;
#63609 = DIRECTION('center_axis',(-0.81649658092775,0.408248290463875,0.408248290463804)) ;
#63610 = DIRECTION('ref_axis',(0.577350269189602,0.577350269189744,0.577350269189531)) ;
#63611 = DIRECTION('center_axis',(0.,0.,1.)) ;
#63612 = DIRECTION('ref_axis',(0.,1.,0.)) ;
#63613 = DIRECTION('center_axis',(1.,0.,0.)) ;
#63614 = DIRECTION('ref_axis',(0.,0.,1.)) ;
#63615 = DIRECTION('center_axis',(0.,1.,0.)) ;
#63616 = DIRECTION('ref_axis',(1.,0.,0.)) ;
#63617 = DIRECTION('center_axis',(1.,0.,2.46519032881572E-32)) ;
#63618 = DIRECTION('ref_axis',(-1.74315279842063E-32,0.707106781186736,0.707106781186359)) ;
#63619 = DIRECTION('center_axis',(0.70710678118661,0.707106781186485,0.)) ;
#63620 = DIRECTION('ref_axis',(-0.707106781186485,0.70710678118661,6.13317366673404E-17)) ;
#63621 = DIRECTION('',(1.,0.,2.46519032881572E-32)) ;
#63622 = DIRECTION('',(-1.,0.,-2.46519032881572E-32)) ;
#63623 = DIRECTION('center_axis',(2.46519032881572E-32,8.55284707229503E-50,
-1.)) ;
#63624 = DIRECTION('ref_axis',(-1.,0.,0.)) ;
#63625 = DIRECTION('center_axis',(2.46519032881572E-32,8.55284707229503E-50,
-1.)) ;
#63626 = DIRECTION('ref_axis',(-0.339202113889148,0.940713519586666,-8.36197770673376E-33)) ;
#63627 = DIRECTION('center_axis',(-1.,0.,0.)) ;
#63628 = DIRECTION('ref_axis',(0.,-1.,0.)) ;
#63629 = DIRECTION('center_axis',(-2.46519032881572E-32,-8.55284707229503E-50,
1.)) ;
#63630 = DIRECTION('ref_axis',(-0.339202113889148,0.940713519586666,-8.36197770673376E-33)) ;
#63631 = DIRECTION('center_axis',(-1.,3.55271367880048E-14,-2.46519032881572E-32)) ;
#63632 = DIRECTION('ref_axis',(-2.51214793389469E-14,-0.707106781186736,0.707106781186359)) ;
#63633 = DIRECTION('center_axis',(-1.,0.,0.)) ;
#63634 = DIRECTION('ref_axis',(0.,-1.,0.)) ;
#63635 = DIRECTION('',(-1.,3.55271367880048E-14,-2.46519032881572E-32)) ;
#63636 = DIRECTION('',(1.,-3.55271367880048E-14,2.46519032881572E-32)) ;
#63637 = DIRECTION('center_axis',(2.46519032881572E-32,8.55284707229503E-50,
-1.)) ;
#63638 = DIRECTION('ref_axis',(-1.,0.,0.)) ;
#63639 = DIRECTION('center_axis',(-0.624999999999801,-0.780624749799959,0.)) ;
#63640 = DIRECTION('ref_axis',(0.780624749799959,-0.624999999999801,0.)) ;
#63641 = DIRECTION('center_axis',(2.46519032881572E-32,8.55284707229503E-50,
-1.)) ;
#63642 = DIRECTION('ref_axis',(0.433012701892204,-0.901387818866005,1.06745872495903E-32)) ;
#63643 = DIRECTION('center_axis',(-2.46519032881572E-32,-8.55284707229503E-50,
1.)) ;
#63644 = DIRECTION('ref_axis',(0.433012701892204,-0.901387818866005,1.06745872495903E-32)) ;
#63645 = DIRECTION('center_axis',(2.46519032881572E-32,8.55284707229503E-50,
-1.)) ;
#63646 = DIRECTION('ref_axis',(-1.,0.,0.)) ;
#63647 = DIRECTION('center_axis',(-0.707106781186459,-0.707106781186636,0.)) ;
#63648 = DIRECTION('ref_axis',(0.707106781186636,-0.707106781186459,0.)) ;
#63649 = DIRECTION('center_axis',(-2.46519032881572E-32,-8.55284707229503E-50,
1.)) ;
#63650 = DIRECTION('ref_axis',(-0.744997757011397,0.667066969687443,-1.8365612655739E-32)) ;
#63651 = DIRECTION('center_axis',(2.46519032881572E-32,8.55284707229503E-50,
-1.)) ;
#63652 = DIRECTION('ref_axis',(-0.744997757011397,0.667066969687443,-1.8365612655739E-32)) ;
#63653 = DIRECTION('center_axis',(0.70710678118654,0.707106781186555,1.74315279842107E-32)) ;
#63654 = DIRECTION('ref_axis',(0.499999999999972,-0.499999999999962,0.707106781186594)) ;
#63655 = DIRECTION('center_axis',(-0.707106781186548,-0.707106781186548,0.)) ;
#63656 = DIRECTION('ref_axis',(0.707106781186547,-0.707106781186547,0.)) ;
#63657 = DIRECTION('',(-0.70710678118654,-0.707106781186555,-1.74315279842107E-32)) ;
#63658 = DIRECTION('',(0.70710678118654,0.707106781186555,1.74315279842107E-32)) ;
#63659 = DIRECTION('center_axis',(2.46519032881572E-32,8.55284707229503E-50,
-1.)) ;
#63660 = DIRECTION('ref_axis',(-1.,0.,0.)) ;
#63661 = DIRECTION('center_axis',(0.,-1.,0.)) ;
#63662 = DIRECTION('ref_axis',(1.,0.,0.)) ;
#63663 = DIRECTION('center_axis',(2.46519032881572E-32,8.55284707229503E-50,
-1.)) ;
#63664 = DIRECTION('ref_axis',(0.923879532511298,-0.382683432365064,2.27753888853764E-32)) ;
#63665 = DIRECTION('center_axis',(-2.46519032881572E-32,-8.55284707229503E-50,
1.)) ;
#63666 = DIRECTION('ref_axis',(0.923879532511297,-0.382683432365064,2.27753888853764E-32)) ;
#63667 = DIRECTION('center_axis',(0.,1.,8.55284707229503E-50)) ;
#63668 = DIRECTION('ref_axis',(0.707106781186485,-6.04777616327186E-50,0.70710678118661)) ;
#63669 = DIRECTION('',(0.,-1.,-8.55284707229503E-50)) ;
#63670 = DIRECTION('',(0.,1.,8.55284707229503E-50)) ;
#63671 = DIRECTION('center_axis',(0.,0.,-1.)) ;
#63672 = DIRECTION('ref_axis',(0.707106781186296,0.707106781186799,0.)) ;
#63673 = DIRECTION('center_axis',(0.,0.,1.)) ;
#63674 = DIRECTION('ref_axis',(1.,0.,0.)) ;
#63675 = DIRECTION('',(0.,0.,1.)) ;
#63676 = DIRECTION('',(0.,0.,-1.)) ;
#63677 = DIRECTION('center_axis',(0.,1.,0.)) ;
#63678 = DIRECTION('ref_axis',(0.,0.,1.)) ;
#63679 = DIRECTION('center_axis',(0.,1.,0.)) ;
#63680 = DIRECTION('ref_axis',(-0.707106781186481,0.,-0.707106781186614)) ;
#63681 = DIRECTION('center_axis',(0.,-1.,0.)) ;
#63682 = DIRECTION('ref_axis',(-0.707106781186481,0.,-0.707106781186614)) ;
#63683 = DIRECTION('center_axis',(2.46519032881572E-32,8.55284707229503E-50,
-1.)) ;
#63684 = DIRECTION('ref_axis',(1.,-2.20382687031672E-110,2.46519032881572E-32)) ;
#63685 = DIRECTION('',(0.,1.,8.55284707229503E-50)) ;
#63686 = DIRECTION('center_axis',(2.46519032881566E-32,0.,-1.)) ;
#63687 = DIRECTION('ref_axis',(0.,1.,0.)) ;
#63688 = DIRECTION('',(1.77635683939373E-14,1.,-2.46519032880661E-33)) ;
#63689 = DIRECTION('center_axis',(2.46519032881572E-32,8.55284707229503E-50,
-1.)) ;
#63690 = DIRECTION('ref_axis',(1.,-2.20382687031672E-110,2.46519032881572E-32)) ;
#63691 = DIRECTION('',(1.,0.,6.12949496482233E-35)) ;
#63692 = DIRECTION('',(0.,1.,0.)) ;
#63693 = DIRECTION('',(-1.,3.55271367880048E-14,0.)) ;
#63694 = DIRECTION('center_axis',(0.,0.,-1.)) ;
#63695 = DIRECTION('ref_axis',(-1.,3.9474596431117E-14,0.)) ;
#63696 = DIRECTION('center_axis',(2.46519032881572E-32,8.55284707229503E-50,
-1.)) ;
#63697 = DIRECTION('ref_axis',(-1.,2.10843958864616E-81,-2.46519032881572E-32)) ;
#63698 = DIRECTION('center_axis',(2.46519032881572E-32,8.55284707229503E-50,
-1.)) ;
#63699 = DIRECTION('ref_axis',(-0.498769364572801,-0.86673474659993,-1.22956141385443E-32)) ;
#63700 = DIRECTION('center_axis',(0.,1.,8.55284707229503E-50)) ;
#63701 = DIRECTION('ref_axis',(-0.707106781186485,-6.04777616327186E-50,0.70710678118661)) ;
#63702 = DIRECTION('',(0.,-1.,-8.55284707229503E-50)) ;
#63703 = DIRECTION('center_axis',(0.,1.,0.)) ;
#63704 = DIRECTION('ref_axis',(-0.707106781186485,0.,0.70710678118661)) ;
#63705 = DIRECTION('center_axis',(0.,1.,0.)) ;
#63706 = DIRECTION('ref_axis',(1.,0.,1.30736459881558E-32)) ;
#63707 = DIRECTION('',(1.,0.,0.)) ;
#63708 = DIRECTION('',(0.,0.,-1.)) ;
#63709 = DIRECTION('center_axis',(0.,0.,-1.)) ;
#63710 = DIRECTION('ref_axis',(0.480391553143902,-0.877054134970008,0.)) ;
#63711 = DIRECTION('center_axis',(0.,0.,1.)) ;
#63712 = DIRECTION('ref_axis',(0.480391553143902,-0.877054134970008,0.)) ;
#63713 = DIRECTION('',(0.,0.,1.)) ;
#63714 = DIRECTION('center_axis',(0.,0.,1.)) ;
#63715 = DIRECTION('ref_axis',(-0.538447911335745,-0.842658796179197,0.)) ;
#63716 = DIRECTION('',(0.,0.,-1.)) ;
#63717 = DIRECTION('center_axis',(0.,-0.70710678118661,0.707106781186485)) ;
#63718 = DIRECTION('ref_axis',(-6.13317366673295E-17,-0.707106781186485,-0.70710678118661)) ;
#63719 = DIRECTION('center_axis',(0.,0.,-1.)) ;
#63720 = DIRECTION('ref_axis',(8.28966525053379E-14,1.,0.)) ;
#63721 = DIRECTION('center_axis',(0.,0.,-1.)) ;
#63722 = DIRECTION('ref_axis',(8.28966525053379E-14,1.,0.)) ;
#63723 = DIRECTION('',(0.,0.,-1.)) ;
#63724 = DIRECTION('center_axis',(-1.01307418018711E-45,-5.52427741944263E-33,
-1.)) ;
#63725 = DIRECTION('ref_axis',(8.28966525053379E-14,1.,-5.52427741944263E-33)) ;
#63726 = DIRECTION('center_axis',(0.,1.,0.)) ;
#63727 = DIRECTION('ref_axis',(-0.707106781186485,0.,-0.70710678118661)) ;
#63728 = DIRECTION('',(0.,-1.,0.)) ;
#63729 = DIRECTION('center_axis',(0.,-1.,0.)) ;
#63730 = DIRECTION('ref_axis',(-1.,0.,0.)) ;
#63731 = DIRECTION('',(0.,1.,0.)) ;
#63732 = DIRECTION('center_axis',(1.,0.,0.)) ;
#63733 = DIRECTION('ref_axis',(0.,-1.,0.)) ;
#63734 = DIRECTION('',(0.,0.,-1.)) ;
#63735 = DIRECTION('',(0.,-1.,0.)) ;
#63736 = DIRECTION('',(0.,0.,-1.)) ;
#63737 = DIRECTION('center_axis',(1.,9.79313055424617E-16,0.)) ;
#63738 = DIRECTION('ref_axis',(0.,0.,-1.)) ;
#63739 = DIRECTION('center_axis',(-1.,-9.79313055424617E-16,0.)) ;
#63740 = DIRECTION('ref_axis',(3.43729761245549E-16,-0.3509906861157,0.936378950137192)) ;
#63741 = DIRECTION('center_axis',(0.,1.,0.)) ;
#63742 = DIRECTION('ref_axis',(0.,0.,-1.)) ;
#63743 = DIRECTION('center_axis',(1.,9.79313055424617E-16,0.)) ;
#63744 = DIRECTION('ref_axis',(3.43729761245549E-16,-0.3509906861157,0.936378950137192)) ;
#63745 = DIRECTION('center_axis',(0.,-0.753611076520055,-0.65732058034591)) ;
#63746 = DIRECTION('ref_axis',(-1.,0.,0.)) ;
#63747 = DIRECTION('center_axis',(-9.79313055424617E-16,1.,0.)) ;
#63748 = DIRECTION('ref_axis',(-0.707106781186532,-6.92478902395249E-16,-0.707106781186563)) ;
#63749 = DIRECTION('center_axis',(0.,-1.,0.)) ;
#63750 = DIRECTION('ref_axis',(-1.,0.,0.)) ;
#63751 = DIRECTION('',(-9.79313055424617E-16,1.,0.)) ;
#63752 = DIRECTION('center_axis',(0.,0.,1.)) ;
#63753 = DIRECTION('ref_axis',(1.,0.,0.)) ;
#63754 = DIRECTION('center_axis',(0.,0.,1.)) ;
#63755 = DIRECTION('ref_axis',(0.707106781186554,0.707106781186541,0.)) ;
#63756 = DIRECTION('center_axis',(-1.,4.33257765707378E-15,0.)) ;
#63757 = DIRECTION('ref_axis',(-1.52069440450512E-15,-0.350990686115526,0.936378950137257)) ;
#63758 = DIRECTION('center_axis',(1.,0.,0.)) ;
#63759 = DIRECTION('ref_axis',(0.,0.,1.)) ;
#63760 = DIRECTION('',(-1.,4.33257765707378E-15,0.)) ;
#63761 = DIRECTION('center_axis',(0.604947702565294,0.517761097730612,0.60494770256425)) ;
#63762 = DIRECTION('ref_axis',(-0.707106781185937,-2.45097362971974E-16,0.707106781187158)) ;
#63763 = DIRECTION('center_axis',(0.707106781186503,-9.42055475210098E-14,
0.707106781186592)) ;
#63764 = DIRECTION('ref_axis',(-0.707106781186592,-8.04690672217442E-31,0.707106781186503)) ;
#63765 = DIRECTION('center_axis',(-0.661621637086846,-8.8798640187934E-15,
0.749837855365093)) ;
#63766 = DIRECTION('ref_axis',(-0.749837855365093,-5.16196667825131E-32,-0.661621637086846)) ;
#63767 = DIRECTION('center_axis',(0.707106781186548,4.05185150628068E-15,
-0.707106781186548)) ;
#63768 = DIRECTION('ref_axis',(-0.707106781186548,1.02171457789349E-14,-0.707106781186548)) ;
#63769 = DIRECTION('center_axis',(-0.707106781186548,3.06359504133419E-15,
-0.707106781186548)) ;
#63770 = DIRECTION('ref_axis',(-0.499999999999867,-0.707106781186738,0.499999999999864)) ;
#63771 = DIRECTION('center_axis',(0.707106781186525,0.,0.70710678118657)) ;
#63772 = DIRECTION('ref_axis',(-0.70710678118657,0.,0.707106781186525)) ;
#63773 = DIRECTION('',(-0.707106781186547,3.06359504133419E-15,-0.707106781186547)) ;
#63774 = DIRECTION('',(0.707106781186547,-3.06359504133419E-15,0.707106781186547)) ;
#63775 = DIRECTION('center_axis',(-0.89442719099992,0.,0.44721359549995)) ;
#63776 = DIRECTION('ref_axis',(0.44721359549995,0.,0.89442719099992)) ;
#63777 = DIRECTION('center_axis',(0.707106781186548,4.05185150628068E-15,
-0.707106781186548)) ;
#63778 = DIRECTION('ref_axis',(0.707106781186548,3.92523114670944E-15,0.707106781186548)) ;
#63779 = DIRECTION('center_axis',(0.,0.,-1.)) ;
#63780 = DIRECTION('ref_axis',(-1.,0.,0.)) ;
#63781 = DIRECTION('center_axis',(-0.983423055146244,0.181325534454923,0.000381000609942105)) ;
#63782 = DIRECTION('ref_axis',(0.181316738273391,0.983349845304303,0.0121376341146972)) ;
#63783 = DIRECTION('center_axis',(0.,0.,-1.)) ;
#63784 = DIRECTION('ref_axis',(-0.624947614806638,-0.780666688637022,0.)) ;
#63785 = DIRECTION('center_axis',(0.573576436350949,-0.81915204428906,0.)) ;
#63786 = DIRECTION('ref_axis',(-0.81915204428906,-0.573576436350949,0.)) ;
#63787 = DIRECTION('center_axis',(-0.573576436351043,0.819152044288994,0.)) ;
#63788 = DIRECTION('ref_axis',(-0.579227965339645,-0.405579787672689,-0.707106781186457)) ;
#63789 = DIRECTION('center_axis',(0.573576436351158,-0.819152044288914,0.)) ;
#63790 = DIRECTION('ref_axis',(-0.819152044288914,-0.573576436351158,0.)) ;
#63791 = DIRECTION('',(-0.573576436351043,0.819152044288994,0.)) ;
#63792 = DIRECTION('center_axis',(0.,0.,-1.)) ;
#63793 = DIRECTION('ref_axis',(-1.,0.,0.)) ;
#63794 = DIRECTION('center_axis',(0.,-1.,0.)) ;
#63795 = DIRECTION('ref_axis',(-1.,0.,0.)) ;
#63796 = DIRECTION('center_axis',(0.,0.,-1.)) ;
#63797 = DIRECTION('ref_axis',(-0.95371695074823,-0.300705799504264,0.)) ;
#63798 = DIRECTION('center_axis',(-9.79313055424617E-16,1.,0.)) ;
#63799 = DIRECTION('ref_axis',(-0.707106781186532,-6.92478902395249E-16,-0.707106781186563)) ;
#63800 = DIRECTION('center_axis',(0.,-1.,0.)) ;
#63801 = DIRECTION('ref_axis',(-1.,0.,0.)) ;
#63802 = DIRECTION('',(-9.79313055424617E-16,1.,0.)) ;
#63803 = DIRECTION('center_axis',(1.,9.79313055424617E-16,0.)) ;
#63804 = DIRECTION('ref_axis',(0.,0.,-1.)) ;
#63805 = DIRECTION('center_axis',(0.,-0.94868329805046,-0.316227766016998)) ;
#63806 = DIRECTION('ref_axis',(-1.,0.,0.)) ;
#63807 = DIRECTION('center_axis',(-1.,-9.79313055424617E-16,0.)) ;
#63808 = DIRECTION('ref_axis',(-1.56868561823944E-16,0.16018224300699,-0.987087457637493)) ;
#63809 = DIRECTION('center_axis',(1.,9.79313055424617E-16,0.)) ;
#63810 = DIRECTION('ref_axis',(-1.56868561823944E-16,0.16018224300699,-0.987087457637493)) ;
#63811 = DIRECTION('center_axis',(-9.2905793924415E-16,0.948683298050513,
0.316227766016839)) ;
#63812 = DIRECTION('ref_axis',(-0.707106781186599,0.223606797749963,-0.670820393249888)) ;
#63813 = DIRECTION('center_axis',(0.,-0.948683298050571,-0.316227766016665)) ;
#63814 = DIRECTION('ref_axis',(-1.,0.,0.)) ;
#63815 = DIRECTION('',(9.29057939244151E-16,-0.948683298050513,-0.316227766016839)) ;
#63816 = DIRECTION('',(-9.29057939244151E-16,0.948683298050513,0.316227766016839)) ;
#63817 = DIRECTION('center_axis',(1.,9.79313055424617E-16,0.)) ;
#63818 = DIRECTION('ref_axis',(0.,0.,-1.)) ;
#63819 = DIRECTION('center_axis',(-1.,-9.79313055424617E-16,0.)) ;
#63820 = DIRECTION('ref_axis',(-5.0670923265072E-16,0.517412925156009,-0.855735861631089)) ;
#63821 = DIRECTION('center_axis',(1.,9.79313055424617E-16,0.)) ;
#63822 = DIRECTION('ref_axis',(-5.0670923265072E-16,0.517412925156009,-0.855735861631089)) ;
#63823 = DIRECTION('center_axis',(0.,0.,-1.)) ;
#63824 = DIRECTION('ref_axis',(0.,1.,0.)) ;
#63825 = DIRECTION('',(0.,0.,-1.)) ;
#63826 = DIRECTION('center_axis',(-8.57083562089732E-97,-5.13170824337699E-49,
-1.)) ;
#63827 = DIRECTION('ref_axis',(0.,1.,-5.13170824337699E-49)) ;
#63828 = DIRECTION('center_axis',(-1.,-9.79313055424617E-16,0.)) ;
#63829 = DIRECTION('ref_axis',(-9.79313055424617E-16,1.,-5.30037252443606E-33)) ;
#63830 = DIRECTION('',(0.,0.,-1.)) ;
#63831 = DIRECTION('',(-9.79313055424617E-16,1.,-5.30037252443606E-33)) ;
#63832 = DIRECTION('center_axis',(0.,0.,-1.)) ;
#63833 = DIRECTION('ref_axis',(-0.819152044288991,-0.573576436351047,0.)) ;
#63834 = DIRECTION('',(0.,0.,-1.)) ;
#63835 = DIRECTION('center_axis',(-8.11022789614398E-33,1.15826058041052E-32,
-1.)) ;
#63836 = DIRECTION('ref_axis',(-0.819152044288991,-0.573576436351047,-1.67157598811966E-45)) ;
#63837 = DIRECTION('center_axis',(-0.819152044288994,-0.573576436351043,0.)) ;
#63838 = DIRECTION('ref_axis',(-0.573576436351043,0.819152044288994,0.)) ;
#63839 = DIRECTION('',(0.,0.,-1.)) ;
#63840 = DIRECTION('',(0.573576436351043,-0.819152044288994,4.46962256005402E-32)) ;
#63841 = DIRECTION('',(0.,0.,-1.)) ;
#63842 = DIRECTION('',(-0.573576436351043,0.819152044288994,0.)) ;
#63843 = DIRECTION('center_axis',(0.,0.,-1.)) ;
#63844 = DIRECTION('ref_axis',(-0.173648177666935,-0.984807753012207,0.)) ;
#63845 = DIRECTION('',(0.,0.,-1.)) ;
#63846 = DIRECTION('center_axis',(1.09763027743844E-32,6.22497063709847E-32,
1.)) ;
#63847 = DIRECTION('ref_axis',(-0.587740293442623,-0.809049656982796,5.68143190002567E-32)) ;
#63848 = DIRECTION('center_axis',(-0.997835226140326,0.0657636789837963,0.)) ;
#63849 = DIRECTION('ref_axis',(-0.0465019433652248,-0.705576054910746,-0.707106781186438)) ;
#63850 = DIRECTION('center_axis',(0.997835226140338,-0.0657636789836146,0.)) ;
#63851 = DIRECTION('ref_axis',(-0.0657636789836146,-0.997835226140338,0.)) ;
#63852 = DIRECTION('',(-0.997835226140326,0.0657636789837963,0.)) ;
#63853 = DIRECTION('center_axis',(-0.672457840829202,0.309193959537835,0.672457840829181)) ;
#63854 = DIRECTION('ref_axis',(1.60829332345463E-16,-0.90856053509436,0.41775322149452)) ;
#63855 = DIRECTION('center_axis',(-0.707106781186536,-3.14018491736822E-14,
0.707106781186559)) ;
#63856 = DIRECTION('ref_axis',(-4.43693537133302E-29,-1.,-4.44089209850151E-14)) ;
#63857 = DIRECTION('center_axis',(-0.70710678118655,-8.10370301256138E-15,
-0.707106781186545)) ;
#63858 = DIRECTION('ref_axis',(0.707106781186545,-1.41676311701544E-14,-0.70710678118655)) ;
#63859 = DIRECTION('center_axis',(0.447213595499966,1.9860273225975E-14,0.894427190999912)) ;
#63860 = DIRECTION('ref_axis',(0.894427190999912,-1.8300617384979E-31,-0.447213595499966)) ;
#63861 = DIRECTION('center_axis',(-0.707106781186545,3.06359504133419E-15,
0.70710678118655)) ;
#63862 = DIRECTION('ref_axis',(0.500000000000059,-0.707106781186465,0.500000000000058)) ;
#63863 = DIRECTION('center_axis',(-0.707106781186525,0.,0.70710678118657)) ;
#63864 = DIRECTION('ref_axis',(0.,-1.,0.)) ;
#63865 = DIRECTION('',(0.707106781186545,-3.06359504133419E-15,-0.70710678118655)) ;
#63866 = DIRECTION('',(-0.707106781186545,3.06359504133419E-15,0.70710678118655)) ;
#63867 = DIRECTION('center_axis',(-0.624695047554719,-0.468521285665242,0.624695047554562)) ;
#63868 = DIRECTION('ref_axis',(0.599999999999318,-0.800000000000512,-4.45819707740118E-14)) ;
#63869 = DIRECTION('center_axis',(-0.70710678118655,-8.10370301256138E-15,
-0.707106781186545)) ;
#63870 = DIRECTION('ref_axis',(-0.707106781186545,-8.04672385075432E-15,0.70710678118655)) ;
#63871 = DIRECTION('center_axis',(0.780868809443032,1.73387706291061E-14,
0.624695047554423)) ;
#63872 = DIRECTION('ref_axis',(-0.624695047554423,-1.75046575158144E-31,0.780868809443031)) ;
#63873 = DIRECTION('center_axis',(-0.514495755427105,-0.685994340570717,0.51449575542704)) ;
#63874 = DIRECTION('ref_axis',(0.800000000000522,-0.599999999999304,-6.96026688936854E-17)) ;
#63875 = DIRECTION('center_axis',(-0.707106781185896,-1.3346564596511E-12,
-0.707106781187199)) ;
#63876 = DIRECTION('ref_axis',(0.664495781864865,0.341892836673091,-0.664495781864286)) ;
#63877 = DIRECTION('center_axis',(0.781646665849804,-0.00199881414324549,
0.623718281364195)) ;
#63878 = DIRECTION('ref_axis',(0.613196036400756,-0.180472748793488,-0.769038495710927)) ;
#63879 = DIRECTION('center_axis',(0.780868809443032,1.73387706291061E-14,
0.624695047554423)) ;
#63880 = DIRECTION('ref_axis',(-0.624695047554423,-1.75046575158144E-31,0.780868809443031)) ;
#63881 = DIRECTION('center_axis',(-0.70710678118655,-8.10370301256138E-15,
-0.707106781186545)) ;
#63882 = DIRECTION('ref_axis',(-0.707106781186545,-8.04672385075432E-15,0.70710678118655)) ;
#63883 = DIRECTION('center_axis',(0.,0.,-1.)) ;
#63884 = DIRECTION('ref_axis',(-0.707106781186548,0.707106781186548,0.)) ;
#63885 = DIRECTION('',(0.,0.,-1.)) ;
#63886 = DIRECTION('center_axis',(0.,0.242535625036338,-0.970142500145331)) ;
#63887 = DIRECTION('ref_axis',(0.,0.970142500145331,0.242535625036338)) ;
#63888 = DIRECTION('',(0.,0.,1.)) ;
#63889 = DIRECTION('center_axis',(-0.70710678118655,-8.10370301256138E-15,
-0.707106781186545)) ;
#63890 = DIRECTION('ref_axis',(-0.707106781186545,-1.02766135666342E-31,0.70710678118655)) ;
#63891 = DIRECTION('',(-0.577350269189617,-0.577350269189633,0.577350269189627)) ;
#63892 = DIRECTION('',(1.1460366705808E-14,-1.,1.11561779098947E-30)) ;
#63893 = DIRECTION('',(0.577350269189627,-0.577350269189627,-0.577350269189624)) ;
#63894 = DIRECTION('',(-1.1460366705808E-14,1.,0.)) ;
#63895 = DIRECTION('center_axis',(-0.70710678118655,-8.10370301256138E-15,
-0.707106781186545)) ;
#63896 = DIRECTION('ref_axis',(-0.707106781186545,1.41902270731371E-14,0.70710678118655)) ;
#63897 = DIRECTION('center_axis',(-4.33257765707378E-15,-1.,0.)) ;
#63898 = DIRECTION('ref_axis',(-1.,4.33257765707378E-15,0.)) ;
#63899 = DIRECTION('',(1.,-4.33257765707378E-15,0.)) ;
#63900 = DIRECTION('center_axis',(-1.,4.33257765707378E-15,0.)) ;
#63901 = DIRECTION('ref_axis',(3.44001377016025E-15,0.793987792588958,-0.607933701335692)) ;
#63902 = DIRECTION('',(-1.,4.33257765707378E-15,0.)) ;
#63903 = DIRECTION('center_axis',(-1.,0.,0.)) ;
#63904 = DIRECTION('ref_axis',(0.,1.,0.)) ;
#63905 = DIRECTION('center_axis',(-1.38777878078145E-15,1.,0.)) ;
#63906 = DIRECTION('ref_axis',(-0.707106781186532,-9.81307786677341E-16,-0.707106781186563)) ;
#63907 = DIRECTION('center_axis',(0.70710678118661,0.707106781186485,0.)) ;
#63908 = DIRECTION('ref_axis',(0.707106781186485,-0.70710678118661,0.)) ;
#63909 = DIRECTION('',(-1.38777878078145E-15,1.,0.)) ;
#63910 = DIRECTION('center_axis',(0.,0.,-1.)) ;
#63911 = DIRECTION('ref_axis',(-1.,0.,0.)) ;
#63912 = DIRECTION('center_axis',(0.,0.,-1.)) ;
#63913 = DIRECTION('ref_axis',(0.,-1.,0.)) ;
#63914 = DIRECTION('center_axis',(0.,-1.,0.)) ;
#63915 = DIRECTION('ref_axis',(0.707106781186532,0.,-0.707106781186563)) ;
#63916 = DIRECTION('',(0.,-1.,0.)) ;
#63917 = DIRECTION('center_axis',(-0.70710678118661,0.707106781186485,0.)) ;
#63918 = DIRECTION('ref_axis',(0.707106781186485,0.70710678118661,0.)) ;
#63919 = DIRECTION('center_axis',(1.,0.,0.)) ;
#63920 = DIRECTION('ref_axis',(0.,0.707106781186469,-0.707106781186626)) ;
#63921 = DIRECTION('',(1.,0.,0.)) ;
#63922 = DIRECTION('center_axis',(0.,0.,-1.)) ;
#63923 = DIRECTION('ref_axis',(1.,0.,0.)) ;
#63924 = DIRECTION('',(0.,0.,-1.)) ;
#63925 = DIRECTION('center_axis',(1.09763027743844E-32,6.22497063709847E-32,
1.)) ;
#63926 = DIRECTION('ref_axis',(1.,-6.83271624744454E-64,-1.09763027743844E-32)) ;
#63927 = DIRECTION('',(0.,0.,-1.)) ;
#63928 = DIRECTION('center_axis',(1.,1.38777878078145E-15,0.)) ;
#63929 = DIRECTION('ref_axis',(1.38777878078145E-15,-1.,0.)) ;
#63930 = DIRECTION('',(0.,0.,1.)) ;
#63931 = DIRECTION('',(1.38777878078145E-15,-1.,6.22497063709847E-32)) ;
#63932 = DIRECTION('center_axis',(0.,0.,-1.)) ;
#63933 = DIRECTION('ref_axis',(1.,0.,0.)) ;
#63934 = DIRECTION('center_axis',(-1.,8.88178419700302E-14,-8.88178419700105E-14)) ;
#63935 = DIRECTION('ref_axis',(8.88178419700302E-14,1.,-3.58732406902838E-43)) ;
#63936 = DIRECTION('center_axis',(-3.97205464519572E-14,0.447213595499958,
0.894427190999916)) ;
#63937 = DIRECTION('ref_axis',(-3.97205464519572E-14,-0.894427190999916,0.447213595499958)) ;
#63938 = DIRECTION('center_axis',(3.97205464519622E-14,-0.894427190999888,
-0.447213595500014)) ;
#63939 = DIRECTION('ref_axis',(-3.97205464519551E-14,-0.447213595500014,0.894427190999888)) ;
#63940 = DIRECTION('center_axis',(1.09763027743844E-32,6.22497063709847E-32,
1.)) ;
#63941 = DIRECTION('ref_axis',(1.,0.,0.)) ;
#63942 = DIRECTION('center_axis',(-0.707106781186459,0.707106781186636,0.)) ;
#63943 = DIRECTION('ref_axis',(0.707106781186636,0.707106781186459,0.)) ;
#63944 = DIRECTION('center_axis',(1.09763027743844E-32,6.22497063709847E-32,
1.)) ;
#63945 = DIRECTION('ref_axis',(-0.38268343236507,-0.923879532511295,6.17116788413704E-32)) ;
#63946 = DIRECTION('center_axis',(-1.09763027743844E-32,-6.22497063709847E-32,
-1.)) ;
#63947 = DIRECTION('ref_axis',(-0.38268343236507,-0.923879532511295,6.17116788413704E-32)) ;
#63948 = DIRECTION('center_axis',(0.707106781186472,-0.707106781186624,3.62557713776763E-32)) ;
#63949 = DIRECTION('ref_axis',(0.500000000000021,0.499999999999913,-0.707106781186594)) ;
#63950 = DIRECTION('',(0.707106781186472,-0.707106781186624,3.62557713776763E-32)) ;
#63951 = DIRECTION('',(-0.707106781186472,0.707106781186624,-3.62557713776763E-32)) ;
#63952 = DIRECTION('center_axis',(-0.707106781186624,-0.707106781186472,0.)) ;
#63953 = DIRECTION('ref_axis',(-0.707106781186472,0.707106781186624,0.)) ;
#63954 = DIRECTION('',(0.,0.,-1.)) ;
#63955 = DIRECTION('',(-0.707106781186471,0.707106781186624,0.)) ;
#63956 = DIRECTION('',(0.,0.,-1.)) ;
#63957 = DIRECTION('',(-0.707106781186471,0.707106781186624,0.)) ;
#63958 = DIRECTION('',(0.,0.,-1.)) ;
#63959 = DIRECTION('center_axis',(0.,0.,-1.)) ;
#63960 = DIRECTION('ref_axis',(0.382683432365038,-0.923879532511308,0.)) ;
#63961 = DIRECTION('',(0.,0.,1.)) ;
#63962 = DIRECTION('center_axis',(2.46519032881572E-32,8.55284707229503E-50,
-1.)) ;
#63963 = DIRECTION('ref_axis',(0.382683432365038,-0.923879532511308,9.43387496464296E-33)) ;
#63964 = DIRECTION('center_axis',(3.67742382159233E-14,1.,-6.22497063709851E-32)) ;
#63965 = DIRECTION('ref_axis',(0.707106781186548,-2.60033132154489E-14,0.707106781186548)) ;
#63966 = DIRECTION('',(-3.67742382159233E-14,-1.,6.22497063709851E-32)) ;
#63967 = DIRECTION('center_axis',(0.,-1.,0.)) ;
#63968 = DIRECTION('ref_axis',(1.,0.,0.)) ;
#63969 = DIRECTION('',(3.67742382159233E-14,1.,-6.22497063709851E-32)) ;
#63970 = DIRECTION('center_axis',(-0.439732612032359,-0.182143211721388,-0.879465224064611)) ;
#63971 = DIRECTION('ref_axis',(0.812519920068743,0.336556770590752,-0.475963149477991)) ;
#63972 = DIRECTION('center_axis',(0.,0.,1.)) ;
#63973 = DIRECTION('ref_axis',(0.707106781186547,0.707106781186547,0.)) ;
#63974 = DIRECTION('center_axis',(-0.707106781186548,0.707106781186548,0.)) ;
#63975 = DIRECTION('ref_axis',(0.,0.,-1.)) ;
#63976 = DIRECTION('center_axis',(0.,-1.,0.)) ;
#63977 = DIRECTION('ref_axis',(1.,0.,0.)) ;
#63978 = DIRECTION('center_axis',(-0.707106781186607,0.707106781186488,0.)) ;
#63979 = DIRECTION('ref_axis',(0.499999999999925,0.500000000000009,-0.707106781186594)) ;
#63980 = DIRECTION('',(0.707106781186607,-0.707106781186488,0.)) ;
#63981 = DIRECTION('',(-0.707106781186607,0.707106781186488,0.)) ;
#63982 = DIRECTION('center_axis',(1.08152878803189E-14,1.,0.)) ;
#63983 = DIRECTION('ref_axis',(0.707106781186485,-7.6475634006575E-15,-0.70710678118661)) ;
#63984 = DIRECTION('',(1.08152878803189E-14,1.,0.)) ;
#63985 = DIRECTION('',(-1.08152878803189E-14,-1.,0.)) ;
#63986 = DIRECTION('center_axis',(0.,0.,-1.)) ;
#63987 = DIRECTION('ref_axis',(-1.,0.,0.)) ;
#63988 = DIRECTION('center_axis',(0.,0.,-1.)) ;
#63989 = DIRECTION('ref_axis',(1.,0.,0.)) ;
#63990 = DIRECTION('center_axis',(0.,-1.,0.)) ;
#63991 = DIRECTION('ref_axis',(0.,0.,1.)) ;
#63992 = DIRECTION('center_axis',(7.16300942304673E-47,-7.6997105554314E-34,
1.)) ;
#63993 = DIRECTION('ref_axis',(0.923879532511283,0.382683432365099,2.94655166356961E-34)) ;
#63994 = DIRECTION('center_axis',(-0.707106781186548,0.707106781186548,0.)) ;
#63995 = DIRECTION('ref_axis',(-0.707106781186547,-0.707106781186547,0.)) ;
#63996 = DIRECTION('center_axis',(-1.08152878803189E-14,-1.,-7.6997105554314E-34)) ;
#63997 = DIRECTION('ref_axis',(-0.70710678118661,7.64756340065885E-15,0.707106781186485)) ;
#63998 = DIRECTION('',(1.08152878803189E-14,1.,7.6997105554314E-34)) ;
#63999 = DIRECTION('',(-1.08152878803189E-14,-1.,-7.6997105554314E-34)) ;
#64000 = DIRECTION('center_axis',(0.707106781186607,-0.707106781186488,-5.44451754691923E-34)) ;
#64001 = DIRECTION('ref_axis',(-0.499999999999925,-0.500000000000009,0.707106781186594)) ;
#64002 = DIRECTION('',(0.707106781186607,-0.707106781186488,-5.44451754691923E-34)) ;
#64003 = DIRECTION('',(-0.707106781186607,0.707106781186488,5.44451754691923E-34)) ;
#64004 = DIRECTION('center_axis',(0.,0.,-1.)) ;
#64005 = DIRECTION('ref_axis',(0.923879532511283,0.382683432365099,0.)) ;
#64006 = DIRECTION('',(0.,0.,1.)) ;
#64007 = DIRECTION('',(0.,0.,-1.)) ;
#64008 = DIRECTION('center_axis',(0.,0.,-1.)) ;
#64009 = DIRECTION('ref_axis',(1.,0.,0.)) ;
#64010 = DIRECTION('',(0.800000000000003,0.599999999999996,0.)) ;
#64011 = DIRECTION('center_axis',(0.,0.,-1.)) ;
#64012 = DIRECTION('ref_axis',(-0.894427190999906,0.447213595499978,0.)) ;
#64013 = DIRECTION('',(0.,1.,0.)) ;
#64014 = DIRECTION('center_axis',(2.46519032881566E-32,2.3408381773461E-97,
-1.)) ;
#64015 = DIRECTION('ref_axis',(1.,1.99159183953863E-159,2.46519032881566E-32)) ;
#64016 = DIRECTION('',(0.,-1.,0.)) ;
#64017 = DIRECTION('center_axis',(0.,0.,-1.)) ;
#64018 = DIRECTION('ref_axis',(1.,0.,0.)) ;
#64019 = DIRECTION('',(-1.,0.,2.76147456380442E-35)) ;
#64020 = DIRECTION('center_axis',(0.,5.60383084497445E-34,1.)) ;
#64021 = DIRECTION('ref_axis',(0.,1.,-5.60383084497445E-34)) ;
#64022 = DIRECTION('',(1.77635683940243E-14,1.,0.)) ;
#64023 = DIRECTION('',(1.,0.,0.)) ;
#64024 = DIRECTION('',(-6.34413156929222E-15,1.,0.)) ;
#64025 = DIRECTION('',(-1.,0.,0.)) ;
#64026 = DIRECTION('',(0.,1.,0.)) ;
#64027 = DIRECTION('center_axis',(0.,0.,1.)) ;
#64028 = DIRECTION('ref_axis',(1.,0.,0.)) ;
#64029 = DIRECTION('',(1.,-1.75071816546432E-14,-2.18941313571177E-49)) ;
#64030 = DIRECTION('center_axis',(-2.46519032881566E-32,4.44295269748681E-48,
1.)) ;
#64031 = DIRECTION('ref_axis',(0.,-1.,4.44295269748681E-48)) ;
#64032 = DIRECTION('',(0.707106781186581,-0.707106781186514,0.)) ;
#64033 = DIRECTION('center_axis',(0.,0.,1.)) ;
#64034 = DIRECTION('ref_axis',(-0.707106781186481,-0.707106781186614,0.)) ;
#64035 = DIRECTION('',(-5.35505761538791E-15,-1.,1.48632706569949E-33)) ;
#64036 = DIRECTION('center_axis',(0.,0.,-1.)) ;
#64037 = DIRECTION('ref_axis',(1.,0.,0.)) ;
#64038 = DIRECTION('',(0.,1.,0.)) ;
#64039 = DIRECTION('center_axis',(2.46519032881566E-32,2.3408381773461E-97,
-1.)) ;
#64040 = DIRECTION('ref_axis',(1.,1.99159183953863E-159,2.46519032881566E-32)) ;
#64041 = DIRECTION('',(2.61228946970624E-14,1.,0.)) ;
#64042 = DIRECTION('center_axis',(0.,0.,-1.)) ;
#64043 = DIRECTION('ref_axis',(0.948683298050522,0.316227766016813,0.)) ;
#64044 = DIRECTION('',(0.599999999999982,-0.800000000000014,0.)) ;
#64045 = DIRECTION('',(1.,0.,3.20175569450239E-16)) ;
#64046 = DIRECTION('',(0.800000000000002,0.599999999999998,0.)) ;
#64047 = DIRECTION('center_axis',(0.,0.,-1.)) ;
#64048 = DIRECTION('ref_axis',(-0.89442719099992,0.44721359549995,0.)) ;
#64049 = DIRECTION('',(0.,1.,0.)) ;
#64050 = DIRECTION('center_axis',(2.46519032881566E-32,2.3408381773461E-97,
-1.)) ;
#64051 = DIRECTION('ref_axis',(1.,1.99159183953863E-159,2.46519032881566E-32)) ;
#64052 = DIRECTION('',(0.,-1.,0.)) ;
#64053 = DIRECTION('center_axis',(0.,0.,-1.)) ;
#64054 = DIRECTION('ref_axis',(1.,0.,0.)) ;
#64055 = DIRECTION('',(0.,1.,0.)) ;
#64056 = DIRECTION('center_axis',(2.46519032881566E-32,2.3408381773461E-97,
-1.)) ;
#64057 = DIRECTION('ref_axis',(1.,1.99159183953863E-159,2.46519032881566E-32)) ;
#64058 = DIRECTION('',(0.,1.,0.)) ;
#64059 = DIRECTION('center_axis',(0.,0.,-1.)) ;
#64060 = DIRECTION('ref_axis',(0.948683298050519,0.316227766016821,0.)) ;
#64061 = DIRECTION('',(0.600000000000002,-0.799999999999998,0.)) ;
#64062 = DIRECTION('',(-1.,0.,0.)) ;
#64063 = DIRECTION('',(0.,-1.,0.)) ;
#64064 = DIRECTION('',(1.,0.,0.)) ;
#64065 = DIRECTION('',(-1.30614473485314E-15,1.,0.)) ;
#64066 = DIRECTION('',(1.,0.,0.)) ;
#64067 = DIRECTION('',(-1.,0.,0.)) ;
#64068 = DIRECTION('',(1.,0.,0.)) ;
#64069 = DIRECTION('',(0.,-1.,0.)) ;
#64070 = DIRECTION('',(1.,-4.35522519302374E-15,0.)) ;
#64071 = DIRECTION('center_axis',(0.,0.,-1.)) ;
#64072 = DIRECTION('ref_axis',(0.,1.,0.)) ;
#64073 = DIRECTION('',(-1.46896958313692E-15,-1.,0.)) ;
#64074 = DIRECTION('center_axis',(0.,0.,1.)) ;
#64075 = DIRECTION('ref_axis',(-0.819152044288993,-0.573576436351044,0.)) ;
#64076 = DIRECTION('',(0.573576436351043,-0.819152044288994,0.)) ;
#64077 = DIRECTION('',(0.,1.,0.)) ;
#64078 = DIRECTION('center_axis',(0.,0.,-1.)) ;
#64079 = DIRECTION('ref_axis',(-1.,0.,0.)) ;
#64080 = DIRECTION('',(0.529919264233188,0.848048096156437,0.)) ;
#64081 = DIRECTION('',(-0.707106781186471,0.707106781186624,0.)) ;
#64082 = DIRECTION('center_axis',(0.,0.,-1.)) ;
#64083 = DIRECTION('ref_axis',(-1.,0.,0.)) ;
#64084 = DIRECTION('',(0.801695394071906,-0.597732795757345,0.)) ;
#64085 = DIRECTION('',(3.67742382159233E-14,1.,0.)) ;
#64086 = DIRECTION('',(1.,0.,0.)) ;
#64087 = DIRECTION('',(-3.67742382159233E-14,-1.,0.)) ;
#64088 = DIRECTION('center_axis',(0.,0.,1.)) ;
#64089 = DIRECTION('ref_axis',(-0.918360381793699,0.395745131557839,0.)) ;
#64090 = DIRECTION('center_axis',(0.,0.,1.)) ;
#64091 = DIRECTION('ref_axis',(-0.977748097404052,0.209782406370878,0.)) ;
#64092 = DIRECTION('center_axis',(2.52374105052742E-18,5.60383084497445E-34,
-1.)) ;
#64093 = DIRECTION('ref_axis',(-1.,3.9474596431117E-14,-2.52374105052742E-18)) ;
#64094 = DIRECTION('center_axis',(2.46519032881566E-32,-1.7915701050753E-48,
-1.)) ;
#64095 = DIRECTION('ref_axis',(0.,-1.,1.7915701050753E-48)) ;
#64096 = DIRECTION('',(-3.17206578464333E-15,-1.,1.76085023486835E-33)) ;
#64097 = DIRECTION('center_axis',(2.46519032881571E-32,4.87512283120816E-48,
-1.)) ;
#64098 = DIRECTION('ref_axis',(-1.,-3.7453410837561E-96,-2.46519032881571E-32)) ;
#64099 = DIRECTION('',(-1.,-3.55271367880026E-13,3.80009837042949E-30)) ;
#64100 = DIRECTION('',(0.,-1.,1.41044871512355E-33)) ;
#64101 = DIRECTION('center_axis',(2.46519032881571E-32,4.87512283120816E-48,
-1.)) ;
#64102 = DIRECTION('ref_axis',(-1.,-3.7453410837561E-96,-2.46519032881571E-32)) ;
#64103 = DIRECTION('',(-1.,0.,-1.40067632319071E-31)) ;
#64104 = DIRECTION('center_axis',(2.46519032881566E-32,-1.7915701050753E-48,
-1.)) ;
#64105 = DIRECTION('ref_axis',(0.,1.,-1.7915701050753E-48)) ;
#64106 = DIRECTION('',(1.53134210293125E-15,1.,-6.60793205056998E-32)) ;
#64107 = DIRECTION('',(-1.,0.,3.83260058933034E-30)) ;
#64108 = DIRECTION('center_axis',(2.46519032881566E-32,0.,-1.)) ;
#64109 = DIRECTION('ref_axis',(0.,1.,0.)) ;
#64110 = DIRECTION('',(3.17206578464333E-15,1.,-1.76085023486835E-33)) ;
#64111 = DIRECTION('center_axis',(0.,0.,-1.)) ;
#64112 = DIRECTION('ref_axis',(-1.,3.9474596431117E-14,0.)) ;
#64113 = DIRECTION('',(1.,-3.55271367880048E-14,0.)) ;
#64114 = DIRECTION('',(0.,1.,0.)) ;
#64115 = DIRECTION('',(1.,0.,6.12949496482233E-35)) ;
#64116 = DIRECTION('center_axis',(2.46519032881566E-32,-2.48770373612753E-33,
1.)) ;
#64117 = DIRECTION('ref_axis',(0.,-1.,-2.48770373612753E-33)) ;
#64118 = DIRECTION('',(0.707106781186586,-0.707106781186509,-7.3914897815741E-47)) ;
#64119 = DIRECTION('center_axis',(8.71576399210415E-33,-8.71576399210634E-33,
1.)) ;
#64120 = DIRECTION('ref_axis',(-0.707106781186681,-0.707106781186414,7.78326232344021E-46)) ;
#64121 = DIRECTION('',(-5.35505761538786E-15,-1.,7.43163532849736E-34)) ;
#64122 = DIRECTION('center_axis',(-2.46519032881571E-32,-5.98699295060652E-49,
1.)) ;
#64123 = DIRECTION('ref_axis',(-1.,7.31836847501401E-110,-2.46519032881571E-32)) ;
#64124 = DIRECTION('',(-0.707106781186539,-0.707106781186556,1.17554800907501E-33)) ;
#64125 = DIRECTION('center_axis',(3.18850138855159E-46,1.74315279842113E-32,
1.)) ;
#64126 = DIRECTION('ref_axis',(-0.707106781186636,0.707106781186459,-1.23259516440771E-32)) ;
#64127 = DIRECTION('',(-1.,0.,0.)) ;
#64128 = DIRECTION('',(0.,1.,0.)) ;
#64129 = DIRECTION('center_axis',(0.,0.,1.)) ;
#64130 = DIRECTION('ref_axis',(-0.73407014073105,0.679073654684893,0.)) ;
#64131 = DIRECTION('center_axis',(0.,0.,-1.)) ;
#64132 = DIRECTION('ref_axis',(0.457543425680166,-0.889187277021471,0.)) ;
#64133 = DIRECTION('',(-0.642787609686516,-0.766044443118998,0.)) ;
#64134 = DIRECTION('center_axis',(0.,0.,-1.)) ;
#64135 = DIRECTION('ref_axis',(0.939692620785897,-0.3420201433257,0.)) ;
#64136 = DIRECTION('',(-1.20119700805775E-14,-1.,0.)) ;
#64137 = DIRECTION('',(0.642787609686599,-0.766044443118928,0.)) ;
#64138 = DIRECTION('center_axis',(0.,0.,-1.)) ;
#64139 = DIRECTION('ref_axis',(0.422618261740741,0.906307787036631,0.)) ;
#64140 = DIRECTION('',(1.,-1.28403006865249E-14,0.)) ;
#64141 = DIRECTION('center_axis',(0.,0.,1.)) ;
#64142 = DIRECTION('ref_axis',(0.,1.,0.)) ;
#64143 = DIRECTION('center_axis',(0.,0.,1.)) ;
#64144 = DIRECTION('ref_axis',(1.,0.,0.)) ;
#64145 = DIRECTION('',(0.,1.,0.)) ;
#64146 = DIRECTION('',(1.,0.,0.)) ;
#64147 = DIRECTION('center_axis',(0.,0.,1.)) ;
#64148 = DIRECTION('ref_axis',(1.,0.,0.)) ;
#64149 = DIRECTION('',(1.,0.,-1.93235546378459E-35)) ;
#64150 = DIRECTION('center_axis',(0.,5.60383084497445E-34,1.)) ;
#64151 = DIRECTION('ref_axis',(0.,-1.,5.60383084497445E-34)) ;
#64152 = DIRECTION('',(-5.69345140833415E-16,-1.,3.47655046371441E-32)) ;
#64153 = DIRECTION('center_axis',(-1.35585468084861E-30,4.50611349139124E-93,
1.)) ;
#64154 = DIRECTION('ref_axis',(-1.,4.98510362034913E-139,-1.35585468084861E-30)) ;
#64155 = DIRECTION('',(-1.,-6.125368411725E-15,1.93235546378459E-35)) ;
#64156 = DIRECTION('center_axis',(0.,5.60383084497445E-34,1.)) ;
#64157 = DIRECTION('ref_axis',(0.,1.,-5.60383084497445E-34)) ;
#64158 = DIRECTION('',(-1.13869028166683E-15,1.,0.)) ;
#64159 = DIRECTION('center_axis',(0.,0.,1.)) ;
#64160 = DIRECTION('ref_axis',(1.,0.,0.)) ;
#64161 = DIRECTION('center_axis',(-2.46519032881571E-32,-4.87512283120816E-48,
1.)) ;
#64162 = DIRECTION('ref_axis',(-1.,-3.7453410837561E-96,-2.46519032881571E-32)) ;
#64163 = DIRECTION('',(-1.,0.,1.62870009552296E-49)) ;
#64164 = DIRECTION('center_axis',(-2.46519032881566E-32,1.7915701050753E-48,
1.)) ;
#64165 = DIRECTION('ref_axis',(0.,1.,-1.7915701050753E-48)) ;
#64166 = DIRECTION('',(1.53134210293126E-15,1.,0.)) ;
#64167 = DIRECTION('',(-1.,3.55271367880026E-13,9.05696233641872E-48)) ;
#64168 = DIRECTION('center_axis',(-2.46519032881566E-32,4.52848116820976E-48,
1.)) ;
#64169 = DIRECTION('ref_axis',(0.,1.,-4.52848116820976E-48)) ;
#64170 = DIRECTION('',(0.,1.,-1.76085023486835E-33)) ;
#64171 = DIRECTION('center_axis',(-2.46519032881572E-32,-8.55284707229503E-50,
1.)) ;
#64172 = DIRECTION('ref_axis',(1.,-2.20382687031672E-110,2.46519032881572E-32)) ;
#64173 = DIRECTION('',(1.,-1.26882631385732E-14,-1.27969293219661E-49)) ;
#64174 = DIRECTION('center_axis',(-2.46519032881566E-32,1.7915701050753E-48,
1.)) ;
#64175 = DIRECTION('ref_axis',(0.,-1.,1.7915701050753E-48)) ;
#64176 = DIRECTION('',(0.,-1.,1.76085023486835E-33)) ;
#64177 = DIRECTION('center_axis',(-2.46519032881571E-32,-4.87512283120816E-48,
1.)) ;
#64178 = DIRECTION('ref_axis',(-1.,-3.7453410837561E-96,-2.46519032881571E-32)) ;
#64179 = DIRECTION('',(-1.,-3.55271367880026E-13,5.47382212626845E-48)) ;
#64180 = DIRECTION('',(0.,-1.,8.50065630626093E-34)) ;
#64181 = DIRECTION('center_axis',(0.,0.,1.)) ;
#64182 = DIRECTION('ref_axis',(1.,0.,0.)) ;
#64183 = DIRECTION('',(0.,-1.,0.)) ;
#64184 = DIRECTION('',(-1.,8.7535908273216E-15,2.56873619635494E-49)) ;
#64185 = DIRECTION('center_axis',(-2.46519032881566E-32,5.21270893399338E-48,
1.)) ;
#64186 = DIRECTION('ref_axis',(0.,1.,-5.21270893399338E-48)) ;
#64187 = DIRECTION('',(-0.707106781186556,0.707106781186539,0.)) ;
#64188 = DIRECTION('center_axis',(0.,0.,1.)) ;
#64189 = DIRECTION('ref_axis',(0.707106781186636,0.707106781186459,0.)) ;
#64190 = DIRECTION('',(0.,1.,-1.48632706569949E-33)) ;
#64191 = DIRECTION('center_axis',(-2.46519032881571E-32,-3.84878118253276E-49,
1.)) ;
#64192 = DIRECTION('ref_axis',(1.,7.31836847501401E-110,2.46519032881571E-32)) ;
#64193 = DIRECTION('',(0.707106781186522,0.707106781186573,-4.31889331967372E-49)) ;
#64194 = DIRECTION('center_axis',(-8.71576399210634E-33,-8.71576399210415E-33,
1.)) ;
#64195 = DIRECTION('ref_axis',(0.707106781186459,-0.707106781186636,6.33174217877954E-48)) ;
#64196 = DIRECTION('',(1.,0.,0.)) ;
#64197 = DIRECTION('',(-1.,0.,0.)) ;
#64198 = DIRECTION('',(0.,1.,0.)) ;
#64199 = DIRECTION('',(-1.,3.55271367880026E-13,2.00046065889556E-47)) ;
#64200 = DIRECTION('center_axis',(-2.46519032881566E-32,1.00023032944787E-47,
1.)) ;
#64201 = DIRECTION('ref_axis',(0.,1.,-1.00023032944787E-47)) ;
#64202 = DIRECTION('',(0.,1.,-1.76085023486835E-33)) ;
#64203 = DIRECTION('center_axis',(-2.46519032881571E-32,0.,1.)) ;
#64204 = DIRECTION('ref_axis',(1.,0.,2.46519032881571E-32)) ;
#64205 = DIRECTION('',(1.,0.,-4.0027363178395E-35)) ;
#64206 = DIRECTION('center_axis',(0.,5.60383084497445E-34,1.)) ;
#64207 = DIRECTION('ref_axis',(0.,-1.,5.60383084497445E-34)) ;
#64208 = DIRECTION('',(0.,-1.,1.76085023486835E-33)) ;
#64209 = DIRECTION('center_axis',(-2.46519032881571E-32,-4.6816763546922E-97,
1.)) ;
#64210 = DIRECTION('ref_axis',(-1.,1.001486182168E-157,-2.46519032881571E-32)) ;
#64211 = DIRECTION('',(-1.,0.,0.)) ;
#64212 = DIRECTION('',(0.,-1.,0.)) ;
#64213 = DIRECTION('center_axis',(-2.46519032881571E-32,-4.87512283120816E-48,
1.)) ;
#64214 = DIRECTION('ref_axis',(-1.,-3.7453410837561E-96,-2.46519032881571E-32)) ;
#64215 = DIRECTION('',(-1.,0.,1.62870009552296E-49)) ;
#64216 = DIRECTION('center_axis',(-2.46519032881566E-32,1.7915701050753E-48,
1.)) ;
#64217 = DIRECTION('ref_axis',(0.,1.,-1.7915701050753E-48)) ;
#64218 = DIRECTION('',(1.53134210293126E-15,1.,0.)) ;
#64219 = DIRECTION('',(-1.,3.55271367880026E-13,9.05696233641872E-48)) ;
#64220 = DIRECTION('center_axis',(-2.46519032881566E-32,4.52848116820976E-48,
1.)) ;
#64221 = DIRECTION('ref_axis',(0.,1.,-4.52848116820976E-48)) ;
#64222 = DIRECTION('',(0.,1.,-1.76085023486835E-33)) ;
#64223 = DIRECTION('center_axis',(-2.46519032881571E-32,-5.98699295060652E-49,
1.)) ;
#64224 = DIRECTION('ref_axis',(1.,-7.31836847501401E-110,2.46519032881571E-32)) ;
#64225 = DIRECTION('',(1.,-1.26882631385732E-14,-1.27969293219661E-49)) ;
#64226 = DIRECTION('center_axis',(-2.46519032881566E-32,1.7915701050753E-48,
1.)) ;
#64227 = DIRECTION('ref_axis',(0.,-1.,1.7915701050753E-48)) ;
#64228 = DIRECTION('',(0.,-1.,1.76085023486835E-33)) ;
#64229 = DIRECTION('center_axis',(-2.46519032881571E-32,-4.87512283120816E-48,
1.)) ;
#64230 = DIRECTION('ref_axis',(-1.,-3.7453410837561E-96,-2.46519032881571E-32)) ;
#64231 = DIRECTION('',(-1.,-3.55271367880026E-13,5.47382212626845E-48)) ;
#64232 = DIRECTION('',(0.,-1.,8.50065630626093E-34)) ;
#64233 = DIRECTION('center_axis',(-0.707106781186488,-0.707106781186607,0.)) ;
#64234 = DIRECTION('ref_axis',(-0.707106781186607,0.707106781186488,3.7126864764714E-32)) ;
#64235 = DIRECTION('center_axis',(0.,0.,1.)) ;
#64236 = DIRECTION('ref_axis',(-0.986303541071623,0.164940367616834,0.)) ;
#64237 = DIRECTION('center_axis',(-0.720370089059342,-0.693589889479825,1.27963433459996E-13)) ;
#64238 = DIRECTION('ref_axis',(0.693589889479825,-0.720370089059342,3.63922431499158E-30)) ;
#64239 = DIRECTION('center_axis',(0.,0.,-1.)) ;
#64240 = DIRECTION('ref_axis',(-0.498769364572801,-0.86673474659993,0.)) ;
#64241 = DIRECTION('',(0.,0.,-1.)) ;
#64242 = DIRECTION('',(0.,0.,1.)) ;
#64243 = DIRECTION('center_axis',(0.,0.,1.)) ;
#64244 = DIRECTION('ref_axis',(1.,0.,0.)) ;
#64245 = DIRECTION('center_axis',(0.,0.,-1.)) ;
#64246 = DIRECTION('ref_axis',(-0.977748097404052,0.209782406370878,0.)) ;
#64247 = DIRECTION('center_axis',(0.,0.,1.)) ;
#64248 = DIRECTION('ref_axis',(1.,0.,0.)) ;
#64249 = DIRECTION('center_axis',(0.,1.,0.)) ;
#64250 = DIRECTION('ref_axis',(0.,0.,1.)) ;
#64251 = DIRECTION('center_axis',(0.,0.,-1.)) ;
#64252 = DIRECTION('ref_axis',(-0.918360381793699,0.395745131557839,0.)) ;
#64253 = DIRECTION('center_axis',(3.67742382159233E-14,1.,0.)) ;
#64254 = DIRECTION('ref_axis',(0.707106781186548,-2.60033132154489E-14,0.707106781186548)) ;
#64255 = DIRECTION('center_axis',(0.,-1.,0.)) ;
#64256 = DIRECTION('ref_axis',(0.707106781186548,0.,0.707106781186548)) ;
#64257 = DIRECTION('',(3.67742382159233E-14,1.,0.)) ;
#64258 = DIRECTION('center_axis',(0.,0.,-1.)) ;
#64259 = DIRECTION('ref_axis',(-1.,0.,0.)) ;
#64260 = DIRECTION('',(0.,0.,1.)) ;
#64261 = DIRECTION('center_axis',(0.,0.,-1.)) ;
#64262 = DIRECTION('ref_axis',(-1.,3.55271367880053E-14,0.)) ;
#64263 = DIRECTION('',(0.,0.,-1.)) ;
#64264 = DIRECTION('center_axis',(0.,0.,1.)) ;
#64265 = DIRECTION('ref_axis',(-0.707106781186519,0.707106781186576,0.)) ;
#64266 = DIRECTION('',(0.,0.,-1.)) ;
#64267 = DIRECTION('center_axis',(1.,-3.67742382159233E-14,0.)) ;
#64268 = DIRECTION('ref_axis',(-3.67742382159233E-14,-1.,0.)) ;
#64269 = DIRECTION('',(0.,0.,-1.)) ;
#64270 = DIRECTION('',(-3.67742382159233E-14,-1.,0.)) ;
#64271 = DIRECTION('',(0.,0.,-1.)) ;
#64272 = DIRECTION('',(-3.67742382159233E-14,-1.,0.)) ;
#64273 = DIRECTION('center_axis',(0.,-1.,0.)) ;
#64274 = DIRECTION('ref_axis',(-1.,0.,0.)) ;
#64275 = DIRECTION('',(0.,0.,-1.)) ;
#64276 = DIRECTION('',(0.,0.,-1.)) ;
#64277 = DIRECTION('',(1.,0.,-3.18850138855159E-46)) ;
#64278 = DIRECTION('',(0.,0.,-1.)) ;
#64279 = DIRECTION('center_axis',(-0.120859073829245,-0.847660295597975,-0.516589883311598)) ;
#64280 = DIRECTION('ref_axis',(0.193100538836725,-0.530539370138308,0.825372739211936)) ;
#64281 = DIRECTION('center_axis',(0.,0.,1.)) ;
#64282 = DIRECTION('ref_axis',(1.,0.,0.)) ;
#64283 = DIRECTION('center_axis',(0.,-1.,0.)) ;
#64284 = DIRECTION('ref_axis',(0.,0.,1.)) ;
#64285 = DIRECTION('center_axis',(0.642787609686577,-0.766044443118946,-1.14182016674851E-13)) ;
#64286 = DIRECTION('ref_axis',(-0.766044443118946,-0.642787609686577,1.64598929132938E-30)) ;
#64287 = DIRECTION('center_axis',(0.,-1.,-7.6997105554314E-34)) ;
#64288 = DIRECTION('ref_axis',(0.707106781186548,-5.44451754691918E-34,0.707106781186548)) ;
#64289 = DIRECTION('',(0.,-1.,-7.6997105554314E-34)) ;
#64290 = DIRECTION('center_axis',(0.,1.,0.)) ;
#64291 = DIRECTION('ref_axis',(0.,0.,1.)) ;
#64292 = DIRECTION('',(0.,1.,7.6997105554314E-34)) ;
#64293 = DIRECTION('center_axis',(-7.16300942304673E-47,7.6997105554314E-34,
-1.)) ;
#64294 = DIRECTION('ref_axis',(-1.,0.,0.)) ;
#64295 = DIRECTION('center_axis',(-0.707106781186725,0.70710678118637,0.)) ;
#64296 = DIRECTION('ref_axis',(0.,0.,1.)) ;
#64297 = DIRECTION('center_axis',(-7.16300942304673E-47,7.6997105554314E-34,
-1.)) ;
#64298 = DIRECTION('ref_axis',(-0.923879532511266,-0.382683432365139,-2.94655166356992E-34)) ;
#64299 = DIRECTION('center_axis',(7.16300942304673E-47,-7.6997105554314E-34,
1.)) ;
#64300 = DIRECTION('ref_axis',(-0.923879532511267,-0.382683432365139,-2.94655166356992E-34)) ;
#64301 = DIRECTION('center_axis',(-0.70710678118661,0.707106781186485,5.4445175469192E-34)) ;
#64302 = DIRECTION('ref_axis',(0.499999999999923,0.500000000000011,0.707106781186594)) ;
#64303 = DIRECTION('center_axis',(-0.707106781186548,0.707106781186548,0.)) ;
#64304 = DIRECTION('ref_axis',(0.,0.,1.)) ;
#64305 = DIRECTION('',(-0.70710678118661,0.707106781186485,5.4445175469192E-34)) ;
#64306 = DIRECTION('',(0.70710678118661,-0.707106781186485,-5.4445175469192E-34)) ;
#64307 = DIRECTION('center_axis',(-7.16300942304673E-47,7.6997105554314E-34,
-1.)) ;
#64308 = DIRECTION('ref_axis',(-1.,0.,0.)) ;
#64309 = DIRECTION('center_axis',(0.,1.,0.)) ;
#64310 = DIRECTION('ref_axis',(0.,0.,1.)) ;
#64311 = DIRECTION('center_axis',(7.16300942304673E-47,-7.6997105554314E-34,
1.)) ;
#64312 = DIRECTION('ref_axis',(0.923879532511283,0.382683432365099,2.94655166356961E-34)) ;
#64313 = DIRECTION('center_axis',(-7.16300942304673E-47,7.6997105554314E-34,
-1.)) ;
#64314 = DIRECTION('ref_axis',(0.923879532511283,0.382683432365099,2.94655166356961E-34)) ;
#64315 = DIRECTION('center_axis',(-1.20119700805775E-14,-1.,-7.6997105554314E-34)) ;
#64316 = DIRECTION('ref_axis',(0.70710678118661,-8.49374549938702E-15,0.707106781186485)) ;
#64317 = DIRECTION('',(1.20119700805775E-14,1.,7.6997105554314E-34)) ;
#64318 = DIRECTION('',(-1.20119700805775E-14,-1.,-7.6997105554314E-34)) ;
#64319 = DIRECTION('center_axis',(1.,-1.28403006865249E-14,-8.15167541035622E-47)) ;
#64320 = DIRECTION('ref_axis',(-9.07946368791524E-15,-0.707106781186485,0.70710678118661)) ;
#64321 = DIRECTION('',(1.,-1.28403006865249E-14,-8.15167541035622E-47)) ;
#64322 = DIRECTION('center_axis',(-1.,0.,0.)) ;
#64323 = DIRECTION('ref_axis',(0.,-1.,0.)) ;
#64324 = DIRECTION('',(-1.,1.28403006865249E-14,8.15167541035622E-47)) ;
#64325 = DIRECTION('center_axis',(-7.16300942304673E-47,7.6997105554314E-34,
-1.)) ;
#64326 = DIRECTION('ref_axis',(-1.,0.,0.)) ;
#64327 = DIRECTION('center_axis',(-0.64278760968649,0.76604444311902,0.)) ;
#64328 = DIRECTION('ref_axis',(-0.76604444311902,-0.64278760968649,0.)) ;
#64329 = DIRECTION('center_axis',(7.16300942304673E-47,-7.6997105554314E-34,
1.)) ;
#64330 = DIRECTION('ref_axis',(0.42261826174077,0.906307787036617,6.97830763431521E-34)) ;
#64331 = DIRECTION('center_axis',(-7.16300942304673E-47,7.6997105554314E-34,
-1.)) ;
#64332 = DIRECTION('ref_axis',(0.42261826174077,0.906307787036617,6.97830763431521E-34)) ;
#64333 = DIRECTION('center_axis',(0.642787609686599,-0.766044443118928,-5.89832048461284E-34)) ;
#64334 = DIRECTION('ref_axis',(-0.541675220419631,-0.454519477672056,0.707106781186594)) ;
#64335 = DIRECTION('',(-0.642787609686599,0.766044443118928,5.89832048461284E-34)) ;
#64336 = DIRECTION('',(0.642787609686599,-0.766044443118928,-5.89832048461284E-34)) ;
#64337 = DIRECTION('center_axis',(-0.95507414978076,-0.296366948934188,0.)) ;
#64338 = DIRECTION('ref_axis',(-0.296366948934188,0.955074149780759,0.)) ;
#64339 = DIRECTION('center_axis',(0.,-1.,0.)) ;
#64340 = DIRECTION('ref_axis',(1.,0.,0.)) ;
#64341 = DIRECTION('center_axis',(1.,-1.20119700805775E-14,0.)) ;
#64342 = DIRECTION('ref_axis',(1.20119700805775E-14,1.,-5.57529378295193E-17)) ;
#64343 = DIRECTION('center_axis',(0.,0.,1.)) ;
#64344 = DIRECTION('ref_axis',(-0.76604444311902,-0.64278760968649,0.)) ;
#64345 = DIRECTION('center_axis',(0.,0.,-1.)) ;
#64346 = DIRECTION('ref_axis',(-1.,0.,0.)) ;
#64347 = DIRECTION('center_axis',(0.,0.,-1.)) ;
#64348 = DIRECTION('ref_axis',(-0.73407014073105,0.679073654684893,0.)) ;
#64349 = DIRECTION('center_axis',(-0.996975386522573,-0.0777179430258286,
0.)) ;
#64350 = DIRECTION('ref_axis',(0.0777179430258286,-0.996975386522573,0.)) ;
#64351 = DIRECTION('center_axis',(-0.642787609686786,-0.766044443118771,0.)) ;
#64352 = DIRECTION('ref_axis',(0.766044443118771,-0.642787609686786,0.)) ;
#64353 = DIRECTION('center_axis',(0.,0.,1.)) ;
#64354 = DIRECTION('ref_axis',(0.457543425680166,-0.889187277021471,0.)) ;
#64355 = DIRECTION('center_axis',(0.642787609686516,0.766044443118998,0.)) ;
#64356 = DIRECTION('ref_axis',(0.54167522041968,-0.454519477671997,0.707106781186594)) ;
#64357 = DIRECTION('center_axis',(-0.642787609686577,-0.766044443118946,0.)) ;
#64358 = DIRECTION('ref_axis',(0.766044443118946,-0.642787609686577,0.)) ;
#64359 = DIRECTION('',(0.642787609686516,0.766044443118998,0.)) ;
#64360 = DIRECTION('center_axis',(0.,0.,-1.)) ;
#64361 = DIRECTION('ref_axis',(-1.,0.,0.)) ;
#64362 = DIRECTION('center_axis',(3.55271367880058E-13,-1.,0.)) ;
#64363 = DIRECTION('ref_axis',(1.,3.55271367880058E-13,0.)) ;
#64364 = DIRECTION('center_axis',(0.,0.,1.)) ;
#64365 = DIRECTION('ref_axis',(0.939692620785897,-0.3420201433257,0.)) ;
#64366 = DIRECTION('center_axis',(-1.20119700805775E-14,-1.,0.)) ;
#64367 = DIRECTION('ref_axis',(0.70710678118661,-8.49374549938702E-15,0.707106781186485)) ;
#64368 = DIRECTION('',(1.20119700805775E-14,1.,0.)) ;
#64369 = DIRECTION('center_axis',(0.,0.,-1.)) ;
#64370 = DIRECTION('ref_axis',(0.342020143325632,-0.939692620785922,0.)) ;
#64371 = DIRECTION('',(0.,0.,1.)) ;
#64372 = DIRECTION('',(0.,0.,-1.)) ;
#64373 = DIRECTION('center_axis',(-0.642787609686599,0.766044443118928,0.)) ;
#64374 = DIRECTION('ref_axis',(0.541675220419631,0.454519477672056,-0.707106781186594)) ;
#64375 = DIRECTION('center_axis',(-0.642787609686503,0.766044443119009,0.)) ;
#64376 = DIRECTION('ref_axis',(0.766044443119009,0.642787609686503,0.)) ;
#64377 = DIRECTION('',(-0.642787609686599,0.766044443118928,0.)) ;
#64378 = DIRECTION('center_axis',(0.,0.,1.)) ;
#64379 = DIRECTION('ref_axis',(1.,0.,0.)) ;
#64380 = DIRECTION('center_axis',(-1.,1.7763568394006E-13,0.)) ;
#64381 = DIRECTION('ref_axis',(1.7763568394006E-13,1.,0.)) ;
#64382 = DIRECTION('center_axis',(0.,0.,1.)) ;
#64383 = DIRECTION('ref_axis',(0.422618261740741,0.906307787036631,0.)) ;
#64384 = DIRECTION('center_axis',(-1.,1.28403006865249E-14,0.)) ;
#64385 = DIRECTION('ref_axis',(9.07946368791846E-15,0.707106781186736,-0.707106781186359)) ;
#64386 = DIRECTION('center_axis',(-1.,0.,0.)) ;
#64387 = DIRECTION('ref_axis',(0.,1.,0.)) ;
#64388 = DIRECTION('',(-1.,1.28403006865249E-14,0.)) ;
#64389 = DIRECTION('center_axis',(-7.16300942304673E-47,7.6997105554314E-34,
-1.)) ;
#64390 = DIRECTION('ref_axis',(1.,7.82584617141943E-97,-7.16300942304673E-47)) ;
#64391 = DIRECTION('',(-1.,0.,2.99489585516063E-33)) ;
#64392 = DIRECTION('',(0.,-1.,2.39087358882206E-65)) ;
#64393 = DIRECTION('center_axis',(-7.16300942304673E-47,7.6997105554314E-34,
-1.)) ;
#64394 = DIRECTION('ref_axis',(1.,7.82584617141943E-97,-7.16300942304673E-47)) ;
#64395 = DIRECTION('center_axis',(1.,0.,0.)) ;
#64396 = DIRECTION('ref_axis',(0.,-1.,0.)) ;
#64397 = DIRECTION('',(0.,0.,-1.)) ;
#64398 = DIRECTION('',(0.,-1.,0.)) ;
#64399 = DIRECTION('',(0.,-0.624695047554423,-0.780868809443031)) ;
#64400 = DIRECTION('center_axis',(-1.,0.,0.)) ;
#64401 = DIRECTION('ref_axis',(0.,0.624695047554423,0.780868809443031)) ;
#64402 = DIRECTION('center_axis',(0.,0.,-1.)) ;
#64403 = DIRECTION('ref_axis',(-0.707106781186437,-0.707106781186659,0.)) ;
#64404 = DIRECTION('',(0.,0.,-1.)) ;
#64405 = DIRECTION('center_axis',(0.,0.,1.)) ;
#64406 = DIRECTION('ref_axis',(-0.923879532511266,-0.382683432365139,0.)) ;
#64407 = DIRECTION('center_axis',(0.707106781186485,0.70710678118661,0.)) ;
#64408 = DIRECTION('ref_axis',(0.70710678118661,-0.707106781186485,-2.64349870476783E-32)) ;
#64409 = DIRECTION('',(0.,0.,1.)) ;
#64410 = DIRECTION('',(0.70710678118661,-0.707106781186485,0.)) ;
#64411 = DIRECTION('center_axis',(0.,0.,-1.)) ;
#64412 = DIRECTION('ref_axis',(0.923879532511278,0.38268343236511,0.)) ;
#64413 = DIRECTION('',(0.,0.,-1.)) ;
#64414 = DIRECTION('center_axis',(0.,0.,-1.)) ;
#64415 = DIRECTION('ref_axis',(0.923879532511283,0.382683432365099,0.)) ;
#64416 = DIRECTION('center_axis',(1.,-1.20119700805775E-14,0.)) ;
#64417 = DIRECTION('ref_axis',(-1.20119700805775E-14,-1.,2.16979082419566E-32)) ;
#64418 = DIRECTION('',(0.,0.,-1.)) ;
#64419 = DIRECTION('',(-1.13955553921264E-14,-0.948683298050513,-0.316227766016839)) ;
#64420 = DIRECTION('center_axis',(1.,-1.20119700805775E-14,0.)) ;
#64421 = DIRECTION('ref_axis',(-1.92410431043973E-15,-0.160182243006988,0.987087457637493)) ;
#64422 = DIRECTION('',(-1.20119700805775E-14,-1.,0.)) ;
#64423 = DIRECTION('center_axis',(-1.,1.20119700805775E-14,0.)) ;
#64424 = DIRECTION('ref_axis',(4.59678193990225E-15,0.382683432365097,-0.923879532511284)) ;
#64425 = DIRECTION('',(-8.49374549938626E-15,-0.707106781186546,-0.707106781186549)) ;
#64426 = DIRECTION('center_axis',(1.,-1.20119700805775E-14,0.)) ;
#64427 = DIRECTION('ref_axis',(-4.59678193990225E-15,-0.382683432365097,0.923879532511284)) ;
#64428 = DIRECTION('',(-1.20119700805775E-14,-1.,0.)) ;
#64429 = DIRECTION('center_axis',(0.,0.,-1.)) ;
#64430 = DIRECTION('ref_axis',(1.,7.10542735760242E-14,0.)) ;
#64431 = DIRECTION('',(0.,0.,-1.)) ;
#64432 = DIRECTION('center_axis',(-1.14425202895153E-15,0.257662650560322,
-0.966234939601249)) ;
#64433 = DIRECTION('ref_axis',(1.02982682605711E-13,-0.966234939601249,-0.257662650560322)) ;
#64434 = DIRECTION('center_axis',(0.766044443118998,-0.642787609686516,0.)) ;
#64435 = DIRECTION('ref_axis',(-0.642787609686516,-0.766044443118998,0.)) ;
#64436 = DIRECTION('',(0.,0.,-1.)) ;
#64437 = DIRECTION('',(-0.622803969959022,-0.742228868680647,-0.247409622893551)) ;
#64438 = DIRECTION('center_axis',(0.,0.,-1.)) ;
#64439 = DIRECTION('ref_axis',(0.766044443118867,-0.642787609686671,0.)) ;
#64440 = DIRECTION('',(0.,0.,1.)) ;
#64441 = DIRECTION('center_axis',(0.,0.16439898730545,-0.986393923832128)) ;
#64442 = DIRECTION('ref_axis',(0.,-0.986393923832128,-0.16439898730545)) ;
#64443 = DIRECTION('center_axis',(0.,0.,-1.)) ;
#64444 = DIRECTION('ref_axis',(1.,0.,0.)) ;
#64445 = DIRECTION('center_axis',(0.,0.,1.)) ;
#64446 = DIRECTION('ref_axis',(-0.933145676371942,0.359498465460357,0.)) ;
#64447 = DIRECTION('center_axis',(-2.08472420634511E-15,-0.344254649158429,
0.938876315886606)) ;
#64448 = DIRECTION('ref_axis',(-7.36069948638338E-33,0.938876315886606,0.344254649158429)) ;
#64449 = DIRECTION('center_axis',(0.,0.983937861384704,0.178511301977483)) ;
#64450 = DIRECTION('ref_axis',(1.,0.,0.)) ;
#64451 = DIRECTION('center_axis',(1.,0.,0.)) ;
#64452 = DIRECTION('ref_axis',(0.,0.511844635310909,-0.85907803446686)) ;
#64453 = DIRECTION('center_axis',(0.,0.,-1.)) ;
#64454 = DIRECTION('ref_axis',(-0.707106781186359,-0.707106781186736,0.)) ;
#64455 = DIRECTION('center_axis',(0.,0.,-1.)) ;
#64456 = DIRECTION('ref_axis',(-0.707106781186359,-0.707106781186736,0.)) ;
#64457 = DIRECTION('',(0.,0.,-1.)) ;
#64458 = DIRECTION('',(0.,0.,1.)) ;
#64459 = DIRECTION('center_axis',(0.,0.,1.)) ;
#64460 = DIRECTION('ref_axis',(1.,0.,0.)) ;
#64461 = DIRECTION('center_axis',(0.,0.,1.)) ;
#64462 = DIRECTION('ref_axis',(-1.,0.,0.)) ;
#64463 = DIRECTION('center_axis',(0.,-1.,0.)) ;
#64464 = DIRECTION('ref_axis',(0.,0.,-1.)) ;
#64465 = DIRECTION('center_axis',(0.,0.,-1.)) ;
#64466 = DIRECTION('ref_axis',(-0.707106781186485,0.70710678118661,0.)) ;
#64467 = DIRECTION('center_axis',(1.,0.,0.)) ;
#64468 = DIRECTION('ref_axis',(0.,-1.,0.)) ;
#64469 = DIRECTION('center_axis',(0.,-1.,0.)) ;
#64470 = DIRECTION('ref_axis',(0.707106781186548,0.,-0.707106781186548)) ;
#64471 = DIRECTION('center_axis',(0.,1.,0.)) ;
#64472 = DIRECTION('ref_axis',(1.,0.,0.)) ;
#64473 = DIRECTION('',(0.,1.,0.)) ;
#64474 = DIRECTION('',(0.,-1.,0.)) ;
#64475 = DIRECTION('center_axis',(-1.,0.,0.)) ;
#64476 = DIRECTION('ref_axis',(0.,0.,1.)) ;
#64477 = DIRECTION('center_axis',(1.,0.,0.)) ;
#64478 = DIRECTION('ref_axis',(0.,-0.211920125136302,0.977286989866443)) ;
#64479 = DIRECTION('center_axis',(-1.,0.,0.)) ;
#64480 = DIRECTION('ref_axis',(0.,-0.211920125136302,0.977286989866444)) ;
#64481 = DIRECTION('center_axis',(0.,0.,-1.)) ;
#64482 = DIRECTION('ref_axis',(-1.,0.,0.)) ;
#64483 = DIRECTION('center_axis',(0.,0.,-1.)) ;
#64484 = DIRECTION('ref_axis',(0.707106781186485,0.70710678118661,0.)) ;
#64485 = DIRECTION('center_axis',(0.,-1.,0.)) ;
#64486 = DIRECTION('ref_axis',(-1.,0.,0.)) ;
#64487 = DIRECTION('center_axis',(0.,0.,1.)) ;
#64488 = DIRECTION('ref_axis',(0.,1.,0.)) ;
#64489 = DIRECTION('center_axis',(-1.,0.,0.)) ;
#64490 = DIRECTION('ref_axis',(0.,0.,-1.)) ;
#64491 = DIRECTION('center_axis',(3.495649499231E-13,0.983937861384641,0.178511301977827)) ;
#64492 = DIRECTION('ref_axis',(-1.96833879041829E-30,0.178511301977827,-0.983937861384641)) ;
#64493 = DIRECTION('center_axis',(-1.,0.,0.)) ;
#64494 = DIRECTION('ref_axis',(0.,1.,0.)) ;
#64495 = DIRECTION('center_axis',(-1.,0.,0.)) ;
#64496 = DIRECTION('ref_axis',(0.,0.,1.)) ;
#64497 = DIRECTION('center_axis',(0.,-1.,0.)) ;
#64498 = DIRECTION('ref_axis',(-1.,0.,0.)) ;
#64499 = DIRECTION('center_axis',(1.,0.,0.)) ;
#64500 = DIRECTION('ref_axis',(0.,-0.211920125136302,0.977286989866444)) ;
#64501 = DIRECTION('center_axis',(-1.,0.,0.)) ;
#64502 = DIRECTION('ref_axis',(0.,-0.211920125136302,0.977286989866443)) ;
#64503 = DIRECTION('center_axis',(0.,1.,0.)) ;
#64504 = DIRECTION('ref_axis',(-0.707106781186548,0.,-0.707106781186548)) ;
#64505 = DIRECTION('',(0.,-1.,0.)) ;
#64506 = DIRECTION('',(0.,1.,0.)) ;
#64507 = DIRECTION('center_axis',(-1.,0.,0.)) ;
#64508 = DIRECTION('ref_axis',(0.,0.869437932031723,-0.49404218680635)) ;
#64509 = DIRECTION('center_axis',(1.,0.,0.)) ;
#64510 = DIRECTION('ref_axis',(0.,0.511844635310909,-0.85907803446686)) ;
#64511 = DIRECTION('',(1.,0.,0.)) ;
#64512 = DIRECTION('',(-1.,0.,0.)) ;
#64513 = DIRECTION('center_axis',(0.477592250328493,0.621251013257736,0.62125101283813)) ;
#64514 = DIRECTION('ref_axis',(5.81314738453177E-17,0.70710678094775,-0.707106781425345)) ;
#64515 = DIRECTION('center_axis',(0.,0.70710678118657,0.707106781186525)) ;
#64516 = DIRECTION('ref_axis',(0.,0.707106781186525,-0.70710678118657)) ;
#64517 = DIRECTION('center_axis',(0.,0.600000000000011,-0.799999999999992)) ;
#64518 = DIRECTION('ref_axis',(0.,0.799999999999991,0.600000000000011)) ;
#64519 = DIRECTION('center_axis',(-8.05175619837835E-16,0.707106781186546,
0.707106781186549)) ;
#64520 = DIRECTION('ref_axis',(-0.707106781186594,0.499999999999968,-0.499999999999966)) ;
#64521 = DIRECTION('',(-8.05175619837834E-16,0.707106781186546,0.707106781186549)) ;
#64522 = DIRECTION('center_axis',(0.,0.,1.)) ;
#64523 = DIRECTION('ref_axis',(0.707106781186359,-0.707106781186736,0.)) ;
#64524 = DIRECTION('center_axis',(0.,0.,-1.)) ;
#64525 = DIRECTION('ref_axis',(0.707106781186359,-0.707106781186736,0.)) ;
#64526 = DIRECTION('',(0.,0.,-1.)) ;
#64527 = DIRECTION('',(0.,0.,1.)) ;
#64528 = DIRECTION('center_axis',(0.,0.,-1.)) ;
#64529 = DIRECTION('ref_axis',(-1.,0.,0.)) ;
#64530 = DIRECTION('center_axis',(1.,0.,0.)) ;
#64531 = DIRECTION('ref_axis',(0.,0.,-1.)) ;
#64532 = DIRECTION('center_axis',(0.,0.,1.)) ;
#64533 = DIRECTION('ref_axis',(0.707106781186503,-0.707106781186592,0.)) ;
#64534 = DIRECTION('center_axis',(-1.,0.,0.)) ;
#64535 = DIRECTION('ref_axis',(0.,0.707106781186469,-0.707106781186626)) ;
#64536 = DIRECTION('center_axis',(1.,0.,0.)) ;
#64537 = DIRECTION('ref_axis',(0.,0.,-1.)) ;
#64538 = DIRECTION('',(1.,0.,0.)) ;
#64539 = DIRECTION('center_axis',(0.,0.,-1.)) ;
#64540 = DIRECTION('ref_axis',(-1.,0.,0.)) ;
#64541 = DIRECTION('center_axis',(0.,-1.,0.)) ;
#64542 = DIRECTION('ref_axis',(0.,0.,-1.)) ;
#64543 = DIRECTION('center_axis',(0.,0.,1.)) ;
#64544 = DIRECTION('ref_axis',(-0.70710678118657,-0.707106781186525,0.)) ;
#64545 = DIRECTION('center_axis',(5.69345140833415E-16,1.,0.)) ;
#64546 = DIRECTION('ref_axis',(0.707106781186532,-4.02587809918909E-16,-0.707106781186563)) ;
#64547 = DIRECTION('',(-5.69345140833415E-16,-1.,0.)) ;
#64548 = DIRECTION('center_axis',(0.,0.,1.)) ;
#64549 = DIRECTION('ref_axis',(0.707106781186359,0.707106781186736,0.)) ;
#64550 = DIRECTION('center_axis',(0.,0.,-1.)) ;
#64551 = DIRECTION('ref_axis',(0.707106781186359,0.707106781186736,0.)) ;
#64552 = DIRECTION('',(0.,0.,-1.)) ;
#64553 = DIRECTION('',(0.,0.,1.)) ;
#64554 = DIRECTION('center_axis',(-1.,0.,0.)) ;
#64555 = DIRECTION('ref_axis',(0.,-0.707106781186736,-0.707106781186359)) ;
#64556 = DIRECTION('center_axis',(1.,0.,0.)) ;
#64557 = DIRECTION('ref_axis',(0.,-1.,0.)) ;
#64558 = DIRECTION('',(1.,0.,0.)) ;
#64559 = DIRECTION('',(-1.,0.,0.)) ;
#64560 = DIRECTION('center_axis',(0.,0.,1.)) ;
#64561 = DIRECTION('ref_axis',(1.,0.,0.)) ;
#64562 = DIRECTION('center_axis',(0.,-1.,0.)) ;
#64563 = DIRECTION('ref_axis',(-1.,0.,0.)) ;
#64564 = DIRECTION('center_axis',(0.,0.,1.)) ;
#64565 = DIRECTION('ref_axis',(-0.707106781186559,-0.707106781186536,0.)) ;
#64566 = DIRECTION('center_axis',(0.,0.,-1.)) ;
#64567 = DIRECTION('ref_axis',(-0.707106781186559,-0.707106781186536,0.)) ;
#64568 = DIRECTION('center_axis',(-1.13869028166683E-15,1.,0.)) ;
#64569 = DIRECTION('ref_axis',(-0.707106781186548,-8.05175619837835E-16,-0.707106781186548)) ;
#64570 = DIRECTION('center_axis',(0.,-1.,0.)) ;
#64571 = DIRECTION('ref_axis',(-1.,0.,0.)) ;
#64572 = DIRECTION('',(1.13869028166683E-15,-1.,0.)) ;
#64573 = DIRECTION('',(-1.13869028166683E-15,1.,0.)) ;
#64574 = DIRECTION('center_axis',(0.,0.,1.)) ;
#64575 = DIRECTION('ref_axis',(1.,0.,0.)) ;
#64576 = DIRECTION('center_axis',(1.,0.,0.)) ;
#64577 = DIRECTION('ref_axis',(0.,-1.,0.)) ;
#64578 = DIRECTION('center_axis',(0.,0.,-1.)) ;
#64579 = DIRECTION('ref_axis',(0.70710678118657,0.707106781186525,0.)) ;
#64580 = DIRECTION('center_axis',(0.,0.,1.)) ;
#64581 = DIRECTION('ref_axis',(0.70710678118657,0.707106781186525,0.)) ;
#64582 = DIRECTION('center_axis',(-1.,-6.125368411725E-15,0.)) ;
#64583 = DIRECTION('ref_axis',(4.33128954119624E-15,-0.707106781186485,-0.70710678118661)) ;
#64584 = DIRECTION('center_axis',(1.,0.,0.)) ;
#64585 = DIRECTION('ref_axis',(0.,-1.,0.)) ;
#64586 = DIRECTION('',(1.,6.125368411725E-15,0.)) ;
#64587 = DIRECTION('',(-1.,-6.125368411725E-15,0.)) ;
#64588 = DIRECTION('center_axis',(0.,0.,1.)) ;
#64589 = DIRECTION('ref_axis',(1.,0.,0.)) ;
#64590 = DIRECTION('center_axis',(0.,1.,0.)) ;
#64591 = DIRECTION('ref_axis',(1.,0.,0.)) ;
#64592 = DIRECTION('center_axis',(0.,0.,-1.)) ;
#64593 = DIRECTION('ref_axis',(-0.707106781186514,0.707106781186581,0.)) ;
#64594 = DIRECTION('center_axis',(0.,0.,1.)) ;
#64595 = DIRECTION('ref_axis',(-0.707106781186514,0.707106781186581,0.)) ;
#64596 = DIRECTION('center_axis',(-5.69345140833415E-16,-1.,0.)) ;
#64597 = DIRECTION('ref_axis',(0.707106781186548,-4.02587809918918E-16,-0.707106781186548)) ;
#64598 = DIRECTION('center_axis',(0.,1.,0.)) ;
#64599 = DIRECTION('ref_axis',(1.,0.,0.)) ;
#64600 = DIRECTION('',(5.69345140833415E-16,1.,0.)) ;
#64601 = DIRECTION('',(-5.69345140833415E-16,-1.,0.)) ;
#64602 = DIRECTION('center_axis',(0.,0.,1.)) ;
#64603 = DIRECTION('ref_axis',(1.,0.,0.)) ;
#64604 = DIRECTION('center_axis',(1.,0.,0.)) ;
#64605 = DIRECTION('ref_axis',(0.,-1.,0.)) ;
#64606 = DIRECTION('center_axis',(0.,0.,1.)) ;
#64607 = DIRECTION('ref_axis',(0.707106781186553,-0.707106781186542,0.)) ;
#64608 = DIRECTION('center_axis',(0.,0.,-1.)) ;
#64609 = DIRECTION('ref_axis',(0.707106781186553,-0.707106781186542,0.)) ;
#64610 = DIRECTION('center_axis',(-1.,0.,0.)) ;
#64611 = DIRECTION('ref_axis',(0.,-0.707106781186736,-0.707106781186359)) ;
#64612 = DIRECTION('',(1.,0.,0.)) ;
#64613 = DIRECTION('',(-1.,0.,0.)) ;
#64614 = DIRECTION('center_axis',(1.,0.,0.)) ;
#64615 = DIRECTION('ref_axis',(0.,0.869437932031723,-0.49404218680635)) ;
#64616 = DIRECTION('center_axis',(-1.,0.,0.)) ;
#64617 = DIRECTION('ref_axis',(0.,1.,0.)) ;
#64618 = DIRECTION('',(-1.,0.,0.)) ;
#64619 = DIRECTION('',(1.,0.,0.)) ;
#64620 = DIRECTION('center_axis',(-0.477592250328042,0.621251013257686,0.621251012838527)) ;
#64621 = DIRECTION('ref_axis',(0.792804743230373,0.60947570838502,-1.22539280089609E-16)) ;
#64622 = DIRECTION('center_axis',(0.,0.600000000000011,-0.799999999999992)) ;
#64623 = DIRECTION('ref_axis',(0.,0.799999999999991,0.600000000000011)) ;
#64624 = DIRECTION('center_axis',(0.,0.,1.)) ;
#64625 = DIRECTION('ref_axis',(-0.707106781186359,0.707106781186736,0.)) ;
#64626 = DIRECTION('center_axis',(0.,0.,-1.)) ;
#64627 = DIRECTION('ref_axis',(-0.707106781186359,0.707106781186736,0.)) ;
#64628 = DIRECTION('',(0.,0.,-1.)) ;
#64629 = DIRECTION('',(0.,0.,1.)) ;
#64630 = DIRECTION('center_axis',(-1.,0.,0.)) ;
#64631 = DIRECTION('ref_axis',(0.,-0.382683432365103,0.923879532511281)) ;
#64632 = DIRECTION('center_axis',(1.,1.24744160070242E-15,0.)) ;
#64633 = DIRECTION('ref_axis',(4.77375233431813E-16,-0.382683432365097,0.923879532511284)) ;
#64634 = DIRECTION('',(1.,0.,0.)) ;
#64635 = DIRECTION('center_axis',(-1.,0.,0.)) ;
#64636 = DIRECTION('ref_axis',(0.,-0.382683432365103,0.923879532511281)) ;
#64637 = DIRECTION('',(1.,0.,0.)) ;
#64638 = DIRECTION('center_axis',(0.,0.,-1.)) ;
#64639 = DIRECTION('ref_axis',(-0.707106781186548,0.707106781186548,0.)) ;
#64640 = DIRECTION('',(0.,0.,1.)) ;
#64641 = DIRECTION('center_axis',(0.,0.,1.)) ;
#64642 = DIRECTION('ref_axis',(-0.707106781186548,0.707106781186548,0.)) ;
#64643 = DIRECTION('',(0.,0.,-1.)) ;
#64644 = DIRECTION('center_axis',(0.,0.,-1.)) ;
#64645 = DIRECTION('ref_axis',(1.,0.,0.)) ;
#64646 = DIRECTION('',(0.,0.,-1.)) ;
#64647 = DIRECTION('',(0.,0.,-1.)) ;
#64648 = DIRECTION('center_axis',(0.,1.,0.)) ;
#64649 = DIRECTION('ref_axis',(1.,0.,-1.93235546378459E-35)) ;
#64650 = DIRECTION('',(0.,0.,-1.)) ;
#64651 = DIRECTION('center_axis',(0.,0.,-1.)) ;
#64652 = DIRECTION('ref_axis',(0.,-1.,0.)) ;
#64653 = DIRECTION('',(0.,0.,-1.)) ;
#64654 = DIRECTION('center_axis',(0.,0.,1.)) ;
#64655 = DIRECTION('ref_axis',(0.707106781186548,0.707106781186548,0.)) ;
#64656 = DIRECTION('',(0.,0.,1.)) ;
#64657 = DIRECTION('center_axis',(0.,0.,1.)) ;
#64658 = DIRECTION('ref_axis',(0.707106781186548,0.707106781186548,0.)) ;
#64659 = DIRECTION('',(0.,0.,-1.)) ;
#64660 = DIRECTION('center_axis',(-1.,-1.13869028166683E-15,0.)) ;
#64661 = DIRECTION('ref_axis',(-1.13869028166683E-15,1.,0.)) ;
#64662 = DIRECTION('',(0.,0.,-1.)) ;
#64663 = DIRECTION('',(0.,0.,-1.)) ;
#64664 = DIRECTION('',(1.13869028166683E-15,-1.,0.)) ;
#64665 = DIRECTION('center_axis',(0.,-1.,0.)) ;
#64666 = DIRECTION('ref_axis',(1.,0.,0.)) ;
#64667 = DIRECTION('',(1.,0.,0.)) ;
#64668 = DIRECTION('center_axis',(1.,-5.69345140833415E-16,0.)) ;
#64669 = DIRECTION('ref_axis',(-5.69345140833415E-16,-1.,3.47655046371441E-32)) ;
#64670 = DIRECTION('',(5.69345140833415E-16,1.,0.)) ;
#64671 = DIRECTION('',(0.,0.,1.)) ;
#64672 = DIRECTION('',(0.,0.,-1.)) ;
#64673 = DIRECTION('center_axis',(-1.,0.,0.)) ;
#64674 = DIRECTION('ref_axis',(0.,-1.,0.)) ;
#64675 = DIRECTION('',(0.,-1.,0.)) ;
#64676 = DIRECTION('center_axis',(0.,0.,1.)) ;
#64677 = DIRECTION('ref_axis',(1.,0.,0.)) ;
#64678 = DIRECTION('',(-1.,0.,0.)) ;
#64679 = DIRECTION('center_axis',(0.,0.,1.)) ;
#64680 = DIRECTION('ref_axis',(0.707106781186555,-0.70710678118654,0.)) ;
#64681 = DIRECTION('center_axis',(0.,0.,1.)) ;
#64682 = DIRECTION('ref_axis',(-0.70710678118661,0.707106781186485,0.)) ;
#64683 = DIRECTION('center_axis',(0.,0.,-1.)) ;
#64684 = DIRECTION('ref_axis',(-0.70710678118661,0.707106781186485,0.)) ;
#64685 = DIRECTION('',(0.,0.,1.)) ;
#64686 = DIRECTION('center_axis',(0.,0.,1.)) ;
#64687 = DIRECTION('ref_axis',(-0.70710678118661,0.707106781186485,0.)) ;
#64688 = DIRECTION('',(0.,0.,-1.)) ;
#64689 = DIRECTION('center_axis',(-1.,0.,0.)) ;
#64690 = DIRECTION('ref_axis',(0.,-1.,0.)) ;
#64691 = DIRECTION('',(0.,1.,0.)) ;
#64692 = DIRECTION('',(0.,0.,-1.)) ;
#64693 = DIRECTION('',(0.,-1.,0.)) ;
#64694 = DIRECTION('center_axis',(0.,0.,-1.)) ;
#64695 = DIRECTION('ref_axis',(-0.707106781186359,-0.707106781186736,0.)) ;
#64696 = DIRECTION('center_axis',(0.,0.,1.)) ;
#64697 = DIRECTION('ref_axis',(-0.707106781186359,-0.707106781186736,0.)) ;
#64698 = DIRECTION('center_axis',(0.,0.,-1.)) ;
#64699 = DIRECTION('ref_axis',(-0.707106781186359,-0.707106781186736,0.)) ;
#64700 = DIRECTION('',(0.,0.,1.)) ;
#64701 = DIRECTION('center_axis',(-1.,0.,0.)) ;
#64702 = DIRECTION('ref_axis',(0.,0.,1.)) ;
#64703 = DIRECTION('center_axis',(-1.,-1.24744160070242E-15,0.)) ;
#64704 = DIRECTION('ref_axis',(-8.8207441499096E-16,0.70710678118661,0.707106781186485)) ;
#64705 = DIRECTION('center_axis',(0.,0.,-1.)) ;
#64706 = DIRECTION('ref_axis',(0.,-1.,0.)) ;
#64707 = DIRECTION('center_axis',(1.,0.,0.)) ;
#64708 = DIRECTION('ref_axis',(0.,0.,1.)) ;
#64709 = DIRECTION('center_axis',(0.,-1.,0.)) ;
#64710 = DIRECTION('ref_axis',(-1.,0.,0.)) ;
#64711 = DIRECTION('center_axis',(1.,0.,0.)) ;
#64712 = DIRECTION('ref_axis',(0.,0.,-1.)) ;
#64713 = DIRECTION('center_axis',(1.,0.,0.)) ;
#64714 = DIRECTION('ref_axis',(0.,1.,0.)) ;
#64715 = DIRECTION('center_axis',(0.,0.,1.)) ;
#64716 = DIRECTION('ref_axis',(-1.,0.,0.)) ;
#64717 = DIRECTION('center_axis',(-1.,-1.24744160070242E-15,0.)) ;
#64718 = DIRECTION('ref_axis',(-8.82074414991118E-16,0.707106781186736,-0.707106781186359)) ;
#64719 = DIRECTION('center_axis',(0.,-1.,0.)) ;
#64720 = DIRECTION('ref_axis',(0.,0.,1.)) ;
#64721 = DIRECTION('center_axis',(0.,0.,1.)) ;
#64722 = DIRECTION('ref_axis',(-0.70710678118661,-0.707106781186485,0.)) ;
#64723 = DIRECTION('',(0.,0.,-1.)) ;
#64724 = DIRECTION('',(0.,0.,1.)) ;
#64725 = DIRECTION('center_axis',(-1.,8.30329439001789E-15,0.)) ;
#64726 = DIRECTION('ref_axis',(-5.87131576937143E-15,-0.707106781186736,0.707106781186359)) ;
#64727 = DIRECTION('center_axis',(1.,0.,0.)) ;
#64728 = DIRECTION('ref_axis',(0.,0.,1.)) ;
#64729 = DIRECTION('',(1.,-8.30329439001789E-15,0.)) ;
#64730 = DIRECTION('center_axis',(1.,0.,0.)) ;
#64731 = DIRECTION('ref_axis',(0.,-0.707106781186736,0.707106781186359)) ;
#64732 = DIRECTION('',(-1.,8.30329439001789E-15,0.)) ;
#64733 = DIRECTION('center_axis',(0.,0.,-1.)) ;
#64734 = DIRECTION('ref_axis',(-1.,0.,0.)) ;
#64735 = DIRECTION('center_axis',(0.,-1.,0.)) ;
#64736 = DIRECTION('ref_axis',(0.,0.,1.)) ;
#64737 = DIRECTION('center_axis',(0.,0.,1.)) ;
#64738 = DIRECTION('ref_axis',(-0.707106781186548,-0.707106781186548,0.)) ;
#64739 = DIRECTION('center_axis',(0.,0.,-1.)) ;
#64740 = DIRECTION('ref_axis',(-0.707106781186547,-0.707106781186547,0.)) ;
#64741 = DIRECTION('center_axis',(-1.24744160070242E-15,1.,0.)) ;
#64742 = DIRECTION('ref_axis',(-0.707106781186548,-8.82074414990883E-16,0.707106781186548)) ;
#64743 = DIRECTION('',(1.24744160070242E-15,-1.,0.)) ;
#64744 = DIRECTION('',(-1.24744160070242E-15,1.,0.)) ;
#64745 = DIRECTION('center_axis',(1.,0.,0.)) ;
#64746 = DIRECTION('ref_axis',(0.,0.707106781186736,-0.707106781186359)) ;
#64747 = DIRECTION('center_axis',(-1.,0.,0.)) ;
#64748 = DIRECTION('ref_axis',(0.,0.707106781186736,-0.707106781186359)) ;
#64749 = DIRECTION('',(-1.,0.,0.)) ;
#64750 = DIRECTION('',(1.,0.,0.)) ;
#64751 = DIRECTION('center_axis',(1.,0.,0.)) ;
#64752 = DIRECTION('ref_axis',(0.,0.707106781186485,0.70710678118661)) ;
#64753 = DIRECTION('center_axis',(-1.,0.,0.)) ;
#64754 = DIRECTION('ref_axis',(0.,0.707106781186485,0.70710678118661)) ;
#64755 = DIRECTION('',(-1.,0.,0.)) ;
#64756 = DIRECTION('',(1.,0.,0.)) ;
#64757 = DIRECTION('center_axis',(1.24744160070242E-15,-1.,0.)) ;
#64758 = DIRECTION('ref_axis',(-0.707106781186548,-8.82074414990883E-16,-0.707106781186548)) ;
#64759 = DIRECTION('center_axis',(0.,1.,0.)) ;
#64760 = DIRECTION('ref_axis',(0.,0.,-1.)) ;
#64761 = DIRECTION('',(-1.24744160070242E-15,1.,0.)) ;
#64762 = DIRECTION('',(1.24744160070242E-15,-1.,0.)) ;
#64763 = DIRECTION('center_axis',(0.,0.,1.)) ;
#64764 = DIRECTION('ref_axis',(1.,0.,0.)) ;
#64765 = DIRECTION('center_axis',(-1.,4.44089209850151E-14,0.)) ;
#64766 = DIRECTION('ref_axis',(0.,0.,-1.)) ;
#64767 = DIRECTION('center_axis',(0.,0.,-1.)) ;
#64768 = DIRECTION('ref_axis',(-0.707106781186539,-0.707106781186556,0.)) ;
#64769 = DIRECTION('center_axis',(0.,0.,1.)) ;
#64770 = DIRECTION('ref_axis',(-0.707106781186539,-0.707106781186556,0.)) ;
#64771 = DIRECTION('center_axis',(1.,-8.30329439001789E-15,0.)) ;
#64772 = DIRECTION('ref_axis',(-5.87131576937143E-15,-0.707106781186736,-0.707106781186359)) ;
#64773 = DIRECTION('center_axis',(1.,0.,0.)) ;
#64774 = DIRECTION('ref_axis',(0.,-0.707106781186736,-0.707106781186359)) ;
#64775 = DIRECTION('',(-1.,8.30329439001789E-15,0.)) ;
#64776 = DIRECTION('',(1.,-8.30329439001789E-15,0.)) ;
#64777 = DIRECTION('center_axis',(0.,0.,-1.)) ;
#64778 = DIRECTION('ref_axis',(-4.44089209850056E-14,-1.,0.)) ;
#64779 = DIRECTION('',(0.,0.,-1.)) ;
#64780 = DIRECTION('center_axis',(0.,0.,-1.)) ;
#64781 = DIRECTION('ref_axis',(-0.707106781186548,-0.707106781186548,0.)) ;
#64782 = DIRECTION('',(0.,0.,-1.)) ;
#64783 = DIRECTION('center_axis',(-1.,-1.24744160070242E-15,0.)) ;
#64784 = DIRECTION('ref_axis',(-1.24744160070242E-15,1.,-3.26886029821929E-63)) ;
#64785 = DIRECTION('',(0.,0.,-1.)) ;
#64786 = DIRECTION('',(1.24744160070242E-15,-1.,-1.96585022416868E-45)) ;
#64787 = DIRECTION('center_axis',(1.,1.24744160070242E-15,0.)) ;
#64788 = DIRECTION('ref_axis',(-8.82074414990876E-16,0.707106781186542,0.707106781186553)) ;
#64789 = DIRECTION('',(0.,0.,1.)) ;
#64790 = DIRECTION('',(-7.79270590072164E-16,0.624695047554423,0.780868809443031)) ;
#64791 = DIRECTION('center_axis',(1.,1.24744160070242E-15,0.)) ;
#64792 = DIRECTION('ref_axis',(-5.40377643367589E-16,0.433188730489114,-0.901303236306866)) ;
#64793 = DIRECTION('',(-1.24744160070242E-15,1.,0.)) ;
#64794 = DIRECTION('center_axis',(-1.,-1.24744160070242E-15,0.)) ;
#64795 = DIRECTION('ref_axis',(4.77375233431813E-16,-0.382683432365097,0.923879532511284)) ;
#64796 = DIRECTION('',(-8.82074414990881E-16,0.707106781186546,0.707106781186549)) ;
#64797 = DIRECTION('center_axis',(1.,1.24744160070242E-15,0.)) ;
#64798 = DIRECTION('ref_axis',(-4.77375233431814E-16,0.382683432365098,-0.923879532511283)) ;
#64799 = DIRECTION('',(-1.24744160070242E-15,1.,0.)) ;
#64800 = DIRECTION('center_axis',(0.,0.,-1.)) ;
#64801 = DIRECTION('ref_axis',(-4.44089209850056E-14,-1.,0.)) ;
#64802 = DIRECTION('',(0.,0.,-1.)) ;
#64803 = DIRECTION('center_axis',(-1.95689141014107E-45,-1.96585022416868E-45,
1.)) ;
#64804 = DIRECTION('ref_axis',(-0.707106781186548,-0.707106781186548,-2.77379721046322E-45)) ;
#64805 = DIRECTION('center_axis',(-8.30329439001789E-15,-1.,0.)) ;
#64806 = DIRECTION('ref_axis',(-1.,8.30329439001789E-15,4.19778536698447E-50)) ;
#64807 = DIRECTION('',(-1.,8.30329439001789E-15,0.)) ;
#64808 = DIRECTION('',(0.,0.,1.)) ;
#64809 = DIRECTION('',(1.,-9.87859509815899E-15,0.)) ;
#64810 = DIRECTION('',(0.,0.,-1.)) ;
#64811 = DIRECTION('',(1.,-8.30329439001789E-15,1.95689141014106E-45)) ;
#64812 = DIRECTION('',(0.,0.,-1.)) ;
#64813 = DIRECTION('',(-1.,8.30329439001789E-15,0.)) ;
#64814 = DIRECTION('center_axis',(0.,-1.,0.)) ;
#64815 = DIRECTION('ref_axis',(0.707106781186548,0.,-0.707106781186548)) ;
#64816 = DIRECTION('center_axis',(0.,1.,0.)) ;
#64817 = DIRECTION('ref_axis',(1.,0.,0.)) ;
#64818 = DIRECTION('',(0.,1.,0.)) ;
#64819 = DIRECTION('center_axis',(-1.92374441038943E-14,-0.901303236306783,
-0.433188730489285)) ;
#64820 = DIRECTION('ref_axis',(-4.00259042046792E-14,0.433188730489285,-0.901303236306783)) ;
#64821 = DIRECTION('center_axis',(0.,0.624695047554251,0.780868809443169)) ;
#64822 = DIRECTION('ref_axis',(1.,0.,0.)) ;
#64823 = DIRECTION('center_axis',(0.993839018553024,0.0692369708135714,0.0865462135169529)) ;
#64824 = DIRECTION('ref_axis',(-0.110833231485694,0.620846312956424,0.77605789119553)) ;
#64825 = DIRECTION('center_axis',(0.,-0.624695047554423,-0.780868809443031)) ;
#64826 = DIRECTION('ref_axis',(0.707106781186373,0.55215763037437,-0.441726104299494)) ;
#64827 = DIRECTION('',(0.,0.624695047554423,0.780868809443031)) ;
#64828 = DIRECTION('center_axis',(0.,0.,1.)) ;
#64829 = DIRECTION('ref_axis',(1.,0.,0.)) ;
#64830 = DIRECTION('center_axis',(-0.707106781186725,0.70710678118637,0.)) ;
#64831 = DIRECTION('ref_axis',(0.70710678118637,0.707106781186725,0.)) ;
#64832 = DIRECTION('center_axis',(0.,0.,-1.)) ;
#64833 = DIRECTION('ref_axis',(-0.923879532511267,-0.382683432365139,0.)) ;
#64834 = DIRECTION('center_axis',(0.70710678118661,-0.707106781186485,0.)) ;
#64835 = DIRECTION('ref_axis',(0.499999999999892,0.49999999999998,-0.707106781186638)) ;
#64836 = DIRECTION('center_axis',(-0.707106781186548,0.707106781186548,0.)) ;
#64837 = DIRECTION('ref_axis',(0.707106781186547,0.707106781186547,0.)) ;
#64838 = DIRECTION('',(-0.70710678118661,0.707106781186485,0.)) ;
#64839 = DIRECTION('center_axis',(0.,0.,1.)) ;
#64840 = DIRECTION('ref_axis',(1.,0.,0.)) ;
#64841 = DIRECTION('center_axis',(0.,1.,0.)) ;
#64842 = DIRECTION('ref_axis',(1.,0.,0.)) ;
#64843 = DIRECTION('center_axis',(0.,0.,1.)) ;
#64844 = DIRECTION('ref_axis',(0.923879532511283,0.382683432365099,0.)) ;
#64845 = DIRECTION('center_axis',(-1.20119700805775E-14,-1.,0.)) ;
#64846 = DIRECTION('ref_axis',(0.70710678118661,-8.49374549938702E-15,-0.707106781186485)) ;
#64847 = DIRECTION('center_axis',(0.,1.,0.)) ;
#64848 = DIRECTION('ref_axis',(1.,0.,0.)) ;
#64849 = DIRECTION('',(1.20119700805775E-14,1.,0.)) ;
#64850 = DIRECTION('center_axis',(1.,-1.20119700805775E-14,0.)) ;
#64851 = DIRECTION('ref_axis',(0.,0.,-1.)) ;
#64852 = DIRECTION('center_axis',(0.,0.707106781186548,0.707106781186548)) ;
#64853 = DIRECTION('ref_axis',(1.,0.,0.)) ;
#64854 = DIRECTION('center_axis',(-1.,1.20119700805775E-14,0.)) ;
#64855 = DIRECTION('ref_axis',(-4.59678193990225E-15,-0.382683432365097,0.923879532511284)) ;
#64856 = DIRECTION('center_axis',(-8.49374549938626E-15,-0.707106781186546,
-0.707106781186549)) ;
#64857 = DIRECTION('ref_axis',(0.707106781186531,0.500000000000009,-0.500000000000015)) ;
#64858 = DIRECTION('center_axis',(0.,0.707106781186503,0.707106781186592)) ;
#64859 = DIRECTION('ref_axis',(1.,0.,0.)) ;
#64860 = DIRECTION('',(8.49374549938626E-15,0.707106781186546,0.707106781186549)) ;
#64861 = DIRECTION('center_axis',(-1.,1.20119700805775E-14,0.)) ;
#64862 = DIRECTION('ref_axis',(0.,0.,1.)) ;
#64863 = DIRECTION('center_axis',(0.,1.,0.)) ;
#64864 = DIRECTION('ref_axis',(1.,0.,0.)) ;
#64865 = DIRECTION('center_axis',(1.,-1.20119700805775E-14,0.)) ;
#64866 = DIRECTION('ref_axis',(4.59678193990225E-15,0.382683432365097,-0.923879532511284)) ;
#64867 = DIRECTION('center_axis',(-1.20119700805775E-14,-1.,0.)) ;
#64868 = DIRECTION('ref_axis',(0.707106781186469,-8.49374549938533E-15,-0.707106781186626)) ;
#64869 = DIRECTION('center_axis',(0.,1.,0.)) ;
#64870 = DIRECTION('ref_axis',(1.,0.,0.)) ;
#64871 = DIRECTION('',(1.20119700805775E-14,1.,0.)) ;
#64872 = DIRECTION('center_axis',(1.,-1.20119700805775E-14,0.)) ;
#64873 = DIRECTION('ref_axis',(0.,0.,-1.)) ;
#64874 = DIRECTION('center_axis',(0.,0.948683298050458,0.316227766017004)) ;
#64875 = DIRECTION('ref_axis',(1.,0.,0.)) ;
#64876 = DIRECTION('center_axis',(-1.,1.20119700805775E-14,0.)) ;
#64877 = DIRECTION('ref_axis',(-1.92410431043973E-15,-0.160182243006988,0.987087457637493)) ;
#64878 = DIRECTION('center_axis',(-1.13955553921264E-14,-0.948683298050513,
-0.316227766016839)) ;
#64879 = DIRECTION('ref_axis',(0.707106781186476,0.223606797749995,-0.670820393250007)) ;
#64880 = DIRECTION('center_axis',(0.,0.948683298050465,0.316227766016985)) ;
#64881 = DIRECTION('ref_axis',(1.,0.,0.)) ;
#64882 = DIRECTION('',(1.13955553921264E-14,0.948683298050513,0.316227766016839)) ;
#64883 = DIRECTION('center_axis',(0.622803969958969,0.742228868680653,0.247409622893667)) ;
#64884 = DIRECTION('ref_axis',(0.76604444311902,-0.64278760968649,4.44819739379099E-14)) ;
#64885 = DIRECTION('center_axis',(-1.37008135359091E-15,-0.316227766016839,
0.948683298050513)) ;
#64886 = DIRECTION('ref_axis',(6.7408002596686E-14,-0.948683298050513,-0.316227766016839)) ;
#64887 = DIRECTION('center_axis',(-0.622803969959022,-0.742228868680647,-0.247409622893551)) ;
#64888 = DIRECTION('ref_axis',(0.606851800616499,-0.258697038951143,-0.751536249376186)) ;
#64889 = DIRECTION('center_axis',(0.622803969958982,0.742228868680643,0.247409622893663)) ;
#64890 = DIRECTION('ref_axis',(0.76604444311902,-0.642787609686489,-2.20979765740922E-14)) ;
#64891 = DIRECTION('',(0.622803969959022,0.742228868680647,0.247409622893551)) ;
#64892 = DIRECTION('center_axis',(0.996641009831356,0.0776918771178938,0.025897292372644)) ;
#64893 = DIRECTION('ref_axis',(0.0777179430258286,-0.996975386522573,-4.44097402191553E-14)) ;
#64894 = DIRECTION('center_axis',(-1.37008135359091E-15,-0.316227766016839,
0.948683298050513)) ;
#64895 = DIRECTION('ref_axis',(-3.86740249272492E-15,-0.948683298050513,-0.316227766016839)) ;
#64896 = DIRECTION('center_axis',(0.781110574983513,0.592350945541578,0.197450315180618)) ;
#64897 = DIRECTION('ref_axis',(0.604246815762238,-0.796797204840226,-2.22012953032117E-14)) ;
#64898 = DIRECTION('center_axis',(1.37008135359091E-15,0.316227766016839,
-0.948683298050513)) ;
#64899 = DIRECTION('ref_axis',(6.51683787482125E-33,0.948683298050513,0.316227766016839)) ;
#64900 = DIRECTION('center_axis',(0.609935343346627,0.792451182683597,-8.98660408355326E-10)) ;
#64901 = DIRECTION('ref_axis',(0.792451182683597,-0.609935343346627,1.791498019765E-26)) ;
#64902 = DIRECTION('center_axis',(0.,0.,-1.)) ;
#64903 = DIRECTION('ref_axis',(-1.,0.,0.)) ;
#64904 = DIRECTION('center_axis',(0.,1.,0.)) ;
#64905 = DIRECTION('ref_axis',(1.,0.,0.)) ;
#64906 = DIRECTION('center_axis',(0.,-1.,0.)) ;
#64907 = DIRECTION('ref_axis',(0.707106781186469,0.,-0.707106781186626)) ;
#64908 = DIRECTION('center_axis',(0.,1.,0.)) ;
#64909 = DIRECTION('ref_axis',(1.,0.,0.)) ;
#64910 = DIRECTION('center_axis',(0.,0.,-1.)) ;
#64911 = DIRECTION('ref_axis',(-1.,0.,0.)) ;
#64912 = DIRECTION('center_axis',(0.707106781186459,0.707106781186636,0.)) ;
#64913 = DIRECTION('ref_axis',(0.707106781186636,-0.707106781186459,0.)) ;
#64914 = DIRECTION('center_axis',(0.,0.,-1.)) ;
#64915 = DIRECTION('ref_axis',(0.923879532511297,-0.382683432365064,0.)) ;
#64916 = DIRECTION('center_axis',(-0.70710678118654,-0.707106781186555,0.)) ;
#64917 = DIRECTION('ref_axis',(0.499999999999993,-0.499999999999982,-0.707106781186565)) ;
#64918 = DIRECTION('center_axis',(0.707106781186459,0.707106781186636,0.)) ;
#64919 = DIRECTION('ref_axis',(0.707106781186636,-0.707106781186459,0.)) ;
#64920 = DIRECTION('',(-0.70710678118654,-0.707106781186555,0.)) ;
#64921 = DIRECTION('center_axis',(0.,0.,1.)) ;
#64922 = DIRECTION('ref_axis',(1.,0.,0.)) ;
#64923 = DIRECTION('center_axis',(0.625000000000018,0.780624749799786,0.)) ;
#64924 = DIRECTION('ref_axis',(0.780624749799786,-0.625000000000018,0.)) ;
#64925 = DIRECTION('center_axis',(0.,0.,1.)) ;
#64926 = DIRECTION('ref_axis',(-0.744997757011426,0.66706696968741,0.)) ;
#64927 = DIRECTION('center_axis',(0.,0.,1.)) ;
#64928 = DIRECTION('ref_axis',(1.,0.,0.)) ;
#64929 = DIRECTION('center_axis',(1.,0.,0.)) ;
#64930 = DIRECTION('ref_axis',(0.,-1.,0.)) ;
#64931 = DIRECTION('center_axis',(0.,0.,-1.)) ;
#64932 = DIRECTION('ref_axis',(0.433012701892204,-0.901387818866005,0.)) ;
#64933 = DIRECTION('center_axis',(-1.,3.55271367880048E-14,0.)) ;
#64934 = DIRECTION('ref_axis',(-2.51214793389375E-14,-0.707106781186469,-0.707106781186626)) ;
#64935 = DIRECTION('center_axis',(1.,0.,0.)) ;
#64936 = DIRECTION('ref_axis',(0.,-1.,0.)) ;
#64937 = DIRECTION('',(-1.,3.55271367880048E-14,0.)) ;
#64938 = DIRECTION('center_axis',(0.,0.,1.)) ;
#64939 = DIRECTION('ref_axis',(1.,0.,0.)) ;
#64940 = DIRECTION('center_axis',(0.,1.,0.)) ;
#64941 = DIRECTION('ref_axis',(1.,0.,0.)) ;
#64942 = DIRECTION('center_axis',(-3.67742382159233E-14,-1.,0.)) ;
#64943 = DIRECTION('ref_axis',(0.707106781186532,-2.60033132154483E-14,-0.707106781186563)) ;
#64944 = DIRECTION('center_axis',(0.,1.,0.)) ;
#64945 = DIRECTION('ref_axis',(1.,0.,0.)) ;
#64946 = DIRECTION('center_axis',(0.,0.,-1.)) ;
#64947 = DIRECTION('ref_axis',(-1.,0.,0.)) ;
#64948 = DIRECTION('center_axis',(0.,0.,-1.)) ;
#64949 = DIRECTION('ref_axis',(0.683460430828417,-0.729987561189802,0.)) ;
#64950 = DIRECTION('center_axis',(-0.0657636789837963,-0.997835226140326,
0.)) ;
#64951 = DIRECTION('ref_axis',(-0.997835226140326,0.0657636789837963,0.)) ;
#64952 = DIRECTION('',(0.,0.,-1.)) ;
#64953 = DIRECTION('',(0.997835226140326,-0.0657636789837963,-6.85877185444556E-33)) ;
#64954 = DIRECTION('center_axis',(0.,0.,-1.)) ;
#64955 = DIRECTION('ref_axis',(1.,-2.36847578586694E-14,0.)) ;
#64956 = DIRECTION('center_axis',(1.09763027743844E-32,6.22497063709847E-32,
1.)) ;
#64957 = DIRECTION('ref_axis',(0.683460430828417,-0.729987561189802,3.79396427154525E-32)) ;
#64958 = DIRECTION('center_axis',(-3.55271367880048E-14,-1.,0.)) ;
#64959 = DIRECTION('ref_axis',(-1.,3.55271367880048E-14,0.)) ;
#64960 = DIRECTION('',(0.,0.,-1.)) ;
#64961 = DIRECTION('center_axis',(0.,0.,-1.)) ;
#64962 = DIRECTION('ref_axis',(0.433012701892208,-0.901387818866003,0.)) ;
#64963 = DIRECTION('',(0.,0.,1.)) ;
#64964 = DIRECTION('center_axis',(0.,0.,-1.)) ;
#64965 = DIRECTION('ref_axis',(-1.,5.92118946466623E-14,0.)) ;
#64966 = DIRECTION('',(0.,0.,-1.)) ;
#64967 = DIRECTION('center_axis',(0.707106781186555,-0.70710678118654,0.)) ;
#64968 = DIRECTION('ref_axis',(-0.70710678118654,-0.707106781186555,-1.79753461476134E-31)) ;
#64969 = DIRECTION('',(0.,0.,-1.)) ;
#64970 = DIRECTION('center_axis',(0.,0.,-1.)) ;
#64971 = DIRECTION('ref_axis',(1.,-5.92118946466623E-14,0.)) ;
#64972 = DIRECTION('center_axis',(-1.,8.30329439001789E-15,0.)) ;
#64973 = DIRECTION('ref_axis',(-5.87131576936922E-15,-0.707106781186469,-0.707106781186626)) ;
#64974 = DIRECTION('center_axis',(1.,0.,0.)) ;
#64975 = DIRECTION('ref_axis',(0.,-1.,0.)) ;
#64976 = DIRECTION('',(1.,-8.30329439001789E-15,0.)) ;
#64977 = DIRECTION('center_axis',(1.,-8.30329439001789E-15,0.)) ;
#64978 = DIRECTION('ref_axis',(-5.87131576936922E-15,-0.707106781186469,-0.707106781186626)) ;
#64979 = DIRECTION('center_axis',(-0.707106781186626,0.707106781186469,0.)) ;
#64980 = DIRECTION('ref_axis',(-0.707106781186469,-0.707106781186626,0.)) ;
#64981 = DIRECTION('center_axis',(1.11022302462516E-14,-1.,0.)) ;
#64982 = DIRECTION('ref_axis',(0.707106781186548,7.8504622934189E-15,-0.707106781186548)) ;
#64983 = DIRECTION('',(1.11022302462516E-14,-1.,0.)) ;
#64984 = DIRECTION('center_axis',(0.,1.,0.)) ;
#64985 = DIRECTION('ref_axis',(1.,0.,0.)) ;
#64986 = DIRECTION('center_axis',(0.,0.,-1.)) ;
#64987 = DIRECTION('ref_axis',(-1.,0.,0.)) ;
#64988 = DIRECTION('center_axis',(0.,-1.,0.)) ;
#64989 = DIRECTION('ref_axis',(-1.,0.,0.)) ;
#64990 = DIRECTION('center_axis',(0.,0.,-1.)) ;
#64991 = DIRECTION('ref_axis',(0.,-1.,0.)) ;
#64992 = DIRECTION('center_axis',(-2.22044604925032E-15,1.,0.)) ;
#64993 = DIRECTION('ref_axis',(-0.707106781186548,-1.57009245868378E-15,-0.707106781186548)) ;
#64994 = DIRECTION('',(-2.22044604925032E-15,1.,0.)) ;
#64995 = DIRECTION('center_axis',(0.,0.,-1.)) ;
#64996 = DIRECTION('ref_axis',(-1.,0.,0.)) ;
#64997 = DIRECTION('center_axis',(0.,-1.,0.)) ;
#64998 = DIRECTION('ref_axis',(-1.,0.,0.)) ;
#64999 = DIRECTION('center_axis',(0.,0.,1.)) ;
#65000 = DIRECTION('ref_axis',(-0.707106781186547,-0.707106781186547,0.)) ;
#65001 = DIRECTION('center_axis',(-1.24744160070242E-15,1.,0.)) ;
#65002 = DIRECTION('ref_axis',(-0.707106781186532,-8.82074414990863E-16,-0.707106781186563)) ;
#65003 = DIRECTION('center_axis',(0.,-1.,0.)) ;
#65004 = DIRECTION('ref_axis',(-1.,0.,0.)) ;
#65005 = DIRECTION('',(1.24744160070242E-15,-1.,0.)) ;
#65006 = DIRECTION('center_axis',(1.,1.24744160070242E-15,0.)) ;
#65007 = DIRECTION('ref_axis',(0.,0.,-1.)) ;
#65008 = DIRECTION('center_axis',(0.,-0.707106781186581,-0.707106781186514)) ;
#65009 = DIRECTION('ref_axis',(-1.,0.,0.)) ;
#65010 = DIRECTION('center_axis',(-1.,-1.24744160070242E-15,0.)) ;
#65011 = DIRECTION('ref_axis',(-4.77375233431814E-16,0.382683432365098,-0.923879532511283)) ;
#65012 = DIRECTION('center_axis',(-8.82074414990881E-16,0.707106781186546,
0.707106781186549)) ;
#65013 = DIRECTION('ref_axis',(-0.707106781186616,0.499999999999952,-0.499999999999951)) ;
#65014 = DIRECTION('center_axis',(0.,-0.707106781186414,-0.707106781186681)) ;
#65015 = DIRECTION('ref_axis',(-1.,0.,0.)) ;
#65016 = DIRECTION('center_axis',(-1.,-1.24744160070242E-15,0.)) ;
#65017 = DIRECTION('ref_axis',(0.,0.,1.)) ;
#65018 = DIRECTION('center_axis',(0.,-1.,0.)) ;
#65019 = DIRECTION('ref_axis',(-1.,0.,0.)) ;
#65020 = DIRECTION('center_axis',(-1.24744160070242E-15,1.,0.)) ;
#65021 = DIRECTION('ref_axis',(-0.707106781186548,-8.82074414990883E-16,-0.707106781186548)) ;
#65022 = DIRECTION('center_axis',(0.,-1.,0.)) ;
#65023 = DIRECTION('ref_axis',(-1.,0.,0.)) ;
#65024 = DIRECTION('',(1.24744160070242E-15,-1.,0.)) ;
#65025 = DIRECTION('center_axis',(1.,1.24744160070242E-15,0.)) ;
#65026 = DIRECTION('ref_axis',(0.,0.,-1.)) ;
#65027 = DIRECTION('center_axis',(0.,-0.624695047554359,-0.780868809443082)) ;
#65028 = DIRECTION('ref_axis',(-1.,0.,0.)) ;
#65029 = DIRECTION('center_axis',(-1.,-1.24744160070242E-15,0.)) ;
#65030 = DIRECTION('ref_axis',(-5.4037764336759E-16,0.433188730489114,-0.901303236306866)) ;
#65031 = DIRECTION('center_axis',(-7.79270590072164E-16,0.624695047554423,
0.780868809443031)) ;
#65032 = DIRECTION('ref_axis',(-0.707106781186341,0.552157630374394,-0.441726104299515)) ;
#65033 = DIRECTION('',(7.79270590072164E-16,-0.624695047554423,-0.780868809443031)) ;
#65034 = DIRECTION('center_axis',(0.,-0.331006941435217,-0.943628319160517)) ;
#65035 = DIRECTION('ref_axis',(2.3542424418412E-15,-0.943628319160517,0.331006941435217)) ;
#65036 = DIRECTION('center_axis',(1.34572487833352E-15,-1.,-1.96585022416868E-45)) ;
#65037 = DIRECTION('ref_axis',(0.707106781186516,9.51571187081031E-16,0.707106781186579)) ;
#65038 = DIRECTION('center_axis',(0.,-1.,0.)) ;
#65039 = DIRECTION('ref_axis',(0.707106781186516,0.,0.707106781186579)) ;
#65040 = DIRECTION('',(1.34572487833352E-15,-1.,-1.96585022416868E-45)) ;
#65041 = DIRECTION('center_axis',(0.,1.,0.)) ;
#65042 = DIRECTION('ref_axis',(0.,0.,1.)) ;
#65043 = DIRECTION('',(-1.34572487833352E-15,1.,1.96585022416868E-45)) ;
#65044 = DIRECTION('center_axis',(1.95689141014107E-45,1.96585022416868E-45,
-1.)) ;
#65045 = DIRECTION('ref_axis',(-1.,0.,0.)) ;
#65046 = DIRECTION('center_axis',(1.,8.88178419700302E-14,0.)) ;
#65047 = DIRECTION('ref_axis',(0.,0.,1.)) ;
#65048 = DIRECTION('center_axis',(-1.95689141014107E-45,-1.96585022416868E-45,
1.)) ;
#65049 = DIRECTION('ref_axis',(0.707106781186525,-0.70710678118657,-6.3348381504005E-48)) ;
#65050 = DIRECTION('center_axis',(1.95689141014107E-45,1.96585022416868E-45,
-1.)) ;
#65051 = DIRECTION('ref_axis',(0.707106781186525,-0.70710678118657,-6.3348381504005E-48)) ;
#65052 = DIRECTION('center_axis',(-1.,8.30329439001789E-15,-1.95689141014106E-45)) ;
#65053 = DIRECTION('ref_axis',(-5.87131576937143E-15,-0.707106781186736,0.707106781186359)) ;
#65054 = DIRECTION('center_axis',(1.,0.,0.)) ;
#65055 = DIRECTION('ref_axis',(0.,0.,1.)) ;
#65056 = DIRECTION('',(-1.,8.30329439001789E-15,-1.95689141014106E-45)) ;
#65057 = DIRECTION('center_axis',(1.95689141014107E-45,1.96585022416868E-45,
-1.)) ;
#65058 = DIRECTION('ref_axis',(-1.,0.,0.)) ;
#65059 = DIRECTION('center_axis',(0.,-1.,0.)) ;
#65060 = DIRECTION('ref_axis',(0.,0.,1.)) ;
#65061 = DIRECTION('center_axis',(1.95689141014107E-45,1.96585022416868E-45,
-1.)) ;
#65062 = DIRECTION('ref_axis',(-0.707106781186547,-0.707106781186547,-2.77379721046322E-45)) ;
#65063 = DIRECTION('center_axis',(-1.24744160070242E-15,1.,1.96585022416868E-45)) ;
#65064 = DIRECTION('ref_axis',(-0.707106781186548,-8.82074414990883E-16,0.707106781186548)) ;
#65065 = DIRECTION('center_axis',(0.,-1.,0.)) ;
#65066 = DIRECTION('ref_axis',(0.,0.,1.)) ;
#65067 = DIRECTION('',(-1.24744160070242E-15,1.,1.96585022416868E-45)) ;
#65068 = DIRECTION('center_axis',(1.,1.24744160070242E-15,0.)) ;
#65069 = DIRECTION('ref_axis',(0.,0.,-1.)) ;
#65070 = DIRECTION('center_axis',(0.,0.,1.)) ;
#65071 = DIRECTION('ref_axis',(0.,1.,0.)) ;
#65072 = DIRECTION('center_axis',(-1.,-1.24744160070242E-15,0.)) ;
#65073 = DIRECTION('ref_axis',(-8.82074414990876E-16,0.707106781186542,0.707106781186553)) ;
#65074 = DIRECTION('center_axis',(0.,0.,-1.)) ;
#65075 = DIRECTION('ref_axis',(-0.707106781186359,0.707106781186736,0.)) ;
#65076 = DIRECTION('',(0.,0.,-1.)) ;
#65077 = DIRECTION('center_axis',(1.,8.88178419700125E-16,0.)) ;
#65078 = DIRECTION('ref_axis',(-8.88178419700125E-16,1.,0.)) ;
#65079 = DIRECTION('center_axis',(0.,0.,-1.)) ;
#65080 = DIRECTION('ref_axis',(1.,0.,0.)) ;
#65081 = DIRECTION('',(-1.,0.,0.)) ;
#65082 = DIRECTION('center_axis',(-1.,0.,0.)) ;
#65083 = DIRECTION('ref_axis',(0.,0.382683432365084,-0.923879532511289)) ;
#65084 = DIRECTION('center_axis',(0.,0.,-1.)) ;
#65085 = DIRECTION('ref_axis',(1.,0.,0.)) ;
#65086 = DIRECTION('',(-1.,0.,0.)) ;
#65087 = DIRECTION('center_axis',(0.,0.,1.)) ;
#65088 = DIRECTION('ref_axis',(0.985598559653495,0.169101978725727,0.)) ;
#65089 = DIRECTION('',(0.,1.,0.)) ;
#65090 = DIRECTION('center_axis',(0.,0.,-1.)) ;
#65091 = DIRECTION('ref_axis',(-0.999082519440321,-0.0428266196282222,0.)) ;
#65092 = DIRECTION('',(0.,1.,0.)) ;
#65093 = DIRECTION('center_axis',(0.,0.,-1.)) ;
#65094 = DIRECTION('ref_axis',(-0.945182639171645,-0.326542154412755,0.)) ;
#65095 = DIRECTION('',(0.0419797672693987,0.999118461014512,0.)) ;
#65096 = DIRECTION('',(-0.906307787036666,0.422618261740665,0.)) ;
#65097 = DIRECTION('',(-0.0501684275789832,-0.998740771609056,0.)) ;
#65098 = DIRECTION('',(0.732832174562208,0.680409438446018,0.)) ;
#65099 = DIRECTION('',(-0.906307787036666,0.422618261740665,0.)) ;
#65100 = DIRECTION('',(0.0501684275790028,0.998740771609055,0.)) ;
#65101 = DIRECTION('',(-0.732832174562234,-0.68040943844599,0.)) ;
#65102 = DIRECTION('',(0.906307787036654,-0.42261826174069,0.)) ;
#65103 = DIRECTION('',(0.1631941084961,-0.986593980800695,0.)) ;
#65104 = DIRECTION('',(0.906307787036654,-0.42261826174069,0.)) ;
#65105 = DIRECTION('center_axis',(-1.,0.,0.)) ;
#65106 = DIRECTION('ref_axis',(0.,0.433188730489175,-0.901303236306837)) ;
#65107 = DIRECTION('',(1.,0.,0.)) ;
#65108 = DIRECTION('center_axis',(1.,0.,0.)) ;
#65109 = DIRECTION('ref_axis',(0.,0.780868809443035,-0.624695047554418)) ;
#65110 = DIRECTION('center_axis',(0.,0.780868809443031,-0.624695047554423)) ;
#65111 = DIRECTION('ref_axis',(-1.,0.,0.)) ;
#65112 = DIRECTION('',(1.,0.,0.)) ;
#65113 = DIRECTION('',(-0.42426406871193,0.565685424949236,0.707106781186548)) ;
#65114 = DIRECTION('center_axis',(0.,-0.780868809443031,0.624695047554423)) ;
#65115 = DIRECTION('ref_axis',(0.,0.624695047554423,0.780868809443031)) ;
#65116 = DIRECTION('center_axis',(0.,1.,0.)) ;
#65117 = DIRECTION('ref_axis',(1.,0.,0.)) ;
#65118 = DIRECTION('',(-1.,0.,-1.95689141014107E-45)) ;
#65119 = DIRECTION('',(0.,0.,-1.)) ;
#65120 = DIRECTION('',(0.,0.,1.)) ;
#65121 = DIRECTION('center_axis',(0.,-1.,0.)) ;
#65122 = DIRECTION('ref_axis',(0.514495755427527,0.,-0.857492925712544)) ;
#65123 = DIRECTION('center_axis',(0.,-1.,0.)) ;
#65124 = DIRECTION('ref_axis',(-1.,0.,0.)) ;
#65125 = DIRECTION('center_axis',(-1.,0.,-1.95689141014107E-45)) ;
#65126 = DIRECTION('ref_axis',(-1.38373118615647E-45,0.70710678118654,0.707106781186555)) ;
#65127 = DIRECTION('',(1.,0.,1.95689141014107E-45)) ;
#65128 = DIRECTION('center_axis',(-1.,0.,0.)) ;
#65129 = DIRECTION('ref_axis',(0.,0.70710678118654,0.707106781186555)) ;
#65130 = DIRECTION('center_axis',(1.95689141014107E-45,1.96585022416868E-45,
-1.)) ;
#65131 = DIRECTION('ref_axis',(1.,1.86628956086257E-106,1.95689141014107E-45)) ;
#65132 = DIRECTION('',(-1.,0.,0.)) ;
#65133 = DIRECTION('',(1.30614473485314E-15,-1.,0.)) ;
#65134 = DIRECTION('',(1.,0.,0.)) ;
#65135 = DIRECTION('',(0.,-1.,0.)) ;
#65136 = DIRECTION('center_axis',(0.,1.,0.)) ;
#65137 = DIRECTION('ref_axis',(1.,0.,0.)) ;
#65138 = DIRECTION('',(0.,0.,-1.)) ;
#65139 = DIRECTION('',(0.,0.,-1.)) ;
#65140 = DIRECTION('center_axis',(1.37008135359091E-15,0.316227766016839,
-0.948683298050513)) ;
#65141 = DIRECTION('ref_axis',(-4.03197281156824E-15,-0.948683298050513,-0.316227766016839)) ;
#65142 = DIRECTION('center_axis',(-1.,0.,0.)) ;
#65143 = DIRECTION('ref_axis',(0.,1.,0.)) ;
#65144 = DIRECTION('center_axis',(0.,-0.554700196225204,0.832050294337861)) ;
#65145 = DIRECTION('ref_axis',(0.,-0.832050294337861,-0.554700196225204)) ;
#65146 = DIRECTION('center_axis',(0.,0.94868329805046,0.316227766016998)) ;
#65147 = DIRECTION('ref_axis',(0.,0.316227766016998,-0.94868329805046)) ;
#65148 = DIRECTION('center_axis',(1.37008135359091E-15,0.316227766016839,
-0.948683298050513)) ;
#65149 = DIRECTION('ref_axis',(-4.0319728115686E-15,-0.948683298050513,-0.316227766016839)) ;
#65150 = DIRECTION('center_axis',(0.,0.948683298050465,0.316227766016985)) ;
#65151 = DIRECTION('ref_axis',(1.,0.,0.)) ;
#65152 = DIRECTION('center_axis',(0.,-0.554700196225165,0.832050294337886)) ;
#65153 = DIRECTION('ref_axis',(0.,-0.832050294337886,-0.554700196225165)) ;
#65154 = DIRECTION('center_axis',(1.,0.,0.)) ;
#65155 = DIRECTION('ref_axis',(0.,0.316227766016984,-0.948683298050465)) ;
#65156 = DIRECTION('center_axis',(0.,0.,1.)) ;
#65157 = DIRECTION('ref_axis',(0.496136371636827,0.868244608816573,0.)) ;
#65158 = DIRECTION('',(0.,0.,-1.)) ;
#65159 = DIRECTION('center_axis',(0.,0.,1.)) ;
#65160 = DIRECTION('ref_axis',(0.861535459822987,0.507697401478079,0.)) ;
#65161 = DIRECTION('',(0.,0.,1.)) ;
#65162 = DIRECTION('center_axis',(0.,0.643223921263855,0.765678122394751)) ;
#65163 = DIRECTION('ref_axis',(1.,0.,0.)) ;
#65164 = DIRECTION('center_axis',(-1.,0.,0.)) ;
#65165 = DIRECTION('ref_axis',(0.,0.,1.)) ;
#65166 = DIRECTION('center_axis',(0.,0.948683298050574,0.316227766016658)) ;
#65167 = DIRECTION('ref_axis',(1.,0.,0.)) ;
#65168 = DIRECTION('center_axis',(1.,0.,0.)) ;
#65169 = DIRECTION('ref_axis',(0.,0.500068151122686,-0.865986053139852)) ;
#65170 = DIRECTION('center_axis',(-1.,0.,0.)) ;
#65171 = DIRECTION('ref_axis',(0.,0.500068151122686,-0.865986053139852)) ;
#65172 = DIRECTION('center_axis',(0.,-0.948683298050513,-0.316227766016839)) ;
#65173 = DIRECTION('ref_axis',(0.707106781186539,0.223606797749982,-0.670820393249945)) ;
#65174 = DIRECTION('',(0.,0.948683298050513,0.316227766016839)) ;
#65175 = DIRECTION('',(0.,-0.948683298050513,-0.316227766016839)) ;
#65176 = DIRECTION('center_axis',(0.,0.,-1.)) ;
#65177 = DIRECTION('ref_axis',(-0.707106781186359,-0.707106781186736,0.)) ;
#65178 = DIRECTION('center_axis',(0.,0.,-1.)) ;
#65179 = DIRECTION('ref_axis',(-0.707106781186359,-0.707106781186736,0.)) ;
#65180 = DIRECTION('',(0.,0.,-1.)) ;
#65181 = DIRECTION('',(0.,0.,1.)) ;
#65182 = DIRECTION('center_axis',(1.,0.,1.44419255235793E-15)) ;
#65183 = DIRECTION('ref_axis',(8.44434238398369E-16,0.811242185175624,-0.584710284663678)) ;
#65184 = DIRECTION('',(-1.,0.,-1.44419255235793E-15)) ;
#65185 = DIRECTION('',(1.,0.,1.44419255235793E-15)) ;
#65186 = DIRECTION('center_axis',(0.,0.,-1.)) ;
#65187 = DIRECTION('ref_axis',(0.707106781186359,-0.707106781186736,0.)) ;
#65188 = DIRECTION('center_axis',(0.,0.,-1.)) ;
#65189 = DIRECTION('ref_axis',(0.707106781186359,-0.707106781186736,0.)) ;
#65190 = DIRECTION('',(0.,0.,-1.)) ;
#65191 = DIRECTION('',(0.,0.,1.)) ;
#65192 = DIRECTION('center_axis',(0.,0.948683298050513,0.316227766016839)) ;
#65193 = DIRECTION('ref_axis',(-0.707106781186474,0.223606797750003,-0.670820393250006)) ;
#65194 = DIRECTION('center_axis',(0.,-0.94868329805046,-0.316227766016998)) ;
#65195 = DIRECTION('ref_axis',(-1.,0.,0.)) ;
#65196 = DIRECTION('',(0.,-0.948683298050513,-0.316227766016839)) ;
#65197 = DIRECTION('',(0.,0.948683298050513,0.316227766016839)) ;
#65198 = DIRECTION('center_axis',(-0.829818692458,-0.529396679138204,-0.176465559712756)) ;
#65199 = DIRECTION('ref_axis',(-0.537837055500907,0.843048813373291,-5.64517599036335E-17)) ;
#65200 = DIRECTION('center_axis',(-1.37008135359091E-15,-0.316227766016839,
0.948683298050513)) ;
#65201 = DIRECTION('ref_axis',(4.05940119804181E-15,0.948683298050513,0.316227766016839)) ;
#65202 = DIRECTION('center_axis',(0.,0.,-1.)) ;
#65203 = DIRECTION('ref_axis',(0.891721613427202,0.452584317168402,0.)) ;
#65204 = DIRECTION('',(0.,0.,-1.)) ;
#65205 = DIRECTION('center_axis',(0.,0.,1.)) ;
#65206 = DIRECTION('ref_axis',(0.891721613427202,0.452584317168402,0.)) ;
#65207 = DIRECTION('',(0.,0.,-1.)) ;
#65208 = DIRECTION('center_axis',(-4.33257765707378E-15,-1.,0.)) ;
#65209 = DIRECTION('ref_axis',(-1.,4.33257765707378E-15,0.)) ;
#65210 = DIRECTION('',(1.,-4.33257765707378E-15,0.)) ;
#65211 = DIRECTION('center_axis',(1.,-4.33257765707378E-15,0.)) ;
#65212 = DIRECTION('ref_axis',(3.51476976596738E-15,0.811242185175568,-0.584710284663755)) ;
#65213 = DIRECTION('',(-1.,4.33257765707378E-15,-1.87094791317046E-31)) ;
#65214 = DIRECTION('center_axis',(1.37008135359091E-15,0.316227766016839,
-0.948683298050513)) ;
#65215 = DIRECTION('ref_axis',(-1.,2.21856832751295E-31,-1.44419255235793E-15)) ;
#65216 = DIRECTION('',(-1.,4.33257765707378E-15,0.)) ;
#65217 = DIRECTION('center_axis',(-1.37008135359091E-15,-0.316227766016839,
0.948683298050513)) ;
#65218 = DIRECTION('ref_axis',(6.51683787482125E-33,0.948683298050513,0.316227766016839)) ;
#65219 = DIRECTION('',(1.,-4.33257765707378E-15,0.)) ;
#65220 = DIRECTION('center_axis',(-1.,4.33257765707378E-15,0.)) ;
#65221 = DIRECTION('ref_axis',(-6.94002007111956E-16,-0.160182243006969,0.987087457637497)) ;
#65222 = DIRECTION('center_axis',(-0.619644288569963,3.43140279610413E-12,
-0.784882765540577)) ;
#65223 = DIRECTION('ref_axis',(-0.758435045527754,-0.257405018879986,0.59876450961184)) ;
#65224 = DIRECTION('center_axis',(0.619644288579022,1.3942318686827E-14,0.784882765533426)) ;
#65225 = DIRECTION('ref_axis',(-0.784882765533426,2.93522498670039E-14,0.619644288579022)) ;
#65226 = DIRECTION('',(1.,-4.33257765707378E-15,0.)) ;
#65227 = DIRECTION('center_axis',(-1.1460366705808E-14,1.,0.)) ;
#65228 = DIRECTION('ref_axis',(-0.923879532511294,-1.05879982345699E-14,-0.382683432365072)) ;
#65229 = DIRECTION('',(-1.1460366705808E-14,1.,0.)) ;
#65230 = DIRECTION('center_axis',(0.707106781186548,0.707106781186548,0.)) ;
#65231 = DIRECTION('ref_axis',(-0.707106781186548,0.707106781186548,-6.13317366673343E-17)) ;
#65232 = DIRECTION('center_axis',(0.325057583671787,0.888073833977182,-0.325057583671767)) ;
#65233 = DIRECTION('ref_axis',(0.627963030199634,-0.459700843380854,-0.627963030199569)) ;
#65234 = DIRECTION('center_axis',(-0.577350269189617,-0.577350269189633,0.577350269189627)) ;
#65235 = DIRECTION('ref_axis',(-0.816496580927732,0.408248290463818,-0.408248290463895)) ;
#65236 = DIRECTION('',(-0.577350269189617,-0.577350269189633,0.577350269189627)) ;
#65237 = DIRECTION('center_axis',(1.,0.,0.)) ;
#65238 = DIRECTION('ref_axis',(0.,0.707106781186527,-0.707106781186567)) ;
#65239 = DIRECTION('',(0.577350269189617,0.577350269189633,-0.577350269189627)) ;
#65240 = DIRECTION('center_axis',(-1.,-1.1460366705808E-14,0.)) ;
#65241 = DIRECTION('ref_axis',(-8.10370301256115E-15,0.707106781186528,-0.707106781186567)) ;
#65242 = DIRECTION('center_axis',(1.,1.1460366705808E-14,0.)) ;
#65243 = DIRECTION('ref_axis',(1.1460366705808E-14,-1.,0.)) ;
#65244 = DIRECTION('',(0.,0.,-1.)) ;
#65245 = DIRECTION('',(0.,0.,-1.)) ;
#65246 = DIRECTION('',(-1.1460366705808E-14,1.,0.)) ;
#65247 = DIRECTION('',(0.,0.,-1.)) ;
#65248 = DIRECTION('',(1.1460366705808E-14,-1.,0.)) ;
#65249 = DIRECTION('center_axis',(-0.707106781186557,0.707106781186538,0.)) ;
#65250 = DIRECTION('ref_axis',(0.,0.,1.)) ;
#65251 = DIRECTION('',(0.,0.,1.)) ;
#65252 = DIRECTION('',(-0.707106781186538,-0.707106781186557,0.)) ;
#65253 = DIRECTION('center_axis',(1.,0.,0.)) ;
#65254 = DIRECTION('ref_axis',(0.,-1.,0.)) ;
#65255 = DIRECTION('',(0.,-1.,0.)) ;
#65256 = DIRECTION('',(0.,1.,-1.1460366705808E-14)) ;
#65257 = DIRECTION('center_axis',(-0.775298772960297,-0.446604865986822,-0.446604865986871)) ;
#65258 = DIRECTION('ref_axis',(2.37792745215863E-16,0.707106781186586,-0.707106781186509)) ;
#65259 = DIRECTION('center_axis',(0.562259334229024,0.584749707598188,0.58474970759819)) ;
#65260 = DIRECTION('ref_axis',(0.713802383285103,0.0138615341031294,-0.700209979569568)) ;
#65261 = DIRECTION('center_axis',(0.562259334229093,0.584749707598142,0.58474970759817)) ;
#65262 = DIRECTION('ref_axis',(0.720833064901749,-0.693108716251896,7.79318925176357E-14)) ;
#65263 = DIRECTION('center_axis',(-0.562259334229085,-0.584749707598146,-0.584749707598173)) ;
#65264 = DIRECTION('ref_axis',(-1.18627502215973E-16,0.707106781186564,-0.707106781186531)) ;
#65265 = DIRECTION('center_axis',(0.19685783251961,-0.583304900665865,0.78803704648631)) ;
#65266 = DIRECTION('ref_axis',(0.78119171350986,0.579006600237654,0.233432781812587)) ;
#65267 = DIRECTION('center_axis',(0.565722293792106,0.583077304611728,0.583077304611765)) ;
#65268 = DIRECTION('ref_axis',(0.789377540093176,-0.587385910954562,-0.178496192700365)) ;
#65269 = DIRECTION('center_axis',(0.564625956820454,0.583608399907212,0.583608399907276)) ;
#65270 = DIRECTION('ref_axis',(0.77036467547575,-0.626421912814156,-0.118885886148851)) ;
#65271 = DIRECTION('center_axis',(0.00458966530060586,-0.702402377604852,
0.711765294818088)) ;
#65272 = DIRECTION('ref_axis',(-0.569710409149352,-0.58680098182834,-0.575408252836344)) ;
#65273 = DIRECTION('center_axis',(-0.693108716251782,-0.720833064901858,0.)) ;
#65274 = DIRECTION('ref_axis',(-0.509705948295558,0.49010187336111,0.707106781186587)) ;
#65275 = DIRECTION('',(-0.693108716251782,-0.720833064901858,0.)) ;
#65276 = DIRECTION('center_axis',(-1.,0.,0.)) ;
#65277 = DIRECTION('ref_axis',(0.,-0.382683432365103,0.923879532511281)) ;
#65278 = DIRECTION('',(1.,0.,0.)) ;
#65279 = DIRECTION('',(-1.,0.,0.)) ;
#65280 = DIRECTION('center_axis',(0.5812381937191,0.813733471206732,0.)) ;
#65281 = DIRECTION('ref_axis',(0.813733471206732,-0.5812381937191,0.)) ;
#65282 = DIRECTION('',(1.,0.,0.)) ;
#65283 = DIRECTION('center_axis',(0.,1.,0.)) ;
#65284 = DIRECTION('ref_axis',(0.999543602081496,0.,-0.0302090638376767)) ;
#65285 = DIRECTION('center_axis',(-0.57735026918968,0.577350269189644,0.577350269189553)) ;
#65286 = DIRECTION('ref_axis',(4.44309531493773E-14,0.707106781186514,-0.707106781186581)) ;
#65287 = DIRECTION('center_axis',(-0.707106781186548,-0.707106781186548,0.)) ;
#65288 = DIRECTION('ref_axis',(0.707106781186548,-0.707106781186548,1.05140120001146E-16)) ;
#65289 = DIRECTION('center_axis',(0.577350269189625,-0.577350269189625,-0.577350269189627)) ;
#65290 = DIRECTION('ref_axis',(-0.707106781186519,5.9788700148313E-14,-0.707106781186576)) ;
#65291 = DIRECTION('center_axis',(-0.577350269189553,0.577350269189626,0.577350269189698)) ;
#65292 = DIRECTION('ref_axis',(2.33165764110149E-16,0.707106781186592,-0.707106781186503)) ;
#65293 = DIRECTION('',(-0.577350269189625,0.577350269189625,0.577350269189627)) ;
#65294 = DIRECTION('',(0.577350269189625,-0.577350269189625,-0.577350269189627)) ;
#65295 = DIRECTION('center_axis',(-0.685916369319234,0.685916369319179,0.242976271680828)) ;
#65296 = DIRECTION('ref_axis',(1.06456572474764E-16,0.33390521253534,-0.942606656586791)) ;
#65297 = DIRECTION('center_axis',(0.707106781186548,0.707106781186548,0.)) ;
#65298 = DIRECTION('ref_axis',(-0.707106781186547,0.707106781186547,4.46048993944254E-17)) ;
#65299 = DIRECTION('center_axis',(-0.806404995855704,-0.591363663627519,0.)) ;
#65300 = DIRECTION('ref_axis',(-0.591363663627519,0.806404995855704,0.)) ;
#65301 = DIRECTION('center_axis',(-0.806404995855704,-0.591363663627519,0.)) ;
#65302 = DIRECTION('ref_axis',(-0.591363663627519,0.806404995855704,0.)) ;
#65303 = DIRECTION('center_axis',(0.,0.,-1.)) ;
#65304 = DIRECTION('ref_axis',(1.,0.,0.)) ;
#65305 = DIRECTION('',(1.,-4.33257765707378E-15,0.)) ;
#65306 = DIRECTION('center_axis',(0.,0.,1.)) ;
#65307 = DIRECTION('ref_axis',(1.,0.,0.)) ;
#65308 = DIRECTION('',(0.,1.,0.)) ;
#65309 = DIRECTION('',(-1.,1.97372982155583E-14,0.)) ;
#65310 = DIRECTION('',(7.40148683083432E-15,-1.,0.)) ;
#65311 = DIRECTION('center_axis',(0.,0.,1.)) ;
#65312 = DIRECTION('ref_axis',(1.,0.,0.)) ;
#65313 = DIRECTION('',(1.1460366705808E-14,-1.,0.)) ;
#65314 = DIRECTION('',(-1.,0.,0.)) ;
#65315 = DIRECTION('',(1.32407757812447E-14,1.,0.)) ;
#65316 = DIRECTION('center_axis',(0.,0.,-1.)) ;
#65317 = DIRECTION('ref_axis',(-0.483396168210882,-0.875401704681363,0.)) ;
#65318 = DIRECTION('',(-0.846331659376489,-0.532656289118076,0.)) ;
#65319 = DIRECTION('',(0.532656289118094,-0.846331659376477,0.)) ;
#65320 = DIRECTION('',(0.846331659376502,0.532656289118055,0.)) ;
#65321 = DIRECTION('center_axis',(0.,0.,1.)) ;
#65322 = DIRECTION('ref_axis',(-0.483396168210815,-0.8754017046814,0.)) ;
#65323 = DIRECTION('',(-8.82718385416297E-15,-1.,0.)) ;
#65324 = DIRECTION('',(-1.,-2.61228946970635E-14,0.)) ;
#65325 = DIRECTION('',(0.376618052248766,-0.926368632197974,0.)) ;
#65326 = DIRECTION('',(0.376618052248709,0.926368632197997,0.)) ;
#65327 = DIRECTION('',(-1.,-2.61228946970635E-14,0.)) ;
#65328 = DIRECTION('',(0.532656289118094,-0.846331659376477,0.)) ;
#65329 = DIRECTION('',(-0.846331659376499,-0.532656289118059,0.)) ;
#65330 = DIRECTION('center_axis',(0.,0.,1.)) ;
#65331 = DIRECTION('ref_axis',(0.483396168210815,0.8754017046814,0.)) ;
#65332 = DIRECTION('',(8.82718385416297E-15,1.,0.)) ;
#65333 = DIRECTION('',(1.,2.61228946970635E-14,0.)) ;
#65334 = DIRECTION('',(-0.376618052248766,0.926368632197974,0.)) ;
#65335 = DIRECTION('',(-0.376618052248709,-0.926368632197997,0.)) ;
#65336 = DIRECTION('',(1.,2.61228946970635E-14,0.)) ;
#65337 = DIRECTION('',(-1.32407757812447E-14,-1.,0.)) ;
#65338 = DIRECTION('center_axis',(0.,0.,-1.)) ;
#65339 = DIRECTION('ref_axis',(0.483396168210882,0.875401704681363,0.)) ;
#65340 = DIRECTION('',(0.846331659376486,0.532656289118079,0.)) ;
#65341 = DIRECTION('',(1.,0.,0.)) ;
#65342 = DIRECTION('',(0.,1.,0.)) ;
#65343 = DIRECTION('',(-1.,0.,0.)) ;
#65344 = DIRECTION('',(0.,-1.,0.)) ;
#65345 = DIRECTION('center_axis',(-1.,0.,0.)) ;
#65346 = DIRECTION('ref_axis',(0.,0.382683432365084,-0.923879532511289)) ;
#65347 = DIRECTION('center_axis',(-0.887969814182011,-0.45887534031808,0.0307088122455258)) ;
#65348 = DIRECTION('ref_axis',(0.459384428746892,-0.888157645910459,0.011913968091454)) ;
#65349 = DIRECTION('',(1.,0.,0.)) ;
#65350 = DIRECTION('center_axis',(0.,0.707106781186549,-0.707106781186546)) ;
#65351 = DIRECTION('ref_axis',(-1.,0.,0.)) ;
#65352 = DIRECTION('center_axis',(0.,0.707106781186549,-0.707106781186546)) ;
#65353 = DIRECTION('ref_axis',(0.,-0.707106781186546,-0.707106781186549)) ;
#65354 = DIRECTION('',(-1.,0.,0.)) ;
#65355 = DIRECTION('center_axis',(1.1460366705808E-14,-1.,0.)) ;
#65356 = DIRECTION('ref_axis',(-0.382683432365084,-4.38569246714114E-15,-0.923879532511289)) ;
#65357 = DIRECTION('center_axis',(0.,1.,0.)) ;
#65358 = DIRECTION('ref_axis',(0.,0.,-1.)) ;
#65359 = DIRECTION('center_axis',(-0.901252424525186,0.433294434867879,0.)) ;
#65360 = DIRECTION('ref_axis',(0.433294434867879,0.901252424525186,0.)) ;
#65361 = DIRECTION('center_axis',(0.569654939187224,0.592441136754725,0.569654939187197)) ;
#65362 = DIRECTION('ref_axis',(-0.720833064901863,0.693108716251777,1.10346919822314E-16)) ;
#65363 = DIRECTION('center_axis',(-0.569654939187217,-0.592441136754709,-0.569654939187221)) ;
#65364 = DIRECTION('ref_axis',(-0.821767065280649,0.398878088061543,0.406933853696639)) ;
#65365 = DIRECTION('',(-0.569654939187217,-0.592441136754709,-0.56965493918722)) ;
#65366 = DIRECTION('center_axis',(5.73018335290399E-15,-1.,1.11561779098947E-30)) ;
#65367 = DIRECTION('ref_axis',(0.923879532511287,5.2939991172849E-15,-0.382683432365089)) ;
#65368 = DIRECTION('center_axis',(-0.707106781186548,-0.707106781186548,0.)) ;
#65369 = DIRECTION('ref_axis',(0.707106781186548,-0.707106781186548,3.06658683336673E-17)) ;
#65370 = DIRECTION('',(-5.73018335290399E-15,1.,-1.11561779098947E-30)) ;
#65371 = DIRECTION('center_axis',(0.,0.,-1.)) ;
#65372 = DIRECTION('ref_axis',(1.,0.,0.)) ;
#65373 = DIRECTION('',(0.707106781186547,-3.06359504133421E-15,0.707106781186547)) ;
#65374 = DIRECTION('center_axis',(0.576796645215489,0.816887770791164,-7.08636583986139E-13)) ;
#65375 = DIRECTION('ref_axis',(0.632637288397505,-0.446699141098588,-0.632637288397417)) ;
#65376 = DIRECTION('center_axis',(4.3325776570738E-15,1.,0.)) ;
#65377 = DIRECTION('ref_axis',(0.382683432365084,-1.65800568879728E-15,-0.923879532511289)) ;
#65378 = DIRECTION('',(-0.707106781186547,3.06359504133421E-15,-0.707106781186547)) ;
#65379 = DIRECTION('center_axis',(-5.73018335290399E-15,1.,0.)) ;
#65380 = DIRECTION('ref_axis',(0.382683432365084,2.19284623357057E-15,-0.923879532511289)) ;
#65381 = DIRECTION('',(5.73018335290399E-15,-1.,0.)) ;
#65382 = DIRECTION('center_axis',(0.707106781186548,4.05185150628068E-15,
-0.707106781186548)) ;
#65383 = DIRECTION('ref_axis',(-0.707106781186548,-8.49416976177182E-32,-0.707106781186548)) ;
#65384 = DIRECTION('',(-0.577350269189627,0.577350269189627,-0.577350269189624)) ;
#65385 = DIRECTION('center_axis',(0.707106781186548,4.05185150628068E-15,
-0.707106781186548)) ;
#65386 = DIRECTION('ref_axis',(-0.707106781186548,-4.04789462004418E-15,-0.707106781186548)) ;
#65387 = DIRECTION('center_axis',(0.,1.,0.)) ;
#65388 = DIRECTION('ref_axis',(1.,0.,0.)) ;
#65389 = DIRECTION('',(-1.,0.,0.)) ;
#65390 = DIRECTION('',(0.,0.,1.)) ;
#65391 = DIRECTION('center_axis',(-0.707106781186548,-0.707106781186548,0.)) ;
#65392 = DIRECTION('ref_axis',(0.,0.,1.)) ;
#65393 = DIRECTION('',(0.707106781186547,-0.707106781186547,0.)) ;
#65394 = DIRECTION('',(0.707106781186547,-0.707106781186547,0.)) ;
#65395 = DIRECTION('center_axis',(-1.,4.33257765707378E-15,0.)) ;
#65396 = DIRECTION('ref_axis',(6.94002007111956E-16,0.160182243006969,-0.987087457637497)) ;
#65397 = DIRECTION('',(1.,-4.33257765707378E-15,0.)) ;
#65398 = DIRECTION('center_axis',(0.,0.,1.)) ;
#65399 = DIRECTION('ref_axis',(8.05483811725849E-15,-1.,0.)) ;
#65400 = DIRECTION('',(0.,0.,1.)) ;
#65401 = DIRECTION('center_axis',(0.,0.,1.)) ;
#65402 = DIRECTION('ref_axis',(1.,0.,0.)) ;
#65403 = DIRECTION('',(0.,0.,1.)) ;
#65404 = DIRECTION('center_axis',(-1.37008135359091E-15,-0.316227766016839,
0.948683298050513)) ;
#65405 = DIRECTION('ref_axis',(6.51683787482125E-33,0.948683298050513,0.316227766016839)) ;
#65406 = DIRECTION('center_axis',(-0.707106781186548,-0.707106781186548,0.)) ;
#65407 = DIRECTION('ref_axis',(0.,0.,1.)) ;
#65408 = DIRECTION('center_axis',(-1.,4.33257765707378E-15,0.)) ;
#65409 = DIRECTION('ref_axis',(-6.94002007111956E-16,-0.160182243006969,0.987087457637497)) ;
#65410 = DIRECTION('',(-1.,4.33257765707378E-15,0.)) ;
#65411 = DIRECTION('center_axis',(-1.,0.,0.)) ;
#65412 = DIRECTION('ref_axis',(0.,1.,0.)) ;
#65413 = DIRECTION('',(0.,1.,0.)) ;
#65414 = DIRECTION('center_axis',(-1.,4.33257765707378E-15,0.)) ;
#65415 = DIRECTION('ref_axis',(6.94002007111956E-16,0.160182243006969,-0.987087457637497)) ;
#65416 = DIRECTION('center_axis',(-1.,0.,0.)) ;
#65417 = DIRECTION('ref_axis',(0.,-1.,0.)) ;
#65418 = DIRECTION('',(0.,1.,1.15826058041052E-32)) ;
#65419 = DIRECTION('',(0.,0.,1.)) ;
#65420 = DIRECTION('',(0.,-1.,0.)) ;
#65421 = DIRECTION('',(0.,0.,1.)) ;
#65422 = DIRECTION('',(0.,0.,-1.)) ;
#65423 = DIRECTION('center_axis',(0.,0.,1.)) ;
#65424 = DIRECTION('ref_axis',(-1.,0.,0.)) ;
#65425 = DIRECTION('center_axis',(-1.09763027743844E-32,-3.07546720254364E-67,
1.)) ;
#65426 = DIRECTION('ref_axis',(-1.,1.74482680966927E-115,-1.09763027743844E-32)) ;
#65427 = DIRECTION('',(0.,0.,-1.)) ;
#65428 = DIRECTION('center_axis',(0.597732795757345,0.801695394071906,0.)) ;
#65429 = DIRECTION('ref_axis',(-0.801695394071906,0.597732795757345,-4.49124931094878E-33)) ;
#65430 = DIRECTION('',(0.,0.,1.)) ;
#65431 = DIRECTION('',(0.801695394071906,-0.597732795757345,4.49124931094878E-33)) ;
#65432 = DIRECTION('',(0.,0.,1.)) ;
#65433 = DIRECTION('center_axis',(0.,0.,1.)) ;
#65434 = DIRECTION('ref_axis',(-1.,0.,0.)) ;
#65435 = DIRECTION('center_axis',(-8.11022789614398E-33,1.15826058041052E-32,
-1.)) ;
#65436 = DIRECTION('ref_axis',(-1.,-9.39375727024932E-65,8.11022789614398E-33)) ;
#65437 = DIRECTION('',(0.,0.,1.)) ;
#65438 = DIRECTION('center_axis',(-1.09763027743844E-32,-3.07546720254364E-67,
1.)) ;
#65439 = DIRECTION('ref_axis',(-1.,1.74482680966927E-115,-1.09763027743844E-32)) ;
#65440 = DIRECTION('center_axis',(0.,0.,1.)) ;
#65441 = DIRECTION('ref_axis',(-1.,0.,0.)) ;
#65442 = DIRECTION('',(0.,0.,1.)) ;
#65443 = DIRECTION('center_axis',(-1.09763027743844E-32,-3.07546720254364E-67,
1.)) ;
#65444 = DIRECTION('ref_axis',(-1.,1.74482680966927E-115,-1.09763027743844E-32)) ;
#65445 = DIRECTION('center_axis',(0.819152044288994,0.573576436351043,0.)) ;
#65446 = DIRECTION('ref_axis',(0.573576436351043,-0.819152044288994,-1.49215481678704E-49)) ;
#65447 = DIRECTION('',(0.,0.,-1.)) ;
#65448 = DIRECTION('',(0.573576436351043,-0.819152044288994,-1.49215481678704E-49)) ;
#65449 = DIRECTION('center_axis',(-0.707106781186624,-0.707106781186472,0.)) ;
#65450 = DIRECTION('ref_axis',(-0.707106781186472,0.707106781186624,0.)) ;
#65451 = DIRECTION('',(0.,0.,-1.)) ;
#65452 = DIRECTION('',(-0.707106781186472,0.707106781186624,-3.62557713776763E-32)) ;
#65453 = DIRECTION('center_axis',(0.848048096156437,-0.529919264233188,0.)) ;
#65454 = DIRECTION('ref_axis',(-0.529919264233188,-0.848048096156437,0.)) ;
#65455 = DIRECTION('',(-0.529919264233188,-0.848048096156437,5.86072992644132E-32)) ;
#65456 = DIRECTION('center_axis',(-1.09763027743844E-32,-6.22497063709847E-32,
-1.)) ;
#65457 = DIRECTION('ref_axis',(1.,6.87414502838482E-81,-1.09763027743844E-32)) ;
#65458 = DIRECTION('',(-0.529919264233188,-0.848048096156437,5.86072992644132E-32)) ;
#65459 = DIRECTION('',(-0.573576436351043,0.819152044288994,-4.46962256005402E-32)) ;
#65460 = DIRECTION('center_axis',(-1.09763027743844E-32,-6.22497063709847E-32,
-1.)) ;
#65461 = DIRECTION('ref_axis',(-0.587740293442623,-0.809049656982796,5.68143190002567E-32)) ;
#65462 = DIRECTION('',(-0.997835226140326,0.0657636789837963,6.85877185444556E-33)) ;
#65463 = DIRECTION('center_axis',(-1.09763027743844E-32,-6.22497063709847E-32,
-1.)) ;
#65464 = DIRECTION('ref_axis',(0.683460430828417,-0.729987561189802,3.79396427154525E-32)) ;
#65465 = DIRECTION('',(-1.,0.,1.09763027743844E-32)) ;
#65466 = DIRECTION('',(0.,1.,-6.22497063709847E-32)) ;
#65467 = DIRECTION('center_axis',(1.09763027743844E-32,6.22497063709847E-32,
1.)) ;
#65468 = DIRECTION('ref_axis',(1.,0.,0.)) ;
#65469 = DIRECTION('center_axis',(0.573576436350949,-0.81915204428906,0.)) ;
#65470 = DIRECTION('ref_axis',(0.,0.,1.)) ;
#65471 = DIRECTION('center_axis',(-0.98342301872822,0.181325731544663,-0.000381202396841977)) ;
#65472 = DIRECTION('ref_axis',(0.181316930497745,0.983349760701326,-0.0121416161824282)) ;
#65473 = DIRECTION('center_axis',(0.997835226140326,-0.0657636789837963,-6.85877185444556E-33)) ;
#65474 = DIRECTION('ref_axis',(-0.0465019433652248,-0.705576054910746,0.707106781186438)) ;
#65475 = DIRECTION('center_axis',(-0.997835226140325,0.0657636789838148,0.)) ;
#65476 = DIRECTION('ref_axis',(-0.0657636789838148,-0.997835226140325,0.)) ;
#65477 = DIRECTION('center_axis',(1.09763027743844E-32,6.22497063709847E-32,
1.)) ;
#65478 = DIRECTION('ref_axis',(1.,0.,0.)) ;
#65479 = DIRECTION('center_axis',(-0.573576436351043,0.819152044288994,-4.46962256005402E-32)) ;
#65480 = DIRECTION('ref_axis',(-0.579227965339615,-0.405579787672668,0.707106781186493)) ;
#65481 = DIRECTION('center_axis',(-0.848048096156437,0.529919264233188,0.)) ;
#65482 = DIRECTION('ref_axis',(-0.529919264233188,-0.848048096156437,7.98410689517261E-17)) ;
#65483 = DIRECTION('center_axis',(0.848048096156437,-0.529919264233188,0.)) ;
#65484 = DIRECTION('ref_axis',(-0.529919264233188,-0.848048096156437,0.)) ;
#65485 = DIRECTION('',(0.529919264233188,0.848048096156437,0.)) ;
#65486 = DIRECTION('center_axis',(0.,1.,0.)) ;
#65487 = DIRECTION('ref_axis',(0.,0.,1.)) ;
#65488 = DIRECTION('',(-1.,0.,0.)) ;
#65489 = DIRECTION('',(0.,0.,1.)) ;
#65490 = DIRECTION('',(1.,0.,0.)) ;
#65491 = DIRECTION('center_axis',(0.,-1.,0.)) ;
#65492 = DIRECTION('ref_axis',(0.,0.,-1.)) ;
#65493 = DIRECTION('',(-1.,0.,0.)) ;
#65494 = DIRECTION('',(0.,0.,-1.)) ;
#65495 = DIRECTION('',(1.,0.,0.)) ;
#65496 = DIRECTION('center_axis',(1.,0.,0.)) ;
#65497 = DIRECTION('ref_axis',(0.,0.,-1.)) ;
#65498 = DIRECTION('',(0.,1.,0.)) ;
#65499 = DIRECTION('',(0.,-1.,0.)) ;
#65500 = DIRECTION('center_axis',(0.,0.,1.)) ;
#65501 = DIRECTION('ref_axis',(0.,-1.,0.)) ;
#65502 = DIRECTION('',(0.,-1.,0.)) ;
#65503 = DIRECTION('center_axis',(0.,1.,0.)) ;
#65504 = DIRECTION('ref_axis',(0.,0.,1.)) ;
#65505 = DIRECTION('',(0.,0.,1.)) ;
#65506 = DIRECTION('center_axis',(0.,0.,-1.)) ;
#65507 = DIRECTION('ref_axis',(0.,1.,0.)) ;
#65508 = DIRECTION('',(0.,1.,0.)) ;
#65509 = DIRECTION('center_axis',(1.,0.,0.)) ;
#65510 = DIRECTION('ref_axis',(0.,0.,-1.)) ;
#65511 = DIRECTION('center_axis',(0.906307787036666,-0.422618261740665,0.)) ;
#65512 = DIRECTION('ref_axis',(-0.298836238730083,-0.640856382055773,0.707106781186577)) ;
#65513 = DIRECTION('',(0.906307787036666,-0.422618261740665,0.)) ;
#65514 = DIRECTION('',(-0.906307787036666,0.422618261740665,0.)) ;
#65515 = DIRECTION('center_axis',(0.155362542872172,-0.987857520228647,6.89948289044009E-15)) ;
#65516 = DIRECTION('ref_axis',(0.987857520228647,0.155362542872172,4.6428742654117E-15)) ;
#65517 = DIRECTION('center_axis',(-0.0419797672693987,-0.999118461014512,
0.)) ;
#65518 = DIRECTION('ref_axis',(-0.706483438992048,0.0296841781088257,0.707106781186528)) ;
#65519 = DIRECTION('',(-0.0419797672693987,-0.999118461014512,0.)) ;
#65520 = DIRECTION('',(0.0419797672693987,0.999118461014512,0.)) ;
#65521 = DIRECTION('center_axis',(0.906307787036666,-0.422618261740665,0.)) ;
#65522 = DIRECTION('ref_axis',(-0.298836238730185,-0.640856382055991,0.707106781186336)) ;
#65523 = DIRECTION('',(-0.906307787036666,0.422618261740665,0.)) ;
#65524 = DIRECTION('',(0.906307787036666,-0.422618261740665,0.)) ;
#65525 = DIRECTION('center_axis',(0.856607881531938,0.51596796150281,0.)) ;
#65526 = DIRECTION('ref_axis',(-0.51596796150281,0.856607881531938,0.)) ;
#65527 = DIRECTION('center_axis',(0.0501684275789832,0.998740771609056,0.)) ;
#65528 = DIRECTION('ref_axis',(0.706216372252235,-0.0354744353425645,0.707106781186561)) ;
#65529 = DIRECTION('',(-0.0501684275789832,-0.998740771609056,0.)) ;
#65530 = DIRECTION('',(0.0501684275789832,0.998740771609056,0.)) ;
#65531 = DIRECTION('center_axis',(-0.906307787036635,0.422618261740731,-8.04963018052133E-14)) ;
#65532 = DIRECTION('ref_axis',(-0.422618261740731,-0.906307787036635,-3.27260221745424E-14)) ;
#65533 = DIRECTION('center_axis',(-0.732832174562208,-0.680409438446018,0.)) ;
#65534 = DIRECTION('ref_axis',(-0.48112212790844,0.518190600104545,0.707106781186651)) ;
#65535 = DIRECTION('',(0.732832174562208,0.680409438446018,0.)) ;
#65536 = DIRECTION('',(-0.732832174562208,-0.680409438446018,0.)) ;
#65537 = DIRECTION('center_axis',(-0.422618261740665,-0.906307787036666,0.)) ;
#65538 = DIRECTION('ref_axis',(0.906307787036666,-0.422618261740665,0.)) ;
#65539 = DIRECTION('',(0.,0.,1.)) ;
#65540 = DIRECTION('',(0.906307787036666,-0.422618261740665,0.)) ;
#65541 = DIRECTION('',(0.,0.,1.)) ;
#65542 = DIRECTION('center_axis',(0.998740771609056,-0.0501684275789832,0.)) ;
#65543 = DIRECTION('ref_axis',(0.0501684275789832,0.998740771609056,0.)) ;
#65544 = DIRECTION('',(0.,0.,1.)) ;
#65545 = DIRECTION('',(0.0501684275789832,0.998740771609056,0.)) ;
#65546 = DIRECTION('center_axis',(-0.680409438446018,0.732832174562208,0.)) ;
#65547 = DIRECTION('ref_axis',(-0.732832174562208,-0.680409438446018,0.)) ;
#65548 = DIRECTION('',(0.,0.,1.)) ;
#65549 = DIRECTION('',(-0.732832174562208,-0.680409438446018,0.)) ;
#65550 = DIRECTION('center_axis',(-0.422618261740665,-0.906307787036666,0.)) ;
#65551 = DIRECTION('ref_axis',(0.906307787036666,-0.422618261740665,0.)) ;
#65552 = DIRECTION('',(0.,0.,1.)) ;
#65553 = DIRECTION('',(0.906307787036666,-0.422618261740665,0.)) ;
#65554 = DIRECTION('center_axis',(0.,0.,-1.)) ;
#65555 = DIRECTION('ref_axis',(1.,0.,0.)) ;
#65556 = DIRECTION('center_axis',(-0.906307787036654,0.42261826174069,0.)) ;
#65557 = DIRECTION('ref_axis',(0.298836238730101,0.640856382055765,0.707106781186577)) ;
#65558 = DIRECTION('',(-0.906307787036654,0.42261826174069,0.)) ;
#65559 = DIRECTION('center_axis',(-0.856607881531938,-0.51596796150281,0.)) ;
#65560 = DIRECTION('ref_axis',(0.51596796150281,-0.856607881531938,0.)) ;
#65561 = DIRECTION('',(0.906307787036654,-0.42261826174069,0.)) ;
#65562 = DIRECTION('center_axis',(-0.0501684275790028,-0.998740771609055,
0.)) ;
#65563 = DIRECTION('ref_axis',(-0.706216372252234,0.0354744353425784,0.707106781186561)) ;
#65564 = DIRECTION('',(-0.0501684275790028,-0.998740771609055,0.)) ;
#65565 = DIRECTION('center_axis',(0.906307787036677,-0.422618261740641,0.)) ;
#65566 = DIRECTION('ref_axis',(0.422618261740641,0.906307787036677,0.)) ;
#65567 = DIRECTION('',(0.0501684275790028,0.998740771609055,0.)) ;
#65568 = DIRECTION('center_axis',(0.732832174562234,0.68040943844599,0.)) ;
#65569 = DIRECTION('ref_axis',(0.481122127908406,-0.518190600104549,0.707106781186672)) ;
#65570 = DIRECTION('',(-0.732832174562234,-0.68040943844599,0.)) ;
#65571 = DIRECTION('',(0.732832174562234,0.68040943844599,0.)) ;
#65572 = DIRECTION('center_axis',(-0.155362542872191,0.987857520228644,-6.89948289044093E-15)) ;
#65573 = DIRECTION('ref_axis',(-0.987857520228644,-0.155362542872191,-4.64287426541169E-15)) ;
#65574 = DIRECTION('center_axis',(-0.906307787036654,0.42261826174069,0.)) ;
#65575 = DIRECTION('ref_axis',(0.298836238730106,0.640856382055777,0.707106781186564)) ;
#65576 = DIRECTION('',(0.906307787036654,-0.42261826174069,0.)) ;
#65577 = DIRECTION('',(-0.906307787036654,0.42261826174069,0.)) ;
#65578 = DIRECTION('center_axis',(-0.1631941084961,0.986593980800695,0.)) ;
#65579 = DIRECTION('ref_axis',(0.69762729410203,0.11539566076729,0.707106781186519)) ;
#65580 = DIRECTION('',(0.1631941084961,-0.986593980800695,0.)) ;
#65581 = DIRECTION('',(-0.1631941084961,0.986593980800695,0.)) ;
#65582 = DIRECTION('center_axis',(0.42261826174069,0.906307787036654,0.)) ;
#65583 = DIRECTION('ref_axis',(-0.906307787036654,0.42261826174069,0.)) ;
#65584 = DIRECTION('',(0.,0.,1.)) ;
#65585 = DIRECTION('',(-0.906307787036654,0.42261826174069,0.)) ;
#65586 = DIRECTION('',(0.,0.,1.)) ;
#65587 = DIRECTION('',(0.,0.,1.)) ;
#65588 = DIRECTION('center_axis',(0.986593980800695,0.1631941084961,0.)) ;
#65589 = DIRECTION('ref_axis',(-0.1631941084961,0.986593980800696,0.)) ;
#65590 = DIRECTION('',(0.,0.,1.)) ;
#65591 = DIRECTION('',(-0.1631941084961,0.986593980800695,0.)) ;
#65592 = DIRECTION('',(0.,0.,1.)) ;
#65593 = DIRECTION('center_axis',(0.,0.,-1.)) ;
#65594 = DIRECTION('ref_axis',(1.,0.,0.)) ;
#65595 = DIRECTION('center_axis',(6.53072367426566E-15,-1.,0.)) ;
#65596 = DIRECTION('ref_axis',(-0.707106781186485,-4.61791899612837E-15,0.70710678118661)) ;
#65597 = DIRECTION('',(6.53072367426566E-15,-1.,0.)) ;
#65598 = DIRECTION('center_axis',(0.829643915257841,-0.558292910465143,0.)) ;
#65599 = DIRECTION('ref_axis',(0.558292910465143,0.829643915257841,0.)) ;
#65600 = DIRECTION('',(-6.53072367426566E-15,1.,0.)) ;
#65601 = DIRECTION('center_axis',(0.707106781186642,-0.707106781186453,0.)) ;
#65602 = DIRECTION('ref_axis',(-0.707106781186453,-0.707106781186642,0.)) ;
#65603 = DIRECTION('center_axis',(0.926368632197979,0.376618052248755,0.)) ;
#65604 = DIRECTION('ref_axis',(0.266309178662358,-0.655041541705682,0.707106781186564)) ;
#65605 = DIRECTION('',(0.926368632197979,0.376618052248755,0.)) ;
#65606 = DIRECTION('center_axis',(-1.33801610590714E-13,1.,1.18839703047794E-26)) ;
#65607 = DIRECTION('ref_axis',(-1.,-1.33801610590714E-13,4.83146513558743E-27)) ;
#65608 = DIRECTION('',(-0.926368632197979,-0.376618052248755,0.)) ;
#65609 = DIRECTION('center_axis',(-0.926368632197992,0.376618052248722,0.)) ;
#65610 = DIRECTION('ref_axis',(0.266309178662343,0.655041541705713,0.707106781186541)) ;
#65611 = DIRECTION('',(-0.926368632197992,0.376618052248721,0.)) ;
#65612 = DIRECTION('center_axis',(-0.829643915257841,-0.558292910465143,0.)) ;
#65613 = DIRECTION('ref_axis',(0.558292910465143,-0.829643915257841,0.)) ;
#65614 = DIRECTION('',(0.926368632197992,-0.376618052248721,0.)) ;
#65615 = DIRECTION('center_axis',(6.53072367426566E-15,-1.,0.)) ;
#65616 = DIRECTION('ref_axis',(-0.707106781186548,-4.61791899612877E-15,0.707106781186548)) ;
#65617 = DIRECTION('',(-6.53072367426566E-15,1.,0.)) ;
#65618 = DIRECTION('',(6.53072367426566E-15,-1.,0.)) ;
#65619 = DIRECTION('center_axis',(-0.707106781186485,-0.70710678118661,0.)) ;
#65620 = DIRECTION('ref_axis',(-0.70710678118661,0.707106781186485,0.)) ;
#65621 = DIRECTION('center_axis',(-1.,-1.77635683940026E-14,0.)) ;
#65622 = DIRECTION('ref_axis',(-1.25607396694692E-14,0.707106781186485,0.70710678118661)) ;
#65623 = DIRECTION('',(1.,1.77635683940026E-14,0.)) ;
#65624 = DIRECTION('',(-1.,-1.77635683940026E-14,0.)) ;
#65625 = DIRECTION('center_axis',(-0.707106781186485,-0.70710678118661,0.)) ;
#65626 = DIRECTION('ref_axis',(0.70710678118661,-0.707106781186485,0.)) ;
#65627 = DIRECTION('center_axis',(0.,-1.,0.)) ;
#65628 = DIRECTION('ref_axis',(-0.707106781186548,0.,0.707106781186548)) ;
#65629 = DIRECTION('',(0.,1.,0.)) ;
#65630 = DIRECTION('',(0.,-1.,0.)) ;
#65631 = DIRECTION('center_axis',(0.70710678118661,-0.707106781186485,0.)) ;
#65632 = DIRECTION('ref_axis',(0.707106781186485,0.70710678118661,0.)) ;
#65633 = DIRECTION('center_axis',(1.,0.,0.)) ;
#65634 = DIRECTION('ref_axis',(0.,-0.707106781186736,0.707106781186359)) ;
#65635 = DIRECTION('',(-1.,0.,0.)) ;
#65636 = DIRECTION('',(1.,0.,0.)) ;
#65637 = DIRECTION('center_axis',(-1.77635683940026E-14,1.,0.)) ;
#65638 = DIRECTION('ref_axis',(-1.,-1.77635683940026E-14,0.)) ;
#65639 = DIRECTION('',(0.,0.,1.)) ;
#65640 = DIRECTION('',(-1.,-1.77635683940026E-14,0.)) ;
#65641 = DIRECTION('',(0.,0.,1.)) ;
#65642 = DIRECTION('center_axis',(-1.,0.,0.)) ;
#65643 = DIRECTION('ref_axis',(0.,-1.,0.)) ;
#65644 = DIRECTION('',(0.,0.,1.)) ;
#65645 = DIRECTION('',(0.,-1.,0.)) ;
#65646 = DIRECTION('center_axis',(0.,-1.,0.)) ;
#65647 = DIRECTION('ref_axis',(1.,0.,0.)) ;
#65648 = DIRECTION('',(0.,0.,1.)) ;
#65649 = DIRECTION('',(1.,0.,0.)) ;
#65650 = DIRECTION('center_axis',(-1.,-6.53072367426566E-15,0.)) ;
#65651 = DIRECTION('ref_axis',(6.53072367426566E-15,-1.,0.)) ;
#65652 = DIRECTION('',(0.,0.,1.)) ;
#65653 = DIRECTION('',(6.53072367426566E-15,-1.,0.)) ;
#65654 = DIRECTION('center_axis',(0.,0.,1.)) ;
#65655 = DIRECTION('ref_axis',(1.,0.,0.)) ;
#65656 = DIRECTION('center_axis',(1.,8.88178419700144E-14,0.)) ;
#65657 = DIRECTION('ref_axis',(6.28036983473691E-14,-0.707106781186736,0.707106781186359)) ;
#65658 = DIRECTION('',(1.,8.88178419700144E-14,0.)) ;
#65659 = DIRECTION('center_axis',(0.70710678118661,0.707106781186485,0.)) ;
#65660 = DIRECTION('ref_axis',(-0.707106781186485,0.70710678118661,0.)) ;
#65661 = DIRECTION('',(-1.,-8.88178419700144E-14,0.)) ;
#65662 = DIRECTION('center_axis',(0.707106781186736,-0.707106781186359,0.)) ;
#65663 = DIRECTION('ref_axis',(0.707106781186359,0.707106781186736,0.)) ;
#65664 = DIRECTION('center_axis',(0.,1.,0.)) ;
#65665 = DIRECTION('ref_axis',(0.707106781186548,0.,0.707106781186548)) ;
#65666 = DIRECTION('',(0.,-1.,0.)) ;
#65667 = DIRECTION('',(0.,1.,0.)) ;
#65668 = DIRECTION('center_axis',(-0.70710678118661,0.707106781186485,0.)) ;
#65669 = DIRECTION('ref_axis',(-0.707106781186485,-0.70710678118661,0.)) ;
#65670 = DIRECTION('center_axis',(-1.,0.,0.)) ;
#65671 = DIRECTION('ref_axis',(0.,0.707106781186736,0.707106781186359)) ;
#65672 = DIRECTION('',(1.,0.,0.)) ;
#65673 = DIRECTION('',(-1.,0.,0.)) ;
#65674 = DIRECTION('center_axis',(-0.70710678118661,-0.707106781186485,0.)) ;
#65675 = DIRECTION('ref_axis',(0.707106781186485,-0.70710678118661,0.)) ;
#65676 = DIRECTION('center_axis',(0.,-1.,0.)) ;
#65677 = DIRECTION('ref_axis',(-0.707106781186548,0.,0.707106781186548)) ;
#65678 = DIRECTION('',(0.,1.,0.)) ;
#65679 = DIRECTION('',(0.,-1.,0.)) ;
#65680 = DIRECTION('center_axis',(-1.,0.,0.)) ;
#65681 = DIRECTION('ref_axis',(0.,-1.,0.)) ;
#65682 = DIRECTION('',(0.,0.,1.)) ;
#65683 = DIRECTION('',(0.,-1.,0.)) ;
#65684 = DIRECTION('',(0.,0.,1.)) ;
#65685 = DIRECTION('center_axis',(8.88178419700144E-14,-1.,0.)) ;
#65686 = DIRECTION('ref_axis',(1.,8.88178419700144E-14,0.)) ;
#65687 = DIRECTION('',(0.,0.,1.)) ;
#65688 = DIRECTION('',(1.,8.88178419700144E-14,0.)) ;
#65689 = DIRECTION('center_axis',(0.,0.,1.)) ;
#65690 = DIRECTION('ref_axis',(1.,0.,0.)) ;
#65691 = DIRECTION('center_axis',(6.53072367426566E-15,1.,0.)) ;
#65692 = DIRECTION('ref_axis',(0.707106781186548,-4.61791899612877E-15,0.707106781186548)) ;
#65693 = DIRECTION('',(6.53072367426566E-15,1.,0.)) ;
#65694 = DIRECTION('center_axis',(0.70710678118661,0.707106781186485,0.)) ;
#65695 = DIRECTION('ref_axis',(0.707106781186485,-0.70710678118661,0.)) ;
#65696 = DIRECTION('',(-6.53072367426566E-15,-1.,0.)) ;
#65697 = DIRECTION('center_axis',(0.82964391525788,0.558292910465086,0.)) ;
#65698 = DIRECTION('ref_axis',(-0.558292910465086,0.82964391525788,0.)) ;
#65699 = DIRECTION('center_axis',(1.,0.,0.)) ;
#65700 = DIRECTION('ref_axis',(0.,-0.707106781186736,0.707106781186359)) ;
#65701 = DIRECTION('',(1.,0.,0.)) ;
#65702 = DIRECTION('center_axis',(0.70710678118661,0.707106781186485,0.)) ;
#65703 = DIRECTION('ref_axis',(-0.707106781186485,0.70710678118661,0.)) ;
#65704 = DIRECTION('',(-1.,0.,0.)) ;
#65705 = DIRECTION('center_axis',(-2.22044604925036E-14,1.,0.)) ;
#65706 = DIRECTION('ref_axis',(0.707106781186548,1.57009245868381E-14,0.707106781186548)) ;
#65707 = DIRECTION('',(-2.22044604925036E-14,1.,0.)) ;
#65708 = DIRECTION('center_axis',(-0.707106781186642,0.707106781186453,0.)) ;
#65709 = DIRECTION('ref_axis',(-0.707106781186453,-0.707106781186642,0.)) ;
#65710 = DIRECTION('',(2.22044604925036E-14,-1.,0.)) ;
#65711 = DIRECTION('center_axis',(-1.,1.77635683940026E-14,0.)) ;
#65712 = DIRECTION('ref_axis',(1.25607396694736E-14,0.707106781186736,0.707106781186359)) ;
#65713 = DIRECTION('',(1.,-1.77635683940026E-14,0.)) ;
#65714 = DIRECTION('',(-1.,1.77635683940026E-14,0.)) ;
#65715 = DIRECTION('center_axis',(-0.707106781186736,0.707106781186359,0.)) ;
#65716 = DIRECTION('ref_axis',(0.707106781186359,0.707106781186736,0.)) ;
#65717 = DIRECTION('center_axis',(6.53072367426566E-15,1.,0.)) ;
#65718 = DIRECTION('ref_axis',(0.707106781186548,-4.61791899612877E-15,0.707106781186548)) ;
#65719 = DIRECTION('',(-6.53072367426566E-15,-1.,0.)) ;
#65720 = DIRECTION('',(6.53072367426566E-15,1.,0.)) ;
#65721 = DIRECTION('center_axis',(-0.829643915257779,0.558292910465235,0.)) ;
#65722 = DIRECTION('ref_axis',(-0.558292910465235,-0.829643915257779,0.)) ;
#65723 = DIRECTION('center_axis',(-0.926368632197986,-0.376618052248738,0.)) ;
#65724 = DIRECTION('ref_axis',(-0.266309178662346,0.655041541705687,0.707106781186564)) ;
#65725 = DIRECTION('',(0.926368632197986,0.376618052248738,0.)) ;
#65726 = DIRECTION('',(-0.926368632197986,-0.376618052248738,0.)) ;
#65727 = DIRECTION('center_axis',(0.,-1.,0.)) ;
#65728 = DIRECTION('ref_axis',(1.,0.,0.)) ;
#65729 = DIRECTION('center_axis',(0.926368632197979,-0.376618052248755,0.)) ;
#65730 = DIRECTION('ref_axis',(-0.266309178662367,-0.655041541705704,0.707106781186541)) ;
#65731 = DIRECTION('',(-0.926368632197979,0.376618052248755,0.)) ;
#65732 = DIRECTION('',(0.926368632197979,-0.376618052248755,0.)) ;
#65733 = DIRECTION('center_axis',(1.,-6.53072367426566E-15,0.)) ;
#65734 = DIRECTION('ref_axis',(6.53072367426566E-15,1.,0.)) ;
#65735 = DIRECTION('',(0.,0.,1.)) ;
#65736 = DIRECTION('',(6.53072367426566E-15,1.,0.)) ;
#65737 = DIRECTION('',(0.,0.,1.)) ;
#65738 = DIRECTION('center_axis',(-0.376618052248738,0.926368632197986,0.)) ;
#65739 = DIRECTION('ref_axis',(-0.926368632197986,-0.376618052248738,0.)) ;
#65740 = DIRECTION('',(0.,0.,1.)) ;
#65741 = DIRECTION('',(-0.926368632197986,-0.376618052248738,0.)) ;
#65742 = DIRECTION('center_axis',(-0.376618052248755,-0.926368632197979,0.)) ;
#65743 = DIRECTION('ref_axis',(0.926368632197979,-0.376618052248755,0.)) ;
#65744 = DIRECTION('',(0.,0.,1.)) ;
#65745 = DIRECTION('',(0.926368632197979,-0.376618052248755,0.)) ;
#65746 = DIRECTION('center_axis',(1.,-6.53072367426566E-15,0.)) ;
#65747 = DIRECTION('ref_axis',(6.53072367426566E-15,1.,0.)) ;
#65748 = DIRECTION('',(0.,0.,1.)) ;
#65749 = DIRECTION('',(6.53072367426566E-15,1.,0.)) ;
#65750 = DIRECTION('center_axis',(0.,0.,1.)) ;
#65751 = DIRECTION('ref_axis',(1.,0.,0.)) ;
#65752 = DIRECTION('center_axis',(0.,-1.,0.)) ;
#65753 = DIRECTION('ref_axis',(-0.707106781186532,0.,0.707106781186563)) ;
#65754 = DIRECTION('',(0.,-1.,0.)) ;
#65755 = DIRECTION('center_axis',(0.70710678118661,-0.707106781186485,0.)) ;
#65756 = DIRECTION('ref_axis',(0.707106781186485,0.70710678118661,0.)) ;
#65757 = DIRECTION('',(0.,1.,0.)) ;
#65758 = DIRECTION('center_axis',(-0.70710678118661,-0.707106781186485,0.)) ;
#65759 = DIRECTION('ref_axis',(0.707106781186485,-0.70710678118661,0.)) ;
#65760 = DIRECTION('center_axis',(1.,0.,0.)) ;
#65761 = DIRECTION('ref_axis',(0.,-0.70710678118672,0.707106781186375)) ;
#65762 = DIRECTION('',(-1.,0.,0.)) ;
#65763 = DIRECTION('',(1.,0.,0.)) ;
#65764 = DIRECTION('center_axis',(0.70710678118661,0.707106781186485,0.)) ;
#65765 = DIRECTION('ref_axis',(-0.707106781186485,0.70710678118661,0.)) ;
#65766 = DIRECTION('center_axis',(0.,1.,0.)) ;
#65767 = DIRECTION('ref_axis',(0.707106781186532,0.,0.707106781186563)) ;
#65768 = DIRECTION('',(0.,-1.,0.)) ;
#65769 = DIRECTION('',(0.,1.,0.)) ;
#65770 = DIRECTION('center_axis',(-0.70710678118661,0.707106781186485,0.)) ;
#65771 = DIRECTION('ref_axis',(-0.707106781186485,-0.70710678118661,0.)) ;
#65772 = DIRECTION('center_axis',(-1.,0.,0.)) ;
#65773 = DIRECTION('ref_axis',(0.,0.70710678118672,0.707106781186375)) ;
#65774 = DIRECTION('',(1.,0.,0.)) ;
#65775 = DIRECTION('',(-1.,0.,0.)) ;
#65776 = DIRECTION('center_axis',(0.,1.,0.)) ;
#65777 = DIRECTION('ref_axis',(-1.,0.,0.)) ;
#65778 = DIRECTION('',(0.,0.,1.)) ;
#65779 = DIRECTION('',(-1.,0.,0.)) ;
#65780 = DIRECTION('',(0.,0.,1.)) ;
#65781 = DIRECTION('center_axis',(-1.,0.,0.)) ;
#65782 = DIRECTION('ref_axis',(0.,-1.,0.)) ;
#65783 = DIRECTION('',(0.,0.,1.)) ;
#65784 = DIRECTION('',(0.,-1.,0.)) ;
#65785 = DIRECTION('center_axis',(0.,0.,1.)) ;
#65786 = DIRECTION('ref_axis',(1.,0.,0.)) ;
#65787 = DIRECTION('center_axis',(0.376618052248709,0.926368632197998,0.)) ;
#65788 = DIRECTION('ref_axis',(0.655041541705691,-0.266309178662323,0.707106781186569)) ;
#65789 = DIRECTION('',(0.376618052248709,0.926368632197997,0.)) ;
#65790 = DIRECTION('center_axis',(-0.558292910465349,0.829643915257702,0.)) ;
#65791 = DIRECTION('ref_axis',(-0.829643915257702,-0.558292910465349,0.)) ;
#65792 = DIRECTION('',(-0.376618052248709,-0.926368632197997,0.)) ;
#65793 = DIRECTION('center_axis',(1.,1.67252013238358E-13,0.)) ;
#65794 = DIRECTION('ref_axis',(-1.67252013238358E-13,1.,0.)) ;
#65795 = DIRECTION('center_axis',(-1.,-2.61228946970635E-14,0.)) ;
#65796 = DIRECTION('ref_axis',(-1.84716759845137E-14,0.707106781186469,0.707106781186626)) ;
#65797 = DIRECTION('',(-1.,-2.61228946970635E-14,0.)) ;
#65798 = DIRECTION('center_axis',(-0.70710678118661,0.707106781186485,0.)) ;
#65799 = DIRECTION('ref_axis',(0.707106781186485,0.70710678118661,0.)) ;
#65800 = DIRECTION('',(1.,2.61228946970635E-14,0.)) ;
#65801 = DIRECTION('center_axis',(1.32407757812447E-14,1.,0.)) ;
#65802 = DIRECTION('ref_axis',(0.707106781186532,-9.36264234308853E-15,0.707106781186563)) ;
#65803 = DIRECTION('',(1.32407757812447E-14,1.,0.)) ;
#65804 = DIRECTION('center_axis',(0.,1.,0.)) ;
#65805 = DIRECTION('ref_axis',(0.,0.,1.)) ;
#65806 = DIRECTION('',(-1.32407757812447E-14,-1.,0.)) ;
#65807 = DIRECTION('center_axis',(0.,0.,1.)) ;
#65808 = DIRECTION('ref_axis',(1.,0.,0.)) ;
#65809 = DIRECTION('center_axis',(-0.846331659376392,-0.53265628911823,0.)) ;
#65810 = DIRECTION('ref_axis',(0.,0.,1.)) ;
#65811 = DIRECTION('center_axis',(0.,0.,-1.)) ;
#65812 = DIRECTION('ref_axis',(0.483396168210882,0.875401704681363,0.)) ;
#65813 = DIRECTION('center_axis',(0.,0.,1.)) ;
#65814 = DIRECTION('ref_axis',(0.483396168210882,0.875401704681363,0.)) ;
#65815 = DIRECTION('center_axis',(-0.846331659376486,-0.532656289118079,0.)) ;
#65816 = DIRECTION('ref_axis',(-0.376644874077004,0.598446855477894,0.707106781186646)) ;
#65817 = DIRECTION('',(0.846331659376486,0.532656289118079,0.)) ;
#65818 = DIRECTION('',(-0.846331659376486,-0.532656289118079,0.)) ;
#65819 = DIRECTION('center_axis',(-0.221801981400905,-0.975091729555037,0.)) ;
#65820 = DIRECTION('ref_axis',(0.975091729555037,-0.221801981400905,0.)) ;
#65821 = DIRECTION('center_axis',(0.532656289118094,-0.846331659376477,0.)) ;
#65822 = DIRECTION('ref_axis',(-0.598446855477921,-0.376644874077035,0.707106781186606)) ;
#65823 = DIRECTION('',(-0.532656289118094,0.846331659376477,0.)) ;
#65824 = DIRECTION('',(0.532656289118094,-0.846331659376477,0.)) ;
#65825 = DIRECTION('center_axis',(0.975091729555031,-0.221801981400932,0.)) ;
#65826 = DIRECTION('ref_axis',(0.221801981400932,0.97509172955503,0.)) ;
#65827 = DIRECTION('center_axis',(0.846331659376499,0.532656289118059,0.)) ;
#65828 = DIRECTION('ref_axis',(0.376644874077103,-0.598446855478083,0.707106781186433)) ;
#65829 = DIRECTION('',(0.846331659376499,0.532656289118059,0.)) ;
#65830 = DIRECTION('center_axis',(0.846331659376493,0.53265628911807,0.)) ;
#65831 = DIRECTION('ref_axis',(0.,0.,1.)) ;
#65832 = DIRECTION('',(-0.846331659376499,-0.532656289118059,0.)) ;
#65833 = DIRECTION('center_axis',(0.,0.,-1.)) ;
#65834 = DIRECTION('ref_axis',(-1.,0.,0.)) ;
#65835 = DIRECTION('center_axis',(0.,-1.,0.)) ;
#65836 = DIRECTION('ref_axis',(0.,0.,1.)) ;
#65837 = DIRECTION('center_axis',(0.,0.,1.)) ;
#65838 = DIRECTION('ref_axis',(0.483396168210815,0.8754017046814,0.)) ;
#65839 = DIRECTION('center_axis',(0.,0.,-1.)) ;
#65840 = DIRECTION('ref_axis',(0.483396168210815,0.8754017046814,0.)) ;
#65841 = DIRECTION('center_axis',(-8.82718385416297E-15,-1.,0.)) ;
#65842 = DIRECTION('ref_axis',(-0.707106781186469,6.24176156205835E-15,0.707106781186626)) ;
#65843 = DIRECTION('',(8.82718385416297E-15,1.,0.)) ;
#65844 = DIRECTION('',(-8.82718385416297E-15,-1.,0.)) ;
#65845 = DIRECTION('center_axis',(-0.707106781186642,-0.707106781186453,0.)) ;
#65846 = DIRECTION('ref_axis',(-0.707106781186453,0.707106781186642,0.)) ;
#65847 = DIRECTION('center_axis',(-1.,-2.61228946970635E-14,0.)) ;
#65848 = DIRECTION('ref_axis',(-1.84716759845202E-14,0.70710678118672,0.707106781186375)) ;
#65849 = DIRECTION('',(1.,2.61228946970635E-14,0.)) ;
#65850 = DIRECTION('',(-1.,-2.61228946970635E-14,0.)) ;
#65851 = DIRECTION('center_axis',(-0.558292910465166,-0.829643915257826,0.)) ;
#65852 = DIRECTION('ref_axis',(0.829643915257826,-0.558292910465166,0.)) ;
#65853 = DIRECTION('center_axis',(0.376618052248766,-0.926368632197974,0.)) ;
#65854 = DIRECTION('ref_axis',(-0.65504154170562,-0.266309178662342,0.707106781186627)) ;
#65855 = DIRECTION('',(-0.376618052248766,0.926368632197974,0.)) ;
#65856 = DIRECTION('',(0.376618052248766,-0.926368632197974,0.)) ;
#65857 = DIRECTION('center_axis',(0.532656289118059,-0.846331659376499,0.)) ;
#65858 = DIRECTION('ref_axis',(0.846331659376499,0.532656289118059,0.)) ;
#65859 = DIRECTION('',(0.,0.,1.)) ;
#65860 = DIRECTION('',(0.846331659376499,0.532656289118059,0.)) ;
#65861 = DIRECTION('',(0.,0.,1.)) ;
#65862 = DIRECTION('center_axis',(0.,0.,1.)) ;
#65863 = DIRECTION('ref_axis',(-0.532656289118219,0.846331659376399,0.)) ;
#65864 = DIRECTION('',(0.,0.,1.)) ;
#65865 = DIRECTION('center_axis',(0.,0.,-1.)) ;
#65866 = DIRECTION('ref_axis',(0.483396168210815,0.8754017046814,0.)) ;
#65867 = DIRECTION('center_axis',(-1.,8.82718385416297E-15,0.)) ;
#65868 = DIRECTION('ref_axis',(-8.82718385416297E-15,-1.,0.)) ;
#65869 = DIRECTION('',(0.,0.,1.)) ;
#65870 = DIRECTION('',(-8.82718385416297E-15,-1.,0.)) ;
#65871 = DIRECTION('center_axis',(-2.61228946970635E-14,1.,0.)) ;
#65872 = DIRECTION('ref_axis',(-1.,-2.61228946970635E-14,0.)) ;
#65873 = DIRECTION('',(0.,0.,1.)) ;
#65874 = DIRECTION('',(-1.,-2.61228946970635E-14,0.)) ;
#65875 = DIRECTION('center_axis',(-0.926368632197974,-0.376618052248766,0.)) ;
#65876 = DIRECTION('ref_axis',(0.376618052248766,-0.926368632197974,0.)) ;
#65877 = DIRECTION('',(0.,0.,1.)) ;
#65878 = DIRECTION('',(0.376618052248766,-0.926368632197974,0.)) ;
#65879 = DIRECTION('center_axis',(0.926368632197998,-0.376618052248709,0.)) ;
#65880 = DIRECTION('ref_axis',(0.376618052248709,0.926368632197998,0.)) ;
#65881 = DIRECTION('',(0.,0.,1.)) ;
#65882 = DIRECTION('',(0.376618052248709,0.926368632197997,0.)) ;
#65883 = DIRECTION('center_axis',(0.,0.,-1.)) ;
#65884 = DIRECTION('ref_axis',(1.,0.,0.)) ;
#65885 = DIRECTION('center_axis',(1.,2.61228946970635E-14,0.)) ;
#65886 = DIRECTION('ref_axis',(1.84716759845137E-14,-0.707106781186469,0.707106781186626)) ;
#65887 = DIRECTION('',(1.,2.61228946970635E-14,0.)) ;
#65888 = DIRECTION('center_axis',(0.70710678118661,-0.707106781186485,0.)) ;
#65889 = DIRECTION('ref_axis',(-0.707106781186485,-0.70710678118661,0.)) ;
#65890 = DIRECTION('',(-1.,-2.61228946970635E-14,0.)) ;
#65891 = DIRECTION('center_axis',(0.558292910465349,-0.829643915257702,0.)) ;
#65892 = DIRECTION('ref_axis',(0.829643915257702,0.558292910465349,0.)) ;
#65893 = DIRECTION('center_axis',(-1.32407757812447E-14,-1.,0.)) ;
#65894 = DIRECTION('ref_axis',(-0.707106781186532,9.36264234308853E-15,0.707106781186563)) ;
#65895 = DIRECTION('',(-1.32407757812447E-14,-1.,0.)) ;
#65896 = DIRECTION('center_axis',(0.,-1.,0.)) ;
#65897 = DIRECTION('ref_axis',(0.,0.,1.)) ;
#65898 = DIRECTION('',(1.32407757812447E-14,1.,0.)) ;
#65899 = DIRECTION('center_axis',(0.,0.,1.)) ;
#65900 = DIRECTION('ref_axis',(1.,0.,0.)) ;
#65901 = DIRECTION('center_axis',(0.846331659376392,0.53265628911823,0.)) ;
#65902 = DIRECTION('ref_axis',(0.,0.,1.)) ;
#65903 = DIRECTION('center_axis',(0.,0.,-1.)) ;
#65904 = DIRECTION('ref_axis',(-0.483396168210882,-0.875401704681363,0.)) ;
#65905 = DIRECTION('center_axis',(0.,0.,1.)) ;
#65906 = DIRECTION('ref_axis',(-0.483396168210882,-0.875401704681363,0.)) ;
#65907 = DIRECTION('center_axis',(0.846331659376489,0.532656289118076,0.)) ;
#65908 = DIRECTION('ref_axis',(0.376644874077132,-0.598446855478104,0.7071067811864)) ;
#65909 = DIRECTION('',(-0.846331659376489,-0.532656289118076,0.)) ;
#65910 = DIRECTION('',(0.846331659376489,0.532656289118076,0.)) ;
#65911 = DIRECTION('center_axis',(0.221801981400905,0.975091729555037,0.)) ;
#65912 = DIRECTION('ref_axis',(-0.975091729555037,0.221801981400905,0.)) ;
#65913 = DIRECTION('center_axis',(-0.532656289118094,0.846331659376477,0.)) ;
#65914 = DIRECTION('ref_axis',(0.598446855477966,0.376644874077064,0.707106781186553)) ;
#65915 = DIRECTION('',(-0.532656289118094,0.846331659376477,0.)) ;
#65916 = DIRECTION('center_axis',(-0.975091729555031,0.221801981400932,0.)) ;
#65917 = DIRECTION('ref_axis',(-0.221801981400932,-0.97509172955503,0.)) ;
#65918 = DIRECTION('',(0.532656289118094,-0.846331659376477,0.)) ;
#65919 = DIRECTION('center_axis',(-0.846331659376502,-0.532656289118055,0.)) ;
#65920 = DIRECTION('ref_axis',(-0.3766448740771,0.598446855478085,0.707106781186433)) ;
#65921 = DIRECTION('',(-0.846331659376502,-0.532656289118055,0.)) ;
#65922 = DIRECTION('center_axis',(-0.846331659376493,-0.53265628911807,0.)) ;
#65923 = DIRECTION('ref_axis',(0.,0.,1.)) ;
#65924 = DIRECTION('',(0.846331659376502,0.532656289118055,0.)) ;
#65925 = DIRECTION('center_axis',(0.,0.,-1.)) ;
#65926 = DIRECTION('ref_axis',(-1.,0.,0.)) ;
#65927 = DIRECTION('center_axis',(0.,1.,0.)) ;
#65928 = DIRECTION('ref_axis',(0.,0.,1.)) ;
#65929 = DIRECTION('center_axis',(0.,0.,1.)) ;
#65930 = DIRECTION('ref_axis',(-0.483396168210815,-0.8754017046814,0.)) ;
#65931 = DIRECTION('center_axis',(0.,0.,-1.)) ;
#65932 = DIRECTION('ref_axis',(-0.483396168210815,-0.8754017046814,0.)) ;
#65933 = DIRECTION('center_axis',(8.82718385416297E-15,1.,0.)) ;
#65934 = DIRECTION('ref_axis',(0.707106781186469,-6.24176156205835E-15,0.707106781186626)) ;
#65935 = DIRECTION('',(-8.82718385416297E-15,-1.,0.)) ;
#65936 = DIRECTION('',(8.82718385416297E-15,1.,0.)) ;
#65937 = DIRECTION('center_axis',(0.707106781186642,0.707106781186453,0.)) ;
#65938 = DIRECTION('ref_axis',(0.707106781186453,-0.707106781186642,0.)) ;
#65939 = DIRECTION('center_axis',(1.,2.61228946970635E-14,0.)) ;
#65940 = DIRECTION('ref_axis',(1.84716759845202E-14,-0.70710678118672,0.707106781186375)) ;
#65941 = DIRECTION('',(-1.,-2.61228946970635E-14,0.)) ;
#65942 = DIRECTION('',(1.,2.61228946970635E-14,0.)) ;
#65943 = DIRECTION('center_axis',(0.558292910465166,0.829643915257826,0.)) ;
#65944 = DIRECTION('ref_axis',(-0.829643915257826,0.558292910465166,0.)) ;
#65945 = DIRECTION('center_axis',(-0.376618052248766,0.926368632197974,0.)) ;
#65946 = DIRECTION('ref_axis',(0.65504154170562,0.266309178662342,0.707106781186627)) ;
#65947 = DIRECTION('',(0.376618052248766,-0.926368632197974,0.)) ;
#65948 = DIRECTION('',(-0.376618052248766,0.926368632197974,0.)) ;
#65949 = DIRECTION('center_axis',(-1.,-1.67252013238358E-13,0.)) ;
#65950 = DIRECTION('ref_axis',(1.67252013238358E-13,-1.,0.)) ;
#65951 = DIRECTION('center_axis',(-0.376618052248709,-0.926368632197998,0.)) ;
#65952 = DIRECTION('ref_axis',(-0.655041541705691,0.266309178662323,0.707106781186569)) ;
#65953 = DIRECTION('',(0.376618052248709,0.926368632197997,0.)) ;
#65954 = DIRECTION('',(-0.376618052248709,-0.926368632197997,0.)) ;
#65955 = DIRECTION('center_axis',(0.,0.,1.)) ;
#65956 = DIRECTION('ref_axis',(0.532656289118219,-0.846331659376399,0.)) ;
#65957 = DIRECTION('',(0.,0.,1.)) ;
#65958 = DIRECTION('center_axis',(0.,0.,-1.)) ;
#65959 = DIRECTION('ref_axis',(-0.483396168210815,-0.8754017046814,0.)) ;
#65960 = DIRECTION('',(0.,0.,1.)) ;
#65961 = DIRECTION('center_axis',(1.,-8.82718385416297E-15,0.)) ;
#65962 = DIRECTION('ref_axis',(8.82718385416297E-15,1.,0.)) ;
#65963 = DIRECTION('',(0.,0.,1.)) ;
#65964 = DIRECTION('',(8.82718385416297E-15,1.,0.)) ;
#65965 = DIRECTION('center_axis',(2.61228946970635E-14,-1.,0.)) ;
#65966 = DIRECTION('ref_axis',(1.,2.61228946970635E-14,0.)) ;
#65967 = DIRECTION('',(0.,0.,1.)) ;
#65968 = DIRECTION('',(1.,2.61228946970635E-14,0.)) ;
#65969 = DIRECTION('center_axis',(0.926368632197974,0.376618052248766,0.)) ;
#65970 = DIRECTION('ref_axis',(-0.376618052248766,0.926368632197974,0.)) ;
#65971 = DIRECTION('',(0.,0.,1.)) ;
#65972 = DIRECTION('',(-0.376618052248766,0.926368632197974,0.)) ;
#65973 = DIRECTION('center_axis',(-0.926368632197998,0.376618052248709,0.)) ;
#65974 = DIRECTION('ref_axis',(-0.376618052248709,-0.926368632197998,0.)) ;
#65975 = DIRECTION('',(0.,0.,1.)) ;
#65976 = DIRECTION('',(-0.376618052248709,-0.926368632197997,0.)) ;
#65977 = DIRECTION('center_axis',(2.61228946970635E-14,-1.,0.)) ;
#65978 = DIRECTION('ref_axis',(1.,2.61228946970635E-14,0.)) ;
#65979 = DIRECTION('',(0.,0.,1.)) ;
#65980 = DIRECTION('',(1.,2.61228946970635E-14,0.)) ;
#65981 = DIRECTION('center_axis',(0.,0.,-1.)) ;
#65982 = DIRECTION('ref_axis',(1.,0.,0.)) ;
#65983 = DIRECTION('center_axis',(-0.0419797672693987,-0.999118461014512,
0.)) ;
#65984 = DIRECTION('ref_axis',(0.706483438992037,-0.0296841781088253,-0.707106781186539)) ;
#65985 = DIRECTION('',(-0.0419797672693987,-0.999118461014512,0.)) ;
#65986 = DIRECTION('center_axis',(0.906307787036666,-0.422618261740665,0.)) ;
#65987 = DIRECTION('ref_axis',(0.298836238730083,0.640856382055773,-0.707106781186577)) ;
#65988 = DIRECTION('center_axis',(0.155362542871686,-0.987857520228724,6.8994828904185E-15)) ;
#65989 = DIRECTION('ref_axis',(-0.987857520228724,-0.155362542871686,4.64287426539732E-15)) ;
#65990 = DIRECTION('center_axis',(-0.732832174562208,-0.680409438446018,0.)) ;
#65991 = DIRECTION('ref_axis',(0.48112212790844,-0.518190600104545,-0.707106781186651)) ;
#65992 = DIRECTION('center_axis',(-0.906307787036715,0.422618261740561,0.)) ;
#65993 = DIRECTION('ref_axis',(0.422618261740561,0.906307787036715,0.)) ;
#65994 = DIRECTION('center_axis',(0.0501684275789832,0.998740771609056,0.)) ;
#65995 = DIRECTION('ref_axis',(-0.706216372252266,0.0354744353425661,-0.70710678118653)) ;
#65996 = DIRECTION('center_axis',(0.856607881531863,0.515967961502934,0.)) ;
#65997 = DIRECTION('ref_axis',(0.515967961502934,-0.856607881531863,0.)) ;
#65998 = DIRECTION('center_axis',(0.906307787036666,-0.422618261740665,0.)) ;
#65999 = DIRECTION('ref_axis',(0.298836238730072,0.64085638205575,-0.707106781186603)) ;
#66000 = DIRECTION('',(0.,0.,1.)) ;
#66001 = DIRECTION('center_axis',(-0.999118461014512,0.0419797672693987,0.)) ;
#66002 = DIRECTION('ref_axis',(-0.0419797672693987,-0.999118461014512,0.)) ;
#66003 = DIRECTION('',(0.,0.,1.)) ;
#66004 = DIRECTION('center_axis',(-0.906307787036654,0.42261826174069,0.)) ;
#66005 = DIRECTION('ref_axis',(-0.298836238730101,-0.640856382055765,-0.707106781186577)) ;
#66006 = DIRECTION('center_axis',(-0.15536254287169,0.987857520228723,-6.89948289041867E-15)) ;
#66007 = DIRECTION('ref_axis',(0.987857520228723,0.15536254287169,-4.64287426539775E-15)) ;
#66008 = DIRECTION('center_axis',(-0.0501684275790028,-0.998740771609055,
0.)) ;
#66009 = DIRECTION('ref_axis',(0.706216372252234,-0.0354744353425784,-0.707106781186561)) ;
#66010 = DIRECTION('center_axis',(-0.856607881531885,-0.515967961502898,0.)) ;
#66011 = DIRECTION('ref_axis',(-0.515967961502898,0.856607881531885,0.)) ;
#66012 = DIRECTION('',(-0.0501684275790028,-0.998740771609055,0.)) ;
#66013 = DIRECTION('center_axis',(-0.906307787036588,0.422618261740832,-4.02481509026046E-14)) ;
#66014 = DIRECTION('ref_axis',(0.422618261740832,0.906307787036588,1.63630110872747E-14)) ;
#66015 = DIRECTION('center_axis',(-0.906307787036654,0.42261826174069,0.)) ;
#66016 = DIRECTION('ref_axis',(-0.298836238730101,-0.640856382055765,-0.707106781186577)) ;
#66017 = DIRECTION('',(-0.906307787036654,0.42261826174069,0.)) ;
#66018 = DIRECTION('center_axis',(0.732832174562234,0.68040943844599,0.)) ;
#66019 = DIRECTION('ref_axis',(-0.481122127908406,0.518190600104549,-0.707106781186672)) ;
#66020 = DIRECTION('',(0.732832174562234,0.68040943844599,0.)) ;
#66021 = DIRECTION('center_axis',(-0.1631941084961,0.986593980800695,0.)) ;
#66022 = DIRECTION('ref_axis',(-0.69762729410203,-0.11539566076729,-0.707106781186519)) ;
#66023 = DIRECTION('center_axis',(0.68040943844599,-0.732832174562234,0.)) ;
#66024 = DIRECTION('ref_axis',(0.732832174562234,0.68040943844599,0.)) ;
#66025 = DIRECTION('',(0.,0.,1.)) ;
#66026 = DIRECTION('center_axis',(-0.998740771609055,0.0501684275790028,0.)) ;
#66027 = DIRECTION('ref_axis',(-0.0501684275790028,-0.998740771609055,0.)) ;
#66028 = DIRECTION('',(0.,0.,1.)) ;
#66029 = DIRECTION('center_axis',(0.926368632197979,0.376618052248755,0.)) ;
#66030 = DIRECTION('ref_axis',(-0.266309178662367,0.655041541705704,-0.707106781186541)) ;
#66031 = DIRECTION('',(-0.926368632197979,-0.376618052248755,0.)) ;
#66032 = DIRECTION('center_axis',(0.829643915257887,-0.558292910465075,0.)) ;
#66033 = DIRECTION('ref_axis',(-0.558292910465075,-0.829643915257887,0.)) ;
#66034 = DIRECTION('',(0.926368632197979,0.376618052248755,0.)) ;
#66035 = DIRECTION('center_axis',(1.33801610590758E-13,1.,0.)) ;
#66036 = DIRECTION('ref_axis',(1.,-1.33801610590758E-13,0.)) ;
#66037 = DIRECTION('center_axis',(-0.926368632197992,0.376618052248722,0.)) ;
#66038 = DIRECTION('ref_axis',(-0.266309178662335,-0.655041541705692,-0.707106781186564)) ;
#66039 = DIRECTION('',(-0.926368632197992,0.376618052248721,0.)) ;
#66040 = DIRECTION('center_axis',(0.829643915257841,0.558292910465143,0.)) ;
#66041 = DIRECTION('ref_axis',(0.558292910465143,-0.829643915257841,0.)) ;
#66042 = DIRECTION('',(0.926368632197992,-0.376618052248721,0.)) ;
#66043 = DIRECTION('center_axis',(6.53072367426566E-15,-1.,0.)) ;
#66044 = DIRECTION('ref_axis',(0.707106781186548,4.61791899612877E-15,-0.707106781186548)) ;
#66045 = DIRECTION('',(-6.53072367426566E-15,1.,0.)) ;
#66046 = DIRECTION('center_axis',(0.707106781186642,-0.707106781186453,0.)) ;
#66047 = DIRECTION('ref_axis',(0.707106781186453,0.707106781186642,0.)) ;
#66048 = DIRECTION('center_axis',(1.,0.,0.)) ;
#66049 = DIRECTION('ref_axis',(0.,0.707106781186736,-0.707106781186359)) ;
#66050 = DIRECTION('',(-1.,0.,0.)) ;
#66051 = DIRECTION('center_axis',(0.70710678118661,-0.707106781186485,0.)) ;
#66052 = DIRECTION('ref_axis',(-0.707106781186485,-0.70710678118661,0.)) ;
#66053 = DIRECTION('center_axis',(0.,-1.,0.)) ;
#66054 = DIRECTION('ref_axis',(0.707106781186548,0.,-0.707106781186548)) ;
#66055 = DIRECTION('',(0.,1.,0.)) ;
#66056 = DIRECTION('center_axis',(-0.707106781186736,-0.707106781186359,0.)) ;
#66057 = DIRECTION('ref_axis',(-0.707106781186359,0.707106781186736,0.)) ;
#66058 = DIRECTION('center_axis',(-1.,-1.77635683940026E-14,0.)) ;
#66059 = DIRECTION('ref_axis',(1.25607396694692E-14,-0.707106781186485,-0.70710678118661)) ;
#66060 = DIRECTION('',(1.,1.77635683940026E-14,0.)) ;
#66061 = DIRECTION('center_axis',(-0.70710678118661,-0.707106781186485,0.)) ;
#66062 = DIRECTION('ref_axis',(0.707106781186485,-0.70710678118661,0.)) ;
#66063 = DIRECTION('center_axis',(6.53072367426566E-15,-1.,0.)) ;
#66064 = DIRECTION('ref_axis',(0.707106781186548,4.61791899612877E-15,-0.707106781186548)) ;
#66065 = DIRECTION('',(6.53072367426566E-15,-1.,0.)) ;
#66066 = DIRECTION('',(-6.53072367426566E-15,1.,0.)) ;
#66067 = DIRECTION('center_axis',(-1.,-6.53072367426566E-15,0.)) ;
#66068 = DIRECTION('ref_axis',(6.53072367426566E-15,-1.,0.)) ;
#66069 = DIRECTION('',(0.,0.,1.)) ;
#66070 = DIRECTION('center_axis',(0.376618052248722,0.926368632197992,0.)) ;
#66071 = DIRECTION('ref_axis',(-0.926368632197992,0.376618052248722,0.)) ;
#66072 = DIRECTION('',(0.,0.,1.)) ;
#66073 = DIRECTION('center_axis',(0.376618052248755,-0.926368632197979,0.)) ;
#66074 = DIRECTION('ref_axis',(0.926368632197979,0.376618052248755,0.)) ;
#66075 = DIRECTION('center_axis',(0.,0.,-1.)) ;
#66076 = DIRECTION('ref_axis',(1.,0.,0.)) ;
#66077 = DIRECTION('',(2.61228946970624E-14,1.,0.)) ;
#66078 = DIRECTION('center_axis',(0.,0.,-1.)) ;
#66079 = DIRECTION('ref_axis',(-0.999082519440321,-0.0428266196282222,0.)) ;
#66080 = DIRECTION('',(0.,1.,0.)) ;
#66081 = DIRECTION('center_axis',(0.,0.,-1.)) ;
#66082 = DIRECTION('ref_axis',(-0.945182639171645,-0.326542154412755,0.)) ;
#66083 = DIRECTION('center_axis',(0.,0.,-1.)) ;
#66084 = DIRECTION('ref_axis',(0.945182639171645,-0.326542154412755,0.)) ;
#66085 = DIRECTION('',(0.,-1.,0.)) ;
#66086 = DIRECTION('center_axis',(0.,0.,-1.)) ;
#66087 = DIRECTION('ref_axis',(0.999082519440321,-0.0428266196282222,0.)) ;
#66088 = DIRECTION('',(0.,-1.,0.)) ;
#66089 = DIRECTION('',(-1.,0.,0.)) ;
#66090 = DIRECTION('center_axis',(0.,0.,1.)) ;
#66091 = DIRECTION('ref_axis',(0.985598559653489,0.169101978725763,0.)) ;
#66092 = DIRECTION('',(-1.,-8.88178419700144E-14,0.)) ;
#66093 = DIRECTION('',(0.,-1.,0.)) ;
#66094 = DIRECTION('',(1.,0.,0.)) ;
#66095 = DIRECTION('',(0.,1.,0.)) ;
#66096 = DIRECTION('',(2.22044604925036E-14,-1.,0.)) ;
#66097 = DIRECTION('',(1.,-1.77635683940026E-14,0.)) ;
#66098 = DIRECTION('',(-6.53072367426566E-15,-1.,0.)) ;
#66099 = DIRECTION('',(0.926368632197986,0.376618052248738,0.)) ;
#66100 = DIRECTION('',(-0.926368632197979,0.376618052248755,0.)) ;
#66101 = DIRECTION('',(-6.53072367426566E-15,-1.,0.)) ;
#66102 = DIRECTION('',(-1.,0.,0.)) ;
#66103 = DIRECTION('center_axis',(1.,8.88178419700144E-14,0.)) ;
#66104 = DIRECTION('ref_axis',(-6.28036983473468E-14,0.707106781186485,-0.70710678118661)) ;
#66105 = DIRECTION('center_axis',(0.70710678118661,-0.707106781186485,0.)) ;
#66106 = DIRECTION('ref_axis',(-0.707106781186485,-0.70710678118661,0.)) ;
#66107 = DIRECTION('center_axis',(-0.70710678118661,-0.707106781186485,0.)) ;
#66108 = DIRECTION('ref_axis',(-0.707106781186485,0.70710678118661,0.)) ;
#66109 = DIRECTION('center_axis',(0.,-1.,0.)) ;
#66110 = DIRECTION('ref_axis',(0.707106781186548,0.,-0.707106781186548)) ;
#66111 = DIRECTION('center_axis',(-0.70710678118661,-0.707106781186485,0.)) ;
#66112 = DIRECTION('ref_axis',(-0.707106781186485,0.70710678118661,0.)) ;
#66113 = DIRECTION('center_axis',(-1.,0.,0.)) ;
#66114 = DIRECTION('ref_axis',(0.,-0.707106781186736,-0.707106781186359)) ;
#66115 = DIRECTION('',(-1.,0.,0.)) ;
#66116 = DIRECTION('center_axis',(-0.70710678118661,0.707106781186485,0.)) ;
#66117 = DIRECTION('ref_axis',(0.707106781186485,0.70710678118661,0.)) ;
#66118 = DIRECTION('center_axis',(0.,1.,0.)) ;
#66119 = DIRECTION('ref_axis',(-0.707106781186548,0.,-0.707106781186548)) ;
#66120 = DIRECTION('',(0.,1.,0.)) ;
#66121 = DIRECTION('center_axis',(1.,0.,0.)) ;
#66122 = DIRECTION('ref_axis',(0.,1.,0.)) ;
#66123 = DIRECTION('',(0.,0.,1.)) ;
#66124 = DIRECTION('center_axis',(-2.22044604925036E-14,1.,0.)) ;
#66125 = DIRECTION('ref_axis',(-0.707106781186548,-1.57009245868381E-14,-0.707106781186548)) ;
#66126 = DIRECTION('center_axis',(0.70710678118661,0.707106781186485,0.)) ;
#66127 = DIRECTION('ref_axis',(0.707106781186485,-0.70710678118661,0.)) ;
#66128 = DIRECTION('',(-2.22044604925036E-14,1.,0.)) ;
#66129 = DIRECTION('center_axis',(0.70710678118661,-0.707106781186485,0.)) ;
#66130 = DIRECTION('ref_axis',(-0.707106781186485,-0.70710678118661,0.)) ;
#66131 = DIRECTION('center_axis',(1.,0.,0.)) ;
#66132 = DIRECTION('ref_axis',(0.,0.707106781186736,-0.707106781186359)) ;
#66133 = DIRECTION('center_axis',(0.707106781186579,0.707106781186516,0.)) ;
#66134 = DIRECTION('ref_axis',(-0.707106781186516,0.707106781186579,0.)) ;
#66135 = DIRECTION('',(1.,0.,0.)) ;
#66136 = DIRECTION('center_axis',(6.53072367426566E-15,1.,0.)) ;
#66137 = DIRECTION('ref_axis',(-0.707106781186548,4.61791899612877E-15,-0.707106781186548)) ;
#66138 = DIRECTION('center_axis',(0.829643915257864,0.558292910465109,0.)) ;
#66139 = DIRECTION('ref_axis',(0.558292910465109,-0.829643915257864,0.)) ;
#66140 = DIRECTION('center_axis',(0.926368632197979,-0.376618052248755,0.)) ;
#66141 = DIRECTION('ref_axis',(0.266309178662367,0.655041541705704,-0.707106781186541)) ;
#66142 = DIRECTION('center_axis',(1.33801610590799E-13,-1.,0.)) ;
#66143 = DIRECTION('ref_axis',(-1.,-1.33801610590799E-13,0.)) ;
#66144 = DIRECTION('center_axis',(-0.926368632197986,-0.376618052248738,0.)) ;
#66145 = DIRECTION('ref_axis',(0.266309178662354,-0.655041541705708,-0.707106781186541)) ;
#66146 = DIRECTION('center_axis',(-0.829643915257841,0.558292910465143,0.)) ;
#66147 = DIRECTION('ref_axis',(0.558292910465143,0.829643915257841,0.)) ;
#66148 = DIRECTION('center_axis',(6.53072367426566E-15,1.,0.)) ;
#66149 = DIRECTION('ref_axis',(-0.707106781186548,4.61791899612877E-15,-0.707106781186548)) ;
#66150 = DIRECTION('center_axis',(-0.70710678118661,0.707106781186485,0.)) ;
#66151 = DIRECTION('ref_axis',(-0.707106781186485,-0.70710678118661,0.)) ;
#66152 = DIRECTION('center_axis',(-1.,1.77635683940026E-14,0.)) ;
#66153 = DIRECTION('ref_axis',(-1.25607396694736E-14,-0.707106781186736,-0.707106781186359)) ;
#66154 = DIRECTION('',(-1.,1.77635683940026E-14,0.)) ;
#66155 = DIRECTION('center_axis',(1.77635683940026E-14,1.,0.)) ;
#66156 = DIRECTION('ref_axis',(-1.,1.77635683940026E-14,0.)) ;
#66157 = DIRECTION('',(0.,0.,1.)) ;
#66158 = DIRECTION('center_axis',(1.,2.22044604925036E-14,0.)) ;
#66159 = DIRECTION('ref_axis',(-2.22044604925036E-14,1.,0.)) ;
#66160 = DIRECTION('',(0.,0.,1.)) ;
#66161 = DIRECTION('center_axis',(-1.,0.,0.)) ;
#66162 = DIRECTION('ref_axis',(0.,-0.707106781186736,-0.707106781186359)) ;
#66163 = DIRECTION('center_axis',(-0.70710678118661,0.707106781186485,0.)) ;
#66164 = DIRECTION('ref_axis',(0.707106781186485,0.70710678118661,0.)) ;
#66165 = DIRECTION('center_axis',(-0.70710678118661,-0.707106781186485,0.)) ;
#66166 = DIRECTION('ref_axis',(-0.707106781186485,0.70710678118661,0.)) ;
#66167 = DIRECTION('center_axis',(0.,1.,0.)) ;
#66168 = DIRECTION('ref_axis',(-0.707106781186548,0.,-0.707106781186548)) ;
#66169 = DIRECTION('center_axis',(0.70710678118661,0.707106781186485,0.)) ;
#66170 = DIRECTION('ref_axis',(0.707106781186485,-0.70710678118661,0.)) ;
#66171 = DIRECTION('',(0.,1.,0.)) ;
#66172 = DIRECTION('center_axis',(0.,-1.,0.)) ;
#66173 = DIRECTION('ref_axis',(0.707106781186548,0.,-0.707106781186548)) ;
#66174 = DIRECTION('center_axis',(-0.70710678118661,0.707106781186485,0.)) ;
#66175 = DIRECTION('ref_axis',(0.707106781186485,0.70710678118661,0.)) ;
#66176 = DIRECTION('center_axis',(1.,0.,0.)) ;
#66177 = DIRECTION('ref_axis',(0.,0.707106781186736,-0.707106781186359)) ;
#66178 = DIRECTION('',(1.,0.,0.)) ;
#66179 = DIRECTION('center_axis',(1.32407757812447E-14,1.,0.)) ;
#66180 = DIRECTION('ref_axis',(-0.707106781186485,9.36264234308791E-15,-0.70710678118661)) ;
#66181 = DIRECTION('',(1.32407757812447E-14,1.,0.)) ;
#66182 = DIRECTION('center_axis',(0.,-1.,0.)) ;
#66183 = DIRECTION('ref_axis',(-1.,0.,0.)) ;
#66184 = DIRECTION('center_axis',(-0.70710678118661,0.707106781186485,0.)) ;
#66185 = DIRECTION('ref_axis',(-0.707106781186485,-0.70710678118661,0.)) ;
#66186 = DIRECTION('center_axis',(-1.,-2.61228946970635E-14,0.)) ;
#66187 = DIRECTION('ref_axis',(1.84716759845141E-14,-0.707106781186485,-0.70710678118661)) ;
#66188 = DIRECTION('center_axis',(-0.558292910464982,0.82964391525795,4.95863714946571E-14)) ;
#66189 = DIRECTION('ref_axis',(0.82964391525795,0.558292910464982,3.3368194657995E-14)) ;
#66190 = DIRECTION('',(-1.,-2.61228946970635E-14,0.)) ;
#66191 = DIRECTION('center_axis',(0.376618052248709,0.926368632197998,0.)) ;
#66192 = DIRECTION('ref_axis',(-0.655041541705793,0.266309178662365,-0.707106781186459)) ;
#66193 = DIRECTION('center_axis',(1.,-6.69008052953881E-14,0.)) ;
#66194 = DIRECTION('ref_axis',(-6.69008052953881E-14,-1.,0.)) ;
#66195 = DIRECTION('center_axis',(0.376618052248766,-0.926368632197974,0.)) ;
#66196 = DIRECTION('ref_axis',(0.655041541705581,0.266309178662326,-0.70710678118667)) ;
#66197 = DIRECTION('center_axis',(-0.558292910465075,-0.829643915257887,0.)) ;
#66198 = DIRECTION('ref_axis',(-0.829643915257887,0.558292910465075,0.)) ;
#66199 = DIRECTION('center_axis',(-1.,-2.61228946970635E-14,0.)) ;
#66200 = DIRECTION('ref_axis',(1.84716759845206E-14,-0.707106781186736,-0.707106781186359)) ;
#66201 = DIRECTION('center_axis',(-0.70710678118661,-0.707106781186485,0.)) ;
#66202 = DIRECTION('ref_axis',(0.707106781186485,-0.70710678118661,0.)) ;
#66203 = DIRECTION('center_axis',(0.846331659376499,0.532656289118059,0.)) ;
#66204 = DIRECTION('ref_axis',(-0.376644874076998,0.598446855477916,-0.70710678118663)) ;
#66205 = DIRECTION('center_axis',(-0.846331659376493,-0.53265628911807,0.)) ;
#66206 = DIRECTION('ref_axis',(-0.53265628911807,0.846331659376493,0.)) ;
#66207 = DIRECTION('center_axis',(-0.846331659376477,-0.532656289118094,0.)) ;
#66208 = DIRECTION('ref_axis',(-0.376644874077023,0.598446855477901,-0.70710678118663)) ;
#66209 = DIRECTION('center_axis',(0.,0.,-1.)) ;
#66210 = DIRECTION('ref_axis',(-1.,0.,0.)) ;
#66211 = DIRECTION('center_axis',(0.,1.,0.)) ;
#66212 = DIRECTION('ref_axis',(1.,0.,0.)) ;
#66213 = DIRECTION('center_axis',(-8.82718385416297E-15,-1.,0.)) ;
#66214 = DIRECTION('ref_axis',(0.707106781186548,-6.24176156205904E-15,-0.707106781186548)) ;
#66215 = DIRECTION('center_axis',(0.,0.,1.)) ;
#66216 = DIRECTION('ref_axis',(1.,0.,0.)) ;
#66217 = DIRECTION('center_axis',(0.846331659376392,0.53265628911823,0.)) ;
#66218 = DIRECTION('ref_axis',(0.53265628911823,-0.846331659376392,0.)) ;
#66219 = DIRECTION('center_axis',(0.,0.,1.)) ;
#66220 = DIRECTION('ref_axis',(0.483396168210882,0.875401704681363,0.)) ;
#66221 = DIRECTION('center_axis',(-0.846331659376486,-0.532656289118079,0.)) ;
#66222 = DIRECTION('ref_axis',(0.376644874077126,-0.598446855478087,-0.707106781186417)) ;
#66223 = DIRECTION('center_axis',(-0.846331659376477,-0.532656289118094,0.)) ;
#66224 = DIRECTION('ref_axis',(0.376644874077136,-0.598446855478081,-0.707106781186417)) ;
#66225 = DIRECTION('',(-0.846331659376486,-0.532656289118079,0.)) ;
#66226 = DIRECTION('center_axis',(-0.532656289118079,0.846331659376486,0.)) ;
#66227 = DIRECTION('ref_axis',(-0.846331659376486,-0.532656289118079,0.)) ;
#66228 = DIRECTION('',(0.,0.,1.)) ;
#66229 = DIRECTION('',(0.,0.,1.)) ;
#66230 = DIRECTION('center_axis',(0.,0.,1.)) ;
#66231 = DIRECTION('ref_axis',(-0.532656289118115,0.846331659376464,0.)) ;
#66232 = DIRECTION('',(0.,0.,1.)) ;
#66233 = DIRECTION('center_axis',(1.,-1.32407757812447E-14,0.)) ;
#66234 = DIRECTION('ref_axis',(1.32407757812447E-14,1.,0.)) ;
#66235 = DIRECTION('',(0.,0.,1.)) ;
#66236 = DIRECTION('center_axis',(-2.61228946970635E-14,1.,0.)) ;
#66237 = DIRECTION('ref_axis',(-1.,-2.61228946970635E-14,0.)) ;
#66238 = DIRECTION('center_axis',(-0.532656289118094,0.846331659376477,0.)) ;
#66239 = DIRECTION('ref_axis',(-0.598446855478002,-0.376644874077087,-0.70710678118651)) ;
#66240 = DIRECTION('center_axis',(0.221801981400932,0.975091729555031,1.96999733327036E-14)) ;
#66241 = DIRECTION('ref_axis',(0.97509172955503,-0.221801981400932,1.96999733327025E-14)) ;
#66242 = DIRECTION('',(-0.532656289118094,0.846331659376477,0.)) ;
#66243 = DIRECTION('center_axis',(0.975091729555058,-0.221801981400812,0.)) ;
#66244 = DIRECTION('ref_axis',(-0.221801981400812,-0.975091729555058,0.)) ;
#66245 = DIRECTION('center_axis',(-1.32407757812447E-14,-1.,0.)) ;
#66246 = DIRECTION('ref_axis',(0.707106781186548,-9.36264234308873E-15,-0.707106781186548)) ;
#66247 = DIRECTION('',(-1.32407757812447E-14,-1.,0.)) ;
#66248 = DIRECTION('center_axis',(0.,1.,0.)) ;
#66249 = DIRECTION('ref_axis',(1.,0.,0.)) ;
#66250 = DIRECTION('center_axis',(0.70710678118661,-0.707106781186485,0.)) ;
#66251 = DIRECTION('ref_axis',(0.707106781186485,0.70710678118661,0.)) ;
#66252 = DIRECTION('center_axis',(1.,2.61228946970635E-14,0.)) ;
#66253 = DIRECTION('ref_axis',(-1.84716759845141E-14,0.707106781186485,-0.70710678118661)) ;
#66254 = DIRECTION('center_axis',(0.558292910464982,-0.82964391525795,0.)) ;
#66255 = DIRECTION('ref_axis',(-0.82964391525795,-0.558292910464982,0.)) ;
#66256 = DIRECTION('center_axis',(-0.376618052248709,-0.926368632197998,0.)) ;
#66257 = DIRECTION('ref_axis',(0.655041541705652,-0.266309178662307,-0.707106781186612)) ;
#66258 = DIRECTION('center_axis',(-1.,3.3450402647694E-14,-8.88178419700124E-14)) ;
#66259 = DIRECTION('ref_axis',(3.34504026476972E-14,1.,-3.61091702428531E-14)) ;
#66260 = DIRECTION('center_axis',(-0.376618052248766,0.926368632197974,0.)) ;
#66261 = DIRECTION('ref_axis',(-0.655041541705635,-0.266309178662348,-0.707106781186612)) ;
#66262 = DIRECTION('center_axis',(0.558292910465098,0.829643915257871,0.)) ;
#66263 = DIRECTION('ref_axis',(0.829643915257871,-0.558292910465098,0.)) ;
#66264 = DIRECTION('center_axis',(1.,2.61228946970635E-14,0.)) ;
#66265 = DIRECTION('ref_axis',(-1.84716759845206E-14,0.707106781186736,-0.707106781186359)) ;
#66266 = DIRECTION('center_axis',(0.70710678118661,0.707106781186485,0.)) ;
#66267 = DIRECTION('ref_axis',(-0.707106781186485,0.70710678118661,0.)) ;
#66268 = DIRECTION('center_axis',(0.,0.,1.)) ;
#66269 = DIRECTION('ref_axis',(1.,0.,0.)) ;
#66270 = DIRECTION('center_axis',(-0.846331659376392,-0.53265628911823,0.)) ;
#66271 = DIRECTION('ref_axis',(-0.53265628911823,0.846331659376392,0.)) ;
#66272 = DIRECTION('center_axis',(0.,0.,1.)) ;
#66273 = DIRECTION('ref_axis',(-0.483396168210882,-0.875401704681363,0.)) ;
#66274 = DIRECTION('center_axis',(0.846331659376489,0.532656289118076,0.)) ;
#66275 = DIRECTION('ref_axis',(-0.376644874077123,0.598446855478089,-0.707106781186417)) ;
#66276 = DIRECTION('',(0.846331659376489,0.532656289118076,0.)) ;
#66277 = DIRECTION('center_axis',(-0.846331659376502,-0.532656289118055,0.)) ;
#66278 = DIRECTION('ref_axis',(0.376644874076995,-0.598446855477918,-0.70710678118663)) ;
#66279 = DIRECTION('',(-0.846331659376502,-0.532656289118055,0.)) ;
#66280 = DIRECTION('center_axis',(0.846331659376493,0.53265628911807,0.)) ;
#66281 = DIRECTION('ref_axis',(0.53265628911807,-0.846331659376493,0.)) ;
#66282 = DIRECTION('center_axis',(0.,0.,-1.)) ;
#66283 = DIRECTION('ref_axis',(-1.,0.,0.)) ;
#66284 = DIRECTION('center_axis',(0.,-1.,0.)) ;
#66285 = DIRECTION('ref_axis',(-1.,0.,0.)) ;
#66286 = DIRECTION('center_axis',(8.82718385416297E-15,1.,0.)) ;
#66287 = DIRECTION('ref_axis',(-0.707106781186548,6.24176156205904E-15,-0.707106781186548)) ;
#66288 = DIRECTION('center_axis',(-0.532656289118055,0.846331659376502,0.)) ;
#66289 = DIRECTION('ref_axis',(-0.846331659376502,-0.532656289118055,0.)) ;
#66290 = DIRECTION('',(0.,0.,1.)) ;
#66291 = DIRECTION('center_axis',(0.846331659376477,0.532656289118094,0.)) ;
#66292 = DIRECTION('ref_axis',(-0.532656289118094,0.846331659376477,0.)) ;
#66293 = DIRECTION('',(0.,0.,1.)) ;
#66294 = DIRECTION('center_axis',(0.532656289118076,-0.846331659376489,0.)) ;
#66295 = DIRECTION('ref_axis',(0.846331659376489,0.532656289118076,0.)) ;
#66296 = DIRECTION('',(0.,0.,1.)) ;
#66297 = DIRECTION('center_axis',(0.,0.,1.)) ;
#66298 = DIRECTION('ref_axis',(0.532656289118115,-0.846331659376464,0.)) ;
#66299 = DIRECTION('',(0.,0.,1.)) ;
#66300 = DIRECTION('center_axis',(-1.,1.32407757812447E-14,0.)) ;
#66301 = DIRECTION('ref_axis',(-1.32407757812447E-14,-1.,0.)) ;
#66302 = DIRECTION('center_axis',(-0.846331659376477,-0.532656289118094,0.)) ;
#66303 = DIRECTION('ref_axis',(0.532656289118094,-0.846331659376477,0.)) ;
#66304 = DIRECTION('center_axis',(1.,0.,0.)) ;
#66305 = DIRECTION('ref_axis',(0.,1.,0.)) ;
#66306 = DIRECTION('',(0.,0.,1.)) ;
#66307 = DIRECTION('center_axis',(0.,-1.,0.)) ;
#66308 = DIRECTION('ref_axis',(1.,0.,0.)) ;
#66309 = DIRECTION('center_axis',(0.,1.,0.)) ;
#66310 = DIRECTION('ref_axis',(-1.,0.,0.)) ;
#66311 = DIRECTION('center_axis',(0.42261826174069,0.906307787036654,0.)) ;
#66312 = DIRECTION('ref_axis',(-0.906307787036654,0.42261826174069,0.)) ;
#66313 = DIRECTION('center_axis',(0.,-1.,0.)) ;
#66314 = DIRECTION('ref_axis',(1.,0.,0.)) ;
#66315 = DIRECTION('center_axis',(2.46519032881572E-32,8.55284707229503E-50,
-1.)) ;
#66316 = DIRECTION('ref_axis',(1.,-2.20382687031672E-110,2.46519032881572E-32)) ;
#66317 = DIRECTION('',(1.,0.,2.46519032881572E-32)) ;
#66318 = DIRECTION('',(-3.67742382159233E-14,-1.,0.)) ;
#66319 = DIRECTION('center_axis',(0.,0.,-1.)) ;
#66320 = DIRECTION('ref_axis',(1.,0.,0.)) ;
#66321 = DIRECTION('',(1.,0.,0.)) ;
#66322 = DIRECTION('center_axis',(0.,0.,-1.)) ;
#66323 = DIRECTION('ref_axis',(0.945182639171645,-0.326542154412755,0.)) ;
#66324 = DIRECTION('',(0.,-1.,0.)) ;
#66325 = DIRECTION('center_axis',(0.,0.,-1.)) ;
#66326 = DIRECTION('ref_axis',(0.99891280361996,0.0466177086965058,0.)) ;
#66327 = DIRECTION('',(0.,-1.,0.)) ;
#66328 = DIRECTION('',(-1.,0.,0.)) ;
#66329 = DIRECTION('center_axis',(1.,0.,0.)) ;
#66330 = DIRECTION('ref_axis',(0.,-1.,0.)) ;
#66331 = DIRECTION('',(0.,0.,-1.)) ;
#66332 = DIRECTION('center_axis',(0.,0.,-1.)) ;
#66333 = DIRECTION('ref_axis',(-0.819152044288993,-0.573576436351044,0.)) ;
#66334 = DIRECTION('',(0.,0.,-1.)) ;
#66335 = DIRECTION('center_axis',(-3.21481891221798E-49,-2.25104043631415E-49,
-1.)) ;
#66336 = DIRECTION('ref_axis',(-0.819152044288993,-0.573576436351044,3.92456923550545E-49)) ;
#66337 = DIRECTION('center_axis',(1.,-1.46896958313692E-15,0.)) ;
#66338 = DIRECTION('ref_axis',(-1.46896958313692E-15,-1.,9.70774749479708E-52)) ;
#66339 = DIRECTION('',(0.,0.,-1.)) ;
#66340 = DIRECTION('',(-1.46896958313692E-15,-1.,9.70774749479708E-52)) ;
#66341 = DIRECTION('center_axis',(0.,0.,-1.)) ;
#66342 = DIRECTION('ref_axis',(0.,1.,0.)) ;
#66343 = DIRECTION('',(0.,0.,-1.)) ;
#66344 = DIRECTION('center_axis',(0.,0.,-1.)) ;
#66345 = DIRECTION('ref_axis',(0.,1.,0.)) ;
#66346 = DIRECTION('center_axis',(4.35522519302374E-15,1.,0.)) ;
#66347 = DIRECTION('ref_axis',(1.,-4.35522519302374E-15,-1.99220223446153E-34)) ;
#66348 = DIRECTION('',(0.,0.,-1.)) ;
#66349 = DIRECTION('',(1.,-4.35522519302374E-15,-1.99220223446153E-34)) ;
#66350 = DIRECTION('center_axis',(1.,0.,0.)) ;
#66351 = DIRECTION('ref_axis',(0.,-1.,5.60383084497476E-34)) ;
#66352 = DIRECTION('',(0.,0.,-1.)) ;
#66353 = DIRECTION('',(0.,-1.,5.60383084497476E-34)) ;
#66354 = DIRECTION('center_axis',(0.,1.,0.)) ;
#66355 = DIRECTION('ref_axis',(1.,0.,0.)) ;
#66356 = DIRECTION('',(0.,0.,-1.)) ;
#66357 = DIRECTION('',(-1.,0.,0.)) ;
#66358 = DIRECTION('center_axis',(-8.11022789614398E-33,1.15826058041052E-32,
-1.)) ;
#66359 = DIRECTION('ref_axis',(1.,-2.17980433592234E-81,-8.11022789614398E-33)) ;
#66360 = DIRECTION('',(8.07434927000127E-15,1.,9.03922915636472E-64)) ;
#66361 = DIRECTION('center_axis',(-6.80308557388104E-64,1.462910905831E-62,
-1.)) ;
#66362 = DIRECTION('ref_axis',(-1.06581410364006E-13,-1.,-1.46291090583099E-62)) ;
#66363 = DIRECTION('center_axis',(0.,0.,-1.)) ;
#66364 = DIRECTION('ref_axis',(-1.06581410364006E-13,-1.,0.)) ;
#66365 = DIRECTION('',(0.,0.,-1.)) ;
#66366 = DIRECTION('center_axis',(-6.80308557388104E-64,1.462910905831E-62,
-1.)) ;
#66367 = DIRECTION('ref_axis',(-1.06581410364006E-13,-1.,-1.46291090583099E-62)) ;
#66368 = DIRECTION('center_axis',(-1.,8.07434927000127E-15,0.)) ;
#66369 = DIRECTION('ref_axis',(8.07434927000127E-15,1.,9.03922915636472E-64)) ;
#66370 = DIRECTION('',(0.,0.,-1.)) ;
#66371 = DIRECTION('',(8.07434927000127E-15,1.,9.03922915636472E-64)) ;
#66372 = DIRECTION('center_axis',(-1.,-1.30614473485314E-15,0.)) ;
#66373 = DIRECTION('ref_axis',(-1.30614473485314E-15,1.,0.)) ;
#66374 = DIRECTION('',(0.,0.,-1.)) ;
#66375 = DIRECTION('center_axis',(0.,1.,0.)) ;
#66376 = DIRECTION('ref_axis',(1.,0.,0.)) ;
#66377 = DIRECTION('center_axis',(1.,1.34572487833352E-15,0.)) ;
#66378 = DIRECTION('ref_axis',(1.34572487833352E-15,-1.,0.)) ;
#66379 = DIRECTION('',(0.,0.,-1.)) ;
#66380 = DIRECTION('',(1.34572487833352E-15,-1.,0.)) ;
#66381 = DIRECTION('',(0.,0.,-1.)) ;
#66382 = DIRECTION('center_axis',(1.,0.,0.)) ;
#66383 = DIRECTION('ref_axis',(0.,1.,0.)) ;
#66384 = DIRECTION('',(0.,1.,0.)) ;
#66385 = DIRECTION('',(0.,0.,1.)) ;
#66386 = DIRECTION('center_axis',(1.97372982155583E-14,1.,0.)) ;
#66387 = DIRECTION('ref_axis',(-1.,1.97372982155583E-14,0.)) ;
#66388 = DIRECTION('',(-1.,1.97372982155583E-14,0.)) ;
#66389 = DIRECTION('',(0.,0.,1.)) ;
#66390 = DIRECTION('center_axis',(-1.,-7.40148683083432E-15,0.)) ;
#66391 = DIRECTION('ref_axis',(7.40148683083432E-15,-1.,0.)) ;
#66392 = DIRECTION('',(7.40148683083432E-15,-1.,0.)) ;
#66393 = DIRECTION('center_axis',(0.,0.,-1.)) ;
#66394 = DIRECTION('ref_axis',(1.,0.,0.)) ;
#66395 = DIRECTION('center_axis',(6.22031196910783E-15,1.,0.)) ;
#66396 = DIRECTION('ref_axis',(-1.,6.22031196910783E-15,0.)) ;
#66397 = DIRECTION('',(1.,-9.87859509815899E-15,0.)) ;
#66398 = DIRECTION('',(0.,0.,1.)) ;
#66399 = DIRECTION('',(-1.,6.22031196910783E-15,0.)) ;
#66400 = DIRECTION('',(0.,0.,1.)) ;
#66401 = DIRECTION('center_axis',(0.,0.,1.)) ;
#66402 = DIRECTION('ref_axis',(1.,0.,0.)) ;
#66403 = DIRECTION('',(0.,0.,1.)) ;
#66404 = DIRECTION('center_axis',(0.,0.,1.)) ;
#66405 = DIRECTION('ref_axis',(1.,0.,0.)) ;
#66406 = DIRECTION('',(0.,0.,1.)) ;
#66407 = DIRECTION('center_axis',(-1.,-2.22044604925032E-15,0.)) ;
#66408 = DIRECTION('ref_axis',(2.22044604925032E-15,-1.,0.)) ;
#66409 = DIRECTION('',(2.22044604925032E-15,-1.,0.)) ;
#66410 = DIRECTION('center_axis',(1.,1.11022302462516E-14,0.)) ;
#66411 = DIRECTION('ref_axis',(-1.11022302462516E-14,1.,0.)) ;
#66412 = DIRECTION('',(-1.11022302462516E-14,1.,0.)) ;
#66413 = DIRECTION('center_axis',(0.,0.,-1.)) ;
#66414 = DIRECTION('ref_axis',(1.,0.,0.)) ;
#66415 = DIRECTION('center_axis',(0.,0.,-1.)) ;
#66416 = DIRECTION('ref_axis',(-0.180669743412801,-0.983543818960372,0.)) ;
#66417 = DIRECTION('',(0.,0.,1.)) ;
#66418 = DIRECTION('center_axis',(0.,0.,-1.)) ;
#66419 = DIRECTION('ref_axis',(-0.180669743412801,-0.983543818960372,0.)) ;
#66420 = DIRECTION('center_axis',(1.37008135359091E-15,0.316227766016839,
-0.948683298050513)) ;
#66421 = DIRECTION('ref_axis',(-1.,2.21856832751295E-31,-1.44419255235793E-15)) ;
#66422 = DIRECTION('center_axis',(0.,0.,1.)) ;
#66423 = DIRECTION('ref_axis',(1.,0.,0.)) ;
#66424 = DIRECTION('center_axis',(0.,0.,1.)) ;
#66425 = DIRECTION('ref_axis',(1.,0.,0.)) ;
#66426 = DIRECTION('',(0.693108716251782,0.720833064901858,0.)) ;
#66427 = DIRECTION('center_axis',(0.,0.,-1.)) ;
#66428 = DIRECTION('ref_axis',(1.,0.,0.)) ;
#66429 = DIRECTION('',(-0.707106781186547,0.707106781186547,0.)) ;
#66430 = DIRECTION('',(0.693108716251782,0.720833064901858,0.)) ;
#66431 = DIRECTION('',(-1.,0.,0.)) ;
#66432 = DIRECTION('center_axis',(0.707106781186548,0.707106781186548,0.)) ;
#66433 = DIRECTION('ref_axis',(0.,0.,-1.)) ;
#66434 = DIRECTION('center_axis',(0.,0.,1.)) ;
#66435 = DIRECTION('ref_axis',(-0.707106781186563,-0.707106781186532,0.)) ;
#66436 = DIRECTION('',(0.,0.,1.)) ;
#66437 = DIRECTION('center_axis',(0.,0.,1.)) ;
#66438 = DIRECTION('ref_axis',(-0.707106781186563,-0.707106781186532,0.)) ;
#66439 = DIRECTION('center_axis',(0.,1.,0.)) ;
#66440 = DIRECTION('ref_axis',(-1.,0.,0.)) ;
#66441 = DIRECTION('',(-1.,0.,0.)) ;
#66442 = DIRECTION('center_axis',(0.,0.,-1.)) ;
#66443 = DIRECTION('ref_axis',(0.707106781186555,-0.70710678118654,0.)) ;
#66444 = DIRECTION('',(0.,0.,-1.)) ;
#66445 = DIRECTION('center_axis',(0.720833064901858,-0.693108716251782,0.)) ;
#66446 = DIRECTION('ref_axis',(0.,0.,-1.)) ;
#66447 = DIRECTION('center_axis',(-1.,0.,0.)) ;
#66448 = DIRECTION('ref_axis',(0.,1.,0.)) ;
#66449 = DIRECTION('',(0.,0.,-1.)) ;
#66450 = DIRECTION('center_axis',(0.,-1.,0.)) ;
#66451 = DIRECTION('ref_axis',(-1.,0.,0.)) ;
#66452 = DIRECTION('center_axis',(0.,-1.,0.)) ;
#66453 = DIRECTION('ref_axis',(-1.,0.,0.)) ;
#66454 = DIRECTION('center_axis',(-0.70710678118655,-8.10370301256138E-15,
-0.707106781186545)) ;
#66455 = DIRECTION('ref_axis',(-0.707106781186545,-1.02766135666342E-31,0.70710678118655)) ;
#66456 = DIRECTION('center_axis',(0.,1.,0.)) ;
#66457 = DIRECTION('ref_axis',(-0.707106781186554,0.,-0.707106781186541)) ;
#66458 = DIRECTION('',(0.,1.,0.)) ;
#66459 = DIRECTION('center_axis',(0.,-0.901303236306861,-0.433188730489123)) ;
#66460 = DIRECTION('ref_axis',(0.,-0.433188730489123,0.901303236306861)) ;
#66461 = DIRECTION('center_axis',(0.234832610329562,-0.891105237687952,-0.388310572211089)) ;
#66462 = DIRECTION('ref_axis',(0.461132845926743,0.453796711496567,-0.762512323206913)) ;
#66463 = DIRECTION('center_axis',(-0.186041819180148,0.98254182685326,0.)) ;
#66464 = DIRECTION('ref_axis',(0.,0.,-1.)) ;
#66465 = DIRECTION('center_axis',(1.,0.,0.)) ;
#66466 = DIRECTION('ref_axis',(0.,0.780868809443035,-0.624695047554418)) ;
#66467 = DIRECTION('center_axis',(0.117465545166938,-0.620370257876694,-0.77546282234588)) ;
#66468 = DIRECTION('ref_axis',(0.98254182685326,0.186041819180148,-2.37800624313497E-16)) ;
#66469 = DIRECTION('center_axis',(0.,0.,1.)) ;
#66470 = DIRECTION('ref_axis',(1.,0.,0.)) ;
#66471 = DIRECTION('center_axis',(0.,0.,1.)) ;
#66472 = DIRECTION('ref_axis',(0.998912803619959,0.0466177086965058,0.)) ;
#66473 = DIRECTION('center_axis',(1.,0.,0.)) ;
#66474 = DIRECTION('ref_axis',(0.,0.,-1.)) ;
#66475 = DIRECTION('center_axis',(-1.,0.,0.)) ;
#66476 = DIRECTION('ref_axis',(0.,0.433188730489175,-0.901303236306837)) ;
#66477 = DIRECTION('',(1.,0.,0.)) ;
#66478 = DIRECTION('center_axis',(0.503932575563369,0.863742993769599,0.)) ;
#66479 = DIRECTION('ref_axis',(0.,0.,-1.)) ;
#66480 = DIRECTION('center_axis',(-0.527005614249989,-0.600943043286542,-0.60094304328655)) ;
#66481 = DIRECTION('ref_axis',(-0.751844328927355,0.65934065934066,8.09346471661972E-17)) ;
#66482 = DIRECTION('center_axis',(0.,0.,1.)) ;
#66483 = DIRECTION('ref_axis',(1.,0.,0.)) ;
#66484 = DIRECTION('center_axis',(0.,-1.,0.)) ;
#66485 = DIRECTION('ref_axis',(-1.,0.,0.)) ;
#66486 = DIRECTION('center_axis',(0.,0.,1.)) ;
#66487 = DIRECTION('ref_axis',(0.945182639171645,-0.326542154412755,0.)) ;
#66488 = DIRECTION('center_axis',(0.,1.,0.)) ;
#66489 = DIRECTION('ref_axis',(-0.707106781186554,0.,-0.707106781186541)) ;
#66490 = DIRECTION('',(0.,1.,0.)) ;
#66491 = DIRECTION('center_axis',(-1.,0.,0.)) ;
#66492 = DIRECTION('ref_axis',(0.,-0.382683432365103,0.923879532511281)) ;
#66493 = DIRECTION('center_axis',(0.234832610329551,-0.891105237687967,-0.388310572211061)) ;
#66494 = DIRECTION('ref_axis',(0.461132845926749,0.453796711496559,-0.762512323206914)) ;
#66495 = DIRECTION('center_axis',(-0.186041819180008,0.982541826853286,0.)) ;
#66496 = DIRECTION('ref_axis',(0.,0.,-1.)) ;
#66497 = DIRECTION('center_axis',(0.117465545166847,-0.620370257876695,-0.775462822345893)) ;
#66498 = DIRECTION('ref_axis',(0.982541826853286,0.186041819180008,1.81771110290286E-17)) ;
#66499 = DIRECTION('center_axis',(0.424264068711907,-0.565685424949239,-0.70710678118656)) ;
#66500 = DIRECTION('ref_axis',(6.96661453349048E-17,0.780868809443035,-0.624695047554418)) ;
#66501 = DIRECTION('center_axis',(0.,0.529998940003177,-0.84799830400509)) ;
#66502 = DIRECTION('ref_axis',(0.,0.84799830400509,0.529998940003177)) ;
#66503 = DIRECTION('center_axis',(-0.42426406871193,0.565685424949236,0.707106781186548)) ;
#66504 = DIRECTION('ref_axis',(0.466804319685465,0.805744406458676,-0.364512933355658)) ;
#66505 = DIRECTION('',(0.42426406871193,-0.565685424949236,-0.707106781186548)) ;
#66506 = DIRECTION('center_axis',(0.,0.,1.)) ;
#66507 = DIRECTION('ref_axis',(1.,0.,0.)) ;
#66508 = DIRECTION('center_axis',(0.,0.,1.)) ;
#66509 = DIRECTION('ref_axis',(0.999082519440321,-0.0428266196282222,0.)) ;
#66510 = DIRECTION('center_axis',(0.,-1.,0.)) ;
#66511 = DIRECTION('ref_axis',(-1.,0.,0.)) ;
#66512 = DIRECTION('center_axis',(-0.503932575563422,0.863742993769568,6.1372630978665E-14)) ;
#66513 = DIRECTION('ref_axis',(0.863742993769568,0.503932575563422,6.75875089903394E-31)) ;
#66514 = DIRECTION('center_axis',(0.527005614249974,-0.600943043286547,-0.600943043286559)) ;
#66515 = DIRECTION('ref_axis',(-3.7754359406558E-16,0.707106781186554,-0.707106781186541)) ;
#66516 = DIRECTION('center_axis',(0.,-1.,0.)) ;
#66517 = DIRECTION('ref_axis',(0.707106781186554,0.,-0.707106781186541)) ;
#66518 = DIRECTION('',(0.,-1.,0.)) ;
#66519 = DIRECTION('center_axis',(0.,1.,0.)) ;
#66520 = DIRECTION('ref_axis',(1.,0.,0.)) ;
#66521 = DIRECTION('center_axis',(0.,0.,1.)) ;
#66522 = DIRECTION('ref_axis',(1.,0.,0.)) ;
#66523 = DIRECTION('center_axis',(0.,0.,1.)) ;
#66524 = DIRECTION('ref_axis',(-0.945182639171645,-0.326542154412755,0.)) ;
#66525 = DIRECTION('center_axis',(0.,-0.74695627272243,0.664873165829855)) ;
#66526 = DIRECTION('ref_axis',(0.,-0.664873165829855,-0.74695627272243)) ;
#66527 = DIRECTION('center_axis',(0.503932575563377,0.863742993769594,0.)) ;
#66528 = DIRECTION('ref_axis',(0.,0.,-1.)) ;
#66529 = DIRECTION('center_axis',(-0.527005614249989,-0.600943043286542,-0.60094304328655)) ;
#66530 = DIRECTION('ref_axis',(-0.751844328927355,0.65934065934066,8.09346471661972E-17)) ;
#66531 = DIRECTION('center_axis',(0.,0.,1.)) ;
#66532 = DIRECTION('ref_axis',(1.,0.,0.)) ;
#66533 = DIRECTION('center_axis',(0.,-1.,0.)) ;
#66534 = DIRECTION('ref_axis',(-1.,0.,0.)) ;
#66535 = DIRECTION('center_axis',(0.,0.,1.)) ;
#66536 = DIRECTION('ref_axis',(0.945182639171645,-0.326542154412755,0.)) ;
#66537 = DIRECTION('center_axis',(0.,1.,0.)) ;
#66538 = DIRECTION('ref_axis',(-0.707106781186541,0.,-0.707106781186554)) ;
#66539 = DIRECTION('',(0.,1.,0.)) ;
#66540 = DIRECTION('center_axis',(-0.50393257556343,0.863742993769564,6.13726309786647E-14)) ;
#66541 = DIRECTION('ref_axis',(0.863742993769564,0.50393257556343,-3.71214407864697E-30)) ;
#66542 = DIRECTION('center_axis',(0.527005614249974,-0.600943043286547,-0.600943043286559)) ;
#66543 = DIRECTION('ref_axis',(-3.7754359406558E-16,0.707106781186554,-0.707106781186541)) ;
#66544 = DIRECTION('center_axis',(0.,-1.,0.)) ;
#66545 = DIRECTION('ref_axis',(0.707106781186541,0.,-0.707106781186554)) ;
#66546 = DIRECTION('',(0.,-1.,0.)) ;
#66547 = DIRECTION('center_axis',(0.,1.,0.)) ;
#66548 = DIRECTION('ref_axis',(1.,0.,0.)) ;
#66549 = DIRECTION('center_axis',(0.,0.,1.)) ;
#66550 = DIRECTION('ref_axis',(1.,0.,0.)) ;
#66551 = DIRECTION('center_axis',(0.,0.,1.)) ;
#66552 = DIRECTION('ref_axis',(-0.945182639171645,-0.326542154412755,0.)) ;
#66553 = DIRECTION('center_axis',(0.,-0.74695627272243,0.664873165829855)) ;
#66554 = DIRECTION('ref_axis',(0.,-0.664873165829855,-0.74695627272243)) ;
#66555 = DIRECTION('center_axis',(0.,-1.,0.)) ;
#66556 = DIRECTION('ref_axis',(0.707106781186541,0.,-0.707106781186554)) ;
#66557 = DIRECTION('center_axis',(0.,-1.,0.)) ;
#66558 = DIRECTION('ref_axis',(0.,0.,-1.)) ;
#66559 = DIRECTION('',(0.,-1.,0.)) ;
#66560 = DIRECTION('center_axis',(0.,1.,0.)) ;
#66561 = DIRECTION('ref_axis',(1.,0.,0.)) ;
#66562 = DIRECTION('center_axis',(0.,0.,1.)) ;
#66563 = DIRECTION('ref_axis',(1.,0.,0.)) ;
#66564 = DIRECTION('center_axis',(0.,0.,1.)) ;
#66565 = DIRECTION('ref_axis',(-0.999082519440321,-0.0428266196282222,0.)) ;
#66566 = DIRECTION('center_axis',(0.,0.,-1.)) ;
#66567 = DIRECTION('ref_axis',(0.985598559653495,0.169101978725727,0.)) ;
#66568 = DIRECTION('center_axis',(0.,1.,0.)) ;
#66569 = DIRECTION('ref_axis',(-0.707106781186548,0.,-0.707106781186548)) ;
#66570 = DIRECTION('',(0.,1.,0.)) ;
#66571 = DIRECTION('center_axis',(-2.61228946970624E-14,-1.,0.)) ;
#66572 = DIRECTION('ref_axis',(0.707106781186554,-1.84716759845151E-14,-0.707106781186541)) ;
#66573 = DIRECTION('center_axis',(0.,-1.,0.)) ;
#66574 = DIRECTION('ref_axis',(0.,0.,-1.)) ;
#66575 = DIRECTION('',(-2.61228946970624E-14,-1.,0.)) ;
#66576 = DIRECTION('center_axis',(0.,1.,0.)) ;
#66577 = DIRECTION('ref_axis',(1.,0.,0.)) ;
#66578 = DIRECTION('center_axis',(0.,0.,1.)) ;
#66579 = DIRECTION('ref_axis',(1.,0.,0.)) ;
#66580 = DIRECTION('center_axis',(0.,0.,1.)) ;
#66581 = DIRECTION('ref_axis',(-0.999082519440321,-0.0428266196282222,0.)) ;
#66582 = DIRECTION('center_axis',(-0.640000000000002,-0.479999999999999,-0.599999999999999)) ;
#66583 = DIRECTION('ref_axis',(-0.332851351149329,0.876990532021574,-0.346550984391306)) ;
#66584 = DIRECTION('center_axis',(0.,-1.,0.)) ;
#66585 = DIRECTION('ref_axis',(-0.729537204140087,0.,-0.683941128881328)) ;
#66586 = DIRECTION('',(-0.640000000000002,-0.479999999999999,-0.599999999999999)) ;
#66587 = DIRECTION('center_axis',(0.640000000000011,0.479999999999994,0.599999999999994)) ;
#66588 = DIRECTION('ref_axis',(-1.29788565499151E-16,0.780868809443031,-0.624695047554423)) ;
#66589 = DIRECTION('',(0.640000000000002,0.479999999999998,0.599999999999999)) ;
#66590 = DIRECTION('center_axis',(0.,0.529998940003175,-0.847998304005091)) ;
#66591 = DIRECTION('ref_axis',(0.,0.847998304005091,0.529998940003175)) ;
#66592 = DIRECTION('center_axis',(0.,-0.780868809443031,0.624695047554424)) ;
#66593 = DIRECTION('ref_axis',(8.66938531455285E-17,0.624695047554424,0.780868809443031)) ;
#66594 = DIRECTION('center_axis',(0.,0.,-1.)) ;
#66595 = DIRECTION('ref_axis',(0.985598559653489,0.169101978725763,0.)) ;
#66596 = DIRECTION('center_axis',(0.42426406871193,-0.565685424949232,-0.707106781186552)) ;
#66597 = DIRECTION('ref_axis',(-1.36184273839256E-16,0.780868809443035,-0.624695047554418)) ;
#66598 = DIRECTION('center_axis',(0.,0.529998940003175,-0.847998304005091)) ;
#66599 = DIRECTION('ref_axis',(0.,0.847998304005091,0.529998940003175)) ;
#66600 = DIRECTION('center_axis',(0.,-0.780868809443031,0.624695047554424)) ;
#66601 = DIRECTION('ref_axis',(0.,0.624695047554424,0.780868809443031)) ;
#66602 = DIRECTION('center_axis',(-0.424264068711912,0.565685424949242,0.707106781186554)) ;
#66603 = DIRECTION('ref_axis',(0.466804319685494,0.805744406458664,-0.364512933355647)) ;
#66604 = DIRECTION('center_axis',(0.,-1.,0.)) ;
#66605 = DIRECTION('ref_axis',(0.514495755427508,0.,-0.857492925712555)) ;
#66606 = DIRECTION('',(0.424264068711912,-0.565685424949242,-0.707106781186554)) ;
#66607 = DIRECTION('',(-0.424264068711912,0.565685424949242,0.707106781186554)) ;
#66608 = DIRECTION('center_axis',(-0.640000000000003,-0.479999999999997,-0.599999999999999)) ;
#66609 = DIRECTION('ref_axis',(-0.332851351149322,0.876990532021575,-0.346550984391311)) ;
#66610 = DIRECTION('',(-0.640000000000003,-0.479999999999997,-0.599999999999999)) ;
#66611 = DIRECTION('center_axis',(0.639999999999996,0.479999999999997,0.600000000000007)) ;
#66612 = DIRECTION('ref_axis',(4.28317217346062E-16,0.780868809443036,-0.624695047554418)) ;
#66613 = DIRECTION('',(0.640000000000003,0.479999999999997,0.599999999999999)) ;
#66614 = DIRECTION('center_axis',(0.,0.624695047554418,0.780868809443036)) ;
#66615 = DIRECTION('ref_axis',(0.,0.780868809443036,-0.624695047554418)) ;
#66616 = DIRECTION('center_axis',(0.,0.529998940003177,-0.84799830400509)) ;
#66617 = DIRECTION('ref_axis',(0.,0.84799830400509,0.529998940003177)) ;
#66618 = DIRECTION('center_axis',(0.,-0.780868809443031,0.624695047554423)) ;
#66619 = DIRECTION('ref_axis',(8.66938531455284E-17,0.624695047554423,0.780868809443031)) ;
#66620 = DIRECTION('center_axis',(0.,-0.624695047554423,-0.780868809443031)) ;
#66621 = DIRECTION('ref_axis',(-0.707106781186523,0.552157630374252,-0.441726104299401)) ;
#66622 = DIRECTION('',(0.,0.624695047554423,0.780868809443031)) ;
#66623 = DIRECTION('',(0.,-0.624695047554423,-0.780868809443031)) ;
#66624 = DIRECTION('center_axis',(-1.,0.,0.)) ;
#66625 = DIRECTION('ref_axis',(0.,1.,0.)) ;
#66626 = DIRECTION('',(0.,0.,-1.)) ;
#66627 = DIRECTION('',(0.,0.,-1.)) ;
#66628 = DIRECTION('center_axis',(0.,0.,-1.)) ;
#66629 = DIRECTION('ref_axis',(1.,0.,0.)) ;
#66630 = DIRECTION('',(0.,0.,-1.)) ;
#66631 = DIRECTION('center_axis',(1.,0.,0.)) ;
#66632 = DIRECTION('ref_axis',(0.,-1.,0.)) ;
#66633 = DIRECTION('',(0.,0.,-1.)) ;
#66634 = DIRECTION('center_axis',(0.,0.,-1.)) ;
#66635 = DIRECTION('ref_axis',(0.948683298050519,0.316227766016821,0.)) ;
#66636 = DIRECTION('',(0.,0.,1.)) ;
#66637 = DIRECTION('center_axis',(0.799999999999998,0.600000000000002,0.)) ;
#66638 = DIRECTION('ref_axis',(0.,0.,-1.)) ;
#66639 = DIRECTION('center_axis',(0.,0.780868809443031,-0.624695047554423)) ;
#66640 = DIRECTION('ref_axis',(-1.,0.,0.)) ;
#66641 = DIRECTION('center_axis',(0.,0.,-1.)) ;
#66642 = DIRECTION('ref_axis',(1.,-7.1054273576004E-14,0.)) ;
#66643 = DIRECTION('center_axis',(1.95689141014107E-45,1.96585022416868E-45,
-1.)) ;
#66644 = DIRECTION('ref_axis',(1.,-7.1054273576004E-14,1.95689141014093E-45)) ;
#66645 = DIRECTION('center_axis',(0.,0.,-1.)) ;
#66646 = DIRECTION('ref_axis',(1.,0.,0.)) ;
#66647 = DIRECTION('',(0.,0.,1.)) ;
#66648 = DIRECTION('',(0.,0.,-1.)) ;
#66649 = DIRECTION('center_axis',(0.,0.,-1.)) ;
#66650 = DIRECTION('ref_axis',(1.,0.,0.)) ;
#66651 = DIRECTION('',(0.,0.,-1.)) ;
#66652 = DIRECTION('',(0.,0.,-1.)) ;
#66653 = DIRECTION('center_axis',(-1.,3.17206578464333E-15,0.)) ;
#66654 = DIRECTION('ref_axis',(3.17206578464333E-15,1.,-1.76085023486835E-33)) ;
#66655 = DIRECTION('',(0.,0.,1.)) ;
#66656 = DIRECTION('',(0.,0.,-1.)) ;
#66657 = DIRECTION('',(-3.17206578464333E-15,-1.,6.60793205057061E-32)) ;
#66658 = DIRECTION('center_axis',(0.,0.,-1.)) ;
#66659 = DIRECTION('ref_axis',(0.,1.,0.)) ;
#66660 = DIRECTION('center_axis',(-3.83260058933034E-30,-6.60793205056939E-32,
-1.)) ;
#66661 = DIRECTION('ref_axis',(-2.53255642712671E-61,1.,-6.60793205056939E-32)) ;
#66662 = DIRECTION('',(0.,0.,-1.)) ;
#66663 = DIRECTION('center_axis',(0.,-1.,0.)) ;
#66664 = DIRECTION('ref_axis',(-1.,0.,3.83260058933034E-30)) ;
#66665 = DIRECTION('',(1.,0.,-3.83260058933034E-30)) ;
#66666 = DIRECTION('',(0.,0.,-1.)) ;
#66667 = DIRECTION('center_axis',(-1.,1.53134210293125E-15,0.)) ;
#66668 = DIRECTION('ref_axis',(1.53134210293125E-15,1.,-6.60793205056998E-32)) ;
#66669 = DIRECTION('',(-1.53134210293125E-15,-1.,6.60793205056998E-32)) ;
#66670 = DIRECTION('',(0.,0.,-1.)) ;
#66671 = DIRECTION('center_axis',(0.,0.,-1.)) ;
#66672 = DIRECTION('ref_axis',(0.,1.,0.)) ;
#66673 = DIRECTION('center_axis',(-3.83260058933034E-30,-6.60793205056939E-32,
-1.)) ;
#66674 = DIRECTION('ref_axis',(-2.53255642712671E-61,1.,-6.60793205056939E-32)) ;
#66675 = DIRECTION('',(0.,0.,-1.)) ;
#66676 = DIRECTION('center_axis',(0.,-1.,0.)) ;
#66677 = DIRECTION('ref_axis',(-1.,0.,-1.40067632319071E-31)) ;
#66678 = DIRECTION('',(1.,0.,-3.83260058933034E-30)) ;
#66679 = DIRECTION('',(0.,0.,-1.)) ;
#66680 = DIRECTION('center_axis',(0.,0.,-1.)) ;
#66681 = DIRECTION('ref_axis',(-1.,0.,0.)) ;
#66682 = DIRECTION('center_axis',(-3.83260058933034E-30,-6.60793205056939E-32,
-1.)) ;
#66683 = DIRECTION('ref_axis',(-1.,2.53255642712671E-61,3.83260058933034E-30)) ;
#66684 = DIRECTION('',(0.,0.,-1.)) ;
#66685 = DIRECTION('center_axis',(1.,0.,0.)) ;
#66686 = DIRECTION('ref_axis',(0.,-1.,1.41044871512355E-33)) ;
#66687 = DIRECTION('',(0.,1.,-6.60793205056939E-32)) ;
#66688 = DIRECTION('',(0.,0.,-1.)) ;
#66689 = DIRECTION('center_axis',(3.55271367880026E-13,-1.,0.)) ;
#66690 = DIRECTION('ref_axis',(-1.,-3.55271367880026E-13,3.80009837042949E-30)) ;
#66691 = DIRECTION('',(1.,3.55271367880026E-13,-3.83260058933036E-30)) ;
#66692 = DIRECTION('',(0.,0.,-1.)) ;
#66693 = DIRECTION('',(0.,0.,-1.)) ;
#66694 = DIRECTION('center_axis',(0.,-1.,0.)) ;
#66695 = DIRECTION('ref_axis',(-1.,0.,0.)) ;
#66696 = DIRECTION('',(0.,0.,-1.)) ;
#66697 = DIRECTION('',(-1.,0.,0.)) ;
#66698 = DIRECTION('center_axis',(0.,0.,-1.)) ;
#66699 = DIRECTION('ref_axis',(0.,1.,0.)) ;
#66700 = DIRECTION('',(0.,0.,-1.)) ;
#66701 = DIRECTION('center_axis',(6.125368411725E-15,-1.,0.)) ;
#66702 = DIRECTION('ref_axis',(-1.,-6.125368411725E-15,1.93235546378459E-35)) ;
#66703 = DIRECTION('',(0.,0.,-1.)) ;
#66704 = DIRECTION('center_axis',(-6.125368411725E-15,1.,0.)) ;
#66705 = DIRECTION('ref_axis',(-1.,-6.125368411725E-15,0.)) ;
#66706 = DIRECTION('center_axis',(0.,0.,-1.)) ;
#66707 = DIRECTION('ref_axis',(-1.,0.,0.)) ;
#66708 = DIRECTION('center_axis',(0.,0.,-1.)) ;
#66709 = DIRECTION('ref_axis',(1.,0.,0.)) ;
#66710 = DIRECTION('',(0.,0.,-1.)) ;
#66711 = DIRECTION('center_axis',(0.,0.,-1.)) ;
#66712 = DIRECTION('ref_axis',(1.,0.,0.)) ;
#66713 = DIRECTION('center_axis',(1.,-5.35505761538791E-15,0.)) ;
#66714 = DIRECTION('ref_axis',(-5.35505761538791E-15,-1.,1.48632706569949E-33)) ;
#66715 = DIRECTION('',(0.,0.,1.)) ;
#66716 = DIRECTION('',(0.,0.,-1.)) ;
#66717 = DIRECTION('',(5.35505761538791E-15,1.,0.)) ;
#66718 = DIRECTION('center_axis',(0.,0.,-1.)) ;
#66719 = DIRECTION('ref_axis',(-0.707106781186481,-0.707106781186614,0.)) ;
#66720 = DIRECTION('center_axis',(0.,0.,-1.)) ;
#66721 = DIRECTION('ref_axis',(-0.707106781186481,-0.707106781186614,0.)) ;
#66722 = DIRECTION('',(0.,0.,-1.)) ;
#66723 = DIRECTION('center_axis',(0.707106781186514,0.707106781186581,0.)) ;
#66724 = DIRECTION('ref_axis',(0.707106781186581,-0.707106781186514,0.)) ;
#66725 = DIRECTION('',(-0.707106781186581,0.707106781186514,0.)) ;
#66726 = DIRECTION('',(0.,0.,-1.)) ;
#66727 = DIRECTION('center_axis',(0.,0.,-1.)) ;
#66728 = DIRECTION('ref_axis',(0.,-1.,0.)) ;
#66729 = DIRECTION('center_axis',(0.,0.,-1.)) ;
#66730 = DIRECTION('ref_axis',(0.,-1.,0.)) ;
#66731 = DIRECTION('',(0.,0.,-1.)) ;
#66732 = DIRECTION('center_axis',(1.75071816546432E-14,1.,0.)) ;
#66733 = DIRECTION('ref_axis',(1.,-1.75071816546432E-14,-2.18941313571177E-49)) ;
#66734 = DIRECTION('',(-1.,1.75071816546432E-14,0.)) ;
#66735 = DIRECTION('',(0.,0.,-1.)) ;
#66736 = DIRECTION('center_axis',(0.,0.,-1.)) ;
#66737 = DIRECTION('ref_axis',(1.,0.,0.)) ;
#66738 = DIRECTION('center_axis',(2.46519032881571E-32,4.87512283120816E-48,
-1.)) ;
#66739 = DIRECTION('ref_axis',(1.,-1.2018105655283E-79,2.46519032881571E-32)) ;
#66740 = DIRECTION('',(0.,0.,-1.)) ;
#66741 = DIRECTION('',(0.,0.,-1.)) ;
#66742 = DIRECTION('center_axis',(-1.,0.,0.)) ;
#66743 = DIRECTION('ref_axis',(0.,1.,-1.76085023486835E-33)) ;
#66744 = DIRECTION('',(0.,-1.,-4.87512283120816E-48)) ;
#66745 = DIRECTION('',(0.,0.,-1.)) ;
#66746 = DIRECTION('center_axis',(0.,0.,-1.)) ;
#66747 = DIRECTION('ref_axis',(0.,1.,0.)) ;
#66748 = DIRECTION('center_axis',(2.46519032881571E-32,4.87512283120816E-48,
-1.)) ;
#66749 = DIRECTION('ref_axis',(-1.2018105655283E-79,1.,4.87512283120816E-48)) ;
#66750 = DIRECTION('',(0.,0.,-1.)) ;
#66751 = DIRECTION('center_axis',(-3.55271367880026E-13,-1.,0.)) ;
#66752 = DIRECTION('ref_axis',(-1.,3.55271367880026E-13,9.05696233641872E-48)) ;
#66753 = DIRECTION('',(1.,-3.55271367880026E-13,2.46519032881571E-32)) ;
#66754 = DIRECTION('',(0.,0.,-1.)) ;
#66755 = DIRECTION('center_axis',(-1.,1.53134210293125E-15,0.)) ;
#66756 = DIRECTION('ref_axis',(1.53134210293125E-15,1.,0.)) ;
#66757 = DIRECTION('',(-1.53134210293126E-15,-1.,-4.26256202537526E-47)) ;
#66758 = DIRECTION('',(0.,0.,-1.)) ;
#66759 = DIRECTION('center_axis',(0.,0.,-1.)) ;
#66760 = DIRECTION('ref_axis',(0.,1.,0.)) ;
#66761 = DIRECTION('center_axis',(2.46519032881571E-32,4.87512283120816E-48,
-1.)) ;
#66762 = DIRECTION('ref_axis',(-1.2018105655283E-79,1.,4.87512283120816E-48)) ;
#66763 = DIRECTION('',(0.,0.,-1.)) ;
#66764 = DIRECTION('center_axis',(0.,-1.,0.)) ;
#66765 = DIRECTION('ref_axis',(-1.,0.,1.62870009552296E-49)) ;
#66766 = DIRECTION('',(1.,0.,2.46519032881571E-32)) ;
#66767 = DIRECTION('',(0.,0.,-1.)) ;
#66768 = DIRECTION('center_axis',(0.,0.,-1.)) ;
#66769 = DIRECTION('ref_axis',(1.,0.,0.)) ;
#66770 = DIRECTION('',(0.,0.,-1.)) ;
#66771 = DIRECTION('center_axis',(0.,0.,-1.)) ;
#66772 = DIRECTION('ref_axis',(1.,0.,0.)) ;
#66773 = DIRECTION('center_axis',(-1.,0.,0.)) ;
#66774 = DIRECTION('ref_axis',(0.,1.,-1.48632706569949E-33)) ;
#66775 = DIRECTION('',(0.,-1.,0.)) ;
#66776 = DIRECTION('',(0.,0.,-1.)) ;
#66777 = DIRECTION('',(0.,0.,-1.)) ;
#66778 = DIRECTION('center_axis',(0.,0.,-1.)) ;
#66779 = DIRECTION('ref_axis',(0.707106781186636,0.707106781186459,0.)) ;
#66780 = DIRECTION('center_axis',(0.,0.,-1.)) ;
#66781 = DIRECTION('ref_axis',(0.707106781186636,0.707106781186459,0.)) ;
#66782 = DIRECTION('',(0.,0.,-1.)) ;
#66783 = DIRECTION('center_axis',(-0.707106781186539,-0.707106781186556,0.)) ;
#66784 = DIRECTION('ref_axis',(-0.707106781186556,0.707106781186539,0.)) ;
#66785 = DIRECTION('',(0.707106781186556,-0.707106781186539,0.)) ;
#66786 = DIRECTION('',(0.,0.,-1.)) ;
#66787 = DIRECTION('center_axis',(0.,0.,-1.)) ;
#66788 = DIRECTION('ref_axis',(0.,1.,0.)) ;
#66789 = DIRECTION('center_axis',(0.,0.,-1.)) ;
#66790 = DIRECTION('ref_axis',(0.,1.,0.)) ;
#66791 = DIRECTION('',(0.,0.,-1.)) ;
#66792 = DIRECTION('center_axis',(-8.7535908273216E-15,-1.,0.)) ;
#66793 = DIRECTION('ref_axis',(-1.,8.7535908273216E-15,2.56873619635494E-49)) ;
#66794 = DIRECTION('',(1.,-8.7535908273216E-15,0.)) ;
#66795 = DIRECTION('',(0.,0.,-1.)) ;
#66796 = DIRECTION('',(0.,0.,-1.)) ;
#66797 = DIRECTION('center_axis',(0.,0.,-1.)) ;
#66798 = DIRECTION('ref_axis',(1.,0.,0.)) ;
#66799 = DIRECTION('center_axis',(0.,0.,-1.)) ;
#66800 = DIRECTION('ref_axis',(1.,0.,0.)) ;
#66801 = DIRECTION('',(0.,0.,-1.)) ;
#66802 = DIRECTION('',(0.,0.,-1.)) ;
#66803 = DIRECTION('center_axis',(-1.,0.,0.)) ;
#66804 = DIRECTION('ref_axis',(0.,1.,-1.76085023486835E-33)) ;
#66805 = DIRECTION('',(0.,-1.,0.)) ;
#66806 = DIRECTION('',(0.,0.,-1.)) ;
#66807 = DIRECTION('center_axis',(0.,0.,-1.)) ;
#66808 = DIRECTION('ref_axis',(0.,1.,0.)) ;
#66809 = DIRECTION('center_axis',(0.,0.,-1.)) ;
#66810 = DIRECTION('ref_axis',(0.,1.,0.)) ;
#66811 = DIRECTION('',(0.,0.,-1.)) ;
#66812 = DIRECTION('center_axis',(-3.55271367880026E-13,-1.,0.)) ;
#66813 = DIRECTION('ref_axis',(-1.,3.55271367880026E-13,2.00046065889556E-47)) ;
#66814 = DIRECTION('',(1.,-3.55271367880026E-13,0.)) ;
#66815 = DIRECTION('',(0.,0.,-1.)) ;
#66816 = DIRECTION('center_axis',(-1.,0.,0.)) ;
#66817 = DIRECTION('ref_axis',(0.,1.,0.)) ;
#66818 = DIRECTION('',(0.,-1.,0.)) ;
#66819 = DIRECTION('center_axis',(0.,-1.,0.)) ;
#66820 = DIRECTION('ref_axis',(-1.,0.,0.)) ;
#66821 = DIRECTION('',(1.,0.,0.)) ;
#66822 = DIRECTION('',(0.,0.,-1.)) ;
#66823 = DIRECTION('center_axis',(0.,0.,-1.)) ;
#66824 = DIRECTION('ref_axis',(0.,-1.,0.)) ;
#66825 = DIRECTION('center_axis',(-3.18850138855159E-46,-1.74315279842113E-32,
-1.)) ;
#66826 = DIRECTION('ref_axis',(5.55804511822336E-78,-1.,1.74315279842113E-32)) ;
#66827 = DIRECTION('',(0.,0.,-1.)) ;
#66828 = DIRECTION('',(0.,0.,-1.)) ;
#66829 = DIRECTION('center_axis',(0.,1.,0.)) ;
#66830 = DIRECTION('ref_axis',(1.,0.,6.12949496482233E-35)) ;
#66831 = DIRECTION('',(-1.,0.,3.18850138855159E-46)) ;
#66832 = DIRECTION('',(0.,0.,-1.)) ;
#66833 = DIRECTION('',(0.,0.,-1.)) ;
#66834 = DIRECTION('center_axis',(0.,0.,-1.)) ;
#66835 = DIRECTION('ref_axis',(1.,0.,0.)) ;
#66836 = DIRECTION('center_axis',(-3.18850138855159E-46,-1.74315279842113E-32,
-1.)) ;
#66837 = DIRECTION('ref_axis',(1.,-5.55804511822336E-78,-3.18850138855159E-46)) ;
#66838 = DIRECTION('',(0.,0.,-1.)) ;
#66839 = DIRECTION('center_axis',(-1.,1.7763568394025E-14,0.)) ;
#66840 = DIRECTION('ref_axis',(1.7763568394025E-14,1.,0.)) ;
#66841 = DIRECTION('',(-1.7763568394025E-14,-1.,1.74315279842113E-32)) ;
#66842 = DIRECTION('',(0.,0.,-1.)) ;
#66843 = DIRECTION('center_axis',(0.,0.,-1.)) ;
#66844 = DIRECTION('ref_axis',(0.,1.,0.)) ;
#66845 = DIRECTION('center_axis',(-3.18850138855159E-46,-1.74315279842113E-32,
-1.)) ;
#66846 = DIRECTION('ref_axis',(-5.55804511822336E-78,1.,-1.74315279842113E-32)) ;
#66847 = DIRECTION('center_axis',(0.,0.,-1.)) ;
#66848 = DIRECTION('ref_axis',(1.,0.,0.)) ;
#66849 = DIRECTION('center_axis',(2.46519032881571E-32,4.87512283120816E-48,
-1.)) ;
#66850 = DIRECTION('ref_axis',(1.,-1.2018105655283E-79,2.46519032881571E-32)) ;
#66851 = DIRECTION('',(0.,0.,-1.)) ;
#66852 = DIRECTION('',(0.,0.,-1.)) ;
#66853 = DIRECTION('center_axis',(-1.,0.,0.)) ;
#66854 = DIRECTION('ref_axis',(0.,1.,-1.76085023486835E-33)) ;
#66855 = DIRECTION('',(0.,-1.,-4.87512283120816E-48)) ;
#66856 = DIRECTION('',(0.,0.,-1.)) ;
#66857 = DIRECTION('center_axis',(0.,0.,-1.)) ;
#66858 = DIRECTION('ref_axis',(0.,1.,0.)) ;
#66859 = DIRECTION('center_axis',(2.46519032881571E-32,4.87512283120816E-48,
-1.)) ;
#66860 = DIRECTION('ref_axis',(-1.2018105655283E-79,1.,4.87512283120816E-48)) ;
#66861 = DIRECTION('',(0.,0.,-1.)) ;
#66862 = DIRECTION('center_axis',(-3.55271367880026E-13,-1.,0.)) ;
#66863 = DIRECTION('ref_axis',(-1.,3.55271367880026E-13,9.05696233641872E-48)) ;
#66864 = DIRECTION('',(1.,-3.55271367880026E-13,2.46519032881571E-32)) ;
#66865 = DIRECTION('',(0.,0.,-1.)) ;
#66866 = DIRECTION('center_axis',(-1.,1.53134210293125E-15,0.)) ;
#66867 = DIRECTION('ref_axis',(1.53134210293125E-15,1.,0.)) ;
#66868 = DIRECTION('',(-1.53134210293126E-15,-1.,-4.26256202537526E-47)) ;
#66869 = DIRECTION('',(0.,0.,-1.)) ;
#66870 = DIRECTION('center_axis',(0.,0.,-1.)) ;
#66871 = DIRECTION('ref_axis',(0.,1.,0.)) ;
#66872 = DIRECTION('center_axis',(2.46519032881571E-32,4.87512283120816E-48,
-1.)) ;
#66873 = DIRECTION('ref_axis',(-1.2018105655283E-79,1.,4.87512283120816E-48)) ;
#66874 = DIRECTION('',(0.,0.,-1.)) ;
#66875 = DIRECTION('center_axis',(0.,-1.,0.)) ;
#66876 = DIRECTION('ref_axis',(-1.,0.,1.62870009552296E-49)) ;
#66877 = DIRECTION('',(1.,0.,2.46519032881571E-32)) ;
#66878 = DIRECTION('',(0.,0.,-1.)) ;
#66879 = DIRECTION('center_axis',(0.,0.,-1.)) ;
#66880 = DIRECTION('ref_axis',(-1.,0.,0.)) ;
#66881 = DIRECTION('center_axis',(2.46519032881571E-32,4.87512283120816E-48,
-1.)) ;
#66882 = DIRECTION('ref_axis',(-1.,1.2018105655283E-79,-2.46519032881571E-32)) ;
#66883 = DIRECTION('',(0.,0.,-1.)) ;
#66884 = DIRECTION('center_axis',(1.,0.,0.)) ;
#66885 = DIRECTION('ref_axis',(0.,-1.,8.50065630626093E-34)) ;
#66886 = DIRECTION('',(0.,1.,4.87512283120816E-48)) ;
#66887 = DIRECTION('',(0.,0.,-1.)) ;
#66888 = DIRECTION('center_axis',(3.55271367880026E-13,-1.,0.)) ;
#66889 = DIRECTION('ref_axis',(-1.,-3.55271367880026E-13,5.47382212626845E-48)) ;
#66890 = DIRECTION('',(1.,3.55271367880026E-13,2.46519032881571E-32)) ;
#66891 = DIRECTION('',(0.,0.,-1.)) ;
#66892 = DIRECTION('center_axis',(0.,0.,-1.)) ;
#66893 = DIRECTION('ref_axis',(-1.,0.,0.)) ;
#66894 = DIRECTION('center_axis',(2.46519032881571E-32,4.87512283120816E-48,
-1.)) ;
#66895 = DIRECTION('ref_axis',(-1.,1.2018105655283E-79,-2.46519032881571E-32)) ;
#66896 = DIRECTION('',(0.,0.,-1.)) ;
#66897 = DIRECTION('center_axis',(1.,0.,0.)) ;
#66898 = DIRECTION('ref_axis',(0.,-1.,1.76085023486835E-33)) ;
#66899 = DIRECTION('',(0.,1.,4.87512283120816E-48)) ;
#66900 = DIRECTION('',(0.,0.,-1.)) ;
#66901 = DIRECTION('center_axis',(0.,0.,-1.)) ;
#66902 = DIRECTION('ref_axis',(0.,-1.,0.)) ;
#66903 = DIRECTION('center_axis',(2.46519032881571E-32,4.87512283120816E-48,
-1.)) ;
#66904 = DIRECTION('ref_axis',(1.2018105655283E-79,-1.,-4.87512283120816E-48)) ;
#66905 = DIRECTION('',(0.,0.,-1.)) ;
#66906 = DIRECTION('center_axis',(1.26882631385732E-14,1.,0.)) ;
#66907 = DIRECTION('ref_axis',(1.,-1.26882631385732E-14,-1.27969293219661E-49)) ;
#66908 = DIRECTION('',(-1.,1.26882631385732E-14,-2.46519032881571E-32)) ;
#66909 = DIRECTION('center_axis',(2.46519032881571E-32,4.87512283120816E-48,
-1.)) ;
#66910 = DIRECTION('ref_axis',(1.,3.7453410837561E-96,2.46519032881571E-32)) ;
#66911 = DIRECTION('center_axis',(1.,0.,0.)) ;
#66912 = DIRECTION('ref_axis',(0.,-1.,0.)) ;
#66913 = DIRECTION('',(0.,1.,0.)) ;
#66914 = DIRECTION('',(0.,0.,-1.)) ;
#66915 = DIRECTION('',(0.,0.,-1.)) ;
#66916 = DIRECTION('center_axis',(0.,1.,0.)) ;
#66917 = DIRECTION('ref_axis',(1.,0.,0.)) ;
#66918 = DIRECTION('',(-1.,0.,0.)) ;
#66919 = DIRECTION('',(0.,0.,-1.)) ;
#66920 = DIRECTION('center_axis',(0.,0.,-1.)) ;
#66921 = DIRECTION('ref_axis',(0.707106781186459,-0.707106781186636,0.)) ;
#66922 = DIRECTION('center_axis',(0.,0.,-1.)) ;
#66923 = DIRECTION('ref_axis',(0.707106781186459,-0.707106781186636,0.)) ;
#66924 = DIRECTION('',(0.,0.,-1.)) ;
#66925 = DIRECTION('center_axis',(-0.707106781186573,0.707106781186522,0.)) ;
#66926 = DIRECTION('ref_axis',(0.707106781186522,0.707106781186573,-4.31889331967372E-49)) ;
#66927 = DIRECTION('',(-0.707106781186522,-0.707106781186573,0.)) ;
#66928 = DIRECTION('',(0.,0.,-1.)) ;
#66929 = DIRECTION('center_axis',(0.,0.,-1.)) ;
#66930 = DIRECTION('ref_axis',(1.,0.,0.)) ;
#66931 = DIRECTION('center_axis',(0.,0.,-1.)) ;
#66932 = DIRECTION('ref_axis',(1.,0.,0.)) ;
#66933 = DIRECTION('center_axis',(0.,0.,-1.)) ;
#66934 = DIRECTION('ref_axis',(1.,0.,0.)) ;
#66935 = DIRECTION('',(0.,0.,-1.)) ;
#66936 = DIRECTION('center_axis',(1.,0.,0.)) ;
#66937 = DIRECTION('ref_axis',(0.,-1.,0.)) ;
#66938 = DIRECTION('',(0.,1.,0.)) ;
#66939 = DIRECTION('',(0.,0.,-1.)) ;
#66940 = DIRECTION('center_axis',(0.,-1.,0.)) ;
#66941 = DIRECTION('ref_axis',(-1.,0.,0.)) ;
#66942 = DIRECTION('',(1.,0.,0.)) ;
#66943 = DIRECTION('',(0.,0.,-1.)) ;
#66944 = DIRECTION('center_axis',(0.,0.,-1.)) ;
#66945 = DIRECTION('ref_axis',(-1.,0.,0.)) ;
#66946 = DIRECTION('center_axis',(0.,0.,-1.)) ;
#66947 = DIRECTION('ref_axis',(-1.,0.,0.)) ;
#66948 = DIRECTION('',(0.,0.,-1.)) ;
#66949 = DIRECTION('center_axis',(1.,0.,0.)) ;
#66950 = DIRECTION('ref_axis',(0.,-1.,1.76085023486835E-33)) ;
#66951 = DIRECTION('',(0.,1.,0.)) ;
#66952 = DIRECTION('',(0.,0.,-1.)) ;
#66953 = DIRECTION('center_axis',(0.,0.,-1.)) ;
#66954 = DIRECTION('ref_axis',(0.,-1.,0.)) ;
#66955 = DIRECTION('center_axis',(0.,0.,-1.)) ;
#66956 = DIRECTION('ref_axis',(0.,-1.,0.)) ;
#66957 = DIRECTION('',(0.,0.,-1.)) ;
#66958 = DIRECTION('center_axis',(0.,1.,0.)) ;
#66959 = DIRECTION('ref_axis',(1.,0.,-4.0027363178395E-35)) ;
#66960 = DIRECTION('',(-1.,0.,0.)) ;
#66961 = DIRECTION('center_axis',(0.,0.,-1.)) ;
#66962 = DIRECTION('ref_axis',(1.,0.,0.)) ;
#66963 = DIRECTION('center_axis',(0.,0.,-1.)) ;
#66964 = DIRECTION('ref_axis',(1.,0.,0.)) ;
#66965 = DIRECTION('center_axis',(0.,0.,-1.)) ;
#66966 = DIRECTION('ref_axis',(1.,0.,0.)) ;
#66967 = DIRECTION('',(0.,0.,-1.)) ;
#66968 = DIRECTION('center_axis',(-1.,0.,0.)) ;
#66969 = DIRECTION('ref_axis',(0.,1.,0.)) ;
#66970 = DIRECTION('',(0.,-1.,0.)) ;
#66971 = DIRECTION('',(0.,0.,-1.)) ;
#66972 = DIRECTION('center_axis',(0.,-1.,0.)) ;
#66973 = DIRECTION('ref_axis',(-1.,0.,0.)) ;
#66974 = DIRECTION('',(1.,0.,0.)) ;
#66975 = DIRECTION('',(0.,0.,-1.)) ;
#66976 = DIRECTION('center_axis',(-1.,-6.34413156929222E-15,0.)) ;
#66977 = DIRECTION('ref_axis',(-6.34413156929222E-15,1.,0.)) ;
#66978 = DIRECTION('',(6.34413156929222E-15,-1.,0.)) ;
#66979 = DIRECTION('',(0.,0.,-1.)) ;
#66980 = DIRECTION('center_axis',(0.,1.,0.)) ;
#66981 = DIRECTION('ref_axis',(1.,0.,0.)) ;
#66982 = DIRECTION('',(-1.,0.,0.)) ;
#66983 = DIRECTION('',(0.,0.,-1.)) ;
#66984 = DIRECTION('center_axis',(-1.,1.77635683940243E-14,0.)) ;
#66985 = DIRECTION('ref_axis',(1.77635683940243E-14,1.,0.)) ;
#66986 = DIRECTION('',(-1.77635683940243E-14,-1.,0.)) ;
#66987 = DIRECTION('',(0.,0.,-1.)) ;
#66988 = DIRECTION('center_axis',(0.,0.,-1.)) ;
#66989 = DIRECTION('ref_axis',(0.,1.,0.)) ;
#66990 = DIRECTION('center_axis',(0.,0.,-1.)) ;
#66991 = DIRECTION('ref_axis',(0.,1.,0.)) ;
#66992 = DIRECTION('',(0.,0.,-1.)) ;
#66993 = DIRECTION('center_axis',(0.,0.,-1.)) ;
#66994 = DIRECTION('ref_axis',(1.,0.,0.)) ;
#66995 = DIRECTION('center_axis',(0.,0.,-1.)) ;
#66996 = DIRECTION('ref_axis',(1.,0.,0.)) ;
#66997 = DIRECTION('',(1.,0.,0.)) ;
#66998 = DIRECTION('center_axis',(0.,0.,-1.)) ;
#66999 = DIRECTION('ref_axis',(-1.,0.,0.)) ;
#67000 = DIRECTION('center_axis',(2.46519032881571E-32,4.87512283120816E-48,
-1.)) ;
#67001 = DIRECTION('ref_axis',(-1.,1.2018105655283E-79,-2.46519032881571E-32)) ;
#67002 = DIRECTION('',(0.,0.,-1.)) ;
#67003 = DIRECTION('center_axis',(1.,0.,0.)) ;
#67004 = DIRECTION('ref_axis',(0.,-1.,8.50065630626093E-34)) ;
#67005 = DIRECTION('',(0.,1.,4.87512283120816E-48)) ;
#67006 = DIRECTION('',(0.,0.,-1.)) ;
#67007 = DIRECTION('center_axis',(3.55271367880026E-13,-1.,0.)) ;
#67008 = DIRECTION('ref_axis',(-1.,-3.55271367880026E-13,5.47382212626845E-48)) ;
#67009 = DIRECTION('',(1.,3.55271367880026E-13,2.46519032881571E-32)) ;
#67010 = DIRECTION('',(0.,0.,-1.)) ;
#67011 = DIRECTION('center_axis',(0.,0.,-1.)) ;
#67012 = DIRECTION('ref_axis',(-1.,0.,0.)) ;
#67013 = DIRECTION('center_axis',(2.46519032881571E-32,4.87512283120816E-48,
-1.)) ;
#67014 = DIRECTION('ref_axis',(-1.,1.2018105655283E-79,-2.46519032881571E-32)) ;
#67015 = DIRECTION('',(0.,0.,-1.)) ;
#67016 = DIRECTION('center_axis',(1.,0.,0.)) ;
#67017 = DIRECTION('ref_axis',(0.,-1.,1.76085023486835E-33)) ;
#67018 = DIRECTION('',(0.,1.,4.87512283120816E-48)) ;
#67019 = DIRECTION('',(0.,0.,-1.)) ;
#67020 = DIRECTION('center_axis',(0.,0.,-1.)) ;
#67021 = DIRECTION('ref_axis',(0.,-1.,0.)) ;
#67022 = DIRECTION('center_axis',(2.46519032881571E-32,4.87512283120816E-48,
-1.)) ;
#67023 = DIRECTION('ref_axis',(1.2018105655283E-79,-1.,-4.87512283120816E-48)) ;
#67024 = DIRECTION('',(0.,0.,-1.)) ;
#67025 = DIRECTION('center_axis',(1.26882631385732E-14,1.,0.)) ;
#67026 = DIRECTION('ref_axis',(1.,-1.26882631385732E-14,-1.27969293219661E-49)) ;
#67027 = DIRECTION('',(-1.,1.26882631385732E-14,-2.46519032881571E-32)) ;
#67028 = DIRECTION('center_axis',(2.46519032881571E-32,4.87512283120816E-48,
-1.)) ;
#67029 = DIRECTION('ref_axis',(1.,3.7453410837561E-96,2.46519032881571E-32)) ;
#67030 = DIRECTION('center_axis',(0.,0.,-1.)) ;
#67031 = DIRECTION('ref_axis',(-0.707106781186636,0.707106781186459,0.)) ;
#67032 = DIRECTION('center_axis',(-3.18850138855159E-46,-1.74315279842113E-32,
-1.)) ;
#67033 = DIRECTION('ref_axis',(-0.707106781186636,0.707106781186459,-1.23259516440771E-32)) ;
#67034 = DIRECTION('',(0.,0.,-1.)) ;
#67035 = DIRECTION('center_axis',(0.707106781186556,-0.707106781186539,0.)) ;
#67036 = DIRECTION('ref_axis',(-0.707106781186539,-0.707106781186556,1.17554800907501E-33)) ;
#67037 = DIRECTION('',(0.707106781186539,0.707106781186556,-1.23259516440793E-32)) ;
#67038 = DIRECTION('',(0.,0.,-1.)) ;
#67039 = DIRECTION('center_axis',(0.,0.,-1.)) ;
#67040 = DIRECTION('ref_axis',(-1.,0.,0.)) ;
#67041 = DIRECTION('center_axis',(-3.18850138855159E-46,-1.74315279842113E-32,
-1.)) ;
#67042 = DIRECTION('ref_axis',(-1.,5.55804511822336E-78,3.18850138855159E-46)) ;
#67043 = DIRECTION('',(0.,0.,-1.)) ;
#67044 = DIRECTION('center_axis',(1.,-5.35505761538786E-15,0.)) ;
#67045 = DIRECTION('ref_axis',(-5.35505761538786E-15,-1.,7.43163532849736E-34)) ;
#67046 = DIRECTION('',(5.35505761538786E-15,1.,-1.74315279842113E-32)) ;
#67047 = DIRECTION('',(0.,0.,-1.)) ;
#67048 = DIRECTION('center_axis',(0.,0.,-1.)) ;
#67049 = DIRECTION('ref_axis',(-0.707106781186681,-0.707106781186414,0.)) ;
#67050 = DIRECTION('center_axis',(-3.18850138855159E-46,-1.74315279842113E-32,
-1.)) ;
#67051 = DIRECTION('ref_axis',(-0.707106781186681,-0.707106781186414,1.23259516440768E-32)) ;
#67052 = DIRECTION('',(0.,0.,-1.)) ;
#67053 = DIRECTION('center_axis',(0.707106781186509,0.707106781186586,0.)) ;
#67054 = DIRECTION('ref_axis',(0.707106781186586,-0.707106781186509,-7.3914897815741E-47)) ;
#67055 = DIRECTION('',(-0.707106781186586,0.707106781186509,-1.2325951644078E-32)) ;
#67056 = DIRECTION('center_axis',(-3.18850138855159E-46,-1.74315279842113E-32,
-1.)) ;
#67057 = DIRECTION('ref_axis',(1.,5.16381567742834E-95,-3.18850138855159E-46)) ;
#67058 = DIRECTION('center_axis',(0.,0.,-1.)) ;
#67059 = DIRECTION('ref_axis',(1.,0.,0.)) ;
#67060 = DIRECTION('center_axis',(0.,0.,-1.)) ;
#67061 = DIRECTION('ref_axis',(-1.,0.,0.)) ;
#67062 = DIRECTION('center_axis',(-3.83260058933034E-30,-6.60793205056939E-32,
-1.)) ;
#67063 = DIRECTION('ref_axis',(-1.,2.53255642712671E-61,3.83260058933034E-30)) ;
#67064 = DIRECTION('',(0.,0.,-1.)) ;
#67065 = DIRECTION('center_axis',(1.,-3.17206578464333E-15,0.)) ;
#67066 = DIRECTION('ref_axis',(-3.17206578464333E-15,-1.,1.76085023486835E-33)) ;
#67067 = DIRECTION('',(3.17206578464333E-15,1.,-6.60793205057061E-32)) ;
#67068 = DIRECTION('',(0.,0.,-1.)) ;
#67069 = DIRECTION('center_axis',(0.,0.,-1.)) ;
#67070 = DIRECTION('ref_axis',(1.,0.,0.)) ;
#67071 = DIRECTION('center_axis',(-0.599999999999998,0.800000000000002,0.)) ;
#67072 = DIRECTION('ref_axis',(0.,0.,1.)) ;
#67073 = DIRECTION('',(0.,0.,-1.)) ;
#67074 = DIRECTION('',(0.,0.,-1.)) ;
#67075 = DIRECTION('center_axis',(0.,1.,0.)) ;
#67076 = DIRECTION('ref_axis',(1.,0.,3.20175569450239E-16)) ;
#67077 = DIRECTION('',(0.,0.,1.)) ;
#67078 = DIRECTION('',(1.,0.,0.)) ;
#67079 = DIRECTION('center_axis',(0.800000000000014,0.599999999999982,0.)) ;
#67080 = DIRECTION('ref_axis',(0.,0.,-1.)) ;
#67081 = DIRECTION('',(0.,0.,1.)) ;
#67082 = DIRECTION('center_axis',(-1.,0.,0.)) ;
#67083 = DIRECTION('ref_axis',(0.,1.,0.)) ;
#67084 = DIRECTION('',(0.,0.,-1.)) ;
#67085 = DIRECTION('',(0.,0.,1.)) ;
#67086 = DIRECTION('center_axis',(-1.,1.08152878803189E-14,0.)) ;
#67087 = DIRECTION('ref_axis',(1.08152878803189E-14,1.,-2.09196947838501E-32)) ;
#67088 = DIRECTION('center_axis',(0.,1.,0.)) ;
#67089 = DIRECTION('ref_axis',(1.,0.,-2.99489585516063E-33)) ;
#67090 = DIRECTION('',(0.,0.,-1.)) ;
#67091 = DIRECTION('center_axis',(-0.766044443118928,-0.642787609686599,0.)) ;
#67092 = DIRECTION('ref_axis',(-0.642787609686599,0.766044443118928,1.23259516440792E-32)) ;
#67093 = DIRECTION('',(0.,0.,-1.)) ;
#67094 = DIRECTION('center_axis',(0.,0.,-1.)) ;
#67095 = DIRECTION('ref_axis',(1.42108547151988E-13,1.,0.)) ;
#67096 = DIRECTION('',(0.,0.,-1.)) ;
#67097 = DIRECTION('center_axis',(-1.28403006865249E-14,-1.,0.)) ;
#67098 = DIRECTION('ref_axis',(-1.,1.28403006865249E-14,0.)) ;
#67099 = DIRECTION('',(0.,0.,-1.)) ;
#67100 = DIRECTION('center_axis',(0.,0.,-1.)) ;
#67101 = DIRECTION('ref_axis',(1.,0.,0.)) ;
#67102 = DIRECTION('',(0.,0.,-1.)) ;
#67103 = DIRECTION('center_axis',(-1.,0.,0.)) ;
#67104 = DIRECTION('ref_axis',(0.,1.,-2.39087358882206E-65)) ;
#67105 = DIRECTION('center_axis',(-3.83260058933034E-30,-6.60793205056939E-32,
-1.)) ;
#67106 = DIRECTION('ref_axis',(1.,1.51420860759427E-77,-3.83260058933034E-30)) ;
#67107 = DIRECTION('center_axis',(-3.83260058933034E-30,-6.60793205056939E-32,
-1.)) ;
#67108 = DIRECTION('ref_axis',(-1.,3.9474596431117E-14,3.83260058933034E-30)) ;
#67109 = DIRECTION('center_axis',(-3.83260058933034E-30,-6.60793205056939E-32,
-1.)) ;
#67110 = DIRECTION('ref_axis',(2.53255642712671E-61,-1.,6.60793205056939E-32)) ;
#67111 = DIRECTION('center_axis',(0.,0.,-1.)) ;
#67112 = DIRECTION('ref_axis',(0.,-1.,0.)) ;
#67113 = DIRECTION('',(0.,0.,-1.)) ;
#67114 = DIRECTION('center_axis',(-1.,0.,0.)) ;
#67115 = DIRECTION('ref_axis',(0.,1.,0.)) ;
#67116 = DIRECTION('center_axis',(0.,0.,-1.)) ;
#67117 = DIRECTION('ref_axis',(-1.,3.9474596431117E-14,0.)) ;
#67118 = DIRECTION('',(0.,0.,-1.)) ;
#67119 = DIRECTION('center_axis',(3.55271367880048E-14,1.,0.)) ;
#67120 = DIRECTION('ref_axis',(1.,-3.55271367880048E-14,0.)) ;
#67121 = DIRECTION('',(0.,0.,-1.)) ;
#67122 = DIRECTION('center_axis',(-1.,0.,0.)) ;
#67123 = DIRECTION('ref_axis',(0.,1.,0.)) ;
#67124 = DIRECTION('center_axis',(0.,-1.,0.)) ;
#67125 = DIRECTION('ref_axis',(-1.,0.,-2.52374105052742E-18)) ;
#67126 = DIRECTION('',(0.,0.,1.)) ;
#67127 = DIRECTION('center_axis',(-1.,3.67742382159233E-14,0.)) ;
#67128 = DIRECTION('ref_axis',(3.67742382159233E-14,1.,0.)) ;
#67129 = DIRECTION('center_axis',(1.,-2.61228946970624E-14,0.)) ;
#67130 = DIRECTION('ref_axis',(-2.61228946970624E-14,-1.,0.)) ;
#67131 = DIRECTION('',(0.,0.,-1.)) ;
#67132 = DIRECTION('center_axis',(0.,0.,-1.)) ;
#67133 = DIRECTION('ref_axis',(0.948683298050522,0.316227766016813,0.)) ;
#67134 = DIRECTION('center_axis',(-0.599999999999996,0.800000000000003,0.)) ;
#67135 = DIRECTION('ref_axis',(0.,0.,1.)) ;
#67136 = DIRECTION('',(0.,0.,-1.)) ;
#67137 = DIRECTION('center_axis',(0.,0.,1.)) ;
#67138 = DIRECTION('ref_axis',(-0.894427190999906,0.447213595499978,0.)) ;
#67139 = DIRECTION('center_axis',(0.,0.780868809443031,-0.624695047554424)) ;
#67140 = DIRECTION('ref_axis',(-1.,0.,0.)) ;
#67141 = DIRECTION('center_axis',(-1.,0.,0.)) ;
#67142 = DIRECTION('ref_axis',(0.,1.,0.)) ;
#67143 = DIRECTION('',(0.,0.,1.)) ;
#67144 = DIRECTION('center_axis',(0.,0.,1.)) ;
#67145 = DIRECTION('ref_axis',(-0.89442719099992,0.44721359549995,0.)) ;
#67146 = DIRECTION('center_axis',(0.,-1.,0.)) ;
#67147 = DIRECTION('ref_axis',(-1.,0.,0.)) ;
#67148 = DIRECTION('',(0.,-1.,0.)) ;
#67149 = DIRECTION('center_axis',(0.,-1.,0.)) ;
#67150 = DIRECTION('ref_axis',(-1.,0.,2.76147456380442E-35)) ;
#67151 = DIRECTION('',(0.,0.,-1.)) ;
#67152 = DIRECTION('center_axis',(0.,0.,-1.)) ;
#67153 = DIRECTION('ref_axis',(1.,0.,0.)) ;
#67154 = DIRECTION('',(0.,0.,1.)) ;
#67155 = DIRECTION('center_axis',(-1.,0.,0.)) ;
#67156 = DIRECTION('ref_axis',(0.,1.,0.)) ;
#67157 = DIRECTION('',(0.,0.,-1.)) ;
#67158 = DIRECTION('center_axis',(0.,0.,-1.)) ;
#67159 = DIRECTION('ref_axis',(1.,0.,0.)) ;
#67160 = DIRECTION('',(0.,0.,-1.)) ;
#67161 = DIRECTION('center_axis',(1.,0.,0.)) ;
#67162 = DIRECTION('ref_axis',(0.,-1.,0.)) ;
#67163 = DIRECTION('center_axis',(1.,0.,0.)) ;
#67164 = DIRECTION('ref_axis',(0.,-1.,0.)) ;
#67165 = DIRECTION('',(0.,0.,-1.)) ;
#67166 = DIRECTION('center_axis',(0.,0.,-1.)) ;
#67167 = DIRECTION('ref_axis',(1.,0.,0.)) ;
#67168 = DIRECTION('center_axis',(0.,0.,1.)) ;
#67169 = DIRECTION('ref_axis',(1.,0.,0.)) ;
#67170 = DIRECTION('',(1.,0.,0.)) ;
#67171 = DIRECTION('',(0.,1.,0.)) ;
#67172 = DIRECTION('center_axis',(1.,0.,0.)) ;
#67173 = DIRECTION('ref_axis',(0.,1.,0.)) ;
#67174 = DIRECTION('center_axis',(0.,1.,0.)) ;
#67175 = DIRECTION('ref_axis',(-1.,0.,0.)) ;
#67176 = DIRECTION('center_axis',(0.,0.,-1.)) ;
#67177 = DIRECTION('ref_axis',(1.,0.,0.)) ;
#67178 = DIRECTION('center_axis',(0.,-1.,0.)) ;
#67179 = DIRECTION('ref_axis',(1.,0.,0.)) ;
#67180 = DIRECTION('axis',(0.,0.,1.)) ;
#67181 = DIRECTION('refdir',(1.,0.,0.)) ;
#67182 = DIRECTION('center_axis',(0.,1.,0.)) ;
#67183 = DIRECTION('ref_axis',(1.,0.,0.)) ;
#67184 = DIRECTION('',(1.,0.,0.)) ;
#67185 = DIRECTION('',(0.,0.,1.)) ;
#67186 = DIRECTION('',(1.,0.,0.)) ;
#67187 = DIRECTION('',(0.,0.,-1.)) ;
#67188 = DIRECTION('center_axis',(-1.,0.,0.)) ;
#67189 = DIRECTION('ref_axis',(0.,1.,0.)) ;
#67190 = DIRECTION('',(0.,1.,0.)) ;
#67191 = DIRECTION('',(0.,1.,0.)) ;
#67192 = DIRECTION('',(0.,0.,-1.)) ;
#67193 = DIRECTION('center_axis',(0.,1.,0.)) ;
#67194 = DIRECTION('ref_axis',(1.,0.,0.)) ;
#67195 = DIRECTION('',(1.,0.,0.)) ;
#67196 = DIRECTION('',(1.,0.,0.)) ;
#67197 = DIRECTION('',(0.,0.,-1.)) ;
#67198 = DIRECTION('center_axis',(-1.,0.,0.)) ;
#67199 = DIRECTION('ref_axis',(0.,1.,0.)) ;
#67200 = DIRECTION('',(0.,1.,0.)) ;
#67201 = DIRECTION('',(0.,1.,0.)) ;
#67202 = DIRECTION('',(0.,0.,-1.)) ;
#67203 = DIRECTION('center_axis',(0.,1.,0.)) ;
#67204 = DIRECTION('ref_axis',(1.,0.,0.)) ;
#67205 = DIRECTION('',(1.,0.,0.)) ;
#67206 = DIRECTION('',(1.,0.,0.)) ;
#67207 = DIRECTION('',(0.,0.,-1.)) ;
#67208 = DIRECTION('center_axis',(-1.,0.,0.)) ;
#67209 = DIRECTION('ref_axis',(0.,1.,0.)) ;
#67210 = DIRECTION('',(0.,1.,0.)) ;
#67211 = DIRECTION('',(0.,1.,0.)) ;
#67212 = DIRECTION('',(0.,0.,-1.)) ;
#67213 = DIRECTION('center_axis',(-0.819152044288993,-0.573576436351045,0.)) ;
#67214 = DIRECTION('ref_axis',(-0.573576436351045,0.819152044288993,-8.99089246287955E-32)) ;
#67215 = DIRECTION('',(-0.573576436351045,0.819152044288993,-8.99089246287955E-32)) ;
#67216 = DIRECTION('',(-0.573576436351045,0.819152044288993,-8.99089246287955E-32)) ;
#67217 = DIRECTION('',(0.,0.,-1.)) ;
#67218 = DIRECTION('center_axis',(0.,0.,-1.)) ;
#67219 = DIRECTION('ref_axis',(-1.,0.,0.)) ;
#67220 = DIRECTION('',(0.,1.,0.)) ;
#67221 = DIRECTION('center_axis',(1.56751426541813E-31,0.,-1.)) ;
#67222 = DIRECTION('ref_axis',(1.,0.,1.56751426541813E-31)) ;
#67223 = DIRECTION('',(0.,-1.,0.)) ;
#67224 = DIRECTION('center_axis',(0.,1.,0.)) ;
#67225 = DIRECTION('ref_axis',(1.,0.,0.)) ;
#67226 = DIRECTION('',(1.,0.,0.)) ;
#67227 = DIRECTION('',(0.,0.,-1.)) ;
#67228 = DIRECTION('',(1.,0.,0.)) ;
#67229 = DIRECTION('',(0.,0.,-1.)) ;
#67230 = DIRECTION('center_axis',(-1.,0.,0.)) ;
#67231 = DIRECTION('ref_axis',(0.,1.,0.)) ;
#67232 = DIRECTION('',(0.,0.,-1.)) ;
#67233 = DIRECTION('',(0.,1.,0.)) ;
#67234 = DIRECTION('',(0.,1.,0.)) ;
#67235 = DIRECTION('',(0.,0.,-1.)) ;
#67236 = DIRECTION('center_axis',(0.,-1.,0.)) ;
#67237 = DIRECTION('ref_axis',(-1.,0.,1.04893745400262E-30)) ;
#67238 = DIRECTION('',(-1.,0.,1.04893745400262E-30)) ;
#67239 = DIRECTION('',(-1.,0.,1.04893745400262E-30)) ;
#67240 = DIRECTION('',(0.,0.,-1.)) ;
#67241 = DIRECTION('center_axis',(1.,0.,0.)) ;
#67242 = DIRECTION('ref_axis',(0.,-1.,-6.29362472401568E-32)) ;
#67243 = DIRECTION('',(0.,-1.,-6.29362472401568E-32)) ;
#67244 = DIRECTION('',(0.,-1.,-6.29362472401568E-32)) ;
#67245 = DIRECTION('center_axis',(0.,0.,-1.)) ;
#67246 = DIRECTION('ref_axis',(-1.,0.,0.)) ;
#67247 = DIRECTION('center_axis',(-1.04893745400262E-30,0.,-1.)) ;
#67248 = DIRECTION('ref_axis',(1.,0.,-1.04893745400262E-30)) ;
#67249 = DIRECTION('axis',(0.,0.,1.)) ;
#67250 = DIRECTION('refdir',(1.,0.,0.)) ;
#67251 = DIRECTION('center_axis',(0.,-1.,0.)) ;
#67252 = DIRECTION('ref_axis',(0.457808359486171,0.,0.889050901796169)) ;
#67253 = DIRECTION('',(0.,1.,0.)) ;
#67254 = DIRECTION('center_axis',(0.,1.,0.)) ;
#67255 = DIRECTION('ref_axis',(-1.,0.,0.)) ;
#67256 = DIRECTION('center_axis',(0.,-1.,0.)) ;
#67257 = DIRECTION('ref_axis',(0.457808359486171,0.,0.889050901796169)) ;
#67258 = DIRECTION('',(0.,1.,0.)) ;
#67259 = DIRECTION('center_axis',(0.,-1.,0.)) ;
#67260 = DIRECTION('ref_axis',(0.457808359486171,0.,0.889050901796169)) ;
#67261 = DIRECTION('',(0.,1.,0.)) ;
#67262 = DIRECTION('center_axis',(0.,-1.,0.)) ;
#67263 = DIRECTION('ref_axis',(0.457808359486171,0.,0.889050901796169)) ;
#67264 = DIRECTION('',(0.,1.,0.)) ;
#67265 = DIRECTION('center_axis',(0.,-1.,0.)) ;
#67266 = DIRECTION('ref_axis',(-1.,0.,0.)) ;
#67267 = DIRECTION('center_axis',(0.,-1.,0.)) ;
#67268 = DIRECTION('ref_axis',(-1.,0.,0.)) ;
#67269 = DIRECTION('center_axis',(0.,-1.,0.)) ;
#67270 = DIRECTION('ref_axis',(-1.,0.,0.)) ;
#67271 = DIRECTION('center_axis',(0.,-1.,0.)) ;
#67272 = DIRECTION('ref_axis',(-1.,0.,0.)) ;
#67273 = DIRECTION('center_axis',(0.,-1.,0.)) ;
#67274 = DIRECTION('ref_axis',(0.457808359486171,0.,0.889050901796169)) ;
#67275 = DIRECTION('center_axis',(0.,-1.,0.)) ;
#67276 = DIRECTION('ref_axis',(-1.,0.,0.)) ;
#67277 = DIRECTION('center_axis',(0.,1.,0.)) ;
#67278 = DIRECTION('ref_axis',(0.,0.,1.)) ;
#67279 = DIRECTION('center_axis',(0.,1.,0.)) ;
#67280 = DIRECTION('ref_axis',(-1.,0.,0.)) ;
#67281 = DIRECTION('center_axis',(0.,1.,0.)) ;
#67282 = DIRECTION('ref_axis',(-1.,0.,0.)) ;
#67283 = DIRECTION('axis',(0.,0.,1.)) ;
#67284 = DIRECTION('refdir',(1.,0.,0.)) ;
#67285 = DIRECTION('center_axis',(0.,-1.,0.)) ;
#67286 = DIRECTION('ref_axis',(1.,0.,0.)) ;
#67287 = DIRECTION('center_axis',(0.,-1.,0.)) ;
#67288 = DIRECTION('ref_axis',(-1.,0.,0.)) ;
#67289 = DIRECTION('center_axis',(0.,0.,1.)) ;
#67290 = DIRECTION('ref_axis',(-1.,0.,0.)) ;
#67291 = DIRECTION('center_axis',(0.,-1.,0.)) ;
#67292 = DIRECTION('ref_axis',(1.,0.,0.)) ;
#67293 = DIRECTION('center_axis',(0.,1.,0.)) ;
#67294 = DIRECTION('ref_axis',(-1.,0.,0.)) ;
#67295 = DIRECTION('center_axis',(0.,-1.,0.)) ;
#67296 = DIRECTION('ref_axis',(0.,0.,-1.)) ;
#67297 = DIRECTION('center_axis',(0.,1.,0.)) ;
#67298 = DIRECTION('ref_axis',(-1.,0.,0.)) ;
#67299 = DIRECTION('center_axis',(1.,0.,0.)) ;
#67300 = DIRECTION('ref_axis',(0.,0.,1.)) ;
#67301 = DIRECTION('center_axis',(0.,1.,0.)) ;
#67302 = DIRECTION('ref_axis',(-1.,0.,0.)) ;
#67303 = DIRECTION('center_axis',(0.,1.,0.)) ;
#67304 = DIRECTION('ref_axis',(-1.,0.,0.)) ;
#67305 = DIRECTION('center_axis',(0.,1.,0.)) ;
#67306 = DIRECTION('ref_axis',(-1.,0.,0.)) ;
#67307 = DIRECTION('center_axis',(0.,-1.,0.)) ;
#67308 = DIRECTION('ref_axis',(-1.,0.,0.)) ;
#67309 = DIRECTION('center_axis',(0.,1.,0.)) ;
#67310 = DIRECTION('ref_axis',(-1.,0.,0.)) ;
#67311 = DIRECTION('center_axis',(0.,1.,0.)) ;
#67312 = DIRECTION('ref_axis',(-1.,0.,0.)) ;
#67313 = DIRECTION('center_axis',(0.,-1.,0.)) ;
#67314 = DIRECTION('ref_axis',(0.,0.,-1.)) ;
#67315 = DIRECTION('center_axis',(0.,-1.,0.)) ;
#67316 = DIRECTION('ref_axis',(-0.406305370818768,0.,0.913737350469939)) ;
#67317 = DIRECTION('center_axis',(0.,-1.,0.)) ;
#67318 = DIRECTION('ref_axis',(-0.453990499739547,0.,0.891006524188368)) ;
#67319 = DIRECTION('center_axis',(0.309016994374948,0.,-0.951056516295154)) ;
#67320 = DIRECTION('ref_axis',(-0.672498511963948,-0.707106781186557,-0.218508012224408)) ;
#67321 = DIRECTION('',(-0.309016994374947,0.,0.951056516295154)) ;
#67322 = DIRECTION('',(0.309016994374948,0.,-0.951056516295154)) ;
#67323 = DIRECTION('center_axis',(0.,-1.,0.)) ;
#67324 = DIRECTION('ref_axis',(-0.309016994374914,0.,0.951056516295165)) ;
#67325 = DIRECTION('center_axis',(0.,1.,0.)) ;
#67326 = DIRECTION('ref_axis',(-0.309016994374945,0.,0.951056516295154)) ;
#67327 = DIRECTION('center_axis',(0.,-1.,0.)) ;
#67328 = DIRECTION('ref_axis',(-0.309016994374945,0.,0.951056516295154)) ;
#67329 = DIRECTION('center_axis',(-0.309016994374948,0.,0.951056516295154)) ;
#67330 = DIRECTION('ref_axis',(0.672498511963948,-0.707106781186557,0.218508012224408)) ;
#67331 = DIRECTION('',(0.309016994374948,0.,-0.951056516295154)) ;
#67332 = DIRECTION('',(-0.309016994374948,0.,0.951056516295154)) ;
#67333 = DIRECTION('center_axis',(0.,-1.,0.)) ;
#67334 = DIRECTION('ref_axis',(0.,0.,-1.)) ;
#67335 = DIRECTION('center_axis',(0.,-1.,0.)) ;
#67336 = DIRECTION('ref_axis',(-0.406305370818768,0.,0.913737350469939)) ;
#67337 = DIRECTION('center_axis',(0.,-1.,0.)) ;
#67338 = DIRECTION('ref_axis',(-0.156434465040232,0.,0.987688340595138)) ;
#67339 = DIRECTION('center_axis',(1.11022302462516E-16,0.,-1.)) ;
#67340 = DIRECTION('ref_axis',(-0.707106781186527,-0.707106781186568,-7.85046229341867E-17)) ;
#67341 = DIRECTION('',(-1.11022302462516E-16,0.,1.)) ;
#67342 = DIRECTION('',(1.11022302462516E-16,0.,-1.)) ;
#67343 = DIRECTION('center_axis',(0.,-1.,0.)) ;
#67344 = DIRECTION('ref_axis',(-9.9475983006414E-14,0.,1.)) ;
#67345 = DIRECTION('center_axis',(0.,1.,0.)) ;
#67346 = DIRECTION('ref_axis',(0.,0.,1.)) ;
#67347 = DIRECTION('center_axis',(0.,-1.,0.)) ;
#67348 = DIRECTION('ref_axis',(0.,0.,1.)) ;
#67349 = DIRECTION('center_axis',(-1.11022302462516E-16,0.,1.)) ;
#67350 = DIRECTION('ref_axis',(0.707106781186506,-0.707106781186589,7.85046229341844E-17)) ;
#67351 = DIRECTION('',(1.11022302462516E-16,0.,-1.)) ;
#67352 = DIRECTION('',(-1.11022302462516E-16,0.,1.)) ;
#67353 = DIRECTION('center_axis',(0.,-1.,0.)) ;
#67354 = DIRECTION('ref_axis',(0.,0.,-1.)) ;
#67355 = DIRECTION('center_axis',(0.,-1.,0.)) ;
#67356 = DIRECTION('ref_axis',(-0.406305370818768,0.,0.913737350469939)) ;
#67357 = DIRECTION('center_axis',(0.,-1.,0.)) ;
#67358 = DIRECTION('ref_axis',(0.156434465040233,0.,0.987688340595137)) ;
#67359 = DIRECTION('center_axis',(-0.309016994374947,0.,-0.951056516295154)) ;
#67360 = DIRECTION('ref_axis',(-0.672498511963948,-0.707106781186557,0.218508012224407)) ;
#67361 = DIRECTION('',(0.309016994374947,0.,0.951056516295154)) ;
#67362 = DIRECTION('',(-0.309016994374947,0.,-0.951056516295154)) ;
#67363 = DIRECTION('center_axis',(0.,-1.,0.)) ;
#67364 = DIRECTION('ref_axis',(0.309016994374783,0.,0.951056516295207)) ;
#67365 = DIRECTION('center_axis',(0.,1.,0.)) ;
#67366 = DIRECTION('ref_axis',(0.309016994374945,0.,0.951056516295154)) ;
#67367 = DIRECTION('center_axis',(0.,-1.,0.)) ;
#67368 = DIRECTION('ref_axis',(0.309016994374945,0.,0.951056516295154)) ;
#67369 = DIRECTION('center_axis',(0.309016994374947,0.,0.951056516295154)) ;
#67370 = DIRECTION('ref_axis',(0.672498511963948,-0.707106781186557,-0.218508012224407)) ;
#67371 = DIRECTION('',(-0.309016994374947,0.,-0.951056516295154)) ;
#67372 = DIRECTION('',(0.309016994374947,0.,0.951056516295154)) ;
#67373 = DIRECTION('center_axis',(0.,-1.,0.)) ;
#67374 = DIRECTION('ref_axis',(0.,0.,-1.)) ;
#67375 = DIRECTION('center_axis',(0.,-1.,0.)) ;
#67376 = DIRECTION('ref_axis',(-0.406305370818768,0.,0.913737350469939)) ;
#67377 = DIRECTION('center_axis',(0.,-1.,0.)) ;
#67378 = DIRECTION('ref_axis',(0.453990499739549,0.,0.891006524188367)) ;
#67379 = DIRECTION('center_axis',(-0.587785252292473,0.,-0.809016994374948)) ;
#67380 = DIRECTION('ref_axis',(-0.572061402817695,-0.707106781186534,0.415626937777461)) ;
#67381 = DIRECTION('',(0.587785252292473,0.,0.809016994374948)) ;
#67382 = DIRECTION('',(-0.587785252292473,0.,-0.809016994374947)) ;
#67383 = DIRECTION('center_axis',(0.,-1.,0.)) ;
#67384 = DIRECTION('ref_axis',(0.587785252292717,0.,0.80901699437477)) ;
#67385 = DIRECTION('center_axis',(0.,1.,0.)) ;
#67386 = DIRECTION('ref_axis',(0.587785252292468,0.,0.809016994374951)) ;
#67387 = DIRECTION('center_axis',(0.,-1.,0.)) ;
#67388 = DIRECTION('ref_axis',(0.587785252292468,0.,0.809016994374951)) ;
#67389 = DIRECTION('center_axis',(0.587785252292473,0.,0.809016994374948)) ;
#67390 = DIRECTION('ref_axis',(0.572061402817668,-0.707106781186568,-0.415626937777441)) ;
#67391 = DIRECTION('',(-0.587785252292473,0.,-0.809016994374947)) ;
#67392 = DIRECTION('',(0.587785252292473,0.,0.809016994374947)) ;
#67393 = DIRECTION('center_axis',(0.,-1.,0.)) ;
#67394 = DIRECTION('ref_axis',(0.,0.,-1.)) ;
#67395 = DIRECTION('center_axis',(0.,-1.,0.)) ;
#67396 = DIRECTION('ref_axis',(-0.406305370818768,0.,0.913737350469939)) ;
#67397 = DIRECTION('center_axis',(0.,-1.,0.)) ;
#67398 = DIRECTION('ref_axis',(0.70710678118655,0.,0.707106781186545)) ;
#67399 = DIRECTION('center_axis',(-0.809016994374947,0.,-0.587785252292473)) ;
#67400 = DIRECTION('ref_axis',(-0.415626937777452,-0.707106781186551,0.572061402817681)) ;
#67401 = DIRECTION('',(0.809016994374947,0.,0.587785252292473)) ;
#67402 = DIRECTION('',(-0.809016994374947,0.,-0.587785252292473)) ;
#67403 = DIRECTION('center_axis',(0.,-1.,0.)) ;
#67404 = DIRECTION('ref_axis',(0.809016994375165,0.,0.587785252292174)) ;
#67405 = DIRECTION('center_axis',(0.,1.,0.)) ;
#67406 = DIRECTION('ref_axis',(0.809016994374947,0.,0.587785252292474)) ;
#67407 = DIRECTION('center_axis',(0.,-1.,0.)) ;
#67408 = DIRECTION('ref_axis',(0.809016994374947,0.,0.587785252292474)) ;
#67409 = DIRECTION('center_axis',(0.809016994374947,0.,0.587785252292473)) ;
#67410 = DIRECTION('ref_axis',(0.415626937777427,-0.707106781186592,-0.572061402817648)) ;
#67411 = DIRECTION('',(-0.809016994374947,0.,-0.587785252292473)) ;
#67412 = DIRECTION('',(0.809016994374947,0.,0.587785252292473)) ;
#67413 = DIRECTION('center_axis',(0.,-1.,0.)) ;
#67414 = DIRECTION('ref_axis',(0.,0.,-1.)) ;
#67415 = DIRECTION('center_axis',(0.,-1.,0.)) ;
#67416 = DIRECTION('ref_axis',(-0.406305370818768,0.,0.913737350469939)) ;
#67417 = DIRECTION('center_axis',(0.,-1.,0.)) ;
#67418 = DIRECTION('ref_axis',(0.891006524188368,0.,0.453990499739546)) ;
#67419 = DIRECTION('center_axis',(-0.951056516295154,0.,-0.309016994374948)) ;
#67420 = DIRECTION('ref_axis',(-0.2185080122244,-0.707106781186583,0.672498511963923)) ;
#67421 = DIRECTION('',(0.951056516295153,0.,0.309016994374948)) ;
#67422 = DIRECTION('',(-0.951056516295153,0.,-0.309016994374948)) ;
#67423 = DIRECTION('center_axis',(0.,-1.,0.)) ;
#67424 = DIRECTION('ref_axis',(0.95105651629519,0.,0.309016994374834)) ;
#67425 = DIRECTION('center_axis',(0.,1.,0.)) ;
#67426 = DIRECTION('ref_axis',(0.951056516295153,0.,0.309016994374948)) ;
#67427 = DIRECTION('center_axis',(0.,-1.,0.)) ;
#67428 = DIRECTION('ref_axis',(0.951056516295153,0.,0.309016994374948)) ;
#67429 = DIRECTION('center_axis',(0.951056516295154,0.,0.309016994374948)) ;
#67430 = DIRECTION('ref_axis',(0.218508012224406,-0.707106781186563,-0.672498511963942)) ;
#67431 = DIRECTION('',(-0.951056516295153,0.,-0.309016994374948)) ;
#67432 = DIRECTION('',(0.951056516295153,0.,0.309016994374948)) ;
#67433 = DIRECTION('center_axis',(0.,-1.,0.)) ;
#67434 = DIRECTION('ref_axis',(0.,0.,-1.)) ;
#67435 = DIRECTION('center_axis',(0.,-1.,0.)) ;
#67436 = DIRECTION('ref_axis',(-0.406305370818768,0.,0.913737350469939)) ;
#67437 = DIRECTION('center_axis',(0.,-1.,0.)) ;
#67438 = DIRECTION('ref_axis',(0.987688340595138,0.,0.15643446504023)) ;
#67439 = DIRECTION('center_axis',(-1.,0.,-2.22044604925031E-16)) ;
#67440 = DIRECTION('ref_axis',(-1.57009245868373E-16,-0.707106781186568,0.707106781186527)) ;
#67441 = DIRECTION('',(1.,0.,2.22044604925031E-16)) ;
#67442 = DIRECTION('',(-1.,0.,-2.22044604925031E-16)) ;
#67443 = DIRECTION('center_axis',(0.,-1.,0.)) ;
#67444 = DIRECTION('ref_axis',(1.,0.,-1.49213974509621E-13)) ;
#67445 = DIRECTION('center_axis',(0.,1.,0.)) ;
#67446 = DIRECTION('ref_axis',(1.,0.,0.)) ;
#67447 = DIRECTION('center_axis',(0.,-1.,0.)) ;
#67448 = DIRECTION('ref_axis',(1.,0.,0.)) ;
#67449 = DIRECTION('center_axis',(1.,0.,2.22044604925031E-16)) ;
#67450 = DIRECTION('ref_axis',(1.57009245868373E-16,-0.707106781186568,-0.707106781186527)) ;
#67451 = DIRECTION('',(-1.,0.,-2.22044604925031E-16)) ;
#67452 = DIRECTION('',(1.,0.,2.22044604925031E-16)) ;
#67453 = DIRECTION('center_axis',(0.,-1.,0.)) ;
#67454 = DIRECTION('ref_axis',(0.,0.,-1.)) ;
#67455 = DIRECTION('center_axis',(0.,-1.,0.)) ;
#67456 = DIRECTION('ref_axis',(-0.406305370818768,0.,0.913737350469939)) ;
#67457 = DIRECTION('center_axis',(0.,-1.,0.)) ;
#67458 = DIRECTION('ref_axis',(0.987688340595138,0.,-0.156434465040229)) ;
#67459 = DIRECTION('center_axis',(-0.951056516295154,0.,0.309016994374947)) ;
#67460 = DIRECTION('ref_axis',(0.218508012224405,-0.707106781186563,0.672498511963943)) ;
#67461 = DIRECTION('',(0.951056516295154,0.,-0.309016994374947)) ;
#67462 = DIRECTION('',(-0.951056516295154,0.,0.309016994374947)) ;
#67463 = DIRECTION('center_axis',(0.,-1.,0.)) ;
#67464 = DIRECTION('ref_axis',(0.,0.,-1.)) ;
#67465 = DIRECTION('center_axis',(0.,1.,0.)) ;
#67466 = DIRECTION('ref_axis',(0.951056516295153,0.,-0.309016994374948)) ;
#67467 = DIRECTION('center_axis',(0.,-1.,0.)) ;
#67468 = DIRECTION('ref_axis',(0.951056516295153,0.,-0.309016994374948)) ;
#67469 = DIRECTION('center_axis',(0.951056516295154,0.,-0.309016994374947)) ;
#67470 = DIRECTION('ref_axis',(-0.218508012224405,-0.707106781186563,-0.672498511963943)) ;
#67471 = DIRECTION('',(-0.951056516295154,0.,0.309016994374947)) ;
#67472 = DIRECTION('',(0.951056516295154,0.,-0.309016994374947)) ;
#67473 = DIRECTION('center_axis',(0.,-1.,0.)) ;
#67474 = DIRECTION('ref_axis',(0.,0.,-1.)) ;
#67475 = DIRECTION('center_axis',(0.,-1.,0.)) ;
#67476 = DIRECTION('ref_axis',(-0.406305370818768,0.,0.913737350469939)) ;
#67477 = DIRECTION('center_axis',(0.,-1.,0.)) ;
#67478 = DIRECTION('ref_axis',(0.891006524188368,0.,-0.453990499739547)) ;
#67479 = DIRECTION('center_axis',(-0.809016994374948,0.,0.587785252292473)) ;
#67480 = DIRECTION('ref_axis',(0.415626937777451,-0.707106781186551,0.572061402817682)) ;
#67481 = DIRECTION('',(0.809016994374948,0.,-0.587785252292473)) ;
#67482 = DIRECTION('',(-0.809016994374948,0.,0.587785252292473)) ;
#67483 = DIRECTION('center_axis',(0.,-1.,0.)) ;
#67484 = DIRECTION('ref_axis',(0.,0.,-1.)) ;
#67485 = DIRECTION('center_axis',(0.,1.,0.)) ;
#67486 = DIRECTION('ref_axis',(0.809016994374947,0.,-0.587785252292474)) ;
#67487 = DIRECTION('center_axis',(0.,-1.,0.)) ;
#67488 = DIRECTION('ref_axis',(0.809016994374947,0.,-0.587785252292474)) ;
#67489 = DIRECTION('center_axis',(0.809016994374948,0.,-0.587785252292473)) ;
#67490 = DIRECTION('ref_axis',(-0.415626937777437,-0.707106781186575,-0.572061402817662)) ;
#67491 = DIRECTION('',(-0.809016994374948,0.,0.587785252292473)) ;
#67492 = DIRECTION('',(0.809016994374948,0.,-0.587785252292473)) ;
#67493 = DIRECTION('center_axis',(0.,-1.,0.)) ;
#67494 = DIRECTION('ref_axis',(0.,0.,-1.)) ;
#67495 = DIRECTION('center_axis',(0.,-1.,0.)) ;
#67496 = DIRECTION('ref_axis',(-0.406305370818768,0.,0.913737350469939)) ;
#67497 = DIRECTION('center_axis',(0.,-1.,0.)) ;
#67498 = DIRECTION('ref_axis',(0.707106781186547,0.,-0.707106781186547)) ;
#67499 = DIRECTION('center_axis',(-0.587785252292473,0.,0.809016994374947)) ;
#67500 = DIRECTION('ref_axis',(0.572061402817686,-0.707106781186546,0.415626937777454)) ;
#67501 = DIRECTION('',(0.587785252292473,0.,-0.809016994374947)) ;
#67502 = DIRECTION('',(-0.587785252292473,0.,0.809016994374947)) ;
#67503 = DIRECTION('center_axis',(0.,-1.,0.)) ;
#67504 = DIRECTION('ref_axis',(0.,0.,-1.)) ;
#67505 = DIRECTION('center_axis',(0.,1.,0.)) ;
#67506 = DIRECTION('ref_axis',(0.587785252292468,0.,-0.809016994374951)) ;
#67507 = DIRECTION('center_axis',(0.,-1.,0.)) ;
#67508 = DIRECTION('ref_axis',(0.587785252292468,0.,-0.809016994374951)) ;
#67509 = DIRECTION('center_axis',(0.587785252292473,0.,-0.809016994374947)) ;
#67510 = DIRECTION('ref_axis',(-0.572061402817695,-0.707106781186534,-0.415626937777461)) ;
#67511 = DIRECTION('',(-0.587785252292473,0.,0.809016994374947)) ;
#67512 = DIRECTION('',(0.587785252292473,0.,-0.809016994374947)) ;
#67513 = DIRECTION('center_axis',(0.,-1.,0.)) ;
#67514 = DIRECTION('ref_axis',(0.,0.,-1.)) ;
#67515 = DIRECTION('center_axis',(0.,-1.,0.)) ;
#67516 = DIRECTION('ref_axis',(-0.406305370818768,0.,0.913737350469939)) ;
#67517 = DIRECTION('center_axis',(0.,-1.,0.)) ;
#67518 = DIRECTION('ref_axis',(0.453990499739547,0.,-0.891006524188368)) ;
#67519 = DIRECTION('center_axis',(-0.309016994374948,0.,0.951056516295154)) ;
#67520 = DIRECTION('ref_axis',(0.672498511963948,-0.707106781186557,0.218508012224408)) ;
#67521 = DIRECTION('',(-0.309016994374948,0.,0.951056516295153)) ;
#67522 = DIRECTION('',(0.309016994374948,0.,-0.951056516295153)) ;
#67523 = DIRECTION('center_axis',(0.,-1.,0.)) ;
#67524 = DIRECTION('ref_axis',(0.,0.,-1.)) ;
#67525 = DIRECTION('center_axis',(0.,-1.,0.)) ;
#67526 = DIRECTION('ref_axis',(0.309016994374945,0.,-0.951056516295154)) ;
#67527 = DIRECTION('center_axis',(0.,1.,0.)) ;
#67528 = DIRECTION('ref_axis',(0.309016994374945,0.,-0.951056516295154)) ;
#67529 = DIRECTION('center_axis',(0.309016994374948,0.,-0.951056516295154)) ;
#67530 = DIRECTION('ref_axis',(-0.672498511963948,-0.707106781186557,-0.218508012224408)) ;
#67531 = DIRECTION('',(0.309016994374948,0.,-0.951056516295153)) ;
#67532 = DIRECTION('',(-0.309016994374948,0.,0.951056516295153)) ;
#67533 = DIRECTION('center_axis',(0.,-1.,0.)) ;
#67534 = DIRECTION('ref_axis',(0.,0.,-1.)) ;
#67535 = DIRECTION('center_axis',(0.,-1.,0.)) ;
#67536 = DIRECTION('ref_axis',(0.156434465040232,0.,-0.987688340595138)) ;
#67537 = DIRECTION('center_axis',(0.,-1.,0.)) ;
#67538 = DIRECTION('ref_axis',(-0.406305370818768,0.,0.913737350469939)) ;
#67539 = DIRECTION('center_axis',(0.,0.,1.)) ;
#67540 = DIRECTION('ref_axis',(0.707106781186506,-0.707106781186589,0.)) ;
#67541 = DIRECTION('',(0.,0.,1.)) ;
#67542 = DIRECTION('',(0.,0.,-1.)) ;
#67543 = DIRECTION('center_axis',(0.,-1.,0.)) ;
#67544 = DIRECTION('ref_axis',(0.,0.,-1.)) ;
#67545 = DIRECTION('center_axis',(0.,-1.,0.)) ;
#67546 = DIRECTION('ref_axis',(0.,0.,-1.)) ;
#67547 = DIRECTION('center_axis',(0.,1.,0.)) ;
#67548 = DIRECTION('ref_axis',(0.,0.,-1.)) ;
#67549 = DIRECTION('center_axis',(0.,0.,-1.)) ;
#67550 = DIRECTION('ref_axis',(-0.707106781186527,-0.707106781186568,0.)) ;
#67551 = DIRECTION('',(0.,0.,-1.)) ;
#67552 = DIRECTION('',(0.,0.,1.)) ;
#67553 = DIRECTION('center_axis',(0.,-1.,0.)) ;
#67554 = DIRECTION('ref_axis',(0.,0.,-1.)) ;
#67555 = DIRECTION('center_axis',(0.,-1.,0.)) ;
#67556 = DIRECTION('ref_axis',(-0.156434465040231,0.,-0.987688340595138)) ;
#67557 = DIRECTION('center_axis',(0.,-1.,0.)) ;
#67558 = DIRECTION('ref_axis',(-0.406305370818768,0.,0.913737350469939)) ;
#67559 = DIRECTION('center_axis',(0.309016994374947,0.,0.951056516295154)) ;
#67560 = DIRECTION('ref_axis',(0.672498511963948,-0.707106781186557,-0.218508012224407)) ;
#67561 = DIRECTION('',(0.309016994374947,0.,0.951056516295154)) ;
#67562 = DIRECTION('',(-0.309016994374947,0.,-0.951056516295154)) ;
#67563 = DIRECTION('center_axis',(0.,-1.,0.)) ;
#67564 = DIRECTION('ref_axis',(0.,0.,-1.)) ;
#67565 = DIRECTION('center_axis',(0.,-1.,0.)) ;
#67566 = DIRECTION('ref_axis',(-0.309016994374945,0.,-0.951056516295154)) ;
#67567 = DIRECTION('center_axis',(0.,1.,0.)) ;
#67568 = DIRECTION('ref_axis',(-0.309016994374945,0.,-0.951056516295154)) ;
#67569 = DIRECTION('center_axis',(-0.309016994374947,0.,-0.951056516295154)) ;
#67570 = DIRECTION('ref_axis',(-0.672498511963948,-0.707106781186557,0.218508012224407)) ;
#67571 = DIRECTION('',(-0.309016994374947,0.,-0.951056516295154)) ;
#67572 = DIRECTION('',(0.309016994374947,0.,0.951056516295154)) ;
#67573 = DIRECTION('center_axis',(0.,-1.,0.)) ;
#67574 = DIRECTION('ref_axis',(0.,0.,-1.)) ;
#67575 = DIRECTION('center_axis',(0.,-1.,0.)) ;
#67576 = DIRECTION('ref_axis',(-0.453990499739546,0.,-0.891006524188368)) ;
#67577 = DIRECTION('center_axis',(0.,-1.,0.)) ;
#67578 = DIRECTION('ref_axis',(-0.406305370818768,0.,0.913737350469939)) ;
#67579 = DIRECTION('center_axis',(0.587785252292473,0.,0.809016994374948)) ;
#67580 = DIRECTION('ref_axis',(0.572061402817682,-0.707106781186551,-0.415626937777451)) ;
#67581 = DIRECTION('',(0.587785252292473,0.,0.809016994374947)) ;
#67582 = DIRECTION('',(-0.587785252292473,0.,-0.809016994374947)) ;
#67583 = DIRECTION('center_axis',(0.,-1.,0.)) ;
#67584 = DIRECTION('ref_axis',(0.,0.,-1.)) ;
#67585 = DIRECTION('center_axis',(0.,-1.,0.)) ;
#67586 = DIRECTION('ref_axis',(-0.587785252292474,0.,-0.809016994374947)) ;
#67587 = DIRECTION('center_axis',(0.,1.,0.)) ;
#67588 = DIRECTION('ref_axis',(-0.587785252292474,0.,-0.809016994374947)) ;
#67589 = DIRECTION('center_axis',(-0.587785252292473,0.,-0.809016994374948)) ;
#67590 = DIRECTION('ref_axis',(-0.572061402817672,-0.707106781186563,0.415626937777444)) ;
#67591 = DIRECTION('',(-0.587785252292473,0.,-0.809016994374947)) ;
#67592 = DIRECTION('',(0.587785252292473,0.,0.809016994374947)) ;
#67593 = DIRECTION('center_axis',(0.,-1.,0.)) ;
#67594 = DIRECTION('ref_axis',(0.,0.,-1.)) ;
#67595 = DIRECTION('center_axis',(0.,-1.,0.)) ;
#67596 = DIRECTION('ref_axis',(-0.707106781186547,0.,-0.707106781186548)) ;
#67597 = DIRECTION('center_axis',(0.,-1.,0.)) ;
#67598 = DIRECTION('ref_axis',(-0.406305370818768,0.,0.913737350469939)) ;
#67599 = DIRECTION('center_axis',(0.809016994374947,0.,0.587785252292473)) ;
#67600 = DIRECTION('ref_axis',(0.415626937777442,-0.707106781186568,-0.572061402817668)) ;
#67601 = DIRECTION('',(0.809016994374947,0.,0.587785252292473)) ;
#67602 = DIRECTION('',(-0.809016994374947,0.,-0.587785252292473)) ;
#67603 = DIRECTION('center_axis',(0.,-1.,0.)) ;
#67604 = DIRECTION('ref_axis',(0.,0.,-1.)) ;
#67605 = DIRECTION('center_axis',(0.,-1.,0.)) ;
#67606 = DIRECTION('ref_axis',(-0.809016994374947,0.,-0.587785252292474)) ;
#67607 = DIRECTION('center_axis',(0.,1.,0.)) ;
#67608 = DIRECTION('ref_axis',(-0.809016994374947,0.,-0.587785252292474)) ;
#67609 = DIRECTION('center_axis',(-0.809016994374947,0.,-0.587785252292473)) ;
#67610 = DIRECTION('ref_axis',(-0.415626937777444,-0.707106781186563,0.572061402817672)) ;
#67611 = DIRECTION('',(-0.809016994374947,0.,-0.587785252292473)) ;
#67612 = DIRECTION('',(0.809016994374947,0.,0.587785252292473)) ;
#67613 = DIRECTION('center_axis',(0.,-1.,0.)) ;
#67614 = DIRECTION('ref_axis',(0.,0.,-1.)) ;
#67615 = DIRECTION('center_axis',(0.,-1.,0.)) ;
#67616 = DIRECTION('ref_axis',(-0.891006524188368,0.,-0.453990499739547)) ;
#67617 = DIRECTION('center_axis',(0.,-1.,0.)) ;
#67618 = DIRECTION('ref_axis',(-0.406305370818768,0.,0.913737350469939)) ;
#67619 = DIRECTION('center_axis',(0.951056516295154,0.,0.309016994374948)) ;
#67620 = DIRECTION('ref_axis',(0.218508012224408,-0.707106781186557,-0.672498511963948)) ;
#67621 = DIRECTION('',(0.951056516295154,0.,0.309016994374948)) ;
#67622 = DIRECTION('',(-0.951056516295154,0.,-0.309016994374948)) ;
#67623 = DIRECTION('center_axis',(0.,-1.,0.)) ;
#67624 = DIRECTION('ref_axis',(0.,0.,-1.)) ;
#67625 = DIRECTION('center_axis',(0.,-1.,0.)) ;
#67626 = DIRECTION('ref_axis',(-0.951056516295154,0.,-0.309016994374945)) ;
#67627 = DIRECTION('center_axis',(0.,1.,0.)) ;
#67628 = DIRECTION('ref_axis',(-0.951056516295154,0.,-0.309016994374945)) ;
#67629 = DIRECTION('center_axis',(-0.951056516295154,0.,-0.309016994374948)) ;
#67630 = DIRECTION('ref_axis',(-0.218508012224408,-0.707106781186557,0.672498511963948)) ;
#67631 = DIRECTION('',(-0.951056516295154,0.,-0.309016994374948)) ;
#67632 = DIRECTION('',(0.951056516295154,0.,0.309016994374948)) ;
#67633 = DIRECTION('center_axis',(0.,-1.,0.)) ;
#67634 = DIRECTION('ref_axis',(0.,0.,-1.)) ;
#67635 = DIRECTION('center_axis',(0.,-1.,0.)) ;
#67636 = DIRECTION('ref_axis',(-0.987688340595138,0.,-0.156434465040231)) ;
#67637 = DIRECTION('center_axis',(0.,-1.,0.)) ;
#67638 = DIRECTION('ref_axis',(-0.406305370818768,0.,0.913737350469939)) ;
#67639 = DIRECTION('center_axis',(1.,0.,5.55111512312578E-17)) ;
#67640 = DIRECTION('ref_axis',(3.92523114670932E-17,-0.707106781186568,-0.707106781186527)) ;
#67641 = DIRECTION('',(1.,0.,5.55111512312578E-17)) ;
#67642 = DIRECTION('',(-1.,0.,-5.55111512312578E-17)) ;
#67643 = DIRECTION('center_axis',(0.,-1.,0.)) ;
#67644 = DIRECTION('ref_axis',(-1.,0.,4.90274487674469E-13)) ;
#67645 = DIRECTION('center_axis',(0.,-1.,0.)) ;
#67646 = DIRECTION('ref_axis',(-1.,0.,0.)) ;
#67647 = DIRECTION('center_axis',(0.,1.,0.)) ;
#67648 = DIRECTION('ref_axis',(-1.,0.,0.)) ;
#67649 = DIRECTION('center_axis',(-1.,0.,-5.55111512312578E-17)) ;
#67650 = DIRECTION('ref_axis',(-3.92523114670932E-17,-0.707106781186568,0.707106781186527)) ;
#67651 = DIRECTION('',(-1.,0.,-5.55111512312578E-17)) ;
#67652 = DIRECTION('',(1.,0.,5.55111512312578E-17)) ;
#67653 = DIRECTION('center_axis',(0.,-1.,0.)) ;
#67654 = DIRECTION('ref_axis',(0.,0.,-1.)) ;
#67655 = DIRECTION('center_axis',(0.,-1.,0.)) ;
#67656 = DIRECTION('ref_axis',(-0.987688340595138,0.,0.156434465040229)) ;
#67657 = DIRECTION('center_axis',(0.,-1.,0.)) ;
#67658 = DIRECTION('ref_axis',(-0.406305370818768,0.,0.913737350469939)) ;
#67659 = DIRECTION('center_axis',(0.951056516295154,0.,-0.309016994374947)) ;
#67660 = DIRECTION('ref_axis',(-0.218508012224407,-0.707106781186557,-0.672498511963948)) ;
#67661 = DIRECTION('',(0.951056516295154,0.,-0.309016994374947)) ;
#67662 = DIRECTION('',(-0.951056516295154,0.,0.309016994374947)) ;
#67663 = DIRECTION('center_axis',(0.,-1.,0.)) ;
#67664 = DIRECTION('ref_axis',(-0.951056516295038,0.,0.309016994375305)) ;
#67665 = DIRECTION('center_axis',(0.,-1.,0.)) ;
#67666 = DIRECTION('ref_axis',(-0.951056516295154,0.,0.309016994374945)) ;
#67667 = DIRECTION('center_axis',(0.,1.,0.)) ;
#67668 = DIRECTION('ref_axis',(-0.951056516295154,0.,0.309016994374945)) ;
#67669 = DIRECTION('center_axis',(-0.951056516295154,0.,0.309016994374947)) ;
#67670 = DIRECTION('ref_axis',(0.218508012224407,-0.707106781186557,0.672498511963948)) ;
#67671 = DIRECTION('',(-0.951056516295154,0.,0.309016994374947)) ;
#67672 = DIRECTION('',(0.951056516295154,0.,-0.309016994374947)) ;
#67673 = DIRECTION('center_axis',(0.,-1.,0.)) ;
#67674 = DIRECTION('ref_axis',(0.,0.,-1.)) ;
#67675 = DIRECTION('center_axis',(0.,-1.,0.)) ;
#67676 = DIRECTION('ref_axis',(-0.891006524188369,0.,0.453990499739545)) ;
#67677 = DIRECTION('center_axis',(0.,-1.,0.)) ;
#67678 = DIRECTION('ref_axis',(-0.406305370818768,0.,0.913737350469939)) ;
#67679 = DIRECTION('center_axis',(0.809016994374948,0.,-0.587785252292473)) ;
#67680 = DIRECTION('ref_axis',(-0.415626937777444,-0.707106781186563,-0.572061402817672)) ;
#67681 = DIRECTION('',(0.809016994374947,0.,-0.587785252292473)) ;
#67682 = DIRECTION('',(-0.809016994374947,0.,0.587785252292473)) ;
#67683 = DIRECTION('center_axis',(0.,-1.,0.)) ;
#67684 = DIRECTION('ref_axis',(-0.809016994374941,0.,0.587785252292482)) ;
#67685 = DIRECTION('center_axis',(0.,-1.,0.)) ;
#67686 = DIRECTION('ref_axis',(-0.809016994374947,0.,0.587785252292474)) ;
#67687 = DIRECTION('center_axis',(0.,1.,0.)) ;
#67688 = DIRECTION('ref_axis',(-0.809016994374947,0.,0.587785252292474)) ;
#67689 = DIRECTION('center_axis',(-0.809016994374948,0.,0.587785252292473)) ;
#67690 = DIRECTION('ref_axis',(0.415626937777444,-0.707106781186563,0.572061402817672)) ;
#67691 = DIRECTION('',(-0.809016994374947,0.,0.587785252292473)) ;
#67692 = DIRECTION('',(0.809016994374947,0.,-0.587785252292473)) ;
#67693 = DIRECTION('center_axis',(0.,-1.,0.)) ;
#67694 = DIRECTION('ref_axis',(0.,0.,-1.)) ;
#67695 = DIRECTION('center_axis',(0.,-1.,0.)) ;
#67696 = DIRECTION('ref_axis',(-0.707106781186548,0.,0.707106781186547)) ;
#67697 = DIRECTION('center_axis',(0.,-1.,0.)) ;
#67698 = DIRECTION('ref_axis',(-0.406305370818768,0.,0.913737350469939)) ;
#67699 = DIRECTION('center_axis',(0.587785252292473,0.,-0.809016994374947)) ;
#67700 = DIRECTION('ref_axis',(-0.572061402817681,-0.707106781186551,-0.415626937777452)) ;
#67701 = DIRECTION('',(0.587785252292473,0.,-0.809016994374947)) ;
#67702 = DIRECTION('',(-0.587785252292473,0.,0.809016994374947)) ;
#67703 = DIRECTION('center_axis',(0.,-1.,0.)) ;
#67704 = DIRECTION('ref_axis',(-0.587785252292018,0.,0.809016994375278)) ;
#67705 = DIRECTION('center_axis',(0.,-1.,0.)) ;
#67706 = DIRECTION('ref_axis',(-0.587785252292474,0.,0.809016994374947)) ;
#67707 = DIRECTION('center_axis',(0.,1.,0.)) ;
#67708 = DIRECTION('ref_axis',(-0.587785252292474,0.,0.809016994374947)) ;
#67709 = DIRECTION('center_axis',(-0.587785252292473,0.,0.809016994374947)) ;
#67710 = DIRECTION('ref_axis',(0.572061402817672,-0.707106781186563,0.415626937777444)) ;
#67711 = DIRECTION('',(-0.587785252292473,0.,0.809016994374947)) ;
#67712 = DIRECTION('',(0.587785252292473,0.,-0.809016994374947)) ;
#67713 = DIRECTION('center_axis',(0.951056516295154,0.,0.309016994374948)) ;
#67714 = DIRECTION('ref_axis',(-0.309016994374948,0.,0.951056516295153)) ;
#67715 = DIRECTION('',(0.,-1.,0.)) ;
#67716 = DIRECTION('',(0.309016994374948,0.,-0.951056516295153)) ;
#67717 = DIRECTION('',(0.,1.,0.)) ;
#67718 = DIRECTION('center_axis',(0.,-1.,0.)) ;
#67719 = DIRECTION('ref_axis',(0.309016994374938,0.,-0.951056516295157)) ;
#67720 = DIRECTION('',(0.,-1.,0.)) ;
#67721 = DIRECTION('center_axis',(0.,1.,0.)) ;
#67722 = DIRECTION('ref_axis',(0.309016994374945,0.,-0.951056516295154)) ;
#67723 = DIRECTION('center_axis',(-0.951056516295154,0.,-0.309016994374948)) ;
#67724 = DIRECTION('ref_axis',(0.309016994374948,0.,-0.951056516295153)) ;
#67725 = DIRECTION('',(0.,-1.,0.)) ;
#67726 = DIRECTION('',(-0.309016994374948,0.,0.951056516295153)) ;
#67727 = DIRECTION('center_axis',(0.,-1.,0.)) ;
#67728 = DIRECTION('ref_axis',(-1.,0.,0.)) ;
#67729 = DIRECTION('',(0.,1.,0.)) ;
#67730 = DIRECTION('center_axis',(0.,1.,0.)) ;
#67731 = DIRECTION('ref_axis',(0.156434465040232,0.,-0.987688340595138)) ;
#67732 = DIRECTION('center_axis',(1.,0.,0.)) ;
#67733 = DIRECTION('ref_axis',(0.,0.,1.)) ;
#67734 = DIRECTION('',(0.,-1.,0.)) ;
#67735 = DIRECTION('',(0.,0.,-1.)) ;
#67736 = DIRECTION('center_axis',(0.,-1.,0.)) ;
#67737 = DIRECTION('ref_axis',(-4.50212443845799E-15,0.,-1.)) ;
#67738 = DIRECTION('',(0.,-1.,0.)) ;
#67739 = DIRECTION('center_axis',(0.,1.,0.)) ;
#67740 = DIRECTION('ref_axis',(0.,0.,-1.)) ;
#67741 = DIRECTION('center_axis',(-1.,0.,0.)) ;
#67742 = DIRECTION('ref_axis',(0.,0.,-1.)) ;
#67743 = DIRECTION('',(0.,-1.,0.)) ;
#67744 = DIRECTION('',(0.,0.,1.)) ;
#67745 = DIRECTION('center_axis',(0.,-1.,0.)) ;
#67746 = DIRECTION('ref_axis',(-1.,0.,0.)) ;
#67747 = DIRECTION('',(0.,1.,0.)) ;
#67748 = DIRECTION('center_axis',(0.,1.,0.)) ;
#67749 = DIRECTION('ref_axis',(-0.15643446504023,0.,-0.987688340595138)) ;
#67750 = DIRECTION('center_axis',(0.951056516295154,0.,-0.309016994374947)) ;
#67751 = DIRECTION('ref_axis',(0.309016994374947,0.,0.951056516295154)) ;
#67752 = DIRECTION('',(0.,-1.,0.)) ;
#67753 = DIRECTION('',(-0.309016994374947,0.,-0.951056516295154)) ;
#67754 = DIRECTION('center_axis',(0.,-1.,0.)) ;
#67755 = DIRECTION('ref_axis',(-0.309016994374953,0.,-0.951056516295152)) ;
#67756 = DIRECTION('',(0.,-1.,0.)) ;
#67757 = DIRECTION('center_axis',(0.,1.,0.)) ;
#67758 = DIRECTION('ref_axis',(-0.309016994374945,0.,-0.951056516295154)) ;
#67759 = DIRECTION('center_axis',(-0.951056516295154,0.,0.309016994374947)) ;
#67760 = DIRECTION('ref_axis',(-0.309016994374947,0.,-0.951056516295154)) ;
#67761 = DIRECTION('',(0.,-1.,0.)) ;
#67762 = DIRECTION('',(0.309016994374947,0.,0.951056516295154)) ;
#67763 = DIRECTION('center_axis',(0.,-1.,0.)) ;
#67764 = DIRECTION('ref_axis',(-1.,0.,0.)) ;
#67765 = DIRECTION('',(0.,1.,0.)) ;
#67766 = DIRECTION('center_axis',(0.,1.,0.)) ;
#67767 = DIRECTION('ref_axis',(-0.453990499739546,0.,-0.891006524188368)) ;
#67768 = DIRECTION('center_axis',(0.809016994374948,0.,-0.587785252292473)) ;
#67769 = DIRECTION('ref_axis',(0.587785252292473,0.,0.809016994374948)) ;
#67770 = DIRECTION('',(0.,-1.,0.)) ;
#67771 = DIRECTION('',(-0.587785252292473,0.,-0.809016994374947)) ;
#67772 = DIRECTION('center_axis',(0.,-1.,0.)) ;
#67773 = DIRECTION('ref_axis',(-0.587785252292477,0.,-0.809016994374945)) ;
#67774 = DIRECTION('',(0.,-1.,0.)) ;
#67775 = DIRECTION('center_axis',(0.,1.,0.)) ;
#67776 = DIRECTION('ref_axis',(-0.587785252292474,0.,-0.809016994374947)) ;
#67777 = DIRECTION('center_axis',(-0.809016994374948,0.,0.587785252292473)) ;
#67778 = DIRECTION('ref_axis',(-0.587785252292473,0.,-0.809016994374948)) ;
#67779 = DIRECTION('',(0.,-1.,0.)) ;
#67780 = DIRECTION('',(0.587785252292473,0.,0.809016994374947)) ;
#67781 = DIRECTION('center_axis',(0.,-1.,0.)) ;
#67782 = DIRECTION('ref_axis',(-1.,0.,0.)) ;
#67783 = DIRECTION('',(0.,1.,0.)) ;
#67784 = DIRECTION('center_axis',(0.,1.,0.)) ;
#67785 = DIRECTION('ref_axis',(-0.707106781186547,0.,-0.707106781186548)) ;
#67786 = DIRECTION('center_axis',(0.587785252292473,0.,-0.809016994374947)) ;
#67787 = DIRECTION('ref_axis',(0.809016994374947,0.,0.587785252292473)) ;
#67788 = DIRECTION('',(0.,-1.,0.)) ;
#67789 = DIRECTION('',(-0.809016994374947,0.,-0.587785252292473)) ;
#67790 = DIRECTION('center_axis',(0.,-1.,0.)) ;
#67791 = DIRECTION('ref_axis',(-0.809016994374942,0.,-0.587785252292481)) ;
#67792 = DIRECTION('',(0.,-1.,0.)) ;
#67793 = DIRECTION('center_axis',(0.,1.,0.)) ;
#67794 = DIRECTION('ref_axis',(-0.809016994374947,0.,-0.587785252292474)) ;
#67795 = DIRECTION('center_axis',(-0.587785252292473,0.,0.809016994374947)) ;
#67796 = DIRECTION('ref_axis',(-0.809016994374947,0.,-0.587785252292473)) ;
#67797 = DIRECTION('',(0.,-1.,0.)) ;
#67798 = DIRECTION('',(0.809016994374947,0.,0.587785252292473)) ;
#67799 = DIRECTION('center_axis',(0.,-1.,0.)) ;
#67800 = DIRECTION('ref_axis',(-1.,0.,0.)) ;
#67801 = DIRECTION('',(0.,1.,0.)) ;
#67802 = DIRECTION('center_axis',(0.,1.,0.)) ;
#67803 = DIRECTION('ref_axis',(-0.891006524188368,0.,-0.453990499739547)) ;
#67804 = DIRECTION('center_axis',(0.309016994374948,0.,-0.951056516295154)) ;
#67805 = DIRECTION('ref_axis',(0.951056516295154,0.,0.309016994374948)) ;
#67806 = DIRECTION('',(0.,-1.,0.)) ;
#67807 = DIRECTION('',(-0.951056516295154,0.,-0.309016994374948)) ;
#67808 = DIRECTION('center_axis',(0.,-1.,0.)) ;
#67809 = DIRECTION('ref_axis',(-0.951056516295152,0.,-0.309016994374953)) ;
#67810 = DIRECTION('',(0.,-1.,0.)) ;
#67811 = DIRECTION('center_axis',(0.,1.,0.)) ;
#67812 = DIRECTION('ref_axis',(-0.951056516295154,0.,-0.309016994374945)) ;
#67813 = DIRECTION('center_axis',(-0.309016994374948,0.,0.951056516295154)) ;
#67814 = DIRECTION('ref_axis',(-0.951056516295154,0.,-0.309016994374948)) ;
#67815 = DIRECTION('',(0.,-1.,0.)) ;
#67816 = DIRECTION('',(0.951056516295154,0.,0.309016994374948)) ;
#67817 = DIRECTION('center_axis',(0.,-1.,0.)) ;
#67818 = DIRECTION('ref_axis',(-1.,0.,0.)) ;
#67819 = DIRECTION('',(0.,1.,0.)) ;
#67820 = DIRECTION('center_axis',(0.,1.,0.)) ;
#67821 = DIRECTION('ref_axis',(-0.987688340595138,0.,-0.156434465040231)) ;
#67822 = DIRECTION('center_axis',(5.55111512312578E-17,0.,-1.)) ;
#67823 = DIRECTION('ref_axis',(1.,0.,5.55111512312578E-17)) ;
#67824 = DIRECTION('',(0.,-1.,0.)) ;
#67825 = DIRECTION('',(-1.,0.,-5.55111512312578E-17)) ;
#67826 = DIRECTION('center_axis',(0.,-1.,0.)) ;
#67827 = DIRECTION('ref_axis',(-1.,0.,9.31771680776961E-15)) ;
#67828 = DIRECTION('',(0.,-1.,0.)) ;
#67829 = DIRECTION('center_axis',(0.,1.,0.)) ;
#67830 = DIRECTION('ref_axis',(-1.,0.,0.)) ;
#67831 = DIRECTION('center_axis',(-5.55111512312578E-17,0.,1.)) ;
#67832 = DIRECTION('ref_axis',(-1.,0.,-5.55111512312578E-17)) ;
#67833 = DIRECTION('',(0.,-1.,0.)) ;
#67834 = DIRECTION('',(1.,0.,5.55111512312578E-17)) ;
#67835 = DIRECTION('center_axis',(0.,-1.,0.)) ;
#67836 = DIRECTION('ref_axis',(-1.,0.,0.)) ;
#67837 = DIRECTION('',(0.,1.,0.)) ;
#67838 = DIRECTION('center_axis',(0.,1.,0.)) ;
#67839 = DIRECTION('ref_axis',(-0.987688340595138,0.,0.156434465040229)) ;
#67840 = DIRECTION('center_axis',(-0.309016994374947,0.,-0.951056516295154)) ;
#67841 = DIRECTION('ref_axis',(0.951056516295154,0.,-0.309016994374947)) ;
#67842 = DIRECTION('',(0.,-1.,0.)) ;
#67843 = DIRECTION('',(-0.951056516295154,0.,0.309016994374947)) ;
#67844 = DIRECTION('center_axis',(0.,-1.,0.)) ;
#67845 = DIRECTION('ref_axis',(-0.951056516295152,0.,0.309016994374954)) ;
#67846 = DIRECTION('',(0.,-1.,0.)) ;
#67847 = DIRECTION('center_axis',(0.,1.,0.)) ;
#67848 = DIRECTION('ref_axis',(-0.951056516295154,0.,0.309016994374945)) ;
#67849 = DIRECTION('center_axis',(0.309016994374947,0.,0.951056516295154)) ;
#67850 = DIRECTION('ref_axis',(-0.951056516295154,0.,0.309016994374947)) ;
#67851 = DIRECTION('',(0.,-1.,0.)) ;
#67852 = DIRECTION('',(0.951056516295154,0.,-0.309016994374947)) ;
#67853 = DIRECTION('center_axis',(0.,-1.,0.)) ;
#67854 = DIRECTION('ref_axis',(-1.,0.,0.)) ;
#67855 = DIRECTION('',(0.,1.,0.)) ;
#67856 = DIRECTION('center_axis',(0.,1.,0.)) ;
#67857 = DIRECTION('ref_axis',(-0.891006524188369,0.,0.453990499739545)) ;
#67858 = DIRECTION('center_axis',(-0.587785252292473,0.,-0.809016994374948)) ;
#67859 = DIRECTION('ref_axis',(0.809016994374948,0.,-0.587785252292473)) ;
#67860 = DIRECTION('',(0.,-1.,0.)) ;
#67861 = DIRECTION('',(-0.809016994374947,0.,0.587785252292473)) ;
#67862 = DIRECTION('center_axis',(0.,-1.,0.)) ;
#67863 = DIRECTION('ref_axis',(-0.809016994374949,0.,0.587785252292471)) ;
#67864 = DIRECTION('',(0.,-1.,0.)) ;
#67865 = DIRECTION('center_axis',(0.,1.,0.)) ;
#67866 = DIRECTION('ref_axis',(-0.809016994374947,0.,0.587785252292474)) ;
#67867 = DIRECTION('center_axis',(0.587785252292473,0.,0.809016994374948)) ;
#67868 = DIRECTION('ref_axis',(-0.809016994374948,0.,0.587785252292473)) ;
#67869 = DIRECTION('',(0.,-1.,0.)) ;
#67870 = DIRECTION('',(0.809016994374947,0.,-0.587785252292473)) ;
#67871 = DIRECTION('center_axis',(0.,-1.,0.)) ;
#67872 = DIRECTION('ref_axis',(-1.,0.,0.)) ;
#67873 = DIRECTION('',(0.,1.,0.)) ;
#67874 = DIRECTION('center_axis',(0.,1.,0.)) ;
#67875 = DIRECTION('ref_axis',(-0.707106781186548,0.,0.707106781186547)) ;
#67876 = DIRECTION('center_axis',(-0.809016994374947,0.,-0.587785252292473)) ;
#67877 = DIRECTION('ref_axis',(0.587785252292473,0.,-0.809016994374947)) ;
#67878 = DIRECTION('',(0.,-1.,0.)) ;
#67879 = DIRECTION('',(-0.587785252292473,0.,0.809016994374947)) ;
#67880 = DIRECTION('center_axis',(0.,-1.,0.)) ;
#67881 = DIRECTION('ref_axis',(-0.587785252292476,0.,0.809016994374946)) ;
#67882 = DIRECTION('',(0.,-1.,0.)) ;
#67883 = DIRECTION('center_axis',(0.,1.,0.)) ;
#67884 = DIRECTION('ref_axis',(-0.587785252292474,0.,0.809016994374947)) ;
#67885 = DIRECTION('center_axis',(0.809016994374947,0.,0.587785252292473)) ;
#67886 = DIRECTION('ref_axis',(-0.587785252292473,0.,0.809016994374947)) ;
#67887 = DIRECTION('',(0.,-1.,0.)) ;
#67888 = DIRECTION('',(0.587785252292473,0.,-0.809016994374947)) ;
#67889 = DIRECTION('center_axis',(0.,-1.,0.)) ;
#67890 = DIRECTION('ref_axis',(-1.,0.,0.)) ;
#67891 = DIRECTION('',(0.,1.,0.)) ;
#67892 = DIRECTION('center_axis',(0.,1.,0.)) ;
#67893 = DIRECTION('ref_axis',(-0.453990499739546,0.,0.891006524188368)) ;
#67894 = DIRECTION('center_axis',(0.,1.,0.)) ;
#67895 = DIRECTION('ref_axis',(-1.,0.,0.)) ;
#67896 = DIRECTION('center_axis',(0.,-1.,0.)) ;
#67897 = DIRECTION('ref_axis',(-0.406305370818768,0.,0.913737350469939)) ;
#67898 = DIRECTION('center_axis',(0.,1.,0.)) ;
#67899 = DIRECTION('ref_axis',(-1.,0.,0.)) ;
#67900 = DIRECTION('center_axis',(0.,-1.,0.)) ;
#67901 = DIRECTION('ref_axis',(-0.406305370818768,0.,0.913737350469939)) ;
#67902 = DIRECTION('center_axis',(0.,1.,0.)) ;
#67903 = DIRECTION('ref_axis',(-1.,0.,0.)) ;
#67904 = DIRECTION('center_axis',(0.,-1.,0.)) ;
#67905 = DIRECTION('ref_axis',(-0.406305370818768,0.,0.913737350469939)) ;
#67906 = DIRECTION('center_axis',(0.,1.,0.)) ;
#67907 = DIRECTION('ref_axis',(-1.,0.,0.)) ;
#67908 = DIRECTION('center_axis',(0.,-1.,0.)) ;
#67909 = DIRECTION('ref_axis',(-0.406305370818768,0.,0.913737350469939)) ;
#67910 = DIRECTION('center_axis',(0.,1.,0.)) ;
#67911 = DIRECTION('ref_axis',(-1.,0.,0.)) ;
#67912 = DIRECTION('center_axis',(0.,-1.,0.)) ;
#67913 = DIRECTION('ref_axis',(-0.406305370818768,0.,0.913737350469939)) ;
#67914 = DIRECTION('center_axis',(0.,1.,0.)) ;
#67915 = DIRECTION('ref_axis',(-1.,0.,0.)) ;
#67916 = DIRECTION('center_axis',(0.,-1.,0.)) ;
#67917 = DIRECTION('ref_axis',(-0.406305370818768,0.,0.913737350469939)) ;
#67918 = DIRECTION('center_axis',(0.,1.,0.)) ;
#67919 = DIRECTION('ref_axis',(-1.,0.,0.)) ;
#67920 = DIRECTION('center_axis',(0.,-1.,0.)) ;
#67921 = DIRECTION('ref_axis',(-0.406305370818768,0.,0.913737350469939)) ;
#67922 = DIRECTION('center_axis',(0.,1.,0.)) ;
#67923 = DIRECTION('ref_axis',(-1.,0.,0.)) ;
#67924 = DIRECTION('center_axis',(0.,-1.,0.)) ;
#67925 = DIRECTION('ref_axis',(-0.406305370818768,0.,0.913737350469939)) ;
#67926 = DIRECTION('center_axis',(0.,1.,0.)) ;
#67927 = DIRECTION('ref_axis',(-1.,0.,0.)) ;
#67928 = DIRECTION('center_axis',(0.,-1.,0.)) ;
#67929 = DIRECTION('ref_axis',(-0.406305370818768,0.,0.913737350469939)) ;
#67930 = DIRECTION('center_axis',(0.,1.,0.)) ;
#67931 = DIRECTION('ref_axis',(-1.,0.,0.)) ;
#67932 = DIRECTION('center_axis',(0.,-1.,0.)) ;
#67933 = DIRECTION('ref_axis',(-0.406305370818768,0.,0.913737350469939)) ;
#67934 = DIRECTION('center_axis',(0.,1.,0.)) ;
#67935 = DIRECTION('ref_axis',(-1.,0.,0.)) ;
#67936 = DIRECTION('center_axis',(0.,-1.,0.)) ;
#67937 = DIRECTION('ref_axis',(-0.406305370818768,0.,0.913737350469939)) ;
#67938 = DIRECTION('center_axis',(0.,1.,0.)) ;
#67939 = DIRECTION('ref_axis',(-1.,0.,0.)) ;
#67940 = DIRECTION('center_axis',(0.,-1.,0.)) ;
#67941 = DIRECTION('ref_axis',(-0.406305370818768,0.,0.913737350469939)) ;
#67942 = DIRECTION('center_axis',(0.,1.,0.)) ;
#67943 = DIRECTION('ref_axis',(-1.,0.,0.)) ;
#67944 = DIRECTION('center_axis',(0.,-1.,0.)) ;
#67945 = DIRECTION('ref_axis',(-0.406305370818768,0.,0.913737350469939)) ;
#67946 = DIRECTION('center_axis',(0.,1.,0.)) ;
#67947 = DIRECTION('ref_axis',(-1.,0.,0.)) ;
#67948 = DIRECTION('center_axis',(0.,-1.,0.)) ;
#67949 = DIRECTION('ref_axis',(-0.406305370818768,0.,0.913737350469939)) ;
#67950 = DIRECTION('center_axis',(0.,1.,0.)) ;
#67951 = DIRECTION('ref_axis',(-1.,0.,0.)) ;
#67952 = DIRECTION('center_axis',(0.,-1.,0.)) ;
#67953 = DIRECTION('ref_axis',(-0.406305370818768,0.,0.913737350469939)) ;
#67954 = DIRECTION('center_axis',(0.,1.,0.)) ;
#67955 = DIRECTION('ref_axis',(-1.,0.,0.)) ;
#67956 = DIRECTION('center_axis',(0.,-1.,0.)) ;
#67957 = DIRECTION('ref_axis',(-0.406305370818768,0.,0.913737350469939)) ;
#67958 = DIRECTION('center_axis',(0.,1.,0.)) ;
#67959 = DIRECTION('ref_axis',(-1.,0.,0.)) ;
#67960 = DIRECTION('center_axis',(0.,-1.,0.)) ;
#67961 = DIRECTION('ref_axis',(-0.406305370818768,0.,0.913737350469939)) ;
#67962 = DIRECTION('center_axis',(0.,1.,0.)) ;
#67963 = DIRECTION('ref_axis',(-1.,0.,0.)) ;
#67964 = DIRECTION('center_axis',(0.,-1.,0.)) ;
#67965 = DIRECTION('ref_axis',(-0.406305370818768,0.,0.913737350469939)) ;
#67966 = DIRECTION('center_axis',(0.,1.,0.)) ;
#67967 = DIRECTION('ref_axis',(-1.,0.,0.)) ;
#67968 = DIRECTION('center_axis',(0.,-1.,0.)) ;
#67969 = DIRECTION('ref_axis',(-0.406305370818768,0.,0.913737350469939)) ;
#67970 = DIRECTION('center_axis',(0.,-1.,0.)) ;
#67971 = DIRECTION('ref_axis',(-0.406305370818768,0.,0.913737350469939)) ;
#67972 = DIRECTION('center_axis',(0.,-1.,0.)) ;
#67973 = DIRECTION('ref_axis',(0.,0.,-1.)) ;
#67974 = DIRECTION('center_axis',(1.,0.,0.)) ;
#67975 = DIRECTION('ref_axis',(0.,0.,1.)) ;
#67976 = DIRECTION('center_axis',(0.,-1.,0.)) ;
#67977 = DIRECTION('ref_axis',(-0.406305370818768,0.,0.913737350469939)) ;
#67978 = DIRECTION('center_axis',(0.,1.,0.)) ;
#67979 = DIRECTION('ref_axis',(-1.,0.,0.)) ;
#67980 = DIRECTION('center_axis',(0.,1.,0.)) ;
#67981 = DIRECTION('ref_axis',(0.,0.,1.)) ;
#67982 = DIRECTION('center_axis',(1.,0.,0.)) ;
#67983 = DIRECTION('ref_axis',(0.,0.,-1.)) ;
#67984 = DIRECTION('center_axis',(0.,1.,0.)) ;
#67985 = DIRECTION('ref_axis',(-0.208373389176835,0.,0.978049349819813)) ;
#67986 = DIRECTION('center_axis',(0.,-1.,0.)) ;
#67987 = DIRECTION('ref_axis',(-0.15643446504023,0.,-0.987688340595138)) ;
#67988 = DIRECTION('center_axis',(0.,1.,0.)) ;
#67989 = DIRECTION('ref_axis',(-0.208373389176835,0.,0.978049349819813)) ;
#67990 = DIRECTION('center_axis',(0.,-1.,0.)) ;
#67991 = DIRECTION('ref_axis',(-0.453990499739546,0.,-0.891006524188368)) ;
#67992 = DIRECTION('center_axis',(0.,1.,0.)) ;
#67993 = DIRECTION('ref_axis',(-0.208373389176835,0.,0.978049349819813)) ;
#67994 = DIRECTION('center_axis',(0.,-1.,0.)) ;
#67995 = DIRECTION('ref_axis',(-0.707106781186547,0.,-0.707106781186548)) ;
#67996 = DIRECTION('center_axis',(0.,1.,0.)) ;
#67997 = DIRECTION('ref_axis',(-0.208373389176835,0.,0.978049349819813)) ;
#67998 = DIRECTION('center_axis',(0.,-1.,0.)) ;
#67999 = DIRECTION('ref_axis',(-0.891006524188368,0.,-0.453990499739547)) ;
#68000 = DIRECTION('center_axis',(0.,1.,0.)) ;
#68001 = DIRECTION('ref_axis',(-0.208373389176835,0.,0.978049349819813)) ;
#68002 = DIRECTION('center_axis',(0.,-1.,0.)) ;
#68003 = DIRECTION('ref_axis',(-0.987688340595138,0.,-0.156434465040231)) ;
#68004 = DIRECTION('center_axis',(0.,1.,0.)) ;
#68005 = DIRECTION('ref_axis',(-0.208373389176835,0.,0.978049349819813)) ;
#68006 = DIRECTION('center_axis',(0.,-1.,0.)) ;
#68007 = DIRECTION('ref_axis',(-0.987688340595138,0.,0.156434465040229)) ;
#68008 = DIRECTION('center_axis',(0.,1.,0.)) ;
#68009 = DIRECTION('ref_axis',(-0.208373389176835,0.,0.978049349819813)) ;
#68010 = DIRECTION('center_axis',(0.,-1.,0.)) ;
#68011 = DIRECTION('ref_axis',(-0.891006524188369,0.,0.453990499739545)) ;
#68012 = DIRECTION('center_axis',(0.,1.,0.)) ;
#68013 = DIRECTION('ref_axis',(-0.208373389176835,0.,0.978049349819813)) ;
#68014 = DIRECTION('center_axis',(0.,-1.,0.)) ;
#68015 = DIRECTION('ref_axis',(-0.707106781186548,0.,0.707106781186547)) ;
#68016 = DIRECTION('center_axis',(0.,1.,0.)) ;
#68017 = DIRECTION('ref_axis',(-0.208373389176835,0.,0.978049349819813)) ;
#68018 = DIRECTION('center_axis',(0.,-1.,0.)) ;
#68019 = DIRECTION('ref_axis',(-0.453990499739546,0.,0.891006524188368)) ;
#68020 = DIRECTION('center_axis',(0.,1.,0.)) ;
#68021 = DIRECTION('ref_axis',(-0.208373389176835,0.,0.978049349819813)) ;
#68022 = DIRECTION('center_axis',(0.,-1.,0.)) ;
#68023 = DIRECTION('ref_axis',(-0.156434465040232,0.,0.987688340595138)) ;
#68024 = DIRECTION('center_axis',(0.,1.,0.)) ;
#68025 = DIRECTION('ref_axis',(-0.208373389176835,0.,0.978049349819813)) ;
#68026 = DIRECTION('center_axis',(0.,-1.,0.)) ;
#68027 = DIRECTION('ref_axis',(0.156434465040233,0.,0.987688340595137)) ;
#68028 = DIRECTION('center_axis',(0.,1.,0.)) ;
#68029 = DIRECTION('ref_axis',(-0.208373389176835,0.,0.978049349819813)) ;
#68030 = DIRECTION('center_axis',(0.,-1.,0.)) ;
#68031 = DIRECTION('ref_axis',(0.453990499739549,0.,0.891006524188367)) ;
#68032 = DIRECTION('center_axis',(0.,1.,0.)) ;
#68033 = DIRECTION('ref_axis',(-0.208373389176835,0.,0.978049349819813)) ;
#68034 = DIRECTION('center_axis',(0.,-1.,0.)) ;
#68035 = DIRECTION('ref_axis',(0.707106781186548,0.,0.707106781186547)) ;
#68036 = DIRECTION('center_axis',(0.,1.,0.)) ;
#68037 = DIRECTION('ref_axis',(-0.208373389176835,0.,0.978049349819813)) ;
#68038 = DIRECTION('center_axis',(0.,-1.,0.)) ;
#68039 = DIRECTION('ref_axis',(0.891006524188368,0.,0.453990499739546)) ;
#68040 = DIRECTION('center_axis',(0.,1.,0.)) ;
#68041 = DIRECTION('ref_axis',(-0.208373389176835,0.,0.978049349819813)) ;
#68042 = DIRECTION('center_axis',(0.,-1.,0.)) ;
#68043 = DIRECTION('ref_axis',(0.987688340595138,0.,0.156434465040232)) ;
#68044 = DIRECTION('center_axis',(0.,1.,0.)) ;
#68045 = DIRECTION('ref_axis',(-0.208373389176835,0.,0.978049349819813)) ;
#68046 = DIRECTION('center_axis',(0.,-1.,0.)) ;
#68047 = DIRECTION('ref_axis',(0.987688340595138,0.,-0.156434465040228)) ;
#68048 = DIRECTION('center_axis',(0.,1.,0.)) ;
#68049 = DIRECTION('ref_axis',(-0.208373389176835,0.,0.978049349819813)) ;
#68050 = DIRECTION('center_axis',(0.,-1.,0.)) ;
#68051 = DIRECTION('ref_axis',(0.891006524188368,0.,-0.453990499739547)) ;
#68052 = DIRECTION('center_axis',(0.,1.,0.)) ;
#68053 = DIRECTION('ref_axis',(-0.208373389176835,0.,0.978049349819813)) ;
#68054 = DIRECTION('center_axis',(0.,-1.,0.)) ;
#68055 = DIRECTION('ref_axis',(0.707106781186547,0.,-0.707106781186547)) ;
#68056 = DIRECTION('center_axis',(0.,1.,0.)) ;
#68057 = DIRECTION('ref_axis',(-0.208373389176835,0.,0.978049349819813)) ;
#68058 = DIRECTION('center_axis',(0.,-1.,0.)) ;
#68059 = DIRECTION('ref_axis',(0.453990499739547,0.,-0.891006524188368)) ;
#68060 = DIRECTION('center_axis',(0.,1.,0.)) ;
#68061 = DIRECTION('ref_axis',(-0.208373389176835,0.,0.978049349819813)) ;
#68062 = DIRECTION('center_axis',(0.,-1.,0.)) ;
#68063 = DIRECTION('ref_axis',(0.156434465040232,0.,-0.987688340595138)) ;
#68064 = DIRECTION('center_axis',(0.,1.,0.)) ;
#68065 = DIRECTION('ref_axis',(-0.208373389176835,0.,0.978049349819813)) ;
#68066 = DIRECTION('center_axis',(0.,1.,0.)) ;
#68067 = DIRECTION('ref_axis',(-1.,0.,0.)) ;
#68068 = DIRECTION('',(-0.309016994374948,0.,0.951056516295153)) ;
#68069 = DIRECTION('center_axis',(0.,-1.,0.)) ;
#68070 = DIRECTION('ref_axis',(0.309016994374945,0.,-0.951056516295154)) ;
#68071 = DIRECTION('',(0.309016994374948,0.,-0.951056516295153)) ;
#68072 = DIRECTION('center_axis',(0.,1.,0.)) ;
#68073 = DIRECTION('ref_axis',(-1.,0.,0.)) ;
#68074 = DIRECTION('',(-0.587785252292473,0.,0.809016994374947)) ;
#68075 = DIRECTION('center_axis',(0.,-1.,0.)) ;
#68076 = DIRECTION('ref_axis',(0.587785252292468,0.,-0.809016994374951)) ;
#68077 = DIRECTION('',(0.587785252292473,0.,-0.809016994374947)) ;
#68078 = DIRECTION('center_axis',(0.,1.,0.)) ;
#68079 = DIRECTION('ref_axis',(-1.,0.,0.)) ;
#68080 = DIRECTION('',(-0.809016994374948,0.,0.587785252292473)) ;
#68081 = DIRECTION('center_axis',(0.,-1.,0.)) ;
#68082 = DIRECTION('ref_axis',(0.809016994374947,0.,-0.587785252292474)) ;
#68083 = DIRECTION('',(0.809016994374948,0.,-0.587785252292473)) ;
#68084 = DIRECTION('center_axis',(0.,1.,0.)) ;
#68085 = DIRECTION('ref_axis',(-1.,0.,0.)) ;
#68086 = DIRECTION('',(-0.951056516295154,0.,0.309016994374947)) ;
#68087 = DIRECTION('center_axis',(0.,-1.,0.)) ;
#68088 = DIRECTION('ref_axis',(0.951056516295153,0.,-0.309016994374948)) ;
#68089 = DIRECTION('',(0.951056516295154,0.,-0.309016994374947)) ;
#68090 = DIRECTION('center_axis',(0.,1.,0.)) ;
#68091 = DIRECTION('ref_axis',(-1.,0.,0.)) ;
#68092 = DIRECTION('',(-1.,0.,-2.22044604925031E-16)) ;
#68093 = DIRECTION('center_axis',(0.,-1.,0.)) ;
#68094 = DIRECTION('ref_axis',(1.,0.,0.)) ;
#68095 = DIRECTION('',(1.,0.,2.22044604925031E-16)) ;
#68096 = DIRECTION('center_axis',(0.,1.,0.)) ;
#68097 = DIRECTION('ref_axis',(-1.,0.,0.)) ;
#68098 = DIRECTION('',(-0.951056516295153,0.,-0.309016994374948)) ;
#68099 = DIRECTION('center_axis',(0.,-1.,0.)) ;
#68100 = DIRECTION('ref_axis',(0.951056516295153,0.,0.309016994374948)) ;
#68101 = DIRECTION('',(0.951056516295153,0.,0.309016994374948)) ;
#68102 = DIRECTION('center_axis',(0.,1.,0.)) ;
#68103 = DIRECTION('ref_axis',(-1.,0.,0.)) ;
#68104 = DIRECTION('',(-0.809016994374947,0.,-0.587785252292473)) ;
#68105 = DIRECTION('center_axis',(0.,-1.,0.)) ;
#68106 = DIRECTION('ref_axis',(0.809016994374947,0.,0.587785252292474)) ;
#68107 = DIRECTION('',(0.809016994374947,0.,0.587785252292473)) ;
#68108 = DIRECTION('center_axis',(0.,1.,0.)) ;
#68109 = DIRECTION('ref_axis',(-1.,0.,0.)) ;
#68110 = DIRECTION('',(-0.587785252292473,0.,-0.809016994374947)) ;
#68111 = DIRECTION('center_axis',(0.,-1.,0.)) ;
#68112 = DIRECTION('ref_axis',(0.587785252292468,0.,0.809016994374951)) ;
#68113 = DIRECTION('',(0.587785252292473,0.,0.809016994374947)) ;
#68114 = DIRECTION('center_axis',(0.,1.,0.)) ;
#68115 = DIRECTION('ref_axis',(-1.,0.,0.)) ;
#68116 = DIRECTION('',(-0.309016994374947,0.,-0.951056516295154)) ;
#68117 = DIRECTION('center_axis',(0.,-1.,0.)) ;
#68118 = DIRECTION('ref_axis',(0.309016994374945,0.,0.951056516295154)) ;
#68119 = DIRECTION('',(0.309016994374947,0.,0.951056516295154)) ;
#68120 = DIRECTION('center_axis',(0.,1.,0.)) ;
#68121 = DIRECTION('ref_axis',(-1.,0.,0.)) ;
#68122 = DIRECTION('',(1.11022302462516E-16,0.,-1.)) ;
#68123 = DIRECTION('center_axis',(0.,-1.,0.)) ;
#68124 = DIRECTION('ref_axis',(0.,0.,1.)) ;
#68125 = DIRECTION('',(-1.11022302462516E-16,0.,1.)) ;
#68126 = DIRECTION('center_axis',(0.,1.,0.)) ;
#68127 = DIRECTION('ref_axis',(-1.,0.,0.)) ;
#68128 = DIRECTION('',(0.309016994374948,0.,-0.951056516295154)) ;
#68129 = DIRECTION('center_axis',(0.,-1.,0.)) ;
#68130 = DIRECTION('ref_axis',(-0.309016994374945,0.,0.951056516295154)) ;
#68131 = DIRECTION('',(-0.309016994374948,0.,0.951056516295154)) ;
#68132 = DIRECTION('center_axis',(0.,1.,0.)) ;
#68133 = DIRECTION('ref_axis',(-1.,0.,0.)) ;
#68134 = DIRECTION('',(0.587785252292473,0.,-0.809016994374947)) ;
#68135 = DIRECTION('center_axis',(0.,-1.,0.)) ;
#68136 = DIRECTION('ref_axis',(-0.587785252292474,0.,0.809016994374947)) ;
#68137 = DIRECTION('',(-0.587785252292473,0.,0.809016994374947)) ;
#68138 = DIRECTION('center_axis',(0.,1.,0.)) ;
#68139 = DIRECTION('ref_axis',(-1.,0.,0.)) ;
#68140 = DIRECTION('',(0.809016994374947,0.,-0.587785252292473)) ;
#68141 = DIRECTION('center_axis',(0.,-1.,0.)) ;
#68142 = DIRECTION('ref_axis',(-0.809016994374947,0.,0.587785252292474)) ;
#68143 = DIRECTION('',(-0.809016994374947,0.,0.587785252292473)) ;
#68144 = DIRECTION('center_axis',(0.,1.,0.)) ;
#68145 = DIRECTION('ref_axis',(-1.,0.,0.)) ;
#68146 = DIRECTION('',(0.951056516295154,0.,-0.309016994374947)) ;
#68147 = DIRECTION('center_axis',(0.,-1.,0.)) ;
#68148 = DIRECTION('ref_axis',(-0.951056516295154,0.,0.309016994374945)) ;
#68149 = DIRECTION('',(-0.951056516295154,0.,0.309016994374947)) ;
#68150 = DIRECTION('center_axis',(0.,1.,0.)) ;
#68151 = DIRECTION('ref_axis',(-1.,0.,0.)) ;
#68152 = DIRECTION('',(1.,0.,5.55111512312578E-17)) ;
#68153 = DIRECTION('center_axis',(0.,-1.,0.)) ;
#68154 = DIRECTION('ref_axis',(-1.,0.,0.)) ;
#68155 = DIRECTION('',(-1.,0.,-5.55111512312578E-17)) ;
#68156 = DIRECTION('center_axis',(0.,1.,0.)) ;
#68157 = DIRECTION('ref_axis',(-1.,0.,0.)) ;
#68158 = DIRECTION('',(0.951056516295154,0.,0.309016994374948)) ;
#68159 = DIRECTION('center_axis',(0.,-1.,0.)) ;
#68160 = DIRECTION('ref_axis',(-0.951056516295154,0.,-0.309016994374945)) ;
#68161 = DIRECTION('',(-0.951056516295154,0.,-0.309016994374948)) ;
#68162 = DIRECTION('center_axis',(0.,1.,0.)) ;
#68163 = DIRECTION('ref_axis',(-1.,0.,0.)) ;
#68164 = DIRECTION('',(0.809016994374947,0.,0.587785252292473)) ;
#68165 = DIRECTION('center_axis',(0.,-1.,0.)) ;
#68166 = DIRECTION('ref_axis',(-0.809016994374947,0.,-0.587785252292474)) ;
#68167 = DIRECTION('',(-0.809016994374947,0.,-0.587785252292473)) ;
#68168 = DIRECTION('center_axis',(0.,1.,0.)) ;
#68169 = DIRECTION('ref_axis',(-1.,0.,0.)) ;
#68170 = DIRECTION('',(0.587785252292473,0.,0.809016994374947)) ;
#68171 = DIRECTION('center_axis',(0.,-1.,0.)) ;
#68172 = DIRECTION('ref_axis',(-0.587785252292474,0.,-0.809016994374947)) ;
#68173 = DIRECTION('',(-0.587785252292473,0.,-0.809016994374947)) ;
#68174 = DIRECTION('center_axis',(0.,1.,0.)) ;
#68175 = DIRECTION('ref_axis',(-1.,0.,0.)) ;
#68176 = DIRECTION('',(0.309016994374947,0.,0.951056516295154)) ;
#68177 = DIRECTION('center_axis',(0.,-1.,0.)) ;
#68178 = DIRECTION('ref_axis',(-0.309016994374945,0.,-0.951056516295154)) ;
#68179 = DIRECTION('',(-0.309016994374947,0.,-0.951056516295154)) ;
#68180 = DIRECTION('center_axis',(0.,1.,0.)) ;
#68181 = DIRECTION('ref_axis',(-1.,0.,0.)) ;
#68182 = DIRECTION('',(0.,0.,1.)) ;
#68183 = DIRECTION('center_axis',(0.,-1.,0.)) ;
#68184 = DIRECTION('ref_axis',(0.,0.,-1.)) ;
#68185 = DIRECTION('',(0.,0.,-1.)) ;
#68186 = DIRECTION('center_axis',(0.,1.,0.)) ;
#68187 = DIRECTION('ref_axis',(0.,0.,1.)) ;
#68188 = DIRECTION('center_axis',(0.,1.,0.)) ;
#68189 = DIRECTION('ref_axis',(-0.156434465040232,0.,0.987688340595138)) ;
#68190 = DIRECTION('center_axis',(0.309016994374948,0.,-0.951056516295154)) ;
#68191 = DIRECTION('ref_axis',(0.672498511963948,0.707106781186557,0.218508012224408)) ;
#68192 = DIRECTION('',(0.309016994374948,0.,-0.951056516295154)) ;
#68193 = DIRECTION('center_axis',(1.11022302462516E-16,0.,-1.)) ;
#68194 = DIRECTION('ref_axis',(-0.707106781186547,0.707106781186547,-7.8504622934189E-17)) ;
#68195 = DIRECTION('',(-1.11022302462516E-16,0.,1.)) ;
#68196 = DIRECTION('center_axis',(0.309016994374948,0.,-0.951056516295154)) ;
#68197 = DIRECTION('ref_axis',(-0.672498511963948,0.707106781186557,-0.218508012224408)) ;
#68198 = DIRECTION('',(-0.309016994374948,0.,0.951056516295154)) ;
#68199 = DIRECTION('center_axis',(0.,1.,0.)) ;
#68200 = DIRECTION('ref_axis',(0.,0.,1.)) ;
#68201 = DIRECTION('center_axis',(0.587785252292473,0.,-0.809016994374947)) ;
#68202 = DIRECTION('ref_axis',(0.572061402817672,0.707106781186563,0.415626937777444)) ;
#68203 = DIRECTION('center_axis',(-0.309016994374947,0.,-0.951056516295154)) ;
#68204 = DIRECTION('ref_axis',(-0.672498511963948,0.707106781186557,0.218508012224407)) ;
#68205 = DIRECTION('',(0.309016994374947,0.,0.951056516295154)) ;
#68206 = DIRECTION('center_axis',(0.587785252292473,0.,-0.809016994374947)) ;
#68207 = DIRECTION('ref_axis',(-0.572061402817681,0.707106781186551,-0.415626937777452)) ;
#68208 = DIRECTION('center_axis',(0.,1.,0.)) ;
#68209 = DIRECTION('ref_axis',(0.,0.,1.)) ;
#68210 = DIRECTION('center_axis',(0.809016994374948,0.,-0.587785252292473)) ;
#68211 = DIRECTION('ref_axis',(0.415626937777444,0.707106781186563,0.572061402817672)) ;
#68212 = DIRECTION('center_axis',(-0.587785252292473,0.,-0.809016994374948)) ;
#68213 = DIRECTION('ref_axis',(-0.572061402817695,0.707106781186534,0.415626937777461)) ;
#68214 = DIRECTION('',(0.587785252292473,0.,0.809016994374947)) ;
#68215 = DIRECTION('center_axis',(0.809016994374948,0.,-0.587785252292473)) ;
#68216 = DIRECTION('ref_axis',(-0.415626937777444,0.707106781186563,-0.572061402817672)) ;
#68217 = DIRECTION('center_axis',(0.,1.,0.)) ;
#68218 = DIRECTION('ref_axis',(0.,0.,1.)) ;
#68219 = DIRECTION('center_axis',(0.951056516295154,0.,-0.309016994374947)) ;
#68220 = DIRECTION('ref_axis',(0.218508012224407,0.707106781186557,0.672498511963948)) ;
#68221 = DIRECTION('center_axis',(-0.809016994374947,0.,-0.587785252292473)) ;
#68222 = DIRECTION('ref_axis',(-0.415626937777452,0.707106781186551,0.572061402817681)) ;
#68223 = DIRECTION('',(0.809016994374947,0.,0.587785252292473)) ;
#68224 = DIRECTION('center_axis',(0.951056516295154,0.,-0.309016994374947)) ;
#68225 = DIRECTION('ref_axis',(-0.218508012224407,0.707106781186557,-0.672498511963948)) ;
#68226 = DIRECTION('center_axis',(0.,1.,0.)) ;
#68227 = DIRECTION('ref_axis',(0.,0.,1.)) ;
#68228 = DIRECTION('center_axis',(1.,0.,5.55111512312578E-17)) ;
#68229 = DIRECTION('ref_axis',(-3.92523114670932E-17,0.707106781186568,0.707106781186527)) ;
#68230 = DIRECTION('center_axis',(-0.951056516295154,0.,-0.309016994374948)) ;
#68231 = DIRECTION('ref_axis',(-0.2185080122244,0.707106781186583,0.672498511963923)) ;
#68232 = DIRECTION('',(0.951056516295153,0.,0.309016994374948)) ;
#68233 = DIRECTION('center_axis',(1.,0.,5.55111512312578E-17)) ;
#68234 = DIRECTION('ref_axis',(3.92523114670932E-17,0.707106781186568,-0.707106781186527)) ;
#68235 = DIRECTION('center_axis',(0.,1.,0.)) ;
#68236 = DIRECTION('ref_axis',(0.,0.,1.)) ;
#68237 = DIRECTION('center_axis',(0.951056516295154,0.,0.309016994374948)) ;
#68238 = DIRECTION('ref_axis',(-0.218508012224408,0.707106781186557,0.672498511963948)) ;
#68239 = DIRECTION('center_axis',(-1.,0.,-2.22044604925031E-16)) ;
#68240 = DIRECTION('ref_axis',(-1.57009245868373E-16,0.707106781186568,0.707106781186527)) ;
#68241 = DIRECTION('',(1.,0.,2.22044604925031E-16)) ;
#68242 = DIRECTION('center_axis',(0.951056516295154,0.,0.309016994374948)) ;
#68243 = DIRECTION('ref_axis',(0.218508012224408,0.707106781186557,-0.672498511963948)) ;
#68244 = DIRECTION('center_axis',(0.,1.,0.)) ;
#68245 = DIRECTION('ref_axis',(0.,0.,1.)) ;
#68246 = DIRECTION('center_axis',(0.809016994374947,0.,0.587785252292473)) ;
#68247 = DIRECTION('ref_axis',(-0.415626937777444,0.707106781186563,0.572061402817672)) ;
#68248 = DIRECTION('center_axis',(-0.951056516295154,0.,0.309016994374947)) ;
#68249 = DIRECTION('ref_axis',(0.218508012224405,0.707106781186563,0.672498511963943)) ;
#68250 = DIRECTION('',(0.951056516295154,0.,-0.309016994374947)) ;
#68251 = DIRECTION('center_axis',(0.809016994374947,0.,0.587785252292473)) ;
#68252 = DIRECTION('ref_axis',(0.415626937777442,0.707106781186568,-0.572061402817668)) ;
#68253 = DIRECTION('center_axis',(0.,1.,0.)) ;
#68254 = DIRECTION('ref_axis',(0.,0.,1.)) ;
#68255 = DIRECTION('center_axis',(0.587785252292473,0.,0.809016994374948)) ;
#68256 = DIRECTION('ref_axis',(-0.572061402817672,0.707106781186563,0.415626937777444)) ;
#68257 = DIRECTION('center_axis',(-0.809016994374948,0.,0.587785252292473)) ;
#68258 = DIRECTION('ref_axis',(0.415626937777451,0.707106781186551,0.572061402817682)) ;
#68259 = DIRECTION('',(0.809016994374948,0.,-0.587785252292473)) ;
#68260 = DIRECTION('center_axis',(0.587785252292473,0.,0.809016994374948)) ;
#68261 = DIRECTION('ref_axis',(0.572061402817682,0.707106781186551,-0.415626937777451)) ;
#68262 = DIRECTION('center_axis',(0.,1.,0.)) ;
#68263 = DIRECTION('ref_axis',(0.,0.,1.)) ;
#68264 = DIRECTION('center_axis',(0.309016994374947,0.,0.951056516295154)) ;
#68265 = DIRECTION('ref_axis',(-0.672498511963948,0.707106781186557,0.218508012224407)) ;
#68266 = DIRECTION('center_axis',(-0.587785252292473,0.,0.809016994374947)) ;
#68267 = DIRECTION('ref_axis',(0.572061402817695,0.707106781186534,0.415626937777461)) ;
#68268 = DIRECTION('',(0.587785252292473,0.,-0.809016994374947)) ;
#68269 = DIRECTION('center_axis',(0.309016994374947,0.,0.951056516295154)) ;
#68270 = DIRECTION('ref_axis',(0.672498511963948,0.707106781186557,-0.218508012224407)) ;
#68271 = DIRECTION('center_axis',(0.,1.,0.)) ;
#68272 = DIRECTION('ref_axis',(0.,0.,1.)) ;
#68273 = DIRECTION('center_axis',(0.,0.,1.)) ;
#68274 = DIRECTION('ref_axis',(-0.707106781186527,0.707106781186568,0.)) ;
#68275 = DIRECTION('center_axis',(-0.309016994374948,0.,0.951056516295154)) ;
#68276 = DIRECTION('ref_axis',(0.672498511963948,0.707106781186557,0.218508012224408)) ;
#68277 = DIRECTION('center_axis',(0.,0.,1.)) ;
#68278 = DIRECTION('ref_axis',(0.707106781186506,0.707106781186589,0.)) ;
#68279 = DIRECTION('center_axis',(0.,1.,0.)) ;
#68280 = DIRECTION('ref_axis',(0.,0.,1.)) ;
#68281 = DIRECTION('center_axis',(-0.309016994374948,0.,0.951056516295154)) ;
#68282 = DIRECTION('ref_axis',(-0.672498511963948,0.707106781186557,-0.218508012224408)) ;
#68283 = DIRECTION('center_axis',(0.,1.,0.)) ;
#68284 = DIRECTION('ref_axis',(0.309016994374031,0.,-0.951056516295451)) ;
#68285 = DIRECTION('center_axis',(0.,1.,0.)) ;
#68286 = DIRECTION('ref_axis',(-3.69482222595252E-13,0.,-1.)) ;
#68287 = DIRECTION('center_axis',(0.,1.,0.)) ;
#68288 = DIRECTION('ref_axis',(0.,0.,1.)) ;
#68289 = DIRECTION('center_axis',(0.,1.,0.)) ;
#68290 = DIRECTION('ref_axis',(0.453990499739547,0.,-0.891006524188368)) ;
#68291 = DIRECTION('center_axis',(-0.587785252292473,0.,0.809016994374947)) ;
#68292 = DIRECTION('ref_axis',(-0.572061402817695,0.707106781186534,-0.415626937777461)) ;
#68293 = DIRECTION('',(-0.587785252292473,0.,0.809016994374947)) ;
#68294 = DIRECTION('center_axis',(0.,1.,0.)) ;
#68295 = DIRECTION('ref_axis',(0.587785252293384,0.,-0.809016994374286)) ;
#68296 = DIRECTION('center_axis',(0.,1.,0.)) ;
#68297 = DIRECTION('ref_axis',(0.587785252292468,0.,-0.809016994374951)) ;
#68298 = DIRECTION('center_axis',(0.,1.,0.)) ;
#68299 = DIRECTION('ref_axis',(-0.309016994375651,0.,-0.951056516294925)) ;
#68300 = DIRECTION('center_axis',(0.,1.,0.)) ;
#68301 = DIRECTION('ref_axis',(0.,0.,1.)) ;
#68302 = DIRECTION('center_axis',(0.,1.,0.)) ;
#68303 = DIRECTION('ref_axis',(0.707106781186547,0.,-0.707106781186547)) ;
#68304 = DIRECTION('center_axis',(-0.809016994374948,0.,0.587785252292473)) ;
#68305 = DIRECTION('ref_axis',(-0.415626937777437,0.707106781186575,-0.572061402817662)) ;
#68306 = DIRECTION('',(-0.809016994374948,0.,0.587785252292473)) ;
#68307 = DIRECTION('center_axis',(0.,1.,0.)) ;
#68308 = DIRECTION('ref_axis',(0.809016994375308,0.,-0.587785252291977)) ;
#68309 = DIRECTION('center_axis',(0.,1.,0.)) ;
#68310 = DIRECTION('ref_axis',(0.809016994374947,0.,-0.587785252292474)) ;
#68311 = DIRECTION('center_axis',(0.,1.,0.)) ;
#68312 = DIRECTION('ref_axis',(-0.587785252292334,0.,-0.809016994375048)) ;
#68313 = DIRECTION('center_axis',(0.,1.,0.)) ;
#68314 = DIRECTION('ref_axis',(0.,0.,1.)) ;
#68315 = DIRECTION('center_axis',(0.,1.,0.)) ;
#68316 = DIRECTION('ref_axis',(0.891006524188368,0.,-0.453990499739547)) ;
#68317 = DIRECTION('center_axis',(-0.951056516295154,0.,0.309016994374947)) ;
#68318 = DIRECTION('ref_axis',(-0.218508012224405,0.707106781186563,-0.672498511963943)) ;
#68319 = DIRECTION('',(-0.951056516295154,0.,0.309016994374947)) ;
#68320 = DIRECTION('center_axis',(0.,1.,0.)) ;
#68321 = DIRECTION('ref_axis',(0.951056516294886,0.,-0.309016994375771)) ;
#68322 = DIRECTION('center_axis',(0.,1.,0.)) ;
#68323 = DIRECTION('ref_axis',(0.951056516295153,0.,-0.309016994374948)) ;
#68324 = DIRECTION('center_axis',(0.,1.,0.)) ;
#68325 = DIRECTION('ref_axis',(-0.809016994374774,0.,-0.587785252292712)) ;
#68326 = DIRECTION('center_axis',(0.,1.,0.)) ;
#68327 = DIRECTION('ref_axis',(0.,0.,1.)) ;
#68328 = DIRECTION('center_axis',(0.,1.,0.)) ;
#68329 = DIRECTION('ref_axis',(0.987688340595138,0.,-0.156434465040228)) ;
#68330 = DIRECTION('center_axis',(-1.,0.,-2.22044604925031E-16)) ;
#68331 = DIRECTION('ref_axis',(1.57009245868373E-16,0.707106781186568,-0.707106781186527)) ;
#68332 = DIRECTION('',(-1.,0.,-2.22044604925031E-16)) ;
#68333 = DIRECTION('center_axis',(0.,1.,0.)) ;
#68334 = DIRECTION('ref_axis',(1.,0.,-4.2632564145606E-14)) ;
#68335 = DIRECTION('center_axis',(0.,1.,0.)) ;
#68336 = DIRECTION('ref_axis',(1.,0.,0.)) ;
#68337 = DIRECTION('center_axis',(0.,1.,0.)) ;
#68338 = DIRECTION('ref_axis',(-0.951056516295327,0.,-0.309016994374414)) ;
#68339 = DIRECTION('center_axis',(0.,1.,0.)) ;
#68340 = DIRECTION('ref_axis',(0.,0.,1.)) ;
#68341 = DIRECTION('center_axis',(0.,1.,0.)) ;
#68342 = DIRECTION('ref_axis',(0.987688340595138,0.,0.156434465040232)) ;
#68343 = DIRECTION('center_axis',(-0.951056516295154,0.,-0.309016994374948)) ;
#68344 = DIRECTION('ref_axis',(0.218508012224406,0.707106781186563,-0.672498511963942)) ;
#68345 = DIRECTION('',(-0.951056516295153,0.,-0.309016994374948)) ;
#68346 = DIRECTION('center_axis',(0.,1.,0.)) ;
#68347 = DIRECTION('ref_axis',(0.,0.,1.)) ;
#68348 = DIRECTION('center_axis',(0.,1.,0.)) ;
#68349 = DIRECTION('ref_axis',(0.951056516295153,0.,0.309016994374948)) ;
#68350 = DIRECTION('center_axis',(0.,1.,0.)) ;
#68351 = DIRECTION('ref_axis',(-1.,0.,4.68958205601666E-13)) ;
#68352 = DIRECTION('center_axis',(0.,1.,0.)) ;
#68353 = DIRECTION('ref_axis',(0.,0.,1.)) ;
#68354 = DIRECTION('center_axis',(0.,1.,0.)) ;
#68355 = DIRECTION('ref_axis',(0.891006524188368,0.,0.453990499739546)) ;
#68356 = DIRECTION('center_axis',(-0.809016994374947,0.,-0.587785252292473)) ;
#68357 = DIRECTION('ref_axis',(0.415626937777427,0.707106781186592,-0.572061402817648)) ;
#68358 = DIRECTION('',(-0.809016994374947,0.,-0.587785252292473)) ;
#68359 = DIRECTION('center_axis',(0.,1.,0.)) ;
#68360 = DIRECTION('ref_axis',(0.,0.,1.)) ;
#68361 = DIRECTION('center_axis',(0.,1.,0.)) ;
#68362 = DIRECTION('ref_axis',(0.809016994374947,0.,0.587785252292474)) ;
#68363 = DIRECTION('center_axis',(0.,1.,0.)) ;
#68364 = DIRECTION('ref_axis',(0.,0.,1.)) ;
#68365 = DIRECTION('center_axis',(0.,1.,0.)) ;
#68366 = DIRECTION('ref_axis',(0.,0.,1.)) ;
#68367 = DIRECTION('center_axis',(0.,1.,0.)) ;
#68368 = DIRECTION('ref_axis',(0.707106781186548,0.,0.707106781186547)) ;
#68369 = DIRECTION('center_axis',(-0.587785252292473,0.,-0.809016994374948)) ;
#68370 = DIRECTION('ref_axis',(0.572061402817668,0.707106781186568,-0.415626937777441)) ;
#68371 = DIRECTION('',(-0.587785252292473,0.,-0.809016994374947)) ;
#68372 = DIRECTION('center_axis',(0.,1.,0.)) ;
#68373 = DIRECTION('ref_axis',(0.,0.,1.)) ;
#68374 = DIRECTION('center_axis',(0.,1.,0.)) ;
#68375 = DIRECTION('ref_axis',(0.587785252292468,0.,0.809016994374951)) ;
#68376 = DIRECTION('center_axis',(0.,1.,0.)) ;
#68377 = DIRECTION('ref_axis',(0.,0.,1.)) ;
#68378 = DIRECTION('center_axis',(0.,1.,0.)) ;
#68379 = DIRECTION('ref_axis',(0.,0.,1.)) ;
#68380 = DIRECTION('center_axis',(0.,1.,0.)) ;
#68381 = DIRECTION('ref_axis',(0.453990499739549,0.,0.891006524188367)) ;
#68382 = DIRECTION('center_axis',(-0.309016994374947,0.,-0.951056516295154)) ;
#68383 = DIRECTION('ref_axis',(0.672498511963948,0.707106781186557,-0.218508012224407)) ;
#68384 = DIRECTION('',(-0.309016994374947,0.,-0.951056516295154)) ;
#68385 = DIRECTION('center_axis',(0.,1.,0.)) ;
#68386 = DIRECTION('ref_axis',(0.,0.,1.)) ;
#68387 = DIRECTION('center_axis',(0.,1.,0.)) ;
#68388 = DIRECTION('ref_axis',(0.309016994374945,0.,0.951056516295154)) ;
#68389 = DIRECTION('center_axis',(0.,1.,0.)) ;
#68390 = DIRECTION('ref_axis',(0.,0.,1.)) ;
#68391 = DIRECTION('center_axis',(0.,1.,0.)) ;
#68392 = DIRECTION('ref_axis',(0.,0.,1.)) ;
#68393 = DIRECTION('center_axis',(0.,1.,0.)) ;
#68394 = DIRECTION('ref_axis',(0.156434465040233,0.,0.987688340595137)) ;
#68395 = DIRECTION('center_axis',(1.11022302462516E-16,0.,-1.)) ;
#68396 = DIRECTION('ref_axis',(0.707106781186506,0.707106781186589,7.85046229341844E-17)) ;
#68397 = DIRECTION('',(1.11022302462516E-16,0.,-1.)) ;
#68398 = DIRECTION('center_axis',(0.,1.,0.)) ;
#68399 = DIRECTION('ref_axis',(0.,0.,1.)) ;
#68400 = DIRECTION('center_axis',(0.,1.,0.)) ;
#68401 = DIRECTION('ref_axis',(0.,0.,1.)) ;
#68402 = DIRECTION('center_axis',(0.,1.,0.)) ;
#68403 = DIRECTION('ref_axis',(0.,0.,1.)) ;
#68404 = DIRECTION('center_axis',(0.,1.,0.)) ;
#68405 = DIRECTION('ref_axis',(-0.309016994374945,0.,0.951056516295154)) ;
#68406 = DIRECTION('center_axis',(0.,-1.,0.)) ;
#68407 = DIRECTION('ref_axis',(-1.,0.,0.)) ;
#68408 = DIRECTION('',(0.,1.,0.)) ;
#68409 = DIRECTION('',(0.,-1.,0.)) ;
#68410 = DIRECTION('center_axis',(0.951056516295154,0.,0.309016994374948)) ;
#68411 = DIRECTION('ref_axis',(-0.309016994374948,0.,0.951056516295154)) ;
#68412 = DIRECTION('',(0.,-1.,0.)) ;
#68413 = DIRECTION('center_axis',(0.,-1.,0.)) ;
#68414 = DIRECTION('ref_axis',(-0.309016994374937,0.,0.951056516295157)) ;
#68415 = DIRECTION('',(0.,-1.,0.)) ;
#68416 = DIRECTION('center_axis',(-0.951056516295154,0.,-0.309016994374948)) ;
#68417 = DIRECTION('ref_axis',(0.309016994374948,0.,-0.951056516295154)) ;
#68418 = DIRECTION('center_axis',(-0.809016994374947,0.,-0.587785252292473)) ;
#68419 = DIRECTION('ref_axis',(0.587785252292473,0.,-0.809016994374947)) ;
#68420 = DIRECTION('',(0.,-1.,0.)) ;
#68421 = DIRECTION('',(0.,-1.,0.)) ;
#68422 = DIRECTION('center_axis',(0.809016994374947,0.,0.587785252292473)) ;
#68423 = DIRECTION('ref_axis',(-0.587785252292473,0.,0.809016994374947)) ;
#68424 = DIRECTION('',(0.,-1.,0.)) ;
#68425 = DIRECTION('',(0.,1.,0.)) ;
#68426 = DIRECTION('center_axis',(0.,-1.,0.)) ;
#68427 = DIRECTION('ref_axis',(0.58778525229247,0.,-0.80901699437495)) ;
#68428 = DIRECTION('center_axis',(-0.587785252292473,0.,-0.809016994374948)) ;
#68429 = DIRECTION('ref_axis',(0.809016994374948,0.,-0.587785252292473)) ;
#68430 = DIRECTION('',(0.,-1.,0.)) ;
#68431 = DIRECTION('',(0.,-1.,0.)) ;
#68432 = DIRECTION('center_axis',(0.587785252292473,0.,0.809016994374948)) ;
#68433 = DIRECTION('ref_axis',(-0.809016994374948,0.,0.587785252292473)) ;
#68434 = DIRECTION('',(0.,-1.,0.)) ;
#68435 = DIRECTION('',(0.,1.,0.)) ;
#68436 = DIRECTION('center_axis',(0.,-1.,0.)) ;
#68437 = DIRECTION('ref_axis',(0.809016994374946,0.,-0.587785252292475)) ;
#68438 = DIRECTION('center_axis',(-0.309016994374947,0.,-0.951056516295154)) ;
#68439 = DIRECTION('ref_axis',(0.951056516295154,0.,-0.309016994374947)) ;
#68440 = DIRECTION('',(0.,-1.,0.)) ;
#68441 = DIRECTION('',(0.,-1.,0.)) ;
#68442 = DIRECTION('center_axis',(0.309016994374947,0.,0.951056516295154)) ;
#68443 = DIRECTION('ref_axis',(-0.951056516295154,0.,0.309016994374947)) ;
#68444 = DIRECTION('',(0.,-1.,0.)) ;
#68445 = DIRECTION('',(0.,1.,0.)) ;
#68446 = DIRECTION('center_axis',(0.,-1.,0.)) ;
#68447 = DIRECTION('ref_axis',(0.951056516295149,0.,-0.309016994374963)) ;
#68448 = DIRECTION('center_axis',(2.22044604925031E-16,0.,-1.)) ;
#68449 = DIRECTION('ref_axis',(1.,0.,2.22044604925031E-16)) ;
#68450 = DIRECTION('',(0.,-1.,0.)) ;
#68451 = DIRECTION('',(0.,-1.,0.)) ;
#68452 = DIRECTION('center_axis',(-2.22044604925031E-16,0.,1.)) ;
#68453 = DIRECTION('ref_axis',(-1.,0.,-2.22044604925031E-16)) ;
#68454 = DIRECTION('',(0.,-1.,0.)) ;
#68455 = DIRECTION('',(0.,1.,0.)) ;
#68456 = DIRECTION('center_axis',(0.,-1.,0.)) ;
#68457 = DIRECTION('ref_axis',(1.,0.,-5.19199337615246E-16)) ;
#68458 = DIRECTION('center_axis',(0.309016994374948,0.,-0.951056516295154)) ;
#68459 = DIRECTION('ref_axis',(0.951056516295154,0.,0.309016994374948)) ;
#68460 = DIRECTION('',(0.,-1.,0.)) ;
#68461 = DIRECTION('',(0.,-1.,0.)) ;
#68462 = DIRECTION('center_axis',(-0.309016994374948,0.,0.951056516295154)) ;
#68463 = DIRECTION('ref_axis',(-0.951056516295154,0.,-0.309016994374948)) ;
#68464 = DIRECTION('',(0.,-1.,0.)) ;
#68465 = DIRECTION('',(0.,1.,0.)) ;
#68466 = DIRECTION('center_axis',(0.,-1.,0.)) ;
#68467 = DIRECTION('ref_axis',(0.951056516295154,0.,0.309016994374945)) ;
#68468 = DIRECTION('center_axis',(0.587785252292473,0.,-0.809016994374947)) ;
#68469 = DIRECTION('ref_axis',(0.809016994374947,0.,0.587785252292473)) ;
#68470 = DIRECTION('',(0.,-1.,0.)) ;
#68471 = DIRECTION('',(0.,-1.,0.)) ;
#68472 = DIRECTION('center_axis',(-0.587785252292473,0.,0.809016994374947)) ;
#68473 = DIRECTION('ref_axis',(-0.809016994374947,0.,-0.587785252292473)) ;
#68474 = DIRECTION('',(0.,-1.,0.)) ;
#68475 = DIRECTION('',(0.,1.,0.)) ;
#68476 = DIRECTION('center_axis',(0.,-1.,0.)) ;
#68477 = DIRECTION('ref_axis',(0.809016994374945,0.,0.587785252292477)) ;
#68478 = DIRECTION('center_axis',(0.809016994374948,0.,-0.587785252292473)) ;
#68479 = DIRECTION('ref_axis',(0.587785252292473,0.,0.809016994374948)) ;
#68480 = DIRECTION('',(0.,-1.,0.)) ;
#68481 = DIRECTION('',(0.,-1.,0.)) ;
#68482 = DIRECTION('center_axis',(-0.809016994374948,0.,0.587785252292473)) ;
#68483 = DIRECTION('ref_axis',(-0.587785252292473,0.,-0.809016994374948)) ;
#68484 = DIRECTION('',(0.,-1.,0.)) ;
#68485 = DIRECTION('',(0.,1.,0.)) ;
#68486 = DIRECTION('center_axis',(0.,-1.,0.)) ;
#68487 = DIRECTION('ref_axis',(0.587785252292472,0.,0.809016994374948)) ;
#68488 = DIRECTION('center_axis',(0.951056516295154,0.,-0.309016994374947)) ;
#68489 = DIRECTION('ref_axis',(0.309016994374947,0.,0.951056516295154)) ;
#68490 = DIRECTION('',(0.,-1.,0.)) ;
#68491 = DIRECTION('',(0.,-1.,0.)) ;
#68492 = DIRECTION('center_axis',(-0.951056516295154,0.,0.309016994374947)) ;
#68493 = DIRECTION('ref_axis',(-0.309016994374947,0.,-0.951056516295154)) ;
#68494 = DIRECTION('',(0.,-1.,0.)) ;
#68495 = DIRECTION('',(0.,1.,0.)) ;
#68496 = DIRECTION('center_axis',(0.,-1.,0.)) ;
#68497 = DIRECTION('ref_axis',(0.309016994374948,0.,0.951056516295153)) ;
#68498 = DIRECTION('center_axis',(1.,0.,1.11022302462516E-16)) ;
#68499 = DIRECTION('ref_axis',(-1.11022302462516E-16,0.,1.)) ;
#68500 = DIRECTION('',(0.,-1.,0.)) ;
#68501 = DIRECTION('',(0.,-1.,0.)) ;
#68502 = DIRECTION('center_axis',(-1.,0.,-1.11022302462516E-16)) ;
#68503 = DIRECTION('ref_axis',(1.11022302462516E-16,0.,-1.)) ;
#68504 = DIRECTION('',(0.,-1.,0.)) ;
#68505 = DIRECTION('center_axis',(0.,-1.,0.)) ;
#68506 = DIRECTION('ref_axis',(8.83893312840001E-15,0.,1.)) ;
#68507 = DIRECTION('center_axis',(0.,-1.,0.)) ;
#68508 = DIRECTION('ref_axis',(-1.,0.,0.)) ;
#68509 = DIRECTION('center_axis',(0.,-1.,0.)) ;
#68510 = DIRECTION('ref_axis',(-1.,0.,0.)) ;
#68511 = DIRECTION('center_axis',(0.,-1.,0.)) ;
#68512 = DIRECTION('ref_axis',(-1.,0.,0.)) ;
#68513 = DIRECTION('center_axis',(0.,-1.,0.)) ;
#68514 = DIRECTION('ref_axis',(-1.,0.,0.)) ;
#68515 = DIRECTION('center_axis',(0.,-1.,0.)) ;
#68516 = DIRECTION('ref_axis',(-1.,0.,0.)) ;
#68517 = DIRECTION('center_axis',(0.,-1.,0.)) ;
#68518 = DIRECTION('ref_axis',(-1.,0.,0.)) ;
#68519 = DIRECTION('center_axis',(0.,-1.,0.)) ;
#68520 = DIRECTION('ref_axis',(-1.,0.,0.)) ;
#68521 = DIRECTION('center_axis',(0.,-1.,0.)) ;
#68522 = DIRECTION('ref_axis',(-1.,0.,0.)) ;
#68523 = DIRECTION('center_axis',(0.,-1.,0.)) ;
#68524 = DIRECTION('ref_axis',(-1.,0.,0.)) ;
#68525 = DIRECTION('center_axis',(0.,-1.,0.)) ;
#68526 = DIRECTION('ref_axis',(-1.,0.,0.)) ;
#68527 = DIRECTION('',(0.,-1.,0.)) ;
#68528 = DIRECTION('axis',(0.,0.,1.)) ;
#68529 = DIRECTION('refdir',(1.,0.,0.)) ;
#68530 = DIRECTION('center_axis',(1.,2.22044604925031E-16,0.)) ;
#68531 = DIRECTION('ref_axis',(0.,1.,0.)) ;
#68532 = DIRECTION('center_axis',(1.,2.22044604925031E-16,0.)) ;
#68533 = DIRECTION('ref_axis',(2.22044604925031E-16,-1.,0.)) ;
#68534 = DIRECTION('center_axis',(0.,0.,1.)) ;
#68535 = DIRECTION('ref_axis',(0.,-1.,0.)) ;
#68536 = DIRECTION('center_axis',(1.,2.22044604925031E-16,0.)) ;
#68537 = DIRECTION('ref_axis',(-2.22044604925031E-16,1.,0.)) ;
#68538 = DIRECTION('center_axis',(-1.,-2.22044604925031E-16,0.)) ;
#68539 = DIRECTION('ref_axis',(2.22044604925031E-16,-1.,0.)) ;
#68540 = DIRECTION('center_axis',(1.,2.22044604925031E-16,0.)) ;
#68541 = DIRECTION('ref_axis',(0.,0.,-1.)) ;
#68542 = DIRECTION('center_axis',(-1.,-2.22044604925031E-16,0.)) ;
#68543 = DIRECTION('ref_axis',(2.22044604925031E-16,-1.,0.)) ;
#68544 = DIRECTION('center_axis',(-2.22044604925031E-16,1.,0.)) ;
#68545 = DIRECTION('ref_axis',(0.,0.,1.)) ;
#68546 = DIRECTION('center_axis',(-1.,-2.22044604925031E-16,0.)) ;
#68547 = DIRECTION('ref_axis',(2.22044604925031E-16,-1.,0.)) ;
#68548 = DIRECTION('center_axis',(-1.,-2.22044604925031E-16,0.)) ;
#68549 = DIRECTION('ref_axis',(2.22044604925031E-16,-1.,0.)) ;
#68550 = DIRECTION('center_axis',(-1.,-2.22044604925031E-16,0.)) ;
#68551 = DIRECTION('ref_axis',(2.22044604925031E-16,-1.,0.)) ;
#68552 = DIRECTION('center_axis',(1.,2.22044604925031E-16,0.)) ;
#68553 = DIRECTION('ref_axis',(2.22044604925031E-16,-1.,0.)) ;
#68554 = DIRECTION('center_axis',(-1.,-2.22044604925031E-16,0.)) ;
#68555 = DIRECTION('ref_axis',(2.22044604925031E-16,-1.,0.)) ;
#68556 = DIRECTION('center_axis',(-1.,-2.22044604925031E-16,0.)) ;
#68557 = DIRECTION('ref_axis',(2.22044604925031E-16,-1.,0.)) ;
#68558 = DIRECTION('center_axis',(1.,2.22044604925031E-16,0.)) ;
#68559 = DIRECTION('ref_axis',(0.,0.,-1.)) ;
#68560 = DIRECTION('center_axis',(1.,2.22044604925031E-16,0.)) ;
#68561 = DIRECTION('ref_axis',(9.02179155423715E-17,-0.406305370818768,0.913737350469939)) ;
#68562 = DIRECTION('center_axis',(1.,2.22044604925031E-16,0.)) ;
#68563 = DIRECTION('ref_axis',(1.00806141154385E-16,-0.453990499739547,0.891006524188368)) ;
#68564 = DIRECTION('center_axis',(-6.86155564311058E-17,0.309016994374948,
-0.951056516295154)) ;
#68565 = DIRECTION('ref_axis',(0.707106781186557,-0.672498511963948,-0.218508012224408)) ;
#68566 = DIRECTION('',(6.86155564311058E-17,-0.309016994374947,0.951056516295154)) ;
#68567 = DIRECTION('',(-6.86155564311058E-17,0.309016994374948,-0.951056516295154)) ;
#68568 = DIRECTION('center_axis',(1.,2.22044604925031E-16,0.)) ;
#68569 = DIRECTION('ref_axis',(0.,-0.309016994374926,0.95105651629516)) ;
#68570 = DIRECTION('center_axis',(-1.,-2.22044604925031E-16,0.)) ;
#68571 = DIRECTION('ref_axis',(6.86155564311052E-17,-0.309016994374945,0.951056516295154)) ;
#68572 = DIRECTION('center_axis',(1.,2.22044604925031E-16,0.)) ;
#68573 = DIRECTION('ref_axis',(6.86155564311052E-17,-0.309016994374945,0.951056516295154)) ;
#68574 = DIRECTION('center_axis',(6.86155564311058E-17,-0.309016994374948,
0.951056516295154)) ;
#68575 = DIRECTION('ref_axis',(0.707106781186557,0.672498511963948,0.218508012224408)) ;
#68576 = DIRECTION('',(-6.86155564311058E-17,0.309016994374948,-0.951056516295154)) ;
#68577 = DIRECTION('',(6.86155564311058E-17,-0.309016994374948,0.951056516295154)) ;
#68578 = DIRECTION('center_axis',(1.,2.22044604925031E-16,0.)) ;
#68579 = DIRECTION('ref_axis',(0.,0.,-1.)) ;
#68580 = DIRECTION('center_axis',(1.,2.22044604925031E-16,0.)) ;
#68581 = DIRECTION('ref_axis',(9.02179155423715E-17,-0.406305370818768,0.913737350469939)) ;
#68582 = DIRECTION('center_axis',(1.,2.22044604925031E-16,0.)) ;
#68583 = DIRECTION('ref_axis',(3.47354289865169E-17,-0.156434465040232,0.987688340595138)) ;
#68584 = DIRECTION('center_axis',(-2.46519032881566E-32,1.11022302462516E-16,
-1.)) ;
#68585 = DIRECTION('ref_axis',(0.707106781186569,-0.707106781186526,-7.85046229341866E-17)) ;
#68586 = DIRECTION('',(2.46519032881566E-32,-1.11022302462516E-16,1.)) ;
#68587 = DIRECTION('',(-2.46519032881566E-32,1.11022302462516E-16,-1.)) ;
#68588 = DIRECTION('center_axis',(1.,2.22044604925031E-16,0.)) ;
#68589 = DIRECTION('ref_axis',(0.,-1.13686837721616E-13,1.)) ;
#68590 = DIRECTION('center_axis',(-1.,-2.22044604925031E-16,0.)) ;
#68591 = DIRECTION('ref_axis',(0.,0.,1.)) ;
#68592 = DIRECTION('center_axis',(1.,2.22044604925031E-16,0.)) ;
#68593 = DIRECTION('ref_axis',(0.,0.,1.)) ;
#68594 = DIRECTION('center_axis',(2.46519032881566E-32,-1.11022302462516E-16,
1.)) ;
#68595 = DIRECTION('ref_axis',(0.707106781186589,0.707106781186506,7.85046229341844E-17)) ;
#68596 = DIRECTION('',(-2.46519032881566E-32,1.11022302462516E-16,-1.)) ;
#68597 = DIRECTION('',(2.46519032881566E-32,-1.11022302462516E-16,1.)) ;
#68598 = DIRECTION('center_axis',(1.,2.22044604925031E-16,0.)) ;
#68599 = DIRECTION('ref_axis',(0.,0.,-1.)) ;
#68600 = DIRECTION('center_axis',(1.,2.22044604925031E-16,0.)) ;
#68601 = DIRECTION('ref_axis',(9.02179155423715E-17,-0.406305370818768,0.913737350469939)) ;
#68602 = DIRECTION('center_axis',(1.,2.22044604925031E-16,0.)) ;
#68603 = DIRECTION('ref_axis',(-3.47354289865171E-17,0.156434465040233,0.987688340595137)) ;
#68604 = DIRECTION('center_axis',(6.86155564311058E-17,-0.309016994374947,
-0.951056516295154)) ;
#68605 = DIRECTION('ref_axis',(0.707106781186557,-0.672498511963948,0.218508012224407)) ;
#68606 = DIRECTION('',(-6.86155564311058E-17,0.309016994374947,0.951056516295154)) ;
#68607 = DIRECTION('',(6.86155564311058E-17,-0.309016994374947,-0.951056516295154)) ;
#68608 = DIRECTION('center_axis',(1.,2.22044604925031E-16,0.)) ;
#68609 = DIRECTION('ref_axis',(0.,0.309016994374757,0.951056516295215)) ;
#68610 = DIRECTION('center_axis',(-1.,-2.22044604925031E-16,0.)) ;
#68611 = DIRECTION('ref_axis',(-6.86155564311052E-17,0.309016994374945,0.951056516295154)) ;
#68612 = DIRECTION('center_axis',(1.,2.22044604925031E-16,0.)) ;
#68613 = DIRECTION('ref_axis',(-6.86155564311052E-17,0.309016994374945,0.951056516295154)) ;
#68614 = DIRECTION('center_axis',(-6.86155564311058E-17,0.309016994374947,
0.951056516295154)) ;
#68615 = DIRECTION('ref_axis',(0.707106781186557,0.672498511963948,-0.218508012224407)) ;
#68616 = DIRECTION('',(6.86155564311058E-17,-0.309016994374947,-0.951056516295154)) ;
#68617 = DIRECTION('',(-6.86155564311058E-17,0.309016994374947,0.951056516295154)) ;
#68618 = DIRECTION('center_axis',(1.,2.22044604925031E-16,0.)) ;
#68619 = DIRECTION('ref_axis',(0.,0.,-1.)) ;
#68620 = DIRECTION('center_axis',(1.,2.22044604925031E-16,0.)) ;
#68621 = DIRECTION('ref_axis',(9.02179155423715E-17,-0.406305370818768,0.913737350469939)) ;
#68622 = DIRECTION('center_axis',(1.,2.22044604925031E-16,0.)) ;
#68623 = DIRECTION('ref_axis',(-1.00806141154386E-16,0.453990499739549,0.891006524188367)) ;
#68624 = DIRECTION('center_axis',(1.30514544126042E-16,-0.587785252292473,
-0.809016994374948)) ;
#68625 = DIRECTION('ref_axis',(0.707106781186534,-0.572061402817695,0.415626937777461)) ;
#68626 = DIRECTION('',(-1.30514544126042E-16,0.587785252292473,0.809016994374948)) ;
#68627 = DIRECTION('',(1.30514544126042E-16,-0.587785252292473,-0.809016994374947)) ;
#68628 = DIRECTION('center_axis',(1.,2.22044604925031E-16,0.)) ;
#68629 = DIRECTION('ref_axis',(0.,0.587785252292692,0.809016994374789)) ;
#68630 = DIRECTION('center_axis',(-1.,-2.22044604925031E-16,0.)) ;
#68631 = DIRECTION('ref_axis',(-1.30514544126041E-16,0.587785252292468,0.809016994374951)) ;
#68632 = DIRECTION('center_axis',(1.,2.22044604925031E-16,0.)) ;
#68633 = DIRECTION('ref_axis',(-1.30514544126041E-16,0.587785252292468,0.809016994374951)) ;
#68634 = DIRECTION('center_axis',(-1.30514544126042E-16,0.587785252292473,
0.809016994374948)) ;
#68635 = DIRECTION('ref_axis',(0.707106781186568,0.572061402817668,-0.415626937777441)) ;
#68636 = DIRECTION('',(1.30514544126042E-16,-0.587785252292473,-0.809016994374947)) ;
#68637 = DIRECTION('',(-1.30514544126042E-16,0.587785252292473,0.809016994374947)) ;
#68638 = DIRECTION('center_axis',(1.,2.22044604925031E-16,0.)) ;
#68639 = DIRECTION('ref_axis',(0.,0.,-1.)) ;
#68640 = DIRECTION('center_axis',(1.,2.22044604925031E-16,0.)) ;
#68641 = DIRECTION('ref_axis',(9.02179155423715E-17,-0.406305370818768,0.913737350469939)) ;
#68642 = DIRECTION('center_axis',(1.,2.22044604925031E-16,0.)) ;
#68643 = DIRECTION('ref_axis',(-1.57009245868378E-16,0.70710678118655,0.707106781186545)) ;
#68644 = DIRECTION('center_axis',(1.79637858893621E-16,-0.809016994374947,
-0.587785252292473)) ;
#68645 = DIRECTION('ref_axis',(0.707106781186551,-0.415626937777451,0.572061402817682)) ;
#68646 = DIRECTION('',(-1.79637858893621E-16,0.809016994374947,0.587785252292473)) ;
#68647 = DIRECTION('',(1.79637858893621E-16,-0.809016994374947,-0.587785252292473)) ;
#68648 = DIRECTION('center_axis',(1.,2.22044604925031E-16,0.)) ;
#68649 = DIRECTION('ref_axis',(0.,0.809016994375189,0.58778525229214)) ;
#68650 = DIRECTION('center_axis',(-1.,-2.22044604925031E-16,0.)) ;
#68651 = DIRECTION('ref_axis',(-1.79637858893621E-16,0.809016994374947,0.587785252292474)) ;
#68652 = DIRECTION('center_axis',(1.,2.22044604925031E-16,0.)) ;
#68653 = DIRECTION('ref_axis',(-1.79637858893621E-16,0.809016994374947,0.587785252292474)) ;
#68654 = DIRECTION('center_axis',(-1.79637858893621E-16,0.809016994374947,
0.587785252292473)) ;
#68655 = DIRECTION('ref_axis',(0.707106781186592,0.415626937777427,-0.572061402817648)) ;
#68656 = DIRECTION('',(1.79637858893621E-16,-0.809016994374947,-0.587785252292473)) ;
#68657 = DIRECTION('',(-1.79637858893621E-16,0.809016994374947,0.587785252292473)) ;
#68658 = DIRECTION('center_axis',(1.,2.22044604925031E-16,0.)) ;
#68659 = DIRECTION('ref_axis',(0.,0.,-1.)) ;
#68660 = DIRECTION('center_axis',(1.,2.22044604925031E-16,0.)) ;
#68661 = DIRECTION('ref_axis',(9.02179155423715E-17,-0.406305370818768,0.913737350469939)) ;
#68662 = DIRECTION('center_axis',(1.,2.22044604925031E-16,0.)) ;
#68663 = DIRECTION('ref_axis',(-1.97843191649031E-16,0.891006524188368,0.453990499739546)) ;
#68664 = DIRECTION('center_axis',(2.11176968422134E-16,-0.951056516295154,
-0.309016994374948)) ;
#68665 = DIRECTION('ref_axis',(0.707106781186583,-0.2185080122244,0.672498511963923)) ;
#68666 = DIRECTION('',(-2.11176968422134E-16,0.951056516295153,0.309016994374948)) ;
#68667 = DIRECTION('',(2.11176968422134E-16,-0.951056516295153,-0.309016994374948)) ;
#68668 = DIRECTION('center_axis',(1.,2.22044604925031E-16,0.)) ;
#68669 = DIRECTION('ref_axis',(0.,0.951056516295183,0.309016994374858)) ;
#68670 = DIRECTION('center_axis',(-1.,-2.22044604925031E-16,0.)) ;
#68671 = DIRECTION('ref_axis',(-2.11176968422134E-16,0.951056516295153,0.309016994374948)) ;
#68672 = DIRECTION('center_axis',(1.,2.22044604925031E-16,0.)) ;
#68673 = DIRECTION('ref_axis',(-2.11176968422134E-16,0.951056516295153,0.309016994374948)) ;
#68674 = DIRECTION('center_axis',(-2.11176968422134E-16,0.951056516295154,
0.309016994374948)) ;
#68675 = DIRECTION('ref_axis',(0.707106781186563,0.218508012224406,-0.672498511963943)) ;
#68676 = DIRECTION('',(2.11176968422134E-16,-0.951056516295153,-0.309016994374948)) ;
#68677 = DIRECTION('',(-2.11176968422134E-16,0.951056516295153,0.309016994374948)) ;
#68678 = DIRECTION('center_axis',(1.,2.22044604925031E-16,0.)) ;
#68679 = DIRECTION('ref_axis',(0.,0.,-1.)) ;
#68680 = DIRECTION('center_axis',(1.,2.22044604925031E-16,0.)) ;
#68681 = DIRECTION('ref_axis',(9.02179155423715E-17,-0.406305370818768,0.913737350469939)) ;
#68682 = DIRECTION('center_axis',(1.,2.22044604925031E-16,0.)) ;
#68683 = DIRECTION('ref_axis',(-2.19310867376507E-16,0.987688340595138,0.15643446504023)) ;
#68684 = DIRECTION('center_axis',(2.22044604925031E-16,-1.,-2.22044604925031E-16)) ;
#68685 = DIRECTION('ref_axis',(0.707106781186568,9.08458920382451E-30,0.707106781186527)) ;
#68686 = DIRECTION('',(-2.22044604925031E-16,1.,2.22044604925031E-16)) ;
#68687 = DIRECTION('',(2.22044604925031E-16,-1.,-2.22044604925031E-16)) ;
#68688 = DIRECTION('center_axis',(1.,2.22044604925031E-16,0.)) ;
#68689 = DIRECTION('ref_axis',(0.,1.,-1.49213974509621E-13)) ;
#68690 = DIRECTION('center_axis',(-1.,-2.22044604925031E-16,0.)) ;
#68691 = DIRECTION('ref_axis',(-2.22044604925031E-16,1.,0.)) ;
#68692 = DIRECTION('center_axis',(1.,2.22044604925031E-16,0.)) ;
#68693 = DIRECTION('ref_axis',(-2.22044604925031E-16,1.,0.)) ;
#68694 = DIRECTION('center_axis',(-2.22044604925031E-16,1.,2.22044604925031E-16)) ;
#68695 = DIRECTION('ref_axis',(0.707106781186568,3.14018491736755E-16,-0.707106781186527)) ;
#68696 = DIRECTION('',(2.22044604925031E-16,-1.,-2.22044604925031E-16)) ;
#68697 = DIRECTION('',(-2.22044604925031E-16,1.,2.22044604925031E-16)) ;
#68698 = DIRECTION('center_axis',(1.,2.22044604925031E-16,0.)) ;
#68699 = DIRECTION('ref_axis',(0.,0.,-1.)) ;
#68700 = DIRECTION('center_axis',(1.,2.22044604925031E-16,0.)) ;
#68701 = DIRECTION('ref_axis',(9.02179155423715E-17,-0.406305370818768,0.913737350469939)) ;
#68702 = DIRECTION('center_axis',(1.,2.22044604925031E-16,0.)) ;
#68703 = DIRECTION('ref_axis',(-2.19310867376507E-16,0.987688340595138,-0.156434465040229)) ;
#68704 = DIRECTION('center_axis',(2.11176968422134E-16,-0.951056516295154,
0.309016994374947)) ;
#68705 = DIRECTION('ref_axis',(0.707106781186563,0.218508012224406,0.672498511963943)) ;
#68706 = DIRECTION('',(-2.11176968422134E-16,0.951056516295154,-0.309016994374947)) ;
#68707 = DIRECTION('',(2.11176968422134E-16,-0.951056516295154,0.309016994374947)) ;
#68708 = DIRECTION('center_axis',(1.,2.22044604925031E-16,0.)) ;
#68709 = DIRECTION('ref_axis',(0.,0.,-1.)) ;
#68710 = DIRECTION('center_axis',(-1.,-2.22044604925031E-16,0.)) ;
#68711 = DIRECTION('ref_axis',(-2.11176968422134E-16,0.951056516295153,-0.309016994374948)) ;
#68712 = DIRECTION('center_axis',(1.,2.22044604925031E-16,0.)) ;
#68713 = DIRECTION('ref_axis',(-2.11176968422134E-16,0.951056516295153,-0.309016994374948)) ;
#68714 = DIRECTION('center_axis',(-2.11176968422134E-16,0.951056516295154,
-0.309016994374947)) ;
#68715 = DIRECTION('ref_axis',(0.707106781186563,-0.218508012224405,-0.672498511963943)) ;
#68716 = DIRECTION('',(2.11176968422134E-16,-0.951056516295154,0.309016994374947)) ;
#68717 = DIRECTION('',(-2.11176968422134E-16,0.951056516295154,-0.309016994374947)) ;
#68718 = DIRECTION('center_axis',(1.,2.22044604925031E-16,0.)) ;
#68719 = DIRECTION('ref_axis',(0.,0.,-1.)) ;
#68720 = DIRECTION('center_axis',(1.,2.22044604925031E-16,0.)) ;
#68721 = DIRECTION('ref_axis',(9.02179155423715E-17,-0.406305370818768,0.913737350469939)) ;
#68722 = DIRECTION('center_axis',(1.,2.22044604925031E-16,0.)) ;
#68723 = DIRECTION('ref_axis',(-1.97843191649031E-16,0.891006524188368,-0.453990499739547)) ;
#68724 = DIRECTION('center_axis',(1.79637858893621E-16,-0.809016994374948,
0.587785252292473)) ;
#68725 = DIRECTION('ref_axis',(0.707106781186551,0.415626937777452,0.572061402817682)) ;
#68726 = DIRECTION('',(-1.79637858893621E-16,0.809016994374948,-0.587785252292473)) ;
#68727 = DIRECTION('',(1.79637858893621E-16,-0.809016994374948,0.587785252292473)) ;
#68728 = DIRECTION('center_axis',(1.,2.22044604925031E-16,0.)) ;
#68729 = DIRECTION('ref_axis',(0.,0.,-1.)) ;
#68730 = DIRECTION('center_axis',(-1.,-2.22044604925031E-16,0.)) ;
#68731 = DIRECTION('ref_axis',(-1.79637858893621E-16,0.809016994374947,-0.587785252292474)) ;
#68732 = DIRECTION('center_axis',(1.,2.22044604925031E-16,0.)) ;
#68733 = DIRECTION('ref_axis',(-1.79637858893621E-16,0.809016994374947,-0.587785252292474)) ;
#68734 = DIRECTION('center_axis',(-1.79637858893621E-16,0.809016994374948,
-0.587785252292473)) ;
#68735 = DIRECTION('ref_axis',(0.707106781186575,-0.415626937777437,-0.572061402817662)) ;
#68736 = DIRECTION('',(1.79637858893621E-16,-0.809016994374948,0.587785252292473)) ;
#68737 = DIRECTION('',(-1.79637858893621E-16,0.809016994374948,-0.587785252292473)) ;
#68738 = DIRECTION('center_axis',(1.,2.22044604925031E-16,0.)) ;
#68739 = DIRECTION('ref_axis',(0.,0.,-1.)) ;
#68740 = DIRECTION('center_axis',(1.,2.22044604925031E-16,0.)) ;
#68741 = DIRECTION('ref_axis',(9.02179155423715E-17,-0.406305370818768,0.913737350469939)) ;
#68742 = DIRECTION('center_axis',(1.,2.22044604925031E-16,0.)) ;
#68743 = DIRECTION('ref_axis',(-1.57009245868377E-16,0.707106781186547,-0.707106781186547)) ;
#68744 = DIRECTION('center_axis',(1.30514544126042E-16,-0.587785252292473,
0.809016994374947)) ;
#68745 = DIRECTION('ref_axis',(0.707106781186546,0.572061402817686,0.415626937777454)) ;
#68746 = DIRECTION('',(-1.30514544126042E-16,0.587785252292473,-0.809016994374947)) ;
#68747 = DIRECTION('',(1.30514544126042E-16,-0.587785252292473,0.809016994374947)) ;
#68748 = DIRECTION('center_axis',(1.,2.22044604925031E-16,0.)) ;
#68749 = DIRECTION('ref_axis',(0.,0.,-1.)) ;
#68750 = DIRECTION('center_axis',(-1.,-2.22044604925031E-16,0.)) ;
#68751 = DIRECTION('ref_axis',(-1.30514544126041E-16,0.587785252292468,-0.809016994374951)) ;
#68752 = DIRECTION('center_axis',(1.,2.22044604925031E-16,0.)) ;
#68753 = DIRECTION('ref_axis',(-1.30514544126041E-16,0.587785252292468,-0.809016994374951)) ;
#68754 = DIRECTION('center_axis',(-1.30514544126042E-16,0.587785252292473,
-0.809016994374947)) ;
#68755 = DIRECTION('ref_axis',(0.707106781186534,-0.572061402817695,-0.415626937777462)) ;
#68756 = DIRECTION('',(1.30514544126042E-16,-0.587785252292473,0.809016994374947)) ;
#68757 = DIRECTION('',(-1.30514544126042E-16,0.587785252292473,-0.809016994374947)) ;
#68758 = DIRECTION('center_axis',(1.,2.22044604925031E-16,0.)) ;
#68759 = DIRECTION('ref_axis',(0.,0.,-1.)) ;
#68760 = DIRECTION('center_axis',(1.,2.22044604925031E-16,0.)) ;
#68761 = DIRECTION('ref_axis',(9.02179155423715E-17,-0.406305370818768,0.913737350469939)) ;
#68762 = DIRECTION('center_axis',(1.,2.22044604925031E-16,0.)) ;
#68763 = DIRECTION('ref_axis',(-1.00806141154385E-16,0.453990499739547,-0.891006524188368)) ;
#68764 = DIRECTION('center_axis',(6.86155564311059E-17,-0.309016994374948,
0.951056516295154)) ;
#68765 = DIRECTION('ref_axis',(0.707106781186557,0.672498511963948,0.218508012224408)) ;
#68766 = DIRECTION('',(6.86155564311059E-17,-0.309016994374948,0.951056516295153)) ;
#68767 = DIRECTION('',(-6.86155564311059E-17,0.309016994374948,-0.951056516295153)) ;
#68768 = DIRECTION('center_axis',(1.,2.22044604925031E-16,0.)) ;
#68769 = DIRECTION('ref_axis',(0.,0.,-1.)) ;
#68770 = DIRECTION('center_axis',(1.,2.22044604925031E-16,0.)) ;
#68771 = DIRECTION('ref_axis',(-6.86155564311052E-17,0.309016994374945,-0.951056516295154)) ;
#68772 = DIRECTION('center_axis',(-1.,-2.22044604925031E-16,0.)) ;
#68773 = DIRECTION('ref_axis',(-6.86155564311052E-17,0.309016994374945,-0.951056516295154)) ;
#68774 = DIRECTION('center_axis',(-6.86155564311059E-17,0.309016994374948,
-0.951056516295154)) ;
#68775 = DIRECTION('ref_axis',(0.707106781186557,-0.672498511963948,-0.218508012224408)) ;
#68776 = DIRECTION('',(-6.86155564311059E-17,0.309016994374948,-0.951056516295153)) ;
#68777 = DIRECTION('',(6.86155564311059E-17,-0.309016994374948,0.951056516295153)) ;
#68778 = DIRECTION('center_axis',(1.,2.22044604925031E-16,0.)) ;
#68779 = DIRECTION('ref_axis',(0.,0.,-1.)) ;
#68780 = DIRECTION('center_axis',(1.,2.22044604925031E-16,0.)) ;
#68781 = DIRECTION('ref_axis',(-3.47354289865169E-17,0.156434465040232,-0.987688340595138)) ;
#68782 = DIRECTION('center_axis',(1.,2.22044604925031E-16,0.)) ;
#68783 = DIRECTION('ref_axis',(9.02179155423715E-17,-0.406305370818768,0.913737350469939)) ;
#68784 = DIRECTION('center_axis',(0.,0.,1.)) ;
#68785 = DIRECTION('ref_axis',(0.707106781186589,0.707106781186506,0.)) ;
#68786 = DIRECTION('',(0.,0.,1.)) ;
#68787 = DIRECTION('',(0.,0.,-1.)) ;
#68788 = DIRECTION('center_axis',(1.,2.22044604925031E-16,0.)) ;
#68789 = DIRECTION('ref_axis',(0.,0.,-1.)) ;
#68790 = DIRECTION('center_axis',(1.,2.22044604925031E-16,0.)) ;
#68791 = DIRECTION('ref_axis',(0.,0.,-1.)) ;
#68792 = DIRECTION('center_axis',(-1.,-2.22044604925031E-16,0.)) ;
#68793 = DIRECTION('ref_axis',(0.,0.,-1.)) ;
#68794 = DIRECTION('center_axis',(0.,0.,-1.)) ;
#68795 = DIRECTION('ref_axis',(0.707106781186569,-0.707106781186526,0.)) ;
#68796 = DIRECTION('',(0.,0.,-1.)) ;
#68797 = DIRECTION('',(0.,0.,1.)) ;
#68798 = DIRECTION('center_axis',(1.,2.22044604925031E-16,0.)) ;
#68799 = DIRECTION('ref_axis',(0.,0.,-1.)) ;
#68800 = DIRECTION('center_axis',(1.,2.22044604925031E-16,0.)) ;
#68801 = DIRECTION('ref_axis',(3.47354289865167E-17,-0.156434465040231,-0.987688340595138)) ;
#68802 = DIRECTION('center_axis',(1.,2.22044604925031E-16,0.)) ;
#68803 = DIRECTION('ref_axis',(9.02179155423715E-17,-0.406305370818768,0.913737350469939)) ;
#68804 = DIRECTION('center_axis',(-6.86155564311058E-17,0.309016994374947,
0.951056516295154)) ;
#68805 = DIRECTION('ref_axis',(0.707106781186557,0.672498511963948,-0.218508012224407)) ;
#68806 = DIRECTION('',(-6.86155564311058E-17,0.309016994374947,0.951056516295154)) ;
#68807 = DIRECTION('',(6.86155564311058E-17,-0.309016994374947,-0.951056516295154)) ;
#68808 = DIRECTION('center_axis',(1.,2.22044604925031E-16,0.)) ;
#68809 = DIRECTION('ref_axis',(0.,0.,-1.)) ;
#68810 = DIRECTION('center_axis',(1.,2.22044604925031E-16,0.)) ;
#68811 = DIRECTION('ref_axis',(6.86155564311052E-17,-0.309016994374945,-0.951056516295154)) ;
#68812 = DIRECTION('center_axis',(-1.,-2.22044604925031E-16,0.)) ;
#68813 = DIRECTION('ref_axis',(6.86155564311052E-17,-0.309016994374945,-0.951056516295154)) ;
#68814 = DIRECTION('center_axis',(6.86155564311058E-17,-0.309016994374947,
-0.951056516295154)) ;
#68815 = DIRECTION('ref_axis',(0.707106781186557,-0.672498511963948,0.218508012224407)) ;
#68816 = DIRECTION('',(6.86155564311058E-17,-0.309016994374947,-0.951056516295154)) ;
#68817 = DIRECTION('',(-6.86155564311058E-17,0.309016994374947,0.951056516295154)) ;
#68818 = DIRECTION('center_axis',(1.,2.22044604925031E-16,0.)) ;
#68819 = DIRECTION('ref_axis',(0.,0.,-1.)) ;
#68820 = DIRECTION('center_axis',(1.,2.22044604925031E-16,0.)) ;
#68821 = DIRECTION('ref_axis',(1.00806141154385E-16,-0.453990499739546,-0.891006524188368)) ;
#68822 = DIRECTION('center_axis',(1.,2.22044604925031E-16,0.)) ;
#68823 = DIRECTION('ref_axis',(9.02179155423715E-17,-0.406305370818768,0.913737350469939)) ;
#68824 = DIRECTION('center_axis',(-1.30514544126042E-16,0.587785252292473,
0.809016994374948)) ;
#68825 = DIRECTION('ref_axis',(0.707106781186551,0.572061402817682,-0.415626937777451)) ;
#68826 = DIRECTION('',(-1.30514544126042E-16,0.587785252292473,0.809016994374947)) ;
#68827 = DIRECTION('',(1.30514544126042E-16,-0.587785252292473,-0.809016994374947)) ;
#68828 = DIRECTION('center_axis',(1.,2.22044604925031E-16,0.)) ;
#68829 = DIRECTION('ref_axis',(0.,0.,-1.)) ;
#68830 = DIRECTION('center_axis',(1.,2.22044604925031E-16,0.)) ;
#68831 = DIRECTION('ref_axis',(1.30514544126042E-16,-0.587785252292474,-0.809016994374947)) ;
#68832 = DIRECTION('center_axis',(-1.,-2.22044604925031E-16,0.)) ;
#68833 = DIRECTION('ref_axis',(1.30514544126042E-16,-0.587785252292474,-0.809016994374947)) ;
#68834 = DIRECTION('center_axis',(1.30514544126042E-16,-0.587785252292473,
-0.809016994374948)) ;
#68835 = DIRECTION('ref_axis',(0.707106781186563,-0.572061402817672,0.415626937777444)) ;
#68836 = DIRECTION('',(1.30514544126042E-16,-0.587785252292473,-0.809016994374947)) ;
#68837 = DIRECTION('',(-1.30514544126042E-16,0.587785252292473,0.809016994374947)) ;
#68838 = DIRECTION('center_axis',(1.,2.22044604925031E-16,0.)) ;
#68839 = DIRECTION('ref_axis',(0.,0.,-1.)) ;
#68840 = DIRECTION('center_axis',(1.,2.22044604925031E-16,0.)) ;
#68841 = DIRECTION('ref_axis',(1.57009245868377E-16,-0.707106781186547,-0.707106781186548)) ;
#68842 = DIRECTION('center_axis',(1.,2.22044604925031E-16,0.)) ;
#68843 = DIRECTION('ref_axis',(9.02179155423715E-17,-0.406305370818768,0.913737350469939)) ;
#68844 = DIRECTION('center_axis',(-1.79637858893621E-16,0.809016994374947,
0.587785252292473)) ;
#68845 = DIRECTION('ref_axis',(0.707106781186568,0.415626937777442,-0.572061402817668)) ;
#68846 = DIRECTION('',(-1.79637858893621E-16,0.809016994374947,0.587785252292473)) ;
#68847 = DIRECTION('',(1.79637858893621E-16,-0.809016994374947,-0.587785252292473)) ;
#68848 = DIRECTION('center_axis',(1.,2.22044604925031E-16,0.)) ;
#68849 = DIRECTION('ref_axis',(0.,0.,-1.)) ;
#68850 = DIRECTION('center_axis',(1.,2.22044604925031E-16,0.)) ;
#68851 = DIRECTION('ref_axis',(1.79637858893621E-16,-0.809016994374947,-0.587785252292474)) ;
#68852 = DIRECTION('center_axis',(-1.,-2.22044604925031E-16,0.)) ;
#68853 = DIRECTION('ref_axis',(1.79637858893621E-16,-0.809016994374947,-0.587785252292474)) ;
#68854 = DIRECTION('center_axis',(1.79637858893621E-16,-0.809016994374947,
-0.587785252292473)) ;
#68855 = DIRECTION('ref_axis',(0.707106781186563,-0.415626937777444,0.572061402817672)) ;
#68856 = DIRECTION('',(1.79637858893621E-16,-0.809016994374947,-0.587785252292473)) ;
#68857 = DIRECTION('',(-1.79637858893621E-16,0.809016994374947,0.587785252292473)) ;
#68858 = DIRECTION('center_axis',(1.,2.22044604925031E-16,0.)) ;
#68859 = DIRECTION('ref_axis',(0.,0.,-1.)) ;
#68860 = DIRECTION('center_axis',(1.,2.22044604925031E-16,0.)) ;
#68861 = DIRECTION('ref_axis',(1.97843191649031E-16,-0.891006524188368,-0.453990499739547)) ;
#68862 = DIRECTION('center_axis',(1.,2.22044604925031E-16,0.)) ;
#68863 = DIRECTION('ref_axis',(9.02179155423715E-17,-0.406305370818768,0.913737350469939)) ;
#68864 = DIRECTION('center_axis',(-2.11176968422134E-16,0.951056516295154,
0.309016994374948)) ;
#68865 = DIRECTION('ref_axis',(0.707106781186557,0.218508012224408,-0.672498511963948)) ;
#68866 = DIRECTION('',(-2.11176968422134E-16,0.951056516295154,0.309016994374948)) ;
#68867 = DIRECTION('',(2.11176968422134E-16,-0.951056516295154,-0.309016994374948)) ;
#68868 = DIRECTION('center_axis',(1.,2.22044604925031E-16,0.)) ;
#68869 = DIRECTION('ref_axis',(0.,0.,-1.)) ;
#68870 = DIRECTION('center_axis',(1.,2.22044604925031E-16,0.)) ;
#68871 = DIRECTION('ref_axis',(2.11176968422134E-16,-0.951056516295154,-0.309016994374945)) ;
#68872 = DIRECTION('center_axis',(-1.,-2.22044604925031E-16,0.)) ;
#68873 = DIRECTION('ref_axis',(2.11176968422134E-16,-0.951056516295154,-0.309016994374945)) ;
#68874 = DIRECTION('center_axis',(2.11176968422134E-16,-0.951056516295154,
-0.309016994374948)) ;
#68875 = DIRECTION('ref_axis',(0.707106781186557,-0.218508012224408,0.672498511963948)) ;
#68876 = DIRECTION('',(2.11176968422134E-16,-0.951056516295154,-0.309016994374948)) ;
#68877 = DIRECTION('',(-2.11176968422134E-16,0.951056516295154,0.309016994374948)) ;
#68878 = DIRECTION('center_axis',(1.,2.22044604925031E-16,0.)) ;
#68879 = DIRECTION('ref_axis',(0.,0.,-1.)) ;
#68880 = DIRECTION('center_axis',(1.,2.22044604925031E-16,0.)) ;
#68881 = DIRECTION('ref_axis',(2.19310867376507E-16,-0.987688340595138,-0.156434465040231)) ;
#68882 = DIRECTION('center_axis',(1.,2.22044604925031E-16,0.)) ;
#68883 = DIRECTION('ref_axis',(9.02179155423715E-17,-0.406305370818768,0.913737350469939)) ;
#68884 = DIRECTION('center_axis',(-2.22044604925031E-16,1.,5.55111512312578E-17)) ;
#68885 = DIRECTION('ref_axis',(0.707106781186568,1.96261557335475E-16,-0.707106781186527)) ;
#68886 = DIRECTION('',(-2.22044604925031E-16,1.,5.55111512312578E-17)) ;
#68887 = DIRECTION('',(2.22044604925031E-16,-1.,-5.55111512312578E-17)) ;
#68888 = DIRECTION('center_axis',(1.,2.22044604925031E-16,0.)) ;
#68889 = DIRECTION('ref_axis',(0.,-1.,4.68958205601666E-13)) ;
#68890 = DIRECTION('center_axis',(1.,2.22044604925031E-16,0.)) ;
#68891 = DIRECTION('ref_axis',(2.22044604925031E-16,-1.,0.)) ;
#68892 = DIRECTION('center_axis',(-1.,-2.22044604925031E-16,0.)) ;
#68893 = DIRECTION('ref_axis',(2.22044604925031E-16,-1.,0.)) ;
#68894 = DIRECTION('center_axis',(2.22044604925031E-16,-1.,-5.55111512312578E-17)) ;
#68895 = DIRECTION('ref_axis',(0.707106781186568,1.17756934401289E-16,0.707106781186527)) ;
#68896 = DIRECTION('',(2.22044604925031E-16,-1.,-5.55111512312578E-17)) ;
#68897 = DIRECTION('',(-2.22044604925031E-16,1.,5.55111512312578E-17)) ;
#68898 = DIRECTION('center_axis',(1.,2.22044604925031E-16,0.)) ;
#68899 = DIRECTION('ref_axis',(0.,0.,-1.)) ;
#68900 = DIRECTION('center_axis',(1.,2.22044604925031E-16,0.)) ;
#68901 = DIRECTION('ref_axis',(2.19310867376507E-16,-0.987688340595138,0.156434465040229)) ;
#68902 = DIRECTION('center_axis',(1.,2.22044604925031E-16,0.)) ;
#68903 = DIRECTION('ref_axis',(9.02179155423715E-17,-0.406305370818768,0.913737350469939)) ;
#68904 = DIRECTION('center_axis',(-2.11176968422134E-16,0.951056516295154,
-0.309016994374947)) ;
#68905 = DIRECTION('ref_axis',(0.707106781186557,-0.218508012224407,-0.672498511963949)) ;
#68906 = DIRECTION('',(-2.11176968422134E-16,0.951056516295154,-0.309016994374947)) ;
#68907 = DIRECTION('',(2.11176968422134E-16,-0.951056516295154,0.309016994374947)) ;
#68908 = DIRECTION('center_axis',(1.,2.22044604925031E-16,0.)) ;
#68909 = DIRECTION('ref_axis',(0.,-0.95105651629504,0.309016994375296)) ;
#68910 = DIRECTION('center_axis',(1.,2.22044604925031E-16,0.)) ;
#68911 = DIRECTION('ref_axis',(2.11176968422134E-16,-0.951056516295154,0.309016994374945)) ;
#68912 = DIRECTION('center_axis',(-1.,-2.22044604925031E-16,0.)) ;
#68913 = DIRECTION('ref_axis',(2.11176968422134E-16,-0.951056516295154,0.309016994374945)) ;
#68914 = DIRECTION('center_axis',(2.11176968422134E-16,-0.951056516295154,
0.309016994374947)) ;
#68915 = DIRECTION('ref_axis',(0.707106781186557,0.218508012224407,0.672498511963948)) ;
#68916 = DIRECTION('',(2.11176968422134E-16,-0.951056516295154,0.309016994374947)) ;
#68917 = DIRECTION('',(-2.11176968422134E-16,0.951056516295154,-0.309016994374947)) ;
#68918 = DIRECTION('center_axis',(1.,2.22044604925031E-16,0.)) ;
#68919 = DIRECTION('ref_axis',(0.,0.,-1.)) ;
#68920 = DIRECTION('center_axis',(1.,2.22044604925031E-16,0.)) ;
#68921 = DIRECTION('ref_axis',(1.97843191649031E-16,-0.891006524188369,0.453990499739545)) ;
#68922 = DIRECTION('center_axis',(1.,2.22044604925031E-16,0.)) ;
#68923 = DIRECTION('ref_axis',(9.02179155423715E-17,-0.406305370818768,0.913737350469939)) ;
#68924 = DIRECTION('center_axis',(-1.79637858893621E-16,0.809016994374948,
-0.587785252292473)) ;
#68925 = DIRECTION('ref_axis',(0.707106781186563,-0.415626937777444,-0.572061402817672)) ;
#68926 = DIRECTION('',(-1.79637858893621E-16,0.809016994374947,-0.587785252292473)) ;
#68927 = DIRECTION('',(1.79637858893621E-16,-0.809016994374947,0.587785252292473)) ;
#68928 = DIRECTION('center_axis',(1.,2.22044604925031E-16,0.)) ;
#68929 = DIRECTION('ref_axis',(0.,-0.809016994374969,0.587785252292443)) ;
#68930 = DIRECTION('center_axis',(1.,2.22044604925031E-16,0.)) ;
#68931 = DIRECTION('ref_axis',(1.79637858893621E-16,-0.809016994374947,0.587785252292474)) ;
#68932 = DIRECTION('center_axis',(-1.,-2.22044604925031E-16,0.)) ;
#68933 = DIRECTION('ref_axis',(1.79637858893621E-16,-0.809016994374947,0.587785252292474)) ;
#68934 = DIRECTION('center_axis',(1.79637858893621E-16,-0.809016994374948,
0.587785252292473)) ;
#68935 = DIRECTION('ref_axis',(0.707106781186563,0.415626937777444,0.572061402817672)) ;
#68936 = DIRECTION('',(1.79637858893621E-16,-0.809016994374947,0.587785252292473)) ;
#68937 = DIRECTION('',(-1.79637858893621E-16,0.809016994374947,-0.587785252292473)) ;
#68938 = DIRECTION('center_axis',(1.,2.22044604925031E-16,0.)) ;
#68939 = DIRECTION('ref_axis',(0.,0.,-1.)) ;
#68940 = DIRECTION('center_axis',(1.,2.22044604925031E-16,0.)) ;
#68941 = DIRECTION('ref_axis',(1.57009245868377E-16,-0.707106781186548,0.707106781186547)) ;
#68942 = DIRECTION('center_axis',(1.,2.22044604925031E-16,0.)) ;
#68943 = DIRECTION('ref_axis',(9.02179155423715E-17,-0.406305370818768,0.913737350469939)) ;
#68944 = DIRECTION('center_axis',(-1.30514544126042E-16,0.587785252292473,
-0.809016994374947)) ;
#68945 = DIRECTION('ref_axis',(0.707106781186551,-0.572061402817681,-0.415626937777452)) ;
#68946 = DIRECTION('',(-1.30514544126042E-16,0.587785252292473,-0.809016994374947)) ;
#68947 = DIRECTION('',(1.30514544126042E-16,-0.587785252292473,0.809016994374947)) ;
#68948 = DIRECTION('center_axis',(1.,2.22044604925031E-16,0.)) ;
#68949 = DIRECTION('ref_axis',(0.,-0.587785252292056,0.809016994375251)) ;
#68950 = DIRECTION('center_axis',(1.,2.22044604925031E-16,0.)) ;
#68951 = DIRECTION('ref_axis',(1.30514544126042E-16,-0.587785252292474,0.809016994374947)) ;
#68952 = DIRECTION('center_axis',(-1.,-2.22044604925031E-16,0.)) ;
#68953 = DIRECTION('ref_axis',(1.30514544126042E-16,-0.587785252292474,0.809016994374947)) ;
#68954 = DIRECTION('center_axis',(1.30514544126042E-16,-0.587785252292473,
0.809016994374947)) ;
#68955 = DIRECTION('ref_axis',(0.707106781186563,0.572061402817672,0.415626937777444)) ;
#68956 = DIRECTION('',(1.30514544126042E-16,-0.587785252292473,0.809016994374947)) ;
#68957 = DIRECTION('',(-1.30514544126042E-16,0.587785252292473,-0.809016994374947)) ;
#68958 = DIRECTION('center_axis',(-2.11176968422134E-16,0.951056516295154,
0.309016994374948)) ;
#68959 = DIRECTION('ref_axis',(6.86155564311059E-17,-0.309016994374948,0.951056516295153)) ;
#68960 = DIRECTION('',(1.,2.22044604925031E-16,0.)) ;
#68961 = DIRECTION('',(-6.86155564311059E-17,0.309016994374948,-0.951056516295153)) ;
#68962 = DIRECTION('',(-1.,-2.22044604925031E-16,0.)) ;
#68963 = DIRECTION('center_axis',(1.,2.22044604925031E-16,0.)) ;
#68964 = DIRECTION('ref_axis',(-6.8615556431103E-17,0.309016994374935,-0.951056516295158)) ;
#68965 = DIRECTION('',(1.,2.22044604925031E-16,0.)) ;
#68966 = DIRECTION('center_axis',(-1.,-2.22044604925031E-16,0.)) ;
#68967 = DIRECTION('ref_axis',(-6.86155564311052E-17,0.309016994374945,-0.951056516295154)) ;
#68968 = DIRECTION('center_axis',(2.11176968422134E-16,-0.951056516295154,
-0.309016994374948)) ;
#68969 = DIRECTION('ref_axis',(-6.86155564311059E-17,0.309016994374948,-0.951056516295153)) ;
#68970 = DIRECTION('',(1.,2.22044604925031E-16,0.)) ;
#68971 = DIRECTION('',(6.86155564311059E-17,-0.309016994374948,0.951056516295153)) ;
#68972 = DIRECTION('center_axis',(1.,2.22044604925031E-16,0.)) ;
#68973 = DIRECTION('ref_axis',(2.22044604925031E-16,-1.,0.)) ;
#68974 = DIRECTION('',(-1.,-2.22044604925031E-16,0.)) ;
#68975 = DIRECTION('center_axis',(-1.,-2.22044604925031E-16,0.)) ;
#68976 = DIRECTION('ref_axis',(-3.47354289865169E-17,0.156434465040232,-0.987688340595138)) ;
#68977 = DIRECTION('center_axis',(-2.22044604925031E-16,1.,0.)) ;
#68978 = DIRECTION('ref_axis',(0.,0.,1.)) ;
#68979 = DIRECTION('',(1.,2.22044604925031E-16,0.)) ;
#68980 = DIRECTION('',(0.,0.,-1.)) ;
#68981 = DIRECTION('center_axis',(1.,2.22044604925031E-16,0.)) ;
#68982 = DIRECTION('ref_axis',(9.99672442260732E-31,-4.50212443845799E-15,
-1.)) ;
#68983 = DIRECTION('',(1.,2.22044604925031E-16,0.)) ;
#68984 = DIRECTION('center_axis',(-1.,-2.22044604925031E-16,0.)) ;
#68985 = DIRECTION('ref_axis',(0.,0.,-1.)) ;
#68986 = DIRECTION('center_axis',(2.22044604925031E-16,-1.,0.)) ;
#68987 = DIRECTION('ref_axis',(0.,0.,-1.)) ;
#68988 = DIRECTION('',(1.,2.22044604925031E-16,0.)) ;
#68989 = DIRECTION('',(0.,0.,1.)) ;
#68990 = DIRECTION('center_axis',(1.,2.22044604925031E-16,0.)) ;
#68991 = DIRECTION('ref_axis',(2.22044604925031E-16,-1.,0.)) ;
#68992 = DIRECTION('',(-1.,-2.22044604925031E-16,0.)) ;
#68993 = DIRECTION('center_axis',(-1.,-2.22044604925031E-16,0.)) ;
#68994 = DIRECTION('ref_axis',(3.47354289865164E-17,-0.15643446504023,-0.987688340595138)) ;
#68995 = DIRECTION('center_axis',(-2.11176968422134E-16,0.951056516295154,
-0.309016994374947)) ;
#68996 = DIRECTION('ref_axis',(-6.86155564311058E-17,0.309016994374947,0.951056516295154)) ;
#68997 = DIRECTION('',(1.,2.22044604925031E-16,0.)) ;
#68998 = DIRECTION('',(6.86155564311058E-17,-0.309016994374947,-0.951056516295154)) ;
#68999 = DIRECTION('center_axis',(1.,2.22044604925031E-16,0.)) ;
#69000 = DIRECTION('ref_axis',(6.86155564311052E-17,-0.309016994374945,-0.951056516295154)) ;
#69001 = DIRECTION('',(1.,2.22044604925031E-16,0.)) ;
#69002 = DIRECTION('center_axis',(-1.,-2.22044604925031E-16,0.)) ;
#69003 = DIRECTION('ref_axis',(6.86155564311052E-17,-0.309016994374945,-0.951056516295154)) ;
#69004 = DIRECTION('center_axis',(2.11176968422134E-16,-0.951056516295154,
0.309016994374947)) ;
#69005 = DIRECTION('ref_axis',(6.86155564311058E-17,-0.309016994374947,-0.951056516295154)) ;
#69006 = DIRECTION('',(1.,2.22044604925031E-16,0.)) ;
#69007 = DIRECTION('',(-6.86155564311058E-17,0.309016994374947,0.951056516295154)) ;
#69008 = DIRECTION('center_axis',(1.,2.22044604925031E-16,0.)) ;
#69009 = DIRECTION('ref_axis',(2.22044604925031E-16,-1.,0.)) ;
#69010 = DIRECTION('',(-1.,-2.22044604925031E-16,0.)) ;
#69011 = DIRECTION('center_axis',(-1.,-2.22044604925031E-16,0.)) ;
#69012 = DIRECTION('ref_axis',(1.00806141154385E-16,-0.453990499739546,-0.891006524188368)) ;
#69013 = DIRECTION('center_axis',(-1.79637858893621E-16,0.809016994374948,
-0.587785252292473)) ;
#69014 = DIRECTION('ref_axis',(-1.30514544126042E-16,0.587785252292473,0.809016994374948)) ;
#69015 = DIRECTION('',(1.,2.22044604925031E-16,0.)) ;
#69016 = DIRECTION('',(1.30514544126042E-16,-0.587785252292473,-0.809016994374947)) ;
#69017 = DIRECTION('center_axis',(1.,2.22044604925031E-16,0.)) ;
#69018 = DIRECTION('ref_axis',(1.30514544126041E-16,-0.587785252292468,-0.809016994374951)) ;
#69019 = DIRECTION('',(1.,2.22044604925031E-16,0.)) ;
#69020 = DIRECTION('center_axis',(-1.,-2.22044604925031E-16,0.)) ;
#69021 = DIRECTION('ref_axis',(1.30514544126042E-16,-0.587785252292474,-0.809016994374947)) ;
#69022 = DIRECTION('center_axis',(1.79637858893621E-16,-0.809016994374948,
0.587785252292473)) ;
#69023 = DIRECTION('ref_axis',(1.30514544126042E-16,-0.587785252292473,-0.809016994374948)) ;
#69024 = DIRECTION('',(1.,2.22044604925031E-16,0.)) ;
#69025 = DIRECTION('',(-1.30514544126042E-16,0.587785252292473,0.809016994374947)) ;
#69026 = DIRECTION('center_axis',(1.,2.22044604925031E-16,0.)) ;
#69027 = DIRECTION('ref_axis',(2.22044604925031E-16,-1.,0.)) ;
#69028 = DIRECTION('',(-1.,-2.22044604925031E-16,0.)) ;
#69029 = DIRECTION('center_axis',(-1.,-2.22044604925031E-16,0.)) ;
#69030 = DIRECTION('ref_axis',(1.57009245868377E-16,-0.707106781186547,-0.707106781186548)) ;
#69031 = DIRECTION('center_axis',(-1.30514544126042E-16,0.587785252292473,
-0.809016994374947)) ;
#69032 = DIRECTION('ref_axis',(-1.79637858893621E-16,0.809016994374947,0.587785252292473)) ;
#69033 = DIRECTION('',(1.,2.22044604925031E-16,0.)) ;
#69034 = DIRECTION('',(1.79637858893621E-16,-0.809016994374947,-0.587785252292473)) ;
#69035 = DIRECTION('center_axis',(1.,2.22044604925031E-16,0.)) ;
#69036 = DIRECTION('ref_axis',(1.79637858893621E-16,-0.809016994374949,-0.587785252292472)) ;
#69037 = DIRECTION('',(1.,2.22044604925031E-16,0.)) ;
#69038 = DIRECTION('center_axis',(-1.,-2.22044604925031E-16,0.)) ;
#69039 = DIRECTION('ref_axis',(1.79637858893621E-16,-0.809016994374947,-0.587785252292474)) ;
#69040 = DIRECTION('center_axis',(1.30514544126042E-16,-0.587785252292473,
0.809016994374947)) ;
#69041 = DIRECTION('ref_axis',(1.79637858893621E-16,-0.809016994374947,-0.587785252292473)) ;
#69042 = DIRECTION('',(1.,2.22044604925031E-16,0.)) ;
#69043 = DIRECTION('',(-1.79637858893621E-16,0.809016994374947,0.587785252292473)) ;
#69044 = DIRECTION('center_axis',(1.,2.22044604925031E-16,0.)) ;
#69045 = DIRECTION('ref_axis',(2.22044604925031E-16,-1.,0.)) ;
#69046 = DIRECTION('',(-1.,-2.22044604925031E-16,0.)) ;
#69047 = DIRECTION('center_axis',(-1.,-2.22044604925031E-16,0.)) ;
#69048 = DIRECTION('ref_axis',(1.97843191649031E-16,-0.891006524188368,-0.453990499739547)) ;
#69049 = DIRECTION('center_axis',(-6.86155564311058E-17,0.309016994374948,
-0.951056516295154)) ;
#69050 = DIRECTION('ref_axis',(-2.11176968422134E-16,0.951056516295154,0.309016994374948)) ;
#69051 = DIRECTION('',(1.,2.22044604925031E-16,0.)) ;
#69052 = DIRECTION('',(2.11176968422134E-16,-0.951056516295154,-0.309016994374948)) ;
#69053 = DIRECTION('center_axis',(1.,2.22044604925031E-16,0.)) ;
#69054 = DIRECTION('ref_axis',(2.11176968422134E-16,-0.951056516295157,-0.309016994374937)) ;
#69055 = DIRECTION('',(1.,2.22044604925031E-16,0.)) ;
#69056 = DIRECTION('center_axis',(-1.,-2.22044604925031E-16,0.)) ;
#69057 = DIRECTION('ref_axis',(2.11176968422134E-16,-0.951056516295154,-0.309016994374945)) ;
#69058 = DIRECTION('center_axis',(6.86155564311058E-17,-0.309016994374948,
0.951056516295154)) ;
#69059 = DIRECTION('ref_axis',(2.11176968422134E-16,-0.951056516295154,-0.309016994374948)) ;
#69060 = DIRECTION('',(1.,2.22044604925031E-16,0.)) ;
#69061 = DIRECTION('',(-2.11176968422134E-16,0.951056516295154,0.309016994374948)) ;
#69062 = DIRECTION('center_axis',(1.,2.22044604925031E-16,0.)) ;
#69063 = DIRECTION('ref_axis',(2.22044604925031E-16,-1.,0.)) ;
#69064 = DIRECTION('',(-1.,-2.22044604925031E-16,0.)) ;
#69065 = DIRECTION('center_axis',(-1.,-2.22044604925031E-16,0.)) ;
#69066 = DIRECTION('ref_axis',(2.19310867376507E-16,-0.987688340595138,-0.156434465040231)) ;
#69067 = DIRECTION('center_axis',(-1.23259516440783E-32,5.55111512312578E-17,
-1.)) ;
#69068 = DIRECTION('ref_axis',(-2.22044604925031E-16,1.,5.55111512312578E-17)) ;
#69069 = DIRECTION('',(1.,2.22044604925031E-16,0.)) ;
#69070 = DIRECTION('',(2.22044604925031E-16,-1.,-5.55111512312578E-17)) ;
#69071 = DIRECTION('center_axis',(1.,2.22044604925031E-16,0.)) ;
#69072 = DIRECTION('ref_axis',(2.22044604925031E-16,-1.,6.5797721569339E-16)) ;
#69073 = DIRECTION('',(1.,2.22044604925031E-16,0.)) ;
#69074 = DIRECTION('center_axis',(-1.,-2.22044604925031E-16,0.)) ;
#69075 = DIRECTION('ref_axis',(2.22044604925031E-16,-1.,0.)) ;
#69076 = DIRECTION('center_axis',(1.23259516440783E-32,-5.55111512312578E-17,
1.)) ;
#69077 = DIRECTION('ref_axis',(2.22044604925031E-16,-1.,-5.55111512312578E-17)) ;
#69078 = DIRECTION('',(1.,2.22044604925031E-16,0.)) ;
#69079 = DIRECTION('',(-2.22044604925031E-16,1.,5.55111512312578E-17)) ;
#69080 = DIRECTION('center_axis',(1.,2.22044604925031E-16,0.)) ;
#69081 = DIRECTION('ref_axis',(2.22044604925031E-16,-1.,0.)) ;
#69082 = DIRECTION('',(-1.,-2.22044604925031E-16,0.)) ;
#69083 = DIRECTION('center_axis',(-1.,-2.22044604925031E-16,0.)) ;
#69084 = DIRECTION('ref_axis',(2.19310867376507E-16,-0.987688340595138,0.156434465040229)) ;
#69085 = DIRECTION('center_axis',(6.86155564311058E-17,-0.309016994374947,
-0.951056516295154)) ;
#69086 = DIRECTION('ref_axis',(-2.11176968422134E-16,0.951056516295154,-0.309016994374947)) ;
#69087 = DIRECTION('',(1.,2.22044604925031E-16,0.)) ;
#69088 = DIRECTION('',(2.11176968422134E-16,-0.951056516295154,0.309016994374947)) ;
#69089 = DIRECTION('center_axis',(1.,2.22044604925031E-16,0.)) ;
#69090 = DIRECTION('ref_axis',(2.11176968422134E-16,-0.951056516295156,0.309016994374939)) ;
#69091 = DIRECTION('',(1.,2.22044604925031E-16,0.)) ;
#69092 = DIRECTION('center_axis',(-1.,-2.22044604925031E-16,0.)) ;
#69093 = DIRECTION('ref_axis',(2.11176968422134E-16,-0.951056516295154,0.309016994374945)) ;
#69094 = DIRECTION('center_axis',(-6.86155564311058E-17,0.309016994374947,
0.951056516295154)) ;
#69095 = DIRECTION('ref_axis',(2.11176968422134E-16,-0.951056516295154,0.309016994374947)) ;
#69096 = DIRECTION('',(1.,2.22044604925031E-16,0.)) ;
#69097 = DIRECTION('',(-2.11176968422134E-16,0.951056516295154,-0.309016994374947)) ;
#69098 = DIRECTION('center_axis',(1.,2.22044604925031E-16,0.)) ;
#69099 = DIRECTION('ref_axis',(2.22044604925031E-16,-1.,0.)) ;
#69100 = DIRECTION('',(-1.,-2.22044604925031E-16,0.)) ;
#69101 = DIRECTION('center_axis',(-1.,-2.22044604925031E-16,0.)) ;
#69102 = DIRECTION('ref_axis',(1.97843191649031E-16,-0.891006524188369,0.453990499739545)) ;
#69103 = DIRECTION('center_axis',(1.30514544126042E-16,-0.587785252292473,
-0.809016994374948)) ;
#69104 = DIRECTION('ref_axis',(-1.79637858893621E-16,0.809016994374948,-0.587785252292473)) ;
#69105 = DIRECTION('',(1.,2.22044604925031E-16,0.)) ;
#69106 = DIRECTION('',(1.79637858893621E-16,-0.809016994374947,0.587785252292473)) ;
#69107 = DIRECTION('center_axis',(1.,2.22044604925031E-16,0.)) ;
#69108 = DIRECTION('ref_axis',(1.79637858893618E-16,-0.809016994374932,0.587785252292495)) ;
#69109 = DIRECTION('',(1.,2.22044604925031E-16,0.)) ;
#69110 = DIRECTION('center_axis',(-1.,-2.22044604925031E-16,0.)) ;
#69111 = DIRECTION('ref_axis',(1.79637858893621E-16,-0.809016994374947,0.587785252292474)) ;
#69112 = DIRECTION('center_axis',(-1.30514544126042E-16,0.587785252292473,
0.809016994374948)) ;
#69113 = DIRECTION('ref_axis',(1.79637858893621E-16,-0.809016994374948,0.587785252292473)) ;
#69114 = DIRECTION('',(1.,2.22044604925031E-16,0.)) ;
#69115 = DIRECTION('',(-1.79637858893621E-16,0.809016994374947,-0.587785252292473)) ;
#69116 = DIRECTION('center_axis',(1.,2.22044604925031E-16,0.)) ;
#69117 = DIRECTION('ref_axis',(2.22044604925031E-16,-1.,0.)) ;
#69118 = DIRECTION('',(-1.,-2.22044604925031E-16,0.)) ;
#69119 = DIRECTION('center_axis',(-1.,-2.22044604925031E-16,0.)) ;
#69120 = DIRECTION('ref_axis',(1.57009245868377E-16,-0.707106781186548,0.707106781186547)) ;
#69121 = DIRECTION('center_axis',(1.79637858893621E-16,-0.809016994374947,
-0.587785252292473)) ;
#69122 = DIRECTION('ref_axis',(-1.30514544126042E-16,0.587785252292473,-0.809016994374947)) ;
#69123 = DIRECTION('',(1.,2.22044604925031E-16,0.)) ;
#69124 = DIRECTION('',(1.30514544126042E-16,-0.587785252292473,0.809016994374947)) ;
#69125 = DIRECTION('center_axis',(1.,2.22044604925031E-16,0.)) ;
#69126 = DIRECTION('ref_axis',(1.30514544126042E-16,-0.587785252292474,0.809016994374947)) ;
#69127 = DIRECTION('',(1.,2.22044604925031E-16,0.)) ;
#69128 = DIRECTION('center_axis',(-1.,-2.22044604925031E-16,0.)) ;
#69129 = DIRECTION('ref_axis',(1.30514544126042E-16,-0.587785252292474,0.809016994374947)) ;
#69130 = DIRECTION('center_axis',(-1.79637858893621E-16,0.809016994374947,
0.587785252292473)) ;
#69131 = DIRECTION('ref_axis',(1.30514544126042E-16,-0.587785252292473,0.809016994374947)) ;
#69132 = DIRECTION('',(1.,2.22044604925031E-16,0.)) ;
#69133 = DIRECTION('',(-1.30514544126042E-16,0.587785252292473,-0.809016994374947)) ;
#69134 = DIRECTION('center_axis',(1.,2.22044604925031E-16,0.)) ;
#69135 = DIRECTION('ref_axis',(2.22044604925031E-16,-1.,0.)) ;
#69136 = DIRECTION('',(-1.,-2.22044604925031E-16,0.)) ;
#69137 = DIRECTION('center_axis',(-1.,-2.22044604925031E-16,0.)) ;
#69138 = DIRECTION('ref_axis',(1.00806141154385E-16,-0.453990499739546,0.891006524188368)) ;
#69139 = DIRECTION('center_axis',(-1.,-2.22044604925031E-16,0.)) ;
#69140 = DIRECTION('ref_axis',(2.22044604925031E-16,-1.,0.)) ;
#69141 = DIRECTION('center_axis',(1.,2.22044604925031E-16,0.)) ;
#69142 = DIRECTION('ref_axis',(9.02179155423715E-17,-0.406305370818768,0.913737350469939)) ;
#69143 = DIRECTION('center_axis',(-1.,-2.22044604925031E-16,0.)) ;
#69144 = DIRECTION('ref_axis',(2.22044604925031E-16,-1.,0.)) ;
#69145 = DIRECTION('center_axis',(1.,2.22044604925031E-16,0.)) ;
#69146 = DIRECTION('ref_axis',(9.02179155423715E-17,-0.406305370818768,0.913737350469939)) ;
#69147 = DIRECTION('center_axis',(-1.,-2.22044604925031E-16,0.)) ;
#69148 = DIRECTION('ref_axis',(2.22044604925031E-16,-1.,0.)) ;
#69149 = DIRECTION('center_axis',(1.,2.22044604925031E-16,0.)) ;
#69150 = DIRECTION('ref_axis',(9.02179155423715E-17,-0.406305370818768,0.913737350469939)) ;
#69151 = DIRECTION('center_axis',(-1.,-2.22044604925031E-16,0.)) ;
#69152 = DIRECTION('ref_axis',(2.22044604925031E-16,-1.,0.)) ;
#69153 = DIRECTION('center_axis',(1.,2.22044604925031E-16,0.)) ;
#69154 = DIRECTION('ref_axis',(9.02179155423715E-17,-0.406305370818768,0.913737350469939)) ;
#69155 = DIRECTION('center_axis',(-1.,-2.22044604925031E-16,0.)) ;
#69156 = DIRECTION('ref_axis',(2.22044604925031E-16,-1.,0.)) ;
#69157 = DIRECTION('center_axis',(1.,2.22044604925031E-16,0.)) ;
#69158 = DIRECTION('ref_axis',(9.02179155423715E-17,-0.406305370818768,0.913737350469939)) ;
#69159 = DIRECTION('center_axis',(-1.,-2.22044604925031E-16,0.)) ;
#69160 = DIRECTION('ref_axis',(2.22044604925031E-16,-1.,0.)) ;
#69161 = DIRECTION('center_axis',(1.,2.22044604925031E-16,0.)) ;
#69162 = DIRECTION('ref_axis',(9.02179155423715E-17,-0.406305370818768,0.913737350469939)) ;
#69163 = DIRECTION('center_axis',(-1.,-2.22044604925031E-16,0.)) ;
#69164 = DIRECTION('ref_axis',(2.22044604925031E-16,-1.,0.)) ;
#69165 = DIRECTION('center_axis',(1.,2.22044604925031E-16,0.)) ;
#69166 = DIRECTION('ref_axis',(9.02179155423715E-17,-0.406305370818768,0.913737350469939)) ;
#69167 = DIRECTION('center_axis',(-1.,-2.22044604925031E-16,0.)) ;
#69168 = DIRECTION('ref_axis',(2.22044604925031E-16,-1.,0.)) ;
#69169 = DIRECTION('center_axis',(1.,2.22044604925031E-16,0.)) ;
#69170 = DIRECTION('ref_axis',(9.02179155423715E-17,-0.406305370818768,0.913737350469939)) ;
#69171 = DIRECTION('center_axis',(-1.,-2.22044604925031E-16,0.)) ;
#69172 = DIRECTION('ref_axis',(2.22044604925031E-16,-1.,0.)) ;
#69173 = DIRECTION('center_axis',(1.,2.22044604925031E-16,0.)) ;
#69174 = DIRECTION('ref_axis',(9.02179155423715E-17,-0.406305370818768,0.913737350469939)) ;
#69175 = DIRECTION('center_axis',(-1.,-2.22044604925031E-16,0.)) ;
#69176 = DIRECTION('ref_axis',(2.22044604925031E-16,-1.,0.)) ;
#69177 = DIRECTION('center_axis',(1.,2.22044604925031E-16,0.)) ;
#69178 = DIRECTION('ref_axis',(9.02179155423715E-17,-0.406305370818768,0.913737350469939)) ;
#69179 = DIRECTION('center_axis',(-1.,-2.22044604925031E-16,0.)) ;
#69180 = DIRECTION('ref_axis',(2.22044604925031E-16,-1.,0.)) ;
#69181 = DIRECTION('center_axis',(1.,2.22044604925031E-16,0.)) ;
#69182 = DIRECTION('ref_axis',(9.02179155423715E-17,-0.406305370818768,0.913737350469939)) ;
#69183 = DIRECTION('center_axis',(-1.,-2.22044604925031E-16,0.)) ;
#69184 = DIRECTION('ref_axis',(2.22044604925031E-16,-1.,0.)) ;
#69185 = DIRECTION('center_axis',(1.,2.22044604925031E-16,0.)) ;
#69186 = DIRECTION('ref_axis',(9.02179155423715E-17,-0.406305370818768,0.913737350469939)) ;
#69187 = DIRECTION('center_axis',(-1.,-2.22044604925031E-16,0.)) ;
#69188 = DIRECTION('ref_axis',(2.22044604925031E-16,-1.,0.)) ;
#69189 = DIRECTION('center_axis',(1.,2.22044604925031E-16,0.)) ;
#69190 = DIRECTION('ref_axis',(9.02179155423715E-17,-0.406305370818768,0.913737350469939)) ;
#69191 = DIRECTION('center_axis',(-1.,-2.22044604925031E-16,0.)) ;
#69192 = DIRECTION('ref_axis',(2.22044604925031E-16,-1.,0.)) ;
#69193 = DIRECTION('center_axis',(1.,2.22044604925031E-16,0.)) ;
#69194 = DIRECTION('ref_axis',(9.02179155423715E-17,-0.406305370818768,0.913737350469939)) ;
#69195 = DIRECTION('center_axis',(-1.,-2.22044604925031E-16,0.)) ;
#69196 = DIRECTION('ref_axis',(2.22044604925031E-16,-1.,0.)) ;
#69197 = DIRECTION('center_axis',(1.,2.22044604925031E-16,0.)) ;
#69198 = DIRECTION('ref_axis',(9.02179155423715E-17,-0.406305370818768,0.913737350469939)) ;
#69199 = DIRECTION('center_axis',(-1.,-2.22044604925031E-16,0.)) ;
#69200 = DIRECTION('ref_axis',(2.22044604925031E-16,-1.,0.)) ;
#69201 = DIRECTION('center_axis',(1.,2.22044604925031E-16,0.)) ;
#69202 = DIRECTION('ref_axis',(9.02179155423715E-17,-0.406305370818768,0.913737350469939)) ;
#69203 = DIRECTION('center_axis',(-1.,-2.22044604925031E-16,0.)) ;
#69204 = DIRECTION('ref_axis',(2.22044604925031E-16,-1.,0.)) ;
#69205 = DIRECTION('center_axis',(1.,2.22044604925031E-16,0.)) ;
#69206 = DIRECTION('ref_axis',(9.02179155423715E-17,-0.406305370818768,0.913737350469939)) ;
#69207 = DIRECTION('center_axis',(-1.,-2.22044604925031E-16,0.)) ;
#69208 = DIRECTION('ref_axis',(2.22044604925031E-16,-1.,0.)) ;
#69209 = DIRECTION('center_axis',(1.,2.22044604925031E-16,0.)) ;
#69210 = DIRECTION('ref_axis',(9.02179155423715E-17,-0.406305370818768,0.913737350469939)) ;
#69211 = DIRECTION('center_axis',(-1.,-2.22044604925031E-16,0.)) ;
#69212 = DIRECTION('ref_axis',(2.22044604925031E-16,-1.,0.)) ;
#69213 = DIRECTION('center_axis',(1.,2.22044604925031E-16,0.)) ;
#69214 = DIRECTION('ref_axis',(9.02179155423715E-17,-0.406305370818768,0.913737350469939)) ;
#69215 = DIRECTION('center_axis',(1.,2.22044604925031E-16,0.)) ;
#69216 = DIRECTION('ref_axis',(9.02179155423715E-17,-0.406305370818768,0.913737350469939)) ;
#69217 = DIRECTION('center_axis',(1.,2.22044604925031E-16,0.)) ;
#69218 = DIRECTION('ref_axis',(0.,0.,-1.)) ;
#69219 = DIRECTION('center_axis',(-2.22044604925031E-16,1.,0.)) ;
#69220 = DIRECTION('ref_axis',(0.,0.,1.)) ;
#69221 = DIRECTION('center_axis',(1.,2.22044604925031E-16,0.)) ;
#69222 = DIRECTION('ref_axis',(9.02179155423715E-17,-0.406305370818768,0.913737350469939)) ;
#69223 = DIRECTION('center_axis',(-1.,-2.22044604925031E-16,0.)) ;
#69224 = DIRECTION('ref_axis',(2.22044604925031E-16,-1.,0.)) ;
#69225 = DIRECTION('center_axis',(-1.,-2.22044604925031E-16,0.)) ;
#69226 = DIRECTION('ref_axis',(0.,0.,1.)) ;
#69227 = DIRECTION('center_axis',(-2.22044604925031E-16,1.,0.)) ;
#69228 = DIRECTION('ref_axis',(0.,0.,-1.)) ;
#69229 = DIRECTION('center_axis',(-1.,-2.22044604925031E-16,0.)) ;
#69230 = DIRECTION('ref_axis',(4.62681868766601E-17,-0.208373389176835,0.978049349819813)) ;
#69231 = DIRECTION('center_axis',(1.,2.22044604925031E-16,0.)) ;
#69232 = DIRECTION('ref_axis',(3.47354289865164E-17,-0.15643446504023,-0.987688340595138)) ;
#69233 = DIRECTION('center_axis',(-1.,-2.22044604925031E-16,0.)) ;
#69234 = DIRECTION('ref_axis',(4.62681868766601E-17,-0.208373389176835,0.978049349819813)) ;
#69235 = DIRECTION('center_axis',(1.,2.22044604925031E-16,0.)) ;
#69236 = DIRECTION('ref_axis',(1.00806141154385E-16,-0.453990499739546,-0.891006524188368)) ;
#69237 = DIRECTION('center_axis',(-1.,-2.22044604925031E-16,0.)) ;
#69238 = DIRECTION('ref_axis',(4.62681868766601E-17,-0.208373389176835,0.978049349819813)) ;
#69239 = DIRECTION('center_axis',(1.,2.22044604925031E-16,0.)) ;
#69240 = DIRECTION('ref_axis',(1.57009245868377E-16,-0.707106781186547,-0.707106781186548)) ;
#69241 = DIRECTION('center_axis',(-1.,-2.22044604925031E-16,0.)) ;
#69242 = DIRECTION('ref_axis',(4.62681868766601E-17,-0.208373389176835,0.978049349819813)) ;
#69243 = DIRECTION('center_axis',(1.,2.22044604925031E-16,0.)) ;
#69244 = DIRECTION('ref_axis',(1.97843191649031E-16,-0.891006524188368,-0.453990499739547)) ;
#69245 = DIRECTION('center_axis',(-1.,-2.22044604925031E-16,0.)) ;
#69246 = DIRECTION('ref_axis',(4.62681868766601E-17,-0.208373389176835,0.978049349819813)) ;
#69247 = DIRECTION('center_axis',(1.,2.22044604925031E-16,0.)) ;
#69248 = DIRECTION('ref_axis',(2.19310867376507E-16,-0.987688340595138,-0.156434465040231)) ;
#69249 = DIRECTION('center_axis',(-1.,-2.22044604925031E-16,0.)) ;
#69250 = DIRECTION('ref_axis',(4.62681868766601E-17,-0.208373389176835,0.978049349819813)) ;
#69251 = DIRECTION('center_axis',(1.,2.22044604925031E-16,0.)) ;
#69252 = DIRECTION('ref_axis',(2.19310867376507E-16,-0.987688340595138,0.156434465040229)) ;
#69253 = DIRECTION('center_axis',(-1.,-2.22044604925031E-16,0.)) ;
#69254 = DIRECTION('ref_axis',(4.62681868766601E-17,-0.208373389176835,0.978049349819813)) ;
#69255 = DIRECTION('center_axis',(1.,2.22044604925031E-16,0.)) ;
#69256 = DIRECTION('ref_axis',(1.97843191649031E-16,-0.891006524188369,0.453990499739545)) ;
#69257 = DIRECTION('center_axis',(-1.,-2.22044604925031E-16,0.)) ;
#69258 = DIRECTION('ref_axis',(4.62681868766601E-17,-0.208373389176835,0.978049349819813)) ;
#69259 = DIRECTION('center_axis',(1.,2.22044604925031E-16,0.)) ;
#69260 = DIRECTION('ref_axis',(1.57009245868377E-16,-0.707106781186548,0.707106781186547)) ;
#69261 = DIRECTION('center_axis',(-1.,-2.22044604925031E-16,0.)) ;
#69262 = DIRECTION('ref_axis',(4.62681868766601E-17,-0.208373389176835,0.978049349819813)) ;
#69263 = DIRECTION('center_axis',(1.,2.22044604925031E-16,0.)) ;
#69264 = DIRECTION('ref_axis',(1.00806141154385E-16,-0.453990499739546,0.891006524188368)) ;
#69265 = DIRECTION('center_axis',(-1.,-2.22044604925031E-16,0.)) ;
#69266 = DIRECTION('ref_axis',(4.62681868766601E-17,-0.208373389176835,0.978049349819813)) ;
#69267 = DIRECTION('center_axis',(1.,2.22044604925031E-16,0.)) ;
#69268 = DIRECTION('ref_axis',(3.47354289865169E-17,-0.156434465040232,0.987688340595138)) ;
#69269 = DIRECTION('center_axis',(-1.,-2.22044604925031E-16,0.)) ;
#69270 = DIRECTION('ref_axis',(4.62681868766601E-17,-0.208373389176835,0.978049349819813)) ;
#69271 = DIRECTION('center_axis',(1.,2.22044604925031E-16,0.)) ;
#69272 = DIRECTION('ref_axis',(-3.47354289865171E-17,0.156434465040233,0.987688340595137)) ;
#69273 = DIRECTION('center_axis',(-1.,-2.22044604925031E-16,0.)) ;
#69274 = DIRECTION('ref_axis',(4.62681868766601E-17,-0.208373389176835,0.978049349819813)) ;
#69275 = DIRECTION('center_axis',(1.,2.22044604925031E-16,0.)) ;
#69276 = DIRECTION('ref_axis',(-1.00806141154386E-16,0.453990499739549,0.891006524188367)) ;
#69277 = DIRECTION('center_axis',(-1.,-2.22044604925031E-16,0.)) ;
#69278 = DIRECTION('ref_axis',(4.62681868766601E-17,-0.208373389176835,0.978049349819813)) ;
#69279 = DIRECTION('center_axis',(1.,2.22044604925031E-16,0.)) ;
#69280 = DIRECTION('ref_axis',(-1.57009245868377E-16,0.707106781186548,0.707106781186547)) ;
#69281 = DIRECTION('center_axis',(-1.,-2.22044604925031E-16,0.)) ;
#69282 = DIRECTION('ref_axis',(4.62681868766601E-17,-0.208373389176835,0.978049349819813)) ;
#69283 = DIRECTION('center_axis',(1.,2.22044604925031E-16,0.)) ;
#69284 = DIRECTION('ref_axis',(-1.97843191649031E-16,0.891006524188368,0.453990499739546)) ;
#69285 = DIRECTION('center_axis',(-1.,-2.22044604925031E-16,0.)) ;
#69286 = DIRECTION('ref_axis',(4.62681868766601E-17,-0.208373389176835,0.978049349819813)) ;
#69287 = DIRECTION('center_axis',(1.,2.22044604925031E-16,0.)) ;
#69288 = DIRECTION('ref_axis',(-2.19310867376507E-16,0.987688340595138,0.156434465040232)) ;
#69289 = DIRECTION('center_axis',(-1.,-2.22044604925031E-16,0.)) ;
#69290 = DIRECTION('ref_axis',(4.62681868766601E-17,-0.208373389176835,0.978049349819813)) ;
#69291 = DIRECTION('center_axis',(1.,2.22044604925031E-16,0.)) ;
#69292 = DIRECTION('ref_axis',(-2.19310867376507E-16,0.987688340595138,-0.156434465040228)) ;
#69293 = DIRECTION('center_axis',(-1.,-2.22044604925031E-16,0.)) ;
#69294 = DIRECTION('ref_axis',(4.62681868766601E-17,-0.208373389176835,0.978049349819813)) ;
#69295 = DIRECTION('center_axis',(1.,2.22044604925031E-16,0.)) ;
#69296 = DIRECTION('ref_axis',(-1.97843191649031E-16,0.891006524188368,-0.453990499739547)) ;
#69297 = DIRECTION('center_axis',(-1.,-2.22044604925031E-16,0.)) ;
#69298 = DIRECTION('ref_axis',(4.62681868766601E-17,-0.208373389176835,0.978049349819813)) ;
#69299 = DIRECTION('center_axis',(1.,2.22044604925031E-16,0.)) ;
#69300 = DIRECTION('ref_axis',(-1.57009245868377E-16,0.707106781186547,-0.707106781186547)) ;
#69301 = DIRECTION('center_axis',(-1.,-2.22044604925031E-16,0.)) ;
#69302 = DIRECTION('ref_axis',(4.62681868766601E-17,-0.208373389176835,0.978049349819813)) ;
#69303 = DIRECTION('center_axis',(1.,2.22044604925031E-16,0.)) ;
#69304 = DIRECTION('ref_axis',(-1.00806141154385E-16,0.453990499739547,-0.891006524188368)) ;
#69305 = DIRECTION('center_axis',(-1.,-2.22044604925031E-16,0.)) ;
#69306 = DIRECTION('ref_axis',(4.62681868766601E-17,-0.208373389176835,0.978049349819813)) ;
#69307 = DIRECTION('center_axis',(1.,2.22044604925031E-16,0.)) ;
#69308 = DIRECTION('ref_axis',(-3.47354289865169E-17,0.156434465040232,-0.987688340595138)) ;
#69309 = DIRECTION('center_axis',(-1.,-2.22044604925031E-16,0.)) ;
#69310 = DIRECTION('ref_axis',(4.62681868766601E-17,-0.208373389176835,0.978049349819813)) ;
#69311 = DIRECTION('center_axis',(-1.,-2.22044604925031E-16,0.)) ;
#69312 = DIRECTION('ref_axis',(2.22044604925031E-16,-1.,0.)) ;
#69313 = DIRECTION('',(6.86155564311059E-17,-0.309016994374948,0.951056516295153)) ;
#69314 = DIRECTION('center_axis',(1.,2.22044604925031E-16,0.)) ;
#69315 = DIRECTION('ref_axis',(-6.86155564311052E-17,0.309016994374945,-0.951056516295154)) ;
#69316 = DIRECTION('',(-6.86155564311059E-17,0.309016994374948,-0.951056516295153)) ;
#69317 = DIRECTION('center_axis',(-1.,-2.22044604925031E-16,0.)) ;
#69318 = DIRECTION('ref_axis',(2.22044604925031E-16,-1.,0.)) ;
#69319 = DIRECTION('',(1.30514544126042E-16,-0.587785252292473,0.809016994374947)) ;
#69320 = DIRECTION('center_axis',(1.,2.22044604925031E-16,0.)) ;
#69321 = DIRECTION('ref_axis',(-1.30514544126041E-16,0.587785252292468,-0.809016994374951)) ;
#69322 = DIRECTION('',(-1.30514544126042E-16,0.587785252292473,-0.809016994374947)) ;
#69323 = DIRECTION('center_axis',(-1.,-2.22044604925031E-16,0.)) ;
#69324 = DIRECTION('ref_axis',(2.22044604925031E-16,-1.,0.)) ;
#69325 = DIRECTION('',(1.79637858893621E-16,-0.809016994374948,0.587785252292473)) ;
#69326 = DIRECTION('center_axis',(1.,2.22044604925031E-16,0.)) ;
#69327 = DIRECTION('ref_axis',(-1.79637858893621E-16,0.809016994374947,-0.587785252292474)) ;
#69328 = DIRECTION('',(-1.79637858893621E-16,0.809016994374948,-0.587785252292473)) ;
#69329 = DIRECTION('center_axis',(-1.,-2.22044604925031E-16,0.)) ;
#69330 = DIRECTION('ref_axis',(2.22044604925031E-16,-1.,0.)) ;
#69331 = DIRECTION('',(2.11176968422134E-16,-0.951056516295154,0.309016994374947)) ;
#69332 = DIRECTION('center_axis',(1.,2.22044604925031E-16,0.)) ;
#69333 = DIRECTION('ref_axis',(-2.11176968422134E-16,0.951056516295153,-0.309016994374948)) ;
#69334 = DIRECTION('',(-2.11176968422134E-16,0.951056516295154,-0.309016994374947)) ;
#69335 = DIRECTION('center_axis',(-1.,-2.22044604925031E-16,0.)) ;
#69336 = DIRECTION('ref_axis',(2.22044604925031E-16,-1.,0.)) ;
#69337 = DIRECTION('',(2.22044604925031E-16,-1.,-2.22044604925031E-16)) ;
#69338 = DIRECTION('center_axis',(1.,2.22044604925031E-16,0.)) ;
#69339 = DIRECTION('ref_axis',(-2.22044604925031E-16,1.,0.)) ;
#69340 = DIRECTION('',(-2.22044604925031E-16,1.,2.22044604925031E-16)) ;
#69341 = DIRECTION('center_axis',(-1.,-2.22044604925031E-16,0.)) ;
#69342 = DIRECTION('ref_axis',(2.22044604925031E-16,-1.,0.)) ;
#69343 = DIRECTION('',(2.11176968422134E-16,-0.951056516295153,-0.309016994374948)) ;
#69344 = DIRECTION('center_axis',(1.,2.22044604925031E-16,0.)) ;
#69345 = DIRECTION('ref_axis',(-2.11176968422134E-16,0.951056516295153,0.309016994374948)) ;
#69346 = DIRECTION('',(-2.11176968422134E-16,0.951056516295153,0.309016994374948)) ;
#69347 = DIRECTION('center_axis',(-1.,-2.22044604925031E-16,0.)) ;
#69348 = DIRECTION('ref_axis',(2.22044604925031E-16,-1.,0.)) ;
#69349 = DIRECTION('',(1.79637858893621E-16,-0.809016994374947,-0.587785252292473)) ;
#69350 = DIRECTION('center_axis',(1.,2.22044604925031E-16,0.)) ;
#69351 = DIRECTION('ref_axis',(-1.79637858893621E-16,0.809016994374947,0.587785252292474)) ;
#69352 = DIRECTION('',(-1.79637858893621E-16,0.809016994374947,0.587785252292473)) ;
#69353 = DIRECTION('center_axis',(-1.,-2.22044604925031E-16,0.)) ;
#69354 = DIRECTION('ref_axis',(2.22044604925031E-16,-1.,0.)) ;
#69355 = DIRECTION('',(1.30514544126042E-16,-0.587785252292473,-0.809016994374947)) ;
#69356 = DIRECTION('center_axis',(1.,2.22044604925031E-16,0.)) ;
#69357 = DIRECTION('ref_axis',(-1.30514544126041E-16,0.587785252292468,0.809016994374951)) ;
#69358 = DIRECTION('',(-1.30514544126042E-16,0.587785252292473,0.809016994374947)) ;
#69359 = DIRECTION('center_axis',(-1.,-2.22044604925031E-16,0.)) ;
#69360 = DIRECTION('ref_axis',(2.22044604925031E-16,-1.,0.)) ;
#69361 = DIRECTION('',(6.86155564311058E-17,-0.309016994374947,-0.951056516295154)) ;
#69362 = DIRECTION('center_axis',(1.,2.22044604925031E-16,0.)) ;
#69363 = DIRECTION('ref_axis',(-6.86155564311052E-17,0.309016994374945,0.951056516295154)) ;
#69364 = DIRECTION('',(-6.86155564311058E-17,0.309016994374947,0.951056516295154)) ;
#69365 = DIRECTION('center_axis',(-1.,-2.22044604925031E-16,0.)) ;
#69366 = DIRECTION('ref_axis',(2.22044604925031E-16,-1.,0.)) ;
#69367 = DIRECTION('',(-2.46519032881566E-32,1.11022302462516E-16,-1.)) ;
#69368 = DIRECTION('center_axis',(1.,2.22044604925031E-16,0.)) ;
#69369 = DIRECTION('ref_axis',(0.,0.,1.)) ;
#69370 = DIRECTION('',(2.46519032881566E-32,-1.11022302462516E-16,1.)) ;
#69371 = DIRECTION('center_axis',(-1.,-2.22044604925031E-16,0.)) ;
#69372 = DIRECTION('ref_axis',(2.22044604925031E-16,-1.,0.)) ;
#69373 = DIRECTION('',(-6.86155564311058E-17,0.309016994374948,-0.951056516295154)) ;
#69374 = DIRECTION('center_axis',(1.,2.22044604925031E-16,0.)) ;
#69375 = DIRECTION('ref_axis',(6.86155564311052E-17,-0.309016994374945,0.951056516295154)) ;
#69376 = DIRECTION('',(6.86155564311058E-17,-0.309016994374948,0.951056516295154)) ;
#69377 = DIRECTION('center_axis',(-1.,-2.22044604925031E-16,0.)) ;
#69378 = DIRECTION('ref_axis',(2.22044604925031E-16,-1.,0.)) ;
#69379 = DIRECTION('',(-1.30514544126042E-16,0.587785252292473,-0.809016994374947)) ;
#69380 = DIRECTION('center_axis',(1.,2.22044604925031E-16,0.)) ;
#69381 = DIRECTION('ref_axis',(1.30514544126042E-16,-0.587785252292474,0.809016994374947)) ;
#69382 = DIRECTION('',(1.30514544126042E-16,-0.587785252292473,0.809016994374947)) ;
#69383 = DIRECTION('center_axis',(-1.,-2.22044604925031E-16,0.)) ;
#69384 = DIRECTION('ref_axis',(2.22044604925031E-16,-1.,0.)) ;
#69385 = DIRECTION('',(-1.79637858893621E-16,0.809016994374947,-0.587785252292473)) ;
#69386 = DIRECTION('center_axis',(1.,2.22044604925031E-16,0.)) ;
#69387 = DIRECTION('ref_axis',(1.79637858893621E-16,-0.809016994374947,0.587785252292474)) ;
#69388 = DIRECTION('',(1.79637858893621E-16,-0.809016994374947,0.587785252292473)) ;
#69389 = DIRECTION('center_axis',(-1.,-2.22044604925031E-16,0.)) ;
#69390 = DIRECTION('ref_axis',(2.22044604925031E-16,-1.,0.)) ;
#69391 = DIRECTION('',(-2.11176968422134E-16,0.951056516295154,-0.309016994374947)) ;
#69392 = DIRECTION('center_axis',(1.,2.22044604925031E-16,0.)) ;
#69393 = DIRECTION('ref_axis',(2.11176968422134E-16,-0.951056516295154,0.309016994374945)) ;
#69394 = DIRECTION('',(2.11176968422134E-16,-0.951056516295154,0.309016994374947)) ;
#69395 = DIRECTION('center_axis',(-1.,-2.22044604925031E-16,0.)) ;
#69396 = DIRECTION('ref_axis',(2.22044604925031E-16,-1.,0.)) ;
#69397 = DIRECTION('',(-2.22044604925031E-16,1.,5.55111512312578E-17)) ;
#69398 = DIRECTION('center_axis',(1.,2.22044604925031E-16,0.)) ;
#69399 = DIRECTION('ref_axis',(2.22044604925031E-16,-1.,0.)) ;
#69400 = DIRECTION('',(2.22044604925031E-16,-1.,-5.55111512312578E-17)) ;
#69401 = DIRECTION('center_axis',(-1.,-2.22044604925031E-16,0.)) ;
#69402 = DIRECTION('ref_axis',(2.22044604925031E-16,-1.,0.)) ;
#69403 = DIRECTION('',(-2.11176968422134E-16,0.951056516295154,0.309016994374948)) ;
#69404 = DIRECTION('center_axis',(1.,2.22044604925031E-16,0.)) ;
#69405 = DIRECTION('ref_axis',(2.11176968422134E-16,-0.951056516295154,-0.309016994374945)) ;
#69406 = DIRECTION('',(2.11176968422134E-16,-0.951056516295154,-0.309016994374948)) ;
#69407 = DIRECTION('center_axis',(-1.,-2.22044604925031E-16,0.)) ;
#69408 = DIRECTION('ref_axis',(2.22044604925031E-16,-1.,0.)) ;
#69409 = DIRECTION('',(-1.79637858893621E-16,0.809016994374947,0.587785252292473)) ;
#69410 = DIRECTION('center_axis',(1.,2.22044604925031E-16,0.)) ;
#69411 = DIRECTION('ref_axis',(1.79637858893621E-16,-0.809016994374947,-0.587785252292474)) ;
#69412 = DIRECTION('',(1.79637858893621E-16,-0.809016994374947,-0.587785252292473)) ;
#69413 = DIRECTION('center_axis',(-1.,-2.22044604925031E-16,0.)) ;
#69414 = DIRECTION('ref_axis',(2.22044604925031E-16,-1.,0.)) ;
#69415 = DIRECTION('',(-1.30514544126042E-16,0.587785252292473,0.809016994374947)) ;
#69416 = DIRECTION('center_axis',(1.,2.22044604925031E-16,0.)) ;
#69417 = DIRECTION('ref_axis',(1.30514544126042E-16,-0.587785252292474,-0.809016994374947)) ;
#69418 = DIRECTION('',(1.30514544126042E-16,-0.587785252292473,-0.809016994374947)) ;
#69419 = DIRECTION('center_axis',(-1.,-2.22044604925031E-16,0.)) ;
#69420 = DIRECTION('ref_axis',(2.22044604925031E-16,-1.,0.)) ;
#69421 = DIRECTION('',(-6.86155564311058E-17,0.309016994374947,0.951056516295154)) ;
#69422 = DIRECTION('center_axis',(1.,2.22044604925031E-16,0.)) ;
#69423 = DIRECTION('ref_axis',(6.86155564311052E-17,-0.309016994374945,-0.951056516295154)) ;
#69424 = DIRECTION('',(6.86155564311058E-17,-0.309016994374947,-0.951056516295154)) ;
#69425 = DIRECTION('center_axis',(-1.,-2.22044604925031E-16,0.)) ;
#69426 = DIRECTION('ref_axis',(2.22044604925031E-16,-1.,0.)) ;
#69427 = DIRECTION('',(0.,0.,1.)) ;
#69428 = DIRECTION('center_axis',(1.,2.22044604925031E-16,0.)) ;
#69429 = DIRECTION('ref_axis',(0.,0.,-1.)) ;
#69430 = DIRECTION('',(0.,0.,-1.)) ;
#69431 = DIRECTION('center_axis',(-1.,-2.22044604925031E-16,0.)) ;
#69432 = DIRECTION('ref_axis',(0.,0.,1.)) ;
#69433 = DIRECTION('center_axis',(-1.,-2.22044604925031E-16,0.)) ;
#69434 = DIRECTION('ref_axis',(3.47354289865169E-17,-0.156434465040232,0.987688340595138)) ;
#69435 = DIRECTION('center_axis',(-6.86155564311058E-17,0.309016994374948,
-0.951056516295154)) ;
#69436 = DIRECTION('ref_axis',(-0.707106781186557,0.672498511963948,0.218508012224408)) ;
#69437 = DIRECTION('',(-6.86155564311058E-17,0.309016994374948,-0.951056516295154)) ;
#69438 = DIRECTION('center_axis',(-2.46519032881566E-32,1.11022302462516E-16,
-1.)) ;
#69439 = DIRECTION('ref_axis',(-0.707106781186547,-0.707106781186548,-7.8504622934189E-17)) ;
#69440 = DIRECTION('',(2.46519032881566E-32,-1.11022302462516E-16,1.)) ;
#69441 = DIRECTION('center_axis',(-6.86155564311058E-17,0.309016994374948,
-0.951056516295154)) ;
#69442 = DIRECTION('ref_axis',(-0.707106781186557,-0.672498511963948,-0.218508012224408)) ;
#69443 = DIRECTION('',(6.86155564311058E-17,-0.309016994374948,0.951056516295154)) ;
#69444 = DIRECTION('center_axis',(-1.,-2.22044604925031E-16,0.)) ;
#69445 = DIRECTION('ref_axis',(0.,0.,1.)) ;
#69446 = DIRECTION('center_axis',(-1.30514544126042E-16,0.587785252292473,
-0.809016994374947)) ;
#69447 = DIRECTION('ref_axis',(-0.707106781186563,0.572061402817672,0.415626937777444)) ;
#69448 = DIRECTION('center_axis',(6.86155564311058E-17,-0.309016994374947,
-0.951056516295154)) ;
#69449 = DIRECTION('ref_axis',(-0.707106781186557,-0.672498511963948,0.218508012224407)) ;
#69450 = DIRECTION('',(-6.86155564311058E-17,0.309016994374947,0.951056516295154)) ;
#69451 = DIRECTION('center_axis',(-1.30514544126042E-16,0.587785252292473,
-0.809016994374947)) ;
#69452 = DIRECTION('ref_axis',(-0.707106781186551,-0.572061402817681,-0.415626937777451)) ;
#69453 = DIRECTION('center_axis',(-1.,-2.22044604925031E-16,0.)) ;
#69454 = DIRECTION('ref_axis',(0.,0.,1.)) ;
#69455 = DIRECTION('center_axis',(-1.79637858893621E-16,0.809016994374948,
-0.587785252292473)) ;
#69456 = DIRECTION('ref_axis',(-0.707106781186563,0.415626937777444,0.572061402817672)) ;
#69457 = DIRECTION('center_axis',(1.30514544126042E-16,-0.587785252292473,
-0.809016994374948)) ;
#69458 = DIRECTION('ref_axis',(-0.707106781186534,-0.572061402817695,0.415626937777461)) ;
#69459 = DIRECTION('',(-1.30514544126042E-16,0.587785252292473,0.809016994374947)) ;
#69460 = DIRECTION('center_axis',(-1.79637858893621E-16,0.809016994374948,
-0.587785252292473)) ;
#69461 = DIRECTION('ref_axis',(-0.707106781186563,-0.415626937777444,-0.572061402817672)) ;
#69462 = DIRECTION('center_axis',(-1.,-2.22044604925031E-16,0.)) ;
#69463 = DIRECTION('ref_axis',(0.,0.,1.)) ;
#69464 = DIRECTION('center_axis',(-2.11176968422134E-16,0.951056516295154,
-0.309016994374947)) ;
#69465 = DIRECTION('ref_axis',(-0.707106781186557,0.218508012224407,0.672498511963949)) ;
#69466 = DIRECTION('center_axis',(1.79637858893621E-16,-0.809016994374947,
-0.587785252292473)) ;
#69467 = DIRECTION('ref_axis',(-0.707106781186551,-0.415626937777452,0.572061402817682)) ;
#69468 = DIRECTION('',(-1.79637858893621E-16,0.809016994374947,0.587785252292473)) ;
#69469 = DIRECTION('center_axis',(-2.11176968422134E-16,0.951056516295154,
-0.309016994374947)) ;
#69470 = DIRECTION('ref_axis',(-0.707106781186557,-0.218508012224407,-0.672498511963948)) ;
#69471 = DIRECTION('center_axis',(-1.,-2.22044604925031E-16,0.)) ;
#69472 = DIRECTION('ref_axis',(0.,0.,1.)) ;
#69473 = DIRECTION('center_axis',(-2.22044604925031E-16,1.,5.55111512312578E-17)) ;
#69474 = DIRECTION('ref_axis',(-0.707106781186568,-1.96261557335475E-16,0.707106781186527)) ;
#69475 = DIRECTION('center_axis',(2.11176968422134E-16,-0.951056516295154,
-0.309016994374948)) ;
#69476 = DIRECTION('ref_axis',(-0.707106781186583,-0.2185080122244,0.672498511963923)) ;
#69477 = DIRECTION('',(-2.11176968422134E-16,0.951056516295153,0.309016994374948)) ;
#69478 = DIRECTION('center_axis',(-2.22044604925031E-16,1.,5.55111512312578E-17)) ;
#69479 = DIRECTION('ref_axis',(-0.707106781186568,-1.17756934401289E-16,-0.707106781186527)) ;
#69480 = DIRECTION('center_axis',(-1.,-2.22044604925031E-16,0.)) ;
#69481 = DIRECTION('ref_axis',(0.,0.,1.)) ;
#69482 = DIRECTION('center_axis',(-2.11176968422134E-16,0.951056516295154,
0.309016994374948)) ;
#69483 = DIRECTION('ref_axis',(-0.707106781186557,-0.218508012224408,0.672498511963948)) ;
#69484 = DIRECTION('center_axis',(2.22044604925031E-16,-1.,-2.22044604925031E-16)) ;
#69485 = DIRECTION('ref_axis',(-0.707106781186568,-3.14018491736755E-16,0.707106781186527)) ;
#69486 = DIRECTION('',(-2.22044604925031E-16,1.,2.22044604925031E-16)) ;
#69487 = DIRECTION('center_axis',(-2.11176968422134E-16,0.951056516295154,
0.309016994374948)) ;
#69488 = DIRECTION('ref_axis',(-0.707106781186557,0.218508012224408,-0.672498511963948)) ;
#69489 = DIRECTION('center_axis',(-1.,-2.22044604925031E-16,0.)) ;
#69490 = DIRECTION('ref_axis',(0.,0.,1.)) ;
#69491 = DIRECTION('center_axis',(-1.79637858893621E-16,0.809016994374947,
0.587785252292473)) ;
#69492 = DIRECTION('ref_axis',(-0.707106781186563,-0.415626937777444,0.572061402817672)) ;
#69493 = DIRECTION('center_axis',(2.11176968422134E-16,-0.951056516295154,
0.309016994374947)) ;
#69494 = DIRECTION('ref_axis',(-0.707106781186563,0.218508012224405,0.672498511963943)) ;
#69495 = DIRECTION('',(-2.11176968422134E-16,0.951056516295154,-0.309016994374947)) ;
#69496 = DIRECTION('center_axis',(-1.79637858893621E-16,0.809016994374947,
0.587785252292473)) ;
#69497 = DIRECTION('ref_axis',(-0.707106781186568,0.415626937777441,-0.572061402817668)) ;
#69498 = DIRECTION('center_axis',(-1.,-2.22044604925031E-16,0.)) ;
#69499 = DIRECTION('ref_axis',(0.,0.,1.)) ;
#69500 = DIRECTION('center_axis',(-1.30514544126042E-16,0.587785252292473,
0.809016994374948)) ;
#69501 = DIRECTION('ref_axis',(-0.707106781186563,-0.572061402817672,0.415626937777444)) ;
#69502 = DIRECTION('center_axis',(1.79637858893621E-16,-0.809016994374948,
0.587785252292473)) ;
#69503 = DIRECTION('ref_axis',(-0.707106781186551,0.415626937777451,0.572061402817682)) ;
#69504 = DIRECTION('',(-1.79637858893621E-16,0.809016994374948,-0.587785252292473)) ;
#69505 = DIRECTION('center_axis',(-1.30514544126042E-16,0.587785252292473,
0.809016994374948)) ;
#69506 = DIRECTION('ref_axis',(-0.707106781186551,0.572061402817682,-0.415626937777451)) ;
#69507 = DIRECTION('center_axis',(-1.,-2.22044604925031E-16,0.)) ;
#69508 = DIRECTION('ref_axis',(0.,0.,1.)) ;
#69509 = DIRECTION('center_axis',(-6.86155564311058E-17,0.309016994374947,
0.951056516295154)) ;
#69510 = DIRECTION('ref_axis',(-0.707106781186557,-0.672498511963948,0.218508012224407)) ;
#69511 = DIRECTION('center_axis',(1.30514544126042E-16,-0.587785252292473,
0.809016994374947)) ;
#69512 = DIRECTION('ref_axis',(-0.707106781186534,0.572061402817695,0.415626937777462)) ;
#69513 = DIRECTION('',(-1.30514544126042E-16,0.587785252292473,-0.809016994374947)) ;
#69514 = DIRECTION('center_axis',(-6.86155564311058E-17,0.309016994374947,
0.951056516295154)) ;
#69515 = DIRECTION('ref_axis',(-0.707106781186557,0.672498511963948,-0.218508012224407)) ;
#69516 = DIRECTION('center_axis',(-1.,-2.22044604925031E-16,0.)) ;
#69517 = DIRECTION('ref_axis',(0.,0.,1.)) ;
#69518 = DIRECTION('center_axis',(0.,0.,1.)) ;
#69519 = DIRECTION('ref_axis',(-0.707106781186568,-0.707106781186527,0.)) ;
#69520 = DIRECTION('center_axis',(6.86155564311059E-17,-0.309016994374948,
0.951056516295154)) ;
#69521 = DIRECTION('ref_axis',(-0.707106781186557,0.672498511963948,0.218508012224408)) ;
#69522 = DIRECTION('center_axis',(0.,0.,1.)) ;
#69523 = DIRECTION('ref_axis',(-0.707106781186589,0.707106781186506,0.)) ;
#69524 = DIRECTION('center_axis',(-1.,-2.22044604925031E-16,0.)) ;
#69525 = DIRECTION('ref_axis',(0.,0.,1.)) ;
#69526 = DIRECTION('center_axis',(6.86155564311059E-17,-0.309016994374948,
0.951056516295154)) ;
#69527 = DIRECTION('ref_axis',(-0.707106781186557,-0.672498511963948,-0.218508012224408)) ;
#69528 = DIRECTION('center_axis',(-1.,-2.22044604925031E-16,0.)) ;
#69529 = DIRECTION('ref_axis',(0.,0.309016994374018,-0.951056516295456)) ;
#69530 = DIRECTION('center_axis',(-1.,-2.22044604925031E-16,0.)) ;
#69531 = DIRECTION('ref_axis',(0.,-3.41060513164848E-13,-1.)) ;
#69532 = DIRECTION('center_axis',(-1.,-2.22044604925031E-16,0.)) ;
#69533 = DIRECTION('ref_axis',(0.,0.,1.)) ;
#69534 = DIRECTION('center_axis',(-1.,-2.22044604925031E-16,0.)) ;
#69535 = DIRECTION('ref_axis',(-1.00806141154385E-16,0.453990499739547,-0.891006524188368)) ;
#69536 = DIRECTION('center_axis',(1.30514544126042E-16,-0.587785252292473,
0.809016994374947)) ;
#69537 = DIRECTION('ref_axis',(-0.707106781186534,-0.572061402817695,-0.415626937777461)) ;
#69538 = DIRECTION('',(1.30514544126042E-16,-0.587785252292473,0.809016994374947)) ;
#69539 = DIRECTION('center_axis',(-1.,-2.22044604925031E-16,0.)) ;
#69540 = DIRECTION('ref_axis',(0.,0.587785252293422,-0.809016994374258)) ;
#69541 = DIRECTION('center_axis',(-1.,-2.22044604925031E-16,0.)) ;
#69542 = DIRECTION('ref_axis',(-1.30514544126041E-16,0.587785252292468,-0.809016994374951)) ;
#69543 = DIRECTION('center_axis',(-1.,-2.22044604925031E-16,0.)) ;
#69544 = DIRECTION('ref_axis',(0.,-0.309016994375666,-0.95105651629492)) ;
#69545 = DIRECTION('center_axis',(-1.,-2.22044604925031E-16,0.)) ;
#69546 = DIRECTION('ref_axis',(0.,0.,1.)) ;
#69547 = DIRECTION('center_axis',(-1.,-2.22044604925031E-16,0.)) ;
#69548 = DIRECTION('ref_axis',(-1.57009245868377E-16,0.707106781186547,-0.707106781186547)) ;
#69549 = DIRECTION('center_axis',(1.79637858893621E-16,-0.809016994374948,
0.587785252292473)) ;
#69550 = DIRECTION('ref_axis',(-0.707106781186575,-0.415626937777437,-0.572061402817662)) ;
#69551 = DIRECTION('',(1.79637858893621E-16,-0.809016994374948,0.587785252292473)) ;
#69552 = DIRECTION('center_axis',(-1.,-2.22044604925031E-16,0.)) ;
#69553 = DIRECTION('ref_axis',(0.,0.809016994375283,-0.587785252292011)) ;
#69554 = DIRECTION('center_axis',(-1.,-2.22044604925031E-16,0.)) ;
#69555 = DIRECTION('ref_axis',(-1.79637858893621E-16,0.809016994374947,-0.587785252292474)) ;
#69556 = DIRECTION('center_axis',(-1.,-2.22044604925031E-16,0.)) ;
#69557 = DIRECTION('ref_axis',(0.,-0.587785252292347,-0.809016994375039)) ;
#69558 = DIRECTION('center_axis',(-1.,-2.22044604925031E-16,0.)) ;
#69559 = DIRECTION('ref_axis',(0.,0.,1.)) ;
#69560 = DIRECTION('center_axis',(-1.,-2.22044604925031E-16,0.)) ;
#69561 = DIRECTION('ref_axis',(-1.97843191649031E-16,0.891006524188368,-0.453990499739547)) ;
#69562 = DIRECTION('center_axis',(2.11176968422134E-16,-0.951056516295154,
0.309016994374947)) ;
#69563 = DIRECTION('ref_axis',(-0.707106781186563,-0.218508012224406,-0.672498511963943)) ;
#69564 = DIRECTION('',(2.11176968422134E-16,-0.951056516295154,0.309016994374947)) ;
#69565 = DIRECTION('center_axis',(-1.,-2.22044604925031E-16,0.)) ;
#69566 = DIRECTION('ref_axis',(0.,0.951056516294897,-0.309016994375738)) ;
#69567 = DIRECTION('center_axis',(-1.,-2.22044604925031E-16,0.)) ;
#69568 = DIRECTION('ref_axis',(-2.11176968422134E-16,0.951056516295153,-0.309016994374948)) ;
#69569 = DIRECTION('center_axis',(-1.,-2.22044604925031E-16,0.)) ;
#69570 = DIRECTION('ref_axis',(0.,-0.809016994374792,-0.587785252292687)) ;
#69571 = DIRECTION('center_axis',(-1.,-2.22044604925031E-16,0.)) ;
#69572 = DIRECTION('ref_axis',(0.,0.,1.)) ;
#69573 = DIRECTION('center_axis',(-1.,-2.22044604925031E-16,0.)) ;
#69574 = DIRECTION('ref_axis',(-2.19310867376507E-16,0.987688340595138,-0.156434465040228)) ;
#69575 = DIRECTION('center_axis',(2.22044604925031E-16,-1.,-2.22044604925031E-16)) ;
#69576 = DIRECTION('ref_axis',(-0.707106781186568,-9.08458920382451E-30,-0.707106781186527)) ;
#69577 = DIRECTION('',(2.22044604925031E-16,-1.,-2.22044604925031E-16)) ;
#69578 = DIRECTION('center_axis',(-1.,-2.22044604925031E-16,0.)) ;
#69579 = DIRECTION('ref_axis',(0.,1.,-4.9737991503207E-14)) ;
#69580 = DIRECTION('center_axis',(-1.,-2.22044604925031E-16,0.)) ;
#69581 = DIRECTION('ref_axis',(-2.22044604925031E-16,1.,0.)) ;
#69582 = DIRECTION('center_axis',(-1.,-2.22044604925031E-16,0.)) ;
#69583 = DIRECTION('ref_axis',(0.,-0.951056516295317,-0.309016994374445)) ;
#69584 = DIRECTION('center_axis',(-1.,-2.22044604925031E-16,0.)) ;
#69585 = DIRECTION('ref_axis',(0.,0.,1.)) ;
#69586 = DIRECTION('center_axis',(-1.,-2.22044604925031E-16,0.)) ;
#69587 = DIRECTION('ref_axis',(-2.19310867376507E-16,0.987688340595138,0.156434465040232)) ;
#69588 = DIRECTION('center_axis',(2.11176968422134E-16,-0.951056516295154,
-0.309016994374948)) ;
#69589 = DIRECTION('ref_axis',(-0.707106781186563,0.218508012224406,-0.672498511963942)) ;
#69590 = DIRECTION('',(2.11176968422134E-16,-0.951056516295153,-0.309016994374948)) ;
#69591 = DIRECTION('center_axis',(-1.,-2.22044604925031E-16,0.)) ;
#69592 = DIRECTION('ref_axis',(0.,0.,1.)) ;
#69593 = DIRECTION('center_axis',(-1.,-2.22044604925031E-16,0.)) ;
#69594 = DIRECTION('ref_axis',(-2.11176968422134E-16,0.951056516295153,0.309016994374948)) ;
#69595 = DIRECTION('center_axis',(-1.,-2.22044604925031E-16,0.)) ;
#69596 = DIRECTION('ref_axis',(0.,-1.,5.04485342389671E-13)) ;
#69597 = DIRECTION('center_axis',(-1.,-2.22044604925031E-16,0.)) ;
#69598 = DIRECTION('ref_axis',(0.,0.,1.)) ;
#69599 = DIRECTION('center_axis',(-1.,-2.22044604925031E-16,0.)) ;
#69600 = DIRECTION('ref_axis',(-1.97843191649031E-16,0.891006524188368,0.453990499739546)) ;
#69601 = DIRECTION('center_axis',(1.79637858893621E-16,-0.809016994374947,
-0.587785252292473)) ;
#69602 = DIRECTION('ref_axis',(-0.707106781186592,0.415626937777427,-0.572061402817648)) ;
#69603 = DIRECTION('',(1.79637858893621E-16,-0.809016994374947,-0.587785252292473)) ;
#69604 = DIRECTION('center_axis',(-1.,-2.22044604925031E-16,0.)) ;
#69605 = DIRECTION('ref_axis',(0.,0.,1.)) ;
#69606 = DIRECTION('center_axis',(-1.,-2.22044604925031E-16,0.)) ;
#69607 = DIRECTION('ref_axis',(-1.79637858893621E-16,0.809016994374947,0.587785252292474)) ;
#69608 = DIRECTION('center_axis',(-1.,-2.22044604925031E-16,0.)) ;
#69609 = DIRECTION('ref_axis',(0.,0.,1.)) ;
#69610 = DIRECTION('center_axis',(-1.,-2.22044604925031E-16,0.)) ;
#69611 = DIRECTION('ref_axis',(0.,0.,1.)) ;
#69612 = DIRECTION('center_axis',(-1.,-2.22044604925031E-16,0.)) ;
#69613 = DIRECTION('ref_axis',(-1.57009245868377E-16,0.707106781186548,0.707106781186547)) ;
#69614 = DIRECTION('center_axis',(1.30514544126042E-16,-0.587785252292473,
-0.809016994374948)) ;
#69615 = DIRECTION('ref_axis',(-0.707106781186568,0.572061402817668,-0.415626937777441)) ;
#69616 = DIRECTION('',(1.30514544126042E-16,-0.587785252292473,-0.809016994374947)) ;
#69617 = DIRECTION('center_axis',(-1.,-2.22044604925031E-16,0.)) ;
#69618 = DIRECTION('ref_axis',(0.,0.,1.)) ;
#69619 = DIRECTION('center_axis',(-1.,-2.22044604925031E-16,0.)) ;
#69620 = DIRECTION('ref_axis',(-1.30514544126041E-16,0.587785252292468,0.809016994374951)) ;
#69621 = DIRECTION('center_axis',(-1.,-2.22044604925031E-16,0.)) ;
#69622 = DIRECTION('ref_axis',(0.,0.,1.)) ;
#69623 = DIRECTION('center_axis',(-1.,-2.22044604925031E-16,0.)) ;
#69624 = DIRECTION('ref_axis',(0.,0.,1.)) ;
#69625 = DIRECTION('center_axis',(-1.,-2.22044604925031E-16,0.)) ;
#69626 = DIRECTION('ref_axis',(-1.00806141154386E-16,0.453990499739549,0.891006524188367)) ;
#69627 = DIRECTION('center_axis',(6.86155564311058E-17,-0.309016994374947,
-0.951056516295154)) ;
#69628 = DIRECTION('ref_axis',(-0.707106781186557,0.672498511963948,-0.218508012224407)) ;
#69629 = DIRECTION('',(6.86155564311058E-17,-0.309016994374947,-0.951056516295154)) ;
#69630 = DIRECTION('center_axis',(-1.,-2.22044604925031E-16,0.)) ;
#69631 = DIRECTION('ref_axis',(0.,0.,1.)) ;
#69632 = DIRECTION('center_axis',(-1.,-2.22044604925031E-16,0.)) ;
#69633 = DIRECTION('ref_axis',(-6.86155564311052E-17,0.309016994374945,0.951056516295154)) ;
#69634 = DIRECTION('center_axis',(-1.,-2.22044604925031E-16,0.)) ;
#69635 = DIRECTION('ref_axis',(0.,0.,1.)) ;
#69636 = DIRECTION('center_axis',(-1.,-2.22044604925031E-16,0.)) ;
#69637 = DIRECTION('ref_axis',(0.,0.,1.)) ;
#69638 = DIRECTION('center_axis',(-1.,-2.22044604925031E-16,0.)) ;
#69639 = DIRECTION('ref_axis',(-3.47354289865171E-17,0.156434465040233,0.987688340595137)) ;
#69640 = DIRECTION('center_axis',(-2.46519032881566E-32,1.11022302462516E-16,
-1.)) ;
#69641 = DIRECTION('ref_axis',(-0.707106781186589,0.707106781186506,7.85046229341844E-17)) ;
#69642 = DIRECTION('',(-2.46519032881566E-32,1.11022302462516E-16,-1.)) ;
#69643 = DIRECTION('center_axis',(-1.,-2.22044604925031E-16,0.)) ;
#69644 = DIRECTION('ref_axis',(0.,0.,1.)) ;
#69645 = DIRECTION('center_axis',(-1.,-2.22044604925031E-16,0.)) ;
#69646 = DIRECTION('ref_axis',(0.,0.,1.)) ;
#69647 = DIRECTION('center_axis',(-1.,-2.22044604925031E-16,0.)) ;
#69648 = DIRECTION('ref_axis',(0.,0.,1.)) ;
#69649 = DIRECTION('center_axis',(-1.,-2.22044604925031E-16,0.)) ;
#69650 = DIRECTION('ref_axis',(6.86155564311052E-17,-0.309016994374945,0.951056516295154)) ;
#69651 = DIRECTION('center_axis',(1.,2.22044604925031E-16,0.)) ;
#69652 = DIRECTION('ref_axis',(2.22044604925031E-16,-1.,0.)) ;
#69653 = DIRECTION('',(-1.,-2.22044604925031E-16,0.)) ;
#69654 = DIRECTION('',(1.,2.22044604925031E-16,0.)) ;
#69655 = DIRECTION('center_axis',(-2.11176968422134E-16,0.951056516295154,
0.309016994374948)) ;
#69656 = DIRECTION('ref_axis',(6.86155564311058E-17,-0.309016994374948,0.951056516295154)) ;
#69657 = DIRECTION('',(1.,2.22044604925031E-16,0.)) ;
#69658 = DIRECTION('center_axis',(1.,2.22044604925031E-16,0.)) ;
#69659 = DIRECTION('ref_axis',(6.8615556431103E-17,-0.309016994374935,0.951056516295158)) ;
#69660 = DIRECTION('',(1.,2.22044604925031E-16,0.)) ;
#69661 = DIRECTION('center_axis',(2.11176968422134E-16,-0.951056516295154,
-0.309016994374948)) ;
#69662 = DIRECTION('ref_axis',(-6.86155564311058E-17,0.309016994374948,-0.951056516295154)) ;
#69663 = DIRECTION('center_axis',(1.79637858893621E-16,-0.809016994374947,
-0.587785252292473)) ;
#69664 = DIRECTION('ref_axis',(-1.30514544126042E-16,0.587785252292473,-0.809016994374947)) ;
#69665 = DIRECTION('',(1.,2.22044604925031E-16,0.)) ;
#69666 = DIRECTION('',(1.,2.22044604925031E-16,0.)) ;
#69667 = DIRECTION('center_axis',(-1.79637858893621E-16,0.809016994374947,
0.587785252292473)) ;
#69668 = DIRECTION('ref_axis',(1.30514544126042E-16,-0.587785252292473,0.809016994374947)) ;
#69669 = DIRECTION('',(1.,2.22044604925031E-16,0.)) ;
#69670 = DIRECTION('',(-1.,-2.22044604925031E-16,0.)) ;
#69671 = DIRECTION('center_axis',(1.,2.22044604925031E-16,0.)) ;
#69672 = DIRECTION('ref_axis',(-1.3051454412604E-16,0.587785252292467,-0.809016994374952)) ;
#69673 = DIRECTION('center_axis',(1.30514544126042E-16,-0.587785252292473,
-0.809016994374948)) ;
#69674 = DIRECTION('ref_axis',(-1.79637858893621E-16,0.809016994374948,-0.587785252292473)) ;
#69675 = DIRECTION('',(1.,2.22044604925031E-16,0.)) ;
#69676 = DIRECTION('',(1.,2.22044604925031E-16,0.)) ;
#69677 = DIRECTION('center_axis',(-1.30514544126042E-16,0.587785252292473,
0.809016994374948)) ;
#69678 = DIRECTION('ref_axis',(1.79637858893621E-16,-0.809016994374948,0.587785252292473)) ;
#69679 = DIRECTION('',(1.,2.22044604925031E-16,0.)) ;
#69680 = DIRECTION('',(-1.,-2.22044604925031E-16,0.)) ;
#69681 = DIRECTION('center_axis',(1.,2.22044604925031E-16,0.)) ;
#69682 = DIRECTION('ref_axis',(-1.79637858893622E-16,0.809016994374951,-0.587785252292468)) ;
#69683 = DIRECTION('center_axis',(6.86155564311058E-17,-0.309016994374947,
-0.951056516295154)) ;
#69684 = DIRECTION('ref_axis',(-2.11176968422134E-16,0.951056516295154,-0.309016994374947)) ;
#69685 = DIRECTION('',(1.,2.22044604925031E-16,0.)) ;
#69686 = DIRECTION('',(1.,2.22044604925031E-16,0.)) ;
#69687 = DIRECTION('center_axis',(-6.86155564311058E-17,0.309016994374947,
0.951056516295154)) ;
#69688 = DIRECTION('ref_axis',(2.11176968422134E-16,-0.951056516295154,0.309016994374947)) ;
#69689 = DIRECTION('',(1.,2.22044604925031E-16,0.)) ;
#69690 = DIRECTION('',(-1.,-2.22044604925031E-16,0.)) ;
#69691 = DIRECTION('center_axis',(1.,2.22044604925031E-16,0.)) ;
#69692 = DIRECTION('ref_axis',(-2.11176968422134E-16,0.951056516295157,-0.309016994374937)) ;
#69693 = DIRECTION('center_axis',(-4.93038065763132E-32,2.22044604925031E-16,
-1.)) ;
#69694 = DIRECTION('ref_axis',(-2.22044604925031E-16,1.,2.22044604925031E-16)) ;
#69695 = DIRECTION('',(1.,2.22044604925031E-16,0.)) ;
#69696 = DIRECTION('',(1.,2.22044604925031E-16,0.)) ;
#69697 = DIRECTION('center_axis',(4.93038065763132E-32,-2.22044604925031E-16,
1.)) ;
#69698 = DIRECTION('ref_axis',(2.22044604925031E-16,-1.,-2.22044604925031E-16)) ;
#69699 = DIRECTION('',(1.,2.22044604925031E-16,0.)) ;
#69700 = DIRECTION('',(-1.,-2.22044604925031E-16,0.)) ;
#69701 = DIRECTION('center_axis',(1.,2.22044604925031E-16,0.)) ;
#69702 = DIRECTION('ref_axis',(-2.22044604925031E-16,1.,-7.51101277651833E-17)) ;
#69703 = DIRECTION('center_axis',(-6.86155564311059E-17,0.309016994374948,
-0.951056516295154)) ;
#69704 = DIRECTION('ref_axis',(-2.11176968422134E-16,0.951056516295154,0.309016994374948)) ;
#69705 = DIRECTION('',(1.,2.22044604925031E-16,0.)) ;
#69706 = DIRECTION('',(1.,2.22044604925031E-16,0.)) ;
#69707 = DIRECTION('center_axis',(6.86155564311059E-17,-0.309016994374948,
0.951056516295154)) ;
#69708 = DIRECTION('ref_axis',(2.11176968422134E-16,-0.951056516295154,-0.309016994374948)) ;
#69709 = DIRECTION('',(1.,2.22044604925031E-16,0.)) ;
#69710 = DIRECTION('',(-1.,-2.22044604925031E-16,0.)) ;
#69711 = DIRECTION('center_axis',(1.,2.22044604925031E-16,0.)) ;
#69712 = DIRECTION('ref_axis',(-2.11176968422134E-16,0.951056516295157,0.309016994374937)) ;
#69713 = DIRECTION('center_axis',(-1.30514544126042E-16,0.587785252292473,
-0.809016994374947)) ;
#69714 = DIRECTION('ref_axis',(-1.79637858893621E-16,0.809016994374947,0.587785252292473)) ;
#69715 = DIRECTION('',(1.,2.22044604925031E-16,0.)) ;
#69716 = DIRECTION('',(1.,2.22044604925031E-16,0.)) ;
#69717 = DIRECTION('center_axis',(1.30514544126042E-16,-0.587785252292473,
0.809016994374947)) ;
#69718 = DIRECTION('ref_axis',(1.79637858893621E-16,-0.809016994374947,-0.587785252292473)) ;
#69719 = DIRECTION('',(1.,2.22044604925031E-16,0.)) ;
#69720 = DIRECTION('',(-1.,-2.22044604925031E-16,0.)) ;
#69721 = DIRECTION('center_axis',(1.,2.22044604925031E-16,0.)) ;
#69722 = DIRECTION('ref_axis',(-1.79637858893622E-16,0.80901699437495,0.587785252292469)) ;
#69723 = DIRECTION('center_axis',(-1.79637858893621E-16,0.809016994374948,
-0.587785252292473)) ;
#69724 = DIRECTION('ref_axis',(-1.30514544126042E-16,0.587785252292473,0.809016994374948)) ;
#69725 = DIRECTION('',(1.,2.22044604925031E-16,0.)) ;
#69726 = DIRECTION('',(1.,2.22044604925031E-16,0.)) ;
#69727 = DIRECTION('center_axis',(1.79637858893621E-16,-0.809016994374948,
0.587785252292473)) ;
#69728 = DIRECTION('ref_axis',(1.30514544126042E-16,-0.587785252292473,-0.809016994374948)) ;
#69729 = DIRECTION('',(1.,2.22044604925031E-16,0.)) ;
#69730 = DIRECTION('',(-1.,-2.22044604925031E-16,0.)) ;
#69731 = DIRECTION('center_axis',(1.,2.22044604925031E-16,0.)) ;
#69732 = DIRECTION('ref_axis',(-1.30514544126041E-16,0.587785252292468,0.809016994374951)) ;
#69733 = DIRECTION('center_axis',(-2.11176968422134E-16,0.951056516295154,
-0.309016994374947)) ;
#69734 = DIRECTION('ref_axis',(-6.86155564311058E-17,0.309016994374947,0.951056516295154)) ;
#69735 = DIRECTION('',(1.,2.22044604925031E-16,0.)) ;
#69736 = DIRECTION('',(1.,2.22044604925031E-16,0.)) ;
#69737 = DIRECTION('center_axis',(2.11176968422134E-16,-0.951056516295154,
0.309016994374947)) ;
#69738 = DIRECTION('ref_axis',(6.86155564311058E-17,-0.309016994374947,-0.951056516295154)) ;
#69739 = DIRECTION('',(1.,2.22044604925031E-16,0.)) ;
#69740 = DIRECTION('',(-1.,-2.22044604925031E-16,0.)) ;
#69741 = DIRECTION('center_axis',(1.,2.22044604925031E-16,0.)) ;
#69742 = DIRECTION('ref_axis',(-6.8615556431105E-17,0.309016994374944,0.951056516295155)) ;
#69743 = DIRECTION('center_axis',(-2.22044604925031E-16,1.,1.11022302462516E-16)) ;
#69744 = DIRECTION('ref_axis',(2.46519032881566E-32,-1.11022302462516E-16,
1.)) ;
#69745 = DIRECTION('',(1.,2.22044604925031E-16,0.)) ;
#69746 = DIRECTION('',(1.,2.22044604925031E-16,0.)) ;
#69747 = DIRECTION('center_axis',(2.22044604925031E-16,-1.,-1.11022302462516E-16)) ;
#69748 = DIRECTION('ref_axis',(-2.46519032881566E-32,1.11022302462516E-16,
-1.)) ;
#69749 = DIRECTION('',(1.,2.22044604925031E-16,0.)) ;
#69750 = DIRECTION('center_axis',(1.,2.22044604925031E-16,0.)) ;
#69751 = DIRECTION('ref_axis',(-2.01194122103066E-30,9.06097773332504E-15,
1.)) ;
#69752 = DIRECTION('center_axis',(1.,2.22044604925031E-16,0.)) ;
#69753 = DIRECTION('ref_axis',(2.22044604925031E-16,-1.,0.)) ;
#69754 = DIRECTION('center_axis',(1.,2.22044604925031E-16,0.)) ;
#69755 = DIRECTION('ref_axis',(2.22044604925031E-16,-1.,0.)) ;
#69756 = DIRECTION('center_axis',(1.,2.22044604925031E-16,0.)) ;
#69757 = DIRECTION('ref_axis',(2.22044604925031E-16,-1.,0.)) ;
#69758 = DIRECTION('center_axis',(1.,2.22044604925031E-16,0.)) ;
#69759 = DIRECTION('ref_axis',(2.22044604925031E-16,-1.,0.)) ;
#69760 = DIRECTION('center_axis',(1.,2.22044604925031E-16,0.)) ;
#69761 = DIRECTION('ref_axis',(2.22044604925031E-16,-1.,0.)) ;
#69762 = DIRECTION('center_axis',(1.,2.22044604925031E-16,0.)) ;
#69763 = DIRECTION('ref_axis',(2.22044604925031E-16,-1.,0.)) ;
#69764 = DIRECTION('center_axis',(1.,2.22044604925031E-16,0.)) ;
#69765 = DIRECTION('ref_axis',(2.22044604925031E-16,-1.,0.)) ;
#69766 = DIRECTION('center_axis',(1.,2.22044604925031E-16,0.)) ;
#69767 = DIRECTION('ref_axis',(2.22044604925031E-16,-1.,0.)) ;
#69768 = DIRECTION('center_axis',(1.,2.22044604925031E-16,0.)) ;
#69769 = DIRECTION('ref_axis',(2.22044604925031E-16,-1.,0.)) ;
#69770 = DIRECTION('center_axis',(1.,2.22044604925031E-16,0.)) ;
#69771 = DIRECTION('ref_axis',(2.22044604925031E-16,-1.,0.)) ;
#69772 = DIRECTION('',(1.,2.22044604925031E-16,0.)) ;
#69773 = DIRECTION('axis',(0.,0.,1.)) ;
#69774 = DIRECTION('refdir',(1.,0.,0.)) ;
#69775 = DIRECTION('center_axis',(-1.,0.,0.)) ;
#69776 = DIRECTION('ref_axis',(0.,0.45781237757936,-0.889048832705568)) ;
#69777 = DIRECTION('',(1.,0.,0.)) ;
#69778 = DIRECTION('center_axis',(1.,0.,0.)) ;
#69779 = DIRECTION('ref_axis',(0.,-1.,5.29386630725752E-15)) ;
#69780 = DIRECTION('center_axis',(-1.,0.,0.)) ;
#69781 = DIRECTION('ref_axis',(0.,0.45781237757936,-0.889048832705568)) ;
#69782 = DIRECTION('',(1.,0.,0.)) ;
#69783 = DIRECTION('center_axis',(-1.,0.,0.)) ;
#69784 = DIRECTION('ref_axis',(0.,0.45781237757936,-0.889048832705568)) ;
#69785 = DIRECTION('',(1.,0.,0.)) ;
#69786 = DIRECTION('center_axis',(-1.,0.,0.)) ;
#69787 = DIRECTION('ref_axis',(0.,0.45781237757936,-0.889048832705568)) ;
#69788 = DIRECTION('',(1.,0.,0.)) ;
#69789 = DIRECTION('center_axis',(-1.,0.,0.)) ;
#69790 = DIRECTION('ref_axis',(0.,0.457902639548171,-0.889002346844381)) ;
#69791 = DIRECTION('',(1.,0.,0.)) ;
#69792 = DIRECTION('center_axis',(1.,0.,0.)) ;
#69793 = DIRECTION('ref_axis',(0.,-1.,5.29386630725752E-15)) ;
#69794 = DIRECTION('center_axis',(-1.,0.,0.)) ;
#69795 = DIRECTION('ref_axis',(0.,0.457902639548171,-0.889002346844381)) ;
#69796 = DIRECTION('',(1.,0.,0.)) ;
#69797 = DIRECTION('center_axis',(-1.,0.,0.)) ;
#69798 = DIRECTION('ref_axis',(0.,0.457902639548171,-0.889002346844381)) ;
#69799 = DIRECTION('',(1.,0.,0.)) ;
#69800 = DIRECTION('center_axis',(-1.,0.,0.)) ;
#69801 = DIRECTION('ref_axis',(0.,0.457902639548171,-0.889002346844381)) ;
#69802 = DIRECTION('',(1.,0.,0.)) ;
#69803 = DIRECTION('center_axis',(-1.,0.,0.)) ;
#69804 = DIRECTION('ref_axis',(0.,0.457902639548171,-0.889002346844381)) ;
#69805 = DIRECTION('',(1.,0.,0.)) ;
#69806 = DIRECTION('center_axis',(-1.,0.,0.)) ;
#69807 = DIRECTION('ref_axis',(0.,0.457902639548171,-0.889002346844381)) ;
#69808 = DIRECTION('',(1.,0.,0.)) ;
#69809 = DIRECTION('center_axis',(-1.,0.,0.)) ;
#69810 = DIRECTION('ref_axis',(0.,-1.,0.)) ;
#69811 = DIRECTION('center_axis',(1.,0.,0.)) ;
#69812 = DIRECTION('ref_axis',(0.,-1.,0.)) ;
#69813 = DIRECTION('center_axis',(-1.,0.,0.)) ;
#69814 = DIRECTION('ref_axis',(0.,-1.,0.)) ;
#69815 = DIRECTION('center_axis',(1.,0.,0.)) ;
#69816 = DIRECTION('ref_axis',(0.,-1.,0.)) ;
#69817 = DIRECTION('center_axis',(-1.,0.,0.)) ;
#69818 = DIRECTION('ref_axis',(0.,-1.,0.)) ;
#69819 = DIRECTION('center_axis',(1.,0.,0.)) ;
#69820 = DIRECTION('ref_axis',(0.,-1.,0.)) ;
#69821 = DIRECTION('center_axis',(1.,0.,0.)) ;
#69822 = DIRECTION('ref_axis',(0.,-1.,0.)) ;
#69823 = DIRECTION('center_axis',(-1.,0.,0.)) ;
#69824 = DIRECTION('ref_axis',(0.,0.457902639548171,-0.889002346844381)) ;
#69825 = DIRECTION('center_axis',(-1.,0.,0.)) ;
#69826 = DIRECTION('ref_axis',(0.,-1.,5.29386630725752E-15)) ;
#69827 = DIRECTION('center_axis',(-1.,0.,0.)) ;
#69828 = DIRECTION('ref_axis',(0.,0.45781237757936,-0.889048832705568)) ;
#69829 = DIRECTION('center_axis',(-1.,0.,0.)) ;
#69830 = DIRECTION('ref_axis',(0.,-1.,5.29386630725752E-15)) ;
#69831 = DIRECTION('center_axis',(1.,0.,0.)) ;
#69832 = DIRECTION('ref_axis',(0.,0.,-1.)) ;
#69833 = DIRECTION('center_axis',(1.,0.,0.)) ;
#69834 = DIRECTION('ref_axis',(0.,0.,-1.)) ;
#69835 = DIRECTION('center_axis',(1.,0.,0.)) ;
#69836 = DIRECTION('ref_axis',(0.,0.,-1.)) ;
#69837 = DIRECTION('center_axis',(1.,0.,0.)) ;
#69838 = DIRECTION('ref_axis',(0.,0.,-1.)) ;
#69839 = DIRECTION('center_axis',(-1.,0.,0.)) ;
#69840 = DIRECTION('ref_axis',(0.,-1.,0.)) ;
#69841 = DIRECTION('center_axis',(-1.,0.,0.)) ;
#69842 = DIRECTION('ref_axis',(0.,-1.,0.)) ;
#69843 = DIRECTION('',(0.,0.,1.)) ;
#69844 = DIRECTION('',(1.,0.,0.)) ;
#69845 = DIRECTION('',(0.,0.,1.)) ;
#69846 = DIRECTION('',(1.,0.,0.)) ;
#69847 = DIRECTION('',(0.,0.,1.)) ;
#69848 = DIRECTION('',(1.,0.,0.)) ;
#69849 = DIRECTION('',(0.,0.,1.)) ;
#69850 = DIRECTION('',(1.,0.,0.)) ;
#69851 = DIRECTION('',(0.,0.,1.)) ;
#69852 = DIRECTION('',(1.,0.,0.)) ;
#69853 = DIRECTION('',(0.,0.,1.)) ;
#69854 = DIRECTION('',(1.,0.,0.)) ;
#69855 = DIRECTION('',(0.,0.,1.)) ;
#69856 = DIRECTION('',(1.,0.,0.)) ;
#69857 = DIRECTION('',(0.,0.,1.)) ;
#69858 = DIRECTION('',(1.,0.,0.)) ;
#69859 = DIRECTION('',(0.,0.,1.)) ;
#69860 = DIRECTION('',(1.,0.,0.)) ;
#69861 = DIRECTION('',(0.,0.,1.)) ;
#69862 = DIRECTION('',(1.,0.,0.)) ;
#69863 = DIRECTION('',(0.,0.,1.)) ;
#69864 = DIRECTION('',(1.,0.,0.)) ;
#69865 = DIRECTION('',(0.,0.,1.)) ;
#69866 = DIRECTION('',(1.,0.,0.)) ;
#69867 = DIRECTION('',(0.,0.,1.)) ;
#69868 = DIRECTION('',(1.,0.,0.)) ;
#69869 = DIRECTION('',(0.,0.,1.)) ;
#69870 = DIRECTION('',(1.,0.,0.)) ;
#69871 = DIRECTION('',(0.,0.,1.)) ;
#69872 = DIRECTION('',(1.,0.,0.)) ;
#69873 = DIRECTION('',(0.,0.,1.)) ;
#69874 = DIRECTION('',(1.,0.,0.)) ;
#69875 = DIRECTION('',(0.,0.,1.)) ;
#69876 = DIRECTION('',(1.,0.,0.)) ;
#69877 = DIRECTION('',(0.,0.,1.)) ;
#69878 = DIRECTION('',(1.,0.,0.)) ;
#69879 = DIRECTION('',(0.,0.,1.)) ;
#69880 = DIRECTION('',(1.,0.,0.)) ;
#69881 = DIRECTION('',(0.,0.,1.)) ;
#69882 = DIRECTION('',(1.,0.,0.)) ;
#69883 = DIRECTION('',(0.,0.,1.)) ;
#69884 = DIRECTION('',(1.,0.,0.)) ;
#69885 = CARTESIAN_POINT('',(0.,0.,0.)) ;
#69886 = CARTESIAN_POINT('',(0.,0.,0.)) ;
#69887 = CARTESIAN_POINT('Origin',(74.5283628290597,239.4,18.3213203435596)) ;
#69888 = CARTESIAN_POINT('',(68.7283628290597,239.4,18.5213203435596)) ;
#69889 = CARTESIAN_POINT('Origin',(74.5283628290597,239.4,18.5213203435596)) ;
#69890 = CARTESIAN_POINT('',(68.5283628290597,239.4,18.3213203435596)) ;
#69891 = CARTESIAN_POINT('Origin',(68.7283628290597,239.4,18.3213203435596)) ;
#69892 = CARTESIAN_POINT('Origin',(74.5283628290597,239.4,18.3213203435596)) ;
#69893 = CARTESIAN_POINT('Origin',(74.5283628290597,239.4,16.0213203435596)) ;
#69894 = CARTESIAN_POINT('',(68.5283628290597,239.4,16.2213203435596)) ;
#69895 = CARTESIAN_POINT('',(68.5283628290597,239.4,16.0213203435596)) ;
#69896 = CARTESIAN_POINT('',(68.5800869669907,238.61386116447,16.2213203435596)) ;
#69897 = CARTESIAN_POINT('Origin',(74.5283628290597,239.4,16.2213203435596)) ;
#69898 = CARTESIAN_POINT('',(68.5800869669907,238.61386116447,7.2786795888419)) ;
#69899 = CARTESIAN_POINT('',(68.5800869669907,238.61386116447,16.0213203435596)) ;
#69900 = CARTESIAN_POINT('',(68.6282860496011,238.309544133633,7.2786795888419)) ;
#69901 = CARTESIAN_POINT('Origin',(74.5283628290597,239.4,7.2786795888419)) ;
#69902 = CARTESIAN_POINT('',(68.6282860496011,238.309544133633,16.2213203435596)) ;
#69903 = CARTESIAN_POINT('',(68.6282860496011,238.309544133633,16.0213203435596)) ;
#69904 = CARTESIAN_POINT('',(69.1141465698346,236.814219209147,16.2213203435596)) ;
#69905 = CARTESIAN_POINT('Origin',(74.5283628290597,239.4,16.2213203435596)) ;
#69906 = CARTESIAN_POINT('',(69.1141465698346,236.814219209147,7.2786795888419)) ;
#69907 = CARTESIAN_POINT('',(69.1141465698346,236.814219209147,16.0213203435596)) ;
#69908 = CARTESIAN_POINT('',(69.254025755637,236.53969084959,7.2786795888419)) ;
#69909 = CARTESIAN_POINT('Origin',(74.5283628290597,239.4,7.2786795888419)) ;
#69910 = CARTESIAN_POINT('',(69.254025755637,236.53969084959,16.2213203435596)) ;
#69911 = CARTESIAN_POINT('',(69.254025755637,236.53969084959,16.0213203435596)) ;
#69912 = CARTESIAN_POINT('',(70.1781873831942,235.267691493827,16.2213203435596)) ;
#69913 = CARTESIAN_POINT('Origin',(74.5283628290597,239.4,16.2213203435596)) ;
#69914 = CARTESIAN_POINT('',(70.1781873831942,235.267691493827,7.2786795888419)) ;
#69915 = CARTESIAN_POINT('',(70.1781873831942,235.267691493827,16.0213203435596)) ;
#69916 = CARTESIAN_POINT('',(70.3960543228867,235.049824554134,7.2786795888419)) ;
#69917 = CARTESIAN_POINT('Origin',(74.5283628290597,239.4,7.2786795888419)) ;
#69918 = CARTESIAN_POINT('',(70.3960543228867,235.049824554134,16.2213203435596)) ;
#69919 = CARTESIAN_POINT('',(70.3960543228867,235.049824554134,16.0213203435596)) ;
#69920 = CARTESIAN_POINT('',(71.6680536786498,234.125662926577,16.2213203435596)) ;
#69921 = CARTESIAN_POINT('Origin',(74.5283628290597,239.4,16.2213203435596)) ;
#69922 = CARTESIAN_POINT('',(71.6680536786497,234.125662926577,7.2786795888419)) ;
#69923 = CARTESIAN_POINT('',(71.6680536786497,234.125662926577,16.0213203435596)) ;
#69924 = CARTESIAN_POINT('',(71.942582038207,233.985783740775,7.2786795888419)) ;
#69925 = CARTESIAN_POINT('Origin',(74.5283628290597,239.4,7.2786795888419)) ;
#69926 = CARTESIAN_POINT('',(71.942582038207,233.985783740775,16.2213203435596)) ;
#69927 = CARTESIAN_POINT('',(71.942582038207,233.985783740775,16.0213203435596)) ;
#69928 = CARTESIAN_POINT('',(73.4379069626931,233.499923220541,16.2213203435596)) ;
#69929 = CARTESIAN_POINT('Origin',(74.5283628290597,239.4,16.2213203435596)) ;
#69930 = CARTESIAN_POINT('',(73.4379069626931,233.499923220541,7.2786795888419)) ;
#69931 = CARTESIAN_POINT('',(73.4379069626931,233.499923220541,16.0213203435596)) ;
#69932 = CARTESIAN_POINT('',(73.7422239935301,233.451724137931,7.2786795888419)) ;
#69933 = CARTESIAN_POINT('Origin',(74.5283628290597,239.4,7.2786795888419)) ;
#69934 = CARTESIAN_POINT('',(73.7422239935301,233.451724137931,16.2213203435596)) ;
#69935 = CARTESIAN_POINT('',(73.7422239935301,233.451724137931,16.0213203435596)) ;
#69936 = CARTESIAN_POINT('',(75.3145016645892,233.451724137931,16.2213203435596)) ;
#69937 = CARTESIAN_POINT('Origin',(74.5283628290597,239.4,16.2213203435596)) ;
#69938 = CARTESIAN_POINT('',(75.3145016645892,233.451724137931,7.2786795888419)) ;
#69939 = CARTESIAN_POINT('',(75.3145016645892,233.451724137931,16.0213203435596)) ;
#69940 = CARTESIAN_POINT('',(75.6188186954263,233.499923220541,7.2786795888419)) ;
#69941 = CARTESIAN_POINT('Origin',(74.5283628290597,239.4,7.2786795888419)) ;
#69942 = CARTESIAN_POINT('',(75.6188186954263,233.499923220541,16.2213203435596)) ;
#69943 = CARTESIAN_POINT('',(75.6188186954263,233.499923220541,16.0213203435596)) ;
#69944 = CARTESIAN_POINT('',(77.1141436199124,233.985783740775,16.2213203435596)) ;
#69945 = CARTESIAN_POINT('Origin',(74.5283628290597,239.4,16.2213203435596)) ;
#69946 = CARTESIAN_POINT('',(77.1141436199123,233.985783740775,7.2786795888419)) ;
#69947 = CARTESIAN_POINT('',(77.1141436199123,233.985783740775,16.0213203435596)) ;
#69948 = CARTESIAN_POINT('',(77.3886719794696,234.125662926577,7.2786795888419)) ;
#69949 = CARTESIAN_POINT('Origin',(74.5283628290597,239.4,7.2786795888419)) ;
#69950 = CARTESIAN_POINT('',(77.3886719794696,234.125662926577,16.2213203435596)) ;
#69951 = CARTESIAN_POINT('',(77.3886719794696,234.125662926577,16.0213203435596)) ;
#69952 = CARTESIAN_POINT('',(78.6606713352326,235.049824554134,16.2213203435596)) ;
#69953 = CARTESIAN_POINT('Origin',(74.5283628290597,239.4,16.2213203435596)) ;
#69954 = CARTESIAN_POINT('',(78.6606713352326,235.049824554134,7.2786795888419)) ;
#69955 = CARTESIAN_POINT('',(78.6606713352326,235.049824554134,16.0213203435596)) ;
#69956 = CARTESIAN_POINT('',(78.8785382749251,235.267691493827,7.2786795888419)) ;
#69957 = CARTESIAN_POINT('Origin',(74.5283628290597,239.4,7.2786795888419)) ;
#69958 = CARTESIAN_POINT('',(78.8785382749251,235.267691493827,16.2213203435596)) ;
#69959 = CARTESIAN_POINT('',(78.8785382749251,235.267691493827,16.0213203435596)) ;
#69960 = CARTESIAN_POINT('',(79.8026999024824,236.53969084959,16.2213203435596)) ;
#69961 = CARTESIAN_POINT('Origin',(74.5283628290597,239.4,16.2213203435596)) ;
#69962 = CARTESIAN_POINT('',(79.8026999024824,236.53969084959,7.2786795888419)) ;
#69963 = CARTESIAN_POINT('',(79.8026999024824,236.53969084959,16.0213203435596)) ;
#69964 = CARTESIAN_POINT('',(79.9425790882848,236.814219209147,7.2786795888419)) ;
#69965 = CARTESIAN_POINT('Origin',(74.5283628290597,239.4,7.2786795888419)) ;
#69966 = CARTESIAN_POINT('',(79.9425790882848,236.814219209147,16.2213203435596)) ;
#69967 = CARTESIAN_POINT('',(79.9425790882848,236.814219209147,16.0213203435596)) ;
#69968 = CARTESIAN_POINT('',(80.4284396085183,238.309544133633,16.2213203435596)) ;
#69969 = CARTESIAN_POINT('Origin',(74.5283628290597,239.4,16.2213203435596)) ;
#69970 = CARTESIAN_POINT('',(80.4284396085183,238.309544133633,7.2786795888419)) ;
#69971 = CARTESIAN_POINT('',(80.4284396085183,238.309544133633,16.0213203435596)) ;
#69972 = CARTESIAN_POINT('',(80.4766386911286,238.61386116447,7.2786795888419)) ;
#69973 = CARTESIAN_POINT('Origin',(74.5283628290597,239.4,7.2786795888419)) ;
#69974 = CARTESIAN_POINT('',(80.4766386911286,238.61386116447,16.2213203435596)) ;
#69975 = CARTESIAN_POINT('',(80.4766386911286,238.61386116447,16.0213203435596)) ;
#69976 = CARTESIAN_POINT('',(80.4766386911286,240.186138835529,16.2213203435596)) ;
#69977 = CARTESIAN_POINT('Origin',(74.5283628290597,239.4,16.2213203435596)) ;
#69978 = CARTESIAN_POINT('',(80.4766386911286,240.186138835529,7.2786795888419)) ;
#69979 = CARTESIAN_POINT('',(80.4766386911286,240.186138835529,16.0213203435596)) ;
#69980 = CARTESIAN_POINT('',(80.4284396085183,240.490455866367,7.2786795888419)) ;
#69981 = CARTESIAN_POINT('Origin',(74.5283628290597,239.4,7.2786795888419)) ;
#69982 = CARTESIAN_POINT('',(80.4284396085183,240.490455866367,16.2213203435596)) ;
#69983 = CARTESIAN_POINT('',(80.4284396085183,240.490455866367,16.0213203435596)) ;
#69984 = CARTESIAN_POINT('',(79.9425790882847,241.985780790853,16.2213203435596)) ;
#69985 = CARTESIAN_POINT('Origin',(74.5283628290597,239.4,16.2213203435596)) ;
#69986 = CARTESIAN_POINT('',(79.9425790882848,241.985780790853,7.2786795888419)) ;
#69987 = CARTESIAN_POINT('',(79.9425790882848,241.985780790853,16.0213203435596)) ;
#69988 = CARTESIAN_POINT('',(79.8026999024823,242.26030915041,7.2786795888419)) ;
#69989 = CARTESIAN_POINT('Origin',(74.5283628290597,239.4,7.2786795888419)) ;
#69990 = CARTESIAN_POINT('',(79.8026999024823,242.26030915041,16.2213203435596)) ;
#69991 = CARTESIAN_POINT('',(79.8026999024823,242.26030915041,16.0213203435596)) ;
#69992 = CARTESIAN_POINT('',(78.8785382749251,243.532308506173,16.2213203435596)) ;
#69993 = CARTESIAN_POINT('Origin',(74.5283628290597,239.4,16.2213203435596)) ;
#69994 = CARTESIAN_POINT('',(78.8785382749251,243.532308506173,7.2786795888419)) ;
#69995 = CARTESIAN_POINT('',(78.8785382749251,243.532308506173,16.0213203435596)) ;
#69996 = CARTESIAN_POINT('',(78.6606713352326,243.750175445865,7.2786795888419)) ;
#69997 = CARTESIAN_POINT('Origin',(74.5283628290597,239.4,7.2786795888419)) ;
#69998 = CARTESIAN_POINT('',(78.6606713352326,243.750175445865,16.2213203435596)) ;
#69999 = CARTESIAN_POINT('',(78.6606713352326,243.750175445865,16.0213203435596)) ;
#70000 = CARTESIAN_POINT('',(77.3886719794696,244.674337073423,16.2213203435596)) ;
#70001 = CARTESIAN_POINT('Origin',(74.5283628290597,239.4,16.2213203435596)) ;
#70002 = CARTESIAN_POINT('',(77.3886719794696,244.674337073423,7.2786795888419)) ;
#70003 = CARTESIAN_POINT('',(77.3886719794696,244.674337073423,16.0213203435596)) ;
#70004 = CARTESIAN_POINT('',(77.1141436199123,244.814216259225,7.2786795888419)) ;
#70005 = CARTESIAN_POINT('Origin',(74.5283628290597,239.4,7.2786795888419)) ;
#70006 = CARTESIAN_POINT('',(77.1141436199123,244.814216259225,16.2213203435596)) ;
#70007 = CARTESIAN_POINT('',(77.1141436199123,244.814216259225,16.0213203435596)) ;
#70008 = CARTESIAN_POINT('',(75.6188186954263,245.300076779458,16.2213203435596)) ;
#70009 = CARTESIAN_POINT('Origin',(74.5283628290597,239.4,16.2213203435596)) ;
#70010 = CARTESIAN_POINT('',(75.6188186954263,245.300076779458,7.2786795888419)) ;
#70011 = CARTESIAN_POINT('',(75.6188186954263,245.300076779458,16.0213203435596)) ;
#70012 = CARTESIAN_POINT('',(75.3145016645892,245.348275862069,7.2786795888419)) ;
#70013 = CARTESIAN_POINT('Origin',(74.5283628290597,239.4,7.2786795888419)) ;
#70014 = CARTESIAN_POINT('',(75.3145016645892,245.348275862069,16.2213203435596)) ;
#70015 = CARTESIAN_POINT('',(75.3145016645892,245.348275862069,16.0213203435596)) ;
#70016 = CARTESIAN_POINT('',(73.7422239935302,245.348275862069,16.2213203435596)) ;
#70017 = CARTESIAN_POINT('Origin',(74.5283628290597,239.4,16.2213203435596)) ;
#70018 = CARTESIAN_POINT('',(73.7422239935302,245.348275862069,7.2786795888419)) ;
#70019 = CARTESIAN_POINT('',(73.7422239935302,245.348275862069,16.0213203435596)) ;
#70020 = CARTESIAN_POINT('',(73.4379069626931,245.300076779459,7.2786795888419)) ;
#70021 = CARTESIAN_POINT('Origin',(74.5283628290597,239.4,7.2786795888419)) ;
#70022 = CARTESIAN_POINT('',(73.4379069626931,245.300076779459,16.2213203435596)) ;
#70023 = CARTESIAN_POINT('',(73.4379069626931,245.300076779459,16.0213203435596)) ;
#70024 = CARTESIAN_POINT('',(71.9425820382071,244.814216259225,16.2213203435596)) ;
#70025 = CARTESIAN_POINT('Origin',(74.5283628290597,239.4,16.2213203435596)) ;
#70026 = CARTESIAN_POINT('',(71.9425820382071,244.814216259225,7.2786795888419)) ;
#70027 = CARTESIAN_POINT('',(71.9425820382071,244.814216259225,16.0213203435596)) ;
#70028 = CARTESIAN_POINT('',(71.6680536786498,244.674337073423,7.2786795888419)) ;
#70029 = CARTESIAN_POINT('Origin',(74.5283628290597,239.4,7.2786795888419)) ;
#70030 = CARTESIAN_POINT('',(71.6680536786498,244.674337073423,16.2213203435596)) ;
#70031 = CARTESIAN_POINT('',(71.6680536786498,244.674337073423,16.0213203435596)) ;
#70032 = CARTESIAN_POINT('',(70.3960543228867,243.750175445865,16.2213203435596)) ;
#70033 = CARTESIAN_POINT('Origin',(74.5283628290597,239.4,16.2213203435596)) ;
#70034 = CARTESIAN_POINT('',(70.3960543228867,243.750175445865,7.2786795888419)) ;
#70035 = CARTESIAN_POINT('',(70.3960543228867,243.750175445865,16.0213203435596)) ;
#70036 = CARTESIAN_POINT('',(70.1781873831942,243.532308506173,7.2786795888419)) ;
#70037 = CARTESIAN_POINT('Origin',(74.5283628290597,239.4,7.2786795888419)) ;
#70038 = CARTESIAN_POINT('',(70.1781873831942,243.532308506173,16.2213203435596)) ;
#70039 = CARTESIAN_POINT('',(70.1781873831942,243.532308506173,16.0213203435596)) ;
#70040 = CARTESIAN_POINT('',(69.254025755637,242.26030915041,16.2213203435596)) ;
#70041 = CARTESIAN_POINT('Origin',(74.5283628290597,239.4,16.2213203435596)) ;
#70042 = CARTESIAN_POINT('',(69.254025755637,242.26030915041,7.2786795888419)) ;
#70043 = CARTESIAN_POINT('',(69.254025755637,242.26030915041,16.0213203435596)) ;
#70044 = CARTESIAN_POINT('',(69.1141465698346,241.985780790853,7.2786795888419)) ;
#70045 = CARTESIAN_POINT('Origin',(74.5283628290597,239.4,7.2786795888419)) ;
#70046 = CARTESIAN_POINT('',(69.1141465698346,241.985780790853,16.2213203435596)) ;
#70047 = CARTESIAN_POINT('',(69.1141465698346,241.985780790853,16.0213203435596)) ;
#70048 = CARTESIAN_POINT('',(68.6282860496011,240.490455866366,16.2213203435596)) ;
#70049 = CARTESIAN_POINT('Origin',(74.5283628290597,239.4,16.2213203435596)) ;
#70050 = CARTESIAN_POINT('',(68.6282860496011,240.490455866367,7.2786795888419)) ;
#70051 = CARTESIAN_POINT('',(68.6282860496011,240.490455866367,16.0213203435596)) ;
#70052 = CARTESIAN_POINT('',(68.5800869669907,240.186138835529,7.2786795888419)) ;
#70053 = CARTESIAN_POINT('Origin',(74.5283628290597,239.4,7.2786795888419)) ;
#70054 = CARTESIAN_POINT('',(68.5800869669907,240.186138835529,16.2213203435596)) ;
#70055 = CARTESIAN_POINT('',(68.5800869669907,240.186138835529,16.0213203435596)) ;
#70056 = CARTESIAN_POINT('Origin',(74.5283628290597,239.4,16.2213203435596)) ;
#70057 = CARTESIAN_POINT('Origin',(74.5283628290597,239.4,18.5213203435596)) ;
#70058 = CARTESIAN_POINT('Origin',(77.8283628290598,239.7,10.8213203435596)) ;
#70059 = CARTESIAN_POINT('',(78.0283628290598,239.,10.8213203435596)) ;
#70060 = CARTESIAN_POINT('',(77.8283628290598,239.,11.0213203435596)) ;
#70061 = CARTESIAN_POINT('Origin',(77.8283628290598,239.,10.8213203435596)) ;
#70062 = CARTESIAN_POINT('',(77.8283628290598,239.8,11.0213203435596)) ;
#70063 = CARTESIAN_POINT('',(77.8283628290598,239.7,11.0213203435596)) ;
#70064 = CARTESIAN_POINT('',(78.0283628290598,239.8,10.8213203435596)) ;
#70065 = CARTESIAN_POINT('Origin',(77.8283628290598,239.8,10.8213203435596)) ;
#70066 = CARTESIAN_POINT('',(78.0283628290598,239.7,10.8213203435596)) ;
#70067 = CARTESIAN_POINT('Origin',(74.9283628290597,239.1,10.8213203435596)) ;
#70068 = CARTESIAN_POINT('',(75.1283628290597,236.1,10.8213203435596)) ;
#70069 = CARTESIAN_POINT('',(74.9283628290597,236.1,11.0213203435596)) ;
#70070 = CARTESIAN_POINT('Origin',(74.9283628290597,236.1,10.8213203435596)) ;
#70071 = CARTESIAN_POINT('',(74.9283628290597,237.85,11.0213203435596)) ;
#70072 = CARTESIAN_POINT('',(74.9283628290597,239.1,11.0213203435596)) ;
#70073 = CARTESIAN_POINT('',(75.1283628290597,237.85,10.8213203435596)) ;
#70074 = CARTESIAN_POINT('Origin',(74.9283628290597,237.85,10.8213203435596)) ;
#70075 = CARTESIAN_POINT('',(75.1283628290597,239.1,10.8213203435596)) ;
#70076 = CARTESIAN_POINT('Origin',(76.0783628290597,237.85,10.8213203435596)) ;
#70077 = CARTESIAN_POINT('',(76.0783628290597,239.,11.0213203435596)) ;
#70078 = CARTESIAN_POINT('',(76.0783628290597,238.8,10.8213203435596)) ;
#70079 = CARTESIAN_POINT('Origin',(76.0783628290597,239.,10.8213203435596)) ;
#70080 = CARTESIAN_POINT('Origin',(76.0783628290597,237.85,10.8213203435596)) ;
#70081 = CARTESIAN_POINT('Origin',(76.0783628290597,237.85,11.0213203435596)) ;
#70082 = CARTESIAN_POINT('Origin',(76.2783628290598,239.,10.8213203435596)) ;
#70083 = CARTESIAN_POINT('',(77.8283628290598,238.8,10.8213203435596)) ;
#70084 = CARTESIAN_POINT('Origin',(77.8283628290598,239.,10.8213203435596)) ;
#70085 = CARTESIAN_POINT('',(76.2783628290598,238.8,10.8213203435596)) ;
#70086 = CARTESIAN_POINT('',(76.2783628290598,239.,11.0213203435596)) ;
#70087 = CARTESIAN_POINT('Origin',(74.8283628290597,236.1,10.8213203435596)) ;
#70088 = CARTESIAN_POINT('',(74.1283628290597,235.9,10.8213203435596)) ;
#70089 = CARTESIAN_POINT('',(74.1283628290597,236.1,11.0213203435596)) ;
#70090 = CARTESIAN_POINT('Origin',(74.1283628290597,236.1,10.8213203435596)) ;
#70091 = CARTESIAN_POINT('',(74.8283628290597,236.1,11.0213203435596)) ;
#70092 = CARTESIAN_POINT('',(74.9283628290597,235.9,10.8213203435596)) ;
#70093 = CARTESIAN_POINT('Origin',(74.9283628290597,236.1,10.8213203435596)) ;
#70094 = CARTESIAN_POINT('',(74.8283628290598,235.9,10.8213203435596)) ;
#70095 = CARTESIAN_POINT('Origin',(74.2283628290597,239.,10.8213203435596)) ;
#70096 = CARTESIAN_POINT('',(71.2283628290597,238.8,10.8213203435596)) ;
#70097 = CARTESIAN_POINT('',(71.2283628290597,239.,11.0213203435596)) ;
#70098 = CARTESIAN_POINT('Origin',(71.2283628290597,239.,10.8213203435596)) ;
#70099 = CARTESIAN_POINT('',(72.9783628290596,239.,11.0213203435596)) ;
#70100 = CARTESIAN_POINT('',(74.2283628290597,239.,11.0213203435596)) ;
#70101 = CARTESIAN_POINT('',(72.9783628290596,238.8,10.8213203435596)) ;
#70102 = CARTESIAN_POINT('Origin',(72.9783628290596,239.,10.8213203435596)) ;
#70103 = CARTESIAN_POINT('',(74.2283628290597,238.8,10.8213203435596)) ;
#70104 = CARTESIAN_POINT('Origin',(72.9783628290596,237.85,10.8213203435596)) ;
#70105 = CARTESIAN_POINT('',(74.1283628290597,237.85,11.0213203435596)) ;
#70106 = CARTESIAN_POINT('',(73.9283628290597,237.85,10.8213203435596)) ;
#70107 = CARTESIAN_POINT('Origin',(74.1283628290597,237.85,10.8213203435596)) ;
#70108 = CARTESIAN_POINT('Origin',(72.9783628290596,237.85,10.8213203435596)) ;
#70109 = CARTESIAN_POINT('Origin',(72.9783628290596,237.85,11.0213203435596)) ;
#70110 = CARTESIAN_POINT('Origin',(74.1283628290597,237.65,10.8213203435596)) ;
#70111 = CARTESIAN_POINT('',(73.9283628290597,236.1,10.8213203435596)) ;
#70112 = CARTESIAN_POINT('Origin',(74.1283628290597,236.1,10.8213203435596)) ;
#70113 = CARTESIAN_POINT('',(73.9283628290597,237.65,10.8213203435596)) ;
#70114 = CARTESIAN_POINT('',(74.1283628290597,237.65,11.0213203435596)) ;
#70115 = CARTESIAN_POINT('Origin',(71.2283628290597,239.1,10.8213203435596)) ;
#70116 = CARTESIAN_POINT('',(71.0283628290598,239.8,10.8213203435596)) ;
#70117 = CARTESIAN_POINT('',(71.2283628290598,239.8,11.0213203435596)) ;
#70118 = CARTESIAN_POINT('Origin',(71.2283628290598,239.8,10.8213203435596)) ;
#70119 = CARTESIAN_POINT('',(71.2283628290597,239.1,11.0213203435596)) ;
#70120 = CARTESIAN_POINT('',(71.0283628290597,239.,10.8213203435596)) ;
#70121 = CARTESIAN_POINT('Origin',(71.2283628290597,239.,10.8213203435596)) ;
#70122 = CARTESIAN_POINT('',(71.0283628290597,239.1,10.8213203435596)) ;
#70123 = CARTESIAN_POINT('Origin',(74.1283628290597,239.7,10.8213203435596)) ;
#70124 = CARTESIAN_POINT('',(73.9283628290597,242.7,10.8213203435596)) ;
#70125 = CARTESIAN_POINT('',(74.1283628290597,242.7,11.0213203435596)) ;
#70126 = CARTESIAN_POINT('Origin',(74.1283628290597,242.7,10.8213203435596)) ;
#70127 = CARTESIAN_POINT('',(74.1283628290597,240.95,11.0213203435596)) ;
#70128 = CARTESIAN_POINT('',(74.1283628290597,239.7,11.0213203435596)) ;
#70129 = CARTESIAN_POINT('',(73.9283628290597,240.95,10.8213203435596)) ;
#70130 = CARTESIAN_POINT('Origin',(74.1283628290597,240.95,10.8213203435596)) ;
#70131 = CARTESIAN_POINT('',(73.9283628290597,239.7,10.8213203435596)) ;
#70132 = CARTESIAN_POINT('Origin',(72.9783628290596,240.95,10.8213203435596)) ;
#70133 = CARTESIAN_POINT('',(72.9783628290596,239.8,11.0213203435596)) ;
#70134 = CARTESIAN_POINT('',(72.9783628290596,240.,10.8213203435596)) ;
#70135 = CARTESIAN_POINT('Origin',(72.9783628290596,239.8,10.8213203435596)) ;
#70136 = CARTESIAN_POINT('Origin',(72.9783628290596,240.95,10.8213203435596)) ;
#70137 = CARTESIAN_POINT('Origin',(72.9783628290596,240.95,11.0213203435596)) ;
#70138 = CARTESIAN_POINT('Origin',(72.7783628290598,239.8,10.8213203435596)) ;
#70139 = CARTESIAN_POINT('',(71.2283628290598,240.,10.8213203435596)) ;
#70140 = CARTESIAN_POINT('Origin',(71.2283628290598,239.8,10.8213203435596)) ;
#70141 = CARTESIAN_POINT('',(72.7783628290598,240.,10.8213203435596)) ;
#70142 = CARTESIAN_POINT('',(72.7783628290598,239.8,11.0213203435596)) ;
#70143 = CARTESIAN_POINT('Origin',(74.2283628290597,242.7,10.8213203435596)) ;
#70144 = CARTESIAN_POINT('',(74.9283628290597,242.9,10.8213203435596)) ;
#70145 = CARTESIAN_POINT('',(74.9283628290597,242.7,11.0213203435596)) ;
#70146 = CARTESIAN_POINT('Origin',(74.9283628290597,242.7,10.8213203435596)) ;
#70147 = CARTESIAN_POINT('',(74.2283628290597,242.7,11.0213203435596)) ;
#70148 = CARTESIAN_POINT('',(74.1283628290597,242.9,10.8213203435596)) ;
#70149 = CARTESIAN_POINT('Origin',(74.1283628290597,242.7,10.8213203435596)) ;
#70150 = CARTESIAN_POINT('',(74.2283628290597,242.9,10.8213203435596)) ;
#70151 = CARTESIAN_POINT('Origin',(76.0783628290596,240.95,10.8213203435596)) ;
#70152 = CARTESIAN_POINT('',(76.0783628290596,240.,10.8213203435596)) ;
#70153 = CARTESIAN_POINT('',(76.0783628290596,239.8,11.0213203435596)) ;
#70154 = CARTESIAN_POINT('Origin',(76.0783628290596,239.8,10.8213203435596)) ;
#70155 = CARTESIAN_POINT('',(74.9283628290596,240.95,11.0213203435596)) ;
#70156 = CARTESIAN_POINT('Origin',(76.0783628290596,240.95,11.0213203435596)) ;
#70157 = CARTESIAN_POINT('',(75.1283628290596,240.95,10.8213203435596)) ;
#70158 = CARTESIAN_POINT('Origin',(74.9283628290596,240.95,10.8213203435596)) ;
#70159 = CARTESIAN_POINT('Origin',(76.0783628290596,240.95,10.8213203435596)) ;
#70160 = CARTESIAN_POINT('Origin',(74.9283628290597,241.15,10.8213203435596)) ;
#70161 = CARTESIAN_POINT('',(75.1283628290596,242.7,10.8213203435596)) ;
#70162 = CARTESIAN_POINT('Origin',(74.9283628290597,242.7,10.8213203435596)) ;
#70163 = CARTESIAN_POINT('',(75.1283628290596,241.15,10.8213203435596)) ;
#70164 = CARTESIAN_POINT('',(74.9283628290597,241.15,11.0213203435596)) ;
#70165 = CARTESIAN_POINT('Origin',(74.8283628290597,239.8,10.8213203435596)) ;
#70166 = CARTESIAN_POINT('',(77.8283628290598,240.,10.8213203435596)) ;
#70167 = CARTESIAN_POINT('Origin',(77.8283628290598,239.8,10.8213203435596)) ;
#70168 = CARTESIAN_POINT('',(74.8283628290597,239.8,11.0213203435596)) ;
#70169 = CARTESIAN_POINT('',(74.8283628290597,240.,10.8213203435596)) ;
#70170 = CARTESIAN_POINT('Origin',(74.9283628290597,242.7,10.8213203435596)) ;
#70171 = CARTESIAN_POINT('Origin',(74.9283628290597,242.7,10.8213203435596)) ;
#70172 = CARTESIAN_POINT('Origin',(74.1283628290597,242.7,10.8213203435596)) ;
#70173 = CARTESIAN_POINT('Origin',(74.1283628290597,242.7,10.8213203435596)) ;
#70174 = CARTESIAN_POINT('Origin',(71.2283628290598,239.8,10.8213203435596)) ;
#70175 = CARTESIAN_POINT('Origin',(71.2283628290598,239.8,10.8213203435596)) ;
#70176 = CARTESIAN_POINT('Origin',(71.2283628290597,239.,10.8213203435596)) ;
#70177 = CARTESIAN_POINT('Origin',(71.2283628290597,239.,10.8213203435596)) ;
#70178 = CARTESIAN_POINT('Origin',(74.1283628290597,236.1,10.8213203435596)) ;
#70179 = CARTESIAN_POINT('Origin',(74.1283628290597,236.1,10.8213203435596)) ;
#70180 = CARTESIAN_POINT('Origin',(74.9283628290597,236.1,10.8213203435596)) ;
#70181 = CARTESIAN_POINT('Origin',(74.9283628290597,236.1,10.8213203435596)) ;
#70182 = CARTESIAN_POINT('Origin',(77.8283628290598,239.,10.8213203435596)) ;
#70183 = CARTESIAN_POINT('Origin',(77.8283628290598,239.,10.8213203435596)) ;
#70184 = CARTESIAN_POINT('Origin',(77.8283628290598,239.8,10.8213203435596)) ;
#70185 = CARTESIAN_POINT('Origin',(77.8283628290598,239.8,10.8213203435596)) ;
#70186 = CARTESIAN_POINT('Origin',(73.9283628290597,235.9,11.0213203435596)) ;
#70187 = CARTESIAN_POINT('',(73.9283628290597,236.1,6.22132034355964)) ;
#70188 = CARTESIAN_POINT('',(73.9283628290597,236.1,11.0213203435596)) ;
#70189 = CARTESIAN_POINT('',(73.9283628290597,237.85,6.22132034355964)) ;
#70190 = CARTESIAN_POINT('',(73.9283628290597,237.65,6.22132034355964)) ;
#70191 = CARTESIAN_POINT('',(73.9283628290597,237.85,11.0213203435596)) ;
#70192 = CARTESIAN_POINT('Origin',(74.1283628290597,236.1,11.0213203435596)) ;
#70193 = CARTESIAN_POINT('',(74.1283628290597,235.9,6.22132034355964)) ;
#70194 = CARTESIAN_POINT('',(74.1283628290597,235.9,11.0213203435596)) ;
#70195 = CARTESIAN_POINT('Origin',(74.1283628290597,236.1,6.22132034355964)) ;
#70196 = CARTESIAN_POINT('Origin',(75.1283628290597,235.9,11.0213203435596)) ;
#70197 = CARTESIAN_POINT('',(74.9283628290597,235.9,6.22132034355964)) ;
#70198 = CARTESIAN_POINT('',(74.9283628290597,235.9,11.0213203435596)) ;
#70199 = CARTESIAN_POINT('',(74.8283628290597,235.9,6.22132034355964)) ;
#70200 = CARTESIAN_POINT('Origin',(74.9283628290597,236.1,11.0213203435596)) ;
#70201 = CARTESIAN_POINT('',(75.1283628290597,236.1,6.22132034355964)) ;
#70202 = CARTESIAN_POINT('',(75.1283628290597,236.1,11.0213203435596)) ;
#70203 = CARTESIAN_POINT('Origin',(74.9283628290597,236.1,6.22132034355964)) ;
#70204 = CARTESIAN_POINT('Origin',(75.1283628290597,238.8,11.0213203435596)) ;
#70205 = CARTESIAN_POINT('',(75.1283628290597,237.85,6.22132034355964)) ;
#70206 = CARTESIAN_POINT('',(75.1283628290597,237.85,11.0213203435596)) ;
#70207 = CARTESIAN_POINT('',(75.1283628290597,239.1,6.22132034355964)) ;
#70208 = CARTESIAN_POINT('Origin',(76.0783628290597,237.85,11.0213203435596)) ;
#70209 = CARTESIAN_POINT('',(76.0783628290597,238.8,6.22132034355964)) ;
#70210 = CARTESIAN_POINT('',(76.0783628290597,238.8,11.0213203435596)) ;
#70211 = CARTESIAN_POINT('Origin',(76.0783628290597,237.85,6.22132034355964)) ;
#70212 = CARTESIAN_POINT('Origin',(78.0283628290598,238.8,11.0213203435596)) ;
#70213 = CARTESIAN_POINT('',(77.8283628290598,238.8,6.22132034355964)) ;
#70214 = CARTESIAN_POINT('',(77.8283628290598,238.8,11.0213203435596)) ;
#70215 = CARTESIAN_POINT('',(76.2783628290597,238.8,6.22132034355964)) ;
#70216 = CARTESIAN_POINT('Origin',(77.8283628290598,239.,11.0213203435596)) ;
#70217 = CARTESIAN_POINT('',(78.0283628290598,239.,6.22132034355964)) ;
#70218 = CARTESIAN_POINT('',(78.0283628290598,239.,11.0213203435596)) ;
#70219 = CARTESIAN_POINT('Origin',(77.8283628290598,239.,6.22132034355964)) ;
#70220 = CARTESIAN_POINT('Origin',(78.0283628290598,240.,11.0213203435596)) ;
#70221 = CARTESIAN_POINT('',(78.0283628290598,239.8,6.22132034355964)) ;
#70222 = CARTESIAN_POINT('',(78.0283628290598,239.8,11.0213203435596)) ;
#70223 = CARTESIAN_POINT('',(78.0283628290598,239.7,6.22132034355964)) ;
#70224 = CARTESIAN_POINT('Origin',(77.8283628290598,239.8,11.0213203435596)) ;
#70225 = CARTESIAN_POINT('',(77.8283628290598,240.,6.22132034355964)) ;
#70226 = CARTESIAN_POINT('',(77.8283628290598,240.,11.0213203435596)) ;
#70227 = CARTESIAN_POINT('Origin',(77.8283628290598,239.8,6.22132034355964)) ;
#70228 = CARTESIAN_POINT('Origin',(75.1283628290596,240.,11.0213203435596)) ;
#70229 = CARTESIAN_POINT('',(76.0783628290596,240.,6.22132034355964)) ;
#70230 = CARTESIAN_POINT('',(76.0783628290596,240.,11.0213203435596)) ;
#70231 = CARTESIAN_POINT('',(74.8283628290597,240.,6.22132034355964)) ;
#70232 = CARTESIAN_POINT('Origin',(76.0783628290596,240.95,11.0213203435596)) ;
#70233 = CARTESIAN_POINT('',(75.1283628290596,240.95,6.22132034355964)) ;
#70234 = CARTESIAN_POINT('',(75.1283628290596,240.95,11.0213203435596)) ;
#70235 = CARTESIAN_POINT('Origin',(76.0783628290596,240.95,6.22132034355964)) ;
#70236 = CARTESIAN_POINT('Origin',(74.5283628290598,239.4,11.0213203435596)) ;
#70237 = CARTESIAN_POINT('Origin',(72.0287747312354,244.633742383918,7.27867958884205)) ;
#70238 = CARTESIAN_POINT('',(72.1901462641302,244.751891562379,7.27867958883792)) ;
#70239 = CARTESIAN_POINT('Origin',(72.0287747312355,244.633742383918,7.27867958883752)) ;
#70240 = CARTESIAN_POINT('',(71.9556834737297,244.786783924095,7.17267980084126)) ;
#70241 = CARTESIAN_POINT('Origin',(72.0287747312354,244.633742383918,7.27867958884205)) ;
#70242 = CARTESIAN_POINT('Origin',(72.0287747312355,244.633742383918,7.2786795888419)) ;
#70243 = CARTESIAN_POINT('Origin',(73.474255491572,245.103407553477,7.2786795888419)) ;
#70244 = CARTESIAN_POINT('',(73.2742568343815,245.10414043955,7.27867958883757)) ;
#70245 = CARTESIAN_POINT('Origin',(73.474255491572,245.103407553477,7.2786795888419)) ;
#70246 = CARTESIAN_POINT('',(73.4434320007296,245.270182723559,7.17267980084145)) ;
#70247 = CARTESIAN_POINT('Origin',(73.474255491572,245.103407553477,7.2786795888419)) ;
#70248 = CARTESIAN_POINT('Origin',(73.474255491572,245.103407553474,7.27867958883797)) ;
#70249 = CARTESIAN_POINT('Origin',(71.7633973169968,244.498525837642,7.2786795888419)) ;
#70250 = CARTESIAN_POINT('',(71.5729608165738,244.437419869794,7.27867958883749)) ;
#70251 = CARTESIAN_POINT('Origin',(71.7633973169968,244.498525837642,7.2786795888419)) ;
#70252 = CARTESIAN_POINT('',(71.6825460733808,244.647613467409,7.17267980084143)) ;
#70253 = CARTESIAN_POINT('Origin',(71.7633973169968,244.498525837642,7.2786795888419)) ;
#70254 = CARTESIAN_POINT('Origin',(71.7633973169975,244.498525837639,7.2786795888379)) ;
#70255 = CARTESIAN_POINT('Origin',(74.5283628290597,239.4,7.2786795888419)) ;
#70256 = CARTESIAN_POINT('Origin',(74.5283628290597,239.4,7.17267980084126)) ;
#70257 = CARTESIAN_POINT('Origin',(73.7684286213811,245.15,7.27867958884205)) ;
#70258 = CARTESIAN_POINT('',(73.9584121733014,245.212499999998,7.27867958883793)) ;
#70259 = CARTESIAN_POINT('Origin',(73.7684286213812,245.15,7.2786795888375)) ;
#70260 = CARTESIAN_POINT('',(73.7462071414064,245.31813759476,7.17267980084126)) ;
#70261 = CARTESIAN_POINT('Origin',(73.7684286213811,245.15,7.27867958884205)) ;
#70262 = CARTESIAN_POINT('Origin',(73.7684286213811,245.15,7.2786795888419)) ;
#70263 = CARTESIAN_POINT('Origin',(70.5337979397465,243.605169597679,7.27867958886637)) ;
#70264 = CARTESIAN_POINT('',(70.6507612838972,243.767402689633,7.27867958819172)) ;
#70265 = CARTESIAN_POINT('Origin',(70.5337979397592,243.60516959767,7.2786795881253)) ;
#70266 = CARTESIAN_POINT('',(70.4169915862605,243.728134311007,7.17267980084127)) ;
#70267 = CARTESIAN_POINT('Origin',(70.5337979397465,243.605169597679,7.27867958886637)) ;
#70268 = CARTESIAN_POINT('Origin',(70.5337979397592,243.60516959767,7.2786795888419)) ;
#70269 = CARTESIAN_POINT('Ctrl Pts',(70.6501568829842,243.767838986024,7.28037086445601)) ;
#70270 = CARTESIAN_POINT('Ctrl Pts',(70.695018761352,243.735411937294,7.16429143740118)) ;
#70271 = CARTESIAN_POINT('Ctrl Pts',(70.7949584384066,243.681786355863,6.93457499380776)) ;
#70272 = CARTESIAN_POINT('Ctrl Pts',(70.9495221917943,243.649443421145,6.66101676411208)) ;
#70273 = CARTESIAN_POINT('Ctrl Pts',(71.0970424533863,243.657858652391,6.46925478973694)) ;
#70274 = CARTESIAN_POINT('Ctrl Pts',(71.2015317828535,243.685094051328,6.37321776533927)) ;
#70275 = CARTESIAN_POINT('Ctrl Pts',(71.2899862061965,243.726262429777,6.32731112524896)) ;
#70276 = CARTESIAN_POINT('Ctrl Pts',(71.3551880178236,243.767424556722,6.31493581996192)) ;
#70277 = CARTESIAN_POINT('Ctrl Pts',(71.414511662802,243.816727035925,6.32729394384689)) ;
#70278 = CARTESIAN_POINT('Ctrl Pts',(71.4809943478713,243.888111400172,6.37316824150563)) ;
#70279 = CARTESIAN_POINT('Ctrl Pts',(71.5392090359803,243.979129806174,6.469294125934)) ;
#70280 = CARTESIAN_POINT('Ctrl Pts',(71.5928225191086,244.116852003807,6.66106251922067)) ;
#70281 = CARTESIAN_POINT('Ctrl Pts',(71.609820551523,244.273797881523,6.93454059478913)) ;
#70282 = CARTESIAN_POINT('Ctrl Pts',(71.5897065079004,244.385452427618,7.16431248483623)) ;
#70283 = CARTESIAN_POINT('Ctrl Pts',(71.572732687827,244.438129374609,7.28037056287155)) ;
#70284 = CARTESIAN_POINT('Ctrl Pts',(70.6133143716979,243.794496370374,7.25145480381165)) ;
#70285 = CARTESIAN_POINT('Ctrl Pts',(70.6579201115597,243.756943743429,7.13666531376885)) ;
#70286 = CARTESIAN_POINT('Ctrl Pts',(70.759669756855,243.693403731017,6.90913510331608)) ;
#70287 = CARTESIAN_POINT('Ctrl Pts',(70.9218627556374,243.650786986153,6.63763508188674)) ;
#70288 = CARTESIAN_POINT('Ctrl Pts',(71.079042730125,243.654281538889,6.44713797226046)) ;
#70289 = CARTESIAN_POINT('Ctrl Pts',(71.190989976115,243.680725469535,6.35168754197124)) ;
#70290 = CARTESIAN_POINT('Ctrl Pts',(71.2857727915241,243.723478511816,6.30605227260946)) ;
#70291 = CARTESIAN_POINT('Ctrl Pts',(71.3554410054417,243.767068640434,6.2937492054939)) ;
#70292 = CARTESIAN_POINT('Ctrl Pts',(71.4184657724347,243.819875939003,6.30603519484955)) ;
#70293 = CARTESIAN_POINT('Ctrl Pts',(71.4884050005537,243.896782573748,6.35163826841188)) ;
#70294 = CARTESIAN_POINT('Ctrl Pts',(71.5481929415663,243.99516005771,6.44717720448016)) ;
#70295 = CARTESIAN_POINT('Ctrl Pts',(71.6000835672938,244.143570042457,6.63768049386459)) ;
#70296 = CARTESIAN_POINT('Ctrl Pts',(71.6096864560401,244.310955271312,6.90910115397914)) ;
#70297 = CARTESIAN_POINT('Ctrl Pts',(71.5806917188778,244.427389248978,7.13668612730514)) ;
#70298 = CARTESIAN_POINT('Ctrl Pts',(71.5587649839846,244.481406266543,7.25145450557636)) ;
#70299 = CARTESIAN_POINT('Ctrl Pts',(70.5257088411162,243.808149962819,7.20122603502762)) ;
#70300 = CARTESIAN_POINT('Ctrl Pts',(70.575768050217,243.76371921269,7.08852834828282)) ;
#70301 = CARTESIAN_POINT('Ctrl Pts',(70.6900507860591,243.688214812907,6.86460074648092)) ;
#70302 = CARTESIAN_POINT('Ctrl Pts',(70.8726290515606,243.636494804644,6.59656897970077)) ;
#70303 = CARTESIAN_POINT('Ctrl Pts',(71.0492486924007,243.637943299584,6.40823334015557)) ;
#70304 = CARTESIAN_POINT('Ctrl Pts',(71.1748856832364,243.666416799429,6.31379313877718)) ;
#70305 = CARTESIAN_POINT('Ctrl Pts',(71.2810357577914,243.713684729473,6.26862706307453)) ;
#70306 = CARTESIAN_POINT('Ctrl Pts',(71.3589348514346,243.762249702892,6.25644899326161)) ;
#70307 = CARTESIAN_POINT('Ctrl Pts',(71.4292274030523,243.821341305003,6.26861012760492)) ;
#70308 = CARTESIAN_POINT('Ctrl Pts',(71.5069799006174,243.907665972781,6.3137443011777)) ;
#70309 = CARTESIAN_POINT('Ctrl Pts',(71.5729076291523,244.018427912558,6.40827217011468)) ;
#70310 = CARTESIAN_POINT('Ctrl Pts',(71.6288977778067,244.185986520421,6.59661403907028)) ;
#70311 = CARTESIAN_POINT('Ctrl Pts',(71.6361239251143,244.375552037511,6.86456746639935)) ;
#70312 = CARTESIAN_POINT('Ctrl Pts',(71.5996334283149,244.507615608175,7.0885487827586)) ;
#70313 = CARTESIAN_POINT('Ctrl Pts',(71.5728512558348,244.568943250038,7.20122574222209)) ;
#70314 = CARTESIAN_POINT('Ctrl Pts',(70.4438236562226,243.75797324979,7.17772391322105)) ;
#70315 = CARTESIAN_POINT('Ctrl Pts',(70.5015563262582,243.71393505825,7.06321986768199)) ;
#70316 = CARTESIAN_POINT('Ctrl Pts',(70.631018084871,243.640737186515,6.83627960612169)) ;
#70317 = CARTESIAN_POINT('Ctrl Pts',(70.8333007271835,243.595570389089,6.56550158124689)) ;
#70318 = CARTESIAN_POINT('Ctrl Pts',(71.0274438557767,243.6052704527,6.37551287208947)) ;
#70319 = CARTESIAN_POINT('Ctrl Pts',(71.1653543352155,243.640682678267,6.28031724281592)) ;
#70320 = CARTESIAN_POINT('Ctrl Pts',(71.2822399569048,243.694858370743,6.23480374698507)) ;
#70321 = CARTESIAN_POINT('Ctrl Pts',(71.3684114405816,243.749198508394,6.22253350040122)) ;
#70322 = CARTESIAN_POINT('Ctrl Pts',(71.4467557829302,243.814374864135,6.23478671054199)) ;
#70323 = CARTESIAN_POINT('Ctrl Pts',(71.5343942575121,243.908773769962,6.28026810039496)) ;
#70324 = CARTESIAN_POINT('Ctrl Pts',(71.6107180544398,244.029068327693,6.37555197849753)) ;
#70325 = CARTESIAN_POINT('Ctrl Pts',(71.6799733584262,244.210745485926,6.56554689303006)) ;
#70326 = CARTESIAN_POINT('Ctrl Pts',(71.6995177608991,244.417020600932,6.83624573656735)) ;
#70327 = CARTESIAN_POINT('Ctrl Pts',(71.6699141621299,244.562812309387,7.06324062946311)) ;
#70328 = CARTESIAN_POINT('Ctrl Pts',(71.6458760522509,244.631315212985,7.17772361572752)) ;
#70329 = CARTESIAN_POINT('Ctrl Pts',(70.4161308161459,243.728748828007,7.17434119724341)) ;
#70330 = CARTESIAN_POINT('Ctrl Pts',(70.4762342283297,243.685779217861,7.05826310306117)) ;
#70331 = CARTESIAN_POINT('Ctrl Pts',(70.6105145005683,243.615236269817,6.82854891848138)) ;
#70332 = CARTESIAN_POINT('Ctrl Pts',(70.8194164063599,243.574668856811,6.554992815528)) ;
#70333 = CARTESIAN_POINT('Ctrl Pts',(71.0198900905357,243.589126800135,6.36323214814111)) ;
#70334 = CARTESIAN_POINT('Ctrl Pts',(71.162493478287,243.628114813195,6.26719572987436)) ;
#70335 = CARTESIAN_POINT('Ctrl Pts',(71.2837091433123,243.685533784822,6.22128937019327)) ;
#70336 = CARTESIAN_POINT('Ctrl Pts',(71.3733381280523,243.742414020762,6.20891413955045)) ;
#70337 = CARTESIAN_POINT('Ctrl Pts',(71.4551693674424,243.810095751249,6.22127218889828)) ;
#70338 = CARTESIAN_POINT('Ctrl Pts',(71.5472287971451,243.907609473381,6.26714620629932)) ;
#70339 = CARTESIAN_POINT('Ctrl Pts',(71.6284090431722,244.031265917727,6.36327148423066)) ;
#70340 = CARTESIAN_POINT('Ctrl Pts',(71.7041419702003,244.217490856572,6.55503857028213)) ;
#70341 = CARTESIAN_POINT('Ctrl Pts',(71.7301069186013,244.428640448521,6.82851451992736)) ;
#70342 = CARTESIAN_POINT('Ctrl Pts',(71.704517229436,244.578194768653,7.05828415025454)) ;
#70343 = CARTESIAN_POINT('Ctrl Pts',(71.6822276827102,244.648621821033,7.17434089566242)) ;
#70344 = CARTESIAN_POINT('Ctrl Pts',(71.6825460733808,244.647613467409,7.17267980084144)) ;
#70345 = CARTESIAN_POINT('Ctrl Pts',(71.6935886426337,244.612559352449,7.11495383284403)) ;
#70346 = CARTESIAN_POINT('Ctrl Pts',(71.7022927623503,244.576361719043,7.05741591593104)) ;
#70347 = CARTESIAN_POINT('Ctrl Pts',(71.7083791693549,244.538999323656,7.00033196889614)) ;
#70348 = CARTESIAN_POINT('Ctrl Pts',(71.7126272417874,244.512921842846,6.96048962158692)) ;
#70349 = CARTESIAN_POINT('Ctrl Pts',(71.715600317724,244.486277068799,6.92086843822223)) ;
#70350 = CARTESIAN_POINT('Ctrl Pts',(71.7172074984982,244.459059598684,6.88155816675306)) ;
#70351 = CARTESIAN_POINT('Ctrl Pts',(71.7179029988757,244.447281358772,6.86454682049581)) ;
#70352 = CARTESIAN_POINT('Ctrl Pts',(71.7183428322704,244.435395593456,6.84759321077135)) ;
#70353 = CARTESIAN_POINT('Ctrl Pts',(71.7185197039289,244.423398003082,6.83069915794562)) ;
#70354 = CARTESIAN_POINT('Ctrl Pts',(71.7195612719805,244.352746170378,6.73121286472363)) ;
#70355 = CARTESIAN_POINT('Ctrl Pts',(71.711478526729,244.278245478875,6.633836781897)) ;
#70356 = CARTESIAN_POINT('Ctrl Pts',(71.6894930170596,244.199202524374,6.54295091299619)) ;
#70357 = CARTESIAN_POINT('Ctrl Pts',(71.6867556442851,244.189361040827,6.53163489135909)) ;
#70358 = CARTESIAN_POINT('Ctrl Pts',(71.6838028080864,244.179449163839,6.52041945932379)) ;
#70359 = CARTESIAN_POINT('Ctrl Pts',(71.6806253447614,244.169465574853,6.5093130441619)) ;
#70360 = CARTESIAN_POINT('Ctrl Pts',(71.6727462032902,244.144709314288,6.4817725165935)) ;
#70361 = CARTESIAN_POINT('Ctrl Pts',(71.6634872275843,244.119517200743,6.45490825271367)) ;
#70362 = CARTESIAN_POINT('Ctrl Pts',(71.6524916152515,244.093896418644,6.42914051265344)) ;
#70363 = CARTESIAN_POINT('Ctrl Pts',(71.6434485774699,244.072825313779,6.40794854627107)) ;
#70364 = CARTESIAN_POINT('Ctrl Pts',(71.6332306941195,244.051463461098,6.38749730975455)) ;
#70365 = CARTESIAN_POINT('Ctrl Pts',(71.6216396098452,244.029812746213,6.36801731440074)) ;
#70366 = CARTESIAN_POINT('Ctrl Pts',(71.6143706676241,244.016235259257,6.35580111811206)) ;
#70367 = CARTESIAN_POINT('Ctrl Pts',(71.6065616958071,244.002544178426,6.34396688159399)) ;
#70368 = CARTESIAN_POINT('Ctrl Pts',(71.5981620367324,243.988783067631,6.33264057742806)) ;
#70369 = CARTESIAN_POINT('Ctrl Pts',(71.5925581358654,243.979602230643,6.32508414148572)) ;
#70370 = CARTESIAN_POINT('Ctrl Pts',(71.5866877247482,243.970384272286,6.31774884713379)) ;
#70371 = CARTESIAN_POINT('Ctrl Pts',(71.5805340060758,243.961141063887,6.31067237243103)) ;
#70372 = CARTESIAN_POINT('Ctrl Pts',(71.5633212059787,243.935286534796,6.29087849641324)) ;
#70373 = CARTESIAN_POINT('Ctrl Pts',(71.5438942831396,243.909242925014,6.27311943149809)) ;
#70374 = CARTESIAN_POINT('Ctrl Pts',(71.5219543369792,243.883348662293,6.25826321902762)) ;
#70375 = CARTESIAN_POINT('Ctrl Pts',(71.5108882767763,243.870288125677,6.25077004924574)) ;
#70376 = CARTESIAN_POINT('Ctrl Pts',(71.4991835316302,243.857265683635,6.24401485835062)) ;
#70377 = CARTESIAN_POINT('Ctrl Pts',(71.4868681437631,243.844407671654,6.23816299485402)) ;
#70378 = CARTESIAN_POINT('Ctrl Pts',(71.4777070320372,243.834842915302,6.23380993867133)) ;
#70379 = CARTESIAN_POINT('Ctrl Pts',(71.4682072078246,243.825367887728,6.22995574083448)) ;
#70380 = CARTESIAN_POINT('Ctrl Pts',(71.45836978832,243.816024472857,6.2266646345835)) ;
#70381 = CARTESIAN_POINT('Ctrl Pts',(71.4566034155626,243.81434680185,6.22607369501641)) ;
#70382 = CARTESIAN_POINT('Ctrl Pts',(71.4548262223221,243.812673441663,6.22550094157797)) ;
#70383 = CARTESIAN_POINT('Ctrl Pts',(71.4530382562569,243.811004678101,6.2249467661821)) ;
#70384 = CARTESIAN_POINT('Ctrl Pts',(71.4323658483102,243.791710485783,6.21853940751896)) ;
#70385 = CARTESIAN_POINT('Ctrl Pts',(71.4102573909446,243.77303338664,6.21461505937639)) ;
#70386 = CARTESIAN_POINT('Ctrl Pts',(71.3871541199649,243.755454107357,6.21342329168862)) ;
#70387 = CARTESIAN_POINT('Ctrl Pts',(71.3821602173354,243.751654246761,6.21316568436562)) ;
#70388 = CARTESIAN_POINT('Ctrl Pts',(71.3771200764926,243.747905917213,6.21303584367958)) ;
#70389 = CARTESIAN_POINT('Ctrl Pts',(71.3720385038273,243.744214269853,6.21303635288226)) ;
#70390 = CARTESIAN_POINT('Ctrl Pts',(71.3556121478995,243.7322808946,6.21303799889719)) ;
#70391 = CARTESIAN_POINT('Ctrl Pts',(71.338757067714,243.720943084757,6.21440203650676)) ;
#70392 = CARTESIAN_POINT('Ctrl Pts',(71.3216869500583,243.710299988263,6.21704113221422)) ;
#70393 = CARTESIAN_POINT('Ctrl Pts',(71.3090499734372,243.702420923555,6.21899484989965)) ;
#70394 = CARTESIAN_POINT('Ctrl Pts',(71.2962921174743,243.694920539031,6.22164757766141)) ;
#70395 = CARTESIAN_POINT('Ctrl Pts',(71.2834953493073,243.687836452692,6.22496512671297)) ;
#70396 = CARTESIAN_POINT('Ctrl Pts',(71.2706004162921,243.680698023862,6.22830812490099)) ;
#70397 = CARTESIAN_POINT('Ctrl Pts',(71.25766693237,243.673982902621,6.23232603291034)) ;
#70398 = CARTESIAN_POINT('Ctrl Pts',(71.2447600103528,243.667682392571,6.23693149431686)) ;
#70399 = CARTESIAN_POINT('Ctrl Pts',(71.2352301656824,243.6630304018,6.24033194345426)) ;
#70400 = CARTESIAN_POINT('Ctrl Pts',(71.2257122185925,243.658603091933,6.24405349551631)) ;
#70401 = CARTESIAN_POINT('Ctrl Pts',(71.216226504895,243.654394834633,6.24806417943962)) ;
#70402 = CARTESIAN_POINT('Ctrl Pts',(71.2085878920803,243.651006028143,6.25129388493034)) ;
#70403 = CARTESIAN_POINT('Ctrl Pts',(71.2009715347077,243.647759930132,6.25471059910582)) ;
#70404 = CARTESIAN_POINT('Ctrl Pts',(71.1933918074453,243.644655269533,6.25829603786513)) ;
#70405 = CARTESIAN_POINT('Ctrl Pts',(71.1611612922872,243.631453632189,6.27354204003386)) ;
#70406 = CARTESIAN_POINT('Ctrl Pts',(71.1295941708611,243.620812694726,6.29184252320046)) ;
#70407 = CARTESIAN_POINT('Ctrl Pts',(71.0989314377017,243.612317013262,6.3122744441402)) ;
#70408 = CARTESIAN_POINT('Ctrl Pts',(71.0820668876359,243.607644375482,6.32351203186064)) ;
#70409 = CARTESIAN_POINT('Ctrl Pts',(71.0654757041949,243.603619907437,6.33539347318128)) ;
#70410 = CARTESIAN_POINT('Ctrl Pts',(71.0491959191737,243.600170118652,6.34776114160793)) ;
#70411 = CARTESIAN_POINT('Ctrl Pts',(71.0404977678413,243.598326925705,6.35436908215903)) ;
#70412 = CARTESIAN_POINT('Ctrl Pts',(71.0318814733597,243.596646250274,6.36112111245423)) ;
#70413 = CARTESIAN_POINT('Ctrl Pts',(71.0233515826097,243.595117214015,6.36799498925902)) ;
#70414 = CARTESIAN_POINT('Ctrl Pts',(70.96981984014,243.585521314418,6.41113394773635)) ;
#70415 = CARTESIAN_POINT('Ctrl Pts',(70.9196911860922,243.581899679019,6.45907508759202)) ;
#70416 = CARTESIAN_POINT('Ctrl Pts',(70.8723567390609,243.582213043482,6.50928897930807)) ;
#70417 = CARTESIAN_POINT('Ctrl Pts',(70.8498554030447,243.582362007281,6.53315911450659)) ;
#70418 = CARTESIAN_POINT('Ctrl Pts',(70.8279854810731,243.583399804612,6.5575421964682)) ;
#70419 = CARTESIAN_POINT('Ctrl Pts',(70.8067113969608,243.585247990717,6.58235409106085)) ;
#70420 = CARTESIAN_POINT('Ctrl Pts',(70.7633271573144,243.589016996635,6.63295298760588)) ;
#70421 = CARTESIAN_POINT('Ctrl Pts',(70.7224350251622,243.596073422295,6.68522047956527)) ;
#70422 = CARTESIAN_POINT('Ctrl Pts',(70.6836563803347,243.605727456895,6.73849780320215)) ;
#70423 = CARTESIAN_POINT('Ctrl Pts',(70.6614902200515,243.611245774496,6.76895151555969)) ;
#70424 = CARTESIAN_POINT('Ctrl Pts',(70.6400153868192,243.617613628525,6.79973533853582)) ;
#70425 = CARTESIAN_POINT('Ctrl Pts',(70.6191665025799,243.624707302679,6.83072647984526)) ;
#70426 = CARTESIAN_POINT('Ctrl Pts',(70.5810380909751,243.637680204481,6.88740303761148)) ;
#70427 = CARTESIAN_POINT('Ctrl Pts',(70.5450012307065,243.653079304507,6.94477373817397)) ;
#70428 = CARTESIAN_POINT('Ctrl Pts',(70.5109406822167,243.670718836386,7.00266316541486)) ;
#70429 = CARTESIAN_POINT('Ctrl Pts',(70.4778053242332,243.687879223679,7.05898013563804)) ;
#70430 = CARTESIAN_POINT('Ctrl Pts',(70.446515553258,243.707086570428,7.11572953304929)) ;
#70431 = CARTESIAN_POINT('Ctrl Pts',(70.4169915862637,243.728134311011,7.17267980084145)) ;
#70432 = CARTESIAN_POINT('Ctrl Pts',(70.6507612838973,243.767402689634,7.27867958819153)) ;
#70433 = CARTESIAN_POINT('Ctrl Pts',(70.6684362520318,243.754659769268,7.23300052669799)) ;
#70434 = CARTESIAN_POINT('Ctrl Pts',(70.6869194298059,243.742792494175,7.18746933677425)) ;
#70435 = CARTESIAN_POINT('Ctrl Pts',(70.7062562007618,243.73185516032,7.14219315636161)) ;
#70436 = CARTESIAN_POINT('Ctrl Pts',(70.7248835542395,243.721319089727,7.09857804510088)) ;
#70437 = CARTESIAN_POINT('Ctrl Pts',(70.7443039240259,243.711645777375,7.05519957527199)) ;
#70438 = CARTESIAN_POINT('Ctrl Pts',(70.7645634985461,243.702931060682,7.01215352027502)) ;
#70439 = CARTESIAN_POINT('Ctrl Pts',(70.7764572906237,243.697814910377,6.98688246498295)) ;
#70440 = CARTESIAN_POINT('Ctrl Pts',(70.7886403641635,243.693030055314,6.96172597692718)) ;
#70441 = CARTESIAN_POINT('Ctrl Pts',(70.8011210393687,243.688604301858,6.93670343437627)) ;
#70442 = CARTESIAN_POINT('Ctrl Pts',(70.8183500983234,243.682494731184,6.9021608432327)) ;
#70443 = CARTESIAN_POINT('Ctrl Pts',(70.836126802622,243.677073327903,6.86787350758113)) ;
#70444 = CARTESIAN_POINT('Ctrl Pts',(70.854531822304,243.672418328196,6.83402414428508)) ;
#70445 = CARTESIAN_POINT('Ctrl Pts',(70.8724247945859,243.667892835578,6.80111650660351)) ;
#70446 = CARTESIAN_POINT('Ctrl Pts',(70.8909123497292,243.664091596054,6.76862281055142)) ;
#70447 = CARTESIAN_POINT('Ctrl Pts',(70.9100593736244,243.661134078233,6.73671094319522)) ;
#70448 = CARTESIAN_POINT('Ctrl Pts',(70.9283638588753,243.658306701946,6.70620331399155)) ;
#70449 = CARTESIAN_POINT('Ctrl Pts',(70.947271724205,243.65625053939,6.67622743493549)) ;
#70450 = CARTESIAN_POINT('Ctrl Pts',(70.9668210539553,243.655113775303,6.64692999111437)) ;
#70451 = CARTESIAN_POINT('Ctrl Pts',(70.9739232856404,243.654700791225,6.63628628943998)) ;
#70452 = CARTESIAN_POINT('Ctrl Pts',(70.9811099480349,243.65440957849,6.62573213131839)) ;
#70453 = CARTESIAN_POINT('Ctrl Pts',(70.9883819374054,243.654248714521,6.61527455030405)) ;
#70454 = CARTESIAN_POINT('Ctrl Pts',(71.0058228527503,243.653862903331,6.59019341006963)) ;
#70455 = CARTESIAN_POINT('Ctrl Pts',(71.0237569280687,243.654222647332,6.56566779824074)) ;
#70456 = CARTESIAN_POINT('Ctrl Pts',(71.0422577508755,243.655477612093,6.54201530058587)) ;
#70457 = CARTESIAN_POINT('Ctrl Pts',(71.0591803639201,243.656625522283,6.52038047550117)) ;
#70458 = CARTESIAN_POINT('Ctrl Pts',(71.0765776157427,243.658522933216,6.49947615643607)) ;
#70459 = CARTESIAN_POINT('Ctrl Pts',(71.0944794582127,243.661326346066,6.47954539033945)) ;
#70460 = CARTESIAN_POINT('Ctrl Pts',(71.0961489913088,243.661587793487,6.47768663900227)) ;
#70461 = CARTESIAN_POINT('Ctrl Pts',(71.0978228895911,243.661857150439,6.47583635514527)) ;
#70462 = CARTESIAN_POINT('Ctrl Pts',(71.0995011620659,243.662134562174,6.47399473591177)) ;
#70463 = CARTESIAN_POINT('Ctrl Pts',(71.1177037387764,243.665143375378,6.45402049700077)) ;
#70464 = CARTESIAN_POINT('Ctrl Pts',(71.1364174559616,243.669096373618,6.43506553102507)) ;
#70465 = CARTESIAN_POINT('Ctrl Pts',(71.1555892310845,243.674185491156,6.41767878130173)) ;
#70466 = CARTESIAN_POINT('Ctrl Pts',(71.1738953556318,243.679044823111,6.40107708407407)) ;
#70467 = CARTESIAN_POINT('Ctrl Pts',(71.1926195333131,243.684940452386,6.38590518299697)) ;
#70468 = CARTESIAN_POINT('Ctrl Pts',(71.211672149302,243.69205993109,6.37264097007206)) ;
#70469 = CARTESIAN_POINT('Ctrl Pts',(71.2157986470463,243.693601898493,6.36976814962858)) ;
#70470 = CARTESIAN_POINT('Ctrl Pts',(71.2199403691951,243.695201339153,6.36698481647962)) ;
#70471 = CARTESIAN_POINT('Ctrl Pts',(71.2240960892816,243.696860256998,6.36429582586576)) ;
#70472 = CARTESIAN_POINT('Ctrl Pts',(71.2401983004994,243.703288082976,6.35387676637042)) ;
#70473 = CARTESIAN_POINT('Ctrl Pts',(71.2565168735863,243.710615594979,6.34487410716004)) ;
#70474 = CARTESIAN_POINT('Ctrl Pts',(71.2728169071997,243.71887377027,6.3377356388658)) ;
#70475 = CARTESIAN_POINT('Ctrl Pts',(71.2785027662801,243.721754428192,6.33524556272643)) ;
#70476 = CARTESIAN_POINT('Ctrl Pts',(71.2841863608018,243.724747868746,6.33298231923947)) ;
#70477 = CARTESIAN_POINT('Ctrl Pts',(71.2898577861283,243.727853897203,6.33096491471358)) ;
#70478 = CARTESIAN_POINT('Ctrl Pts',(71.3034194112714,243.735281094282,6.32614085685032)) ;
#70479 = CARTESIAN_POINT('Ctrl Pts',(71.316912179818,243.743356911529,6.32272248960801)) ;
#70480 = CARTESIAN_POINT('Ctrl Pts',(71.3301413890697,243.75201206251,6.32081539597999)) ;
#70481 = CARTESIAN_POINT('Ctrl Pts',(71.3383047211844,243.757352886033,6.31963858802697)) ;
#70482 = CARTESIAN_POINT('Ctrl Pts',(71.3463680534785,243.76291335346,6.31903723360498)) ;
#70483 = CARTESIAN_POINT('Ctrl Pts',(71.3542903145311,243.768668411348,6.31903614088288)) ;
#70484 = CARTESIAN_POINT('Ctrl Pts',(71.3670532685345,243.777939948681,6.31903438048116)) ;
#70485 = CARTESIAN_POINT('Ctrl Pts',(71.3794502709664,243.787720035148,6.32059053861267)) ;
#70486 = CARTESIAN_POINT('Ctrl Pts',(71.391331743839,243.797868294085,6.32360061213219)) ;
#70487 = CARTESIAN_POINT('Ctrl Pts',(71.3987772128469,243.804227652744,6.32548686052423)) ;
#70488 = CARTESIAN_POINT('Ctrl Pts',(71.4060208997469,243.810730744532,6.32794403869006)) ;
#70489 = CARTESIAN_POINT('Ctrl Pts',(71.4130334230589,243.817335711349,6.33094655418276)) ;
#70490 = CARTESIAN_POINT('Ctrl Pts',(71.4266399543435,243.830151453079,6.3367723916404)) ;
#70491 = CARTESIAN_POINT('Ctrl Pts',(71.4393767723351,243.843353445295,6.34465133540946)) ;
#70492 = CARTESIAN_POINT('Ctrl Pts',(71.4511861305303,243.856712421974,6.35412854620593)) ;
#70493 = CARTESIAN_POINT('Ctrl Pts',(71.4551755784542,243.861225363396,6.35733014601447)) ;
#70494 = CARTESIAN_POINT('Ctrl Pts',(71.4590596019843,243.865756070438,6.36071414477957)) ;
#70495 = CARTESIAN_POINT('Ctrl Pts',(71.462837250583,243.870295331209,6.36426300702838)) ;
#70496 = CARTESIAN_POINT('Ctrl Pts',(71.4760836447931,243.886212332493,6.37670715769954)) ;
#70497 = CARTESIAN_POINT('Ctrl Pts',(71.4880287658818,243.902237362419,6.39117841554036)) ;
#70498 = CARTESIAN_POINT('Ctrl Pts',(71.4988220697557,243.918213233306,6.40719115654323)) ;
#70499 = CARTESIAN_POINT('Ctrl Pts',(71.5101121008671,243.934924342476,6.42394083265832)) ;
#70500 = CARTESIAN_POINT('Ctrl Pts',(71.5201425169332,243.951581936066,6.44237714045534)) ;
#70501 = CARTESIAN_POINT('Ctrl Pts',(71.5290803896567,243.968062508258,6.46194427505928)) ;
#70502 = CARTESIAN_POINT('Ctrl Pts',(71.5308979488639,243.971413911512,6.46592334555604)) ;
#70503 = CARTESIAN_POINT('Ctrl Pts',(71.5326702971534,243.974758164482,6.46994917932546)) ;
#70504 = CARTESIAN_POINT('Ctrl Pts',(71.53439878569,243.978094479398,6.47401710240149)) ;
#70505 = CARTESIAN_POINT('Ctrl Pts',(71.5427855239735,243.994282495369,6.49375492852842)) ;
#70506 = CARTESIAN_POINT('Ctrl Pts',(71.5501387651293,244.010273697668,6.51448364351368)) ;
#70507 = CARTESIAN_POINT('Ctrl Pts',(71.5566194596361,244.026044169239,6.53596191343711)) ;
#70508 = CARTESIAN_POINT('Ctrl Pts',(71.5633848267489,244.042507378485,6.55838364321145)) ;
#70509 = CARTESIAN_POINT('Ctrl Pts',(71.5691996947475,244.058730639276,6.58162222447675)) ;
#70510 = CARTESIAN_POINT('Ctrl Pts',(71.5742121078923,244.074730455715,6.60540310320344)) ;
#70511 = CARTESIAN_POINT('Ctrl Pts',(71.5749062081047,244.076946050413,6.60869619028523)) ;
#70512 = CARTESIAN_POINT('Ctrl Pts',(71.5755848629926,244.079157417819,6.61199967628627)) ;
#70513 = CARTESIAN_POINT('Ctrl Pts',(71.5762484098432,244.081364654275,6.6153128321625)) ;
#70514 = CARTESIAN_POINT('Ctrl Pts',(71.5820478706719,244.100656104999,6.64427012087318)) ;
#70515 = CARTESIAN_POINT('Ctrl Pts',(71.5866962665371,244.119629043175,6.67396608377127)) ;
#70516 = CARTESIAN_POINT('Ctrl Pts',(71.5903623616101,244.13826024683,6.70425263042087)) ;
#70517 = CARTESIAN_POINT('Ctrl Pts',(71.5941409686902,244.157463239835,6.73546866746413)) ;
#70518 = CARTESIAN_POINT('Ctrl Pts',(71.5968763478246,244.176303979186,6.76731209439664)) ;
#70519 = CARTESIAN_POINT('Ctrl Pts',(71.5987132229992,244.194797005408,6.79962076342479)) ;
#70520 = CARTESIAN_POINT('Ctrl Pts',(71.6006246850276,244.21404094637,6.83324133541157)) ;
#70521 = CARTESIAN_POINT('Ctrl Pts',(71.6015634590013,244.23290912843,6.86736569916324)) ;
#70522 = CARTESIAN_POINT('Ctrl Pts',(71.6016454480536,244.251448540695,6.90181114181182)) ;
#70523 = CARTESIAN_POINT('Ctrl Pts',(71.6016730476434,244.257689376029,6.91340634949709)) ;
#70524 = CARTESIAN_POINT('Ctrl Pts',(71.6016031603688,244.263893152714,6.9250379407503)) ;
#70525 = CARTESIAN_POINT('Ctrl Pts',(71.6014390043077,244.27006217053,6.93669894594631)) ;
#70526 = CARTESIAN_POINT('Ctrl Pts',(71.6008393973384,244.292595521116,6.97929268228135)) ;
#70527 = CARTESIAN_POINT('Ctrl Pts',(71.598986155638,244.314631427322,7.02227885814213)) ;
#70528 = CARTESIAN_POINT('Ctrl Pts',(71.5960122668263,244.336169373341,7.06555758389289)) ;
#70529 = CARTESIAN_POINT('Ctrl Pts',(71.5929199249018,244.358565198356,7.11056014671543)) ;
#70530 = CARTESIAN_POINT('Ctrl Pts',(71.5886160783604,244.380423612925,7.15587902870036)) ;
#70531 = CARTESIAN_POINT('Ctrl Pts',(71.5831973640719,244.401764396013,7.20140192234408)) ;
#70532 = CARTESIAN_POINT('Ctrl Pts',(71.5801381119917,244.413812795611,7.22710285427377)) ;
#70533 = CARTESIAN_POINT('Ctrl Pts',(71.5767225386487,244.425696478238,7.25286881309734)) ;
#70534 = CARTESIAN_POINT('Ctrl Pts',(71.5729608165744,244.437419869792,7.27867958883833)) ;
#70535 = CARTESIAN_POINT('Origin',(75.2882970367382,245.15,7.2786795888419)) ;
#70536 = CARTESIAN_POINT('',(75.0983134848186,245.2125,7.27867958883755)) ;
#70537 = CARTESIAN_POINT('Origin',(75.2882970367382,245.15,7.2786795888419)) ;
#70538 = CARTESIAN_POINT('',(75.3105185167129,245.31813759476,7.17267980084143)) ;
#70539 = CARTESIAN_POINT('Origin',(75.2882970367382,245.15,7.2786795888419)) ;
#70540 = CARTESIAN_POINT('Origin',(75.2882970367374,245.149999999998,7.27867958883798)) ;
#70541 = CARTESIAN_POINT('Origin',(70.3231932313898,243.3945648893,7.2786795888419)) ;
#70542 = CARTESIAN_POINT('',(70.1609601392448,243.277601545414,7.27867958883745)) ;
#70543 = CARTESIAN_POINT('Origin',(70.3231932313898,243.3945648893,7.2786795888419)) ;
#70544 = CARTESIAN_POINT('',(70.2002285180491,243.511371242796,7.17267980084141)) ;
#70545 = CARTESIAN_POINT('Origin',(70.3231932313898,243.3945648893,7.2786795888419)) ;
#70546 = CARTESIAN_POINT('Origin',(70.3231932313913,243.394564889298,7.27867958883786)) ;
#70547 = CARTESIAN_POINT('Origin',(74.5283628290597,239.4,7.2786795888419)) ;
#70548 = CARTESIAN_POINT('Origin',(74.5283628290597,239.4,7.17267980084127)) ;
#70549 = CARTESIAN_POINT('Origin',(75.5824701665474,245.103407553477,7.27867958884206)) ;
#70550 = CARTESIAN_POINT('',(75.7824688237379,245.104140439548,7.27867958883791)) ;
#70551 = CARTESIAN_POINT('Origin',(75.5824701665474,245.103407553477,7.27867958883751)) ;
#70552 = CARTESIAN_POINT('',(75.6132936573898,245.270182723559,7.17267980084128)) ;
#70553 = CARTESIAN_POINT('Origin',(75.5824701665474,245.103407553477,7.27867958884206)) ;
#70554 = CARTESIAN_POINT('Origin',(75.5824701665474,245.103407553477,7.2786795888419)) ;
#70555 = CARTESIAN_POINT('Origin',(69.4298369914029,242.164965512068,7.27867958886636)) ;
#70556 = CARTESIAN_POINT('',(69.4909429595611,242.355402012391,7.27867958819176)) ;
#70557 = CARTESIAN_POINT('Origin',(69.4298369914177,242.164965512063,7.27867958812535)) ;
#70558 = CARTESIAN_POINT('',(69.2807493616484,242.245816755675,7.17267980084126)) ;
#70559 = CARTESIAN_POINT('Origin',(69.4298369914029,242.164965512068,7.27867958886636)) ;
#70560 = CARTESIAN_POINT('Origin',(69.4298369914177,242.164965512063,7.2786795888419)) ;
#70561 = CARTESIAN_POINT('Ctrl Pts',(69.4909429592547,242.355402012489,7.27867958886636)) ;
#70562 = CARTESIAN_POINT('Ctrl Pts',(69.5434105984377,242.338566553604,7.16316434207535)) ;
#70563 = CARTESIAN_POINT('Ctrl Pts',(69.6548363472646,242.318447141452,6.93376983755156)) ;
#70564 = CARTESIAN_POINT('Ctrl Pts',(69.8115179376631,242.335283243238,6.66059049824912)) ;
#70565 = CARTESIAN_POINT('Ctrl Pts',(69.9320961586154,242.382043605764,6.4924392790701)) ;
#70566 = CARTESIAN_POINT('Ctrl Pts',(70.0038423289643,242.42384128837,6.4112217229231)) ;
#70567 = CARTESIAN_POINT('Ctrl Pts',(70.0853128564862,242.483004335118,6.33512166788152)) ;
#70568 = CARTESIAN_POINT('Ctrl Pts',(70.1739356804575,242.581754164171,6.30139292105391)) ;
#70569 = CARTESIAN_POINT('Ctrl Pts',(70.2630551704512,242.761871347334,6.38459950069724)) ;
#70570 = CARTESIAN_POINT('Ctrl Pts',(70.2766922354173,242.880428587697,6.52710936966954)) ;
#70571 = CARTESIAN_POINT('Ctrl Pts',(70.2731493424206,242.966128315359,6.65331963180678)) ;
#70572 = CARTESIAN_POINT('Ctrl Pts',(70.2672749757801,243.03292209962,6.75725826388023)) ;
#70573 = CARTESIAN_POINT('Ctrl Pts',(70.2400533595442,243.145774108243,6.96268987067883)) ;
#70574 = CARTESIAN_POINT('Ctrl Pts',(70.1931792067253,243.232912339636,7.16318512433994)) ;
#70575 = CARTESIAN_POINT('Ctrl Pts',(70.1609601392448,243.277601545414,7.27867958884205)) ;
#70576 = CARTESIAN_POINT('Ctrl Pts',(69.4476956000447,242.369278930705,7.24979207610077)) ;
#70577 = CARTESIAN_POINT('Ctrl Pts',(69.50150865405,242.347521264376,7.13555826270376)) ;
#70578 = CARTESIAN_POINT('Ctrl Pts',(69.6176942987279,242.318512021194,6.9083440833659)) ;
#70579 = CARTESIAN_POINT('Ctrl Pts',(69.7848017901261,242.327968834837,6.6372185129258)) ;
#70580 = CARTESIAN_POINT('Ctrl Pts',(69.9147387087311,242.37320396469,6.47017552473)) ;
#70581 = CARTESIAN_POINT('Ctrl Pts',(69.9922050270014,242.415732076274,6.38946597909784)) ;
#70582 = CARTESIAN_POINT('Ctrl Pts',(70.0801887888135,242.477057954304,6.3138257023692)) ;
#70583 = CARTESIAN_POINT('Ctrl Pts',(70.1754581944923,242.581877167593,6.28029131424589)) ;
#70584 = CARTESIAN_POINT('Ctrl Pts',(70.2684663048936,242.774904229625,6.36301246673742)) ;
#70585 = CARTESIAN_POINT('Ctrl Pts',(70.2790542356121,242.90185505708,6.50464021891)) ;
#70586 = CARTESIAN_POINT('Ctrl Pts',(70.2715880028707,242.992611796454,6.62996444336295)) ;
#70587 = CARTESIAN_POINT('Ctrl Pts',(70.2622816507088,243.06319032064,6.73315738197291)) ;
#70588 = CARTESIAN_POINT('Ctrl Pts',(70.227188364081,243.181213854183,6.93698950249586)) ;
#70589 = CARTESIAN_POINT('Ctrl Pts',(70.1717134407734,243.269996255639,7.13557881442655)) ;
#70590 = CARTESIAN_POINT('Ctrl Pts',(70.1343982367933,243.314444024645,7.24979207607672)) ;
#70591 = CARTESIAN_POINT('Ctrl Pts',(69.3602854366959,242.355114488823,7.19960833957127)) ;
#70592 = CARTESIAN_POINT('Ctrl Pts',(69.4213790495086,242.328536560427,7.08745246144888)) ;
#70593 = CARTESIAN_POINT('Ctrl Pts',(69.5531897217821,242.292089762554,6.86383160650544)) ;
#70594 = CARTESIAN_POINT('Ctrl Pts',(69.7424264478363,242.29914527047,6.59616795491574)) ;
#70595 = CARTESIAN_POINT('Ctrl Pts',(69.8891297803734,242.347952204288,6.43101832592783)) ;
#70596 = CARTESIAN_POINT('Ctrl Pts',(69.9764181098155,242.394722276976,6.35118125015187)) ;
#70597 = CARTESIAN_POINT('Ctrl Pts',(70.0753852288502,242.462564006987,6.27633386832372)) ;
#70598 = CARTESIAN_POINT('Ctrl Pts',(70.1820851481564,242.579361897691,6.24313659439274)) ;
#70599 = CARTESIAN_POINT('Ctrl Pts',(70.2851436276679,242.795516871846,6.32501770065842)) ;
#70600 = CARTESIAN_POINT('Ctrl Pts',(70.2953060969612,242.938129691503,6.46512808573764)) ;
#70601 = CARTESIAN_POINT('Ctrl Pts',(70.2852400421153,243.040198107596,6.5889491341787)) ;
#70602 = CARTESIAN_POINT('Ctrl Pts',(70.2733858425031,243.119595484145,6.69087987237211)) ;
#70603 = CARTESIAN_POINT('Ctrl Pts',(70.2309948427504,243.252450612718,6.89202719270369)) ;
#70604 = CARTESIAN_POINT('Ctrl Pts',(70.1650063280899,243.352071612089,7.0874726393318)) ;
#70605 = CARTESIAN_POINT('Ctrl Pts',(70.1208581955899,243.401953083345,7.19960833954767)) ;
#70606 = CARTESIAN_POINT('Ctrl Pts',(69.2980284313546,242.282143340439,7.17608503413729)) ;
#70607 = CARTESIAN_POINT('Ctrl Pts',(69.3662601562767,242.258303056981,7.06213458186476)) ;
#70608 = CARTESIAN_POINT('Ctrl Pts',(69.5117541198825,242.228719169598,6.83550818080611)) ;
#70609 = CARTESIAN_POINT('Ctrl Pts',(69.7176650261854,242.248060838742,6.56510244268801)) ;
#70610 = CARTESIAN_POINT('Ctrl Pts',(69.8767158105699,242.30846111626,6.39850449270415)) ;
#70611 = CARTESIAN_POINT('Ctrl Pts',(69.9714892930823,242.363136499339,6.31801004275899)) ;
#70612 = CARTESIAN_POINT('Ctrl Pts',(70.0791779627476,242.440864892285,6.24257136321944)) ;
#70613 = CARTESIAN_POINT('Ctrl Pts',(70.1963946085699,242.571276507691,6.20912630982003)) ;
#70614 = CARTESIAN_POINT('Ctrl Pts',(70.3137925639844,242.809340189588,6.29162715593499)) ;
#70615 = CARTESIAN_POINT('Ctrl Pts',(70.3308790897817,242.965626066389,6.43287720578516)) ;
#70616 = CARTESIAN_POINT('Ctrl Pts',(70.3251826391914,243.07816667912,6.55786814745459)) ;
#70617 = CARTESIAN_POINT('Ctrl Pts',(70.3165658070084,243.16580527229,6.66078695502675)) ;
#70618 = CARTESIAN_POINT('Ctrl Pts',(70.2787474042028,243.313338909124,6.8640798425796)) ;
#70619 = CARTESIAN_POINT('Ctrl Pts',(70.2147697560625,243.426197514365,7.06215508260825)) ;
#70620 = CARTESIAN_POINT('Ctrl Pts',(70.1710194090925,243.483712338908,7.1760850341133)) ;
#70621 = CARTESIAN_POINT('Ctrl Pts',(69.2807493616358,242.245816755683,7.17267980086572)) ;
#70622 = CARTESIAN_POINT('Ctrl Pts',(69.3508960370599,242.223719506269,7.05716455407472)) ;
#70623 = CARTESIAN_POINT('Ctrl Pts',(69.5001356158098,242.198132189401,6.82777004955092)) ;
#70624 = CARTESIAN_POINT('Ctrl Pts',(69.710911608549,242.223881724253,6.55459071024847)) ;
#70625 = CARTESIAN_POINT('Ctrl Pts',(69.8739373345158,242.28994594427,6.38643949106947)) ;
#70626 = CARTESIAN_POINT('Ctrl Pts',(69.9712979550201,242.348344696013,6.30522193492245)) ;
#70627 = CARTESIAN_POINT('Ctrl Pts',(70.082153166785,242.43062586115,6.22912187988088)) ;
#70628 = CARTESIAN_POINT('Ctrl Pts',(70.2036250939698,242.567006326368,6.19539313305328)) ;
#70629 = CARTESIAN_POINT('Ctrl Pts',(70.3276776120394,242.813968315643,6.2785997126966)) ;
#70630 = CARTESIAN_POINT('Ctrl Pts',(70.348633230693,242.975275641354,6.42110958166891)) ;
#70631 = CARTESIAN_POINT('Ctrl Pts',(70.3456213203833,243.09149482855,6.54731984380613)) ;
#70632 = CARTESIAN_POINT('Ctrl Pts',(70.3390649159907,243.181991491806,6.65125847587959)) ;
#70633 = CARTESIAN_POINT('Ctrl Pts',(70.3045673928554,243.334423102977,6.85669008267818)) ;
#70634 = CARTESIAN_POINT('Ctrl Pts',(70.2429130851605,243.451496989519,7.05718533633929)) ;
#70635 = CARTESIAN_POINT('Ctrl Pts',(70.2002285180491,243.511371242796,7.17267980084141)) ;
#70636 = CARTESIAN_POINT('Ctrl Pts',(70.2002285180491,243.511371242796,7.17267980084141)) ;
#70637 = CARTESIAN_POINT('Ctrl Pts',(70.2313933057879,243.467655948939,7.08835516749437)) ;
#70638 = CARTESIAN_POINT('Ctrl Pts',(70.2585789380893,243.42009714279,7.00442256017519)) ;
#70639 = CARTESIAN_POINT('Ctrl Pts',(70.2809775421819,243.368344041036,6.92172413787986)) ;
#70640 = CARTESIAN_POINT('Ctrl Pts',(70.2858591151139,243.357064921158,6.90370076561406)) ;
#70641 = CARTESIAN_POINT('Ctrl Pts',(70.2905133120903,243.345586461082,6.88573585920702)) ;
#70642 = CARTESIAN_POINT('Ctrl Pts',(70.2949317635032,243.33390483265,6.86783787320399)) ;
#70643 = CARTESIAN_POINT('Ctrl Pts',(70.2979780832332,243.325850885272,6.85549803220697)) ;
#70644 = CARTESIAN_POINT('Ctrl Pts',(70.3009109484532,243.317698916943,6.84319006572952)) ;
#70645 = CARTESIAN_POINT('Ctrl Pts',(70.3037274475218,243.309447539126,6.83091681197913)) ;
#70646 = CARTESIAN_POINT('Ctrl Pts',(70.3204319542847,243.260509054436,6.75812479420123)) ;
#70647 = CARTESIAN_POINT('Ctrl Pts',(70.3330403214039,243.208071641295,6.6865553202387)) ;
#70648 = CARTESIAN_POINT('Ctrl Pts',(70.3401180984443,243.151348445742,6.61757279026188)) ;
#70649 = CARTESIAN_POINT('Ctrl Pts',(70.3411905548211,243.142753493904,6.60712024933831)) ;
#70650 = CARTESIAN_POINT('Ctrl Pts',(70.3421361030927,243.134060194437,6.59672706305293)) ;
#70651 = CARTESIAN_POINT('Ctrl Pts',(70.3429498371333,243.125265870193,6.58639792831063)) ;
#70652 = CARTESIAN_POINT('Ctrl Pts',(70.3439815081954,243.114116220087,6.57330240953252)) ;
#70653 = CARTESIAN_POINT('Ctrl Pts',(70.344801294108,243.102804186611,6.56030986280214)) ;
#70654 = CARTESIAN_POINT('Ctrl Pts',(70.3453617679955,243.091339667682,6.5475056875169)) ;
#70655 = CARTESIAN_POINT('Ctrl Pts',(70.3459224809741,243.079870258134,6.53469605013184)) ;
#70656 = CARTESIAN_POINT('Ctrl Pts',(70.346223677288,243.068248220193,6.52207490449511)) ;
#70657 = CARTESIAN_POINT('Ctrl Pts',(70.3462973843869,243.056426804173,6.50953957109844)) ;
#70658 = CARTESIAN_POINT('Ctrl Pts',(70.346312595762,243.053987147801,6.50695257932533)) ;
#70659 = CARTESIAN_POINT('Ctrl Pts',(70.3463181179843,243.051539000306,6.50436924332236)) ;
#70660 = CARTESIAN_POINT('Ctrl Pts',(70.3463136044882,243.049082390573,6.50179014031024)) ;
#70661 = CARTESIAN_POINT('Ctrl Pts',(70.3462749444578,243.028040474061,6.47969901630214)) ;
#70662 = CARTESIAN_POINT('Ctrl Pts',(70.3454302657341,243.006412398833,6.45803982307202)) ;
#70663 = CARTESIAN_POINT('Ctrl Pts',(70.3436337525118,242.984193617895,6.43706415935564)) ;
#70664 = CARTESIAN_POINT('Ctrl Pts',(70.3419956946639,242.963934569402,6.41793858313386)) ;
#70665 = CARTESIAN_POINT('Ctrl Pts',(70.339566698251,242.943184067893,6.39938013482495)) ;
#70666 = CARTESIAN_POINT('Ctrl Pts',(70.336207088231,242.921910636217,6.38158470105561)) ;
#70667 = CARTESIAN_POINT('Ctrl Pts',(70.332847478211,242.900637204541,6.36378926728627)) ;
#70668 = CARTESIAN_POINT('Ctrl Pts',(70.3285580513409,242.878841054704,6.34675571504515)) ;
#70669 = CARTESIAN_POINT('Ctrl Pts',(70.3231594750068,242.856461675999,6.3307017817941)) ;
#70670 = CARTESIAN_POINT('Ctrl Pts',(70.3179443203035,242.834842657411,6.31519329579368)) ;
#70671 = CARTESIAN_POINT('Ctrl Pts',(70.3117103388422,242.812760858963,6.30066206320242)) ;
#70672 = CARTESIAN_POINT('Ctrl Pts',(70.3042672680503,242.790239415608,6.28741860766138)) ;
#70673 = CARTESIAN_POINT('Ctrl Pts',(70.2982890477912,242.772150356308,6.27678156061052)) ;
#70674 = CARTESIAN_POINT('Ctrl Pts',(70.2915312746284,242.753778155301,6.26697531069235)) ;
#70675 = CARTESIAN_POINT('Ctrl Pts',(70.2839131880942,242.735149852357,6.2581530367002)) ;
#70676 = CARTESIAN_POINT('Ctrl Pts',(70.2762425980247,242.716393163924,6.249269959963)) ;
#70677 = CARTESIAN_POINT('Ctrl Pts',(70.2676997909606,242.69737744558,6.24138521936161)) ;
#70678 = CARTESIAN_POINT('Ctrl Pts',(70.2582982006726,242.678406955222,6.23482036252682)) ;
#70679 = CARTESIAN_POINT('Ctrl Pts',(70.2505801554145,242.662833515126,6.22943107618143)) ;
#70680 = CARTESIAN_POINT('Ctrl Pts',(70.2422224563955,242.647221418542,6.22494162734417)) ;
#70681 = CARTESIAN_POINT('Ctrl Pts',(70.2332777382532,242.631713974233,6.22144947621304)) ;
#70682 = CARTESIAN_POINT('Ctrl Pts',(70.2282164607882,242.62293924515,6.21947347813873)) ;
#70683 = CARTESIAN_POINT('Ctrl Pts',(70.2229666179565,242.614197342908,6.21781685667503)) ;
#70684 = CARTESIAN_POINT('Ctrl Pts',(70.2175328092121,242.605508743235,6.21649820450614)) ;
#70685 = CARTESIAN_POINT('Ctrl Pts',(70.2163743948262,242.603656451532,6.21621708573398)) ;
#70686 = CARTESIAN_POINT('Ctrl Pts',(70.2152080325008,242.601806717165,6.21595091938064)) ;
#70687 = CARTESIAN_POINT('Ctrl Pts',(70.2140335854535,242.599959879669,6.21570025794295)) ;
#70688 = CARTESIAN_POINT('Ctrl Pts',(70.2055139162308,242.586562558252,6.21388191071223)) ;
#70689 = CARTESIAN_POINT('Ctrl Pts',(70.1965658083798,242.573314830591,6.21288076424351)) ;
#70690 = CARTESIAN_POINT('Ctrl Pts',(70.1872375019662,242.560327455973,6.21273140721762)) ;
#70691 = CARTESIAN_POINT('Ctrl Pts',(70.1850974079421,242.557347900888,6.21269714182534)) ;
#70692 = CARTESIAN_POINT('Ctrl Pts',(70.1829374521883,242.55438219318,6.21270764357374)) ;
#70693 = CARTESIAN_POINT('Ctrl Pts',(70.1807584781267,242.551431924514,6.21276321324356)) ;
#70694 = CARTESIAN_POINT('Ctrl Pts',(70.1687049623989,242.535111808368,6.21307061015158)) ;
#70695 = CARTESIAN_POINT('Ctrl Pts',(70.1560696732988,242.519265969027,6.2147585524089)) ;
#70696 = CARTESIAN_POINT('Ctrl Pts',(70.1430567186737,242.504001518625,6.21764257922973)) ;
#70697 = CARTESIAN_POINT('Ctrl Pts',(70.1289995289569,242.487512160027,6.2207580371205)) ;
#70698 = CARTESIAN_POINT('Ctrl Pts',(70.1144902283092,242.471701143486,6.22528409350145)) ;
#70699 = CARTESIAN_POINT('Ctrl Pts',(70.0996916826711,242.456735839965,6.23114390838201)) ;
#70700 = CARTESIAN_POINT('Ctrl Pts',(70.0939033603583,242.450882291758,6.23343592396595)) ;
#70701 = CARTESIAN_POINT('Ctrl Pts',(70.0880709269218,242.445158604079,6.23593225992976)) ;
#70702 = CARTESIAN_POINT('Ctrl Pts',(70.0822047726577,242.43957665699,6.23862924141461)) ;
#70703 = CARTESIAN_POINT('Ctrl Pts',(70.0699166428066,242.427883870275,6.24427874485421)) ;
#70704 = CARTESIAN_POINT('Ctrl Pts',(70.0574947471439,242.416711633889,6.25069645438963)) ;
#70705 = CARTESIAN_POINT('Ctrl Pts',(70.0450391756289,242.406159149867,6.25783532677176)) ;
#70706 = CARTESIAN_POINT('Ctrl Pts',(70.0267404124392,242.390656255764,6.2683232064331)) ;
#70707 = CARTESIAN_POINT('Ctrl Pts',(70.0083678172079,242.37649017468,6.28036889709359)) ;
#70708 = CARTESIAN_POINT('Ctrl Pts',(69.9900275617557,242.363426272423,6.29352850225734)) ;
#70709 = CARTESIAN_POINT('Ctrl Pts',(69.9838292441962,242.359011164086,6.29797595458291)) ;
#70710 = CARTESIAN_POINT('Ctrl Pts',(69.9776349202651,242.354722200375,6.30255041575482)) ;
#70711 = CARTESIAN_POINT('Ctrl Pts',(69.9714495377026,242.350551114819,6.30723414323133)) ;
#70712 = CARTESIAN_POINT('Ctrl Pts',(69.9546992737991,242.339255647946,6.31991786497235)) ;
#70713 = CARTESIAN_POINT('Ctrl Pts',(69.9380132958858,242.328823185994,6.33340373088781)) ;
#70714 = CARTESIAN_POINT('Ctrl Pts',(69.9214895956895,242.319297806037,6.34757136463829)) ;
#70715 = CARTESIAN_POINT('Ctrl Pts',(69.9138517594529,242.314894839913,6.35412014397709)) ;
#70716 = CARTESIAN_POINT('Ctrl Pts',(69.9062427572804,242.310664931116,6.36080436695981)) ;
#70717 = CARTESIAN_POINT('Ctrl Pts',(69.8986686267112,242.306604278837,6.3676101865645)) ;
#70718 = CARTESIAN_POINT('Ctrl Pts',(69.8659264492777,242.289050502043,6.39703103573528)) ;
#70719 = CARTESIAN_POINT('Ctrl Pts',(69.8338335372565,242.274655893542,6.42872449053609)) ;
#70720 = CARTESIAN_POINT('Ctrl Pts',(69.8024037650707,242.262721225499,6.46185807151192)) ;
#70721 = CARTESIAN_POINT('Ctrl Pts',(69.7878029806823,242.257176943669,6.47725036481219)) ;
#70722 = CARTESIAN_POINT('Ctrl Pts',(69.7733457297794,242.252164212083,6.49295339842054)) ;
#70723 = CARTESIAN_POINT('Ctrl Pts',(69.7590354098376,242.247615994147,6.50888317841182)) ;
#70724 = CARTESIAN_POINT('Ctrl Pts',(69.7375091503596,242.240774349805,6.53284550622236)) ;
#70725 = CARTESIAN_POINT('Ctrl Pts',(69.7163151111706,242.234983455156,6.55732102883111)) ;
#70726 = CARTESIAN_POINT('Ctrl Pts',(69.6954473136586,242.230180873332,6.58223895379559)) ;
#70727 = CARTESIAN_POINT('Ctrl Pts',(69.6546794117156,242.220798417672,6.6309192958869)) ;
#70728 = CARTESIAN_POINT('Ctrl Pts',(69.615164454165,242.214993311974,6.6811176994941)) ;
#70729 = CARTESIAN_POINT('Ctrl Pts',(69.5767655747089,242.212087601469,6.73226793926176)) ;
#70730 = CARTESIAN_POINT('Ctrl Pts',(69.5524260639884,242.210245788037,6.76469002622929)) ;
#70731 = CARTESIAN_POINT('Ctrl Pts',(69.5285355441474,242.209570019988,6.79749468373767)) ;
#70732 = CARTESIAN_POINT('Ctrl Pts',(69.5050643349143,242.20989684534,6.83053755702586)) ;
#70733 = CARTESIAN_POINT('Ctrl Pts',(69.4647641483364,242.210458006145,6.88727233985513)) ;
#70734 = CARTESIAN_POINT('Ctrl Pts',(69.4256984745267,242.213972936061,6.94471044687498)) ;
#70735 = CARTESIAN_POINT('Ctrl Pts',(69.3878301535716,242.220237135349,7.00265575379959)) ;
#70736 = CARTESIAN_POINT('Ctrl Pts',(69.3510225444185,242.226325871085,7.05897798187159)) ;
#70737 = CARTESIAN_POINT('Ctrl Pts',(69.3153324323798,242.234922572387,7.11572953305061)) ;
#70738 = CARTESIAN_POINT('Ctrl Pts',(69.2807493616506,242.245816755679,7.17267980084179)) ;
#70739 = CARTESIAN_POINT('Ctrl Pts',(69.4909429592547,242.355402012489,7.27867958886636)) ;
#70740 = CARTESIAN_POINT('Ctrl Pts',(69.5434105984377,242.338566553604,7.16316434207535)) ;
#70741 = CARTESIAN_POINT('Ctrl Pts',(69.6548363472646,242.318447141452,6.93376983755156)) ;
#70742 = CARTESIAN_POINT('Ctrl Pts',(69.8115179376631,242.335283243238,6.66059049824912)) ;
#70743 = CARTESIAN_POINT('Ctrl Pts',(69.9320961586154,242.382043605764,6.4924392790701)) ;
#70744 = CARTESIAN_POINT('Ctrl Pts',(70.0038423289643,242.42384128837,6.4112217229231)) ;
#70745 = CARTESIAN_POINT('Ctrl Pts',(70.0853128564862,242.483004335118,6.33512166788152)) ;
#70746 = CARTESIAN_POINT('Ctrl Pts',(70.1739356804575,242.581754164171,6.30139292105391)) ;
#70747 = CARTESIAN_POINT('Ctrl Pts',(70.2630551704512,242.761871347334,6.38459950069724)) ;
#70748 = CARTESIAN_POINT('Ctrl Pts',(70.2766922354173,242.880428587697,6.52710936966954)) ;
#70749 = CARTESIAN_POINT('Ctrl Pts',(70.2731493424206,242.966128315359,6.65331963180678)) ;
#70750 = CARTESIAN_POINT('Ctrl Pts',(70.2672749757801,243.03292209962,6.75725826388023)) ;
#70751 = CARTESIAN_POINT('Ctrl Pts',(70.2400533595442,243.145774108243,6.96268987067883)) ;
#70752 = CARTESIAN_POINT('Ctrl Pts',(70.1931792067253,243.232912339636,7.16318512433994)) ;
#70753 = CARTESIAN_POINT('Ctrl Pts',(70.1609601392448,243.277601545414,7.27867958884205)) ;
#70754 = CARTESIAN_POINT('Origin',(77.0279509268838,244.633742383918,7.2786795888419)) ;
#70755 = CARTESIAN_POINT('',(76.8665793939902,244.751891562381,7.27867958883744)) ;
#70756 = CARTESIAN_POINT('Origin',(77.0279509268838,244.633742383918,7.2786795888419)) ;
#70757 = CARTESIAN_POINT('',(77.1010421843896,244.786783924096,7.1726798008414)) ;
#70758 = CARTESIAN_POINT('Origin',(77.0279509268838,244.633742383918,7.2786795888419)) ;
#70759 = CARTESIAN_POINT('Origin',(77.0279509268823,244.633742383915,7.27867958883784)) ;
#70760 = CARTESIAN_POINT('Origin',(69.2946204451421,241.899588097824,7.2786795888419)) ;
#70761 = CARTESIAN_POINT('',(69.1764712666787,241.738216564931,7.27867958883751)) ;
#70762 = CARTESIAN_POINT('Origin',(69.2946204451421,241.899588097824,7.2786795888419)) ;
#70763 = CARTESIAN_POINT('',(69.141578904964,241.97267935533,7.17267980084143)) ;
#70764 = CARTESIAN_POINT('Origin',(69.2946204451421,241.899588097824,7.2786795888419)) ;
#70765 = CARTESIAN_POINT('Origin',(69.2946204451441,241.899588097823,7.27867958883792)) ;
#70766 = CARTESIAN_POINT('Origin',(74.5283628290597,239.4,7.2786795888419)) ;
#70767 = CARTESIAN_POINT('Origin',(74.5283628290597,239.4,7.17267980084126)) ;
#70768 = CARTESIAN_POINT('Origin',(77.2933283411274,244.498525837657,7.27867958886636)) ;
#70769 = CARTESIAN_POINT('',(77.4837648414508,244.437419869498,7.27867958819177)) ;
#70770 = CARTESIAN_POINT('Origin',(77.2933283411226,244.498525837642,7.27867958812533)) ;
#70771 = CARTESIAN_POINT('',(77.3741795847345,244.647613467411,7.17267980084127)) ;
#70772 = CARTESIAN_POINT('Origin',(77.2933283411274,244.498525837657,7.27867958886636)) ;
#70773 = CARTESIAN_POINT('Origin',(77.2933283411226,244.498525837642,7.2786795888419)) ;
#70774 = CARTESIAN_POINT('Origin',(68.8249552755829,240.454107337488,7.27867958884205)) ;
#70775 = CARTESIAN_POINT('',(68.8242223895113,240.654105994678,7.27867958883789)) ;
#70776 = CARTESIAN_POINT('Origin',(68.824955275583,240.454107337488,7.27867958883748)) ;
#70777 = CARTESIAN_POINT('',(68.6581801055003,240.48493082833,7.17267980084126)) ;
#70778 = CARTESIAN_POINT('Origin',(68.8249552755829,240.454107337488,7.27867958884205)) ;
#70779 = CARTESIAN_POINT('Origin',(68.824955275583,240.454107337488,7.2786795888419)) ;
#70780 = CARTESIAN_POINT('Ctrl Pts',(68.823478978367,240.65410371336,7.28036633815045)) ;
#70781 = CARTESIAN_POINT('Ctrl Pts',(68.8788199964157,240.654238914554,7.16431454328368)) ;
#70782 = CARTESIAN_POINT('Ctrl Pts',(68.9912316969021,240.669605262881,6.93452062458097)) ;
#70783 = CARTESIAN_POINT('Ctrl Pts',(69.1352415531504,240.73427548165,6.66105171324341)) ;
#70784 = CARTESIAN_POINT('Ctrl Pts',(69.2496672165496,240.827807397918,6.46924271771741)) ;
#70785 = CARTESIAN_POINT('Ctrl Pts',(69.3181848499291,240.911256512681,6.37322074285091)) ;
#70786 = CARTESIAN_POINT('Ctrl Pts',(69.3655488171773,240.996556047987,6.32731305663253)) ;
#70787 = CARTESIAN_POINT('Ctrl Pts',(69.3941022131729,241.068181512082,6.31494113130069)) ;
#70788 = CARTESIAN_POINT('Ctrl Pts',(69.413116155554,241.142937408252,6.32730060289559)) ;
#70789 = CARTESIAN_POINT('Ctrl Pts',(69.4249419942325,241.239765149908,6.37317673297408)) ;
#70790 = CARTESIAN_POINT('Ctrl Pts',(69.4185389338756,241.347617143788,6.46930275432656)) ;
#70791 = CARTESIAN_POINT('Ctrl Pts',(69.3809619428502,241.490548424926,6.66107020782191)) ;
#70792 = CARTESIAN_POINT('Ctrl Pts',(69.3024638526453,241.627509960403,6.93454546811374)) ;
#70793 = CARTESIAN_POINT('Ctrl Pts',(69.2205648017604,241.706016476848,7.16431125123397)) ;
#70794 = CARTESIAN_POINT('Ctrl Pts',(69.1758711574328,241.738655389459,7.28036638463671)) ;
#70795 = CARTESIAN_POINT('Ctrl Pts',(68.7780040901399,240.654014301732,7.25145035187167)) ;
#70796 = CARTESIAN_POINT('Ctrl Pts',(68.8361499763342,240.649853313117,7.13668818254113)) ;
#70797 = CARTESIAN_POINT('Ctrl Pts',(68.9558559523436,240.658260475784,6.90908120499668)) ;
#70798 = CARTESIAN_POINT('Ctrl Pts',(69.112073402727,240.719105343023,6.63766971564194)) ;
#70799 = CARTESIAN_POINT('Ctrl Pts',(69.2372083217771,240.814333745853,6.44712593764351)) ;
#70800 = CARTESIAN_POINT('Ctrl Pts',(69.3122241176583,240.90152651754,6.35169043930914)) ;
#70801 = CARTESIAN_POINT('Ctrl Pts',(69.3637764481677,240.991827836744,6.30605413587496)) ;
#70802 = CARTESIAN_POINT('Ctrl Pts',(69.3945159315641,241.068042932172,6.29375442711715)) ;
#70803 = CARTESIAN_POINT('Ctrl Pts',(69.414463970372,241.14780971815,6.30604175826672)) ;
#70804 = CARTESIAN_POINT('Ctrl Pts',(69.4258401804862,241.251136693392,6.35164665503157)) ;
#70805 = CARTESIAN_POINT('Ctrl Pts',(69.4163843073265,241.36586689815,6.44718573025484)) ;
#70806 = CARTESIAN_POINT('Ctrl Pts',(69.371131407933,241.516431939832,6.63768809472266)) ;
#70807 = CARTESIAN_POINT('Ctrl Pts',(69.2805145667129,241.657492172259,6.90910596666903)) ;
#70808 = CARTESIAN_POINT('Ctrl Pts',(69.1886219438466,241.734645309753,7.13668492609714)) ;
#70809 = CARTESIAN_POINT('Ctrl Pts',(69.1391337530583,241.765457193289,7.25145039784871)) ;
#70810 = CARTESIAN_POINT('Ctrl Pts',(68.6991046675913,240.613567029917,7.20122166120201)) ;
#70811 = CARTESIAN_POINT('Ctrl Pts',(68.7657033479242,240.607047577728,7.08855078925677)) ;
#70812 = CARTESIAN_POINT('Ctrl Pts',(68.9025872549629,240.61314163398,6.86454768292916)) ;
#70813 = CARTESIAN_POINT('Ctrl Pts',(69.0806405675914,240.67860356143,6.59660315772466)) ;
#70814 = CARTESIAN_POINT('Ctrl Pts',(69.2227090288745,240.783604097628,6.40822147676959)) ;
#70815 = CARTESIAN_POINT('Ctrl Pts',(69.3076059616354,240.880485387066,6.31379600947305)) ;
#70816 = CARTESIAN_POINT('Ctrl Pts',(69.365700953512,240.981120970982,6.26862892350856)) ;
#70817 = CARTESIAN_POINT('Ctrl Pts',(69.4001749811632,241.066198804175,6.25645417405324)) ;
#70818 = CARTESIAN_POINT('Ctrl Pts',(69.4223088609324,241.155321559545,6.26861663959037)) ;
#70819 = CARTESIAN_POINT('Ctrl Pts',(69.4344701867662,241.270860282556,6.31375261664818)) ;
#70820 = CARTESIAN_POINT('Ctrl Pts',(69.4227020381915,241.399218428313,6.40828062353936)) ;
#70821 = CARTESIAN_POINT('Ctrl Pts',(69.3695104139579,241.567684448781,6.59662156925732)) ;
#70822 = CARTESIAN_POINT('Ctrl Pts',(69.2639336121494,241.725291673058,6.86457223317537)) ;
#70823 = CARTESIAN_POINT('Ctrl Pts',(69.1567902570243,241.810683344395,7.08854759093498)) ;
#70824 = CARTESIAN_POINT('Ctrl Pts',(69.099077085805,241.844555641315,7.20122170635049)) ;
#70825 = CARTESIAN_POINT('Ctrl Pts',(68.6623516026379,240.524842467592,7.1777195209085)) ;
#70826 = CARTESIAN_POINT('Ctrl Pts',(68.7349260692677,240.52314980779,7.06324272629545)) ;
#70827 = CARTESIAN_POINT('Ctrl Pts',(68.8827380168196,240.540035758777,6.83622590255729)) ;
#70828 = CARTESIAN_POINT('Ctrl Pts',(69.0728764366945,240.622376363191,6.56553617725173)) ;
#70829 = CARTESIAN_POINT('Ctrl Pts',(69.2242737408035,240.744355820845,6.37550092461942)) ;
#70830 = CARTESIAN_POINT('Ctrl Pts',(69.315021033008,240.854064083064,6.2803201868701)) ;
#70831 = CARTESIAN_POINT('Ctrl Pts',(69.3777411120263,240.966598605412,6.23480565964425)) ;
#70832 = CARTESIAN_POINT('Ctrl Pts',(69.415512997241,241.061210952531,6.2225387622577)) ;
#70833 = CARTESIAN_POINT('Ctrl Pts',(69.4405843624923,241.159989075466,6.23479331069613)) ;
#70834 = CARTESIAN_POINT('Ctrl Pts',(69.4559976225698,241.28787069269,6.28027651889111)) ;
#70835 = CARTESIAN_POINT('Ctrl Pts',(69.4470369050469,241.430051431758,6.37556053614025)) ;
#70836 = CARTESIAN_POINT('Ctrl Pts',(69.3962783214387,241.617736510688,6.56555452752839)) ;
#70837 = CARTESIAN_POINT('Ctrl Pts',(69.2908455632846,241.796102429654,6.83625059124941)) ;
#70838 = CARTESIAN_POINT('Ctrl Pts',(69.1812048429608,241.896648294788,7.06323947800677)) ;
#70839 = CARTESIAN_POINT('Ctrl Pts',(69.1214942201225,241.93793823252,7.17771956677077)) ;
#70840 = CARTESIAN_POINT('Ctrl Pts',(68.6571253579994,240.484922057358,7.17433674456111)) ;
#70841 = CARTESIAN_POINT('Ctrl Pts',(68.7309893897257,240.48548685222,7.05828627896513)) ;
#70842 = CARTESIAN_POINT('Ctrl Pts',(68.8811399119051,240.507354683134,6.82849461444546)) ;
#70843 = CARTESIAN_POINT('Ctrl Pts',(69.0739290706077,240.597304732332,6.55502782380495)) ;
#70844 = CARTESIAN_POINT('Ctrl Pts',(69.2276518090002,240.726855840636,6.36322013241374)) ;
#70845 = CARTESIAN_POINT('Ctrl Pts',(69.320093824317,240.842215057189,6.26719876206499)) ;
#70846 = CARTESIAN_POINT('Ctrl Pts',(69.3844106748995,240.959918688398,6.22129135557805)) ;
#70847 = CARTESIAN_POINT('Ctrl Pts',(69.4234866951096,241.058618246624,6.20891950468442)) ;
#70848 = CARTESIAN_POINT('Ctrl Pts',(69.4499063975124,241.16147279248,6.22127890191958)) ;
#70849 = CARTESIAN_POINT('Ctrl Pts',(69.4670654246099,241.294472860653,6.26715475242069)) ;
#70850 = CARTESIAN_POINT('Ctrl Pts',(69.460057572545,241.442227922388,6.36328016877133)) ;
#70851 = CARTESIAN_POINT('Ctrl Pts',(69.4118663483261,241.63739962514,6.55504631826445)) ;
#70852 = CARTESIAN_POINT('Ctrl Pts',(69.308762748304,241.823482930368,6.82851945789384)) ;
#70853 = CARTESIAN_POINT('Ctrl Pts',(69.2001577213478,241.929432109674,7.05828298695213)) ;
#70854 = CARTESIAN_POINT('Ctrl Pts',(69.1407307279281,241.973306433417,7.17433679104683)) ;
#70855 = CARTESIAN_POINT('Ctrl Pts',(69.141578904964,241.97267935533,7.17267980084139)) ;
#70856 = CARTESIAN_POINT('Ctrl Pts',(69.20067570445,241.928926404034,7.05718689586838)) ;
#70857 = CARTESIAN_POINT('Ctrl Pts',(69.3089595963666,241.823127655304,6.8279973358951)) ;
#70858 = CARTESIAN_POINT('Ctrl Pts',(69.4118663483261,241.63739962514,6.55504631826448)) ;
#70859 = CARTESIAN_POINT('Ctrl Pts',(69.4600575725451,241.442227922388,6.36328016877132)) ;
#70860 = CARTESIAN_POINT('Ctrl Pts',(69.4670654246099,241.294472860653,6.2671547524207)) ;
#70861 = CARTESIAN_POINT('Ctrl Pts',(69.4499063975123,241.16147279248,6.22127890191957)) ;
#70862 = CARTESIAN_POINT('Ctrl Pts',(69.4234866951097,241.058618246625,6.20891950468443)) ;
#70863 = CARTESIAN_POINT('Ctrl Pts',(69.3844106748994,240.959918688398,6.22129135557804)) ;
#70864 = CARTESIAN_POINT('Ctrl Pts',(69.320093824317,240.84221505719,6.26719876206501)) ;
#70865 = CARTESIAN_POINT('Ctrl Pts',(69.2276518090002,240.726855840635,6.36322013241375)) ;
#70866 = CARTESIAN_POINT('Ctrl Pts',(69.0739290706076,240.597304732333,6.55502782380495)) ;
#70867 = CARTESIAN_POINT('Ctrl Pts',(68.8815079899584,240.507526418096,6.82797250456833)) ;
#70868 = CARTESIAN_POINT('Ctrl Pts',(68.7317057496143,240.485591464222,7.05719005384199)) ;
#70869 = CARTESIAN_POINT('Ctrl Pts',(68.6581801055003,240.48493082833,7.17267980084126)) ;
#70870 = CARTESIAN_POINT('Ctrl Pts',(68.8242223895114,240.654105994679,7.27867958883793)) ;
#70871 = CARTESIAN_POINT('Ctrl Pts',(68.846136652679,240.654186298509,7.23273887151479)) ;
#70872 = CARTESIAN_POINT('Ctrl Pts',(68.8681968853879,240.655463750951,7.18693755682195)) ;
#70873 = CARTESIAN_POINT('Ctrl Pts',(68.8904046060548,240.658011322165,7.14139111650319)) ;
#70874 = CARTESIAN_POINT('Ctrl Pts',(68.9117833995295,240.660463802528,7.09754474632908)) ;
#70875 = CARTESIAN_POINT('Ctrl Pts',(68.9332997260423,240.664093734056,7.05393457870595)) ;
#70876 = CARTESIAN_POINT('Ctrl Pts',(68.9549311097582,240.669007419404,7.01066363168771)) ;
#70877 = CARTESIAN_POINT('Ctrl Pts',(68.9673169131455,240.671820921372,6.98588734140569)) ;
#70878 = CARTESIAN_POINT('Ctrl Pts',(68.9797399341188,240.675056046509,6.96122226577)) ;
#70879 = CARTESIAN_POINT('Ctrl Pts',(68.9921905637294,240.678738386296,6.93668774373476)) ;
#70880 = CARTESIAN_POINT('Ctrl Pts',(69.0096876499474,240.683913242409,6.90220895344093)) ;
#70881 = CARTESIAN_POINT('Ctrl Pts',(69.0272213641983,240.68996292711,6.86798799566502)) ;
#70882 = CARTESIAN_POINT('Ctrl Pts',(69.0448122049251,240.696997581045,6.83420433559753)) ;
#70883 = CARTESIAN_POINT('Ctrl Pts',(69.0619154995078,240.70383726315,6.80135702038434)) ;
#70884 = CARTESIAN_POINT('Ctrl Pts',(69.0790734570707,240.711608425905,6.76892309859212)) ;
#70885 = CARTESIAN_POINT('Ctrl Pts',(69.0962696297009,240.720445534448,6.73706752304788)) ;
#70886 = CARTESIAN_POINT('Ctrl Pts',(69.1127093625799,240.728893908803,6.70661323743941)) ;
#70887 = CARTESIAN_POINT('Ctrl Pts',(69.1291845017098,240.73831699583,6.67668753562406)) ;
#70888 = CARTESIAN_POINT('Ctrl Pts',(69.1456400045051,240.748856968541,6.64743454569603)) ;
#70889 = CARTESIAN_POINT('Ctrl Pts',(69.1517207684508,240.752751780317,6.63662475588462)) ;
#70890 = CARTESIAN_POINT('Ctrl Pts',(69.1577984019575,240.756799317963,6.62590682536183)) ;
#70891 = CARTESIAN_POINT('Ctrl Pts',(69.1638684211109,240.76100744383,6.61528802672607)) ;
#70892 = CARTESIAN_POINT('Ctrl Pts',(69.1782061081319,240.770947246342,6.59020589641802)) ;
#70893 = CARTESIAN_POINT('Ctrl Pts',(69.1925055813629,240.781780951008,6.56567685055204)) ;
#70894 = CARTESIAN_POINT('Ctrl Pts',(69.2067372272363,240.793672247361,6.54202080782637)) ;
#70895 = CARTESIAN_POINT('Ctrl Pts',(69.219775148156,240.804566123085,6.52034899157445)) ;
#70896 = CARTESIAN_POINT('Ctrl Pts',(69.2327562318609,240.816348281174,6.49940986864529)) ;
#70897 = CARTESIAN_POINT('Ctrl Pts',(69.245611680359,240.829162853668,6.47944941873786)) ;
#70898 = CARTESIAN_POINT('Ctrl Pts',(69.2467886985169,240.830336129303,6.47762188141132)) ;
#70899 = CARTESIAN_POINT('Ctrl Pts',(69.2479646283666,240.83151806915,6.47580254815704)) ;
#70900 = CARTESIAN_POINT('Ctrl Pts',(69.2491393952322,240.83270878926,6.47399160776851)) ;
#70901 = CARTESIAN_POINT('Ctrl Pts',(69.2620888106481,240.845834056741,6.45402967313127)) ;
#70902 = CARTESIAN_POINT('Ctrl Pts',(69.2748961857949,240.860021506773,6.43508752022125)) ;
#70903 = CARTESIAN_POINT('Ctrl Pts',(69.2874067034248,240.875395365772,6.41771166031512)) ;
#70904 = CARTESIAN_POINT('Ctrl Pts',(69.299351774167,240.890074361378,6.40112114968035)) ;
#70905 = CARTESIAN_POINT('Ctrl Pts',(69.3110262930533,240.905835564842,6.38595854597711)) ;
#70906 = CARTESIAN_POINT('Ctrl Pts',(69.3222483340953,240.922778337834,6.37269955612442)) ;
#70907 = CARTESIAN_POINT('Ctrl Pts',(69.3246968500832,240.926475049545,6.36980660211394)) ;
#70908 = CARTESIAN_POINT('Ctrl Pts',(69.3271236375482,240.930227955764,6.36700427164681)) ;
#70909 = CARTESIAN_POINT('Ctrl Pts',(69.3295264854414,240.934037981198,6.36429750592655)) ;
#70910 = CARTESIAN_POINT('Ctrl Pts',(69.3387699425403,240.948694675342,6.35388491473295)) ;
#70911 = CARTESIAN_POINT('Ctrl Pts',(69.347660159287,240.96420569066,6.34488653389899)) ;
#70912 = CARTESIAN_POINT('Ctrl Pts',(69.3559890267521,240.980457921475,6.33775012566548)) ;
#70913 = CARTESIAN_POINT('Ctrl Pts',(69.3589006596617,240.986139429831,6.33525535658002)) ;
#70914 = CARTESIAN_POINT('Ctrl Pts',(69.3617439552097,240.99191114303,6.33298813633262)) ;
#70915 = CARTESIAN_POINT('Ctrl Pts',(69.3645109707409,240.997767038799,6.3309675942406)) ;
#70916 = CARTESIAN_POINT('Ctrl Pts',(69.3711177208506,241.011749049227,6.32614318449746)) ;
#70917 = CARTESIAN_POINT('Ctrl Pts',(69.3772873424095,241.026215350409,6.32272509186126)) ;
#70918 = CARTESIAN_POINT('Ctrl Pts',(69.3829030519906,241.040995449201,6.32081869565777)) ;
#70919 = CARTESIAN_POINT('Ctrl Pts',(69.3863671653803,241.050112718779,6.31964271379489)) ;
#70920 = CARTESIAN_POINT('Ctrl Pts',(69.3896213529679,241.059348834208,6.31904195925508)) ;
#70921 = CARTESIAN_POINT('Ctrl Pts',(69.3926471329311,241.06865943203,6.31904116737318)) ;
#70922 = CARTESIAN_POINT('Ctrl Pts',(69.3975225423784,241.08366150658,6.31903989142167)) ;
#70923 = CARTESIAN_POINT('Ctrl Pts',(69.4018030292884,241.098859895763,6.3205962720868)) ;
#70924 = CARTESIAN_POINT('Ctrl Pts',(69.4054500916838,241.114053110503,6.32360639934854)) ;
#70925 = CARTESIAN_POINT('Ctrl Pts',(69.4077357611952,241.123574929421,6.32549289191755)) ;
#70926 = CARTESIAN_POINT('Ctrl Pts',(69.4097736671126,241.133094421285,6.32795037539676)) ;
#70927 = CARTESIAN_POINT('Ctrl Pts',(69.4115646430805,241.142560434417,6.33095327169366)) ;
#70928 = CARTESIAN_POINT('Ctrl Pts',(69.4150396945331,241.160927449538,6.33677982622377)) ;
#70929 = CARTESIAN_POINT('Ctrl Pts',(69.4175839820238,241.179095664348,6.34465975590413)) ;
#70930 = CARTESIAN_POINT('Ctrl Pts',(69.419285579022,241.196845654439,6.35413807111322)) ;
#70931 = CARTESIAN_POINT('Ctrl Pts',(69.4198602664029,241.20284043189,6.35733922164867)) ;
#70932 = CARTESIAN_POINT('Ctrl Pts',(69.4203392605828,241.208787630448,6.360722690978)) ;
#70933 = CARTESIAN_POINT('Ctrl Pts',(69.4207272046842,241.214679245084,6.36427095134432)) ;
#70934 = CARTESIAN_POINT('Ctrl Pts',(69.4220878086829,241.235342413832,6.37671546905823)) ;
#70935 = CARTESIAN_POINT('Ctrl Pts',(69.4223321688101,241.255328098782,6.39118701019276)) ;
#70936 = CARTESIAN_POINT('Ctrl Pts',(69.4216735910866,241.274596981359,6.40719997765687)) ;
#70937 = CARTESIAN_POINT('Ctrl Pts',(69.4209847045839,241.294752648119,6.42394988698749)) ;
#70938 = CARTESIAN_POINT('Ctrl Pts',(69.4193082317437,241.31412462535,6.44238636507748)) ;
#70939 = CARTESIAN_POINT('Ctrl Pts',(69.4168519322734,241.332711197981,6.46195363822342)) ;
#70940 = CARTESIAN_POINT('Ctrl Pts',(69.4163524690264,241.336490586459,6.46593244206969)) ;
#70941 = CARTESIAN_POINT('Ctrl Pts',(69.4158206373757,241.340237620289,6.46995800094641)) ;
#70942 = CARTESIAN_POINT('Ctrl Pts',(69.4152579931402,241.343952456318,6.47402564218845)) ;
#70943 = CARTESIAN_POINT('Ctrl Pts',(69.4125278222751,241.361978300102,6.4937634354645)) ;
#70944 = CARTESIAN_POINT('Ctrl Pts',(69.4090772342052,241.379237445774,6.51449208817806)) ;
#70945 = CARTESIAN_POINT('Ctrl Pts',(69.405050494928,241.395805152101,6.53597027769904)) ;
#70946 = CARTESIAN_POINT('Ctrl Pts',(69.4008468772236,241.413100610993,6.55839191752057)) ;
#70947 = CARTESIAN_POINT('Ctrl Pts',(69.3960153407041,241.429643264669,6.58163038863598)) ;
#70948 = CARTESIAN_POINT('Ctrl Pts',(69.3906659501294,241.445533486518,6.60541115008098)) ;
#70949 = CARTESIAN_POINT('Ctrl Pts',(69.3899251894502,241.447733896333,6.60870420800095)) ;
#70950 = CARTESIAN_POINT('Ctrl Pts',(69.389174418218,241.449921807944,6.6120076646218)) ;
#70951 = CARTESIAN_POINT('Ctrl Pts',(69.3884138526593,241.452097497548,6.61532079094276)) ;
#70952 = CARTESIAN_POINT('Ctrl Pts',(69.3817662594347,241.471113740534,6.64427860507523)) ;
#70953 = CARTESIAN_POINT('Ctrl Pts',(69.3743746279503,241.489195694726,6.67397512000546)) ;
#70954 = CARTESIAN_POINT('Ctrl Pts',(69.366389151171,241.506423764033,6.70426221644862)) ;
#70955 = CARTESIAN_POINT('Ctrl Pts',(69.3581585948493,241.524180574135,6.73547884383175)) ;
#70956 = CARTESIAN_POINT('Ctrl Pts',(69.3492969611863,241.541031083459,6.7673228596776)) ;
#70957 = CARTESIAN_POINT('Ctrl Pts',(69.3399127997696,241.557072117829,6.79963208423623)) ;
#70958 = CARTESIAN_POINT('Ctrl Pts',(69.3301475774069,241.573764527582,6.83325328363505)) ;
#70959 = CARTESIAN_POINT('Ctrl Pts',(69.3198162940651,241.589581162529,6.86737824012789)) ;
#70960 = CARTESIAN_POINT('Ctrl Pts',(69.3089851119557,241.60462816176,6.90182420403309)) ;
#70961 = CARTESIAN_POINT('Ctrl Pts',(69.3053399164247,241.609692175438,6.9134168697661)) ;
#70962 = CARTESIAN_POINT('Ctrl Pts',(69.3016376626116,241.614668941972,6.92504589391921)) ;
#70963 = CARTESIAN_POINT('Ctrl Pts',(69.2978796019434,241.619562210823,6.93670431036293)) ;
#70964 = CARTESIAN_POINT('Ctrl Pts',(69.2841507989065,241.637438112838,6.97929438998378)) ;
#70965 = CARTESIAN_POINT('Ctrl Pts',(69.2697003402215,241.654174836329,7.02227672706127)) ;
#70966 = CARTESIAN_POINT('Ctrl Pts',(69.2546360794563,241.669850154716,7.06555154403451)) ;
#70967 = CARTESIAN_POINT('Ctrl Pts',(69.238971885953,241.686149741152,7.11054977643727)) ;
#70968 = CARTESIAN_POINT('Ctrl Pts',(69.2226435914711,241.701302627729,7.15586424858313)) ;
#70969 = CARTESIAN_POINT('Ctrl Pts',(69.2057177073066,241.715381634963,7.20138278096512)) ;
#70970 = CARTESIAN_POINT('Ctrl Pts',(69.1961585686188,241.723332958594,7.22709003263231)) ;
#70971 = CARTESIAN_POINT('Ctrl Pts',(69.1864078798304,241.73094141138,7.25286237113867)) ;
#70972 = CARTESIAN_POINT('Ctrl Pts',(69.1764712666801,241.73821656493,7.27867958883835)) ;
#70973 = CARTESIAN_POINT('Origin',(78.5229277183602,243.60516959767,7.2786795888419)) ;
#70974 = CARTESIAN_POINT('',(78.4059643744738,243.767402689815,7.27867958883747)) ;
#70975 = CARTESIAN_POINT('Origin',(78.5229277183602,243.60516959767,7.2786795888419)) ;
#70976 = CARTESIAN_POINT('',(78.6397340718556,243.728134311011,7.17267980084143)) ;
#70977 = CARTESIAN_POINT('Origin',(78.5229277183602,243.60516959767,7.2786795888419)) ;
#70978 = CARTESIAN_POINT('Origin',(78.5229277183581,243.605169597668,7.27867958883789)) ;
#70979 = CARTESIAN_POINT('Origin',(68.7783628290597,240.159934207678,7.2786795888419)) ;
#70980 = CARTESIAN_POINT('',(68.7158628290597,239.969950655759,7.27867958883747)) ;
#70981 = CARTESIAN_POINT('Origin',(68.7783628290597,240.159934207678,7.2786795888419)) ;
#70982 = CARTESIAN_POINT('',(68.6102252343,240.182155687653,7.17267980084141)) ;
#70983 = CARTESIAN_POINT('Origin',(68.7783628290597,240.159934207678,7.2786795888419)) ;
#70984 = CARTESIAN_POINT('Origin',(68.7783628290621,240.159934207678,7.27867958883788)) ;
#70985 = CARTESIAN_POINT('Origin',(74.5283628290597,239.4,7.2786795888419)) ;
#70986 = CARTESIAN_POINT('Origin',(74.5283628290597,239.4,7.17267980084126)) ;
#70987 = CARTESIAN_POINT('Origin',(78.7335324267387,243.394564889313,7.27867958886638)) ;
#70988 = CARTESIAN_POINT('',(78.8957655186932,243.277601545162,7.27867958819176)) ;
#70989 = CARTESIAN_POINT('Origin',(78.7335324267296,243.3945648893,7.27867958812535)) ;
#70990 = CARTESIAN_POINT('',(78.8564971400671,243.511371242799,7.17267980084127)) ;
#70991 = CARTESIAN_POINT('Origin',(78.7335324267387,243.394564889313,7.27867958886638)) ;
#70992 = CARTESIAN_POINT('Origin',(78.7335324267296,243.3945648893,7.2786795888419)) ;
#70993 = CARTESIAN_POINT('Origin',(68.7783628290596,238.640065792321,7.27867958884205)) ;
#70994 = CARTESIAN_POINT('',(68.7158628290615,238.830049344242,7.27867958883789)) ;
#70995 = CARTESIAN_POINT('Origin',(68.7783628290597,238.640065792321,7.27867958883748)) ;
#70996 = CARTESIAN_POINT('',(68.6102252343,238.617844312347,7.17267980084126)) ;
#70997 = CARTESIAN_POINT('Origin',(68.7783628290596,238.640065792321,7.27867958884205)) ;
#70998 = CARTESIAN_POINT('Origin',(68.7783628290597,238.640065792321,7.2786795888419)) ;
#70999 = CARTESIAN_POINT('Ctrl Pts',(68.7151564547179,238.829817430435,7.28036646542746)) ;
#71000 = CARTESIAN_POINT('Ctrl Pts',(68.7677472638065,238.847047374589,7.16431433428589)) ;
#71001 = CARTESIAN_POINT('Ctrl Pts',(68.8699090234134,238.896398863056,6.9345196468735)) ;
#71002 = CARTESIAN_POINT('Ctrl Pts',(68.9868866279225,239.002405841546,6.66105002053093)) ;
#71003 = CARTESIAN_POINT('Ctrl Pts',(69.0668090557642,239.126720084162,6.46924073836522)) ;
#71004 = CARTESIAN_POINT('Ctrl Pts',(69.1061859143773,239.227258632282,6.37321895942679)) ;
#71005 = CARTESIAN_POINT('Ctrl Pts',(69.1248724477467,239.323020115618,6.32731193280284)) ;
#71006 = CARTESIAN_POINT('Ctrl Pts',(69.1298945349666,239.399963762342,6.31494079700328)) ;
#71007 = CARTESIAN_POINT('Ctrl Pts',(69.124876650076,239.476936565362,6.327301195844)) ;
#71008 = CARTESIAN_POINT('Ctrl Pts',(69.1062018481551,239.572679465908,6.37317836881852)) ;
#71009 = CARTESIAN_POINT('Ctrl Pts',(69.0667835939042,239.673273882465,6.46930552948702)) ;
#71010 = CARTESIAN_POINT('Ctrl Pts',(68.9868773192842,239.797597092518,6.66107350241436)) ;
#71011 = CARTESIAN_POINT('Ctrl Pts',(68.8698963856411,239.903598102475,6.93455177394916)) ;
#71012 = CARTESIAN_POINT('Ctrl Pts',(68.7677473243042,239.952952639913,7.1643141804926)) ;
#71013 = CARTESIAN_POINT('Ctrl Pts',(68.7151564542834,239.97018256946,7.28036646653197)) ;
#71014 = CARTESIAN_POINT('Ctrl Pts',(68.6719348898594,238.815679885867,7.2514504770069)) ;
#71015 = CARTESIAN_POINT('Ctrl Pts',(68.7285208935238,238.829690652319,7.13668797515578)) ;
#71016 = CARTESIAN_POINT('Ctrl Pts',(68.8397705467902,238.87467760555,6.90908026728084)) ;
#71017 = CARTESIAN_POINT('Ctrl Pts',(68.9695404171102,238.980818841841,6.63766807130544)) ;
#71018 = CARTESIAN_POINT('Ctrl Pts',(69.0591237601837,239.110055937278,6.44712401885435)) ;
#71019 = CARTESIAN_POINT('Ctrl Pts',(69.1035238771675,239.216163012018,6.35168871470428)) ;
#71020 = CARTESIAN_POINT('Ctrl Pts',(69.1246481142455,239.317975797227,6.30605306835811)) ;
#71021 = CARTESIAN_POINT('Ctrl Pts',(69.1303309769686,239.399960004748,6.29375414423265)) ;
#71022 = CARTESIAN_POINT('Ctrl Pts',(69.1246529708336,239.481987102395,6.30604239722425)) ;
#71023 = CARTESIAN_POINT('Ctrl Pts',(69.1035421141245,239.583772178745,6.35164832951223)) ;
#71024 = CARTESIAN_POINT('Ctrl Pts',(69.0590949179342,239.689964746438,6.44718853433347)) ;
#71025 = CARTESIAN_POINT('Ctrl Pts',(68.9695294166725,239.819176040241,6.63769140569591)) ;
#71026 = CARTESIAN_POINT('Ctrl Pts',(68.8397561656441,239.925330127068,6.90911225122715)) ;
#71027 = CARTESIAN_POINT('Ctrl Pts',(68.7285209623689,239.970309310713,7.13668782204785)) ;
#71028 = CARTESIAN_POINT('Ctrl Pts',(68.6719348893648,239.984320114399,7.25145047810647)) ;
#71029 = CARTESIAN_POINT('Ctrl Pts',(68.6093959258621,238.752831004033,7.20122176499298)) ;
#71030 = CARTESIAN_POINT('Ctrl Pts',(68.6747498460143,238.767210795544,7.08855056705061)) ;
#71031 = CARTESIAN_POINT('Ctrl Pts',(68.8030514227131,238.815306131544,6.8645467034792)) ;
#71032 = CARTESIAN_POINT('Ctrl Pts',(68.9521617110681,238.932586154345,6.59660147265197)) ;
#71033 = CARTESIAN_POINT('Ctrl Pts',(69.0548300315723,239.076349928799,6.40821950545246)) ;
#71034 = CARTESIAN_POINT('Ctrl Pts',(69.1056337366415,239.194724847852,6.31379422957587)) ;
#71035 = CARTESIAN_POINT('Ctrl Pts',(69.1297869018418,239.308387963015,6.26862779205968)) ;
#71036 = CARTESIAN_POINT('Ctrl Pts',(69.1362827398811,239.39995521031,6.2564538196623)) ;
#71037 = CARTESIAN_POINT('Ctrl Pts',(69.1297923775911,239.491555834057,6.26861719768716)) ;
#71038 = CARTESIAN_POINT('Ctrl Pts',(69.1056545079565,239.605197565579,6.31375420105852)) ;
#71039 = CARTESIAN_POINT('Ctrl Pts',(69.0547968682434,239.723636495491,6.408283325731)) ;
#71040 = CARTESIAN_POINT('Ctrl Pts',(68.9521494703146,239.867419347135,6.59662477927506)) ;
#71041 = CARTESIAN_POINT('Ctrl Pts',(68.8030349447908,239.984687634551,6.86457837515914)) ;
#71042 = CARTESIAN_POINT('Ctrl Pts',(68.6747499248955,240.032789234252,7.08855041543658)) ;
#71043 = CARTESIAN_POINT('Ctrl Pts',(68.6093959252955,240.047168995753,7.20122176608181)) ;
#71044 = CARTESIAN_POINT('Ctrl Pts',(68.6018591141068,238.657091578019,7.17771964424042)) ;
#71045 = CARTESIAN_POINT('Ctrl Pts',(68.6714047962981,238.677908559888,7.06324251803697)) ;
#71046 = CARTESIAN_POINT('Ctrl Pts',(68.8067647486738,238.739644581446,6.83622495555726)) ;
#71047 = CARTESIAN_POINT('Ctrl Pts',(68.9621528761349,238.876711748343,6.56553452424404)) ;
#71048 = CARTESIAN_POINT('Ctrl Pts',(69.0684466966744,239.039506283962,6.37549899432774)) ;
#71049 = CARTESIAN_POINT('Ctrl Pts',(69.1208506659138,239.171888309829,6.28031845030118)) ;
#71050 = CARTESIAN_POINT('Ctrl Pts',(69.1457255676693,239.298297281133,6.23480457795015)) ;
#71051 = CARTESIAN_POINT('Ctrl Pts',(69.1524115152463,239.399951520372,6.22253846320574)) ;
#71052 = CARTESIAN_POINT('Ctrl Pts',(69.1457311807739,239.501642692904,6.23479393102029)) ;
#71053 = CARTESIAN_POINT('Ctrl Pts',(69.1208719019535,239.62802810922,6.28027817234562)) ;
#71054 = CARTESIAN_POINT('Ctrl Pts',(69.0684128446976,239.760480643033,6.37556331663666)) ;
#71055 = CARTESIAN_POINT('Ctrl Pts',(68.962140361611,239.923293707433,6.56555781595963)) ;
#71056 = CARTESIAN_POINT('Ctrl Pts',(68.8067479265598,240.060349330392,6.83625684756693)) ;
#71057 = CARTESIAN_POINT('Ctrl Pts',(68.6714048768271,240.12209146921,7.06324236536902)) ;
#71058 = CARTESIAN_POINT('Ctrl Pts',(68.6018591135284,240.142908421772,7.17771964533681)) ;
#71059 = CARTESIAN_POINT('Ctrl Pts',(68.6092247447017,238.61751001058,7.17433686958768)) ;
#71060 = CARTESIAN_POINT('Ctrl Pts',(68.679299286119,238.640872464225,7.05828606782104)) ;
#71061 = CARTESIAN_POINT('Ctrl Pts',(68.8153438440691,238.708069202037,6.82849363480124)) ;
#71062 = CARTESIAN_POINT('Ctrl Pts',(68.9709015206617,238.853192530671,6.55502612932433)) ;
#71063 = CARTESIAN_POINT('Ctrl Pts',(69.0770671806673,239.0239067636,6.36321815140438)) ;
#71064 = CARTESIAN_POINT('Ctrl Pts',(69.1293366859553,239.162186895062,6.26719697702747)) ;
#71065 = CARTESIAN_POINT('Ctrl Pts',(69.1541328649434,239.294005437406,6.22129023015348)) ;
#71066 = CARTESIAN_POINT('Ctrl Pts',(69.1607961026436,239.39994986084,6.20891916879272)) ;
#71067 = CARTESIAN_POINT('Ctrl Pts',(69.1541384307542,239.50593460718,6.2212794932625)) ;
#71068 = CARTESIAN_POINT('Ctrl Pts',(69.1293577894806,239.637727426768,6.26715638663095)) ;
#71069 = CARTESIAN_POINT('Ctrl Pts',(69.077033458404,239.776084919601,6.36328294224198)) ;
#71070 = CARTESIAN_POINT('Ctrl Pts',(68.9708891897341,239.94681152009,6.55504961105578)) ;
#71071 = CARTESIAN_POINT('Ctrl Pts',(68.8153271059694,240.091926611612,6.82852576172937)) ;
#71072 = CARTESIAN_POINT('Ctrl Pts',(68.6792993662451,240.159127555783,7.05828591402844)) ;
#71073 = CARTESIAN_POINT('Ctrl Pts',(68.6092247441262,240.182489989276,7.17433687069216)) ;
#71074 = CARTESIAN_POINT('',(69.1585759510679,239.399999978945,6.21304106630657)) ;
#71075 = CARTESIAN_POINT('Ctrl Pts',(68.6102252342999,240.182155687653,7.17267980084141)) ;
#71076 = CARTESIAN_POINT('Ctrl Pts',(68.6799483073472,240.158806652482,7.05718975930635)) ;
#71077 = CARTESIAN_POINT('Ctrl Pts',(68.8156241307394,240.091649533961,6.82800359598836)) ;
#71078 = CARTESIAN_POINT('Ctrl Pts',(68.9708891897341,239.94681152009,6.55504961105578)) ;
#71079 = CARTESIAN_POINT('Ctrl Pts',(69.077033458404,239.776084919601,6.36328294224198)) ;
#71080 = CARTESIAN_POINT('Ctrl Pts',(69.1293577894806,239.637727426768,6.26715638663095)) ;
#71081 = CARTESIAN_POINT('Ctrl Pts',(69.1541358935304,239.505948101095,6.22128419047529)) ;
#71082 = CARTESIAN_POINT('Ctrl Pts',(69.1585750605836,239.435307046742,6.21304265234076)) ;
#71083 = CARTESIAN_POINT('Ctrl Pts',(69.1585759510679,239.399999979053,6.21304106630657)) ;
#71084 = CARTESIAN_POINT('Ctrl Pts',(69.1585759510679,239.399999978837,6.21304106630656)) ;
#71085 = CARTESIAN_POINT('Ctrl Pts',(69.1585768422728,239.364663979398,6.21303947898959)) ;
#71086 = CARTESIAN_POINT('Ctrl Pts',(69.1563556683963,239.329334225001,6.21716334848777)) ;
#71087 = CARTESIAN_POINT('Ctrl Pts',(69.1479338201964,239.26105080182,6.23276691687198)) ;
#71088 = CARTESIAN_POINT('Ctrl Pts',(69.1293366859554,239.162186895062,6.26719697702748)) ;
#71089 = CARTESIAN_POINT('Ctrl Pts',(69.0770671806673,239.0239067636,6.36321815140438)) ;
#71090 = CARTESIAN_POINT('Ctrl Pts',(68.9709015206618,238.85319253067,6.55502612932432)) ;
#71091 = CARTESIAN_POINT('Ctrl Pts',(68.8156408604242,238.708346295415,6.82797148556704)) ;
#71092 = CARTESIAN_POINT('Ctrl Pts',(68.6799483073473,238.641193347518,7.05718975930627)) ;
#71093 = CARTESIAN_POINT('Ctrl Pts',(68.6102252343001,238.617844312347,7.17267980084128)) ;
#71094 = CARTESIAN_POINT('Ctrl Pts',(68.7158628290615,238.830049344242,7.27867958883784)) ;
#71095 = CARTESIAN_POINT('Ctrl Pts',(68.7366797982012,238.836897624306,7.23273869142603)) ;
#71096 = CARTESIAN_POINT('Ctrl Pts',(68.7572656540277,238.84492957757,7.18693718631418)) ;
#71097 = CARTESIAN_POINT('Ctrl Pts',(68.7775992891298,238.854215072605,7.14139055287856)) ;
#71098 = CARTESIAN_POINT('Ctrl Pts',(68.7971739401569,238.863153972315,7.09754401729895)) ;
#71099 = CARTESIAN_POINT('Ctrl Pts',(68.8165155389829,238.873255203555,7.05393368154921)) ;
#71100 = CARTESIAN_POINT('Ctrl Pts',(68.8355698580483,238.884612920864,7.01066257034807)) ;
#71101 = CARTESIAN_POINT('Ctrl Pts',(68.8464800190241,238.891116145867,6.98588630900877)) ;
#71102 = CARTESIAN_POINT('Ctrl Pts',(68.8572952869515,238.898031858053,6.96122126250497)) ;
#71103 = CARTESIAN_POINT('Ctrl Pts',(68.8679986147481,238.905381426673,6.93668677075398)) ;
#71104 = CARTESIAN_POINT('Ctrl Pts',(68.8830401948506,238.915709908359,6.90220800583574)) ;
#71105 = CARTESIAN_POINT('Ctrl Pts',(68.897846272571,238.926881718366,6.86798707596825)) ;
#71106 = CARTESIAN_POINT('Ctrl Pts',(68.9124023081378,238.939007940948,6.83420344555356)) ;
#71107 = CARTESIAN_POINT('Ctrl Pts',(68.9265549103273,238.950798074564,6.80135615828349)) ;
#71108 = CARTESIAN_POINT('Ctrl Pts',(68.9404716563316,238.963490988979,6.76892226610576)) ;
#71109 = CARTESIAN_POINT('Ctrl Pts',(68.9540953516258,238.977209485407,6.73706672113604)) ;
#71110 = CARTESIAN_POINT('Ctrl Pts',(68.9671197548697,238.990324519583,6.7066124681395)) ;
#71111 = CARTESIAN_POINT('Ctrl Pts',(68.9798766287053,239.004377499894,6.67668679969608)) ;
#71112 = CARTESIAN_POINT('Ctrl Pts',(68.9922696910491,239.019486631773,6.64743384323044)) ;
#71113 = CARTESIAN_POINT('Ctrl Pts',(68.9968494259556,239.025070063596,6.63662369944769)) ;
#71114 = CARTESIAN_POINT('Ctrl Pts',(69.0013789854125,239.030797788519,6.62590542119213)) ;
#71115 = CARTESIAN_POINT('Ctrl Pts',(69.0058516746882,239.036675899092,6.6152862817678)) ;
#71116 = CARTESIAN_POINT('Ctrl Pts',(69.016416069623,239.05055986861,6.59020410506638)) ;
#71117 = CARTESIAN_POINT('Ctrl Pts',(69.0266678867807,239.06528218644,6.56567501809567)) ;
#71118 = CARTESIAN_POINT('Ctrl Pts',(69.0365283781207,239.08098938145,6.54201894628589)) ;
#71119 = CARTESIAN_POINT('Ctrl Pts',(69.0455617472285,239.095379018364,6.52034720388181)) ;
#71120 = CARTESIAN_POINT('Ctrl Pts',(69.0542665659304,239.110595896997,6.49940815809408)) ;
#71121 = CARTESIAN_POINT('Ctrl Pts',(69.0625328641691,239.126755835211,6.47944779037588)) ;
#71122 = CARTESIAN_POINT('Ctrl Pts',(69.0632897511035,239.128235487377,6.47762015954337)) ;
#71123 = CARTESIAN_POINT('Ctrl Pts',(69.0640429251907,239.129723044254,6.47580073373255)) ;
#71124 = CARTESIAN_POINT('Ctrl Pts',(69.06479227953,239.13121859315,6.47398970176958)) ;
#71125 = CARTESIAN_POINT('Ctrl Pts',(69.0730519606016,239.147703126922,6.45402778837199)) ;
#71126 = CARTESIAN_POINT('Ctrl Pts',(69.0808483160851,239.165153969754,6.43508567072191)) ;
#71127 = CARTESIAN_POINT('Ctrl Pts',(69.0879957148478,239.183641424611,6.41770986762872)) ;
#71128 = CARTESIAN_POINT('Ctrl Pts',(69.094820068071,239.201293290182,6.40111940978772)) ;
#71129 = CARTESIAN_POINT('Ctrl Pts',(69.1010526832419,239.219890795336,6.38595687877681)) ;
#71130 = CARTESIAN_POINT('Ctrl Pts',(69.1064898316604,239.239472217782,6.37269798819665)) ;
#71131 = CARTESIAN_POINT('Ctrl Pts',(69.1076761643912,239.24374469309,6.36980502764829)) ;
#71132 = CARTESIAN_POINT('Ctrl Pts',(69.1088244658108,239.248063899034,6.36700269367533)) ;
#71133 = CARTESIAN_POINT('Ctrl Pts',(69.1099323472444,239.252430031787,6.3642959276952)) ;
#71134 = CARTESIAN_POINT('Ctrl Pts',(69.1141941375064,239.269225639588,6.35388355995823)) ;
#71135 = CARTESIAN_POINT('Ctrl Pts',(69.1178559830534,239.286724581721,6.34488538964452)) ;
#71136 = CARTESIAN_POINT('Ctrl Pts',(69.1207549168715,239.304754977569,6.33774916486814)) ;
#71137 = CARTESIAN_POINT('Ctrl Pts',(69.1217683854168,239.311058411934,6.33525433752933)) ;
#71138 = CARTESIAN_POINT('Ctrl Pts',(69.1226889787148,239.317426522997,6.33298707804794)) ;
#71139 = CARTESIAN_POINT('Ctrl Pts',(69.1235110032382,239.323851127572,6.3309665179532)) ;
#71140 = CARTESIAN_POINT('Ctrl Pts',(69.1254736522473,239.339190382601,6.32614226982525)) ;
#71141 = CARTESIAN_POINT('Ctrl Pts',(69.1268709134684,239.354855134897,6.32272434055556)) ;
#71142 = CARTESIAN_POINT('Ctrl Pts',(69.1276444073157,239.370647147276,6.32081810135888)) ;
#71143 = CARTESIAN_POINT('Ctrl Pts',(69.1281215532427,239.380388781824,6.31964219766971)) ;
#71144 = CARTESIAN_POINT('Ctrl Pts',(69.1283623161023,239.390178572222,6.31904153715748)) ;
#71145 = CARTESIAN_POINT('Ctrl Pts',(69.1283628282387,239.399968612813,6.31904085443174)) ;
#71146 = CARTESIAN_POINT('Ctrl Pts',(69.1283636534311,239.415743057411,6.31903975437303)) ;
#71147 = CARTESIAN_POINT('Ctrl Pts',(69.1277380059827,239.431520354394,6.3205963203152)) ;
#71148 = CARTESIAN_POINT('Ctrl Pts',(69.1265115351569,239.44709697861,6.32360663121809)) ;
#71149 = CARTESIAN_POINT('Ctrl Pts',(69.125742887679,239.456859080297,6.32549323775971)) ;
#71150 = CARTESIAN_POINT('Ctrl Pts',(69.1247393224569,239.466542400804,6.3279508338922)) ;
#71151 = CARTESIAN_POINT('Ctrl Pts',(69.1235174398229,239.476098549837,6.33095383885585)) ;
#71152 = CARTESIAN_POINT('Ctrl Pts',(69.1211465654452,239.494640779885,6.33678070579572)) ;
#71153 = CARTESIAN_POINT('Ctrl Pts',(69.1179518902521,239.512706283228,6.34466100445943)) ;
#71154 = CARTESIAN_POINT('Ctrl Pts',(69.1140849924868,239.530113593718,6.35413972745554)) ;
#71155 = CARTESIAN_POINT('Ctrl Pts',(69.1127790974153,239.535992239174,6.35734079932138)) ;
#71156 = CARTESIAN_POINT('Ctrl Pts',(69.1113969040053,239.541796070096,6.3607241697595)) ;
#71157 = CARTESIAN_POINT('Ctrl Pts',(69.1099453007327,239.547518909441,6.3642723138828)) ;
#71158 = CARTESIAN_POINT('Ctrl Pts',(69.1048539417821,239.567591218367,6.37671708834856)) ;
#71159 = CARTESIAN_POINT('Ctrl Pts',(69.098910326907,239.586674255091,6.3911888892425)) ;
#71160 = CARTESIAN_POINT('Ctrl Pts',(69.092329474663,239.604796539636,6.40720210496948)) ;
#71161 = CARTESIAN_POINT('Ctrl Pts',(69.0854457626439,239.623752836377,6.42395227067415)) ;
#71162 = CARTESIAN_POINT('Ctrl Pts',(69.0778649776355,239.641658609174,6.44238899189171)) ;
#71163 = CARTESIAN_POINT('Ctrl Pts',(69.069785243753,239.658576427517,6.46195647864843)) ;
#71164 = CARTESIAN_POINT('Ctrl Pts',(69.0681423609093,239.662016391496,6.46593520972473)) ;
#71165 = CARTESIAN_POINT('Ctrl Pts',(69.0664786935224,239.665415583934,6.46996069188013)) ;
#71166 = CARTESIAN_POINT('Ctrl Pts',(69.0647956726972,239.668774634716,6.47402825272209)) ;
#71167 = CARTESIAN_POINT('Ctrl Pts',(69.0566289234863,239.685074210408,6.49376582744493)) ;
#71168 = CARTESIAN_POINT('Ctrl Pts',(69.0480139653239,239.700422018716,6.5144941922125)) ;
#71169 = CARTESIAN_POINT('Ctrl Pts',(69.039064734617,239.714934221164,6.53597206760508)) ;
#71170 = CARTESIAN_POINT('Ctrl Pts',(69.0297224046819,239.730083879028,6.55839336892089)) ;
#71171 = CARTESIAN_POINT('Ctrl Pts',(69.0200155328915,239.744323575318,6.58163147222669)) ;
#71172 = CARTESIAN_POINT('Ctrl Pts',(69.01001776566,239.757782786127,6.60541188610505)) ;
#71173 = CARTESIAN_POINT('Ctrl Pts',(69.0086329381958,239.759647070856,6.6087057985843)) ;
#71174 = CARTESIAN_POINT('Ctrl Pts',(69.007242449196,239.761496368199,6.61201011585464)) ;
#71175 = CARTESIAN_POINT('Ctrl Pts',(69.0058464190132,239.763331007932,6.61532410844729)) ;
#71176 = CARTESIAN_POINT('Ctrl Pts',(68.9936472426615,239.779362963344,6.64428335342889)) ;
#71177 = CARTESIAN_POINT('Ctrl Pts',(68.9810291007366,239.794276365259,6.67398141534986)) ;
#71178 = CARTESIAN_POINT('Ctrl Pts',(68.968110015568,239.808194086138,6.70427010590999)) ;
#71179 = CARTESIAN_POINT('Ctrl Pts',(68.9547944157724,239.82253897193,6.73548842180239)) ;
#71180 = CARTESIAN_POINT('Ctrl Pts',(68.9411586577516,239.835826812852,6.76733417804846)) ;
#71181 = CARTESIAN_POINT('Ctrl Pts',(68.9272760863257,239.848183236163,6.79964511862253)) ;
#71182 = CARTESIAN_POINT('Ctrl Pts',(68.9128297461076,239.861041451658,6.83326820082954)) ;
#71183 = CARTESIAN_POINT('Ctrl Pts',(68.898115676083,239.87289172878,6.86739501663498)) ;
#71184 = CARTESIAN_POINT('Ctrl Pts',(68.8831640328237,239.883855459624,6.90184272882289)) ;
#71185 = CARTESIAN_POINT('Ctrl Pts',(68.878134330881,239.887543636058,6.91343086812699)) ;
#71186 = CARTESIAN_POINT('Ctrl Pts',(68.8730773513663,239.891131280772,6.92505532121191)) ;
#71187 = CARTESIAN_POINT('Ctrl Pts',(68.8679931270226,239.894622341495,6.93670912783197)) ;
#71188 = CARTESIAN_POINT('Ctrl Pts',(68.8494131707771,239.907380188333,6.97929718108381)) ;
#71189 = CARTESIAN_POINT('Ctrl Pts',(68.8304990267295,239.918831679828,7.02227724724999)) ;
#71190 = CARTESIAN_POINT('Ctrl Pts',(68.8113292278266,239.929084130521,7.06554957763077)) ;
#71191 = CARTESIAN_POINT('Ctrl Pts',(68.7913959354002,239.939744915164,7.11054535561578)) ;
#71192 = CARTESIAN_POINT('Ctrl Pts',(68.7711855162388,239.949109995399,7.1558571419846)) ;
#71193 = CARTESIAN_POINT('Ctrl Pts',(68.7507387129936,239.957269204465,7.20137278869765)) ;
#71194 = CARTESIAN_POINT('Ctrl Pts',(68.7391888375968,239.961878132663,7.22708341161682)) ;
#71195 = CARTESIAN_POINT('Ctrl Pts',(68.7275627458053,239.966101665732,7.25285908292051)) ;
#71196 = CARTESIAN_POINT('Ctrl Pts',(68.7158628290613,239.969950655758,7.27867958883829)) ;
#71197 = CARTESIAN_POINT('Origin',(79.6268886667016,242.164965512063,7.2786795888419)) ;
#71198 = CARTESIAN_POINT('',(79.5657826988536,242.355402012486,7.27867958883753)) ;
#71199 = CARTESIAN_POINT('Origin',(79.6268886667016,242.164965512063,7.2786795888419)) ;
#71200 = CARTESIAN_POINT('',(79.7759762964688,242.245816755679,7.17267980084142)) ;
#71201 = CARTESIAN_POINT('Origin',(79.6268886667016,242.164965512063,7.2786795888419)) ;
#71202 = CARTESIAN_POINT('Origin',(79.6268886666992,242.164965512062,7.27867958883793)) ;
#71203 = CARTESIAN_POINT('Origin',(68.824955275583,238.345892662512,7.2786795888419)) ;
#71204 = CARTESIAN_POINT('',(68.8242223895095,238.145894005322,7.27867958883747)) ;
#71205 = CARTESIAN_POINT('Origin',(68.824955275583,238.345892662512,7.2786795888419)) ;
#71206 = CARTESIAN_POINT('',(68.6581801055002,238.31506917167,7.17267980084141)) ;
#71207 = CARTESIAN_POINT('Origin',(68.824955275583,238.345892662512,7.2786795888419)) ;
#71208 = CARTESIAN_POINT('Origin',(68.8249552755856,238.345892662512,7.27867958883788)) ;
#71209 = CARTESIAN_POINT('Origin',(74.5283628290597,239.4,7.2786795888419)) ;
#71210 = CARTESIAN_POINT('Origin',(74.5283628290597,239.4,7.17267980084126)) ;
#71211 = CARTESIAN_POINT('Origin',(79.7621052129774,241.899588097824,7.27867958884204)) ;
#71212 = CARTESIAN_POINT('',(79.8802543914391,241.738216564929,7.27867958883795)) ;
#71213 = CARTESIAN_POINT('Origin',(79.7621052129773,241.899588097824,7.27867958883753)) ;
#71214 = CARTESIAN_POINT('',(79.9151467531553,241.97267935533,7.17267980084126)) ;
#71215 = CARTESIAN_POINT('Origin',(79.7621052129774,241.899588097824,7.27867958884204)) ;
#71216 = CARTESIAN_POINT('Origin',(79.7621052129773,241.899588097824,7.2786795888419)) ;
#71217 = CARTESIAN_POINT('Origin',(69.294620445142,236.900411902176,7.27867958884205)) ;
#71218 = CARTESIAN_POINT('',(69.1764712666803,237.06178343507,7.2786795888379)) ;
#71219 = CARTESIAN_POINT('Origin',(69.2946204451421,236.900411902176,7.27867958883748)) ;
#71220 = CARTESIAN_POINT('',(69.1415789049641,236.82732064467,7.17267980084126)) ;
#71221 = CARTESIAN_POINT('Origin',(69.294620445142,236.900411902176,7.27867958884205)) ;
#71222 = CARTESIAN_POINT('Origin',(69.2946204451421,236.900411902176,7.2786795888419)) ;
#71223 = CARTESIAN_POINT('Ctrl Pts',(69.1764712666787,237.061783435069,7.27867958884205)) ;
#71224 = CARTESIAN_POINT('Ctrl Pts',(69.243148183502,237.110601357313,7.10544023141379)) ;
#71225 = CARTESIAN_POINT('Ctrl Pts',(69.3221531999422,237.194392857808,6.875738735788)) ;
#71226 = CARTESIAN_POINT('Ctrl Pts',(69.3907109930823,237.344712076154,6.61255350476255)) ;
#71227 = CARTESIAN_POINT('Ctrl Pts',(69.4139986922107,237.434159724772,6.49311022572802)) ;
#71228 = CARTESIAN_POINT('Ctrl Pts',(69.4226403902003,237.51671011904,6.41124585525348)) ;
#71229 = CARTESIAN_POINT('Ctrl Pts',(69.4220357539442,237.583935565768,6.3619402730086)) ;
#71230 = CARTESIAN_POINT('Ctrl Pts',(69.408113128478,237.705993381689,6.3017093864378)) ;
#71231 = CARTESIAN_POINT('Ctrl Pts',(69.3463002437199,237.856072726253,6.33249341474089)) ;
#71232 = CARTESIAN_POINT('Ctrl Pts',(69.2496003997641,237.971560196244,6.4698470585811)) ;
#71233 = CARTESIAN_POINT('Ctrl Pts',(69.1354707359804,238.065806393091,6.66035004570858)) ;
#71234 = CARTESIAN_POINT('Ctrl Pts',(68.9914670223674,238.129856863735,6.93430623056252)) ;
#71235 = CARTESIAN_POINT('Ctrl Pts',(68.8793123588541,238.14569213061,7.16318984183832)) ;
#71236 = CARTESIAN_POINT('Ctrl Pts',(68.8242223895094,238.145894005322,7.27867958884204)) ;
#71237 = CARTESIAN_POINT('Ctrl Pts',(69.1398244440697,237.03495223438,7.24979207607672)) ;
#71238 = CARTESIAN_POINT('Ctrl Pts',(69.2136594228754,237.081063573975,7.07847449697579)) ;
#71239 = CARTESIAN_POINT('Ctrl Pts',(69.3029051206822,237.164631115907,6.85078050509009)) ;
#71240 = CARTESIAN_POINT('Ctrl Pts',(69.3828266366339,237.320754685321,6.58950105248792)) ;
#71241 = CARTESIAN_POINT('Ctrl Pts',(69.4108817593994,237.414984669568,6.47084518025989)) ;
#71242 = CARTESIAN_POINT('Ctrl Pts',(69.422335402039,237.502586585413,6.38949218624853)) ;
#71243 = CARTESIAN_POINT('Ctrl Pts',(69.4230316106547,237.574170392916,6.34048601917785)) ;
#71244 = CARTESIAN_POINT('Ctrl Pts',(69.409808159248,237.70446059159,6.2806080333673)) ;
#71245 = CARTESIAN_POINT('Ctrl Pts',(69.3430376940479,237.864409604147,6.3112178366199)) ;
#71246 = CARTESIAN_POINT('Ctrl Pts',(69.2371135689013,237.985002035298,6.44773619808466)) ;
#71247 = CARTESIAN_POINT('Ctrl Pts',(69.1123412792411,238.081000391347,6.63698036173261)) ;
#71248 = CARTESIAN_POINT('Ctrl Pts',(68.9561282905968,238.141140136422,6.90887829015515)) ;
#71249 = CARTESIAN_POINT('Ctrl Pts',(68.8366934655611,238.150123165881,7.1355834795928)) ;
#71250 = CARTESIAN_POINT('Ctrl Pts',(68.7788035031626,238.146060440786,7.24979207607672)) ;
#71251 = CARTESIAN_POINT('Ctrl Pts',(69.099905192383,236.955910305836,7.19960828841391)) ;
#71252 = CARTESIAN_POINT('Ctrl Pts',(69.1860064168498,237.006605983873,7.03140700938371)) ;
#71253 = CARTESIAN_POINT('Ctrl Pts',(69.2900259465182,237.09923082272,6.80705467385308)) ;
#71254 = CARTESIAN_POINT('Ctrl Pts',(69.3832650913571,237.27387614127,6.54899621389332)) ;
#71255 = CARTESIAN_POINT('Ctrl Pts',(69.4162520055124,237.379299887585,6.43168582586966)) ;
#71256 = CARTESIAN_POINT('Ctrl Pts',(69.4300886371973,237.47734191796,6.35121101255399)) ;
#71257 = CARTESIAN_POINT('Ctrl Pts',(69.4314780745408,237.557412263923,6.3027208476791)) ;
#71258 = CARTESIAN_POINT('Ctrl Pts',(69.4174156669863,237.703106817915,6.24345333299259)) ;
#71259 = CARTESIAN_POINT('Ctrl Pts',(69.342501106197,237.881643096035,6.27376032922433)) ;
#71260 = CARTESIAN_POINT('Ctrl Pts',(69.2226188574627,238.015603497768,6.40883966351126)) ;
#71261 = CARTESIAN_POINT('Ctrl Pts',(69.0809642347923,238.121495468969,6.59593332022851)) ;
#71262 = CARTESIAN_POINT('Ctrl Pts',(68.902901648932,238.186234982861,6.8643640810213)) ;
#71263 = CARTESIAN_POINT('Ctrl Pts',(68.7663503411012,238.192939491825,7.08747716850402)) ;
#71264 = CARTESIAN_POINT('Ctrl Pts',(68.7000484702344,238.186542756822,7.19960828841391)) ;
#71265 = CARTESIAN_POINT('Ctrl Pts',(69.1223464629029,236.862651936505,7.17608503411331)) ;
#71266 = CARTESIAN_POINT('Ctrl Pts',(69.2114184263084,236.924421474316,7.00519241449165)) ;
#71267 = CARTESIAN_POINT('Ctrl Pts',(69.3172779787112,237.032178811751,6.77809747419061)) ;
#71268 = CARTESIAN_POINT('Ctrl Pts',(69.4094503328369,237.228581096615,6.51751159801928)) ;
#71269 = CARTESIAN_POINT('Ctrl Pts',(69.4409048676736,237.346030918506,6.39917202871152)) ;
#71270 = CARTESIAN_POINT('Ctrl Pts',(69.4527579169206,237.454760983212,6.31803579114758)) ;
#71271 = CARTESIAN_POINT('Ctrl Pts',(69.4522076854779,237.543435565293,6.26916026780418)) ;
#71272 = CARTESIAN_POINT('Ctrl Pts',(69.4340864408003,237.704639718483,6.20944181386913)) ;
#71273 = CARTESIAN_POINT('Ctrl Pts',(69.3522671333801,237.902982353965,6.23997013594573)) ;
#71274 = CARTESIAN_POINT('Ctrl Pts',(69.2242009113928,238.05477780945,6.37612467492586)) ;
#71275 = CARTESIAN_POINT('Ctrl Pts',(69.0732121226385,238.177710520412,6.56486468658063)) ;
#71276 = CARTESIAN_POINT('Ctrl Pts',(68.883092282389,238.259246394865,6.8360410390703)) ;
#71277 = CARTESIAN_POINT('Ctrl Pts',(68.7356312735506,238.276769354007,7.0621597362024)) ;
#71278 = CARTESIAN_POINT('Ctrl Pts',(68.6633879453144,238.275181010333,7.1760850341133)) ;
#71279 = CARTESIAN_POINT('Ctrl Pts',(69.141578904964,236.82732064467,7.17267980084142)) ;
#71280 = CARTESIAN_POINT('Ctrl Pts',(69.2302241041771,236.892950071602,6.99944044341316)) ;
#71281 = CARTESIAN_POINT('Ctrl Pts',(69.334840073065,237.006158216377,6.76973894778735)) ;
#71282 = CARTESIAN_POINT('Ctrl Pts',(69.4244038080695,237.210771326455,6.50655371676194)) ;
#71283 = CARTESIAN_POINT('Ctrl Pts',(69.4542517733073,237.332909486872,6.38711043772741)) ;
#71284 = CARTESIAN_POINT('Ctrl Pts',(69.4646137832507,237.445912417774,6.30524606725286)) ;
#71285 = CARTESIAN_POINT('Ctrl Pts',(69.4628489697551,237.53809374039,6.25594048500798)) ;
#71286 = CARTESIAN_POINT('Ctrl Pts',(69.4425255895883,237.705725559621,6.19570959843718)) ;
#71287 = CARTESIAN_POINT('Ctrl Pts',(69.3580050351793,237.912593058043,6.22649362674026)) ;
#71288 = CARTESIAN_POINT('Ctrl Pts',(69.2275905708934,238.072255835849,6.36384727058048)) ;
#71289 = CARTESIAN_POINT('Ctrl Pts',(69.0742642050193,238.202782237888,6.55435025770793)) ;
#71290 = CARTESIAN_POINT('Ctrl Pts',(68.8815106963087,238.29188736988,6.8283064425619)) ;
#71291 = CARTESIAN_POINT('Ctrl Pts',(68.731705749617,238.314408535778,7.05719005383769)) ;
#71292 = CARTESIAN_POINT('Ctrl Pts',(68.6581801055002,238.31506917167,7.17267980084141)) ;
#71293 = CARTESIAN_POINT('Ctrl Pts',(68.6581801055002,238.31506917167,7.17267980084144)) ;
#71294 = CARTESIAN_POINT('Ctrl Pts',(68.6999525110751,238.314693842072,7.10706616889675)) ;
#71295 = CARTESIAN_POINT('Ctrl Pts',(68.7422057617377,238.310890803021,7.04171162773037)) ;
#71296 = CARTESIAN_POINT('Ctrl Pts',(68.7848246201634,238.303370652585,6.97698800180934)) ;
#71297 = CARTESIAN_POINT('Ctrl Pts',(68.8089147256669,238.299119923586,6.94040328240097)) ;
#71298 = CARTESIAN_POINT('Ctrl Pts',(68.833122153762,238.293682517859,6.90402046522006)) ;
#71299 = CARTESIAN_POINT('Ctrl Pts',(68.8574309924011,238.287014704168,6.8679090476063)) ;
#71300 = CARTESIAN_POINT('Ctrl Pts',(68.8657978603999,238.284719706952,6.85547984566426)) ;
#71301 = CARTESIAN_POINT('Ctrl Pts',(68.8741783905198,238.282278268265,6.84308050324332)) ;
#71302 = CARTESIAN_POINT('Ctrl Pts',(68.8825729718501,238.279688415001,6.83071258016738)) ;
#71303 = CARTESIAN_POINT('Ctrl Pts',(68.9148256813734,238.269737974146,6.78319394705386)) ;
#71304 = CARTESIAN_POINT('Ctrl Pts',(68.9472835743097,238.257599262249,6.73613620680623)) ;
#71305 = CARTESIAN_POINT('Ctrl Pts',(68.9798286619572,238.242680053236,6.69003521439263)) ;
#71306 = CARTESIAN_POINT('Ctrl Pts',(68.9876568819059,238.239091467121,6.67894633018452)) ;
#71307 = CARTESIAN_POINT('Ctrl Pts',(68.995490333041,238.235342151787,6.6679128004386)) ;
#71308 = CARTESIAN_POINT('Ctrl Pts',(69.0033277607713,238.231424121694,6.65694152576342)) ;
#71309 = CARTESIAN_POINT('Ctrl Pts',(69.0332777274343,238.216451751332,6.61501586825413)) ;
#71310 = CARTESIAN_POINT('Ctrl Pts',(69.0632828822616,238.199013116527,6.57399853749883)) ;
#71311 = CARTESIAN_POINT('Ctrl Pts',(69.0932880711879,238.178638120891,6.53430592114766)) ;
#71312 = CARTESIAN_POINT('Ctrl Pts',(69.0996874302936,238.174292642042,6.52584047517086)) ;
#71313 = CARTESIAN_POINT('Ctrl Pts',(69.1060869684763,238.169813657528,6.51743528549824)) ;
#71314 = CARTESIAN_POINT('Ctrl Pts',(69.1124864583777,238.165196694566,6.50909439154214)) ;
#71315 = CARTESIAN_POINT('Ctrl Pts',(69.114322160242,238.163872312835,6.50670179544144)) ;
#71316 = CARTESIAN_POINT('Ctrl Pts',(69.1161578518097,238.162536566453,6.50431450491999)) ;
#71317 = CARTESIAN_POINT('Ctrl Pts',(69.1179934839805,238.16118927711,6.50193271268924)) ;
#71318 = CARTESIAN_POINT('Ctrl Pts',(69.1441271017158,238.142008122402,6.46802349673852)) ;
#71319 = CARTESIAN_POINT('Ctrl Pts',(69.1701834997951,238.12052377075,6.43531103830365)) ;
#71320 = CARTESIAN_POINT('Ctrl Pts',(69.1960235506317,238.096256908892,6.40437140018978)) ;
#71321 = CARTESIAN_POINT('Ctrl Pts',(69.200602813238,238.091956440066,6.39888841067231)) ;
#71322 = CARTESIAN_POINT('Ctrl Pts',(69.205175413079,238.087568580314,6.39346109729161)) ;
#71323 = CARTESIAN_POINT('Ctrl Pts',(69.2097407553992,238.08309065004,6.38809266614272)) ;
#71324 = CARTESIAN_POINT('Ctrl Pts',(69.2155047995749,238.077436969307,6.38131466963642)) ;
#71325 = CARTESIAN_POINT('Ctrl Pts',(69.2212571502427,238.071639928937,6.37463063750665)) ;
#71326 = CARTESIAN_POINT('Ctrl Pts',(69.2269965636579,238.065694458748,6.36804717288461)) ;
#71327 = CARTESIAN_POINT('Ctrl Pts',(69.2381520120765,238.054138506733,6.35525117881787)) ;
#71328 = CARTESIAN_POINT('Ctrl Pts',(69.2492584241303,238.04202171314,6.34283511840792)) ;
#71329 = CARTESIAN_POINT('Ctrl Pts',(69.2602291524054,238.029272223066,6.33098424685138)) ;
#71330 = CARTESIAN_POINT('Ctrl Pts',(69.2762291953482,238.010677979953,6.31370057624549)) ;
#71331 = CARTESIAN_POINT('Ctrl Pts',(69.2920266123677,237.990684501173,6.2975066182331)) ;
#71332 = CARTESIAN_POINT('Ctrl Pts',(69.3073059712954,237.969089607455,6.28306176861731)) ;
#71333 = CARTESIAN_POINT('Ctrl Pts',(69.3170064523572,237.955379552045,6.27389109654915)) ;
#71334 = CARTESIAN_POINT('Ctrl Pts',(69.3264982581306,237.94102462448,6.26542539348726)) ;
#71335 = CARTESIAN_POINT('Ctrl Pts',(69.3357048535214,237.9259819694,6.25782719378357)) ;
#71336 = CARTESIAN_POINT('Ctrl Pts',(69.3461971715583,237.908838572247,6.24916788766498)) ;
#71337 = CARTESIAN_POINT('Ctrl Pts',(69.3563194560639,237.890802280141,6.2416363146655)) ;
#71338 = CARTESIAN_POINT('Ctrl Pts',(69.3659433718682,237.872119457317,6.23535445238633)) ;
#71339 = CARTESIAN_POINT('Ctrl Pts',(69.3766889235219,237.851259212716,6.22834045964418)) ;
#71340 = CARTESIAN_POINT('Ctrl Pts',(69.3868213007338,237.829528899656,6.22290107667885)) ;
#71341 = CARTESIAN_POINT('Ctrl Pts',(69.3962054482908,237.807176353626,6.21916216383858)) ;
#71342 = CARTESIAN_POINT('Ctrl Pts',(69.3977249759491,237.803556918646,6.21855674055017)) ;
#71343 = CARTESIAN_POINT('Ctrl Pts',(69.3992248348919,237.799921090119,6.21799596731962)) ;
#71344 = CARTESIAN_POINT('Ctrl Pts',(69.400704389067,237.796269834308,6.21748045696162)) ;
#71345 = CARTESIAN_POINT('Ctrl Pts',(69.4080873978986,237.778049985144,6.2149080486036)) ;
#71346 = CARTESIAN_POINT('Ctrl Pts',(69.4149663679611,237.759443906188,6.2134623227348)) ;
#71347 = CARTESIAN_POINT('Ctrl Pts',(69.4212371552491,237.740594005388,6.21324003078939)) ;
#71348 = CARTESIAN_POINT('Ctrl Pts',(69.426060889559,237.726093926044,6.21306903514967)) ;
#71349 = CARTESIAN_POINT('Ctrl Pts',(69.4305257936821,237.711444249265,6.2136230224309)) ;
#71350 = CARTESIAN_POINT('Ctrl Pts',(69.4345108735777,237.696744168001,6.21503461181594)) ;
#71351 = CARTESIAN_POINT('Ctrl Pts',(69.4357063419349,237.69233434876,6.21545806893285)) ;
#71352 = CARTESIAN_POINT('Ctrl Pts',(69.4368585389515,237.68792033025,6.21595862038417)) ;
#71353 = CARTESIAN_POINT('Ctrl Pts',(69.437963971472,237.683505637975,6.21653961743159)) ;
#71354 = CARTESIAN_POINT('Ctrl Pts',(69.4416896620956,237.668626595328,6.2184977787954)) ;
#71355 = CARTESIAN_POINT('Ctrl Pts',(69.4450076180945,237.653759748461,6.22117270210315)) ;
#71356 = CARTESIAN_POINT('Ctrl Pts',(69.4478694000204,237.638976148692,6.22459317008967)) ;
#71357 = CARTESIAN_POINT('Ctrl Pts',(69.4502989061332,237.62642563054,6.22749697202036)) ;
#71358 = CARTESIAN_POINT('Ctrl Pts',(69.4523999327019,237.613935243742,6.23093747154904)) ;
#71359 = CARTESIAN_POINT('Ctrl Pts',(69.4542212766179,237.60156814121,6.2348010738459)) ;
#71360 = CARTESIAN_POINT('Ctrl Pts',(69.4573114671906,237.580585446333,6.24135627041758)) ;
#71361 = CARTESIAN_POINT('Ctrl Pts',(69.4594928621059,237.559803752785,6.24936900793142)) ;
#71362 = CARTESIAN_POINT('Ctrl Pts',(69.4609730875372,237.539562477922,6.25830745765639)) ;
#71363 = CARTESIAN_POINT('Ctrl Pts',(69.4627412442874,237.515383899426,6.2689846017476)) ;
#71364 = CARTESIAN_POINT('Ctrl Pts',(69.4635077874243,237.491978141513,6.28098058459061)) ;
#71365 = CARTESIAN_POINT('Ctrl Pts',(69.4633411171518,237.469303713581,6.29415175647048)) ;
#71366 = CARTESIAN_POINT('Ctrl Pts',(69.4632865875771,237.461885312617,6.29846097364117)) ;
#71367 = CARTESIAN_POINT('Ctrl Pts',(69.4631324052817,237.45454483693,6.30289591312325)) ;
#71368 = CARTESIAN_POINT('Ctrl Pts',(69.4628816398225,237.447279844771,6.30745136656849)) ;
#71369 = CARTESIAN_POINT('Ctrl Pts',(69.462471076266,237.435385299853,6.31490974290758)) ;
#71370 = CARTESIAN_POINT('Ctrl Pts',(69.4618015271505,237.423693246438,6.3226911622136)) ;
#71371 = CARTESIAN_POINT('Ctrl Pts',(69.4609119195854,237.412204661752,6.33072881419273)) ;
#71372 = CARTESIAN_POINT('Ctrl Pts',(69.4595971175969,237.395225024232,6.34260812055181)) ;
#71373 = CARTESIAN_POINT('Ctrl Pts',(69.4577775214589,237.378689956509,6.35508284132056)) ;
#71374 = CARTESIAN_POINT('Ctrl Pts',(69.4555569265135,237.362609472007,6.36796878250284)) ;
#71375 = CARTESIAN_POINT('Ctrl Pts',(69.4507548146022,237.327834878683,6.3958350675119)) ;
#71376 = CARTESIAN_POINT('Ctrl Pts',(69.4440744559395,237.29518858729,6.42562177225894)) ;
#71377 = CARTESIAN_POINT('Ctrl Pts',(69.4359262687737,237.264342959413,6.45673144071841)) ;
#71378 = CARTESIAN_POINT('Ctrl Pts',(69.4342394440246,237.257957346584,6.46317171480956)) ;
#71379 = CARTESIAN_POINT('Ctrl Pts',(69.4324898504687,237.251649019488,6.4696686866564)) ;
#71380 = CARTESIAN_POINT('Ctrl Pts',(69.4306813372517,237.24541523496,6.47621705556352)) ;
#71381 = CARTESIAN_POINT('Ctrl Pts',(69.4283565397334,237.237401864274,6.48463481642947)) ;
#71382 = CARTESIAN_POINT('Ctrl Pts',(69.425934386871,237.229511324476,6.49313770431927)) ;
#71383 = CARTESIAN_POINT('Ctrl Pts',(69.4234232194315,237.221737373948,6.50171478323276)) ;
#71384 = CARTESIAN_POINT('Ctrl Pts',(69.422697088201,237.219489452055,6.50419493838598)) ;
#71385 = CARTESIAN_POINT('Ctrl Pts',(69.4219633340238,237.217251526371,6.50668140853608)) ;
#71386 = CARTESIAN_POINT('Ctrl Pts',(69.4212221518793,237.215023460709,6.50917393353464)) ;
#71387 = CARTESIAN_POINT('Ctrl Pts',(69.4097619220254,237.180572894409,6.54771359562661)) ;
#71388 = CARTESIAN_POINT('Ctrl Pts',(69.3965230580414,237.148480564374,6.58769691391626)) ;
#71389 = CARTESIAN_POINT('Ctrl Pts',(69.3819367159882,237.11836673977,6.62856039271017)) ;
#71390 = CARTESIAN_POINT('Ctrl Pts',(69.377526011194,237.109260742525,6.64091693427264)) ;
#71391 = CARTESIAN_POINT('Ctrl Pts',(69.3729924469871,237.10033577619,6.65335395529858)) ;
#71392 = CARTESIAN_POINT('Ctrl Pts',(69.3683488142593,237.091581581043,6.66585587550309)) ;
#71393 = CARTESIAN_POINT('Ctrl Pts',(69.3501266653189,237.057229112367,6.71491484837152)) ;
#71394 = CARTESIAN_POINT('Ctrl Pts',(69.3302050449842,237.025505003706,6.76497458145779)) ;
#71395 = CARTESIAN_POINT('Ctrl Pts',(69.308820855372,236.996090564452,6.81573937973999)) ;
#71396 = CARTESIAN_POINT('Ctrl Pts',(69.304921177765,236.990726469195,6.82499698316901)) ;
#71397 = CARTESIAN_POINT('Ctrl Pts',(69.3009730003124,236.985439192709,6.83427803434362)) ;
#71398 = CARTESIAN_POINT('Ctrl Pts',(69.2969779405296,236.980226805711,6.84358073996881)) ;
#71399 = CARTESIAN_POINT('Ctrl Pts',(69.2935131871895,236.975706313842,6.85164859930998)) ;
#71400 = CARTESIAN_POINT('Ctrl Pts',(69.2900131259033,236.971242114419,6.85973283718352)) ;
#71401 = CARTESIAN_POINT('Ctrl Pts',(69.2864787978978,236.966832920126,6.86783236707)) ;
#71402 = CARTESIAN_POINT('Ctrl Pts',(69.2664829520006,236.941887422852,6.91365634016876)) ;
#71403 = CARTESIAN_POINT('Ctrl Pts',(69.2454268139038,236.918699739166,6.95991626883178)) ;
#71404 = CARTESIAN_POINT('Ctrl Pts',(69.2234260967364,236.897138360149,7.00647220769083)) ;
#71405 = CARTESIAN_POINT('Ctrl Pts',(69.2007985755099,236.874962693889,7.05435453292341)) ;
#71406 = CARTESIAN_POINT('Ctrl Pts',(69.177171544277,236.854507667279,7.10255069985114)) ;
#71407 = CARTESIAN_POINT('Ctrl Pts',(69.1526704057878,236.835685711672,7.15089895991494)) ;
#71408 = CARTESIAN_POINT('Ctrl Pts',(69.1489927835866,236.832860535126,7.15815603634354)) ;
#71409 = CARTESIAN_POINT('Ctrl Pts',(69.145295472849,236.830072245688,7.16541651035403)) ;
#71410 = CARTESIAN_POINT('Ctrl Pts',(69.1415789049641,236.82732064467,7.17267980084127)) ;
#71411 = CARTESIAN_POINT('Ctrl Pts',(69.1764712666787,237.061783435069,7.27867958884205)) ;
#71412 = CARTESIAN_POINT('Ctrl Pts',(69.243148183502,237.110601357313,7.10544023141379)) ;
#71413 = CARTESIAN_POINT('Ctrl Pts',(69.3221531999422,237.194392857808,6.875738735788)) ;
#71414 = CARTESIAN_POINT('Ctrl Pts',(69.3907109930823,237.344712076154,6.61255350476255)) ;
#71415 = CARTESIAN_POINT('Ctrl Pts',(69.4139986922107,237.434159724772,6.49311022572802)) ;
#71416 = CARTESIAN_POINT('Ctrl Pts',(69.4226403902003,237.51671011904,6.41124585525348)) ;
#71417 = CARTESIAN_POINT('Ctrl Pts',(69.4220357539442,237.583935565768,6.3619402730086)) ;
#71418 = CARTESIAN_POINT('Ctrl Pts',(69.408113128478,237.705993381689,6.3017093864378)) ;
#71419 = CARTESIAN_POINT('Ctrl Pts',(69.3463002437199,237.856072726253,6.33249341474089)) ;
#71420 = CARTESIAN_POINT('Ctrl Pts',(69.2496003997641,237.971560196244,6.4698470585811)) ;
#71421 = CARTESIAN_POINT('Ctrl Pts',(69.1354707359804,238.065806393091,6.66035004570858)) ;
#71422 = CARTESIAN_POINT('Ctrl Pts',(68.9914670223674,238.129856863735,6.93430623056252)) ;
#71423 = CARTESIAN_POINT('Ctrl Pts',(68.8793123588541,238.14569213061,7.16318984183832)) ;
#71424 = CARTESIAN_POINT('Ctrl Pts',(68.8242223895094,238.145894005322,7.27867958884204)) ;
#71425 = CARTESIAN_POINT('Origin',(80.2317703825363,240.454107337488,7.2786795888419)) ;
#71426 = CARTESIAN_POINT('',(80.2325032686099,240.654105994678,7.27867958883746)) ;
#71427 = CARTESIAN_POINT('Origin',(80.2317703825363,240.454107337488,7.2786795888419)) ;
#71428 = CARTESIAN_POINT('',(80.3985455526191,240.48493082833,7.17267980084138)) ;
#71429 = CARTESIAN_POINT('Origin',(80.2317703825363,240.454107337488,7.2786795888419)) ;
#71430 = CARTESIAN_POINT('Origin',(80.2317703825338,240.454107337488,7.27867958883787)) ;
#71431 = CARTESIAN_POINT('Origin',(69.4298369914177,236.635034487937,7.2786795888419)) ;
#71432 = CARTESIAN_POINT('',(69.4909429592657,236.444597987514,7.27867958883751)) ;
#71433 = CARTESIAN_POINT('Origin',(69.4298369914177,236.635034487937,7.2786795888419)) ;
#71434 = CARTESIAN_POINT('',(69.2807493616505,236.554183244321,7.17267980084143)) ;
#71435 = CARTESIAN_POINT('Origin',(69.4298369914177,236.635034487937,7.2786795888419)) ;
#71436 = CARTESIAN_POINT('Origin',(69.4298369914201,236.635034487938,7.27867958883792)) ;
#71437 = CARTESIAN_POINT('Origin',(74.5283628290597,239.4,7.2786795888419)) ;
#71438 = CARTESIAN_POINT('Origin',(74.5283628290597,239.4,7.17267980084126)) ;
#71439 = CARTESIAN_POINT('Origin',(80.2783628290598,240.159934207678,7.27867958884206)) ;
#71440 = CARTESIAN_POINT('',(80.3408628290578,239.969950655758,7.27867958883786)) ;
#71441 = CARTESIAN_POINT('Origin',(80.2783628290597,240.159934207678,7.27867958883746)) ;
#71442 = CARTESIAN_POINT('',(80.4465004238193,240.182155687653,7.17267980084126)) ;
#71443 = CARTESIAN_POINT('Origin',(80.2783628290598,240.159934207678,7.27867958884206)) ;
#71444 = CARTESIAN_POINT('Origin',(80.2783628290597,240.159934207678,7.2786795888419)) ;
#71445 = CARTESIAN_POINT('Origin',(70.3231932313806,235.405435110687,7.27867958886635)) ;
#71446 = CARTESIAN_POINT('',(70.1609601394261,235.522398454837,7.27867958819177)) ;
#71447 = CARTESIAN_POINT('Origin',(70.3231932313897,235.405435110699,7.27867958812537)) ;
#71448 = CARTESIAN_POINT('',(70.2002285180522,235.288628757201,7.17267980084125)) ;
#71449 = CARTESIAN_POINT('Origin',(70.3231932313806,235.405435110687,7.27867958886635)) ;
#71450 = CARTESIAN_POINT('Origin',(70.3231932313897,235.405435110699,7.2786795888419)) ;
#71451 = CARTESIAN_POINT('Ctrl Pts',(70.1609601392379,235.522398454576,7.27867958886635)) ;
#71452 = CARTESIAN_POINT('Ctrl Pts',(70.1931850042782,235.567095701812,7.16316434207535)) ;
#71453 = CARTESIAN_POINT('Ctrl Pts',(70.2467521307728,235.666850632939,6.93376990304091)) ;
#71454 = CARTESIAN_POINT('Ctrl Pts',(70.2791573181385,235.82106630907,6.66059058867321)) ;
#71455 = CARTESIAN_POINT('Ctrl Pts',(70.2719462922848,235.950192751371,6.49243937586827)) ;
#71456 = CARTESIAN_POINT('Ctrl Pts',(70.2543651218475,236.031343606776,6.41122181800393)) ;
#71457 = CARTESIAN_POINT('Ctrl Pts',(70.2232735078896,236.127109061982,6.335121754773)) ;
#71458 = CARTESIAN_POINT('Ctrl Pts',(70.1567428205062,236.241909737955,6.30139298231289)) ;
#71459 = CARTESIAN_POINT('Ctrl Pts',(70.0129806384832,236.38232667883,6.38459956034722)) ;
#71460 = CARTESIAN_POINT('Ctrl Pts',(69.9044401094434,236.431932501241,6.52710938218576)) ;
#71461 = CARTESIAN_POINT('Ctrl Pts',(69.82184001658,236.455045685299,6.65331962753031)) ;
#71462 = CARTESIAN_POINT('Ctrl Pts',(69.7565000731658,236.470099247129,6.75725825753585)) ;
#71463 = CARTESIAN_POINT('Ctrl Pts',(69.640759497392,236.479083143309,6.96268985033138)) ;
#71464 = CARTESIAN_POINT('Ctrl Pts',(69.5434011590231,236.46143041754,7.16318512433996)) ;
#71465 = CARTESIAN_POINT('Ctrl Pts',(69.4909429592657,236.444597987514,7.27867958884206)) ;
#71466 = CARTESIAN_POINT('Ctrl Pts',(70.1343982367854,235.485555975345,7.24979207610076)) ;
#71467 = CARTESIAN_POINT('Ctrl Pts',(70.1717201553335,235.530011742365,7.13555826270375)) ;
#71468 = CARTESIAN_POINT('Ctrl Pts',(70.2352127941684,235.631546456137,6.90834410930033)) ;
#71469 = CARTESIAN_POINT('Ctrl Pts',(70.2778578331153,235.793397400286,6.63721854494523)) ;
#71470 = CARTESIAN_POINT('Ctrl Pts',(70.2749893652713,235.930953158475,6.47017555478502)) ;
#71471 = CARTESIAN_POINT('Ctrl Pts',(70.2584811374162,236.017769911042,6.38946600679148)) ;
#71472 = CARTESIAN_POINT('Ctrl Pts',(70.2273452442692,236.120398165374,6.31382571916806)) ;
#71473 = CARTESIAN_POINT('Ctrl Pts',(70.1570961352955,236.243395649578,6.2802913028328)) ;
#71474 = CARTESIAN_POINT('Ctrl Pts',(70.002257580433,236.391500260111,6.36301245408811)) ;
#71475 = CARTESIAN_POINT('Ctrl Pts',(69.8847920623921,236.440799947566,6.50464016460755)) ;
#71476 = CARTESIAN_POINT('Ctrl Pts',(69.7961700957007,236.461744519509,6.62996437500457)) ;
#71477 = CARTESIAN_POINT('Ctrl Pts',(69.726170115545,236.474703621702,6.73315731420172)) ;
#71478 = CARTESIAN_POINT('Ctrl Pts',(69.603078658587,236.477799208024,6.9369894242539)) ;
#71479 = CARTESIAN_POINT('Ctrl Pts',(69.501498972583,236.452474821217,7.13557881442658)) ;
#71480 = CARTESIAN_POINT('Ctrl Pts',(69.447695600056,236.4307210693,7.24979207607674)) ;
#71481 = CARTESIAN_POINT('Ctrl Pts',(70.1208580517311,235.398046905423,7.19960828027639)) ;
#71482 = CARTESIAN_POINT('Ctrl Pts',(70.1650141283291,235.447937352443,7.08745240215401)) ;
#71483 = CARTESIAN_POINT('Ctrl Pts',(70.2404088463949,235.562034042248,6.86383162153399)) ;
#71484 = CARTESIAN_POINT('Ctrl Pts',(70.2921760427777,235.744189112754,6.59616799928918)) ;
#71485 = CARTESIAN_POINT('Ctrl Pts',(70.2910917260747,235.898794432699,6.43101837867299)) ;
#71486 = CARTESIAN_POINT('Ctrl Pts',(70.2735843246182,235.996263311767,6.35118130137054)) ;
#71487 = CARTESIAN_POINT('Ctrl Pts',(70.2396455435276,236.111350870535,6.27633391215476)) ;
#71488 = CARTESIAN_POINT('Ctrl Pts',(70.1615362719684,236.248921034682,6.2431366136268)) ;
#71489 = CARTESIAN_POINT('Ctrl Pts',(69.9878074991475,236.413731031267,6.32501771821064)) ;
#71490 = CARTESIAN_POINT('Ctrl Pts',(69.8553150555578,236.467465888111,6.4651280555107)) ;
#71491 = CARTESIAN_POINT('Ctrl Pts',(69.7551316491419,236.489433376344,6.5889490867345)) ;
#71492 = CARTESIAN_POINT('Ctrl Pts',(69.6759571070458,236.502694500453,6.69087982222723)) ;
#71493 = CARTESIAN_POINT('Ctrl Pts',(69.5365048380475,236.503432755258,6.89202712786946)) ;
#71494 = CARTESIAN_POINT('Ctrl Pts',(69.4213680030774,236.471458524615,7.08747258003697)) ;
#71495 = CARTESIAN_POINT('Ctrl Pts',(69.3602853815846,236.444885377841,7.19960828025282)) ;
#71496 = CARTESIAN_POINT('Ctrl Pts',(70.1710194090832,235.31628766108,7.17608503413728)) ;
#71497 = CARTESIAN_POINT('Ctrl Pts',(70.214777628573,235.373812834946,7.06213458186475)) ;
#71498 = CARTESIAN_POINT('Ctrl Pts',(70.2878736317904,235.503043851011,6.83550821975048)) ;
#71499 = CARTESIAN_POINT('Ctrl Pts',(70.3331085651019,235.704853636922,6.56510249374437)) ;
#71500 = CARTESIAN_POINT('Ctrl Pts',(70.3248138804196,235.874784619819,6.39850454451589)) ;
#71501 = CARTESIAN_POINT('Ctrl Pts',(70.3021011200014,235.981815178004,6.31801009241991)) ;
#71502 = CARTESIAN_POINT('Ctrl Pts',(70.2614546651718,236.108252571878,6.24257140290715)) ;
#71503 = CARTESIAN_POINT('Ctrl Pts',(70.1736478114485,236.260031613336,6.20912632225173)) ;
#71504 = CARTESIAN_POINT('Ctrl Pts',(69.983513761331,236.445249425744,6.29162716702857)) ;
#71505 = CARTESIAN_POINT('Ctrl Pts',(69.8401571188674,236.509794674245,6.43287717369066)) ;
#71506 = CARTESIAN_POINT('Ctrl Pts',(69.7313643449563,236.539153995676,6.55786810050257)) ;
#71507 = CARTESIAN_POINT('Ctrl Pts',(69.645352343298,236.558040720169,6.66078690779107)) ;
#71508 = CARTESIAN_POINT('Ctrl Pts',(69.4933529954514,236.567663689091,6.86407978383067)) ;
#71509 = CARTESIAN_POINT('Ctrl Pts',(69.3662478807571,236.541692653929,7.0621550826083)) ;
#71510 = CARTESIAN_POINT('Ctrl Pts',(69.2980284313689,236.517856659565,7.17608503411333)) ;
#71511 = CARTESIAN_POINT('Ctrl Pts',(70.20022851804,235.288628757191,7.17267980086571)) ;
#71512 = CARTESIAN_POINT('Ctrl Pts',(70.2429207658929,235.348513784352,7.05716455407471)) ;
#71513 = CARTESIAN_POINT('Ctrl Pts',(70.3133732877927,235.482542125275,6.82777011504029)) ;
#71514 = CARTESIAN_POINT('Ctrl Pts',(70.3540173856703,235.69095903296,6.55459080067257)) ;
#71515 = CARTESIAN_POINT('Ctrl Pts',(70.3415643017227,235.866420668903,6.38643958786764)) ;
#71516 = CARTESIAN_POINT('Ctrl Pts',(70.3161098774568,235.977062325867,6.30522203000329)) ;
#71517 = CARTESIAN_POINT('Ctrl Pts',(70.2721119966867,236.1079181649,6.22912196677238)) ;
#71518 = CARTESIAN_POINT('Ctrl Pts',(70.1799433867558,236.265588695095,6.19539319431226)) ;
#71519 = CARTESIAN_POINT('Ctrl Pts',(69.9834029162908,236.459885100479,6.27859977234659)) ;
#71520 = CARTESIAN_POINT('Ctrl Pts',(69.8364662050809,236.529661783615,6.42110959418513)) ;
#71521 = CARTESIAN_POINT('Ctrl Pts',(69.7250044659152,236.562710994884,6.54731983952968)) ;
#71522 = CARTESIAN_POINT('Ctrl Pts',(69.6369109834873,236.584440493439,6.65125846953521)) ;
#71523 = CARTESIAN_POINT('Ctrl Pts',(69.4812795913638,236.59873536178,6.85669006233074)) ;
#71524 = CARTESIAN_POINT('Ctrl Pts',(69.3508834170229,236.576276518229,7.05718533633934)) ;
#71525 = CARTESIAN_POINT('Ctrl Pts',(69.2807493616505,236.554183244321,7.17267980084144)) ;
#71526 = CARTESIAN_POINT('Ctrl Pts',(69.2807493616505,236.554183244321,7.17267980084144)) ;
#71527 = CARTESIAN_POINT('Ctrl Pts',(69.3319590779197,236.570315069043,7.08834931793388)) ;
#71528 = CARTESIAN_POINT('Ctrl Pts',(69.3855949027408,236.581474093001,7.00441091771373)) ;
#71529 = CARTESIAN_POINT('Ctrl Pts',(69.4417408216249,236.586783400832,6.92170693026603)) ;
#71530 = CARTESIAN_POINT('Ctrl Pts',(69.4539725728908,236.587940067854,6.90368933213478)) ;
#71531 = CARTESIAN_POINT('Ctrl Pts',(69.4663235692777,236.588819061917,6.88573016534387)) ;
#71532 = CARTESIAN_POINT('Ctrl Pts',(69.4787948641657,236.589411248829,6.86783787638887)) ;
#71533 = CARTESIAN_POINT('Ctrl Pts',(69.4873959952969,236.589819664902,6.85549802516093)) ;
#71534 = CARTESIAN_POINT('Ctrl Pts',(69.4960552909163,236.590089888067,6.84319004873691)) ;
#71535 = CARTESIAN_POINT('Ctrl Pts',(69.5047731716626,236.590218720409,6.83091678535131)) ;
#71536 = CARTESIAN_POINT('Ctrl Pts',(69.556483609808,236.590982894298,6.75811746111013)) ;
#71537 = CARTESIAN_POINT('Ctrl Pts',(69.6102563665989,236.586769160471,6.68654093637314)) ;
#71538 = CARTESIAN_POINT('Ctrl Pts',(69.6663966021717,236.575969671236,6.61755200602656)) ;
#71539 = CARTESIAN_POINT('Ctrl Pts',(69.6748967326721,236.574334532607,6.60710646897029)) ;
#71540 = CARTESIAN_POINT('Ctrl Pts',(69.683451109302,236.572548502764,6.59672021090978)) ;
#71541 = CARTESIAN_POINT('Ctrl Pts',(69.6920607600786,236.57060609939,6.58639791934561)) ;
#71542 = CARTESIAN_POINT('Ctrl Pts',(69.7029835120638,236.568141842609,6.57330240204779)) ;
#71543 = CARTESIAN_POINT('Ctrl Pts',(69.7139952237171,236.565425892264,6.56030985644741)) ;
#71544 = CARTESIAN_POINT('Ctrl Pts',(69.7250718253531,236.562416201434,6.54750568264053)) ;
#71545 = CARTESIAN_POINT('Ctrl Pts',(69.7361531518505,236.559405226783,6.53469604705492)) ;
#71546 = CARTESIAN_POINT('Ctrl Pts',(69.7472994410321,236.556100272868,6.52207490355897)) ;
#71547 = CARTESIAN_POINT('Ctrl Pts',(69.7585650517838,236.552517353318,6.50953957206602)) ;
#71548 = CARTESIAN_POINT('Ctrl Pts',(69.7608899925434,236.551777928187,6.50695259265009)) ;
#71549 = CARTESIAN_POINT('Ctrl Pts',(69.7632200146727,236.551026664361,6.50436926896037)) ;
#71550 = CARTESIAN_POINT('Ctrl Pts',(69.7655549836074,236.550263241167,6.50179017820767)) ;
#71551 = CARTESIAN_POINT('Ctrl Pts',(69.7855553820763,236.543724067204,6.47969873109053)) ;
#71552 = CARTESIAN_POINT('Ctrl Pts',(69.8058641834356,236.53623717337,6.45803922220507)) ;
#71553 = CARTESIAN_POINT('Ctrl Pts',(69.8264406539002,236.527662460389,6.43706326451066)) ;
#71554 = CARTESIAN_POINT('Ctrl Pts',(69.8452018191249,236.519844229014,6.41793785577112)) ;
#71555 = CARTESIAN_POINT('Ctrl Pts',(69.8641859667403,236.511121916942,6.39937956713362)) ;
#71556 = CARTESIAN_POINT('Ctrl Pts',(69.883379872799,236.50135295673,6.38158428357869)) ;
#71557 = CARTESIAN_POINT('Ctrl Pts',(69.9025737788576,236.491583996518,6.36378900002375)) ;
#71558 = CARTESIAN_POINT('Ctrl Pts',(69.9219774879584,236.480769211382,6.34675558860383)) ;
#71559 = CARTESIAN_POINT('Ctrl Pts',(69.941593131925,236.468719349055,6.33070178487188)) ;
#71560 = CARTESIAN_POINT('Ctrl Pts',(69.9605431655999,236.457078370189,6.31519272884248)) ;
#71561 = CARTESIAN_POINT('Ctrl Pts',(69.979618503998,236.444325329231,6.30066100820867)) ;
#71562 = CARTESIAN_POINT('Ctrl Pts',(69.9987383388959,236.430286420514,6.28741717047954)) ;
#71563 = CARTESIAN_POINT('Ctrl Pts',(70.0140939925225,236.419011395353,6.27678068821174)) ;
#71564 = CARTESIAN_POINT('Ctrl Pts',(70.0294780291067,236.406907548822,6.26697493503162)) ;
#71565 = CARTESIAN_POINT('Ctrl Pts',(70.0448397839834,236.393906442639,6.25815306298493)) ;
#71566 = CARTESIAN_POINT('Ctrl Pts',(70.060308101801,236.380815149096,6.24926999450349)) ;
#71567 = CARTESIAN_POINT('Ctrl Pts',(70.0757532422095,236.366814289963,6.24138525515254)) ;
#71568 = CARTESIAN_POINT('Ctrl Pts',(70.0908899939579,236.352010662878,6.23482038635288)) ;
#71569 = CARTESIAN_POINT('Ctrl Pts',(70.1033160142712,236.339858110341,6.22943117244389)) ;
#71570 = CARTESIAN_POINT('Ctrl Pts',(70.115581139014,236.32708527742,6.22494177541271)) ;
#71571 = CARTESIAN_POINT('Ctrl Pts',(70.1275653443907,236.313786509202,6.22144964599584)) ;
#71572 = CARTESIAN_POINT('Ctrl Pts',(70.1343467817221,236.306261207322,6.21947357365321)) ;
#71573 = CARTESIAN_POINT('Ctrl Pts',(70.1410387242341,236.298566702784,6.21781689625157)) ;
#71574 = CARTESIAN_POINT('Ctrl Pts',(70.147623118448,236.2907136989,6.21649820714759)) ;
#71575 = CARTESIAN_POINT('Ctrl Pts',(70.1490267954304,236.289039576659,6.21621708583529)) ;
#71576 = CARTESIAN_POINT('Ctrl Pts',(70.1504255841125,236.287358685623,6.21595091721346)) ;
#71577 = CARTESIAN_POINT('Ctrl Pts',(70.1518191192861,236.285671000608,6.21570025382672)) ;
#71578 = CARTESIAN_POINT('Ctrl Pts',(70.16192767474,236.273428713588,6.21388196836604)) ;
#71579 = CARTESIAN_POINT('Ctrl Pts',(70.1717615809203,236.260825207069,6.21288083219659)) ;
#71580 = CARTESIAN_POINT('Ctrl Pts',(70.1812304076324,236.247940575129,6.21273144315338)) ;
#71581 = CARTESIAN_POINT('Ctrl Pts',(70.1834031091985,236.244984088455,6.21269716458667)) ;
#71582 = CARTESIAN_POINT('Ctrl Pts',(70.1855564979326,236.242012986854,6.21270766617075)) ;
#71583 = CARTESIAN_POINT('Ctrl Pts',(70.1876893200618,236.239028564853,6.21276324896012)) ;
#71584 = CARTESIAN_POINT('Ctrl Pts',(70.1994859153622,236.222521788191,6.21307067622421)) ;
#71585 = CARTESIAN_POINT('Ctrl Pts',(70.2106516821943,236.205608285263,6.21475861764742)) ;
#71586 = CARTESIAN_POINT('Ctrl Pts',(70.2211478113664,236.188515258521,6.21764264372665)) ;
#71587 = CARTESIAN_POINT('Ctrl Pts',(70.2324846782147,236.170053084034,6.220757679671)) ;
#71588 = CARTESIAN_POINT('Ctrl Pts',(70.2430369254153,236.151370609642,6.22528290282593)) ;
#71589 = CARTESIAN_POINT('Ctrl Pts',(70.2526957215038,236.132674355337,6.23114154687197)) ;
#71590 = CARTESIAN_POINT('Ctrl Pts',(70.2564754921352,236.125357961835,6.2334342063817)) ;
#71591 = CARTESIAN_POINT('Ctrl Pts',(70.260118033631,236.11803973881,6.23593133092263)) ;
#71592 = CARTESIAN_POINT('Ctrl Pts',(70.2636152474668,236.110733253645,6.23862924431399)) ;
#71593 = CARTESIAN_POINT('Ctrl Pts',(70.2709385177015,236.095433255464,6.2442787555428)) ;
#71594 = CARTESIAN_POINT('Ctrl Pts',(70.2777253779092,236.080166897609,6.25069647533058)) ;
#71595 = CARTESIAN_POINT('Ctrl Pts',(70.2839124106202,236.065060026814,6.25783535999049)) ;
#71596 = CARTESIAN_POINT('Ctrl Pts',(70.2930019121523,236.04286620117,6.26832324749414)) ;
#71597 = CARTESIAN_POINT('Ctrl Pts',(70.3007972127425,236.021015255836,6.28036894733972)) ;
#71598 = CARTESIAN_POINT('Ctrl Pts',(70.3075542718491,235.99953565987,6.29352856224887)) ;
#71599 = CARTESIAN_POINT('Ctrl Pts',(70.3098379004578,235.992276374568,6.29797601085224)) ;
#71600 = CARTESIAN_POINT('Ctrl Pts',(70.3120027927952,235.985059868179,6.3025504679656)) ;
#71601 = CARTESIAN_POINT('Ctrl Pts',(70.3140583396407,235.977888291778,6.30723419110208)) ;
#71602 = CARTESIAN_POINT('Ctrl Pts',(70.3196248424662,235.958467376908,6.31991790012607)) ;
#71603 = CARTESIAN_POINT('Ctrl Pts',(70.3243904463304,235.939374283972,6.33340375113264)) ;
#71604 = CARTESIAN_POINT('Ctrl Pts',(70.3283435121341,235.92071582897,6.3475713681177)) ;
#71605 = CARTESIAN_POINT('Ctrl Pts',(70.3301707656114,235.912091199764,6.35412016560448)) ;
#71606 = CARTESIAN_POINT('Ctrl Pts',(70.3318423411922,235.903547471452,6.36080440747604)) ;
#71607 = CARTESIAN_POINT('Ctrl Pts',(70.3333637193716,235.895089211632,6.36761024660822)) ;
#71608 = CARTESIAN_POINT('Ctrl Pts',(70.3399404610533,235.858525133966,6.39703110100394)) ;
#71609 = CARTESIAN_POINT('Ctrl Pts',(70.3437132892228,235.823554781582,6.42872456076543)) ;
#71610 = CARTESIAN_POINT('Ctrl Pts',(70.3453514963652,235.789975276158,6.46185814658185)) ;
#71611 = CARTESIAN_POINT('Ctrl Pts',(70.3461125296866,235.774375830958,6.47725043868668)) ;
#71612 = CARTESIAN_POINT('Ctrl Pts',(70.3464123831586,235.75907715216,6.49295347092891)) ;
#71613 = CARTESIAN_POINT('Ctrl Pts',(70.3463158622058,235.74406175549,6.50888324943074)) ;
#71614 = CARTESIAN_POINT('Ctrl Pts',(70.3461706709433,235.721474904293,6.53284555589007)) ;
#71615 = CARTESIAN_POINT('Ctrl Pts',(70.3451288208109,235.699528711558,6.55732105604831)) ;
#71616 = CARTESIAN_POINT('Ctrl Pts',(70.3432478451576,235.678198197327,6.58223895751767)) ;
#71617 = CARTESIAN_POINT('Ctrl Pts',(70.3395731031339,235.636526133739,6.63091947048106)) ;
#71618 = CARTESIAN_POINT('Ctrl Pts',(70.332883258592,235.597151168654,6.68111805683607)) ;
#71619 = CARTESIAN_POINT('Ctrl Pts',(70.3237807975196,235.559733632043,6.73226848360573)) ;
#71620 = CARTESIAN_POINT('Ctrl Pts',(70.3180111619245,235.536016359385,6.76469041001147)) ;
#71621 = CARTESIAN_POINT('Ctrl Pts',(70.3112713077793,235.513086421843,6.79749490207164)) ;
#71622 = CARTESIAN_POINT('Ctrl Pts',(70.3037075134353,235.490865083653,6.83053760674758)) ;
#71623 = CARTESIAN_POINT('Ctrl Pts',(70.2907203769847,235.452710747606,6.8872723743532)) ;
#71624 = CARTESIAN_POINT('Ctrl Pts',(70.2753055266936,235.416643266994,6.94471046359219)) ;
#71625 = CARTESIAN_POINT('Ctrl Pts',(70.2576459683243,235.382564105862,7.00265575482928)) ;
#71626 = CARTESIAN_POINT('Ctrl Pts',(70.2404810591012,235.349439511521,7.05897798232704)) ;
#71627 = CARTESIAN_POINT('Ctrl Pts',(70.221276258631,235.318152724197,7.11572953305135)) ;
#71628 = CARTESIAN_POINT('Ctrl Pts',(70.2002285180487,235.288628757204,7.17267980084144)) ;
#71629 = CARTESIAN_POINT('Ctrl Pts',(70.1609601392379,235.522398454576,7.27867958886635)) ;
#71630 = CARTESIAN_POINT('Ctrl Pts',(70.1931850042782,235.567095701812,7.16316434207535)) ;
#71631 = CARTESIAN_POINT('Ctrl Pts',(70.2467521307728,235.666850632939,6.93376990304091)) ;
#71632 = CARTESIAN_POINT('Ctrl Pts',(70.2791573181385,235.82106630907,6.66059058867321)) ;
#71633 = CARTESIAN_POINT('Ctrl Pts',(70.2719462922848,235.950192751371,6.49243937586827)) ;
#71634 = CARTESIAN_POINT('Ctrl Pts',(70.2543651218475,236.031343606776,6.41122181800393)) ;
#71635 = CARTESIAN_POINT('Ctrl Pts',(70.2232735078896,236.127109061982,6.335121754773)) ;
#71636 = CARTESIAN_POINT('Ctrl Pts',(70.1567428205062,236.241909737955,6.30139298231289)) ;
#71637 = CARTESIAN_POINT('Ctrl Pts',(70.0129806384832,236.38232667883,6.38459956034722)) ;
#71638 = CARTESIAN_POINT('Ctrl Pts',(69.9044401094434,236.431932501241,6.52710938218576)) ;
#71639 = CARTESIAN_POINT('Ctrl Pts',(69.82184001658,236.455045685299,6.65331962753031)) ;
#71640 = CARTESIAN_POINT('Ctrl Pts',(69.7565000731658,236.470099247129,6.75725825753585)) ;
#71641 = CARTESIAN_POINT('Ctrl Pts',(69.640759497392,236.479083143309,6.96268985033138)) ;
#71642 = CARTESIAN_POINT('Ctrl Pts',(69.5434011590231,236.46143041754,7.16318512433996)) ;
#71643 = CARTESIAN_POINT('Ctrl Pts',(69.4909429592657,236.444597987514,7.27867958884206)) ;
#71644 = CARTESIAN_POINT('Origin',(80.2783628290597,238.640065792321,7.2786795888419)) ;
#71645 = CARTESIAN_POINT('',(80.3408628290597,238.830049344241,7.27867958883748)) ;
#71646 = CARTESIAN_POINT('Origin',(80.2783628290597,238.640065792321,7.2786795888419)) ;
#71647 = CARTESIAN_POINT('',(80.4465004238194,238.617844312347,7.17267980084142)) ;
#71648 = CARTESIAN_POINT('Origin',(80.2783628290597,238.640065792321,7.2786795888419)) ;
#71649 = CARTESIAN_POINT('Origin',(80.2783628290572,238.640065792322,7.27867958883786)) ;
#71650 = CARTESIAN_POINT('Origin',(70.5337979397592,235.19483040233,7.2786795888419)) ;
#71651 = CARTESIAN_POINT('',(70.6507612836456,235.032597310185,7.2786795888375)) ;
#71652 = CARTESIAN_POINT('Origin',(70.5337979397592,235.19483040233,7.2786795888419)) ;
#71653 = CARTESIAN_POINT('',(70.4169915862637,235.071865688989,7.17267980084143)) ;
#71654 = CARTESIAN_POINT('Origin',(70.5337979397592,235.19483040233,7.2786795888419)) ;
#71655 = CARTESIAN_POINT('Origin',(70.5337979397612,235.194830402331,7.27867958883792)) ;
#71656 = CARTESIAN_POINT('Origin',(74.5283628290597,239.4,7.2786795888419)) ;
#71657 = CARTESIAN_POINT('Origin',(74.5283628290597,239.4,7.17267980084126)) ;
#71658 = CARTESIAN_POINT('Origin',(80.2317703825364,238.345892662512,7.27867958884205)) ;
#71659 = CARTESIAN_POINT('',(80.232503268608,238.145894005322,7.2786795888379)) ;
#71660 = CARTESIAN_POINT('Origin',(80.2317703825363,238.345892662512,7.27867958883749)) ;
#71661 = CARTESIAN_POINT('',(80.398545552619,238.31506917167,7.17267980084126)) ;
#71662 = CARTESIAN_POINT('Origin',(80.2317703825364,238.345892662512,7.27867958884205)) ;
#71663 = CARTESIAN_POINT('Origin',(80.2317703825363,238.345892662512,7.2786795888419)) ;
#71664 = CARTESIAN_POINT('Origin',(71.763397316992,234.301474162343,7.27867958886637)) ;
#71665 = CARTESIAN_POINT('',(71.5729608166685,234.362580130501,7.27867958819176)) ;
#71666 = CARTESIAN_POINT('Origin',(71.7633973169967,234.301474162358,7.27867958812535)) ;
#71667 = CARTESIAN_POINT('',(71.6825460733849,234.152386532589,7.17267980084127)) ;
#71668 = CARTESIAN_POINT('Origin',(71.763397316992,234.301474162343,7.27867958886637)) ;
#71669 = CARTESIAN_POINT('Origin',(71.7633973169967,234.301474162358,7.2786795888419)) ;
#71670 = CARTESIAN_POINT('Ctrl Pts',(71.5729608165702,234.362580130195,7.27867958886637)) ;
#71671 = CARTESIAN_POINT('Ctrl Pts',(71.5897962754558,234.415047769378,7.16316434207538)) ;
#71672 = CARTESIAN_POINT('Ctrl Pts',(71.6099156712164,234.526473499131,6.93376990288358)) ;
#71673 = CARTESIAN_POINT('Ctrl Pts',(71.5930795710948,234.683155076464,6.66059058845597)) ;
#71674 = CARTESIAN_POINT('Ctrl Pts',(71.546319212863,234.80373329132,6.49243937563568)) ;
#71675 = CARTESIAN_POINT('Ctrl Pts',(71.5045215327204,234.875479460712,6.41122181777537)) ;
#71676 = CARTESIAN_POINT('Ctrl Pts',(71.4453584975031,234.956949983836,6.33512175456427)) ;
#71677 = CARTESIAN_POINT('Ctrl Pts',(71.3466086938307,235.045572801762,6.30139298216567)) ;
#71678 = CARTESIAN_POINT('Ctrl Pts',(71.1664915127874,235.134692290987,6.38459956020394)) ;
#71679 = CARTESIAN_POINT('Ctrl Pts',(71.0479342931672,235.148329363567,6.52710938215577)) ;
#71680 = CARTESIAN_POINT('Ctrl Pts',(70.9622345699239,235.144786475434,6.65331962754072)) ;
#71681 = CARTESIAN_POINT('Ctrl Pts',(70.8954407845371,235.138912110575,6.75725825755124)) ;
#71682 = CARTESIAN_POINT('Ctrl Pts',(70.7825887791445,235.111690498715,6.96268985038042)) ;
#71683 = CARTESIAN_POINT('Ctrl Pts',(70.6954504894233,235.064816377666,7.16318512433998)) ;
#71684 = CARTESIAN_POINT('Ctrl Pts',(70.6507612836455,235.032597310185,7.2786795888421)) ;
#71685 = CARTESIAN_POINT('Ctrl Pts',(71.5590838983549,234.319332770985,7.24979207610078)) ;
#71686 = CARTESIAN_POINT('Ctrl Pts',(71.5808415646835,234.37314582499,7.13555826270378)) ;
#71687 = CARTESIAN_POINT('Ctrl Pts',(71.6098507007678,234.489331380785,6.90834410923801)) ;
#71688 = CARTESIAN_POINT('Ctrl Pts',(71.6003938507359,234.656438817778,6.6372185448683)) ;
#71689 = CARTESIAN_POINT('Ctrl Pts',(71.5551587087757,234.786375712703,6.47017555471278)) ;
#71690 = CARTESIAN_POINT('Ctrl Pts',(71.5126305991571,234.863842028009,6.38946600672481)) ;
#71691 = CARTESIAN_POINT('Ctrl Pts',(71.4513047303754,234.951825777958,6.3138257191277)) ;
#71692 = CARTESIAN_POINT('Ctrl Pts',(71.3464855445711,235.047095168322,6.28029130286015)) ;
#71693 = CARTESIAN_POINT('Ctrl Pts',(71.1534584863863,235.140103278427,6.36301245411851)) ;
#71694 = CARTESIAN_POINT('Ctrl Pts',(71.0265076986766,235.150691226064,6.50464016473808)) ;
#71695 = CARTESIAN_POINT('Ctrl Pts',(70.9357509710693,235.143225003883,6.62996437516892)) ;
#71696 = CARTESIAN_POINT('Ctrl Pts',(70.8651724509822,235.133918658977,6.73315731436466)) ;
#71697 = CARTESIAN_POINT('Ctrl Pts',(70.747148929931,235.098825384429,6.93698942444201)) ;
#71698 = CARTESIAN_POINT('Ctrl Pts',(70.658366573421,235.043350611714,7.1355788144266)) ;
#71699 = CARTESIAN_POINT('Ctrl Pts',(70.6139188044143,235.006035407734,7.24979207607677)) ;
#71700 = CARTESIAN_POINT('Ctrl Pts',(71.573248206895,234.231922552512,7.19960828027642)) ;
#71701 = CARTESIAN_POINT('Ctrl Pts',(71.5998261352915,234.293016165325,7.08745240215403)) ;
#71702 = CARTESIAN_POINT('Ctrl Pts',(71.6362729570513,234.42482681484,6.86383162135823)) ;
#71703 = CARTESIAN_POINT('Ctrl Pts',(71.6292174740789,234.61406352507,6.59616799904429)) ;
#71704 = CARTESIAN_POINT('Ctrl Pts',(71.5804105563069,234.760766849778,6.43101837840856)) ;
#71705 = CARTESIAN_POINT('Ctrl Pts',(71.5336404880062,234.848055177775,6.35118130110973)) ;
#71706 = CARTESIAN_POINT('Ctrl Pts',(71.4657987775582,234.947022290368,6.27633391191204)) ;
#71707 = CARTESIAN_POINT('Ctrl Pts',(71.3490009271422,235.053722199109,6.24313661344331)) ;
#71708 = CARTESIAN_POINT('Ctrl Pts',(71.1328459558896,235.156780677101,6.32501771803124)) ;
#71709 = CARTESIAN_POINT('Ctrl Pts',(70.9902331700443,235.166943146138,6.46512805544576)) ;
#71710 = CARTESIAN_POINT('Ctrl Pts',(70.88816476135,235.15687709382,6.58894908671078)) ;
#71711 = CARTESIAN_POINT('Ctrl Pts',(70.8087673844567,235.145022893286,6.69087982220983)) ;
#71712 = CARTESIAN_POINT('Ctrl Pts',(70.6759122620273,235.102631894295,6.8920271278871)) ;
#71713 = CARTESIAN_POINT('Ctrl Pts',(70.5762912057495,235.036643355181,7.08747258003699)) ;
#71714 = CARTESIAN_POINT('Ctrl Pts',(70.5264097344936,234.992495222681,7.19960828025285)) ;
#71715 = CARTESIAN_POINT('Ctrl Pts',(71.6462194886202,234.169665602295,7.17608503413731)) ;
#71716 = CARTESIAN_POINT('Ctrl Pts',(71.6700597720785,234.237897327217,7.06213458186478)) ;
#71717 = CARTESIAN_POINT('Ctrl Pts',(71.6996436221789,234.383391234504,6.83550821965688)) ;
#71718 = CARTESIAN_POINT('Ctrl Pts',(71.6803019468063,234.589302109655,6.5651024936217)) ;
#71719 = CARTESIAN_POINT('Ctrl Pts',(71.6199016712978,234.748352879764,6.39850454439136)) ;
#71720 = CARTESIAN_POINT('Ctrl Pts',(71.5652262910956,234.843126360614,6.31801009230045)) ;
#71721 = CARTESIAN_POINT('Ctrl Pts',(71.4874979119008,234.950815022676,6.24257140281179)) ;
#71722 = CARTESIAN_POINT('Ctrl Pts',(71.3570863282151,235.068031659091,6.20912632222179)) ;
#71723 = CARTESIAN_POINT('Ctrl Pts',(71.1190226491792,235.185429613822,6.29162716700193)) ;
#71724 = CARTESIAN_POINT('Ctrl Pts',(70.962736801447,235.202516154191,6.43287717376783)) ;
#71725 = CARTESIAN_POINT('Ctrl Pts',(70.8501961956108,235.196819712128,6.55786810061549)) ;
#71726 = CARTESIAN_POINT('Ctrl Pts',(70.7625576021184,235.188202884286,6.66078690790468)) ;
#71727 = CARTESIAN_POINT('Ctrl Pts',(70.6150239709294,235.150384489946,6.86407978397195)) ;
#71728 = CARTESIAN_POINT('Ctrl Pts',(70.5021653146945,235.086406927003,7.06215508260831)) ;
#71729 = CARTESIAN_POINT('Ctrl Pts',(70.444650490152,235.042656580033,7.17608503411336)) ;
#71730 = CARTESIAN_POINT('Ctrl Pts',(71.6825460733761,234.152386532576,7.17267980086574)) ;
#71731 = CARTESIAN_POINT('Ctrl Pts',(71.7046433227907,234.222533208,7.05716455407474)) ;
#71732 = CARTESIAN_POINT('Ctrl Pts',(71.7302306178125,234.371772761628,6.82777011488293)) ;
#71733 = CARTESIAN_POINT('Ctrl Pts',(71.7044810855518,234.582548736796,6.55459080045533)) ;
#71734 = CARTESIAN_POINT('Ctrl Pts',(71.6384168715341,234.745574454467,6.38643958763504)) ;
#71735 = CARTESIAN_POINT('Ctrl Pts',(71.5800181231714,234.842935073619,6.30522202977473)) ;
#71736 = CARTESIAN_POINT('Ctrl Pts',(71.4977369738496,234.953790279167,6.22912196656362)) ;
#71737 = CARTESIAN_POINT('Ctrl Pts',(71.3613565433507,235.075262197541,6.19539319416503)) ;
#71738 = CARTESIAN_POINT('Ctrl Pts',(71.1143945569827,235.199314714521,6.27859977220329)) ;
#71739 = CARTESIAN_POINT('Ctrl Pts',(70.9530872593356,235.220270342818,6.42110959415512)) ;
#71740 = CARTESIAN_POINT('Ctrl Pts',(70.8368680780374,235.217258438914,6.54731983954008)) ;
#71741 = CARTESIAN_POINT('Ctrl Pts',(70.7463714132023,235.210702036941,6.65125846955059)) ;
#71742 = CARTESIAN_POINT('Ctrl Pts',(70.5939398063231,235.176204519588,6.85669006237978)) ;
#71743 = CARTESIAN_POINT('Ctrl Pts',(70.4768658395408,235.114550256101,7.05718533633935)) ;
#71744 = CARTESIAN_POINT('Ctrl Pts',(70.4169915862637,235.071865688989,7.17267980084146)) ;
#71745 = CARTESIAN_POINT('Ctrl Pts',(70.4169915862637,235.071865688989,7.17267980084144)) ;
#71746 = CARTESIAN_POINT('Ctrl Pts',(70.4607099053372,235.103032633416,7.08834933200133)) ;
#71747 = CARTESIAN_POINT('Ctrl Pts',(70.5082722694194,235.130219873369,7.00441094571219)) ;
#71748 = CARTESIAN_POINT('Ctrl Pts',(70.5600295350521,235.152619366136,6.92170697164805)) ;
#71749 = CARTESIAN_POINT('Ctrl Pts',(70.5713052003606,235.15749924494,6.90368935963091)) ;
#71750 = CARTESIAN_POINT('Ctrl Pts',(70.5827800804835,235.162151889495,6.88573017903702)) ;
#71751 = CARTESIAN_POINT('Ctrl Pts',(70.5944579998749,235.166568938161,6.86783787638139)) ;
#71752 = CARTESIAN_POINT('Ctrl Pts',(70.6025119541606,235.169615260612,6.85549802517807)) ;
#71753 = CARTESIAN_POINT('Ctrl Pts',(70.6106639301175,235.172548127615,6.84319004877812)) ;
#71754 = CARTESIAN_POINT('Ctrl Pts',(70.618915316007,235.175364627756,6.83091678541572)) ;
#71755 = CARTESIAN_POINT('Ctrl Pts',(70.6678587106083,235.19207080047,6.75811747874931)) ;
#71756 = CARTESIAN_POINT('Ctrl Pts',(70.7203017431665,235.204679995143,6.68654097097228)) ;
#71757 = CARTESIAN_POINT('Ctrl Pts',(70.7770314899421,235.211757358392,6.61755205602087)) ;
#71758 = CARTESIAN_POINT('Ctrl Pts',(70.7856208934466,235.212828936041,6.60710650211769)) ;
#71759 = CARTESIAN_POINT('Ctrl Pts',(70.7943085163447,235.213773770197,6.59672022739229)) ;
#71760 = CARTESIAN_POINT('Ctrl Pts',(70.8030970304804,235.214586964518,6.5863979193675)) ;
#71761 = CARTESIAN_POINT('Ctrl Pts',(70.8142466821517,235.215618633044,6.57330240206598)) ;
#71762 = CARTESIAN_POINT('Ctrl Pts',(70.8255587170839,235.216438416814,6.56030985646277)) ;
#71763 = CARTESIAN_POINT('Ctrl Pts',(70.8370232368604,235.216998888888,6.54750568265232)) ;
#71764 = CARTESIAN_POINT('Ctrl Pts',(70.8484926469705,235.217559600038,6.53469604706237)) ;
#71765 = CARTESIAN_POINT('Ctrl Pts',(70.8601146848551,235.217860794865,6.52207490356155)) ;
#71766 = CARTESIAN_POINT('Ctrl Pts',(70.8719361004024,235.217934501056,6.50953957206406)) ;
#71767 = CARTESIAN_POINT('Ctrl Pts',(70.8743757454206,235.217949712173,6.50695259261839)) ;
#71768 = CARTESIAN_POINT('Ctrl Pts',(70.8768238814666,235.217955234252,6.50436926889872)) ;
#71769 = CARTESIAN_POINT('Ctrl Pts',(70.8792804796558,235.217950720732,6.5017901781165)) ;
#71770 = CARTESIAN_POINT('Ctrl Pts',(70.9003227040899,235.217912059745,6.47969873177633)) ;
#71771 = CARTESIAN_POINT('Ctrl Pts',(70.9219510986209,235.217067365371,6.45803922365016)) ;
#71772 = CARTESIAN_POINT('Ctrl Pts',(70.94417021616,235.21527080788,6.43706326666271)) ;
#71773 = CARTESIAN_POINT('Ctrl Pts',(70.9644291113308,235.213632746881,6.41793785752039)) ;
#71774 = CARTESIAN_POINT('Ctrl Pts',(70.9851794516754,235.211203759364,6.39937956849862)) ;
#71775 = CARTESIAN_POINT('Ctrl Pts',(71.0064527162314,235.207844169209,6.38158428458251)) ;
#71776 = CARTESIAN_POINT('Ctrl Pts',(71.0277259807874,235.204484579055,6.3637890006664)) ;
#71777 = CARTESIAN_POINT('Ctrl Pts',(71.0495219575831,235.20019518297,6.34675558890809)) ;
#71778 = CARTESIAN_POINT('Ctrl Pts',(71.0719011562713,235.194796650121,6.33070178486451)) ;
#71779 = CARTESIAN_POINT('Ctrl Pts',(71.0935209676707,235.189581304225,6.31519273020627)) ;
#71780 = CARTESIAN_POINT('Ctrl Pts',(71.1156035969373,235.183347045925,6.30066101074671)) ;
#71781 = CARTESIAN_POINT('Ctrl Pts',(71.1381258998109,235.175903605113,6.287417173937)) ;
#71782 = CARTESIAN_POINT('Ctrl Pts',(71.1562141705429,235.169925576431,6.27678069031052)) ;
#71783 = CARTESIAN_POINT('Ctrl Pts',(71.1745855550277,235.163168062437,6.26697493593538)) ;
#71784 = CARTESIAN_POINT('Ctrl Pts',(71.1932130168892,235.155550318177,6.25815306292166)) ;
#71785 = CARTESIAN_POINT('Ctrl Pts',(71.2119696935569,235.14787973122,6.24926999442026)) ;
#71786 = CARTESIAN_POINT('Ctrl Pts',(71.2309853984281,235.139336933751,6.2413852550664)) ;
#71787 = CARTESIAN_POINT('Ctrl Pts',(71.2499558771897,235.129935361234,6.23482038629555)) ;
#71788 = CARTESIAN_POINT('Ctrl Pts',(71.2655290706333,235.122217448085,6.22943117221267)) ;
#71789 = CARTESIAN_POINT('Ctrl Pts',(71.2811409204754,235.11385989374,6.22494177505686)) ;
#71790 = CARTESIAN_POINT('Ctrl Pts',(71.2966481230571,235.104915336306,6.22144964558793)) ;
#71791 = CARTESIAN_POINT('Ctrl Pts',(71.3054230987959,235.099853928611,6.21947357342371)) ;
#71792 = CARTESIAN_POINT('Ctrl Pts',(71.3141652464035,235.094603944233,6.21781689615633)) ;
#71793 = CARTESIAN_POINT('Ctrl Pts',(71.3228540885002,235.089169983791,6.21649820714117)) ;
#71794 = CARTESIAN_POINT('Ctrl Pts',(71.324706396824,235.088011558992,6.21621708583501)) ;
#71795 = CARTESIAN_POINT('Ctrl Pts',(71.3265561477709,235.086845186119,6.21595091721855)) ;
#71796 = CARTESIAN_POINT('Ctrl Pts',(71.3284030017896,235.085670728364,6.21570025383654)) ;
#71797 = CARTESIAN_POINT('Ctrl Pts',(71.3417998851196,235.077151336275,6.21388196822763)) ;
#71798 = CARTESIAN_POINT('Ctrl Pts',(71.355047184409,235.068203532669,6.2128808320335)) ;
#71799 = CARTESIAN_POINT('Ctrl Pts',(71.3680341449888,235.0588755471,6.21273144306716)) ;
#71800 = CARTESIAN_POINT('Ctrl Pts',(71.3710141106076,235.056735163589,6.21269716453211)) ;
#71801 = CARTESIAN_POINT('Ctrl Pts',(71.3739802249021,235.054574912477,6.21270766611658)) ;
#71802 = CARTESIAN_POINT('Ctrl Pts',(71.376930895434,235.052395637495,6.21276324887439)) ;
#71803 = CARTESIAN_POINT('Ctrl Pts',(71.3932509988059,235.040342108444,6.21307067606536)) ;
#71804 = CARTESIAN_POINT('Ctrl Pts',(71.4090968339605,235.027706822968,6.21475861749067)) ;
#71805 = CARTESIAN_POINT('Ctrl Pts',(71.4243612817605,235.014693870785,6.21764264357176)) ;
#71806 = CARTESIAN_POINT('Ctrl Pts',(71.4408484138844,235.00063857938,6.22075768053023)) ;
#71807 = CARTESIAN_POINT('Ctrl Pts',(71.456657404311,234.986131309192,6.22528290568737)) ;
#71808 = CARTESIAN_POINT('Ctrl Pts',(71.4716209298653,234.971334841834,6.23114155254727)) ;
#71809 = CARTESIAN_POINT('Ctrl Pts',(71.4774765901959,234.965544556208,6.23343421050972)) ;
#71810 = CARTESIAN_POINT('Ctrl Pts',(71.4832023034251,234.959710124551,6.23593133315564)) ;
#71811 = CARTESIAN_POINT('Ctrl Pts',(71.4887861748817,234.953841947605,6.23862924430743)) ;
#71812 = CARTESIAN_POINT('Ctrl Pts',(71.5004789781708,234.941553799636,6.24427875551742)) ;
#71813 = CARTESIAN_POINT('Ctrl Pts',(71.5116512297788,234.929131885705,6.2506964752804)) ;
#71814 = CARTESIAN_POINT('Ctrl Pts',(71.52220372733,234.91667629609,6.25783535991065)) ;
#71815 = CARTESIAN_POINT('Ctrl Pts',(71.5377066262744,234.898377524056,6.26832324739526)) ;
#71816 = CARTESIAN_POINT('Ctrl Pts',(71.5518727111388,234.880004920488,6.28036894721856)) ;
#71817 = CARTESIAN_POINT('Ctrl Pts',(71.5649366164117,234.861664656893,6.293528562104)) ;
#71818 = CARTESIAN_POINT('Ctrl Pts',(71.5693517188205,234.855466346335,6.29797601071645)) ;
#71819 = CARTESIAN_POINT('Ctrl Pts',(71.5736406769129,234.849272029415,6.30255046783972)) ;
#71820 = CARTESIAN_POINT('Ctrl Pts',(71.5778117571322,234.843086653838,6.30723419098684)) ;
#71821 = CARTESIAN_POINT('Ctrl Pts',(71.589107208696,234.826336410121,6.31991790004191)) ;
#71822 = CARTESIAN_POINT('Ctrl Pts',(71.5995396575293,234.809650452202,6.33340375108472)) ;
#71823 = CARTESIAN_POINT('Ctrl Pts',(71.6090650262337,234.793126771453,6.34757136811092)) ;
#71824 = CARTESIAN_POINT('Ctrl Pts',(71.6134680045255,234.785488914075,6.35412016555376)) ;
#71825 = CARTESIAN_POINT('Ctrl Pts',(71.6176979245902,234.777879890904,6.36080440737922)) ;
#71826 = CARTESIAN_POINT('Ctrl Pts',(71.6217585872235,234.770305739548,6.36761024646398)) ;
#71827 = CARTESIAN_POINT('Ctrl Pts',(71.6393123616443,234.737563560173,6.39703110084805)) ;
#71828 = CARTESIAN_POINT('Ctrl Pts',(71.6537069676523,234.705470646685,6.42872456059852)) ;
#71829 = CARTESIAN_POINT('Ctrl Pts',(71.6656416330752,234.674040873088,6.46185814640417)) ;
#71830 = CARTESIAN_POINT('Ctrl Pts',(71.6711859124497,234.659440091304,6.47725043851097)) ;
#71831 = CARTESIAN_POINT('Ctrl Pts',(71.6761986417932,234.644982842956,6.49295347075555)) ;
#71832 = CARTESIAN_POINT('Ctrl Pts',(71.6807468576651,234.630672525488,6.50888324926009)) ;
#71833 = CARTESIAN_POINT('Ctrl Pts',(71.6875884934589,234.609146286856,6.53284555577163)) ;
#71834 = CARTESIAN_POINT('Ctrl Pts',(71.6933793816343,234.587952267802,6.55732105598457)) ;
#71835 = CARTESIAN_POINT('Ctrl Pts',(71.6981819588895,234.567084489756,6.5822389575114)) ;
#71836 = CARTESIAN_POINT('Ctrl Pts',(71.7075644473025,234.526316444743,6.63091947006312)) ;
#71837 = CARTESIAN_POINT('Ctrl Pts',(71.7133695604041,234.486801352293,6.68111805597746)) ;
#71838 = CARTESIAN_POINT('Ctrl Pts',(71.7162752602129,234.448402345422,6.73226848229616)) ;
#71839 = CARTESIAN_POINT('Ctrl Pts',(71.7181170510495,234.424062962952,6.76469040908816)) ;
#71840 = CARTESIAN_POINT('Ctrl Pts',(71.7187928092504,234.400172566665,6.79749490154681)) ;
#71841 = CARTESIAN_POINT('Ctrl Pts',(71.7184659844885,234.376701476897,6.83053760662836)) ;
#71842 = CARTESIAN_POINT('Ctrl Pts',(71.7179048219905,234.336401301076,6.88727237427162)) ;
#71843 = CARTESIAN_POINT('Ctrl Pts',(71.7143898926252,234.297335637882,6.94471046355436)) ;
#71844 = CARTESIAN_POINT('Ctrl Pts',(71.7081256945041,234.259467325945,7.00265575483063)) ;
#71845 = CARTESIAN_POINT('Ctrl Pts',(71.7020369583204,234.222659715993,7.0589779823287)) ;
#71846 = CARTESIAN_POINT('Ctrl Pts',(71.693440256672,234.186969603319,7.11572953305254)) ;
#71847 = CARTESIAN_POINT('Ctrl Pts',(71.6825460733806,234.152386532591,7.17267980084152)) ;
#71848 = CARTESIAN_POINT('Ctrl Pts',(71.5729608165702,234.362580130195,7.27867958886637)) ;
#71849 = CARTESIAN_POINT('Ctrl Pts',(71.5897962754558,234.415047769378,7.16316434207538)) ;
#71850 = CARTESIAN_POINT('Ctrl Pts',(71.6099156712164,234.526473499131,6.93376990288358)) ;
#71851 = CARTESIAN_POINT('Ctrl Pts',(71.5930795710948,234.683155076464,6.66059058845597)) ;
#71852 = CARTESIAN_POINT('Ctrl Pts',(71.546319212863,234.80373329132,6.49243937563568)) ;
#71853 = CARTESIAN_POINT('Ctrl Pts',(71.5045215327204,234.875479460712,6.41122181777537)) ;
#71854 = CARTESIAN_POINT('Ctrl Pts',(71.4453584975031,234.956949983836,6.33512175456427)) ;
#71855 = CARTESIAN_POINT('Ctrl Pts',(71.3466086938307,235.045572801762,6.30139298216567)) ;
#71856 = CARTESIAN_POINT('Ctrl Pts',(71.1664915127874,235.134692290987,6.38459956020394)) ;
#71857 = CARTESIAN_POINT('Ctrl Pts',(71.0479342931672,235.148329363567,6.52710938215577)) ;
#71858 = CARTESIAN_POINT('Ctrl Pts',(70.9622345699239,235.144786475434,6.65331962754072)) ;
#71859 = CARTESIAN_POINT('Ctrl Pts',(70.8954407845371,235.138912110575,6.75725825755124)) ;
#71860 = CARTESIAN_POINT('Ctrl Pts',(70.7825887791445,235.111690498715,6.96268985038042)) ;
#71861 = CARTESIAN_POINT('Ctrl Pts',(70.6954504894233,235.064816377666,7.16318512433998)) ;
#71862 = CARTESIAN_POINT('Ctrl Pts',(70.6507612836455,235.032597310185,7.2786795888421)) ;
#71863 = CARTESIAN_POINT('Origin',(79.7621052129773,236.900411902176,7.2786795888419)) ;
#71864 = CARTESIAN_POINT('',(79.8802543914407,237.061783435069,7.27867958883751)) ;
#71865 = CARTESIAN_POINT('Origin',(79.7621052129773,236.900411902176,7.2786795888419)) ;
#71866 = CARTESIAN_POINT('',(79.9151467531554,236.82732064467,7.17267980084143)) ;
#71867 = CARTESIAN_POINT('Origin',(79.7621052129773,236.900411902176,7.2786795888419)) ;
#71868 = CARTESIAN_POINT('Origin',(79.7621052129753,236.900411902177,7.27867958883791)) ;
#71869 = CARTESIAN_POINT('Origin',(72.0287747312354,234.166257616082,7.2786795888419)) ;
#71870 = CARTESIAN_POINT('',(72.1901462641291,234.048108437619,7.27867958883748)) ;
#71871 = CARTESIAN_POINT('Origin',(72.0287747312355,234.166257616082,7.2786795888419)) ;
#71872 = CARTESIAN_POINT('',(71.9556834737297,234.013216075904,7.1726798008414)) ;
#71873 = CARTESIAN_POINT('Origin',(72.0287747312354,234.166257616082,7.2786795888419)) ;
#71874 = CARTESIAN_POINT('Origin',(72.028774731237,234.166257616084,7.2786795888379)) ;
#71875 = CARTESIAN_POINT('Origin',(74.5283628290597,239.4,7.2786795888419)) ;
#71876 = CARTESIAN_POINT('Origin',(74.5283628290597,239.4,7.17267980084127)) ;
#71877 = CARTESIAN_POINT('Origin',(79.6268886667165,236.635034487932,7.27867958886636)) ;
#71878 = CARTESIAN_POINT('',(79.5657826985583,236.444597987609,7.27867958819178)) ;
#71879 = CARTESIAN_POINT('Origin',(79.6268886667016,236.635034487937,7.27867958812537)) ;
#71880 = CARTESIAN_POINT('',(79.775976296471,236.554183244325,7.17267980084126)) ;
#71881 = CARTESIAN_POINT('Origin',(79.6268886667165,236.635034487932,7.27867958886636)) ;
#71882 = CARTESIAN_POINT('Origin',(79.6268886667016,236.635034487937,7.2786795888419)) ;
#71883 = CARTESIAN_POINT('Origin',(73.474255491572,233.696592446523,7.27867958884206)) ;
#71884 = CARTESIAN_POINT('',(73.2742568343815,233.695859560452,7.2786795888379)) ;
#71885 = CARTESIAN_POINT('Origin',(73.474255491572,233.696592446523,7.27867958883749)) ;
#71886 = CARTESIAN_POINT('',(73.4434320007296,233.529817276441,7.17267980084128)) ;
#71887 = CARTESIAN_POINT('Origin',(73.474255491572,233.696592446523,7.27867958884206)) ;
#71888 = CARTESIAN_POINT('Origin',(73.474255491572,233.696592446523,7.2786795888419)) ;
#71889 = CARTESIAN_POINT('Ctrl Pts',(73.2742568343815,233.69585956045,7.27867958884206)) ;
#71890 = CARTESIAN_POINT('Ctrl Pts',(73.2740549596697,233.750949529716,7.16318984200169)) ;
#71891 = CARTESIAN_POINT('Ctrl Pts',(73.2587365790027,233.863147817193,6.93380129444964)) ;
#71892 = CARTESIAN_POINT('Ctrl Pts',(73.1943130298186,234.006881253322,6.66079578040121)) ;
#71893 = CARTESIAN_POINT('Ctrl Pts',(73.1125662143234,234.107132168956,6.49260105919638)) ;
#71894 = CARTESIAN_POINT('Ctrl Pts',(73.0506452553059,234.162420516523,6.41145403426995)) ;
#71895 = CARTESIAN_POINT('Ctrl Pts',(72.9691982052928,234.221689136819,6.33519282548988)) ;
#71896 = CARTESIAN_POINT('Ctrl Pts',(72.8478698697775,234.275176193887,6.30217004615784)) ;
#71897 = CARTESIAN_POINT('Ctrl Pts',(72.723618971598,234.293644522184,6.35347099290516)) ;
#71898 = CARTESIAN_POINT('Ctrl Pts',(72.6451468245962,234.294029054113,6.41180850518493)) ;
#71899 = CARTESIAN_POINT('Ctrl Pts',(72.5625951046027,234.285547981313,6.49328289149882)) ;
#71900 = CARTESIAN_POINT('Ctrl Pts',(72.4375721749348,234.252605836027,6.66117410704378)) ;
#71901 = CARTESIAN_POINT('Ctrl Pts',(72.3009698631611,234.174128957134,6.93432838635655)) ;
#71902 = CARTESIAN_POINT('Ctrl Pts',(72.2226915456342,234.092559715514,7.16318668385647)) ;
#71903 = CARTESIAN_POINT('Ctrl Pts',(72.1901462641291,234.048108437619,7.27867958884204)) ;
#71904 = CARTESIAN_POINT('Ctrl Pts',(73.2744232698453,233.650440674103,7.24979207607673)) ;
#71905 = CARTESIAN_POINT('Ctrl Pts',(73.2784859949353,233.708330636419,7.13558347975436)) ;
#71906 = CARTESIAN_POINT('Ctrl Pts',(73.2701535035563,233.827800206243,6.90837543967858)) ;
#71907 = CARTESIAN_POINT('Ctrl Pts',(73.2095239949662,233.983720993006,6.63742243131242)) ;
#71908 = CARTESIAN_POINT('Ctrl Pts',(73.1263364797546,234.093345744578,6.47033622807258)) ;
#71909 = CARTESIAN_POINT('Ctrl Pts',(73.0619522577372,234.153844863798,6.38969679257593)) ;
#71910 = CARTESIAN_POINT('Ctrl Pts',(72.9764379699748,234.218648084035,6.31389624857319)) ;
#71911 = CARTESIAN_POINT('Ctrl Pts',(72.8472724531709,234.27654322756,6.28106387226434)) ;
#71912 = CARTESIAN_POINT('Ctrl Pts',(72.7146084425558,234.294866821401,6.33206532553425)) ;
#71913 = CARTESIAN_POINT('Ctrl Pts',(72.6310406400458,234.293688802942,6.39004922954425)) ;
#71914 = CARTESIAN_POINT('Ctrl Pts',(72.543443716397,234.282416742709,6.47101436009728)) ;
#71915 = CARTESIAN_POINT('Ctrl Pts',(72.4117100575662,234.242768487736,6.63779863647138)) ;
#71916 = CARTESIAN_POINT('Ctrl Pts',(72.2710645809142,234.152174672608,6.90889868284266)) ;
#71917 = CARTESIAN_POINT('Ctrl Pts',(72.1940559565118,234.060684934228,7.13558035664306)) ;
#71918 = CARTESIAN_POINT('Ctrl Pts',(72.1633150634402,234.01146161501,7.24979207607672)) ;
#71919 = CARTESIAN_POINT('Ctrl Pts',(73.3149055858816,233.571685641175,7.19960828841392)) ;
#71920 = CARTESIAN_POINT('Ctrl Pts',(73.3213023208757,233.637987511948,7.08747716866263)) ;
#71921 = CARTESIAN_POINT('Ctrl Pts',(73.3152112594166,233.774618048049,6.86386304009817)) ;
#71922 = CARTESIAN_POINT('Ctrl Pts',(73.2500249475578,233.952315913544,6.59637000664605)) ;
#71923 = CARTESIAN_POINT('Ctrl Pts',(73.158257430726,234.076786632763,6.43117772982988)) ;
#71924 = CARTESIAN_POINT('Ctrl Pts',(73.0868032929897,234.145311645297,6.35141005998548)) ;
#71925 = CARTESIAN_POINT('Ctrl Pts',(72.9916981507112,234.218557730749,6.27640397003883)) ;
#71926 = CARTESIAN_POINT('Ctrl Pts',(72.8475995469222,234.283579186381,6.24390204216934)) ;
#71927 = CARTESIAN_POINT('Ctrl Pts',(72.6992543275143,234.303453400385,6.29438512175569)) ;
#71928 = CARTESIAN_POINT('Ctrl Pts',(72.605779290744,234.301415798299,6.35175959624848)) ;
#71929 = CARTESIAN_POINT('Ctrl Pts',(72.507738968611,234.287787061284,6.43185018953203)) ;
#71930 = CARTESIAN_POINT('Ctrl Pts',(72.3603935603073,234.241172455663,6.59674275110135)) ;
#71931 = CARTESIAN_POINT('Ctrl Pts',(72.2031972386972,234.135653153317,6.86438198127782)) ;
#71932 = CARTESIAN_POINT('Ctrl Pts',(72.1180702535969,234.028943179651,7.08747410236134)) ;
#71933 = CARTESIAN_POINT('Ctrl Pts',(72.0842731348961,233.971542363323,7.1996082884139)) ;
#71934 = CARTESIAN_POINT('Ctrl Pts',(73.4035438393931,233.535025116255,7.17608503411332)) ;
#71935 = CARTESIAN_POINT('Ctrl Pts',(73.4051321830648,233.607268444389,7.06215973636355)) ;
#71936 = CARTESIAN_POINT('Ctrl Pts',(73.3882813088143,233.754794547639,6.83553949296448)) ;
#71937 = CARTESIAN_POINT('Ctrl Pts',(73.3062624638023,233.944548706618,6.56530588838826)) ;
#71938 = CARTESIAN_POINT('Ctrl Pts',(73.1996503539424,234.077181947362,6.39866484639538)) ;
#71939 = CARTESIAN_POINT('Ctrl Pts',(73.1183663427792,234.150381296654,6.31824032527891)) ;
#71940 = CARTESIAN_POINT('Ctrl Pts',(73.011160084709,234.228870150154,6.24264180022651)) ;
#71941 = CARTESIAN_POINT('Ctrl Pts',(72.8508725252478,234.299674522912,6.20989694476306)) ;
#71942 = CARTESIAN_POINT('Ctrl Pts',(72.6867266829953,234.323853007396,6.26076252232513)) ;
#71943 = CARTESIAN_POINT('Ctrl Pts',(72.5832167238411,234.324067353368,6.31859191036259)) ;
#71944 = CARTESIAN_POINT('Ctrl Pts',(72.4744843130502,234.312428441163,6.39934128183629)) ;
#71945 = CARTESIAN_POINT('Ctrl Pts',(72.3103311568753,234.26793932169,6.56568114913269)) ;
#71946 = CARTESIAN_POINT('Ctrl Pts',(72.1324342534315,234.162555555409,6.83606168702106)) ;
#71947 = CARTESIAN_POINT('Ctrl Pts',(72.0321944574505,234.053364942797,7.06215662099925)) ;
#71948 = CARTESIAN_POINT('Ctrl Pts',(71.9910147655643,233.993983633843,7.1760850341133)) ;
#71949 = CARTESIAN_POINT('Ctrl Pts',(73.4434320007296,233.52981727644,7.17267980084142)) ;
#71950 = CARTESIAN_POINT('Ctrl Pts',(73.4427713648384,233.603342920453,7.05719005400105)) ;
#71951 = CARTESIAN_POINT('Ctrl Pts',(73.4209606328348,233.753197403932,6.827801506449)) ;
#71952 = CARTESIAN_POINT('Ctrl Pts',(73.3313468227806,233.945597739259,6.55479599240056)) ;
#71953 = CARTESIAN_POINT('Ctrl Pts',(73.2181183729435,234.080261564928,6.38660127119577)) ;
#71954 = CARTESIAN_POINT('Ctrl Pts',(73.1324946015359,234.154770746277,6.30545424626932)) ;
#71955 = CARTESIAN_POINT('Ctrl Pts',(73.0199781972657,234.234864355979,6.22919303748926)) ;
#71956 = CARTESIAN_POINT('Ctrl Pts',(72.8527043400124,234.307871726469,6.19617025815722)) ;
#71957 = CARTESIAN_POINT('Ctrl Pts',(72.6819787802051,234.334286679362,6.24747120490454)) ;
#71958 = CARTESIAN_POINT('Ctrl Pts',(72.5743809047495,234.335919683504,6.30580871718431)) ;
#71959 = CARTESIAN_POINT('Ctrl Pts',(72.4613734565605,234.325771256962,6.38728310349819)) ;
#71960 = CARTESIAN_POINT('Ctrl Pts',(72.2906661705782,234.283529574643,6.55517431904313)) ;
#71961 = CARTESIAN_POINT('Ctrl Pts',(72.1050805550541,234.180466586174,6.82832859835594)) ;
#71962 = CARTESIAN_POINT('Ctrl Pts',(71.9994364250301,234.072312875397,7.05718689585584)) ;
#71963 = CARTESIAN_POINT('Ctrl Pts',(71.9556834737297,234.013216075904,7.17267980084141)) ;
#71964 = CARTESIAN_POINT('Ctrl Pts',(71.9556834737297,234.013216075904,7.17267980084141)) ;
#71965 = CARTESIAN_POINT('Ctrl Pts',(71.9775380676966,234.042734920217,7.11499110854748)) ;
#71966 = CARTESIAN_POINT('Ctrl Pts',(72.00168629204,234.071039609707,7.0574911746497)) ;
#71967 = CARTESIAN_POINT('Ctrl Pts',(72.0283121753549,234.097913331845,7.00044364508764)) ;
#71968 = CARTESIAN_POINT('Ctrl Pts',(72.0463388677926,234.116107820189,6.96182039050547)) ;
#71969 = CARTESIAN_POINT('Ctrl Pts',(72.0655008578513,234.13364659012,6.92340451249123)) ;
#71970 = CARTESIAN_POINT('Ctrl Pts',(72.0858489590221,234.15046595221,6.88527679966823)) ;
#71971 = CARTESIAN_POINT('Ctrl Pts',(72.0955555209196,234.158489215797,6.86708891071367)) ;
#71972 = CARTESIAN_POINT('Ctrl Pts',(72.1055316863788,234.16634874434,6.84896683649129)) ;
#71973 = CARTESIAN_POINT('Ctrl Pts',(72.115786645653,234.174040756174,6.83091231686833)) ;
#71974 = CARTESIAN_POINT('Ctrl Pts',(72.1793344697666,234.221706534458,6.71903225895876)) ;
#71975 = CARTESIAN_POINT('Ctrl Pts',(72.2535635063277,234.26292178182,6.60978900838434)) ;
#71976 = CARTESIAN_POINT('Ctrl Pts',(72.343325143251,234.2927507782,6.50942604602813)) ;
#71977 = CARTESIAN_POINT('Ctrl Pts',(72.3809678070854,234.305259940485,6.46733758393119)) ;
#71978 = CARTESIAN_POINT('Ctrl Pts',(72.4213378420412,234.315764249845,6.42681718884272)) ;
#71979 = CARTESIAN_POINT('Ctrl Pts',(72.4651746871031,234.323195626295,6.3893990922628)) ;
#71980 = CARTESIAN_POINT('Ctrl Pts',(72.4736237817096,234.324627946586,6.38218714446975)) ;
#71981 = CARTESIAN_POINT('Ctrl Pts',(72.4822016825239,234.325946132109,6.37509039685455)) ;
#71982 = CARTESIAN_POINT('Ctrl Pts',(72.4909136875768,234.327142557127,6.36811979451503)) ;
#71983 = CARTESIAN_POINT('Ctrl Pts',(72.506400120543,234.329269318501,6.35572887357221)) ;
#71984 = CARTESIAN_POINT('Ctrl Pts',(72.5223103024083,234.331011329692,6.34373656253294)) ;
#71985 = CARTESIAN_POINT('Ctrl Pts',(72.5386357642041,234.33230514034,6.33226488075079)) ;
#71986 = CARTESIAN_POINT('Ctrl Pts',(72.5507341861932,234.333263953474,6.32376348282031)) ;
#71987 = CARTESIAN_POINT('Ctrl Pts',(72.5630662071469,234.333977025601,6.31554417524479)) ;
#71988 = CARTESIAN_POINT('Ctrl Pts',(72.575626098791,234.33441784388,6.30765908514812)) ;
#71989 = CARTESIAN_POINT('Ctrl Pts',(72.6051375771739,234.335453617075,6.28913180222824)) ;
#71990 = CARTESIAN_POINT('Ctrl Pts',(72.6359049160563,234.334983592938,6.2724556364998)) ;
#71991 = CARTESIAN_POINT('Ctrl Pts',(72.6679687998726,234.332593398481,6.25836820375113)) ;
#71992 = CARTESIAN_POINT('Ctrl Pts',(72.680889243656,234.331630247127,6.25269154012778)) ;
#71993 = CARTESIAN_POINT('Ctrl Pts',(72.694019862766,234.330355709935,6.24743472601835)) ;
#71994 = CARTESIAN_POINT('Ctrl Pts',(72.7072883464412,234.328754661154,6.2426686581949)) ;
#71995 = CARTESIAN_POINT('Ctrl Pts',(72.7143126179355,234.327907073623,6.24014552479311)) ;
#71996 = CARTESIAN_POINT('Ctrl Pts',(72.7213755301905,234.326967996892,6.23775989279003)) ;
#71997 = CARTESIAN_POINT('Ctrl Pts',(72.7284664014194,234.325935319766,6.23552201762156)) ;
#71998 = CARTESIAN_POINT('Ctrl Pts',(72.7357423661804,234.324875686593,6.23322572703334)) ;
#71999 = CARTESIAN_POINT('Ctrl Pts',(72.7430560512114,234.323716350896,6.23108229789024)) ;
#72000 = CARTESIAN_POINT('Ctrl Pts',(72.7504018230615,234.32245331508,6.22910244381318)) ;
#72001 = CARTESIAN_POINT('Ctrl Pts',(72.7662299130018,234.319731825098,6.22483641036702)) ;
#72002 = CARTESIAN_POINT('Ctrl Pts',(72.7822005848587,234.316529935791,6.22133160592553)) ;
#72003 = CARTESIAN_POINT('Ctrl Pts',(72.798211826618,234.312812791759,6.21871235430216)) ;
#72004 = CARTESIAN_POINT('Ctrl Pts',(72.8048606278438,234.311269216803,6.21762468829436)) ;
#72005 = CARTESIAN_POINT('Ctrl Pts',(72.8115173655257,234.309636512685,6.2166896807269)) ;
#72006 = CARTESIAN_POINT('Ctrl Pts',(72.8181709115136,234.307913070068,6.21591686669063)) ;
#72007 = CARTESIAN_POINT('Ctrl Pts',(72.837047957555,234.303023420897,6.21372428454407)) ;
#72008 = CARTESIAN_POINT('Ctrl Pts',(72.8558939618855,234.297403478447,6.21284016126948)) ;
#72009 = CARTESIAN_POINT('Ctrl Pts',(72.8744943463362,234.291170524958,6.21317725828574)) ;
#72010 = CARTESIAN_POINT('Ctrl Pts',(72.8915027733682,234.285471033375,6.21348550406523)) ;
#72011 = CARTESIAN_POINT('Ctrl Pts',(72.9083106447413,234.27925859489,6.21481277495926)) ;
#72012 = CARTESIAN_POINT('Ctrl Pts',(72.9247998340907,234.272613244744,6.21708308597247)) ;
#72013 = CARTESIAN_POINT('Ctrl Pts',(72.9442413098504,234.264778086141,6.21975988199892)) ;
#72014 = CARTESIAN_POINT('Ctrl Pts',(72.9632457496712,234.256340047346,6.22374636219899)) ;
#72015 = CARTESIAN_POINT('Ctrl Pts',(72.9816154090083,234.247380942209,6.2289966565276)) ;
#72016 = CARTESIAN_POINT('Ctrl Pts',(72.9880616494754,234.244237032732,6.23083907827009)) ;
#72017 = CARTESIAN_POINT('Ctrl Pts',(72.9944292805357,234.241028994714,6.23283728580596)) ;
#72018 = CARTESIAN_POINT('Ctrl Pts',(73.0007083082323,234.237760516865,6.2349897519224)) ;
#72019 = CARTESIAN_POINT('Ctrl Pts',(73.0194856569107,234.227986177398,6.24142667316875)) ;
#72020 = CARTESIAN_POINT('Ctrl Pts',(73.0376043277885,234.217735081624,6.24908212275534)) ;
#72021 = CARTESIAN_POINT('Ctrl Pts',(73.0548238897132,234.207125592467,6.25787622350305)) ;
#72022 = CARTESIAN_POINT('Ctrl Pts',(73.0756315647307,234.194305359092,6.26850278829196)) ;
#72023 = CARTESIAN_POINT('Ctrl Pts',(73.0951264737041,234.180961642225,6.28079280784326)) ;
#72024 = CARTESIAN_POINT('Ctrl Pts',(73.1135027160114,234.167300408393,6.29423878512697)) ;
#72025 = CARTESIAN_POINT('Ctrl Pts',(73.1192898960236,234.162998113177,6.29847329018414)) ;
#72026 = CARTESIAN_POINT('Ctrl Pts',(73.1249658256639,234.158664500401,6.30282225079387)) ;
#72027 = CARTESIAN_POINT('Ctrl Pts',(73.1305357448685,234.154306431645,6.30726934661585)) ;
#72028 = CARTESIAN_POINT('Ctrl Pts',(73.1399823771323,234.146915108466,6.31481166048607)) ;
#72029 = CARTESIAN_POINT('Ctrl Pts',(73.1491242321405,234.139453369777,6.3226363299253)) ;
#72030 = CARTESIAN_POINT('Ctrl Pts',(73.1579468348379,234.131936426963,6.33072042621225)) ;
#72031 = CARTESIAN_POINT('Ctrl Pts',(73.1708502985423,234.12094255111,6.34254379020126)) ;
#72032 = CARTESIAN_POINT('Ctrl Pts',(73.1831308047004,234.109832984206,6.35489353170787)) ;
#72033 = CARTESIAN_POINT('Ctrl Pts',(73.1947996145563,234.098652078751,6.36768106647146)) ;
#72034 = CARTESIAN_POINT('Ctrl Pts',(73.2322011063735,234.062814444146,6.40866835504048)) ;
#72035 = CARTESIAN_POINT('Ctrl Pts',(73.2633187933714,234.026243273988,6.4541543849551)) ;
#72036 = CARTESIAN_POINT('Ctrl Pts',(73.2900031699536,233.989653097423,6.5017061491635)) ;
#72037 = CARTESIAN_POINT('Ctrl Pts',(73.2913623326756,233.987789385005,6.50412818758281)) ;
#72038 = CARTESIAN_POINT('Ctrl Pts',(73.2927099386585,233.985925520695,6.50655576541892)) ;
#72039 = CARTESIAN_POINT('Ctrl Pts',(73.2940462311482,233.984061599677,6.50898856002465)) ;
#72040 = CARTESIAN_POINT('Ctrl Pts',(73.3245036847171,233.941578170117,6.56443804381528)) ;
#72041 = CARTESIAN_POINT('Ctrl Pts',(73.3490786188089,233.899066190412,6.62259797169379)) ;
#72042 = CARTESIAN_POINT('Ctrl Pts',(73.3689099777686,233.856725100102,6.68241697443128)) ;
#72043 = CARTESIAN_POINT('Ctrl Pts',(73.3849820467182,233.822410309864,6.73089651324879)) ;
#72044 = CARTESIAN_POINT('Ctrl Pts',(73.3979401376789,233.788207585212,6.78046537481758)) ;
#72045 = CARTESIAN_POINT('Ctrl Pts',(73.4084145403143,233.754217734094,6.83056538013866)) ;
#72046 = CARTESIAN_POINT('Ctrl Pts',(73.4110048032138,233.745812228465,6.84295483942932)) ;
#72047 = CARTESIAN_POINT('Ctrl Pts',(73.4134432575565,233.737419716346,6.85537680140795)) ;
#72048 = CARTESIAN_POINT('Ctrl Pts',(73.415733427501,233.729040807646,6.86782833608266)) ;
#72049 = CARTESIAN_POINT('Ctrl Pts',(73.4309142280092,233.673499714833,6.95036555755346)) ;
#72050 = CARTESIAN_POINT('Ctrl Pts',(73.4395025790421,233.618495791153,7.03432129089791)) ;
#72051 = CARTESIAN_POINT('Ctrl Pts',(73.4423703243965,233.564227299757,7.11885358141502)) ;
#72052 = CARTESIAN_POINT('Ctrl Pts',(73.4429782186783,233.552723661349,7.13677243043561)) ;
#72053 = CARTESIAN_POINT('Ctrl Pts',(73.4433292491485,233.541253040478,7.1547171768976)) ;
#72054 = CARTESIAN_POINT('Ctrl Pts',(73.4434320007295,233.52981727644,7.17267980084087)) ;
#72055 = CARTESIAN_POINT('Ctrl Pts',(73.2742568343815,233.69585956045,7.27867958884206)) ;
#72056 = CARTESIAN_POINT('Ctrl Pts',(73.2740549596697,233.750949529716,7.16318984200169)) ;
#72057 = CARTESIAN_POINT('Ctrl Pts',(73.2587365790027,233.863147817193,6.93380129444964)) ;
#72058 = CARTESIAN_POINT('Ctrl Pts',(73.1943130298186,234.006881253322,6.66079578040121)) ;
#72059 = CARTESIAN_POINT('Ctrl Pts',(73.1125662143234,234.107132168956,6.49260105919638)) ;
#72060 = CARTESIAN_POINT('Ctrl Pts',(73.0506452553059,234.162420516523,6.41145403426995)) ;
#72061 = CARTESIAN_POINT('Ctrl Pts',(72.9691982052928,234.221689136819,6.33519282548988)) ;
#72062 = CARTESIAN_POINT('Ctrl Pts',(72.8478698697775,234.275176193887,6.30217004615784)) ;
#72063 = CARTESIAN_POINT('Ctrl Pts',(72.723618971598,234.293644522184,6.35347099290516)) ;
#72064 = CARTESIAN_POINT('Ctrl Pts',(72.6451468245962,234.294029054113,6.41180850518493)) ;
#72065 = CARTESIAN_POINT('Ctrl Pts',(72.5625951046027,234.285547981313,6.49328289149882)) ;
#72066 = CARTESIAN_POINT('Ctrl Pts',(72.4375721749348,234.252605836027,6.66117410704378)) ;
#72067 = CARTESIAN_POINT('Ctrl Pts',(72.3009698631611,234.174128957134,6.93432838635655)) ;
#72068 = CARTESIAN_POINT('Ctrl Pts',(72.2226915456342,234.092559715514,7.16318668385647)) ;
#72069 = CARTESIAN_POINT('Ctrl Pts',(72.1901462641291,234.048108437619,7.27867958884204)) ;
#72070 = CARTESIAN_POINT('Origin',(78.7335324267296,235.405435110699,7.2786795888419)) ;
#72071 = CARTESIAN_POINT('',(78.8957655188746,235.522398454586,7.27867958883752)) ;
#72072 = CARTESIAN_POINT('Origin',(78.7335324267296,235.405435110699,7.2786795888419)) ;
#72073 = CARTESIAN_POINT('',(78.8564971400703,235.288628757204,7.17267980084146)) ;
#72074 = CARTESIAN_POINT('Origin',(78.7335324267296,235.405435110699,7.2786795888419)) ;
#72075 = CARTESIAN_POINT('Origin',(78.7335324267282,235.405435110702,7.27867958883793)) ;
#72076 = CARTESIAN_POINT('Origin',(73.7684286213811,233.65,7.2786795888419)) ;
#72077 = CARTESIAN_POINT('',(73.9584121733008,233.5875,7.27867958883753)) ;
#72078 = CARTESIAN_POINT('Origin',(73.7684286213811,233.65,7.2786795888419)) ;
#72079 = CARTESIAN_POINT('',(73.7462071414064,233.48186240524,7.17267980084138)) ;
#72080 = CARTESIAN_POINT('Origin',(73.7684286213811,233.65,7.2786795888419)) ;
#72081 = CARTESIAN_POINT('Origin',(73.7684286213819,233.650000000002,7.27867958883792)) ;
#72082 = CARTESIAN_POINT('Origin',(74.5283628290597,239.4,7.2786795888419)) ;
#72083 = CARTESIAN_POINT('Origin',(74.5283628290597,239.4,7.17267980084128)) ;
#72084 = CARTESIAN_POINT('Origin',(78.5229277183728,235.194830402321,7.27867958886636)) ;
#72085 = CARTESIAN_POINT('',(78.4059643742222,235.032597310366,7.27867958819179)) ;
#72086 = CARTESIAN_POINT('Origin',(78.5229277183602,235.19483040233,7.27867958812537)) ;
#72087 = CARTESIAN_POINT('',(78.6397340718589,235.071865688993,7.17267980084126)) ;
#72088 = CARTESIAN_POINT('Origin',(78.5229277183728,235.194830402321,7.27867958886636)) ;
#72089 = CARTESIAN_POINT('Origin',(78.5229277183602,235.19483040233,7.2786795888419)) ;
#72090 = CARTESIAN_POINT('Origin',(75.2882970367382,233.65,7.27867958884202)) ;
#72091 = CARTESIAN_POINT('',(75.098313484818,233.587500000002,7.27867958883787)) ;
#72092 = CARTESIAN_POINT('Origin',(75.2882970367382,233.65,7.27867958883749)) ;
#72093 = CARTESIAN_POINT('',(75.3105185167129,233.48186240524,7.17267980084126)) ;
#72094 = CARTESIAN_POINT('Origin',(75.2882970367382,233.65,7.27867958884202)) ;
#72095 = CARTESIAN_POINT('Origin',(75.2882970367382,233.65,7.2786795888419)) ;
#72096 = CARTESIAN_POINT('Ctrl Pts',(75.0983134848186,233.5875,7.27867958884202)) ;
#72097 = CARTESIAN_POINT('Ctrl Pts',(75.0810977099062,233.63983142507,7.16318954730697)) ;
#72098 = CARTESIAN_POINT('Ctrl Pts',(75.0318577462829,233.741804969875,6.93380038570087)) ;
#72099 = CARTESIAN_POINT('Ctrl Pts',(74.9261707880323,233.858595877082,6.66079423640237)) ;
#72100 = CARTESIAN_POINT('Ctrl Pts',(74.8174451204396,233.928679077915,6.49259931810746)) ;
#72101 = CARTESIAN_POINT('Ctrl Pts',(74.7414693009496,233.962126737956,6.41145241095834)) ;
#72102 = CARTESIAN_POINT('Ctrl Pts',(74.6456929341906,233.99332587631,6.33519154784912)) ;
#72103 = CARTESIAN_POINT('Ctrl Pts',(74.5137737498694,234.006702012445,6.30217015984433)) ;
#72104 = CARTESIAN_POINT('Ctrl Pts',(74.3898972177444,233.985870163199,6.35347266041592)) ;
#72105 = CARTESIAN_POINT('Ctrl Pts',(74.3151471323012,233.961986344105,6.4118109039499)) ;
#72106 = CARTESIAN_POINT('Ctrl Pts',(74.2392567867269,233.928410119706,6.4932861327103)) ;
#72107 = CARTESIAN_POINT('Ctrl Pts',(74.1305331522724,233.858445916787,6.66117766958715)) ;
#72108 = CARTESIAN_POINT('Ctrl Pts',(74.0248674005834,233.741596368342,6.93433448515046)) ;
#72109 = CARTESIAN_POINT('Ctrl Pts',(73.9756279482132,233.63983142507,7.16318954730701)) ;
#72110 = CARTESIAN_POINT('Ctrl Pts',(73.9584121733007,233.5875,7.27867958884203)) ;
#72111 = CARTESIAN_POINT('Ctrl Pts',(75.1125069820977,233.544355503564,7.24979207607669)) ;
#72112 = CARTESIAN_POINT('Ctrl Pts',(75.0984818453212,233.600667724241,7.13558318832874)) ;
#72113 = CARTESIAN_POINT('Ctrl Pts',(75.0536389656137,233.711715621496,6.90837460070416)) ;
#72114 = CARTESIAN_POINT('Ctrl Pts',(74.9477942437258,233.841269933359,6.63742098993475)) ;
#72115 = CARTESIAN_POINT('Ctrl Pts',(74.8348016731915,233.919823032627,6.4703346030079)) ;
#72116 = CARTESIAN_POINT('Ctrl Pts',(74.7548728956437,233.957465240244,6.38969528531651)) ;
#72117 = CARTESIAN_POINT('Ctrl Pts',(74.6535180161129,233.992671246009,6.31389508883174)) ;
#72118 = CARTESIAN_POINT('Ctrl Pts',(74.5127829922739,234.007817842091,6.28106410226516)) ;
#72119 = CARTESIAN_POINT('Ctrl Pts',(74.3809498631099,233.984248460513,6.33206709849415)) ;
#72120 = CARTESIAN_POINT('Ctrl Pts',(74.3018363988415,233.957303882483,6.39005172782796)) ;
#72121 = CARTESIAN_POINT('Ctrl Pts',(74.2220102801505,233.919514179975,6.47101769533025)) ;
#72122 = CARTESIAN_POINT('Ctrl Pts',(74.1089767078142,233.841098288102,6.63780226952725)) ;
#72123 = CARTESIAN_POINT('Ctrl Pts',(74.0032101259291,233.711475333851,6.90890481997371)) ;
#72124 = CARTESIAN_POINT('Ctrl Pts',(73.9582438127981,233.600667724241,7.13558318832878)) ;
#72125 = CARTESIAN_POINT('Ctrl Pts',(73.9442186760216,233.544355503564,7.24979207607671)) ;
#72126 = CARTESIAN_POINT('Ctrl Pts',(75.1753446132139,233.481964767775,7.19960830183853)) ;
#72127 = CARTESIAN_POINT('Ctrl Pts',(75.1609398281288,233.546998459783,7.08747689596276)) ;
#72128 = CARTESIAN_POINT('Ctrl Pts',(75.1129255576136,233.675059882258,6.86386215376673)) ;
#72129 = CARTESIAN_POINT('Ctrl Pts',(74.9960174923802,233.823917230629,6.59636848724759)) ;
#72130 = CARTESIAN_POINT('Ctrl Pts',(74.8702771117857,233.913938281557,6.43117601138465)) ;
#72131 = CARTESIAN_POINT('Ctrl Pts',(74.7811442493929,233.957028829249,6.35140845594426)) ;
#72132 = CARTESIAN_POINT('Ctrl Pts',(74.668058857727,233.997300700229,6.27640270416242)) ;
#72133 = CARTESIAN_POINT('Ctrl Pts',(74.5109193901771,234.014610130897,6.24390214489264)) ;
#72134 = CARTESIAN_POINT('Ctrl Pts',(74.3636933974101,233.987669619988,6.29438675335505)) ;
#72135 = CARTESIAN_POINT('Ctrl Pts',(74.2754232494263,233.956845980595,6.35176194667064)) ;
#72136 = CARTESIAN_POINT('Ctrl Pts',(74.1863931543353,233.913587695583,6.43185336540903)) ;
#72137 = CARTESIAN_POINT('Ctrl Pts',(74.0606647370925,233.823722161856,6.59674624426879)) ;
#72138 = CARTESIAN_POINT('Ctrl Pts',(73.9437696527188,233.674789559215,6.86438794160944)) ;
#72139 = CARTESIAN_POINT('Ctrl Pts',(73.8957858299905,233.546998459783,7.0874768959628)) ;
#72140 = CARTESIAN_POINT('Ctrl Pts',(73.8813810449054,233.481964767775,7.19960830183855)) ;
#72141 = CARTESIAN_POINT('Ctrl Pts',(75.2709733099442,233.474489235504,7.17608503411327)) ;
#72142 = CARTESIAN_POINT('Ctrl Pts',(75.2501594453092,233.543687725245,7.06215944566083)) ;
#72143 = CARTESIAN_POINT('Ctrl Pts',(75.1885450487657,233.678786595009,6.83553863585668)) ;
#72144 = CARTESIAN_POINT('Ctrl Pts',(75.0519026388913,233.833908676329,6.56530442100143)) ;
#72145 = CARTESIAN_POINT('Ctrl Pts',(74.9095217874548,233.927105534872,6.39866319155849)) ;
#72146 = CARTESIAN_POINT('Ctrl Pts',(74.8095956592821,233.971604040945,6.31823878756062)) ;
#72147 = CARTESIAN_POINT('Ctrl Pts',(74.6833812504254,234.013122629692,6.24264060772189)) ;
#72148 = CARTESIAN_POINT('Ctrl Pts',(74.5090580770188,234.030929268947,6.20989713631634)) ;
#72149 = CARTESIAN_POINT('Ctrl Pts',(74.3454747092792,234.003199674091,6.26076425322068)) ;
#72150 = CARTESIAN_POINT('Ctrl Pts',(74.2469649068908,233.971416787748,6.31859436504268)) ;
#72151 = CARTESIAN_POINT('Ctrl Pts',(74.147151148607,233.926746883521,6.39934457097928)) ;
#72152 = CARTESIAN_POINT('Ctrl Pts',(74.0047808590601,233.833708884127,6.56568474185533)) ;
#72153 = CARTESIAN_POINT('Ctrl Pts',(73.8681563771895,233.678508252996,6.83606777892758)) ;
#72154 = CARTESIAN_POINT('Ctrl Pts',(73.8065662128101,233.543687725245,7.06215944566088)) ;
#72155 = CARTESIAN_POINT('Ctrl Pts',(73.7857523481751,233.474489235504,7.1760850341133)) ;
#72156 = CARTESIAN_POINT('Ctrl Pts',(75.3105185167129,233.48186240524,7.17267980084138)) ;
#72157 = CARTESIAN_POINT('Ctrl Pts',(75.2871694815419,233.551585478288,7.05718975930633)) ;
#72158 = CARTESIAN_POINT('Ctrl Pts',(75.2201184690921,233.687366037109,6.82780059770023)) ;
#72159 = CARTESIAN_POINT('Ctrl Pts',(75.0754350826972,233.842657781476,6.55479444840173)) ;
#72160 = CARTESIAN_POINT('Ctrl Pts',(74.9261342046016,233.935741266691,6.38659953010682)) ;
#72161 = CARTESIAN_POINT('Ctrl Pts',(74.821675936371,233.980144435879,6.3054526229577)) ;
#72162 = CARTESIAN_POINT('Ctrl Pts',(74.6899153511409,234.021548309364,6.22919175984848)) ;
#72163 = CARTESIAN_POINT('Ctrl Pts',(74.5082670156342,234.039291236966,6.1961703718437)) ;
#72164 = CARTESIAN_POINT('Ctrl Pts',(74.3377348599184,234.011655409264,6.24747287241529)) ;
#72165 = CARTESIAN_POINT('Ctrl Pts',(74.2348988344899,233.979958513117,6.30581111594926)) ;
#72166 = CARTESIAN_POINT('Ctrl Pts',(74.1305586930738,233.935385084639,6.38728634470966)) ;
#72167 = CARTESIAN_POINT('Ctrl Pts',(73.9812605807285,233.842459203332,6.55517788158652)) ;
#72168 = CARTESIAN_POINT('Ctrl Pts',(73.8366065041384,233.687089813394,6.82833469714983)) ;
#72169 = CARTESIAN_POINT('Ctrl Pts',(73.7695561765774,233.551585478287,7.05718975930638)) ;
#72170 = CARTESIAN_POINT('Ctrl Pts',(73.7462071414064,233.48186240524,7.1726798008414)) ;
#72171 = CARTESIAN_POINT('Ctrl Pts',(73.7462071414064,233.48186240524,7.17267980084137)) ;
#72172 = CARTESIAN_POINT('Ctrl Pts',(73.7695561765774,233.551585478287,7.05718975930636)) ;
#72173 = CARTESIAN_POINT('Ctrl Pts',(73.8366065041384,233.687089813395,6.82833469714981)) ;
#72174 = CARTESIAN_POINT('Ctrl Pts',(73.9812605807285,233.842459203331,6.55517788158652)) ;
#72175 = CARTESIAN_POINT('Ctrl Pts',(74.1305586930738,233.935385084639,6.38728634470966)) ;
#72176 = CARTESIAN_POINT('Ctrl Pts',(74.2348988344899,233.979958513118,6.30581111594926)) ;
#72177 = CARTESIAN_POINT('Ctrl Pts',(74.3377348599184,234.011655409263,6.24747287241529)) ;
#72178 = CARTESIAN_POINT('Ctrl Pts',(74.5082670156342,234.039291236967,6.1961703718437)) ;
#72179 = CARTESIAN_POINT('Ctrl Pts',(74.689915351141,234.021548309363,6.22919175984849)) ;
#72180 = CARTESIAN_POINT('Ctrl Pts',(74.821675936371,233.98014443588,6.3054526229577)) ;
#72181 = CARTESIAN_POINT('Ctrl Pts',(74.9261342046016,233.93574126669,6.38659953010682)) ;
#72182 = CARTESIAN_POINT('Ctrl Pts',(75.0754350826972,233.842657781477,6.55479444840175)) ;
#72183 = CARTESIAN_POINT('Ctrl Pts',(75.220118469092,233.687366037109,6.82780059770018)) ;
#72184 = CARTESIAN_POINT('Ctrl Pts',(75.2871694815419,233.551585478288,7.05718975930624)) ;
#72185 = CARTESIAN_POINT('Ctrl Pts',(75.3105185167129,233.48186240524,7.17267980084124)) ;
#72186 = CARTESIAN_POINT('Ctrl Pts',(75.0983134848186,233.5875,7.27867958884202)) ;
#72187 = CARTESIAN_POINT('Ctrl Pts',(75.0810977099062,233.63983142507,7.16318954730697)) ;
#72188 = CARTESIAN_POINT('Ctrl Pts',(75.0318577462829,233.741804969875,6.93380038570087)) ;
#72189 = CARTESIAN_POINT('Ctrl Pts',(74.9261707880323,233.858595877082,6.66079423640237)) ;
#72190 = CARTESIAN_POINT('Ctrl Pts',(74.8174451204396,233.928679077915,6.49259931810746)) ;
#72191 = CARTESIAN_POINT('Ctrl Pts',(74.7414693009496,233.962126737956,6.41145241095834)) ;
#72192 = CARTESIAN_POINT('Ctrl Pts',(74.6456929341906,233.99332587631,6.33519154784912)) ;
#72193 = CARTESIAN_POINT('Ctrl Pts',(74.5137737498694,234.006702012445,6.30217015984433)) ;
#72194 = CARTESIAN_POINT('Ctrl Pts',(74.3898972177444,233.985870163199,6.35347266041592)) ;
#72195 = CARTESIAN_POINT('Ctrl Pts',(74.3151471323012,233.961986344105,6.4118109039499)) ;
#72196 = CARTESIAN_POINT('Ctrl Pts',(74.2392567867269,233.928410119706,6.4932861327103)) ;
#72197 = CARTESIAN_POINT('Ctrl Pts',(74.1305331522724,233.858445916787,6.66117766958715)) ;
#72198 = CARTESIAN_POINT('Ctrl Pts',(74.0248674005834,233.741596368342,6.93433448515046)) ;
#72199 = CARTESIAN_POINT('Ctrl Pts',(73.9756279482132,233.63983142507,7.16318954730701)) ;
#72200 = CARTESIAN_POINT('Ctrl Pts',(73.9584121733007,233.5875,7.27867958884203)) ;
#72201 = CARTESIAN_POINT('Origin',(77.2933283411226,234.301474162358,7.2786795888419)) ;
#72202 = CARTESIAN_POINT('',(77.4837648415456,234.362580130206,7.27867958883759)) ;
#72203 = CARTESIAN_POINT('Origin',(77.2933283411226,234.301474162358,7.2786795888419)) ;
#72204 = CARTESIAN_POINT('',(77.3741795847386,234.152386532591,7.17267980084137)) ;
#72205 = CARTESIAN_POINT('Origin',(77.2933283411226,234.301474162358,7.2786795888419)) ;
#72206 = CARTESIAN_POINT('Origin',(77.2933283411219,234.30147416236,7.27867958883799)) ;
#72207 = CARTESIAN_POINT('Origin',(75.5824701665474,233.696592446523,7.2786795888419)) ;
#72208 = CARTESIAN_POINT('',(75.7824688237379,233.69585956045,7.27867958883755)) ;
#72209 = CARTESIAN_POINT('Origin',(75.5824701665474,233.696592446523,7.2786795888419)) ;
#72210 = CARTESIAN_POINT('',(75.6132936573898,233.529817276441,7.17267980084132)) ;
#72211 = CARTESIAN_POINT('Origin',(75.5824701665474,233.696592446523,7.2786795888419)) ;
#72212 = CARTESIAN_POINT('Origin',(75.5824701665474,233.696592446526,7.27867958883797)) ;
#72213 = CARTESIAN_POINT('Origin',(74.5283628290597,239.4,7.2786795888419)) ;
#72214 = CARTESIAN_POINT('Origin',(74.5283628290597,239.4,7.17267980084126)) ;
#72215 = CARTESIAN_POINT('Origin',(77.027950926884,234.166257616082,7.27867958884205)) ;
#72216 = CARTESIAN_POINT('',(76.8665793939892,234.04810843762,7.278679588838)) ;
#72217 = CARTESIAN_POINT('Origin',(77.0279509268839,234.166257616082,7.27867958883759)) ;
#72218 = CARTESIAN_POINT('',(77.1010421843897,234.013216075904,7.17267980084126)) ;
#72219 = CARTESIAN_POINT('Origin',(77.027950926884,234.166257616082,7.27867958884205)) ;
#72220 = CARTESIAN_POINT('Origin',(77.0279509268839,234.166257616082,7.2786795888419)) ;
#72221 = CARTESIAN_POINT('Ctrl Pts',(76.8665793939903,234.048108437619,7.27867958884205)) ;
#72222 = CARTESIAN_POINT('Ctrl Pts',(76.8340341124953,234.0925597155,7.16318668389241)) ;
#72223 = CARTESIAN_POINT('Ctrl Pts',(76.7556911392885,234.174326892791,6.93379514728806)) ;
#72224 = CARTESIAN_POINT('Ctrl Pts',(76.6190866745073,234.252741595594,6.66079114111062)) ;
#72225 = CARTESIAN_POINT('Ctrl Pts',(76.4940251112423,234.285796227647,6.49259672460371)) ;
#72226 = CARTESIAN_POINT('Ctrl Pts',(76.4114318303287,234.2941286283,6.41145063262659)) ;
#72227 = CARTESIAN_POINT('Ctrl Pts',(76.3107018814125,234.294203813326,6.33519065213031)) ;
#72228 = CARTESIAN_POINT('Ctrl Pts',(76.1811060983148,234.266159399846,6.30217089588981)) ;
#72229 = CARTESIAN_POINT('Ctrl Pts',(76.0697307124536,234.208067009127,6.35347440234159)) ;
#72230 = CARTESIAN_POINT('Ctrl Pts',(76.0060201171914,234.162253139921,6.4118128891193)) ;
#72231 = CARTESIAN_POINT('Ctrl Pts',(75.9442201811444,234.106868936771,6.4932882288145)) ;
#72232 = CARTESIAN_POINT('Ctrl Pts',(75.8624384710468,234.006731853917,6.66117946366231)) ;
#72233 = CARTESIAN_POINT('Ctrl Pts',(75.7980532024828,233.862949209186,6.93433560993259)) ;
#72234 = CARTESIAN_POINT('Ctrl Pts',(75.7826706984499,233.750949529794,7.16318984183889)) ;
#72235 = CARTESIAN_POINT('Ctrl Pts',(75.7824688237379,233.69585956045,7.27867958884195)) ;
#72236 = CARTESIAN_POINT('Ctrl Pts',(76.8934105946792,234.01146161501,7.24979207607672)) ;
#72237 = CARTESIAN_POINT('Ctrl Pts',(76.8626697016171,234.060684934213,7.1355803566786)) ;
#72238 = CARTESIAN_POINT('Ctrl Pts',(76.7857043976302,234.152441111515,6.90836936466691)) ;
#72239 = CARTESIAN_POINT('Ctrl Pts',(76.6450057114788,234.242945622551,6.63741785480387)) ;
#72240 = CARTESIAN_POINT('Ctrl Pts',(76.5132686922221,234.282736999639,6.47033195643384)) ;
#72241 = CARTESIAN_POINT('Ctrl Pts',(76.4256197164491,234.29383707081,6.38969344711358)) ;
#72242 = CARTESIAN_POINT('Ctrl Pts',(76.3183460791628,234.295999096524,6.31389412481953)) ;
#72243 = CARTESIAN_POINT('Ctrl Pts',(76.1798188650716,234.266914151536,6.28106475682608)) ;
#72244 = CARTESIAN_POINT('Ctrl Pts',(76.0617223233092,234.203759460484,6.33206875395753)) ;
#72245 = CARTESIAN_POINT('Ctrl Pts',(75.9948077770194,234.153686282076,6.39005362566642)) ;
#72246 = CARTESIAN_POINT('Ctrl Pts',(75.9305667724029,234.093078609259,6.47101970243042)) ;
#72247 = CARTESIAN_POINT('Ctrl Pts',(75.8472978214838,233.983571719713,6.63780398898495)) ;
#72248 = CARTESIAN_POINT('Ctrl Pts',(75.7867638696866,233.827609742269,6.90890587698616)) ;
#72249 = CARTESIAN_POINT('Ctrl Pts',(75.7782396631783,233.708330636501,7.13558347959336)) ;
#72250 = CARTESIAN_POINT('Ctrl Pts',(75.782302388274,233.650440674103,7.24979207607662)) ;
#72251 = CARTESIAN_POINT('Ctrl Pts',(76.9724525410908,233.971542437522,7.19960831977766)) ;
#72252 = CARTESIAN_POINT('Ctrl Pts',(76.9386554224005,234.028943253832,7.08747413375999)) ;
#72253 = CARTESIAN_POINT('Ctrl Pts',(76.8534162817674,234.135900487607,6.86385705380188)) ;
#72254 = CARTESIAN_POINT('Ctrl Pts',(76.6962307517854,234.241344408245,6.59636547374966)) ;
#72255 = CARTESIAN_POINT('Ctrl Pts',(76.54882599141,234.288103136327,6.43117348883828)) ;
#72256 = CARTESIAN_POINT('Ctrl Pts',(76.4507397668635,234.301540606073,6.35140673253532)) ;
#72257 = CARTESIAN_POINT('Ctrl Pts',(76.3307442874739,234.30489556795,6.27640184858989)) ;
#72258 = CARTESIAN_POINT('Ctrl Pts',(76.1759471961323,234.272798261829,6.24390289678572)) ;
#72259 = CARTESIAN_POINT('Ctrl Pts',(76.0442530152415,234.201680740727,6.29438849455214)) ;
#72260 = CARTESIAN_POINT('Ctrl Pts',(75.9698286986536,234.145088782522,6.35176392641701)) ;
#72261 = CARTESIAN_POINT('Ctrl Pts',(75.8985241358216,234.076436004797,6.43185545307777)) ;
#72262 = CARTESIAN_POINT('Ctrl Pts',(75.8067198650261,233.952116925724,6.59674803075384)) ;
#72263 = CARTESIAN_POINT('Ctrl Pts',(75.7415691250071,233.774351527382,6.86438906719111)) ;
#72264 = CARTESIAN_POINT('Ctrl Pts',(75.7354232791666,233.637987561567,7.08747719986831)) ;
#72265 = CARTESIAN_POINT('Ctrl Pts',(75.7418200141697,233.5716856907,7.19960831977756)) ;
#72266 = CARTESIAN_POINT('Ctrl Pts',(77.0657108925551,233.993983633843,7.17608503411331)) ;
#72267 = CARTESIAN_POINT('Ctrl Pts',(77.0245312006817,234.053364942779,7.0621566210347)) ;
#72268 = CARTESIAN_POINT('Ctrl Pts',(76.9241827243705,234.16281243188,6.83553342683033)) ;
#72269 = CARTESIAN_POINT('Ctrl Pts',(76.746292915967,234.2681161407,6.56530131356024)) ;
#72270 = CARTESIAN_POINT('Ctrl Pts',(76.582080718942,234.312753012577,6.39866057413136)) ;
#72271 = CARTESIAN_POINT('Ctrl Pts',(76.473294405035,234.32419420694,6.31823697659248)) ;
#72272 = CARTESIAN_POINT('Ctrl Pts',(76.3404272191003,234.32467775301,6.24263966949842)) ;
#72273 = CARTESIAN_POINT('Ctrl Pts',(76.1691338319105,234.287743240048,6.20989781362796)) ;
#72274 = CARTESIAN_POINT('Ctrl Pts',(76.0221267858857,234.21082056027,6.26076592844773)) ;
#72275 = CARTESIAN_POINT('Ctrl Pts',(75.9382604527896,234.150152089044,6.31859628173874)) ;
#72276 = CARTESIAN_POINT('Ctrl Pts',(75.8571362822314,234.076824457925,6.39934659681402)) ;
#72277 = CARTESIAN_POINT('Ctrl Pts',(75.7504850514437,233.944345605192,6.56568647657609)) ;
#72278 = CARTESIAN_POINT('Ctrl Pts',(75.6685075209583,233.754522270794,6.83606885194659)) ;
#72279 = CARTESIAN_POINT('Ctrl Pts',(75.6515934750524,233.607268444491,7.06215973620294)) ;
#72280 = CARTESIAN_POINT('Ctrl Pts',(75.6531818187263,233.535025116255,7.1760850341132)) ;
#72281 = CARTESIAN_POINT('Ctrl Pts',(77.1010421843897,234.013216075904,7.17267980084142)) ;
#72282 = CARTESIAN_POINT('Ctrl Pts',(77.0572892331029,234.072312875378,7.05718689589178)) ;
#72283 = CARTESIAN_POINT('Ctrl Pts',(76.9515594887745,234.180728684329,6.82779535928743)) ;
#72284 = CARTESIAN_POINT('Ctrl Pts',(76.765969850139,234.283708967173,6.55479135310999)) ;
#72285 = CARTESIAN_POINT('Ctrl Pts',(76.5952113296033,234.326099607554,6.38659693660311)) ;
#72286 = CARTESIAN_POINT('Ctrl Pts',(76.4821441508519,234.336049621713,6.30545084462598)) ;
#72287 = CARTESIAN_POINT('Ctrl Pts',(76.3440376762746,234.334710204215,6.22919086412971)) ;
#72288 = CARTESIAN_POINT('Ctrl Pts',(76.1657973375852,234.295451506702,6.19617110788921)) ;
#72289 = CARTESIAN_POINT('Ctrl Pts',(76.012152659647,234.216470723001,6.247474614341)) ;
#72290 = CARTESIAN_POINT('Ctrl Pts',(75.9241452928115,234.154547163083,6.3058131011187)) ;
#72291 = CARTESIAN_POINT('Ctrl Pts',(75.8386864850542,234.079912563388,6.38728844081392)) ;
#72292 = CARTESIAN_POINT('Ctrl Pts',(75.7254118872703,233.945399523016,6.55517967566167)) ;
#72293 = CARTESIAN_POINT('Ctrl Pts',(75.6358499337627,233.752934411719,6.82833582193194)) ;
#72294 = CARTESIAN_POINT('Ctrl Pts',(75.6139542932819,233.603342920557,7.05719005383824)) ;
#72295 = CARTESIAN_POINT('Ctrl Pts',(75.6132936573898,233.529817276441,7.17267980084131)) ;
#72296 = CARTESIAN_POINT('Ctrl Pts',(75.6132936573898,233.529817276441,7.17267980084131)) ;
#72297 = CARTESIAN_POINT('Ctrl Pts',(75.6136811483567,233.572943184788,7.10494016653924)) ;
#72298 = CARTESIAN_POINT('Ctrl Pts',(75.6176122445359,233.616573569928,7.03746115712619)) ;
#72299 = CARTESIAN_POINT('Ctrl Pts',(75.6255308442543,233.660599858183,6.97066813692428)) ;
#72300 = CARTESIAN_POINT('Ctrl Pts',(75.6289443535501,233.679578484399,6.94187534483236)) ;
#72301 = CARTESIAN_POINT('Ctrl Pts',(75.6330982419626,233.698630602532,6.91320997325321)) ;
#72302 = CARTESIAN_POINT('Ctrl Pts',(75.6380250264329,233.717747190309,6.88470563298376)) ;
#72303 = CARTESIAN_POINT('Ctrl Pts',(75.6411351900574,233.729815044361,6.86671151069543)) ;
#72304 = CARTESIAN_POINT('Ctrl Pts',(75.6445532067144,233.741908437271,6.84878174976668)) ;
#72305 = CARTESIAN_POINT('Ctrl Pts',(75.648288414344,233.754029561188,6.83091815065467)) ;
#72306 = CARTESIAN_POINT('Ctrl Pts',(75.6716820890904,233.829944385364,6.7190380976912)) ;
#72307 = CARTESIAN_POINT('Ctrl Pts',(75.7075083786311,233.906918899165,6.6097947220493)) ;
#72308 = CARTESIAN_POINT('Ctrl Pts',(75.762593318097,233.983811578595,6.50943151975669)) ;
#72309 = CARTESIAN_POINT('Ctrl Pts',(75.7856514095903,234.015998206277,6.46742032897639)) ;
#72310 = CARTESIAN_POINT('Ctrl Pts',(75.8120819738222,234.048166034233,6.42697146264465)) ;
#72311 = CARTESIAN_POINT('Ctrl Pts',(75.8431042190517,234.079888023935,6.38961057401096)) ;
#72312 = CARTESIAN_POINT('Ctrl Pts',(75.8491515604238,234.086071770446,6.3823276051007)) ;
#72313 = CARTESIAN_POINT('Ctrl Pts',(75.8553733890211,234.092238603552,6.37516193216405)) ;
#72314 = CARTESIAN_POINT('Ctrl Pts',(75.8617787258407,234.098385380411,6.36812481495593)) ;
#72315 = CARTESIAN_POINT('Ctrl Pts',(75.8814155988188,234.117229584832,6.34655108969537)) ;
#72316 = CARTESIAN_POINT('Ctrl Pts',(75.9027719322721,234.135881745757,6.32618883113316)) ;
#72317 = CARTESIAN_POINT('Ctrl Pts',(75.9260354228183,234.154064060967,6.30766344904101)) ;
#72318 = CARTESIAN_POINT('Ctrl Pts',(75.9493016230525,234.172248494018,6.28913590914689)) ;
#72319 = CARTESIAN_POINT('Ctrl Pts',(75.974468907875,234.18995289281,6.27245946560264)) ;
#72320 = CARTESIAN_POINT('Ctrl Pts',(76.0018137681245,234.206865984575,6.25837165899619)) ;
#72321 = CARTESIAN_POINT('Ctrl Pts',(76.0128320016159,234.213680881139,6.25269517203829)) ;
#72322 = CARTESIAN_POINT('Ctrl Pts',(76.0242032579975,234.22036742268,6.24743847065808)) ;
#72323 = CARTESIAN_POINT('Ctrl Pts',(76.0358779409522,234.226870878186,6.24267244279208)) ;
#72324 = CARTESIAN_POINT('Ctrl Pts',(76.0420504804806,234.23030933012,6.24015258889024)) ;
#72325 = CARTESIAN_POINT('Ctrl Pts',(76.0483078300303,234.233696619766,6.23776986110493)) ;
#72326 = CARTESIAN_POINT('Ctrl Pts',(76.0546426194486,234.237024792671,6.23553447411149)) ;
#72327 = CARTESIAN_POINT('Ctrl Pts',(76.0656791909796,234.242823188782,6.23163994710773)) ;
#72328 = CARTESIAN_POINT('Ctrl Pts',(76.0769749732387,234.248455064872,6.22818372039071)) ;
#72329 = CARTESIAN_POINT('Ctrl Pts',(76.0885070092412,234.253881919748,6.22522266061593)) ;
#72330 = CARTESIAN_POINT('Ctrl Pts',(76.1023829873427,234.260411809128,6.22165975111902)) ;
#72331 = CARTESIAN_POINT('Ctrl Pts',(76.116598572473,234.266643535812,6.21881469107473)) ;
#72332 = CARTESIAN_POINT('Ctrl Pts',(76.1310985238889,234.272500575675,6.21679454309188)) ;
#72333 = CARTESIAN_POINT('Ctrl Pts',(76.1333376264178,234.273405027862,6.21648258904959)) ;
#72334 = CARTESIAN_POINT('Ctrl Pts',(76.1355833747657,234.274300487348,6.21619033071521)) ;
#72335 = CARTESIAN_POINT('Ctrl Pts',(76.1378354138322,234.275186615266,6.21591817623244)) ;
#72336 = CARTESIAN_POINT('Ctrl Pts',(76.1559817557798,234.282326802329,6.21372522657167)) ;
#72337 = CARTESIAN_POINT('Ctrl Pts',(76.1745322866635,234.288857900258,6.21284080371351)) ;
#72338 = CARTESIAN_POINT('Ctrl Pts',(76.1932444556825,234.294748660884,6.21317766952897)) ;
#72339 = CARTESIAN_POINT('Ctrl Pts',(76.2103563728474,234.300135647704,6.21348572681106)) ;
#72340 = CARTESIAN_POINT('Ctrl Pts',(76.2276075834206,234.304989663888,6.2148130177342)) ;
#72341 = CARTESIAN_POINT('Ctrl Pts',(76.2448554373945,234.309306022186,6.21708354113517)) ;
#72342 = CARTESIAN_POINT('Ctrl Pts',(76.2651911446345,234.314395130595,6.21976055238733)) ;
#72343 = CARTESIAN_POINT('Ctrl Pts',(76.2855276520082,234.318739484644,6.22374748057868)) ;
#72344 = CARTESIAN_POINT('Ctrl Pts',(76.3056568399921,234.32228904216,6.22899842713304)) ;
#72345 = CARTESIAN_POINT('Ctrl Pts',(76.3127180447779,234.323534206771,6.23084042935237)) ;
#72346 = CARTESIAN_POINT('Ctrl Pts',(76.3197533595581,234.324681337781,6.23283813295313)) ;
#72347 = CARTESIAN_POINT('Ctrl Pts',(76.3267525396858,234.32572754817,6.23499001125318)) ;
#72348 = CARTESIAN_POINT('Ctrl Pts',(76.3476867356452,234.328856710857,6.24142617108782)) ;
#72349 = CARTESIAN_POINT('Ctrl Pts',(76.3683683305024,234.331213157323,6.2490806240269)) ;
#72350 = CARTESIAN_POINT('Ctrl Pts',(76.3885333174352,234.332751329204,6.2578735309604)) ;
#72351 = CARTESIAN_POINT('Ctrl Pts',(76.4129027393853,234.334610212611,6.2684997743566)) ;
#72352 = CARTESIAN_POINT('Ctrl Pts',(76.436517835923,234.335273938245,6.28078953588881)) ;
#72353 = CARTESIAN_POINT('Ctrl Pts',(76.4594145442388,234.335023230649,6.29423529210409)) ;
#72354 = CARTESIAN_POINT('Ctrl Pts',(76.4666253803013,234.334944275571,6.29846974984659)) ;
#72355 = CARTESIAN_POINT('Ctrl Pts',(76.4737646201994,234.334774589698,6.3028186680162)) ;
#72356 = CARTESIAN_POINT('Ctrl Pts',(76.4808324691104,234.334522804414,6.30726572519078)) ;
#72357 = CARTESIAN_POINT('Ctrl Pts',(76.4928214739417,234.334095707707,6.3148091504426)) ;
#72358 = CARTESIAN_POINT('Ctrl Pts',(76.5046052294152,234.333432418532,6.32263503033504)) ;
#72359 = CARTESIAN_POINT('Ctrl Pts',(76.5161630752768,234.332536734824,6.33072042872202)) ;
#72360 = CARTESIAN_POINT('Ctrl Pts',(76.533062389186,234.331227110148,6.34254250067724)) ;
#72361 = CARTESIAN_POINT('Ctrl Pts',(76.5495258068277,234.3294578278,6.35489082553211)) ;
#72362 = CARTESIAN_POINT('Ctrl Pts',(76.5655363846225,234.327271369833,6.36767686175465)) ;
#72363 = CARTESIAN_POINT('Ctrl Pts',(76.6168616972201,234.320262213757,6.40866522047711)) ;
#72364 = CARTESIAN_POINT('Ctrl Pts',(76.6635341884214,234.308965735347,6.45415276711694)) ;
#72365 = CARTESIAN_POINT('Ctrl Pts',(76.706630938113,234.295047867349,6.501706150284)) ;
#72366 = CARTESIAN_POINT('Ctrl Pts',(76.7088245661434,234.294339446747,6.5041266213173)) ;
#72367 = CARTESIAN_POINT('Ctrl Pts',(76.7110089459639,234.293624119443,6.50655262448272)) ;
#72368 = CARTESIAN_POINT('Ctrl Pts',(76.7131842181064,234.292902105009,6.50898383770951)) ;
#72369 = CARTESIAN_POINT('Ctrl Pts',(76.7627696395436,234.276443755138,6.56440344709885)) ;
#72370 = CARTESIAN_POINT('Ctrl Pts',(76.8076178592959,234.25650836791,6.62253062439344)) ;
#72371 = CARTESIAN_POINT('Ctrl Pts',(76.8485317332352,234.233925379128,6.68231570506646)) ;
#72372 = CARTESIAN_POINT('Ctrl Pts',(76.8817296004144,234.215601348918,6.73082583076176)) ;
#72373 = CARTESIAN_POINT('Ctrl Pts',(76.91233859002,234.195535005202,6.78042711783452)) ;
#72374 = CARTESIAN_POINT('Ctrl Pts',(76.9408102796966,234.174179291345,6.83056026478223)) ;
#72375 = CARTESIAN_POINT('Ctrl Pts',(76.9478474826703,234.168900907984,6.84295142016449)) ;
#72376 = CARTESIAN_POINT('Ctrl Pts',(76.9547541967589,234.163543783773,6.85537508796248)) ;
#72377 = CARTESIAN_POINT('Ctrl Pts',(76.9615329145985,234.15811048499,6.86782833575028)) ;
#72378 = CARTESIAN_POINT('Ctrl Pts',(77.0061519430116,234.122347304027,6.94979838230172)) ;
#72379 = CARTESIAN_POINT('Ctrl Pts',(77.0452003554324,234.083189875681,7.03316975346642)) ;
#72380 = CARTESIAN_POINT('Ctrl Pts',(77.0792533061722,234.041297979296,7.11711563024325)) ;
#72381 = CARTESIAN_POINT('Ctrl Pts',(77.0867564620173,234.032067606585,7.13561208891489)) ;
#72382 = CARTESIAN_POINT('Ctrl Pts',(77.0940172741218,234.022704572136,7.15413642788044)) ;
#72383 = CARTESIAN_POINT('Ctrl Pts',(77.1010421843897,234.013216075904,7.17267980084131)) ;
#72384 = CARTESIAN_POINT('Ctrl Pts',(76.8665793939903,234.048108437619,7.27867958884205)) ;
#72385 = CARTESIAN_POINT('Ctrl Pts',(76.8340341124953,234.0925597155,7.16318668389241)) ;
#72386 = CARTESIAN_POINT('Ctrl Pts',(76.7556911392885,234.174326892791,6.93379514728806)) ;
#72387 = CARTESIAN_POINT('Ctrl Pts',(76.6190866745073,234.252741595594,6.66079114111062)) ;
#72388 = CARTESIAN_POINT('Ctrl Pts',(76.4940251112423,234.285796227647,6.49259672460371)) ;
#72389 = CARTESIAN_POINT('Ctrl Pts',(76.4114318303287,234.2941286283,6.41145063262659)) ;
#72390 = CARTESIAN_POINT('Ctrl Pts',(76.3107018814125,234.294203813326,6.33519065213031)) ;
#72391 = CARTESIAN_POINT('Ctrl Pts',(76.1811060983148,234.266159399846,6.30217089588981)) ;
#72392 = CARTESIAN_POINT('Ctrl Pts',(76.0697307124536,234.208067009127,6.35347440234159)) ;
#72393 = CARTESIAN_POINT('Ctrl Pts',(76.0060201171914,234.162253139921,6.4118128891193)) ;
#72394 = CARTESIAN_POINT('Ctrl Pts',(75.9442201811444,234.106868936771,6.4932882288145)) ;
#72395 = CARTESIAN_POINT('Ctrl Pts',(75.8624384710468,234.006731853917,6.66117946366231)) ;
#72396 = CARTESIAN_POINT('Ctrl Pts',(75.7980532024828,233.862949209186,6.93433560993259)) ;
#72397 = CARTESIAN_POINT('Ctrl Pts',(75.7826706984499,233.750949529794,7.16318984183889)) ;
#72398 = CARTESIAN_POINT('Ctrl Pts',(75.7824688237379,233.69585956045,7.27867958884195)) ;
#72399 = CARTESIAN_POINT('Origin',(74.5283628290597,239.4,7.2786795888419)) ;
#72400 = CARTESIAN_POINT('Origin',(74.5283628290597,239.4,7.17267980084126)) ;
#72401 = CARTESIAN_POINT('Origin',(77.0279509268839,234.166257616082,16.0213203435596)) ;
#72402 = CARTESIAN_POINT('',(76.8665793939903,234.048108437619,16.0254384350469)) ;
#72403 = CARTESIAN_POINT('',(76.8665793939903,234.048108437619,16.0213203435596)) ;
#72404 = CARTESIAN_POINT('Ctrl Pts',(77.1141436199122,233.985783740775,16.2213203435596)) ;
#72405 = CARTESIAN_POINT('Ctrl Pts',(77.1135321137219,233.985491690941,16.2206540664685)) ;
#72406 = CARTESIAN_POINT('Ctrl Pts',(77.1129191197593,233.985202747452,16.2199877856837)) ;
#72407 = CARTESIAN_POINT('Ctrl Pts',(77.0934911866169,233.976165511075,16.1989219658753)) ;
#72408 = CARTESIAN_POINT('Ctrl Pts',(77.0732014734155,233.970288661947,16.1784289743533)) ;
#72409 = CARTESIAN_POINT('Ctrl Pts',(77.0319798567454,233.965272578478,16.1396302535167)) ;
#72410 = CARTESIAN_POINT('Ctrl Pts',(77.0108918072688,233.965813478537,16.1210537744675)) ;
#72411 = CARTESIAN_POINT('Ctrl Pts',(76.9671930590858,233.974342228868,16.0855257633)) ;
#72412 = CARTESIAN_POINT('Ctrl Pts',(76.944270848093,233.982813988936,16.068487609488)) ;
#72413 = CARTESIAN_POINT('Ctrl Pts',(76.9062880703046,234.006370689004,16.0440628922443)) ;
#72414 = CARTESIAN_POINT('Ctrl Pts',(76.8907647861873,234.019226794601,16.0353723462237)) ;
#72415 = CARTESIAN_POINT('Ctrl Pts',(76.8733833952847,234.039215229877,16.0279192770514)) ;
#72416 = CARTESIAN_POINT('Ctrl Pts',(76.8698946334441,234.043580388592,16.0265673132456)) ;
#72417 = CARTESIAN_POINT('Ctrl Pts',(76.8665793939901,234.048108437619,16.0254384350468)) ;
#72418 = CARTESIAN_POINT('Origin',(75.5824701665474,233.696592446523,16.0213203435596)) ;
#72419 = CARTESIAN_POINT('',(75.7824688237379,233.69585956045,16.0254384350469)) ;
#72420 = CARTESIAN_POINT('',(75.7824688237379,233.69585956045,16.0213203435596)) ;
#72421 = CARTESIAN_POINT('Ctrl Pts',(75.7824688237379,233.69585956045,16.0254384350469)) ;
#72422 = CARTESIAN_POINT('Ctrl Pts',(75.7823954804048,233.675844760517,16.0294645582753)) ;
#72423 = CARTESIAN_POINT('Ctrl Pts',(75.7793263768937,233.656704801068,16.0362204083692)) ;
#72424 = CARTESIAN_POINT('Ctrl Pts',(75.7670900599968,233.616042723181,16.056050217191)) ;
#72425 = CARTESIAN_POINT('Ctrl Pts',(75.7565172414146,233.595758150279,16.070223718736)) ;
#72426 = CARTESIAN_POINT('Ctrl Pts',(75.7284792865434,233.557458099226,16.1046945816758)) ;
#72427 = CARTESIAN_POINT('Ctrl Pts',(75.7098594549003,233.540583950888,16.1258672215767)) ;
#72428 = CARTESIAN_POINT('Ctrl Pts',(75.6683571515081,233.514199267903,16.1708720249642)) ;
#72429 = CARTESIAN_POINT('Ctrl Pts',(75.6449193023295,233.505011527087,16.1951765216887)) ;
#72430 = CARTESIAN_POINT('Ctrl Pts',(75.6201508361424,233.500172930197,16.2199877856672)) ;
#72431 = CARTESIAN_POINT('Ctrl Pts',(75.6194850768967,233.50004638158,16.2206540664837)) ;
#72432 = CARTESIAN_POINT('Ctrl Pts',(75.6188186954263,233.499923220541,16.2213203435596)) ;
#72433 = CARTESIAN_POINT('Ctrl Pts',(78.4059643744832,235.032597310178,7.27867958886636)) ;
#72434 = CARTESIAN_POINT('Ctrl Pts',(78.3389185036295,235.080934607739,7.10540671867987)) ;
#72435 = CARTESIAN_POINT('Ctrl Pts',(78.234821145,235.130175045901,6.8757228796813)) ;
#72436 = CARTESIAN_POINT('Ctrl Pts',(78.0706643466897,235.148929220103,6.61251961592784)) ;
#72437 = CARTESIAN_POINT('Ctrl Pts',(77.9784150954104,235.143436282111,6.49309971889691)) ;
#72438 = CARTESIAN_POINT('Ctrl Pts',(77.8972265351195,235.126146469199,6.41122237377758)) ;
#72439 = CARTESIAN_POINT('Ctrl Pts',(77.8334871500539,235.1048001745,6.36192442727363)) ;
#72440 = CARTESIAN_POINT('Ctrl Pts',(77.7217018252731,235.053842764399,6.30168464935698)) ;
#72441 = CARTESIAN_POINT('Ctrl Pts',(77.5980687835801,234.948679457524,6.33246526297836)) ;
#72442 = CARTESIAN_POINT('Ctrl Pts',(77.5181116348167,234.821023036642,6.4698168706527)) ;
#72443 = CARTESIAN_POINT('Ctrl Pts',(77.4637464544563,234.683353081259,6.66032498688208)) ;
#72444 = CARTESIAN_POINT('Ctrl Pts',(77.447328463511,234.526604137613,6.93427994562925)) ;
#72445 = CARTESIAN_POINT('Ctrl Pts',(77.4669324115197,234.415038329963,7.1631851243399)) ;
#72446 = CARTESIAN_POINT('Ctrl Pts',(77.4837648415456,234.362580130206,7.27867958884201)) ;
#72447 = CARTESIAN_POINT('Ctrl Pts',(78.4428068537144,235.006035407726,7.24979207610077)) ;
#72448 = CARTESIAN_POINT('Ctrl Pts',(78.3761232031844,235.062018285548,7.07844135600527)) ;
#72449 = CARTESIAN_POINT('Ctrl Pts',(78.2690741390837,235.121066834892,6.85076492565332)) ;
#72450 = CARTESIAN_POINT('Ctrl Pts',(78.095885173777,235.14883561158,6.58946758288809)) ;
#72451 = CARTESIAN_POINT('Ctrl Pts',(77.9976154072437,235.146398293685,6.47083493132605)) ;
#72452 = CARTESIAN_POINT('Ctrl Pts',(77.9107531594458,235.130222234622,6.38946905227889)) ;
#72453 = CARTESIAN_POINT('Ctrl Pts',(77.8424673215011,235.108766275007,6.34047046809846)) ;
#72454 = CARTESIAN_POINT('Ctrl Pts',(77.722636167835,235.05593023867,6.28058364221613)) ;
#72455 = CARTESIAN_POINT('Ctrl Pts',(77.5911482552061,234.943002197512,6.31119003477298)) ;
#72456 = CARTESIAN_POINT('Ctrl Pts',(77.5091860379167,234.804995268577,6.44770636852286)) ;
#72457 = CARTESIAN_POINT('Ctrl Pts',(77.4564431115047,234.656661721284,6.63695559928427)) ;
#72458 = CARTESIAN_POINT('Ctrl Pts',(77.4475171063426,234.48950940537,6.90885232947085)) ;
#72459 = CARTESIAN_POINT('Ctrl Pts',(77.4758880078429,234.373136143523,7.13557881442652)) ;
#72460 = CARTESIAN_POINT('Ctrl Pts',(77.4976417597599,234.319332770996,7.24979207607669)) ;
#72461 = CARTESIAN_POINT('Ctrl Pts',(78.5303159124148,234.992495366521,7.19960833957127)) ;
#72462 = CARTESIAN_POINT('Ctrl Pts',(78.4554802418853,235.058729481418,7.0313745223877)) ;
#72463 = CARTESIAN_POINT('Ctrl Pts',(78.3352528450103,235.129028614954,6.80703932187651)) ;
#72464 = CARTESIAN_POINT('Ctrl Pts',(78.1403320618317,235.163740445657,6.54896323857508)) ;
#72465 = CARTESIAN_POINT('Ctrl Pts',(78.0298946126099,235.162534045408,6.43167577284028)) ;
#72466 = CARTESIAN_POINT('Ctrl Pts',(77.9323657714883,235.145398507738,6.35118822945158)) ;
#72467 = CARTESIAN_POINT('Ctrl Pts',(77.8557956985622,235.121979552267,6.30270555414491)) ;
#72468 = CARTESIAN_POINT('Ctrl Pts',(77.7215728499806,235.063585748907,6.24342928702186)) ;
#72469 = CARTESIAN_POINT('Ctrl Pts',(77.5749239465817,234.937168605196,6.27373289217854)) ;
#72470 = CARTESIAN_POINT('Ctrl Pts',(77.4845607759043,234.781755560483,6.40881021948315)) ;
#72471 = CARTESIAN_POINT('Ctrl Pts',(77.4276253550398,234.614308272085,6.59590889111905)) ;
#72472 = CARTESIAN_POINT('Ctrl Pts',(77.4210763090117,234.424954269108,6.86433848773879)) ;
#72473 = CARTESIAN_POINT('Ctrl Pts',(77.4569041711037,234.293005229142,7.08747263933178)) ;
#72474 = CARTESIAN_POINT('Ctrl Pts',(77.4834773178775,234.231922607649,7.19960833954764)) ;
#72475 = CARTESIAN_POINT('Ctrl Pts',(78.6120751679795,235.042656580024,7.17608503413729)) ;
#72476 = CARTESIAN_POINT('Ctrl Pts',(78.5257874071805,235.108293909258,7.00515935572851)) ;
#72477 = CARTESIAN_POINT('Ctrl Pts',(78.3906006573324,235.175667031547,6.77808190130018)) ;
#72478 = CARTESIAN_POINT('Ctrl Pts',(78.1753161685454,235.202640673185,6.51747818540342)) ;
#72479 = CARTESIAN_POINT('Ctrl Pts',(78.0539168452354,235.196261529505,6.39916177246118)) ;
#72480 = CARTESIAN_POINT('Ctrl Pts',(77.9468350659121,235.173936329358,6.31801268447563)) ;
#72481 = CARTESIAN_POINT('Ctrl Pts',(77.8626823795979,235.146014398301,6.269144723575)) ;
#72482 = CARTESIAN_POINT('Ctrl Pts',(77.7149629217121,235.07896759255,6.2094174531271)) ;
#72483 = CARTESIAN_POINT('Ctrl Pts',(77.5516109111798,234.939863263764,6.23994237498883)) ;
#72484 = CARTESIAN_POINT('Ctrl Pts',(77.4468142355107,234.771155243331,6.37609489248998)) ;
#72485 = CARTESIAN_POINT('Ctrl Pts',(77.3765566725479,234.589564664911,6.56483996405531)) ;
#72486 = CARTESIAN_POINT('Ctrl Pts',(77.3577590685433,234.383553168869,6.83601511990593)) ;
#72487 = CARTESIAN_POINT('Ctrl Pts',(77.3866701751303,234.237885051697,7.06215508260823)) ;
#72488 = CARTESIAN_POINT('Ctrl Pts',(77.4105061694942,234.169665602309,7.17608503411327)) ;
#72489 = CARTESIAN_POINT('Ctrl Pts',(78.6397340718682,235.07186568898,7.17267980086572)) ;
#72490 = CARTESIAN_POINT('Ctrl Pts',(78.5499065311274,235.13590406076,6.99940693067923)) ;
#72491 = CARTESIAN_POINT('Ctrl Pts',(78.4099204444132,235.200410168681,6.76972309168069)) ;
#72492 = CARTESIAN_POINT('Ctrl Pts',(78.187632684868,235.222365326873,6.5065198279272)) ;
#72493 = CARTESIAN_POINT('Ctrl Pts',(78.0622716858111,235.213009993023,6.38709993089628)) ;
#72494 = CARTESIAN_POINT('Ctrl Pts',(77.9515865903972,235.187946097367,6.30522258577693)) ;
#72495 = CARTESIAN_POINT('Ctrl Pts',(77.86447454918,235.157785697904,6.25592463927299)) ;
#72496 = CARTESIAN_POINT('Ctrl Pts',(77.7113224120971,235.08665818323,6.19568486135635)) ;
#72497 = CARTESIAN_POINT('Ctrl Pts',(77.5406975816401,234.942350518612,6.22646547497773)) ;
#72498 = CARTESIAN_POINT('Ctrl Pts',(77.429144135509,234.768977939852,6.36381708265207)) ;
#72499 = CARTESIAN_POINT('Ctrl Pts',(77.3523868997445,234.582817627175,6.55432519888145)) ;
#72500 = CARTESIAN_POINT('Ctrl Pts',(77.327204290906,234.371962310836,6.82828015762859)) ;
#72501 = CARTESIAN_POINT('Ctrl Pts',(77.3520863108302,234.222520587963,7.05718533633927)) ;
#72502 = CARTESIAN_POINT('Ctrl Pts',(77.3741795847386,234.152386532591,7.17267980084138)) ;
#72503 = CARTESIAN_POINT('Ctrl Pts',(77.3741795847386,234.152386532591,7.17267980084132)) ;
#72504 = CARTESIAN_POINT('Ctrl Pts',(77.3616101223674,234.192287697697,7.106971869474)) ;
#72505 = CARTESIAN_POINT('Ctrl Pts',(77.3521598145269,234.233709426668,7.04152334195408)) ;
#72506 = CARTESIAN_POINT('Ctrl Pts',(77.3461415055067,234.276630953922,6.97670888987274)) ;
#72507 = CARTESIAN_POINT('Ctrl Pts',(77.3427531126356,234.300796379205,6.94021743909526)) ;
#72508 = CARTESIAN_POINT('Ctrl Pts',(77.3404515536967,234.325437412815,6.90392730454654)) ;
#72509 = CARTESIAN_POINT('Ctrl Pts',(77.3392831405174,234.350552376217,6.86790768240443)) ;
#72510 = CARTESIAN_POINT('Ctrl Pts',(77.3388797538195,234.359223146399,6.85547215301052)) ;
#72511 = CARTESIAN_POINT('Ctrl Pts',(77.3386116782838,234.367952282434,6.84306652227551)) ;
#72512 = CARTESIAN_POINT('Ctrl Pts',(77.338480649152,234.376740738638,6.83069237265686)) ;
#72513 = CARTESIAN_POINT('Ctrl Pts',(77.3379770938846,234.410515467598,6.7831375416669)) ;
#72514 = CARTESIAN_POINT('Ctrl Pts',(77.3394958704025,234.445163335056,6.73604483330478)) ;
#72515 = CARTESIAN_POINT('Ctrl Pts',(77.343636060906,234.480754703633,6.68991055366433)) ;
#72516 = CARTESIAN_POINT('Ctrl Pts',(77.3445932458965,234.488983195477,6.67924460967454)) ;
#72517 = CARTESIAN_POINT('Ctrl Pts',(77.3456903680287,234.497262242329,6.66862989410104)) ;
#72518 = CARTESIAN_POINT('Ctrl Pts',(77.34693451014,234.505592968877,6.65807253999053)) ;
#72519 = CARTESIAN_POINT('Ctrl Pts',(77.3518801742937,234.538708941152,6.61610536654)) ;
#72520 = CARTESIAN_POINT('Ctrl Pts',(77.3591521949255,234.572639578347,6.57504372092637)) ;
#72521 = CARTESIAN_POINT('Ctrl Pts',(77.3692148632958,234.607477534717,6.5353038730101)) ;
#72522 = CARTESIAN_POINT('Ctrl Pts',(77.3714459871851,234.615201907006,6.52649263917198)) ;
#72523 = CARTESIAN_POINT('Ctrl Pts',(77.3738141831599,234.622971045816,6.51774638628193)) ;
#72524 = CARTESIAN_POINT('Ctrl Pts',(77.3763243098519,234.630786261121,6.50906965173452)) ;
#72525 = CARTESIAN_POINT('Ctrl Pts',(77.3770145717788,234.632935373989,6.50668362893874)) ;
#72526 = CARTESIAN_POINT('Ctrl Pts',(77.3777155795123,234.63508796889,6.50430287822882)) ;
#72527 = CARTESIAN_POINT('Ctrl Pts',(77.3784275163327,234.637244054133,6.50192759076481)) ;
#72528 = CARTESIAN_POINT('Ctrl Pts',(77.3885926649084,234.668028986472,6.46801285382404)) ;
#72529 = CARTESIAN_POINT('Ctrl Pts',(77.4009736446465,234.699452872062,6.43529517311966)) ;
#72530 = CARTESIAN_POINT('Ctrl Pts',(77.4160710196623,234.731531497338,6.4043522398541)) ;
#72531 = CARTESIAN_POINT('Ctrl Pts',(77.4185087934634,234.736711234357,6.39935588307255)) ;
#72532 = CARTESIAN_POINT('Ctrl Pts',(77.4210173606465,234.741908148382,6.39440579852665)) ;
#72533 = CARTESIAN_POINT('Ctrl Pts',(77.4235987954642,234.747122436193,6.38950441826156)) ;
#72534 = CARTESIAN_POINT('Ctrl Pts',(77.4274281313007,234.754857382293,6.38223364350942)) ;
#72535 = CARTESIAN_POINT('Ctrl Pts',(77.4314176194649,234.762630344498,6.37507015782897)) ;
#72536 = CARTESIAN_POINT('Ctrl Pts',(77.4355736599342,234.770441778795,6.36802208736112)) ;
#72537 = CARTESIAN_POINT('Ctrl Pts',(77.4431151830721,234.784616355036,6.35523270600096)) ;
#72538 = CARTESIAN_POINT('Ctrl Pts',(77.4512052664404,234.798917493541,6.3428233691989)) ;
#72539 = CARTESIAN_POINT('Ctrl Pts',(77.4599388214992,234.813284958107,6.33097919152505)) ;
#72540 = CARTESIAN_POINT('Ctrl Pts',(77.4727287173272,234.834325459239,6.31363392976204)) ;
#72541 = CARTESIAN_POINT('Ctrl Pts',(77.4869207989778,234.855607065859,6.2973856652023)) ;
#72542 = CARTESIAN_POINT('Ctrl Pts',(77.5028075979575,234.876890083662,6.2829000606871)) ;
#72543 = CARTESIAN_POINT('Ctrl Pts',(77.5128022833951,234.89027963233,6.27378689316436)) ;
#72544 = CARTESIAN_POINT('Ctrl Pts',(77.52346710991,234.903669696134,6.26537131953454)) ;
#72545 = CARTESIAN_POINT('Ctrl Pts',(77.5348655206898,234.917001932592,6.25781298087135)) ;
#72546 = CARTESIAN_POINT('Ctrl Pts',(77.5479220204083,234.932273565183,6.24915515579955)) ;
#72547 = CARTESIAN_POINT('Ctrl Pts',(77.5619406209771,234.947469595829,6.24162312159313)) ;
#72548 = CARTESIAN_POINT('Ctrl Pts',(77.5767273170561,234.962392577957,6.23533841590271)) ;
#72549 = CARTESIAN_POINT('Ctrl Pts',(77.5931271779032,234.978943593074,6.22836807592698)) ;
#72550 = CARTESIAN_POINT('Ctrl Pts',(77.610533619044,234.995184164585,6.22295448141433)) ;
#72551 = CARTESIAN_POINT('Ctrl Pts',(77.6287531529318,235.01091373282,6.21921752589672)) ;
#72552 = CARTESIAN_POINT('Ctrl Pts',(77.631852838839,235.013589801334,6.21858175835048)) ;
#72553 = CARTESIAN_POINT('Ctrl Pts',(77.6349761614252,235.016251058131,6.21799458776082)) ;
#72554 = CARTESIAN_POINT('Ctrl Pts',(77.6381222895719,235.018896483061,6.21745669291191)) ;
#72555 = CARTESIAN_POINT('Ctrl Pts',(77.654656351138,235.032799164904,6.2146298574706)) ;
#72556 = CARTESIAN_POINT('Ctrl Pts',(77.6718229084934,235.046267967594,6.21316348490088)) ;
#72557 = CARTESIAN_POINT('Ctrl Pts',(77.6894823515512,235.059110451571,6.21318607169313)) ;
#72558 = CARTESIAN_POINT('Ctrl Pts',(77.7048365201591,235.070276469869,6.21320570999176)) ;
#72559 = CARTESIAN_POINT('Ctrl Pts',(77.7205882506528,235.080940505187,6.21441169855859)) ;
#72560 = CARTESIAN_POINT('Ctrl Pts',(77.7365768790082,235.090876830127,6.21693669735049)) ;
#72561 = CARTESIAN_POINT('Ctrl Pts',(77.7376569000736,235.091548022178,6.21710725931645)) ;
#72562 = CARTESIAN_POINT('Ctrl Pts',(77.7387379880425,235.092215887671,6.21728382721156)) ;
#72563 = CARTESIAN_POINT('Ctrl Pts',(77.7398200874826,235.092880354597,6.2174664363144)) ;
#72564 = CARTESIAN_POINT('Ctrl Pts',(77.7508744945164,235.0996683517,6.21933191676467)) ;
#72565 = CARTESIAN_POINT('Ctrl Pts',(77.7619927080453,235.106176198894,6.22169249857145)) ;
#72566 = CARTESIAN_POINT('Ctrl Pts',(77.7731573385193,235.112355623372,6.22458829330823)) ;
#72567 = CARTESIAN_POINT('Ctrl Pts',(77.7879486527031,235.120542352806,6.22842474896731)) ;
#72568 = CARTESIAN_POINT('Ctrl Pts',(77.8028220367511,235.128153742158,6.23320001862001)) ;
#72569 = CARTESIAN_POINT('Ctrl Pts',(77.8176165123455,235.135214037743,6.23871136915441)) ;
#72570 = CARTESIAN_POINT('Ctrl Pts',(77.833003966678,235.142557317685,6.24444362063687)) ;
#72571 = CARTESIAN_POINT('Ctrl Pts',(77.848419888985,235.149315531718,6.2510693938749)) ;
#72572 = CARTESIAN_POINT('Ctrl Pts',(77.8636522359854,235.155531306993,6.25830795380365)) ;
#72573 = CARTESIAN_POINT('Ctrl Pts',(77.8854684142047,235.164433707991,6.26867521457129)) ;
#72574 = CARTESIAN_POINT('Ctrl Pts',(77.9069060915642,235.172221298945,6.28029834834182)) ;
#72575 = CARTESIAN_POINT('Ctrl Pts',(77.927961829551,235.178948105379,6.29304763982214)) ;
#72576 = CARTESIAN_POINT('Ctrl Pts',(77.9356336646272,235.181399073831,6.29769295131094)) ;
#72577 = CARTESIAN_POINT('Ctrl Pts',(77.9432550757436,235.183709627116,6.30248760576134)) ;
#72578 = CARTESIAN_POINT('Ctrl Pts',(77.9508268025495,235.185883737378,6.30742481813906)) ;
#72579 = CARTESIAN_POINT('Ctrl Pts',(77.9701099120664,235.191420599359,6.31999854265769)) ;
#72580 = CARTESIAN_POINT('Ctrl Pts',(77.9890694837187,235.196070917094,6.33349709476029)) ;
#72581 = CARTESIAN_POINT('Ctrl Pts',(78.0076268293722,235.200005114599,6.34759111946657)) ;
#72582 = CARTESIAN_POINT('Ctrl Pts',(78.0163745748408,235.2018596556,6.35423490048245)) ;
#72583 = CARTESIAN_POINT('Ctrl Pts',(78.0250425173661,235.203549292818,6.36102798943507)) ;
#72584 = CARTESIAN_POINT('Ctrl Pts',(78.0336233074686,235.205088399391,6.36794163166575)) ;
#72585 = CARTESIAN_POINT('Ctrl Pts',(78.0699367923575,235.211601823283,6.3971998281341)) ;
#72586 = CARTESIAN_POINT('Ctrl Pts',(78.1046886470117,235.215413254151,6.42861607705246)) ;
#72587 = CARTESIAN_POINT('Ctrl Pts',(78.1380455613265,235.21707104078,6.46147659275002)) ;
#72588 = CARTESIAN_POINT('Ctrl Pts',(78.1538675906542,235.217857370967,6.47706316764065)) ;
#72589 = CARTESIAN_POINT('Ctrl Pts',(78.1693759091666,235.218160283575,6.49297483602705)) ;
#72590 = CARTESIAN_POINT('Ctrl Pts',(78.184588856189,235.218043521371,6.50913654336621)) ;
#72591 = CARTESIAN_POINT('Ctrl Pts',(78.2070668421853,235.217870998639,6.53301637616342)) ;
#72592 = CARTESIAN_POINT('Ctrl Pts',(78.2288998377486,235.216781901257,6.55744192341381)) ;
#72593 = CARTESIAN_POINT('Ctrl Pts',(78.2501404992287,235.214912122256,6.58226166134351)) ;
#72594 = CARTESIAN_POINT('Ctrl Pts',(78.2735769892242,235.212849048236,6.6096472274769)) ;
#72595 = CARTESIAN_POINT('Ctrl Pts',(78.296297808578,235.209804393606,6.63755574293694)) ;
#72596 = CARTESIAN_POINT('Ctrl Pts',(78.3183648534066,235.205949915774,6.66580368541426)) ;
#72597 = CARTESIAN_POINT('Ctrl Pts',(78.3568347764113,235.199230327059,6.71504889158392)) ;
#72598 = CARTESIAN_POINT('Ctrl Pts',(78.3933163504242,235.19004732315,6.76532387402165)) ;
#72599 = CARTESIAN_POINT('Ctrl Pts',(78.4280131127771,235.178728979788,6.81629655261704)) ;
#72600 = CARTESIAN_POINT('Ctrl Pts',(78.4315249867773,235.177583380225,6.82145581280564)) ;
#72601 = CARTESIAN_POINT('Ctrl Pts',(78.43501855861,235.176415944776,6.82662222069363)) ;
#72602 = CARTESIAN_POINT('Ctrl Pts',(78.4384940288008,235.175227040323,6.83179543193681)) ;
#72603 = CARTESIAN_POINT('Ctrl Pts',(78.4743358912824,235.162966095017,6.88514577470656)) ;
#72604 = CARTESIAN_POINT('Ctrl Pts',(78.508254558857,235.148418773849,6.93921964827946)) ;
#72605 = CARTESIAN_POINT('Ctrl Pts',(78.5404913241743,235.132011538704,6.99367466100287)) ;
#72606 = CARTESIAN_POINT('Ctrl Pts',(78.5422638099616,235.131109413729,6.99666878076482)) ;
#72607 = CARTESIAN_POINT('Ctrl Pts',(78.5440312099124,235.13020167882,6.99966405277532)) ;
#72608 = CARTESIAN_POINT('Ctrl Pts',(78.5457935638897,235.129288409307,7.00266042012063)) ;
#72609 = CARTESIAN_POINT('Ctrl Pts',(78.5725232220026,235.115436832295,7.0481063837325)) ;
#72610 = CARTESIAN_POINT('Ctrl Pts',(78.59805570937,235.100254606844,7.09382974369312)) ;
#72611 = CARTESIAN_POINT('Ctrl Pts',(78.6224329066999,235.083850652226,7.13971415669166)) ;
#72612 = CARTESIAN_POINT('Ctrl Pts',(78.6282662782212,235.07992524766,7.15069412393042)) ;
#72613 = CARTESIAN_POINT('Ctrl Pts',(78.6340332765776,235.075929806123,7.16168324953904)) ;
#72614 = CARTESIAN_POINT('Ctrl Pts',(78.6397340718556,235.071865688989,7.17267980084157)) ;
#72615 = CARTESIAN_POINT('Ctrl Pts',(78.4059643744832,235.032597310178,7.27867958886636)) ;
#72616 = CARTESIAN_POINT('Ctrl Pts',(78.3389185036295,235.080934607739,7.10540671867987)) ;
#72617 = CARTESIAN_POINT('Ctrl Pts',(78.234821145,235.130175045901,6.8757228796813)) ;
#72618 = CARTESIAN_POINT('Ctrl Pts',(78.0706643466897,235.148929220103,6.61251961592784)) ;
#72619 = CARTESIAN_POINT('Ctrl Pts',(77.9784150954104,235.143436282111,6.49309971889691)) ;
#72620 = CARTESIAN_POINT('Ctrl Pts',(77.8972265351195,235.126146469199,6.41122237377758)) ;
#72621 = CARTESIAN_POINT('Ctrl Pts',(77.8334871500539,235.1048001745,6.36192442727363)) ;
#72622 = CARTESIAN_POINT('Ctrl Pts',(77.7217018252731,235.053842764399,6.30168464935698)) ;
#72623 = CARTESIAN_POINT('Ctrl Pts',(77.5980687835801,234.948679457524,6.33246526297836)) ;
#72624 = CARTESIAN_POINT('Ctrl Pts',(77.5181116348167,234.821023036642,6.4698168706527)) ;
#72625 = CARTESIAN_POINT('Ctrl Pts',(77.4637464544563,234.683353081259,6.66032498688208)) ;
#72626 = CARTESIAN_POINT('Ctrl Pts',(77.447328463511,234.526604137613,6.93427994562925)) ;
#72627 = CARTESIAN_POINT('Ctrl Pts',(77.4669324115197,234.415038329963,7.1631851243399)) ;
#72628 = CARTESIAN_POINT('Ctrl Pts',(77.4837648415456,234.362580130206,7.27867958884201)) ;
#72629 = CARTESIAN_POINT('Origin',(77.2933283411226,234.301474162358,16.0213203435596)) ;
#72630 = CARTESIAN_POINT('',(77.4837648415456,234.362580130206,16.0254384350469)) ;
#72631 = CARTESIAN_POINT('',(77.4837648415456,234.362580130206,16.0213203435596)) ;
#72632 = CARTESIAN_POINT('Ctrl Pts',(77.4837648415456,234.362580130206,16.0254384350469)) ;
#72633 = CARTESIAN_POINT('Ctrl Pts',(77.4898800012088,234.343522259972,16.0294645582753)) ;
#72634 = CARTESIAN_POINT('Ctrl Pts',(77.492875683057,234.324370671673,16.0362204083692)) ;
#72635 = CARTESIAN_POINT('Ctrl Pts',(77.4938035272304,234.281917507663,16.056050217191)) ;
#72636 = CARTESIAN_POINT('Ctrl Pts',(77.4900164569724,234.259358551804,16.0702237187361)) ;
#72637 = CARTESIAN_POINT('Ctrl Pts',(77.4751861439491,234.214268834133,16.1046945816763)) ;
#72638 = CARTESIAN_POINT('Ctrl Pts',(77.4626920303345,234.192466720987,16.1258672215778)) ;
#72639 = CARTESIAN_POINT('Ctrl Pts',(77.4313743096848,234.15454847925,16.1708720249663)) ;
#72640 = CARTESIAN_POINT('Ctrl Pts',(77.4119227585275,234.138567724759,16.1951765216655)) ;
#72641 = CARTESIAN_POINT('Ctrl Pts',(77.3898617560505,234.126312068692,16.2199877856737)) ;
#72642 = CARTESIAN_POINT('Ctrl Pts',(77.3892676870572,234.125985982886,16.2206540664817)) ;
#72643 = CARTESIAN_POINT('Ctrl Pts',(77.3886719794696,234.125662926577,16.2213203435596)) ;
#72644 = CARTESIAN_POINT('Origin',(74.5283628290597,239.4,16.2213203435596)) ;
#72645 = CARTESIAN_POINT('',(75.7840731199179,233.737563098327,16.0213203435596)) ;
#72646 = CARTESIAN_POINT('Ctrl Pts',(75.7824688237379,233.69585956045,16.0254384350468)) ;
#72647 = CARTESIAN_POINT('Ctrl Pts',(75.7825092685165,233.706896612048,16.0232182514845)) ;
#72648 = CARTESIAN_POINT('Ctrl Pts',(75.7828565073841,233.718128254652,16.0218983740811)) ;
#72649 = CARTESIAN_POINT('Ctrl Pts',(75.7836951033986,233.732160271511,16.0213707571522)) ;
#72650 = CARTESIAN_POINT('Ctrl Pts',(75.7838750549479,233.734863451389,16.0213203435596)) ;
#72651 = CARTESIAN_POINT('Ctrl Pts',(75.784073119918,233.737563098327,16.0213203435596)) ;
#72652 = CARTESIAN_POINT('',(76.8407687665842,234.080904326852,16.0213203435596)) ;
#72653 = CARTESIAN_POINT('Origin',(74.5283628290597,239.4,16.0213203435596)) ;
#72654 = CARTESIAN_POINT('Ctrl Pts',(76.8407687665842,234.080904326852,16.0213203435596)) ;
#72655 = CARTESIAN_POINT('Ctrl Pts',(76.8480493410532,234.072287741056,16.0213203435596)) ;
#72656 = CARTESIAN_POINT('Ctrl Pts',(76.8550882213081,234.063461822359,16.0221950109068)) ;
#72657 = CARTESIAN_POINT('Ctrl Pts',(76.8634346692571,234.052374031266,16.0244263118334)) ;
#72658 = CARTESIAN_POINT('Ctrl Pts',(76.865018268209,234.050240667937,16.0249068532759)) ;
#72659 = CARTESIAN_POINT('Ctrl Pts',(76.8665793939903,234.048108437619,16.0254384350468)) ;
#72660 = CARTESIAN_POINT('Origin',(75.2882970367382,233.65,16.0213203435596)) ;
#72661 = CARTESIAN_POINT('',(75.0983134848186,233.5875,16.0254384350469)) ;
#72662 = CARTESIAN_POINT('',(75.0983134848186,233.5875,16.0213203435596)) ;
#72663 = CARTESIAN_POINT('Ctrl Pts',(75.3145016645892,233.451724137931,16.2213203435596)) ;
#72664 = CARTESIAN_POINT('Ctrl Pts',(75.3138298392977,233.45163534784,16.2206540664858)) ;
#72665 = CARTESIAN_POINT('Ctrl Pts',(75.3131575589563,233.451549971806,16.2199877856686)) ;
#72666 = CARTESIAN_POINT('Ctrl Pts',(75.291887836757,233.448958610743,16.1989219660293)) ;
#72667 = CARTESIAN_POINT('Ctrl Pts',(75.2707751266654,233.449639261295,16.1784289743322)) ;
#72668 = CARTESIAN_POINT('Ctrl Pts',(75.2300209844512,233.457606862526,16.1396302534681)) ;
#72669 = CARTESIAN_POINT('Ctrl Pts',(75.2101322048779,233.46463785473,16.1210537744074)) ;
#72670 = CARTESIAN_POINT('Ctrl Pts',(75.1712077544563,233.486252834152,16.0855257632413)) ;
#72671 = CARTESIAN_POINT('Ctrl Pts',(75.1520253541674,233.501393309518,16.06848760944)) ;
#72672 = CARTESIAN_POINT('Ctrl Pts',(75.1231810065142,233.535534386453,16.0440628922134)) ;
#72673 = CARTESIAN_POINT('Ctrl Pts',(75.1123902411184,233.552558228057,16.0353723462)) ;
#72674 = CARTESIAN_POINT('Ctrl Pts',(75.102036322246,233.576939504834,16.0279192770417)) ;
#72675 = CARTESIAN_POINT('Ctrl Pts',(75.1000672207974,233.582169104154,16.0265673132415)) ;
#72676 = CARTESIAN_POINT('Ctrl Pts',(75.0983134848186,233.5875,16.0254384350468)) ;
#72677 = CARTESIAN_POINT('Origin',(74.5283628290597,239.4,7.2786795888419)) ;
#72678 = CARTESIAN_POINT('Origin',(74.5283628290597,239.4,7.17267980084126)) ;
#72679 = CARTESIAN_POINT('Origin',(78.5229277183602,235.19483040233,16.0213203435596)) ;
#72680 = CARTESIAN_POINT('',(78.4059643744738,235.032597310185,16.0254384350469)) ;
#72681 = CARTESIAN_POINT('',(78.4059643744738,235.032597310185,16.0213203435596)) ;
#72682 = CARTESIAN_POINT('Ctrl Pts',(78.6606713352325,235.049824554134,16.2213203435594)) ;
#72683 = CARTESIAN_POINT('Ctrl Pts',(78.6601800066574,235.049357832441,16.2206540664819)) ;
#72684 = CARTESIAN_POINT('Ctrl Pts',(78.6596863032101,235.048893605308,16.2199877856694)) ;
#72685 = CARTESIAN_POINT('Ctrl Pts',(78.6440019003139,235.034295121153,16.1989219660103)) ;
#72686 = CARTESIAN_POINT('Ctrl Pts',(78.6265212826879,235.022436039381,16.1784289743341)) ;
#72687 = CARTESIAN_POINT('Ctrl Pts',(78.5888672505516,235.004927280419,16.1396302534752)) ;
#72688 = CARTESIAN_POINT('Ctrl Pts',(78.568644176356,234.99892514128,16.1210537744168)) ;
#72689 = CARTESIAN_POINT('Ctrl Pts',(78.5244486683382,234.993532809052,16.0855257632509)) ;
#72690 = CARTESIAN_POINT('Ctrl Pts',(78.5000304323776,234.994506578931,16.0684876094478)) ;
#72691 = CARTESIAN_POINT('Ctrl Pts',(78.4566272434126,235.005173008213,16.0440628922183)) ;
#72692 = CARTESIAN_POINT('Ctrl Pts',(78.4378909677921,235.012602932619,16.0353723462039)) ;
#72693 = CARTESIAN_POINT('Ctrl Pts',(78.4151835165405,235.02624191906,16.0279192770432)) ;
#72694 = CARTESIAN_POINT('Ctrl Pts',(78.4105165986467,235.029315344993,16.0265673132422)) ;
#72695 = CARTESIAN_POINT('Ctrl Pts',(78.4059643744738,235.032597310185,16.0254384350468)) ;
#72696 = CARTESIAN_POINT('Origin',(74.5283628290597,239.4,16.2213203435596)) ;
#72697 = CARTESIAN_POINT('',(77.4724035159522,234.40273830644,16.0213203435596)) ;
#72698 = CARTESIAN_POINT('Ctrl Pts',(77.4837648415455,234.362580130206,16.0254384350468)) ;
#72699 = CARTESIAN_POINT('Ctrl Pts',(77.4803926703042,234.373089488173,16.0232182514845)) ;
#72700 = CARTESIAN_POINT('Ctrl Pts',(77.4772521456526,234.383878717771,16.0218983740811)) ;
#72701 = CARTESIAN_POINT('Ctrl Pts',(77.473713566182,234.397483099261,16.0213707571522)) ;
#72702 = CARTESIAN_POINT('Ctrl Pts',(77.4730493817544,234.400109584186,16.0213203435596)) ;
#72703 = CARTESIAN_POINT('Ctrl Pts',(77.4724035159521,234.40273830644,16.0213203435596)) ;
#72704 = CARTESIAN_POINT('',(78.3712825219709,235.055812131844,16.0213203435596)) ;
#72705 = CARTESIAN_POINT('Origin',(74.5283628290597,239.4,16.0213203435596)) ;
#72706 = CARTESIAN_POINT('Ctrl Pts',(78.3712825219707,235.055812131844,16.0213203435596)) ;
#72707 = CARTESIAN_POINT('Ctrl Pts',(78.3808694312064,235.049867093014,16.0213203435596)) ;
#72708 = CARTESIAN_POINT('Ctrl Pts',(78.3902911630086,235.043648279145,16.0221950109068)) ;
#72709 = CARTESIAN_POINT('Ctrl Pts',(78.4016554225963,235.035682357433,16.0244263118334)) ;
#72710 = CARTESIAN_POINT('Ctrl Pts',(78.4038207602224,235.034142767326,16.0249068532759)) ;
#72711 = CARTESIAN_POINT('Ctrl Pts',(78.4059643744737,235.032597310185,16.0254384350468)) ;
#72712 = CARTESIAN_POINT('Origin',(73.7684286213811,233.65,16.0213203435596)) ;
#72713 = CARTESIAN_POINT('',(73.9584121733008,233.5875,16.0254384350469)) ;
#72714 = CARTESIAN_POINT('',(73.9584121733008,233.5875,16.0213203435596)) ;
#72715 = CARTESIAN_POINT('Ctrl Pts',(73.9584121733008,233.5875,16.0254384350469)) ;
#72716 = CARTESIAN_POINT('Ctrl Pts',(73.9521575063278,233.568487458438,16.0294645582753)) ;
#72717 = CARTESIAN_POINT('Ctrl Pts',(73.9433240426927,233.551232680424,16.0362204083692)) ;
#72718 = CARTESIAN_POINT('Ctrl Pts',(73.9191213406789,233.516341976154,16.056050217191)) ;
#72719 = CARTESIAN_POINT('Ctrl Pts',(73.9027977149204,233.500317381536,16.070223718736)) ;
#72720 = CARTESIAN_POINT('Ctrl Pts',(73.8642966685758,233.47255607295,16.1046945816758)) ;
#72721 = CARTESIAN_POINT('Ctrl Pts',(73.8413737577571,233.462261648626,16.1258672215766)) ;
#72722 = CARTESIAN_POINT('Ctrl Pts',(73.7937494062409,233.449993240996,16.1708720249644)) ;
#72723 = CARTESIAN_POINT('Ctrl Pts',(73.7686195190054,233.44849787393,16.1951765216962)) ;
#72724 = CARTESIAN_POINT('Ctrl Pts',(73.7435680991658,233.451549971806,16.2199877856659)) ;
#72725 = CARTESIAN_POINT('Ctrl Pts',(73.7428958188225,233.45163534784,16.220654066485)) ;
#72726 = CARTESIAN_POINT('Ctrl Pts',(73.7422239935301,233.451724137931,16.2213203435596)) ;
#72727 = CARTESIAN_POINT('Origin',(74.5283628290597,239.4,16.2213203435596)) ;
#72728 = CARTESIAN_POINT('',(73.9728250515664,233.626666666667,16.0213203435596)) ;
#72729 = CARTESIAN_POINT('Ctrl Pts',(73.9584121733008,233.5875,16.0254384350468)) ;
#72730 = CARTESIAN_POINT('Ctrl Pts',(73.9618612750826,233.597984361719,16.0232182514845)) ;
#72731 = CARTESIAN_POINT('Ctrl Pts',(73.9656622873096,233.608558985895,16.0218983740811)) ;
#72732 = CARTESIAN_POINT('Ctrl Pts',(73.9707959711885,233.621645086545,16.0213707571522)) ;
#72733 = CARTESIAN_POINT('Ctrl Pts',(73.9718024438033,233.624160355296,16.0213203435596)) ;
#72734 = CARTESIAN_POINT('Ctrl Pts',(73.9728250515665,233.626666666667,16.0213203435596)) ;
#72735 = CARTESIAN_POINT('',(75.083900606553,233.626666666667,16.0213203435596)) ;
#72736 = CARTESIAN_POINT('Origin',(74.5283628290597,239.4,16.0213203435596)) ;
#72737 = CARTESIAN_POINT('Ctrl Pts',(75.0839006065529,233.626666666667,16.0213203435596)) ;
#72738 = CARTESIAN_POINT('Ctrl Pts',(75.0881621728995,233.616221985357,16.0213203435596)) ;
#72739 = CARTESIAN_POINT('Ctrl Pts',(75.0921291869651,233.605652904248,16.0221950109068)) ;
#72740 = CARTESIAN_POINT('Ctrl Pts',(75.0966408147971,233.592528594019,16.0244263118334)) ;
#72741 = CARTESIAN_POINT('Ctrl Pts',(75.0974876613757,233.590010285935,16.0249068532759)) ;
#72742 = CARTESIAN_POINT('Ctrl Pts',(75.0983134848186,233.5875,16.0254384350468)) ;
#72743 = CARTESIAN_POINT('Ctrl Pts',(79.5657826988647,236.44459798751,7.27867958886636)) ;
#72744 = CARTESIAN_POINT('Ctrl Pts',(79.4870812400902,236.469851175839,7.10540671867988)) ;
#72745 = CARTESIAN_POINT('Ctrl Pts',(79.3728626924325,236.484513827223,6.87572289449329)) ;
#72746 = CARTESIAN_POINT('Ctrl Pts',(79.2109449345459,236.451622856973,6.61251963169561)) ;
#72747 = CARTESIAN_POINT('Ctrl Pts',(79.1249080993041,236.417892181793,6.49309973646919)) ;
#72748 = CARTESIAN_POINT('Ctrl Pts',(79.0530360354225,236.376359946734,6.41122239160556)) ;
#72749 = CARTESIAN_POINT('Ctrl Pts',(78.9990126464368,236.336361861471,6.36192444560416)) ;
#72750 = CARTESIAN_POINT('Ctrl Pts',(78.908445191216,236.253354919289,6.30168466926149)) ;
#72751 = CARTESIAN_POINT('Ctrl Pts',(78.8233604283728,236.115133957597,6.33246528275406)) ;
#72752 = CARTESIAN_POINT('Ctrl Pts',(78.7867646631746,235.969017367392,6.46981689000949)) ;
#72753 = CARTESIAN_POINT('Ctrl Pts',(78.7776026491497,235.821285683305,6.66032500142642)) ;
#72754 = CARTESIAN_POINT('Ctrl Pts',(78.8104263003458,235.66713514265,6.93427995946187)) ;
#72755 = CARTESIAN_POINT('Ctrl Pts',(78.8635464513941,235.567087660364,7.16318512434001)) ;
#72756 = CARTESIAN_POINT('Ctrl Pts',(78.8957655188746,235.522398454586,7.27867958884211)) ;
#72757 = CARTESIAN_POINT('Ctrl Pts',(79.6090300580747,236.430721069295,7.24979207610077)) ;
#72758 = CARTESIAN_POINT('Ctrl Pts',(79.5283104770667,236.463357568788,7.07844135600528)) ;
#72759 = CARTESIAN_POINT('Ctrl Pts',(79.4082537819674,236.486436190288,6.85076495835015)) ;
#72760 = CARTESIAN_POINT('Ctrl Pts',(79.2349602606826,236.459327520044,6.5894676145758)) ;
#72761 = CARTESIAN_POINT('Ctrl Pts',(79.1422533331441,236.426642473391,6.47083496648431)) ;
#72762 = CARTESIAN_POINT('Ctrl Pts',(79.0646411031859,236.384416214936,6.38946908750231)) ;
#72763 = CARTESIAN_POINT('Ctrl Pts',(79.0063276682255,236.342908901173,6.34047050406937)) ;
#72764 = CARTESIAN_POINT('Ctrl Pts',(78.9086887020337,236.255628981196,6.28058367983847)) ;
#72765 = CARTESIAN_POINT('Ctrl Pts',(78.8185329489278,236.10759602833,6.31119007162906)) ;
#72766 = CARTESIAN_POINT('Ctrl Pts',(78.7832287335185,235.951015918468,6.44770640459992)) ;
#72767 = CARTESIAN_POINT('Ctrl Pts',(78.7789048125338,235.793643854386,6.63695562729077)) ;
#72768 = CARTESIAN_POINT('Ctrl Pts',(78.8220685829243,235.631914269905,6.9088523574302)) ;
#72769 = CARTESIAN_POINT('Ctrl Pts',(78.885012217346,235.530003744361,7.13557881442663)) ;
#72770 = CARTESIAN_POINT('Ctrl Pts',(78.9223274213261,235.485555975355,7.24979207607679)) ;
#72771 = CARTESIAN_POINT('Ctrl Pts',(79.6964402031828,236.444885555299,7.19960835919207)) ;
#72772 = CARTESIAN_POINT('Ctrl Pts',(79.6047997839638,236.484752447894,7.03137454200852)) ;
#72773 = CARTESIAN_POINT('Ctrl Pts',(79.4687331749363,236.514458639794,6.80703935301077)) ;
#72774 = CARTESIAN_POINT('Ctrl Pts',(79.2726259399176,236.487237708637,6.5489632709138)) ;
#72775 = CARTESIAN_POINT('Ctrl Pts',(79.1679664882912,236.45196330917,6.43167580665653)) ;
#72776 = CARTESIAN_POINT('Ctrl Pts',(79.0805062198949,236.40552837394,6.35118826354325)) ;
#72777 = CARTESIAN_POINT('Ctrl Pts',(79.0149206087179,236.359594169686,6.30270558867851)) ;
#72778 = CARTESIAN_POINT('Ctrl Pts',(78.9053117717612,236.262581220077,6.24342932307369)) ;
#72779 = CARTESIAN_POINT('Ctrl Pts',(78.804905418412,236.097034364148,6.27373292820263)) ;
#72780 = CARTESIAN_POINT('Ctrl Pts',(78.7669902051957,235.921304016953,6.40881025513765)) ;
#72781 = CARTESIAN_POINT('Ctrl Pts',(78.7645854417403,235.744458153853,6.5959089226156)) ;
#72782 = CARTESIAN_POINT('Ctrl Pts',(78.8168705353506,235.562348030992,6.86433851840462)) ;
#72783 = CARTESIAN_POINT('Ctrl Pts',(78.8917192824295,235.447928391624,7.0874726589527)) ;
#72784 = CARTESIAN_POINT('Ctrl Pts',(78.9358674149294,235.398046920369,7.19960835916855)) ;
#72785 = CARTESIAN_POINT('Ctrl Pts',(79.7586972267648,236.51785665956,7.17608503413728)) ;
#72786 = CARTESIAN_POINT('Ctrl Pts',(79.6563496393816,236.553617084748,7.00515935572852)) ;
#72787 = CARTESIAN_POINT('Ctrl Pts',(79.5069600229606,236.575917823757,6.7780819280561)) ;
#72788 = CARTESIAN_POINT('Ctrl Pts',(79.293876985863,236.535044702284,6.51747821181318)) ;
#72789 = CARTESIAN_POINT('Ctrl Pts',(79.1803906379132,236.491463330501,6.39916180179056)) ;
#72790 = CARTESIAN_POINT('Ctrl Pts',(79.085448679511,236.43714071249,6.31801271393377)) ;
#72791 = CARTESIAN_POINT('Ctrl Pts',(79.0140430708291,236.384580768783,6.26914475369938)) ;
#72792 = CARTESIAN_POINT('Ctrl Pts',(78.8942721210401,236.275167644272,6.20941748487202)) ;
#72793 = CARTESIAN_POINT('Ctrl Pts',(78.7819007264524,236.092393015084,6.23994240617312)) ;
#72794 = CARTESIAN_POINT('Ctrl Pts',(78.7343668090907,235.899558197127,6.37609492300486)) ;
#72795 = CARTESIAN_POINT('Ctrl Pts',(78.7236624584774,235.705144496605,6.56483998757442)) ;
#72796 = CARTESIAN_POINT('Ctrl Pts',(78.7694459290053,235.503407144677,6.83601514313855)) ;
#72797 = CARTESIAN_POINT('Ctrl Pts',(78.841955902057,235.373802485635,7.06215508260834)) ;
#72798 = CARTESIAN_POINT('Ctrl Pts',(78.8857062490269,235.316287661092,7.17608503411338)) ;
#72799 = CARTESIAN_POINT('Ctrl Pts',(79.7759762964836,236.554183244316,7.17267980086571)) ;
#72800 = CARTESIAN_POINT('Ctrl Pts',(79.6707562833474,236.587329118438,6.99940693067923)) ;
#72801 = CARTESIAN_POINT('Ctrl Pts',(79.5176881965809,236.60542008249,6.76972310649274)) ;
#72802 = CARTESIAN_POINT('Ctrl Pts',(79.2994954482259,236.557609970426,6.50651984369493)) ;
#72803 = CARTESIAN_POINT('Ctrl Pts',(79.1831610173716,236.509973847899,6.38709994846854)) ;
#72804 = CARTESIAN_POINT('Ctrl Pts',(79.0856384050087,236.451933089803,6.3052226036049)) ;
#72805 = CARTESIAN_POINT('Ctrl Pts',(79.0121100075054,236.396329745053,6.2559246576035)) ;
#72806 = CARTESIAN_POINT('Ctrl Pts',(78.888433281189,236.281356845433,6.19568488126083)) ;
#72807 = CARTESIAN_POINT('Ctrl Pts',(78.7707529424765,236.091386124969,6.22646549475341)) ;
#72808 = CARTESIAN_POINT('Ctrl Pts',(78.7182343819777,235.892027091496,6.36381710200884)) ;
#72809 = CARTESIAN_POINT('Ctrl Pts',(78.7027605981832,235.691258807103,6.55432521342576)) ;
#72810 = CARTESIAN_POINT('Ctrl Pts',(78.7439683914917,235.482941632937,6.8282801714612)) ;
#72811 = CARTESIAN_POINT('Ctrl Pts',(78.8138125729589,235.348503010481,7.05718533633938)) ;
#72812 = CARTESIAN_POINT('Ctrl Pts',(78.8564971400703,235.288628757204,7.17267980084148)) ;
#72813 = CARTESIAN_POINT('Ctrl Pts',(78.8564971400703,235.288628757204,7.17267980084147)) ;
#72814 = CARTESIAN_POINT('Ctrl Pts',(78.8322127772666,235.322692780517,7.10697198962071)) ;
#72815 = CARTESIAN_POINT('Ctrl Pts',(78.8104250280159,235.359166818334,7.04152358318827)) ;
#72816 = CARTESIAN_POINT('Ctrl Pts',(78.7914378312746,235.398127786439,6.97670925058748)) ;
#72817 = CARTESIAN_POINT('Ctrl Pts',(78.7807477174163,235.420063472405,6.94021768184272)) ;
#72818 = CARTESIAN_POINT('Ctrl Pts',(78.7709442790968,235.442787344193,6.90392743085573)) ;
#72819 = CARTESIAN_POINT('Ctrl Pts',(78.7620720790055,235.466312115078,6.86790769436091)) ;
#72820 = CARTESIAN_POINT('Ctrl Pts',(78.7590090216288,235.474433857402,6.85547216332687)) ;
#72821 = CARTESIAN_POINT('Ctrl Pts',(78.7560566159773,235.482652921741,6.84306653074808)) ;
#72822 = CARTESIAN_POINT('Ctrl Pts',(78.7532162176156,235.490970752063,6.83069237910109)) ;
#72823 = CARTESIAN_POINT('Ctrl Pts',(78.7423004157144,235.522936616169,6.78313785650423)) ;
#72824 = CARTESIAN_POINT('Ctrl Pts',(78.7330381191646,235.556357792529,6.73604544693575)) ;
#72825 = CARTESIAN_POINT('Ctrl Pts',(78.7259773485412,235.591486331508,6.68991145156326)) ;
#72826 = CARTESIAN_POINT('Ctrl Pts',(78.7243443243909,235.599610905379,6.67924152152199)) ;
#72827 = CARTESIAN_POINT('Ctrl Pts',(78.7228288537345,235.607826871102,6.66862285804887)) ;
#72828 = CARTESIAN_POINT('Ctrl Pts',(78.7214373324945,235.61613749082,6.65806160112184)) ;
#72829 = CARTESIAN_POINT('Ctrl Pts',(78.7159079051888,235.649161038197,6.61609479475419)) ;
#72830 = CARTESIAN_POINT('Ctrl Pts',(78.7123392499051,235.683678268544,6.575033543448)) ;
#72831 = CARTESIAN_POINT('Ctrl Pts',(78.7111442988235,235.719920776149,6.5352941167486)) ;
#72832 = CARTESIAN_POINT('Ctrl Pts',(78.7108794472324,235.727953645404,6.52648618263948)) ;
#72833 = CARTESIAN_POINT('Ctrl Pts',(78.7107310413867,235.736071386349,6.51774318351641)) ;
#72834 = CARTESIAN_POINT('Ctrl Pts',(78.7107032926989,235.744276743245,6.50906965181891)) ;
#72835 = CARTESIAN_POINT('Ctrl Pts',(78.7106956592731,235.746533966463,6.50668363773311)) ;
#72836 = CARTESIAN_POINT('Ctrl Pts',(78.7106971696829,235.748797821899,6.50430289572339)) ;
#72837 = CARTESIAN_POINT('Ctrl Pts',(78.7107079956681,235.751068374094,6.50192761694854)) ;
#72838 = CARTESIAN_POINT('Ctrl Pts',(78.7108625712828,235.783487779315,6.46801290435377)) ;
#72839 = CARTESIAN_POINT('Ctrl Pts',(78.7129270713278,235.817199587996,6.43529524449621)) ;
#72840 = CARTESIAN_POINT('Ctrl Pts',(78.7173726789433,235.852373496539,6.40435232380597)) ;
#72841 = CARTESIAN_POINT('Ctrl Pts',(78.7180907228513,235.85805470211,6.39935449727259)) ;
#72842 = CARTESIAN_POINT('Ctrl Pts',(78.7188708235085,235.863774142674,6.39440297002402)) ;
#72843 = CARTESIAN_POINT('Ctrl Pts',(78.7197148945106,235.869532647099,6.3895001762352)) ;
#72844 = CARTESIAN_POINT('Ctrl Pts',(78.7209663891753,235.87807071741,6.38223085854324)) ;
#72845 = CARTESIAN_POINT('Ctrl Pts',(78.7223583960393,235.886694399858,6.37506878931773)) ;
#72846 = CARTESIAN_POINT('Ctrl Pts',(78.7238968574451,235.895406104459,6.3680220898963)) ;
#72847 = CARTESIAN_POINT('Ctrl Pts',(78.7266890802744,235.911217369126,6.3552327180466)) ;
#72848 = CARTESIAN_POINT('Ctrl Pts',(78.7299639023541,235.927318514931,6.34282338850292)) ;
#72849 = CARTESIAN_POINT('Ctrl Pts',(78.7338302037624,235.943681583749,6.33097921492544)) ;
#72850 = CARTESIAN_POINT('Ctrl Pts',(78.7394922114334,235.967644490772,6.31363400704614)) ;
#72851 = CARTESIAN_POINT('Ctrl Pts',(78.7464132687362,235.992270001039,6.29738579228852)) ;
#72852 = CARTESIAN_POINT('Ctrl Pts',(78.7549456537334,236.017420547968,6.28290022688547)) ;
#72853 = CARTESIAN_POINT('Ctrl Pts',(78.7603135972084,236.033243405741,6.27378698406848)) ;
#72854 = CARTESIAN_POINT('Ctrl Pts',(78.7663187342802,236.049273842205,6.26537134622199)) ;
#72855 = CARTESIAN_POINT('Ctrl Pts',(78.7730394330041,236.065475973807,6.2578129580718)) ;
#72856 = CARTESIAN_POINT('Ctrl Pts',(78.7807377033575,236.084034816347,6.24915515063138)) ;
#72857 = CARTESIAN_POINT('Ctrl Pts',(78.7893743477905,236.102819061703,6.24162313405724)) ;
#72858 = CARTESIAN_POINT('Ctrl Pts',(78.7988258701155,236.12158097562,6.23533844570994)) ;
#72859 = CARTESIAN_POINT('Ctrl Pts',(78.8093087363274,236.142390177217,6.22836797631217)) ;
#72860 = CARTESIAN_POINT('Ctrl Pts',(78.8208448817506,236.163215179485,6.22295430296987)) ;
#72861 = CARTESIAN_POINT('Ctrl Pts',(78.833312267638,236.183805435466,6.21921733601531)) ;
#72862 = CARTESIAN_POINT('Ctrl Pts',(78.835433049314,236.187307969035,6.21858165415606)) ;
#72863 = CARTESIAN_POINT('Ctrl Pts',(78.8375808814211,236.190803721444,6.21799455781567)) ;
#72864 = CARTESIAN_POINT('Ctrl Pts',(78.8397552889646,236.194291466072,6.21745672558774)) ;
#72865 = CARTESIAN_POINT('Ctrl Pts',(78.8511839473342,236.21262300744,6.21462988624397)) ;
#72866 = CARTESIAN_POINT('Ctrl Pts',(78.863348221106,236.230737357873,6.21316350919955)) ;
#72867 = CARTESIAN_POINT('Ctrl Pts',(78.8761748005146,236.248408354793,6.21318609107912)) ;
#72868 = CARTESIAN_POINT('Ctrl Pts',(78.8873264039381,236.263771761004,6.21320572407383)) ;
#72869 = CARTESIAN_POINT('Ctrl Pts',(78.8990111727565,236.278780648428,6.21441157326701)) ;
#72870 = CARTESIAN_POINT('Ctrl Pts',(78.9111460827114,236.293170722242,6.21693629918754)) ;
#72871 = CARTESIAN_POINT('Ctrl Pts',(78.911966469022,236.294143569968,6.21710698447412)) ;
#72872 = CARTESIAN_POINT('Ctrl Pts',(78.9127889012084,236.295113579268,6.2172836850705)) ;
#72873 = CARTESIAN_POINT('Ctrl Pts',(78.9136133487335,236.296080664322,6.21746643634462)) ;
#72874 = CARTESIAN_POINT('Ctrl Pts',(78.9220291325022,236.30595246143,6.21933192221197)) ;
#72875 = CARTESIAN_POINT('Ctrl Pts',(78.9305921718208,236.315577536009,6.22169251234177)) ;
#72876 = CARTESIAN_POINT('Ctrl Pts',(78.9393008450243,236.324904604269,6.22458831777945)) ;
#72877 = CARTESIAN_POINT('Ctrl Pts',(78.9508383577829,236.337261385438,6.22842476810926)) ;
#72878 = CARTESIAN_POINT('Ctrl Pts',(78.962631711809,236.349096349494,6.2332000270552)) ;
#72879 = CARTESIAN_POINT('Ctrl Pts',(78.9745203159935,236.360382813319,6.23871136073391)) ;
#72880 = CARTESIAN_POINT('Ctrl Pts',(78.9868854803053,236.3721217002,6.24444361873968)) ;
#72881 = CARTESIAN_POINT('Ctrl Pts',(78.9994585165609,236.3833129496,6.25106940511979)) ;
#72882 = CARTESIAN_POINT('Ctrl Pts',(79.0120245851066,236.393931577287,6.25830798208034)) ;
#72883 = CARTESIAN_POINT('Ctrl Pts',(79.0300218321948,236.409139680403,6.26867514326938)) ;
#72884 = CARTESIAN_POINT('Ctrl Pts',(79.0480035991304,236.423170593099,6.28029815534635)) ;
#72885 = CARTESIAN_POINT('Ctrl Pts',(79.0659499208125,236.436074634652,6.29304730407198)) ;
#72886 = CARTESIAN_POINT('Ctrl Pts',(79.072489055785,236.440776504534,6.29769273536301)) ;
#72887 = CARTESIAN_POINT('Ctrl Pts',(79.0790236250942,236.4453292415,6.30248751787712)) ;
#72888 = CARTESIAN_POINT('Ctrl Pts',(79.0855531046979,236.449736852335,6.30742486590055)) ;
#72889 = CARTESIAN_POINT('Ctrl Pts',(79.1021814237119,236.460961507822,6.31999857820217)) ;
#72890 = CARTESIAN_POINT('Ctrl Pts',(79.1187759968485,236.471243033782,6.33349711463422)) ;
#72891 = CARTESIAN_POINT('Ctrl Pts',(79.1352093243399,236.480719199796,6.34759111950266)) ;
#72892 = CARTESIAN_POINT('Ctrl Pts',(79.1429558612837,236.485186187395,6.3542349187854)) ;
#72893 = CARTESIAN_POINT('Ctrl Pts',(79.1506774590654,236.489471680698,6.36102802685583)) ;
#72894 = CARTESIAN_POINT('Ctrl Pts',(79.1583626862522,236.493587078316,6.36794168881472)) ;
#72895 = CARTESIAN_POINT('Ctrl Pts',(79.1908862082282,236.511003248537,6.3971999828363)) ;
#72896 = CARTESIAN_POINT('Ctrl Pts',(79.2227594884558,236.525367080393,6.42861634230867)) ;
#72897 = CARTESIAN_POINT('Ctrl Pts',(79.2539716103905,236.537251601533,6.46147697523877)) ;
#72898 = CARTESIAN_POINT('Ctrl Pts',(79.2687761578396,236.542888672844,6.47706344515064)) ;
#72899 = CARTESIAN_POINT('Ctrl Pts',(79.283431735008,236.547969053286,6.49297500336267)) ;
#72900 = CARTESIAN_POINT('Ctrl Pts',(79.2979360861574,236.552559031693,6.50913659697102)) ;
#72901 = CARTESIAN_POINT('Ctrl Pts',(79.31936721735,236.559341026172,6.5330164127128)) ;
#72902 = CARTESIAN_POINT('Ctrl Pts',(79.3404681642074,236.565051995616,6.55744194205068)) ;
#72903 = CARTESIAN_POINT('Ctrl Pts',(79.3612470116278,236.569837451894,6.58226166137312)) ;
#72904 = CARTESIAN_POINT('Ctrl Pts',(79.3841739753656,236.575117628428,6.60964724216949)) ;
#72905 = CARTESIAN_POINT('Ctrl Pts',(79.4067236213163,236.579243111831,6.63755577298641)) ;
#72906 = CARTESIAN_POINT('Ctrl Pts',(79.4289017391005,236.582396378662,6.66580373102021)) ;
#72907 = CARTESIAN_POINT('Ctrl Pts',(79.46756525416,236.58789352593,6.71504890869803)) ;
#72908 = CARTESIAN_POINT('Ctrl Pts',(79.5050989743834,236.590433394674,6.76532386095455)) ;
#72909 = CARTESIAN_POINT('Ctrl Pts',(79.5415950952572,236.590390900578,6.81629650876979)) ;
#72910 = CARTESIAN_POINT('Ctrl Pts',(79.5452891117263,236.590386599466,6.82145579134549)) ;
#72911 = CARTESIAN_POINT('Ctrl Pts',(79.5489724693669,236.590355875279,6.82662222168512)) ;
#72912 = CARTESIAN_POINT('Ctrl Pts',(79.5526452455199,236.590299138915,6.83179545544048)) ;
#72913 = CARTESIAN_POINT('Ctrl Pts',(79.5905217161694,236.589714030228,6.88514578999395)) ;
#72914 = CARTESIAN_POINT('Ctrl Pts',(79.6272756492694,236.586360149865,6.93921965527791)) ;
#72915 = CARTESIAN_POINT('Ctrl Pts',(79.6630047438853,236.580717651161,6.99367465948525)) ;
#72916 = CARTESIAN_POINT('Ctrl Pts',(79.6649692503233,236.580407407503,6.99666877975323)) ;
#72917 = CARTESIAN_POINT('Ctrl Pts',(79.6669306534082,236.58009025687,6.99966405226983)) ;
#72918 = CARTESIAN_POINT('Ctrl Pts',(79.6688889677733,236.579766283224,7.00266042012122)) ;
#72919 = CARTESIAN_POINT('Ctrl Pts',(79.6985906537757,236.574852586182,7.04810622731801)) ;
#72920 = CARTESIAN_POINT('Ctrl Pts',(79.727564960678,236.568303432379,7.09382942892827)) ;
#72921 = CARTESIAN_POINT('Ctrl Pts',(79.7558180615633,236.560235350949,7.13971368291887)) ;
#72922 = CARTESIAN_POINT('Ctrl Pts',(79.7625790427186,236.558304655033,7.15069380781977)) ;
#72923 = CARTESIAN_POINT('Ctrl Pts',(79.7692985406671,236.556286837037,7.16168309137831)) ;
#72924 = CARTESIAN_POINT('Ctrl Pts',(79.775976296469,236.554183244321,7.17267980084166)) ;
#72925 = CARTESIAN_POINT('Ctrl Pts',(79.5657826988647,236.44459798751,7.27867958886636)) ;
#72926 = CARTESIAN_POINT('Ctrl Pts',(79.4870812400902,236.469851175839,7.10540671867988)) ;
#72927 = CARTESIAN_POINT('Ctrl Pts',(79.3728626924325,236.484513827223,6.87572289449329)) ;
#72928 = CARTESIAN_POINT('Ctrl Pts',(79.2109449345459,236.451622856973,6.61251963169561)) ;
#72929 = CARTESIAN_POINT('Ctrl Pts',(79.1249080993041,236.417892181793,6.49309973646919)) ;
#72930 = CARTESIAN_POINT('Ctrl Pts',(79.0530360354225,236.376359946734,6.41122239160556)) ;
#72931 = CARTESIAN_POINT('Ctrl Pts',(78.9990126464368,236.336361861471,6.36192444560416)) ;
#72932 = CARTESIAN_POINT('Ctrl Pts',(78.908445191216,236.253354919289,6.30168466926149)) ;
#72933 = CARTESIAN_POINT('Ctrl Pts',(78.8233604283728,236.115133957597,6.33246528275406)) ;
#72934 = CARTESIAN_POINT('Ctrl Pts',(78.7867646631746,235.969017367392,6.46981689000949)) ;
#72935 = CARTESIAN_POINT('Ctrl Pts',(78.7776026491497,235.821285683305,6.66032500142642)) ;
#72936 = CARTESIAN_POINT('Ctrl Pts',(78.8104263003458,235.66713514265,6.93427995946187)) ;
#72937 = CARTESIAN_POINT('Ctrl Pts',(78.8635464513941,235.567087660364,7.16318512434001)) ;
#72938 = CARTESIAN_POINT('Ctrl Pts',(78.8957655188746,235.522398454586,7.27867958884211)) ;
#72939 = CARTESIAN_POINT('Origin',(78.7335324267296,235.405435110699,16.0213203435596)) ;
#72940 = CARTESIAN_POINT('',(78.8957655188746,235.522398454586,16.0254384350469)) ;
#72941 = CARTESIAN_POINT('',(78.8957655188746,235.522398454586,16.0213203435596)) ;
#72942 = CARTESIAN_POINT('Ctrl Pts',(78.8957655188746,235.522398454586,16.0254384350468)) ;
#72943 = CARTESIAN_POINT('Ctrl Pts',(78.9074705870995,235.506163031172,16.0294645582753)) ;
#72944 = CARTESIAN_POINT('Ctrl Pts',(78.9162378160954,235.488874504924,16.0362204083692)) ;
#72945 = CARTESIAN_POINT('Ctrl Pts',(78.9302389974868,235.448785866273,16.056050217191)) ;
#72946 = CARTESIAN_POINT('Ctrl Pts',(78.9336083803761,235.426160755234,16.070223718736)) ;
#72947 = CARTESIAN_POINT('Ctrl Pts',(78.9334374035686,235.378695066669,16.1046945816759)) ;
#72948 = CARTESIAN_POINT('Ctrl Pts',(78.9282920188754,235.354099131457,16.1258672215769)) ;
#72949 = CARTESIAN_POINT('Ctrl Pts',(78.9102244776702,235.308359032661,16.1708720249647)) ;
#72950 = CARTESIAN_POINT('Ctrl Pts',(78.8966632779222,235.287149572103,16.1951765216822)) ;
#72951 = CARTESIAN_POINT('Ctrl Pts',(78.8794692237515,235.26867652585,16.2199877856675)) ;
#72952 = CARTESIAN_POINT('Ctrl Pts',(78.8790049966168,235.2681828224,16.2206540664845)) ;
#72953 = CARTESIAN_POINT('Ctrl Pts',(78.8785382749251,235.267691493827,16.2213203435596)) ;
#72954 = CARTESIAN_POINT('Origin',(73.474255491572,233.696592446523,16.0213203435596)) ;
#72955 = CARTESIAN_POINT('',(73.2742568343815,233.69585956045,16.0254384350468)) ;
#72956 = CARTESIAN_POINT('',(73.2742568343815,233.69585956045,16.0213203435596)) ;
#72957 = CARTESIAN_POINT('Ctrl Pts',(73.4379069626932,233.499923220541,16.2213203435596)) ;
#72958 = CARTESIAN_POINT('Ctrl Pts',(73.4372405812046,233.500046381583,16.2206540664654)) ;
#72959 = CARTESIAN_POINT('Ctrl Pts',(73.4365748219496,233.500172930202,16.2199877856881)) ;
#72960 = CARTESIAN_POINT('Ctrl Pts',(73.4155453396356,233.50428110497,16.1989219658443)) ;
#72961 = CARTESIAN_POINT('Ctrl Pts',(73.3956762915721,233.511452628349,16.1784289743521)) ;
#72962 = CARTESIAN_POINT('Ctrl Pts',(73.3593789232627,233.531623989932,16.1396302535154)) ;
#72963 = CARTESIAN_POINT('Ctrl Pts',(73.3426362659354,233.544456831755,16.1210537744657)) ;
#72964 = CARTESIAN_POINT('Ctrl Pts',(73.3122963096875,233.57704221544,16.0855257632981)) ;
#72965 = CARTESIAN_POINT('Ctrl Pts',(73.2987314270749,233.597369350878,16.0684876094865)) ;
#72966 = CARTESIAN_POINT('Ctrl Pts',(73.2818489952434,233.638752838189,16.0440628922432)) ;
#72967 = CARTESIAN_POINT('Ctrl Pts',(73.2768470238562,233.65827800357,16.0353723462229)) ;
#72968 = CARTESIAN_POINT('Ctrl Pts',(73.2745340907024,233.684665512636,16.027919277051)) ;
#72969 = CARTESIAN_POINT('Ctrl Pts',(73.2742773990004,233.690247642977,16.0265673132454)) ;
#72970 = CARTESIAN_POINT('Ctrl Pts',(73.2742568343815,233.69585956045,16.0254384350468)) ;
#72971 = CARTESIAN_POINT('Origin',(74.5283628290597,239.4,7.2786795888419)) ;
#72972 = CARTESIAN_POINT('Origin',(74.5283628290597,239.4,7.17267980084126)) ;
#72973 = CARTESIAN_POINT('Origin',(79.6268886667016,236.635034487937,16.0213203435596)) ;
#72974 = CARTESIAN_POINT('',(79.5657826988536,236.444597987514,16.0254384350469)) ;
#72975 = CARTESIAN_POINT('',(79.5657826988536,236.444597987514,16.0213203435596)) ;
#72976 = CARTESIAN_POINT('Ctrl Pts',(79.8026999024824,236.53969084959,16.2213203435596)) ;
#72977 = CARTESIAN_POINT('Ctrl Pts',(79.802376846175,236.539095142004,16.2206540664836)) ;
#72978 = CARTESIAN_POINT('Ctrl Pts',(79.8020507603675,236.538501073009,16.2199877856673)) ;
#72979 = CARTESIAN_POINT('Ctrl Pts',(79.7916451864779,236.519770342471,16.1989219660218)) ;
#72980 = CARTESIAN_POINT('Ctrl Pts',(79.7786847889848,236.503089877563,16.1784289743296)) ;
#72981 = CARTESIAN_POINT('Ctrl Pts',(79.7482841804216,236.474802322421,16.1396302534665)) ;
#72982 = CARTESIAN_POINT('Ctrl Pts',(79.7309056569223,236.462844675276,16.1210537744064)) ;
#72983 = CARTESIAN_POINT('Ctrl Pts',(79.6905395533259,236.444059099522,16.0855257632409)) ;
#72984 = CARTESIAN_POINT('Ctrl Pts',(79.6670155194585,236.437439559828,16.0684876094397)) ;
#72985 = CARTESIAN_POINT('Ctrl Pts',(79.6224405258492,236.434171613905,16.0440628922132)) ;
#72986 = CARTESIAN_POINT('Ctrl Pts',(79.6023252959214,236.43544806435,16.0353723461999)) ;
#72987 = CARTESIAN_POINT('Ctrl Pts',(79.5765145478479,236.441402522945,16.0279192770416)) ;
#72988 = CARTESIAN_POINT('Ctrl Pts',(79.5711263043329,236.442883367765,16.0265673132415)) ;
#72989 = CARTESIAN_POINT('Ctrl Pts',(79.5657826988536,236.444597987514,16.0254384350468)) ;
#72990 = CARTESIAN_POINT('Origin',(74.5283628290597,239.4,16.2213203435596)) ;
#72991 = CARTESIAN_POINT('',(78.8725506972158,235.557080307089,16.0213203435596)) ;
#72992 = CARTESIAN_POINT('Ctrl Pts',(78.8957655188745,235.522398454586,16.0254384350468)) ;
#72993 = CARTESIAN_POINT('Ctrl Pts',(78.8893108232296,235.531351389741,16.0232182514845)) ;
#72994 = CARTESIAN_POINT('Ctrl Pts',(78.8829899514931,235.540642081367,16.0218983740811)) ;
#72995 = CARTESIAN_POINT('Ctrl Pts',(78.8754205773507,235.552487135842,16.0213707571522)) ;
#72996 = CARTESIAN_POINT('Ctrl Pts',(78.8739772719456,235.554779827169,16.0213203435596)) ;
#72997 = CARTESIAN_POINT('Ctrl Pts',(78.8725506972157,235.557080307089,16.0213203435596)) ;
#72998 = CARTESIAN_POINT('',(79.5256245226196,236.455959313107,16.0213203435596)) ;
#72999 = CARTESIAN_POINT('Origin',(74.5283628290597,239.4,16.0213203435596)) ;
#73000 = CARTESIAN_POINT('Ctrl Pts',(79.5256245226197,236.455959313107,16.0213203435596)) ;
#73001 = CARTESIAN_POINT('Ctrl Pts',(79.5365793331501,236.453267763066,16.0213203435596)) ;
#73002 = CARTESIAN_POINT('Ctrl Pts',(79.5474616517457,236.450264794855,16.0221950109068)) ;
#73003 = CARTESIAN_POINT('Ctrl Pts',(79.560731310064,236.446200502444,16.0244263118334)) ;
#73004 = CARTESIAN_POINT('Ctrl Pts',(79.5632664280307,236.445405391366,16.0249068532759)) ;
#73005 = CARTESIAN_POINT('Ctrl Pts',(79.5657826988536,236.444597987514,16.0254384350468)) ;
#73006 = CARTESIAN_POINT('Origin',(72.0287747312355,234.166257616082,16.0213203435596)) ;
#73007 = CARTESIAN_POINT('',(72.1901462641291,234.048108437619,16.0254384350468)) ;
#73008 = CARTESIAN_POINT('',(72.1901462641291,234.048108437619,16.0213203435596)) ;
#73009 = CARTESIAN_POINT('Ctrl Pts',(72.1901462641291,234.048108437619,16.0254384350468)) ;
#73010 = CARTESIAN_POINT('Ctrl Pts',(72.1783225238984,234.031959234464,16.0294645582753)) ;
#73011 = CARTESIAN_POINT('Ctrl Pts',(72.1645893811064,234.018278655779,16.0362204083691)) ;
#73012 = CARTESIAN_POINT('Ctrl Pts',(72.1307894230788,233.992574670357,16.056050217191)) ;
#73013 = CARTESIAN_POINT('Ctrl Pts',(72.1103128603666,233.982378652993,16.0702237187361)) ;
#73014 = CARTESIAN_POINT('Ctrl Pts',(72.0651174732175,233.967873557184,16.1046945816758)) ;
#73015 = CARTESIAN_POINT('Ctrl Pts',(72.0401353374473,233.965166546852,16.1258672215766)) ;
#73016 = CARTESIAN_POINT('Ctrl Pts',(71.9910507411521,233.968215331796,16.1708720249644)) ;
#73017 = CARTESIAN_POINT('Ctrl Pts',(71.9666887043084,233.974558715426,16.1951765216982)) ;
#73018 = CARTESIAN_POINT('Ctrl Pts',(71.9438065383368,233.985202747463,16.2199877856666)) ;
#73019 = CARTESIAN_POINT('Ctrl Pts',(71.9431935443829,233.985491690948,16.2206540664842)) ;
#73020 = CARTESIAN_POINT('Ctrl Pts',(71.942582038207,233.985783740775,16.2213203435596)) ;
#73021 = CARTESIAN_POINT('Origin',(74.5283628290597,239.4,16.2213203435596)) ;
#73022 = CARTESIAN_POINT('',(72.2159568915352,234.080904326852,16.0213203435596)) ;
#73023 = CARTESIAN_POINT('Ctrl Pts',(72.1901462641291,234.048108437619,16.0254384350468)) ;
#73024 = CARTESIAN_POINT('Ctrl Pts',(72.1966664008005,234.057013827085,16.0232182514845)) ;
#73025 = CARTESIAN_POINT('Ctrl Pts',(72.2035491168268,234.065896314941,16.0218983740811)) ;
#73026 = CARTESIAN_POINT('Ctrl Pts',(72.2124753678236,234.076755540675,16.0213707571522)) ;
#73027 = CARTESIAN_POINT('Ctrl Pts',(72.2142098409518,234.078836686269,16.0213203435596)) ;
#73028 = CARTESIAN_POINT('Ctrl Pts',(72.2159568915352,234.080904326852,16.0213203435596)) ;
#73029 = CARTESIAN_POINT('',(73.2726525382014,233.737563098327,16.0213203435596)) ;
#73030 = CARTESIAN_POINT('Origin',(74.5283628290597,239.4,16.0213203435596)) ;
#73031 = CARTESIAN_POINT('Ctrl Pts',(73.2726525382014,233.737563098327,16.0213203435596)) ;
#73032 = CARTESIAN_POINT('Ctrl Pts',(73.2734779446195,233.726312719683,16.0213203435596)) ;
#73033 = CARTESIAN_POINT('Ctrl Pts',(73.2739847735191,233.71503505146,16.0221950109068)) ;
#73034 = CARTESIAN_POINT('Ctrl Pts',(73.2742199516675,233.701158921022,16.0244263118334)) ;
#73035 = CARTESIAN_POINT('Ctrl Pts',(73.2742471506295,233.698502177724,16.0249068532759)) ;
#73036 = CARTESIAN_POINT('Ctrl Pts',(73.2742568343815,233.69585956045,16.0254384350468)) ;
#73037 = CARTESIAN_POINT('Ctrl Pts',(80.2332466613993,238.145896286595,7.28036629650082)) ;
#73038 = CARTESIAN_POINT('Ctrl Pts',(80.1779056493182,238.145761083795,7.16431451492221)) ;
#73039 = CARTESIAN_POINT('Ctrl Pts',(80.0654939997404,238.13039472435,6.93452072658987)) ;
#73040 = CARTESIAN_POINT('Ctrl Pts',(79.921484160325,238.065724505406,6.66105185594091)) ;
#73041 = CARTESIAN_POINT('Ctrl Pts',(79.8070585153582,237.972192585025,6.46924290901652)) ;
#73042 = CARTESIAN_POINT('Ctrl Pts',(79.7385408827141,237.888743471261,6.37322093548194)) ;
#73043 = CARTESIAN_POINT('Ctrl Pts',(79.6911769183589,237.803443935991,6.32731325641336)) ;
#73044 = CARTESIAN_POINT('Ctrl Pts',(79.6626235218602,237.731818472063,6.31494132977146)) ;
#73045 = CARTESIAN_POINT('Ctrl Pts',(79.6436095797225,237.657062576281,6.32730080160491)) ;
#73046 = CARTESIAN_POINT('Ctrl Pts',(79.6317837391258,237.560234835217,6.37317692639864)) ;
#73047 = CARTESIAN_POINT('Ctrl Pts',(79.638186797208,237.452382843011,6.46930294056729)) ;
#73048 = CARTESIAN_POINT('Ctrl Pts',(79.6757637756622,237.309451563678,6.66107036149359)) ;
#73049 = CARTESIAN_POINT('Ctrl Pts',(79.7542618476727,237.17249003623,6.93454557156964)) ;
#73050 = CARTESIAN_POINT('Ctrl Pts',(79.8361608473108,237.093983531712,7.16431122291373)) ;
#73051 = CARTESIAN_POINT('Ctrl Pts',(79.8808544858649,237.061344621366,7.28036634298531)) ;
#73052 = CARTESIAN_POINT('Ctrl Pts',(80.2787215482779,238.145985700087,7.25145031090427)) ;
#73053 = CARTESIAN_POINT('Ctrl Pts',(80.2205756685247,238.150146686166,7.13668815450591)) ;
#73054 = CARTESIAN_POINT('Ctrl Pts',(80.1008696697319,238.141739542913,6.90908133772489)) ;
#73055 = CARTESIAN_POINT('Ctrl Pts',(79.9446522226815,238.080894675372,6.6376698933697)) ;
#73056 = CARTESIAN_POINT('Ctrl Pts',(79.8195172933758,237.985666275976,6.44712617479323)) ;
#73057 = CARTESIAN_POINT('Ctrl Pts',(79.7445014978107,237.898473504043,6.35169067773445)) ;
#73058 = CARTESIAN_POINT('Ctrl Pts',(79.692949166172,237.808172185119,6.30605438286228)) ;
#73059 = CARTESIAN_POINT('Ctrl Pts',(79.6622096829835,237.731957089376,6.29375467249613)) ;
#73060 = CARTESIAN_POINT('Ctrl Pts',(79.6422616441879,237.652190302909,6.30604200388241)) ;
#73061 = CARTESIAN_POINT('Ctrl Pts',(79.6308854350235,237.548863326753,6.35164689420351)) ;
#73062 = CARTESIAN_POINT('Ctrl Pts',(79.6403413094888,237.434133119528,6.44718596070129)) ;
#73063 = CARTESIAN_POINT('Ctrl Pts',(79.6855942151938,237.28356807379,6.63768828531303)) ;
#73064 = CARTESIAN_POINT('Ctrl Pts',(79.7762110553406,237.142507839417,6.90910610037119)) ;
#73065 = CARTESIAN_POINT('Ctrl Pts',(79.8681037039669,237.065354698581,7.13668489810488)) ;
#73066 = CARTESIAN_POINT('Ctrl Pts',(79.9175918880526,237.034542816821,7.25145035687956)) ;
#73067 = CARTESIAN_POINT('Ctrl Pts',(80.3576208772263,238.186433078335,7.2012216783622)) ;
#73068 = CARTESIAN_POINT('Ctrl Pts',(80.2910222038791,238.19295252776,7.0885508192026)) ;
#73069 = CARTESIAN_POINT('Ctrl Pts',(80.1541383715028,238.186858411812,6.86454783277039)) ;
#73070 = CARTESIAN_POINT('Ctrl Pts',(79.9760850814639,238.121396473258,6.59660334624683)) ;
#73071 = CARTESIAN_POINT('Ctrl Pts',(79.8340166470322,238.016395912876,6.40822171016601)) ;
#73072 = CARTESIAN_POINT('Ctrl Pts',(79.7491197147048,237.919514622506,6.3137962441714)) ;
#73073 = CARTESIAN_POINT('Ctrl Pts',(79.6910247264725,237.818879034461,6.26862916485266)) ;
#73074 = CARTESIAN_POINT('Ctrl Pts',(79.6565506977968,237.733801201014,6.25645441418595)) ;
#73075 = CARTESIAN_POINT('Ctrl Pts',(79.6344168175111,237.644678443685,6.26861687996125)) ;
#73076 = CARTESIAN_POINT('Ctrl Pts',(79.6222554874394,237.529139719225,6.31375285214006)) ;
#73077 = CARTESIAN_POINT('Ctrl Pts',(79.6340236296205,237.400781569794,6.40828085240387)) ;
#73078 = CARTESIAN_POINT('Ctrl Pts',(79.6872152287998,237.232315543738,6.59662176807364)) ;
#73079 = CARTESIAN_POINT('Ctrl Pts',(79.7927919971073,237.074708318493,6.86457238457136)) ;
#73080 = CARTESIAN_POINT('Ctrl Pts',(79.8999352530856,236.989316632693,7.08854762092014)) ;
#73081 = CARTESIAN_POINT('Ctrl Pts',(79.9576484170219,236.955444337705,7.20122172350898)) ;
#73082 = CARTESIAN_POINT('Ctrl Pts',(80.3943740298942,238.275157533004,7.17771948055087)) ;
#73083 = CARTESIAN_POINT('Ctrl Pts',(80.3217995712605,238.27685019025,7.06324269887043)) ;
#73084 = CARTESIAN_POINT('Ctrl Pts',(80.1739876651028,238.259964231434,6.83622602504918)) ;
#73085 = CARTESIAN_POINT('Ctrl Pts',(79.9838492644881,238.177623628403,6.56553634319181)) ;
#73086 = CARTESIAN_POINT('Ctrl Pts',(79.8324519761851,238.055644168661,6.37550114619807)) ;
#73087 = CARTESIAN_POINT('Ctrl Pts',(79.7417046853161,237.945935908136,6.2803204097403)) ;
#73088 = CARTESIAN_POINT('Ctrl Pts',(79.6789846091568,237.833401386599,6.23480589058125)) ;
#73089 = CARTESIAN_POINT('Ctrl Pts',(79.6412127236151,237.738789039827,6.22253899168853)) ;
#73090 = CARTESIAN_POINT('Ctrl Pts',(79.6161413587739,237.64001091775,6.23479354036237)) ;
#73091 = CARTESIAN_POINT('Ctrl Pts',(79.6007280971451,237.512129301313,6.28027674251987)) ;
#73092 = CARTESIAN_POINT('Ctrl Pts',(79.6096888129855,237.369948564794,6.37556075156494)) ;
#73093 = CARTESIAN_POINT('Ctrl Pts',(79.6604473857773,237.182263486407,6.56555470566056)) ;
#73094 = CARTESIAN_POINT('Ctrl Pts',(79.7658801251764,237.003897576842,6.83625071485809)) ;
#73095 = CARTESIAN_POINT('Ctrl Pts',(79.8755208020787,236.903351717062,7.06323945062391)) ;
#73096 = CARTESIAN_POINT('Ctrl Pts',(79.935231416945,236.862061782038,7.1777195264114)) ;
#73097 = CARTESIAN_POINT('Ctrl Pts',(80.3996002740789,238.315077942443,7.17433670364794)) ;
#73098 = CARTESIAN_POINT('Ctrl Pts',(80.325736250402,238.314513145266,7.05828625130696)) ;
#73099 = CARTESIAN_POINT('Ctrl Pts',(80.1755857959063,238.292645299654,6.82849471713331)) ;
#73100 = CARTESIAN_POINT('Ctrl Pts',(79.9827966599848,238.202695250306,6.55502796713346)) ;
#73101 = CARTESIAN_POINT('Ctrl Pts',(79.8290739463553,238.073144136735,6.36322032432285)) ;
#73102 = CARTESIAN_POINT('Ctrl Pts',(79.7366319322547,237.957784921701,6.26719895529102)) ;
#73103 = CARTESIAN_POINT('Ctrl Pts',(79.6723150856581,237.84008129077,6.22129155594843)) ;
#73104 = CARTESIAN_POINT('Ctrl Pts',(79.6332390648588,237.741381732928,6.20891970374262)) ;
#73105 = CARTESIAN_POINT('Ctrl Pts',(79.6068193628199,237.638527187785,6.22127910121813)) ;
#73106 = CARTESIAN_POINT('Ctrl Pts',(79.5896603331735,237.505527120618,6.26715494644022)) ;
#73107 = CARTESIAN_POINT('Ctrl Pts',(79.5966681821472,237.357772061383,6.36328035562036)) ;
#73108 = CARTESIAN_POINT('Ctrl Pts',(79.6448593894507,237.162600361155,6.55504647256913)) ;
#73109 = CARTESIAN_POINT('Ctrl Pts',(79.7479629649841,236.976517066737,6.82851956202821)) ;
#73110 = CARTESIAN_POINT('Ctrl Pts',(79.8565679236955,236.870567902859,7.05828295933517)) ;
#73111 = CARTESIAN_POINT('Ctrl Pts',(79.9159949092403,236.826693582052,7.17433675013192)) ;
#73112 = CARTESIAN_POINT('Ctrl Pts',(79.9151467531554,236.82732064467,7.17267980084143)) ;
#73113 = CARTESIAN_POINT('Ctrl Pts',(79.8560499536753,236.871073595961,7.05718689587997)) ;
#73114 = CARTESIAN_POINT('Ctrl Pts',(79.7477661218197,236.976872333025,6.82799745299379)) ;
#73115 = CARTESIAN_POINT('Ctrl Pts',(79.6448593894507,237.162600361155,6.55504647256913)) ;
#73116 = CARTESIAN_POINT('Ctrl Pts',(79.5966681821471,237.357772061383,6.36328035562036)) ;
#73117 = CARTESIAN_POINT('Ctrl Pts',(79.5896603331735,237.505527120618,6.26715494644023)) ;
#73118 = CARTESIAN_POINT('Ctrl Pts',(79.6068193628199,237.638527187785,6.22127910121812)) ;
#73119 = CARTESIAN_POINT('Ctrl Pts',(79.6332390648588,237.741381732928,6.20891970374263)) ;
#73120 = CARTESIAN_POINT('Ctrl Pts',(79.672315085658,237.84008129077,6.22129155594842)) ;
#73121 = CARTESIAN_POINT('Ctrl Pts',(79.7366319322548,237.9577849217,6.26719895529104)) ;
#73122 = CARTESIAN_POINT('Ctrl Pts',(79.8290739463553,238.073144136735,6.36322032432284)) ;
#73123 = CARTESIAN_POINT('Ctrl Pts',(79.9827966599849,238.202695250307,6.55502796713348)) ;
#73124 = CARTESIAN_POINT('Ctrl Pts',(80.1752177269682,238.292473568924,6.82797262020198)) ;
#73125 = CARTESIAN_POINT('Ctrl Pts',(80.325019908484,238.314408535778,7.05719005380891)) ;
#73126 = CARTESIAN_POINT('Ctrl Pts',(80.398545552619,238.31506917167,7.17267980084126)) ;
#73127 = CARTESIAN_POINT('Ctrl Pts',(80.232503268608,238.145894005322,7.27867958883789)) ;
#73128 = CARTESIAN_POINT('Ctrl Pts',(80.2105890887182,238.145813701796,7.2327390460971)) ;
#73129 = CARTESIAN_POINT('Ctrl Pts',(80.1885289438461,238.144536258816,7.1869379140836)) ;
#73130 = CARTESIAN_POINT('Ctrl Pts',(80.1663213133667,238.141988707811,7.14139165811073)) ;
#73131 = CARTESIAN_POINT('Ctrl Pts',(80.1449425970939,238.139536245799,7.09754544567358)) ;
#73132 = CARTESIAN_POINT('Ctrl Pts',(80.1234263498375,238.135906341529,7.05393543754444)) ;
#73133 = CARTESIAN_POINT('Ctrl Pts',(80.1017950450755,238.130992693427,7.01066464617939)) ;
#73134 = CARTESIAN_POINT('Ctrl Pts',(80.0894090875243,238.128179167498,6.98588804620328)) ;
#73135 = CARTESIAN_POINT('Ctrl Pts',(80.0769859110699,238.124944008106,6.96122266319468)) ;
#73136 = CARTESIAN_POINT('Ctrl Pts',(80.0645351246606,238.121261622656,6.93668783599072)) ;
#73137 = CARTESIAN_POINT('Ctrl Pts',(80.0470380349159,238.116086766502,6.9022090441019)) ;
#73138 = CARTESIAN_POINT('Ctrl Pts',(80.0295043160675,238.110037081132,6.86798808269392)) ;
#73139 = CARTESIAN_POINT('Ctrl Pts',(80.0119134699705,238.103002425664,6.83420441808968)) ;
#73140 = CARTESIAN_POINT('Ctrl Pts',(79.9948101708734,238.096162742351,6.80135709982332)) ;
#73141 = CARTESIAN_POINT('Ctrl Pts',(79.9776522080704,238.088391577647,6.76892317408853)) ;
#73142 = CARTESIAN_POINT('Ctrl Pts',(79.9604560297924,238.079554466258,6.73706759473268)) ;
#73143 = CARTESIAN_POINT('Ctrl Pts',(79.9440162918452,238.071106089352,6.70661330609378)) ;
#73144 = CARTESIAN_POINT('Ctrl Pts',(79.9275411472763,238.061682998992,6.6766876013464)) ;
#73145 = CARTESIAN_POINT('Ctrl Pts',(79.9110856389802,238.051143022085,6.64743460946756)) ;
#73146 = CARTESIAN_POINT('Ctrl Pts',(79.9050048912538,238.04724822045,6.636624851382)) ;
#73147 = CARTESIAN_POINT('Ctrl Pts',(79.8989272739401,238.043200693744,6.62590695216758)) ;
#73148 = CARTESIAN_POINT('Ctrl Pts',(79.8928572709278,238.038992579685,6.61528818440181)) ;
#73149 = CARTESIAN_POINT('Ctrl Pts',(79.8785195831937,238.029052778139,6.5902060590653)) ;
#73150 = CARTESIAN_POINT('Ctrl Pts',(79.8642201091082,238.018219074385,6.56567701872138)) ;
#73151 = CARTESIAN_POINT('Ctrl Pts',(79.8499884620884,238.006327778712,6.54202098106688)) ;
#73152 = CARTESIAN_POINT('Ctrl Pts',(79.8369505446297,237.995433907381,6.52034917695921)) ;
#73153 = CARTESIAN_POINT('Ctrl Pts',(79.8239694641037,237.983651754103,6.49941006528887)) ;
#73154 = CARTESIAN_POINT('Ctrl Pts',(79.81111401836,237.970837186803,6.4794496247295)) ;
#73155 = CARTESIAN_POINT('Ctrl Pts',(79.8099369955991,237.969663906803,6.47762208072021)) ;
#73156 = CARTESIAN_POINT('Ctrl Pts',(79.8087610611517,237.968481962524,6.47580274083484)) ;
#73157 = CARTESIAN_POINT('Ctrl Pts',(79.8075862896947,237.967291237912,6.47399179386844)) ;
#73158 = CARTESIAN_POINT('Ctrl Pts',(79.7946368721481,237.954165969941,6.45402986145733)) ;
#73159 = CARTESIAN_POINT('Ctrl Pts',(79.7818294946238,237.939978518983,6.43508770960375)) ;
#73160 = CARTESIAN_POINT('Ctrl Pts',(79.7693189745583,237.924604658638,6.41771185041663)) ;
#73161 = CARTESIAN_POINT('Ctrl Pts',(79.7573739014043,237.909925661641,6.40112134034855)) ;
#73162 = CARTESIAN_POINT('Ctrl Pts',(79.7456993800576,237.894164456387,6.38595873692502)) ;
#73163 = CARTESIAN_POINT('Ctrl Pts',(79.734477336668,237.877221681256,6.37269974779979)) ;
#73164 = CARTESIAN_POINT('Ctrl Pts',(79.7320288211619,237.873524970578,6.36980679512248)) ;
#73165 = CARTESIAN_POINT('Ctrl Pts',(79.7296020341664,237.869772065423,6.36700446593625)) ;
#73166 = CARTESIAN_POINT('Ctrl Pts',(79.7271991867293,237.865962041082,6.36429770144624)) ;
#73167 = CARTESIAN_POINT('Ctrl Pts',(79.7179557275126,237.851305345006,6.35388511062318)) ;
#73168 = CARTESIAN_POINT('Ctrl Pts',(79.7090655087212,237.835794327468,6.34488673059512)) ;
#73169 = CARTESIAN_POINT('Ctrl Pts',(79.7007366393481,237.819542094098,6.33775032301849)) ;
#73170 = CARTESIAN_POINT('Ctrl Pts',(79.6978250063942,237.813860586064,6.3352555546962)) ;
#73171 = CARTESIAN_POINT('Ctrl Pts',(79.6949817107896,237.808088873185,6.33298833509643)) ;
#73172 = CARTESIAN_POINT('Ctrl Pts',(79.6922146951874,237.802232977728,6.33096779349927)) ;
#73173 = CARTESIAN_POINT('Ctrl Pts',(79.685607945018,237.788250968276,6.32614338501776)) ;
#73174 = CARTESIAN_POINT('Ctrl Pts',(79.6794383233117,237.773784668057,6.32272529272555)) ;
#73175 = CARTESIAN_POINT('Ctrl Pts',(79.6738226135057,237.759004570215,6.3208188962173)) ;
#73176 = CARTESIAN_POINT('Ctrl Pts',(79.6703584983877,237.749887297038,6.31964291362681)) ;
#73177 = CARTESIAN_POINT('Ctrl Pts',(79.6671043092355,237.740651177896,6.31904215864043)) ;
#73178 = CARTESIAN_POINT('Ctrl Pts',(79.6640785278978,237.731340576308,6.31904136669014)) ;
#73179 = CARTESIAN_POINT('Ctrl Pts',(79.6592031178307,237.716338500596,6.31904009062887)) ;
#73180 = CARTESIAN_POINT('Ctrl Pts',(79.6549226304001,237.701140110227,6.320596471147)) ;
#73181 = CARTESIAN_POINT('Ctrl Pts',(79.6512755675814,237.685946894271,6.32360659801529)) ;
#73182 = CARTESIAN_POINT('Ctrl Pts',(79.6489898975475,237.676425073519,6.32549309054995)) ;
#73183 = CARTESIAN_POINT('Ctrl Pts',(79.6469519912017,237.666905579811,6.3279505740265)) ;
#73184 = CARTESIAN_POINT('Ctrl Pts',(79.6451610148983,237.65743956484,6.33095347029228)) ;
#73185 = CARTESIAN_POINT('Ctrl Pts',(79.6416859636402,237.63907255062,6.33678002334399)) ;
#73186 = CARTESIAN_POINT('Ctrl Pts',(79.6391416762444,237.620904336649,6.34465995043934)) ;
#73187 = CARTESIAN_POINT('Ctrl Pts',(79.6374400792673,237.603154347333,6.35413826247109)) ;
#73188 = CARTESIAN_POINT('Ctrl Pts',(79.636865391497,237.597159566008,6.35733941414242)) ;
#73189 = CARTESIAN_POINT('Ctrl Pts',(79.6363863970514,237.591212363634,6.36072288479166)) ;
#73190 = CARTESIAN_POINT('Ctrl Pts',(79.6359984527991,237.585320745256,6.36427114664549)) ;
#73191 = CARTESIAN_POINT('Ctrl Pts',(79.6346378491189,237.56465757626,6.37671566182321)) ;
#73192 = CARTESIAN_POINT('Ctrl Pts',(79.6343934893251,237.544671891111,6.39118719995713)) ;
#73193 = CARTESIAN_POINT('Ctrl Pts',(79.635052067383,237.525403008395,6.40720016389703)) ;
#73194 = CARTESIAN_POINT('Ctrl Pts',(79.6357409542367,237.505247341453,6.42395006957119)) ;
#73195 = CARTESIAN_POINT('Ctrl Pts',(79.6374174274326,237.485875364109,6.44238654343785)) ;
#73196 = CARTESIAN_POINT('Ctrl Pts',(79.6398737272436,237.467288791444,6.46195381172284)) ;
#73197 = CARTESIAN_POINT('Ctrl Pts',(79.640373191123,237.463509398697,6.46593261906739)) ;
#73198 = CARTESIAN_POINT('Ctrl Pts',(79.6409050234786,237.459762360674,6.46995818152148)) ;
#73199 = CARTESIAN_POINT('Ctrl Pts',(79.641467668486,237.456047520528,6.47402582640356)) ;
#73200 = CARTESIAN_POINT('Ctrl Pts',(79.6441978400383,237.438021676959,6.49376361523447)) ;
#73201 = CARTESIAN_POINT('Ctrl Pts',(79.6476484287426,237.420762531615,6.51449226275907)) ;
#73202 = CARTESIAN_POINT('Ctrl Pts',(79.6516751685792,237.404194825731,6.53597044669148)) ;
#73203 = CARTESIAN_POINT('Ctrl Pts',(79.6558787868921,237.386899367201,6.55839208080987)) ;
#73204 = CARTESIAN_POINT('Ctrl Pts',(79.6607103239457,237.370356714021,6.58163054579619)) ;
#73205 = CARTESIAN_POINT('Ctrl Pts',(79.6660597149526,237.3544664928,6.60541130107295)) ;
#73206 = CARTESIAN_POINT('Ctrl Pts',(79.6668004767532,237.352266079918,6.60870436285804)) ;
#73207 = CARTESIAN_POINT('Ctrl Pts',(79.6675512491336,237.35007816528,6.61200782337307)) ;
#73208 = CARTESIAN_POINT('Ctrl Pts',(79.6683118158661,237.347902472685,6.61532095361514)) ;
#73209 = CARTESIAN_POINT('Ctrl Pts',(79.6749594114975,237.328886226022,6.64427876780854)) ;
#73210 = CARTESIAN_POINT('Ctrl Pts',(79.6823510456142,237.310804268716,6.67397528311282)) ;
#73211 = CARTESIAN_POINT('Ctrl Pts',(79.6903365250355,237.293576196946,6.70426237962481)) ;
#73212 = CARTESIAN_POINT('Ctrl Pts',(79.6985670842247,237.275819383993,6.73547900762635)) ;
#73213 = CARTESIAN_POINT('Ctrl Pts',(79.707428720787,237.258968872542,6.76732302378836)) ;
#73214 = CARTESIAN_POINT('Ctrl Pts',(79.7168128848841,237.242927836814,6.7996322476753)) ;
#73215 = CARTESIAN_POINT('Ctrl Pts',(79.7265781104582,237.226235424926,6.83325344782879)) ;
#73216 = CARTESIAN_POINT('Ctrl Pts',(79.7369093968226,237.210418788751,6.86737840405015)) ;
#73217 = CARTESIAN_POINT('Ctrl Pts',(79.7477405814739,237.195371789186,6.90182436586147)) ;
#73218 = CARTESIAN_POINT('Ctrl Pts',(79.7513857712113,237.190307784632,6.91341700974418)) ;
#73219 = CARTESIAN_POINT('Ctrl Pts',(79.7550880189685,237.185331027006,6.92504601170794)) ;
#73220 = CARTESIAN_POINT('Ctrl Pts',(79.7588460733137,237.180437766862,6.93670440563104)) ;
#73221 = CARTESIAN_POINT('Ctrl Pts',(79.7725748310283,237.162561925596,6.97929433403692)) ;
#73222 = CARTESIAN_POINT('Ctrl Pts',(79.7870252383589,237.145825256622,7.02227651420834)) ;
#73223 = CARTESIAN_POINT('Ctrl Pts',(79.8020894436934,237.130149985728,7.06555117398127)) ;
#73224 = CARTESIAN_POINT('Ctrl Pts',(79.8177535740407,237.113850454419,7.11054922707215)) ;
#73225 = CARTESIAN_POINT('Ctrl Pts',(79.8340818004957,237.09869761457,7.15586351936518)) ;
#73226 = CARTESIAN_POINT('Ctrl Pts',(79.8510076139652,237.084618645229,7.20138187753961)) ;
#73227 = CARTESIAN_POINT('Ctrl Pts',(79.8605668598529,237.076667220618,7.22708942648398)) ;
#73228 = CARTESIAN_POINT('Ctrl Pts',(79.8703176608738,237.069058674587,7.25286206607173)) ;
#73229 = CARTESIAN_POINT('Ctrl Pts',(79.8802543914393,237.06178343507,7.27867958883835)) ;
#73230 = CARTESIAN_POINT('Origin',(79.7621052129773,236.900411902176,16.0213203435596)) ;
#73231 = CARTESIAN_POINT('',(79.8802543914407,237.061783435069,16.0254384350469)) ;
#73232 = CARTESIAN_POINT('',(79.8802543914407,237.061783435069,16.0213203435596)) ;
#73233 = CARTESIAN_POINT('Ctrl Pts',(79.8802543914407,237.061783435069,16.0254384350469)) ;
#73234 = CARTESIAN_POINT('Ctrl Pts',(79.8964035945954,237.049959694839,16.0294645582753)) ;
#73235 = CARTESIAN_POINT('Ctrl Pts',(79.9100841732802,237.036226552047,16.0362204083692)) ;
#73236 = CARTESIAN_POINT('Ctrl Pts',(79.9357881587029,237.002426594019,16.056050217191)) ;
#73237 = CARTESIAN_POINT('Ctrl Pts',(79.9459841760662,236.981950031307,16.070223718736)) ;
#73238 = CARTESIAN_POINT('Ctrl Pts',(79.9604892718756,236.936754644158,16.1046945816758)) ;
#73239 = CARTESIAN_POINT('Ctrl Pts',(79.9631962822073,236.911772508388,16.1258672215767)) ;
#73240 = CARTESIAN_POINT('Ctrl Pts',(79.9601474972632,236.862687912092,16.1708720249643)) ;
#73241 = CARTESIAN_POINT('Ctrl Pts',(79.9538041136321,236.838325875245,16.195176521693)) ;
#73242 = CARTESIAN_POINT('Ctrl Pts',(79.9431600815964,236.815443709278,16.2199877856673)) ;
#73243 = CARTESIAN_POINT('Ctrl Pts',(79.9428711381123,236.814830715324,16.2206540664837)) ;
#73244 = CARTESIAN_POINT('Ctrl Pts',(79.9425790882848,236.814219209147,16.2213203435596)) ;
#73245 = CARTESIAN_POINT('Origin',(71.7633973169967,234.301474162358,16.0213203435596)) ;
#73246 = CARTESIAN_POINT('',(71.5729608165738,234.362580130206,16.0254384350468)) ;
#73247 = CARTESIAN_POINT('',(71.5729608165738,234.362580130206,16.0213203435596)) ;
#73248 = CARTESIAN_POINT('Ctrl Pts',(71.6680536786497,234.125662926577,16.2213203435596)) ;
#73249 = CARTESIAN_POINT('Ctrl Pts',(71.6674579710607,234.125985982886,16.22065406648)) ;
#73250 = CARTESIAN_POINT('Ctrl Pts',(71.6668639020618,234.126312068696,16.2199877856681)) ;
#73251 = CARTESIAN_POINT('Ctrl Pts',(71.6481331715546,234.136717642569,16.19892196599)) ;
#73252 = CARTESIAN_POINT('Ctrl Pts',(71.6314527066269,234.149678040072,16.1784289743351)) ;
#73253 = CARTESIAN_POINT('Ctrl Pts',(71.6031651514905,234.180078648626,16.1396302534806)) ;
#73254 = CARTESIAN_POINT('Ctrl Pts',(71.5912075043469,234.19745717212,16.1210537744242)) ;
#73255 = CARTESIAN_POINT('Ctrl Pts',(71.5724219285888,234.23782327571,16.0855257632587)) ;
#73256 = CARTESIAN_POINT('Ctrl Pts',(71.5658023888919,234.261347309579,16.0684876094541)) ;
#73257 = CARTESIAN_POINT('Ctrl Pts',(71.5625344429639,234.305922303191,16.0440628922224)) ;
#73258 = CARTESIAN_POINT('Ctrl Pts',(71.5638108934068,234.326037533119,16.035372346207)) ;
#73259 = CARTESIAN_POINT('Ctrl Pts',(71.5697653520014,234.3518482812,16.0279192770445)) ;
#73260 = CARTESIAN_POINT('Ctrl Pts',(71.5712461968226,234.357236524721,16.0265673132427)) ;
#73261 = CARTESIAN_POINT('Ctrl Pts',(71.5729608165737,234.362580130206,16.0254384350468)) ;
#73262 = CARTESIAN_POINT('Origin',(74.5283628290597,239.4,7.2786795888419)) ;
#73263 = CARTESIAN_POINT('Origin',(74.5283628290597,239.4,7.17267980084126)) ;
#73264 = CARTESIAN_POINT('Origin',(80.2317703825363,238.345892662512,16.0213203435596)) ;
#73265 = CARTESIAN_POINT('',(80.2325032686099,238.145894005322,16.0254384350469)) ;
#73266 = CARTESIAN_POINT('',(80.2325032686099,238.145894005322,16.0213203435596)) ;
#73267 = CARTESIAN_POINT('Ctrl Pts',(80.4284396085182,238.309544133633,16.2213203435595)) ;
#73268 = CARTESIAN_POINT('Ctrl Pts',(80.4283164474799,238.308877752164,16.2206540664845)) ;
#73269 = CARTESIAN_POINT('Ctrl Pts',(80.428189898863,238.308211992918,16.2199877856662)) ;
#73270 = CARTESIAN_POINT('Ctrl Pts',(80.4240817240622,238.287182510412,16.1989219660283)) ;
#73271 = CARTESIAN_POINT('Ctrl Pts',(80.4169102007044,238.267313462493,16.1784289743315)) ;
#73272 = CARTESIAN_POINT('Ctrl Pts',(80.3967388391005,238.231016094161,16.1396302534697)) ;
#73273 = CARTESIAN_POINT('Ctrl Pts',(80.3839059972643,238.214273436827,16.1210537744103)) ;
#73274 = CARTESIAN_POINT('Ctrl Pts',(80.3513206135603,238.183933480584,16.0855257632447)) ;
#73275 = CARTESIAN_POINT('Ctrl Pts',(80.3309934781214,238.170368597982,16.0684876094427)) ;
#73276 = CARTESIAN_POINT('Ctrl Pts',(80.2896099908123,238.153486166166,16.0440628922152)) ;
#73277 = CARTESIAN_POINT('Ctrl Pts',(80.2700848254327,238.148484194786,16.0353723462014)) ;
#73278 = CARTESIAN_POINT('Ctrl Pts',(80.2436973163872,238.146171261641,16.0279192770422)) ;
#73279 = CARTESIAN_POINT('Ctrl Pts',(80.2381151860642,238.14591456994,16.0265673132417)) ;
#73280 = CARTESIAN_POINT('Ctrl Pts',(80.2325032686099,238.145894005322,16.0254384350468)) ;
#73281 = CARTESIAN_POINT('Origin',(74.5283628290597,239.4,16.2213203435596)) ;
#73282 = CARTESIAN_POINT('',(79.8474585022077,237.087594062475,16.0213203435596)) ;
#73283 = CARTESIAN_POINT('Ctrl Pts',(79.8802543914408,237.061783435069,16.0254384350469)) ;
#73284 = CARTESIAN_POINT('Ctrl Pts',(79.8713490019745,237.068303571741,16.0232182514845)) ;
#73285 = CARTESIAN_POINT('Ctrl Pts',(79.8624665141187,237.075186287767,16.0218983740811)) ;
#73286 = CARTESIAN_POINT('Ctrl Pts',(79.8516072883844,237.084112538764,16.0213707571522)) ;
#73287 = CARTESIAN_POINT('Ctrl Pts',(79.8495261427911,237.085847011892,16.0213203435596)) ;
#73288 = CARTESIAN_POINT('Ctrl Pts',(79.8474585022078,237.087594062475,16.0213203435596)) ;
#73289 = CARTESIAN_POINT('',(80.1907997307331,238.144289709142,16.0213203435596)) ;
#73290 = CARTESIAN_POINT('Origin',(74.5283628290597,239.4,16.0213203435596)) ;
#73291 = CARTESIAN_POINT('Ctrl Pts',(80.1907997307331,238.144289709141,16.0213203435596)) ;
#73292 = CARTESIAN_POINT('Ctrl Pts',(80.2020501093769,238.14511511556,16.0213203435596)) ;
#73293 = CARTESIAN_POINT('Ctrl Pts',(80.2133277776002,238.145621944459,16.0221950109068)) ;
#73294 = CARTESIAN_POINT('Ctrl Pts',(80.227203908038,238.145857122608,16.0244263118334)) ;
#73295 = CARTESIAN_POINT('Ctrl Pts',(80.2298606513355,238.145884321569,16.0249068532759)) ;
#73296 = CARTESIAN_POINT('Ctrl Pts',(80.2325032686099,238.145894005322,16.0254384350468)) ;
#73297 = CARTESIAN_POINT('Origin',(70.5337979397592,235.19483040233,16.0213203435596)) ;
#73298 = CARTESIAN_POINT('',(70.6507612836456,235.032597310185,16.0254384350468)) ;
#73299 = CARTESIAN_POINT('',(70.6507612836456,235.032597310185,16.0213203435596)) ;
#73300 = CARTESIAN_POINT('Ctrl Pts',(70.6507612836456,235.032597310185,16.0254384350468)) ;
#73301 = CARTESIAN_POINT('Ctrl Pts',(70.6345258602317,235.02089224196,16.0294645582753)) ;
#73302 = CARTESIAN_POINT('Ctrl Pts',(70.6172373339836,235.012125012964,16.0362204083692)) ;
#73303 = CARTESIAN_POINT('Ctrl Pts',(70.5771486953323,234.998123831573,16.0560502171909)) ;
#73304 = CARTESIAN_POINT('Ctrl Pts',(70.5545235842934,234.994754448684,16.070223718736)) ;
#73305 = CARTESIAN_POINT('Ctrl Pts',(70.5070578957287,234.994925425491,16.1046945816757)) ;
#73306 = CARTESIAN_POINT('Ctrl Pts',(70.4824619605172,235.000070810184,16.1258672215763)) ;
#73307 = CARTESIAN_POINT('Ctrl Pts',(70.436721861721,235.018138351389,16.1708720249638)) ;
#73308 = CARTESIAN_POINT('Ctrl Pts',(70.4155124011642,235.031699551137,16.1951765216815)) ;
#73309 = CARTESIAN_POINT('Ctrl Pts',(70.3970393549092,235.048893605308,16.2199877856679)) ;
#73310 = CARTESIAN_POINT('Ctrl Pts',(70.3965456514613,235.049357832442,16.2206540664828)) ;
#73311 = CARTESIAN_POINT('Ctrl Pts',(70.3960543228867,235.049824554134,16.2213203435596)) ;
#73312 = CARTESIAN_POINT('Origin',(74.5283628290597,239.4,16.2213203435596)) ;
#73313 = CARTESIAN_POINT('',(70.6854431361484,235.055812131844,16.0213203435596)) ;
#73314 = CARTESIAN_POINT('Ctrl Pts',(70.6507612836457,235.032597310185,16.0254384350469)) ;
#73315 = CARTESIAN_POINT('Ctrl Pts',(70.6597142188007,235.03905200583,16.0232182514845)) ;
#73316 = CARTESIAN_POINT('Ctrl Pts',(70.6690049104272,235.045372877566,16.0218983740811)) ;
#73317 = CARTESIAN_POINT('Ctrl Pts',(70.6808499649014,235.052942251709,16.0213707571522)) ;
#73318 = CARTESIAN_POINT('Ctrl Pts',(70.6831426562284,235.054385557114,16.0213203435596)) ;
#73319 = CARTESIAN_POINT('Ctrl Pts',(70.6854431361486,235.055812131844,16.0213203435596)) ;
#73320 = CARTESIAN_POINT('',(71.5843221421672,234.40273830644,16.0213203435596)) ;
#73321 = CARTESIAN_POINT('Origin',(74.5283628290597,239.4,16.0213203435596)) ;
#73322 = CARTESIAN_POINT('Ctrl Pts',(71.5843221421672,234.40273830644,16.0213203435596)) ;
#73323 = CARTESIAN_POINT('Ctrl Pts',(71.5816305921256,234.39178349591,16.0213203435596)) ;
#73324 = CARTESIAN_POINT('Ctrl Pts',(71.5786276239152,234.380901177314,16.0221950109068)) ;
#73325 = CARTESIAN_POINT('Ctrl Pts',(71.5745633315043,234.367631518996,16.0244263118334)) ;
#73326 = CARTESIAN_POINT('Ctrl Pts',(71.5737682204258,234.365096401029,16.0249068532759)) ;
#73327 = CARTESIAN_POINT('Ctrl Pts',(71.5729608165738,234.362580130206,16.0254384350468)) ;
#73328 = CARTESIAN_POINT('Ctrl Pts',(80.3408628290597,239.969950655759,7.27867958884207)) ;
#73329 = CARTESIAN_POINT('Ctrl Pts',(80.2885314039892,239.952734880846,7.16318954730702)) ;
#73330 = CARTESIAN_POINT('Ctrl Pts',(80.1867665649176,239.903495511764,6.93433474994972)) ;
#73331 = CARTESIAN_POINT('Ctrl Pts',(80.0699170197431,239.797829761707,6.66117794267636)) ;
#73332 = CARTESIAN_POINT('Ctrl Pts',(79.9999528336347,239.689106134798,6.49328644843112)) ;
#73333 = CARTESIAN_POINT('Ctrl Pts',(79.9663766082065,239.6132157885,6.41181121705511)) ;
#73334 = CARTESIAN_POINT('Ctrl Pts',(79.9424927848733,239.538465694316,6.35347296267418)) ;
#73335 = CARTESIAN_POINT('Ctrl Pts',(79.9216609370228,239.414589162551,6.30217046564654)) ;
#73336 = CARTESIAN_POINT('Ctrl Pts',(79.9350370465868,239.282669940057,6.33519178586446)) ;
#73337 = CARTESIAN_POINT('Ctrl Pts',(79.9662361722743,239.186893556273,6.41145261667877)) ;
#73338 = CARTESIAN_POINT('Ctrl Pts',(79.9996838292369,239.11091773279,6.49259951597652)) ;
#73339 = CARTESIAN_POINT('Ctrl Pts',(80.0697670156571,239.002192054553,6.66079439764563)) ;
#73340 = CARTESIAN_POINT('Ctrl Pts',(80.1865578960656,238.896505082212,6.93380047883317)) ;
#73341 = CARTESIAN_POINT('Ctrl Pts',(80.2885314039892,238.847265119153,7.163189547307)) ;
#73342 = CARTESIAN_POINT('Ctrl Pts',(80.3408628290597,238.830049344241,7.27867958884205)) ;
#73343 = CARTESIAN_POINT('Ctrl Pts',(80.3840073254959,239.984144153038,7.24979207607674)) ;
#73344 = CARTESIAN_POINT('Ctrl Pts',(80.327695104819,239.970119016261,7.1355831883288)) ;
#73345 = CARTESIAN_POINT('Ctrl Pts',(80.2168873775464,239.92515275458,6.90890516875886)) ;
#73346 = CARTESIAN_POINT('Ctrl Pts',(80.0872644090126,239.819386167439,6.63780263189585)) ;
#73347 = CARTESIAN_POINT('Ctrl Pts',(80.0088484791991,239.706352588273,6.47101811980176)) ;
#73348 = CARTESIAN_POINT('Ctrl Pts',(79.9710587774453,239.626526469016,6.39005214895656)) ;
#73349 = CARTESIAN_POINT('Ctrl Pts',(79.9441141909301,239.547412991843,6.33206751004184)) ;
#73350 = CARTESIAN_POINT('Ctrl Pts',(79.9205448061692,239.415579861931,6.2810645188759)) ;
#73351 = CARTESIAN_POINT('Ctrl Pts',(79.9356913897779,239.274844790961,6.31389543197584)) ;
#73352 = CARTESIAN_POINT('Ctrl Pts',(79.9708973932049,239.173489891446,6.38969559217925)) ;
#73353 = CARTESIAN_POINT('Ctrl Pts',(80.008539600943,239.093561108983,6.47033490089508)) ;
#73354 = CARTESIAN_POINT('Ctrl Pts',(80.0870927203403,238.98056853352,6.63742123865058)) ;
#73355 = CARTESIAN_POINT('Ctrl Pts',(80.2166470863611,238.874723810129,6.90837475287206)) ;
#73356 = CARTESIAN_POINT('Ctrl Pts',(80.327695104819,238.829880983738,7.13558318832877)) ;
#73357 = CARTESIAN_POINT('Ctrl Pts',(80.3840073254959,238.815855846962,7.24979207607673)) ;
#73358 = CARTESIAN_POINT('Ctrl Pts',(80.4463978769533,240.046981897287,7.19960839071963)) ;
#73359 = CARTESIAN_POINT('Ctrl Pts',(80.3813641849446,240.032577112202,7.08747698484387)) ;
#73360 = CARTESIAN_POINT('Ctrl Pts',(80.2535732837017,239.984593320072,6.86438826993785)) ;
#73361 = CARTESIAN_POINT('Ctrl Pts',(80.1046406899897,239.867698231238,6.59674657937938)) ;
#73362 = CARTESIAN_POINT('Ctrl Pts',(80.0147751931735,239.741969801163,6.43185373754287)) ;
#73363 = CARTESIAN_POINT('Ctrl Pts',(79.971516906311,239.652939705859,6.35176231641288)) ;
#73364 = CARTESIAN_POINT('Ctrl Pts',(79.9406932623428,239.56466954151,6.2943871120956)) ;
#73365 = CARTESIAN_POINT('Ctrl Pts',(79.9137527545012,239.417443548513,6.24390250673371)) ;
#73366 = CARTESIAN_POINT('Ctrl Pts',(79.9310621458369,239.260304020071,6.27640300071354)) ;
#73367 = CARTESIAN_POINT('Ctrl Pts',(79.9713339971205,239.14721859975,6.351408721716)) ;
#73368 = CARTESIAN_POINT('Ctrl Pts',(80.0144245398524,239.058085730517,6.43117626971816)) ;
#73369 = CARTESIAN_POINT('Ctrl Pts',(80.1044455623915,238.93234532304,6.59636871271608)) ;
#73370 = CARTESIAN_POINT('Ctrl Pts',(80.2533028536955,238.815437211919,6.86386231950446)) ;
#73371 = CARTESIAN_POINT('Ctrl Pts',(80.3813641849446,238.767422887798,7.08747698484384)) ;
#73372 = CARTESIAN_POINT('Ctrl Pts',(80.4463978769533,238.753018102712,7.19960839071962)) ;
#73373 = CARTESIAN_POINT('Ctrl Pts',(80.4538735935557,240.142610480885,7.17608503411334)) ;
#73374 = CARTESIAN_POINT('Ctrl Pts',(80.3846751038144,240.121796616249,7.0621594456609)) ;
#73375 = CARTESIAN_POINT('Ctrl Pts',(80.2498546406098,240.060206570595,6.83606809856264)) ;
#73376 = CARTESIAN_POINT('Ctrl Pts',(80.0946540093807,239.923582092156,6.56568507344859)) ;
#73377 = CARTESIAN_POINT('Ctrl Pts',(80.0016160154075,239.781211815477,6.39934495813426)) ;
#73378 = CARTESIAN_POINT('Ctrl Pts',(79.956946110464,239.681398056183,6.31859474911535)) ;
#73379 = CARTESIAN_POINT('Ctrl Pts',(79.925163217437,239.582888242748,6.26076462735161)) ;
#73380 = CARTESIAN_POINT('Ctrl Pts',(79.8974336231358,239.419304875701,6.2098975150157)) ;
#73381 = CARTESIAN_POINT('Ctrl Pts',(79.9152402321547,239.244981652347,6.24264091507684)) ;
#73382 = CARTESIAN_POINT('Ctrl Pts',(79.9567588075993,239.118767221015,6.31823906006946)) ;
#73383 = CARTESIAN_POINT('Ctrl Pts',(80.0012573105604,239.018841087611,6.39866345547881)) ;
#73384 = CARTESIAN_POINT('Ctrl Pts',(80.0944541609073,238.876460220697,6.56530464002502)) ;
#73385 = CARTESIAN_POINT('Ctrl Pts',(80.2495762313356,238.739817789344,6.83553876784972)) ;
#73386 = CARTESIAN_POINT('Ctrl Pts',(80.3846751038144,238.67820338375,7.06215944566087)) ;
#73387 = CARTESIAN_POINT('Ctrl Pts',(80.4538735935557,238.657389519115,7.17608503411333)) ;
#73388 = CARTESIAN_POINT('Ctrl Pts',(80.4465004238194,240.182155687653,7.17267980084145)) ;
#73389 = CARTESIAN_POINT('Ctrl Pts',(80.3767773507721,240.158806652482,7.0571897593064)) ;
#73390 = CARTESIAN_POINT('Ctrl Pts',(80.2412731536591,240.091756439979,6.8283349619491)) ;
#73391 = CARTESIAN_POINT('Ctrl Pts',(80.0859037680535,239.947102365642,6.55517815467574)) ;
#73392 = CARTESIAN_POINT('Ctrl Pts',(79.9929779090082,239.797804263718,6.3872866604305)) ;
#73393 = CARTESIAN_POINT('Ctrl Pts',(79.9484044791676,239.693464121303,6.30581142905449)) ;
#73394 = CARTESIAN_POINT('Ctrl Pts',(79.9167075774066,239.590628083797,6.24747317467356)) ;
#73395 = CARTESIAN_POINT('Ctrl Pts',(79.8890717515519,239.420095928579,6.19617067764592)) ;
#73396 = CARTESIAN_POINT('Ctrl Pts',(79.9068146439663,239.238447540333,6.22919199786384)) ;
#73397 = CARTESIAN_POINT('Ctrl Pts',(79.9482185006771,239.10668693158,6.30545282867815)) ;
#73398 = CARTESIAN_POINT('Ctrl Pts',(79.992621665789,239.002228657834,6.3865997279759)) ;
#73399 = CARTESIAN_POINT('Ctrl Pts',(80.0857051319182,238.852927765033,6.55479460964501)) ;
#73400 = CARTESIAN_POINT('Ctrl Pts',(80.2409968407949,238.708244359177,6.82780069083255)) ;
#73401 = CARTESIAN_POINT('Ctrl Pts',(80.3767773507721,238.641193347518,7.05718975930638)) ;
#73402 = CARTESIAN_POINT('Ctrl Pts',(80.4465004238194,238.617844312347,7.17267980084143)) ;
#73403 = CARTESIAN_POINT('Ctrl Pts',(80.4465004238194,238.617844312347,7.17267980084143)) ;
#73404 = CARTESIAN_POINT('Ctrl Pts',(80.3767773507721,238.641193347518,7.05718975930637)) ;
#73405 = CARTESIAN_POINT('Ctrl Pts',(80.2409968407949,238.708244359176,6.82780069083255)) ;
#73406 = CARTESIAN_POINT('Ctrl Pts',(80.0857051319181,238.852927765034,6.55479460964501)) ;
#73407 = CARTESIAN_POINT('Ctrl Pts',(79.9926216657891,239.002228657833,6.38659972797591)) ;
#73408 = CARTESIAN_POINT('Ctrl Pts',(79.9482185006771,239.106686931581,6.30545282867815)) ;
#73409 = CARTESIAN_POINT('Ctrl Pts',(79.9068146439663,239.238447540332,6.22919199786383)) ;
#73410 = CARTESIAN_POINT('Ctrl Pts',(79.889071751552,239.420095928579,6.19617067764593)) ;
#73411 = CARTESIAN_POINT('Ctrl Pts',(79.9167075774066,239.590628083797,6.24747317467357)) ;
#73412 = CARTESIAN_POINT('Ctrl Pts',(79.9484044791676,239.693464121303,6.3058114290545)) ;
#73413 = CARTESIAN_POINT('Ctrl Pts',(79.9929779090082,239.797804263719,6.3872866604305)) ;
#73414 = CARTESIAN_POINT('Ctrl Pts',(80.0859037680535,239.947102365641,6.55517815467574)) ;
#73415 = CARTESIAN_POINT('Ctrl Pts',(80.241273153659,240.091756439979,6.82833496194906)) ;
#73416 = CARTESIAN_POINT('Ctrl Pts',(80.3767773507721,240.158806652482,7.05718975930632)) ;
#73417 = CARTESIAN_POINT('Ctrl Pts',(80.4465004238193,240.182155687653,7.17267980084132)) ;
#73418 = CARTESIAN_POINT('Ctrl Pts',(80.3408628290597,239.969950655759,7.27867958884207)) ;
#73419 = CARTESIAN_POINT('Ctrl Pts',(80.2885314039892,239.952734880846,7.16318954730702)) ;
#73420 = CARTESIAN_POINT('Ctrl Pts',(80.1867665649176,239.903495511764,6.93433474994972)) ;
#73421 = CARTESIAN_POINT('Ctrl Pts',(80.0699170197431,239.797829761707,6.66117794267636)) ;
#73422 = CARTESIAN_POINT('Ctrl Pts',(79.9999528336347,239.689106134798,6.49328644843112)) ;
#73423 = CARTESIAN_POINT('Ctrl Pts',(79.9663766082065,239.6132157885,6.41181121705511)) ;
#73424 = CARTESIAN_POINT('Ctrl Pts',(79.9424927848733,239.538465694316,6.35347296267418)) ;
#73425 = CARTESIAN_POINT('Ctrl Pts',(79.9216609370228,239.414589162551,6.30217046564654)) ;
#73426 = CARTESIAN_POINT('Ctrl Pts',(79.9350370465868,239.282669940057,6.33519178586446)) ;
#73427 = CARTESIAN_POINT('Ctrl Pts',(79.9662361722743,239.186893556273,6.41145261667877)) ;
#73428 = CARTESIAN_POINT('Ctrl Pts',(79.9996838292369,239.11091773279,6.49259951597652)) ;
#73429 = CARTESIAN_POINT('Ctrl Pts',(80.0697670156571,239.002192054553,6.66079439764563)) ;
#73430 = CARTESIAN_POINT('Ctrl Pts',(80.1865578960656,238.896505082212,6.93380047883317)) ;
#73431 = CARTESIAN_POINT('Ctrl Pts',(80.2885314039892,238.847265119153,7.163189547307)) ;
#73432 = CARTESIAN_POINT('Ctrl Pts',(80.3408628290597,238.830049344241,7.27867958884205)) ;
#73433 = CARTESIAN_POINT('Origin',(80.2783628290597,238.640065792321,16.0213203435596)) ;
#73434 = CARTESIAN_POINT('',(80.3408628290597,238.830049344241,16.0254384350468)) ;
#73435 = CARTESIAN_POINT('',(80.3408628290597,238.830049344241,16.0213203435596)) ;
#73436 = CARTESIAN_POINT('Ctrl Pts',(80.3408628290597,238.830049344241,16.0254384350468)) ;
#73437 = CARTESIAN_POINT('Ctrl Pts',(80.3598753706213,238.823794677268,16.0294645582753)) ;
#73438 = CARTESIAN_POINT('Ctrl Pts',(80.377130148635,238.814961213633,16.0362204083691)) ;
#73439 = CARTESIAN_POINT('Ctrl Pts',(80.4120208529058,238.790758511619,16.0560502171909)) ;
#73440 = CARTESIAN_POINT('Ctrl Pts',(80.4280454475239,238.774434885861,16.070223718736)) ;
#73441 = CARTESIAN_POINT('Ctrl Pts',(80.4558067561093,238.735933839516,16.1046945816758)) ;
#73442 = CARTESIAN_POINT('Ctrl Pts',(80.4661011804338,238.713010928697,16.1258672215766)) ;
#73443 = CARTESIAN_POINT('Ctrl Pts',(80.4783695880631,238.665386577181,16.1708720249644)) ;
#73444 = CARTESIAN_POINT('Ctrl Pts',(80.4798649551292,238.640256689945,16.1951765216955)) ;
#73445 = CARTESIAN_POINT('Ctrl Pts',(80.4768128572537,238.615205270105,16.2199877856669)) ;
#73446 = CARTESIAN_POINT('Ctrl Pts',(80.4767274812194,238.614532989764,16.220654066484)) ;
#73447 = CARTESIAN_POINT('Ctrl Pts',(80.4766386911286,238.61386116447,16.2213203435596)) ;
#73448 = CARTESIAN_POINT('Origin',(70.3231932313897,235.405435110699,16.0213203435596)) ;
#73449 = CARTESIAN_POINT('',(70.1609601392447,235.522398454586,16.0254384350469)) ;
#73450 = CARTESIAN_POINT('',(70.1609601392447,235.522398454586,16.0213203435596)) ;
#73451 = CARTESIAN_POINT('Ctrl Pts',(70.1781873831944,235.267691493827,16.2213203435594)) ;
#73452 = CARTESIAN_POINT('Ctrl Pts',(70.177720661491,235.268182822413,16.2206540664675)) ;
#73453 = CARTESIAN_POINT('Ctrl Pts',(70.1772564343506,235.268676525868,16.2199877856904)) ;
#73454 = CARTESIAN_POINT('Ctrl Pts',(70.1626579503238,235.284360928632,16.1989219658475)) ;
#73455 = CARTESIAN_POINT('Ctrl Pts',(70.1507988684555,235.30184154635,16.1784289743615)) ;
#73456 = CARTESIAN_POINT('Ctrl Pts',(70.1332901094989,235.339495578454,16.1396302535283)) ;
#73457 = CARTESIAN_POINT('Ctrl Pts',(70.1272879703583,235.359718652633,16.1210537744804)) ;
#73458 = CARTESIAN_POINT('Ctrl Pts',(70.1218956381112,235.403914160637,16.0855257633118)) ;
#73459 = CARTESIAN_POINT('Ctrl Pts',(70.1228694079808,235.428332396604,16.0684876094977)) ;
#73460 = CARTESIAN_POINT('Ctrl Pts',(70.1335358372496,235.471735585582,16.0440628922505)) ;
#73461 = CARTESIAN_POINT('Ctrl Pts',(70.1409657616503,235.490471861208,16.0353723462285)) ;
#73462 = CARTESIAN_POINT('Ctrl Pts',(70.1546047480969,235.513179312484,16.0279192770533)) ;
#73463 = CARTESIAN_POINT('Ctrl Pts',(70.1576781740409,235.517846230396,16.0265673132464)) ;
#73464 = CARTESIAN_POINT('Ctrl Pts',(70.160960139245,235.522398454586,16.0254384350468)) ;
#73465 = CARTESIAN_POINT('Origin',(74.5283628290597,239.4,7.2786795888419)) ;
#73466 = CARTESIAN_POINT('Origin',(74.5283628290597,239.4,7.17267980084126)) ;
#73467 = CARTESIAN_POINT('Origin',(80.2783628290597,240.159934207678,16.0213203435596)) ;
#73468 = CARTESIAN_POINT('',(80.3408628290597,239.969950655759,16.0254384350468)) ;
#73469 = CARTESIAN_POINT('',(80.3408628290597,239.969950655759,16.0213203435596)) ;
#73470 = CARTESIAN_POINT('Ctrl Pts',(80.4766386911288,240.186138835529,16.2213203435596)) ;
#73471 = CARTESIAN_POINT('Ctrl Pts',(80.476727481219,240.18546701024,16.2206540664879)) ;
#73472 = CARTESIAN_POINT('Ctrl Pts',(80.4768128572532,240.184794729899,16.2199877856617)) ;
#73473 = CARTESIAN_POINT('Ctrl Pts',(80.4794042183208,240.163525007664,16.1989219660609)) ;
#73474 = CARTESIAN_POINT('Ctrl Pts',(80.4787235677644,240.142412297601,16.1784289743283)) ;
#73475 = CARTESIAN_POINT('Ctrl Pts',(80.4707559665322,240.101658155386,16.1396302534631)) ;
#73476 = CARTESIAN_POINT('Ctrl Pts',(80.4637249743274,240.081769375812,16.1210537744024)) ;
#73477 = CARTESIAN_POINT('Ctrl Pts',(80.4421099949043,240.042844925392,16.0855257632372)) ;
#73478 = CARTESIAN_POINT('Ctrl Pts',(80.4269695195379,240.023662525103,16.0684876094366)) ;
#73479 = CARTESIAN_POINT('Ctrl Pts',(80.3928284426024,239.994818177451,16.0440628922111)) ;
#73480 = CARTESIAN_POINT('Ctrl Pts',(80.3758046009983,239.984027412056,16.0353723461983)) ;
#73481 = CARTESIAN_POINT('Ctrl Pts',(80.3514233242228,239.973673493185,16.027919277041)) ;
#73482 = CARTESIAN_POINT('Ctrl Pts',(80.3461937249045,239.971704391737,16.0265673132412)) ;
#73483 = CARTESIAN_POINT('Ctrl Pts',(80.3408628290599,239.969950655758,16.0254384350468)) ;
#73484 = CARTESIAN_POINT('Origin',(74.5283628290597,239.4,16.2213203435596)) ;
#73485 = CARTESIAN_POINT('',(80.301696162393,238.844462222507,16.0213203435596)) ;
#73486 = CARTESIAN_POINT('Ctrl Pts',(80.3408628290597,238.830049344241,16.0254384350468)) ;
#73487 = CARTESIAN_POINT('Ctrl Pts',(80.3303784673406,238.833498446023,16.0232182514845)) ;
#73488 = CARTESIAN_POINT('Ctrl Pts',(80.3198038431649,238.83729945825,16.0218983740811)) ;
#73489 = CARTESIAN_POINT('Ctrl Pts',(80.3067177425144,238.842433142129,16.0213707571522)) ;
#73490 = CARTESIAN_POINT('Ctrl Pts',(80.3042024737635,238.843439614744,16.0213203435596)) ;
#73491 = CARTESIAN_POINT('Ctrl Pts',(80.3016961623929,238.844462222507,16.0213203435596)) ;
#73492 = CARTESIAN_POINT('',(80.301696162393,239.955537777493,16.0213203435596)) ;
#73493 = CARTESIAN_POINT('Origin',(74.5283628290597,239.4,16.0213203435596)) ;
#73494 = CARTESIAN_POINT('Ctrl Pts',(80.3016961623929,239.955537777493,16.0213203435596)) ;
#73495 = CARTESIAN_POINT('Ctrl Pts',(80.3121408437025,239.95979934384,16.0213203435596)) ;
#73496 = CARTESIAN_POINT('Ctrl Pts',(80.3227099248118,239.963766357905,16.0221950109068)) ;
#73497 = CARTESIAN_POINT('Ctrl Pts',(80.3358342350411,239.968277985737,16.0244263118334)) ;
#73498 = CARTESIAN_POINT('Ctrl Pts',(80.3383525431248,239.969124832316,16.0249068532759)) ;
#73499 = CARTESIAN_POINT('Ctrl Pts',(80.3408628290598,239.969950655759,16.0254384350468)) ;
#73500 = CARTESIAN_POINT('Origin',(69.4298369914177,236.635034487937,16.0213203435596)) ;
#73501 = CARTESIAN_POINT('',(69.4909429592657,236.444597987514,16.0254384350469)) ;
#73502 = CARTESIAN_POINT('',(69.4909429592657,236.444597987514,16.0213203435596)) ;
#73503 = CARTESIAN_POINT('Ctrl Pts',(69.4909429592658,236.444597987514,16.0254384350469)) ;
#73504 = CARTESIAN_POINT('Ctrl Pts',(69.4718850890315,236.438482827851,16.0294645582753)) ;
#73505 = CARTESIAN_POINT('Ctrl Pts',(69.4527335007328,236.435487146003,16.0362204083691)) ;
#73506 = CARTESIAN_POINT('Ctrl Pts',(69.4102803367226,236.434559301829,16.056050217191)) ;
#73507 = CARTESIAN_POINT('Ctrl Pts',(69.3877213808638,236.438346372087,16.0702237187361)) ;
#73508 = CARTESIAN_POINT('Ctrl Pts',(69.3426316631928,236.45317668511,16.1046945816759)) ;
#73509 = CARTESIAN_POINT('Ctrl Pts',(69.320829550048,236.465670798725,16.1258672215769)) ;
#73510 = CARTESIAN_POINT('Ctrl Pts',(69.2829113083105,236.496988519374,16.1708720249652)) ;
#73511 = CARTESIAN_POINT('Ctrl Pts',(69.2669305538229,236.516440070524,16.1951765216735)) ;
#73512 = CARTESIAN_POINT('Ctrl Pts',(69.2546748977525,236.538501073008,16.2199877856701)) ;
#73513 = CARTESIAN_POINT('Ctrl Pts',(69.2543488119446,236.539095142004,16.2206540664831)) ;
#73514 = CARTESIAN_POINT('Ctrl Pts',(69.254025755637,236.53969084959,16.2213203435596)) ;
#73515 = CARTESIAN_POINT('Origin',(74.5283628290597,239.4,16.2213203435596)) ;
#73516 = CARTESIAN_POINT('',(69.5311011354997,236.455959313107,16.0213203435596)) ;
#73517 = CARTESIAN_POINT('Ctrl Pts',(69.4909429592657,236.444597987514,16.0254384350469)) ;
#73518 = CARTESIAN_POINT('Ctrl Pts',(69.5014523172327,236.447970158755,16.0232182514845)) ;
#73519 = CARTESIAN_POINT('Ctrl Pts',(69.5122415468308,236.451110683407,16.0218983740811)) ;
#73520 = CARTESIAN_POINT('Ctrl Pts',(69.5258459283211,236.454649262878,16.0213707571522)) ;
#73521 = CARTESIAN_POINT('Ctrl Pts',(69.5284724132457,236.455313447305,16.0213203435596)) ;
#73522 = CARTESIAN_POINT('Ctrl Pts',(69.5311011354996,236.455959313107,16.0213203435596)) ;
#73523 = CARTESIAN_POINT('',(70.1841749609035,235.557080307089,16.0213203435596)) ;
#73524 = CARTESIAN_POINT('Origin',(74.5283628290597,239.4,16.0213203435596)) ;
#73525 = CARTESIAN_POINT('Ctrl Pts',(70.1841749609037,235.557080307089,16.0213203435596)) ;
#73526 = CARTESIAN_POINT('Ctrl Pts',(70.1782299220736,235.547493397853,16.0213203435596)) ;
#73527 = CARTESIAN_POINT('Ctrl Pts',(70.1720111082046,235.538071666051,16.0221950109068)) ;
#73528 = CARTESIAN_POINT('Ctrl Pts',(70.1640451864931,235.526707406463,16.0244263118334)) ;
#73529 = CARTESIAN_POINT('Ctrl Pts',(70.1625055963862,235.524542068837,16.0249068532759)) ;
#73530 = CARTESIAN_POINT('Ctrl Pts',(70.1609601392448,235.522398454586,16.0254384350468)) ;
#73531 = CARTESIAN_POINT('Ctrl Pts',(79.8802543914407,241.738216564931,7.27867958884204)) ;
#73532 = CARTESIAN_POINT('Ctrl Pts',(79.835803113544,241.705671283424,7.16318668385245)) ;
#73533 = CARTESIAN_POINT('Ctrl Pts',(79.7540359687551,241.627328321488,6.93379523402446)) ;
#73534 = CARTESIAN_POINT('Ctrl Pts',(79.675621293688,241.490723852039,6.66079129118985)) ;
#73535 = CARTESIAN_POINT('Ctrl Pts',(79.6425666774348,241.365662283546,6.49259690874814)) ;
#73536 = CARTESIAN_POINT('Ctrl Pts',(79.6342342806502,241.283068999992,6.41145082407054)) ;
#73537 = CARTESIAN_POINT('Ctrl Pts',(79.6341591116984,241.182339039687,6.33519087357569)) ;
#73538 = CARTESIAN_POINT('Ctrl Pts',(79.6622035595951,241.052743230527,6.30217118028935)) ;
#73539 = CARTESIAN_POINT('Ctrl Pts',(79.7202959489803,240.941367844591,6.35347468345946)) ;
#73540 = CARTESIAN_POINT('Ctrl Pts',(79.7661098244323,240.877657242828,6.41181318029812)) ;
#73541 = CARTESIAN_POINT('Ctrl Pts',(79.8214940286967,240.815857306447,6.49328852242612)) ;
#73542 = CARTESIAN_POINT('Ctrl Pts',(79.9216310945127,240.734075598131,6.66117971759687)) ;
#73543 = CARTESIAN_POINT('Ctrl Pts',(80.065413735872,240.669690330056,6.93433585613084)) ;
#73544 = CARTESIAN_POINT('Ctrl Pts',(80.1774132992676,240.65430786939,7.16318984184328)) ;
#73545 = CARTESIAN_POINT('Ctrl Pts',(80.23250326861,240.654105994678,7.27867958884203)) ;
#73546 = CARTESIAN_POINT('Ctrl Pts',(79.9169012140497,241.765047765619,7.24979207607672)) ;
#73547 = CARTESIAN_POINT('Ctrl Pts',(79.8676778948299,241.734306872547,7.13558035663909)) ;
#73548 = CARTESIAN_POINT('Ctrl Pts',(79.7759215956017,241.657341581077,6.90836950611157)) ;
#73549 = CARTESIAN_POINT('Ctrl Pts',(79.6854170373555,241.516642878156,6.63741808594036)) ;
#73550 = CARTESIAN_POINT('Ctrl Pts',(79.6456256439924,241.384905848815,6.47033223326042)) ;
#73551 = CARTESIAN_POINT('Ctrl Pts',(79.6345255741363,241.297256868669,6.38969373228111)) ;
#73552 = CARTESIAN_POINT('Ctrl Pts',(79.6323635562481,241.18998321442,6.3138944436818)) ;
#73553 = CARTESIAN_POINT('Ctrl Pts',(79.6614485258077,241.051455962317,6.28106514390401)) ;
#73554 = CARTESIAN_POINT('Ctrl Pts',(79.7246032198788,240.933359420814,6.33206913634608)) ;
#73555 = CARTESIAN_POINT('Ctrl Pts',(79.7746764094695,240.866444865567,6.39005401694239)) ;
#73556 = CARTESIAN_POINT('Ctrl Pts',(79.8352840817867,240.802203860244,6.47102009681309)) ;
#73557 = CARTESIAN_POINT('Ctrl Pts',(79.944791006663,240.718934914115,6.63780432564773)) ;
#73558 = CARTESIAN_POINT('Ctrl Pts',(80.1007529981817,240.658400961759,6.90890620100791)) ;
#73559 = CARTESIAN_POINT('Ctrl Pts',(80.2200321925607,240.649876834119,7.1355834795977)) ;
#73560 = CARTESIAN_POINT('Ctrl Pts',(80.2779221549567,240.653939559214,7.2497920760767)) ;
#73561 = CARTESIAN_POINT('Ctrl Pts',(79.9568202021994,241.844089757625,7.19960839981096)) ;
#73562 = CARTESIAN_POINT('Ctrl Pts',(79.8994193858697,241.810292638923,7.08747421375449)) ;
#73563 = CARTESIAN_POINT('Ctrl Pts',(79.7924622476912,241.72505347842,6.86385720549173)) ;
#73564 = CARTESIAN_POINT('Ctrl Pts',(79.6870183903762,241.567867925046,6.59636568101839)) ;
#73565 = CARTESIAN_POINT('Ctrl Pts',(79.6402596949716,241.420463149438,6.43117372668737)) ;
#73566 = CARTESIAN_POINT('Ctrl Pts',(79.6268222315534,241.322376920331,6.35140697730098)) ;
#73567 = CARTESIAN_POINT('Ctrl Pts',(79.6234672952181,241.202381421516,6.27640212195239)) ;
#73568 = CARTESIAN_POINT('Ctrl Pts',(79.6555646533985,241.047584288124,6.24390323078809)) ;
#73569 = CARTESIAN_POINT('Ctrl Pts',(79.7266821718544,240.915890106185,6.29438882568343)) ;
#73570 = CARTESIAN_POINT('Ctrl Pts',(79.7832741387335,240.841465776635,6.35176426775246)) ;
#73571 = CARTESIAN_POINT('Ctrl Pts',(79.8519269181584,240.770161214137,6.43185579663839)) ;
#73572 = CARTESIAN_POINT('Ctrl Pts',(79.9762459680929,240.678356922049,6.59674833983391)) ;
#73573 = CARTESIAN_POINT('Ctrl Pts',(80.1540113597504,240.613206175734,6.86438936993202)) ;
#73574 = CARTESIAN_POINT('Ctrl Pts',(80.2903751411169,240.60706030193,7.08747727990587)) ;
#73575 = CARTESIAN_POINT('Ctrl Pts',(80.3566770119809,240.613457036933,7.19960839981093)) ;
#73576 = CARTESIAN_POINT('Ctrl Pts',(79.9343791952164,241.937348063495,7.17608503411331)) ;
#73577 = CARTESIAN_POINT('Ctrl Pts',(79.8749978862602,241.896168371608,7.0621566209953)) ;
#73578 = CARTESIAN_POINT('Ctrl Pts',(79.765550397568,241.795819886808,6.83553354957588)) ;
#73579 = CARTESIAN_POINT('Ctrl Pts',(79.6602467046092,241.617930062692,6.56530151717807)) ;
#73580 = CARTESIAN_POINT('Ctrl Pts',(79.6156098444531,241.453717854407,6.39866081947765)) ;
#73581 = CARTESIAN_POINT('Ctrl Pts',(79.6041686543468,241.344931536776,6.31823722992109)) ;
#73582 = CARTESIAN_POINT('Ctrl Pts',(79.6036851264843,241.212064334829,6.24263995519171)) ;
#73583 = CARTESIAN_POINT('Ctrl Pts',(79.6406196804877,241.040770912242,6.20989816557033)) ;
#73584 = CARTESIAN_POINT('Ctrl Pts',(79.7175423595761,240.893763866678,6.26076627615902)) ;
#73585 = CARTESIAN_POINT('Ctrl Pts',(79.7782108398639,240.809897525748,6.31859663867191)) ;
#73586 = CARTESIAN_POINT('Ctrl Pts',(79.8515384719066,240.728773354515,6.39934695661234)) ;
#73587 = CARTESIAN_POINT('Ctrl Pts',(79.9840173160935,240.622122133448,6.56568678471671)) ;
#73588 = CARTESIAN_POINT('Ctrl Pts',(80.1738406495645,240.540144605999,6.83606914895208)) ;
#73589 = CARTESIAN_POINT('Ctrl Pts',(80.3210943845718,240.523230645993,7.06215973620728)) ;
#73590 = CARTESIAN_POINT('Ctrl Pts',(80.393337712805,240.524818989667,7.17608503411328)) ;
#73591 = CARTESIAN_POINT('Ctrl Pts',(79.9151467531554,241.97267935533,7.17267980084141)) ;
#73592 = CARTESIAN_POINT('Ctrl Pts',(79.8560499536608,241.928926404028,7.05718689585183)) ;
#73593 = CARTESIAN_POINT('Ctrl Pts',(79.7476341877425,241.823196674671,6.82779544602381)) ;
#73594 = CARTESIAN_POINT('Ctrl Pts',(79.6446539418595,241.637607029148,6.55479150318921)) ;
#73595 = CARTESIAN_POINT('Ctrl Pts',(79.6022633225759,241.466848501153,6.38659712074747)) ;
#73596 = CARTESIAN_POINT('Ctrl Pts',(79.5923133136054,241.353781318703,6.30545103606987)) ;
#73597 = CARTESIAN_POINT('Ctrl Pts',(79.5936527526702,241.215674828182,6.22919108557502)) ;
#73598 = CARTESIAN_POINT('Ctrl Pts',(79.6329114963884,241.037434453048,6.19617139228868)) ;
#73599 = CARTESIAN_POINT('Ctrl Pts',(79.711892278316,240.883789775029,6.2474748954588)) ;
#73600 = CARTESIAN_POINT('Ctrl Pts',(79.7738158466498,240.795782399142,6.30581339229746)) ;
#73601 = CARTESIAN_POINT('Ctrl Pts',(79.8484504478331,240.710323590906,6.38728873442546)) ;
#73602 = CARTESIAN_POINT('Ctrl Pts',(79.9829634655173,240.597048995858,6.55517992959621)) ;
#73603 = CARTESIAN_POINT('Ctrl Pts',(80.1754285723234,240.507487043079,6.82833606813018)) ;
#73604 = CARTESIAN_POINT('Ctrl Pts',(80.3250199085055,240.485591464222,7.05719005384264)) ;
#73605 = CARTESIAN_POINT('Ctrl Pts',(80.3985455526191,240.48493082833,7.17267980084139)) ;
#73606 = CARTESIAN_POINT('Ctrl Pts',(80.3985455526191,240.48493082833,7.17267980084139)) ;
#73607 = CARTESIAN_POINT('Ctrl Pts',(80.3618194988804,240.485260815909,7.11499268084841)) ;
#73608 = CARTESIAN_POINT('Ctrl Pts',(80.324727685632,240.488159890155,7.05749448559109)) ;
#73609 = CARTESIAN_POINT('Ctrl Pts',(80.2873368929612,240.493904456482,7.00044815896927)) ;
#73610 = CARTESIAN_POINT('Ctrl Pts',(80.2618946329122,240.497813299807,6.96163145108278)) ;
#73611 = CARTESIAN_POINT('Ctrl Pts',(80.2363140175748,240.503039163732,6.92302396449324)) ;
#73612 = CARTESIAN_POINT('Ctrl Pts',(80.210616885397,240.509661862821,6.88470750123333)) ;
#73613 = CARTESIAN_POINT('Ctrl Pts',(80.1985486563354,240.512772102869,6.86671281403429)) ;
#73614 = CARTESIAN_POINT('Ctrl Pts',(80.1864548869752,240.516190215325,6.84878249237319)) ;
#73615 = CARTESIAN_POINT('Ctrl Pts',(80.1743333850077,240.519925538921,6.83091833685153)) ;
#73616 = CARTESIAN_POINT('Ctrl Pts',(80.098418576038,240.543319205645,6.71903831097155)) ;
#73617 = CARTESIAN_POINT('Ctrl Pts',(80.0214440764623,240.579145495968,6.60979495876411)) ;
#73618 = CARTESIAN_POINT('Ctrl Pts',(79.9445514182818,240.634230425691,6.50943178829059)) ;
#73619 = CARTESIAN_POINT('Ctrl Pts',(79.9123655188488,240.65728799777,6.46742154975707)) ;
#73620 = CARTESIAN_POINT('Ctrl Pts',(79.8801984195234,240.683717891127,6.42697356775467)) ;
#73621 = CARTESIAN_POINT('Ctrl Pts',(79.8484771304882,240.714739226689,6.38961339026822)) ;
#73622 = CARTESIAN_POINT('Ctrl Pts',(79.8422926650729,240.720787227346,6.382329552423)) ;
#73623 = CARTESIAN_POINT('Ctrl Pts',(79.836125116678,240.727009754421,6.37516303641361)) ;
#73624 = CARTESIAN_POINT('Ctrl Pts',(79.829977629233,240.733415831983,6.36812510586717)) ;
#73625 = CARTESIAN_POINT('Ctrl Pts',(79.8111334235099,240.753052707135,6.3465513796467)) ;
#73626 = CARTESIAN_POINT('Ctrl Pts',(79.7924812621589,240.774409041284,6.32618912069019)) ;
#73627 = CARTESIAN_POINT('Ctrl Pts',(79.77429894775,240.797672530382,6.30766373908655)) ;
#73628 = CARTESIAN_POINT('Ctrl Pts',(79.7561145116039,240.820938734152,6.28913619571245)) ;
#73629 = CARTESIAN_POINT('Ctrl Pts',(79.7384101107657,240.846106021557,6.27245974990907)) ;
#73630 = CARTESIAN_POINT('Ctrl Pts',(79.7214970190476,240.873450881185,6.25837194296375)) ;
#73631 = CARTESIAN_POINT('Ctrl Pts',(79.7146821158104,240.884469125248,6.25269545029417)) ;
#73632 = CARTESIAN_POINT('Ctrl Pts',(79.7079955681862,240.895840392378,6.24743874433886)) ;
#73633 = CARTESIAN_POINT('Ctrl Pts',(79.7014921071138,240.907515086282,6.242672712917)) ;
#73634 = CARTESIAN_POINT('Ctrl Pts',(79.6980536963052,240.91368755249,6.24015288943036)) ;
#73635 = CARTESIAN_POINT('Ctrl Pts',(79.6946664466173,240.919944826602,6.23777018882985)) ;
#73636 = CARTESIAN_POINT('Ctrl Pts',(79.6913383121865,240.926279538755,6.23553482538221)) ;
#73637 = CARTESIAN_POINT('Ctrl Pts',(79.6879136502032,240.932797979742,6.23323462856712)) ;
#73638 = CARTESIAN_POINT('Ctrl Pts',(79.6845476657179,240.939405752671,6.23108774124764)) ;
#73639 = CARTESIAN_POINT('Ctrl Pts',(79.6812468904301,240.946100720566,6.22910489548604)) ;
#73640 = CARTESIAN_POINT('Ctrl Pts',(79.6741449092849,240.960505680497,6.22483858469992)) ;
#73641 = CARTESIAN_POINT('Ctrl Pts',(79.6673477720867,240.975308385753,6.22133351577758)) ;
#73642 = CARTESIAN_POINT('Ctrl Pts',(79.6609436456837,240.990446791267,6.21871402346865)) ;
#73643 = CARTESIAN_POINT('Ctrl Pts',(79.6582845127394,240.996732587376,6.21762635313585)) ;
#73644 = CARTESIAN_POINT('Ctrl Pts',(79.6556928113517,241.003077185731,6.21669131846351)) ;
#73645 = CARTESIAN_POINT('Ctrl Pts',(79.6531763820724,241.00947253337,6.21591845252413)) ;
#73646 = CARTESIAN_POINT('Ctrl Pts',(79.6460361761062,241.027618920294,6.21372549521083)) ;
#73647 = CARTESIAN_POINT('Ctrl Pts',(79.6395050619444,241.046169497294,6.21284107003716)) ;
#73648 = CARTESIAN_POINT('Ctrl Pts',(79.6336142875784,241.06488171304,6.21317793824772)) ;
#73649 = CARTESIAN_POINT('Ctrl Pts',(79.6282273107571,241.081993601263,6.21348599642979)) ;
#73650 = CARTESIAN_POINT('Ctrl Pts',(79.6233733021783,241.099244782297,6.21481328366312)) ;
#73651 = CARTESIAN_POINT('Ctrl Pts',(79.6190569490978,241.116492607629,6.21708379967837)) ;
#73652 = CARTESIAN_POINT('Ctrl Pts',(79.6139675194462,241.136829589344,6.2197609744407)) ;
#73653 = CARTESIAN_POINT('Ctrl Pts',(79.6096229368009,241.157167371827,6.22374822935041)) ;
#73654 = CARTESIAN_POINT('Ctrl Pts',(79.6060732379793,241.177297802026,6.22899963880159)) ;
#73655 = CARTESIAN_POINT('Ctrl Pts',(79.6048283277671,241.184357718765,6.23084135371402)) ;
#73656 = CARTESIAN_POINT('Ctrl Pts',(79.6036814140677,241.191391754094,6.23283871080453)) ;
#73657 = CARTESIAN_POINT('Ctrl Pts',(79.6026353815707,241.19838966958,6.23499018345485)) ;
#73658 = CARTESIAN_POINT('Ctrl Pts',(79.5995061822654,241.21932388753,6.24142629967671)) ;
#73659 = CARTESIAN_POINT('Ctrl Pts',(79.5971497090951,241.240005510031,6.24908072642258)) ;
#73660 = CARTESIAN_POINT('Ctrl Pts',(79.5956115194735,241.260170523062,6.2578736201391)) ;
#73661 = CARTESIAN_POINT('Ctrl Pts',(79.5937525470279,241.284540862756,6.2685002339889)) ;
#73662 = CARTESIAN_POINT('Ctrl Pts',(79.5930888324691,241.30815681995,6.28079050605985)) ;
#73663 = CARTESIAN_POINT('Ctrl Pts',(79.5933396151476,241.331054331832,6.29423684717359)) ;
#73664 = CARTESIAN_POINT('Ctrl Pts',(79.5934185816702,241.338264307019,6.29847083496588)) ;
#73665 = CARTESIAN_POINT('Ctrl Pts',(79.5935882572895,241.345402702503,6.30281925516304)) ;
#73666 = CARTESIAN_POINT('Ctrl Pts',(79.5938400134437,241.352469723438,6.30726579180144)) ;
#73667 = CARTESIAN_POINT('Ctrl Pts',(79.5942671096927,241.364458698018,6.31480919873539)) ;
#73668 = CARTESIAN_POINT('Ctrl Pts',(79.5949303982531,241.376242423441,6.32263506012216)) ;
#73669 = CARTESIAN_POINT('Ctrl Pts',(79.5958260797627,241.387800240562,6.33072043841245)) ;
#73670 = CARTESIAN_POINT('Ctrl Pts',(79.5971357071902,241.404699589427,6.34254253483526)) ;
#73671 = CARTESIAN_POINT('Ctrl Pts',(79.5989049944979,241.42116304008,6.35489088672781)) ;
#73672 = CARTESIAN_POINT('Ctrl Pts',(79.6010914589459,241.437173649127,6.36767695139974)) ;
#73673 = CARTESIAN_POINT('Ctrl Pts',(79.6081006167596,241.488498922498,6.40866528998672)) ;
#73674 = CARTESIAN_POINT('Ctrl Pts',(79.6193970894368,241.535171381628,6.45415280681338)) ;
#73675 = CARTESIAN_POINT('Ctrl Pts',(79.6333149493275,241.578268103782,6.50170615868925)) ;
#73676 = CARTESIAN_POINT('Ctrl Pts',(79.634023379827,241.580461762336,6.50412666335619)) ;
#73677 = CARTESIAN_POINT('Ctrl Pts',(79.6347387172234,241.58264617242,6.50655270031136)) ;
#73678 = CARTESIAN_POINT('Ctrl Pts',(79.6354607419339,241.584821474574,6.5089839474707)) ;
#73679 = CARTESIAN_POINT('Ctrl Pts',(79.6519191897111,241.634407169332,6.56440387122385)) ;
#73680 = CARTESIAN_POINT('Ctrl Pts',(79.6718547135415,241.679255609474,6.6225313924061)) ;
#73681 = CARTESIAN_POINT('Ctrl Pts',(79.6944378635415,241.720169665047,6.68231682911335)) ;
#73682 = CARTESIAN_POINT('Ctrl Pts',(79.7127617888956,241.753367252641,6.73082661979756)) ;
#73683 = CARTESIAN_POINT('Ctrl Pts',(79.7328279991205,241.783976003764,6.78042755176838)) ;
#73684 = CARTESIAN_POINT('Ctrl Pts',(79.7541835606384,241.812447485982,6.83056033541379)) ;
#73685 = CARTESIAN_POINT('Ctrl Pts',(79.7594619350772,241.819484675983,6.84295146844575)) ;
#73686 = CARTESIAN_POINT('Ctrl Pts',(79.7648190500719,241.826391377569,6.85537511374401)) ;
#73687 = CARTESIAN_POINT('Ctrl Pts',(79.7702523393973,241.833170083374,6.86782833897358)) ;
#73688 = CARTESIAN_POINT('Ctrl Pts',(79.8060142023963,241.877787465916,6.94979535892975)) ;
#73689 = CARTESIAN_POINT('Ctrl Pts',(79.8451700619027,241.916834644221,7.03316360005255)) ;
#73690 = CARTESIAN_POINT('Ctrl Pts',(79.8870602112502,241.950886706729,7.11710633589805)) ;
#73691 = CARTESIAN_POINT('Ctrl Pts',(79.8962920857629,241.958391200575,7.13560588330129)) ;
#73692 = CARTESIAN_POINT('Ctrl Pts',(79.905656667599,241.965653268388,7.15413332186264)) ;
#73693 = CARTESIAN_POINT('Ctrl Pts',(79.9151467531553,241.97267935533,7.17267980084126)) ;
#73694 = CARTESIAN_POINT('Ctrl Pts',(79.8802543914407,241.738216564931,7.27867958884204)) ;
#73695 = CARTESIAN_POINT('Ctrl Pts',(79.835803113544,241.705671283424,7.16318668385245)) ;
#73696 = CARTESIAN_POINT('Ctrl Pts',(79.7540359687551,241.627328321488,6.93379523402446)) ;
#73697 = CARTESIAN_POINT('Ctrl Pts',(79.675621293688,241.490723852039,6.66079129118985)) ;
#73698 = CARTESIAN_POINT('Ctrl Pts',(79.6425666774348,241.365662283546,6.49259690874814)) ;
#73699 = CARTESIAN_POINT('Ctrl Pts',(79.6342342806502,241.283068999992,6.41145082407054)) ;
#73700 = CARTESIAN_POINT('Ctrl Pts',(79.6341591116984,241.182339039687,6.33519087357569)) ;
#73701 = CARTESIAN_POINT('Ctrl Pts',(79.6622035595951,241.052743230527,6.30217118028935)) ;
#73702 = CARTESIAN_POINT('Ctrl Pts',(79.7202959489803,240.941367844591,6.35347468345946)) ;
#73703 = CARTESIAN_POINT('Ctrl Pts',(79.7661098244323,240.877657242828,6.41181318029812)) ;
#73704 = CARTESIAN_POINT('Ctrl Pts',(79.8214940286967,240.815857306447,6.49328852242612)) ;
#73705 = CARTESIAN_POINT('Ctrl Pts',(79.9216310945127,240.734075598131,6.66117971759687)) ;
#73706 = CARTESIAN_POINT('Ctrl Pts',(80.065413735872,240.669690330056,6.93433585613084)) ;
#73707 = CARTESIAN_POINT('Ctrl Pts',(80.1774132992676,240.65430786939,7.16318984184328)) ;
#73708 = CARTESIAN_POINT('Ctrl Pts',(80.23250326861,240.654105994678,7.27867958884203)) ;
#73709 = CARTESIAN_POINT('Origin',(80.2317703825363,240.454107337488,16.0213203435596)) ;
#73710 = CARTESIAN_POINT('',(80.2325032686099,240.654105994678,16.0254384350469)) ;
#73711 = CARTESIAN_POINT('',(80.2325032686099,240.654105994678,16.0213203435596)) ;
#73712 = CARTESIAN_POINT('Ctrl Pts',(80.2325032686099,240.654105994678,16.0254384350469)) ;
#73713 = CARTESIAN_POINT('Ctrl Pts',(80.2525180685422,240.654032651345,16.0294645582753)) ;
#73714 = CARTESIAN_POINT('Ctrl Pts',(80.2716580279919,240.650963547834,16.0362204083692)) ;
#73715 = CARTESIAN_POINT('Ctrl Pts',(80.3123201058787,240.638727230937,16.056050217191)) ;
#73716 = CARTESIAN_POINT('Ctrl Pts',(80.3326046787805,240.628154412355,16.070223718736)) ;
#73717 = CARTESIAN_POINT('Ctrl Pts',(80.3709047298332,240.600116457484,16.1046945816758)) ;
#73718 = CARTESIAN_POINT('Ctrl Pts',(80.3877788781721,240.58149662584,16.1258672215767)) ;
#73719 = CARTESIAN_POINT('Ctrl Pts',(80.414163561157,240.539994322448,16.1708720249643)) ;
#73720 = CARTESIAN_POINT('Ctrl Pts',(80.4233513019733,240.516556473268,16.1951765216869)) ;
#73721 = CARTESIAN_POINT('Ctrl Pts',(80.4281898988627,240.491788007084,16.2199877856666)) ;
#73722 = CARTESIAN_POINT('Ctrl Pts',(80.4283164474799,240.491122247836,16.2206540664846)) ;
#73723 = CARTESIAN_POINT('Ctrl Pts',(80.4284396085183,240.490455866367,16.2213203435596)) ;
#73724 = CARTESIAN_POINT('Origin',(69.2946204451421,236.900411902176,16.0213203435596)) ;
#73725 = CARTESIAN_POINT('',(69.1764712666787,237.061783435069,16.0254384350468)) ;
#73726 = CARTESIAN_POINT('',(69.1764712666787,237.061783435069,16.0213203435596)) ;
#73727 = CARTESIAN_POINT('Ctrl Pts',(69.1141465698345,236.814219209148,16.2213203435596)) ;
#73728 = CARTESIAN_POINT('Ctrl Pts',(69.113854520009,236.81483071532,16.2206540664882)) ;
#73729 = CARTESIAN_POINT('Ctrl Pts',(69.1135655765251,236.815443709273,16.2199877856604)) ;
#73730 = CARTESIAN_POINT('Ctrl Pts',(69.1045283400562,236.834871642603,16.1989219660652)) ;
#73731 = CARTESIAN_POINT('Ctrl Pts',(69.0986514909987,236.855161355671,16.1784289743247)) ;
#73732 = CARTESIAN_POINT('Ctrl Pts',(69.0936354075348,236.896382972379,16.1396302534571)) ;
#73733 = CARTESIAN_POINT('Ctrl Pts',(69.0941763076024,236.917471021874,16.1210537743952)) ;
#73734 = CARTESIAN_POINT('Ctrl Pts',(69.102705057958,236.961169770065,16.0855257632304)) ;
#73735 = CARTESIAN_POINT('Ctrl Pts',(69.1111768180338,236.984091981047,16.068487609431)) ;
#73736 = CARTESIAN_POINT('Ctrl Pts',(69.1347335181114,237.022074758818,16.0440628922076)) ;
#73737 = CARTESIAN_POINT('Ctrl Pts',(69.1475896237123,237.037598042927,16.0353723461956)) ;
#73738 = CARTESIAN_POINT('Ctrl Pts',(69.1675780589742,237.054979433805,16.0279192770399)) ;
#73739 = CARTESIAN_POINT('Ctrl Pts',(69.1719432176706,237.058468195629,16.0265673132408)) ;
#73740 = CARTESIAN_POINT('Ctrl Pts',(69.1764712666784,237.061783435069,16.0254384350469)) ;
#73741 = CARTESIAN_POINT('Origin',(74.5283628290597,239.4,7.2786795888419)) ;
#73742 = CARTESIAN_POINT('Origin',(74.5283628290597,239.4,7.17267980084126)) ;
#73743 = CARTESIAN_POINT('Origin',(79.7621052129773,241.899588097824,16.0213203435596)) ;
#73744 = CARTESIAN_POINT('',(79.8802543914406,241.73821656493,16.0254384350469)) ;
#73745 = CARTESIAN_POINT('',(79.8802543914406,241.73821656493,16.0213203435596)) ;
#73746 = CARTESIAN_POINT('Ctrl Pts',(79.9425790882849,241.985780790852,16.2213203435596)) ;
#73747 = CARTESIAN_POINT('Ctrl Pts',(79.9428711381098,241.985169284681,16.2206540664895)) ;
#73748 = CARTESIAN_POINT('Ctrl Pts',(79.9431600815935,241.984556290729,16.2199877856614)) ;
#73749 = CARTESIAN_POINT('Ctrl Pts',(79.952197318064,241.965128357396,16.1989219660712)) ;
#73750 = CARTESIAN_POINT('Ctrl Pts',(79.9580741671204,241.944838644331,16.178428974326)) ;
#73751 = CARTESIAN_POINT('Ctrl Pts',(79.9630902505847,241.903617027621,16.1396302534574)) ;
#73752 = CARTESIAN_POINT('Ctrl Pts',(79.962549350517,241.882528978126,16.121053774395)) ;
#73753 = CARTESIAN_POINT('Ctrl Pts',(79.9540206001612,241.838830229934,16.0855257632299)) ;
#73754 = CARTESIAN_POINT('Ctrl Pts',(79.9455488400853,241.815908018952,16.0684876094306)) ;
#73755 = CARTESIAN_POINT('Ctrl Pts',(79.9219921400076,241.777925241182,16.0440628922073)) ;
#73756 = CARTESIAN_POINT('Ctrl Pts',(79.9091360344067,241.762401957072,16.0353723461954)) ;
#73757 = CARTESIAN_POINT('Ctrl Pts',(79.8891475991448,241.745020566195,16.0279192770397)) ;
#73758 = CARTESIAN_POINT('Ctrl Pts',(79.8847824404483,241.74153180437,16.0265673132406)) ;
#73759 = CARTESIAN_POINT('Ctrl Pts',(79.8802543914405,241.73821656493,16.0254384350468)) ;
#73760 = CARTESIAN_POINT('Origin',(74.5283628290597,239.4,16.2213203435596)) ;
#73761 = CARTESIAN_POINT('',(80.1907997307331,240.655710290858,16.0213203435596)) ;
#73762 = CARTESIAN_POINT('Ctrl Pts',(80.2325032686099,240.654105994679,16.0254384350468)) ;
#73763 = CARTESIAN_POINT('Ctrl Pts',(80.2214662170119,240.654146439457,16.0232182514845)) ;
#73764 = CARTESIAN_POINT('Ctrl Pts',(80.2102345744082,240.654493678325,16.0218983740811)) ;
#73765 = CARTESIAN_POINT('Ctrl Pts',(80.1962025575493,240.655332274339,16.0213707571522)) ;
#73766 = CARTESIAN_POINT('Ctrl Pts',(80.1934993776713,240.655512225888,16.0213203435596)) ;
#73767 = CARTESIAN_POINT('Ctrl Pts',(80.1907997307331,240.655710290859,16.0213203435596)) ;
#73768 = CARTESIAN_POINT('',(79.8474585022076,241.712405937524,16.0213203435596)) ;
#73769 = CARTESIAN_POINT('Origin',(74.5283628290597,239.4,16.0213203435596)) ;
#73770 = CARTESIAN_POINT('Ctrl Pts',(79.8474585022072,241.712405937525,16.0213203435596)) ;
#73771 = CARTESIAN_POINT('Ctrl Pts',(79.8560750880036,241.719686511994,16.0213203435596)) ;
#73772 = CARTESIAN_POINT('Ctrl Pts',(79.8649010067008,241.726725392249,16.0221950109068)) ;
#73773 = CARTESIAN_POINT('Ctrl Pts',(79.8759887977938,241.735071840198,16.0244263118334)) ;
#73774 = CARTESIAN_POINT('Ctrl Pts',(79.8781221611223,241.736655439149,16.0249068532758)) ;
#73775 = CARTESIAN_POINT('Ctrl Pts',(79.8802543914402,241.738216564931,16.0254384350467)) ;
#73776 = CARTESIAN_POINT('Origin',(68.824955275583,238.345892662512,16.0213203435596)) ;
#73777 = CARTESIAN_POINT('',(68.8242223895095,238.145894005322,16.0254384350468)) ;
#73778 = CARTESIAN_POINT('',(68.8242223895095,238.145894005322,16.0213203435596)) ;
#73779 = CARTESIAN_POINT('Ctrl Pts',(68.8242223895095,238.145894005322,16.0254384350468)) ;
#73780 = CARTESIAN_POINT('Ctrl Pts',(68.8042075895772,238.145967348655,16.0294645582753)) ;
#73781 = CARTESIAN_POINT('Ctrl Pts',(68.7850676301275,238.149036452166,16.0362204083691)) ;
#73782 = CARTESIAN_POINT('Ctrl Pts',(68.7444055522406,238.161272769063,16.056050217191)) ;
#73783 = CARTESIAN_POINT('Ctrl Pts',(68.7241209793388,238.171845587645,16.0702237187361)) ;
#73784 = CARTESIAN_POINT('Ctrl Pts',(68.6858209282861,238.199883542516,16.1046945816758)) ;
#73785 = CARTESIAN_POINT('Ctrl Pts',(68.6689467799472,238.218503374159,16.1258672215767)) ;
#73786 = CARTESIAN_POINT('Ctrl Pts',(68.6425620969623,238.260005677552,16.1708720249643)) ;
#73787 = CARTESIAN_POINT('Ctrl Pts',(68.6333743561474,238.283443526724,16.1951765216964)) ;
#73788 = CARTESIAN_POINT('Ctrl Pts',(68.6285357592563,238.308211992918,16.2199877856667)) ;
#73789 = CARTESIAN_POINT('Ctrl Pts',(68.6284092106395,238.308877752164,16.2206540664842)) ;
#73790 = CARTESIAN_POINT('Ctrl Pts',(68.6282860496011,238.309544133633,16.2213203435596)) ;
#73791 = CARTESIAN_POINT('Origin',(74.5283628290597,239.4,16.2213203435596)) ;
#73792 = CARTESIAN_POINT('',(68.8659259273863,238.144289709142,16.0213203435596)) ;
#73793 = CARTESIAN_POINT('Ctrl Pts',(68.8242223895095,238.145894005322,16.0254384350468)) ;
#73794 = CARTESIAN_POINT('Ctrl Pts',(68.8352594411076,238.145853560543,16.0232182514845)) ;
#73795 = CARTESIAN_POINT('Ctrl Pts',(68.8464910837112,238.145506321675,16.0218983740811)) ;
#73796 = CARTESIAN_POINT('Ctrl Pts',(68.8605231005701,238.144667725661,16.0213707571522)) ;
#73797 = CARTESIAN_POINT('Ctrl Pts',(68.8632262804481,238.144487774112,16.0213203435596)) ;
#73798 = CARTESIAN_POINT('Ctrl Pts',(68.8659259273863,238.144289709142,16.0213203435596)) ;
#73799 = CARTESIAN_POINT('',(69.2092671559117,237.087594062475,16.0213203435596)) ;
#73800 = CARTESIAN_POINT('Origin',(74.5283628290597,239.4,16.0213203435596)) ;
#73801 = CARTESIAN_POINT('Ctrl Pts',(69.2092671559116,237.087594062475,16.0213203435596)) ;
#73802 = CARTESIAN_POINT('Ctrl Pts',(69.2006505701154,237.080313488006,16.0213203435596)) ;
#73803 = CARTESIAN_POINT('Ctrl Pts',(69.1918246514184,237.073274607751,16.0221950109068)) ;
#73804 = CARTESIAN_POINT('Ctrl Pts',(69.1807368603254,237.064928159802,16.0244263118334)) ;
#73805 = CARTESIAN_POINT('Ctrl Pts',(69.1786034969968,237.06334456085,16.0249068532759)) ;
#73806 = CARTESIAN_POINT('Ctrl Pts',(69.1764712666787,237.061783435069,16.0254384350469)) ;
#73807 = CARTESIAN_POINT('Ctrl Pts',(78.8957655188814,243.277601545423,7.27867958886638)) ;
#73808 = CARTESIAN_POINT('Ctrl Pts',(78.8635406538411,243.232904298188,7.16316434207538)) ;
#73809 = CARTESIAN_POINT('Ctrl Pts',(78.8166813609821,243.145809292233,6.96275402987872)) ;
#73810 = CARTESIAN_POINT('Ctrl Pts',(78.7894462740705,243.032917191841,6.75724340359379)) ;
#73811 = CARTESIAN_POINT('Ctrl Pts',(78.7835736824138,242.966127546698,6.65331354906745)) ;
#73812 = CARTESIAN_POINT('Ctrl Pts',(78.7800312335663,242.880452545767,6.52713876856571)) ;
#73813 = CARTESIAN_POINT('Ctrl Pts',(78.7936621040222,242.761889135694,6.38460879774661)) ;
#73814 = CARTESIAN_POINT('Ctrl Pts',(78.882776252335,242.581776447516,6.30139782015858)) ;
#73815 = CARTESIAN_POINT('Ctrl Pts',(78.9713921561075,242.483020602554,6.33510444744903)) ;
#73816 = CARTESIAN_POINT('Ctrl Pts',(79.0528714154968,242.423850222314,6.41121110896327)) ;
#73817 = CARTESIAN_POINT('Ctrl Pts',(79.1246096777318,242.38205224677,6.49241324931206)) ;
#73818 = CARTESIAN_POINT('Ctrl Pts',(79.2452124162956,242.335284322678,6.66060069906232)) ;
#73819 = CARTESIAN_POINT('Ctrl Pts',(79.4018524165444,242.318447164155,6.93370165979781)) ;
#73820 = CARTESIAN_POINT('Ctrl Pts',(79.5133244990962,242.33856958246,7.16318512433992)) ;
#73821 = CARTESIAN_POINT('Ctrl Pts',(79.5657826988536,242.355402012486,7.27867958884205)) ;
#73822 = CARTESIAN_POINT('Ctrl Pts',(78.9223274213339,243.314444024655,7.2497920761008)) ;
#73823 = CARTESIAN_POINT('Ctrl Pts',(78.8850055027858,243.269988257635,7.1355582627038)) ;
#73824 = CARTESIAN_POINT('Ctrl Pts',(78.8295487878093,243.181250060656,6.93705316628695)) ;
#73825 = CARTESIAN_POINT('Ctrl Pts',(78.79443887902,243.063184983711,6.7331427106619)) ;
#73826 = CARTESIAN_POINT('Ctrl Pts',(78.7851346722495,242.992610689095,6.62995847244708)) ;
#73827 = CARTESIAN_POINT('Ctrl Pts',(78.7776699511723,242.901880178901,6.50466949064327)) ;
#73828 = CARTESIAN_POINT('Ctrl Pts',(78.7882507062251,242.774922910966,6.36302179397673)) ;
#73829 = CARTESIAN_POINT('Ctrl Pts',(78.8812529483899,242.581900610752,6.28029626114192)) ;
#73830 = CARTESIAN_POINT('Ctrl Pts',(78.9765146123003,242.477074597148,6.31380866775496)) ;
#73831 = CARTESIAN_POINT('Ctrl Pts',(79.0645077757404,242.415741033935,6.38945550249625)) ;
#73832 = CARTESIAN_POINT('Ctrl Pts',(79.1419656410233,242.373212149684,6.47014974693021)) ;
#73833 = CARTESIAN_POINT('Ctrl Pts',(79.2719287950657,242.327970036664,6.6372286847837)) ;
#73834 = CARTESIAN_POINT('Ctrl Pts',(79.4389924679933,242.318509674686,6.90827654234774)) ;
#73835 = CARTESIAN_POINT('Ctrl Pts',(79.5552266855363,242.347525178783,7.13557881442655)) ;
#73836 = CARTESIAN_POINT('Ctrl Pts',(79.6090300580634,242.3692789307,7.24979207607673)) ;
#73837 = CARTESIAN_POINT('Ctrl Pts',(78.9358673079361,243.401953071295,7.19960840329867)) ;
#73838 = CARTESIAN_POINT('Ctrl Pts',(78.8917112313382,243.352062624275,7.08745252517629)) ;
#73839 = CARTESIAN_POINT('Ctrl Pts',(78.8257448247605,243.252491402447,6.89208991795338)) ;
#73840 = CARTESIAN_POINT('Ctrl Pts',(78.7833339311877,243.11958953286,6.69086538804954)) ;
#73841 = CARTESIAN_POINT('Ctrl Pts',(78.7714822977875,243.040196918718,6.58894321460344)) ;
#73842 = CARTESIAN_POINT('Ctrl Pts',(78.7614184058194,242.938158012405,6.46515699374508)) ;
#73843 = CARTESIAN_POINT('Ctrl Pts',(78.7715725864411,242.795537886239,6.32502691287734)) ;
#73844 = CARTESIAN_POINT('Ctrl Pts',(78.8746244794737,242.579388215166,6.24314145731071)) ;
#73845 = CARTESIAN_POINT('Ctrl Pts',(78.9813155195012,242.462582539517,6.27631699480972)) ;
#73846 = CARTESIAN_POINT('Ctrl Pts',(79.080293196982,242.394732278809,6.35117086109098)) ;
#73847 = CARTESIAN_POINT('Ctrl Pts',(79.1675719341539,242.347961153938,6.43099283075982)) ;
#73848 = CARTESIAN_POINT('Ctrl Pts',(79.314304889617,242.299146827055,6.59617796284487)) ;
#73849 = CARTESIAN_POINT('Ctrl Pts',(79.5034918835788,242.29208610874,6.86376506350529)) ;
#73850 = CARTESIAN_POINT('Ctrl Pts',(79.6353575406729,242.328541198735,7.08747270305917)) ;
#73851 = CARTESIAN_POINT('Ctrl Pts',(79.6964401621657,242.355114345509,7.19960840327504)) ;
#73852 = CARTESIAN_POINT('Ctrl Pts',(78.885706249036,243.48371233892,7.17608503413733)) ;
#73853 = CARTESIAN_POINT('Ctrl Pts',(78.8419480295462,243.426187165054,7.06213458186481)) ;
#73854 = CARTESIAN_POINT('Ctrl Pts',(78.7779908352468,243.313384703808,6.86414331997508)) ;
#73855 = CARTESIAN_POINT('Ctrl Pts',(78.7401538986497,243.165798805056,6.66077230046967)) ;
#73856 = CARTESIAN_POINT('Ctrl Pts',(78.7315394990012,243.078165584419,6.55786216980516)) ;
#73857 = CARTESIAN_POINT('Ctrl Pts',(78.7258439115146,242.965657464675,6.43290637600473)) ;
#73858 = CARTESIAN_POINT('Ctrl Pts',(78.7429220836931,242.809363558599,6.29163643302005)) ;
#73859 = CARTESIAN_POINT('Ctrl Pts',(78.8603129422467,242.571305830164,6.20913121818275)) ;
#73860 = CARTESIAN_POINT('Ctrl Pts',(78.9775204042057,242.440886187788,6.24255434951516)) ;
#73861 = CARTESIAN_POINT('Ctrl Pts',(79.0852206169547,242.363148138656,6.31799957071972)) ;
#73862 = CARTESIAN_POINT('Ctrl Pts',(79.1799837053198,242.308472216173,6.3984787601664)) ;
#73863 = CARTESIAN_POINT('Ctrl Pts',(79.3390667698205,242.248062299045,6.56511256803953)) ;
#73864 = CARTESIAN_POINT('Ctrl Pts',(79.5449231900932,242.228718340238,6.83544080204649)) ;
#73865 = CARTESIAN_POINT('Ctrl Pts',(79.6904777773622,242.258307346071,7.06215508260826)) ;
#73866 = CARTESIAN_POINT('Ctrl Pts',(79.7586972267504,242.282143340434,7.17608503411332)) ;
#73867 = CARTESIAN_POINT('Ctrl Pts',(78.8564971400792,243.511371242808,7.17267980086576)) ;
#73868 = CARTESIAN_POINT('Ctrl Pts',(78.8138048922264,243.451486215648,7.05716455407476)) ;
#73869 = CARTESIAN_POINT('Ctrl Pts',(78.7521698261773,243.33447060512,6.85675424187814)) ;
#73870 = CARTESIAN_POINT('Ctrl Pts',(78.717654904468,243.181984925503,6.6512436155932)) ;
#73871 = CARTESIAN_POINT('Ctrl Pts',(78.7111008184567,243.091493832933,6.54731376106682)) ;
#73872 = CARTESIAN_POINT('Ctrl Pts',(78.7080889934782,242.975308192762,6.42113898056508)) ;
#73873 = CARTESIAN_POINT('Ctrl Pts',(78.7290363766315,242.813992657412,6.27860900974601)) ;
#73874 = CARTESIAN_POINT('Ctrl Pts',(78.8530816050133,242.567036921856,6.19539803215796)) ;
#73875 = CARTESIAN_POINT('Ctrl Pts',(78.974544375891,242.430648427085,6.22910465944839)) ;
#73876 = CARTESIAN_POINT('Ctrl Pts',(79.08541149884,242.348357089493,6.30521132096265)) ;
#73877 = CARTESIAN_POINT('Ctrl Pts',(79.1827615086478,242.289958082444,6.38641346131143)) ;
#73878 = CARTESIAN_POINT('Ctrl Pts',(79.345820343214,242.223883095797,6.5546009110617)) ;
#73879 = CARTESIAN_POINT('Ctrl Pts',(79.556540488253,242.198132848066,6.82770187179718)) ;
#73880 = CARTESIAN_POINT('Ctrl Pts',(79.7058422410964,242.22372348177,7.0571853363393)) ;
#73881 = CARTESIAN_POINT('Ctrl Pts',(79.7759762964688,242.245816755679,7.17267980084142)) ;
#73882 = CARTESIAN_POINT('Ctrl Pts',(79.7759762964688,242.245816755679,7.17267980084142)) ;
#73883 = CARTESIAN_POINT('Ctrl Pts',(79.7232193461811,242.229197529155,7.08580138364638)) ;
#73884 = CARTESIAN_POINT('Ctrl Pts',(79.6678914478665,242.217855098603,6.99933943687075)) ;
#73885 = CARTESIAN_POINT('Ctrl Pts',(79.6099012824163,242.212757564659,6.91420575471137)) ;
#73886 = CARTESIAN_POINT('Ctrl Pts',(79.5993389727162,242.2118291015,6.89869953378746)) ;
#73887 = CARTESIAN_POINT('Ctrl Pts',(79.5886884059039,242.211107688293,6.8832373733379)) ;
#73888 = CARTESIAN_POINT('Ctrl Pts',(79.5779491165789,242.210598998763,6.86782476897472)) ;
#73889 = CARTESIAN_POINT('Ctrl Pts',(79.5692533403923,242.210187104627,6.85534493404905)) ;
#73890 = CARTESIAN_POINT('Ctrl Pts',(79.5604985101053,242.209912688296,6.84289479517368)) ;
#73891 = CARTESIAN_POINT('Ctrl Pts',(79.5516841294921,242.209779310136,6.8304773353399)) ;
#73892 = CARTESIAN_POINT('Ctrl Pts',(79.5069926687389,242.209103044261,6.76751722014109)) ;
#73893 = CARTESIAN_POINT('Ctrl Pts',(79.4607683535687,242.212055319315,6.70539635549695)) ;
#73894 = CARTESIAN_POINT('Ctrl Pts',(79.4128176850172,242.2198822012,6.64522313485622)) ;
#73895 = CARTESIAN_POINT('Ctrl Pts',(79.3755141178245,242.225971180209,6.59841094542943)) ;
#73896 = CARTESIAN_POINT('Ctrl Pts',(79.3371660871178,242.235010068117,6.55277794871554)) ;
#73897 = CARTESIAN_POINT('Ctrl Pts',(79.2976938567602,242.247566646749,6.50884764848157)) ;
#73898 = CARTESIAN_POINT('Ctrl Pts',(79.29554782224,242.248249325456,6.50645923668091)) ;
#73899 = CARTESIAN_POINT('Ctrl Pts',(79.2933984675045,242.248942396971,6.50407585761679)) ;
#73900 = CARTESIAN_POINT('Ctrl Pts',(79.2912458053789,242.24964610781,6.50169781367092)) ;
#73901 = CARTESIAN_POINT('Ctrl Pts',(79.2481610140484,242.263730637972,6.45410208280152)) ;
#73902 = CARTESIAN_POINT('Ctrl Pts',(79.2037281831097,242.282048812277,6.40858833733514)) ;
#73903 = CARTESIAN_POINT('Ctrl Pts',(79.1580399707387,242.306577949011,6.36756443793904)) ;
#73904 = CARTESIAN_POINT('Ctrl Pts',(79.1438410202519,242.314201096862,6.35481505935611)) ;
#73905 = CARTESIAN_POINT('Ctrl Pts',(79.1295207322322,242.322424215564,6.34249926125844)) ;
#73906 = CARTESIAN_POINT('Ctrl Pts',(79.1151203415642,242.331272739319,6.33071074220801)) ;
#73907 = CARTESIAN_POINT('Ctrl Pts',(79.1052060542713,242.337364713394,6.32259465929625)) ;
#73908 = CARTESIAN_POINT('Ctrl Pts',(79.0952451490836,242.343777718423,6.3147383662346)) ;
#73909 = CARTESIAN_POINT('Ctrl Pts',(79.0852580707614,242.350503720341,6.30716801584339)) ;
#73910 = CARTESIAN_POINT('Ctrl Pts',(79.066498156481,242.363137967851,6.29294772840495)) ;
#73911 = CARTESIAN_POINT('Ctrl Pts',(79.0476478742883,242.37687482735,6.2797379183036)) ;
#73912 = CARTESIAN_POINT('Ctrl Pts',(79.0288431685158,242.391954252342,6.26803790430659)) ;
#73913 = CARTESIAN_POINT('Ctrl Pts',(79.0231090081396,242.396552454639,6.26447019325204)) ;
#73914 = CARTESIAN_POINT('Ctrl Pts',(79.0173788556137,242.40127569621,6.26104268604071)) ;
#73915 = CARTESIAN_POINT('Ctrl Pts',(79.0116559086474,242.40613130245,6.25776900129401)) ;
#73916 = CARTESIAN_POINT('Ctrl Pts',(78.9962659455198,242.419188841064,6.24896551458699)) ;
#73917 = CARTESIAN_POINT('Ctrl Pts',(78.9809298436631,242.433202118851,6.24127537358637)) ;
#73918 = CARTESIAN_POINT('Ctrl Pts',(78.9658408069922,242.447981105764,6.23479051959553)) ;
#73919 = CARTESIAN_POINT('Ctrl Pts',(78.9519571307252,242.461579500037,6.22882369643702)) ;
#73920 = CARTESIAN_POINT('Ctrl Pts',(78.938297864686,242.475964516107,6.22402506716956)) ;
#73921 = CARTESIAN_POINT('Ctrl Pts',(78.924995550496,242.490971147193,6.22043027857374)) ;
#73922 = CARTESIAN_POINT('Ctrl Pts',(78.9196512063887,242.497000218471,6.21898603458919)) ;
#73923 = CARTESIAN_POINT('Ctrl Pts',(78.9143642429595,242.503130141156,6.2177362717046)) ;
#73924 = CARTESIAN_POINT('Ctrl Pts',(78.9091423730922,242.50935227171,6.21668407135727)) ;
#73925 = CARTESIAN_POINT('Ctrl Pts',(78.8967790392163,242.524083829448,6.21419287480723)) ;
#73926 = CARTESIAN_POINT('Ctrl Pts',(78.8847765441358,242.539338038286,6.21280926967955)) ;
#73927 = CARTESIAN_POINT('Ctrl Pts',(78.8733271793744,242.555016814374,6.21270853878516)) ;
#73928 = CARTESIAN_POINT('Ctrl Pts',(78.8718843166039,242.556992672666,6.21269584455623)) ;
#73929 = CARTESIAN_POINT('Ctrl Pts',(78.8704502764347,242.558975217609,6.21270352039433)) ;
#73930 = CARTESIAN_POINT('Ctrl Pts',(78.8690254763894,242.560964204611,6.212731913334)) ;
#73931 = CARTESIAN_POINT('Ctrl Pts',(78.8598605994944,242.573758154948,6.21291454794133)) ;
#73932 = CARTESIAN_POINT('Ctrl Pts',(78.8510567308864,242.586800007912,6.2139087962786)) ;
#73933 = CARTESIAN_POINT('Ctrl Pts',(78.8426724286616,242.599987892594,6.21570167975813)) ;
#73934 = CARTESIAN_POINT('Ctrl Pts',(78.8402465142696,242.603803675755,6.21622043274669)) ;
#73935 = CARTESIAN_POINT('Ctrl Pts',(78.8378555423078,242.607631831192,6.21680593800229)) ;
#73936 = CARTESIAN_POINT('Ctrl Pts',(78.835498646092,242.611469363401,6.21745376350985)) ;
#73937 = CARTESIAN_POINT('Ctrl Pts',(78.8257292807457,242.627375984117,6.22013900863075)) ;
#73938 = CARTESIAN_POINT('Ctrl Pts',(78.8165816142084,242.643441255929,6.22393977750336)) ;
#73939 = CARTESIAN_POINT('Ctrl Pts',(78.8080789759729,242.659535824001,6.22873230041116)) ;
#73940 = CARTESIAN_POINT('Ctrl Pts',(78.8028449725826,242.66944322233,6.23168245311112)) ;
#73941 = CARTESIAN_POINT('Ctrl Pts',(78.7978561370969,242.679361044475,6.23500875046676)) ;
#73942 = CARTESIAN_POINT('Ctrl Pts',(78.7931247857659,242.689252533828,6.23868459605083)) ;
#73943 = CARTESIAN_POINT('Ctrl Pts',(78.7857782191515,242.704611462041,6.24439223485403)) ;
#73944 = CARTESIAN_POINT('Ctrl Pts',(78.7789906786787,242.719977150002,6.25093270073982)) ;
#73945 = CARTESIAN_POINT('Ctrl Pts',(78.7727739048653,242.735180703857,6.25813416293056)) ;
#73946 = CARTESIAN_POINT('Ctrl Pts',(78.7640306078395,242.756563046402,6.26826232986162)) ;
#73947 = CARTESIAN_POINT('Ctrl Pts',(78.7564179084365,242.777622793233,6.27969809988633)) ;
#73948 = CARTESIAN_POINT('Ctrl Pts',(78.7498196180722,242.798301334159,6.29219975216049)) ;
#73949 = CARTESIAN_POINT('Ctrl Pts',(78.742764251576,242.820412316971,6.30556741768171)) ;
#73950 = CARTESIAN_POINT('Ctrl Pts',(78.7368685023543,242.842087327435,6.32015310285032)) ;
#73951 = CARTESIAN_POINT('Ctrl Pts',(78.731946840072,242.863288277844,6.33563841294475)) ;
#73952 = CARTESIAN_POINT('Ctrl Pts',(78.7307013116998,242.868653616572,6.3395572907484)) ;
#73953 = CARTESIAN_POINT('Ctrl Pts',(78.7295179741353,242.873988756594,6.34353370729427)) ;
#73954 = CARTESIAN_POINT('Ctrl Pts',(78.7283934480067,242.879293401602,6.3475623765746)) ;
#73955 = CARTESIAN_POINT('Ctrl Pts',(78.7223362189441,242.907866726037,6.36926269284759)) ;
#73956 = CARTESIAN_POINT('Ctrl Pts',(78.718071336267,242.935547325288,6.39257820320909)) ;
#73957 = CARTESIAN_POINT('Ctrl Pts',(78.7152239333612,242.962358867744,6.4169448327128)) ;
#73958 = CARTESIAN_POINT('Ctrl Pts',(78.7120287473669,242.992445184214,6.44428761344905)) ;
#73959 = CARTESIAN_POINT('Ctrl Pts',(78.710618917116,243.021437583673,6.47295541130282)) ;
#73960 = CARTESIAN_POINT('Ctrl Pts',(78.7105120445948,243.049335951623,6.5021775037322)) ;
#73961 = CARTESIAN_POINT('Ctrl Pts',(78.7105030190479,243.051692011209,6.5046453538628)) ;
#73962 = CARTESIAN_POINT('Ctrl Pts',(78.7105033080588,243.054040248191,6.50711716242569)) ;
#73963 = CARTESIAN_POINT('Ctrl Pts',(78.7105126321779,243.056380651557,6.50959246668126)) ;
#73964 = CARTESIAN_POINT('Ctrl Pts',(78.7105597699396,243.068212479896,6.52210628180374)) ;
#73965 = CARTESIAN_POINT('Ctrl Pts',(78.7108377274563,243.079844158621,6.53470937925584)) ;
#73966 = CARTESIAN_POINT('Ctrl Pts',(78.7113824377319,243.091325519317,6.54751229341178)) ;
#73967 = CARTESIAN_POINT('Ctrl Pts',(78.7118695050782,243.101591886844,6.55896036351707)) ;
#73968 = CARTESIAN_POINT('Ctrl Pts',(78.7125699081622,243.111738076409,6.57056828687344)) ;
#73969 = CARTESIAN_POINT('Ctrl Pts',(78.7134534138245,243.121756758647,6.58227904590185)) ;
#73970 = CARTESIAN_POINT('Ctrl Pts',(78.7135566743772,243.122927701528,6.58364775184477)) ;
#73971 = CARTESIAN_POINT('Ctrl Pts',(78.7136623208108,243.12409688938,6.58501770970791)) ;
#73972 = CARTESIAN_POINT('Ctrl Pts',(78.7137702989929,243.125264309918,6.58638882085528)) ;
#73973 = CARTESIAN_POINT('Ctrl Pts',(78.7184533488328,243.175895728805,6.64585436952773)) ;
#73974 = CARTESIAN_POINT('Ctrl Pts',(78.7275259043401,243.223199800337,6.7074904562158)) ;
#73975 = CARTESIAN_POINT('Ctrl Pts',(78.7400249137594,243.267677630087,6.77035648044285)) ;
#73976 = CARTESIAN_POINT('Ctrl Pts',(78.7440175315536,243.281885393962,6.79043807239623)) ;
#73977 = CARTESIAN_POINT('Ctrl Pts',(78.7483594753108,243.295805040432,6.81064506724375)) ;
#73978 = CARTESIAN_POINT('Ctrl Pts',(78.7530185895239,243.309453604173,6.83094660614969)) ;
#73979 = CARTESIAN_POINT('Ctrl Pts',(78.7660061234082,243.347499716791,6.8875382483337)) ;
#73980 = CARTESIAN_POINT('Ctrl Pts',(78.7814591606107,243.383438265301,6.94486438343817)) ;
#73981 = CARTESIAN_POINT('Ctrl Pts',(78.7990763319058,243.417432743563,7.00265863085758)) ;
#73982 = CARTESIAN_POINT('Ctrl Pts',(78.8162440599792,243.450559966375,7.058978451292)) ;
#73983 = CARTESIAN_POINT('Ctrl Pts',(78.8354493994883,243.481847275802,7.11572953305104)) ;
#73984 = CARTESIAN_POINT('Ctrl Pts',(78.8564971400704,243.511371242796,7.17267980084187)) ;
#73985 = CARTESIAN_POINT('Ctrl Pts',(78.8957655188814,243.277601545423,7.27867958886638)) ;
#73986 = CARTESIAN_POINT('Ctrl Pts',(78.8635406538411,243.232904298188,7.16316434207538)) ;
#73987 = CARTESIAN_POINT('Ctrl Pts',(78.8166813609821,243.145809292233,6.96275402987872)) ;
#73988 = CARTESIAN_POINT('Ctrl Pts',(78.7894462740705,243.032917191841,6.75724340359379)) ;
#73989 = CARTESIAN_POINT('Ctrl Pts',(78.7835736824138,242.966127546698,6.65331354906745)) ;
#73990 = CARTESIAN_POINT('Ctrl Pts',(78.7800312335663,242.880452545767,6.52713876856571)) ;
#73991 = CARTESIAN_POINT('Ctrl Pts',(78.7936621040222,242.761889135694,6.38460879774661)) ;
#73992 = CARTESIAN_POINT('Ctrl Pts',(78.882776252335,242.581776447516,6.30139782015858)) ;
#73993 = CARTESIAN_POINT('Ctrl Pts',(78.9713921561075,242.483020602554,6.33510444744903)) ;
#73994 = CARTESIAN_POINT('Ctrl Pts',(79.0528714154968,242.423850222314,6.41121110896327)) ;
#73995 = CARTESIAN_POINT('Ctrl Pts',(79.1246096777318,242.38205224677,6.49241324931206)) ;
#73996 = CARTESIAN_POINT('Ctrl Pts',(79.2452124162956,242.335284322678,6.66060069906232)) ;
#73997 = CARTESIAN_POINT('Ctrl Pts',(79.4018524165444,242.318447164155,6.93370165979781)) ;
#73998 = CARTESIAN_POINT('Ctrl Pts',(79.5133244990962,242.33856958246,7.16318512433992)) ;
#73999 = CARTESIAN_POINT('Ctrl Pts',(79.5657826988536,242.355402012486,7.27867958884205)) ;
#74000 = CARTESIAN_POINT('Origin',(79.6268886667016,242.164965512063,16.0213203435596)) ;
#74001 = CARTESIAN_POINT('',(79.5657826988536,242.355402012486,16.0254384350469)) ;
#74002 = CARTESIAN_POINT('',(79.5657826988536,242.355402012486,16.0213203435596)) ;
#74003 = CARTESIAN_POINT('Ctrl Pts',(79.5657826988536,242.355402012486,16.0254384350469)) ;
#74004 = CARTESIAN_POINT('Ctrl Pts',(79.5848405690879,242.361517172149,16.0294645582753)) ;
#74005 = CARTESIAN_POINT('Ctrl Pts',(79.6039921573866,242.364512853997,16.0362204083692)) ;
#74006 = CARTESIAN_POINT('Ctrl Pts',(79.6464453213966,242.365440698171,16.056050217191)) ;
#74007 = CARTESIAN_POINT('Ctrl Pts',(79.6690042772555,242.361653627913,16.0702237187361)) ;
#74008 = CARTESIAN_POINT('Ctrl Pts',(79.7140939949265,242.34682331489,16.1046945816759)) ;
#74009 = CARTESIAN_POINT('Ctrl Pts',(79.7358961080713,242.334329201275,16.1258672215769)) ;
#74010 = CARTESIAN_POINT('Ctrl Pts',(79.7738143498085,242.303011480626,16.1708720249648)) ;
#74011 = CARTESIAN_POINT('Ctrl Pts',(79.7897951042904,242.283559929487,16.195176521687)) ;
#74012 = CARTESIAN_POINT('Ctrl Pts',(79.8020507603673,242.261498926991,16.2199877856679)) ;
#74013 = CARTESIAN_POINT('Ctrl Pts',(79.8023768461752,242.260904857995,16.220654066484)) ;
#74014 = CARTESIAN_POINT('Ctrl Pts',(79.8026999024823,242.26030915041,16.2213203435596)) ;
#74015 = CARTESIAN_POINT('Origin',(68.7783628290597,238.640065792321,16.0213203435596)) ;
#74016 = CARTESIAN_POINT('',(68.7158628290597,238.830049344241,16.0254384350468)) ;
#74017 = CARTESIAN_POINT('',(68.7158628290597,238.830049344241,16.0213203435596)) ;
#74018 = CARTESIAN_POINT('Ctrl Pts',(68.5800869669908,238.61386116447,16.2213203435596)) ;
#74019 = CARTESIAN_POINT('Ctrl Pts',(68.5799981768998,238.614532989765,16.2206540664825)) ;
#74020 = CARTESIAN_POINT('Ctrl Pts',(68.5799128008651,238.61520527011,16.2199877856702)) ;
#74021 = CARTESIAN_POINT('Ctrl Pts',(68.5773214398071,238.636474992276,16.1989219659976)) ;
#74022 = CARTESIAN_POINT('Ctrl Pts',(68.5780020903549,238.65758770239,16.178428974336)) ;
#74023 = CARTESIAN_POINT('Ctrl Pts',(68.5859696915829,238.698341844598,16.1396302534779)) ;
#74024 = CARTESIAN_POINT('Ctrl Pts',(68.5930006837847,238.718230624168,16.1210537744199)) ;
#74025 = CARTESIAN_POINT('Ctrl Pts',(68.6146156632017,238.757155074589,16.0855257632539)) ;
#74026 = CARTESIAN_POINT('Ctrl Pts',(68.629756138567,238.77633747488,16.0684876094502)) ;
#74027 = CARTESIAN_POINT('Ctrl Pts',(68.6638972155015,238.805181822537,16.0440628922199)) ;
#74028 = CARTESIAN_POINT('Ctrl Pts',(68.6809210571054,238.815972587934,16.0353723462051)) ;
#74029 = CARTESIAN_POINT('Ctrl Pts',(68.7053023338861,238.82632650681,16.0279192770437)) ;
#74030 = CARTESIAN_POINT('Ctrl Pts',(68.7105319332097,238.828295608261,16.0265673132423)) ;
#74031 = CARTESIAN_POINT('Ctrl Pts',(68.7158628290598,238.830049344241,16.0254384350468)) ;
#74032 = CARTESIAN_POINT('Origin',(74.5283628290597,239.4,7.2786795888419)) ;
#74033 = CARTESIAN_POINT('Origin',(74.5283628290597,239.4,7.17267980084127)) ;
#74034 = CARTESIAN_POINT('Origin',(78.7335324267296,243.3945648893,16.0213203435596)) ;
#74035 = CARTESIAN_POINT('',(78.8957655188746,243.277601545414,16.0254384350469)) ;
#74036 = CARTESIAN_POINT('',(78.8957655188746,243.277601545414,16.0213203435596)) ;
#74037 = CARTESIAN_POINT('Ctrl Pts',(78.8785382749254,243.532308506173,16.2213203435596)) ;
#74038 = CARTESIAN_POINT('Ctrl Pts',(78.8790049966057,243.531817177611,16.2206540665006)) ;
#74039 = CARTESIAN_POINT('Ctrl Pts',(78.879469223731,243.531323474171,16.2199877856431)) ;
#74040 = CARTESIAN_POINT('Ctrl Pts',(78.8940677080386,243.515639071118,16.1989219662062)) ;
#74041 = CARTESIAN_POINT('Ctrl Pts',(78.9059267896971,243.498158453602,16.1784289743019)) ;
#74042 = CARTESIAN_POINT('Ctrl Pts',(78.9234355486647,243.460504421427,16.1396302534118)) ;
#74043 = CARTESIAN_POINT('Ctrl Pts',(78.9294376878011,243.440281347212,16.1210537743409)) ;
#74044 = CARTESIAN_POINT('Ctrl Pts',(78.9348300200081,243.396085839179,16.0855257631784)) ;
#74045 = CARTESIAN_POINT('Ctrl Pts',(78.9338562501174,243.371667603226,16.0684876093885)) ;
#74046 = CARTESIAN_POINT('Ctrl Pts',(78.9231898208194,243.328264414275,16.0440628921802)) ;
#74047 = CARTESIAN_POINT('Ctrl Pts',(78.9157598964075,243.309528138661,16.0353723461746)) ;
#74048 = CARTESIAN_POINT('Ctrl Pts',(78.9021209099727,243.286820687439,16.0279192770313)) ;
#74049 = CARTESIAN_POINT('Ctrl Pts',(78.8990474840521,243.282153769567,16.0265673132372)) ;
#74050 = CARTESIAN_POINT('Ctrl Pts',(78.8957655188748,243.277601545414,16.0254384350468)) ;
#74051 = CARTESIAN_POINT('Origin',(74.5283628290597,239.4,16.2213203435596)) ;
#74052 = CARTESIAN_POINT('',(79.5256245226196,242.344040686892,16.0213203435596)) ;
#74053 = CARTESIAN_POINT('Ctrl Pts',(79.5657826988536,242.355402012486,16.0254384350468)) ;
#74054 = CARTESIAN_POINT('Ctrl Pts',(79.5552733408866,242.352029841245,16.0232182514845)) ;
#74055 = CARTESIAN_POINT('Ctrl Pts',(79.5444841112885,242.348889316593,16.0218983740811)) ;
#74056 = CARTESIAN_POINT('Ctrl Pts',(79.5308797297982,242.345350737123,16.0213707571522)) ;
#74057 = CARTESIAN_POINT('Ctrl Pts',(79.5282532448735,242.344686552695,16.0213203435596)) ;
#74058 = CARTESIAN_POINT('Ctrl Pts',(79.5256245226195,242.344040686893,16.0213203435596)) ;
#74059 = CARTESIAN_POINT('',(78.8725506972158,243.242919692911,16.0213203435596)) ;
#74060 = CARTESIAN_POINT('Origin',(74.5283628290597,239.4,16.0213203435596)) ;
#74061 = CARTESIAN_POINT('Ctrl Pts',(78.8725506972156,243.242919692911,16.0213203435596)) ;
#74062 = CARTESIAN_POINT('Ctrl Pts',(78.8784957360457,243.252506602147,16.0213203435596)) ;
#74063 = CARTESIAN_POINT('Ctrl Pts',(78.8847145499147,243.261928333949,16.0221950109068)) ;
#74064 = CARTESIAN_POINT('Ctrl Pts',(78.8926804716262,243.273292593537,16.0244263118334)) ;
#74065 = CARTESIAN_POINT('Ctrl Pts',(78.8942200617331,243.275457931163,16.0249068532759)) ;
#74066 = CARTESIAN_POINT('Ctrl Pts',(78.8957655188745,243.277601545414,16.0254384350468)) ;
#74067 = CARTESIAN_POINT('Origin',(68.7783628290597,240.159934207678,16.0213203435596)) ;
#74068 = CARTESIAN_POINT('',(68.7158628290597,239.969950655759,16.0254384350468)) ;
#74069 = CARTESIAN_POINT('',(68.7158628290597,239.969950655759,16.0213203435596)) ;
#74070 = CARTESIAN_POINT('Ctrl Pts',(68.7158628290597,239.969950655759,16.0254384350468)) ;
#74071 = CARTESIAN_POINT('Ctrl Pts',(68.6968502874981,239.976205322732,16.0294645582753)) ;
#74072 = CARTESIAN_POINT('Ctrl Pts',(68.6795955094843,239.985038786367,16.0362204083692)) ;
#74073 = CARTESIAN_POINT('Ctrl Pts',(68.6447048052136,240.009241488381,16.056050217191)) ;
#74074 = CARTESIAN_POINT('Ctrl Pts',(68.6286802105954,240.025565114139,16.070223718736)) ;
#74075 = CARTESIAN_POINT('Ctrl Pts',(68.6009189020099,240.064066160484,16.1046945816759)) ;
#74076 = CARTESIAN_POINT('Ctrl Pts',(68.5906244776854,240.086989071303,16.125867221577)) ;
#74077 = CARTESIAN_POINT('Ctrl Pts',(68.5783560700561,240.134613422819,16.1708720249648)) ;
#74078 = CARTESIAN_POINT('Ctrl Pts',(68.5768607029914,240.159743310064,16.1951765216854)) ;
#74079 = CARTESIAN_POINT('Ctrl Pts',(68.5799128008655,240.184794729893,16.219987785668)) ;
#74080 = CARTESIAN_POINT('Ctrl Pts',(68.5799981768999,240.185467010236,16.2206540664841)) ;
#74081 = CARTESIAN_POINT('Ctrl Pts',(68.5800869669907,240.186138835529,16.2213203435596)) ;
#74082 = CARTESIAN_POINT('Origin',(74.5283628290597,239.4,16.2213203435596)) ;
#74083 = CARTESIAN_POINT('',(68.7550294957263,239.955537777493,16.0213203435596)) ;
#74084 = CARTESIAN_POINT('Ctrl Pts',(68.7158628290597,239.969950655759,16.0254384350468)) ;
#74085 = CARTESIAN_POINT('Ctrl Pts',(68.7263471907788,239.966501553977,16.0232182514845)) ;
#74086 = CARTESIAN_POINT('Ctrl Pts',(68.7369218149545,239.96270054175,16.0218983740811)) ;
#74087 = CARTESIAN_POINT('Ctrl Pts',(68.750007915605,239.957566857871,16.0213707571522)) ;
#74088 = CARTESIAN_POINT('Ctrl Pts',(68.7525231843559,239.956560385256,16.0213203435596)) ;
#74089 = CARTESIAN_POINT('Ctrl Pts',(68.7550294957264,239.955537777493,16.0213203435596)) ;
#74090 = CARTESIAN_POINT('',(68.7550294957263,238.844462222507,16.0213203435596)) ;
#74091 = CARTESIAN_POINT('Origin',(74.5283628290597,239.4,16.0213203435596)) ;
#74092 = CARTESIAN_POINT('Ctrl Pts',(68.7550294957264,238.844462222507,16.0213203435596)) ;
#74093 = CARTESIAN_POINT('Ctrl Pts',(68.7445848144169,238.84020065616,16.0213203435596)) ;
#74094 = CARTESIAN_POINT('Ctrl Pts',(68.7340157333076,238.836233642095,16.0221950109068)) ;
#74095 = CARTESIAN_POINT('Ctrl Pts',(68.7208914230783,238.831722014263,16.0244263118334)) ;
#74096 = CARTESIAN_POINT('Ctrl Pts',(68.7183731149947,238.830875167684,16.0249068532759)) ;
#74097 = CARTESIAN_POINT('Ctrl Pts',(68.7158628290597,238.830049344241,16.0254384350468)) ;
#74098 = CARTESIAN_POINT('Ctrl Pts',(77.4837648415492,244.437419869805,7.27867958886636)) ;
#74099 = CARTESIAN_POINT('Ctrl Pts',(77.4585116532207,244.35871841103,7.10540671867986)) ;
#74100 = CARTESIAN_POINT('Ctrl Pts',(77.443848797508,244.244500039629,6.87572294129316)) ;
#74101 = CARTESIAN_POINT('Ctrl Pts',(77.4767397974834,244.082582260847,6.61251968150632)) ;
#74102 = CARTESIAN_POINT('Ctrl Pts',(77.5104704548032,243.996545441785,6.49309979197962)) ;
#74103 = CARTESIAN_POINT('Ctrl Pts',(77.5520026928461,243.924673376047,6.41122244792242)) ;
#74104 = CARTESIAN_POINT('Ctrl Pts',(77.5920007761937,243.870649989262,6.36192450350774)) ;
#74105 = CARTESIAN_POINT('Ctrl Pts',(77.6750077189191,243.780082536022,6.30168473213267)) ;
#74106 = CARTESIAN_POINT('Ctrl Pts',(77.8132286883953,243.69499776711,6.3324653452167)) ;
#74107 = CARTESIAN_POINT('Ctrl Pts',(77.9593452832999,243.658401997693,6.46981695114858)) ;
#74108 = CARTESIAN_POINT('Ctrl Pts',(78.1070770030435,243.649239949518,6.66032504736798)) ;
#74109 = CARTESIAN_POINT('Ctrl Pts',(78.261227537895,243.682063603977,6.93428000315929)) ;
#74110 = CARTESIAN_POINT('Ctrl Pts',(78.3612751686961,243.735183622334,7.16318512433995)) ;
#74111 = CARTESIAN_POINT('Ctrl Pts',(78.4059643744738,243.767402689815,7.27867958884208)) ;
#74112 = CARTESIAN_POINT('Ctrl Pts',(77.4976417597645,244.480667229015,7.24979207610077)) ;
#74113 = CARTESIAN_POINT('Ctrl Pts',(77.4650052602715,244.399947648007,7.07844135600526)) ;
#74114 = CARTESIAN_POINT('Ctrl Pts',(77.441926342153,244.27989101645,6.85076506164513)) ;
#74115 = CARTESIAN_POINT('Ctrl Pts',(77.469035052647,244.106597484524,6.58946771467476)) ;
#74116 = CARTESIAN_POINT('Ctrl Pts',(77.5017200730652,244.013890562126,6.47083507754566)) ;
#74117 = CARTESIAN_POINT('Ctrl Pts',(77.5439463357434,243.936278331151,6.38946919876817)) ;
#74118 = CARTESIAN_POINT('Ctrl Pts',(77.5854536468431,243.877964896304,6.34047061769564)) ;
#74119 = CARTESIAN_POINT('Ctrl Pts',(77.6727335680326,243.780325930787,6.28058379867695)) ;
#74120 = CARTESIAN_POINT('Ctrl Pts',(77.8207665331947,243.690170175011,6.31119018804536)) ;
#74121 = CARTESIAN_POINT('Ctrl Pts',(77.9773466517903,243.654865956607,6.44770651855499)) ;
#74122 = CARTESIAN_POINT('Ctrl Pts',(78.1347187687794,243.650542022732,6.63695571575657)) ;
#74123 = CARTESIAN_POINT('Ctrl Pts',(78.296448346719,243.693705791539,6.90885244575103)) ;
#74124 = CARTESIAN_POINT('Ctrl Pts',(78.3983590846983,243.756649388286,7.13557881442657)) ;
#74125 = CARTESIAN_POINT('Ctrl Pts',(78.4428068537051,243.793964592266,7.24979207607676)) ;
#74126 = CARTESIAN_POINT('Ctrl Pts',(77.4834771745742,244.568077333119,7.19960840329863)) ;
#74127 = CARTESIAN_POINT('Ctrl Pts',(77.4436102819794,244.4764369139,7.03137458611506)) ;
#74128 = CARTESIAN_POINT('Ctrl Pts',(77.4139039095814,244.340370527827,6.80703943420276)) ;
#74129 = CARTESIAN_POINT('Ctrl Pts',(77.441124871434,244.144263265602,6.54896335582758)) ;
#74130 = CARTESIAN_POINT('Ctrl Pts',(77.4763992563712,244.039603833945,6.4316758963033)) ;
#74131 = CARTESIAN_POINT('Ctrl Pts',(77.5228341950722,243.952143562869,6.35118835405155)) ;
#74132 = CARTESIAN_POINT('Ctrl Pts',(77.5687683992923,243.886557953544,6.30270568059201)) ;
#74133 = CARTESIAN_POINT('Ctrl Pts',(77.6657813516918,243.776949117914,6.2434294197825)) ;
#74134 = CARTESIAN_POINT('Ctrl Pts',(77.8313282196128,243.676542753242,6.27373302479717)) ;
#74135 = CARTESIAN_POINT('Ctrl Pts',(78.007058574649,243.638627531938,6.40881035055017)) ;
#74136 = CARTESIAN_POINT('Ctrl Pts',(78.1839044841603,243.636222713605,6.59590900476823)) ;
#74137 = CARTESIAN_POINT('Ctrl Pts',(78.3660146003686,243.688507812405,6.86433859796256)) ;
#74138 = CARTESIAN_POINT('Ctrl Pts',(78.480434429088,243.763356346367,7.0874727030592)) ;
#74139 = CARTESIAN_POINT('Ctrl Pts',(78.530315900344,243.807504478867,7.19960840327508)) ;
#74140 = CARTESIAN_POINT('Ctrl Pts',(77.4105061694992,244.630334397705,7.17608503413729)) ;
#74141 = CARTESIAN_POINT('Ctrl Pts',(77.3747457443117,244.527986810322,7.0051593557285)) ;
#74142 = CARTESIAN_POINT('Ctrl Pts',(77.352444704757,244.378597391926,6.77808201258452)) ;
#74143 = CARTESIAN_POINT('Ctrl Pts',(77.3933178687395,244.165514331098,6.51747829524014)) ;
#74144 = CARTESIAN_POINT('Ctrl Pts',(77.4368992140211,244.052028001316,6.39916189443959)) ;
#74145 = CARTESIAN_POINT('Ctrl Pts',(77.4912218362456,243.957086040865,6.3180128069882)) ;
#74146 = CARTESIAN_POINT('Ctrl Pts',(77.5437817769028,243.885680434673,6.26914484885761)) ;
#74147 = CARTESIAN_POINT('Ctrl Pts',(77.6531949017869,243.765909487477,6.2094175851449)) ;
#74148 = CARTESIAN_POINT('Ctrl Pts',(77.8359695421258,243.653538086233,6.23994250467339)) ;
#74149 = CARTESIAN_POINT('Ctrl Pts',(78.0288043665172,243.606004164191,6.37609501939021)) ;
#74150 = CARTESIAN_POINT('Ctrl Pts',(78.2232181197253,243.595299774762,6.56484006186565)) ;
#74151 = CARTESIAN_POINT('Ctrl Pts',(78.424955462476,243.641083248432,6.8360152165287)) ;
#74152 = CARTESIAN_POINT('Ctrl Pts',(78.5545603434248,243.713593072997,7.06215508260829)) ;
#74153 = CARTESIAN_POINT('Ctrl Pts',(78.6120751679673,243.757343419967,7.17608503411335)) ;
#74154 = CARTESIAN_POINT('Ctrl Pts',(77.3741795847432,244.647613467424,7.17267980086573)) ;
#74155 = CARTESIAN_POINT('Ctrl Pts',(77.3410337106214,244.542393454288,6.99940693067922)) ;
#74156 = CARTESIAN_POINT('Ctrl Pts',(77.3229424637377,244.389325610061,6.76972315329249)) ;
#74157 = CARTESIAN_POINT('Ctrl Pts',(77.3707526168182,244.1711328328,6.5065198935057)) ;
#74158 = CARTESIAN_POINT('Ctrl Pts',(77.4183887146006,244.054798424185,6.38710000397899)) ;
#74159 = CARTESIAN_POINT('Ctrl Pts',(77.4764294768079,243.957275809245,6.30522265992179)) ;
#74160 = CARTESIAN_POINT('Ctrl Pts',(77.5320328188919,243.883747414752,6.25592471550711)) ;
#74161 = CARTESIAN_POINT('Ctrl Pts',(77.6470057191962,243.760070691083,6.19568494413203)) ;
#74162 = CARTESIAN_POINT('Ctrl Pts',(77.836976450415,243.642390344,6.22646555721608)) ;
#74163 = CARTESIAN_POINT('Ctrl Pts',(78.0363354903944,243.589871777701,6.36381716314794)) ;
#74164 = CARTESIAN_POINT('Ctrl Pts',(78.237103824237,243.574397947023,6.55432525936736)) ;
#74165 = CARTESIAN_POINT('Ctrl Pts',(78.4454209904142,243.615605744879,6.82828021515864)) ;
#74166 = CARTESIAN_POINT('Ctrl Pts',(78.5798598185785,243.685449743899,7.05718533633932)) ;
#74167 = CARTESIAN_POINT('Ctrl Pts',(78.6397340718556,243.728134311011,7.17267980084145)) ;
#74168 = CARTESIAN_POINT('Ctrl Pts',(78.6397340718555,243.728134311011,7.17267980084155)) ;
#74169 = CARTESIAN_POINT('Ctrl Pts',(78.6056702453262,243.703850088494,7.10697236920578)) ;
#74170 = CARTESIAN_POINT('Ctrl Pts',(78.5691964024876,243.682062483905,7.04152434533095)) ;
#74171 = CARTESIAN_POINT('Ctrl Pts',(78.5302356565323,243.66307540284,6.97671039020929)) ;
#74172 = CARTESIAN_POINT('Ctrl Pts',(78.5082997438497,243.652385182667,6.9402184487615)) ;
#74173 = CARTESIAN_POINT('Ctrl Pts',(78.4855756286922,243.642581657307,6.90392782990232)) ;
#74174 = CARTESIAN_POINT('Ctrl Pts',(78.4620506024934,243.633709385751,6.86790773212447)) ;
#74175 = CARTESIAN_POINT('Ctrl Pts',(78.4539288501039,243.63064633315,6.85547219591187)) ;
#74176 = CARTESIAN_POINT('Ctrl Pts',(78.4457097777806,243.627693929755,6.84306655751141)) ;
#74177 = CARTESIAN_POINT('Ctrl Pts',(78.4373919411165,243.624853531614,6.83069239945942)) ;
#74178 = CARTESIAN_POINT('Ctrl Pts',(78.4054267240316,243.613937959829,6.78313885106156)) ;
#74179 = CARTESIAN_POINT('Ctrl Pts',(78.3720062790205,243.60467579283,6.73604738536763)) ;
#74180 = CARTESIAN_POINT('Ctrl Pts',(78.3368785400582,243.597615059998,6.68991428798604)) ;
#74181 = CARTESIAN_POINT('Ctrl Pts',(78.3287444025781,243.595980085096,6.67923176279163)) ;
#74182 = CARTESIAN_POINT('Ctrl Pts',(78.3205186574952,243.594462941081,6.66860062481077)) ;
#74183 = CARTESIAN_POINT('Ctrl Pts',(78.3121980306879,243.593070046952,6.65802703595722)) ;
#74184 = CARTESIAN_POINT('Ctrl Pts',(78.2791741928448,243.587541772351,6.61606138940173)) ;
#74185 = CARTESIAN_POINT('Ctrl Pts',(78.2446566502133,243.583974335635,6.57500138393977)) ;
#74186 = CARTESIAN_POINT('Ctrl Pts',(78.2084138054501,243.582780658522,6.53526328812201)) ;
#74187 = CARTESIAN_POINT('Ctrl Pts',(78.2003901019826,243.582516393637,6.52646578066122)) ;
#74188 = CARTESIAN_POINT('Ctrl Pts',(78.1922817207221,243.582368309447,6.5177330630473)) ;
#74189 = CARTESIAN_POINT('Ctrl Pts',(78.1840859268662,243.582340602795,6.50906965208559)) ;
#74190 = CARTESIAN_POINT('Ctrl Pts',(78.1818287265343,243.582332972117,6.5066836655122)) ;
#74191 = CARTESIAN_POINT('Ctrl Pts',(78.1795648940714,243.582334485191,6.50430295098332)) ;
#74192 = CARTESIAN_POINT('Ctrl Pts',(78.1772943649429,243.58234531375,6.50192769965503)) ;
#74193 = CARTESIAN_POINT('Ctrl Pts',(78.1448749880298,243.58249992754,6.46801306402757)) ;
#74194 = CARTESIAN_POINT('Ctrl Pts',(78.111163228768,243.584564437887,6.43529547007951)) ;
#74195 = CARTESIAN_POINT('Ctrl Pts',(78.0759893913998,243.589010017353,6.4043525891647)) ;
#74196 = CARTESIAN_POINT('Ctrl Pts',(78.0703029105687,243.589728724901,6.39935011822759)) ;
#74197 = CARTESIAN_POINT('Ctrl Pts',(78.0645781241267,243.590509603748,6.3943940321019)) ;
#74198 = CARTESIAN_POINT('Ctrl Pts',(78.0588142008808,243.591354572783,6.38948677170072)) ;
#74199 = CARTESIAN_POINT('Ctrl Pts',(78.0502812827671,243.592605465844,6.38222205817499)) ;
#74200 = CARTESIAN_POINT('Ctrl Pts',(78.0416628571285,243.593996700239,6.37506446485148)) ;
#74201 = CARTESIAN_POINT('Ctrl Pts',(78.0329565182296,243.595534207291,6.36802209790309)) ;
#74202 = CARTESIAN_POINT('Ctrl Pts',(78.0171453080364,243.598326408175,6.35523275609461)) ;
#74203 = CARTESIAN_POINT('Ctrl Pts',(78.0010442203777,243.601601199969,6.34282344947888)) ;
#74204 = CARTESIAN_POINT('Ctrl Pts',(77.9846812113037,243.605467462449,6.33097928884109)) ;
#74205 = CARTESIAN_POINT('Ctrl Pts',(77.9607186006994,243.611129363747,6.31363425113956)) ;
#74206 = CARTESIAN_POINT('Ctrl Pts',(77.936093389843,243.618050306344,6.29738619367076)) ;
#74207 = CARTESIAN_POINT('Ctrl Pts',(77.9109431483584,243.626582550789,6.28290075179634)) ;
#74208 = CARTESIAN_POINT('Ctrl Pts',(77.8951199349199,243.631950591689,6.27378727116955)) ;
#74209 = CARTESIAN_POINT('Ctrl Pts',(77.8790891308354,243.637955860123,6.26537143050151)) ;
#74210 = CARTESIAN_POINT('Ctrl Pts',(77.8628866246398,243.64467672787,6.25781288605435)) ;
#74211 = CARTESIAN_POINT('Ctrl Pts',(77.844327856176,243.65237498312,6.24915513430744)) ;
#74212 = CARTESIAN_POINT('Ctrl Pts',(77.8255436879687,243.661011610903,6.24162317342905)) ;
#74213 = CARTESIAN_POINT('Ctrl Pts',(77.8067818557341,243.670463113482,6.23533853986355)) ;
#74214 = CARTESIAN_POINT('Ctrl Pts',(77.7859713432594,243.680946663801,6.22836766177561)) ;
#74215 = CARTESIAN_POINT('Ctrl Pts',(77.7651450311656,243.692483594737,6.22295373950091)) ;
#74216 = CARTESIAN_POINT('Ctrl Pts',(77.7445535056794,243.704951875444,6.21921673644277)) ;
#74217 = CARTESIAN_POINT('Ctrl Pts',(77.7410522809034,243.707071886094,6.21858132515651)) ;
#74218 = CARTESIAN_POINT('Ctrl Pts',(77.7375578325966,243.709218926783,6.21799446327862)) ;
#74219 = CARTESIAN_POINT('Ctrl Pts',(77.7340713860324,243.711392523157,6.21745682880153)) ;
#74220 = CARTESIAN_POINT('Ctrl Pts',(77.7157398472004,243.722821169944,6.21462997713103)) ;
#74221 = CARTESIAN_POINT('Ctrl Pts',(77.697625497054,243.73498543254,6.21316358595338)) ;
#74222 = CARTESIAN_POINT('Ctrl Pts',(77.6799544975016,243.747812001882,6.21318615231491)) ;
#74223 = CARTESIAN_POINT('Ctrl Pts',(77.6645936405816,243.758961744479,6.21320576855958)) ;
#74224 = CARTESIAN_POINT('Ctrl Pts',(77.6495871697784,243.77064446397,6.2144111776784)) ;
#74225 = CARTESIAN_POINT('Ctrl Pts',(77.6351992769763,243.782777207783,6.21693504199464)) ;
#74226 = CARTESIAN_POINT('Ctrl Pts',(77.6342240251621,243.783599599261,6.21710611661182)) ;
#74227 = CARTESIAN_POINT('Ctrl Pts',(77.63325162561,243.784424046822,6.21728323621031)) ;
#74228 = CARTESIAN_POINT('Ctrl Pts',(77.6322821647892,243.785250519711,6.21746643644027)) ;
#74229 = CARTESIAN_POINT('Ctrl Pts',(77.6224102773551,243.793666380515,6.21933193941812)) ;
#74230 = CARTESIAN_POINT('Ctrl Pts',(77.6127851169546,243.802229499662,6.22169255583841)) ;
#74231 = CARTESIAN_POINT('Ctrl Pts',(77.603457967227,243.810938254419,6.2245883950779)) ;
#74232 = CARTESIAN_POINT('Ctrl Pts',(77.5911012765818,243.822475689924,6.22842482857422)) ;
#74233 = CARTESIAN_POINT('Ctrl Pts',(77.5792663940833,243.834268961409,6.23320005369937)) ;
#74234 = CARTESIAN_POINT('Ctrl Pts',(77.5679799955803,243.84615748058,6.23871133413667)) ;
#74235 = CARTESIAN_POINT('Ctrl Pts',(77.5562410210379,243.858522720374,6.24444361274899)) ;
#74236 = CARTESIAN_POINT('Ctrl Pts',(77.5450496960544,243.871095838374,6.25106944064198)) ;
#74237 = CARTESIAN_POINT('Ctrl Pts',(77.5344310051272,243.883661988622,6.25830807140166)) ;
#74238 = CARTESIAN_POINT('Ctrl Pts',(77.5192233858284,243.901658672991,6.26867491808675)) ;
#74239 = CARTESIAN_POINT('Ctrl Pts',(77.5051928933561,243.919639878176,6.28029754581556)) ;
#74240 = CARTESIAN_POINT('Ctrl Pts',(77.4922892068279,243.937585638839,6.29304624367543)) ;
#74241 = CARTESIAN_POINT('Ctrl Pts',(77.4875869170504,243.94412533327,6.29769205334324)) ;
#74242 = CARTESIAN_POINT('Ctrl Pts',(77.4830337863889,243.950660461088,6.30248724032742)) ;
#74243 = CARTESIAN_POINT('Ctrl Pts',(77.4786258065215,243.957190498153,6.3074250167697)) ;
#74244 = CARTESIAN_POINT('Ctrl Pts',(77.4674012196598,243.97381874294,6.31999869048131)) ;
#74245 = CARTESIAN_POINT('Ctrl Pts',(77.4571197533067,243.990413240837,6.33349717741477)) ;
#74246 = CARTESIAN_POINT('Ctrl Pts',(77.4476436294181,244.006846495269,6.34759111962041)) ;
#74247 = CARTESIAN_POINT('Ctrl Pts',(77.4431766030217,244.014593099492,6.3542349766027)) ;
#74248 = CARTESIAN_POINT('Ctrl Pts',(77.4388910741257,244.022314764158,6.36102814506278)) ;
#74249 = CARTESIAN_POINT('Ctrl Pts',(77.4347756439215,244.030000057463,6.36794186933745)) ;
#74250 = CARTESIAN_POINT('Ctrl Pts',(77.417359309355,244.062523908629,6.39720047149911)) ;
#74251 = CARTESIAN_POINT('Ctrl Pts',(77.4029953763618,244.094397502566,6.42861718017856)) ;
#74252 = CARTESIAN_POINT('Ctrl Pts',(77.3911107953339,244.125609926009,6.46147818340991)) ;
#74253 = CARTESIAN_POINT('Ctrl Pts',(77.385473879065,244.140414134679,6.47706432172584)) ;
#74254 = CARTESIAN_POINT('Ctrl Pts',(77.3803936266802,244.155069379978,6.49297553193036)) ;
#74255 = CARTESIAN_POINT('Ctrl Pts',(77.3758037534668,244.169573406561,6.50913676629883)) ;
#74256 = CARTESIAN_POINT('Ctrl Pts',(77.3690217789683,244.191004486209,6.53301652816881)) ;
#74257 = CARTESIAN_POINT('Ctrl Pts',(77.3633108223515,244.212105384286,6.5574420009269)) ;
#74258 = CARTESIAN_POINT('Ctrl Pts',(77.3585253774069,244.232884182501,6.58226166147533)) ;
#74259 = CARTESIAN_POINT('Ctrl Pts',(77.3532451919441,244.255811185014,6.60964728858771)) ;
#74260 = CARTESIAN_POINT('Ctrl Pts',(77.3491196999421,244.278360870846,6.63755586791247)) ;
#74261 = CARTESIAN_POINT('Ctrl Pts',(77.3459664292511,244.300539026061,6.66580387508425)) ;
#74262 = CARTESIAN_POINT('Ctrl Pts',(77.3404692948678,244.339202468415,6.71504896270834)) ;
#74263 = CARTESIAN_POINT('Ctrl Pts',(77.33792943213,244.376736116788,6.76532381957312)) ;
#74264 = CARTESIAN_POINT('Ctrl Pts',(77.3379719233937,244.4132321697,6.81629637010306)) ;
#74265 = CARTESIAN_POINT('Ctrl Pts',(77.3379762242859,244.416926237014,6.82145572345211)) ;
#74266 = CARTESIAN_POINT('Ctrl Pts',(77.3380069489883,244.420609645206,6.82662222476909)) ;
#74267 = CARTESIAN_POINT('Ctrl Pts',(77.3380636865819,244.424282471624,6.83179552969322)) ;
#74268 = CARTESIAN_POINT('Ctrl Pts',(77.3386487996133,244.46215892118,6.88514583833158)) ;
#74269 = CARTESIAN_POINT('Ctrl Pts',(77.3420026814919,244.49891283477,6.93921967747165)) ;
#74270 = CARTESIAN_POINT('Ctrl Pts',(77.3476451774573,244.53464191174,6.99367465481829)) ;
#74271 = CARTESIAN_POINT('Ctrl Pts',(77.34795542128,244.536606419201,6.99666877664711)) ;
#74272 = CARTESIAN_POINT('Ctrl Pts',(77.3482725720785,244.538567823308,6.99966405072471)) ;
#74273 = CARTESIAN_POINT('Ctrl Pts',(77.3485965458904,244.540526138695,7.00266042013703)) ;
#74274 = CARTESIAN_POINT('Ctrl Pts',(77.3535101894839,244.570227501896,7.0481057333876)) ;
#74275 = CARTESIAN_POINT('Ctrl Pts',(77.3600592544265,244.59920150165,7.09382843494077)) ;
#74276 = CARTESIAN_POINT('Ctrl Pts',(77.368127215059,244.62745431126,7.13971218679672)) ;
#74277 = CARTESIAN_POINT('Ctrl Pts',(77.3700579907416,244.63421560327,7.1506928095768)) ;
#74278 = CARTESIAN_POINT('Ctrl Pts',(77.3720758964805,244.640935408314,7.16168259192434)) ;
#74279 = CARTESIAN_POINT('Ctrl Pts',(77.3741795847387,244.647613467409,7.17267980084153)) ;
#74280 = CARTESIAN_POINT('Ctrl Pts',(77.4837648415492,244.437419869805,7.27867958886636)) ;
#74281 = CARTESIAN_POINT('Ctrl Pts',(77.4585116532207,244.35871841103,7.10540671867986)) ;
#74282 = CARTESIAN_POINT('Ctrl Pts',(77.443848797508,244.244500039629,6.87572294129316)) ;
#74283 = CARTESIAN_POINT('Ctrl Pts',(77.4767397974834,244.082582260847,6.61251968150632)) ;
#74284 = CARTESIAN_POINT('Ctrl Pts',(77.5104704548032,243.996545441785,6.49309979197962)) ;
#74285 = CARTESIAN_POINT('Ctrl Pts',(77.5520026928461,243.924673376047,6.41122244792242)) ;
#74286 = CARTESIAN_POINT('Ctrl Pts',(77.5920007761937,243.870649989262,6.36192450350774)) ;
#74287 = CARTESIAN_POINT('Ctrl Pts',(77.6750077189191,243.780082536022,6.30168473213267)) ;
#74288 = CARTESIAN_POINT('Ctrl Pts',(77.8132286883953,243.69499776711,6.3324653452167)) ;
#74289 = CARTESIAN_POINT('Ctrl Pts',(77.9593452832999,243.658401997693,6.46981695114858)) ;
#74290 = CARTESIAN_POINT('Ctrl Pts',(78.1070770030435,243.649239949518,6.66032504736798)) ;
#74291 = CARTESIAN_POINT('Ctrl Pts',(78.261227537895,243.682063603977,6.93428000315929)) ;
#74292 = CARTESIAN_POINT('Ctrl Pts',(78.3612751686961,243.735183622334,7.16318512433995)) ;
#74293 = CARTESIAN_POINT('Ctrl Pts',(78.4059643744738,243.767402689815,7.27867958884208)) ;
#74294 = CARTESIAN_POINT('Origin',(78.5229277183602,243.60516959767,16.0213203435596)) ;
#74295 = CARTESIAN_POINT('',(78.4059643744738,243.767402689815,16.0254384350469)) ;
#74296 = CARTESIAN_POINT('',(78.4059643744738,243.767402689815,16.0213203435596)) ;
#74297 = CARTESIAN_POINT('Ctrl Pts',(78.4059643744738,243.767402689815,16.0254384350469)) ;
#74298 = CARTESIAN_POINT('Ctrl Pts',(78.4221997978876,243.77910775804,16.0294645582753)) ;
#74299 = CARTESIAN_POINT('Ctrl Pts',(78.4394883241358,243.787874987036,16.0362204083692)) ;
#74300 = CARTESIAN_POINT('Ctrl Pts',(78.479576962787,243.801876168427,16.0560502171909)) ;
#74301 = CARTESIAN_POINT('Ctrl Pts',(78.5022020738258,243.805245551316,16.0702237187359)) ;
#74302 = CARTESIAN_POINT('Ctrl Pts',(78.5496677623908,243.805074574509,16.1046945816758)) ;
#74303 = CARTESIAN_POINT('Ctrl Pts',(78.5742636976025,243.799929189816,16.1258672215766)) ;
#74304 = CARTESIAN_POINT('Ctrl Pts',(78.6200037963982,243.781861648611,16.1708720249637)) ;
#74305 = CARTESIAN_POINT('Ctrl Pts',(78.6412132569573,243.768300448861,16.1951765216776)) ;
#74306 = CARTESIAN_POINT('Ctrl Pts',(78.65968630321,243.751106394692,16.2199877856684)) ;
#74307 = CARTESIAN_POINT('Ctrl Pts',(78.6601800066578,243.750642167558,16.2206540664824)) ;
#74308 = CARTESIAN_POINT('Ctrl Pts',(78.6606713352326,243.750175445865,16.2213203435596)) ;
#74309 = CARTESIAN_POINT('Origin',(68.824955275583,240.454107337488,16.0213203435596)) ;
#74310 = CARTESIAN_POINT('',(68.8242223895094,240.654105994678,16.0254384350469)) ;
#74311 = CARTESIAN_POINT('',(68.8242223895094,240.654105994678,16.0213203435596)) ;
#74312 = CARTESIAN_POINT('Ctrl Pts',(68.6282860496011,240.490455866367,16.2213203435596)) ;
#74313 = CARTESIAN_POINT('Ctrl Pts',(68.6284092106404,240.491122247841,16.2206540664796)) ;
#74314 = CARTESIAN_POINT('Ctrl Pts',(68.6285357592578,240.49178800709,16.2199877856732)) ;
#74315 = CARTESIAN_POINT('Ctrl Pts',(68.6326439340485,240.512817489538,16.1989219659736)) ;
#74316 = CARTESIAN_POINT('Ctrl Pts',(68.6398154574129,240.532686537501,16.1784289743378)) ;
#74317 = CARTESIAN_POINT('Ctrl Pts',(68.6599868190111,240.568983905827,16.1396302534826)) ;
#74318 = CARTESIAN_POINT('Ctrl Pts',(68.6728196608437,240.58572656316,16.1210537744257)) ;
#74319 = CARTESIAN_POINT('Ctrl Pts',(68.7054050445426,240.616066519404,16.0855257632595)) ;
#74320 = CARTESIAN_POINT('Ctrl Pts',(68.7257321799814,240.629631402009,16.0684876094548)) ;
#74321 = CARTESIAN_POINT('Ctrl Pts',(68.7671156672911,240.646513833829,16.0440628922229)) ;
#74322 = CARTESIAN_POINT('Ctrl Pts',(68.786640832671,240.651515805211,16.0353723462074)) ;
#74323 = CARTESIAN_POINT('Ctrl Pts',(68.8130283417221,240.653828738359,16.0279192770447)) ;
#74324 = CARTESIAN_POINT('Ctrl Pts',(68.8186104720501,240.65408543006,16.0265673132428)) ;
#74325 = CARTESIAN_POINT('Ctrl Pts',(68.8242223895094,240.654105994679,16.0254384350468)) ;
#74326 = CARTESIAN_POINT('Origin',(74.5283628290597,239.4,7.2786795888419)) ;
#74327 = CARTESIAN_POINT('Origin',(74.5283628290597,239.4,7.17267980084127)) ;
#74328 = CARTESIAN_POINT('Origin',(77.2933283411226,244.498525837642,16.0213203435596)) ;
#74329 = CARTESIAN_POINT('',(77.4837648415456,244.437419869794,16.0254384350468)) ;
#74330 = CARTESIAN_POINT('',(77.4837648415456,244.437419869794,16.0213203435596)) ;
#74331 = CARTESIAN_POINT('Ctrl Pts',(77.3886719794696,244.674337073423,16.2213203435596)) ;
#74332 = CARTESIAN_POINT('Ctrl Pts',(77.3892676870572,244.674014017114,16.2206540664816)) ;
#74333 = CARTESIAN_POINT('Ctrl Pts',(77.389861756054,244.673687931306,16.2199877856697)) ;
#74334 = CARTESIAN_POINT('Ctrl Pts',(77.4085924865708,244.663282357428,16.1989219659995)) ;
#74335 = CARTESIAN_POINT('Ctrl Pts',(77.4252729514943,244.650321959927,16.1784289743326)) ;
#74336 = CARTESIAN_POINT('Ctrl Pts',(77.4535605066343,244.619921351367,16.1396302534727)) ;
#74337 = CARTESIAN_POINT('Ctrl Pts',(77.4655181537788,244.60254282787,16.121053774414)) ;
#74338 = CARTESIAN_POINT('Ctrl Pts',(77.4843037295348,244.562176724276,16.0855257632485)) ;
#74339 = CARTESIAN_POINT('Ctrl Pts',(77.4909232692299,244.538652690408,16.0684876094458)) ;
#74340 = CARTESIAN_POINT('Ctrl Pts',(77.4941912151551,244.494077696798,16.0440628922171)) ;
#74341 = CARTESIAN_POINT('Ctrl Pts',(77.4929147647111,244.47396246687,16.0353723462029)) ;
#74342 = CARTESIAN_POINT('Ctrl Pts',(77.4869603061161,244.448151718793,16.0279192770428)) ;
#74343 = CARTESIAN_POINT('Ctrl Pts',(77.4854794612957,244.442763475276,16.026567313242)) ;
#74344 = CARTESIAN_POINT('Ctrl Pts',(77.4837648415456,244.437419869794,16.0254384350468)) ;
#74345 = CARTESIAN_POINT('Origin',(74.5283628290597,239.4,16.2213203435596)) ;
#74346 = CARTESIAN_POINT('',(78.3712825219709,243.744187868156,16.0213203435596)) ;
#74347 = CARTESIAN_POINT('Ctrl Pts',(78.4059643744737,243.767402689815,16.0254384350468)) ;
#74348 = CARTESIAN_POINT('Ctrl Pts',(78.3970114393187,243.76094799417,16.0232182514845)) ;
#74349 = CARTESIAN_POINT('Ctrl Pts',(78.3877207476922,243.754627122434,16.0218983740811)) ;
#74350 = CARTESIAN_POINT('Ctrl Pts',(78.3758756932179,243.747057748291,16.0213707571522)) ;
#74351 = CARTESIAN_POINT('Ctrl Pts',(78.3735830018909,243.745614442886,16.0213203435596)) ;
#74352 = CARTESIAN_POINT('Ctrl Pts',(78.3712825219707,243.744187868156,16.0213203435596)) ;
#74353 = CARTESIAN_POINT('',(77.4724035159522,244.39726169356,16.0213203435596)) ;
#74354 = CARTESIAN_POINT('Origin',(74.5283628290597,239.4,16.0213203435596)) ;
#74355 = CARTESIAN_POINT('Ctrl Pts',(77.4724035159521,244.39726169356,16.0213203435596)) ;
#74356 = CARTESIAN_POINT('Ctrl Pts',(77.4750950659937,244.40821650409,16.0213203435596)) ;
#74357 = CARTESIAN_POINT('Ctrl Pts',(77.4780980342041,244.419098822686,16.0221950109068)) ;
#74358 = CARTESIAN_POINT('Ctrl Pts',(77.482162326615,244.432368481004,16.0244263118334)) ;
#74359 = CARTESIAN_POINT('Ctrl Pts',(77.4829574376935,244.434903598971,16.0249068532759)) ;
#74360 = CARTESIAN_POINT('Ctrl Pts',(77.4837648415455,244.437419869794,16.0254384350468)) ;
#74361 = CARTESIAN_POINT('Origin',(69.2946204451421,241.899588097824,16.0213203435596)) ;
#74362 = CARTESIAN_POINT('',(69.1764712666787,241.738216564931,16.0254384350469)) ;
#74363 = CARTESIAN_POINT('',(69.1764712666787,241.738216564931,16.0213203435596)) ;
#74364 = CARTESIAN_POINT('Ctrl Pts',(69.1764712666787,241.738216564931,16.0254384350469)) ;
#74365 = CARTESIAN_POINT('Ctrl Pts',(69.160322063524,241.750040305161,16.0294645582753)) ;
#74366 = CARTESIAN_POINT('Ctrl Pts',(69.1466414848392,241.763773447953,16.0362204083692)) ;
#74367 = CARTESIAN_POINT('Ctrl Pts',(69.1209374994165,241.797573405981,16.056050217191)) ;
#74368 = CARTESIAN_POINT('Ctrl Pts',(69.1107414820532,241.818049968693,16.070223718736)) ;
#74369 = CARTESIAN_POINT('Ctrl Pts',(69.0962363862438,241.863245355842,16.1046945816758)) ;
#74370 = CARTESIAN_POINT('Ctrl Pts',(69.0935293759121,241.888227491612,16.1258672215767)) ;
#74371 = CARTESIAN_POINT('Ctrl Pts',(69.0965781608562,241.937312087907,16.1708720249643)) ;
#74372 = CARTESIAN_POINT('Ctrl Pts',(69.102921544489,241.961674124758,16.1951765216886)) ;
#74373 = CARTESIAN_POINT('Ctrl Pts',(69.1135655765223,241.984556290721,16.2199877856668)) ;
#74374 = CARTESIAN_POINT('Ctrl Pts',(69.1138545200074,241.985169284677,16.2206540664843)) ;
#74375 = CARTESIAN_POINT('Ctrl Pts',(69.1141465698346,241.985780790853,16.2213203435596)) ;
#74376 = CARTESIAN_POINT('Origin',(74.5283628290597,239.4,16.2213203435596)) ;
#74377 = CARTESIAN_POINT('',(69.2092671559117,241.712405937524,16.0213203435596)) ;
#74378 = CARTESIAN_POINT('Ctrl Pts',(69.1764712666787,241.738216564931,16.0254384350469)) ;
#74379 = CARTESIAN_POINT('Ctrl Pts',(69.1853766561449,241.73169642826,16.0232182514845)) ;
#74380 = CARTESIAN_POINT('Ctrl Pts',(69.1942591440007,241.724813712233,16.0218983740811)) ;
#74381 = CARTESIAN_POINT('Ctrl Pts',(69.2051183697351,241.715887461236,16.0213707571522)) ;
#74382 = CARTESIAN_POINT('Ctrl Pts',(69.2071995153286,241.714152988108,16.0213203435596)) ;
#74383 = CARTESIAN_POINT('Ctrl Pts',(69.2092671559121,241.712405937524,16.0213203435596)) ;
#74384 = CARTESIAN_POINT('',(68.8659259273863,240.655710290858,16.0213203435596)) ;
#74385 = CARTESIAN_POINT('Origin',(74.5283628290597,239.4,16.0213203435596)) ;
#74386 = CARTESIAN_POINT('Ctrl Pts',(68.8659259273863,240.655710290859,16.0213203435596)) ;
#74387 = CARTESIAN_POINT('Ctrl Pts',(68.8546755487425,240.65488488444,16.0213203435596)) ;
#74388 = CARTESIAN_POINT('Ctrl Pts',(68.8433978805191,240.654378055541,16.0221950109068)) ;
#74389 = CARTESIAN_POINT('Ctrl Pts',(68.8295217500814,240.654142877393,16.0244263118334)) ;
#74390 = CARTESIAN_POINT('Ctrl Pts',(68.8268650067839,240.654115678431,16.0249068532759)) ;
#74391 = CARTESIAN_POINT('Ctrl Pts',(68.8242223895094,240.654105994679,16.0254384350468)) ;
#74392 = CARTESIAN_POINT('Ctrl Pts',(75.7824688237379,245.10414043955,7.27867958884206)) ;
#74393 = CARTESIAN_POINT('Ctrl Pts',(75.7826706984503,245.049050470116,7.16318984165068)) ;
#74394 = CARTESIAN_POINT('Ctrl Pts',(75.7979890932181,244.936852228027,6.93380141407689)) ;
#74395 = CARTESIAN_POINT('Ctrl Pts',(75.8624126704611,244.793118819323,6.66079598828704)) ;
#74396 = CARTESIAN_POINT('Ctrl Pts',(75.9441595048601,244.69286791716,6.49260131446618)) ;
#74397 = CARTESIAN_POINT('Ctrl Pts',(76.0060804700526,244.637579571816,6.41145429978875)) ;
#74398 = CARTESIAN_POINT('Ctrl Pts',(76.087527546102,244.578310960323,6.33519313286103)) ;
#74399 = CARTESIAN_POINT('Ctrl Pts',(76.2088559391776,244.524823920756,6.30217044135443)) ;
#74400 = CARTESIAN_POINT('Ctrl Pts',(76.3331068362906,244.506355590964,6.35347138365035)) ;
#74401 = CARTESIAN_POINT('Ctrl Pts',(76.4115789956862,244.505971060786,6.41180890998702)) ;
#74402 = CARTESIAN_POINT('Ctrl Pts',(76.4941307169281,244.514452134586,6.49328329969644)) ;
#74403 = CARTESIAN_POINT('Ctrl Pts',(76.6191536305483,244.547394262234,6.66117446013279)) ;
#74404 = CARTESIAN_POINT('Ctrl Pts',(76.7557559389564,244.625871137754,6.93432872868204)) ;
#74405 = CARTESIAN_POINT('Ctrl Pts',(76.8340341124954,244.7074402845,7.16318668389314)) ;
#74406 = CARTESIAN_POINT('Ctrl Pts',(76.8665793939902,244.751891562381,7.27867958884203)) ;
#74407 = CARTESIAN_POINT('Ctrl Pts',(75.782302388274,245.149559325897,7.24979207607673)) ;
#74408 = CARTESIAN_POINT('Ctrl Pts',(75.7782396631717,245.091669363404,7.13558347940724)) ;
#74409 = CARTESIAN_POINT('Ctrl Pts',(75.7865720408754,244.972199666082,6.90837563545836)) ;
#74410 = CARTESIAN_POINT('Ctrl Pts',(75.8472015298446,244.816278812457,6.63742275202096)) ;
#74411 = CARTESIAN_POINT('Ctrl Pts',(75.9303890431917,244.706654034264,6.47033661234462)) ;
#74412 = CARTESIAN_POINT('Ctrl Pts',(75.9947732712511,244.646154912978,6.38969718854569)) ;
#74413 = CARTESIAN_POINT('Ctrl Pts',(76.0802875845848,244.581351687701,6.31389669153484)) ;
#74414 = CARTESIAN_POINT('Ctrl Pts',(76.2094531643599,244.523456540825,6.2810644103727)) ;
#74415 = CARTESIAN_POINT('Ctrl Pts',(76.342117177089,244.505132950672,6.33206585723125)) ;
#74416 = CARTESIAN_POINT('Ctrl Pts',(76.4256849987979,244.506310974435,6.39004977366433)) ;
#74417 = CARTESIAN_POINT('Ctrl Pts',(76.5132819227883,244.517583033546,6.47101490855074)) ;
#74418 = CARTESIAN_POINT('Ctrl Pts',(76.645015605031,244.55723133231,6.6377991047033)) ;
#74419 = CARTESIAN_POINT('Ctrl Pts',(76.7856610937703,244.647825162852,6.90889913348456)) ;
#74420 = CARTESIAN_POINT('Ctrl Pts',(76.8626697016172,244.739315065788,7.13558035667933)) ;
#74421 = CARTESIAN_POINT('Ctrl Pts',(76.8934105946791,244.78853838499,7.24979207607671)) ;
#74422 = CARTESIAN_POINT('Ctrl Pts',(75.7418198659931,245.228314182921,7.19960839981097)) ;
#74423 = CARTESIAN_POINT('Ctrl Pts',(75.7354231309795,245.162012311947,7.08747727971887)) ;
#74424 = CARTESIAN_POINT('Ctrl Pts',(75.741514293225,245.025381866761,6.86386325013094)) ;
#74425 = CARTESIAN_POINT('Ctrl Pts',(75.8067006833652,244.847684053476,6.59637029411434)) ;
#74426 = CARTESIAN_POINT('Ctrl Pts',(75.8984682441908,244.723213358552,6.43117805982654)) ;
#74427 = CARTESIAN_POINT('Ctrl Pts',(75.9699223922858,244.65468834945,6.35141039969581)) ;
#74428 = CARTESIAN_POINT('Ctrl Pts',(76.065027577409,244.581442276898,6.27640434964301)) ;
#74429 = CARTESIAN_POINT('Ctrl Pts',(76.209126271206,244.51642084558,6.24390250637184)) ;
#74430 = CARTESIAN_POINT('Ctrl Pts',(76.3574714895589,244.496546627825,6.29438558207702)) ;
#74431 = CARTESIAN_POINT('Ctrl Pts',(76.4509465479782,244.498584229117,6.35176007082548)) ;
#74432 = CARTESIAN_POINT('Ctrl Pts',(76.548986871076,244.512212968342,6.43185066721499)) ;
#74433 = CARTESIAN_POINT('Ctrl Pts',(76.6963322794042,244.558827523821,6.59674318091439)) ;
#74434 = CARTESIAN_POINT('Ctrl Pts',(76.853528602567,244.664346813509,6.86438240227357)) ;
#74435 = CARTESIAN_POINT('Ctrl Pts',(76.9386554679947,244.77105655683,7.08747421379399)) ;
#74436 = CARTESIAN_POINT('Ctrl Pts',(76.9724525866849,244.82845737314,7.19960839981094)) ;
#74437 = CARTESIAN_POINT('Ctrl Pts',(75.6531818187263,245.264974883745,7.17608503411332)) ;
#74438 = CARTESIAN_POINT('Ctrl Pts',(75.6515934750498,245.192731555392,7.06215973601728)) ;
#74439 = CARTESIAN_POINT('Ctrl Pts',(75.6684443594419,245.045205445093,6.83553966272154)) ;
#74440 = CARTESIAN_POINT('Ctrl Pts',(75.750463235268,244.855451291138,6.56530617079925)) ;
#74441 = CARTESIAN_POINT('Ctrl Pts',(75.8570753675148,244.722818054325,6.39866518685632)) ;
#74442 = CARTESIAN_POINT('Ctrl Pts',(75.9383593864038,244.649618706818,6.31824067693821)) ;
#74443 = CARTESIAN_POINT('Ctrl Pts',(76.0455656774809,244.571129860748,6.24264219702634)) ;
#74444 = CARTESIAN_POINT('Ctrl Pts',(76.2058533104506,244.500325505336,6.20989743397218)) ;
#74445 = CARTESIAN_POINT('Ctrl Pts',(76.3699991515416,244.476147020544,6.26076300576044)) ;
#74446 = CARTESIAN_POINT('Ctrl Pts',(76.4735091268837,244.475932678415,6.31859240668635)) ;
#74447 = CARTESIAN_POINT('Ctrl Pts',(76.5822415391347,244.487571591132,6.39934178215723)) ;
#74448 = CARTESIAN_POINT('Ctrl Pts',(76.7463946772425,244.532060709051,6.56568157766891)) ;
#74449 = CARTESIAN_POINT('Ctrl Pts',(76.9242915764346,244.637444476803,6.83606210006298)) ;
#74450 = CARTESIAN_POINT('Ctrl Pts',(77.0245312006819,244.746635057221,7.06215662103542)) ;
#74451 = CARTESIAN_POINT('Ctrl Pts',(77.0657108925549,244.806016366157,7.17608503411329)) ;
#74452 = CARTESIAN_POINT('Ctrl Pts',(75.6132936573898,245.270182723559,7.17267980084142)) ;
#74453 = CARTESIAN_POINT('Ctrl Pts',(75.613954293283,245.196657079323,7.05719005365003)) ;
#74454 = CARTESIAN_POINT('Ctrl Pts',(75.6357650439128,245.046802655971,6.82780162607624)) ;
#74455 = CARTESIAN_POINT('Ctrl Pts',(75.725378892112,244.854402356644,6.55479620028639)) ;
#74456 = CARTESIAN_POINT('Ctrl Pts',(75.8386073677345,244.71973854857,6.38660152646554)) ;
#74457 = CARTESIAN_POINT('Ctrl Pts',(75.9242311476023,244.645229370074,6.3054545117881)) ;
#74458 = CARTESIAN_POINT('Ctrl Pts',(76.0367475875534,244.565135771641,6.22919334486037)) ;
#74459 = CARTESIAN_POINT('Ctrl Pts',(76.2040215237222,244.492128423453,6.19617065335378)) ;
#74460 = CARTESIAN_POINT('Ctrl Pts',(76.3747470820875,244.465713468591,6.24747159564971)) ;
#74461 = CARTESIAN_POINT('Ctrl Pts',(76.4823449745696,244.464080466568,6.30580912198637)) ;
#74462 = CARTESIAN_POINT('Ctrl Pts',(76.5953524244594,244.474228894419,6.3872835116958)) ;
#74463 = CARTESIAN_POINT('Ctrl Pts',(76.7660596886604,244.51647055355,6.55517467213211)) ;
#74464 = CARTESIAN_POINT('Ctrl Pts',(76.9516452996115,244.61953353759,6.8283289406814)) ;
#74465 = CARTESIAN_POINT('Ctrl Pts',(77.0572892331031,244.727687124622,7.0571868958925)) ;
#74466 = CARTESIAN_POINT('Ctrl Pts',(77.1010421843896,244.786783924096,7.17267980084139)) ;
#74467 = CARTESIAN_POINT('Ctrl Pts',(77.1010421843896,244.786783924096,7.17267980084139)) ;
#74468 = CARTESIAN_POINT('Ctrl Pts',(77.0791876069748,244.75726510214,7.11499115223938)) ;
#74469 = CARTESIAN_POINT('Ctrl Pts',(77.0550394100041,244.728960426818,7.05749126113466)) ;
#74470 = CARTESIAN_POINT('Ctrl Pts',(77.0284135534917,244.702086718557,7.0004437744973)) ;
#74471 = CARTESIAN_POINT('Ctrl Pts',(77.0103872443349,244.683892608141,6.96182133129954)) ;
#74472 = CARTESIAN_POINT('Ctrl Pts',(76.9912256834656,244.66635418934,6.9234062563154)) ;
#74473 = CARTESIAN_POINT('Ctrl Pts',(76.9708780595307,244.649535148678,6.88527933317742)) ;
#74474 = CARTESIAN_POINT('Ctrl Pts',(76.9611711165242,244.641511535225,6.86709068023696)) ;
#74475 = CARTESIAN_POINT('Ctrl Pts',(76.9511945473649,244.633651670802,6.84896784774311)) ;
#74476 = CARTESIAN_POINT('Ctrl Pts',(76.9409391607941,244.62595933754,6.8309125757743)) ;
#74477 = CARTESIAN_POINT('Ctrl Pts',(76.8773913582901,244.578293569745,6.7190325555223)) ;
#74478 = CARTESIAN_POINT('Ctrl Pts',(76.8031623325145,244.537078339014,6.60978933753953)) ;
#74479 = CARTESIAN_POINT('Ctrl Pts',(76.7134007239805,244.507249358531,6.50942641939294)) ;
#74480 = CARTESIAN_POINT('Ctrl Pts',(76.6685028298768,244.492329189109,6.45922585208486)) ;
#74481 = CARTESIAN_POINT('Ctrl Pts',(76.6197251017638,244.480261484262,6.41125670179517)) ;
#74482 = CARTESIAN_POINT('Ctrl Pts',(76.565812191839,244.472857592713,6.36812019895627)) ;
#74483 = CARTESIAN_POINT('Ctrl Pts',(76.5503252435035,244.470730761012,6.35572886649482)) ;
#74484 = CARTESIAN_POINT('Ctrl Pts',(76.5344145188346,244.4689887049,6.34373617049952)) ;
#74485 = CARTESIAN_POINT('Ctrl Pts',(76.5180884880173,244.467694881079,6.33226414275337)) ;
#74486 = CARTESIAN_POINT('Ctrl Pts',(76.5059905865715,244.466736132854,6.32376315052751)) ;
#74487 = CARTESIAN_POINT('Ctrl Pts',(76.493659107157,244.466023104738,6.31554422546924)) ;
#74488 = CARTESIAN_POINT('Ctrl Pts',(76.4810997783083,244.465582306053,6.30765948836638)) ;
#74489 = CARTESIAN_POINT('Ctrl Pts',(76.4515882934318,244.464546532256,6.28913220059743)) ;
#74490 = CARTESIAN_POINT('Ctrl Pts',(76.420820949984,244.465016556187,6.27245603170864)) ;
#74491 = CARTESIAN_POINT('Ctrl Pts',(76.3887570669136,244.467406750174,6.25836859846688)) ;
#74492 = CARTESIAN_POINT('Ctrl Pts',(76.375058444912,244.468427910458,6.25235003787867)) ;
#74493 = CARTESIAN_POINT('Ctrl Pts',(76.3611235725264,244.469799107948,6.24680344963583)) ;
#74494 = CARTESIAN_POINT('Ctrl Pts',(76.3470386175973,244.471538328129,6.24181324805731)) ;
#74495 = CARTESIAN_POINT('Ctrl Pts',(76.3395945070502,244.472457532157,6.23917585146004)) ;
#74496 = CARTESIAN_POINT('Ctrl Pts',(76.3321107808768,244.473479158553,6.23669452539473)) ;
#74497 = CARTESIAN_POINT('Ctrl Pts',(76.3245924379661,244.47460686297,6.23437907245424)) ;
#74498 = CARTESIAN_POINT('Ctrl Pts',(76.3185272600237,244.475516601731,6.23251115630993)) ;
#74499 = CARTESIAN_POINT('Ctrl Pts',(76.3124366187017,244.476495831121,6.23075031208375)) ;
#74500 = CARTESIAN_POINT('Ctrl Pts',(76.3063237562274,244.477546881836,6.22910275882576)) ;
#74501 = CARTESIAN_POINT('Ctrl Pts',(76.2904956240092,244.480268384201,6.22483672291973)) ;
#74502 = CARTESIAN_POINT('Ctrl Pts',(76.27452491071,244.483470288184,6.22133192052908)) ;
#74503 = CARTESIAN_POINT('Ctrl Pts',(76.2585136290706,244.487187448996,6.21871267557031)) ;
#74504 = CARTESIAN_POINT('Ctrl Pts',(76.2518649603391,244.488730996316,6.21762503671356)) ;
#74505 = CARTESIAN_POINT('Ctrl Pts',(76.2452083557863,244.49036366916,6.21669005024627)) ;
#74506 = CARTESIAN_POINT('Ctrl Pts',(76.2385549428924,244.49208707673,6.21591725061576)) ;
#74507 = CARTESIAN_POINT('Ctrl Pts',(76.2196778307588,244.496976741398,6.21372465780441)) ;
#74508 = CARTESIAN_POINT('Ctrl Pts',(76.2008317612361,244.502596703282,6.21284053128981)) ;
#74509 = CARTESIAN_POINT('Ctrl Pts',(76.1822313129452,244.508829679511,6.21317763161947)) ;
#74510 = CARTESIAN_POINT('Ctrl Pts',(76.1652229263382,244.514529158779,6.21348587863817)) ;
#74511 = CARTESIAN_POINT('Ctrl Pts',(76.1484150941123,244.520741581786,6.21481314442454)) ;
#74512 = CARTESIAN_POINT('Ctrl Pts',(76.131925940963,244.527386914516,6.21708344522214)) ;
#74513 = CARTESIAN_POINT('Ctrl Pts',(76.112482770511,244.535222752768,6.21976046841341)) ;
#74514 = CARTESIAN_POINT('Ctrl Pts',(76.0934767109316,244.543661575844,6.22374740248841)) ;
#74515 = CARTESIAN_POINT('Ctrl Pts',(76.0751055400727,244.552621536501,6.22899833985716)) ;
#74516 = CARTESIAN_POINT('Ctrl Pts',(76.0686609549915,244.555764680137,6.23084036249629)) ;
#74517 = CARTESIAN_POINT('Ctrl Pts',(76.0622949393628,244.55897191764,6.23283808866089)) ;
#74518 = CARTESIAN_POINT('Ctrl Pts',(76.0560174782507,244.562239562755,6.23498999122571)) ;
#74519 = CARTESIAN_POINT('Ctrl Pts',(76.0372400752442,244.572013878853,6.24142685176041)) ;
#74520 = CARTESIAN_POINT('Ctrl Pts',(76.0191213517595,244.58226496701,6.24908226480483)) ;
#74521 = CARTESIAN_POINT('Ctrl Pts',(76.0019017462595,244.592874457357,6.25787634700995)) ;
#74522 = CARTESIAN_POINT('Ctrl Pts',(75.9810929668374,244.605695340181,6.26850342652273)) ;
#74523 = CARTESIAN_POINT('Ctrl Pts',(75.9615970994002,244.619039772416,6.28079415544679)) ;
#74524 = CARTESIAN_POINT('Ctrl Pts',(75.9432200150816,244.632701746941,6.2942409454276)) ;
#74525 = CARTESIAN_POINT('Ctrl Pts',(75.9374338121325,244.637003351913,6.29847479746273)) ;
#74526 = CARTESIAN_POINT('Ctrl Pts',(75.9317588233289,244.641336263499,6.30282306611641)) ;
#74527 = CARTESIAN_POINT('Ctrl Pts',(75.9261898110665,244.645693623271,6.30726943863187)) ;
#74528 = CARTESIAN_POINT('Ctrl Pts',(75.9167432121812,244.65308492141,6.31481172722269)) ;
#74529 = CARTESIAN_POINT('Ctrl Pts',(75.9076013902148,244.66054663505,6.32263637113672)) ;
#74530 = CARTESIAN_POINT('Ctrl Pts',(75.8987788178093,244.668063552107,6.33072043970214)) ;
#74531 = CARTESIAN_POINT('Ctrl Pts',(75.8858753172798,244.679057459413,6.3425438374846)) ;
#74532 = CARTESIAN_POINT('Ctrl Pts',(75.8735947782667,244.690167058658,6.3548936163373)) ;
#74533 = CARTESIAN_POINT('Ctrl Pts',(75.8619259387552,244.701347996727,6.36768119039541)) ;
#74534 = CARTESIAN_POINT('Ctrl Pts',(75.8245244921894,244.737185601429,6.40866845115694)) ;
#74535 = CARTESIAN_POINT('Ctrl Pts',(75.7934068363604,244.77375673915,6.45415443988251)) ;
#74536 = CARTESIAN_POINT('Ctrl Pts',(75.7667224839704,244.81034688431,6.50170616086635)) ;
#74537 = CARTESIAN_POINT('Ctrl Pts',(75.7653632951594,244.812210632591,6.50412824577071)) ;
#74538 = CARTESIAN_POINT('Ctrl Pts',(75.7640156635346,244.814074532772,6.50655587030767)) ;
#74539 = CARTESIAN_POINT('Ctrl Pts',(75.7626793458367,244.815938489662,6.50898871181187)) ;
#74540 = CARTESIAN_POINT('Ctrl Pts',(75.7322216671701,244.8584222494,6.5644386283242)) ;
#74541 = CARTESIAN_POINT('Ctrl Pts',(75.7076465982727,244.900934559548,6.62259902957464)) ;
#74542 = CARTESIAN_POINT('Ctrl Pts',(75.6878151675965,244.943275976356,6.68241852239716)) ;
#74543 = CARTESIAN_POINT('Ctrl Pts',(75.6717433251411,244.977590423529,6.73089759988326)) ;
#74544 = CARTESIAN_POINT('Ctrl Pts',(75.6587853917721,245.011792806485,6.7804659724872)) ;
#74545 = CARTESIAN_POINT('Ctrl Pts',(75.6483110969455,245.045782320021,6.83056547755719)) ;
#74546 = CARTESIAN_POINT('Ctrl Pts',(75.6457208412848,245.054187805192,6.84295490603485)) ;
#74547 = CARTESIAN_POINT('Ctrl Pts',(75.6432823934182,245.062580296907,6.85537683699444)) ;
#74548 = CARTESIAN_POINT('Ctrl Pts',(75.6409922292331,245.070959185311,6.8678283405692)) ;
#74549 = CARTESIAN_POINT('Ctrl Pts',(75.6258122378237,245.126497323067,6.95036116442963)) ;
#74550 = CARTESIAN_POINT('Ctrl Pts',(75.6172239927498,245.181498349157,7.03431234930241)) ;
#74551 = CARTESIAN_POINT('Ctrl Pts',(75.6143557917654,245.23576402968,7.11884007619928)) ;
#74552 = CARTESIAN_POINT('Ctrl Pts',(75.6137476157658,245.24727057496,7.13676341388841)) ;
#74553 = CARTESIAN_POINT('Ctrl Pts',(75.6133964347853,245.258744086487,7.15471266410403)) ;
#74554 = CARTESIAN_POINT('Ctrl Pts',(75.6132936573898,245.270182723559,7.17267980084131)) ;
#74555 = CARTESIAN_POINT('Ctrl Pts',(75.7824688237379,245.10414043955,7.27867958884206)) ;
#74556 = CARTESIAN_POINT('Ctrl Pts',(75.7826706984503,245.049050470116,7.16318984165068)) ;
#74557 = CARTESIAN_POINT('Ctrl Pts',(75.7979890932181,244.936852228027,6.93380141407689)) ;
#74558 = CARTESIAN_POINT('Ctrl Pts',(75.8624126704611,244.793118819323,6.66079598828704)) ;
#74559 = CARTESIAN_POINT('Ctrl Pts',(75.9441595048601,244.69286791716,6.49260131446618)) ;
#74560 = CARTESIAN_POINT('Ctrl Pts',(76.0060804700526,244.637579571816,6.41145429978875)) ;
#74561 = CARTESIAN_POINT('Ctrl Pts',(76.087527546102,244.578310960323,6.33519313286103)) ;
#74562 = CARTESIAN_POINT('Ctrl Pts',(76.2088559391776,244.524823920756,6.30217044135443)) ;
#74563 = CARTESIAN_POINT('Ctrl Pts',(76.3331068362906,244.506355590964,6.35347138365035)) ;
#74564 = CARTESIAN_POINT('Ctrl Pts',(76.4115789956862,244.505971060786,6.41180890998702)) ;
#74565 = CARTESIAN_POINT('Ctrl Pts',(76.4941307169281,244.514452134586,6.49328329969644)) ;
#74566 = CARTESIAN_POINT('Ctrl Pts',(76.6191536305483,244.547394262234,6.66117446013279)) ;
#74567 = CARTESIAN_POINT('Ctrl Pts',(76.7557559389564,244.625871137754,6.93432872868204)) ;
#74568 = CARTESIAN_POINT('Ctrl Pts',(76.8340341124954,244.7074402845,7.16318668389314)) ;
#74569 = CARTESIAN_POINT('Ctrl Pts',(76.8665793939902,244.751891562381,7.27867958884203)) ;
#74570 = CARTESIAN_POINT('Origin',(77.0279509268838,244.633742383918,16.0213203435596)) ;
#74571 = CARTESIAN_POINT('',(76.8665793939902,244.751891562381,16.0254384350469)) ;
#74572 = CARTESIAN_POINT('',(76.8665793939902,244.751891562381,16.0213203435596)) ;
#74573 = CARTESIAN_POINT('Ctrl Pts',(76.8665793939902,244.751891562381,16.0254384350469)) ;
#74574 = CARTESIAN_POINT('Ctrl Pts',(76.8784031342209,244.768040765536,16.0294645582753)) ;
#74575 = CARTESIAN_POINT('Ctrl Pts',(76.892136277013,244.78172134422,16.0362204083692)) ;
#74576 = CARTESIAN_POINT('Ctrl Pts',(76.9259362350405,244.807425329643,16.0560502171909)) ;
#74577 = CARTESIAN_POINT('Ctrl Pts',(76.9464127977525,244.817621347006,16.070223718736)) ;
#74578 = CARTESIAN_POINT('Ctrl Pts',(76.9916081849013,244.832126442816,16.1046945816754)) ;
#74579 = CARTESIAN_POINT('Ctrl Pts',(77.0165903206712,244.834833453147,16.1258672215758)) ;
#74580 = CARTESIAN_POINT('Ctrl Pts',(77.0656749169652,244.831784668204,16.1708720249623)) ;
#74581 = CARTESIAN_POINT('Ctrl Pts',(77.0900369538065,244.825441284576,16.1951765216978)) ;
#74582 = CARTESIAN_POINT('Ctrl Pts',(77.1129191197796,244.814797252538,16.2199877856629)) ;
#74583 = CARTESIAN_POINT('Ctrl Pts',(77.1135321137367,244.814508309052,16.2206540664846)) ;
#74584 = CARTESIAN_POINT('Ctrl Pts',(77.1141436199122,244.814216259225,16.2213203435596)) ;
#74585 = CARTESIAN_POINT('Origin',(69.4298369914177,242.164965512063,16.0213203435596)) ;
#74586 = CARTESIAN_POINT('',(69.4909429592658,242.355402012486,16.0254384350469)) ;
#74587 = CARTESIAN_POINT('',(69.4909429592658,242.355402012486,16.0213203435596)) ;
#74588 = CARTESIAN_POINT('Ctrl Pts',(69.254025755637,242.26030915041,16.2213203435596)) ;
#74589 = CARTESIAN_POINT('Ctrl Pts',(69.2543488119456,242.260904857998,16.220654066481)) ;
#74590 = CARTESIAN_POINT('Ctrl Pts',(69.2546748977555,242.261498926998,16.2199877856714)) ;
#74591 = CARTESIAN_POINT('Ctrl Pts',(69.2650804716231,242.280229657494,16.1989219659808)) ;
#74592 = CARTESIAN_POINT('Ctrl Pts',(69.2780408691307,242.296910122432,16.1784289743361)) ;
#74593 = CARTESIAN_POINT('Ctrl Pts',(69.3084414776869,242.32519767757,16.1396302534792)) ;
#74594 = CARTESIAN_POINT('Ctrl Pts',(69.3258200011823,242.337155324715,16.1210537744217)) ;
#74595 = CARTESIAN_POINT('Ctrl Pts',(69.3661861047741,242.355940900472,16.0855257632557)) ;
#74596 = CARTESIAN_POINT('Ctrl Pts',(69.3897101386423,242.362560440169,16.0684876094517)) ;
#74597 = CARTESIAN_POINT('Ctrl Pts',(69.4342851322535,242.365828386096,16.0440628922209)) ;
#74598 = CARTESIAN_POINT('Ctrl Pts',(69.4544003621822,242.364551935653,16.0353723462058)) ;
#74599 = CARTESIAN_POINT('Ctrl Pts',(69.4802111102619,242.358597477058,16.027919277044)) ;
#74600 = CARTESIAN_POINT('Ctrl Pts',(69.4855993537817,242.357116632237,16.0265673132425)) ;
#74601 = CARTESIAN_POINT('Ctrl Pts',(69.4909429592658,242.355402012486,16.0254384350468)) ;
#74602 = CARTESIAN_POINT('Origin',(74.5283628290597,239.4,7.2786795888419)) ;
#74603 = CARTESIAN_POINT('Origin',(74.5283628290597,239.4,7.17267980084128)) ;
#74604 = CARTESIAN_POINT('Origin',(75.5824701665474,245.103407553477,16.0213203435596)) ;
#74605 = CARTESIAN_POINT('',(75.7824688237379,245.10414043955,16.0254384350469)) ;
#74606 = CARTESIAN_POINT('',(75.7824688237379,245.10414043955,16.0213203435596)) ;
#74607 = CARTESIAN_POINT('Ctrl Pts',(75.6188186954262,245.300076779459,16.2213203435596)) ;
#74608 = CARTESIAN_POINT('Ctrl Pts',(75.6194850769117,245.299953618417,16.2206540664686)) ;
#74609 = CARTESIAN_POINT('Ctrl Pts',(75.6201508361727,245.299827069798,16.2199877856852)) ;
#74610 = CARTESIAN_POINT('Ctrl Pts',(75.6411803184818,245.295718895031,16.1989219658462)) ;
#74611 = CARTESIAN_POINT('Ctrl Pts',(75.6610493665444,245.288547371652,16.1784289743552)) ;
#74612 = CARTESIAN_POINT('Ctrl Pts',(75.6973467348523,245.268376010071,16.1396302535203)) ;
#74613 = CARTESIAN_POINT('Ctrl Pts',(75.7140893921785,245.25554316825,16.1210537744717)) ;
#74614 = CARTESIAN_POINT('Ctrl Pts',(75.744429348427,245.222957784567,16.085525763304)) ;
#74615 = CARTESIAN_POINT('Ctrl Pts',(75.7579942310408,245.202630649128,16.0684876094913)) ;
#74616 = CARTESIAN_POINT('Ctrl Pts',(75.7748766628741,245.161247161817,16.0440628922463)) ;
#74617 = CARTESIAN_POINT('Ctrl Pts',(75.779878634262,245.141721996436,16.0353723462253)) ;
#74618 = CARTESIAN_POINT('Ctrl Pts',(75.7821915674168,245.115334487368,16.027919277052)) ;
#74619 = CARTESIAN_POINT('Ctrl Pts',(75.782448259119,245.109752357025,16.0265673132458)) ;
#74620 = CARTESIAN_POINT('Ctrl Pts',(75.7824688237379,245.10414043955,16.0254384350468)) ;
#74621 = CARTESIAN_POINT('Origin',(74.5283628290597,239.4,16.2213203435596)) ;
#74622 = CARTESIAN_POINT('',(76.8407687665841,244.719095673148,16.0213203435596)) ;
#74623 = CARTESIAN_POINT('Ctrl Pts',(76.8665793939903,244.751891562381,16.0254384350468)) ;
#74624 = CARTESIAN_POINT('Ctrl Pts',(76.8600592573189,244.742986172915,16.0232182514845)) ;
#74625 = CARTESIAN_POINT('Ctrl Pts',(76.8531765412925,244.734103685059,16.0218983740811)) ;
#74626 = CARTESIAN_POINT('Ctrl Pts',(76.8442502902958,244.723244459325,16.0213707571522)) ;
#74627 = CARTESIAN_POINT('Ctrl Pts',(76.8425158171676,244.721163313731,16.0213203435596)) ;
#74628 = CARTESIAN_POINT('Ctrl Pts',(76.8407687665841,244.719095673148,16.0213203435596)) ;
#74629 = CARTESIAN_POINT('',(75.7840731199179,245.062436901673,16.0213203435596)) ;
#74630 = CARTESIAN_POINT('Origin',(74.5283628290597,239.4,16.0213203435596)) ;
#74631 = CARTESIAN_POINT('Ctrl Pts',(75.784073119918,245.062436901673,16.0213203435596)) ;
#74632 = CARTESIAN_POINT('Ctrl Pts',(75.7832477134999,245.073687280317,16.0213203435596)) ;
#74633 = CARTESIAN_POINT('Ctrl Pts',(75.7827408846003,245.084964948541,16.0221950109068)) ;
#74634 = CARTESIAN_POINT('Ctrl Pts',(75.7825057064519,245.098841078978,16.0244263118334)) ;
#74635 = CARTESIAN_POINT('Ctrl Pts',(75.7824785074899,245.101497822276,16.0249068532759)) ;
#74636 = CARTESIAN_POINT('Ctrl Pts',(75.7824688237379,245.10414043955,16.0254384350468)) ;
#74637 = CARTESIAN_POINT('Origin',(70.3231932313898,243.3945648893,16.0213203435596)) ;
#74638 = CARTESIAN_POINT('',(70.1609601392448,243.277601545414,16.0254384350468)) ;
#74639 = CARTESIAN_POINT('',(70.1609601392448,243.277601545414,16.0213203435596)) ;
#74640 = CARTESIAN_POINT('Ctrl Pts',(70.1609601392448,243.277601545414,16.0254384350468)) ;
#74641 = CARTESIAN_POINT('Ctrl Pts',(70.1492550710199,243.293836968828,16.0294645582753)) ;
#74642 = CARTESIAN_POINT('Ctrl Pts',(70.140487842024,243.311125495076,16.0362204083692)) ;
#74643 = CARTESIAN_POINT('Ctrl Pts',(70.1264866606326,243.351214133727,16.0560502171909)) ;
#74644 = CARTESIAN_POINT('Ctrl Pts',(70.1231172777434,243.373839244766,16.070223718736)) ;
#74645 = CARTESIAN_POINT('Ctrl Pts',(70.1232882545508,243.421304933331,16.1046945816756)) ;
#74646 = CARTESIAN_POINT('Ctrl Pts',(70.1284336392439,243.445900868542,16.1258672215763)) ;
#74647 = CARTESIAN_POINT('Ctrl Pts',(70.1465011804487,243.491640967338,16.1708720249636)) ;
#74648 = CARTESIAN_POINT('Ctrl Pts',(70.1600623801825,243.512850427881,16.1951765217044)) ;
#74649 = CARTESIAN_POINT('Ctrl Pts',(70.1772564343691,243.531323474151,16.2199877856641)) ;
#74650 = CARTESIAN_POINT('Ctrl Pts',(70.1777206615032,243.5318171776,16.2206540664853)) ;
#74651 = CARTESIAN_POINT('Ctrl Pts',(70.1781873831942,243.532308506173,16.2213203435596)) ;
#74652 = CARTESIAN_POINT('Origin',(74.5283628290597,239.4,16.2213203435596)) ;
#74653 = CARTESIAN_POINT('',(70.1841749609036,243.242919692911,16.0213203435596)) ;
#74654 = CARTESIAN_POINT('Ctrl Pts',(70.1609601392449,243.277601545414,16.0254384350468)) ;
#74655 = CARTESIAN_POINT('Ctrl Pts',(70.1674148348898,243.268648610259,16.0232182514845)) ;
#74656 = CARTESIAN_POINT('Ctrl Pts',(70.1737357066263,243.259357918633,16.0218983740811)) ;
#74657 = CARTESIAN_POINT('Ctrl Pts',(70.1813050807688,243.247512864158,16.0213707571522)) ;
#74658 = CARTESIAN_POINT('Ctrl Pts',(70.1827483861738,243.245220172831,16.0213203435596)) ;
#74659 = CARTESIAN_POINT('Ctrl Pts',(70.1841749609038,243.242919692911,16.0213203435596)) ;
#74660 = CARTESIAN_POINT('',(69.5311011354998,242.344040686892,16.0213203435596)) ;
#74661 = CARTESIAN_POINT('Origin',(74.5283628290597,239.4,16.0213203435596)) ;
#74662 = CARTESIAN_POINT('Ctrl Pts',(69.5311011355,242.344040686893,16.0213203435596)) ;
#74663 = CARTESIAN_POINT('Ctrl Pts',(69.5201463249695,242.346732236934,16.0213203435596)) ;
#74664 = CARTESIAN_POINT('Ctrl Pts',(69.5092640063738,242.349735205145,16.0221950109068)) ;
#74665 = CARTESIAN_POINT('Ctrl Pts',(69.4959943480554,242.353799497556,16.0244263118334)) ;
#74666 = CARTESIAN_POINT('Ctrl Pts',(69.4934592300887,242.354594608634,16.0249068532759)) ;
#74667 = CARTESIAN_POINT('Ctrl Pts',(69.4909429592658,242.355402012486,16.0254384350468)) ;
#74668 = CARTESIAN_POINT('Ctrl Pts',(73.9584121733008,245.2125,7.27867958884205)) ;
#74669 = CARTESIAN_POINT('Ctrl Pts',(73.9756279482132,245.160168574929,7.163189547307)) ;
#74670 = CARTESIAN_POINT('Ctrl Pts',(74.0248679112718,245.058195067006,6.93380047883313)) ;
#74671 = CARTESIAN_POINT('Ctrl Pts',(74.1305548836119,244.941404186597,6.6607943976457)) ;
#74672 = CARTESIAN_POINT('Ctrl Pts',(74.2392805618495,244.871321000177,6.49259951597657)) ;
#74673 = CARTESIAN_POINT('Ctrl Pts',(74.3152563853318,244.837873343214,6.41145261667884)) ;
#74674 = CARTESIAN_POINT('Ctrl Pts',(74.4110327691165,244.806674217527,6.33519178586455)) ;
#74675 = CARTESIAN_POINT('Ctrl Pts',(74.5429519916097,244.793298107963,6.30217046564658)) ;
#74676 = CARTESIAN_POINT('Ctrl Pts',(74.6668285233745,244.814129955813,6.35347296267426)) ;
#74677 = CARTESIAN_POINT('Ctrl Pts',(74.7415786175593,244.838013779146,6.41181121705515)) ;
#74678 = CARTESIAN_POINT('Ctrl Pts',(74.8174689638568,244.871590004575,6.49328644843118)) ;
#74679 = CARTESIAN_POINT('Ctrl Pts',(74.9261925907657,244.941554190683,6.66117794267636)) ;
#74680 = CARTESIAN_POINT('Ctrl Pts',(75.0318583408227,245.058403735858,6.93433474994977)) ;
#74681 = CARTESIAN_POINT('Ctrl Pts',(75.0810977099062,245.160168574929,7.16318954730704)) ;
#74682 = CARTESIAN_POINT('Ctrl Pts',(75.0983134848186,245.2125,7.27867958884208)) ;
#74683 = CARTESIAN_POINT('Ctrl Pts',(73.9442186760216,245.255644496436,7.24979207607672)) ;
#74684 = CARTESIAN_POINT('Ctrl Pts',(73.9582438127982,245.199332275759,7.13558318832877)) ;
#74685 = CARTESIAN_POINT('Ctrl Pts',(74.0030866391885,245.088284257301,6.90837475287202)) ;
#74686 = CARTESIAN_POINT('Ctrl Pts',(74.1089313625797,244.958729891281,6.63742123865064)) ;
#74687 = CARTESIAN_POINT('Ctrl Pts',(74.2219239380421,244.880176771883,6.47033490089512)) ;
#74688 = CARTESIAN_POINT('Ctrl Pts',(74.301852720505,244.842534564145,6.38969559217932)) ;
#74689 = CARTESIAN_POINT('Ctrl Pts',(74.4032076200201,244.807328560718,6.31389543197594)) ;
#74690 = CARTESIAN_POINT('Ctrl Pts',(74.5439426909897,244.792181977109,6.28106451887594)) ;
#74691 = CARTESIAN_POINT('Ctrl Pts',(74.6757758209022,244.81575136187,6.33206751004191)) ;
#74692 = CARTESIAN_POINT('Ctrl Pts',(74.754889298075,244.842695948385,6.3900521489566)) ;
#74693 = CARTESIAN_POINT('Ctrl Pts',(74.834715417332,244.880485650139,6.47101811980182)) ;
#74694 = CARTESIAN_POINT('Ctrl Pts',(74.9477489964978,244.958901579953,6.63780263189585)) ;
#74695 = CARTESIAN_POINT('Ctrl Pts',(75.0535155836388,245.088524548487,6.90890516875891)) ;
#74696 = CARTESIAN_POINT('Ctrl Pts',(75.0984818453212,245.199332275759,7.13558318832881)) ;
#74697 = CARTESIAN_POINT('Ctrl Pts',(75.1125069820978,245.255644496436,7.24979207607676)) ;
#74698 = CARTESIAN_POINT('Ctrl Pts',(73.8813809317722,245.318035047894,7.19960839071961)) ;
#74699 = CARTESIAN_POINT('Ctrl Pts',(73.8957857168573,245.253001355885,7.08747698484384)) ;
#74700 = CARTESIAN_POINT('Ctrl Pts',(73.9438000409784,245.124940024636,6.86386231950441)) ;
#74701 = CARTESIAN_POINT('Ctrl Pts',(74.0607081520988,244.976082733332,6.59636871271614)) ;
#74702 = CARTESIAN_POINT('Ctrl Pts',(74.1864485595767,244.886061710793,6.4311762697182)) ;
#74703 = CARTESIAN_POINT('Ctrl Pts',(74.2755814288091,244.842971168061,6.35140872171606)) ;
#74704 = CARTESIAN_POINT('Ctrl Pts',(74.3886668491307,244.802699316777,6.27640300071364)) ;
#74705 = CARTESIAN_POINT('Ctrl Pts',(74.5458063775715,244.785389925441,6.24390250673374)) ;
#74706 = CARTESIAN_POINT('Ctrl Pts',(74.6930323705689,244.812330433283,6.29438711209566)) ;
#74707 = CARTESIAN_POINT('Ctrl Pts',(74.7813025349178,244.843154077251,6.35176231641292)) ;
#74708 = CARTESIAN_POINT('Ctrl Pts',(74.8703326302217,244.886412364113,6.43185373754292)) ;
#74709 = CARTESIAN_POINT('Ctrl Pts',(74.9960610602972,244.97627786093,6.59674657937938)) ;
#74710 = CARTESIAN_POINT('Ctrl Pts',(75.1129561491309,245.125210454642,6.86438826993789)) ;
#74711 = CARTESIAN_POINT('Ctrl Pts',(75.1609399412621,245.253001355885,7.08747698484388)) ;
#74712 = CARTESIAN_POINT('Ctrl Pts',(75.1753447263472,245.318035047894,7.19960839071964)) ;
#74713 = CARTESIAN_POINT('Ctrl Pts',(73.7857523481751,245.325510764496,7.17608503411331)) ;
#74714 = CARTESIAN_POINT('Ctrl Pts',(73.8065662128101,245.256312274755,7.06215944566086)) ;
#74715 = CARTESIAN_POINT('Ctrl Pts',(73.8681806184035,245.121213402276,6.83553876784966)) ;
#74716 = CARTESIAN_POINT('Ctrl Pts',(74.0048230497562,244.966091331847,6.56530464002508)) ;
#74717 = CARTESIAN_POINT('Ctrl Pts',(74.1472039166702,244.872894481501,6.39866345547885)) ;
#74718 = CARTESIAN_POINT('Ctrl Pts',(74.2471300500745,244.82839597854,6.31823906006952)) ;
#74719 = CARTESIAN_POINT('Ctrl Pts',(74.373344481406,244.786877403095,6.24264091507692)) ;
#74720 = CARTESIAN_POINT('Ctrl Pts',(74.5476677047595,244.769070794076,6.20989751501573)) ;
#74721 = CARTESIAN_POINT('Ctrl Pts',(74.7112510718069,244.796800388377,6.26076462735167)) ;
#74722 = CARTESIAN_POINT('Ctrl Pts',(74.8097608852416,244.828583281404,6.31859474911539)) ;
#74723 = CARTESIAN_POINT('Ctrl Pts',(74.9095746445357,244.873253186347,6.39934495813431)) ;
#74724 = CARTESIAN_POINT('Ctrl Pts',(75.0519449212146,244.966291180321,6.56568507344858)) ;
#74725 = CARTESIAN_POINT('Ctrl Pts',(75.1885693996538,245.12149181155,6.83606809856267)) ;
#74726 = CARTESIAN_POINT('Ctrl Pts',(75.2501594453092,245.256312274755,7.0621594456609)) ;
#74727 = CARTESIAN_POINT('Ctrl Pts',(75.2709733099443,245.325510764496,7.17608503411335)) ;
#74728 = CARTESIAN_POINT('Ctrl Pts',(73.7462071414064,245.31813759476,7.17267980084142)) ;
#74729 = CARTESIAN_POINT('Ctrl Pts',(73.7695561765774,245.248414521712,7.05718975930637)) ;
#74730 = CARTESIAN_POINT('Ctrl Pts',(73.8366071882365,245.112634011735,6.82780069083249)) ;
#74731 = CARTESIAN_POINT('Ctrl Pts',(73.9812905940924,244.957342302858,6.55479460964506)) ;
#74732 = CARTESIAN_POINT('Ctrl Pts',(74.1305914868933,244.864258836729,6.38659972797594)) ;
#74733 = CARTESIAN_POINT('Ctrl Pts',(74.2350497606397,244.819855671617,6.30545282867821)) ;
#74734 = CARTESIAN_POINT('Ctrl Pts',(74.3668103693923,244.778451814907,6.22919199786392)) ;
#74735 = CARTESIAN_POINT('Ctrl Pts',(74.5484587576374,244.760708922492,6.19617067764595)) ;
#74736 = CARTESIAN_POINT('Ctrl Pts',(74.7189909128558,244.788344748346,6.24747317467362)) ;
#74737 = CARTESIAN_POINT('Ctrl Pts',(74.821826950362,244.820041650107,6.30581142905452)) ;
#74738 = CARTESIAN_POINT('Ctrl Pts',(74.926167092777,244.864615079948,6.38728666043055)) ;
#74739 = CARTESIAN_POINT('Ctrl Pts',(75.0754651947014,244.957540938993,6.55517815467573)) ;
#74740 = CARTESIAN_POINT('Ctrl Pts',(75.220119269038,245.112910324599,6.82833496194914)) ;
#74741 = CARTESIAN_POINT('Ctrl Pts',(75.287169481542,245.248414521712,7.05718975930641)) ;
#74742 = CARTESIAN_POINT('Ctrl Pts',(75.310518516713,245.31813759476,7.17267980084145)) ;
#74743 = CARTESIAN_POINT('Ctrl Pts',(75.3105185167129,245.31813759476,7.17267980084142)) ;
#74744 = CARTESIAN_POINT('Ctrl Pts',(75.287169481542,245.248414521712,7.05718975930639)) ;
#74745 = CARTESIAN_POINT('Ctrl Pts',(75.220119269038,245.1129103246,6.82833496194911)) ;
#74746 = CARTESIAN_POINT('Ctrl Pts',(75.0754651947014,244.957540938994,6.55517815467573)) ;
#74747 = CARTESIAN_POINT('Ctrl Pts',(74.926167092777,244.864615079948,6.38728666043055)) ;
#74748 = CARTESIAN_POINT('Ctrl Pts',(74.8218269503619,244.820041650108,6.30581142905452)) ;
#74749 = CARTESIAN_POINT('Ctrl Pts',(74.7189909128558,244.788344748345,6.24747317467363)) ;
#74750 = CARTESIAN_POINT('Ctrl Pts',(74.5484587576374,244.760708922493,6.19617067764596)) ;
#74751 = CARTESIAN_POINT('Ctrl Pts',(74.3668103693923,244.778451814907,6.22919199786392)) ;
#74752 = CARTESIAN_POINT('Ctrl Pts',(74.2350497606398,244.819855671617,6.3054528286782)) ;
#74753 = CARTESIAN_POINT('Ctrl Pts',(74.1305914868933,244.864258836729,6.38659972797596)) ;
#74754 = CARTESIAN_POINT('Ctrl Pts',(73.9812905940924,244.957342302859,6.55479460964504)) ;
#74755 = CARTESIAN_POINT('Ctrl Pts',(73.8366071882364,245.112634011734,6.82780069083246)) ;
#74756 = CARTESIAN_POINT('Ctrl Pts',(73.7695561765774,245.248414521712,7.05718975930628)) ;
#74757 = CARTESIAN_POINT('Ctrl Pts',(73.7462071414064,245.31813759476,7.17267980084129)) ;
#74758 = CARTESIAN_POINT('Ctrl Pts',(73.9584121733008,245.2125,7.27867958884205)) ;
#74759 = CARTESIAN_POINT('Ctrl Pts',(73.9756279482132,245.160168574929,7.163189547307)) ;
#74760 = CARTESIAN_POINT('Ctrl Pts',(74.0248679112718,245.058195067006,6.93380047883313)) ;
#74761 = CARTESIAN_POINT('Ctrl Pts',(74.1305548836119,244.941404186597,6.6607943976457)) ;
#74762 = CARTESIAN_POINT('Ctrl Pts',(74.2392805618495,244.871321000177,6.49259951597657)) ;
#74763 = CARTESIAN_POINT('Ctrl Pts',(74.3152563853318,244.837873343214,6.41145261667884)) ;
#74764 = CARTESIAN_POINT('Ctrl Pts',(74.4110327691165,244.806674217527,6.33519178586455)) ;
#74765 = CARTESIAN_POINT('Ctrl Pts',(74.5429519916097,244.793298107963,6.30217046564658)) ;
#74766 = CARTESIAN_POINT('Ctrl Pts',(74.6668285233745,244.814129955813,6.35347296267426)) ;
#74767 = CARTESIAN_POINT('Ctrl Pts',(74.7415786175593,244.838013779146,6.41181121705515)) ;
#74768 = CARTESIAN_POINT('Ctrl Pts',(74.8174689638568,244.871590004575,6.49328644843118)) ;
#74769 = CARTESIAN_POINT('Ctrl Pts',(74.9261925907657,244.941554190683,6.66117794267636)) ;
#74770 = CARTESIAN_POINT('Ctrl Pts',(75.0318583408227,245.058403735858,6.93433474994977)) ;
#74771 = CARTESIAN_POINT('Ctrl Pts',(75.0810977099062,245.160168574929,7.16318954730704)) ;
#74772 = CARTESIAN_POINT('Ctrl Pts',(75.0983134848186,245.2125,7.27867958884208)) ;
#74773 = CARTESIAN_POINT('Origin',(75.2882970367382,245.15,16.0213203435596)) ;
#74774 = CARTESIAN_POINT('',(75.0983134848186,245.2125,16.0254384350469)) ;
#74775 = CARTESIAN_POINT('',(75.0983134848186,245.2125,16.0213203435596)) ;
#74776 = CARTESIAN_POINT('Ctrl Pts',(75.0983134848186,245.2125,16.0254384350469)) ;
#74777 = CARTESIAN_POINT('Ctrl Pts',(75.1045681517916,245.231512541561,16.0294645582753)) ;
#74778 = CARTESIAN_POINT('Ctrl Pts',(75.1134016154265,245.248767319575,16.0362204083691)) ;
#74779 = CARTESIAN_POINT('Ctrl Pts',(75.1376043174404,245.283658023846,16.056050217191)) ;
#74780 = CARTESIAN_POINT('Ctrl Pts',(75.153927943199,245.299682618464,16.0702237187361)) ;
#74781 = CARTESIAN_POINT('Ctrl Pts',(75.1924289895435,245.32744392705,16.1046945816758)) ;
#74782 = CARTESIAN_POINT('Ctrl Pts',(75.2153519003623,245.337738351374,16.1258672215766)) ;
#74783 = CARTESIAN_POINT('Ctrl Pts',(75.2629762518785,245.350006759003,16.1708720249644)) ;
#74784 = CARTESIAN_POINT('Ctrl Pts',(75.288106139114,245.351502126069,16.1951765216962)) ;
#74785 = CARTESIAN_POINT('Ctrl Pts',(75.3131575589535,245.348450028194,16.2199877856658)) ;
#74786 = CARTESIAN_POINT('Ctrl Pts',(75.3138298392969,245.34836465216,16.2206540664851)) ;
#74787 = CARTESIAN_POINT('Ctrl Pts',(75.3145016645892,245.348275862069,16.2213203435596)) ;
#74788 = CARTESIAN_POINT('Origin',(70.5337979397592,243.60516959767,16.0213203435596)) ;
#74789 = CARTESIAN_POINT('',(70.6507612836456,243.767402689815,16.0254384350468)) ;
#74790 = CARTESIAN_POINT('',(70.6507612836456,243.767402689815,16.0213203435596)) ;
#74791 = CARTESIAN_POINT('Ctrl Pts',(70.3960543228868,243.750175445865,16.2213203435596)) ;
#74792 = CARTESIAN_POINT('Ctrl Pts',(70.3965456514624,243.750642167559,16.2206540664813)) ;
#74793 = CARTESIAN_POINT('Ctrl Pts',(70.3970393549119,243.751106394694,16.219987785665)) ;
#74794 = CARTESIAN_POINT('Ctrl Pts',(70.4127237578114,243.765704878851,16.1989219660085)) ;
#74795 = CARTESIAN_POINT('Ctrl Pts',(70.4302043754361,243.777563960622,16.1784289743291)) ;
#74796 = CARTESIAN_POINT('Ctrl Pts',(70.4678584075735,243.795072719583,16.1396302534698)) ;
#74797 = CARTESIAN_POINT('Ctrl Pts',(70.4880814817692,243.801074858721,16.1210537744116)) ;
#74798 = CARTESIAN_POINT('Ctrl Pts',(70.5322769897868,243.806467190948,16.0855257632468)) ;
#74799 = CARTESIAN_POINT('Ctrl Pts',(70.5566952257469,243.805493421069,16.0684876094444)) ;
#74800 = CARTESIAN_POINT('Ctrl Pts',(70.6000984147111,243.794826991786,16.0440628922162)) ;
#74801 = CARTESIAN_POINT('Ctrl Pts',(70.6188346903313,243.787397067379,16.0353723462022)) ;
#74802 = CARTESIAN_POINT('Ctrl Pts',(70.6415421415812,243.773758080939,16.0279192770425)) ;
#74803 = CARTESIAN_POINT('Ctrl Pts',(70.6462090594739,243.770684655006,16.0265673132419)) ;
#74804 = CARTESIAN_POINT('Ctrl Pts',(70.6507612836456,243.767402689815,16.0254384350468)) ;
#74805 = CARTESIAN_POINT('Origin',(74.5283628290597,239.4,7.2786795888419)) ;
#74806 = CARTESIAN_POINT('Origin',(74.5283628290597,239.4,7.17267980084126)) ;
#74807 = CARTESIAN_POINT('Origin',(73.7684286213812,245.15,16.0213203435596)) ;
#74808 = CARTESIAN_POINT('',(73.9584121733008,245.2125,16.0254384350469)) ;
#74809 = CARTESIAN_POINT('',(73.9584121733008,245.2125,16.0213203435596)) ;
#74810 = CARTESIAN_POINT('Ctrl Pts',(73.7422239935302,245.348275862069,16.2213203435596)) ;
#74811 = CARTESIAN_POINT('Ctrl Pts',(73.7428958188243,245.34836465216,16.2206540664833)) ;
#74812 = CARTESIAN_POINT('Ctrl Pts',(73.7435680991642,245.348450028194,16.2199877856676)) ;
#74813 = CARTESIAN_POINT('Ctrl Pts',(73.764837821366,245.351041389257,16.1989219660258)) ;
#74814 = CARTESIAN_POINT('Ctrl Pts',(73.7859505314575,245.350360738705,16.178428974329)) ;
#74815 = CARTESIAN_POINT('Ctrl Pts',(73.8267046736716,245.342393137473,16.1396302534651)) ;
#74816 = CARTESIAN_POINT('Ctrl Pts',(73.8465934532444,245.335362145269,16.1210537744048)) ;
#74817 = CARTESIAN_POINT('Ctrl Pts',(73.8855179036651,245.313747165846,16.0855257632396)) ;
#74818 = CARTESIAN_POINT('Ctrl Pts',(73.9047003039537,245.29860669048,16.0684876094385)) ;
#74819 = CARTESIAN_POINT('Ctrl Pts',(73.9335446516065,245.264465613545,16.0440628922123)) ;
#74820 = CARTESIAN_POINT('Ctrl Pts',(73.944335417002,245.247441771941,16.0353723461993)) ;
#74821 = CARTESIAN_POINT('Ctrl Pts',(73.9546893358739,245.223060495165,16.0279192770413)) ;
#74822 = CARTESIAN_POINT('Ctrl Pts',(73.9566584373223,245.217830895845,16.0265673132414)) ;
#74823 = CARTESIAN_POINT('Ctrl Pts',(73.9584121733008,245.2125,16.0254384350468)) ;
#74824 = CARTESIAN_POINT('Origin',(74.5283628290597,239.4,16.2213203435596)) ;
#74825 = CARTESIAN_POINT('',(75.083900606553,245.173333333333,16.0213203435596)) ;
#74826 = CARTESIAN_POINT('Ctrl Pts',(75.0983134848186,245.2125,16.0254384350468)) ;
#74827 = CARTESIAN_POINT('Ctrl Pts',(75.0948643830368,245.202015638281,16.0232182514845)) ;
#74828 = CARTESIAN_POINT('Ctrl Pts',(75.0910633708098,245.191441014105,16.0218983740811)) ;
#74829 = CARTESIAN_POINT('Ctrl Pts',(75.0859296869309,245.178354913455,16.0213707571522)) ;
#74830 = CARTESIAN_POINT('Ctrl Pts',(75.0849232143161,245.175839644704,16.0213203435596)) ;
#74831 = CARTESIAN_POINT('Ctrl Pts',(75.0839006065529,245.173333333333,16.0213203435596)) ;
#74832 = CARTESIAN_POINT('',(73.9728250515664,245.173333333333,16.0213203435596)) ;
#74833 = CARTESIAN_POINT('Origin',(74.5283628290597,239.4,16.0213203435596)) ;
#74834 = CARTESIAN_POINT('Ctrl Pts',(73.9728250515665,245.173333333333,16.0213203435596)) ;
#74835 = CARTESIAN_POINT('Ctrl Pts',(73.9685634852199,245.183778014643,16.0213203435596)) ;
#74836 = CARTESIAN_POINT('Ctrl Pts',(73.9645964711543,245.194347095752,16.0221950109068)) ;
#74837 = CARTESIAN_POINT('Ctrl Pts',(73.9600848433223,245.207471405981,16.0244263118334)) ;
#74838 = CARTESIAN_POINT('Ctrl Pts',(73.9592379967437,245.209989714065,16.0249068532759)) ;
#74839 = CARTESIAN_POINT('Ctrl Pts',(73.9584121733008,245.2125,16.0254384350468)) ;
#74840 = CARTESIAN_POINT('Origin',(71.7633973169968,244.498525837642,16.0213203435596)) ;
#74841 = CARTESIAN_POINT('',(71.5729608165738,244.437419869794,16.0254384350468)) ;
#74842 = CARTESIAN_POINT('',(71.5729608165738,244.437419869794,16.0213203435596)) ;
#74843 = CARTESIAN_POINT('Ctrl Pts',(71.5729608165738,244.437419869794,16.0254384350468)) ;
#74844 = CARTESIAN_POINT('Ctrl Pts',(71.5668456569106,244.456477740028,16.0294645582753)) ;
#74845 = CARTESIAN_POINT('Ctrl Pts',(71.5638499750624,244.475629328327,16.0362204083692)) ;
#74846 = CARTESIAN_POINT('Ctrl Pts',(71.562922130889,244.518082492337,16.056050217191)) ;
#74847 = CARTESIAN_POINT('Ctrl Pts',(71.5667092011469,244.540641448196,16.0702237187361)) ;
#74848 = CARTESIAN_POINT('Ctrl Pts',(71.58153951417,244.585731165867,16.1046945816758)) ;
#74849 = CARTESIAN_POINT('Ctrl Pts',(71.5940336277842,244.607533279011,16.1258672215766)) ;
#74850 = CARTESIAN_POINT('Ctrl Pts',(71.6253513484332,244.645451520748,16.1708720249643)) ;
#74851 = CARTESIAN_POINT('Ctrl Pts',(71.6448028995719,244.66143227523,16.1951765216869)) ;
#74852 = CARTESIAN_POINT('Ctrl Pts',(71.6668639020685,244.673687931308,16.2199877856679)) ;
#74853 = CARTESIAN_POINT('Ctrl Pts',(71.6674579710636,244.674014017115,16.2206540664832)) ;
#74854 = CARTESIAN_POINT('Ctrl Pts',(71.6680536786498,244.674337073423,16.2213203435596)) ;
#74855 = CARTESIAN_POINT('Origin',(74.5283628290597,239.4,16.2213203435596)) ;
#74856 = CARTESIAN_POINT('',(71.5843221421672,244.39726169356,16.0213203435596)) ;
#74857 = CARTESIAN_POINT('Ctrl Pts',(71.5729608165739,244.437419869794,16.0254384350468)) ;
#74858 = CARTESIAN_POINT('Ctrl Pts',(71.5763329878152,244.426910511827,16.0232182514845)) ;
#74859 = CARTESIAN_POINT('Ctrl Pts',(71.5794735124668,244.416121282229,16.0218983740811)) ;
#74860 = CARTESIAN_POINT('Ctrl Pts',(71.5830120919375,244.402516900739,16.0213707571522)) ;
#74861 = CARTESIAN_POINT('Ctrl Pts',(71.583676276365,244.399890415814,16.0213203435596)) ;
#74862 = CARTESIAN_POINT('Ctrl Pts',(71.5843221421673,244.39726169356,16.0213203435596)) ;
#74863 = CARTESIAN_POINT('',(70.6854431361484,243.744187868156,16.0213203435596)) ;
#74864 = CARTESIAN_POINT('Origin',(74.5283628290597,239.4,16.0213203435596)) ;
#74865 = CARTESIAN_POINT('Ctrl Pts',(70.6854431361486,243.744187868156,16.0213203435596)) ;
#74866 = CARTESIAN_POINT('Ctrl Pts',(70.675856226913,243.750132906986,16.0213203435596)) ;
#74867 = CARTESIAN_POINT('Ctrl Pts',(70.6664344951108,243.756351720855,16.0221950109068)) ;
#74868 = CARTESIAN_POINT('Ctrl Pts',(70.6550702355232,243.764317642567,16.0244263118334)) ;
#74869 = CARTESIAN_POINT('Ctrl Pts',(70.652904897897,243.765857232674,16.0249068532759)) ;
#74870 = CARTESIAN_POINT('Ctrl Pts',(70.6507612836457,243.767402689815,16.0254384350468)) ;
#74871 = CARTESIAN_POINT('Ctrl Pts',(72.1901462641291,244.751891562381,7.27867958884205)) ;
#74872 = CARTESIAN_POINT('Ctrl Pts',(72.2226915456361,244.707440284483,7.16318668384993)) ;
#74873 = CARTESIAN_POINT('Ctrl Pts',(72.3010345108137,244.62567313033,6.93379520902284)) ;
#74874 = CARTESIAN_POINT('Ctrl Pts',(72.4376389789193,244.547258447274,6.66079124794237)) ;
#74875 = CARTESIAN_POINT('Ctrl Pts',(72.5627005459071,244.514203826472,6.49259685569267)) ;
#74876 = CARTESIAN_POINT('Ctrl Pts',(72.6452938287017,244.505871428575,6.411450768915)) ;
#74877 = CARTESIAN_POINT('Ctrl Pts',(72.7460237857294,244.505796254997,6.33519080978562)) ;
#74878 = CARTESIAN_POINT('Ctrl Pts',(72.8756195873876,244.533840692988,6.30217109838147)) ;
#74879 = CARTESIAN_POINT('Ctrl Pts',(72.986994973301,244.591933082758,6.35347460249892)) ;
#74880 = CARTESIAN_POINT('Ctrl Pts',(73.0507055731919,244.637746956413,6.41181309644325)) ;
#74881 = CARTESIAN_POINT('Ctrl Pts',(73.1125055094761,244.693131160356,6.49328843787088)) ;
#74882 = CARTESIAN_POINT('Ctrl Pts',(73.1942872183044,244.793268231079,6.66117964447055)) ;
#74883 = CARTESIAN_POINT('Ctrl Pts',(73.2586724865194,244.937050873409,6.93433578523243)) ;
#74884 = CARTESIAN_POINT('Ctrl Pts',(73.2740549596695,245.049050470208,7.1631898418427)) ;
#74885 = CARTESIAN_POINT('Ctrl Pts',(73.2742568343815,245.10414043955,7.27867958884209)) ;
#74886 = CARTESIAN_POINT('Ctrl Pts',(72.1633150634402,244.78853838499,7.24979207607672)) ;
#74887 = CARTESIAN_POINT('Ctrl Pts',(72.1940559565136,244.739315065769,7.13558035663659)) ;
#74888 = CARTESIAN_POINT('Ctrl Pts',(72.2710212515803,244.647558801653,6.90836946535324)) ;
#74889 = CARTESIAN_POINT('Ctrl Pts',(72.4117199496733,244.557054257005,6.63741801934678)) ;
#74890 = CARTESIAN_POINT('Ctrl Pts',(72.5434569761114,244.517262868332,6.47033215351056)) ;
#74891 = CARTESIAN_POINT('Ctrl Pts',(72.631105954999,244.506162798098,6.38969365013118)) ;
#74892 = CARTESIAN_POINT('Ctrl Pts',(72.738379604366,244.50400077796,6.31389435183346)) ;
#74893 = CARTESIAN_POINT('Ctrl Pts',(72.8769068455281,244.533085740452,6.28106503242219)) ;
#74894 = CARTESIAN_POINT('Ctrl Pts',(72.9950033871039,244.596240433655,6.33206902621705)) ;
#74895 = CARTESIAN_POINT('Ctrl Pts',(73.0619179397723,244.646313620026,6.39005390425698)) ;
#74896 = CARTESIAN_POINT('Ctrl Pts',(73.1261589448907,244.706921292487,6.4710199832332)) ;
#74897 = CARTESIAN_POINT('Ctrl Pts',(73.2094278923994,244.816428207189,6.63780422869352)) ;
#74898 = CARTESIAN_POINT('Ctrl Pts',(73.2699618445942,244.972390194654,6.90890610769434)) ;
#74899 = CARTESIAN_POINT('Ctrl Pts',(73.278485994941,245.091669363501,7.13558347959712)) ;
#74900 = CARTESIAN_POINT('Ctrl Pts',(73.2744232698454,245.149559325897,7.24979207607676)) ;
#74901 = CARTESIAN_POINT('Ctrl Pts',(72.0842730845649,244.828457427666,7.19960837676255)) ;
#74902 = CARTESIAN_POINT('Ctrl Pts',(72.1180702032677,244.771056611335,7.08747419070363)) ;
#74903 = CARTESIAN_POINT('Ctrl Pts',(72.2033093580407,244.664099445641,6.86385716177446)) ;
#74904 = CARTESIAN_POINT('Ctrl Pts',(72.3604949046759,244.558655570097,6.59636562128617)) ;
#74905 = CARTESIAN_POINT('Ctrl Pts',(72.5078996758972,244.511896865288,6.43117365814849)) ;
#74906 = CARTESIAN_POINT('Ctrl Pts',(72.6059859036912,244.49845940005,6.35140690677207)) ;
#74907 = CARTESIAN_POINT('Ctrl Pts',(72.7259813969145,244.495104456363,6.27640204319265)) ;
#74908 = CARTESIAN_POINT('Ctrl Pts',(72.8807785181998,244.527201799561,6.24390313457582)) ;
#74909 = CARTESIAN_POINT('Ctrl Pts',(73.0124726998353,244.598319318779,6.2943887303005)) ;
#74910 = CARTESIAN_POINT('Ctrl Pts',(73.0868970256526,244.654911283162,6.35176416943413)) ;
#74911 = CARTESIAN_POINT('Ctrl Pts',(73.1582015882457,244.723564062097,6.43185569767935)) ;
#74912 = CARTESIAN_POINT('Ctrl Pts',(73.2500058742025,244.847883120417,6.59674825081069)) ;
#74913 = CARTESIAN_POINT('Ctrl Pts',(73.3151566187034,245.025648513998,6.8643892827353)) ;
#74914 = CARTESIAN_POINT('Ctrl Pts',(73.3213024844566,245.162012348452,7.0874772568569)) ;
#74915 = CARTESIAN_POINT('Ctrl Pts',(73.3149057494537,245.228314219316,7.19960837676259)) ;
#74916 = CARTESIAN_POINT('Ctrl Pts',(71.9910147655644,244.806016366157,7.17608503411331)) ;
#74917 = CARTESIAN_POINT('Ctrl Pts',(72.0321944574529,244.746635057199,7.0621566209928)) ;
#74918 = CARTESIAN_POINT('Ctrl Pts',(72.1325429398017,244.637187568385,6.83553351420321)) ;
#74919 = CARTESIAN_POINT('Ctrl Pts',(72.3104327593928,244.531883870857,6.5653014585105)) ;
#74920 = CARTESIAN_POINT('Ctrl Pts',(72.4746449644358,244.487247007328,6.39866074879488)) ;
#74921 = CARTESIAN_POINT('Ctrl Pts',(72.5834312809955,244.475805815997,6.31823715694155)) ;
#74922 = CARTESIAN_POINT('Ctrl Pts',(72.7162984783341,244.475322282895,6.24263987289687)) ;
#74923 = CARTESIAN_POINT('Ctrl Pts',(72.8875918907321,244.512256825088,6.20989806420845)) ;
#74924 = CARTESIAN_POINT('Ctrl Pts',(73.0345989364271,244.589179504376,6.26076617601792)) ;
#74925 = CARTESIAN_POINT('Ctrl Pts',(73.1184652751015,244.649847982056,6.31859653587809)) ;
#74926 = CARTESIAN_POINT('Ctrl Pts',(73.1995894461384,244.723175613832,6.39934685299362)) ;
#74927 = CARTESIAN_POINT('Ctrl Pts',(73.3062406700047,244.855654460481,6.56568669597758)) ;
#74928 = CARTESIAN_POINT('Ctrl Pts',(73.388218198327,245.045477794218,6.8360690634198)) ;
#74929 = CARTESIAN_POINT('Ctrl Pts',(73.405132183067,245.192731555512,7.06215973620671)) ;
#74930 = CARTESIAN_POINT('Ctrl Pts',(73.4035438393931,245.264974883745,7.17608503411334)) ;
#74931 = CARTESIAN_POINT('Ctrl Pts',(71.9556834737297,244.786783924096,7.17267980084142)) ;
#74932 = CARTESIAN_POINT('Ctrl Pts',(71.9994364250326,244.7276871246,7.05718689584929)) ;
#74933 = CARTESIAN_POINT('Ctrl Pts',(72.105166158695,244.619271346283,6.82779542102222)) ;
#74934 = CARTESIAN_POINT('Ctrl Pts',(72.290755802235,244.516291089754,6.55479145994173)) ;
#74935 = CARTESIAN_POINT('Ctrl Pts',(72.4615143280827,244.473900464396,6.38659706769207)) ;
#74936 = CARTESIAN_POINT('Ctrl Pts',(72.5745815094689,244.463950453933,6.30545098091439)) ;
#74937 = CARTESIAN_POINT('Ctrl Pts',(72.7126879954014,244.465289886791,6.22919102178501)) ;
#74938 = CARTESIAN_POINT('Ctrl Pts',(72.8909283600454,244.504548617211,6.19617131038086)) ;
#74939 = CARTESIAN_POINT('Ctrl Pts',(73.0445730380394,244.58352939965,6.24747481449832)) ;
#74940 = CARTESIAN_POINT('Ctrl Pts',(73.1325804113198,244.645452965562,6.30581330844265)) ;
#74941 = CARTESIAN_POINT('Ctrl Pts',(73.2180392194167,244.720087566317,6.38728864987029)) ;
#74942 = CARTESIAN_POINT('Ctrl Pts',(73.331313815252,244.854600590535,6.55517985646993)) ;
#74943 = CARTESIAN_POINT('Ctrl Pts',(73.4208757682397,245.047065698635,6.82833599723182)) ;
#74944 = CARTESIAN_POINT('Ctrl Pts',(73.4427713648375,245.196657079445,7.05719005384205)) ;
#74945 = CARTESIAN_POINT('Ctrl Pts',(73.4434320007296,245.270182723559,7.17267980084145)) ;
#74946 = CARTESIAN_POINT('Ctrl Pts',(73.4434320007296,245.270182723559,7.17267980084145)) ;
#74947 = CARTESIAN_POINT('Ctrl Pts',(73.4431020130991,245.233456664063,7.11499267180461)) ;
#74948 = CARTESIAN_POINT('Ctrl Pts',(73.4402029360074,245.196364845114,7.0574944676865)) ;
#74949 = CARTESIAN_POINT('Ctrl Pts',(73.4344583668991,245.158974046861,7.00044813217449)) ;
#74950 = CARTESIAN_POINT('Ctrl Pts',(73.430549504914,245.133531673876,6.96163125173052)) ;
#74951 = CARTESIAN_POINT('Ctrl Pts',(73.4253236110167,245.107950944466,6.92302359436789)) ;
#74952 = CARTESIAN_POINT('Ctrl Pts',(73.4187008698935,245.082253697312,6.88470696318928)) ;
#74953 = CARTESIAN_POINT('Ctrl Pts',(73.4155906518556,245.070185576252,6.86671243868241)) ;
#74954 = CARTESIAN_POINT('Ctrl Pts',(73.4121725669894,245.058091915308,6.84878227850999)) ;
#74955 = CARTESIAN_POINT('Ctrl Pts',(73.4084372767916,245.045970522218,6.83091828323211)) ;
#74956 = CARTESIAN_POINT('Ctrl Pts',(73.3850436077588,244.970055708869,6.71903824955231)) ;
#74957 = CARTESIAN_POINT('Ctrl Pts',(73.3492173176614,244.893081205197,6.60979489059652)) ;
#74958 = CARTESIAN_POINT('Ctrl Pts',(73.294132385133,244.816188540897,6.50943171095909)) ;
#74959 = CARTESIAN_POINT('Ctrl Pts',(73.2710746632426,244.784002431421,6.46742119777713)) ;
#74960 = CARTESIAN_POINT('Ctrl Pts',(73.2446445763898,244.751835121943,6.42697296071601)) ;
#74961 = CARTESIAN_POINT('Ctrl Pts',(73.2136229784609,244.720113630821,6.38961257812027)) ;
#74962 = CARTESIAN_POINT('Ctrl Pts',(73.2075751679563,244.713929372755,6.38232899089704)) ;
#74963 = CARTESIAN_POINT('Ctrl Pts',(73.2013528423385,244.707762030666,6.37516271804997)) ;
#74964 = CARTESIAN_POINT('Ctrl Pts',(73.1949469784241,244.701614748171,6.36812502208952)) ;
#74965 = CARTESIAN_POINT('Ctrl Pts',(73.1836709346794,244.690793877285,6.35573678397329)) ;
#74966 = CARTESIAN_POINT('Ctrl Pts',(73.1718261861905,244.68003516648,6.34374695713007)) ;
#74967 = CARTESIAN_POINT('Ctrl Pts',(73.1593823140545,244.669394897422,6.3322774914791)) ;
#74968 = CARTESIAN_POINT('Ctrl Pts',(73.1501555753554,244.661505473519,6.32377324445519)) ;
#74969 = CARTESIAN_POINT('Ctrl Pts',(73.1405952222296,244.653677586905,6.31555124386587)) ;
#74970 = CARTESIAN_POINT('Ctrl Pts',(73.1306902804345,244.645936066955,6.3076636555575)) ;
#74971 = CARTESIAN_POINT('Ctrl Pts',(73.1074240776829,244.627751631699,6.2891361131851)) ;
#74972 = CARTESIAN_POINT('Ctrl Pts',(73.0822567910222,244.61004723145,6.27245966803159)) ;
#74973 = CARTESIAN_POINT('Ctrl Pts',(73.0549119312148,244.593134139718,6.25837186118317)) ;
#74974 = CARTESIAN_POINT('Ctrl Pts',(73.0438936901924,244.5863192384,6.25269537015611)) ;
#74975 = CARTESIAN_POINT('Ctrl Pts',(73.0325224261536,244.579632692525,6.24743866551629)) ;
#74976 = CARTESIAN_POINT('Ctrl Pts',(73.0208477353986,244.573129233053,6.24267263511688)) ;
#74977 = CARTESIAN_POINT('Ctrl Pts',(73.014675248033,244.569690810378,6.24015280285393)) ;
#74978 = CARTESIAN_POINT('Ctrl Pts',(73.0084179521525,244.56630354916,6.23777009440928)) ;
#74979 = CARTESIAN_POINT('Ctrl Pts',(73.0020832177036,244.562975403627,6.23553472416755)) ;
#74980 = CARTESIAN_POINT('Ctrl Pts',(72.9955648125652,244.559550761108,6.23323454110739)) ;
#74981 = CARTESIAN_POINT('Ctrl Pts',(72.9889570762782,244.556184795348,6.23108766580282)) ;
#74982 = CARTESIAN_POINT('Ctrl Pts',(72.98226214601,244.552884038068,6.22910483023557)) ;
#74983 = CARTESIAN_POINT('Ctrl Pts',(72.9678571946245,244.545782059967,6.22483851993699)) ;
#74984 = CARTESIAN_POINT('Ctrl Pts',(72.9530544980498,244.538984925329,6.22133345057263)) ;
#74985 = CARTESIAN_POINT('Ctrl Pts',(72.937916101209,244.532580800946,6.21871395687209)) ;
#74986 = CARTESIAN_POINT('Ctrl Pts',(72.9316302795469,244.529921656507,6.21762628091671)) ;
#74987 = CARTESIAN_POINT('Ctrl Pts',(72.9252856550904,244.527329944157,6.21669124187431)) ;
#74988 = CARTESIAN_POINT('Ctrl Pts',(72.9188902808961,244.524813504551,6.21591837295059)) ;
#74989 = CARTESIAN_POINT('Ctrl Pts',(72.9007439069117,244.517673304023,6.21372541783891)) ;
#74990 = CARTESIAN_POINT('Ctrl Pts',(72.8821933431793,244.511142194532,6.21284099333179)) ;
#74991 = CARTESIAN_POINT('Ctrl Pts',(72.8634811408771,244.505251424119,6.21317786085357)) ;
#74992 = CARTESIAN_POINT('Ctrl Pts',(72.8463692443292,244.499864444422,6.21348591877695)) ;
#74993 = CARTESIAN_POINT('Ctrl Pts',(72.8291180547982,244.495010433656,6.21481320707205)) ;
#74994 = CARTESIAN_POINT('Ctrl Pts',(72.8118702212274,244.490694079075,6.21708372521223)) ;
#74995 = CARTESIAN_POINT('Ctrl Pts',(72.7915336066829,244.485604741971,6.21976085286675)) ;
#74996 = CARTESIAN_POINT('Ctrl Pts',(72.7711961915529,244.481260225182,6.22374801364797)) ;
#74997 = CARTESIAN_POINT('Ctrl Pts',(72.7510661192296,244.477710567067,6.22899928973749)) ;
#74998 = CARTESIAN_POINT('Ctrl Pts',(72.7440058314115,244.476465583565,6.23084108742252)) ;
#74999 = CARTESIAN_POINT('Ctrl Pts',(72.7369714274797,244.475318607259,6.2328385443403)) ;
#75000 = CARTESIAN_POINT('Ctrl Pts',(72.7299731476575,244.474272523511,6.23499013385452)) ;
#75001 = CARTESIAN_POINT('Ctrl Pts',(72.7090389360436,244.471143334754,6.24142626263776)) ;
#75002 = CARTESIAN_POINT('Ctrl Pts',(72.6883573215069,244.468786869276,6.24908069692733)) ;
#75003 = CARTESIAN_POINT('Ctrl Pts',(72.6681923159947,244.467248684764,6.25787359444939)) ;
#75004 = CARTESIAN_POINT('Ctrl Pts',(72.6438222406551,244.465389737965,6.26850010159001)) ;
#75005 = CARTESIAN_POINT('Ctrl Pts',(72.6202065313713,244.464726020216,6.28079022660041)) ;
#75006 = CARTESIAN_POINT('Ctrl Pts',(72.5973092509544,244.464976781267,6.29423639923435)) ;
#75007 = CARTESIAN_POINT('Ctrl Pts',(72.5900990277946,244.465055744493,6.29847052239526)) ;
#75008 = CARTESIAN_POINT('Ctrl Pts',(72.5829603890789,244.465225423066,6.30281908603248)) ;
#75009 = CARTESIAN_POINT('Ctrl Pts',(72.575893129647,244.465477187611,6.30726577261015)) ;
#75010 = CARTESIAN_POINT('Ctrl Pts',(72.5639041463512,244.465904283992,6.31480918482168)) ;
#75011 = CARTESIAN_POINT('Ctrl Pts',(72.5521204122704,244.466567572729,6.32263505153982)) ;
#75012 = CARTESIAN_POINT('Ctrl Pts',(72.5405625868693,244.467463254872,6.33072043562018)) ;
#75013 = CARTESIAN_POINT('Ctrl Pts',(72.5236632480752,244.468772881507,6.34254252499356)) ;
#75014 = CARTESIAN_POINT('Ctrl Pts',(72.5071998069331,244.470542167386,6.35489086909629)) ;
#75015 = CARTESIAN_POINT('Ctrl Pts',(72.49118920689,244.472728629967,6.36767692557154)) ;
#75016 = CARTESIAN_POINT('Ctrl Pts',(72.4398639222179,244.47973778728,6.40866526995973)) ;
#75017 = CARTESIAN_POINT('Ctrl Pts',(72.3931914538475,244.491034261609,6.45415279537548)) ;
#75018 = CARTESIAN_POINT('Ctrl Pts',(72.3500947237597,244.504952123835,6.50170615626623)) ;
#75019 = CARTESIAN_POINT('Ctrl Pts',(72.3479010740007,244.505660551483,6.50412665124215)) ;
#75020 = CARTESIAN_POINT('Ctrl Pts',(72.3457166726364,244.506375885972,6.50655267846174)) ;
#75021 = CARTESIAN_POINT('Ctrl Pts',(72.3435413791296,244.507097907721,6.50898391584394)) ;
#75022 = CARTESIAN_POINT('Ctrl Pts',(72.2939557630567,244.523556327311,6.56440374909368)) ;
#75023 = CARTESIAN_POINT('Ctrl Pts',(72.2491073863615,244.543491811814,6.62253117127341)) ;
#75024 = CARTESIAN_POINT('Ctrl Pts',(72.2081933830777,244.5660749154,6.68231650548116)) ;
#75025 = CARTESIAN_POINT('Ctrl Pts',(72.1749957149923,244.58439887094,6.73082639261291)) ;
#75026 = CARTESIAN_POINT('Ctrl Pts',(72.144386895211,244.604465119596,6.78042742681575)) ;
#75027 = CARTESIAN_POINT('Ctrl Pts',(72.1159153532659,244.625820724971,6.83056031505395)) ;
#75028 = CARTESIAN_POINT('Ctrl Pts',(72.108878159526,244.631099101981,6.84295145452781)) ;
#75029 = CARTESIAN_POINT('Ctrl Pts',(72.1019714543362,244.636456219632,6.85537510631104)) ;
#75030 = CARTESIAN_POINT('Ctrl Pts',(72.0951927450628,244.641889511684,6.86782833804242)) ;
#75031 = CARTESIAN_POINT('Ctrl Pts',(72.0505748877656,244.677651754852,6.94979623102563)) ;
#75032 = CARTESIAN_POINT('Ctrl Pts',(72.0115273534747,244.716808066892,7.03316537501444)) ;
#75033 = CARTESIAN_POINT('Ctrl Pts',(71.9774750347497,244.758698720179,7.11710901687511)) ;
#75034 = CARTESIAN_POINT('Ctrl Pts',(71.9699709268568,244.767930161495,7.13560767332584)) ;
#75035 = CARTESIAN_POINT('Ctrl Pts',(71.9627092212568,244.777294296984,7.15413421780112)) ;
#75036 = CARTESIAN_POINT('Ctrl Pts',(71.9556834737298,244.786783924096,7.17267980084129)) ;
#75037 = CARTESIAN_POINT('Ctrl Pts',(72.1901462641291,244.751891562381,7.27867958884205)) ;
#75038 = CARTESIAN_POINT('Ctrl Pts',(72.2226915456361,244.707440284483,7.16318668384993)) ;
#75039 = CARTESIAN_POINT('Ctrl Pts',(72.3010345108137,244.62567313033,6.93379520902284)) ;
#75040 = CARTESIAN_POINT('Ctrl Pts',(72.4376389789193,244.547258447274,6.66079124794237)) ;
#75041 = CARTESIAN_POINT('Ctrl Pts',(72.5627005459071,244.514203826472,6.49259685569267)) ;
#75042 = CARTESIAN_POINT('Ctrl Pts',(72.6452938287017,244.505871428575,6.411450768915)) ;
#75043 = CARTESIAN_POINT('Ctrl Pts',(72.7460237857294,244.505796254997,6.33519080978562)) ;
#75044 = CARTESIAN_POINT('Ctrl Pts',(72.8756195873876,244.533840692988,6.30217109838147)) ;
#75045 = CARTESIAN_POINT('Ctrl Pts',(72.986994973301,244.591933082758,6.35347460249892)) ;
#75046 = CARTESIAN_POINT('Ctrl Pts',(73.0507055731919,244.637746956413,6.41181309644325)) ;
#75047 = CARTESIAN_POINT('Ctrl Pts',(73.1125055094761,244.693131160356,6.49328843787088)) ;
#75048 = CARTESIAN_POINT('Ctrl Pts',(73.1942872183044,244.793268231079,6.66117964447055)) ;
#75049 = CARTESIAN_POINT('Ctrl Pts',(73.2586724865194,244.937050873409,6.93433578523243)) ;
#75050 = CARTESIAN_POINT('Ctrl Pts',(73.2740549596695,245.049050470208,7.1631898418427)) ;
#75051 = CARTESIAN_POINT('Ctrl Pts',(73.2742568343815,245.10414043955,7.27867958884209)) ;
#75052 = CARTESIAN_POINT('Origin',(73.474255491572,245.103407553477,16.0213203435596)) ;
#75053 = CARTESIAN_POINT('',(73.2742568343815,245.10414043955,16.0254384350469)) ;
#75054 = CARTESIAN_POINT('',(73.2742568343815,245.10414043955,16.0213203435596)) ;
#75055 = CARTESIAN_POINT('Ctrl Pts',(73.2742568343815,245.10414043955,16.0254384350469)) ;
#75056 = CARTESIAN_POINT('Ctrl Pts',(73.2743301777146,245.124155239482,16.0294645582753)) ;
#75057 = CARTESIAN_POINT('Ctrl Pts',(73.2773992812257,245.143295198932,16.0362204083692)) ;
#75058 = CARTESIAN_POINT('Ctrl Pts',(73.2896355981226,245.183957276819,16.056050217191)) ;
#75059 = CARTESIAN_POINT('Ctrl Pts',(73.3002084167048,245.204241849721,16.070223718736)) ;
#75060 = CARTESIAN_POINT('Ctrl Pts',(73.3282463715764,245.242541900774,16.1046945816763)) ;
#75061 = CARTESIAN_POINT('Ctrl Pts',(73.3468662032201,245.259416049113,16.1258672215778)) ;
#75062 = CARTESIAN_POINT('Ctrl Pts',(73.3883685066135,245.285800732098,16.1708720249666)) ;
#75063 = CARTESIAN_POINT('Ctrl Pts',(73.4118063557929,245.294988472914,16.1951765216919)) ;
#75064 = CARTESIAN_POINT('Ctrl Pts',(73.4365748219814,245.299827069804,16.2199877856716)) ;
#75065 = CARTESIAN_POINT('Ctrl Pts',(73.4372405812222,245.29995361842,16.2206540664831)) ;
#75066 = CARTESIAN_POINT('Ctrl Pts',(73.4379069626931,245.300076779458,16.2213203435596)) ;
#75067 = CARTESIAN_POINT('Origin',(72.0287747312355,244.633742383918,16.0213203435596)) ;
#75068 = CARTESIAN_POINT('',(72.1901462641291,244.751891562381,16.0254384350469)) ;
#75069 = CARTESIAN_POINT('',(72.1901462641291,244.751891562381,16.0213203435596)) ;
#75070 = CARTESIAN_POINT('Ctrl Pts',(71.9425820382072,244.814216259225,16.2213203435596)) ;
#75071 = CARTESIAN_POINT('Ctrl Pts',(71.9431935443975,244.814508309059,16.2206540664685)) ;
#75072 = CARTESIAN_POINT('Ctrl Pts',(71.9438065383602,244.814797252548,16.2199877856879)) ;
#75073 = CARTESIAN_POINT('Ctrl Pts',(71.9632344714873,244.823834488918,16.1989219658621)) ;
#75074 = CARTESIAN_POINT('Ctrl Pts',(71.9835241847008,244.829711338052,16.1784289743563)) ;
#75075 = CARTESIAN_POINT('Ctrl Pts',(72.0247458013708,244.834727421522,16.1396302535195)) ;
#75076 = CARTESIAN_POINT('Ctrl Pts',(72.0458338508477,244.834186521463,16.12105377447)) ;
#75077 = CARTESIAN_POINT('Ctrl Pts',(72.0895325990311,244.825657771132,16.0855257633019)) ;
#75078 = CARTESIAN_POINT('Ctrl Pts',(72.1124548100242,244.817186011065,16.0684876094896)) ;
#75079 = CARTESIAN_POINT('Ctrl Pts',(72.1504375878132,244.793629310998,16.0440628922452)) ;
#75080 = CARTESIAN_POINT('Ctrl Pts',(72.1659608719307,244.780773205401,16.0353723462245)) ;
#75081 = CARTESIAN_POINT('Ctrl Pts',(72.1833422628339,244.760784770124,16.0279192770517)) ;
#75082 = CARTESIAN_POINT('Ctrl Pts',(72.1868310246749,244.756419611409,16.0265673132457)) ;
#75083 = CARTESIAN_POINT('Ctrl Pts',(72.1901462641293,244.751891562381,16.0254384350468)) ;
#75084 = CARTESIAN_POINT('Origin',(74.5283628290597,239.4,16.2213203435596)) ;
#75085 = CARTESIAN_POINT('',(73.2726525382015,245.062436901673,16.0213203435596)) ;
#75086 = CARTESIAN_POINT('Ctrl Pts',(73.2742568343815,245.10414043955,16.0254384350468)) ;
#75087 = CARTESIAN_POINT('Ctrl Pts',(73.2742163896029,245.093103387952,16.0232182514845)) ;
#75088 = CARTESIAN_POINT('Ctrl Pts',(73.2738691507354,245.081871745349,16.0218983740811)) ;
#75089 = CARTESIAN_POINT('Ctrl Pts',(73.2730305547208,245.06783972849,16.0213707571522)) ;
#75090 = CARTESIAN_POINT('Ctrl Pts',(73.2728506031715,245.065136548611,16.0213203435596)) ;
#75091 = CARTESIAN_POINT('Ctrl Pts',(73.2726525382014,245.062436901673,16.0213203435596)) ;
#75092 = CARTESIAN_POINT('',(72.2159568915352,244.719095673148,16.0213203435596)) ;
#75093 = CARTESIAN_POINT('Origin',(74.5283628290597,239.4,16.0213203435596)) ;
#75094 = CARTESIAN_POINT('Ctrl Pts',(72.2159568915352,244.719095673148,16.0213203435596)) ;
#75095 = CARTESIAN_POINT('Ctrl Pts',(72.2086763170662,244.727712258944,16.0213203435596)) ;
#75096 = CARTESIAN_POINT('Ctrl Pts',(72.2016374368113,244.736538177641,16.0221950109068)) ;
#75097 = CARTESIAN_POINT('Ctrl Pts',(72.1932909888623,244.747625968734,16.0244263118334)) ;
#75098 = CARTESIAN_POINT('Ctrl Pts',(72.1917073899104,244.749759332063,16.0249068532759)) ;
#75099 = CARTESIAN_POINT('Ctrl Pts',(72.1901462641291,244.751891562381,16.0254384350468)) ;
#75100 = CARTESIAN_POINT('Origin',(71.0016513153049,244.25410196625,16.0213203435596)) ;
#75101 = CARTESIAN_POINT('Origin',(71.0016513153049,244.25410196625,16.0213203435596)) ;
#75102 = CARTESIAN_POINT('Origin',(69.67426086281,242.926711513755,16.0213203435596)) ;
#75103 = CARTESIAN_POINT('Origin',(69.67426086281,242.926711513755,16.0213203435596)) ;
#75104 = CARTESIAN_POINT('Origin',(68.8220237312887,241.25410196625,16.0213203435596)) ;
#75105 = CARTESIAN_POINT('Origin',(68.8220237312887,241.25410196625,16.0213203435596)) ;
#75106 = CARTESIAN_POINT('Origin',(68.5283628290597,239.4,16.0213203435596)) ;
#75107 = CARTESIAN_POINT('Origin',(68.5283628290597,239.4,16.0213203435596)) ;
#75108 = CARTESIAN_POINT('Origin',(68.8220237312888,237.54589803375,16.0213203435596)) ;
#75109 = CARTESIAN_POINT('Origin',(68.8220237312888,237.54589803375,16.0213203435596)) ;
#75110 = CARTESIAN_POINT('Origin',(69.6742608628099,235.873288486245,16.0213203435596)) ;
#75111 = CARTESIAN_POINT('Origin',(69.6742608628099,235.873288486245,16.0213203435596)) ;
#75112 = CARTESIAN_POINT('Origin',(71.0016513153048,234.54589803375,16.0213203435596)) ;
#75113 = CARTESIAN_POINT('Origin',(71.0016513153048,234.54589803375,16.0213203435596)) ;
#75114 = CARTESIAN_POINT('Origin',(72.67426086281,233.693660902229,16.0213203435596)) ;
#75115 = CARTESIAN_POINT('Origin',(72.67426086281,233.693660902229,16.0213203435596)) ;
#75116 = CARTESIAN_POINT('Origin',(74.5283628290597,233.4,16.0213203435596)) ;
#75117 = CARTESIAN_POINT('Origin',(74.5283628290597,233.4,16.0213203435596)) ;
#75118 = CARTESIAN_POINT('Origin',(76.3824647953094,233.693660902229,16.0213203435596)) ;
#75119 = CARTESIAN_POINT('Origin',(76.3824647953094,233.693660902229,16.0213203435596)) ;
#75120 = CARTESIAN_POINT('Origin',(78.0550743428145,234.54589803375,16.0213203435596)) ;
#75121 = CARTESIAN_POINT('Origin',(78.0550743428145,234.54589803375,16.0213203435596)) ;
#75122 = CARTESIAN_POINT('Origin',(79.3824647953094,235.873288486245,16.0213203435596)) ;
#75123 = CARTESIAN_POINT('Origin',(79.3824647953094,235.873288486245,16.0213203435596)) ;
#75124 = CARTESIAN_POINT('Origin',(80.2347019268307,237.54589803375,16.0213203435596)) ;
#75125 = CARTESIAN_POINT('Origin',(80.2347019268307,237.54589803375,16.0213203435596)) ;
#75126 = CARTESIAN_POINT('Origin',(80.5283628290597,239.4,16.0213203435596)) ;
#75127 = CARTESIAN_POINT('Origin',(80.5283628290597,239.4,16.0213203435596)) ;
#75128 = CARTESIAN_POINT('Origin',(80.2347019268306,241.25410196625,16.0213203435596)) ;
#75129 = CARTESIAN_POINT('Origin',(80.2347019268306,241.25410196625,16.0213203435596)) ;
#75130 = CARTESIAN_POINT('Origin',(79.3824647953094,242.926711513755,16.0213203435596)) ;
#75131 = CARTESIAN_POINT('Origin',(79.3824647953094,242.926711513755,16.0213203435596)) ;
#75132 = CARTESIAN_POINT('Origin',(78.0550743428145,244.25410196625,16.0213203435596)) ;
#75133 = CARTESIAN_POINT('Origin',(78.0550743428145,244.25410196625,16.0213203435596)) ;
#75134 = CARTESIAN_POINT('Origin',(76.3824647953094,245.106339097771,16.0213203435596)) ;
#75135 = CARTESIAN_POINT('Origin',(76.3824647953094,245.106339097771,16.0213203435596)) ;
#75136 = CARTESIAN_POINT('Origin',(74.5283628290597,245.4,16.0213203435596)) ;
#75137 = CARTESIAN_POINT('Origin',(74.5283628290597,245.4,16.0213203435596)) ;
#75138 = CARTESIAN_POINT('Origin',(72.67426086281,245.106339097771,16.0213203435596)) ;
#75139 = CARTESIAN_POINT('Origin',(72.67426086281,245.106339097771,16.0213203435596)) ;
#75140 = CARTESIAN_POINT('Origin',(74.5283628290597,239.4,6.62132034355964)) ;
#75141 = CARTESIAN_POINT('',(69.2196126965601,239.4,6.115320555559)) ;
#75142 = CARTESIAN_POINT('',(68.9033628290597,239.4,6.62132034355964)) ;
#75143 = CARTESIAN_POINT('Origin',(74.5283628290597,239.4,6.115320555559)) ;
#75144 = CARTESIAN_POINT('Origin',(76.0783628290596,240.95,6.22132034355964)) ;
#75145 = CARTESIAN_POINT('',(75.3283628290596,240.95,6.02132034355964)) ;
#75146 = CARTESIAN_POINT('Origin',(75.3283628290596,240.95,6.22132034355964)) ;
#75147 = CARTESIAN_POINT('',(76.0783628290596,240.2,6.02132034355964)) ;
#75148 = CARTESIAN_POINT('Origin',(76.0783628290596,240.95,6.02132034355964)) ;
#75149 = CARTESIAN_POINT('Origin',(76.0783628290596,240.2,6.22132034355964)) ;
#75150 = CARTESIAN_POINT('Origin',(74.5283628290597,239.4,6.02132034355964)) ;
#75151 = CARTESIAN_POINT('',(69.3892123573611,239.4,6.02132034355964)) ;
#75152 = CARTESIAN_POINT('Origin',(74.5283628290597,239.4,6.02132034355964)) ;
#75153 = CARTESIAN_POINT('',(75.3283628290596,242.7,6.02132034355964)) ;
#75154 = CARTESIAN_POINT('',(75.3283628290596,241.15,6.02132034355964)) ;
#75155 = CARTESIAN_POINT('',(74.9283628290597,243.1,6.02132034355964)) ;
#75156 = CARTESIAN_POINT('Origin',(74.9283628290597,242.7,6.02132034355964)) ;
#75157 = CARTESIAN_POINT('',(74.1283628290597,243.1,6.02132034355964)) ;
#75158 = CARTESIAN_POINT('',(74.2283628290596,243.1,6.02132034355964)) ;
#75159 = CARTESIAN_POINT('',(73.7283628290597,242.7,6.02132034355964)) ;
#75160 = CARTESIAN_POINT('Origin',(74.1283628290597,242.7,6.02132034355964)) ;
#75161 = CARTESIAN_POINT('',(73.7283628290597,240.95,6.02132034355964)) ;
#75162 = CARTESIAN_POINT('',(73.7283628290597,239.7,6.02132034355964)) ;
#75163 = CARTESIAN_POINT('',(72.9783628290596,240.2,6.02132034355964)) ;
#75164 = CARTESIAN_POINT('Origin',(72.9783628290596,240.95,6.02132034355964)) ;
#75165 = CARTESIAN_POINT('',(71.2283628290598,240.2,6.02132034355964)) ;
#75166 = CARTESIAN_POINT('',(72.7783628290597,240.2,6.02132034355964)) ;
#75167 = CARTESIAN_POINT('',(70.8283628290598,239.8,6.02132034355964)) ;
#75168 = CARTESIAN_POINT('Origin',(71.2283628290598,239.8,6.02132034355964)) ;
#75169 = CARTESIAN_POINT('',(70.8283628290598,239.,6.02132034355964)) ;
#75170 = CARTESIAN_POINT('',(70.8283628290598,239.1,6.02132034355964)) ;
#75171 = CARTESIAN_POINT('',(71.2283628290597,238.6,6.02132034355964)) ;
#75172 = CARTESIAN_POINT('Origin',(71.2283628290597,239.,6.02132034355964)) ;
#75173 = CARTESIAN_POINT('',(72.9783628290596,238.6,6.02132034355964)) ;
#75174 = CARTESIAN_POINT('',(74.2283628290596,238.6,6.02132034355964)) ;
#75175 = CARTESIAN_POINT('',(73.7283628290597,237.85,6.02132034355964)) ;
#75176 = CARTESIAN_POINT('Origin',(72.9783628290596,237.85,6.02132034355964)) ;
#75177 = CARTESIAN_POINT('',(73.7283628290597,236.1,6.02132034355964)) ;
#75178 = CARTESIAN_POINT('',(73.7283628290597,237.65,6.02132034355964)) ;
#75179 = CARTESIAN_POINT('',(74.1283628290597,235.7,6.02132034355964)) ;
#75180 = CARTESIAN_POINT('Origin',(74.1283628290597,236.1,6.02132034355964)) ;
#75181 = CARTESIAN_POINT('',(74.9283628290597,235.7,6.02132034355964)) ;
#75182 = CARTESIAN_POINT('',(74.8283628290597,235.7,6.02132034355964)) ;
#75183 = CARTESIAN_POINT('',(75.3283628290596,236.1,6.02132034355964)) ;
#75184 = CARTESIAN_POINT('Origin',(74.9283628290597,236.1,6.02132034355964)) ;
#75185 = CARTESIAN_POINT('',(75.3283628290596,237.85,6.02132034355964)) ;
#75186 = CARTESIAN_POINT('',(75.3283628290596,239.1,6.02132034355964)) ;
#75187 = CARTESIAN_POINT('',(76.0783628290597,238.6,6.02132034355964)) ;
#75188 = CARTESIAN_POINT('Origin',(76.0783628290597,237.85,6.02132034355964)) ;
#75189 = CARTESIAN_POINT('',(77.8283628290598,238.6,6.02132034355964)) ;
#75190 = CARTESIAN_POINT('',(76.2783628290597,238.6,6.02132034355964)) ;
#75191 = CARTESIAN_POINT('',(78.2283628290598,239.,6.02132034355964)) ;
#75192 = CARTESIAN_POINT('Origin',(77.8283628290598,239.,6.02132034355964)) ;
#75193 = CARTESIAN_POINT('',(78.2283628290598,239.8,6.02132034355964)) ;
#75194 = CARTESIAN_POINT('',(78.2283628290598,239.7,6.02132034355964)) ;
#75195 = CARTESIAN_POINT('',(77.8283628290598,240.2,6.02132034355964)) ;
#75196 = CARTESIAN_POINT('Origin',(77.8283628290598,239.8,6.02132034355964)) ;
#75197 = CARTESIAN_POINT('',(74.8283628290597,240.2,6.02132034355964)) ;
#75198 = CARTESIAN_POINT('Origin',(75.3283628290596,241.15,6.22132034355964)) ;
#75199 = CARTESIAN_POINT('',(75.1283628290596,242.7,6.22132034355964)) ;
#75200 = CARTESIAN_POINT('',(75.1283628290596,241.15,6.22132034355964)) ;
#75201 = CARTESIAN_POINT('Origin',(75.3283628290596,242.7,6.22132034355964)) ;
#75202 = CARTESIAN_POINT('Origin',(75.1283628290596,242.9,11.0213203435596)) ;
#75203 = CARTESIAN_POINT('',(75.1283628290596,242.7,11.0213203435596)) ;
#75204 = CARTESIAN_POINT('Origin',(76.0783628290597,237.85,6.22132034355964)) ;
#75205 = CARTESIAN_POINT('Origin',(76.0783628290597,238.6,6.22132034355964)) ;
#75206 = CARTESIAN_POINT('Origin',(75.3283628290597,237.85,6.22132034355964)) ;
#75207 = CARTESIAN_POINT('Origin',(76.2783628290597,238.6,6.22132034355964)) ;
#75208 = CARTESIAN_POINT('Origin',(77.8283628290598,238.6,6.22132034355964)) ;
#75209 = CARTESIAN_POINT('Origin',(72.9783628290596,240.95,6.22132034355964)) ;
#75210 = CARTESIAN_POINT('',(72.9783628290596,240.,6.22132034355964)) ;
#75211 = CARTESIAN_POINT('Origin',(72.9783628290596,240.2,6.22132034355964)) ;
#75212 = CARTESIAN_POINT('',(73.9283628290597,240.95,6.22132034355964)) ;
#75213 = CARTESIAN_POINT('Origin',(73.7283628290596,240.95,6.22132034355964)) ;
#75214 = CARTESIAN_POINT('Origin',(72.9783628290596,240.95,6.22132034355964)) ;
#75215 = CARTESIAN_POINT('Origin',(72.9783628290596,240.95,11.0213203435596)) ;
#75216 = CARTESIAN_POINT('',(72.9783628290596,240.,11.0213203435596)) ;
#75217 = CARTESIAN_POINT('',(73.9283628290597,240.95,11.0213203435596)) ;
#75218 = CARTESIAN_POINT('Origin',(72.7783628290597,240.2,6.22132034355964)) ;
#75219 = CARTESIAN_POINT('',(71.2283628290598,240.,6.22132034355964)) ;
#75220 = CARTESIAN_POINT('',(72.7783628290597,240.,6.22132034355964)) ;
#75221 = CARTESIAN_POINT('Origin',(71.2283628290598,240.2,6.22132034355964)) ;
#75222 = CARTESIAN_POINT('Origin',(71.0283628290598,240.,11.0213203435596)) ;
#75223 = CARTESIAN_POINT('',(71.2283628290598,240.,11.0213203435596)) ;
#75224 = CARTESIAN_POINT('Origin',(72.9783628290596,237.85,6.22132034355964)) ;
#75225 = CARTESIAN_POINT('Origin',(73.7283628290596,237.85,6.22132034355964)) ;
#75226 = CARTESIAN_POINT('',(72.9783628290596,238.8,6.22132034355964)) ;
#75227 = CARTESIAN_POINT('Origin',(72.9783628290596,238.6,6.22132034355964)) ;
#75228 = CARTESIAN_POINT('Origin',(72.9783628290596,237.85,6.22132034355964)) ;
#75229 = CARTESIAN_POINT('Origin',(72.9783628290596,237.85,11.0213203435596)) ;
#75230 = CARTESIAN_POINT('',(72.9783628290596,238.8,11.0213203435596)) ;
#75231 = CARTESIAN_POINT('Origin',(73.7283628290597,237.65,6.22132034355964)) ;
#75232 = CARTESIAN_POINT('Origin',(73.7283628290597,236.1,6.22132034355964)) ;
#75233 = CARTESIAN_POINT('Origin',(74.5283628290597,239.4,6.22132034355964)) ;
#75234 = CARTESIAN_POINT('Origin',(69.3892123573611,239.4,6.22132034355964)) ;
#75235 = CARTESIAN_POINT('Origin',(77.8283628290598,239.,6.22132034355964)) ;
#75236 = CARTESIAN_POINT('Origin',(78.2283628290598,239.,6.22132034355964)) ;
#75237 = CARTESIAN_POINT('Origin',(77.8283628290598,239.8,6.22132034355964)) ;
#75238 = CARTESIAN_POINT('Origin',(78.2283628290598,239.8,6.22132034355964)) ;
#75239 = CARTESIAN_POINT('Origin',(77.8283628290598,240.2,6.22132034355964)) ;
#75240 = CARTESIAN_POINT('Origin',(78.2283628290598,239.7,6.22132034355964)) ;
#75241 = CARTESIAN_POINT('Origin',(74.9283628290597,236.1,6.22132034355964)) ;
#75242 = CARTESIAN_POINT('Origin',(75.3283628290596,236.1,6.22132034355964)) ;
#75243 = CARTESIAN_POINT('Origin',(74.9283628290597,235.7,6.22132034355964)) ;
#75244 = CARTESIAN_POINT('Origin',(75.3283628290596,239.1,6.22132034355964)) ;
#75245 = CARTESIAN_POINT('Origin',(74.8283628290597,240.2,6.22132034355964)) ;
#75246 = CARTESIAN_POINT('Origin',(74.1283628290597,236.1,6.22132034355964)) ;
#75247 = CARTESIAN_POINT('Origin',(74.1283628290597,235.7,6.22132034355964)) ;
#75248 = CARTESIAN_POINT('Origin',(74.9283628290597,242.7,6.22132034355964)) ;
#75249 = CARTESIAN_POINT('',(74.9283628290597,242.9,6.22132034355964)) ;
#75250 = CARTESIAN_POINT('Origin',(74.9283628290597,242.7,6.22132034355964)) ;
#75251 = CARTESIAN_POINT('Origin',(74.9283628290597,243.1,6.22132034355964)) ;
#75252 = CARTESIAN_POINT('Origin',(74.9283628290597,242.7,11.0213203435596)) ;
#75253 = CARTESIAN_POINT('',(74.9283628290597,242.9,11.0213203435596)) ;
#75254 = CARTESIAN_POINT('Origin',(74.1283628290597,242.7,6.22132034355964)) ;
#75255 = CARTESIAN_POINT('',(74.1283628290597,242.9,6.22132034355964)) ;
#75256 = CARTESIAN_POINT('Origin',(74.1283628290597,243.1,6.22132034355964)) ;
#75257 = CARTESIAN_POINT('',(73.9283628290597,242.7,6.22132034355964)) ;
#75258 = CARTESIAN_POINT('Origin',(74.1283628290597,242.7,6.22132034355964)) ;
#75259 = CARTESIAN_POINT('Origin',(73.7283628290597,242.7,6.22132034355964)) ;
#75260 = CARTESIAN_POINT('Origin',(74.2283628290596,243.1,6.22132034355964)) ;
#75261 = CARTESIAN_POINT('',(74.2283628290596,242.9,6.22132034355964)) ;
#75262 = CARTESIAN_POINT('Origin',(74.1283628290597,242.7,11.0213203435596)) ;
#75263 = CARTESIAN_POINT('',(73.9283628290597,242.7,11.0213203435596)) ;
#75264 = CARTESIAN_POINT('',(74.1283628290597,242.9,11.0213203435596)) ;
#75265 = CARTESIAN_POINT('Origin',(71.2283628290597,239.,6.22132034355964)) ;
#75266 = CARTESIAN_POINT('',(71.0283628290597,239.,6.22132034355964)) ;
#75267 = CARTESIAN_POINT('Origin',(70.8283628290598,239.,6.22132034355964)) ;
#75268 = CARTESIAN_POINT('',(71.2283628290597,238.8,6.22132034355964)) ;
#75269 = CARTESIAN_POINT('Origin',(71.2283628290597,239.,6.22132034355964)) ;
#75270 = CARTESIAN_POINT('Origin',(71.2283628290597,238.6,6.22132034355964)) ;
#75271 = CARTESIAN_POINT('Origin',(73.7283628290597,239.7,6.22132034355964)) ;
#75272 = CARTESIAN_POINT('',(73.9283628290597,239.7,6.22132034355964)) ;
#75273 = CARTESIAN_POINT('Origin',(71.2283628290598,239.8,6.22132034355964)) ;
#75274 = CARTESIAN_POINT('',(71.0283628290598,239.8,6.22132034355964)) ;
#75275 = CARTESIAN_POINT('Origin',(71.2283628290598,239.8,6.22132034355964)) ;
#75276 = CARTESIAN_POINT('Origin',(70.8283628290598,239.8,6.22132034355964)) ;
#75277 = CARTESIAN_POINT('Origin',(71.2283628290598,239.8,11.0213203435596)) ;
#75278 = CARTESIAN_POINT('',(71.0283628290598,239.8,11.0213203435596)) ;
#75279 = CARTESIAN_POINT('Origin',(70.8283628290598,239.1,6.22132034355964)) ;
#75280 = CARTESIAN_POINT('',(71.0283628290597,239.1,6.22132034355964)) ;
#75281 = CARTESIAN_POINT('Origin',(71.2283628290597,239.,11.0213203435596)) ;
#75282 = CARTESIAN_POINT('',(71.2283628290597,238.8,11.0213203435596)) ;
#75283 = CARTESIAN_POINT('',(71.0283628290597,239.,11.0213203435596)) ;
#75284 = CARTESIAN_POINT('Origin',(74.2283628290596,238.6,6.22132034355964)) ;
#75285 = CARTESIAN_POINT('',(74.2283628290596,238.8,6.22132034355964)) ;
#75286 = CARTESIAN_POINT('Origin',(74.8283628290597,235.7,6.22132034355964)) ;
#75287 = CARTESIAN_POINT('Origin',(76.2897596969969,233.978977857118,16.0213203435596)) ;
#75288 = CARTESIAN_POINT('Origin',(77.8787387671268,234.788603132063,16.0213203435596)) ;
#75289 = CARTESIAN_POINT('Origin',(79.1397596969969,236.049624061933,16.0213203435596)) ;
#75290 = CARTESIAN_POINT('Origin',(79.9493849719421,237.638603132063,16.0213203435596)) ;
#75291 = CARTESIAN_POINT('Origin',(80.2283628290596,239.4,16.0213203435596)) ;
#75292 = CARTESIAN_POINT('Origin',(79.9493849719421,241.161396867937,16.0213203435596)) ;
#75293 = CARTESIAN_POINT('Origin',(79.1397596969969,242.750375938067,16.0213203435596)) ;
#75294 = CARTESIAN_POINT('Origin',(77.8787387671268,244.011396867937,16.0213203435596)) ;
#75295 = CARTESIAN_POINT('Origin',(76.2897596969969,244.821022142882,16.0213203435596)) ;
#75296 = CARTESIAN_POINT('Origin',(74.5283628290597,245.1,16.0213203435596)) ;
#75297 = CARTESIAN_POINT('Origin',(72.7669659611225,244.821022142882,16.0213203435596)) ;
#75298 = CARTESIAN_POINT('Origin',(71.1779868909926,244.011396867937,16.0213203435596)) ;
#75299 = CARTESIAN_POINT('Origin',(69.9169659611225,242.750375938067,16.0213203435596)) ;
#75300 = CARTESIAN_POINT('Origin',(69.1073406861773,241.161396867937,16.0213203435596)) ;
#75301 = CARTESIAN_POINT('Origin',(68.8283628290597,239.4,16.0213203435596)) ;
#75302 = CARTESIAN_POINT('Origin',(69.1073406861773,237.638603132063,16.0213203435596)) ;
#75303 = CARTESIAN_POINT('Origin',(69.9169659611224,236.049624061933,16.0213203435596)) ;
#75304 = CARTESIAN_POINT('Origin',(71.1779868909926,234.788603132063,16.0213203435596)) ;
#75305 = CARTESIAN_POINT('Origin',(72.7669659611225,233.978977857118,16.0213203435596)) ;
#75306 = CARTESIAN_POINT('Origin',(74.5283628290597,233.7,16.0213203435596)) ;
#75307 = CARTESIAN_POINT('Origin',(73.9283628290597,240.,11.0213203435596)) ;
#75308 = CARTESIAN_POINT('Origin',(71.0283628290597,238.8,11.0213203435596)) ;
#75309 = CARTESIAN_POINT('Origin',(73.9283628290597,238.8,11.0213203435596)) ;
#75310 = CARTESIAN_POINT('Origin',(73.9283628290597,242.9,11.0213203435596)) ;
#75311 = CARTESIAN_POINT('',(0.,0.,0.)) ;
#75312 = CARTESIAN_POINT('Ctrl Pts',(70.5067868147823,213.020459099211,23.9913203435596)) ;
#75313 = CARTESIAN_POINT('Ctrl Pts',(70.5067452742029,213.0207906374,23.991193676059)) ;
#75314 = CARTESIAN_POINT('Ctrl Pts',(70.506703653514,213.021122089189,23.9910669545086)) ;
#75315 = CARTESIAN_POINT('Ctrl Pts',(70.4963561265166,213.102640079496,23.959944850052)) ;
#75316 = CARTESIAN_POINT('Ctrl Pts',(70.4746411868221,213.183771458413,23.9281127081016)) ;
#75317 = CARTESIAN_POINT('Ctrl Pts',(70.4402575595134,213.25405758073,23.9037686560088)) ;
#75318 = CARTESIAN_POINT('Ctrl Pts',(70.5067868147823,213.020459099211,23.9913203435596)) ;
#75319 = CARTESIAN_POINT('Ctrl Pts',(70.5067494667161,213.020757176667,23.9911502797591)) ;
#75320 = CARTESIAN_POINT('Ctrl Pts',(70.5067013154789,213.021058548912,23.990983638255)) ;
#75321 = CARTESIAN_POINT('Ctrl Pts',(70.4976711916085,213.094714614612,23.9494396875279)) ;
#75322 = CARTESIAN_POINT('Ctrl Pts',(70.4671561080278,213.166896466404,23.9072539242599)) ;
#75323 = CARTESIAN_POINT('Ctrl Pts',(70.4230475766717,213.224660710976,23.8845404570733)) ;
#75324 = CARTESIAN_POINT('Ctrl Pts',(70.5067868147823,213.020459099211,23.9913203435596)) ;
#75325 = CARTESIAN_POINT('Ctrl Pts',(70.5067533055873,213.020726538375,23.9911092906124)) ;
#75326 = CARTESIAN_POINT('Ctrl Pts',(70.5067104186199,213.020993688966,23.9908979379349)) ;
#75327 = CARTESIAN_POINT('Ctrl Pts',(70.4985845474206,213.086845209486,23.939048435049)) ;
#75328 = CARTESIAN_POINT('Ctrl Pts',(70.4676741716718,213.150728655563,23.8858637118865)) ;
#75329 = CARTESIAN_POINT('Ctrl Pts',(70.4200182523278,213.197323890113,23.8506292595553)) ;
#75330 = CARTESIAN_POINT('Ctrl Pts',(70.5067868147823,213.020459099211,23.9913203435596)) ;
#75331 = CARTESIAN_POINT('Ctrl Pts',(70.5067572623466,213.02069495921,23.9910670085588)) ;
#75332 = CARTESIAN_POINT('Ctrl Pts',(70.5067275799083,213.020930748899,23.9908135654576)) ;
#75333 = CARTESIAN_POINT('Ctrl Pts',(70.4992716079751,213.078911615354,23.928569356544)) ;
#75334 = CARTESIAN_POINT('Ctrl Pts',(70.4754045229177,213.13557710162,23.8649050726435)) ;
#75335 = CARTESIAN_POINT('Ctrl Pts',(70.4324364715585,213.183479571871,23.816216968458)) ;
#75336 = CARTESIAN_POINT('',(70.4324364715585,213.183479571871,23.816216968458)) ;
#75337 = CARTESIAN_POINT('',(70.4402575591012,213.254057580026,23.9037686555483)) ;
#75338 = CARTESIAN_POINT('Origin',(70.5217653290874,213.263606690954,23.816216968458)) ;
#75339 = CARTESIAN_POINT('',(70.5064330146391,213.023239669833,23.9902583635613)) ;
#75340 = CARTESIAN_POINT('Ctrl Pts',(70.4402575595134,213.25405758073,23.9037686560088)) ;
#75341 = CARTESIAN_POINT('Ctrl Pts',(70.4743890527587,213.184286864349,23.9279341939291)) ;
#75342 = CARTESIAN_POINT('Ctrl Pts',(70.4960369753435,213.103829364047,23.9594784045025)) ;
#75343 = CARTESIAN_POINT('Ctrl Pts',(70.5064330146391,213.023239669833,23.9902583635613)) ;
#75344 = CARTESIAN_POINT('',(70.5067868147824,213.020459099211,23.9913203435596)) ;
#75345 = CARTESIAN_POINT('Ctrl Pts',(70.5064330146391,213.023239669833,23.9902583635613)) ;
#75346 = CARTESIAN_POINT('Ctrl Pts',(70.5065098116199,213.022644342611,23.9904857393779)) ;
#75347 = CARTESIAN_POINT('Ctrl Pts',(70.5065859945876,213.022049008174,23.9907130734895)) ;
#75348 = CARTESIAN_POINT('Ctrl Pts',(70.506703653514,213.021122089189,23.9910669545086)) ;
#75349 = CARTESIAN_POINT('Ctrl Pts',(70.5067452742029,213.0207906374,23.991193676059)) ;
#75350 = CARTESIAN_POINT('Ctrl Pts',(70.5067868147823,213.020459099211,23.9913203435596)) ;
#75351 = CARTESIAN_POINT('Ctrl Pts',(70.5067868147823,213.020459099211,23.9913203435596)) ;
#75352 = CARTESIAN_POINT('Ctrl Pts',(70.5067572623466,213.02069495921,23.9910670085588)) ;
#75353 = CARTESIAN_POINT('Ctrl Pts',(70.5067275799083,213.020930748899,23.9908135654576)) ;
#75354 = CARTESIAN_POINT('Ctrl Pts',(70.4992716079751,213.078911615354,23.928569356544)) ;
#75355 = CARTESIAN_POINT('Ctrl Pts',(70.4754045229177,213.13557710162,23.8649050726435)) ;
#75356 = CARTESIAN_POINT('Ctrl Pts',(70.4324364715585,213.183479571871,23.816216968458)) ;
#75357 = CARTESIAN_POINT('Ctrl Pts',(70.3430483908416,213.381234213224,23.8713203435596)) ;
#75358 = CARTESIAN_POINT('Ctrl Pts',(70.3128258349002,213.391402788884,23.8713203435596)) ;
#75359 = CARTESIAN_POINT('Ctrl Pts',(70.281441089983,213.398114352515,23.8713203435596)) ;
#75360 = CARTESIAN_POINT('Ctrl Pts',(70.249702995134,213.401195935541,23.8713203435596)) ;
#75361 = CARTESIAN_POINT('Ctrl Pts',(70.3315989685636,213.347204786009,23.8713203435596)) ;
#75362 = CARTESIAN_POINT('Ctrl Pts',(70.3039711975011,213.356500329407,23.8713203435596)) ;
#75363 = CARTESIAN_POINT('Ctrl Pts',(70.2752464440296,213.362643059298,23.8713203435596)) ;
#75364 = CARTESIAN_POINT('Ctrl Pts',(70.2462332520234,213.365460070225,23.8713203435596)) ;
#75365 = CARTESIAN_POINT('Ctrl Pts',(70.3117855159125,213.288316186349,23.8411618094987)) ;
#75366 = CARTESIAN_POINT('Ctrl Pts',(70.2886148214212,213.296112117325,23.8411618094987)) ;
#75367 = CARTESIAN_POINT('Ctrl Pts',(70.2645614037344,213.301255891594,23.8411618094987)) ;
#75368 = CARTESIAN_POINT('Ctrl Pts',(70.2402287926573,213.303618445541,23.8411618094987)) ;
#75369 = CARTESIAN_POINT('Ctrl Pts',(70.3047815156687,213.267499230635,23.7782482805904)) ;
#75370 = CARTESIAN_POINT('Ctrl Pts',(70.2832009937725,213.274760137691,23.7782482805904)) ;
#75371 = CARTESIAN_POINT('Ctrl Pts',(70.2607689307802,213.279557188569,23.7782482805904)) ;
#75372 = CARTESIAN_POINT('Ctrl Pts',(70.2381062330204,213.281757603718,23.7782482805904)) ;
#75373 = CARTESIAN_POINT('Ctrl Pts',(70.3047815156687,213.267499230635,23.7513203435596)) ;
#75374 = CARTESIAN_POINT('Ctrl Pts',(70.2831939757105,213.274762498963,23.7513203435596)) ;
#75375 = CARTESIAN_POINT('Ctrl Pts',(70.2607763007697,213.279556472986,23.7513203435596)) ;
#75376 = CARTESIAN_POINT('Ctrl Pts',(70.2381062330204,213.281757603718,23.7513203435596)) ;
#75377 = CARTESIAN_POINT('',(70.2381062330204,213.281757603718,23.7513203435596)) ;
#75378 = CARTESIAN_POINT('',(70.249702995134,213.401195935541,23.8713203435596)) ;
#75379 = CARTESIAN_POINT('Origin',(70.249702995134,213.401195935541,23.7513203435596)) ;
#75380 = CARTESIAN_POINT('',(70.343048519498,213.381234190268,23.8713203435596)) ;
#75381 = CARTESIAN_POINT('Origin',(70.2090187857755,212.982714998987,23.8713203435596)) ;
#75382 = CARTESIAN_POINT('',(70.3047803801335,213.267495861574,23.7513203435596)) ;
#75383 = CARTESIAN_POINT('Origin',(70.3430483908416,213.381234213224,23.7513203435596)) ;
#75384 = CARTESIAN_POINT('Origin',(70.2090460834845,212.982842649052,23.7513203435596)) ;
#75385 = CARTESIAN_POINT('Origin',(69.2693585135591,213.496381639902,23.7513203435596)) ;
#75386 = CARTESIAN_POINT('',(60.9673257563026,214.181896061416,23.7513203435596)) ;
#75387 = CARTESIAN_POINT('',(60.9789225184162,214.301334393238,23.8713203435596)) ;
#75388 = CARTESIAN_POINT('Origin',(60.9789225184162,214.301334393238,23.7513203435596)) ;
#75389 = CARTESIAN_POINT('',(69.2693585135591,213.496381639902,23.8713203435596)) ;
#75390 = CARTESIAN_POINT('',(69.2577617514454,213.37694330808,23.7513203435596)) ;
#75391 = CARTESIAN_POINT('Ctrl Pts',(60.8382191089244,214.038138460174,23.7513203435596)) ;
#75392 = CARTESIAN_POINT('Ctrl Pts',(60.8349680037942,214.053847689931,23.7513203435596)) ;
#75393 = CARTESIAN_POINT('Ctrl Pts',(60.8347810847976,214.092067656972,23.7513203435596)) ;
#75394 = CARTESIAN_POINT('Ctrl Pts',(60.8596053972971,214.141559512008,23.7513203435596)) ;
#75395 = CARTESIAN_POINT('Ctrl Pts',(60.9078636356518,214.177314552193,23.7513203435596)) ;
#75396 = CARTESIAN_POINT('Ctrl Pts',(60.9460363791904,214.183963135178,23.7513203435596)) ;
#75397 = CARTESIAN_POINT('Ctrl Pts',(60.9673257563026,214.181896061416,23.7513203435596)) ;
#75398 = CARTESIAN_POINT('Ctrl Pts',(60.8382191089244,214.038138460174,23.7872242596007)) ;
#75399 = CARTESIAN_POINT('Ctrl Pts',(60.8349783938156,214.0537974857,23.7872242596007)) ;
#75400 = CARTESIAN_POINT('Ctrl Pts',(60.8348926282557,214.092007322074,23.7872242596007)) ;
#75401 = CARTESIAN_POINT('Ctrl Pts',(60.8597441877997,214.141459678259,23.7872242596007)) ;
#75402 = CARTESIAN_POINT('Ctrl Pts',(60.9079021315186,214.177160517204,23.7872242596007)) ;
#75403 = CARTESIAN_POINT('Ctrl Pts',(60.9461044166959,214.183956529135,23.7872242596007)) ;
#75404 = CARTESIAN_POINT('Ctrl Pts',(60.9673257563026,214.181896061416,23.7872242596007)) ;
#75405 = CARTESIAN_POINT('Ctrl Pts',(60.8086864986605,214.032026536023,23.8493568285239)) ;
#75406 = CARTESIAN_POINT('Ctrl Pts',(60.8046159279154,214.051695395846,23.8493568285239)) ;
#75407 = CARTESIAN_POINT('Ctrl Pts',(60.8043586945544,214.099523150747,23.8493568285239)) ;
#75408 = CARTESIAN_POINT('Ctrl Pts',(60.8354155723799,214.161462422765,23.8493568285239)) ;
#75409 = CARTESIAN_POINT('Ctrl Pts',(60.8958252215348,214.206215932689,23.8493568285239)) ;
#75410 = CARTESIAN_POINT('Ctrl Pts',(60.9435847316276,214.214501424618,23.8493568285239)) ;
#75411 = CARTESIAN_POINT('Ctrl Pts',(60.9702402571129,214.211913329294,23.8493568285239)) ;
#75412 = CARTESIAN_POINT('Ctrl Pts',(60.7470783802507,214.01927642205,23.8713203435596)) ;
#75413 = CARTESIAN_POINT('Ctrl Pts',(60.741304223938,214.047176949573,23.8713203435596)) ;
#75414 = CARTESIAN_POINT('Ctrl Pts',(60.7409578016198,214.115041798193,23.8713203435596)) ;
#75415 = CARTESIAN_POINT('Ctrl Pts',(60.7850319503784,214.202925235258,23.8713203435596)) ;
#75416 = CARTESIAN_POINT('Ctrl Pts',(60.8707337092228,214.266419688393,23.8713203435596)) ;
#75417 = CARTESIAN_POINT('Ctrl Pts',(60.9385090095622,214.278203740347,23.8713203435596)) ;
#75418 = CARTESIAN_POINT('Ctrl Pts',(60.9763202110832,214.274532494252,23.8713203435596)) ;
#75419 = CARTESIAN_POINT('Ctrl Pts',(60.7207092236599,214.013819190754,23.8713203435596)) ;
#75420 = CARTESIAN_POINT('Ctrl Pts',(60.7142070133995,214.045237650267,23.8713203435596)) ;
#75421 = CARTESIAN_POINT('Ctrl Pts',(60.7138331754062,214.12167758435,23.8713203435596)) ;
#75422 = CARTESIAN_POINT('Ctrl Pts',(60.7634818004053,214.220661294423,23.8713203435596)) ;
#75423 = CARTESIAN_POINT('Ctrl Pts',(60.8599982771146,214.292171374792,23.8713203435596)) ;
#75424 = CARTESIAN_POINT('Ctrl Pts',(60.9363437641918,214.305468540763,23.8713203435596)) ;
#75425 = CARTESIAN_POINT('Ctrl Pts',(60.9789225184162,214.301334393238,23.8713203435596)) ;
#75426 = CARTESIAN_POINT('',(60.8382191089243,214.038138460174,23.7513203435596)) ;
#75427 = CARTESIAN_POINT('',(60.7964818927896,214.241986587567,23.8713203435593)) ;
#75428 = CARTESIAN_POINT('Ctrl Pts',(60.8382191089244,214.038138460174,23.7513203435598)) ;
#75429 = CARTESIAN_POINT('Ctrl Pts',(60.838173023382,214.038361143952,23.7515407958386)) ;
#75430 = CARTESIAN_POINT('Ctrl Pts',(60.8381269353183,214.03858384766,23.7517613397707)) ;
#75431 = CARTESIAN_POINT('Ctrl Pts',(60.832437970542,214.066074644562,23.7789935900481)) ;
#75432 = CARTESIAN_POINT('Ctrl Pts',(60.8266291834655,214.094252337735,23.8078858434553)) ;
#75433 = CARTESIAN_POINT('Ctrl Pts',(60.8172426770213,214.140025265548,23.8402029453431)) ;
#75434 = CARTESIAN_POINT('Ctrl Pts',(60.8134587671683,214.158506292337,23.8514672560685)) ;
#75435 = CARTESIAN_POINT('Ctrl Pts',(60.8048771688427,214.20059701627,23.8670015141976)) ;
#75436 = CARTESIAN_POINT('Ctrl Pts',(60.8006691257539,214.221299002739,23.871320410552)) ;
#75437 = CARTESIAN_POINT('Ctrl Pts',(60.7964789537465,214.24198307187,23.8713203435588)) ;
#75438 = CARTESIAN_POINT('Ctrl Pts',(60.7964883386305,214.241990816335,23.8713203435596)) ;
#75439 = CARTESIAN_POINT('Ctrl Pts',(60.8137096104711,214.257238073522,23.8713203435596)) ;
#75440 = CARTESIAN_POINT('Ctrl Pts',(60.869265568141,214.293785467669,23.8713203435596)) ;
#75441 = CARTESIAN_POINT('Ctrl Pts',(60.9363437641918,214.305468540763,23.8713203435596)) ;
#75442 = CARTESIAN_POINT('Ctrl Pts',(60.9789225184162,214.301334393238,23.8713203435596)) ;
#75443 = CARTESIAN_POINT('Ctrl Pts',(60.9673257563026,214.181896061416,23.7513203435596)) ;
#75444 = CARTESIAN_POINT('Ctrl Pts',(60.9300677412812,214.185513596343,23.7513203435596)) ;
#75445 = CARTESIAN_POINT('Ctrl Pts',(60.8750422973704,214.163785096389,23.7513203435596)) ;
#75446 = CARTESIAN_POINT('Ctrl Pts',(60.8364976384102,214.097504784634,23.7513203435596)) ;
#75447 = CARTESIAN_POINT('Ctrl Pts',(60.8338841153326,214.059085002227,23.7513203435596)) ;
#75448 = CARTESIAN_POINT('Ctrl Pts',(60.8382191089243,214.038138460174,23.7513203435596)) ;
#75449 = CARTESIAN_POINT('Ctrl Pts',(70.4402575595134,213.25405758073,23.9037686560088)) ;
#75450 = CARTESIAN_POINT('Ctrl Pts',(70.4293130460961,213.276430072202,23.8960197991948)) ;
#75451 = CARTESIAN_POINT('Ctrl Pts',(70.400744289201,213.326037220728,23.8797940397281)) ;
#75452 = CARTESIAN_POINT('Ctrl Pts',(70.364672058518,213.365172858634,23.8713203435596)) ;
#75453 = CARTESIAN_POINT('Ctrl Pts',(70.3430483908423,213.381234213224,23.8713203435596)) ;
#75454 = CARTESIAN_POINT('Ctrl Pts',(70.4304232836038,213.237259369442,23.8927811137599)) ;
#75455 = CARTESIAN_POINT('Ctrl Pts',(70.4177874014361,213.257356621761,23.8853350385388)) ;
#75456 = CARTESIAN_POINT('Ctrl Pts',(70.3853635668498,213.301250711437,23.8712650795695)) ;
#75457 = CARTESIAN_POINT('Ctrl Pts',(70.3501402667773,213.333862218516,23.8687526857235)) ;
#75458 = CARTESIAN_POINT('Ctrl Pts',(70.3315989685643,213.347204786009,23.8713203435596)) ;
#75459 = CARTESIAN_POINT('Ctrl Pts',(70.4208736085904,213.208806061158,23.8653880989702)) ;
#75460 = CARTESIAN_POINT('Ctrl Pts',(70.4061885733414,213.225063832397,23.8559692034752)) ;
#75461 = CARTESIAN_POINT('Ctrl Pts',(70.3684654232861,213.259117705828,23.8385706022235)) ;
#75462 = CARTESIAN_POINT('Ctrl Pts',(70.3300695353271,213.280024504393,23.8372025575081)) ;
#75463 = CARTESIAN_POINT('Ctrl Pts',(70.3117855159529,213.288316186467,23.8411618093945)) ;
#75464 = CARTESIAN_POINT('Ctrl Pts',(70.4271143776025,213.189412851118,23.8309650932139)) ;
#75465 = CARTESIAN_POINT('Ctrl Pts',(70.4128585336131,213.204484036889,23.8172879160337)) ;
#75466 = CARTESIAN_POINT('Ctrl Pts',(70.3754254077714,213.236754374851,23.7893499112497)) ;
#75467 = CARTESIAN_POINT('Ctrl Pts',(70.3304143111952,213.258897564795,23.7770689833929)) ;
#75468 = CARTESIAN_POINT('Ctrl Pts',(70.3047815156691,213.267499230635,23.7782482805904)) ;
#75469 = CARTESIAN_POINT('Ctrl Pts',(70.4324364715585,213.183479571871,23.816216968458)) ;
#75470 = CARTESIAN_POINT('Ctrl Pts',(70.4187594848231,213.198727213537,23.80071925483)) ;
#75471 = CARTESIAN_POINT('Ctrl Pts',(70.3822800164705,213.232206696606,23.7682677358966)) ;
#75472 = CARTESIAN_POINT('Ctrl Pts',(70.3342045609418,213.257599655543,23.7513203435596)) ;
#75473 = CARTESIAN_POINT('Ctrl Pts',(70.3047815156691,213.267499230635,23.7513203435596)) ;
#75474 = CARTESIAN_POINT('Ctrl Pts',(70.3430484847436,213.381234143477,23.8713203435596)) ;
#75475 = CARTESIAN_POINT('Ctrl Pts',(70.3646721181921,213.365172793892,23.8713203575776)) ;
#75476 = CARTESIAN_POINT('Ctrl Pts',(70.4007443128316,213.326037179696,23.8797940531492)) ;
#75477 = CARTESIAN_POINT('Ctrl Pts',(70.4293130460961,213.276430072202,23.8960197991948)) ;
#75478 = CARTESIAN_POINT('Ctrl Pts',(70.4402575595134,213.25405758073,23.9037686560088)) ;
#75479 = CARTESIAN_POINT('Ctrl Pts',(70.4322999468881,213.183358207456,23.8162169311491)) ;
#75480 = CARTESIAN_POINT('Ctrl Pts',(70.4234535753444,213.193304216735,23.8061394650786)) ;
#75481 = CARTESIAN_POINT('Ctrl Pts',(70.4137714926804,213.202867974732,23.7967342679728)) ;
#75482 = CARTESIAN_POINT('Ctrl Pts',(70.4031984556939,213.211886624186,23.7883471637087)) ;
#75483 = CARTESIAN_POINT('Ctrl Pts',(70.4010445153906,213.213723904484,23.7866385418695)) ;
#75484 = CARTESIAN_POINT('Ctrl Pts',(70.3988535830009,213.215538390765,23.7849721728023)) ;
#75485 = CARTESIAN_POINT('Ctrl Pts',(70.3966251713264,213.217328431485,23.7833509803679)) ;
#75486 = CARTESIAN_POINT('Ctrl Pts',(70.3929701868672,213.220264410992,23.7806919415464)) ;
#75487 = CARTESIAN_POINT('Ctrl Pts',(70.3892143573437,213.223134648899,23.7781544356857)) ;
#75488 = CARTESIAN_POINT('Ctrl Pts',(70.3853580260576,213.225933855895,23.7757513638946)) ;
#75489 = CARTESIAN_POINT('Ctrl Pts',(70.3751864666561,213.233317116854,23.7694129594228)) ;
#75490 = CARTESIAN_POINT('Ctrl Pts',(70.364316085825,213.240200699965,23.7640098222587)) ;
#75491 = CARTESIAN_POINT('Ctrl Pts',(70.3528777612805,213.246426228203,23.7599089338264)) ;
#75492 = CARTESIAN_POINT('Ctrl Pts',(70.3412021188436,213.252780921271,23.7557229617618)) ;
#75493 = CARTESIAN_POINT('Ctrl Pts',(70.3289354346888,213.258449285322,23.752893836096)) ;
#75494 = CARTESIAN_POINT('Ctrl Pts',(70.3162582762205,213.263297580557,23.7518118574086)) ;
#75495 = CARTESIAN_POINT('Ctrl Pts',(70.3124600132869,213.264750201042,23.7514876806971)) ;
#75496 = CARTESIAN_POINT('Ctrl Pts',(70.308625136255,213.266129475579,23.7513203435596)) ;
#75497 = CARTESIAN_POINT('Ctrl Pts',(70.3047590365879,213.267432536623,23.7513203435596)) ;
#75498 = CARTESIAN_POINT('Origin',(69.2569276623894,213.37702429324,23.8713203435596)) ;
#75499 = CARTESIAN_POINT('',(70.2381062330204,213.281757603718,17.9913203435596)) ;
#75500 = CARTESIAN_POINT('',(70.2381062330204,213.281757603718,17.9913203435596)) ;
#75501 = CARTESIAN_POINT('',(60.9673257563026,214.181896061416,17.9913203435596)) ;
#75502 = CARTESIAN_POINT('',(67.5441762598793,213.543322417734,17.9913203435596)) ;
#75503 = CARTESIAN_POINT('',(60.9673257563026,214.181896061416,23.7513203435596)) ;
#75504 = CARTESIAN_POINT('Ctrl Pts',(70.5067868147823,213.020459099211,23.9913203435596)) ;
#75505 = CARTESIAN_POINT('Ctrl Pts',(70.5067868147823,213.020459099211,16.7913203435596)) ;
#75506 = CARTESIAN_POINT('Ctrl Pts',(70.4972006303894,213.096967088613,23.9913203435596)) ;
#75507 = CARTESIAN_POINT('Ctrl Pts',(70.4972006303894,213.096967088613,16.7913203435596)) ;
#75508 = CARTESIAN_POINT('Ctrl Pts',(70.4262160126144,213.22323691339,23.9913203435596)) ;
#75509 = CARTESIAN_POINT('Ctrl Pts',(70.4262160126144,213.22323691339,16.7913203435596)) ;
#75510 = CARTESIAN_POINT('Ctrl Pts',(70.2956652136715,213.276168963992,23.9913203435596)) ;
#75511 = CARTESIAN_POINT('Ctrl Pts',(70.2956652136715,213.276168963992,16.7913203435596)) ;
#75512 = CARTESIAN_POINT('Ctrl Pts',(70.2381062330204,213.281757603718,23.9913203435596)) ;
#75513 = CARTESIAN_POINT('Ctrl Pts',(70.2381062330204,213.281757603718,16.7913203435596)) ;
#75514 = CARTESIAN_POINT('',(70.5067868147823,213.020459099211,17.9913203435596)) ;
#75515 = CARTESIAN_POINT('',(70.5067868147823,213.020459099211,23.9913203435596)) ;
#75516 = CARTESIAN_POINT('Ctrl Pts',(70.2381062330204,213.281757603718,17.9913203435596)) ;
#75517 = CARTESIAN_POINT('Ctrl Pts',(70.2956652136715,213.276168963992,17.9913203435596)) ;
#75518 = CARTESIAN_POINT('Ctrl Pts',(70.4262160126144,213.22323691339,17.9913203435596)) ;
#75519 = CARTESIAN_POINT('Ctrl Pts',(70.4972006303894,213.096967088613,17.9913203435596)) ;
#75520 = CARTESIAN_POINT('Ctrl Pts',(70.5067868147823,213.020459099211,17.9913203435596)) ;
#75521 = CARTESIAN_POINT('Ctrl Pts',(70.4779346423502,213.258471670562,23.9913203435596)) ;
#75522 = CARTESIAN_POINT('Ctrl Pts',(70.4872340585151,213.179095199652,23.9913203435596)) ;
#75523 = CARTESIAN_POINT('Ctrl Pts',(70.4968510871259,213.099756817164,23.9913203435596)) ;
#75524 = CARTESIAN_POINT('Ctrl Pts',(70.5067868147824,213.020459099211,23.9913203435596)) ;
#75525 = CARTESIAN_POINT('Ctrl Pts',(70.4779346423502,213.258471670562,23.9586110212513)) ;
#75526 = CARTESIAN_POINT('Ctrl Pts',(70.4872340122281,213.179095594742,23.9586110212513)) ;
#75527 = CARTESIAN_POINT('Ctrl Pts',(70.4968511367978,213.099756420729,23.9586110212512)) ;
#75528 = CARTESIAN_POINT('Ctrl Pts',(70.5067868147824,213.020459099211,23.9586110212512)) ;
#75529 = CARTESIAN_POINT('Ctrl Pts',(70.4639600858961,213.256834469831,23.9261378065485)) ;
#75530 = CARTESIAN_POINT('Ctrl Pts',(70.4732638269676,213.177421083075,23.9261378065485)) ;
#75531 = CARTESIAN_POINT('Ctrl Pts',(70.4828854739267,213.098044597579,23.9261378065485)) ;
#75532 = CARTESIAN_POINT('Ctrl Pts',(70.4928258427598,213.01870983808,23.9261378065485)) ;
#75533 = CARTESIAN_POINT('Ctrl Pts',(70.4402575595134,213.25405758073,23.9037686560088)) ;
#75534 = CARTESIAN_POINT('Ctrl Pts',(70.4495687541354,213.174580573148,23.9037686560088)) ;
#75535 = CARTESIAN_POINT('Ctrl Pts',(70.4591979897609,213.095141478033,23.9037686560088)) ;
#75536 = CARTESIAN_POINT('Ctrl Pts',(70.4691463572047,213.015742881078,23.9037686560088)) ;
#75537 = CARTESIAN_POINT('',(70.4779346423502,213.258471670562,23.9913203435596)) ;
#75538 = CARTESIAN_POINT('Origin',(70.3587497899394,213.244508470506,23.9913203435596)) ;
#75539 = CARTESIAN_POINT('Origin',(97.0052522373154,221.373828808523,23.9913203435596)) ;
#75540 = CARTESIAN_POINT('Ctrl Pts',(70.2813572214291,216.003852832275,23.9913203435596)) ;
#75541 = CARTESIAN_POINT('Ctrl Pts',(70.3063010559943,215.086315128482,23.9913203435596)) ;
#75542 = CARTESIAN_POINT('Ctrl Pts',(70.3711537499325,214.169914953712,23.9913203435596)) ;
#75543 = CARTESIAN_POINT('Ctrl Pts',(70.4779346423502,213.258471670562,23.9913203435596)) ;
#75544 = CARTESIAN_POINT('Ctrl Pts',(70.2813572214291,216.003852832275,23.9554164275186)) ;
#75545 = CARTESIAN_POINT('Ctrl Pts',(70.3063007540173,215.086326236448,23.9554164275186)) ;
#75546 = CARTESIAN_POINT('Ctrl Pts',(70.3711551172063,214.169903283155,23.9554164275186)) ;
#75547 = CARTESIAN_POINT('Ctrl Pts',(70.4779346423502,213.258471670562,23.9554164275186)) ;
#75548 = CARTESIAN_POINT('Ctrl Pts',(70.2512097926781,216.003033255628,23.8932840272914)) ;
#75549 = CARTESIAN_POINT('Ctrl Pts',(70.2761774443025,215.084619461598,23.8932840272914)) ;
#75550 = CARTESIAN_POINT('Ctrl Pts',(70.3410922094225,214.167326164876,23.8932840272914)) ;
#75551 = CARTESIAN_POINT('Ctrl Pts',(70.4479809393324,213.254962419687,23.8932840272914)) ;
#75552 = CARTESIAN_POINT('Ctrl Pts',(70.1883195322401,216.001323544685,23.8713203435596)) ;
#75553 = CARTESIAN_POINT('Ctrl Pts',(70.2133366971056,215.081088448267,23.8713203435596)) ;
#75554 = CARTESIAN_POINT('Ctrl Pts',(70.2783818952035,214.161919097311,23.8713203435596)) ;
#75555 = CARTESIAN_POINT('Ctrl Pts',(70.3854948082789,213.247641805271,23.8713203435596)) ;
#75556 = CARTESIAN_POINT('Ctrl Pts',(70.1614015403525,216.000591762292,23.8713203435596)) ;
#75557 = CARTESIAN_POINT('Ctrl Pts',(70.1864398654763,215.079578303801,23.8713203435596)) ;
#75558 = CARTESIAN_POINT('Ctrl Pts',(70.2515410686805,214.159603546732,23.8713203435596)) ;
#75559 = CARTESIAN_POINT('Ctrl Pts',(70.3587497899394,213.244508470506,23.8713203435596)) ;
#75560 = CARTESIAN_POINT('',(70.1614015403524,216.000591762293,23.8713203435596)) ;
#75561 = CARTESIAN_POINT('Origin',(97.3863035375064,222.371901130348,23.8713203435596)) ;
#75562 = CARTESIAN_POINT('',(70.2813572214291,216.003852832276,23.9913203435596)) ;
#75563 = CARTESIAN_POINT('Origin',(70.1614015403524,216.000591762293,23.9913203435596)) ;
#75564 = CARTESIAN_POINT('Origin',(97.5077297430571,222.403214886601,23.9913203435596)) ;
#75565 = CARTESIAN_POINT('Ctrl Pts',(73.7436956568154,200.410454788892,30.2513203435596)) ;
#75566 = CARTESIAN_POINT('Ctrl Pts',(75.7987505865357,196.993517189618,30.2513203435596)) ;
#75567 = CARTESIAN_POINT('Ctrl Pts',(78.3337590639418,193.889658425843,30.2513203435596)) ;
#75568 = CARTESIAN_POINT('Ctrl Pts',(81.068251094894,190.995574215667,30.2513203435596)) ;
#75569 = CARTESIAN_POINT('Ctrl Pts',(73.7436956568154,200.410454788892,30.2872242596007)) ;
#75570 = CARTESIAN_POINT('Ctrl Pts',(75.7987702584097,196.993484481214,30.2872242596007)) ;
#75571 = CARTESIAN_POINT('Ctrl Pts',(78.3337453944066,193.889672893168,30.2872242596007)) ;
#75572 = CARTESIAN_POINT('Ctrl Pts',(81.068251094894,190.995574215667,30.2872242596007)) ;
#75573 = CARTESIAN_POINT('Ctrl Pts',(73.769540015645,200.425998408134,30.3493567430526)) ;
#75574 = CARTESIAN_POINT('Ctrl Pts',(75.8230434158966,197.011640535222,30.3493567430526)) ;
#75575 = CARTESIAN_POINT('Ctrl Pts',(78.3567583097309,193.909229680419,30.3493567430526)) ;
#75576 = CARTESIAN_POINT('Ctrl Pts',(81.0901722183543,191.016286514639,30.3493567430526)) ;
#75577 = CARTESIAN_POINT('Ctrl Pts',(73.8234538668466,200.45842391269,30.3713203435596)) ;
#75578 = CARTESIAN_POINT('Ctrl Pts',(75.8737317953243,197.049429028193,30.3713203435596)) ;
#75579 = CARTESIAN_POINT('Ctrl Pts',(78.4047292161471,193.9500654395,30.3713203435596)) ;
#75580 = CARTESIAN_POINT('Ctrl Pts',(81.1359018182332,191.059494388828,30.3713203435596)) ;
#75581 = CARTESIAN_POINT('Ctrl Pts',(73.8465297930579,200.47230250852,30.3713203435596)) ;
#75582 = CARTESIAN_POINT('Ctrl Pts',(75.8954292657049,197.065599581035,30.3713203435596)) ;
#75583 = CARTESIAN_POINT('Ctrl Pts',(78.4252600190873,193.9675452886,30.3713203435596)) ;
#75584 = CARTESIAN_POINT('Ctrl Pts',(81.1554747637557,191.077987998436,30.3713203435596)) ;
#75585 = CARTESIAN_POINT('',(81.068251094894,190.995574215667,30.2513203435596)) ;
#75586 = CARTESIAN_POINT('',(81.1554747637557,191.077987998436,30.3713203435596)) ;
#75587 = CARTESIAN_POINT('Origin',(81.1554747637557,191.077987998436,30.2513203435596)) ;
#75588 = CARTESIAN_POINT('',(73.8465297930579,200.47230250852,30.3713203435596)) ;
#75589 = CARTESIAN_POINT('Ctrl Pts',(81.1554747637557,191.077987998436,30.3713203435596)) ;
#75590 = CARTESIAN_POINT('Ctrl Pts',(78.4252600190873,193.9675452886,30.3713203435596)) ;
#75591 = CARTESIAN_POINT('Ctrl Pts',(75.8954292657049,197.065599581035,30.3713203435596)) ;
#75592 = CARTESIAN_POINT('Ctrl Pts',(73.8465297930579,200.47230250852,30.3713203435596)) ;
#75593 = CARTESIAN_POINT('',(73.7436956568154,200.410454788892,30.2513203435596)) ;
#75594 = CARTESIAN_POINT('Origin',(73.8465297930579,200.47230250852,30.2513203435596)) ;
#75595 = CARTESIAN_POINT('Ctrl Pts',(73.7436956568154,200.410454788892,30.2513203435596)) ;
#75596 = CARTESIAN_POINT('Ctrl Pts',(75.7987505865357,196.993517189618,30.2513203435596)) ;
#75597 = CARTESIAN_POINT('Ctrl Pts',(78.3337590639418,193.889658425843,30.2513203435596)) ;
#75598 = CARTESIAN_POINT('Ctrl Pts',(81.068251094894,190.995574215667,30.2513203435596)) ;
#75599 = CARTESIAN_POINT('Ctrl Pts',(80.8501919227397,190.369539758744,30.3713203435596)) ;
#75600 = CARTESIAN_POINT('Ctrl Pts',(80.989856244946,190.369539758744,30.3713203435596)) ;
#75601 = CARTESIAN_POINT('Ctrl Pts',(81.2186255309631,190.49593104996,30.3713203435596)) ;
#75602 = CARTESIAN_POINT('Ctrl Pts',(81.299864395013,190.831780335431,30.3713203435596)) ;
#75603 = CARTESIAN_POINT('Ctrl Pts',(81.2194206810384,191.01031002848,30.3713203435596)) ;
#75604 = CARTESIAN_POINT('Ctrl Pts',(81.1554747637557,191.077987998436,30.3713203435596)) ;
#75605 = CARTESIAN_POINT('Ctrl Pts',(80.8501919227397,190.405443674785,30.3713203435596)) ;
#75606 = CARTESIAN_POINT('Ctrl Pts',(80.9778652382259,190.405443674785,30.3713203435596)) ;
#75607 = CARTESIAN_POINT('Ctrl Pts',(81.1870720669225,190.521166083618,30.3713203435596)) ;
#75608 = CARTESIAN_POINT('Ctrl Pts',(81.2613364057291,190.82818145774,30.3713203435596)) ;
#75609 = CARTESIAN_POINT('Ctrl Pts',(81.1878332857695,190.991462435668,30.3713203435596)) ;
#75610 = CARTESIAN_POINT('Ctrl Pts',(81.129377503059,191.053329852293,30.3713203435596)) ;
#75611 = CARTESIAN_POINT('Ctrl Pts',(80.8501919227397,190.467576190064,30.3411618724029)) ;
#75612 = CARTESIAN_POINT('Ctrl Pts',(80.9572682185845,190.467576190064,30.3411618724029)) ;
#75613 = CARTESIAN_POINT('Ctrl Pts',(81.1326396018592,190.564432599516,30.3411618724029)) ;
#75614 = CARTESIAN_POINT('Ctrl Pts',(81.1949228397646,190.821917634261,30.3411618724029)) ;
#75615 = CARTESIAN_POINT('Ctrl Pts',(81.1332409679373,190.958771792307,30.3411618724029)) ;
#75616 = CARTESIAN_POINT('Ctrl Pts',(81.0842156202403,191.010658388817,30.3411618724029)) ;
#75617 = CARTESIAN_POINT('Ctrl Pts',(80.8501919227397,190.489539758744,30.2782482805904)) ;
#75618 = CARTESIAN_POINT('Ctrl Pts',(80.9499197210544,190.489539758744,30.2782482805904)) ;
#75619 = CARTESIAN_POINT('Ctrl Pts',(81.1133225940155,190.579904354768,30.2782482805904)) ;
#75620 = CARTESIAN_POINT('Ctrl Pts',(81.1713316842795,190.819719172513,30.2782482805904)) ;
#75621 = CARTESIAN_POINT('Ctrl Pts',(81.1139119010403,190.947248524242,30.2782482805904)) ;
#75622 = CARTESIAN_POINT('Ctrl Pts',(81.068251094894,190.995574215667,30.2782482805904)) ;
#75623 = CARTESIAN_POINT('Ctrl Pts',(80.8501919227397,190.489539758744,30.2513203435596)) ;
#75624 = CARTESIAN_POINT('Ctrl Pts',(80.9499521528871,190.489539758744,30.2513203435596)) ;
#75625 = CARTESIAN_POINT('Ctrl Pts',(81.1133587857564,190.579819252469,30.2513203435596)) ;
#75626 = CARTESIAN_POINT('Ctrl Pts',(81.1713865457921,190.819711599235,30.2513203435597)) ;
#75627 = CARTESIAN_POINT('Ctrl Pts',(81.1139267500959,190.947232808556,30.2513203435596)) ;
#75628 = CARTESIAN_POINT('Ctrl Pts',(81.068251094894,190.995574215667,30.2513203435596)) ;
#75629 = CARTESIAN_POINT('',(80.8501919227397,190.489539758744,30.2513203435596)) ;
#75630 = CARTESIAN_POINT('Ctrl Pts',(81.068251094894,190.995574215667,30.2513203435596)) ;
#75631 = CARTESIAN_POINT('Ctrl Pts',(81.1139267500959,190.947232808556,30.2513203435596)) ;
#75632 = CARTESIAN_POINT('Ctrl Pts',(81.1713865457921,190.819711599235,30.2513203435597)) ;
#75633 = CARTESIAN_POINT('Ctrl Pts',(81.1133587857564,190.579819252469,30.2513203435596)) ;
#75634 = CARTESIAN_POINT('Ctrl Pts',(80.9499521528871,190.489539758744,30.2513203435596)) ;
#75635 = CARTESIAN_POINT('Ctrl Pts',(80.8501919227397,190.489539758744,30.2513203435596)) ;
#75636 = CARTESIAN_POINT('',(80.8501919227397,190.369539758744,30.3713203435596)) ;
#75637 = CARTESIAN_POINT('Origin',(80.8501919227397,190.369539758744,30.2513203435596)) ;
#75638 = CARTESIAN_POINT('Ctrl Pts',(80.8501919227397,190.369539758744,30.3713203435596)) ;
#75639 = CARTESIAN_POINT('Ctrl Pts',(80.989856244946,190.369539758744,30.3713203435596)) ;
#75640 = CARTESIAN_POINT('Ctrl Pts',(81.2186255309631,190.49593104996,30.3713203435596)) ;
#75641 = CARTESIAN_POINT('Ctrl Pts',(81.299864395013,190.831780335431,30.3713203435596)) ;
#75642 = CARTESIAN_POINT('Ctrl Pts',(81.2194206810384,191.01031002848,30.3713203435596)) ;
#75643 = CARTESIAN_POINT('Ctrl Pts',(81.1554747637557,191.077987998436,30.3713203435596)) ;
#75644 = CARTESIAN_POINT('Origin',(75.6106165726094,190.369539758744,30.2513203435596)) ;
#75645 = CARTESIAN_POINT('',(78.1546571314538,190.489539758744,30.2513203435596)) ;
#75646 = CARTESIAN_POINT('',(78.1546571314538,190.369539758744,30.3713203435596)) ;
#75647 = CARTESIAN_POINT('Origin',(78.1546571314538,190.369539758744,30.2513203435596)) ;
#75648 = CARTESIAN_POINT('',(75.6106165726094,190.369539758744,30.3713203435596)) ;
#75649 = CARTESIAN_POINT('',(75.6106165726094,190.489539758744,30.2513203435596)) ;
#75650 = CARTESIAN_POINT('Ctrl Pts',(77.491702623914,190.586826448256,30.3713203435596)) ;
#75651 = CARTESIAN_POINT('Ctrl Pts',(77.6823045866468,190.44684797572,30.3713203435596)) ;
#75652 = CARTESIAN_POINT('Ctrl Pts',(77.9181765170879,190.369539758744,30.3713203435596)) ;
#75653 = CARTESIAN_POINT('Ctrl Pts',(78.1546571314538,190.369539758744,30.3713203435596)) ;
#75654 = CARTESIAN_POINT('Ctrl Pts',(77.5129550015727,190.615764790139,30.3713203435596)) ;
#75655 = CARTESIAN_POINT('Ctrl Pts',(77.6974203503338,190.480293059496,30.3713203435596)) ;
#75656 = CARTESIAN_POINT('Ctrl Pts',(77.9257902384858,190.405443674785,30.3713203435596)) ;
#75657 = CARTESIAN_POINT('Ctrl Pts',(78.1546571314538,190.405443674785,30.3713203435596)) ;
#75658 = CARTESIAN_POINT('Ctrl Pts',(77.5497327415575,190.665843272201,30.3411619198148)) ;
#75659 = CARTESIAN_POINT('Ctrl Pts',(77.723657194007,190.538112797439,30.3411619198148)) ;
#75660 = CARTESIAN_POINT('Ctrl Pts',(77.9388683705258,190.467576246952,30.3411619198148)) ;
#75661 = CARTESIAN_POINT('Ctrl Pts',(78.1546571314538,190.467576246952,30.3411619198148)) ;
#75662 = CARTESIAN_POINT('Ctrl Pts',(77.5627334640076,190.683545731522,30.2782482805904)) ;
#75663 = CARTESIAN_POINT('Ctrl Pts',(77.7328971903007,190.558577141766,30.2782482805904)) ;
#75664 = CARTESIAN_POINT('Ctrl Pts',(77.9435343184476,190.489539758744,30.2782482805904)) ;
#75665 = CARTESIAN_POINT('Ctrl Pts',(78.1546571314538,190.489539758744,30.2782482805904)) ;
#75666 = CARTESIAN_POINT('Ctrl Pts',(77.5627334640076,190.683545731522,30.2513203435596)) ;
#75667 = CARTESIAN_POINT('Ctrl Pts',(77.732913787876,190.558564952473,30.2513203435596)) ;
#75668 = CARTESIAN_POINT('Ctrl Pts',(77.9435137257698,190.489539758744,30.2513203435596)) ;
#75669 = CARTESIAN_POINT('Ctrl Pts',(78.1546571314538,190.489539758744,30.2513203435596)) ;
#75670 = CARTESIAN_POINT('',(77.5627334640076,190.683545731522,30.2513203435596)) ;
#75671 = CARTESIAN_POINT('Origin',(78.0776054738973,191.254450606239,30.2513203435596)) ;
#75672 = CARTESIAN_POINT('',(77.491702623914,190.586826448256,30.3713203435596)) ;
#75673 = CARTESIAN_POINT('Origin',(77.491702623914,190.586826448256,30.2513203435596)) ;
#75674 = CARTESIAN_POINT('Origin',(78.0683592750124,191.226239907973,30.3713203435596)) ;
#75675 = CARTESIAN_POINT('Ctrl Pts',(77.5627334640075,190.683545731522,30.2513203435596)) ;
#75676 = CARTESIAN_POINT('Ctrl Pts',(73.9385194970161,193.345175905566,30.2513203435596)) ;
#75677 = CARTESIAN_POINT('Ctrl Pts',(70.594189416785,196.433476943649,30.2513203435596)) ;
#75678 = CARTESIAN_POINT('Ctrl Pts',(67.9762844730848,200.080907092773,30.2513203435596)) ;
#75679 = CARTESIAN_POINT('Ctrl Pts',(77.5627334640075,190.683545731522,30.2872242596007)) ;
#75680 = CARTESIAN_POINT('Ctrl Pts',(73.9385438761009,193.345158001516,30.2872242596007)) ;
#75681 = CARTESIAN_POINT('Ctrl Pts',(70.594158916818,196.433519438125,30.2872242596007)) ;
#75682 = CARTESIAN_POINT('Ctrl Pts',(67.9762844730848,200.080907092773,30.2872242596007)) ;
#75683 = CARTESIAN_POINT('Ctrl Pts',(77.544881982401,190.659238226445,30.3493568382152)) ;
#75684 = CARTESIAN_POINT('Ctrl Pts',(73.9187452261289,193.322280500881,30.3493568382152)) ;
#75685 = CARTESIAN_POINT('Ctrl Pts',(70.5720941363296,196.412540172779,30.3493568382152)) ;
#75686 = CARTESIAN_POINT('Ctrl Pts',(67.951783646648,200.063321880163,30.3493568382152)) ;
#75687 = CARTESIAN_POINT('Ctrl Pts',(77.507641907158,190.608530204668,30.3713203435596)) ;
#75688 = CARTESIAN_POINT('Ctrl Pts',(73.8775078677682,193.274508092028,30.3713203435596)) ;
#75689 = CARTESIAN_POINT('Ctrl Pts',(70.5259837109279,196.368888014437,30.3713203435596)) ;
#75690 = CARTESIAN_POINT('Ctrl Pts',(67.9006723361061,200.026637270156,30.3713203435596)) ;
#75691 = CARTESIAN_POINT('Ctrl Pts',(77.491702623914,190.586826448256,30.3713203435596)) ;
#75692 = CARTESIAN_POINT('Ctrl Pts',(73.8598602830395,193.254058915732,30.3713203435596)) ;
#75693 = CARTESIAN_POINT('Ctrl Pts',(70.5062445476854,196.350208787435,30.3713203435596)) ;
#75694 = CARTESIAN_POINT('Ctrl Pts',(67.8787959663517,200.010935733954,30.3713203435596)) ;
#75695 = CARTESIAN_POINT('',(67.9762844730848,200.080907092773,30.2513203435596)) ;
#75696 = CARTESIAN_POINT('',(67.8787959663517,200.010935733954,30.3713203435596)) ;
#75697 = CARTESIAN_POINT('Origin',(67.8787959663517,200.010935733954,30.2513203435596)) ;
#75698 = CARTESIAN_POINT('Ctrl Pts',(67.8787959663517,200.010935733954,30.3713203435596)) ;
#75699 = CARTESIAN_POINT('Ctrl Pts',(70.5062445476854,196.350208787435,30.3713203435596)) ;
#75700 = CARTESIAN_POINT('Ctrl Pts',(73.8598602830395,193.254058915732,30.3713203435596)) ;
#75701 = CARTESIAN_POINT('Ctrl Pts',(77.491702623914,190.586826448256,30.3713203435596)) ;
#75702 = CARTESIAN_POINT('Ctrl Pts',(77.5627334640075,190.683545731522,30.2513203435596)) ;
#75703 = CARTESIAN_POINT('Ctrl Pts',(73.9385194970161,193.345175905566,30.2513203435596)) ;
#75704 = CARTESIAN_POINT('Ctrl Pts',(70.594189416785,196.433476943649,30.2513203435596)) ;
#75705 = CARTESIAN_POINT('Ctrl Pts',(67.9762844730848,200.080907092773,30.2513203435596)) ;
#75706 = CARTESIAN_POINT('Ctrl Pts',(68.2200057399177,200.67583548982,30.3713203435596)) ;
#75707 = CARTESIAN_POINT('Ctrl Pts',(68.0884112603097,200.67583548982,30.3713203435596)) ;
#75708 = CARTESIAN_POINT('Ctrl Pts',(67.8720857272373,200.564584339121,30.3713203435596)) ;
#75709 = CARTESIAN_POINT('Ctrl Pts',(67.7720303794687,200.257091150086,30.3713203435596)) ;
#75710 = CARTESIAN_POINT('Ctrl Pts',(67.8276412744005,200.082207674573,30.3713203435596)) ;
#75711 = CARTESIAN_POINT('Ctrl Pts',(67.8787959663517,200.010935733954,30.3713203435596)) ;
#75712 = CARTESIAN_POINT('Ctrl Pts',(68.2200057399177,200.639931573779,30.3713203435596)) ;
#75713 = CARTESIAN_POINT('Ctrl Pts',(68.0997094233937,200.639931573779,30.3713203435596)) ;
#75714 = CARTESIAN_POINT('Ctrl Pts',(67.9018687303379,200.538060654086,30.3713203435596)) ;
#75715 = CARTESIAN_POINT('Ctrl Pts',(67.8104033772253,200.256966885486,30.3713203435596)) ;
#75716 = CARTESIAN_POINT('Ctrl Pts',(67.8612016997572,200.097023939243,30.3713203435596)) ;
#75717 = CARTESIAN_POINT('Ctrl Pts',(67.9079644593576,200.031871115557,30.3713203435596)) ;
#75718 = CARTESIAN_POINT('Ctrl Pts',(68.2200057399177,200.577799006671,30.3411619155991)) ;
#75719 = CARTESIAN_POINT('Ctrl Pts',(68.1191163416272,200.577799006671,30.3411619155991)) ;
#75720 = CARTESIAN_POINT('Ctrl Pts',(67.9532874484581,200.492547433761,30.341161915599)) ;
#75721 = CARTESIAN_POINT('Ctrl Pts',(67.8765782061601,200.256802125843,30.3411619155991)) ;
#75722 = CARTESIAN_POINT('Ctrl Pts',(67.9192225065329,200.122742265589,30.3411619155991)) ;
#75723 = CARTESIAN_POINT('Ctrl Pts',(67.9584412192484,200.068100283452,30.3411619155991)) ;
#75724 = CARTESIAN_POINT('Ctrl Pts',(68.2200057399177,200.55583548982,30.2782482805904)) ;
#75725 = CARTESIAN_POINT('Ctrl Pts',(68.1260402409674,200.55583548982,30.2782482805904)) ;
#75726 = CARTESIAN_POINT('Ctrl Pts',(67.9715170756471,200.476288797847,30.2782482805904)) ;
#75727 = CARTESIAN_POINT('Ctrl Pts',(67.900071986214,200.256721779767,30.2782482805904)) ;
#75728 = CARTESIAN_POINT('Ctrl Pts',(67.9397572861757,200.131799071535,30.2782482805904)) ;
#75729 = CARTESIAN_POINT('Ctrl Pts',(67.9762844730848,200.080907092773,30.2782482805904)) ;
#75730 = CARTESIAN_POINT('Ctrl Pts',(68.2200057399177,200.55583548982,30.2513203435596)) ;
#75731 = CARTESIAN_POINT('Ctrl Pts',(68.1260096830549,200.55583548982,30.2513203435596)) ;
#75732 = CARTESIAN_POINT('Ctrl Pts',(67.9714914451459,200.476370382178,30.2513203435596)) ;
#75733 = CARTESIAN_POINT('Ctrl Pts',(67.900023339597,200.25673239001,30.2513203435596)) ;
#75734 = CARTESIAN_POINT('Ctrl Pts',(67.9397454074054,200.131815621786,30.2513203435596)) ;
#75735 = CARTESIAN_POINT('Ctrl Pts',(67.9762844730848,200.080907092773,30.2513203435596)) ;
#75736 = CARTESIAN_POINT('',(68.2200057399177,200.55583548982,30.2513203435596)) ;
#75737 = CARTESIAN_POINT('Ctrl Pts',(67.9762844730848,200.080907092773,30.2513203435596)) ;
#75738 = CARTESIAN_POINT('Ctrl Pts',(67.9397454074054,200.131815621786,30.2513203435596)) ;
#75739 = CARTESIAN_POINT('Ctrl Pts',(67.900023339597,200.25673239001,30.2513203435596)) ;
#75740 = CARTESIAN_POINT('Ctrl Pts',(67.9714914451459,200.476370382178,30.2513203435596)) ;
#75741 = CARTESIAN_POINT('Ctrl Pts',(68.1260096830549,200.55583548982,30.2513203435596)) ;
#75742 = CARTESIAN_POINT('Ctrl Pts',(68.2200057399177,200.55583548982,30.2513203435596)) ;
#75743 = CARTESIAN_POINT('',(68.2200057399177,200.67583548982,30.3713203435596)) ;
#75744 = CARTESIAN_POINT('Origin',(68.2200057399177,200.67583548982,30.2513203435596)) ;
#75745 = CARTESIAN_POINT('Ctrl Pts',(68.2200057399177,200.67583548982,30.3713203435596)) ;
#75746 = CARTESIAN_POINT('Ctrl Pts',(68.0884112603097,200.67583548982,30.3713203435596)) ;
#75747 = CARTESIAN_POINT('Ctrl Pts',(67.8720857272373,200.564584339121,30.3713203435596)) ;
#75748 = CARTESIAN_POINT('Ctrl Pts',(67.7720303794687,200.257091150086,30.3713203435596)) ;
#75749 = CARTESIAN_POINT('Ctrl Pts',(67.8276412744005,200.082207674573,30.3713203435596)) ;
#75750 = CARTESIAN_POINT('Ctrl Pts',(67.8787959663517,200.010935733954,30.3713203435596)) ;
#75751 = CARTESIAN_POINT('Origin',(68.6561288592431,200.67583548982,30.2513203435596)) ;
#75752 = CARTESIAN_POINT('',(73.4866103162092,200.55583548982,30.2513203435596)) ;
#75753 = CARTESIAN_POINT('',(73.4866103162092,200.67583548982,30.3713203435596)) ;
#75754 = CARTESIAN_POINT('Origin',(73.4866103162092,200.67583548982,30.2513203435596)) ;
#75755 = CARTESIAN_POINT('',(68.6561288592431,200.67583548982,30.3713203435596)) ;
#75756 = CARTESIAN_POINT('',(68.6561288592431,200.55583548982,30.2513203435596)) ;
#75757 = CARTESIAN_POINT('Ctrl Pts',(73.8469698134568,200.47159949769,30.371320342471)) ;
#75758 = CARTESIAN_POINT('Ctrl Pts',(73.7726721832933,200.595732430761,30.371320342471)) ;
#75759 = CARTESIAN_POINT('Ctrl Pts',(73.6304497677198,200.676158620816,30.371320342471)) ;
#75760 = CARTESIAN_POINT('Ctrl Pts',(73.4857810847946,200.675850235661,30.371320342471)) ;
#75761 = CARTESIAN_POINT('Ctrl Pts',(73.8161607140537,200.453153015436,30.3713253446552)) ;
#75762 = CARTESIAN_POINT('Ctrl Pts',(73.7482432100789,200.566626907111,30.3713253446551)) ;
#75763 = CARTESIAN_POINT('Ctrl Pts',(73.6180983919013,200.640223265598,30.3713253446551)) ;
#75764 = CARTESIAN_POINT('Ctrl Pts',(73.4858522887322,200.639941069093,30.3713253446551)) ;
#75765 = CARTESIAN_POINT('Ctrl Pts',(73.7628460214403,200.421230580689,30.3411670622856)) ;
#75766 = CARTESIAN_POINT('Ctrl Pts',(73.7058860185115,200.516396497646,30.3411670622856)) ;
#75767 = CARTESIAN_POINT('Ctrl Pts',(73.5968841830501,200.578036586515,30.3411670622856)) ;
#75768 = CARTESIAN_POINT('Ctrl Pts',(73.4859745900404,200.577800234443,30.3411670622856)) ;
#75769 = CARTESIAN_POINT('Ctrl Pts',(73.7440002787433,200.40994706903,30.2782482805904)) ;
#75770 = CARTESIAN_POINT('Ctrl Pts',(73.6909501011225,200.498581129447,30.2782482805904)) ;
#75771 = CARTESIAN_POINT('Ctrl Pts',(73.5893152199704,200.556055236005,30.2782482805904)) ;
#75772 = CARTESIAN_POINT('Ctrl Pts',(73.4860182236672,200.555834858296,30.2782482805904)) ;
#75773 = CARTESIAN_POINT('Ctrl Pts',(73.7440003787313,200.409946903396,30.2513203435596)) ;
#75774 = CARTESIAN_POINT('Ctrl Pts',(73.6909326264421,200.49860997033,30.2513203435596)) ;
#75775 = CARTESIAN_POINT('Ctrl Pts',(73.5893489416074,200.556055125582,30.2513203435596)) ;
#75776 = CARTESIAN_POINT('Ctrl Pts',(73.4860180301928,200.555834858614,30.2513203435596)) ;
#75777 = CARTESIAN_POINT('Origin',(73.5222221716454,200.318810051956,30.2513203435596)) ;
#75778 = CARTESIAN_POINT('Origin',(73.5364669138164,200.343999876809,30.3713203435596)) ;
#75779 = CARTESIAN_POINT('Ctrl Pts',(78.1546571314538,190.489539758744,23.4913203435596)) ;
#75780 = CARTESIAN_POINT('Ctrl Pts',(78.1546571314538,190.489539758744,31.6033203435596)) ;
#75781 = CARTESIAN_POINT('Ctrl Pts',(77.9435093125031,190.489539758744,23.4913203435596)) ;
#75782 = CARTESIAN_POINT('Ctrl Pts',(77.9435093125031,190.489539758744,31.6033203435596)) ;
#75783 = CARTESIAN_POINT('Ctrl Pts',(77.7329173449427,190.558562340156,23.4913203435596)) ;
#75784 = CARTESIAN_POINT('Ctrl Pts',(77.7329173449427,190.558562340156,31.6033203435596)) ;
#75785 = CARTESIAN_POINT('Ctrl Pts',(77.5627334640076,190.683545731522,23.4913203435596)) ;
#75786 = CARTESIAN_POINT('Ctrl Pts',(77.5627334640076,190.683545731522,31.6033203435596)) ;
#75787 = CARTESIAN_POINT('',(78.1546571314538,190.489539758744,23.4913203435596)) ;
#75788 = CARTESIAN_POINT('',(78.1546571314538,190.489539758744,30.2513203435596)) ;
#75789 = CARTESIAN_POINT('',(77.5627334640076,190.683545731522,23.4913203435596)) ;
#75790 = CARTESIAN_POINT('Origin',(78.077605473898,191.254450606248,23.4913203435596)) ;
#75791 = CARTESIAN_POINT('',(77.5627334640076,190.683545731522,23.4913203435596)) ;
#75792 = CARTESIAN_POINT('Origin',(81.5507230003364,190.489539758744,23.8713203435596)) ;
#75793 = CARTESIAN_POINT('',(80.8501919227397,190.489539758744,23.4913203435596)) ;
#75794 = CARTESIAN_POINT('',(80.8501919227397,190.489539758744,23.4913203435596)) ;
#75795 = CARTESIAN_POINT('',(78.07353074889,190.489539758744,23.4913203435596)) ;
#75796 = CARTESIAN_POINT('Ctrl Pts',(81.068251094894,190.995574215667,23.4913203435596)) ;
#75797 = CARTESIAN_POINT('Ctrl Pts',(81.068251094894,190.995574215667,31.6033203435596)) ;
#75798 = CARTESIAN_POINT('Ctrl Pts',(81.1139288980579,190.947230535233,23.4913203435596)) ;
#75799 = CARTESIAN_POINT('Ctrl Pts',(81.1139288980579,190.947230535233,31.6033203435596)) ;
#75800 = CARTESIAN_POINT('Ctrl Pts',(81.1716384658622,190.819103522118,23.4913203435596)) ;
#75801 = CARTESIAN_POINT('Ctrl Pts',(81.1716384658622,190.819103522118,31.6033203435596)) ;
#75802 = CARTESIAN_POINT('Ctrl Pts',(81.1216272012763,190.614215654147,23.4913203435596)) ;
#75803 = CARTESIAN_POINT('Ctrl Pts',(81.1216272012763,190.614215654147,31.6033203435596)) ;
#75804 = CARTESIAN_POINT('Ctrl Pts',(80.983303578287,190.505926367357,23.4913203435596)) ;
#75805 = CARTESIAN_POINT('Ctrl Pts',(80.983303578287,190.505926367357,31.6033203435596)) ;
#75806 = CARTESIAN_POINT('Ctrl Pts',(80.8834468965772,190.489539758744,23.4913203435596)) ;
#75807 = CARTESIAN_POINT('Ctrl Pts',(80.8834468965772,190.489539758744,31.6033203435596)) ;
#75808 = CARTESIAN_POINT('Ctrl Pts',(80.8501919227397,190.489539758744,23.4913203435596)) ;
#75809 = CARTESIAN_POINT('Ctrl Pts',(80.8501919227397,190.489539758744,31.6033203435596)) ;
#75810 = CARTESIAN_POINT('',(81.068251094894,190.995574215667,23.4913203435596)) ;
#75811 = CARTESIAN_POINT('',(81.068251094894,190.995574215667,30.2513203435596)) ;
#75812 = CARTESIAN_POINT('Ctrl Pts',(80.8501919227397,190.489539758744,23.4913203435596)) ;
#75813 = CARTESIAN_POINT('Ctrl Pts',(80.8834468965772,190.489539758744,23.4913203435596)) ;
#75814 = CARTESIAN_POINT('Ctrl Pts',(80.983303578287,190.505926367357,23.4913203435596)) ;
#75815 = CARTESIAN_POINT('Ctrl Pts',(81.1216272012763,190.614215654147,23.4913203435596)) ;
#75816 = CARTESIAN_POINT('Ctrl Pts',(81.1716384658622,190.819103522118,23.4913203435596)) ;
#75817 = CARTESIAN_POINT('Ctrl Pts',(81.1139288980579,190.947230535233,23.4913203435596)) ;
#75818 = CARTESIAN_POINT('Ctrl Pts',(81.068251094894,190.995574215667,23.4913203435596)) ;
#75819 = CARTESIAN_POINT('Ctrl Pts',(73.6566785252795,200.55583548982,17.854339447693)) ;
#75820 = CARTESIAN_POINT('Ctrl Pts',(73.6566785252795,200.55583548982,32.8747165227329)) ;
#75821 = CARTESIAN_POINT('Ctrl Pts',(75.7001422864503,197.125245060908,17.854339447693)) ;
#75822 = CARTESIAN_POINT('Ctrl Pts',(75.7001422864503,197.125245060908,32.8747165227329)) ;
#75823 = CARTESIAN_POINT('Ctrl Pts',(78.3842768400396,193.78102322923,17.854339447693)) ;
#75824 = CARTESIAN_POINT('Ctrl Pts',(78.3842768400396,193.78102322923,32.8747165227329)) ;
#75825 = CARTESIAN_POINT('Ctrl Pts',(81.5507230003364,190.489539758744,17.854339447693)) ;
#75826 = CARTESIAN_POINT('Ctrl Pts',(81.5507230003364,190.489539758744,32.8747165227329)) ;
#75827 = CARTESIAN_POINT('',(73.7436956568153,200.410454788892,23.4913203435596)) ;
#75828 = CARTESIAN_POINT('',(73.7436956568153,200.410454788892,23.4913203435596)) ;
#75829 = CARTESIAN_POINT('Ctrl Pts',(81.0682510948939,190.995574215667,23.4913203435596)) ;
#75830 = CARTESIAN_POINT('Ctrl Pts',(78.3304755598256,193.893133563934,23.4913203435596)) ;
#75831 = CARTESIAN_POINT('Ctrl Pts',(75.7953376765802,196.999191831293,23.4913203435596)) ;
#75832 = CARTESIAN_POINT('Ctrl Pts',(73.7436956568154,200.410454788892,23.4913203435596)) ;
#75833 = CARTESIAN_POINT('Origin',(69.6705101448823,217.61928420644,30.3713203435596)) ;
#75834 = CARTESIAN_POINT('',(60.7116108526749,219.655485092203,30.3713203435596)) ;
#75835 = CARTESIAN_POINT('',(60.7116108526749,220.636977801421,30.3713203435596)) ;
#75836 = CARTESIAN_POINT('',(60.7116108526749,219.132346607579,30.3713203435596)) ;
#75837 = CARTESIAN_POINT('',(60.7297059832955,219.541923491104,30.3713203435596)) ;
#75838 = CARTESIAN_POINT('Origin',(64.1568347953872,220.146231446812,30.3713203435596)) ;
#75839 = CARTESIAN_POINT('',(60.7116108526749,219.512965228765,30.3713203435596)) ;
#75840 = CARTESIAN_POINT('',(61.5409585020332,220.840198908612,30.3713203435596)) ;
#75841 = CARTESIAN_POINT('',(60.7116108526749,216.156773929576,30.3713203435596)) ;
#75842 = CARTESIAN_POINT('',(60.7116108526749,218.583329440748,30.3713203435596)) ;
#75843 = CARTESIAN_POINT('',(60.882803220617,214.421530538057,30.3713203435596)) ;
#75844 = CARTESIAN_POINT('Origin',(69.59874093474,216.157477355757,30.3713203435596)) ;
#75845 = CARTESIAN_POINT('',(60.9230784080337,214.221542284825,30.3713203435596)) ;
#75846 = CARTESIAN_POINT('Origin',(144.68997749936,269.113837772005,30.3713203435596)) ;
#75847 = CARTESIAN_POINT('',(61.2615982170421,212.685341204894,30.3713203435596)) ;
#75848 = CARTESIAN_POINT('Origin',(181.381319461017,301.79529262085,30.3713203435596)) ;
#75849 = CARTESIAN_POINT('',(65.371678614805,202.116206289766,30.3713203435596)) ;
#75850 = CARTESIAN_POINT('Origin',(136.119542118133,279.889814321862,30.3713203435596)) ;
#75851 = CARTESIAN_POINT('',(66.2956301826426,200.621620147878,30.3713203435596)) ;
#75852 = CARTESIAN_POINT('Origin',(94.003679466687,218.783592840218,30.3713203435596)) ;
#75853 = CARTESIAN_POINT('',(77.1942359127804,189.615407485539,30.3713203435596)) ;
#75854 = CARTESIAN_POINT('Ctrl Pts',(77.1942359127805,189.615407485539,30.3713203435596)) ;
#75855 = CARTESIAN_POINT('Ctrl Pts',(74.7931595483741,191.357615194406,30.3713203435596)) ;
#75856 = CARTESIAN_POINT('Ctrl Pts',(70.8082383262559,194.719115063076,30.3713203435596)) ;
#75857 = CARTESIAN_POINT('Ctrl Pts',(67.5153419459542,198.760824785205,30.3713203435596)) ;
#75858 = CARTESIAN_POINT('Ctrl Pts',(66.2956301826426,200.621620147878,30.3713203435596)) ;
#75859 = CARTESIAN_POINT('',(77.8285014478222,189.409539758744,30.3713203435596)) ;
#75860 = CARTESIAN_POINT('Origin',(77.7459982214618,190.235352500614,30.3713203435596)) ;
#75861 = CARTESIAN_POINT('',(83.2194473860052,189.409539758744,30.3713203435596)) ;
#75862 = CARTESIAN_POINT('',(73.5558661461117,189.409539758744,30.3713203435596)) ;
#75863 = CARTESIAN_POINT('',(83.4878143389934,190.058573545737,30.3713203435596)) ;
#75864 = CARTESIAN_POINT('Ctrl Pts',(83.4878143389935,190.058573545737,30.3713203435596)) ;
#75865 = CARTESIAN_POINT('Ctrl Pts',(83.5482147548369,189.998322839904,30.3713203435596)) ;
#75866 = CARTESIAN_POINT('Ctrl Pts',(83.6266011938506,189.835494820776,30.3713203435596)) ;
#75867 = CARTESIAN_POINT('Ctrl Pts',(83.576428513561,189.615885650627,30.3713203435596)) ;
#75868 = CARTESIAN_POINT('Ctrl Pts',(83.4319195690048,189.454561122737,30.3713203435596)) ;
#75869 = CARTESIAN_POINT('Ctrl Pts',(83.3047606779792,189.409539758744,30.3713203435596)) ;
#75870 = CARTESIAN_POINT('Ctrl Pts',(83.2194473860052,189.409539758744,30.3713203435596)) ;
#75871 = CARTESIAN_POINT('',(74.0713631125318,201.997275065426,30.3713203435596)) ;
#75872 = CARTESIAN_POINT('Ctrl Pts',(74.071363112532,201.997275065426,30.3713203435596)) ;
#75873 = CARTESIAN_POINT('Ctrl Pts',(75.4893853751038,199.461004730524,30.3713203435596)) ;
#75874 = CARTESIAN_POINT('Ctrl Pts',(78.4869236645555,195.326452202177,30.3713203435596)) ;
#75875 = CARTESIAN_POINT('Ctrl Pts',(81.9448902074828,191.59767334615,30.3713203435596)) ;
#75876 = CARTESIAN_POINT('Ctrl Pts',(83.4878143389934,190.058573545737,30.3713203435596)) ;
#75877 = CARTESIAN_POINT('',(70.3587497899394,213.244508470505,30.3713203435596)) ;
#75878 = CARTESIAN_POINT('Ctrl Pts',(70.3587497899395,213.244508470505,30.3713203435596)) ;
#75879 = CARTESIAN_POINT('Ctrl Pts',(70.6230150970638,210.988834878587,30.3713203435596)) ;
#75880 = CARTESIAN_POINT('Ctrl Pts',(71.5450141265831,207.094613224745,30.3713203435596)) ;
#75881 = CARTESIAN_POINT('Ctrl Pts',(73.2401341423739,203.484008690256,30.3713203435596)) ;
#75882 = CARTESIAN_POINT('Ctrl Pts',(74.0713631125318,201.997275065426,30.3713203435596)) ;
#75883 = CARTESIAN_POINT('',(70.1614015403524,216.000591762293,30.3713203435596)) ;
#75884 = CARTESIAN_POINT('Origin',(97.4802149293723,222.398003042729,30.3713203435596)) ;
#75885 = CARTESIAN_POINT('',(70.1824009080094,218.33629382542,30.3713203435596)) ;
#75886 = CARTESIAN_POINT('Origin',(99.3986297237061,223.018122277912,30.3713203435596)) ;
#75887 = CARTESIAN_POINT('',(70.2600011794933,219.566058197824,30.3713203435596)) ;
#75888 = CARTESIAN_POINT('Origin',(103.749334371737,216.83549248614,30.3713203435596)) ;
#75889 = CARTESIAN_POINT('',(64.9314996085946,223.538913929329,30.3713203435596)) ;
#75890 = CARTESIAN_POINT('',(70.5636770849813,219.33964171939,30.3713203435596)) ;
#75891 = CARTESIAN_POINT('Origin',(64.1568347953872,220.146231446812,30.3713203435596)) ;
#75892 = CARTESIAN_POINT('',(66.8340607823661,201.93583548982,30.3713203435596)) ;
#75893 = CARTESIAN_POINT('',(72.3111547045756,201.93583548982,30.3713203435596)) ;
#75894 = CARTESIAN_POINT('',(71.2393508060962,201.93583548982,30.3713203435596)) ;
#75895 = CARTESIAN_POINT('',(66.4746484362165,202.138527493107,30.3713203435596)) ;
#75896 = CARTESIAN_POINT('Origin',(66.7842973113484,202.267595176532,30.3713203435596)) ;
#75897 = CARTESIAN_POINT('',(62.39752314559,212.090513424339,30.3713203435596)) ;
#75898 = CARTESIAN_POINT('Origin',(123.304723958797,266.258739720462,30.3713203435596)) ;
#75899 = CARTESIAN_POINT('',(62.8448887910812,212.613106134355,30.3713203435596)) ;
#75900 = CARTESIAN_POINT('Ctrl Pts',(62.8448887910812,212.613106134355,30.3713203435596)) ;
#75901 = CARTESIAN_POINT('Ctrl Pts',(62.7302820487196,212.624233777445,30.3713203435596)) ;
#75902 = CARTESIAN_POINT('Ctrl Pts',(62.5327477139549,212.559161211515,30.3713203435596)) ;
#75903 = CARTESIAN_POINT('Ctrl Pts',(62.3821824103364,212.323740151324,30.3713203435596)) ;
#75904 = CARTESIAN_POINT('Ctrl Pts',(62.3784128818005,212.164860433323,30.3713203435596)) ;
#75905 = CARTESIAN_POINT('Ctrl Pts',(62.39752314559,212.090513424339,30.3713203435596)) ;
#75906 = CARTESIAN_POINT('',(69.2431719411391,211.991870334298,30.3713203435596)) ;
#75907 = CARTESIAN_POINT('',(65.7730634668025,212.328797532388,30.3713203435596)) ;
#75908 = CARTESIAN_POINT('',(69.6168298215689,211.643116744604,30.3713203435596)) ;
#75909 = CARTESIAN_POINT('Ctrl Pts',(69.6168298215689,211.643116744604,30.3713203435596)) ;
#75910 = CARTESIAN_POINT('Ctrl Pts',(69.6038817585733,211.72053657915,30.3713203435596)) ;
#75911 = CARTESIAN_POINT('Ctrl Pts',(69.5217274044295,211.89264098624,30.3713203435596)) ;
#75912 = CARTESIAN_POINT('Ctrl Pts',(69.3473422258095,211.981756010092,30.3713203435596)) ;
#75913 = CARTESIAN_POINT('Ctrl Pts',(69.2431719411391,211.991870334298,30.3713203435596)) ;
#75914 = CARTESIAN_POINT('',(72.6841279270487,202.548944203549,30.3713203435596)) ;
#75915 = CARTESIAN_POINT('Origin',(95.7743907326708,211.507553737734,30.3713203435596)) ;
#75916 = CARTESIAN_POINT('Ctrl Pts',(72.3111547045756,201.93583548982,30.3713203435596)) ;
#75917 = CARTESIAN_POINT('Ctrl Pts',(72.434062830227,201.93583548982,30.3713203435596)) ;
#75918 = CARTESIAN_POINT('Ctrl Pts',(72.6367193429415,202.032109677482,30.3713203435596)) ;
#75919 = CARTESIAN_POINT('Ctrl Pts',(72.7529836107094,202.308661221514,30.3713203435596)) ;
#75920 = CARTESIAN_POINT('Ctrl Pts',(72.7218019430032,202.476180013561,30.3713203435596)) ;
#75921 = CARTESIAN_POINT('Ctrl Pts',(72.6841279270486,202.548944203549,30.3713203435596)) ;
#75922 = CARTESIAN_POINT('',(69.2883239479992,219.455458322081,30.3713203435596)) ;
#75923 = CARTESIAN_POINT('',(69.3183833051634,219.827104833273,30.3713203435596)) ;
#75924 = CARTESIAN_POINT('Ctrl Pts',(69.2883239479992,219.455458322081,30.3713203435596)) ;
#75925 = CARTESIAN_POINT('Ctrl Pts',(69.2948338469246,219.541101232703,30.3713203435596)) ;
#75926 = CARTESIAN_POINT('Ctrl Pts',(69.3016608747709,219.626720035554,30.3713203435596)) ;
#75927 = CARTESIAN_POINT('Ctrl Pts',(69.3119969022076,219.750576599373,30.3713203435596)) ;
#75928 = CARTESIAN_POINT('Ctrl Pts',(69.3151901036855,219.788840716323,30.3713203435596)) ;
#75929 = CARTESIAN_POINT('Ctrl Pts',(69.3183833051634,219.827104833273,30.3713203435596)) ;
#75930 = CARTESIAN_POINT('',(69.2071742804062,215.793615651063,30.3713203435596)) ;
#75931 = CARTESIAN_POINT('Origin',(98.9242731431935,222.80312748053,30.3713203435596)) ;
#75932 = CARTESIAN_POINT('',(69.360748483532,213.535508647726,30.3713203435596)) ;
#75933 = CARTESIAN_POINT('Origin',(97.2384671995787,222.414143143253,30.3713203435596)) ;
#75934 = CARTESIAN_POINT('',(69.0988421032155,213.27180916519,30.3713203435596)) ;
#75935 = CARTESIAN_POINT('Ctrl Pts',(69.0988421032155,213.27180916519,30.3713203435596)) ;
#75936 = CARTESIAN_POINT('Ctrl Pts',(69.1391356985346,213.267896893205,30.3713203435596)) ;
#75937 = CARTESIAN_POINT('Ctrl Pts',(69.2113031834343,213.279382916547,30.3713203435596)) ;
#75938 = CARTESIAN_POINT('Ctrl Pts',(69.3050219266113,213.343266910648,30.3713203435596)) ;
#75939 = CARTESIAN_POINT('Ctrl Pts',(69.3577597203562,213.433390646791,30.3713203435596)) ;
#75940 = CARTESIAN_POINT('Ctrl Pts',(69.3638888089739,213.505309174469,30.3713203435596)) ;
#75941 = CARTESIAN_POINT('Ctrl Pts',(69.360748483532,213.535508647726,30.3713203435596)) ;
#75942 = CARTESIAN_POINT('',(62.1323260763097,213.948217047756,30.3713203435596)) ;
#75943 = CARTESIAN_POINT('',(69.2461649893318,213.257504976258,30.3713203435596)) ;
#75944 = CARTESIAN_POINT('',(61.9206232262128,214.13786269141,30.3713203435596)) ;
#75945 = CARTESIAN_POINT('Ctrl Pts',(61.9206232262128,214.13786269141,30.3713203435596)) ;
#75946 = CARTESIAN_POINT('Ctrl Pts',(61.932507773129,214.081157854061,30.3713203435596)) ;
#75947 = CARTESIAN_POINT('Ctrl Pts',(61.9908074934658,213.990274993108,30.3713203435596)) ;
#75948 = CARTESIAN_POINT('Ctrl Pts',(62.0890768060814,213.952416298455,30.3713203435596)) ;
#75949 = CARTESIAN_POINT('Ctrl Pts',(62.1323260763097,213.948217047756,30.3713203435596)) ;
#75950 = CARTESIAN_POINT('',(61.8527608796043,214.467362912516,30.3713203435596)) ;
#75951 = CARTESIAN_POINT('Origin',(157.009443961964,279.366832786929,30.3713203435596)) ;
#75952 = CARTESIAN_POINT('',(61.6716108526749,216.276053366666,30.3713203435596)) ;
#75953 = CARTESIAN_POINT('Origin',(70.7991555701787,216.276809010494,30.3713203435596)) ;
#75954 = CARTESIAN_POINT('',(61.6716108526749,217.7102384348,30.3713203435596)) ;
#75955 = CARTESIAN_POINT('',(61.6716108526749,216.520093569003,30.3713203435596)) ;
#75956 = CARTESIAN_POINT('',(67.635124836556,220.037151707603,30.3713203435596)) ;
#75957 = CARTESIAN_POINT('Origin',(64.1568347953872,220.146231446812,30.3713203435596)) ;
#75958 = CARTESIAN_POINT('',(68.8498979833486,219.885565182264,30.3713203435596)) ;
#75959 = CARTESIAN_POINT('',(66.2768347953872,220.146231446812,30.3713203435596)) ;
#75960 = CARTESIAN_POINT('Origin',(64.1568347953872,220.146231446812,30.3713203435596)) ;
#75961 = CARTESIAN_POINT('Origin',(71.2393508060962,201.93583548982,30.2513203435596)) ;
#75962 = CARTESIAN_POINT('',(72.3111547045756,202.05583548982,30.2513203435596)) ;
#75963 = CARTESIAN_POINT('Origin',(72.3111547045756,201.93583548982,30.2513203435596)) ;
#75964 = CARTESIAN_POINT('',(66.8340607823661,202.05583548982,30.2513203435596)) ;
#75965 = CARTESIAN_POINT('',(71.2393508060962,202.05583548982,30.2513203435596)) ;
#75966 = CARTESIAN_POINT('Origin',(66.8340607823661,201.93583548982,30.2513203435596)) ;
#75967 = CARTESIAN_POINT('Ctrl Pts',(66.4742123255349,202.139220627159,30.3713203424983)) ;
#75968 = CARTESIAN_POINT('Ctrl Pts',(66.5486309050821,202.015550475992,30.3713203424983)) ;
#75969 = CARTESIAN_POINT('Ctrl Pts',(66.6905454482115,201.935517212387,30.3713203424982)) ;
#75970 = CARTESIAN_POINT('Ctrl Pts',(66.8348795711143,201.935820918413,30.3713203424982)) ;
#75971 = CARTESIAN_POINT('Ctrl Pts',(66.5049776890707,202.157739831051,30.3713252816721)) ;
#75972 = CARTESIAN_POINT('Ctrl Pts',(66.5730057722082,202.044688964891,30.3713252816721)) ;
#75973 = CARTESIAN_POINT('Ctrl Pts',(66.7028689699091,201.97145210484,30.371325281672)) ;
#75974 = CARTESIAN_POINT('Ctrl Pts',(66.8348092639751,201.97173001981,30.371325281672)) ;
#75975 = CARTESIAN_POINT('Ctrl Pts',(66.5582167817037,202.189788148438,30.3411670675354)) ;
#75976 = CARTESIAN_POINT('Ctrl Pts',(66.6152695314146,202.094976983773,30.3411670675354)) ;
#75977 = CARTESIAN_POINT('Ctrl Pts',(66.7240353556309,202.033638070306,30.3411670675354)) ;
#75978 = CARTESIAN_POINT('Ctrl Pts',(66.834688502964,202.033870836095,30.3411670675354)) ;
#75979 = CARTESIAN_POINT('Ctrl Pts',(66.5770357137958,202.201116109631,30.2782482805904)) ;
#75980 = CARTESIAN_POINT('Ctrl Pts',(66.6301722813347,202.112812443701,30.2782482805904)) ;
#75981 = CARTESIAN_POINT('Ctrl Pts',(66.7315872550755,202.055619071211,30.2782482805904)) ;
#75982 = CARTESIAN_POINT('Ctrl Pts',(66.8346454188596,202.055836105354,30.2782482805904)) ;
#75983 = CARTESIAN_POINT('Ctrl Pts',(66.5770356146924,202.201116272943,30.2513203435596)) ;
#75984 = CARTESIAN_POINT('Ctrl Pts',(66.6301897811885,202.112783710585,30.2513203435596)) ;
#75985 = CARTESIAN_POINT('Ctrl Pts',(66.7315536124682,202.055619180086,30.2513203435596)) ;
#75986 = CARTESIAN_POINT('Ctrl Pts',(66.8346456098891,202.055836105045,30.2513203435596)) ;
#75987 = CARTESIAN_POINT('',(66.5773388238817,202.200616184912,30.2513203435596)) ;
#75988 = CARTESIAN_POINT('Origin',(66.7985154459214,202.29280669461,30.2513203435596)) ;
#75989 = CARTESIAN_POINT('Origin',(66.4746484362165,202.138527493107,30.2513203435596)) ;
#75990 = CARTESIAN_POINT('Ctrl Pts',(66.5773376779735,202.200615492168,30.2513203435596)) ;
#75991 = CARTESIAN_POINT('Ctrl Pts',(64.7228248908566,205.267850945375,30.2513203435596)) ;
#75992 = CARTESIAN_POINT('Ctrl Pts',(63.4070162709899,208.645184776903,30.2513203435596)) ;
#75993 = CARTESIAN_POINT('Ctrl Pts',(62.513745139331,212.120387295379,30.2513203435596)) ;
#75994 = CARTESIAN_POINT('Ctrl Pts',(66.5773376779735,202.200615492168,30.2872242596007)) ;
#75995 = CARTESIAN_POINT('Ctrl Pts',(64.7228470996252,205.267814213613,30.2872242596007)) ;
#75996 = CARTESIAN_POINT('Ctrl Pts',(63.407008670507,208.645214345997,30.2872242596007)) ;
#75997 = CARTESIAN_POINT('Ctrl Pts',(62.513745139331,212.120387295379,30.2872242596007)) ;
#75998 = CARTESIAN_POINT('Ctrl Pts',(66.5515297315697,202.185011484147,30.3493567394431)) ;
#75999 = CARTESIAN_POINT('Ctrl Pts',(64.6952653289755,205.255143987797,30.3493567394431)) ;
#76000 = CARTESIAN_POINT('Ctrl Pts',(63.3784067154828,208.635344722984,30.3493567394431)) ;
#76001 = CARTESIAN_POINT('Ctrl Pts',(62.4845361303434,212.112879369042,30.3493567394431)) ;
#76002 = CARTESIAN_POINT('Ctrl Pts',(66.4976918481812,202.152460007516,30.3713203435596)) ;
#76003 = CARTESIAN_POINT('Ctrl Pts',(64.6377860153758,205.228615184033,30.3713203435596)) ;
#76004 = CARTESIAN_POINT('Ctrl Pts',(63.3187200878819,208.614834203502,30.3713203435596)) ;
#76005 = CARTESIAN_POINT('Ctrl Pts',(62.4236032999988,212.097217105324,30.3713203435596)) ;
#76006 = CARTESIAN_POINT('Ctrl Pts',(66.4746484362164,202.138527493107,30.3713203435596)) ;
#76007 = CARTESIAN_POINT('Ctrl Pts',(64.6131863812338,205.217256553109,30.3713203435596)) ;
#76008 = CARTESIAN_POINT('Ctrl Pts',(63.2931725177147,208.606058544556,30.3713203435596)) ;
#76009 = CARTESIAN_POINT('Ctrl Pts',(62.39752314559,212.090513424339,30.3713203435596)) ;
#76010 = CARTESIAN_POINT('',(62.5137204444978,212.120380950715,30.2513203435596)) ;
#76011 = CARTESIAN_POINT('Origin',(62.39752314559,212.090513424339,30.2513203435596)) ;
#76012 = CARTESIAN_POINT('Ctrl Pts',(66.5773422616064,202.200618263143,30.2513203435596)) ;
#76013 = CARTESIAN_POINT('Ctrl Pts',(64.7467490262501,205.228710003766,30.2513203435596)) ;
#76014 = CARTESIAN_POINT('Ctrl Pts',(63.430846523082,208.550723522602,30.2513203435596)) ;
#76015 = CARTESIAN_POINT('Ctrl Pts',(62.5137204444978,212.120380950715,30.2513203435596)) ;
#76016 = CARTESIAN_POINT('Ctrl Pts',(62.8448887910812,212.613106134355,30.3713203435596)) ;
#76017 = CARTESIAN_POINT('Ctrl Pts',(62.7302820487196,212.624233777445,30.3713203435596)) ;
#76018 = CARTESIAN_POINT('Ctrl Pts',(62.5327477139549,212.559161211515,30.3713203435596)) ;
#76019 = CARTESIAN_POINT('Ctrl Pts',(62.3821824103364,212.323740151324,30.3713203435596)) ;
#76020 = CARTESIAN_POINT('Ctrl Pts',(62.3784128818005,212.164860433323,30.3713203435596)) ;
#76021 = CARTESIAN_POINT('Ctrl Pts',(62.39752314559,212.090513424339,30.3713203435596)) ;
#76022 = CARTESIAN_POINT('Ctrl Pts',(62.8414190479705,212.57737026904,30.3713203435596)) ;
#76023 = CARTESIAN_POINT('Ctrl Pts',(62.736651971145,212.587542538266,30.3713203435596)) ;
#76024 = CARTESIAN_POINT('Ctrl Pts',(62.5559796234245,212.527942988847,30.3713203435596)) ;
#76025 = CARTESIAN_POINT('Ctrl Pts',(62.4183338664848,212.312725587393,30.3713203435596)) ;
#76026 = CARTESIAN_POINT('Ctrl Pts',(62.4148271499965,212.167415544927,30.3713203435596)) ;
#76027 = CARTESIAN_POINT('Ctrl Pts',(62.4322966848017,212.099451665653,30.3713203435596)) ;
#76028 = CARTESIAN_POINT('Ctrl Pts',(62.8354145860493,212.515528618039,30.3411618315345)) ;
#76029 = CARTESIAN_POINT('Ctrl Pts',(62.7475491580212,212.524059836211,30.3411618315345)) ;
#76030 = CARTESIAN_POINT('Ctrl Pts',(62.5961291195913,212.47419804225,30.3411618315345)) ;
#76031 = CARTESIAN_POINT('Ctrl Pts',(62.480697149514,212.293710101782,30.3411618315345)) ;
#76032 = CARTESIAN_POINT('Ctrl Pts',(62.4778217652515,212.171919017848,30.3411618315345)) ;
#76033 = CARTESIAN_POINT('Ctrl Pts',(62.4924730106581,212.114919476352,30.3411618315345)) ;
#76034 = CARTESIAN_POINT('Ctrl Pts',(62.8332920289675,212.493667802533,30.2782482805904)) ;
#76035 = CARTESIAN_POINT('Ctrl Pts',(62.7514566832816,212.501613535045,30.2782482805904)) ;
#76036 = CARTESIAN_POINT('Ctrl Pts',(62.6103454719125,212.455076865844,30.2782482805904)) ;
#76037 = CARTESIAN_POINT('Ctrl Pts',(62.5028291668008,212.286968223387,30.2782482805904)) ;
#76038 = CARTESIAN_POINT('Ctrl Pts',(62.5000993885563,212.173475037474,30.2782482805904)) ;
#76039 = CARTESIAN_POINT('Ctrl Pts',(62.513745139331,212.120387295379,30.2782482805904)) ;
#76040 = CARTESIAN_POINT('Ctrl Pts',(62.8332920289675,212.493667802533,30.2513203435596)) ;
#76041 = CARTESIAN_POINT('Ctrl Pts',(62.7514300701379,212.501616119025,30.2513203435596)) ;
#76042 = CARTESIAN_POINT('Ctrl Pts',(62.6103341167345,212.45513571479,30.2513203435596)) ;
#76043 = CARTESIAN_POINT('Ctrl Pts',(62.5027874712927,212.286977814653,30.2513203435596)) ;
#76044 = CARTESIAN_POINT('Ctrl Pts',(62.5000949509099,212.173492301795,30.2513203435596)) ;
#76045 = CARTESIAN_POINT('Ctrl Pts',(62.513745139331,212.120387295379,30.2513203435596)) ;
#76046 = CARTESIAN_POINT('',(62.8332920289675,212.493667802533,30.2513203435596)) ;
#76047 = CARTESIAN_POINT('Ctrl Pts',(62.513745139331,212.120387295379,30.2513203435596)) ;
#76048 = CARTESIAN_POINT('Ctrl Pts',(62.5000949509099,212.173492301795,30.2513203435596)) ;
#76049 = CARTESIAN_POINT('Ctrl Pts',(62.5027874712927,212.286977814653,30.2513203435596)) ;
#76050 = CARTESIAN_POINT('Ctrl Pts',(62.6103341167345,212.45513571479,30.2513203435596)) ;
#76051 = CARTESIAN_POINT('Ctrl Pts',(62.7514300701379,212.501616119025,30.2513203435596)) ;
#76052 = CARTESIAN_POINT('Ctrl Pts',(62.8332920289675,212.493667802533,30.2513203435596)) ;
#76053 = CARTESIAN_POINT('Origin',(62.8448887910812,212.613106134355,30.2513203435596)) ;
#76054 = CARTESIAN_POINT('Origin',(65.7730634668025,212.328797532388,30.2513203435596)) ;
#76055 = CARTESIAN_POINT('',(69.2315751790255,211.872432002476,30.2513203435596)) ;
#76056 = CARTESIAN_POINT('Origin',(69.2431719411391,211.991870334298,30.2513203435596)) ;
#76057 = CARTESIAN_POINT('',(65.7614667046888,212.209359200566,30.2513203435596)) ;
#76058 = CARTESIAN_POINT('Ctrl Pts',(69.6168298215689,211.643116744604,30.3713203435596)) ;
#76059 = CARTESIAN_POINT('Ctrl Pts',(69.6038817585733,211.72053657915,30.3713203435596)) ;
#76060 = CARTESIAN_POINT('Ctrl Pts',(69.5217274044295,211.89264098624,30.3713203435596)) ;
#76061 = CARTESIAN_POINT('Ctrl Pts',(69.3473422258095,211.981756010092,30.3713203435596)) ;
#76062 = CARTESIAN_POINT('Ctrl Pts',(69.2431719411391,211.991870334298,30.3713203435596)) ;
#76063 = CARTESIAN_POINT('Ctrl Pts',(69.5814177423463,211.637194259297,30.3713203435596)) ;
#76064 = CARTESIAN_POINT('Ctrl Pts',(69.5695813470117,211.707967143915,30.3713203435596)) ;
#76065 = CARTESIAN_POINT('Ctrl Pts',(69.4944320015214,211.865340586305,30.3713203435596)) ;
#76066 = CARTESIAN_POINT('Ctrl Pts',(69.3349288486785,211.946888519231,30.3713203435596)) ;
#76067 = CARTESIAN_POINT('Ctrl Pts',(69.2397021980285,211.956134468983,30.3713203435596)) ;
#76068 = CARTESIAN_POINT('Ctrl Pts',(69.5201364960134,211.626945290895,30.3411617587246)) ;
#76069 = CARTESIAN_POINT('Ctrl Pts',(69.5102096184685,211.686300672263,30.3411617587246)) ;
#76070 = CARTESIAN_POINT('Ctrl Pts',(69.4472360221651,211.818236948212,30.3411617587246)) ;
#76071 = CARTESIAN_POINT('Ctrl Pts',(69.3135618647732,211.886538566864,30.3411617587246)) ;
#76072 = CARTESIAN_POINT('Ctrl Pts',(69.2336977445498,211.894292904935,30.3411617587246)) ;
#76073 = CARTESIAN_POINT('Ctrl Pts',(69.4984736650468,211.623322295552,30.2782482805904)) ;
#76074 = CARTESIAN_POINT('Ctrl Pts',(69.4892280553263,211.678604199499,30.2782482805904)) ;
#76075 = CARTESIAN_POINT('Ctrl Pts',(69.4305350897576,211.801524301052,30.2782482805904)) ;
#76076 = CARTESIAN_POINT('Ctrl Pts',(69.3059583355531,211.865209833861,30.2782482805904)) ;
#76077 = CARTESIAN_POINT('Ctrl Pts',(69.2315751790255,211.872432002476,30.2782482805904)) ;
#76078 = CARTESIAN_POINT('Ctrl Pts',(69.4984736650468,211.623322295552,30.2513203435596)) ;
#76079 = CARTESIAN_POINT('Ctrl Pts',(69.4892250486213,211.67862217737,30.2513203435596)) ;
#76080 = CARTESIAN_POINT('Ctrl Pts',(69.43054336709,211.80155389672,30.2513203435596)) ;
#76081 = CARTESIAN_POINT('Ctrl Pts',(69.3059825252186,211.865207485186,30.2513203435596)) ;
#76082 = CARTESIAN_POINT('Ctrl Pts',(69.2315751790255,211.872432002476,30.2513203435596)) ;
#76083 = CARTESIAN_POINT('',(69.4984736650468,211.623322295552,30.2513203435596)) ;
#76084 = CARTESIAN_POINT('Ctrl Pts',(69.2315751790255,211.872432002476,30.2513203435596)) ;
#76085 = CARTESIAN_POINT('Ctrl Pts',(69.3059825252186,211.865207485186,30.2513203435596)) ;
#76086 = CARTESIAN_POINT('Ctrl Pts',(69.43054336709,211.80155389672,30.2513203435596)) ;
#76087 = CARTESIAN_POINT('Ctrl Pts',(69.4892250486213,211.67862217737,30.2513203435596)) ;
#76088 = CARTESIAN_POINT('Ctrl Pts',(69.4984736650468,211.623322295552,30.2513203435596)) ;
#76089 = CARTESIAN_POINT('Origin',(69.6168298215689,211.643116744604,30.2513203435596)) ;
#76090 = CARTESIAN_POINT('Ctrl Pts',(69.4984736650468,211.623322295552,30.2513203435596)) ;
#76091 = CARTESIAN_POINT('Ctrl Pts',(70.0304244797463,208.442650091984,30.2513203435596)) ;
#76092 = CARTESIAN_POINT('Ctrl Pts',(71.0956312780117,205.355998860028,30.2513203435596)) ;
#76093 = CARTESIAN_POINT('Ctrl Pts',(72.5775641491993,202.49377028534,30.2513203435596)) ;
#76094 = CARTESIAN_POINT('Ctrl Pts',(69.4984736650468,211.623322295552,30.2872242596007)) ;
#76095 = CARTESIAN_POINT('Ctrl Pts',(70.0304311821308,208.442610016684,30.2872242596007)) ;
#76096 = CARTESIAN_POINT('Ctrl Pts',(71.095615141615,205.35603002612,30.2872242596007)) ;
#76097 = CARTESIAN_POINT('Ctrl Pts',(72.5775641491993,202.49377028534,30.2872242596007)) ;
#76098 = CARTESIAN_POINT('Ctrl Pts',(69.5282191152938,211.628297066757,30.3493566400793)) ;
#76099 = CARTESIAN_POINT('Ctrl Pts',(70.059641309941,208.450785619898,30.3493566400793)) ;
#76100 = CARTESIAN_POINT('Ctrl Pts',(71.1236857344122,205.367407169992,30.3493566400794)) ;
#76101 = CARTESIAN_POINT('Ctrl Pts',(72.6043459208053,202.507636678836,30.3493566400794)) ;
#76102 = CARTESIAN_POINT('Ctrl Pts',(69.590270762152,211.638674880624,30.3713203435596)) ;
#76103 = CARTESIAN_POINT('Ctrl Pts',(70.1205940095398,208.467734325105,30.3713203435596)) ;
#76104 = CARTESIAN_POINT('Ctrl Pts',(71.1822006669159,205.391223591054,30.3713203435596)) ;
#76105 = CARTESIAN_POINT('Ctrl Pts',(72.660215071218,202.536563205255,30.3713203435596)) ;
#76106 = CARTESIAN_POINT('Ctrl Pts',(69.616829821569,211.643116744604,30.3713203435596)) ;
#76107 = CARTESIAN_POINT('Ctrl Pts',(70.1466834166504,208.474984362312,30.3713203435596)) ;
#76108 = CARTESIAN_POINT('Ctrl Pts',(71.207244239121,205.401420705868,30.3713203435596)) ;
#76109 = CARTESIAN_POINT('Ctrl Pts',(72.6841279270487,202.548944203549,30.3713203435596)) ;
#76110 = CARTESIAN_POINT('',(72.5775641491992,202.49377028534,30.2513203435596)) ;
#76111 = CARTESIAN_POINT('Origin',(72.6841279270487,202.548944203549,30.2513203435596)) ;
#76112 = CARTESIAN_POINT('Ctrl Pts',(69.4984736650468,211.623322295552,30.2513203435596)) ;
#76113 = CARTESIAN_POINT('Ctrl Pts',(70.0304244797463,208.442650091984,30.2513203435596)) ;
#76114 = CARTESIAN_POINT('Ctrl Pts',(71.0956312780117,205.355998860028,30.2513203435596)) ;
#76115 = CARTESIAN_POINT('Ctrl Pts',(72.5775641491993,202.49377028534,30.2513203435596)) ;
#76116 = CARTESIAN_POINT('Ctrl Pts',(72.3111547045756,201.93583548982,30.3713203435596)) ;
#76117 = CARTESIAN_POINT('Ctrl Pts',(72.434062830227,201.93583548982,30.3713203435596)) ;
#76118 = CARTESIAN_POINT('Ctrl Pts',(72.6367193429415,202.032109677482,30.3713203435596)) ;
#76119 = CARTESIAN_POINT('Ctrl Pts',(72.7529836107094,202.308661221514,30.3713203435596)) ;
#76120 = CARTESIAN_POINT('Ctrl Pts',(72.7218019430032,202.476180013561,30.3713203435596)) ;
#76121 = CARTESIAN_POINT('Ctrl Pts',(72.6841279270486,202.548944203549,30.3713203435596)) ;
#76122 = CARTESIAN_POINT('Ctrl Pts',(72.3111547045756,201.971739405861,30.3713203435596)) ;
#76123 = CARTESIAN_POINT('Ctrl Pts',(72.4235104419194,201.971739405861,30.3713203435596)) ;
#76124 = CARTESIAN_POINT('Ctrl Pts',(72.6088489992096,202.05988145465,30.3713203435596)) ;
#76125 = CARTESIAN_POINT('Ctrl Pts',(72.7151374364996,202.312699539834,30.3713203435596)) ;
#76126 = CARTESIAN_POINT('Ctrl Pts',(72.6866835985101,202.465919251188,30.3713203435596)) ;
#76127 = CARTESIAN_POINT('Ctrl Pts',(72.6522441192743,202.532436205824,30.3713203435596)) ;
#76128 = CARTESIAN_POINT('Ctrl Pts',(72.3111547045756,202.033871875492,30.3411618343582)) ;
#76129 = CARTESIAN_POINT('Ctrl Pts',(72.4053845452112,202.033871875492,30.3411618343582)) ;
#76130 = CARTESIAN_POINT('Ctrl Pts',(72.5607354838846,202.107650247836,30.3411618343582)) ;
#76131 = CARTESIAN_POINT('Ctrl Pts',(72.6498702107552,202.319671293231,30.3411618343582)) ;
#76132 = CARTESIAN_POINT('Ctrl Pts',(72.6259520275162,202.448082730821,30.3411618343582)) ;
#76133 = CARTESIAN_POINT('Ctrl Pts',(72.5970685301829,202.503868774178,30.3411618343582)) ;
#76134 = CARTESIAN_POINT('Ctrl Pts',(72.3111547045756,202.05583548982,30.2782482805904)) ;
#76135 = CARTESIAN_POINT('Ctrl Pts',(72.3989176820674,202.05583548982,30.2782482805904)) ;
#76136 = CARTESIAN_POINT('Ctrl Pts',(72.5436762466237,202.124664150233,30.2782482805904)) ;
#76137 = CARTESIAN_POINT('Ctrl Pts',(72.6266990056788,202.322143095839,30.2782482805904)) ;
#76138 = CARTESIAN_POINT('Ctrl Pts',(72.6044654122095,202.441812760691,30.2782482805904)) ;
#76139 = CARTESIAN_POINT('Ctrl Pts',(72.5775641491992,202.49377028534,30.2782482805904)) ;
#76140 = CARTESIAN_POINT('Ctrl Pts',(72.3111547045756,202.05583548982,30.2513203435596)) ;
#76141 = CARTESIAN_POINT('Ctrl Pts',(72.398946222898,202.05583548982,30.2513203435596)) ;
#76142 = CARTESIAN_POINT('Ctrl Pts',(72.543700874837,202.124602766721,30.2513203435596)) ;
#76143 = CARTESIAN_POINT('Ctrl Pts',(72.6267467803854,202.322139583887,30.2513203435596)) ;
#76144 = CARTESIAN_POINT('Ctrl Pts',(72.6044741605953,202.44179586392,30.2513203435596)) ;
#76145 = CARTESIAN_POINT('Ctrl Pts',(72.5775641491992,202.49377028534,30.2513203435596)) ;
#76146 = CARTESIAN_POINT('Ctrl Pts',(72.5775641491992,202.49377028534,30.2513203435596)) ;
#76147 = CARTESIAN_POINT('Ctrl Pts',(72.6044741605953,202.44179586392,30.2513203435596)) ;
#76148 = CARTESIAN_POINT('Ctrl Pts',(72.6267467803854,202.322139583887,30.2513203435596)) ;
#76149 = CARTESIAN_POINT('Ctrl Pts',(72.543700874837,202.124602766721,30.2513203435596)) ;
#76150 = CARTESIAN_POINT('Ctrl Pts',(72.398946222898,202.05583548982,30.2513203435596)) ;
#76151 = CARTESIAN_POINT('Ctrl Pts',(72.3111547045756,202.05583548982,30.2513203435596)) ;
#76152 = CARTESIAN_POINT('Ctrl Pts',(62.8332920289675,212.493667802533,30.2513203435596)) ;
#76153 = CARTESIAN_POINT('Ctrl Pts',(62.8332920289675,212.493667802533,22.1393203435596)) ;
#76154 = CARTESIAN_POINT('Ctrl Pts',(62.7787149126794,212.498966920703,30.2513203435596)) ;
#76155 = CARTESIAN_POINT('Ctrl Pts',(62.7787149126794,212.498966920703,22.1393203435596)) ;
#76156 = CARTESIAN_POINT('Ctrl Pts',(62.6669957149089,212.478811797326,30.2513203435596)) ;
#76157 = CARTESIAN_POINT('Ctrl Pts',(62.6669957149089,212.478811797326,22.1393203435596)) ;
#76158 = CARTESIAN_POINT('Ctrl Pts',(62.5174244243077,212.346623344547,30.2513203435596)) ;
#76159 = CARTESIAN_POINT('Ctrl Pts',(62.5174244243077,212.346623344547,22.1393203435596)) ;
#76160 = CARTESIAN_POINT('Ctrl Pts',(62.4932689273543,212.200048420549,30.2513203435596)) ;
#76161 = CARTESIAN_POINT('Ctrl Pts',(62.4932689273543,212.200048420549,22.1393203435596)) ;
#76162 = CARTESIAN_POINT('Ctrl Pts',(62.513745139331,212.120387295379,30.2513203435596)) ;
#76163 = CARTESIAN_POINT('Ctrl Pts',(62.513745139331,212.120387295379,22.1393203435596)) ;
#76164 = CARTESIAN_POINT('',(62.5137204444978,212.120380950715,23.4913203435596)) ;
#76165 = CARTESIAN_POINT('',(62.513745139331,212.120387295379,30.2513203435596)) ;
#76166 = CARTESIAN_POINT('',(62.8332920289675,212.493667802533,23.4913203435596)) ;
#76167 = CARTESIAN_POINT('Ctrl Pts',(62.8332920289675,212.493667802533,23.4913203435596)) ;
#76168 = CARTESIAN_POINT('Ctrl Pts',(62.7787149126794,212.498966920703,23.4913203435596)) ;
#76169 = CARTESIAN_POINT('Ctrl Pts',(62.6669957149089,212.478811797326,23.4913203435596)) ;
#76170 = CARTESIAN_POINT('Ctrl Pts',(62.5174244243077,212.346623344547,23.4913203435596)) ;
#76171 = CARTESIAN_POINT('Ctrl Pts',(62.4932689273543,212.200048420549,23.4913203435596)) ;
#76172 = CARTESIAN_POINT('Ctrl Pts',(62.513745139331,212.120387295379,23.4913203435596)) ;
#76173 = CARTESIAN_POINT('',(62.8332920289675,212.493667802533,23.4913203435596)) ;
#76174 = CARTESIAN_POINT('Ctrl Pts',(66.6653986331397,202.05583548982,17.8547522895864)) ;
#76175 = CARTESIAN_POINT('Ctrl Pts',(66.6653986331397,202.05583548982,32.8746339543542)) ;
#76176 = CARTESIAN_POINT('Ctrl Pts',(64.7175672988148,205.239235006074,17.8547522895864)) ;
#76177 = CARTESIAN_POINT('Ctrl Pts',(64.7175672988148,205.239235006074,32.8746339543542)) ;
#76178 = CARTESIAN_POINT('Ctrl Pts',(63.3441806268929,208.750326110011,17.8547522895864)) ;
#76179 = CARTESIAN_POINT('Ctrl Pts',(63.3441806268929,208.750326110011,32.8746339543542)) ;
#76180 = CARTESIAN_POINT('Ctrl Pts',(62.4092970952969,212.53483522599,17.8547522895864)) ;
#76181 = CARTESIAN_POINT('Ctrl Pts',(62.4092970952969,212.53483522599,32.8746339543542)) ;
#76182 = CARTESIAN_POINT('',(66.5773388238817,202.200616184912,23.4913203435596)) ;
#76183 = CARTESIAN_POINT('',(66.5773376779735,202.200615492168,23.4913203435596)) ;
#76184 = CARTESIAN_POINT('Ctrl Pts',(62.5137204444978,212.120380950715,23.4913203435596)) ;
#76185 = CARTESIAN_POINT('Ctrl Pts',(63.430846523082,208.550723522602,23.4913203435596)) ;
#76186 = CARTESIAN_POINT('Ctrl Pts',(64.7467490262501,205.228710003766,23.4913203435596)) ;
#76187 = CARTESIAN_POINT('Ctrl Pts',(66.5773422616064,202.200618263143,23.4913203435596)) ;
#76188 = CARTESIAN_POINT('Ctrl Pts',(66.5773376779735,202.200615492168,30.2513203435596)) ;
#76189 = CARTESIAN_POINT('Ctrl Pts',(66.5773376779735,202.200615492168,22.1393203435596)) ;
#76190 = CARTESIAN_POINT('Ctrl Pts',(66.6304739575799,202.112731773171,30.2513203435596)) ;
#76191 = CARTESIAN_POINT('Ctrl Pts',(66.6304739575799,202.112731773171,22.1393203435596)) ;
#76192 = CARTESIAN_POINT('Ctrl Pts',(66.7313621344916,202.05583548982,30.2513203435596)) ;
#76193 = CARTESIAN_POINT('Ctrl Pts',(66.7313621344916,202.05583548982,22.1393203435596)) ;
#76194 = CARTESIAN_POINT('Ctrl Pts',(66.8340607823661,202.05583548982,30.2513203435596)) ;
#76195 = CARTESIAN_POINT('Ctrl Pts',(66.8340607823661,202.05583548982,22.1393203435596)) ;
#76196 = CARTESIAN_POINT('',(66.8340607823661,202.05583548982,23.4913203435596)) ;
#76197 = CARTESIAN_POINT('',(66.8340607823661,202.05583548982,30.2513203435596)) ;
#76198 = CARTESIAN_POINT('Origin',(66.7985154459218,202.29280669461,23.4913203435596)) ;
#76199 = CARTESIAN_POINT('Origin',(72.8081914673101,202.05583548982,23.8713203435596)) ;
#76200 = CARTESIAN_POINT('',(72.3111547045756,202.05583548982,23.4913203435596)) ;
#76201 = CARTESIAN_POINT('',(72.3111547045756,202.05583548982,23.4913203435596)) ;
#76202 = CARTESIAN_POINT('',(70.2085194795435,202.05583548982,23.4913203435596)) ;
#76203 = CARTESIAN_POINT('Origin',(64.1568347953872,220.146231446812,30.2513203435596)) ;
#76204 = CARTESIAN_POINT('',(66.1568347953872,220.146231446812,30.2513203435596)) ;
#76205 = CARTESIAN_POINT('Origin',(66.2768347953872,220.146231446812,30.2513203435596)) ;
#76206 = CARTESIAN_POINT('Origin',(64.1568347953872,220.146231446812,30.2513203435596)) ;
#76207 = CARTESIAN_POINT('Origin',(64.1568347953872,220.146231446812,23.8713203435596)) ;
#76208 = CARTESIAN_POINT('',(66.1568347953872,220.146231446812,23.8713203435596)) ;
#76209 = CARTESIAN_POINT('Origin',(64.1568347953872,220.146231446812,23.8713203435596)) ;
#76210 = CARTESIAN_POINT('',(66.1568347953872,220.146231446812,23.8713203435596)) ;
#76211 = CARTESIAN_POINT('Origin',(60.7116108526749,219.132346607579,30.2513203435596)) ;
#76212 = CARTESIAN_POINT('',(60.5916108526749,220.645409008718,30.2513203435596)) ;
#76213 = CARTESIAN_POINT('Origin',(60.711617364105,220.636941531386,30.2513105111323)) ;
#76214 = CARTESIAN_POINT('',(60.5916108526749,219.647053884905,30.2513203435596)) ;
#76215 = CARTESIAN_POINT('',(60.5916108526749,219.132346607579,30.2513203435596)) ;
#76216 = CARTESIAN_POINT('Origin',(60.7116173641052,219.655521362237,30.251310511132)) ;
#76217 = CARTESIAN_POINT('Origin',(64.1568347953872,220.146231446812,30.2513203435596)) ;
#76218 = CARTESIAN_POINT('',(64.9830939940346,223.650128668,30.2513203435596)) ;
#76219 = CARTESIAN_POINT('Ctrl Pts',(64.9314996085946,223.538913929329,30.3713203435596)) ;
#76220 = CARTESIAN_POINT('Ctrl Pts',(64.9317215230365,223.539394529153,30.3713203435596)) ;
#76221 = CARTESIAN_POINT('Ctrl Pts',(64.9319434468761,223.539875119568,30.3713169902839)) ;
#76222 = CARTESIAN_POINT('Ctrl Pts',(64.9321653661535,223.540355670364,30.3713102838073)) ;
#76223 = CARTESIAN_POINT('Ctrl Pts',(64.9390997545165,223.555371607189,30.3711007242144)) ;
#76224 = CARTESIAN_POINT('Ctrl Pts',(64.945967748304,223.570213670412,30.3676189963526)) ;
#76225 = CARTESIAN_POINT('Ctrl Pts',(64.9523490912924,223.583980936494,30.3610416978447)) ;
#76226 = CARTESIAN_POINT('Ctrl Pts',(64.9584600142363,223.59716479173,30.3547431233232)) ;
#76227 = CARTESIAN_POINT('Ctrl Pts',(64.9640174018536,223.609132151157,30.3457154332298)) ;
#76228 = CARTESIAN_POINT('Ctrl Pts',(64.9686896141286,223.619182598841,30.3344093373863)) ;
#76229 = CARTESIAN_POINT('Ctrl Pts',(64.9732616895214,223.629017640966,30.3233455586983)) ;
#76230 = CARTESIAN_POINT('Ctrl Pts',(64.9768987673375,223.636829737302,30.3103090834608)) ;
#76231 = CARTESIAN_POINT('Ctrl Pts',(64.9793767861943,223.6421501932,30.295975639056)) ;
#76232 = CARTESIAN_POINT('Ctrl Pts',(64.9818281519998,223.647413423391,30.2817963621737)) ;
#76233 = CARTESIAN_POINT('Ctrl Pts',(64.9830939940349,223.650128668,30.2666404537853)) ;
#76234 = CARTESIAN_POINT('Ctrl Pts',(64.9830939940347,223.650128668,30.2513203435596)) ;
#76235 = CARTESIAN_POINT('Origin',(64.1568347953872,220.146231446812,30.2513203435596)) ;
#76236 = CARTESIAN_POINT('Origin',(70.5636770849813,219.33964171939,30.2513203435596)) ;
#76237 = CARTESIAN_POINT('',(70.3850625789433,219.622496965577,30.2513203435596)) ;
#76238 = CARTESIAN_POINT('Ctrl Pts',(70.260001179114,219.566058198626,30.3713203435596)) ;
#76239 = CARTESIAN_POINT('Ctrl Pts',(70.2603043870942,219.566201490721,30.3713203435588)) ;
#76240 = CARTESIAN_POINT('Ctrl Pts',(70.2606076475466,219.566344671311,30.3713192475164)) ;
#76241 = CARTESIAN_POINT('Ctrl Pts',(70.2756119803025,219.573422118245,30.3712108698978)) ;
#76242 = CARTESIAN_POINT('Ctrl Pts',(70.2904565326987,219.580094181022,30.3685339483272)) ;
#76243 = CARTESIAN_POINT('Ctrl Pts',(70.3148096110176,219.590914525823,30.3596445675472)) ;
#76244 = CARTESIAN_POINT('Ctrl Pts',(70.3303650868265,219.597736373691,30.3526122298557)) ;
#76245 = CARTESIAN_POINT('Ctrl Pts',(70.3569751848126,219.610042404231,30.3283757793828)) ;
#76246 = CARTESIAN_POINT('Ctrl Pts',(70.366511706138,219.614483226237,30.3157125984337)) ;
#76247 = CARTESIAN_POINT('Ctrl Pts',(70.3771460617663,219.619205734236,30.2935959336947)) ;
#76248 = CARTESIAN_POINT('Ctrl Pts',(70.3800723202718,219.620457756702,30.2854122779805)) ;
#76249 = CARTESIAN_POINT('Ctrl Pts',(70.3840287602576,219.622101846434,30.2685540701959)) ;
#76250 = CARTESIAN_POINT('Ctrl Pts',(70.3850625789433,219.622496965577,30.2599631560588)) ;
#76251 = CARTESIAN_POINT('Ctrl Pts',(70.3850625789433,219.622496965577,30.2513203435596)) ;
#76252 = CARTESIAN_POINT('',(70.6354050204722,219.435845166679,30.2513203435596)) ;
#76253 = CARTESIAN_POINT('Ctrl Pts',(70.3022814706893,218.330941191344,30.2513203435596)) ;
#76254 = CARTESIAN_POINT('Ctrl Pts',(70.3215247358121,218.761924034176,30.2513203435596)) ;
#76255 = CARTESIAN_POINT('Ctrl Pts',(70.3491825816751,219.192547142136,30.2513203435596)) ;
#76256 = CARTESIAN_POINT('Ctrl Pts',(70.3850625789433,219.622496965577,30.2513203435596)) ;
#76257 = CARTESIAN_POINT('Ctrl Pts',(70.3022814706893,218.330941191344,30.2872242596007)) ;
#76258 = CARTESIAN_POINT('Ctrl Pts',(70.3215245131287,218.761919046833,30.2872242596007)) ;
#76259 = CARTESIAN_POINT('Ctrl Pts',(70.3491829883129,219.192552014874,30.2872242596007)) ;
#76260 = CARTESIAN_POINT('Ctrl Pts',(70.3850625789433,219.622496965577,30.2872242596007)) ;
#76261 = CARTESIAN_POINT('Ctrl Pts',(70.2721528021911,218.332286428087,30.3493565173742)) ;
#76262 = CARTESIAN_POINT('Ctrl Pts',(70.2914136304585,218.763662624851,30.3493565173742)) ;
#76263 = CARTESIAN_POINT('Ctrl Pts',(70.3190962939392,219.194670899254,30.3493565173742)) ;
#76264 = CARTESIAN_POINT('Ctrl Pts',(70.3550083629108,219.625005037752,30.3493565173742)) ;
#76265 = CARTESIAN_POINT('Ctrl Pts',(70.2093020433682,218.335092697142,30.3713203435596)) ;
#76266 = CARTESIAN_POINT('Ctrl Pts',(70.228599383625,218.767286636677,30.3713203435596)) ;
#76267 = CARTESIAN_POINT('Ctrl Pts',(70.2563341749771,219.199103982098,30.3713203435596)) ;
#76268 = CARTESIAN_POINT('Ctrl Pts',(70.2923129177541,219.630237072465,30.3713203435596)) ;
#76269 = CARTESIAN_POINT('Ctrl Pts',(70.1824009080094,218.33629382542,30.3713203435596)) ;
#76270 = CARTESIAN_POINT('Ctrl Pts',(70.2017138522361,218.768837240123,30.3713203435596)) ;
#76271 = CARTESIAN_POINT('Ctrl Pts',(70.2294710222708,219.201001932499,30.3713203435596)) ;
#76272 = CARTESIAN_POINT('Ctrl Pts',(70.2654782591418,219.632476467448,30.3713203435596)) ;
#76273 = CARTESIAN_POINT('',(70.3022814706893,218.330941191344,30.2513203435596)) ;
#76274 = CARTESIAN_POINT('Origin',(70.1824009080094,218.33629382542,30.2513203435596)) ;
#76275 = CARTESIAN_POINT('Origin',(103.767178705384,216.834469413406,30.2513203435596)) ;
#76276 = CARTESIAN_POINT('Ctrl Pts',(70.2813572214291,216.003852832276,30.2513203435596)) ;
#76277 = CARTESIAN_POINT('Ctrl Pts',(70.2602736675229,216.779393400763,30.2513203435596)) ;
#76278 = CARTESIAN_POINT('Ctrl Pts',(70.2676697182798,217.555757180025,30.2513203435596)) ;
#76279 = CARTESIAN_POINT('Ctrl Pts',(70.3022814706893,218.330941191344,30.2513203435596)) ;
#76280 = CARTESIAN_POINT('Ctrl Pts',(70.2813572214291,216.003852832276,30.2872242596007)) ;
#76281 = CARTESIAN_POINT('Ctrl Pts',(70.2602739227663,216.779384011854,30.2872242596007)) ;
#76282 = CARTESIAN_POINT('Ctrl Pts',(70.2676701188078,217.555766150471,30.2872242596007)) ;
#76283 = CARTESIAN_POINT('Ctrl Pts',(70.3022814706893,218.330941191344,30.2872242596007)) ;
#76284 = CARTESIAN_POINT('Ctrl Pts',(70.2512096898405,216.003033252833,30.3493565363917)) ;
#76285 = CARTESIAN_POINT('Ctrl Pts',(70.2301060047771,216.779314328785,30.3493565363917)) ;
#76286 = CARTESIAN_POINT('Ctrl Pts',(70.2375094757991,217.556394913003,30.3493565363917)) ;
#76287 = CARTESIAN_POINT('Ctrl Pts',(70.2721528180251,218.33228642738,30.3493565363917)) ;
#76288 = CARTESIAN_POINT('Ctrl Pts',(70.1883195322401,216.001323544686,30.3713203435596)) ;
#76289 = CARTESIAN_POINT('Ctrl Pts',(70.1671739965509,216.779144060255,30.3713203435596)) ;
#76290 = CARTESIAN_POINT('Ctrl Pts',(70.1745930291305,217.557730355953,30.3713203435596)) ;
#76291 = CARTESIAN_POINT('Ctrl Pts',(70.2093020433682,218.335092697142,30.3713203435596)) ;
#76292 = CARTESIAN_POINT('Ctrl Pts',(70.1614015403524,216.000591762293,30.3713203435596)) ;
#76293 = CARTESIAN_POINT('Ctrl Pts',(70.1402381191435,216.779070181469,30.3713203435596)) ;
#76294 = CARTESIAN_POINT('Ctrl Pts',(70.14766382781,217.558302903379,30.3713203435596)) ;
#76295 = CARTESIAN_POINT('Ctrl Pts',(70.1824009080094,218.33629382542,30.3713203435596)) ;
#76296 = CARTESIAN_POINT('',(70.2813572214291,216.003852832276,30.2513203435596)) ;
#76297 = CARTESIAN_POINT('Origin',(70.1614015403524,216.000591762293,30.2513203435596)) ;
#76298 = CARTESIAN_POINT('Origin',(99.1329946690443,222.962162901317,30.2513203435596)) ;
#76299 = CARTESIAN_POINT('Ctrl Pts',(70.4779346423502,213.258471670562,30.2513203435596)) ;
#76300 = CARTESIAN_POINT('Ctrl Pts',(70.3711537499326,214.169914953712,30.2513203435596)) ;
#76301 = CARTESIAN_POINT('Ctrl Pts',(70.3063010559943,215.086315128482,30.2513203435596)) ;
#76302 = CARTESIAN_POINT('Ctrl Pts',(70.2813572214291,216.003852832275,30.2513203435596)) ;
#76303 = CARTESIAN_POINT('Ctrl Pts',(70.4779346423502,213.258471670562,30.2872242596007)) ;
#76304 = CARTESIAN_POINT('Ctrl Pts',(70.3711551172064,214.169903283155,30.2872242596007)) ;
#76305 = CARTESIAN_POINT('Ctrl Pts',(70.3063007540173,215.086326236448,30.2872242596007)) ;
#76306 = CARTESIAN_POINT('Ctrl Pts',(70.2813572214291,216.003852832275,30.2872242596007)) ;
#76307 = CARTESIAN_POINT('Ctrl Pts',(70.4479808643574,213.254962410903,30.3493565692531)) ;
#76308 = CARTESIAN_POINT('Ctrl Pts',(70.3410921344475,214.167326156092,30.3493565692531)) ;
#76309 = CARTESIAN_POINT('Ctrl Pts',(70.2761773688426,215.084619459547,30.3493565692531)) ;
#76310 = CARTESIAN_POINT('Ctrl Pts',(70.2512097172181,216.003033253576,30.3493565692531)) ;
#76311 = CARTESIAN_POINT('Ctrl Pts',(70.3854948082789,213.247641805271,30.3713203435596)) ;
#76312 = CARTESIAN_POINT('Ctrl Pts',(70.2783818952035,214.161919097311,30.3713203435596)) ;
#76313 = CARTESIAN_POINT('Ctrl Pts',(70.2133366971056,215.081088448267,30.3713203435596)) ;
#76314 = CARTESIAN_POINT('Ctrl Pts',(70.1883195322401,216.001323544685,30.3713203435596)) ;
#76315 = CARTESIAN_POINT('Ctrl Pts',(70.3587497899394,213.244508470505,30.3713203435596)) ;
#76316 = CARTESIAN_POINT('Ctrl Pts',(70.2515410686806,214.159603546732,30.3713203435596)) ;
#76317 = CARTESIAN_POINT('Ctrl Pts',(70.1864398654763,215.079578303801,30.3713203435596)) ;
#76318 = CARTESIAN_POINT('Ctrl Pts',(70.1614015403525,216.000591762292,30.3713203435596)) ;
#76319 = CARTESIAN_POINT('',(70.4779346423502,213.258471670562,30.2513203435596)) ;
#76320 = CARTESIAN_POINT('Origin',(70.3587497899394,213.244508470505,30.2513203435596)) ;
#76321 = CARTESIAN_POINT('Origin',(97.5077297790289,222.403214896199,30.2513203435596)) ;
#76322 = CARTESIAN_POINT('Ctrl Pts',(74.1761041106882,202.05583548982,30.2513203435596)) ;
#76323 = CARTESIAN_POINT('Ctrl Pts',(73.3476211486845,203.537657612761,30.2513203435596)) ;
#76324 = CARTESIAN_POINT('Ctrl Pts',(71.6591598866693,207.13437740547,30.2513203435596)) ;
#76325 = CARTESIAN_POINT('Ctrl Pts',(70.7411453681046,211.011799605831,30.2513203435596)) ;
#76326 = CARTESIAN_POINT('Ctrl Pts',(70.4779346423502,213.258471670562,30.2513203435596)) ;
#76327 = CARTESIAN_POINT('Ctrl Pts',(74.1761041106882,202.05583548982,30.2872242596007)) ;
#76328 = CARTESIAN_POINT('Ctrl Pts',(73.3476299244953,203.537641916373,30.2872242596007)) ;
#76329 = CARTESIAN_POINT('Ctrl Pts',(71.6591726184549,207.134367457936,30.2872242596007)) ;
#76330 = CARTESIAN_POINT('Ctrl Pts',(70.7411419978282,211.011828373298,30.2872242596007)) ;
#76331 = CARTESIAN_POINT('Ctrl Pts',(70.4779346423502,213.258471670562,30.2872242596007)) ;
#76332 = CARTESIAN_POINT('Ctrl Pts',(74.1497804176814,202.041117980333,30.3493566054646)) ;
#76333 = CARTESIAN_POINT('Ctrl Pts',(73.3206053035724,203.524178084438,30.3493566054646)) ;
#76334 = CARTESIAN_POINT('Ctrl Pts',(71.630469640981,207.124386091449,30.3493566054646)) ;
#76335 = CARTESIAN_POINT('Ctrl Pts',(70.7114574352898,211.006021446736,30.3493566054646)) ;
#76336 = CARTESIAN_POINT('Ctrl Pts',(70.4479808943322,213.254962414415,30.3493566054646)) ;
#76337 = CARTESIAN_POINT('Ctrl Pts',(74.0948669375559,202.010415993931,30.3713203435596)) ;
#76338 = CARTESIAN_POINT('Ctrl Pts',(73.2642529097014,203.496049734815,30.3713203435596)) ;
#76339 = CARTESIAN_POINT('Ctrl Pts',(71.5706265465599,207.103537714816,30.3713203435596)) ;
#76340 = CARTESIAN_POINT('Ctrl Pts',(70.6495239519761,210.993984019407,30.3713203435596)) ;
#76341 = CARTESIAN_POINT('Ctrl Pts',(70.3854948082789,213.247641805271,30.3713203435596)) ;
#76342 = CARTESIAN_POINT('Ctrl Pts',(74.0713631125318,201.997275065426,30.3713203435596)) ;
#76343 = CARTESIAN_POINT('Ctrl Pts',(73.2401341423739,203.484008690256,30.3713203435596)) ;
#76344 = CARTESIAN_POINT('Ctrl Pts',(71.5450141265831,207.094613224745,30.3713203435596)) ;
#76345 = CARTESIAN_POINT('Ctrl Pts',(70.6230150970638,210.988834878587,30.3713203435596)) ;
#76346 = CARTESIAN_POINT('Ctrl Pts',(70.3587497899395,213.244508470505,30.3713203435596)) ;
#76347 = CARTESIAN_POINT('',(74.1761041106883,202.05583548982,30.2513203435596)) ;
#76348 = CARTESIAN_POINT('Origin',(74.0713631125318,201.997275065426,30.2513203435596)) ;
#76349 = CARTESIAN_POINT('Ctrl Pts',(74.1761041106882,202.05583548982,30.2513203435596)) ;
#76350 = CARTESIAN_POINT('Ctrl Pts',(73.9471261103511,202.465384849466,30.2513203435596)) ;
#76351 = CARTESIAN_POINT('Ctrl Pts',(73.4020528825475,203.478780571653,30.2513203435596)) ;
#76352 = CARTESIAN_POINT('Ctrl Pts',(72.6149447082149,205.101979283954,30.2513203435596)) ;
#76353 = CARTESIAN_POINT('Ctrl Pts',(71.7263234125876,207.330523545477,30.2513203435596)) ;
#76354 = CARTESIAN_POINT('Ctrl Pts',(71.0883402872662,209.579226496892,30.2513203435596)) ;
#76355 = CARTESIAN_POINT('Ctrl Pts',(70.7249576044374,211.422049476544,30.2513203435596)) ;
#76356 = CARTESIAN_POINT('Ctrl Pts',(70.5491399848247,212.650688483389,30.2513203435596)) ;
#76357 = CARTESIAN_POINT('Ctrl Pts',(70.4779346423502,213.258471670562,30.2513203435596)) ;
#76358 = CARTESIAN_POINT('Ctrl Pts',(83.5725617978318,190.143531583735,30.2513203435596)) ;
#76359 = CARTESIAN_POINT('Ctrl Pts',(82.0318758172802,191.680398780727,30.2513203435596)) ;
#76360 = CARTESIAN_POINT('Ctrl Pts',(78.5794475585013,195.403251084408,30.2513203435596)) ;
#76361 = CARTESIAN_POINT('Ctrl Pts',(75.589441862932,199.527943855939,30.2513203435596)) ;
#76362 = CARTESIAN_POINT('Ctrl Pts',(74.1761041106884,202.05583548982,30.2513203435596)) ;
#76363 = CARTESIAN_POINT('Ctrl Pts',(83.5725617978318,190.143531583735,30.2872242596007)) ;
#76364 = CARTESIAN_POINT('Ctrl Pts',(82.0318829700591,191.680391645677,30.2872242596007)) ;
#76365 = CARTESIAN_POINT('Ctrl Pts',(78.5794502186911,195.403252953423,30.2872242596007)) ;
#76366 = CARTESIAN_POINT('Ctrl Pts',(75.5894268919727,199.527970632951,30.2872242596007)) ;
#76367 = CARTESIAN_POINT('Ctrl Pts',(74.1761041106884,202.05583548982,30.2872242596007)) ;
#76368 = CARTESIAN_POINT('Ctrl Pts',(83.5512629812335,190.12217984417,30.3493567154327)) ;
#76369 = CARTESIAN_POINT('Ctrl Pts',(82.0100128578202,191.659609785726,30.3493567154327)) ;
#76370 = CARTESIAN_POINT('Ctrl Pts',(78.5561937473121,195.383949481323,30.3493567154327)) ;
#76371 = CARTESIAN_POINT('Ctrl Pts',(75.5642990161483,199.511114476272,30.3493567154327)) ;
#76372 = CARTESIAN_POINT('Ctrl Pts',(74.1497804976783,202.041118025058,30.3493567154327)) ;
#76373 = CARTESIAN_POINT('Ctrl Pts',(83.506831624286,190.077638084883,30.3713203435596)) ;
#76374 = CARTESIAN_POINT('Ctrl Pts',(81.9644087053098,191.61623791508,30.3713203435596)) ;
#76375 = CARTESIAN_POINT('Ctrl Pts',(78.5076855957178,195.3436855626,30.3713203435596)) ;
#76376 = CARTESIAN_POINT('Ctrl Pts',(75.5118401487742,199.476021989111,30.3713203435596)) ;
#76377 = CARTESIAN_POINT('Ctrl Pts',(74.0948669375562,202.010415993931,30.3713203435596)) ;
#76378 = CARTESIAN_POINT('Ctrl Pts',(83.4878143389934,190.058573545737,30.3713203435596)) ;
#76379 = CARTESIAN_POINT('Ctrl Pts',(81.9448902074828,191.59767334615,30.3713203435596)) ;
#76380 = CARTESIAN_POINT('Ctrl Pts',(78.4869236645555,195.326452202177,30.3713203435596)) ;
#76381 = CARTESIAN_POINT('Ctrl Pts',(75.4893853751038,199.461004730524,30.3713203435596)) ;
#76382 = CARTESIAN_POINT('Ctrl Pts',(74.071363112532,201.997275065426,30.3713203435596)) ;
#76383 = CARTESIAN_POINT('',(83.5725617978318,190.143531583735,30.2513203435596)) ;
#76384 = CARTESIAN_POINT('Origin',(83.4878143389934,190.058573545737,30.2513203435596)) ;
#76385 = CARTESIAN_POINT('Ctrl Pts',(83.5725617978318,190.143531583735,30.2513203435596)) ;
#76386 = CARTESIAN_POINT('Ctrl Pts',(83.16020700552,190.554864302944,30.2513203435596)) ;
#76387 = CARTESIAN_POINT('Ctrl Pts',(82.1803361041118,191.549821741792,30.2513203435596)) ;
#76388 = CARTESIAN_POINT('Ctrl Pts',(80.6886895533707,193.132887074724,30.2513203435596)) ;
#76389 = CARTESIAN_POINT('Ctrl Pts',(78.784019206408,195.312002858836,30.2513203435596)) ;
#76390 = CARTESIAN_POINT('Ctrl Pts',(76.933494947875,197.696777376424,30.2513203435596)) ;
#76391 = CARTESIAN_POINT('Ctrl Pts',(75.5850166034805,199.677432982293,30.2513203435596)) ;
#76392 = CARTESIAN_POINT('Ctrl Pts',(74.7358054436199,201.068974645156,30.2513203435596)) ;
#76393 = CARTESIAN_POINT('Ctrl Pts',(74.2838092722993,201.863194363147,30.2513203435596)) ;
#76394 = CARTESIAN_POINT('Ctrl Pts',(74.1761041106884,202.05583548982,30.2513203435596)) ;
#76395 = CARTESIAN_POINT('Ctrl Pts',(83.4878143389935,190.058573545737,30.3713203435596)) ;
#76396 = CARTESIAN_POINT('Ctrl Pts',(83.5482147548369,189.998322839904,30.3713203435596)) ;
#76397 = CARTESIAN_POINT('Ctrl Pts',(83.6266011938506,189.835494820776,30.3713203435596)) ;
#76398 = CARTESIAN_POINT('Ctrl Pts',(83.576428513561,189.615885650627,30.3713203435596)) ;
#76399 = CARTESIAN_POINT('Ctrl Pts',(83.4319195690048,189.454561122737,30.3713203435596)) ;
#76400 = CARTESIAN_POINT('Ctrl Pts',(83.3047606779792,189.409539758744,30.3713203435596)) ;
#76401 = CARTESIAN_POINT('Ctrl Pts',(83.2194473860052,189.409539758744,30.3713203435596)) ;
#76402 = CARTESIAN_POINT('Ctrl Pts',(83.5131707193837,190.083992931264,30.3713203435596)) ;
#76403 = CARTESIAN_POINT('Ctrl Pts',(83.5793027341282,190.018024833018,30.3713203435596)) ;
#76404 = CARTESIAN_POINT('Ctrl Pts',(83.6651610120024,189.839826806225,30.3713203435596)) ;
#76405 = CARTESIAN_POINT('Ctrl Pts',(83.6102436634627,189.599417715804,30.3713203435596)) ;
#76406 = CARTESIAN_POINT('Ctrl Pts',(83.4520401256346,189.422828986583,30.3713203435596)) ;
#76407 = CARTESIAN_POINT('Ctrl Pts',(83.3128563436082,189.373635842703,30.3713203435596)) ;
#76408 = CARTESIAN_POINT('Ctrl Pts',(83.2194473860052,189.373635842703,30.3713203435596)) ;
#76409 = CARTESIAN_POINT('Ctrl Pts',(83.5570504774321,190.127981721049,30.3411618545504)) ;
#76410 = CARTESIAN_POINT('Ctrl Pts',(83.6330276918247,190.052192825717,30.3411618545504)) ;
#76411 = CARTESIAN_POINT('Ctrl Pts',(83.7316213436252,189.847353201833,30.3411618545504)) ;
#76412 = CARTESIAN_POINT('Ctrl Pts',(83.6685055832356,189.571099036852,30.3411618545504)) ;
#76413 = CARTESIAN_POINT('Ctrl Pts',(83.4867244971632,189.368159496056,30.3411618545504)) ;
#76414 = CARTESIAN_POINT('Ctrl Pts',(83.3267623139628,189.311503348844,30.3411618545504)) ;
#76415 = CARTESIAN_POINT('Ctrl Pts',(83.2194473860052,189.311503348844,30.3411618545504)) ;
#76416 = CARTESIAN_POINT('Ctrl Pts',(83.5725617978319,190.143531583735,30.2782482805904)) ;
#76417 = CARTESIAN_POINT('Ctrl Pts',(83.6520515313441,190.064238875503,30.2782482805904)) ;
#76418 = CARTESIAN_POINT('Ctrl Pts',(83.7552326945549,189.850000656062,30.2782482805904)) ;
#76419 = CARTESIAN_POINT('Ctrl Pts',(83.6892134061226,189.561009642818,30.2782482805904)) ;
#76420 = CARTESIAN_POINT('Ctrl Pts',(83.4990444715275,189.348726975021,30.2782482805904)) ;
#76421 = CARTESIAN_POINT('Ctrl Pts',(83.3317236137325,189.289539758744,30.2782482805904)) ;
#76422 = CARTESIAN_POINT('Ctrl Pts',(83.2194473860052,189.289539758744,30.2782482805904)) ;
#76423 = CARTESIAN_POINT('Ctrl Pts',(83.5725617978319,190.143531583735,30.2513203435596)) ;
#76424 = CARTESIAN_POINT('Ctrl Pts',(83.6520360292049,190.064254339218,30.2513203435596)) ;
#76425 = CARTESIAN_POINT('Ctrl Pts',(83.7551760805387,189.850006945628,30.2513203435596)) ;
#76426 = CARTESIAN_POINT('Ctrl Pts',(83.6891593959471,189.561047511221,30.2513203435596)) ;
#76427 = CARTESIAN_POINT('Ctrl Pts',(83.4990160478468,189.348778395577,30.2513203435596)) ;
#76428 = CARTESIAN_POINT('Ctrl Pts',(83.3317017175499,189.289539758744,30.2513203435596)) ;
#76429 = CARTESIAN_POINT('Ctrl Pts',(83.2194473860052,189.289539758744,30.2513203435596)) ;
#76430 = CARTESIAN_POINT('',(83.2194473860052,189.289539758744,30.2513203435596)) ;
#76431 = CARTESIAN_POINT('Origin',(83.2194473860052,189.409539758744,30.2513203435596)) ;
#76432 = CARTESIAN_POINT('Ctrl Pts',(83.2194473860051,189.289539758744,30.2513203435596)) ;
#76433 = CARTESIAN_POINT('Ctrl Pts',(83.2755767988648,189.289539758744,30.2513203435596)) ;
#76434 = CARTESIAN_POINT('Ctrl Pts',(83.4441273250624,189.317541444415,30.2513203435596)) ;
#76435 = CARTESIAN_POINT('Ctrl Pts',(83.6762811453293,189.502581007553,30.2513203435596)) ;
#76436 = CARTESIAN_POINT('Ctrl Pts',(83.7551748851088,189.850164868248,30.2513203435596)) ;
#76437 = CARTESIAN_POINT('Ctrl Pts',(83.6520392110072,190.064251165302,30.2513203435596)) ;
#76438 = CARTESIAN_POINT('Ctrl Pts',(83.5725617978318,190.143531583735,30.2513203435596)) ;
#76439 = CARTESIAN_POINT('Origin',(73.5558661461117,189.409539758744,30.2513203435596)) ;
#76440 = CARTESIAN_POINT('',(77.8285014478222,189.289539758744,30.2513203435596)) ;
#76441 = CARTESIAN_POINT('Origin',(77.8285014478222,189.409539758744,30.2513203435596)) ;
#76442 = CARTESIAN_POINT('',(73.5558661461117,189.289539758744,30.2513203435596)) ;
#76443 = CARTESIAN_POINT('Ctrl Pts',(77.8285014478222,189.409539758744,30.3713203435596)) ;
#76444 = CARTESIAN_POINT('Ctrl Pts',(77.6025348183859,189.409539758744,30.3713203435596)) ;
#76445 = CARTESIAN_POINT('Ctrl Pts',(77.3771291752411,189.482701147464,30.3713203435596)) ;
#76446 = CARTESIAN_POINT('Ctrl Pts',(77.1942359127804,189.615407485539,30.3713203435596)) ;
#76447 = CARTESIAN_POINT('Ctrl Pts',(77.8285014478222,189.373635842703,30.3713203435596)) ;
#76448 = CARTESIAN_POINT('Ctrl Pts',(77.5949901525181,189.373635842703,30.3713203435596)) ;
#76449 = CARTESIAN_POINT('Ctrl Pts',(77.3621499339521,189.449210320354,30.3713203435596)) ;
#76450 = CARTESIAN_POINT('Ctrl Pts',(77.1731501567454,189.5863475117,30.3713203435596)) ;
#76451 = CARTESIAN_POINT('Ctrl Pts',(77.8285014478222,189.311503249434,30.3411619374018)) ;
#76452 = CARTESIAN_POINT('Ctrl Pts',(77.5820306375502,189.311503249434,30.3411619374018)) ;
#76453 = CARTESIAN_POINT('Ctrl Pts',(77.3361497189201,189.391310432679,30.3411619374018)) ;
#76454 = CARTESIAN_POINT('Ctrl Pts',(77.1366607470111,189.536058525595,30.3411619374018)) ;
#76455 = CARTESIAN_POINT('Ctrl Pts',(77.8285014478222,189.289539758744,30.2782482805904)) ;
#76456 = CARTESIAN_POINT('Ctrl Pts',(77.5774070092103,189.289539758744,30.2782482805904)) ;
#76457 = CARTESIAN_POINT('Ctrl Pts',(77.3269932166768,189.370818206616,30.2782482805904)) ;
#76458 = CARTESIAN_POINT('Ctrl Pts',(77.1237619644425,189.518281677405,30.2782482805904)) ;
#76459 = CARTESIAN_POINT('Ctrl Pts',(77.8285014478222,189.289539758744,30.2513203435596)) ;
#76460 = CARTESIAN_POINT('Ctrl Pts',(77.577427415115,189.289539758744,30.2513203435596)) ;
#76461 = CARTESIAN_POINT('Ctrl Pts',(77.3269767005102,189.370830190655,30.2513203435596)) ;
#76462 = CARTESIAN_POINT('Ctrl Pts',(77.1237619644425,189.518281677405,30.2513203435596)) ;
#76463 = CARTESIAN_POINT('',(77.1237619644425,189.518281677405,30.2513203435596)) ;
#76464 = CARTESIAN_POINT('Origin',(77.1942359127804,189.615407485539,30.2513203435596)) ;
#76465 = CARTESIAN_POINT('Origin',(77.736831196317,190.207109471954,30.2513203435596)) ;
#76466 = CARTESIAN_POINT('Ctrl Pts',(66.1952689412979,200.55583548982,30.2513203435596)) ;
#76467 = CARTESIAN_POINT('Ctrl Pts',(67.4193871398855,198.688317658303,30.2513203435596)) ;
#76468 = CARTESIAN_POINT('Ctrl Pts',(70.723607560073,194.63303708426,30.2513203435596)) ;
#76469 = CARTESIAN_POINT('Ctrl Pts',(74.7177688589066,191.264056946398,30.2513203435596)) ;
#76470 = CARTESIAN_POINT('Ctrl Pts',(77.1237619644425,189.518281677405,30.2513203435596)) ;
#76471 = CARTESIAN_POINT('Ctrl Pts',(66.1952689412979,200.55583548982,30.2872242596007)) ;
#76472 = CARTESIAN_POINT('Ctrl Pts',(67.4194012221606,198.688296174348,30.2872242596007)) ;
#76473 = CARTESIAN_POINT('Ctrl Pts',(70.7236224085444,194.63301168528,30.2872242596007)) ;
#76474 = CARTESIAN_POINT('Ctrl Pts',(74.7177531457742,191.26406834776,30.2872242596007)) ;
#76475 = CARTESIAN_POINT('Ctrl Pts',(77.1237619644425,189.518281677405,30.2872242596007)) ;
#76476 = CARTESIAN_POINT('Ctrl Pts',(66.2204917300716,200.572368491131,30.3493568579639)) ;
#76477 = CARTESIAN_POINT('Ctrl Pts',(67.4434992533509,198.706545108684,30.3493568579639)) ;
#76478 = CARTESIAN_POINT('Ctrl Pts',(70.7448735388302,194.654676064875,30.3493568579639)) ;
#76479 = CARTESIAN_POINT('Ctrl Pts',(74.7367196744804,191.287567375558,30.3493568579639)) ;
#76480 = CARTESIAN_POINT('Ctrl Pts',(77.1414734782616,189.542691337053,30.3493568579639)) ;
#76481 = CARTESIAN_POINT('Ctrl Pts',(66.2731091727487,200.60685810513,30.3713203435596)) ;
#76482 = CARTESIAN_POINT('Ctrl Pts',(67.4938077151616,198.744557309755,30.3713203435596)) ;
#76483 = CARTESIAN_POINT('Ctrl Pts',(70.7892450940213,194.699802857899,30.3713203435596)) ;
#76484 = CARTESIAN_POINT('Ctrl Pts',(74.7762441741238,191.336619135049,30.3713203435596)) ;
#76485 = CARTESIAN_POINT('Ctrl Pts',(77.1784215957542,189.59361250516,30.3713203435596)) ;
#76486 = CARTESIAN_POINT('Ctrl Pts',(66.2956301826426,200.621620147878,30.3713203435596)) ;
#76487 = CARTESIAN_POINT('Ctrl Pts',(67.5153419459542,198.760824785205,30.3713203435596)) ;
#76488 = CARTESIAN_POINT('Ctrl Pts',(70.8082383262559,194.719115063076,30.3713203435596)) ;
#76489 = CARTESIAN_POINT('Ctrl Pts',(74.7931595483741,191.357615194406,30.3713203435596)) ;
#76490 = CARTESIAN_POINT('Ctrl Pts',(77.1942359127805,189.615407485539,30.3713203435596)) ;
#76491 = CARTESIAN_POINT('',(66.1952689412922,200.555835489829,30.2513203435596)) ;
#76492 = CARTESIAN_POINT('Origin',(66.2956301826426,200.621620147878,30.2513203435596)) ;
#76493 = CARTESIAN_POINT('Ctrl Pts',(66.1952689412979,200.55583548982,30.2513203435596)) ;
#76494 = CARTESIAN_POINT('Ctrl Pts',(66.518831227978,200.062208043811,30.2513203435596)) ;
#76495 = CARTESIAN_POINT('Ctrl Pts',(67.2058910887118,199.062896363505,30.2513203435596)) ;
#76496 = CARTESIAN_POINT('Ctrl Pts',(68.3175691899266,197.591996864875,30.2513203435596)) ;
#76497 = CARTESIAN_POINT('Ctrl Pts',(69.9484449125888,195.702271045863,30.2513203435596)) ;
#76498 = CARTESIAN_POINT('Ctrl Pts',(72.1605421210852,193.509486853481,30.2513203435596)) ;
#76499 = CARTESIAN_POINT('Ctrl Pts',(74.0936919389024,191.835218710936,30.2513203435596)) ;
#76500 = CARTESIAN_POINT('Ctrl Pts',(75.6101591471701,190.636965311174,30.2513203435596)) ;
#76501 = CARTESIAN_POINT('Ctrl Pts',(76.6350044216196,189.872921442927,30.2513203435596)) ;
#76502 = CARTESIAN_POINT('Ctrl Pts',(77.1237619644427,189.518281677405,30.2513203435596)) ;
#76503 = CARTESIAN_POINT('Ctrl Pts',(65.2679705316394,202.05583548982,30.2513203435596)) ;
#76504 = CARTESIAN_POINT('Ctrl Pts',(65.5637332147712,201.547759052751,30.2513203435596)) ;
#76505 = CARTESIAN_POINT('Ctrl Pts',(65.8729833388595,201.047515223108,30.2513203435596)) ;
#76506 = CARTESIAN_POINT('Ctrl Pts',(66.1952689412975,200.555835489821,30.2513203435596)) ;
#76507 = CARTESIAN_POINT('Ctrl Pts',(65.2679705316394,202.05583548982,30.2872242596007)) ;
#76508 = CARTESIAN_POINT('Ctrl Pts',(65.5637366175854,201.547753207221,30.2872242596007)) ;
#76509 = CARTESIAN_POINT('Ctrl Pts',(65.8729796312809,201.0475208794,30.2872242596007)) ;
#76510 = CARTESIAN_POINT('Ctrl Pts',(66.1952689412975,200.555835489821,30.2872242596007)) ;
#76511 = CARTESIAN_POINT('Ctrl Pts',(65.2940344552751,202.071007884021,30.3493568489088)) ;
#76512 = CARTESIAN_POINT('Ctrl Pts',(65.589528756939,201.563392486522,30.3493568489088)) ;
#76513 = CARTESIAN_POINT('Ctrl Pts',(65.8984985523252,201.063602114333,30.3493568489088)) ;
#76514 = CARTESIAN_POINT('Ctrl Pts',(66.2204917363829,200.572368495269,30.3493568489088)) ;
#76515 = CARTESIAN_POINT('Ctrl Pts',(65.3484065753628,202.102659113937,30.3713203435596)) ;
#76516 = CARTESIAN_POINT('Ctrl Pts',(65.6433429392841,201.596002170755,30.3713203435596)) ;
#76517 = CARTESIAN_POINT('Ctrl Pts',(65.9517238967263,201.097164298152,30.3713203435596)) ;
#76518 = CARTESIAN_POINT('Ctrl Pts',(66.2731091727483,200.60685810513,30.3713203435596)) ;
#76519 = CARTESIAN_POINT('Ctrl Pts',(65.371678614805,202.116206289766,30.3713203435596)) ;
#76520 = CARTESIAN_POINT('Ctrl Pts',(65.6663765353021,201.609958957032,30.3713203435596)) ;
#76521 = CARTESIAN_POINT('Ctrl Pts',(65.9745047056309,201.11152999087,30.3713203435596)) ;
#76522 = CARTESIAN_POINT('Ctrl Pts',(66.2956301826422,200.621620147878,30.3713203435596)) ;
#76523 = CARTESIAN_POINT('',(65.2679705316444,202.055835489811,30.2513203435596)) ;
#76524 = CARTESIAN_POINT('Origin',(65.371678614805,202.116206289766,30.2513203435596)) ;
#76525 = CARTESIAN_POINT('Origin',(94.0039513890618,218.783760942349,30.2513203435596)) ;
#76526 = CARTESIAN_POINT('Ctrl Pts',(61.1448474062769,212.657605881106,30.2513203435596)) ;
#76527 = CARTESIAN_POINT('Ctrl Pts',(62.0239099776425,208.957224782185,30.2513203435596)) ;
#76528 = CARTESIAN_POINT('Ctrl Pts',(63.3524709375853,205.346379782453,30.2513203435596)) ;
#76529 = CARTESIAN_POINT('Ctrl Pts',(65.2679705316376,202.055835489823,30.2513203435596)) ;
#76530 = CARTESIAN_POINT('Ctrl Pts',(61.1448474062769,212.657605881106,30.2872242596007)) ;
#76531 = CARTESIAN_POINT('Ctrl Pts',(62.0239170695688,208.957194928986,30.2872242596007)) ;
#76532 = CARTESIAN_POINT('Ctrl Pts',(63.3524488993448,205.346417640882,30.2872242596007)) ;
#76533 = CARTESIAN_POINT('Ctrl Pts',(65.2679705316376,202.055835489823,30.2872242596007)) ;
#76534 = CARTESIAN_POINT('Ctrl Pts',(61.1741893104987,212.66457634417,30.3493567486976)) ;
#76535 = CARTESIAN_POINT('Ctrl Pts',(62.0526925384775,208.966549780369,30.3493567486976)) ;
#76536 = CARTESIAN_POINT('Ctrl Pts',(63.3802730992418,205.358566307474,30.3493567486976)) ;
#76537 = CARTESIAN_POINT('Ctrl Pts',(65.2940345274534,202.071007926042,30.3493567486976)) ;
#76538 = CARTESIAN_POINT('Ctrl Pts',(61.2353993963707,212.67911741279,30.3713203435596)) ;
#76539 = CARTESIAN_POINT('Ctrl Pts',(62.1127398064059,208.985985687741,30.3713203435596)) ;
#76540 = CARTESIAN_POINT('Ctrl Pts',(63.4382586169361,205.384010090046,30.3713203435596)) ;
#76541 = CARTESIAN_POINT('Ctrl Pts',(65.3484065753611,202.10265911394,30.3713203435596)) ;
#76542 = CARTESIAN_POINT('Ctrl Pts',(61.2615982170421,212.685341204894,30.3713203435596)) ;
#76543 = CARTESIAN_POINT('Ctrl Pts',(62.1384416786349,208.994301365774,30.3713203435596)) ;
#76544 = CARTESIAN_POINT('Ctrl Pts',(63.4630749292305,205.394904434083,30.3713203435596)) ;
#76545 = CARTESIAN_POINT('Ctrl Pts',(65.3716786148033,202.116206289769,30.3713203435596)) ;
#76546 = CARTESIAN_POINT('',(61.1448474062699,212.657605881124,30.2513203435596)) ;
#76547 = CARTESIAN_POINT('Origin',(61.2615982170421,212.685341204894,30.2513203435596)) ;
#76548 = CARTESIAN_POINT('Origin',(136.041288291393,279.717177048122,30.2513203435596)) ;
#76549 = CARTESIAN_POINT('Ctrl Pts',(60.8054892120567,214.197609441503,30.2513203435596)) ;
#76550 = CARTESIAN_POINT('Ctrl Pts',(60.9103243659135,213.682523068924,30.2513203435596)) ;
#76551 = CARTESIAN_POINT('Ctrl Pts',(61.0233429894376,213.16907419082,30.2513203435596)) ;
#76552 = CARTESIAN_POINT('Ctrl Pts',(61.1448474062677,212.657605881144,30.2513203435596)) ;
#76553 = CARTESIAN_POINT('Ctrl Pts',(60.8054892120567,214.197609441503,30.2872242596007)) ;
#76554 = CARTESIAN_POINT('Ctrl Pts',(60.9103251761397,213.682519088041,30.2872242596007)) ;
#76555 = CARTESIAN_POINT('Ctrl Pts',(61.0233420091884,213.169078317142,30.2872242596007)) ;
#76556 = CARTESIAN_POINT('Ctrl Pts',(61.1448474062677,212.657605881144,30.2872242596007)) ;
#76557 = CARTESIAN_POINT('Ctrl Pts',(60.835041834708,214.203624265245,30.3493567305651)) ;
#76558 = CARTESIAN_POINT('Ctrl Pts',(60.9398130856633,213.688851866676,30.3493567305651)) ;
#76559 = CARTESIAN_POINT('Ctrl Pts',(61.0527622210523,213.175719212493,30.3493567305651)) ;
#76560 = CARTESIAN_POINT('Ctrl Pts',(61.1741893251925,212.664576347702,30.3493567305651)) ;
#76561 = CARTESIAN_POINT('Ctrl Pts',(60.8966914541607,214.216171767342,30.3713203435596)) ;
#76562 = CARTESIAN_POINT('Ctrl Pts',(61.0013298574909,213.702052088771,30.3713203435596)) ;
#76563 = CARTESIAN_POINT('Ctrl Pts',(61.114133017431,213.189583710846,30.3713203435596)) ;
#76564 = CARTESIAN_POINT('Ctrl Pts',(61.2353993963615,212.679117412829,30.3713203435596)) ;
#76565 = CARTESIAN_POINT('Ctrl Pts',(60.9230784080337,214.221542284825,30.3713203435596)) ;
#76566 = CARTESIAN_POINT('Ctrl Pts',(61.0276600368527,213.707701556357,30.3713203435596)) ;
#76567 = CARTESIAN_POINT('Ctrl Pts',(61.1404005265357,213.195518361553,30.3713203435596)) ;
#76568 = CARTESIAN_POINT('Ctrl Pts',(61.261598217033,212.685341204933,30.3713203435596)) ;
#76569 = CARTESIAN_POINT('',(60.8054892120567,214.197609441503,30.2513203435596)) ;
#76570 = CARTESIAN_POINT('Origin',(60.9230784080337,214.221542284825,30.2513203435596)) ;
#76571 = CARTESIAN_POINT('Origin',(195.552488558874,312.073624274513,30.2513203435596)) ;
#76572 = CARTESIAN_POINT('Ctrl Pts',(60.7651166309946,214.398081303037,30.2513203435596)) ;
#76573 = CARTESIAN_POINT('Ctrl Pts',(60.7784368168398,214.3312301992,30.2513203435596)) ;
#76574 = CARTESIAN_POINT('Ctrl Pts',(60.7918941539075,214.264406016215,30.2513203435596)) ;
#76575 = CARTESIAN_POINT('Ctrl Pts',(60.8054892120567,214.197609441503,30.2513203435596)) ;
#76576 = CARTESIAN_POINT('Ctrl Pts',(60.7651166309946,214.398081303037,30.2872242596007)) ;
#76577 = CARTESIAN_POINT('Ctrl Pts',(60.7784369192806,214.331229685072,30.2872242596007)) ;
#76578 = CARTESIAN_POINT('Ctrl Pts',(60.7918940488371,214.264406532458,30.2872242596007)) ;
#76579 = CARTESIAN_POINT('Ctrl Pts',(60.8054892120567,214.197609441503,30.2872242596007)) ;
#76580 = CARTESIAN_POINT('Ctrl Pts',(60.7946937326725,214.403974586296,30.3493567281575)) ;
#76581 = CARTESIAN_POINT('Ctrl Pts',(60.8080058389667,214.337164031961,30.3493567281575)) ;
#76582 = CARTESIAN_POINT('Ctrl Pts',(60.821455065475,214.270380124101,30.3493567281575)) ;
#76583 = CARTESIAN_POINT('Ctrl Pts',(60.8350418366743,214.203624265645,30.3493567281575)) ;
#76584 = CARTESIAN_POINT('Ctrl Pts',(60.856394411661,214.416268542024,30.3713203435596)) ;
#76585 = CARTESIAN_POINT('Ctrl Pts',(60.8696897213913,214.349542285975,30.3713203435596)) ;
#76586 = CARTESIAN_POINT('Ctrl Pts',(60.8831219106862,214.282842980849,30.3713203435596)) ;
#76587 = CARTESIAN_POINT('Ctrl Pts',(60.8966914541607,214.216171767342,30.3713203435596)) ;
#76588 = CARTESIAN_POINT('Ctrl Pts',(60.882803220617,214.421530538057,30.3713203435596)) ;
#76589 = CARTESIAN_POINT('Ctrl Pts',(60.8960913520729,214.3548403082,30.3713203435596)) ;
#76590 = CARTESIAN_POINT('Ctrl Pts',(60.9095162270971,214.288177323988,30.3713203435596)) ;
#76591 = CARTESIAN_POINT('Ctrl Pts',(60.9230784080337,214.221542284825,30.3713203435596)) ;
#76592 = CARTESIAN_POINT('',(60.7651166309946,214.398081303037,30.2513203435596)) ;
#76593 = CARTESIAN_POINT('Origin',(60.882803220617,214.421530538057,30.2513203435596)) ;
#76594 = CARTESIAN_POINT('Origin',(151.214887771711,273.326691475263,30.2513203435596)) ;
#76595 = CARTESIAN_POINT('Ctrl Pts',(60.882803220617,214.421530538057,30.3713203435596)) ;
#76596 = CARTESIAN_POINT('Ctrl Pts',(60.7690431212421,214.992467633397,30.3713203435596)) ;
#76597 = CARTESIAN_POINT('Ctrl Pts',(60.7116108526749,215.57461370503,30.3713203435596)) ;
#76598 = CARTESIAN_POINT('Ctrl Pts',(60.7116108526749,216.156773929576,30.3713203435596)) ;
#76599 = CARTESIAN_POINT('Ctrl Pts',(60.8475914753424,214.414514543346,30.3713203435596)) ;
#76600 = CARTESIAN_POINT('Ctrl Pts',(60.7333694243887,214.987770072776,30.3713203435596)) ;
#76601 = CARTESIAN_POINT('Ctrl Pts',(60.6757069366339,215.572249696592,30.3713203435596)) ;
#76602 = CARTESIAN_POINT('Ctrl Pts',(60.6757069366339,216.156773929576,30.3713203435596)) ;
#76603 = CARTESIAN_POINT('Ctrl Pts',(60.7866568455963,214.402373224115,30.3411618139191)) ;
#76604 = CARTESIAN_POINT('Ctrl Pts',(60.6716412978193,214.979611140814,30.3411618139191)) ;
#76605 = CARTESIAN_POINT('Ctrl Pts',(60.613574491527,215.568189026011,30.3411618139191)) ;
#76606 = CARTESIAN_POINT('Ctrl Pts',(60.613574491527,216.156773929576,30.3411618139191)) ;
#76607 = CARTESIAN_POINT('Ctrl Pts',(60.7651166309946,214.398081303037,30.2782482805904)) ;
#76608 = CARTESIAN_POINT('Ctrl Pts',(60.6498179835484,214.976740035151,30.2782482805904)) ;
#76609 = CARTESIAN_POINT('Ctrl Pts',(60.5916108526749,215.566740281083,30.2782482805904)) ;
#76610 = CARTESIAN_POINT('Ctrl Pts',(60.5916108526749,216.156773929576,30.2782482805904)) ;
#76611 = CARTESIAN_POINT('Ctrl Pts',(60.7651166309946,214.398081303037,30.2513203435596)) ;
#76612 = CARTESIAN_POINT('Ctrl Pts',(60.6498192329795,214.976733764529,30.2513203435596)) ;
#76613 = CARTESIAN_POINT('Ctrl Pts',(60.5916108526749,215.566746674968,30.2513203435596)) ;
#76614 = CARTESIAN_POINT('Ctrl Pts',(60.5916108526749,216.156773929576,30.2513203435596)) ;
#76615 = CARTESIAN_POINT('',(60.5916108526749,216.156773929576,30.2513203435596)) ;
#76616 = CARTESIAN_POINT('Origin',(60.7116108526749,216.156773929576,30.2513203435596)) ;
#76617 = CARTESIAN_POINT('Origin',(69.5988372871804,216.157486861515,30.2513203435596)) ;
#76618 = CARTESIAN_POINT('Origin',(60.7116108526749,218.583329440748,30.2513203435596)) ;
#76619 = CARTESIAN_POINT('',(60.5916108526749,219.547374675056,30.2513203435596)) ;
#76620 = CARTESIAN_POINT('',(60.5916108526749,218.583329440748,30.2513203435596)) ;
#76621 = CARTESIAN_POINT('Origin',(60.7116108526749,219.512965228765,30.2513203435596)) ;
#76622 = CARTESIAN_POINT('Origin',(61.5409585020332,220.840198908612,30.2513203435596)) ;
#76623 = CARTESIAN_POINT('',(60.6037668263229,219.566828299419,30.2513203435596)) ;
#76624 = CARTESIAN_POINT('',(61.4391927304944,220.90378922032,30.2513203435596)) ;
#76625 = CARTESIAN_POINT('Ctrl Pts',(60.7297059832955,219.541923491104,30.3713203435596)) ;
#76626 = CARTESIAN_POINT('Ctrl Pts',(60.7291626690358,219.542029099686,30.3713203435596)) ;
#76627 = CARTESIAN_POINT('Ctrl Pts',(60.7286193620522,219.542134730958,30.3713170060568)) ;
#76628 = CARTESIAN_POINT('Ctrl Pts',(60.7280760963346,219.54224037829,30.3713103308243)) ;
#76629 = CARTESIAN_POINT('Ctrl Pts',(60.7189335421281,219.544018304694,30.3711979941303)) ;
#76630 = CARTESIAN_POINT('Ctrl Pts',(60.7098171452966,219.545798043439,30.3701405530434)) ;
#76631 = CARTESIAN_POINT('Ctrl Pts',(60.7008889231376,219.54754742674,30.368145968699)) ;
#76632 = CARTESIAN_POINT('Ctrl Pts',(60.6920179977229,219.549285583397,30.3661641845724)) ;
#76633 = CARTESIAN_POINT('Ctrl Pts',(60.683361871084,219.550988074979,30.3632636735234)) ;
#76634 = CARTESIAN_POINT('Ctrl Pts',(60.6750811551749,219.552622038395,30.3594713481367)) ;
#76635 = CARTESIAN_POINT('Ctrl Pts',(60.6641759608159,219.554773867877,30.3544770884776)) ;
#76636 = CARTESIAN_POINT('Ctrl Pts',(60.6540116015145,219.556788120498,30.3479775495335)) ;
#76637 = CARTESIAN_POINT('Ctrl Pts',(60.644940406564,219.558593136451,30.3401148642541)) ;
#76638 = CARTESIAN_POINT('Ctrl Pts',(60.6419212766097,219.559193892775,30.3374979577961)) ;
#76639 = CARTESIAN_POINT('Ctrl Pts',(60.6390235198649,219.559771296374,30.3347301949426)) ;
#76640 = CARTESIAN_POINT('Ctrl Pts',(60.6362611894693,219.560322040799,30.3318176370222)) ;
#76641 = CARTESIAN_POINT('Ctrl Pts',(60.6280519358831,219.561958775005,30.3231619285703)) ;
#76642 = CARTESIAN_POINT('Ctrl Pts',(60.6211548413867,219.563338504298,30.313349088554)) ;
#76643 = CARTESIAN_POINT('Ctrl Pts',(60.6158491185412,219.564402430005,30.3026493500833)) ;
#76644 = CARTESIAN_POINT('Ctrl Pts',(60.6144636513314,219.564680249677,30.2998553600397)) ;
#76645 = CARTESIAN_POINT('Ctrl Pts',(60.6131868361209,219.564936447647,30.2970010850957)) ;
#76646 = CARTESIAN_POINT('Ctrl Pts',(60.6120239762211,219.565169769653,30.294091919136)) ;
#76647 = CARTESIAN_POINT('Ctrl Pts',(60.6065879367601,219.566260483705,30.2804923952736)) ;
#76648 = CARTESIAN_POINT('Ctrl Pts',(60.6037668263229,219.566828299419,30.2660017542171)) ;
#76649 = CARTESIAN_POINT('Ctrl Pts',(60.6037668263229,219.566828299419,30.2513203435596)) ;
#76650 = CARTESIAN_POINT('Origin',(64.1568347953872,220.146231446812,30.2513203435596)) ;
#76651 = CARTESIAN_POINT('Origin',(64.1568347953872,220.146231446812,30.2513203435596)) ;
#76652 = CARTESIAN_POINT('Ctrl Pts',(66.1952689412979,200.55583548982,17.8713203435596)) ;
#76653 = CARTESIAN_POINT('Ctrl Pts',(66.1952689412979,200.55583548982,32.8713203435596)) ;
#76654 = CARTESIAN_POINT('Ctrl Pts',(66.518831227978,200.062208043811,17.8713203435596)) ;
#76655 = CARTESIAN_POINT('Ctrl Pts',(66.518831227978,200.062208043811,32.8713203435596)) ;
#76656 = CARTESIAN_POINT('Ctrl Pts',(67.2058910887118,199.062896363505,17.8713203435596)) ;
#76657 = CARTESIAN_POINT('Ctrl Pts',(67.2058910887118,199.062896363505,32.8713203435596)) ;
#76658 = CARTESIAN_POINT('Ctrl Pts',(68.3175691899266,197.591996864875,17.8713203435596)) ;
#76659 = CARTESIAN_POINT('Ctrl Pts',(68.3175691899266,197.591996864875,32.8713203435596)) ;
#76660 = CARTESIAN_POINT('Ctrl Pts',(69.9484449125888,195.702271045863,17.8713203435596)) ;
#76661 = CARTESIAN_POINT('Ctrl Pts',(69.9484449125888,195.702271045863,32.8713203435596)) ;
#76662 = CARTESIAN_POINT('Ctrl Pts',(72.2129379945247,193.457548429354,17.8713203435596)) ;
#76663 = CARTESIAN_POINT('Ctrl Pts',(72.2129379945247,193.457548429354,32.8713203435596)) ;
#76664 = CARTESIAN_POINT('Ctrl Pts',(74.2078323511403,191.736557054229,17.8713203435596)) ;
#76665 = CARTESIAN_POINT('Ctrl Pts',(74.2078323511403,191.736557054229,32.8713203435596)) ;
#76666 = CARTESIAN_POINT('Ctrl Pts',(75.7911794288343,190.494445187268,17.8713203435596)) ;
#76667 = CARTESIAN_POINT('Ctrl Pts',(75.7911794288343,190.494445187268,32.8713203435596)) ;
#76668 = CARTESIAN_POINT('Ctrl Pts',(76.884855729364,189.687631312612,17.8713203435596)) ;
#76669 = CARTESIAN_POINT('Ctrl Pts',(76.884855729364,189.687631312612,32.8713203435596)) ;
#76670 = CARTESIAN_POINT('Ctrl Pts',(77.4412221473412,189.289539758744,17.8713203435596)) ;
#76671 = CARTESIAN_POINT('Ctrl Pts',(77.4412221473412,189.289539758744,32.8713203435596)) ;
#76672 = CARTESIAN_POINT('',(66.1952689412922,200.555835489829,17.9913203435596)) ;
#76673 = CARTESIAN_POINT('',(66.1952689412979,200.55583548982,29.8713203435596)) ;
#76674 = CARTESIAN_POINT('',(77.1237619644425,189.518281677405,17.9913203435596)) ;
#76675 = CARTESIAN_POINT('Ctrl Pts',(77.1237619644425,189.518281677405,17.9913203435596)) ;
#76676 = CARTESIAN_POINT('Ctrl Pts',(75.3192709150292,190.827610386593,17.9913203435596)) ;
#76677 = CARTESIAN_POINT('Ctrl Pts',(71.2757417352347,194.115942691271,17.9913203435596)) ;
#76678 = CARTESIAN_POINT('Ctrl Pts',(67.8274231206578,198.065816930128,17.9913203435596)) ;
#76679 = CARTESIAN_POINT('Ctrl Pts',(66.1952689412979,200.55583548982,17.9913203435596)) ;
#76680 = CARTESIAN_POINT('',(77.1237619644425,189.518281677405,30.2513203435596)) ;
#76681 = CARTESIAN_POINT('Origin',(93.970367839097,218.762990507114,17.8713203435596)) ;
#76682 = CARTESIAN_POINT('',(65.2679705316442,202.055835489812,17.9913203435596)) ;
#76683 = CARTESIAN_POINT('',(65.2679705316394,202.05583548982,23.8713203435596)) ;
#76684 = CARTESIAN_POINT('Origin',(94.003951389208,218.783760942439,17.9913203435596)) ;
#76685 = CARTESIAN_POINT('Ctrl Pts',(61.1448474062769,212.657605881106,17.8713203435596)) ;
#76686 = CARTESIAN_POINT('Ctrl Pts',(61.1448474062769,212.657605881106,32.8713203435596)) ;
#76687 = CARTESIAN_POINT('Ctrl Pts',(61.1691058108466,212.55549103208,17.8713203435596)) ;
#76688 = CARTESIAN_POINT('Ctrl Pts',(61.1691058108466,212.55549103208,32.8713203435596)) ;
#76689 = CARTESIAN_POINT('Ctrl Pts',(61.3438459206938,211.828860167372,17.8713203435596)) ;
#76690 = CARTESIAN_POINT('Ctrl Pts',(61.3438459206938,211.828860167372,32.8713203435596)) ;
#76691 = CARTESIAN_POINT('Ctrl Pts',(61.6936838095791,210.491445465305,17.8713203435596)) ;
#76692 = CARTESIAN_POINT('Ctrl Pts',(61.6936838095791,210.491445465305,32.8713203435596)) ;
#76693 = CARTESIAN_POINT('Ctrl Pts',(62.2740054220382,208.574144203583,17.8713203435596)) ;
#76694 = CARTESIAN_POINT('Ctrl Pts',(62.2740054220382,208.574144203583,32.8713203435596)) ;
#76695 = CARTESIAN_POINT('Ctrl Pts',(63.0635008176242,206.4341931397,17.8713203435596)) ;
#76696 = CARTESIAN_POINT('Ctrl Pts',(63.0635008176242,206.4341931397,32.8713203435596)) ;
#76697 = CARTESIAN_POINT('Ctrl Pts',(63.9562176049502,204.467472055247,17.8713203435596)) ;
#76698 = CARTESIAN_POINT('Ctrl Pts',(63.9562176049502,204.467472055247,32.8713203435596)) ;
#76699 = CARTESIAN_POINT('Ctrl Pts',(64.6673132018586,203.107895696197,17.8713203435596)) ;
#76700 = CARTESIAN_POINT('Ctrl Pts',(64.6673132018586,203.107895696197,32.8713203435596)) ;
#76701 = CARTESIAN_POINT('Ctrl Pts',(65.1188571217626,202.311990219034,17.8713203435596)) ;
#76702 = CARTESIAN_POINT('Ctrl Pts',(65.1188571217626,202.311990219034,32.8713203435596)) ;
#76703 = CARTESIAN_POINT('Ctrl Pts',(65.2679705316376,202.055835489823,17.8713203435596)) ;
#76704 = CARTESIAN_POINT('Ctrl Pts',(65.2679705316376,202.055835489823,32.8713203435596)) ;
#76705 = CARTESIAN_POINT('',(61.1448474062677,212.657605881144,17.9913203435596)) ;
#76706 = CARTESIAN_POINT('',(61.1448474062677,212.657605881144,23.8713203435596)) ;
#76707 = CARTESIAN_POINT('Origin',(136.041288291337,279.717177048067,17.9913203435596)) ;
#76708 = CARTESIAN_POINT('Ctrl Pts',(60.8054892120567,214.197609441503,17.8713203435596)) ;
#76709 = CARTESIAN_POINT('Ctrl Pts',(60.8054892120567,214.197609441503,32.8713203435596)) ;
#76710 = CARTESIAN_POINT('Ctrl Pts',(60.8687049964709,213.887011441827,17.8713203435596)) ;
#76711 = CARTESIAN_POINT('Ctrl Pts',(60.8687049964709,213.887011441827,32.8713203435596)) ;
#76712 = CARTESIAN_POINT('Ctrl Pts',(60.9342401816044,213.577707329413,17.8713203435596)) ;
#76713 = CARTESIAN_POINT('Ctrl Pts',(60.9342401816044,213.577707329413,32.8713203435596)) ;
#76714 = CARTESIAN_POINT('Ctrl Pts',(61.0021011324506,213.269700654998,17.8713203435596)) ;
#76715 = CARTESIAN_POINT('Ctrl Pts',(61.0021011324506,213.269700654998,32.8713203435596)) ;
#76716 = CARTESIAN_POINT('Ctrl Pts',(61.0722985912904,212.962997411209,17.8713203435596)) ;
#76717 = CARTESIAN_POINT('Ctrl Pts',(61.0722985912904,212.962997411209,32.8713203435596)) ;
#76718 = CARTESIAN_POINT('Ctrl Pts',(61.1448474062677,212.657605881144,17.8713203435596)) ;
#76719 = CARTESIAN_POINT('Ctrl Pts',(61.1448474062677,212.657605881144,32.8713203435596)) ;
#76720 = CARTESIAN_POINT('',(60.8054892120567,214.197609441503,23.8713203435596)) ;
#76721 = CARTESIAN_POINT('',(60.8054892120567,214.197609441503,23.8713203435596)) ;
#76722 = CARTESIAN_POINT('',(60.8382191089243,214.038138460174,23.8713203435596)) ;
#76723 = CARTESIAN_POINT('Origin',(73.0542750642243,222.307841389544,23.8713203435596)) ;
#76724 = CARTESIAN_POINT('',(60.8382191089243,214.038138460174,23.7513203435596)) ;
#76725 = CARTESIAN_POINT('',(60.8382191089243,214.038138460174,17.9913203435596)) ;
#76726 = CARTESIAN_POINT('',(60.8382191089244,214.038138460174,17.9913203435596)) ;
#76727 = CARTESIAN_POINT('Origin',(202.163078386837,317.851891258764,17.9913203435596)) ;
#76728 = CARTESIAN_POINT('Ctrl Pts',(60.5916108526749,215.31305736582,23.4393203435596)) ;
#76729 = CARTESIAN_POINT('Ctrl Pts',(60.5916108526749,215.31305736582,31.7577203435596)) ;
#76730 = CARTESIAN_POINT('Ctrl Pts',(60.7075588580463,214.669276583145,23.4393203435596)) ;
#76731 = CARTESIAN_POINT('Ctrl Pts',(60.7075588580463,214.669276583145,31.7577203435596)) ;
#76732 = CARTESIAN_POINT('Ctrl Pts',(60.9588614284726,213.392541047196,23.4393203435596)) ;
#76733 = CARTESIAN_POINT('Ctrl Pts',(60.9588614284726,213.392541047196,31.7577203435596)) ;
#76734 = CARTESIAN_POINT('Ctrl Pts',(61.3940337100567,211.509915132417,23.4393203435596)) ;
#76735 = CARTESIAN_POINT('Ctrl Pts',(61.3940337100567,211.509915132417,31.7577203435596)) ;
#76736 = CARTESIAN_POINT('Ctrl Pts',(62.0926267016154,209.065776691758,23.4393203435596)) ;
#76737 = CARTESIAN_POINT('Ctrl Pts',(62.0926267016154,209.065776691758,31.7577203435596)) ;
#76738 = CARTESIAN_POINT('Ctrl Pts',(63.176438760595,206.128071441506,23.4393203435596)) ;
#76739 = CARTESIAN_POINT('Ctrl Pts',(63.176438760595,206.128071441506,31.7577203435596)) ;
#76740 = CARTESIAN_POINT('Ctrl Pts',(64.4892878686988,203.318135454206,23.4393203435596)) ;
#76741 = CARTESIAN_POINT('Ctrl Pts',(64.4892878686988,203.318135454206,31.7577203435596)) ;
#76742 = CARTESIAN_POINT('Ctrl Pts',(66.0493169032885,200.646089808857,23.4393203435596)) ;
#76743 = CARTESIAN_POINT('Ctrl Pts',(66.0493169032885,200.646089808857,31.7577203435596)) ;
#76744 = CARTESIAN_POINT('Ctrl Pts',(67.8654194647057,198.116895837109,23.4393203435596)) ;
#76745 = CARTESIAN_POINT('Ctrl Pts',(67.8654194647057,198.116895837109,31.7577203435596)) ;
#76746 = CARTESIAN_POINT('Ctrl Pts',(69.9262808608795,195.724241591299,23.4393203435596)) ;
#76747 = CARTESIAN_POINT('Ctrl Pts',(69.9262808608795,195.724241591299,31.7577203435596)) ;
#76748 = CARTESIAN_POINT('Ctrl Pts',(72.2129379945247,193.457548429354,23.4393203435596)) ;
#76749 = CARTESIAN_POINT('Ctrl Pts',(72.2129379945247,193.457548429354,31.7577203435596)) ;
#76750 = CARTESIAN_POINT('Ctrl Pts',(74.2078323511403,191.736557054229,23.4393203435596)) ;
#76751 = CARTESIAN_POINT('Ctrl Pts',(74.2078323511403,191.736557054229,31.7577203435596)) ;
#76752 = CARTESIAN_POINT('Ctrl Pts',(75.7911794288343,190.494445187268,23.4393203435596)) ;
#76753 = CARTESIAN_POINT('Ctrl Pts',(75.7911794288343,190.494445187268,31.7577203435596)) ;
#76754 = CARTESIAN_POINT('Ctrl Pts',(76.884855729364,189.687631312612,23.4393203435596)) ;
#76755 = CARTESIAN_POINT('Ctrl Pts',(76.884855729364,189.687631312612,31.7577203435596)) ;
#76756 = CARTESIAN_POINT('Ctrl Pts',(77.4412221473412,189.289539758744,23.4393203435596)) ;
#76757 = CARTESIAN_POINT('Ctrl Pts',(77.4412221473412,189.289539758744,31.7577203435596)) ;
#76758 = CARTESIAN_POINT('',(60.7651166309946,214.398081303037,23.8713203435596)) ;
#76759 = CARTESIAN_POINT('',(60.7651166309946,214.398081303037,23.8713203435596)) ;
#76760 = CARTESIAN_POINT('Origin',(72.876859665819,222.190806294465,23.8713203435596)) ;
#76761 = CARTESIAN_POINT('Ctrl Pts',(60.7651166309946,214.398081303037,23.8713203435596)) ;
#76762 = CARTESIAN_POINT('Ctrl Pts',(60.7651166309946,214.398081303037,31.5273203435596)) ;
#76763 = CARTESIAN_POINT('Ctrl Pts',(60.6498192105232,214.976733877232,23.8713203435596)) ;
#76764 = CARTESIAN_POINT('Ctrl Pts',(60.6498192105232,214.976733877232,31.5273203435596)) ;
#76765 = CARTESIAN_POINT('Ctrl Pts',(60.5916108526749,215.56674656005,23.8713203435596)) ;
#76766 = CARTESIAN_POINT('Ctrl Pts',(60.5916108526749,215.56674656005,31.5273203435596)) ;
#76767 = CARTESIAN_POINT('Ctrl Pts',(60.5916108526749,216.156773929576,23.8713203435596)) ;
#76768 = CARTESIAN_POINT('Ctrl Pts',(60.5916108526749,216.156773929576,31.5273203435596)) ;
#76769 = CARTESIAN_POINT('',(60.5916108526749,216.156773929576,23.8713203435596)) ;
#76770 = CARTESIAN_POINT('',(60.5916108526749,216.156773929576,30.2513203435596)) ;
#76771 = CARTESIAN_POINT('Ctrl Pts',(60.5916108526749,216.156773929576,23.8713203435596)) ;
#76772 = CARTESIAN_POINT('Ctrl Pts',(60.5916108526749,215.861760359297,23.8713203435596)) ;
#76773 = CARTESIAN_POINT('Ctrl Pts',(60.606162930897,215.566750345658,23.8713203435596)) ;
#76774 = CARTESIAN_POINT('Ctrl Pts',(60.664091487419,214.979573790456,23.8713203435596)) ;
#76775 = CARTESIAN_POINT('Ctrl Pts',(60.7074679431304,214.687407477857,23.8713203435596)) ;
#76776 = CARTESIAN_POINT('Ctrl Pts',(60.7651166309946,214.398081303037,23.8713203435596)) ;
#76777 = CARTESIAN_POINT('Origin',(60.5916108526749,219.547374675056,23.8713203435596)) ;
#76778 = CARTESIAN_POINT('',(60.5916108526749,219.547374675056,23.8713203435596)) ;
#76779 = CARTESIAN_POINT('',(60.5916108526749,219.547374675056,23.8713203435596)) ;
#76780 = CARTESIAN_POINT('',(60.5916108526749,220.645409008718,23.8713203435596)) ;
#76781 = CARTESIAN_POINT('Origin',(60.6037668263229,219.566828299419,23.8713203435596)) ;
#76782 = CARTESIAN_POINT('',(60.6037668263229,219.566828299419,23.8713203435596)) ;
#76783 = CARTESIAN_POINT('',(60.6037668263229,219.566828299419,23.8713203435596)) ;
#76784 = CARTESIAN_POINT('',(63.8582048387328,224.775017823302,23.8713203435596)) ;
#76785 = CARTESIAN_POINT('Origin',(64.1568347953872,220.146231446812,23.8713203435596)) ;
#76786 = CARTESIAN_POINT('',(60.5916108526749,219.647053884905,23.8713203435596)) ;
#76787 = CARTESIAN_POINT('',(60.5916108526749,219.647053884905,23.8713203435596)) ;
#76788 = CARTESIAN_POINT('Origin',(64.1568347953872,220.146231446812,23.8713203435596)) ;
#76789 = CARTESIAN_POINT('Origin',(60.5916108526749,220.645409008718,23.8713203435596)) ;
#76790 = CARTESIAN_POINT('',(60.5916108526749,220.645409008718,23.8713203435596)) ;
#76791 = CARTESIAN_POINT('',(60.5916108526749,220.645409008718,23.8713203435596)) ;
#76792 = CARTESIAN_POINT('',(60.5916108526749,220.645409008718,23.8713203435596)) ;
#76793 = CARTESIAN_POINT('Origin',(64.1568347953872,220.146231446812,30.2513203435596)) ;
#76794 = CARTESIAN_POINT('',(61.7916108526749,217.432246240363,30.2513203435596)) ;
#76795 = CARTESIAN_POINT('Ctrl Pts',(61.671610852675,217.7102384348,30.3713203435596)) ;
#76796 = CARTESIAN_POINT('Ctrl Pts',(61.6721253819932,217.708978462956,30.3713203435596)) ;
#76797 = CARTESIAN_POINT('Ctrl Pts',(61.6726402662739,217.70771859947,30.3713170343059)) ;
#76798 = CARTESIAN_POINT('Ctrl Pts',(61.6962023853316,217.650109410363,30.3710137213554)) ;
#76799 = CARTESIAN_POINT('Ctrl Pts',(61.7186676884083,217.597219366085,30.3641419360414)) ;
#76800 = CARTESIAN_POINT('Ctrl Pts',(61.7513364234646,217.522083093465,30.3424118695719)) ;
#76801 = CARTESIAN_POINT('Ctrl Pts',(61.7626310589793,217.496635439055,30.3311044721307)) ;
#76802 = CARTESIAN_POINT('Ctrl Pts',(61.7762176463779,217.466271908482,30.3107533540404)) ;
#76803 = CARTESIAN_POINT('Ctrl Pts',(61.780952629944,217.455762082477,30.3019796043198)) ;
#76804 = CARTESIAN_POINT('Ctrl Pts',(61.7868899451735,217.44263800318,30.2853058545662)) ;
#76805 = CARTESIAN_POINT('Ctrl Pts',(61.7888011111258,217.438427571582,30.2782891621224)) ;
#76806 = CARTESIAN_POINT('Ctrl Pts',(61.7910596764519,217.433457069678,30.2644053677528)) ;
#76807 = CARTESIAN_POINT('Ctrl Pts',(61.7916108526749,217.432246240364,30.257961146373)) ;
#76808 = CARTESIAN_POINT('Ctrl Pts',(61.7916108526749,217.432246240364,30.2513203435596)) ;
#76809 = CARTESIAN_POINT('',(67.7485452644419,219.902067758924,30.2513203435596)) ;
#76810 = CARTESIAN_POINT('Origin',(64.1568347953872,220.146231446812,30.2513203435596)) ;
#76811 = CARTESIAN_POINT('Ctrl Pts',(67.635124836556,220.037151707603,30.3713203435596)) ;
#76812 = CARTESIAN_POINT('Ctrl Pts',(67.6356227882016,220.036569616232,30.3713203435596)) ;
#76813 = CARTESIAN_POINT('Ctrl Pts',(67.636120674921,220.035987456957,30.3713170159727)) ;
#76814 = CARTESIAN_POINT('Ctrl Pts',(67.6490217074181,220.020899064839,30.371144461022)) ;
#76815 = CARTESIAN_POINT('Ctrl Pts',(67.6614649298788,220.006254419689,30.3689095647645)) ;
#76816 = CARTESIAN_POINT('Ctrl Pts',(67.6846753402724,219.978777532849,30.3602924369633)) ;
#76817 = CARTESIAN_POINT('Ctrl Pts',(67.6956816716256,219.965671687184,30.3540979027369)) ;
#76818 = CARTESIAN_POINT('Ctrl Pts',(67.7154693827078,219.941997430011,30.337552097772)) ;
#76819 = CARTESIAN_POINT('Ctrl Pts',(67.7244805588803,219.931158578531,30.327243797285)) ;
#76820 = CARTESIAN_POINT('Ctrl Pts',(67.7371840595297,219.915830858124,30.3052692101847)) ;
#76821 = CARTESIAN_POINT('Ctrl Pts',(67.7416269457272,219.910452972978,30.2947007603144)) ;
#76822 = CARTESIAN_POINT('Ctrl Pts',(67.7471684473396,219.903738959239,30.2728956002824)) ;
#76823 = CARTESIAN_POINT('Ctrl Pts',(67.7485452644419,219.902067758924,30.26223415745)) ;
#76824 = CARTESIAN_POINT('Ctrl Pts',(67.7485452644419,219.902067758924,30.2513203435596)) ;
#76825 = CARTESIAN_POINT('Ctrl Pts',(62.1439228384234,214.067655379578,30.2513203435596)) ;
#76826 = CARTESIAN_POINT('Ctrl Pts',(62.1222982033092,214.069755004928,30.2513203435596)) ;
#76827 = CARTESIAN_POINT('Ctrl Pts',(62.0731635470014,214.088684352254,30.2513203435596)) ;
#76828 = CARTESIAN_POINT('Ctrl Pts',(62.044013686833,214.13412578273,30.2513203435596)) ;
#76829 = CARTESIAN_POINT('Ctrl Pts',(62.0380714133749,214.162478201405,30.2513203435596)) ;
#76830 = CARTESIAN_POINT('Ctrl Pts',(62.1439228384234,214.067655379578,30.2872242596007)) ;
#76831 = CARTESIAN_POINT('Ctrl Pts',(62.1223673122467,214.069748294855,30.2872242596007)) ;
#76832 = CARTESIAN_POINT('Ctrl Pts',(62.0732712928142,214.088723191247,30.2872242596007)) ;
#76833 = CARTESIAN_POINT('Ctrl Pts',(62.0439946962603,214.134216392607,30.2872242596007)) ;
#76834 = CARTESIAN_POINT('Ctrl Pts',(62.0380714133749,214.162478201405,30.2872242596007)) ;
#76835 = CARTESIAN_POINT('Ctrl Pts',(62.1410083285202,214.03763801805,30.3493567156287)) ;
#76836 = CARTESIAN_POINT('Ctrl Pts',(62.1139330407202,214.040266869835,30.3493567156287)) ;
#76837 = CARTESIAN_POINT('Ctrl Pts',(62.0524409085205,214.063943061966,30.3493567156287)) ;
#76838 = CARTESIAN_POINT('Ctrl Pts',(62.0159942853878,214.120792946662,30.3493567156287)) ;
#76839 = CARTESIAN_POINT('Ctrl Pts',(62.0085542170022,214.156291806707,30.3493567156287)) ;
#76840 = CARTESIAN_POINT('Ctrl Pts',(62.1349283836427,213.975018946742,30.3713203435596)) ;
#76841 = CARTESIAN_POINT('Ctrl Pts',(62.0965217439458,213.978748006395,30.3713203435596)) ;
#76842 = CARTESIAN_POINT('Ctrl Pts',(62.0092726729388,214.012352423146,30.3713203435596)) ;
#76843 = CARTESIAN_POINT('Ctrl Pts',(61.9575323693022,214.093030815,30.3713203435596)) ;
#76844 = CARTESIAN_POINT('Ctrl Pts',(61.9469785377818,214.143386398936,30.3713203435596)) ;
#76845 = CARTESIAN_POINT('Ctrl Pts',(62.1323260763097,213.948217047756,30.3713203435596)) ;
#76846 = CARTESIAN_POINT('Ctrl Pts',(62.0890768060814,213.952416298455,30.3713203435596)) ;
#76847 = CARTESIAN_POINT('Ctrl Pts',(61.9908074934658,213.990274993108,30.3713203435596)) ;
#76848 = CARTESIAN_POINT('Ctrl Pts',(61.932507773129,214.081157854061,30.3713203435596)) ;
#76849 = CARTESIAN_POINT('Ctrl Pts',(61.9206232262128,214.13786269141,30.3713203435596)) ;
#76850 = CARTESIAN_POINT('',(62.1439228384234,214.067655379578,30.2513203435596)) ;
#76851 = CARTESIAN_POINT('Origin',(62.1323260763097,213.948217047756,30.2513203435596)) ;
#76852 = CARTESIAN_POINT('',(62.0380714133749,214.162478201405,30.2513203435596)) ;
#76853 = CARTESIAN_POINT('Ctrl Pts',(62.1439228384234,214.067655379578,30.2513203435596)) ;
#76854 = CARTESIAN_POINT('Ctrl Pts',(62.115089064211,214.070454970089,30.2513203435596)) ;
#76855 = CARTESIAN_POINT('Ctrl Pts',(62.0667252302728,214.094448639981,30.2513203435596)) ;
#76856 = CARTESIAN_POINT('Ctrl Pts',(62.0425282618161,214.141213203443,30.2513203435596)) ;
#76857 = CARTESIAN_POINT('Ctrl Pts',(62.0380714133749,214.162478201405,30.2513203435596)) ;
#76858 = CARTESIAN_POINT('Origin',(61.9206232262128,214.13786269141,30.2513203435596)) ;
#76859 = CARTESIAN_POINT('Origin',(62.155519600537,214.1870937114,26.4913203435596)) ;
#76860 = CARTESIAN_POINT('',(62.0380714133749,214.162478201405,26.4913203435596)) ;
#76861 = CARTESIAN_POINT('',(62.1555196005219,214.187093711472,26.3713203435596)) ;
#76862 = CARTESIAN_POINT('Origin',(62.155519600537,214.1870937114,26.4913203435596)) ;
#76863 = CARTESIAN_POINT('',(62.1439228384234,214.067655379578,26.4913203435596)) ;
#76864 = CARTESIAN_POINT('Origin',(62.155519600537,214.1870937114,26.4913203435596)) ;
#76865 = CARTESIAN_POINT('Origin',(62.1555196004967,214.187093711404,26.4913203435596)) ;
#76866 = CARTESIAN_POINT('Ctrl Pts',(62.1439228384234,214.067655379578,26.4913203435596)) ;
#76867 = CARTESIAN_POINT('Ctrl Pts',(62.1439228384234,214.067655379578,31.0033203435597)) ;
#76868 = CARTESIAN_POINT('Ctrl Pts',(62.115089064211,214.070454970089,26.4913203435596)) ;
#76869 = CARTESIAN_POINT('Ctrl Pts',(62.115089064211,214.070454970089,31.0033203435597)) ;
#76870 = CARTESIAN_POINT('Ctrl Pts',(62.0667252302728,214.094448639981,26.4913203435596)) ;
#76871 = CARTESIAN_POINT('Ctrl Pts',(62.0667252302728,214.094448639981,31.0033203435597)) ;
#76872 = CARTESIAN_POINT('Ctrl Pts',(62.0425282618161,214.141213203443,26.4913203435596)) ;
#76873 = CARTESIAN_POINT('Ctrl Pts',(62.0425282618161,214.141213203443,31.0033203435597)) ;
#76874 = CARTESIAN_POINT('Ctrl Pts',(62.0380714133749,214.162478201405,26.4913203435596)) ;
#76875 = CARTESIAN_POINT('Ctrl Pts',(62.0380714133749,214.162478201405,31.0033203435597)) ;
#76876 = CARTESIAN_POINT('',(62.1439228384234,214.067655379578,30.2513203435597)) ;
#76877 = CARTESIAN_POINT('',(62.0380714133749,214.162478201405,26.4913203435596)) ;
#76878 = CARTESIAN_POINT('Ctrl Pts',(69.2413920554874,213.523097238281,30.2513203435596)) ;
#76879 = CARTESIAN_POINT('Ctrl Pts',(69.2429622182083,213.507997501652,30.2513203435596)) ;
#76880 = CARTESIAN_POINT('Ctrl Pts',(69.2398976738995,213.472038237813,30.2513203435596)) ;
#76881 = CARTESIAN_POINT('Ctrl Pts',(69.2135287770271,213.426976369741,30.2513203435596)) ;
#76882 = CARTESIAN_POINT('Ctrl Pts',(69.1666694054386,213.395034372691,30.2513203435596)) ;
#76883 = CARTESIAN_POINT('Ctrl Pts',(69.1305856629887,213.38929136102,30.2513203435596)) ;
#76884 = CARTESIAN_POINT('Ctrl Pts',(69.1104388653291,213.391247497013,30.2513203435596)) ;
#76885 = CARTESIAN_POINT('Ctrl Pts',(69.2413920554874,213.523097238281,30.2872242596007)) ;
#76886 = CARTESIAN_POINT('Ctrl Pts',(69.2429572002149,213.508045758039,30.2872242596007)) ;
#76887 = CARTESIAN_POINT('Ctrl Pts',(69.2398004488935,213.472098680599,30.2872242596007)) ;
#76888 = CARTESIAN_POINT('Ctrl Pts',(69.2134077180135,213.427071983451,30.2872242596007)) ;
#76889 = CARTESIAN_POINT('Ctrl Pts',(69.1666433975403,213.395176978348,30.2872242596007)) ;
#76890 = CARTESIAN_POINT('Ctrl Pts',(69.1305212769876,213.389297612523,30.2872242596007)) ;
#76891 = CARTESIAN_POINT('Ctrl Pts',(69.1104388653291,213.391247497013,30.2872242596007)) ;
#76892 = CARTESIAN_POINT('Ctrl Pts',(69.271388915094,213.526216494719,30.3493566164462)) ;
#76893 = CARTESIAN_POINT('Ctrl Pts',(69.2733548491936,213.507310755373,30.3493566164462)) ;
#76894 = CARTESIAN_POINT('Ctrl Pts',(69.2695413496691,213.462311342459,30.3493566164462)) ;
#76895 = CARTESIAN_POINT('Ctrl Pts',(69.2365508649147,213.405916351071,30.3493566164462)) ;
#76896 = CARTESIAN_POINT('Ctrl Pts',(69.1778928305879,213.365935817039,30.3493566164462)) ;
#76897 = CARTESIAN_POINT('Ctrl Pts',(69.1327492976852,213.358780858359,30.3493566164462)) ;
#76898 = CARTESIAN_POINT('Ctrl Pts',(69.1075243474375,213.36123005321,30.3493566164462)) ;
#76899 = CARTESIAN_POINT('Ctrl Pts',(69.3339649637103,213.532723533959,30.3713203435596)) ;
#76900 = CARTESIAN_POINT('Ctrl Pts',(69.336753666205,213.505905502527,30.3713203435596)) ;
#76901 = CARTESIAN_POINT('Ctrl Pts',(69.3313255035809,213.442054464431,30.3713203435596)) ;
#76902 = CARTESIAN_POINT('Ctrl Pts',(69.2845082997786,213.362037536173,30.3713203435596)) ;
#76903 = CARTESIAN_POINT('Ctrl Pts',(69.2012911226345,213.305314559911,30.3713203435596)) ;
#76904 = CARTESIAN_POINT('Ctrl Pts',(69.1372263229216,213.295136850167,30.3713203435596)) ;
#76905 = CARTESIAN_POINT('Ctrl Pts',(69.1014444105484,213.298611064177,30.3713203435596)) ;
#76906 = CARTESIAN_POINT('Ctrl Pts',(69.360748483532,213.535508647726,30.3713203435596)) ;
#76907 = CARTESIAN_POINT('Ctrl Pts',(69.3638888089739,213.505309174469,30.3713203435596)) ;
#76908 = CARTESIAN_POINT('Ctrl Pts',(69.3577597203562,213.433390646791,30.3713203435596)) ;
#76909 = CARTESIAN_POINT('Ctrl Pts',(69.3050219266113,213.343266910648,30.3713203435596)) ;
#76910 = CARTESIAN_POINT('Ctrl Pts',(69.2113031834343,213.279382916547,30.3713203435596)) ;
#76911 = CARTESIAN_POINT('Ctrl Pts',(69.1391356985346,213.267896893205,30.3713203435596)) ;
#76912 = CARTESIAN_POINT('Ctrl Pts',(69.0988421032155,213.27180916519,30.3713203435596)) ;
#76913 = CARTESIAN_POINT('',(69.2413920554874,213.523097238281,30.2513203435596)) ;
#76914 = CARTESIAN_POINT('Origin',(69.360748483532,213.535508647726,30.2513203435596)) ;
#76915 = CARTESIAN_POINT('',(69.1104388653291,213.391247497013,30.2513203435596)) ;
#76916 = CARTESIAN_POINT('Ctrl Pts',(69.2413920554874,213.523097238281,30.2513203435596)) ;
#76917 = CARTESIAN_POINT('Ctrl Pts',(69.2434856838755,213.502963505109,30.2513203435596)) ;
#76918 = CARTESIAN_POINT('Ctrl Pts',(69.237232259097,213.461730274006,30.2513203435596)) ;
#76919 = CARTESIAN_POINT('Ctrl Pts',(69.1926794105975,213.403591641984,30.2513203435596)) ;
#76920 = CARTESIAN_POINT('Ctrl Pts',(69.1406601890908,213.388313183572,30.2513203435596)) ;
#76921 = CARTESIAN_POINT('Ctrl Pts',(69.1104388653291,213.391247497013,30.2513203435596)) ;
#76922 = CARTESIAN_POINT('Origin',(69.0988421032155,213.27180916519,30.2513203435596)) ;
#76923 = CARTESIAN_POINT('Origin',(69.1220356274428,213.510685828835,26.4913203435596)) ;
#76924 = CARTESIAN_POINT('',(69.1104388653291,213.391247497013,26.4913203435596)) ;
#76925 = CARTESIAN_POINT('',(69.1220356292711,213.51068582655,26.3713203435596)) ;
#76926 = CARTESIAN_POINT('Origin',(69.1220356274428,213.510685828835,26.4913203435596)) ;
#76927 = CARTESIAN_POINT('',(69.2403544421435,213.490669383401,26.4913203435596)) ;
#76928 = CARTESIAN_POINT('Origin',(69.1220356274428,213.510685828835,26.4913203435596)) ;
#76929 = CARTESIAN_POINT('',(69.2413920554874,213.523097238281,26.4913203435596)) ;
#76930 = CARTESIAN_POINT('Origin',(69.1220356274428,213.510685828835,26.4913203435596)) ;
#76931 = CARTESIAN_POINT('Origin',(69.1220356281404,213.510685822126,26.4913203435596)) ;
#76932 = CARTESIAN_POINT('Ctrl Pts',(69.2413920554874,213.523097238281,26.4913203435596)) ;
#76933 = CARTESIAN_POINT('Ctrl Pts',(69.2413920554874,213.523097238281,31.0033203435596)) ;
#76934 = CARTESIAN_POINT('Ctrl Pts',(69.2434856838755,213.502963505109,26.4913203435596)) ;
#76935 = CARTESIAN_POINT('Ctrl Pts',(69.2434856838755,213.502963505109,31.0033203435596)) ;
#76936 = CARTESIAN_POINT('Ctrl Pts',(69.237232259097,213.461730274006,26.4913203435596)) ;
#76937 = CARTESIAN_POINT('Ctrl Pts',(69.237232259097,213.461730274006,31.0033203435596)) ;
#76938 = CARTESIAN_POINT('Ctrl Pts',(69.1926794105975,213.403591641984,26.4913203435596)) ;
#76939 = CARTESIAN_POINT('Ctrl Pts',(69.1926794105975,213.403591641984,31.0033203435596)) ;
#76940 = CARTESIAN_POINT('Ctrl Pts',(69.1406601890908,213.388313183572,26.4913203435596)) ;
#76941 = CARTESIAN_POINT('Ctrl Pts',(69.1406601890908,213.388313183572,31.0033203435596)) ;
#76942 = CARTESIAN_POINT('Ctrl Pts',(69.1104388653291,213.391247497013,26.4913203435596)) ;
#76943 = CARTESIAN_POINT('Ctrl Pts',(69.1104388653291,213.391247497013,31.0033203435596)) ;
#76944 = CARTESIAN_POINT('',(69.2413920554874,213.523097238281,30.2513203435596)) ;
#76945 = CARTESIAN_POINT('',(69.1104388653291,213.391247497013,26.4913203435596)) ;
#76946 = CARTESIAN_POINT('Ctrl Pts',(69.1686691234544,219.464553538579,26.4913203435596)) ;
#76947 = CARTESIAN_POINT('Ctrl Pts',(69.075747399216,218.242094170941,26.4913203435596)) ;
#76948 = CARTESIAN_POINT('Ctrl Pts',(69.0471488167689,217.014745324447,26.4913203435596)) ;
#76949 = CARTESIAN_POINT('Ctrl Pts',(69.0872384835382,215.789690777862,26.4913203435596)) ;
#76950 = CARTESIAN_POINT('Ctrl Pts',(69.1686691234544,219.464553538579,26.4554164275186)) ;
#76951 = CARTESIAN_POINT('Ctrl Pts',(69.0757484199277,218.242107599218,26.4554164275186)) ;
#76952 = CARTESIAN_POINT('Ctrl Pts',(69.0471492860395,217.014730984541,26.4554164275186)) ;
#76953 = CARTESIAN_POINT('Ctrl Pts',(69.0872384835382,215.789690777862,26.4554164275186)) ;
#76954 = CARTESIAN_POINT('Ctrl Pts',(69.1385972482844,219.466839365467,26.3932840972059)) ;
#76955 = CARTESIAN_POINT('Ctrl Pts',(69.0455950200553,218.243320903646,26.3932840972059)) ;
#76956 = CARTESIAN_POINT('Ctrl Pts',(69.0169693155449,217.014889912194,26.3932840972059)) ;
#76957 = CARTESIAN_POINT('Ctrl Pts',(69.0570959938923,215.788704370874,26.3932840972059)) ;
#76958 = CARTESIAN_POINT('Ctrl Pts',(69.0758647787493,219.471607793269,26.3713203435596)) ;
#76959 = CARTESIAN_POINT('Ctrl Pts',(68.9826951909212,218.245887582489,26.3713203435596)) ;
#76960 = CARTESIAN_POINT('Ctrl Pts',(68.9540125949514,217.015183406856,26.3713203435596)) ;
#76961 = CARTESIAN_POINT('Ctrl Pts',(68.9942162166009,215.786646642648,26.3713203435596)) ;
#76962 = CARTESIAN_POINT('Ctrl Pts',(69.0490142989096,219.473648755078,26.3713203435596)) ;
#76963 = CARTESIAN_POINT('Ctrl Pts',(68.9557731873382,218.246987592431,26.3713203435596)) ;
#76964 = CARTESIAN_POINT('Ctrl Pts',(68.9270661821599,217.015307498826,26.3713203435596)) ;
#76965 = CARTESIAN_POINT('Ctrl Pts',(68.9673026867335,215.785765902728,26.3713203435596)) ;
#76966 = CARTESIAN_POINT('',(69.1686691234544,219.464553538579,26.4913203435596)) ;
#76967 = CARTESIAN_POINT('',(69.0490142989096,219.473648755078,26.3713203435596)) ;
#76968 = CARTESIAN_POINT('Origin',(69.0490142989096,219.473648755078,26.4913203435596)) ;
#76969 = CARTESIAN_POINT('',(68.9673026867972,215.785765900781,26.3713203435596)) ;
#76970 = CARTESIAN_POINT('Origin',(98.8235066990713,222.791430341492,26.3713203435596)) ;
#76971 = CARTESIAN_POINT('',(69.0872384836096,215.78969077568,26.4913203435596)) ;
#76972 = CARTESIAN_POINT('Origin',(68.9673026867335,215.785765902728,26.4913203435596)) ;
#76973 = CARTESIAN_POINT('Origin',(98.5678225429277,222.744057364665,26.4913203435596)) ;
#76974 = CARTESIAN_POINT('Ctrl Pts',(69.087238483681,215.789690773497,26.4913203435596)) ;
#76975 = CARTESIAN_POINT('Ctrl Pts',(69.1120141497305,215.032599366639,26.4913203435596)) ;
#76976 = CARTESIAN_POINT('Ctrl Pts',(69.1630580206422,214.276409794352,26.4913203435596)) ;
#76977 = CARTESIAN_POINT('Ctrl Pts',(69.2413920561824,213.523097231597,26.4913203435596)) ;
#76978 = CARTESIAN_POINT('Ctrl Pts',(69.087238483681,215.789690773497,26.4554164275186)) ;
#76979 = CARTESIAN_POINT('Ctrl Pts',(69.1120138597183,215.032608228791,26.4554164275186)) ;
#76980 = CARTESIAN_POINT('Ctrl Pts',(69.163058978161,214.27640058621,26.4554164275186)) ;
#76981 = CARTESIAN_POINT('Ctrl Pts',(69.2413920561824,213.523097231597,26.4554164275186)) ;
#76982 = CARTESIAN_POINT('Ctrl Pts',(69.0570960390057,215.788704367977,26.3932840432188)) ;
#76983 = CARTESIAN_POINT('Ctrl Pts',(69.0818945784431,215.030913999266,26.3932840432188)) ;
#76984 = CARTESIAN_POINT('Ctrl Pts',(69.1329856638633,214.274016790527,26.3932840432188)) ;
#76985 = CARTESIAN_POINT('Ctrl Pts',(69.211395219335,213.519977977518,26.3932840432188)) ;
#76986 = CARTESIAN_POINT('Ctrl Pts',(68.9942162167441,215.786646638271,26.3713203435596)) ;
#76987 = CARTESIAN_POINT('Ctrl Pts',(69.0190623076259,215.027403199043,26.3713203435596)) ;
#76988 = CARTESIAN_POINT('Ctrl Pts',(69.0702525942423,214.26901954923,26.3713203435596)) ;
#76989 = CARTESIAN_POINT('Ctrl Pts',(69.1488191479615,213.513470935898,26.3713203435596)) ;
#76990 = CARTESIAN_POINT('Ctrl Pts',(68.9673026868768,215.785765898347,26.3713203435596)) ;
#76991 = CARTESIAN_POINT('Ctrl Pts',(68.9921690996123,215.025901466698,26.3713203435596)) ;
#76992 = CARTESIAN_POINT('Ctrl Pts',(69.0434019787636,214.266879672249,26.3713203435596)) ;
#76993 = CARTESIAN_POINT('Ctrl Pts',(69.1220356281404,213.510685822126,26.3713203435596)) ;
#76994 = CARTESIAN_POINT('Origin',(97.1540654702609,222.393518409093,26.4913203435596)) ;
#76995 = CARTESIAN_POINT('Origin',(97.133994720273,222.390783272674,26.3713203435596)) ;
#76996 = CARTESIAN_POINT('Origin',(67.2629739196944,213.691189826592,26.4913203435596)) ;
#76997 = CARTESIAN_POINT('',(67.2513771575808,213.57175149477,26.4913203435596)) ;
#76998 = CARTESIAN_POINT('',(67.2629739196944,213.691189826592,26.3713203435596)) ;
#76999 = CARTESIAN_POINT('Origin',(69.2461649893318,213.257504976258,30.2513203435596)) ;
#77000 = CARTESIAN_POINT('',(69.2577617514454,213.37694330808,30.2513203435596)) ;
#77001 = CARTESIAN_POINT('Ctrl Pts',(69.1987989853619,219.837084335145,30.2513203435596)) ;
#77002 = CARTESIAN_POINT('Ctrl Pts',(69.195605783884,219.798820218195,30.2513203435596)) ;
#77003 = CARTESIAN_POINT('Ctrl Pts',(69.1924125824061,219.760556101245,30.2513203435596)) ;
#77004 = CARTESIAN_POINT('Ctrl Pts',(69.1892193809281,219.722291984294,30.2513203435596)) ;
#77005 = CARTESIAN_POINT('Ctrl Pts',(69.1820520081344,219.636405392827,30.2513203435596)) ;
#77006 = CARTESIAN_POINT('Ctrl Pts',(69.1752014751529,219.550491833333,30.2513203435596)) ;
#77007 = CARTESIAN_POINT('Ctrl Pts',(69.1686691234544,219.464553538581,30.2513203435596)) ;
#77008 = CARTESIAN_POINT('Ctrl Pts',(69.1987989853619,219.837084335145,30.2872242596007)) ;
#77009 = CARTESIAN_POINT('Ctrl Pts',(69.195605783884,219.798820218195,30.2872242596007)) ;
#77010 = CARTESIAN_POINT('Ctrl Pts',(69.1924125824061,219.760556101245,30.2872242596007)) ;
#77011 = CARTESIAN_POINT('Ctrl Pts',(69.1892193809281,219.722291984294,30.2872242596007)) ;
#77012 = CARTESIAN_POINT('Ctrl Pts',(69.1820520081344,219.636405392827,30.2872242596007)) ;
#77013 = CARTESIAN_POINT('Ctrl Pts',(69.1752014751529,219.550491833333,30.2872242596007)) ;
#77014 = CARTESIAN_POINT('Ctrl Pts',(69.1686691234544,219.464553538581,30.2872242596007)) ;
#77015 = CARTESIAN_POINT('Ctrl Pts',(69.2288531922854,219.834576263729,30.3493565283418)) ;
#77016 = CARTESIAN_POINT('Ctrl Pts',(69.2256599908075,219.796312146779,30.3493565283418)) ;
#77017 = CARTESIAN_POINT('Ctrl Pts',(69.2224667893296,219.758048029829,30.3493565283418)) ;
#77018 = CARTESIAN_POINT('Ctrl Pts',(69.2192735878516,219.719783912879,30.3493565283418)) ;
#77019 = CARTESIAN_POINT('Ctrl Pts',(69.2121123842297,219.633971246513,30.3493565283418)) ;
#77020 = CARTESIAN_POINT('Ctrl Pts',(69.205267758613,219.548131765938,30.3493565283418)) ;
#77021 = CARTESIAN_POINT('Ctrl Pts',(69.1987410497925,219.462267707803,30.3493565283417)) ;
#77022 = CARTESIAN_POINT('Ctrl Pts',(69.2915486465511,219.829344228257,30.3713203435596)) ;
#77023 = CARTESIAN_POINT('Ctrl Pts',(69.2883554450732,219.791080111306,30.3713203435596)) ;
#77024 = CARTESIAN_POINT('Ctrl Pts',(69.2851622435952,219.752815994356,30.3713203435596)) ;
#77025 = CARTESIAN_POINT('Ctrl Pts',(69.2819690421173,219.714551877406,30.3713203435596)) ;
#77026 = CARTESIAN_POINT('Ctrl Pts',(69.2748207078644,219.628893424645,30.3713203435596)) ;
#77027 = CARTESIAN_POINT('Ctrl Pts',(69.2679884054781,219.543208478558,30.3713203435596)) ;
#77028 = CARTESIAN_POINT('Ctrl Pts',(69.2614734681595,219.457499283891,30.3713203435596)) ;
#77029 = CARTESIAN_POINT('Ctrl Pts',(69.3183833051634,219.827104833273,30.3713203435596)) ;
#77030 = CARTESIAN_POINT('Ctrl Pts',(69.3151901036855,219.788840716323,30.3713203435596)) ;
#77031 = CARTESIAN_POINT('Ctrl Pts',(69.3119969022076,219.750576599373,30.3713203435596)) ;
#77032 = CARTESIAN_POINT('Ctrl Pts',(69.3088037007297,219.712312482423,30.3713203435596)) ;
#77033 = CARTESIAN_POINT('Ctrl Pts',(69.3016608747709,219.626720035554,30.3713203435596)) ;
#77034 = CARTESIAN_POINT('Ctrl Pts',(69.2948338469246,219.541101232703,30.3713203435596)) ;
#77035 = CARTESIAN_POINT('Ctrl Pts',(69.2883239479992,219.455458322081,30.3713203435596)) ;
#77036 = CARTESIAN_POINT('',(69.1892193814451,219.72229198423,30.2513203435596)) ;
#77037 = CARTESIAN_POINT('',(69.1686691234544,219.46455353858,30.2513203435596)) ;
#77038 = CARTESIAN_POINT('Origin',(98.9345171832154,222.024247258091,30.2513203435596)) ;
#77039 = CARTESIAN_POINT('Origin',(69.2883239479992,219.455458322081,30.2513203435596)) ;
#77040 = CARTESIAN_POINT('Ctrl Pts',(69.3183833051634,219.827104833273,30.3713203435596)) ;
#77041 = CARTESIAN_POINT('Ctrl Pts',(69.318101580658,219.826871585683,30.3713203435596)) ;
#77042 = CARTESIAN_POINT('Ctrl Pts',(69.3178198111958,219.826638390472,30.3713194568659)) ;
#77043 = CARTESIAN_POINT('Ctrl Pts',(69.3028143009312,219.814224398279,30.3712250783813)) ;
#77044 = CARTESIAN_POINT('Ctrl Pts',(69.2878306017834,219.802081997314,30.3687143086752)) ;
#77045 = CARTESIAN_POINT('Ctrl Pts',(69.2597178898201,219.779423852337,30.3590473904662)) ;
#77046 = CARTESIAN_POINT('Ctrl Pts',(69.2461518879997,219.768543441465,30.3519487591578)) ;
#77047 = CARTESIAN_POINT('Ctrl Pts',(69.2217945704143,219.748610301608,30.3322980192289)) ;
#77048 = CARTESIAN_POINT('Ctrl Pts',(69.2115959028757,219.740182294065,30.3201725243576)) ;
#77049 = CARTESIAN_POINT('Ctrl Pts',(69.1994121293716,219.730311833466,30.2983574623926)) ;
#77050 = CARTESIAN_POINT('Ctrl Pts',(69.1956759077495,219.727331200005,30.2894514633275)) ;
#77051 = CARTESIAN_POINT('Ctrl Pts',(69.1905841803268,219.723326414298,30.2707124141225)) ;
#77052 = CARTESIAN_POINT('Ctrl Pts',(69.1892193809281,219.722291984294,30.2610938408263)) ;
#77053 = CARTESIAN_POINT('Ctrl Pts',(69.1892193809281,219.722291984294,30.2513203435596)) ;
#77054 = CARTESIAN_POINT('Ctrl Pts',(69.1686691234544,219.464553538579,30.2513203435596)) ;
#77055 = CARTESIAN_POINT('Ctrl Pts',(69.075767060595,218.242352832058,30.2513203435596)) ;
#77056 = CARTESIAN_POINT('Ctrl Pts',(69.0471392129121,217.015038797788,30.2513203435596)) ;
#77057 = CARTESIAN_POINT('Ctrl Pts',(69.0872384835382,215.789690777862,30.2513203435596)) ;
#77058 = CARTESIAN_POINT('Ctrl Pts',(69.1686691234544,219.464553538579,30.2872242596007)) ;
#77059 = CARTESIAN_POINT('Ctrl Pts',(69.0757660400992,218.242339406623,30.2872242596007)) ;
#77060 = CARTESIAN_POINT('Ctrl Pts',(69.0471387435291,217.015053141129,30.2872242596007)) ;
#77061 = CARTESIAN_POINT('Ctrl Pts',(69.0872384835382,215.789690777862,30.2872242596007)) ;
#77062 = CARTESIAN_POINT('Ctrl Pts',(69.1987410451693,219.462267708153,30.3493565339049)) ;
#77063 = CARTESIAN_POINT('Ctrl Pts',(69.1059194692668,218.241125871721,30.3493565339049)) ;
#77064 = CARTESIAN_POINT('Ctrl Pts',(69.0773187696569,217.014893940627,30.3493565339049)) ;
#77065 = CARTESIAN_POINT('Ctrl Pts',(69.1173810198383,215.790677186376,30.3493565339049)) ;
#77066 = CARTESIAN_POINT('Ctrl Pts',(69.2614734681594,219.45749928389,30.3713203435596)) ;
#77067 = CARTESIAN_POINT('Ctrl Pts',(69.1688192164441,218.238558730547,30.3713203435596)) ;
#77068 = CARTESIAN_POINT('Ctrl Pts',(69.1402754620286,217.01459988118,30.3713203435596)) ;
#77069 = CARTESIAN_POINT('Ctrl Pts',(69.1802607504755,215.792734913075,30.3713203435596)) ;
#77070 = CARTESIAN_POINT('Ctrl Pts',(69.2883239479991,219.45545832208,30.3713203435596)) ;
#77071 = CARTESIAN_POINT('Ctrl Pts',(69.1957412048934,218.237458521508,30.3713203435596)) ;
#77072 = CARTESIAN_POINT('Ctrl Pts',(69.1672218826975,217.014475548494,30.3713203435596)) ;
#77073 = CARTESIAN_POINT('Ctrl Pts',(69.2071742803429,215.793615652996,30.3713203435596)) ;
#77074 = CARTESIAN_POINT('',(69.0872384836096,215.78969077568,30.2513203435596)) ;
#77075 = CARTESIAN_POINT('Origin',(69.2071742803429,215.793615652996,30.2513203435596)) ;
#77076 = CARTESIAN_POINT('Origin',(99.1895632998921,222.852119685147,30.2513203435596)) ;
#77077 = CARTESIAN_POINT('Ctrl Pts',(69.087238483681,215.789690773497,30.2513203435596)) ;
#77078 = CARTESIAN_POINT('Ctrl Pts',(69.1120101109511,215.032722783106,30.2513203435596)) ;
#77079 = CARTESIAN_POINT('Ctrl Pts',(69.1630453951407,214.2765312112,30.2513203435596)) ;
#77080 = CARTESIAN_POINT('Ctrl Pts',(69.2413920554874,213.523097238281,30.2513203435596)) ;
#77081 = CARTESIAN_POINT('Ctrl Pts',(69.087238483681,215.789690773497,30.2872242596007)) ;
#77082 = CARTESIAN_POINT('Ctrl Pts',(69.112010400916,215.032713922399,30.2872242596007)) ;
#77083 = CARTESIAN_POINT('Ctrl Pts',(69.1630444374676,214.276540420826,30.2872242596007)) ;
#77084 = CARTESIAN_POINT('Ctrl Pts',(69.2413920554874,213.523097238281,30.2872242596007)) ;
#77085 = CARTESIAN_POINT('Ctrl Pts',(69.1173809762543,215.790677180585,30.3493565863989)) ;
#77086 = CARTESIAN_POINT('Ctrl Pts',(69.1421297338651,215.034408038106,30.3493565863989)) ;
#77087 = CARTESIAN_POINT('Ctrl Pts',(69.1931178117582,214.278924102927,30.3493565863989)) ;
#77088 = CARTESIAN_POINT('Ctrl Pts',(69.2713889400021,213.526216497309,30.3493565863989)) ;
#77089 = CARTESIAN_POINT('Ctrl Pts',(69.1802607506179,215.792734908723,30.3713203435596)) ;
#77090 = CARTESIAN_POINT('Ctrl Pts',(69.204961964536,215.037918599891,30.3713203435596)) ;
#77091 = CARTESIAN_POINT('Ctrl Pts',(69.2558508590168,214.283921095922,30.3713203435596)) ;
#77092 = CARTESIAN_POINT('Ctrl Pts',(69.3339649637103,213.532723533959,30.3713203435596)) ;
#77093 = CARTESIAN_POINT('Ctrl Pts',(69.2071742804852,215.793615648647,30.3713203435596)) ;
#77094 = CARTESIAN_POINT('Ctrl Pts',(69.2318551758623,215.039420231006,30.3713203435596)) ;
#77095 = CARTESIAN_POINT('Ctrl Pts',(69.2827014853096,214.286060868906,30.3713203435596)) ;
#77096 = CARTESIAN_POINT('Ctrl Pts',(69.360748483532,213.535508647726,30.3713203435596)) ;
#77097 = CARTESIAN_POINT('Origin',(97.219772055596,222.411726694737,30.2513203435596)) ;
#77098 = CARTESIAN_POINT('Ctrl Pts',(62.0380714133749,214.162478201405,26.4913203435596)) ;
#77099 = CARTESIAN_POINT('Ctrl Pts',(62.0151252295802,214.27196151861,26.4913203435596)) ;
#77100 = CARTESIAN_POINT('Ctrl Pts',(61.9925614772325,214.381523697747,26.4913203435596)) ;
#77101 = CARTESIAN_POINT('Ctrl Pts',(61.9703773266184,214.491161471123,26.4913203435596)) ;
#77102 = CARTESIAN_POINT('Ctrl Pts',(62.0380714133749,214.162478201405,26.4554164275186)) ;
#77103 = CARTESIAN_POINT('Ctrl Pts',(62.0151250465041,214.271962392122,26.4554164275186)) ;
#77104 = CARTESIAN_POINT('Ctrl Pts',(61.9925616526852,214.381522830631,26.4554164275186)) ;
#77105 = CARTESIAN_POINT('Ctrl Pts',(61.9703773266184,214.491161471123,26.4554164275186)) ;
#77106 = CARTESIAN_POINT('Ctrl Pts',(62.0675885660411,214.168664586943,26.3932839179096)) ;
#77107 = CARTESIAN_POINT('Ctrl Pts',(62.0446568215384,214.278079009834,26.3932839179096)) ;
#77108 = CARTESIAN_POINT('Ctrl Pts',(62.0221070790419,214.387573156395,26.3932839179096)) ;
#77109 = CARTESIAN_POINT('Ctrl Pts',(61.999936766457,214.497142539921,26.3932839179096)) ;
#77110 = CARTESIAN_POINT('Ctrl Pts',(62.129164288968,214.181570003874,26.3713203435596)) ;
#77111 = CARTESIAN_POINT('Ctrl Pts',(62.1062625622829,214.290841202503,26.3713203435596)) ;
#77112 = CARTESIAN_POINT('Ctrl Pts',(62.0837422493721,214.400192437673,26.3713203435596)) ;
#77113 = CARTESIAN_POINT('Ctrl Pts',(62.061600704641,214.509619645667,26.3713203435596)) ;
#77114 = CARTESIAN_POINT('Ctrl Pts',(62.155519600537,214.1870937114,26.3713203435596)) ;
#77115 = CARTESIAN_POINT('Ctrl Pts',(62.1326307024359,214.2963037009,26.3713203435596)) ;
#77116 = CARTESIAN_POINT('Ctrl Pts',(62.1101230239711,214.405593582675,26.3713203435596)) ;
#77117 = CARTESIAN_POINT('Ctrl Pts',(62.0879937736325,214.51496002973,26.3713203435596)) ;
#77118 = CARTESIAN_POINT('',(62.0879937736325,214.51496002973,26.3713203435596)) ;
#77119 = CARTESIAN_POINT('Origin',(158.549722376545,280.559557010502,26.3713203435596)) ;
#77120 = CARTESIAN_POINT('',(61.9703773266191,214.491161471119,26.4913203435596)) ;
#77121 = CARTESIAN_POINT('Origin',(62.0879937736325,214.51496002973,26.4913203435596)) ;
#77122 = CARTESIAN_POINT('Origin',(168.040182093702,286.993621933611,26.4913203435596)) ;
#77123 = CARTESIAN_POINT('Ctrl Pts',(61.9703773266184,214.491161471123,26.4913203435596)) ;
#77124 = CARTESIAN_POINT('Ctrl Pts',(61.8515958146182,215.078199520065,26.4913203435596)) ;
#77125 = CARTESIAN_POINT('Ctrl Pts',(61.7916108526749,215.677118713722,26.4913203435596)) ;
#77126 = CARTESIAN_POINT('Ctrl Pts',(61.7916108526749,216.276053366666,26.4913203435596)) ;
#77127 = CARTESIAN_POINT('Ctrl Pts',(61.9703773266184,214.491161471123,26.4554164275186)) ;
#77128 = CARTESIAN_POINT('Ctrl Pts',(61.8515907531908,215.078224534483,26.4554164275186)) ;
#77129 = CARTESIAN_POINT('Ctrl Pts',(61.7916108526749,215.677093192374,26.4554164275186)) ;
#77130 = CARTESIAN_POINT('Ctrl Pts',(61.7916108526749,216.276053366666,26.4554164275186)) ;
#77131 = CARTESIAN_POINT('Ctrl Pts',(61.9999367861991,214.497142543916,26.3932839420772)) ;
#77132 = CARTESIAN_POINT('Ctrl Pts',(61.8815544712344,215.082207694509,26.3932839420772)) ;
#77133 = CARTESIAN_POINT('Ctrl Pts',(61.8217693486993,215.67913159379,26.3932839420772)) ;
#77134 = CARTESIAN_POINT('Ctrl Pts',(61.8217693486993,216.276053366666,26.3932839420772)) ;
#77135 = CARTESIAN_POINT('Ctrl Pts',(62.061600704641,214.509619645667,26.3713203435596)) ;
#77136 = CARTESIAN_POINT('Ctrl Pts',(61.9440482796633,215.090583341491,26.3713203435596)) ;
#77137 = CARTESIAN_POINT('Ctrl Pts',(61.8846829156441,215.68331616648,26.3713203435596)) ;
#77138 = CARTESIAN_POINT('Ctrl Pts',(61.8846829156441,216.276053366667,26.3713203435596)) ;
#77139 = CARTESIAN_POINT('Ctrl Pts',(62.0879937736325,214.51496002973,26.3713203435596)) ;
#77140 = CARTESIAN_POINT('Ctrl Pts',(61.9707960151257,215.094170904685,26.3713203435596)) ;
#77141 = CARTESIAN_POINT('Ctrl Pts',(61.9116108526749,215.685104509095,26.3713203435596)) ;
#77142 = CARTESIAN_POINT('Ctrl Pts',(61.9116108526749,216.276053366667,26.3713203435596)) ;
#77143 = CARTESIAN_POINT('',(61.9116108526749,216.276053366667,26.3713203435596)) ;
#77144 = CARTESIAN_POINT('',(61.7916108526749,216.276053366666,26.4913203435596)) ;
#77145 = CARTESIAN_POINT('Origin',(61.9116108526749,216.276053366667,26.4913203435596)) ;
#77146 = CARTESIAN_POINT('Origin',(70.7990562975695,216.276799067812,26.4913203435596)) ;
#77147 = CARTESIAN_POINT('Origin',(70.798957024977,216.27678912513,26.3713203435596)) ;
#77148 = CARTESIAN_POINT('Origin',(61.9116108526749,216.02810186684,26.4913203435596)) ;
#77149 = CARTESIAN_POINT('',(61.7916108526749,217.432246240363,26.4913203435596)) ;
#77150 = CARTESIAN_POINT('',(61.9116108526749,217.332165092393,26.3713203435596)) ;
#77151 = CARTESIAN_POINT('Ctrl Pts',(61.7916108526749,217.432246240364,26.4913203435596)) ;
#77152 = CARTESIAN_POINT('Ctrl Pts',(61.7916108526749,217.432246240364,26.4763546071157)) ;
#77153 = CARTESIAN_POINT('Ctrl Pts',(61.7945994481497,217.429633269658,26.4608211829996)) ;
#77154 = CARTESIAN_POINT('Ctrl Pts',(61.8056861138382,217.420035117846,26.4329402504268)) ;
#77155 = CARTESIAN_POINT('Ctrl Pts',(61.8137971189369,217.413045531713,26.420599403965)) ;
#77156 = CARTESIAN_POINT('Ctrl Pts',(61.8340451542424,217.395799093869,26.3981511688094)) ;
#77157 = CARTESIAN_POINT('Ctrl Pts',(61.8484542267829,217.383662220691,26.3878996607103)) ;
#77158 = CARTESIAN_POINT('Ctrl Pts',(61.879478171071,217.358033658104,26.3744685762533)) ;
#77159 = CARTESIAN_POINT('Ctrl Pts',(61.8961032700049,217.344537933513,26.3713203435596)) ;
#77160 = CARTESIAN_POINT('Ctrl Pts',(61.9116108526749,217.332165092393,26.3713203435596)) ;
#77161 = CARTESIAN_POINT('',(61.7916108526749,216.02810186684,26.4913203435596)) ;
#77162 = CARTESIAN_POINT('',(61.9116108526749,216.02810186684,26.3713203435596)) ;
#77163 = CARTESIAN_POINT('Origin',(68.8498979833486,219.885565182264,30.2513203435596)) ;
#77164 = CARTESIAN_POINT('',(68.8350389209693,219.766488701525,30.2513203435596)) ;
#77165 = CARTESIAN_POINT('Ctrl Pts',(62.0380714133749,214.162478201405,30.2513203435596)) ;
#77166 = CARTESIAN_POINT('Ctrl Pts',(62.0151257340927,214.271959111425,30.2513203435596)) ;
#77167 = CARTESIAN_POINT('Ctrl Pts',(61.9925619554488,214.381521334322,30.2513203435596)) ;
#77168 = CARTESIAN_POINT('Ctrl Pts',(61.9703773266184,214.491161471123,30.2513203435596)) ;
#77169 = CARTESIAN_POINT('Ctrl Pts',(62.0380714133749,214.162478201405,30.2872242596007)) ;
#77170 = CARTESIAN_POINT('Ctrl Pts',(62.0151259171648,214.271958237932,30.2872242596007)) ;
#77171 = CARTESIAN_POINT('Ctrl Pts',(61.9925617799923,214.381522201457,30.2872242596007)) ;
#77172 = CARTESIAN_POINT('Ctrl Pts',(61.9703773266184,214.491161471123,30.2872242596007)) ;
#77173 = CARTESIAN_POINT('Ctrl Pts',(62.0085542139792,214.156291806073,30.3493567119227)) ;
#77174 = CARTESIAN_POINT('Ctrl Pts',(61.9855940957225,214.265841608892,30.3493567119227)) ;
#77175 = CARTESIAN_POINT('Ctrl Pts',(61.9630163071413,214.375471864732,30.3493567119227)) ;
#77176 = CARTESIAN_POINT('Ctrl Pts',(61.9408178399833,214.485180392856,30.3493567119227)) ;
#77177 = CARTESIAN_POINT('Ctrl Pts',(61.9469785377818,214.143386398936,30.3713203435596)) ;
#77178 = CARTESIAN_POINT('Ctrl Pts',(61.9239884023675,214.253079422868,30.3713203435596)) ;
#77179 = CARTESIAN_POINT('Ctrl Pts',(61.9013811842277,214.362852589857,30.3713203435596)) ;
#77180 = CARTESIAN_POINT('Ctrl Pts',(61.8791539485958,214.472703296579,30.3713203435596)) ;
#77181 = CARTESIAN_POINT('Ctrl Pts',(61.9206232262128,214.13786269141,30.3713203435596)) ;
#77182 = CARTESIAN_POINT('Ctrl Pts',(61.8976202624965,214.247616923126,30.3713203435596)) ;
#77183 = CARTESIAN_POINT('Ctrl Pts',(61.8750004098937,214.357451443545,30.3713203435596)) ;
#77184 = CARTESIAN_POINT('Ctrl Pts',(61.8527608796043,214.467362912516,30.3713203435596)) ;
#77185 = CARTESIAN_POINT('',(61.9703773266191,214.491161471119,30.2513203435596)) ;
#77186 = CARTESIAN_POINT('Origin',(149.370337688321,274.199128996313,30.2513203435596)) ;
#77187 = CARTESIAN_POINT('Origin',(61.8527608796043,214.467362912516,30.2513203435596)) ;
#77188 = CARTESIAN_POINT('Ctrl Pts',(61.6716108526749,216.276053366666,30.3713203435596)) ;
#77189 = CARTESIAN_POINT('Ctrl Pts',(61.6716108526749,215.669132918349,30.3713203435596)) ;
#77190 = CARTESIAN_POINT('Ctrl Pts',(61.7323956141108,215.062228135443,30.3713203435596)) ;
#77191 = CARTESIAN_POINT('Ctrl Pts',(61.8527608796043,214.467362912515,30.3713203435596)) ;
#77192 = CARTESIAN_POINT('Ctrl Pts',(61.7075147687159,216.276053366666,30.3713203435596)) ;
#77193 = CARTESIAN_POINT('Ctrl Pts',(61.7075147687159,215.671532615249,30.3713203435596)) ;
#77194 = CARTESIAN_POINT('Ctrl Pts',(61.7680622838269,215.066996615668,30.3713203435596)) ;
#77195 = CARTESIAN_POINT('Ctrl Pts',(61.8879516382597,214.4744834246,30.3713203435596)) ;
#77196 = CARTESIAN_POINT('Ctrl Pts',(61.7696471970384,216.276053366666,30.3411617999306)) ;
#77197 = CARTESIAN_POINT('Ctrl Pts',(61.7696471970384,215.6756545881,30.3411617999306)) ;
#77198 = CARTESIAN_POINT('Ctrl Pts',(61.8297780544614,215.075278702629,30.3411617999306)) ;
#77199 = CARTESIAN_POINT('Ctrl Pts',(61.9488499337901,214.486805609907,30.3411617999306)) ;
#77200 = CARTESIAN_POINT('Ctrl Pts',(61.7916108526749,216.276053366666,30.2782482805904)) ;
#77201 = CARTESIAN_POINT('Ctrl Pts',(61.7916108526749,215.677125204134,30.2782482805904)) ;
#77202 = CARTESIAN_POINT('Ctrl Pts',(61.8515971018053,215.078193158571,30.2782482805904)) ;
#77203 = CARTESIAN_POINT('Ctrl Pts',(61.9703773266184,214.491161471123,30.2782482805904)) ;
#77204 = CARTESIAN_POINT('Ctrl Pts',(61.7916108526749,216.276053366666,30.2513203435596)) ;
#77205 = CARTESIAN_POINT('Ctrl Pts',(61.7916108526749,215.677118713722,30.2513203435596)) ;
#77206 = CARTESIAN_POINT('Ctrl Pts',(61.8515958146183,215.078199520064,30.2513203435596)) ;
#77207 = CARTESIAN_POINT('Ctrl Pts',(61.9703773266184,214.491161471123,30.2513203435596)) ;
#77208 = CARTESIAN_POINT('',(61.7916108526749,216.276053366666,30.2513203435596)) ;
#77209 = CARTESIAN_POINT('Origin',(70.7990562975712,216.276799067812,30.2513203435596)) ;
#77210 = CARTESIAN_POINT('Origin',(61.6716108526749,216.276053366666,30.2513203435596)) ;
#77211 = CARTESIAN_POINT('Origin',(61.6716108526749,216.520093569003,30.2513203435596)) ;
#77212 = CARTESIAN_POINT('',(61.7916108526749,216.520093569003,30.2513203435596)) ;
#77213 = CARTESIAN_POINT('Ctrl Pts',(69.0490142989097,219.47364875508,26.3713203435596)) ;
#77214 = CARTESIAN_POINT('Ctrl Pts',(69.0516144229285,219.507855459592,26.3713203435596)) ;
#77215 = CARTESIAN_POINT('Ctrl Pts',(69.0542647955834,219.542058391199,26.3713203435596)) ;
#77216 = CARTESIAN_POINT('Ctrl Pts',(69.0569653274897,219.576257334544,26.3713203435596)) ;
#77217 = CARTESIAN_POINT('Ctrl Pts',(69.084814938696,219.470927472667,26.3713203435596)) ;
#77218 = CARTESIAN_POINT('Ctrl Pts',(69.0874123863672,219.505098967692,26.3713203435596)) ;
#77219 = CARTESIAN_POINT('Ctrl Pts',(69.0900600681774,219.539267174567,26.3713203435596)) ;
#77220 = CARTESIAN_POINT('Ctrl Pts',(69.0927578243876,219.573430967106,26.3713203435596)) ;
#77221 = CARTESIAN_POINT('Ctrl Pts',(69.1467685461534,219.46621824782,26.4014789701773)) ;
#77222 = CARTESIAN_POINT('Ctrl Pts',(69.1493613966472,219.500329263312,26.4014789701773)) ;
#77223 = CARTESIAN_POINT('Ctrl Pts',(69.1520043520586,219.53443647706,26.4014789701773)) ;
#77224 = CARTESIAN_POINT('Ctrl Pts',(69.1546973404401,219.568539890862,26.4014789701773)) ;
#77225 = CARTESIAN_POINT('Ctrl Pts',(69.1686691234544,219.464553538581,26.4643924065289)) ;
#77226 = CARTESIAN_POINT('Ctrl Pts',(69.1712603337912,219.498642976499,26.4643924065289)) ;
#77227 = CARTESIAN_POINT('Ctrl Pts',(69.1739016490944,219.53272902503,26.4643924065289)) ;
#77228 = CARTESIAN_POINT('Ctrl Pts',(69.1765929364347,219.566810897221,26.4643924065289)) ;
#77229 = CARTESIAN_POINT('Ctrl Pts',(69.1686691234544,219.464553538581,26.4913203435596)) ;
#77230 = CARTESIAN_POINT('Ctrl Pts',(69.1712603410299,219.49864307173,26.4913203435596)) ;
#77231 = CARTESIAN_POINT('Ctrl Pts',(69.173901641587,219.532728929959,26.4913203435596)) ;
#77232 = CARTESIAN_POINT('Ctrl Pts',(69.1765929364347,219.566810897221,26.4913203435596)) ;
#77233 = CARTESIAN_POINT('',(69.05696532749,219.576257334543,26.3713203435596)) ;
#77234 = CARTESIAN_POINT('Ctrl Pts',(69.1686691234543,219.464553538579,26.4913203435596)) ;
#77235 = CARTESIAN_POINT('Ctrl Pts',(69.1686691234543,219.464553538579,26.4825755545765)) ;
#77236 = CARTESIAN_POINT('Ctrl Pts',(69.1677442553345,219.465478406699,26.4739056649623)) ;
#77237 = CARTESIAN_POINT('Ctrl Pts',(69.1637138918045,219.469508770229,26.4544411500671)) ;
#77238 = CARTESIAN_POINT('Ctrl Pts',(69.1600464491366,219.473176212897,26.4440224457763)) ;
#77239 = CARTESIAN_POINT('Ctrl Pts',(69.1487510229112,219.484471639122,26.4213114813416)) ;
#77240 = CARTESIAN_POINT('Ctrl Pts',(69.1403360239462,219.492886638031,26.4103700658404)) ;
#77241 = CARTESIAN_POINT('Ctrl Pts',(69.1203185307192,219.512904131258,26.3916682055822)) ;
#77242 = CARTESIAN_POINT('Ctrl Pts',(69.1085784082693,219.524644253764,26.3843267857594)) ;
#77243 = CARTESIAN_POINT('Ctrl Pts',(69.0837605938726,219.549462068161,26.37407374451)) ;
#77244 = CARTESIAN_POINT('Ctrl Pts',(69.0702970781629,219.562925583871,26.3713203435597)) ;
#77245 = CARTESIAN_POINT('Ctrl Pts',(69.0569653274903,219.576257334543,26.3713203435596)) ;
#77246 = CARTESIAN_POINT('Origin',(88.0257792156962,221.138894496662,26.3713203435596)) ;
#77247 = CARTESIAN_POINT('Origin',(65.5243724680055,216.635300802115,26.3713203435596)) ;
#77248 = CARTESIAN_POINT('',(68.8712529610467,219.761969700987,26.3713203435596)) ;
#77249 = CARTESIAN_POINT('',(70.8292893218811,217.803933340152,26.3713203435596)) ;
#77250 = CARTESIAN_POINT('',(67.7485452644419,219.902067758924,26.3713203435596)) ;
#77251 = CARTESIAN_POINT('',(66.8542082278115,220.013668385118,26.3713203435596)) ;
#77252 = CARTESIAN_POINT('Origin',(64.1568347953872,220.146231446812,26.3713203435596)) ;
#77253 = CARTESIAN_POINT('Ctrl Pts',(69.087238483681,215.789690773497,23.8713203435596)) ;
#77254 = CARTESIAN_POINT('Ctrl Pts',(69.087238483681,215.789690773497,31.6713203435596)) ;
#77255 = CARTESIAN_POINT('Ctrl Pts',(69.1136171491181,214.983615131093,23.8713203435596)) ;
#77256 = CARTESIAN_POINT('Ctrl Pts',(69.1136171491181,214.983615131093,31.6713203435596)) ;
#77257 = CARTESIAN_POINT('Ctrl Pts',(69.1697039478106,214.179248099427,23.8713203435596)) ;
#77258 = CARTESIAN_POINT('Ctrl Pts',(69.1697039478106,214.179248099427,31.6713203435596)) ;
#77259 = CARTESIAN_POINT('Ctrl Pts',(69.2569276623894,213.37702429324,23.8713203435596)) ;
#77260 = CARTESIAN_POINT('Ctrl Pts',(69.2569276623894,213.37702429324,31.6713203435596)) ;
#77261 = CARTESIAN_POINT('',(69.087238483681,215.789690773497,23.8713203435596)) ;
#77262 = CARTESIAN_POINT('Ctrl Pts',(69.1686691234544,219.464553538579,23.8713203435596)) ;
#77263 = CARTESIAN_POINT('Ctrl Pts',(69.1686691234544,219.464553538579,31.6713203435596)) ;
#77264 = CARTESIAN_POINT('Ctrl Pts',(69.0753247917718,218.236534433073,23.8713203435596)) ;
#77265 = CARTESIAN_POINT('Ctrl Pts',(69.0753247917718,218.236534433073,31.6713203435596)) ;
#77266 = CARTESIAN_POINT('Ctrl Pts',(69.0472671147723,217.011130390261,23.8713203435596)) ;
#77267 = CARTESIAN_POINT('Ctrl Pts',(69.0472671147723,217.011130390261,31.6713203435596)) ;
#77268 = CARTESIAN_POINT('Ctrl Pts',(69.0872384835382,215.789690777862,23.8713203435596)) ;
#77269 = CARTESIAN_POINT('Ctrl Pts',(69.0872384835382,215.789690777862,31.6713203435596)) ;
#77270 = CARTESIAN_POINT('',(69.1686691234544,219.464553538579,23.8713203435596)) ;
#77271 = CARTESIAN_POINT('Origin',(104.054869375424,216.812621949209,23.8713203435596)) ;
#77272 = CARTESIAN_POINT('',(69.189219381737,219.722291984193,23.8713203435596)) ;
#77273 = CARTESIAN_POINT('',(69.1892193809281,219.722291984294,23.8713203435596)) ;
#77274 = CARTESIAN_POINT('',(69.1686691229769,219.464553539057,23.8713203435596)) ;
#77275 = CARTESIAN_POINT('Origin',(180.960510687652,228.725125033291,23.8713203435596)) ;
#77276 = CARTESIAN_POINT('',(69.1686691234544,219.464553538579,23.8713203435596)) ;
#77277 = CARTESIAN_POINT('Origin',(69.2569276623894,213.37702429324,23.8713203435596)) ;
#77278 = CARTESIAN_POINT('Ctrl Pts',(62.8216952668539,212.37422947071,23.3713203435596)) ;
#77279 = CARTESIAN_POINT('Ctrl Pts',(62.7643918956731,212.379793292255,23.3713203435596)) ;
#77280 = CARTESIAN_POINT('Ctrl Pts',(62.6452781621069,212.331202353327,23.3713203435596)) ;
#77281 = CARTESIAN_POINT('Ctrl Pts',(62.6156344352299,212.206021423155,23.3713203435596)) ;
#77282 = CARTESIAN_POINT('Ctrl Pts',(62.629967133072,212.150261166418,23.3713203435596)) ;
#77283 = CARTESIAN_POINT('Ctrl Pts',(62.8251650099645,212.409965336026,23.3713203435596)) ;
#77284 = CARTESIAN_POINT('Ctrl Pts',(62.7563820289917,212.416643760411,23.3713203435596)) ;
#77285 = CARTESIAN_POINT('Ctrl Pts',(62.6134890558422,212.358415343631,23.3713203435596)) ;
#77286 = CARTESIAN_POINT('Ctrl Pts',(62.5779896202957,212.208253658832,23.3713203435596)) ;
#77287 = CARTESIAN_POINT('Ctrl Pts',(62.5951935938603,212.141322925104,23.3713203435596)) ;
#77288 = CARTESIAN_POINT('Ctrl Pts',(62.8311694823153,212.471807094442,23.4014787656397)) ;
#77289 = CARTESIAN_POINT('Ctrl Pts',(62.7426679110788,212.480400078392,23.4014787656397)) ;
#77290 = CARTESIAN_POINT('Ctrl Pts',(62.5586840514308,212.405331040411,23.4014787656397)) ;
#77291 = CARTESIAN_POINT('Ctrl Pts',(62.5128811834681,212.211973412379,23.4014787656397)) ;
#77292 = CARTESIAN_POINT('Ctrl Pts',(62.5350171634802,212.125855087538,23.4014787656397)) ;
#77293 = CARTESIAN_POINT('Ctrl Pts',(62.8332920289675,212.493667802533,23.4643924065289)) ;
#77294 = CARTESIAN_POINT('Ctrl Pts',(62.7377553616651,212.502943853085,23.4643924065289)) ;
#77295 = CARTESIAN_POINT('Ctrl Pts',(62.539219886079,212.421993293736,23.4643924065289)) ;
#77296 = CARTESIAN_POINT('Ctrl Pts',(62.489849543713,212.21335126917,23.4643924065289)) ;
#77297 = CARTESIAN_POINT('Ctrl Pts',(62.513745139331,212.120387295379,23.4643924065289)) ;
#77298 = CARTESIAN_POINT('Ctrl Pts',(62.8332920289675,212.493667802533,23.4913203435596)) ;
#77299 = CARTESIAN_POINT('Ctrl Pts',(62.7377864103328,212.502940838441,23.4913203435596)) ;
#77300 = CARTESIAN_POINT('Ctrl Pts',(62.539263521056,212.421955940227,23.4913203435596)) ;
#77301 = CARTESIAN_POINT('Ctrl Pts',(62.4898573095942,212.213321056607,23.4913203435596)) ;
#77302 = CARTESIAN_POINT('Ctrl Pts',(62.513745139331,212.120387295379,23.4913203435596)) ;
#77303 = CARTESIAN_POINT('',(62.629967133072,212.150261166418,23.3713203435596)) ;
#77304 = CARTESIAN_POINT('Origin',(62.629967133072,212.150261166418,23.4913203435596)) ;
#77305 = CARTESIAN_POINT('',(62.8216952668539,212.37422947071,23.3713203435596)) ;
#77306 = CARTESIAN_POINT('Ctrl Pts',(62.629967133072,212.150261166418,23.3713203435596)) ;
#77307 = CARTESIAN_POINT('Ctrl Pts',(62.6156344352299,212.206021423155,23.3713203435596)) ;
#77308 = CARTESIAN_POINT('Ctrl Pts',(62.6452781621069,212.331202353327,23.3713203435596)) ;
#77309 = CARTESIAN_POINT('Ctrl Pts',(62.7643918956731,212.379793292255,23.3713203435596)) ;
#77310 = CARTESIAN_POINT('Ctrl Pts',(62.8216952668539,212.37422947071,23.3713203435596)) ;
#77311 = CARTESIAN_POINT('Origin',(62.8216952668539,212.37422947071,23.4913203435596)) ;
#77312 = CARTESIAN_POINT('Ctrl Pts',(66.5773376779735,202.200615492168,23.4913203435596)) ;
#77313 = CARTESIAN_POINT('Ctrl Pts',(64.7210140334605,205.27084597784,23.4913203435596)) ;
#77314 = CARTESIAN_POINT('Ctrl Pts',(63.4059506185125,208.649330615767,23.4913203435596)) ;
#77315 = CARTESIAN_POINT('Ctrl Pts',(62.513745139331,212.120387295379,23.4913203435596)) ;
#77316 = CARTESIAN_POINT('Ctrl Pts',(66.5773376779735,202.200615492168,23.4554164275186)) ;
#77317 = CARTESIAN_POINT('Ctrl Pts',(64.7209918030059,205.27088274547,23.4554164275186)) ;
#77318 = CARTESIAN_POINT('Ctrl Pts',(63.4059582099283,208.649301081949,23.4554164275186)) ;
#77319 = CARTESIAN_POINT('Ctrl Pts',(62.513745139331,212.120387295379,23.4554164275186)) ;
#77320 = CARTESIAN_POINT('Ctrl Pts',(66.6031455496054,202.216219454981,23.3932838428366)) ;
#77321 = CARTESIAN_POINT('Ctrl Pts',(64.748575230952,205.283550061356,23.3932838428366)) ;
#77322 = CARTESIAN_POINT('Ctrl Pts',(63.4345608045287,208.659167865758,23.3932838428366)) ;
#77323 = CARTESIAN_POINT('Ctrl Pts',(62.542954063693,212.127895199963,23.3932838428366)) ;
#77324 = CARTESIAN_POINT('Ctrl Pts',(66.6569835077658,202.24877097682,23.3713203435596)) ;
#77325 = CARTESIAN_POINT('Ctrl Pts',(64.8060581750343,205.310073029429,23.3713203435596)) ;
#77326 = CARTESIAN_POINT('Ctrl Pts',(63.4942490034471,208.679672623132,23.3713203435596)) ;
#77327 = CARTESIAN_POINT('Ctrl Pts',(62.6038869786632,212.143557485433,23.3713203435596)) ;
#77328 = CARTESIAN_POINT('Ctrl Pts',(66.6800269197305,202.262703491229,23.3713203435596)) ;
#77329 = CARTESIAN_POINT('Ctrl Pts',(64.8306593287648,205.32142914706,23.3713203435596)) ;
#77330 = CARTESIAN_POINT('Ctrl Pts',(63.5197972089754,208.688445810254,23.3713203435596)) ;
#77331 = CARTESIAN_POINT('Ctrl Pts',(62.629967133072,212.150261166418,23.3713203435596)) ;
#77332 = CARTESIAN_POINT('',(66.6800269197305,202.262703491229,23.3713203435596)) ;
#77333 = CARTESIAN_POINT('Origin',(66.6800269197305,202.262703491229,23.4913203435596)) ;
#77334 = CARTESIAN_POINT('Origin',(124.488490460381,267.59388982529,23.3713203435596)) ;
#77335 = CARTESIAN_POINT('Ctrl Pts',(66.6800269197305,202.262703491229,23.3713203435596)) ;
#77336 = CARTESIAN_POINT('Ctrl Pts',(66.7119076863592,202.209974915638,23.3713203435596)) ;
#77337 = CARTESIAN_POINT('Ctrl Pts',(66.772443528576,202.17583548982,23.3713203435596)) ;
#77338 = CARTESIAN_POINT('Ctrl Pts',(66.8340607823661,202.17583548982,23.3713203435596)) ;
#77339 = CARTESIAN_POINT('Ctrl Pts',(66.6493023704442,202.24412680535,23.3713203435596)) ;
#77340 = CARTESIAN_POINT('Ctrl Pts',(66.687569825207,202.1808350908,23.3713203435596)) ;
#77341 = CARTESIAN_POINT('Ctrl Pts',(66.7600997167655,202.139931573779,23.3713203435596)) ;
#77342 = CARTESIAN_POINT('Ctrl Pts',(66.8340607823661,202.139931573779,23.3713203435596)) ;
#77343 = CARTESIAN_POINT('Ctrl Pts',(66.5961327241498,202.211979358425,23.4014786793986)) ;
#77344 = CARTESIAN_POINT('Ctrl Pts',(66.6453706290186,202.13054328071,23.4014786793986)) ;
#77345 = CARTESIAN_POINT('Ctrl Pts',(66.7388966818371,202.077798896138,23.4014786793986)) ;
#77346 = CARTESIAN_POINT('Ctrl Pts',(66.8340607823661,202.077798896138,23.4014786793986)) ;
#77347 = CARTESIAN_POINT('Ctrl Pts',(66.5773376779735,202.200615492168,23.4643924065289)) ;
#77348 = CARTESIAN_POINT('Ctrl Pts',(66.6304895629671,202.112705962943,23.4643924065289)) ;
#77349 = CARTESIAN_POINT('Ctrl Pts',(66.7313319733253,202.05583548982,23.4643924065289)) ;
#77350 = CARTESIAN_POINT('Ctrl Pts',(66.8340607823661,202.05583548982,23.4643924065289)) ;
#77351 = CARTESIAN_POINT('Ctrl Pts',(66.5773376779735,202.200615492168,23.4913203435596)) ;
#77352 = CARTESIAN_POINT('Ctrl Pts',(66.6304722890212,202.112734532851,23.4913203435596)) ;
#77353 = CARTESIAN_POINT('Ctrl Pts',(66.7313653593827,202.05583548982,23.4913203435596)) ;
#77354 = CARTESIAN_POINT('Ctrl Pts',(66.8340607823661,202.05583548982,23.4913203435596)) ;
#77355 = CARTESIAN_POINT('',(66.8340607823661,202.17583548982,23.3713203435596)) ;
#77356 = CARTESIAN_POINT('Origin',(66.8340607823661,202.17583548982,23.4913203435596)) ;
#77357 = CARTESIAN_POINT('Origin',(66.8127335805022,202.318018212697,23.3713203435596)) ;
#77358 = CARTESIAN_POINT('Origin',(70.2085194795435,202.17583548982,23.4913203435596)) ;
#77359 = CARTESIAN_POINT('',(72.3111547045756,202.17583548982,23.3713203435596)) ;
#77360 = CARTESIAN_POINT('Origin',(72.3111547045756,202.17583548982,23.4913203435596)) ;
#77361 = CARTESIAN_POINT('',(70.2085194795435,202.17583548982,23.3713203435596)) ;
#77362 = CARTESIAN_POINT('Ctrl Pts',(72.3111547045756,202.17583548982,23.3713203435596)) ;
#77363 = CARTESIAN_POINT('Ctrl Pts',(72.363829615569,202.17583548982,23.3713203435596)) ;
#77364 = CARTESIAN_POINT('Ctrl Pts',(72.4506823622179,202.217096002582,23.3713203435596)) ;
#77365 = CARTESIAN_POINT('Ctrl Pts',(72.5005099444522,202.335617710977,23.3713203435596)) ;
#77366 = CARTESIAN_POINT('Ctrl Pts',(72.4871463781874,202.40741171428,23.3713203435596)) ;
#77367 = CARTESIAN_POINT('Ctrl Pts',(72.4710003713497,202.438596367132,23.3713203435596)) ;
#77368 = CARTESIAN_POINT('Ctrl Pts',(72.3111547045756,202.139931573779,23.3713203435596)) ;
#77369 = CARTESIAN_POINT('Ctrl Pts',(72.3743820038766,202.139931573779,23.3713203435596)) ;
#77370 = CARTESIAN_POINT('Ctrl Pts',(72.4785527184376,202.189324234858,23.3713203435596)) ;
#77371 = CARTESIAN_POINT('Ctrl Pts',(72.5383561337277,202.331579334424,23.3713203435596)) ;
#77372 = CARTESIAN_POINT('Ctrl Pts',(72.5222647226805,202.417672476653,23.3713203435596)) ;
#77373 = CARTESIAN_POINT('Ctrl Pts',(72.5028841791241,202.455104364857,23.3713203435596)) ;
#77374 = CARTESIAN_POINT('Ctrl Pts',(72.3111547045756,202.077798995588,23.4014787622833)) ;
#77375 = CARTESIAN_POINT('Ctrl Pts',(72.3925079005849,202.077798995588,23.4014787622833)) ;
#77376 = CARTESIAN_POINT('Ctrl Pts',(72.5266662486247,202.141555501501,23.4014787622833)) ;
#77377 = CARTESIAN_POINT('Ctrl Pts',(72.6036233984803,202.324607505548,23.4014787622833)) ;
#77378 = CARTESIAN_POINT('Ctrl Pts',(72.5829963900795,202.435509046935,23.4014787622833)) ;
#77379 = CARTESIAN_POINT('Ctrl Pts',(72.5580598646207,202.483671846417,23.4014787622833)) ;
#77380 = CARTESIAN_POINT('Ctrl Pts',(72.3111547045756,202.05583548982,23.4643924065289)) ;
#77381 = CARTESIAN_POINT('Ctrl Pts',(72.3989747637286,202.05583548982,23.4643924065289)) ;
#77382 = CARTESIAN_POINT('Ctrl Pts',(72.5437254422553,202.124541615164,23.4643924065289)) ;
#77383 = CARTESIAN_POINT('Ctrl Pts',(72.6267945558901,202.32213567271,23.4643924065289)) ;
#77384 = CARTESIAN_POINT('Ctrl Pts',(72.6044829089811,202.44177896715,23.4643924065289)) ;
#77385 = CARTESIAN_POINT('Ctrl Pts',(72.5775641491992,202.49377028534,23.4643924065289)) ;
#77386 = CARTESIAN_POINT('Ctrl Pts',(72.3111547045756,202.05583548982,23.4913203435596)) ;
#77387 = CARTESIAN_POINT('Ctrl Pts',(72.398946222898,202.05583548982,23.4913203435596)) ;
#77388 = CARTESIAN_POINT('Ctrl Pts',(72.5437008006462,202.12460301109,23.4913203435596)) ;
#77389 = CARTESIAN_POINT('Ctrl Pts',(72.6267467710367,202.322139191748,23.4913203435596)) ;
#77390 = CARTESIAN_POINT('Ctrl Pts',(72.6044741605953,202.441795863921,23.4913203435596)) ;
#77391 = CARTESIAN_POINT('Ctrl Pts',(72.5775641491992,202.49377028534,23.4913203435596)) ;
#77392 = CARTESIAN_POINT('',(72.5775641491992,202.49377028534,23.4913203435596)) ;
#77393 = CARTESIAN_POINT('',(72.4710003713497,202.438596367132,23.3713203435596)) ;
#77394 = CARTESIAN_POINT('Origin',(72.4710003713497,202.438596367132,23.4913203435596)) ;
#77395 = CARTESIAN_POINT('Ctrl Pts',(72.4710003713497,202.438596367132,23.3713203435596)) ;
#77396 = CARTESIAN_POINT('Ctrl Pts',(72.4871463781874,202.40741171428,23.3713203435596)) ;
#77397 = CARTESIAN_POINT('Ctrl Pts',(72.5005099444522,202.335617710977,23.3713203435596)) ;
#77398 = CARTESIAN_POINT('Ctrl Pts',(72.4506823622179,202.217096002582,23.3713203435596)) ;
#77399 = CARTESIAN_POINT('Ctrl Pts',(72.363829615569,202.17583548982,23.3713203435596)) ;
#77400 = CARTESIAN_POINT('Ctrl Pts',(72.3111547045756,202.17583548982,23.3713203435596)) ;
#77401 = CARTESIAN_POINT('Ctrl Pts',(72.3111547045756,202.05583548982,23.4913203435596)) ;
#77402 = CARTESIAN_POINT('Ctrl Pts',(72.398946222898,202.05583548982,23.4913203435596)) ;
#77403 = CARTESIAN_POINT('Ctrl Pts',(72.5437008006462,202.12460301109,23.4913203435596)) ;
#77404 = CARTESIAN_POINT('Ctrl Pts',(72.6267467710367,202.322139191748,23.4913203435596)) ;
#77405 = CARTESIAN_POINT('Ctrl Pts',(72.6044741605953,202.441795863921,23.4913203435596)) ;
#77406 = CARTESIAN_POINT('Ctrl Pts',(72.5775641491992,202.49377028534,23.4913203435596)) ;
#77407 = CARTESIAN_POINT('Ctrl Pts',(69.4984736650468,211.623322295552,23.4913203435596)) ;
#77408 = CARTESIAN_POINT('Ctrl Pts',(70.0303479865131,208.443107464909,23.4913203435596)) ;
#77409 = CARTESIAN_POINT('Ctrl Pts',(71.0942570395756,205.358653085868,23.4913203435596)) ;
#77410 = CARTESIAN_POINT('Ctrl Pts',(72.5775641491992,202.49377028534,23.4913203435596)) ;
#77411 = CARTESIAN_POINT('Ctrl Pts',(69.4984736650468,211.623322295552,23.4554164275186)) ;
#77412 = CARTESIAN_POINT('Ctrl Pts',(70.0303412850924,208.443147534446,23.4554164275186)) ;
#77413 = CARTESIAN_POINT('Ctrl Pts',(71.0942731909361,205.358621890875,23.4554164275186)) ;
#77414 = CARTESIAN_POINT('Ctrl Pts',(72.5775641491992,202.49377028534,23.4554164275186)) ;
#77415 = CARTESIAN_POINT('Ctrl Pts',(69.4687283004056,211.618347538663,23.3932839428985)) ;
#77416 = CARTESIAN_POINT('Ctrl Pts',(70.0011311659099,208.434972405821,23.3932839428985)) ;
#77417 = CARTESIAN_POINT('Ctrl Pts',(71.0662014800548,205.347247095261,23.3932839428985)) ;
#77418 = CARTESIAN_POINT('Ctrl Pts',(72.5507824546696,202.479903931751,23.3932839428985)) ;
#77419 = CARTESIAN_POINT('Ctrl Pts',(69.4066765679416,211.607969710479,23.3713203435596)) ;
#77420 = CARTESIAN_POINT('Ctrl Pts',(69.9401782226795,208.418024631175,23.3713203435596)) ;
#77421 = CARTESIAN_POINT('Ctrl Pts',(71.0076840169658,205.323435373038,23.3713203435596)) ;
#77422 = CARTESIAN_POINT('Ctrl Pts',(72.4949132271805,202.450977365426,23.3713203435596)) ;
#77423 = CARTESIAN_POINT('Ctrl Pts',(69.3801175085246,211.603527846499,23.3713203435596)) ;
#77424 = CARTESIAN_POINT('Ctrl Pts',(69.9140887480339,208.410774997776,23.3713203435596)) ;
#77425 = CARTESIAN_POINT('Ctrl Pts',(70.9826393962153,205.313240283402,23.3713203435596)) ;
#77426 = CARTESIAN_POINT('Ctrl Pts',(72.4710003713498,202.438596367132,23.3713203435596)) ;
#77427 = CARTESIAN_POINT('',(69.4984736650468,211.623322295552,23.4913203435596)) ;
#77428 = CARTESIAN_POINT('Origin',(96.3696349527109,211.612385354758,23.4913203435596)) ;
#77429 = CARTESIAN_POINT('',(69.3801175085246,211.603527846499,23.3713203435596)) ;
#77430 = CARTESIAN_POINT('Origin',(69.3801175085246,211.603527846499,23.4913203435596)) ;
#77431 = CARTESIAN_POINT('Ctrl Pts',(69.3801175085246,211.603527846499,23.3713203435596)) ;
#77432 = CARTESIAN_POINT('Ctrl Pts',(69.9140887480339,208.410774997776,23.3713203435596)) ;
#77433 = CARTESIAN_POINT('Ctrl Pts',(70.9826393962153,205.313240283402,23.3713203435596)) ;
#77434 = CARTESIAN_POINT('Ctrl Pts',(72.4710003713498,202.438596367132,23.3713203435596)) ;
#77435 = CARTESIAN_POINT('Ctrl Pts',(69.3801175085246,211.603527846499,23.3713203435596)) ;
#77436 = CARTESIAN_POINT('Ctrl Pts',(69.3745683386693,211.63670777559,23.3713203435596)) ;
#77437 = CARTESIAN_POINT('Ctrl Pts',(69.3393549802969,211.7104711332,23.3713203435596)) ;
#77438 = CARTESIAN_POINT('Ctrl Pts',(69.2646228246277,211.74865896028,23.3713203435596)) ;
#77439 = CARTESIAN_POINT('Ctrl Pts',(69.2199784169118,211.752993670653,23.3713203435596)) ;
#77440 = CARTESIAN_POINT('Ctrl Pts',(69.4155295877472,211.609450331806,23.3713203435596)) ;
#77441 = CARTESIAN_POINT('Ctrl Pts',(69.4088687502309,211.649277210824,23.3713203435596)) ;
#77442 = CARTESIAN_POINT('Ctrl Pts',(69.3666495153969,211.737772406659,23.3713203435596)) ;
#77443 = CARTESIAN_POINT('Ctrl Pts',(69.2770362017587,211.783526451141,23.3713203435596)) ;
#77444 = CARTESIAN_POINT('Ctrl Pts',(69.2234481600225,211.788729535969,23.3713203435596)) ;
#77445 = CARTESIAN_POINT('Ctrl Pts',(69.4768109371944,211.619699317454,23.4014788412624)) ;
#77446 = CARTESIAN_POINT('Ctrl Pts',(69.4682405818884,211.670943699722,23.4014788412624)) ;
#77447 = CARTESIAN_POINT('Ctrl Pts',(69.4138440642718,211.784877572449,23.4014788412624)) ;
#77448 = CARTESIAN_POINT('Ctrl Pts',(69.2984031957674,211.843876507565,23.4014788412624)) ;
#77449 = CARTESIAN_POINT('Ctrl Pts',(69.2294526236045,211.850571204073,23.4014788412624)) ;
#77450 = CARTESIAN_POINT('Ctrl Pts',(69.4984736650468,211.623322295552,23.4643924065289)) ;
#77451 = CARTESIAN_POINT('Ctrl Pts',(69.4892220419163,211.678640155241,23.4643924065289)) ;
#77452 = CARTESIAN_POINT('Ctrl Pts',(69.4305443951831,211.801590709054,23.4643924065289)) ;
#77453 = CARTESIAN_POINT('Ctrl Pts',(69.3060067148841,211.865205136511,23.4643924065289)) ;
#77454 = CARTESIAN_POINT('Ctrl Pts',(69.2315751790255,211.872432002476,23.4643924065289)) ;
#77455 = CARTESIAN_POINT('Ctrl Pts',(69.4984736650468,211.623322295552,23.4913203435596)) ;
#77456 = CARTESIAN_POINT('Ctrl Pts',(69.4892250486213,211.67862217737,23.4913203435596)) ;
#77457 = CARTESIAN_POINT('Ctrl Pts',(69.4305361180006,211.801561106719,23.4913203435596)) ;
#77458 = CARTESIAN_POINT('Ctrl Pts',(69.3059825252186,211.865207485186,23.4913203435596)) ;
#77459 = CARTESIAN_POINT('Ctrl Pts',(69.2315751790255,211.872432002476,23.4913203435596)) ;
#77460 = CARTESIAN_POINT('',(69.2315751790255,211.872432002476,23.4913203435596)) ;
#77461 = CARTESIAN_POINT('',(69.2199784169118,211.752993670653,23.3713203435596)) ;
#77462 = CARTESIAN_POINT('Origin',(69.2199784169118,211.752993670653,23.4913203435596)) ;
#77463 = CARTESIAN_POINT('Ctrl Pts',(69.2199784169118,211.752993670653,23.3713203435596)) ;
#77464 = CARTESIAN_POINT('Ctrl Pts',(69.2646228246277,211.74865896028,23.3713203435596)) ;
#77465 = CARTESIAN_POINT('Ctrl Pts',(69.3393549802969,211.7104711332,23.3713203435596)) ;
#77466 = CARTESIAN_POINT('Ctrl Pts',(69.3745683386693,211.63670777559,23.3713203435596)) ;
#77467 = CARTESIAN_POINT('Ctrl Pts',(69.3801175085246,211.603527846499,23.3713203435596)) ;
#77468 = CARTESIAN_POINT('Ctrl Pts',(69.4984736650468,211.623322295552,23.4913203435596)) ;
#77469 = CARTESIAN_POINT('Ctrl Pts',(69.4892250486213,211.67862217737,23.4913203435596)) ;
#77470 = CARTESIAN_POINT('Ctrl Pts',(69.4305361180006,211.801561106719,23.4913203435596)) ;
#77471 = CARTESIAN_POINT('Ctrl Pts',(69.3059825252186,211.865207485186,23.4913203435596)) ;
#77472 = CARTESIAN_POINT('Ctrl Pts',(69.2315751790255,211.872432002476,23.4913203435596)) ;
#77473 = CARTESIAN_POINT('Origin',(65.2251874189933,212.140864467154,23.4913203435596)) ;
#77474 = CARTESIAN_POINT('',(65.236784181107,212.260302798977,23.4913203435596)) ;
#77475 = CARTESIAN_POINT('',(65.2251874189933,212.140864467154,23.3713203435596)) ;
#77476 = CARTESIAN_POINT('Origin',(67.6088474917769,207.295232147432,23.3713203435596)) ;
#77477 = CARTESIAN_POINT('Ctrl Pts',(68.2200057399177,200.43583548982,23.3713203435596)) ;
#77478 = CARTESIAN_POINT('Ctrl Pts',(68.1824073171725,200.43583548982,23.3713203435596)) ;
#77479 = CARTESIAN_POINT('Ctrl Pts',(68.1076443008799,200.411538289219,23.3713203435596)) ;
#77480 = CARTESIAN_POINT('Ctrl Pts',(68.0256156592925,200.299810943276,23.3713203435596)) ;
#77481 = CARTESIAN_POINT('Ctrl Pts',(68.0408878207066,200.196696127704,23.3713203435596)) ;
#77482 = CARTESIAN_POINT('Ctrl Pts',(68.073772979818,200.150878451592,23.3713203435596)) ;
#77483 = CARTESIAN_POINT('Ctrl Pts',(68.2200057399177,200.471739405861,23.3713203435596)) ;
#77484 = CARTESIAN_POINT('Ctrl Pts',(68.1748752084499,200.471739405861,23.3713203435596)) ;
#77485 = CARTESIAN_POINT('Ctrl Pts',(68.0851812979518,200.442665155226,23.3713203435596)) ;
#77486 = CARTESIAN_POINT('Ctrl Pts',(67.9867254555472,200.308566385953,23.3713203435596)) ;
#77487 = CARTESIAN_POINT('Ctrl Pts',(68.0051314291745,200.1849394215,23.3713203435596)) ;
#77488 = CARTESIAN_POINT('Ctrl Pts',(68.044604486812,200.129943069989,23.3713203435596)) ;
#77489 = CARTESIAN_POINT('Ctrl Pts',(68.2200057399177,200.533872085375,23.4014786778375)) ;
#77490 = CARTESIAN_POINT('Ctrl Pts',(68.1619372629609,200.533872085375,23.4014786778375)) ;
#77491 = CARTESIAN_POINT('Ctrl Pts',(68.0464591301393,200.496324714954,23.4014786778375)) ;
#77492 = CARTESIAN_POINT('Ctrl Pts',(67.9197695231301,200.323765978659,23.4014786778375)) ;
#77493 = CARTESIAN_POINT('Ctrl Pts',(67.9433385076373,200.164476450385,23.4014786778375)) ;
#77494 = CARTESIAN_POINT('Ctrl Pts',(67.9941276356022,200.09371383655,23.4014786778375)) ;
#77495 = CARTESIAN_POINT('Ctrl Pts',(68.2200057399177,200.55583548982,23.4643924065289)) ;
#77496 = CARTESIAN_POINT('Ctrl Pts',(68.1573213300674,200.55583548982,23.4643924065289)) ;
#77497 = CARTESIAN_POINT('Ctrl Pts',(68.0327048929491,200.515383677869,23.4643924065289)) ;
#77498 = CARTESIAN_POINT('Ctrl Pts',(67.895949576542,200.329117772152,23.4643924065289)) ;
#77499 = CARTESIAN_POINT('Ctrl Pts',(67.9214580564103,200.15729471167,23.4643924065289)) ;
#77500 = CARTESIAN_POINT('Ctrl Pts',(67.9762844730848,200.080907092773,23.4643924065289)) ;
#77501 = CARTESIAN_POINT('Ctrl Pts',(68.2200057399177,200.55583548982,23.4913203435596)) ;
#77502 = CARTESIAN_POINT('Ctrl Pts',(68.1573417020091,200.55583548982,23.4913203435596)) ;
#77503 = CARTESIAN_POINT('Ctrl Pts',(68.0327366748546,200.515340155485,23.4913203435596)) ;
#77504 = CARTESIAN_POINT('Ctrl Pts',(67.8960222722091,200.329127912246,23.4913203435596)) ;
#77505 = CARTESIAN_POINT('Ctrl Pts',(67.9214758745658,200.157269886293,23.4913203435596)) ;
#77506 = CARTESIAN_POINT('Ctrl Pts',(67.9762844730848,200.080907092773,23.4913203435596)) ;
#77507 = CARTESIAN_POINT('',(67.9762844730848,200.080907092773,23.4913203435596)) ;
#77508 = CARTESIAN_POINT('',(68.073772979818,200.150878451592,23.3713203435596)) ;
#77509 = CARTESIAN_POINT('Origin',(68.073772979818,200.150878451592,23.4913203435596)) ;
#77510 = CARTESIAN_POINT('',(68.2200057399177,200.43583548982,23.3713203435596)) ;
#77511 = CARTESIAN_POINT('Ctrl Pts',(68.073772979818,200.150878451592,23.3713203435596)) ;
#77512 = CARTESIAN_POINT('Ctrl Pts',(68.0408878207066,200.196696127704,23.3713203435596)) ;
#77513 = CARTESIAN_POINT('Ctrl Pts',(68.0256156592925,200.299810943276,23.3713203435596)) ;
#77514 = CARTESIAN_POINT('Ctrl Pts',(68.1076443008799,200.411538289219,23.3713203435596)) ;
#77515 = CARTESIAN_POINT('Ctrl Pts',(68.1824073171725,200.43583548982,23.3713203435596)) ;
#77516 = CARTESIAN_POINT('Ctrl Pts',(68.2200057399177,200.43583548982,23.3713203435596)) ;
#77517 = CARTESIAN_POINT('',(68.2200057399177,200.55583548982,23.4913203435596)) ;
#77518 = CARTESIAN_POINT('Origin',(68.2200057399177,200.43583548982,23.4913203435596)) ;
#77519 = CARTESIAN_POINT('Ctrl Pts',(68.2200057399177,200.55583548982,23.4913203435596)) ;
#77520 = CARTESIAN_POINT('Ctrl Pts',(68.1573417020091,200.55583548982,23.4913203435596)) ;
#77521 = CARTESIAN_POINT('Ctrl Pts',(68.0327366748546,200.515340155485,23.4913203435596)) ;
#77522 = CARTESIAN_POINT('Ctrl Pts',(67.8960222722091,200.329127912246,23.4913203435596)) ;
#77523 = CARTESIAN_POINT('Ctrl Pts',(67.9214758745658,200.157269886293,23.4913203435596)) ;
#77524 = CARTESIAN_POINT('Ctrl Pts',(67.9762844730848,200.080907092773,23.4913203435596)) ;
#77525 = CARTESIAN_POINT('Ctrl Pts',(77.5627334640076,190.683545731522,23.4913203435596)) ;
#77526 = CARTESIAN_POINT('Ctrl Pts',(73.9435688224726,193.341467670589,23.4913203435596)) ;
#77527 = CARTESIAN_POINT('Ctrl Pts',(70.5986101113225,196.427317753425,23.4913203435596)) ;
#77528 = CARTESIAN_POINT('Ctrl Pts',(67.9762844730849,200.080907092773,23.4913203435596)) ;
#77529 = CARTESIAN_POINT('Ctrl Pts',(77.5627334640076,190.683545731522,23.4554164275186)) ;
#77530 = CARTESIAN_POINT('Ctrl Pts',(73.9435444773532,193.341485549695,23.4554164275186)) ;
#77531 = CARTESIAN_POINT('Ctrl Pts',(70.5986406627929,196.427275187191,23.4554164275186)) ;
#77532 = CARTESIAN_POINT('Ctrl Pts',(67.9762844730849,200.080907092773,23.4554164275186)) ;
#77533 = CARTESIAN_POINT('Ctrl Pts',(77.5805848919263,190.707853163496,23.3932837400762)) ;
#77534 = CARTESIAN_POINT('Ctrl Pts',(73.9633403608045,193.364364969535,23.3932837400762)) ;
#77535 = CARTESIAN_POINT('Ctrl Pts',(70.6207012559953,196.448260130978,23.3932837400762)) ;
#77536 = CARTESIAN_POINT('Ctrl Pts',(68.0007852258362,200.098492252496,23.3932837400762)) ;
#77537 = CARTESIAN_POINT('Ctrl Pts',(77.6178250208571,190.758561258377,23.3713203435596)) ;
#77538 = CARTESIAN_POINT('Ctrl Pts',(74.0045722037604,193.412141541445,23.3713203435596)) ;
#77539 = CARTESIAN_POINT('Ctrl Pts',(70.6668033103964,196.491924107876,23.3713203435596)) ;
#77540 = CARTESIAN_POINT('Ctrl Pts',(68.0518966100636,200.13517691539,23.3713203435596)) ;
#77541 = CARTESIAN_POINT('Ctrl Pts',(77.6337643041011,190.780265014789,23.3713203435596)) ;
#77542 = CARTESIAN_POINT('Ctrl Pts',(74.0222174084502,193.432592465647,23.3713203435596)) ;
#77543 = CARTESIAN_POINT('Ctrl Pts',(70.6865388646701,196.510608363121,23.3713203435596)) ;
#77544 = CARTESIAN_POINT('Ctrl Pts',(68.073772979818,200.150878451592,23.3713203435596)) ;
#77545 = CARTESIAN_POINT('Ctrl Pts',(67.9762844730849,200.080907092773,23.4913203435596)) ;
#77546 = CARTESIAN_POINT('Ctrl Pts',(70.5986101113225,196.427317753425,23.4913203435596)) ;
#77547 = CARTESIAN_POINT('Ctrl Pts',(73.9435688224726,193.341467670589,23.4913203435596)) ;
#77548 = CARTESIAN_POINT('Ctrl Pts',(77.5627334640076,190.683545731522,23.4913203435596)) ;
#77549 = CARTESIAN_POINT('',(77.6337643041011,190.780265014789,23.3713203435596)) ;
#77550 = CARTESIAN_POINT('Origin',(77.6337643041011,190.780265014789,23.4913203435596)) ;
#77551 = CARTESIAN_POINT('Ctrl Pts',(77.6337643041011,190.780265014789,23.3713203435596)) ;
#77552 = CARTESIAN_POINT('Ctrl Pts',(74.0222174084502,193.432592465647,23.3713203435596)) ;
#77553 = CARTESIAN_POINT('Ctrl Pts',(70.6865388646701,196.510608363121,23.3713203435596)) ;
#77554 = CARTESIAN_POINT('Ctrl Pts',(68.073772979818,200.150878451592,23.3713203435596)) ;
#77555 = CARTESIAN_POINT('Ctrl Pts',(77.6337643041011,190.780265014789,23.3713203435596)) ;
#77556 = CARTESIAN_POINT('Ctrl Pts',(77.7835229891055,190.670281929225,23.3713203435596)) ;
#77557 = CARTESIAN_POINT('Ctrl Pts',(77.9688509344519,190.609539758744,23.3713203435596)) ;
#77558 = CARTESIAN_POINT('Ctrl Pts',(78.1546571314538,190.609539758744,23.3713203435596)) ;
#77559 = CARTESIAN_POINT('Ctrl Pts',(77.6125119264424,190.751326672906,23.3713203435596)) ;
#77560 = CARTESIAN_POINT('Ctrl Pts',(77.7684072254185,190.63683684545,23.3713203435596)) ;
#77561 = CARTESIAN_POINT('Ctrl Pts',(77.9612372130539,190.573635842703,23.3713203435596)) ;
#77562 = CARTESIAN_POINT('Ctrl Pts',(78.1546571314538,190.573635842703,23.3713203435596)) ;
#77563 = CARTESIAN_POINT('Ctrl Pts',(77.5757341216353,190.701248102578,23.4014786760343)) ;
#77564 = CARTESIAN_POINT('Ctrl Pts',(77.7421703169228,190.579017019241,23.4014786760343)) ;
#77565 = CARTESIAN_POINT('Ctrl Pts',(77.9481590810139,190.511503161025,23.4014786760343)) ;
#77566 = CARTESIAN_POINT('Ctrl Pts',(78.1546571314538,190.511503161025,23.4014786760343)) ;
#77567 = CARTESIAN_POINT('Ctrl Pts',(77.5627334640076,190.683545731522,23.4643924065289)) ;
#77568 = CARTESIAN_POINT('Ctrl Pts',(77.7329303854515,190.558552763179,23.4643924065289)) ;
#77569 = CARTESIAN_POINT('Ctrl Pts',(77.943493133092,190.489539758744,23.4643924065289)) ;
#77570 = CARTESIAN_POINT('Ctrl Pts',(78.1546571314538,190.489539758744,23.4643924065289)) ;
#77571 = CARTESIAN_POINT('Ctrl Pts',(77.5627334640076,190.683545731522,23.4913203435596)) ;
#77572 = CARTESIAN_POINT('Ctrl Pts',(77.7329137878762,190.558564952473,23.4913203435596)) ;
#77573 = CARTESIAN_POINT('Ctrl Pts',(77.9435137257698,190.489539758744,23.4913203435596)) ;
#77574 = CARTESIAN_POINT('Ctrl Pts',(78.1546571314538,190.489539758744,23.4913203435596)) ;
#77575 = CARTESIAN_POINT('',(78.1546571314538,190.609539758744,23.3713203435596)) ;
#77576 = CARTESIAN_POINT('Origin',(78.1546571314538,190.609539758744,23.4913203435596)) ;
#77577 = CARTESIAN_POINT('Origin',(78.0868516728036,191.282661304515,23.3713203435596)) ;
#77578 = CARTESIAN_POINT('Origin',(78.07353074889,190.609539758744,23.4913203435596)) ;
#77579 = CARTESIAN_POINT('',(80.8501919227397,190.609539758744,23.3713203435596)) ;
#77580 = CARTESIAN_POINT('Origin',(80.8501919227397,190.609539758744,23.4913203435596)) ;
#77581 = CARTESIAN_POINT('',(78.07353074889,190.609539758744,23.3713203435596)) ;
#77582 = CARTESIAN_POINT('Ctrl Pts',(80.8501919227397,190.609539758744,23.3713203435596)) ;
#77583 = CARTESIAN_POINT('Ctrl Pts',(80.8900960147986,190.609539758744,23.3713203435596)) ;
#77584 = CARTESIAN_POINT('Ctrl Pts',(80.9697731323004,190.637124645342,23.3713203435596)) ;
#77585 = CARTESIAN_POINT('Ctrl Pts',(81.0384684533381,190.743413070952,23.3713203435596)) ;
#77586 = CARTESIAN_POINT('Ctrl Pts',(81.0287354417464,190.84834644111,23.3713203435596)) ;
#77587 = CARTESIAN_POINT('Ctrl Pts',(80.9947301225929,190.898658010764,23.3713203435596)) ;
#77588 = CARTESIAN_POINT('Ctrl Pts',(80.9810274260323,190.913160432898,23.3713203435596)) ;
#77589 = CARTESIAN_POINT('Ctrl Pts',(80.8501919227397,190.573635842703,23.3713203435596)) ;
#77590 = CARTESIAN_POINT('Ctrl Pts',(80.8980900192787,190.573635842703,23.3713203435596)) ;
#77591 = CARTESIAN_POINT('Ctrl Pts',(80.9936901650968,190.606657008214,23.3713203435596)) ;
#77592 = CARTESIAN_POINT('Ctrl Pts',(81.0761224171995,190.734180607265,23.3713203435596)) ;
#77593 = CARTESIAN_POINT('Ctrl Pts',(81.064410508624,190.860067831686,23.3713203435596)) ;
#77594 = CARTESIAN_POINT('Ctrl Pts',(81.0235724505757,190.920410880242,23.3713203435596)) ;
#77595 = CARTESIAN_POINT('Ctrl Pts',(81.0071246867289,190.937818579041,23.3713203435596)) ;
#77596 = CARTESIAN_POINT('Ctrl Pts',(80.8501919227397,190.511503216626,23.4014787223741)) ;
#77597 = CARTESIAN_POINT('Ctrl Pts',(80.9118213657063,190.511503216626,23.4014787223741)) ;
#77598 = CARTESIAN_POINT('Ctrl Pts',(81.034887159699,190.554128041159,23.4014787223741)) ;
#77599 = CARTESIAN_POINT('Ctrl Pts',(81.1409888893296,190.718297939174,23.4014787223741)) ;
#77600 = CARTESIAN_POINT('Ctrl Pts',(81.1259638528477,190.880377412799,23.4014787223741)) ;
#77601 = CARTESIAN_POINT('Ctrl Pts',(81.073449631436,190.958092009754,23.4014787223741)) ;
#77602 = CARTESIAN_POINT('Ctrl Pts',(81.0522866500825,190.98049011861,23.4014787223741)) ;
#77603 = CARTESIAN_POINT('Ctrl Pts',(80.8501919227397,190.489539758744,23.4643924065289)) ;
#77604 = CARTESIAN_POINT('Ctrl Pts',(80.9167203640597,190.489539758744,23.4643924065289)) ;
#77605 = CARTESIAN_POINT('Ctrl Pts',(81.0495344536617,190.535473208199,23.4643924065289)) ;
#77606 = CARTESIAN_POINT('Ctrl Pts',(81.164048307672,190.7126420413,23.4643924065289)) ;
#77607 = CARTESIAN_POINT('Ctrl Pts',(81.1478031175844,190.887545532602,23.4643924065289)) ;
#77608 = CARTESIAN_POINT('Ctrl Pts',(81.0910963470228,190.971395654268,23.4643924065289)) ;
#77609 = CARTESIAN_POINT('Ctrl Pts',(81.068251094894,190.995574215667,23.4643924065289)) ;
#77610 = CARTESIAN_POINT('Ctrl Pts',(80.8501919227397,190.489539758744,23.4913203435596)) ;
#77611 = CARTESIAN_POINT('Ctrl Pts',(80.9166987428379,190.489539758744,23.4913203435596)) ;
#77612 = CARTESIAN_POINT('Ctrl Pts',(81.0494939386742,190.535514569741,23.4913203435596)) ;
#77613 = CARTESIAN_POINT('Ctrl Pts',(81.1639861404037,190.712661945758,23.4913203435596)) ;
#77614 = CARTESIAN_POINT('Ctrl Pts',(81.1477644544174,190.887550896021,23.4913203435596)) ;
#77615 = CARTESIAN_POINT('Ctrl Pts',(81.091088922495,190.971403512111,23.4913203435596)) ;
#77616 = CARTESIAN_POINT('Ctrl Pts',(81.068251094894,190.995574215667,23.4913203435596)) ;
#77617 = CARTESIAN_POINT('',(80.9810274260323,190.913160432898,23.3713203435596)) ;
#77618 = CARTESIAN_POINT('Origin',(80.9810274260323,190.913160432898,23.4913203435596)) ;
#77619 = CARTESIAN_POINT('Ctrl Pts',(80.9810274260323,190.913160432898,23.3713203435596)) ;
#77620 = CARTESIAN_POINT('Ctrl Pts',(80.9947301225929,190.898658010764,23.3713203435596)) ;
#77621 = CARTESIAN_POINT('Ctrl Pts',(81.0287354417464,190.84834644111,23.3713203435596)) ;
#77622 = CARTESIAN_POINT('Ctrl Pts',(81.0384684533381,190.743413070952,23.3713203435596)) ;
#77623 = CARTESIAN_POINT('Ctrl Pts',(80.9697731323004,190.637124645342,23.3713203435596)) ;
#77624 = CARTESIAN_POINT('Ctrl Pts',(80.8900960147986,190.609539758744,23.3713203435596)) ;
#77625 = CARTESIAN_POINT('Ctrl Pts',(80.8501919227397,190.609539758744,23.3713203435596)) ;
#77626 = CARTESIAN_POINT('Ctrl Pts',(73.7436956568154,200.410454788892,23.4913203435596)) ;
#77627 = CARTESIAN_POINT('Ctrl Pts',(75.7953376765802,196.999191831293,23.4913203435596)) ;
#77628 = CARTESIAN_POINT('Ctrl Pts',(78.3304755598256,193.893133563934,23.4913203435596)) ;
#77629 = CARTESIAN_POINT('Ctrl Pts',(81.0682510948939,190.995574215667,23.4913203435596)) ;
#77630 = CARTESIAN_POINT('Ctrl Pts',(73.7436956568154,200.410454788892,23.4554164275186)) ;
#77631 = CARTESIAN_POINT('Ctrl Pts',(75.795318037376,196.999224485377,23.4554164275186)) ;
#77632 = CARTESIAN_POINT('Ctrl Pts',(78.3304892457748,193.893119079237,23.4554164275186)) ;
#77633 = CARTESIAN_POINT('Ctrl Pts',(81.0682510948939,190.995574215667,23.4554164275186)) ;
#77634 = CARTESIAN_POINT('Ctrl Pts',(73.7178513760089,200.394911216575,23.3932838348228)) ;
#77635 = CARTESIAN_POINT('Ctrl Pts',(75.7710423485568,196.981072816866,23.3932838348228)) ;
#77636 = CARTESIAN_POINT('Ctrl Pts',(78.3074750856353,193.873563742023,23.3932838348228)) ;
#77637 = CARTESIAN_POINT('Ctrl Pts',(81.0463300376127,190.974861979224,23.3932838348228)) ;
#77638 = CARTESIAN_POINT('Ctrl Pts',(73.6639374467842,200.362485665093,23.3713203435596)) ;
#77639 = CARTESIAN_POINT('Ctrl Pts',(75.7203485344392,196.943293183495,23.3713203435596)) ;
#77640 = CARTESIAN_POINT('Ctrl Pts',(78.2595014217398,193.832730768784,23.3713203435596)) ;
#77641 = CARTESIAN_POINT('Ctrl Pts',(81.0006003715547,190.931654042505,23.3713203435596)) ;
#77642 = CARTESIAN_POINT('Ctrl Pts',(73.6408615205729,200.348607069263,23.3713203435596)) ;
#77643 = CARTESIAN_POINT('Ctrl Pts',(75.6986487748031,196.927126436994,23.3713203435596)) ;
#77644 = CARTESIAN_POINT('Ctrl Pts',(78.2389694686303,193.81525213698,23.3713203435596)) ;
#77645 = CARTESIAN_POINT('Ctrl Pts',(80.9810274260322,190.913160432898,23.3713203435596)) ;
#77646 = CARTESIAN_POINT('',(73.6408615205729,200.348607069263,23.3713203435596)) ;
#77647 = CARTESIAN_POINT('Origin',(73.6408615205729,200.348607069263,23.4913203435596)) ;
#77648 = CARTESIAN_POINT('Ctrl Pts',(73.6408615205729,200.348607069263,23.3713203435596)) ;
#77649 = CARTESIAN_POINT('Ctrl Pts',(75.6986487748031,196.927126436994,23.3713203435596)) ;
#77650 = CARTESIAN_POINT('Ctrl Pts',(78.2389694686303,193.81525213698,23.3713203435596)) ;
#77651 = CARTESIAN_POINT('Ctrl Pts',(80.9810274260322,190.913160432898,23.3713203435596)) ;
#77652 = CARTESIAN_POINT('Ctrl Pts',(73.6408615205729,200.348607069263,23.3713203435596)) ;
#77653 = CARTESIAN_POINT('Ctrl Pts',(73.609031832983,200.401530256243,23.3713203435596)) ;
#77654 = CARTESIAN_POINT('Ctrl Pts',(73.548367847994,200.43583548982,23.3713203435596)) ;
#77655 = CARTESIAN_POINT('Ctrl Pts',(73.4866103162092,200.43583548982,23.3713203435596)) ;
#77656 = CARTESIAN_POINT('Ctrl Pts',(73.6716294221879,200.367111863704,23.3713203435596)) ;
#77657 = CARTESIAN_POINT('Ctrl Pts',(73.6334232791504,200.430637176229,23.3713203435596)) ;
#77658 = CARTESIAN_POINT('Ctrl Pts',(73.5607397617575,200.471739405861,23.3713203435596)) ;
#77659 = CARTESIAN_POINT('Ctrl Pts',(73.4866103162092,200.471739405861,23.3713203435596)) ;
#77660 = CARTESIAN_POINT('Ctrl Pts',(73.7248740178776,200.399134856713,23.4014787503538)) ;
#77661 = CARTESIAN_POINT('Ctrl Pts',(73.6757150014773,200.480871499881,23.4014787503538)) ;
#77662 = CARTESIAN_POINT('Ctrl Pts',(73.5819910675684,200.533871998366,23.4014787503538)) ;
#77663 = CARTESIAN_POINT('Ctrl Pts',(73.4866103162092,200.533871998366,23.4014787503538)) ;
#77664 = CARTESIAN_POINT('Ctrl Pts',(73.7436956568153,200.410454788892,23.4643924065289)) ;
#77665 = CARTESIAN_POINT('Ctrl Pts',(73.6906289312292,200.498688775878,23.4643924065289)) ;
#77666 = CARTESIAN_POINT('Ctrl Pts',(73.5895729979147,200.55583548982,23.4643924065289)) ;
#77667 = CARTESIAN_POINT('Ctrl Pts',(73.4866103162092,200.55583548982,23.4643924065289)) ;
#77668 = CARTESIAN_POINT('Ctrl Pts',(73.7436956568153,200.410454788892,23.4913203435596)) ;
#77669 = CARTESIAN_POINT('Ctrl Pts',(73.6906461774989,200.498660100524,23.4913203435596)) ;
#77670 = CARTESIAN_POINT('Ctrl Pts',(73.5895395358505,200.55583548982,23.4913203435596)) ;
#77671 = CARTESIAN_POINT('Ctrl Pts',(73.4866103162092,200.55583548982,23.4913203435596)) ;
#77672 = CARTESIAN_POINT('',(73.4866103162092,200.55583548982,23.4913203435596)) ;
#77673 = CARTESIAN_POINT('',(73.4866103162092,200.43583548982,23.3713203435596)) ;
#77674 = CARTESIAN_POINT('Origin',(73.4866103162092,200.43583548982,23.4913203435596)) ;
#77675 = CARTESIAN_POINT('Origin',(73.5079774294674,200.293620227099,23.3713203435596)) ;
#77676 = CARTESIAN_POINT('Origin',(73.5222221716416,200.318810051951,23.4913203435596)) ;
#77677 = CARTESIAN_POINT('Origin',(71.1190430355237,200.43583548982,23.4913203435596)) ;
#77678 = CARTESIAN_POINT('',(71.1190430355237,200.55583548982,23.4913203435596)) ;
#77679 = CARTESIAN_POINT('',(71.1190430355237,200.43583548982,23.3713203435596)) ;
#77680 = CARTESIAN_POINT('Ctrl Pts',(77.8285014478222,190.489539758744,17.8547522895864)) ;
#77681 = CARTESIAN_POINT('Ctrl Pts',(77.8285014478222,190.489539758744,32.8746339543542)) ;
#77682 = CARTESIAN_POINT('Ctrl Pts',(73.8355349189945,193.386814152385,17.8547522895863)) ;
#77683 = CARTESIAN_POINT('Ctrl Pts',(73.8355349189945,193.386814152385,32.8746339543541)) ;
#77684 = CARTESIAN_POINT('Ctrl Pts',(70.4532522157592,196.594204259059,17.8547522895864)) ;
#77685 = CARTESIAN_POINT('Ctrl Pts',(70.4532522157592,196.594204259059,32.8746339543542)) ;
#77686 = CARTESIAN_POINT('Ctrl Pts',(67.88518965836,200.208466979566,17.8547522895864)) ;
#77687 = CARTESIAN_POINT('Ctrl Pts',(67.88518965836,200.208466979566,32.8746339543542)) ;
#77688 = CARTESIAN_POINT('Ctrl Pts',(67.8032385132701,200.323804110956,17.8547522895864)) ;
#77689 = CARTESIAN_POINT('Ctrl Pts',(67.8032385132701,200.323804110956,32.8746339543542)) ;
#77690 = CARTESIAN_POINT('Ctrl Pts',(67.7220901562832,200.439592363042,17.8547522895864)) ;
#77691 = CARTESIAN_POINT('Ctrl Pts',(67.7220901562832,200.439592363042,32.8746339543542)) ;
#77692 = CARTESIAN_POINT('Ctrl Pts',(67.6417475736103,200.555835489811,17.8547522895864)) ;
#77693 = CARTESIAN_POINT('Ctrl Pts',(67.6417475736103,200.555835489811,32.8746339543542)) ;
#77694 = CARTESIAN_POINT('',(67.9762844730848,200.080907092773,30.2513203435596)) ;
#77695 = CARTESIAN_POINT('Ctrl Pts',(67.9762844730848,200.080907092773,23.4913203435596)) ;
#77696 = CARTESIAN_POINT('Ctrl Pts',(67.9762844730848,200.080907092773,31.6033203435596)) ;
#77697 = CARTESIAN_POINT('Ctrl Pts',(67.9397439452691,200.131817658927,23.4913203435596)) ;
#77698 = CARTESIAN_POINT('Ctrl Pts',(67.9397439452691,200.131817658927,31.6033203435596)) ;
#77699 = CARTESIAN_POINT('Ctrl Pts',(67.8999789504624,200.256667577061,23.4913203435596)) ;
#77700 = CARTESIAN_POINT('Ctrl Pts',(67.8999789504624,200.256667577061,31.6033203435596)) ;
#77701 = CARTESIAN_POINT('Ctrl Pts',(67.9715322297243,200.476322658598,23.4913203435596)) ;
#77702 = CARTESIAN_POINT('Ctrl Pts',(67.9715322297243,200.476322658598,31.6033203435596)) ;
#77703 = CARTESIAN_POINT('Ctrl Pts',(68.1260059217369,200.55583548982,23.4913203435596)) ;
#77704 = CARTESIAN_POINT('Ctrl Pts',(68.1260059217369,200.55583548982,31.6033203435596)) ;
#77705 = CARTESIAN_POINT('Ctrl Pts',(68.2200057399177,200.55583548982,23.4913203435596)) ;
#77706 = CARTESIAN_POINT('Ctrl Pts',(68.2200057399177,200.55583548982,31.6033203435596)) ;
#77707 = CARTESIAN_POINT('',(68.2200057399177,200.55583548982,23.4913203435596)) ;
#77708 = CARTESIAN_POINT('Origin',(74.5963384974435,195.522687624282,23.3713203435596)) ;
#77709 = CARTESIAN_POINT('Origin',(73.5885500808522,200.43583548982,19.2513203435596)) ;
#77710 = CARTESIAN_POINT('',(73.5885500808522,200.55583548982,19.2513203435596)) ;
#77711 = CARTESIAN_POINT('',(73.5885500808522,200.43583548982,19.3713203435596)) ;
#77712 = CARTESIAN_POINT('Origin',(73.5885500808522,200.43583548982,19.2513203435596)) ;
#77713 = CARTESIAN_POINT('',(73.6915408905797,200.497421958396,19.2513203435596)) ;
#77714 = CARTESIAN_POINT('Origin',(73.5885500808522,200.43583548982,19.2513203435596)) ;
#77715 = CARTESIAN_POINT('Origin',(73.5885500808522,200.43583548982,19.2513203435596)) ;
#77716 = CARTESIAN_POINT('Ctrl Pts',(73.6915408905803,200.497421958395,17.9913203435596)) ;
#77717 = CARTESIAN_POINT('Ctrl Pts',(73.6824627768405,200.512603252379,17.9913203435596)) ;
#77718 = CARTESIAN_POINT('Ctrl Pts',(73.6533226941628,200.543288099199,17.9913203435596)) ;
#77719 = CARTESIAN_POINT('Ctrl Pts',(73.6121347778153,200.55583548982,17.9913203435596)) ;
#77720 = CARTESIAN_POINT('Ctrl Pts',(73.5885500808522,200.55583548982,17.9913203435596)) ;
#77721 = CARTESIAN_POINT('Ctrl Pts',(73.6915408905803,200.497421958395,17.9554164275186)) ;
#77722 = CARTESIAN_POINT('Ctrl Pts',(73.6824917890662,200.512554735348,17.9554164275186)) ;
#77723 = CARTESIAN_POINT('Ctrl Pts',(73.653329650592,200.543206850976,17.9554164275186)) ;
#77724 = CARTESIAN_POINT('Ctrl Pts',(73.612059404828,200.55583548982,17.9554164275186)) ;
#77725 = CARTESIAN_POINT('Ctrl Pts',(73.5885500808522,200.55583548982,17.9554164275186)) ;
#77726 = CARTESIAN_POINT('Ctrl Pts',(73.7174244840934,200.512899835719,17.8932837474712)) ;
#77727 = CARTESIAN_POINT('Ctrl Pts',(73.7060581631873,200.531907689569,17.8932837474712)) ;
#77728 = CARTESIAN_POINT('Ctrl Pts',(73.6695997049772,200.570311794726,17.8932837474712)) ;
#77729 = CARTESIAN_POINT('Ctrl Pts',(73.6180794789012,200.585993823654,17.8932837474712)) ;
#77730 = CARTESIAN_POINT('Ctrl Pts',(73.5885500808522,200.585993823654,17.8932837474712)) ;
#77731 = CARTESIAN_POINT('Ctrl Pts',(73.7714206166492,200.545188455739,17.8713203435596)) ;
#77732 = CARTESIAN_POINT('Ctrl Pts',(73.755297346051,200.572151337892,17.8713203435596)) ;
#77733 = CARTESIAN_POINT('Ctrl Pts',(73.703559367871,200.626640069246,17.8713203435596)) ;
#77734 = CARTESIAN_POINT('Ctrl Pts',(73.6304379071134,200.648907552789,17.8713203435596)) ;
#77735 = CARTESIAN_POINT('Ctrl Pts',(73.5885500808522,200.648907552789,17.8713203435596)) ;
#77736 = CARTESIAN_POINT('Ctrl Pts',(73.7945317003084,200.55900842697,17.8713203435596)) ;
#77737 = CARTESIAN_POINT('Ctrl Pts',(73.7763754728287,200.589371014938,17.8713203435596)) ;
#77738 = CARTESIAN_POINT('Ctrl Pts',(73.7180953074733,200.650740708578,17.8713203435596)) ;
#77739 = CARTESIAN_POINT('Ctrl Pts',(73.6357194747785,200.67583548982,17.8713203435596)) ;
#77740 = CARTESIAN_POINT('Ctrl Pts',(73.5885500808522,200.67583548982,17.8713203435596)) ;
#77741 = CARTESIAN_POINT('',(73.6915408905803,200.497421958395,17.9913203435596)) ;
#77742 = CARTESIAN_POINT('',(73.7945317003084,200.55900842697,17.8713203435596)) ;
#77743 = CARTESIAN_POINT('Origin',(73.7945317003084,200.55900842697,17.9913203435596)) ;
#77744 = CARTESIAN_POINT('',(73.5885500808522,200.55583548982,17.9913203435596)) ;
#77745 = CARTESIAN_POINT('Origin',(73.5831295493737,200.427665247194,17.9913203435596)) ;
#77746 = CARTESIAN_POINT('',(73.5885500808522,200.67583548982,17.8713203435596)) ;
#77747 = CARTESIAN_POINT('Origin',(73.5885500808522,200.67583548982,17.9913203435596)) ;
#77748 = CARTESIAN_POINT('Ctrl Pts',(73.5885500808522,200.67583548982,17.8713203435596)) ;
#77749 = CARTESIAN_POINT('Ctrl Pts',(73.6357194747785,200.67583548982,17.8713203435596)) ;
#77750 = CARTESIAN_POINT('Ctrl Pts',(73.7180953074733,200.650740708578,17.8713203435596)) ;
#77751 = CARTESIAN_POINT('Ctrl Pts',(73.7763754728287,200.589371014938,17.8713203435596)) ;
#77752 = CARTESIAN_POINT('Ctrl Pts',(73.7945317003084,200.55900842697,17.8713203435596)) ;
#77753 = CARTESIAN_POINT('Ctrl Pts',(73.6915408905803,200.497421958395,19.2513203435596)) ;
#77754 = CARTESIAN_POINT('Ctrl Pts',(73.6915408905803,200.497421958395,17.7393203435596)) ;
#77755 = CARTESIAN_POINT('Ctrl Pts',(73.6703579522658,200.532846103015,19.2513203435596)) ;
#77756 = CARTESIAN_POINT('Ctrl Pts',(73.6703579522658,200.532846103015,17.7393203435596)) ;
#77757 = CARTESIAN_POINT('Ctrl Pts',(73.6298246117119,200.55583548982,19.2513203435596)) ;
#77758 = CARTESIAN_POINT('Ctrl Pts',(73.6298246117119,200.55583548982,17.7393203435596)) ;
#77759 = CARTESIAN_POINT('Ctrl Pts',(73.5885500808522,200.55583548982,19.2513203435596)) ;
#77760 = CARTESIAN_POINT('Ctrl Pts',(73.5885500808522,200.55583548982,17.7393203435596)) ;
#77761 = CARTESIAN_POINT('',(73.6915408905803,200.497421958395,17.9913203435596)) ;
#77762 = CARTESIAN_POINT('',(73.5885500808522,200.55583548982,19.2513203435596)) ;
#77763 = CARTESIAN_POINT('Origin',(67.8715456014014,200.43583548982,19.2513203435596)) ;
#77764 = CARTESIAN_POINT('',(67.8715456014017,200.55583548982,19.2513203435596)) ;
#77765 = CARTESIAN_POINT('',(67.8530878290255,200.554407453787,19.2513203435596)) ;
#77766 = CARTESIAN_POINT('Origin',(67.8715456014017,200.43583548982,19.2513203435596)) ;
#77767 = CARTESIAN_POINT('',(67.8715456014015,200.43583548982,19.3713203435596)) ;
#77768 = CARTESIAN_POINT('Origin',(67.8715456014014,200.43583548982,19.2513203435596)) ;
#77769 = CARTESIAN_POINT('',(67.7733141415173,200.366911043569,19.2513203435596)) ;
#77770 = CARTESIAN_POINT('Origin',(67.8715456014017,200.43583548982,19.2513203435596)) ;
#77771 = CARTESIAN_POINT('',(67.7526891574347,200.452362610789,19.2513203435596)) ;
#77772 = CARTESIAN_POINT('Origin',(67.8715456014017,200.43583548982,19.2513203435596)) ;
#77773 = CARTESIAN_POINT('Origin',(67.8715456014017,200.43583548982,19.2513203435596)) ;
#77774 = CARTESIAN_POINT('Origin',(71.1190430355237,200.43583548982,19.2513203435596)) ;
#77775 = CARTESIAN_POINT('',(71.1190430355237,200.55583548982,19.2513203435596)) ;
#77776 = CARTESIAN_POINT('',(71.1190430355237,200.43583548982,19.3713203435596)) ;
#77777 = CARTESIAN_POINT('Ctrl Pts',(67.7733141381132,200.366911041181,19.2513203435596)) ;
#77778 = CARTESIAN_POINT('Ctrl Pts',(70.4235001348744,196.589852920486,19.2513203435596)) ;
#77779 = CARTESIAN_POINT('Ctrl Pts',(73.8497225151601,193.410388591247,19.2513203435596)) ;
#77780 = CARTESIAN_POINT('Ctrl Pts',(77.5627334640076,190.683545731522,19.2513203435596)) ;
#77781 = CARTESIAN_POINT('Ctrl Pts',(67.7733141381132,200.366911041181,19.2872242596007)) ;
#77782 = CARTESIAN_POINT('Ctrl Pts',(70.4235312581646,196.58980856342,19.2872242596007)) ;
#77783 = CARTESIAN_POINT('Ctrl Pts',(73.8496975387625,193.410406933965,19.2872242596007)) ;
#77784 = CARTESIAN_POINT('Ctrl Pts',(77.5627334640076,190.683545731522,19.2872242596007)) ;
#77785 = CARTESIAN_POINT('Ctrl Pts',(67.7980015646804,200.384233060089,19.3493570138488)) ;
#77786 = CARTESIAN_POINT('Ctrl Pts',(70.4457328536727,196.610673400983,19.3493570138488)) ;
#77787 = CARTESIAN_POINT('Ctrl Pts',(73.8695438097236,193.433249280034,19.3493570138488)) ;
#77788 = CARTESIAN_POINT('Ctrl Pts',(77.5805848589692,190.70785311862,19.3493570138488)) ;
#77789 = CARTESIAN_POINT('Ctrl Pts',(67.8495025125859,200.420368879713,19.3713203435596)) ;
#77790 = CARTESIAN_POINT('Ctrl Pts',(70.4921307140883,196.654082166003,19.3713203435596)) ;
#77791 = CARTESIAN_POINT('Ctrl Pts',(73.9108791922903,193.480949881322,19.3713203435597)) ;
#77792 = CARTESIAN_POINT('Ctrl Pts',(77.6178250208571,190.758561258377,19.3713203435597)) ;
#77793 = CARTESIAN_POINT('Ctrl Pts',(67.8715456014015,200.43583548982,19.3713203435596)) ;
#77794 = CARTESIAN_POINT('Ctrl Pts',(70.5119929186185,196.672656983123,19.3713203435596)) ;
#77795 = CARTESIAN_POINT('Ctrl Pts',(73.9285686321681,193.501368319111,19.3713203435597)) ;
#77796 = CARTESIAN_POINT('Ctrl Pts',(77.6337643041012,190.780265014789,19.3713203435597)) ;
#77797 = CARTESIAN_POINT('',(77.6337643041012,190.780265014789,19.3713203435596)) ;
#77798 = CARTESIAN_POINT('Ctrl Pts',(67.8715456014015,200.43583548982,19.3713203435596)) ;
#77799 = CARTESIAN_POINT('Ctrl Pts',(70.5119929186185,196.672656983123,19.3713203435596)) ;
#77800 = CARTESIAN_POINT('Ctrl Pts',(73.9285686321681,193.501368319111,19.3713203435597)) ;
#77801 = CARTESIAN_POINT('Ctrl Pts',(77.6337643041012,190.780265014789,19.3713203435597)) ;
#77802 = CARTESIAN_POINT('',(77.5627294322141,190.683540239233,19.2513203435596)) ;
#77803 = CARTESIAN_POINT('Origin',(77.6337643041012,190.780265014789,19.2513203435596)) ;
#77804 = CARTESIAN_POINT('Ctrl Pts',(77.5627126756809,190.683517412735,19.2513203435596)) ;
#77805 = CARTESIAN_POINT('Ctrl Pts',(73.685331711946,193.529834997272,19.2513203435595)) ;
#77806 = CARTESIAN_POINT('Ctrl Pts',(70.3960766724624,196.674672483662,19.2513203435596)) ;
#77807 = CARTESIAN_POINT('Ctrl Pts',(67.88518965836,200.208466979566,19.2513203435596)) ;
#77808 = CARTESIAN_POINT('Ctrl Pts',(67.8477299947086,200.261187294135,19.2513203435596)) ;
#77809 = CARTESIAN_POINT('Ctrl Pts',(67.8104380640988,200.314001865016,19.2513203435596)) ;
#77810 = CARTESIAN_POINT('Ctrl Pts',(67.7733141517289,200.366911050735,19.2513203435596)) ;
#77811 = CARTESIAN_POINT('Ctrl Pts',(78.1546571314538,190.609539758744,19.3713203435596)) ;
#77812 = CARTESIAN_POINT('Ctrl Pts',(77.9688509344519,190.609539758744,19.3713203435596)) ;
#77813 = CARTESIAN_POINT('Ctrl Pts',(77.7835229891055,190.670281929225,19.3713203435596)) ;
#77814 = CARTESIAN_POINT('Ctrl Pts',(77.6337643041011,190.780265014789,19.3713203435596)) ;
#77815 = CARTESIAN_POINT('Ctrl Pts',(78.1546571314538,190.573635842703,19.3713203435596)) ;
#77816 = CARTESIAN_POINT('Ctrl Pts',(77.9612372130539,190.573635842703,19.3713203435596)) ;
#77817 = CARTESIAN_POINT('Ctrl Pts',(77.7684072254185,190.63683684545,19.3713203435596)) ;
#77818 = CARTESIAN_POINT('Ctrl Pts',(77.6125119264425,190.751326672906,19.3713203435596)) ;
#77819 = CARTESIAN_POINT('Ctrl Pts',(78.1546571314538,190.511503094374,19.3411620666336)) ;
#77820 = CARTESIAN_POINT('Ctrl Pts',(77.9481590810139,190.511503094374,19.3411620666336)) ;
#77821 = CARTESIAN_POINT('Ctrl Pts',(77.7421702774708,190.579016965521,19.3411620666336)) ;
#77822 = CARTESIAN_POINT('Ctrl Pts',(77.5757340821833,190.701248048858,19.3411620666336)) ;
#77823 = CARTESIAN_POINT('Ctrl Pts',(78.1546571314538,190.489539758744,19.2782482805904)) ;
#77824 = CARTESIAN_POINT('Ctrl Pts',(77.943493133092,190.489539758744,19.2782482805904)) ;
#77825 = CARTESIAN_POINT('Ctrl Pts',(77.7329303854515,190.558552763179,19.2782482805904)) ;
#77826 = CARTESIAN_POINT('Ctrl Pts',(77.5627334640076,190.683545731522,19.2782482805904)) ;
#77827 = CARTESIAN_POINT('Ctrl Pts',(78.1546571314538,190.489539758744,19.2513203435596)) ;
#77828 = CARTESIAN_POINT('Ctrl Pts',(77.9435137257698,190.489539758744,19.2513203435596)) ;
#77829 = CARTESIAN_POINT('Ctrl Pts',(77.7329137878762,190.558564952473,19.2513203435596)) ;
#77830 = CARTESIAN_POINT('Ctrl Pts',(77.5627334640076,190.683545731522,19.2513203435596)) ;
#77831 = CARTESIAN_POINT('',(78.1546571314538,190.609539758744,19.3713203435596)) ;
#77832 = CARTESIAN_POINT('Origin',(78.0868516728187,191.282661304554,19.3713203435596)) ;
#77833 = CARTESIAN_POINT('',(78.1546571314538,190.489539758744,19.2513203435596)) ;
#77834 = CARTESIAN_POINT('Origin',(78.1546571314538,190.609539758744,19.2513203435596)) ;
#77835 = CARTESIAN_POINT('Origin',(78.0776054738855,191.254450606202,19.2513203435596)) ;
#77836 = CARTESIAN_POINT('Origin',(78.07353074889,190.609539758744,19.2513203435596)) ;
#77837 = CARTESIAN_POINT('',(80.8501919227397,190.609539758744,19.3713203435596)) ;
#77838 = CARTESIAN_POINT('',(80.8501919227397,190.489539758744,19.2513203435596)) ;
#77839 = CARTESIAN_POINT('Origin',(80.8501919227397,190.609539758744,19.2513203435596)) ;
#77840 = CARTESIAN_POINT('',(78.07353074889,190.489539758744,19.2513203435596)) ;
#77841 = CARTESIAN_POINT('',(78.07353074889,190.609539758744,19.3713203435596)) ;
#77842 = CARTESIAN_POINT('Ctrl Pts',(80.9810274260323,190.913160432898,19.3713203435596)) ;
#77843 = CARTESIAN_POINT('Ctrl Pts',(80.9947301225928,190.898658010764,19.3713203435596)) ;
#77844 = CARTESIAN_POINT('Ctrl Pts',(81.0287354417307,190.848346441009,19.3713203435596)) ;
#77845 = CARTESIAN_POINT('Ctrl Pts',(81.0384684533216,190.7434130708,19.3713203435596)) ;
#77846 = CARTESIAN_POINT('Ctrl Pts',(80.9697731322889,190.6371246451,19.3713203435596)) ;
#77847 = CARTESIAN_POINT('Ctrl Pts',(80.8900960147986,190.609539758744,19.3713203435596)) ;
#77848 = CARTESIAN_POINT('Ctrl Pts',(80.8501919227397,190.609539758744,19.3713203435596)) ;
#77849 = CARTESIAN_POINT('Ctrl Pts',(81.0071246867289,190.937818579041,19.3713203435596)) ;
#77850 = CARTESIAN_POINT('Ctrl Pts',(81.0235724505757,190.920410880242,19.3713203435596)) ;
#77851 = CARTESIAN_POINT('Ctrl Pts',(81.064410508442,190.860067831628,19.3713203435596)) ;
#77852 = CARTESIAN_POINT('Ctrl Pts',(81.0761224169453,190.734180607184,19.3713203435596)) ;
#77853 = CARTESIAN_POINT('Ctrl Pts',(80.9936901648285,190.606657008059,19.3713203435596)) ;
#77854 = CARTESIAN_POINT('Ctrl Pts',(80.8980900192786,190.573635842703,19.3713203435596)) ;
#77855 = CARTESIAN_POINT('Ctrl Pts',(80.8501919227397,190.573635842703,19.3713203435596)) ;
#77856 = CARTESIAN_POINT('Ctrl Pts',(81.0522866998738,190.980490165656,19.3411620218365)) ;
#77857 = CARTESIAN_POINT('Ctrl Pts',(81.0734496812273,190.9580920568,19.3411620218365)) ;
#77858 = CARTESIAN_POINT('Ctrl Pts',(81.1259638936544,190.880377438774,19.3411620218365)) ;
#77859 = CARTESIAN_POINT('Ctrl Pts',(81.1409889173476,190.718297935341,19.3411620218365)) ;
#77860 = CARTESIAN_POINT('Ctrl Pts',(81.0348871767947,190.5541280118,19.3411620218365)) ;
#77861 = CARTESIAN_POINT('Ctrl Pts',(80.9118213657062,190.511503148125,19.3411620218365)) ;
#77862 = CARTESIAN_POINT('Ctrl Pts',(80.8501919227397,190.511503148125,19.3411620218365)) ;
#77863 = CARTESIAN_POINT('Ctrl Pts',(81.068251094894,190.995574215667,19.2782482805904)) ;
#77864 = CARTESIAN_POINT('Ctrl Pts',(81.0910963470228,190.971395654268,19.2782482805904)) ;
#77865 = CARTESIAN_POINT('Ctrl Pts',(81.147803117456,190.887545532474,19.2782482805904)) ;
#77866 = CARTESIAN_POINT('Ctrl Pts',(81.1640483074976,190.71264204111,19.2782482805904)) ;
#77867 = CARTESIAN_POINT('Ctrl Pts',(81.049534453483,190.53547320788,19.2782482805904)) ;
#77868 = CARTESIAN_POINT('Ctrl Pts',(80.9167203640596,190.489539758744,19.2782482805904)) ;
#77869 = CARTESIAN_POINT('Ctrl Pts',(80.8501919227397,190.489539758744,19.2782482805904)) ;
#77870 = CARTESIAN_POINT('Ctrl Pts',(81.068251094894,190.995574215667,19.2513203435596)) ;
#77871 = CARTESIAN_POINT('Ctrl Pts',(81.091088922495,190.971403512111,19.2513203435596)) ;
#77872 = CARTESIAN_POINT('Ctrl Pts',(81.1477644543914,190.887550895852,19.2513203435596)) ;
#77873 = CARTESIAN_POINT('Ctrl Pts',(81.1639861403761,190.712661945505,19.2513203435596)) ;
#77874 = CARTESIAN_POINT('Ctrl Pts',(81.0494939386551,190.535514569337,19.2513203435596)) ;
#77875 = CARTESIAN_POINT('Ctrl Pts',(80.9166987428378,190.489539758744,19.2513203435596)) ;
#77876 = CARTESIAN_POINT('Ctrl Pts',(80.8501919227397,190.489539758744,19.2513203435596)) ;
#77877 = CARTESIAN_POINT('',(80.9810274260323,190.913160432898,19.3713203435596)) ;
#77878 = CARTESIAN_POINT('Ctrl Pts',(80.8501919227397,190.609539758744,19.3713203435596)) ;
#77879 = CARTESIAN_POINT('Ctrl Pts',(80.8900960147986,190.609539758744,19.3713203435596)) ;
#77880 = CARTESIAN_POINT('Ctrl Pts',(80.9697731322889,190.6371246451,19.3713203435596)) ;
#77881 = CARTESIAN_POINT('Ctrl Pts',(81.0384684533216,190.7434130708,19.3713203435596)) ;
#77882 = CARTESIAN_POINT('Ctrl Pts',(81.0287354417307,190.848346441009,19.3713203435596)) ;
#77883 = CARTESIAN_POINT('Ctrl Pts',(80.9947301225928,190.898658010764,19.3713203435596)) ;
#77884 = CARTESIAN_POINT('Ctrl Pts',(80.9810274260323,190.913160432898,19.3713203435596)) ;
#77885 = CARTESIAN_POINT('',(81.068251094894,190.995574215667,19.2513203435596)) ;
#77886 = CARTESIAN_POINT('Origin',(80.9810274260323,190.913160432898,19.2513203435596)) ;
#77887 = CARTESIAN_POINT('Ctrl Pts',(81.068251094894,190.995574215667,19.2513203435596)) ;
#77888 = CARTESIAN_POINT('Ctrl Pts',(81.1139288980579,190.947230535233,19.2513203435596)) ;
#77889 = CARTESIAN_POINT('Ctrl Pts',(81.1716387139396,190.819103811481,19.2513203435596)) ;
#77890 = CARTESIAN_POINT('Ctrl Pts',(81.1216272913293,190.614215808398,19.2513203435596)) ;
#77891 = CARTESIAN_POINT('Ctrl Pts',(80.9833036543213,190.505926496137,19.2513203435596)) ;
#77892 = CARTESIAN_POINT('Ctrl Pts',(80.8834468965772,190.489539758744,19.2513203435596)) ;
#77893 = CARTESIAN_POINT('Ctrl Pts',(80.8501919227397,190.489539758744,19.2513203435596)) ;
#77894 = CARTESIAN_POINT('Ctrl Pts',(81.068251094894,190.995574215666,19.2513203435596)) ;
#77895 = CARTESIAN_POINT('Ctrl Pts',(78.3073761253817,193.917581142398,19.2513203435596)) ;
#77896 = CARTESIAN_POINT('Ctrl Pts',(75.75172156108,197.052189907425,19.2513203435596)) ;
#77897 = CARTESIAN_POINT('Ctrl Pts',(73.6915408905803,200.497421958395,19.2513203435596)) ;
#77898 = CARTESIAN_POINT('Ctrl Pts',(81.068251094894,190.995574215666,19.2872242596007)) ;
#77899 = CARTESIAN_POINT('Ctrl Pts',(78.3073899268033,193.917566535489,19.2872242596007)) ;
#77900 = CARTESIAN_POINT('Ctrl Pts',(75.7517017249926,197.052223079236,19.2872242596007)) ;
#77901 = CARTESIAN_POINT('Ctrl Pts',(73.6915408905803,200.497421958395,19.2872242596007)) ;
#77902 = CARTESIAN_POINT('Ctrl Pts',(81.0463300781923,190.974862017566,19.3493569192823)) ;
#77903 = CARTESIAN_POINT('Ctrl Pts',(78.2843665844062,193.898020997724,19.3493569192823)) ;
#77904 = CARTESIAN_POINT('Ctrl Pts',(75.7274024340457,197.034095745875,19.3493569192823)) ;
#77905 = CARTESIAN_POINT('Ctrl Pts',(73.6656572824995,200.48194407236,19.3493569192823)) ;
#77906 = CARTESIAN_POINT('Ctrl Pts',(81.0006003715548,190.931654042505,19.3713203435596)) ;
#77907 = CARTESIAN_POINT('Ctrl Pts',(78.2363739466475,193.857208024423,19.3713203435596)) ;
#77908 = CARTESIAN_POINT('Ctrl Pts',(75.676658712843,196.996368164185,19.3713203435596)) ;
#77909 = CARTESIAN_POINT('Ctrl Pts',(73.6116611645114,200.449655461051,19.3713203435596)) ;
#77910 = CARTESIAN_POINT('Ctrl Pts',(80.9810274260323,190.913160432897,19.3713203435596)) ;
#77911 = CARTESIAN_POINT('Ctrl Pts',(78.215833902103,193.839737956291,19.3713203435596)) ;
#77912 = CARTESIAN_POINT('Ctrl Pts',(75.6549375918393,196.980223763859,19.3713203435596)) ;
#77913 = CARTESIAN_POINT('Ctrl Pts',(73.5885500808522,200.43583548982,19.3713203435596)) ;
#77914 = CARTESIAN_POINT('Ctrl Pts',(73.6915408905803,200.497421958395,19.2513203435596)) ;
#77915 = CARTESIAN_POINT('Ctrl Pts',(75.75172156108,197.052189907425,19.2513203435596)) ;
#77916 = CARTESIAN_POINT('Ctrl Pts',(78.3073761253817,193.917581142398,19.2513203435596)) ;
#77917 = CARTESIAN_POINT('Ctrl Pts',(81.068251094894,190.995574215666,19.2513203435596)) ;
#77918 = CARTESIAN_POINT('Ctrl Pts',(80.9810274260323,190.913160432897,19.3713203435596)) ;
#77919 = CARTESIAN_POINT('Ctrl Pts',(78.215833902103,193.839737956291,19.3713203435596)) ;
#77920 = CARTESIAN_POINT('Ctrl Pts',(75.6549375918393,196.980223763859,19.3713203435596)) ;
#77921 = CARTESIAN_POINT('Ctrl Pts',(73.5885500808522,200.43583548982,19.3713203435596)) ;
#77922 = CARTESIAN_POINT('Ctrl Pts',(67.8715456014017,200.55583548982,17.9913203435596)) ;
#77923 = CARTESIAN_POINT('Ctrl Pts',(67.8466022358902,200.55583548982,17.9913203435596)) ;
#77924 = CARTESIAN_POINT('Ctrl Pts',(67.8093588147496,200.543700298089,17.9913203435596)) ;
#77925 = CARTESIAN_POINT('Ctrl Pts',(67.7643817760585,200.499332389917,17.9913203435596)) ;
#77926 = CARTESIAN_POINT('Ctrl Pts',(67.7435398814255,200.437381726819,17.9913203435596)) ;
#77927 = CARTESIAN_POINT('Ctrl Pts',(67.7589874071544,200.387329568627,17.9913203435596)) ;
#77928 = CARTESIAN_POINT('Ctrl Pts',(67.7733141381135,200.366911041181,17.9913203435596)) ;
#77929 = CARTESIAN_POINT('Ctrl Pts',(67.8715456014017,200.55583548982,17.9554164275186)) ;
#77930 = CARTESIAN_POINT('Ctrl Pts',(67.8466819509688,200.55583548982,17.9554164275186)) ;
#77931 = CARTESIAN_POINT('Ctrl Pts',(67.8094573381231,200.543546439635,17.9554164275186)) ;
#77932 = CARTESIAN_POINT('Ctrl Pts',(67.764591266304,200.499257277487,17.9554164275186)) ;
#77933 = CARTESIAN_POINT('Ctrl Pts',(67.7437368491879,200.437352434046,17.9554164275186)) ;
#77934 = CARTESIAN_POINT('Ctrl Pts',(67.7590331931363,200.38726431422,17.9554164275186)) ;
#77935 = CARTESIAN_POINT('Ctrl Pts',(67.7733141381135,200.366911041181,17.9554164275186)) ;
#77936 = CARTESIAN_POINT('Ctrl Pts',(67.8715456014017,200.585993742446,17.8932836500338)) ;
#77937 = CARTESIAN_POINT('Ctrl Pts',(67.84031507213,200.585993742446,17.8932836500338)) ;
#77938 = CARTESIAN_POINT('Ctrl Pts',(67.7937073322049,200.570844316766,17.8932836500338)) ;
#77939 = CARTESIAN_POINT('Ctrl Pts',(67.7374010671215,200.515307716645,17.8932836500337)) ;
#77940 = CARTESIAN_POINT('Ctrl Pts',(67.7113241079541,200.437777096827,17.8932836500338)) ;
#77941 = CARTESIAN_POINT('Ctrl Pts',(67.7306888356429,200.375154204976,17.8932836500338)) ;
#77942 = CARTESIAN_POINT('Ctrl Pts',(67.7486267273993,200.349589033396,17.8932836500338)) ;
#77943 = CARTESIAN_POINT('Ctrl Pts',(67.8715456014017,200.648907552789,17.8713203435596)) ;
#77944 = CARTESIAN_POINT('Ctrl Pts',(67.8272446988906,200.648907552789,17.8713203435596)) ;
#77945 = CARTESIAN_POINT('Ctrl Pts',(67.7611125593011,200.62738239895,17.8713203435596)) ;
#77946 = CARTESIAN_POINT('Ctrl Pts',(67.6812353674285,200.548591407486,17.8713203435596)) ;
#77947 = CARTESIAN_POINT('Ctrl Pts',(67.6442302870083,200.43858519642,17.8713203435596)) ;
#77948 = CARTESIAN_POINT('Ctrl Pts',(67.671680636309,200.349717723304,17.8713203435596)) ;
#77949 = CARTESIAN_POINT('Ctrl Pts',(67.6971257636407,200.313453202648,17.8713203435596)) ;
#77950 = CARTESIAN_POINT('Ctrl Pts',(67.8715456014017,200.67583548982,17.8713203435596)) ;
#77951 = CARTESIAN_POINT('Ctrl Pts',(67.8216588703786,200.67583548982,17.8713203435596)) ;
#77952 = CARTESIAN_POINT('Ctrl Pts',(67.7471720280976,200.651565106359,17.8713203435596)) ;
#77953 = CARTESIAN_POINT('Ctrl Pts',(67.6572179507153,200.562829290015,17.8713203435596)) ;
#77954 = CARTESIAN_POINT('Ctrl Pts',(67.6155341614493,200.438927963818,17.8713203435596)) ;
#77955 = CARTESIAN_POINT('Ctrl Pts',(67.646429212907,200.338823647433,17.8713203435596)) ;
#77956 = CARTESIAN_POINT('Ctrl Pts',(67.6750826748252,200.297986592541,17.8713203435596)) ;
#77957 = CARTESIAN_POINT('',(67.654399260129,200.537671106355,17.8713203435596)) ;
#77958 = CARTESIAN_POINT('',(67.6638006826676,200.555777405267,17.8713203435596)) ;
#77959 = CARTESIAN_POINT('Origin',(67.8164545295421,200.45482568124,17.8713203435596)) ;
#77960 = CARTESIAN_POINT('',(67.8715456014017,200.67583548982,17.8713203435596)) ;
#77961 = CARTESIAN_POINT('Ctrl Pts',(67.6638006825543,200.55577740507,17.8713203435596)) ;
#77962 = CARTESIAN_POINT('Ctrl Pts',(67.6682504093187,200.563528431557,17.8713203435596)) ;
#77963 = CARTESIAN_POINT('Ctrl Pts',(67.686751282339,200.59196264747,17.8713203435596)) ;
#77964 = CARTESIAN_POINT('Ctrl Pts',(67.7471720280976,200.651565106359,17.8713203435596)) ;
#77965 = CARTESIAN_POINT('Ctrl Pts',(67.8216588703786,200.67583548982,17.8713203435596)) ;
#77966 = CARTESIAN_POINT('Ctrl Pts',(67.8715456014017,200.67583548982,17.8713203435596)) ;
#77967 = CARTESIAN_POINT('',(67.8715456014017,200.55583548982,17.9913203435596)) ;
#77968 = CARTESIAN_POINT('Origin',(67.8715456014017,200.67583548982,17.9913203435596)) ;
#77969 = CARTESIAN_POINT('',(67.7733141381135,200.366911041181,17.9913203435596)) ;
#77970 = CARTESIAN_POINT('Ctrl Pts',(67.8715456014017,200.55583548982,17.9913203435596)) ;
#77971 = CARTESIAN_POINT('Ctrl Pts',(67.8528373343895,200.55583548982,17.9913203435596)) ;
#77972 = CARTESIAN_POINT('Ctrl Pts',(67.8091125279312,200.54551389311,17.9913203435596)) ;
#77973 = CARTESIAN_POINT('Ctrl Pts',(67.7626667658301,200.499540877992,17.9913203435596)) ;
#77974 = CARTESIAN_POINT('Ctrl Pts',(67.7455875249419,200.431050106803,17.9913203435596)) ;
#77975 = CARTESIAN_POINT('Ctrl Pts',(67.7589868382377,200.387330379449,17.9913203435596)) ;
#77976 = CARTESIAN_POINT('Ctrl Pts',(67.7733141381135,200.366911041181,17.9913203435596)) ;
#77977 = CARTESIAN_POINT('',(67.6750826748252,200.297986592541,17.8713203435596)) ;
#77978 = CARTESIAN_POINT('Origin',(67.6750826748252,200.297986592541,17.9913203435596)) ;
#77979 = CARTESIAN_POINT('Ctrl Pts',(67.6750826748252,200.297986592541,17.8713203435596)) ;
#77980 = CARTESIAN_POINT('Ctrl Pts',(67.646429212907,200.338823647433,17.8713203435596)) ;
#77981 = CARTESIAN_POINT('Ctrl Pts',(67.6204094720538,200.423131271072,17.8713203435596)) ;
#77982 = CARTESIAN_POINT('Ctrl Pts',(67.6399564441711,200.506741474643,17.8713203435596)) ;
#77983 = CARTESIAN_POINT('Ctrl Pts',(67.6543992598854,200.537671105833,17.8713203435596)) ;
#77984 = CARTESIAN_POINT('Ctrl Pts',(67.7733141381135,200.366911041181,17.9913203435596)) ;
#77985 = CARTESIAN_POINT('Ctrl Pts',(67.7733141381135,200.366911041181,19.5033203435596)) ;
#77986 = CARTESIAN_POINT('Ctrl Pts',(67.7589868382377,200.387330379449,17.9913203435596)) ;
#77987 = CARTESIAN_POINT('Ctrl Pts',(67.7589868382377,200.387330379449,19.5033203435596)) ;
#77988 = CARTESIAN_POINT('Ctrl Pts',(67.7455875249419,200.431050106803,17.9913203435596)) ;
#77989 = CARTESIAN_POINT('Ctrl Pts',(67.7455875249419,200.431050106803,19.5033203435596)) ;
#77990 = CARTESIAN_POINT('Ctrl Pts',(67.7626667658301,200.499540877992,17.9913203435596)) ;
#77991 = CARTESIAN_POINT('Ctrl Pts',(67.7626667658301,200.499540877992,19.5033203435596)) ;
#77992 = CARTESIAN_POINT('Ctrl Pts',(67.8091125279312,200.54551389311,17.9913203435596)) ;
#77993 = CARTESIAN_POINT('Ctrl Pts',(67.8091125279312,200.54551389311,19.5033203435596)) ;
#77994 = CARTESIAN_POINT('Ctrl Pts',(67.8528373343895,200.55583548982,17.9913203435596)) ;
#77995 = CARTESIAN_POINT('Ctrl Pts',(67.8528373343895,200.55583548982,19.5033203435596)) ;
#77996 = CARTESIAN_POINT('Ctrl Pts',(67.8715456014017,200.55583548982,17.9913203435596)) ;
#77997 = CARTESIAN_POINT('Ctrl Pts',(67.8715456014017,200.55583548982,19.5033203435596)) ;
#77998 = CARTESIAN_POINT('',(67.7733141381135,200.366911041181,19.2513203435596)) ;
#77999 = CARTESIAN_POINT('',(67.8715456014017,200.55583548982,17.9913203435596)) ;
#78000 = CARTESIAN_POINT('Ctrl Pts',(67.7733141381135,200.366911041181,17.9913203435596)) ;
#78001 = CARTESIAN_POINT('Ctrl Pts',(70.4189965819413,196.596271406283,17.9913203435596)) ;
#78002 = CARTESIAN_POINT('Ctrl Pts',(73.8443753644747,193.414315549682,17.9913203435596)) ;
#78003 = CARTESIAN_POINT('Ctrl Pts',(77.5627334640076,190.683545731522,17.9913203435596)) ;
#78004 = CARTESIAN_POINT('Ctrl Pts',(67.7733141381135,200.366911041181,17.9554164275186)) ;
#78005 = CARTESIAN_POINT('Ctrl Pts',(70.4189655115399,196.596315687972,17.9554164275186)) ;
#78006 = CARTESIAN_POINT('Ctrl Pts',(73.8444003768411,193.414297180549,17.9554164275186)) ;
#78007 = CARTESIAN_POINT('Ctrl Pts',(77.5627334640076,190.683545731522,17.9554164275186)) ;
#78008 = CARTESIAN_POINT('Ctrl Pts',(67.7486267295111,200.349589034877,17.8932836469385)) ;
#78009 = CARTESIAN_POINT('Ctrl Pts',(70.3967597097377,196.575456883448,17.8932836469385)) ;
#78010 = CARTESIAN_POINT('Ctrl Pts',(73.8245512460258,193.39145696199,17.8932836469385)) ;
#78011 = CARTESIAN_POINT('Ctrl Pts',(77.5448820820363,190.659238362113,17.8932836469385)) ;
#78012 = CARTESIAN_POINT('Ctrl Pts',(67.6971257636408,200.313453202648,17.8713203435596)) ;
#78013 = CARTESIAN_POINT('Ctrl Pts',(70.3503531595038,196.532060464991,17.8713203435596)) ;
#78014 = CARTESIAN_POINT('Ctrl Pts',(73.7832099528935,193.343760674206,17.8713203435596)) ;
#78015 = CARTESIAN_POINT('Ctrl Pts',(77.5076419071581,190.608530204668,17.8713203435596)) ;
#78016 = CARTESIAN_POINT('Ctrl Pts',(67.6750826748252,200.297986592541,17.8713203435596)) ;
#78017 = CARTESIAN_POINT('Ctrl Pts',(70.3304872489213,196.513490929755,17.8713203435596)) ;
#78018 = CARTESIAN_POINT('Ctrl Pts',(73.7655179925946,193.323344087419,17.8713203435596)) ;
#78019 = CARTESIAN_POINT('Ctrl Pts',(77.4917026239141,190.586826448256,17.8713203435596)) ;
#78020 = CARTESIAN_POINT('',(77.5627334640076,190.683545731522,17.9913203435596)) ;
#78021 = CARTESIAN_POINT('Ctrl Pts',(67.7733141381135,200.366911041181,17.9913203435596)) ;
#78022 = CARTESIAN_POINT('Ctrl Pts',(70.4189965819413,196.596271406283,17.9913203435596)) ;
#78023 = CARTESIAN_POINT('Ctrl Pts',(73.8443753644747,193.414315549682,17.9913203435596)) ;
#78024 = CARTESIAN_POINT('Ctrl Pts',(77.5627334640076,190.683545731522,17.9913203435596)) ;
#78025 = CARTESIAN_POINT('',(77.4917026239141,190.586826448256,17.8713203435596)) ;
#78026 = CARTESIAN_POINT('Origin',(77.4917026239141,190.586826448256,17.9913203435596)) ;
#78027 = CARTESIAN_POINT('Ctrl Pts',(77.4917026239141,190.586826448256,17.8713203435596)) ;
#78028 = CARTESIAN_POINT('Ctrl Pts',(73.7655179925946,193.323344087419,17.8713203435596)) ;
#78029 = CARTESIAN_POINT('Ctrl Pts',(70.3304872489213,196.513490929755,17.8713203435596)) ;
#78030 = CARTESIAN_POINT('Ctrl Pts',(67.6750826748252,200.297986592541,17.8713203435596)) ;
#78031 = CARTESIAN_POINT('Ctrl Pts',(78.1546571314538,190.369539758744,17.8713203435596)) ;
#78032 = CARTESIAN_POINT('Ctrl Pts',(77.9181765170877,190.369539758744,17.8713203435596)) ;
#78033 = CARTESIAN_POINT('Ctrl Pts',(77.6823045866469,190.44684797572,17.8713203435596)) ;
#78034 = CARTESIAN_POINT('Ctrl Pts',(77.4917026239141,190.586826448256,17.8713203435596)) ;
#78035 = CARTESIAN_POINT('Ctrl Pts',(78.1546571314538,190.405443674785,17.8713203435596)) ;
#78036 = CARTESIAN_POINT('Ctrl Pts',(77.9257902384857,190.405443674785,17.8713203435596)) ;
#78037 = CARTESIAN_POINT('Ctrl Pts',(77.6974203503338,190.480293059496,17.8713203435596)) ;
#78038 = CARTESIAN_POINT('Ctrl Pts',(77.5129550015728,190.615764790139,17.8713203435596)) ;
#78039 = CARTESIAN_POINT('Ctrl Pts',(78.1546571314538,190.467576448569,17.9014785992702)) ;
#78040 = CARTESIAN_POINT('Ctrl Pts',(77.9388683705259,190.467576448569,17.9014785992702)) ;
#78041 = CARTESIAN_POINT('Ctrl Pts',(77.7236573133492,190.538112959941,17.9014785992701)) ;
#78042 = CARTESIAN_POINT('Ctrl Pts',(77.5497328608997,190.665843434703,17.9014785992701)) ;
#78043 = CARTESIAN_POINT('Ctrl Pts',(78.1546571314538,190.489539758744,17.9643924065289)) ;
#78044 = CARTESIAN_POINT('Ctrl Pts',(77.9435343184478,190.489539758744,17.9643924065289)) ;
#78045 = CARTESIAN_POINT('Ctrl Pts',(77.7328971903008,190.558577141766,17.9643924065289)) ;
#78046 = CARTESIAN_POINT('Ctrl Pts',(77.5627334640076,190.683545731522,17.9643924065289)) ;
#78047 = CARTESIAN_POINT('Ctrl Pts',(78.1546571314538,190.489539758744,17.9913203435596)) ;
#78048 = CARTESIAN_POINT('Ctrl Pts',(77.94351372577,190.489539758744,17.9913203435596)) ;
#78049 = CARTESIAN_POINT('Ctrl Pts',(77.7329137878761,190.558564952473,17.9913203435596)) ;
#78050 = CARTESIAN_POINT('Ctrl Pts',(77.5627334640076,190.683545731522,17.9913203435596)) ;
#78051 = CARTESIAN_POINT('',(78.1546571314538,190.489539758744,17.9913203435596)) ;
#78052 = CARTESIAN_POINT('Origin',(78.0776054738942,191.254450606233,17.9913203435596)) ;
#78053 = CARTESIAN_POINT('',(78.1546571314538,190.369539758744,17.8713203435596)) ;
#78054 = CARTESIAN_POINT('Origin',(78.1546571314538,190.369539758744,17.9913203435596)) ;
#78055 = CARTESIAN_POINT('Origin',(78.0683592750173,191.22623990799,17.8713203435596)) ;
#78056 = CARTESIAN_POINT('Origin',(73.6548295654295,190.369539758744,17.9913203435596)) ;
#78057 = CARTESIAN_POINT('',(80.8501919227397,190.489539758744,17.9913203435596)) ;
#78058 = CARTESIAN_POINT('',(80.8501919227397,190.369539758744,17.8713203435596)) ;
#78059 = CARTESIAN_POINT('Origin',(80.8501919227397,190.369539758744,17.9913203435596)) ;
#78060 = CARTESIAN_POINT('',(73.6548295654295,190.369539758744,17.8713203435596)) ;
#78061 = CARTESIAN_POINT('',(73.6548295654295,190.489539758744,17.9913203435596)) ;
#78062 = CARTESIAN_POINT('Ctrl Pts',(81.1554747637557,191.077987998436,17.8713203435596)) ;
#78063 = CARTESIAN_POINT('Ctrl Pts',(81.2513936396798,190.976471043503,17.8713203435596)) ;
#78064 = CARTESIAN_POINT('Ctrl Pts',(81.316638910935,190.723383706498,17.8713203435596)) ;
#78065 = CARTESIAN_POINT('Ctrl Pts',(81.1283155314175,190.433679019485,17.8713203435596)) ;
#78066 = CARTESIAN_POINT('Ctrl Pts',(80.9433014708773,190.369539758744,17.8713203435596)) ;
#78067 = CARTESIAN_POINT('Ctrl Pts',(80.8501919227397,190.369539758744,17.8713203435596)) ;
#78068 = CARTESIAN_POINT('Ctrl Pts',(81.129377503059,191.053329852293,17.8713203435596)) ;
#78069 = CARTESIAN_POINT('Ctrl Pts',(81.2170611771247,190.960528727356,17.8713203435596)) ;
#78070 = CARTESIAN_POINT('Ctrl Pts',(81.2766261409266,190.728987825454,17.8713203435596)) ;
#78071 = CARTESIAN_POINT('Ctrl Pts',(81.1044711159146,190.464155266563,17.8713203435596)) ;
#78072 = CARTESIAN_POINT('Ctrl Pts',(80.9353074663972,190.405443674785,17.8713203435596)) ;
#78073 = CARTESIAN_POINT('Ctrl Pts',(80.8501919227397,190.405443674785,17.8713203435596)) ;
#78074 = CARTESIAN_POINT('Ctrl Pts',(81.0842154748565,191.01065825145,17.9014786480176)) ;
#78075 = CARTESIAN_POINT('Ctrl Pts',(81.1577534964021,190.932828356686,17.9014786480176)) ;
#78076 = CARTESIAN_POINT('Ctrl Pts',(81.2077940098548,190.738838272952,17.9014786480176)) ;
#78077 = CARTESIAN_POINT('Ctrl Pts',(81.0634124040283,190.51673086814,17.9014786480176)) ;
#78078 = CARTESIAN_POINT('Ctrl Pts',(80.9215761199696,190.467576390079,17.9014786480176)) ;
#78079 = CARTESIAN_POINT('Ctrl Pts',(80.8501919227397,190.467576390079,17.9014786480176)) ;
#78080 = CARTESIAN_POINT('Ctrl Pts',(81.068251094894,190.995574215667,17.9643924065289)) ;
#78081 = CARTESIAN_POINT('Ctrl Pts',(81.1367423041135,190.923085678529,17.9643924065289)) ;
#78082 = CARTESIAN_POINT('Ctrl Pts',(81.1832816311425,190.742253295466,17.9643924065289)) ;
#78083 = CARTESIAN_POINT('Ctrl Pts',(81.0488084622043,190.535388191718,17.9643924065289)) ;
#78084 = CARTESIAN_POINT('Ctrl Pts',(80.9166771216162,190.489539758744,17.9643924065289)) ;
#78085 = CARTESIAN_POINT('Ctrl Pts',(80.8501919227397,190.489539758744,17.9643924065289)) ;
#78086 = CARTESIAN_POINT('Ctrl Pts',(81.068251094894,190.995574215667,17.9913203435596)) ;
#78087 = CARTESIAN_POINT('Ctrl Pts',(81.1367645776969,190.923062105,17.9913203435596)) ;
#78088 = CARTESIAN_POINT('Ctrl Pts',(81.1833683428792,190.742285435711,17.9913203435596)) ;
#78089 = CARTESIAN_POINT('Ctrl Pts',(81.0488516432238,190.535353516416,17.9913203435596)) ;
#78090 = CARTESIAN_POINT('Ctrl Pts',(80.916698742838,190.489539758744,17.9913203435596)) ;
#78091 = CARTESIAN_POINT('Ctrl Pts',(80.8501919227397,190.489539758744,17.9913203435596)) ;
#78092 = CARTESIAN_POINT('',(81.068251094894,190.995574215667,17.9913203435596)) ;
#78093 = CARTESIAN_POINT('Ctrl Pts',(80.8501919227397,190.489539758744,17.9913203435596)) ;
#78094 = CARTESIAN_POINT('Ctrl Pts',(80.916698742838,190.489539758744,17.9913203435596)) ;
#78095 = CARTESIAN_POINT('Ctrl Pts',(81.0488516432238,190.535353516416,17.9913203435596)) ;
#78096 = CARTESIAN_POINT('Ctrl Pts',(81.1833683428792,190.742285435711,17.9913203435596)) ;
#78097 = CARTESIAN_POINT('Ctrl Pts',(81.1367645776969,190.923062105,17.9913203435596)) ;
#78098 = CARTESIAN_POINT('Ctrl Pts',(81.068251094894,190.995574215667,17.9913203435596)) ;
#78099 = CARTESIAN_POINT('',(81.1554747637557,191.077987998436,17.8713203435596)) ;
#78100 = CARTESIAN_POINT('Origin',(81.1554747637557,191.077987998436,17.9913203435596)) ;
#78101 = CARTESIAN_POINT('Ctrl Pts',(81.1554747637557,191.077987998436,17.8713203435596)) ;
#78102 = CARTESIAN_POINT('Ctrl Pts',(81.2513936396798,190.976471043503,17.8713203435596)) ;
#78103 = CARTESIAN_POINT('Ctrl Pts',(81.316638910935,190.723383706498,17.8713203435596)) ;
#78104 = CARTESIAN_POINT('Ctrl Pts',(81.1283155314175,190.433679019485,17.8713203435596)) ;
#78105 = CARTESIAN_POINT('Ctrl Pts',(80.9433014708773,190.369539758744,17.8713203435596)) ;
#78106 = CARTESIAN_POINT('Ctrl Pts',(80.8501919227397,190.369539758744,17.8713203435596)) ;
#78107 = CARTESIAN_POINT('Ctrl Pts',(81.068251094894,190.995574215667,17.9913203435596)) ;
#78108 = CARTESIAN_POINT('Ctrl Pts',(78.3107281673276,193.914033466429,17.9913203435596)) ;
#78109 = CARTESIAN_POINT('Ctrl Pts',(75.7551903021708,197.046389145311,17.9913203435596)) ;
#78110 = CARTESIAN_POINT('Ctrl Pts',(73.6915408905803,200.497421958395,17.9913203435596)) ;
#78111 = CARTESIAN_POINT('Ctrl Pts',(81.068251094894,190.995574215667,17.9554164275186)) ;
#78112 = CARTESIAN_POINT('Ctrl Pts',(78.3107143826626,193.914048055604,17.9554164275186)) ;
#78113 = CARTESIAN_POINT('Ctrl Pts',(75.7552101716563,197.046355917648,17.9554164275186)) ;
#78114 = CARTESIAN_POINT('Ctrl Pts',(73.6915408905803,200.497421958395,17.9554164275186)) ;
#78115 = CARTESIAN_POINT('Ctrl Pts',(81.0901720991602,191.016286402018,17.8932837473092)) ;
#78116 = CARTESIAN_POINT('Ctrl Pts',(78.3337363742652,193.933594998089,17.8932837473092)) ;
#78117 = CARTESIAN_POINT('Ctrl Pts',(75.7795067803935,197.064487703123,17.8932837473092)) ;
#78118 = CARTESIAN_POINT('Ctrl Pts',(73.7174244839775,200.51289983565,17.8932837473092)) ;
#78119 = CARTESIAN_POINT('Ctrl Pts',(81.1359018182332,191.059494388828,17.8713203435596)) ;
#78120 = CARTESIAN_POINT('Ctrl Pts',(78.3817262769825,193.974410890966,17.8713203435596)) ;
#78121 = CARTESIAN_POINT('Ctrl Pts',(75.8302450401957,197.102224451227,17.8713203435596)) ;
#78122 = CARTESIAN_POINT('Ctrl Pts',(73.7714206166491,200.545188455739,17.8713203435596)) ;
#78123 = CARTESIAN_POINT('Ctrl Pts',(81.1554747637557,191.077987998436,17.8713203435596)) ;
#78124 = CARTESIAN_POINT('Ctrl Pts',(78.4022651473499,193.991882201803,17.8713203435596)) ;
#78125 = CARTESIAN_POINT('Ctrl Pts',(75.8519638209093,197.118372765211,17.8713203435596)) ;
#78126 = CARTESIAN_POINT('Ctrl Pts',(73.7945317003083,200.55900842697,17.8713203435596)) ;
#78127 = CARTESIAN_POINT('Ctrl Pts',(73.7945317003083,200.55900842697,17.8713203435596)) ;
#78128 = CARTESIAN_POINT('Ctrl Pts',(75.8519638209093,197.118372765211,17.8713203435596)) ;
#78129 = CARTESIAN_POINT('Ctrl Pts',(78.4022651473499,193.991882201803,17.8713203435596)) ;
#78130 = CARTESIAN_POINT('Ctrl Pts',(81.1554747637557,191.077987998436,17.8713203435596)) ;
#78131 = CARTESIAN_POINT('Ctrl Pts',(81.068251094894,190.995574215667,17.9913203435596)) ;
#78132 = CARTESIAN_POINT('Ctrl Pts',(78.3107281673276,193.914033466429,17.9913203435596)) ;
#78133 = CARTESIAN_POINT('Ctrl Pts',(75.7551903021708,197.046389145311,17.9913203435596)) ;
#78134 = CARTESIAN_POINT('Ctrl Pts',(73.6915408905803,200.497421958395,17.9913203435596)) ;
#78135 = CARTESIAN_POINT('Origin',(66.7003418520632,200.67583548982,17.9913203435596)) ;
#78136 = CARTESIAN_POINT('',(66.7003418520632,200.67583548982,17.8713203435596)) ;
#78137 = CARTESIAN_POINT('',(66.7003418520632,200.55583548982,17.9913203435596)) ;
#78138 = CARTESIAN_POINT('Ctrl Pts',(81.068251094894,190.995574215667,17.9913203435596)) ;
#78139 = CARTESIAN_POINT('Ctrl Pts',(81.068251094894,190.995574215667,19.5033203435596)) ;
#78140 = CARTESIAN_POINT('Ctrl Pts',(81.1139288980579,190.947230535233,17.9913203435596)) ;
#78141 = CARTESIAN_POINT('Ctrl Pts',(81.1139288980579,190.947230535233,19.5033203435596)) ;
#78142 = CARTESIAN_POINT('Ctrl Pts',(81.1716387139396,190.819103811481,17.9913203435596)) ;
#78143 = CARTESIAN_POINT('Ctrl Pts',(81.1716387139396,190.819103811481,19.5033203435596)) ;
#78144 = CARTESIAN_POINT('Ctrl Pts',(81.1216272913293,190.614215808398,17.9913203435596)) ;
#78145 = CARTESIAN_POINT('Ctrl Pts',(81.1216272913293,190.614215808398,19.5033203435596)) ;
#78146 = CARTESIAN_POINT('Ctrl Pts',(80.9833036543213,190.505926496137,17.9913203435596)) ;
#78147 = CARTESIAN_POINT('Ctrl Pts',(80.9833036543213,190.505926496137,19.5033203435596)) ;
#78148 = CARTESIAN_POINT('Ctrl Pts',(80.8834468965772,190.489539758744,17.9913203435596)) ;
#78149 = CARTESIAN_POINT('Ctrl Pts',(80.8834468965772,190.489539758744,19.5033203435596)) ;
#78150 = CARTESIAN_POINT('Ctrl Pts',(80.8501919227397,190.489539758744,17.9913203435596)) ;
#78151 = CARTESIAN_POINT('Ctrl Pts',(80.8501919227397,190.489539758744,19.5033203435596)) ;
#78152 = CARTESIAN_POINT('',(80.8501919227397,190.489539758744,17.9913203435596)) ;
#78153 = CARTESIAN_POINT('',(81.068251094894,190.995574215667,19.2513203435596)) ;
#78154 = CARTESIAN_POINT('Ctrl Pts',(77.8285014478222,190.489539758744,17.8547522895864)) ;
#78155 = CARTESIAN_POINT('Ctrl Pts',(77.8285014478222,190.489539758744,32.8746339543542)) ;
#78156 = CARTESIAN_POINT('Ctrl Pts',(73.8355349189945,193.386814152385,17.8547522895863)) ;
#78157 = CARTESIAN_POINT('Ctrl Pts',(73.8355349189945,193.386814152385,32.8746339543541)) ;
#78158 = CARTESIAN_POINT('Ctrl Pts',(70.4532522157592,196.594204259059,17.8547522895864)) ;
#78159 = CARTESIAN_POINT('Ctrl Pts',(70.4532522157592,196.594204259059,32.8746339543542)) ;
#78160 = CARTESIAN_POINT('Ctrl Pts',(67.88518965836,200.208466979566,17.8547522895864)) ;
#78161 = CARTESIAN_POINT('Ctrl Pts',(67.88518965836,200.208466979566,32.8746339543542)) ;
#78162 = CARTESIAN_POINT('Ctrl Pts',(67.8032385132701,200.323804110956,17.8547522895864)) ;
#78163 = CARTESIAN_POINT('Ctrl Pts',(67.8032385132701,200.323804110956,32.8746339543542)) ;
#78164 = CARTESIAN_POINT('Ctrl Pts',(67.7220901562832,200.439592363042,17.8547522895864)) ;
#78165 = CARTESIAN_POINT('Ctrl Pts',(67.7220901562832,200.439592363042,32.8746339543542)) ;
#78166 = CARTESIAN_POINT('Ctrl Pts',(67.6417475736103,200.555835489811,17.8547522895864)) ;
#78167 = CARTESIAN_POINT('Ctrl Pts',(67.6417475736103,200.555835489811,32.8746339543542)) ;
#78168 = CARTESIAN_POINT('',(77.5627334640076,190.683545731522,17.9913203435596)) ;
#78169 = CARTESIAN_POINT('Origin',(81.5507230003364,190.489539758744,23.8713203435596)) ;
#78170 = CARTESIAN_POINT('',(78.1546571314538,190.489539758744,19.2513203435596)) ;
#78171 = CARTESIAN_POINT('Ctrl Pts',(78.1546571314538,190.489539758744,17.9913203435596)) ;
#78172 = CARTESIAN_POINT('Ctrl Pts',(78.1546571314538,190.489539758744,19.5033203435596)) ;
#78173 = CARTESIAN_POINT('Ctrl Pts',(77.9435093125031,190.489539758744,17.9913203435596)) ;
#78174 = CARTESIAN_POINT('Ctrl Pts',(77.9435093125031,190.489539758744,19.5033203435596)) ;
#78175 = CARTESIAN_POINT('Ctrl Pts',(77.7329173449427,190.558562340156,17.9913203435596)) ;
#78176 = CARTESIAN_POINT('Ctrl Pts',(77.7329173449427,190.558562340156,19.5033203435596)) ;
#78177 = CARTESIAN_POINT('Ctrl Pts',(77.5627334640076,190.683545731522,17.9913203435596)) ;
#78178 = CARTESIAN_POINT('Ctrl Pts',(77.5627334640076,190.683545731522,19.5033203435596)) ;
#78179 = CARTESIAN_POINT('Origin',(65.7589361305225,212.963038649314,17.8713203435596)) ;
#78180 = CARTESIAN_POINT('',(60.9557289922431,214.062457733496,17.8713203435596)) ;
#78181 = CARTESIAN_POINT('',(61.2615982170329,212.685341204933,17.8713203435596)) ;
#78182 = CARTESIAN_POINT('Origin',(186.600966963329,306.450327238289,17.8713203435596)) ;
#78183 = CARTESIAN_POINT('',(70.2265094709067,213.162319271896,17.8713203435596)) ;
#78184 = CARTESIAN_POINT('',(67.5325794977657,213.423884085911,17.8713203435596)) ;
#78185 = CARTESIAN_POINT('',(70.3877178199639,213.005540169192,17.8713203435596)) ;
#78186 = CARTESIAN_POINT('Ctrl Pts',(70.3877178199639,213.005540169192,17.8713203435596)) ;
#78187 = CARTESIAN_POINT('Ctrl Pts',(70.3834041808396,213.039967616326,17.8713203435596)) ;
#78188 = CARTESIAN_POINT('Ctrl Pts',(70.3494702400649,213.117382991064,17.8713203435596)) ;
#78189 = CARTESIAN_POINT('Ctrl Pts',(70.2725551198838,213.157848509207,17.8713203435596)) ;
#78190 = CARTESIAN_POINT('Ctrl Pts',(70.2265094709067,213.162319271896,17.8713203435596)) ;
#78191 = CARTESIAN_POINT('',(74.071363112532,201.997275065426,17.8713203435596)) ;
#78192 = CARTESIAN_POINT('Ctrl Pts',(74.0713631125318,201.997275065426,17.8713203435596)) ;
#78193 = CARTESIAN_POINT('Ctrl Pts',(72.9854321297061,203.939567940643,17.8713203435596)) ;
#78194 = CARTESIAN_POINT('Ctrl Pts',(71.4053737386935,207.523894544389,17.8713203435596)) ;
#78195 = CARTESIAN_POINT('Ctrl Pts',(70.5952077140308,211.34954921747,17.8713203435596)) ;
#78196 = CARTESIAN_POINT('Ctrl Pts',(70.3877178199639,213.005540169192,17.8713203435596)) ;
#78197 = CARTESIAN_POINT('',(83.4878143389934,190.058573545737,17.8713203435596)) ;
#78198 = CARTESIAN_POINT('Ctrl Pts',(83.4878143389934,190.058573545737,17.8713203435596)) ;
#78199 = CARTESIAN_POINT('Ctrl Pts',(81.4305821636459,192.110706612955,17.8713203435596)) ;
#78200 = CARTESIAN_POINT('Ctrl Pts',(78.0106503827396,195.884693008864,17.8713203435596)) ;
#78201 = CARTESIAN_POINT('Ctrl Pts',(75.1348798094609,200.095072314249,17.8713203435596)) ;
#78202 = CARTESIAN_POINT('Ctrl Pts',(74.071363112532,201.997275065426,17.8713203435596)) ;
#78203 = CARTESIAN_POINT('',(83.2194473860051,189.409539758744,17.8713203435596)) ;
#78204 = CARTESIAN_POINT('Ctrl Pts',(83.2194473860051,189.409539758744,17.8713203435596)) ;
#78205 = CARTESIAN_POINT('Ctrl Pts',(83.3047606779792,189.409539758744,17.8713203435596)) ;
#78206 = CARTESIAN_POINT('Ctrl Pts',(83.4319242412693,189.454563257398,17.8713203435596)) ;
#78207 = CARTESIAN_POINT('Ctrl Pts',(83.5764307889551,189.615888430006,17.8713203435596)) ;
#78208 = CARTESIAN_POINT('Ctrl Pts',(83.6266013556018,189.835500488137,17.8713203435596)) ;
#78209 = CARTESIAN_POINT('Ctrl Pts',(83.5482147548371,189.998322839904,17.8713203435596)) ;
#78210 = CARTESIAN_POINT('Ctrl Pts',(83.4878143389934,190.058573545737,17.8713203435596)) ;
#78211 = CARTESIAN_POINT('',(77.8285014478222,189.409539758744,17.8713203435596)) ;
#78212 = CARTESIAN_POINT('',(71.6000791389318,189.409539758744,17.8713203435596)) ;
#78213 = CARTESIAN_POINT('',(77.1942359127805,189.615407485539,17.8713203435596)) ;
#78214 = CARTESIAN_POINT('Origin',(77.7459982214612,190.235352500613,17.8713203435596)) ;
#78215 = CARTESIAN_POINT('',(66.2956301826422,200.621620147878,17.8713203435596)) ;
#78216 = CARTESIAN_POINT('Ctrl Pts',(66.2956301826426,200.621620147878,17.8713203435596)) ;
#78217 = CARTESIAN_POINT('Ctrl Pts',(67.9219091272743,198.140564861203,17.8713203435596)) ;
#78218 = CARTESIAN_POINT('Ctrl Pts',(71.3588126586277,194.203339283954,17.8713203435596)) ;
#78219 = CARTESIAN_POINT('Ctrl Pts',(75.3934324114903,190.922060530236,17.8713203435596)) ;
#78220 = CARTESIAN_POINT('Ctrl Pts',(77.1942359127805,189.615407485539,17.8713203435596)) ;
#78221 = CARTESIAN_POINT('',(65.3716786148033,202.116206289769,17.8713203435596)) ;
#78222 = CARTESIAN_POINT('Origin',(94.003679466336,218.783592840001,17.8713203435596)) ;
#78223 = CARTESIAN_POINT('Origin',(136.119542118164,279.889814321892,17.8713203435596)) ;
#78224 = CARTESIAN_POINT('',(62.3340105195836,212.340553587281,17.8713203435596)) ;
#78225 = CARTESIAN_POINT('',(62.589983859128,212.63785590951,17.8713203435596)) ;
#78226 = CARTESIAN_POINT('Ctrl Pts',(62.3340105195836,212.340553587281,17.8713203435596)) ;
#78227 = CARTESIAN_POINT('Ctrl Pts',(62.3233636275578,212.382972990323,17.8713203435596)) ;
#78228 = CARTESIAN_POINT('Ctrl Pts',(62.325696101677,212.462284462768,17.8713203435596)) ;
#78229 = CARTESIAN_POINT('Ctrl Pts',(62.385161130142,212.569871661429,17.8713203435596)) ;
#78230 = CARTESIAN_POINT('Ctrl Pts',(62.4795535223665,212.632687025067,17.8713203435596)) ;
#78231 = CARTESIAN_POINT('Ctrl Pts',(62.5573360365752,212.641025821764,17.8713203435596)) ;
#78232 = CARTESIAN_POINT('Ctrl Pts',(62.589983859128,212.63785590951,17.8713203435596)) ;
#78233 = CARTESIAN_POINT('',(66.527756290484,202.051005908224,17.8713203435596)) ;
#78234 = CARTESIAN_POINT('Ctrl Pts',(66.527756290484,202.051005908224,17.8713203435596)) ;
#78235 = CARTESIAN_POINT('Ctrl Pts',(64.5939733104855,205.226459086719,17.8713203435596)) ;
#78236 = CARTESIAN_POINT('Ctrl Pts',(63.2390973142897,208.73450203348,17.8713203435596)) ;
#78237 = CARTESIAN_POINT('Ctrl Pts',(62.3340105195836,212.340553587281,17.8713203435596)) ;
#78238 = CARTESIAN_POINT('',(66.7327381812905,201.93583548982,17.8713203435596)) ;
#78239 = CARTESIAN_POINT('Ctrl Pts',(66.7327381812905,201.93583548982,17.8713203435596)) ;
#78240 = CARTESIAN_POINT('Ctrl Pts',(66.6859373054892,201.93583548982,17.8713203435596)) ;
#78241 = CARTESIAN_POINT('Ctrl Pts',(66.6041999927209,201.960528245756,17.8713203435596)) ;
#78242 = CARTESIAN_POINT('Ctrl Pts',(66.5460129584359,202.021026745683,17.8713203435596)) ;
#78243 = CARTESIAN_POINT('Ctrl Pts',(66.5277562904841,202.051005908224,17.8713203435596)) ;
#78244 = CARTESIAN_POINT('',(72.60844030336,201.93583548982,17.8713203435596)) ;
#78245 = CARTESIAN_POINT('',(69.2835637989163,201.93583548982,17.8713203435596)) ;
#78246 = CARTESIAN_POINT('',(72.8206412688368,202.287954846983,17.8713203435596)) ;
#78247 = CARTESIAN_POINT('Ctrl Pts',(72.8206412688368,202.287954846983,17.8713203435596)) ;
#78248 = CARTESIAN_POINT('Ctrl Pts',(72.8426038333632,202.246387739262,17.8713203435596)) ;
#78249 = CARTESIAN_POINT('Ctrl Pts',(72.8613131310738,202.149998406772,17.8713203435596)) ;
#78250 = CARTESIAN_POINT('Ctrl Pts',(72.8140046703539,202.036931343871,17.8713203435596)) ;
#78251 = CARTESIAN_POINT('Ctrl Pts',(72.7257128617816,201.957306367625,17.8713203435596)) ;
#78252 = CARTESIAN_POINT('Ctrl Pts',(72.6554528408887,201.93583548982,17.8713203435596)) ;
#78253 = CARTESIAN_POINT('Ctrl Pts',(72.60844030336,201.93583548982,17.8713203435596)) ;
#78254 = CARTESIAN_POINT('',(69.5945599532053,211.778145438093,17.8713203435596)) ;
#78255 = CARTESIAN_POINT('Ctrl Pts',(69.5945599532053,211.778145438093,17.8713203435596)) ;
#78256 = CARTESIAN_POINT('Ctrl Pts',(70.1332499807628,208.465417915073,17.8713203435596)) ;
#78257 = CARTESIAN_POINT('Ctrl Pts',(71.2527352912136,205.255427820841,17.8713203435596)) ;
#78258 = CARTESIAN_POINT('Ctrl Pts',(72.8206412688369,202.287954846983,17.8713203435596)) ;
#78259 = CARTESIAN_POINT('',(69.3808650318164,211.978501142072,17.8713203435596)) ;
#78260 = CARTESIAN_POINT('Ctrl Pts',(69.3808650318164,211.978501142072,17.8713203435596)) ;
#78261 = CARTESIAN_POINT('Ctrl Pts',(69.4256633316016,211.97415148968,17.8713203435596)) ;
#78262 = CARTESIAN_POINT('Ctrl Pts',(69.5273477579344,211.933842521524,17.8713203435596)) ;
#78263 = CARTESIAN_POINT('Ctrl Pts',(69.5849277942338,211.837379350916,17.8713203435596)) ;
#78264 = CARTESIAN_POINT('Ctrl Pts',(69.5945599532053,211.778145438093,17.8713203435596)) ;
#78265 = CARTESIAN_POINT('',(64.0594779752363,212.495176642042,17.8713203435596)) ;
#78266 = CARTESIAN_POINT('Origin',(67.6417475736039,200.55583548982,23.8713203435596)) ;
#78267 = CARTESIAN_POINT('Origin',(74.5963384974435,195.522687624282,19.3713203435596)) ;
#78268 = CARTESIAN_POINT('Ctrl Pts',(72.60844030336,202.05583548982,17.9913203435596)) ;
#78269 = CARTESIAN_POINT('Ctrl Pts',(72.6319465721243,202.05583548982,17.9913203435596)) ;
#78270 = CARTESIAN_POINT('Ctrl Pts',(72.6670765825708,202.066570928722,17.9913203435596)) ;
#78271 = CARTESIAN_POINT('Ctrl Pts',(72.7112224868569,202.106383416845,17.9913203435596)) ;
#78272 = CARTESIAN_POINT('Ctrl Pts',(72.7348767172168,202.162916948296,17.9913203435596)) ;
#78273 = CARTESIAN_POINT('Ctrl Pts',(72.7255220683616,202.211111614541,17.9913203435596)) ;
#78274 = CARTESIAN_POINT('Ctrl Pts',(72.7145407860984,202.231895168402,17.9913203435596)) ;
#78275 = CARTESIAN_POINT('Ctrl Pts',(72.60844030336,202.05583548982,17.9554164275186)) ;
#78276 = CARTESIAN_POINT('Ctrl Pts',(72.6318714497812,202.05583548982,17.9554164275186)) ;
#78277 = CARTESIAN_POINT('Ctrl Pts',(72.6669974209846,202.066716144597,17.9554164275186)) ;
#78278 = CARTESIAN_POINT('Ctrl Pts',(72.711037641787,202.106460151246,17.9554164275186)) ;
#78279 = CARTESIAN_POINT('Ctrl Pts',(72.734701742353,202.162954813346,17.9554164275186)) ;
#78280 = CARTESIAN_POINT('Ctrl Pts',(72.7254869739082,202.211178035515,17.9554164275186)) ;
#78281 = CARTESIAN_POINT('Ctrl Pts',(72.7145407860984,202.231895168402,17.9554164275186)) ;
#78282 = CARTESIAN_POINT('Ctrl Pts',(72.60844030336,202.025677145806,17.8932837596863)) ;
#78283 = CARTESIAN_POINT('Ctrl Pts',(72.6378715047901,202.025677145806,17.8932837596863)) ;
#78284 = CARTESIAN_POINT('Ctrl Pts',(72.6818313058633,202.039077075185,17.8932837596863)) ;
#78285 = CARTESIAN_POINT('Ctrl Pts',(72.7370963439361,202.088911033826,17.8932837596863)) ;
#78286 = CARTESIAN_POINT('Ctrl Pts',(72.766693065086,202.159661522209,17.8932837596863)) ;
#78287 = CARTESIAN_POINT('Ctrl Pts',(72.7549551073561,202.219961855007,17.8932837596863)) ;
#78288 = CARTESIAN_POINT('Ctrl Pts',(72.7412059099191,202.245984060668,17.8932837596863)) ;
#78289 = CARTESIAN_POINT('Ctrl Pts',(72.60844030336,201.962763426851,17.8713203435596)) ;
#78290 = CARTESIAN_POINT('Ctrl Pts',(72.6501888364698,201.962763426851,17.8713203435596)) ;
#78291 = CARTESIAN_POINT('Ctrl Pts',(72.7125662816165,201.981804420182,17.8713203435596)) ;
#78292 = CARTESIAN_POINT('Ctrl Pts',(72.7909669519409,202.052505331102,17.8713203435596)) ;
#78293 = CARTESIAN_POINT('Ctrl Pts',(72.8329659981049,202.152891882086,17.8713203435596)) ;
#78294 = CARTESIAN_POINT('Ctrl Pts',(72.8163357874141,202.238462255222,17.8713203435596)) ;
#78295 = CARTESIAN_POINT('Ctrl Pts',(72.7968323761858,202.275375084527,17.8713203435596)) ;
#78296 = CARTESIAN_POINT('Ctrl Pts',(72.60844030336,201.93583548982,17.8713203435596)) ;
#78297 = CARTESIAN_POINT('Ctrl Pts',(72.6554528408887,201.93583548982,17.8713203435596)) ;
#78298 = CARTESIAN_POINT('Ctrl Pts',(72.7257128617816,201.957306367625,17.8713203435596)) ;
#78299 = CARTESIAN_POINT('Ctrl Pts',(72.8140046703539,202.036931343871,17.8713203435596)) ;
#78300 = CARTESIAN_POINT('Ctrl Pts',(72.8613131310738,202.149998406772,17.8713203435596)) ;
#78301 = CARTESIAN_POINT('Ctrl Pts',(72.8426038333632,202.246387739262,17.8713203435596)) ;
#78302 = CARTESIAN_POINT('Ctrl Pts',(72.8206412688368,202.287954846983,17.8713203435596)) ;
#78303 = CARTESIAN_POINT('',(72.60844030336,202.05583548982,17.9913203435596)) ;
#78304 = CARTESIAN_POINT('Origin',(72.60844030336,201.93583548982,17.9913203435596)) ;
#78305 = CARTESIAN_POINT('',(72.7145407860984,202.231895168402,17.9913203435596)) ;
#78306 = CARTESIAN_POINT('Ctrl Pts',(72.60844030336,202.05583548982,17.9913203435596)) ;
#78307 = CARTESIAN_POINT('Ctrl Pts',(72.6319474672212,202.05583548982,17.9913203435596)) ;
#78308 = CARTESIAN_POINT('Ctrl Pts',(72.6729579207971,202.068347425336,17.9913203435596)) ;
#78309 = CARTESIAN_POINT('Ctrl Pts',(72.7188163051483,202.116230495061,17.9913203435596)) ;
#78310 = CARTESIAN_POINT('Ctrl Pts',(72.7339278206143,202.175611043943,17.9913203435596)) ;
#78311 = CARTESIAN_POINT('Ctrl Pts',(72.7227770614135,202.216306909442,17.9913203435596)) ;
#78312 = CARTESIAN_POINT('Ctrl Pts',(72.7145407860984,202.231895168402,17.9913203435596)) ;
#78313 = CARTESIAN_POINT('Origin',(72.8206412688368,202.287954846983,17.9913203435596)) ;
#78314 = CARTESIAN_POINT('Origin',(72.60844030336,202.17583548982,19.2513203435596)) ;
#78315 = CARTESIAN_POINT('',(72.7145407860985,202.231895168402,19.2513203435596)) ;
#78316 = CARTESIAN_POINT('',(72.60844030336,202.17583548982,19.3713203435596)) ;
#78317 = CARTESIAN_POINT('Origin',(72.6084403033599,202.17583548982,19.2513203435596)) ;
#78318 = CARTESIAN_POINT('',(72.60844030336,202.05583548982,19.2513203435596)) ;
#78319 = CARTESIAN_POINT('Origin',(72.60844030336,202.17583548982,19.2513203435596)) ;
#78320 = CARTESIAN_POINT('Origin',(72.60844030336,202.17583548982,19.2513203435596)) ;
#78321 = CARTESIAN_POINT('Ctrl Pts',(72.60844030336,202.05583548982,19.2513203435596)) ;
#78322 = CARTESIAN_POINT('Ctrl Pts',(72.60844030336,202.05583548982,17.7393203435596)) ;
#78323 = CARTESIAN_POINT('Ctrl Pts',(72.6319474672212,202.05583548982,19.2513203435596)) ;
#78324 = CARTESIAN_POINT('Ctrl Pts',(72.6319474672212,202.05583548982,17.7393203435596)) ;
#78325 = CARTESIAN_POINT('Ctrl Pts',(72.6729579207971,202.068347425336,19.2513203435596)) ;
#78326 = CARTESIAN_POINT('Ctrl Pts',(72.6729579207971,202.068347425336,17.7393203435596)) ;
#78327 = CARTESIAN_POINT('Ctrl Pts',(72.7188163051483,202.116230495061,19.2513203435596)) ;
#78328 = CARTESIAN_POINT('Ctrl Pts',(72.7188163051483,202.116230495061,17.7393203435596)) ;
#78329 = CARTESIAN_POINT('Ctrl Pts',(72.7339278206143,202.175611043943,19.2513203435596)) ;
#78330 = CARTESIAN_POINT('Ctrl Pts',(72.7339278206143,202.175611043943,17.7393203435596)) ;
#78331 = CARTESIAN_POINT('Ctrl Pts',(72.7227770614135,202.216306909442,19.2513203435596)) ;
#78332 = CARTESIAN_POINT('Ctrl Pts',(72.7227770614135,202.216306909442,17.7393203435596)) ;
#78333 = CARTESIAN_POINT('Ctrl Pts',(72.7145407860984,202.231895168402,19.2513203435596)) ;
#78334 = CARTESIAN_POINT('Ctrl Pts',(72.7145407860984,202.231895168402,17.7393203435596)) ;
#78335 = CARTESIAN_POINT('',(72.60844030336,202.05583548982,17.9913203435596)) ;
#78336 = CARTESIAN_POINT('',(72.7145407860984,202.231895168402,19.2513203435596)) ;
#78337 = CARTESIAN_POINT('Ctrl Pts',(66.6302472358873,202.113420699022,17.9913203435596)) ;
#78338 = CARTESIAN_POINT('Ctrl Pts',(66.6393755698632,202.098431117751,17.9913203435596)) ;
#78339 = CARTESIAN_POINT('Ctrl Pts',(66.6684690870057,202.068181867788,17.9913203435596)) ;
#78340 = CARTESIAN_POINT('Ctrl Pts',(66.7093377433898,202.05583548982,17.9913203435596)) ;
#78341 = CARTESIAN_POINT('Ctrl Pts',(66.7327381812905,202.05583548982,17.9913203435596)) ;
#78342 = CARTESIAN_POINT('Ctrl Pts',(66.6302472358873,202.113420699022,17.9554164275186)) ;
#78343 = CARTESIAN_POINT('Ctrl Pts',(66.6393463971415,202.098479022099,17.9554164275186)) ;
#78344 = CARTESIAN_POINT('Ctrl Pts',(66.6684615598882,202.068262037652,17.9554164275186)) ;
#78345 = CARTESIAN_POINT('Ctrl Pts',(66.7094125275141,202.05583548982,17.9554164275186)) ;
#78346 = CARTESIAN_POINT('Ctrl Pts',(66.7327381812905,202.05583548982,17.9554164275186)) ;
#78347 = CARTESIAN_POINT('Ctrl Pts',(66.6044893329729,202.09773468778,17.8932836561957)) ;
#78348 = CARTESIAN_POINT('Ctrl Pts',(66.6159185325052,202.078966869282,17.8932836561957)) ;
#78349 = CARTESIAN_POINT('Ctrl Pts',(66.652318794356,202.04110795527,17.8932836561957)) ;
#78350 = CARTESIAN_POINT('Ctrl Pts',(66.703439486193,202.025677232058,17.8932836561957)) ;
#78351 = CARTESIAN_POINT('Ctrl Pts',(66.7327381812905,202.025677232058,17.8932836561957)) ;
#78352 = CARTESIAN_POINT('Ctrl Pts',(66.5507552048511,202.065011754527,17.8713203435596)) ;
#78353 = CARTESIAN_POINT('Ctrl Pts',(66.5669676695792,202.03838936557,17.8713203435596)) ;
#78354 = CARTESIAN_POINT('Ctrl Pts',(66.618623024887,201.984674147107,17.8713203435596)) ;
#78355 = CARTESIAN_POINT('Ctrl Pts',(66.6911776100968,201.962763426851,17.8713203435596)) ;
#78356 = CARTESIAN_POINT('Ctrl Pts',(66.7327381812905,201.962763426851,17.8713203435596)) ;
#78357 = CARTESIAN_POINT('Ctrl Pts',(66.5277562904841,202.051005908224,17.8713203435596)) ;
#78358 = CARTESIAN_POINT('Ctrl Pts',(66.5460129584359,202.021026745683,17.8713203435596)) ;
#78359 = CARTESIAN_POINT('Ctrl Pts',(66.6041999927209,201.960528245756,17.8713203435596)) ;
#78360 = CARTESIAN_POINT('Ctrl Pts',(66.6859373054892,201.93583548982,17.8713203435596)) ;
#78361 = CARTESIAN_POINT('Ctrl Pts',(66.7327381812905,201.93583548982,17.8713203435596)) ;
#78362 = CARTESIAN_POINT('',(66.6302472358873,202.113420699022,17.9913203435596)) ;
#78363 = CARTESIAN_POINT('Origin',(66.527756290484,202.051005908224,17.9913203435596)) ;
#78364 = CARTESIAN_POINT('',(66.7327381812905,202.05583548982,17.9913203435596)) ;
#78365 = CARTESIAN_POINT('Origin',(66.7381174716576,202.184021451547,17.9913203435596)) ;
#78366 = CARTESIAN_POINT('Origin',(66.7327381812905,201.93583548982,17.9913203435596)) ;
#78367 = CARTESIAN_POINT('Ctrl Pts',(69.4761157303972,211.75888495826,17.9913203435596)) ;
#78368 = CARTESIAN_POINT('Ctrl Pts',(69.4712996509114,211.788501914672,17.9913203435596)) ;
#78369 = CARTESIAN_POINT('Ctrl Pts',(69.4425096327617,211.836733499976,17.9913203435596)) ;
#78370 = CARTESIAN_POINT('Ctrl Pts',(69.3916674195954,211.856887984054,17.9913203435596)) ;
#78371 = CARTESIAN_POINT('Ctrl Pts',(69.3692682697028,211.85906281025,17.9913203435596)) ;
#78372 = CARTESIAN_POINT('Ctrl Pts',(69.4761157303972,211.75888495826,17.9554164275186)) ;
#78373 = CARTESIAN_POINT('Ctrl Pts',(69.4713150423451,211.788407263531,17.9554164275186)) ;
#78374 = CARTESIAN_POINT('Ctrl Pts',(69.4423950698463,211.836692828306,17.9554164275186)) ;
#78375 = CARTESIAN_POINT('Ctrl Pts',(69.3915958354303,211.856894934457,17.9554164275186)) ;
#78376 = CARTESIAN_POINT('Ctrl Pts',(69.3692682697028,211.85906281025,17.9554164275186)) ;
#78377 = CARTESIAN_POINT('Ctrl Pts',(69.5058831605967,211.763725506625,17.8932838610488)) ;
#78378 = CARTESIAN_POINT('Ctrl Pts',(69.4998531518842,211.800807640699,17.8932838610488)) ;
#78379 = CARTESIAN_POINT('Ctrl Pts',(69.4638576015521,211.861148345767,17.8932838610488)) ;
#78380 = CARTESIAN_POINT('Ctrl Pts',(69.4002277955916,211.88635707259,17.8932838610488)) ;
#78381 = CARTESIAN_POINT('Ctrl Pts',(69.3721827707107,211.889080080163,17.8932838610488)) ;
#78382 = CARTESIAN_POINT('Ctrl Pts',(69.56798113176,211.773823396525,17.8713203435596)) ;
#78383 = CARTESIAN_POINT('Ctrl Pts',(69.5594274877986,211.826424874784,17.8713203435596)) ;
#78384 = CARTESIAN_POINT('Ctrl Pts',(69.5083265820412,211.912057149791,17.8713203435596)) ;
#78385 = CARTESIAN_POINT('Ctrl Pts',(69.4180449485487,211.947836622252,17.8713203435596)) ;
#78386 = CARTESIAN_POINT('Ctrl Pts',(69.3782627244835,211.951699243085,17.8713203435596)) ;
#78387 = CARTESIAN_POINT('Ctrl Pts',(69.5945599532053,211.778145438093,17.8713203435596)) ;
#78388 = CARTESIAN_POINT('Ctrl Pts',(69.5849277942338,211.837379350916,17.8713203435596)) ;
#78389 = CARTESIAN_POINT('Ctrl Pts',(69.5273477579344,211.933842521524,17.8713203435596)) ;
#78390 = CARTESIAN_POINT('Ctrl Pts',(69.4256633316016,211.97415148968,17.8713203435596)) ;
#78391 = CARTESIAN_POINT('Ctrl Pts',(69.3808650318164,211.978501142072,17.8713203435596)) ;
#78392 = CARTESIAN_POINT('',(69.4761157303972,211.75888495826,17.9913203435596)) ;
#78393 = CARTESIAN_POINT('Origin',(69.5945599532053,211.778145438093,17.9913203435596)) ;
#78394 = CARTESIAN_POINT('',(69.3692682697028,211.85906281025,17.9913203435596)) ;
#78395 = CARTESIAN_POINT('Ctrl Pts',(69.4761157303972,211.75888495826,17.9913203435596)) ;
#78396 = CARTESIAN_POINT('Ctrl Pts',(69.4725035530572,211.781098399535,17.9913203435596)) ;
#78397 = CARTESIAN_POINT('Ctrl Pts',(69.4491186156896,211.830541090259,17.9913203435596)) ;
#78398 = CARTESIAN_POINT('Ctrl Pts',(69.3991347762822,211.856162947478,17.9913203435596)) ;
#78399 = CARTESIAN_POINT('Ctrl Pts',(69.3692682697028,211.85906281025,17.9913203435596)) ;
#78400 = CARTESIAN_POINT('Origin',(69.3808650318164,211.978501142072,17.9913203435596)) ;
#78401 = CARTESIAN_POINT('Origin',(66.7327381812904,202.17583548982,19.2513203435596)) ;
#78402 = CARTESIAN_POINT('',(66.7327381812904,202.05583548982,19.2513203435596)) ;
#78403 = CARTESIAN_POINT('',(66.7327381812905,202.17583548982,19.3713203435596)) ;
#78404 = CARTESIAN_POINT('Origin',(66.7327381812904,202.17583548982,19.2513203435596)) ;
#78405 = CARTESIAN_POINT('',(66.6302472358883,202.11342069902,19.2513203435596)) ;
#78406 = CARTESIAN_POINT('Origin',(66.7327381812904,202.17583548982,19.2513203435596)) ;
#78407 = CARTESIAN_POINT('Origin',(66.7327381812905,202.17583548982,19.2513203435596)) ;
#78408 = CARTESIAN_POINT('Ctrl Pts',(66.6302472358873,202.113420699022,19.2513203435596)) ;
#78409 = CARTESIAN_POINT('Ctrl Pts',(66.6302472358873,202.113420699022,17.7393203435596)) ;
#78410 = CARTESIAN_POINT('Ctrl Pts',(66.6515473457387,202.078443919192,19.2513203435596)) ;
#78411 = CARTESIAN_POINT('Ctrl Pts',(66.6515473457387,202.078443919192,17.7393203435596)) ;
#78412 = CARTESIAN_POINT('Ctrl Pts',(66.6917861385215,202.05583548982,19.2513203435596)) ;
#78413 = CARTESIAN_POINT('Ctrl Pts',(66.6917861385215,202.05583548982,17.7393203435596)) ;
#78414 = CARTESIAN_POINT('Ctrl Pts',(66.7327381812904,202.05583548982,19.2513203435596)) ;
#78415 = CARTESIAN_POINT('Ctrl Pts',(66.7327381812904,202.05583548982,17.7393203435596)) ;
#78416 = CARTESIAN_POINT('',(66.6302472358873,202.113420699022,17.9913203435596)) ;
#78417 = CARTESIAN_POINT('',(66.7327381812904,202.05583548982,19.2513203435596)) ;
#78418 = CARTESIAN_POINT('Origin',(69.3576715158512,211.739624427619,19.2513203435596)) ;
#78419 = CARTESIAN_POINT('',(69.4761157303957,211.758884958269,19.2513203435596)) ;
#78420 = CARTESIAN_POINT('',(69.3692682697028,211.85906281025,19.2513203435596)) ;
#78421 = CARTESIAN_POINT('Origin',(69.3576715075891,211.739624478427,19.2513203435596)) ;
#78422 = CARTESIAN_POINT('',(69.3576715245022,211.739624453345,19.3713203435596)) ;
#78423 = CARTESIAN_POINT('Origin',(69.3576715158512,211.739624427619,19.2513203435596)) ;
#78424 = CARTESIAN_POINT('Origin',(69.3576715075891,211.739624478427,19.2513203435596)) ;
#78425 = CARTESIAN_POINT('Ctrl Pts',(72.7145407860984,202.231895168402,19.2513203435596)) ;
#78426 = CARTESIAN_POINT('Ctrl Pts',(71.1398059575599,205.212292661218,19.2513203435596)) ;
#78427 = CARTESIAN_POINT('Ctrl Pts',(70.0168498128443,208.433587317836,19.2513203435596)) ;
#78428 = CARTESIAN_POINT('Ctrl Pts',(69.4761157303972,211.75888495826,19.2513203435596)) ;
#78429 = CARTESIAN_POINT('Ctrl Pts',(72.7145407860984,202.231895168402,19.2872242596007)) ;
#78430 = CARTESIAN_POINT('Ctrl Pts',(71.1398228541547,205.212260682139,19.2872242596007)) ;
#78431 = CARTESIAN_POINT('Ctrl Pts',(70.016843012287,208.433629138534,19.2872242596007)) ;
#78432 = CARTESIAN_POINT('Ctrl Pts',(69.4761157303972,211.75888495826,19.2872242596007)) ;
#78433 = CARTESIAN_POINT('Ctrl Pts',(72.6878755734951,202.217806229225,19.349356806951)) ;
#78434 = CARTESIAN_POINT('Ctrl Pts',(71.1118081030027,205.200725926204,19.349356806951)) ;
#78435 = CARTESIAN_POINT('Ctrl Pts',(69.9876187299006,208.425448349774,19.349356806951)) ;
#78436 = CARTESIAN_POINT('Ctrl Pts',(69.4463482844696,211.754044407338,19.349356806951)) ;
#78437 = CARTESIAN_POINT('Ctrl Pts',(72.632249196011,202.188415252277,19.3713203435596)) ;
#78438 = CARTESIAN_POINT('Ctrl Pts',(71.0534112985986,205.176578354872,19.3713203435596)) ;
#78439 = CARTESIAN_POINT('Ctrl Pts',(69.9266358184916,208.408493389076,19.3713203435596)) ;
#78440 = CARTESIAN_POINT('Ctrl Pts',(69.3842503290344,211.743946519995,19.3713203435596)) ;
#78441 = CARTESIAN_POINT('Ctrl Pts',(72.60844030336,202.17583548982,19.3713203435596)) ;
#78442 = CARTESIAN_POINT('Ctrl Pts',(71.0284184206553,205.166239443848,19.3713203435596)) ;
#78443 = CARTESIAN_POINT('Ctrl Pts',(69.9005335285577,208.401240869919,19.3713203435596)) ;
#78444 = CARTESIAN_POINT('Ctrl Pts',(69.3576715075891,211.739624478427,19.3713203435596)) ;
#78445 = CARTESIAN_POINT('Ctrl Pts',(69.4761157303972,211.75888495826,19.2513203435596)) ;
#78446 = CARTESIAN_POINT('Ctrl Pts',(70.0168498128443,208.433587317836,19.2513203435596)) ;
#78447 = CARTESIAN_POINT('Ctrl Pts',(71.1398059575599,205.212292661218,19.2513203435596)) ;
#78448 = CARTESIAN_POINT('Ctrl Pts',(72.7145407860984,202.231895168402,19.2513203435596)) ;
#78449 = CARTESIAN_POINT('Ctrl Pts',(72.60844030336,202.17583548982,19.3713203435596)) ;
#78450 = CARTESIAN_POINT('Ctrl Pts',(71.0284184249332,205.166239435752,19.3713203435596)) ;
#78451 = CARTESIAN_POINT('Ctrl Pts',(69.9005335346653,208.401240852402,19.3713203435596)) ;
#78452 = CARTESIAN_POINT('Ctrl Pts',(69.3576715119986,211.739624451311,19.3713203435596)) ;
#78453 = CARTESIAN_POINT('Ctrl Pts',(62.5783870970144,212.518417577687,17.9913203435596)) ;
#78454 = CARTESIAN_POINT('Ctrl Pts',(62.562063185738,212.520002533814,17.9913203435596)) ;
#78455 = CARTESIAN_POINT('Ctrl Pts',(62.5231719286336,212.515833135466,17.9913203435596)) ;
#78456 = CARTESIAN_POINT('Ctrl Pts',(62.4759757325213,212.484425453647,17.9913203435596)) ;
#78457 = CARTESIAN_POINT('Ctrl Pts',(62.4462432182888,212.430631854317,17.9913203435596)) ;
#78458 = CARTESIAN_POINT('Ctrl Pts',(62.4450769812292,212.390976118094,17.9913203435596)) ;
#78459 = CARTESIAN_POINT('Ctrl Pts',(62.4504004272421,212.369766416573,17.9913203435596)) ;
#78460 = CARTESIAN_POINT('Ctrl Pts',(62.5783870970144,212.518417577687,17.9554164275186)) ;
#78461 = CARTESIAN_POINT('Ctrl Pts',(62.5621153543946,212.519997468544,17.9554164275186)) ;
#78462 = CARTESIAN_POINT('Ctrl Pts',(62.5232486540694,212.515725612279,17.9554164275186)) ;
#78463 = CARTESIAN_POINT('Ctrl Pts',(62.4760976399362,212.484295588733,17.9554164275186)) ;
#78464 = CARTESIAN_POINT('Ctrl Pts',(62.4464066667739,212.430611808364,17.9554164275186)) ;
#78465 = CARTESIAN_POINT('Ctrl Pts',(62.4450939941266,212.390908335219,17.9554164275186)) ;
#78466 = CARTESIAN_POINT('Ctrl Pts',(62.4504004272421,212.369766416573,17.9554164275186)) ;
#78467 = CARTESIAN_POINT('Ctrl Pts',(62.5813015900153,212.548434765134,17.8932837616354)) ;
#78468 = CARTESIAN_POINT('Ctrl Pts',(62.560863113551,212.55041922143,17.8932837616354)) ;
#78469 = CARTESIAN_POINT('Ctrl Pts',(62.5121920524828,212.545225632173,17.8932837616354)) ;
#78470 = CARTESIAN_POINT('Ctrl Pts',(62.4531240959624,212.505929745317,17.8932837616354)) ;
#78471 = CARTESIAN_POINT('Ctrl Pts',(62.4159096267281,212.438591402704,17.8932837616354)) ;
#78472 = CARTESIAN_POINT('Ctrl Pts',(62.4144841075688,212.388980428609,17.8932837616354)) ;
#78473 = CARTESIAN_POINT('Ctrl Pts',(62.4211493683755,212.362424661549,17.8932837616354)) ;
#78474 = CARTESIAN_POINT('Ctrl Pts',(62.5873815517951,212.611054010523,17.8713203435596)) ;
#78475 = CARTESIAN_POINT('Ctrl Pts',(62.5583893132889,212.613868986988,17.8713203435596)) ;
#78476 = CARTESIAN_POINT('Ctrl Pts',(62.4893304496322,212.606480517307,17.8713203435596)) ;
#78477 = CARTESIAN_POINT('Ctrl Pts',(62.4055223694806,212.550716229971,17.8713203435596)) ;
#78478 = CARTESIAN_POINT('Ctrl Pts',(62.3527233349889,212.455184513277,17.8713203435596)) ;
#78479 = CARTESIAN_POINT('Ctrl Pts',(62.3506735966604,212.384778623772,17.8713203435596)) ;
#78480 = CARTESIAN_POINT('Ctrl Pts',(62.3601283537873,212.347108930845,17.8713203435596)) ;
#78481 = CARTESIAN_POINT('Ctrl Pts',(62.589983859128,212.63785590951,17.8713203435596)) ;
#78482 = CARTESIAN_POINT('Ctrl Pts',(62.5573360365752,212.641025821764,17.8713203435596)) ;
#78483 = CARTESIAN_POINT('Ctrl Pts',(62.4795535223665,212.632687025067,17.8713203435596)) ;
#78484 = CARTESIAN_POINT('Ctrl Pts',(62.385161130142,212.569871661429,17.8713203435596)) ;
#78485 = CARTESIAN_POINT('Ctrl Pts',(62.325696101677,212.462284462768,17.8713203435596)) ;
#78486 = CARTESIAN_POINT('Ctrl Pts',(62.3233636275578,212.382972990323,17.8713203435596)) ;
#78487 = CARTESIAN_POINT('Ctrl Pts',(62.3340105195836,212.340553587281,17.8713203435596)) ;
#78488 = CARTESIAN_POINT('',(62.5783870970144,212.518417577687,17.9913203435596)) ;
#78489 = CARTESIAN_POINT('Origin',(62.589983859128,212.63785590951,17.9913203435596)) ;
#78490 = CARTESIAN_POINT('',(62.4504004272421,212.369766416573,17.9913203435596)) ;
#78491 = CARTESIAN_POINT('Ctrl Pts',(62.5783870970144,212.518417577687,17.9913203435596)) ;
#78492 = CARTESIAN_POINT('Ctrl Pts',(62.562063185738,212.520002533814,17.9913203435596)) ;
#78493 = CARTESIAN_POINT('Ctrl Pts',(62.5231719286336,212.515833135466,17.9913203435596)) ;
#78494 = CARTESIAN_POINT('Ctrl Pts',(62.4759757325213,212.484425453647,17.9913203435596)) ;
#78495 = CARTESIAN_POINT('Ctrl Pts',(62.4462432182888,212.430631854317,17.9913203435596)) ;
#78496 = CARTESIAN_POINT('Ctrl Pts',(62.4450769812292,212.390976118094,17.9913203435596)) ;
#78497 = CARTESIAN_POINT('Ctrl Pts',(62.4504004272421,212.369766416573,17.9913203435596)) ;
#78498 = CARTESIAN_POINT('Origin',(62.3340105195836,212.340553587281,17.9913203435596)) ;
#78499 = CARTESIAN_POINT('Origin',(62.5667903349007,212.398979245865,19.2513203435596)) ;
#78500 = CARTESIAN_POINT('',(62.450400427238,212.36976641659,19.2513203435596)) ;
#78501 = CARTESIAN_POINT('',(62.5667903349007,212.398979245865,19.3713203435596)) ;
#78502 = CARTESIAN_POINT('Origin',(62.5667903349007,212.398979245865,19.2513203435596)) ;
#78503 = CARTESIAN_POINT('',(62.4617165382906,212.456940416194,19.2513203435596)) ;
#78504 = CARTESIAN_POINT('Origin',(62.5667903349007,212.398979245865,19.2513203435596)) ;
#78505 = CARTESIAN_POINT('',(62.5783870970144,212.518417577687,19.2513203435596)) ;
#78506 = CARTESIAN_POINT('Origin',(62.5667903349007,212.398979245865,19.2513203435596)) ;
#78507 = CARTESIAN_POINT('Origin',(62.5667903349007,212.398979245865,19.2513203435596)) ;
#78508 = CARTESIAN_POINT('Ctrl Pts',(62.5783870970144,212.518417577687,19.2513203435596)) ;
#78509 = CARTESIAN_POINT('Ctrl Pts',(62.5783870970144,212.518417577687,17.7393203435596)) ;
#78510 = CARTESIAN_POINT('Ctrl Pts',(62.5566209022384,212.520530947651,19.2513203435596)) ;
#78511 = CARTESIAN_POINT('Ctrl Pts',(62.5566209022384,212.520530947651,17.7393203435596)) ;
#78512 = CARTESIAN_POINT('Ctrl Pts',(62.5175562241547,212.513505863603,19.2513203435596)) ;
#78513 = CARTESIAN_POINT('Ctrl Pts',(62.5175562241547,212.513505863603,17.7393203435596)) ;
#78514 = CARTESIAN_POINT('Ctrl Pts',(62.473284759297,212.47948630102,19.2513203435596)) ;
#78515 = CARTESIAN_POINT('Ctrl Pts',(62.473284759297,212.47948630102,17.7393203435596)) ;
#78516 = CARTESIAN_POINT('Ctrl Pts',(62.446220083906,212.43065192189,19.2513203435596)) ;
#78517 = CARTESIAN_POINT('Ctrl Pts',(62.446220083906,212.43065192189,17.7393203435596)) ;
#78518 = CARTESIAN_POINT('Ctrl Pts',(62.4450767415993,212.390977072829,19.2513203435596)) ;
#78519 = CARTESIAN_POINT('Ctrl Pts',(62.4450767415993,212.390977072829,17.7393203435596)) ;
#78520 = CARTESIAN_POINT('Ctrl Pts',(62.4504004272421,212.369766416573,19.2513203435596)) ;
#78521 = CARTESIAN_POINT('Ctrl Pts',(62.4504004272421,212.369766416573,17.7393203435596)) ;
#78522 = CARTESIAN_POINT('',(62.5783870970144,212.518417577687,17.9913203435596)) ;
#78523 = CARTESIAN_POINT('',(62.4504004272421,212.369766416573,19.2513203435596)) ;
#78524 = CARTESIAN_POINT('Origin',(65.2251874189933,212.140864467154,19.2513203435596)) ;
#78525 = CARTESIAN_POINT('',(65.236784181107,212.260302798977,19.2513203435596)) ;
#78526 = CARTESIAN_POINT('',(65.2251874189933,212.140864467154,19.3713203435596)) ;
#78527 = CARTESIAN_POINT('Ctrl Pts',(62.4504004272421,212.369766416573,19.2513203435596)) ;
#78528 = CARTESIAN_POINT('Ctrl Pts',(63.3519937332128,208.777633638912,19.2513203435596)) ;
#78529 = CARTESIAN_POINT('Ctrl Pts',(64.7017677689033,205.280165011303,19.2513203435596)) ;
#78530 = CARTESIAN_POINT('Ctrl Pts',(66.6302472358874,202.113420699022,19.2513203435596)) ;
#78531 = CARTESIAN_POINT('Ctrl Pts',(62.4504004272421,212.369766416573,19.2872242596007)) ;
#78532 = CARTESIAN_POINT('Ctrl Pts',(63.3520013377904,208.777603340714,19.2872242596007)) ;
#78533 = CARTESIAN_POINT('Ctrl Pts',(64.701744667191,205.280202946483,19.2872242596007)) ;
#78534 = CARTESIAN_POINT('Ctrl Pts',(66.6302472358874,202.113420699022,19.2872242596007)) ;
#78535 = CARTESIAN_POINT('Ctrl Pts',(62.4796515023926,212.377108175684,19.3493569053396)) ;
#78536 = CARTESIAN_POINT('Ctrl Pts',(63.3806450319406,208.787365030391,19.3493569053396)) ;
#78537 = CARTESIAN_POINT('Ctrl Pts',(64.7293478035486,205.29285911243,19.3493569053396)) ;
#78538 = CARTESIAN_POINT('Ctrl Pts',(66.6560052281957,202.129106764703,19.3493569053396)) ;
#78539 = CARTESIAN_POINT('Ctrl Pts',(62.540672500697,212.392423902301,19.3713203435596)) ;
#78540 = CARTESIAN_POINT('Ctrl Pts',(63.4404191561371,208.807648559368,19.3713203435596)) ;
#78541 = CARTESIAN_POINT('Ctrl Pts',(64.7868696827578,205.319362001607,19.3713203435596)) ;
#78542 = CARTESIAN_POINT('Ctrl Pts',(66.7097392669236,202.161829643516,19.3713203435596)) ;
#78543 = CARTESIAN_POINT('Ctrl Pts',(62.5667903349007,212.398979245865,19.3713203435596)) ;
#78544 = CARTESIAN_POINT('Ctrl Pts',(63.4660041191814,208.816326970999,19.3713203435596)) ;
#78545 = CARTESIAN_POINT('Ctrl Pts',(64.8114873900217,205.330709638017,19.3713203435596)) ;
#78546 = CARTESIAN_POINT('Ctrl Pts',(66.7327381812906,202.17583548982,19.3713203435596)) ;
#78547 = CARTESIAN_POINT('Ctrl Pts',(66.6302472358874,202.113420699022,19.2513203435596)) ;
#78548 = CARTESIAN_POINT('Ctrl Pts',(64.7017677689033,205.280165011303,19.2513203435596)) ;
#78549 = CARTESIAN_POINT('Ctrl Pts',(63.3519937332128,208.777633638912,19.2513203435596)) ;
#78550 = CARTESIAN_POINT('Ctrl Pts',(62.4504004272421,212.369766416573,19.2513203435596)) ;
#78551 = CARTESIAN_POINT('Origin',(125.251450136782,268.303013522014,19.3713203435596)) ;
#78552 = CARTESIAN_POINT('Ctrl Pts',(62.4504004272422,212.369766416573,17.9913203435596)) ;
#78553 = CARTESIAN_POINT('Ctrl Pts',(63.3531047679701,208.773207048405,17.9913203435596)) ;
#78554 = CARTESIAN_POINT('Ctrl Pts',(64.703685742309,205.277015518929,17.9913203435596)) ;
#78555 = CARTESIAN_POINT('Ctrl Pts',(66.6302472358872,202.113420699022,17.9913203435596)) ;
#78556 = CARTESIAN_POINT('Ctrl Pts',(62.4504004272422,212.369766416573,17.9554164275186)) ;
#78557 = CARTESIAN_POINT('Ctrl Pts',(63.3530971540214,208.77323738394,17.9554164275186)) ;
#78558 = CARTESIAN_POINT('Ctrl Pts',(64.7037088210454,205.276977621478,17.9554164275186)) ;
#78559 = CARTESIAN_POINT('Ctrl Pts',(66.6302472358872,202.113420699022,17.9554164275186)) ;
#78560 = CARTESIAN_POINT('Ctrl Pts',(62.4211493721785,212.362424662504,17.8932837569307)) ;
#78561 = CARTESIAN_POINT('Ctrl Pts',(63.3244542284346,208.76347271722,17.8932837569307)) ;
#78562 = CARTESIAN_POINT('Ctrl Pts',(64.6761075374679,205.264318452909,17.8932837569307)) ;
#78563 = CARTESIAN_POINT('Ctrl Pts',(66.6044892612671,202.097734644113,17.8932837569307)) ;
#78564 = CARTESIAN_POINT('Ctrl Pts',(62.3601283537873,212.347108930845,17.8713203435596)) ;
#78565 = CARTESIAN_POINT('Ctrl Pts',(63.264681620676,208.743183061372,17.8713203435596)) ;
#78566 = CARTESIAN_POINT('Ctrl Pts',(64.6185894077755,205.237809366857,17.8713203435596)) ;
#78567 = CARTESIAN_POINT('Ctrl Pts',(66.550755204851,202.065011754527,17.8713203435596)) ;
#78568 = CARTESIAN_POINT('Ctrl Pts',(62.3340105195836,212.340553587281,17.8713203435596)) ;
#78569 = CARTESIAN_POINT('Ctrl Pts',(63.2390973142897,208.73450203348,17.8713203435596)) ;
#78570 = CARTESIAN_POINT('Ctrl Pts',(64.5939733104855,205.226459086719,17.8713203435596)) ;
#78571 = CARTESIAN_POINT('Ctrl Pts',(66.527756290484,202.051005908224,17.8713203435596)) ;
#78572 = CARTESIAN_POINT('Origin',(124.881953702128,267.85635873889,17.9913203435596)) ;
#78573 = CARTESIAN_POINT('Origin',(64.0594779752363,212.495176642042,17.9913203435596)) ;
#78574 = CARTESIAN_POINT('',(64.0478812131227,212.37573831022,17.9913203435596)) ;
#78575 = CARTESIAN_POINT('Ctrl Pts',(69.3692682697028,211.85906281025,17.9913203435596)) ;
#78576 = CARTESIAN_POINT('Ctrl Pts',(69.3692682697028,211.85906281025,19.5033203435596)) ;
#78577 = CARTESIAN_POINT('Ctrl Pts',(69.3991347762822,211.856162947478,17.9913203435596)) ;
#78578 = CARTESIAN_POINT('Ctrl Pts',(69.3991347762822,211.856162947478,19.5033203435596)) ;
#78579 = CARTESIAN_POINT('Ctrl Pts',(69.4491186156896,211.830541090259,17.9913203435596)) ;
#78580 = CARTESIAN_POINT('Ctrl Pts',(69.4491186156896,211.830541090259,19.5033203435596)) ;
#78581 = CARTESIAN_POINT('Ctrl Pts',(69.4725035530572,211.781098399535,17.9913203435596)) ;
#78582 = CARTESIAN_POINT('Ctrl Pts',(69.4725035530572,211.781098399535,19.5033203435596)) ;
#78583 = CARTESIAN_POINT('Ctrl Pts',(69.4761157303972,211.75888495826,17.9913203435596)) ;
#78584 = CARTESIAN_POINT('Ctrl Pts',(69.4761157303972,211.75888495826,19.5033203435596)) ;
#78585 = CARTESIAN_POINT('',(69.3692682697028,211.85906281025,19.2513203435596)) ;
#78586 = CARTESIAN_POINT('',(69.4761157303972,211.75888495826,17.9913203435596)) ;
#78587 = CARTESIAN_POINT('Origin',(70.2085194795435,202.17583548982,19.2513203435596)) ;
#78588 = CARTESIAN_POINT('',(70.2085194795435,202.05583548982,19.2513203435596)) ;
#78589 = CARTESIAN_POINT('',(70.2085194795435,202.17583548982,19.3713203435596)) ;
#78590 = CARTESIAN_POINT('Ctrl Pts',(72.7145407860985,202.231895168401,17.9913203435596)) ;
#78591 = CARTESIAN_POINT('Ctrl Pts',(71.1413529482141,205.209364773308,17.9913203435596)) ;
#78592 = CARTESIAN_POINT('Ctrl Pts',(70.0169340278858,208.433069429121,17.9913203435596)) ;
#78593 = CARTESIAN_POINT('Ctrl Pts',(69.4761157303972,211.75888495826,17.9913203435596)) ;
#78594 = CARTESIAN_POINT('Ctrl Pts',(72.7145407860985,202.231895168401,17.9554164275186)) ;
#78595 = CARTESIAN_POINT('Ctrl Pts',(71.1413360682183,205.209396720971,17.9554164275186)) ;
#78596 = CARTESIAN_POINT('Ctrl Pts',(70.0169408295022,208.433027601909,17.9554164275186)) ;
#78597 = CARTESIAN_POINT('Ctrl Pts',(69.4761157303972,211.75888495826,17.9554164275186)) ;
#78598 = CARTESIAN_POINT('Ctrl Pts',(72.7412059838746,202.245984099743,17.8932838600471)) ;
#78599 = CARTESIAN_POINT('Ctrl Pts',(71.1693494787811,205.220933978255,17.8932838600471)) ;
#78600 = CARTESIAN_POINT('Ctrl Pts',(70.046165010743,208.441208908193,17.8932838600471)) ;
#78601 = CARTESIAN_POINT('Ctrl Pts',(69.5058831597727,211.763725506491,17.8932838600471)) ;
#78602 = CARTESIAN_POINT('Ctrl Pts',(72.7968323761859,202.275375084526,17.8713203435596)) ;
#78603 = CARTESIAN_POINT('Ctrl Pts',(71.2277435763958,205.245086708446,17.8713203435596)) ;
#78604 = CARTESIAN_POINT('Ctrl Pts',(70.1071477650449,208.458164939517,17.8713203435596)) ;
#78605 = CARTESIAN_POINT('Ctrl Pts',(69.56798113176,211.773823396525,17.8713203435596)) ;
#78606 = CARTESIAN_POINT('Ctrl Pts',(72.8206412688369,202.287954846983,17.8713203435596)) ;
#78607 = CARTESIAN_POINT('Ctrl Pts',(71.2527352912136,205.255427820841,17.8713203435596)) ;
#78608 = CARTESIAN_POINT('Ctrl Pts',(70.1332499807628,208.465417915073,17.8713203435596)) ;
#78609 = CARTESIAN_POINT('Ctrl Pts',(69.5945599532053,211.778145438093,17.8713203435596)) ;
#78610 = CARTESIAN_POINT('Ctrl Pts',(72.7145407860985,202.231895168401,17.9913203435596)) ;
#78611 = CARTESIAN_POINT('Ctrl Pts',(71.1413529482141,205.209364773308,17.9913203435596)) ;
#78612 = CARTESIAN_POINT('Ctrl Pts',(70.0169340278858,208.433069429121,17.9913203435596)) ;
#78613 = CARTESIAN_POINT('Ctrl Pts',(69.4761157303972,211.75888495826,17.9913203435596)) ;
#78614 = CARTESIAN_POINT('Origin',(69.2835637989163,201.93583548982,17.9913203435596)) ;
#78615 = CARTESIAN_POINT('',(69.2835637989163,202.05583548982,17.9913203435596)) ;
#78616 = CARTESIAN_POINT('Ctrl Pts',(69.4614223697787,211.850115187154,17.854339447693)) ;
#78617 = CARTESIAN_POINT('Ctrl Pts',(69.4614223697787,211.850115187154,32.8747165227329)) ;
#78618 = CARTESIAN_POINT('Ctrl Pts',(69.905975823669,209.06303762573,17.854339447693)) ;
#78619 = CARTESIAN_POINT('Ctrl Pts',(69.905975823669,209.06303762573,32.8747165227329)) ;
#78620 = CARTESIAN_POINT('Ctrl Pts',(70.7494560159525,206.30693385077,17.854339447693)) ;
#78621 = CARTESIAN_POINT('Ctrl Pts',(70.7494560159525,206.30693385077,32.8747165227329)) ;
#78622 = CARTESIAN_POINT('Ctrl Pts',(72.0309081730459,203.597341394065,17.854339447693)) ;
#78623 = CARTESIAN_POINT('Ctrl Pts',(72.0309081730459,203.597341394065,32.8747165227329)) ;
#78624 = CARTESIAN_POINT('Ctrl Pts',(72.2749463865981,203.081329852839,17.854339447693)) ;
#78625 = CARTESIAN_POINT('Ctrl Pts',(72.2749463865981,203.081329852839,32.8747165227329)) ;
#78626 = CARTESIAN_POINT('Ctrl Pts',(72.5341913976221,202.567520362575,17.854339447693)) ;
#78627 = CARTESIAN_POINT('Ctrl Pts',(72.5341913976221,202.567520362575,32.8747165227329)) ;
#78628 = CARTESIAN_POINT('Ctrl Pts',(72.8081914673101,202.05583548982,17.854339447693)) ;
#78629 = CARTESIAN_POINT('Ctrl Pts',(72.8081914673101,202.05583548982,32.8747165227329)) ;
#78630 = CARTESIAN_POINT('Origin',(72.8081914673101,202.05583548982,23.8713203435596)) ;
#78631 = CARTESIAN_POINT('Origin',(67.6088474917769,207.295232147432,19.3713203435596)) ;
#78632 = CARTESIAN_POINT('Ctrl Pts',(66.6653986331397,202.05583548982,17.8547522895864)) ;
#78633 = CARTESIAN_POINT('Ctrl Pts',(66.6653986331397,202.05583548982,32.8746339543542)) ;
#78634 = CARTESIAN_POINT('Ctrl Pts',(64.7175672988148,205.239235006074,17.8547522895864)) ;
#78635 = CARTESIAN_POINT('Ctrl Pts',(64.7175672988148,205.239235006074,32.8746339543542)) ;
#78636 = CARTESIAN_POINT('Ctrl Pts',(63.3441806268929,208.750326110011,17.8547522895864)) ;
#78637 = CARTESIAN_POINT('Ctrl Pts',(63.3441806268929,208.750326110011,32.8746339543542)) ;
#78638 = CARTESIAN_POINT('Ctrl Pts',(62.4092970952969,212.53483522599,17.8547522895864)) ;
#78639 = CARTESIAN_POINT('Ctrl Pts',(62.4092970952969,212.53483522599,32.8746339543542)) ;
#78640 = CARTESIAN_POINT('Origin',(62.4092970952969,212.53483522599,23.8713203435596)) ;
#78641 = CARTESIAN_POINT('Ctrl Pts',(70.3912832946837,219.697039770423,23.9913203435596)) ;
#78642 = CARTESIAN_POINT('Ctrl Pts',(70.3892097227702,219.672192168808,23.9913203435596)) ;
#78643 = CARTESIAN_POINT('Ctrl Pts',(70.3871361508568,219.647344567192,23.9913203435596)) ;
#78644 = CARTESIAN_POINT('Ctrl Pts',(70.3850625789433,219.622496965577,23.9913203435596)) ;
#78645 = CARTESIAN_POINT('Ctrl Pts',(70.3491825816751,219.192547142135,23.9913203435596)) ;
#78646 = CARTESIAN_POINT('Ctrl Pts',(70.3215247358121,218.761924034176,23.9913203435596)) ;
#78647 = CARTESIAN_POINT('Ctrl Pts',(70.3022814706893,218.330941191344,23.9913203435596)) ;
#78648 = CARTESIAN_POINT('Ctrl Pts',(70.3912832946837,219.697039770423,23.9554164275186)) ;
#78649 = CARTESIAN_POINT('Ctrl Pts',(70.3892097227702,219.672192168808,23.9554164275186)) ;
#78650 = CARTESIAN_POINT('Ctrl Pts',(70.3871361508568,219.647344567192,23.9554164275186)) ;
#78651 = CARTESIAN_POINT('Ctrl Pts',(70.3850625789433,219.622496965577,23.9554164275186)) ;
#78652 = CARTESIAN_POINT('Ctrl Pts',(70.3491825816751,219.192547142135,23.9554164275186)) ;
#78653 = CARTESIAN_POINT('Ctrl Pts',(70.3215247358121,218.761924034176,23.9554164275186)) ;
#78654 = CARTESIAN_POINT('Ctrl Pts',(70.3022814706893,218.330941191344,23.9554164275186)) ;
#78655 = CARTESIAN_POINT('Ctrl Pts',(70.3612291512671,219.699547836539,23.8932840823134)) ;
#78656 = CARTESIAN_POINT('Ctrl Pts',(70.3591555793536,219.674700234924,23.8932840823134)) ;
#78657 = CARTESIAN_POINT('Ctrl Pts',(70.3570820074401,219.649852633308,23.8932840823134)) ;
#78658 = CARTESIAN_POINT('Ctrl Pts',(70.3550084355267,219.625005031693,23.8932840823134)) ;
#78659 = CARTESIAN_POINT('Ctrl Pts',(70.3190964567053,219.194672012347,23.8932840823134)) ;
#78660 = CARTESIAN_POINT('Ctrl Pts',(70.291413648541,218.763661470318,23.8932840823134)) ;
#78661 = CARTESIAN_POINT('Ctrl Pts',(70.2721528749869,218.332286424837,23.8932840823134)) ;
#78662 = CARTESIAN_POINT('Ctrl Pts',(70.2985336334945,219.704779877312,23.8713203435596)) ;
#78663 = CARTESIAN_POINT('Ctrl Pts',(70.2964600615811,219.679932275696,23.8713203435596)) ;
#78664 = CARTESIAN_POINT('Ctrl Pts',(70.2943864896676,219.655084674081,23.8713203435596)) ;
#78665 = CARTESIAN_POINT('Ctrl Pts',(70.2923129177541,219.630237072465,23.8713203435596)) ;
#78666 = CARTESIAN_POINT('Ctrl Pts',(70.2563342313308,219.199104680379,23.8713203435596)) ;
#78667 = CARTESIAN_POINT('Ctrl Pts',(70.2285993496033,218.767285918537,23.8713203435596)) ;
#78668 = CARTESIAN_POINT('Ctrl Pts',(70.2093020433682,218.335092697142,23.8713203435596)) ;
#78669 = CARTESIAN_POINT('Ctrl Pts',(70.2716989748822,219.707019272295,23.8713203435596)) ;
#78670 = CARTESIAN_POINT('Ctrl Pts',(70.2696254029687,219.68217167068,23.8713203435596)) ;
#78671 = CARTESIAN_POINT('Ctrl Pts',(70.2675518310552,219.657324069064,23.8713203435596)) ;
#78672 = CARTESIAN_POINT('Ctrl Pts',(70.2654782591418,219.632476467449,23.8713203435596)) ;
#78673 = CARTESIAN_POINT('Ctrl Pts',(70.2294710222707,219.201001932498,23.8713203435596)) ;
#78674 = CARTESIAN_POINT('Ctrl Pts',(70.201713852236,218.768837240123,23.8713203435596)) ;
#78675 = CARTESIAN_POINT('Ctrl Pts',(70.1824009080094,218.33629382542,23.8713203435596)) ;
#78676 = CARTESIAN_POINT('',(70.2716989748822,219.707019272295,23.8713203435596)) ;
#78677 = CARTESIAN_POINT('',(70.3850625789433,219.622496965576,23.9913203435596)) ;
#78678 = CARTESIAN_POINT('Ctrl Pts',(70.2716989748826,219.707019272295,23.8713203435596)) ;
#78679 = CARTESIAN_POINT('Ctrl Pts',(70.2851494079172,219.696990818844,23.8713203435596)) ;
#78680 = CARTESIAN_POINT('Ctrl Pts',(70.2987229692106,219.686870562696,23.8739545428452)) ;
#78681 = CARTESIAN_POINT('Ctrl Pts',(70.3229190992498,219.668830268886,23.8835461747999)) ;
#78682 = CARTESIAN_POINT('Ctrl Pts',(70.3361962896516,219.6589309827,23.8909151565592)) ;
#78683 = CARTESIAN_POINT('Ctrl Pts',(70.3591097193747,219.641847052182,23.9136254788598)) ;
#78684 = CARTESIAN_POINT('Ctrl Pts',(70.3679199332324,219.635278280804,23.9263737714492)) ;
#78685 = CARTESIAN_POINT('Ctrl Pts',(70.377726918825,219.627966330455,23.9486436004895)) ;
#78686 = CARTESIAN_POINT('Ctrl Pts',(70.380437698525,219.625945211286,23.9569014064467)) ;
#78687 = CARTESIAN_POINT('Ctrl Pts',(70.3840992101215,219.623215239804,23.9739095905764)) ;
#78688 = CARTESIAN_POINT('Ctrl Pts',(70.3850625789433,219.622496965577,23.98258579457)) ;
#78689 = CARTESIAN_POINT('Ctrl Pts',(70.3850625789433,219.622496965577,23.9913203435596)) ;
#78690 = CARTESIAN_POINT('',(70.3022814706893,218.330941191344,23.9913203435596)) ;
#78691 = CARTESIAN_POINT('Origin',(103.767178705518,216.834469413397,23.9913203435596)) ;
#78692 = CARTESIAN_POINT('',(70.1824009080094,218.33629382542,23.8713203435596)) ;
#78693 = CARTESIAN_POINT('Origin',(70.1824009080094,218.33629382542,23.9913203435596)) ;
#78694 = CARTESIAN_POINT('Ctrl Pts',(70.1824009080094,218.33629382542,23.8713203435596)) ;
#78695 = CARTESIAN_POINT('Ctrl Pts',(70.201713852236,218.768837240123,23.8713203435596)) ;
#78696 = CARTESIAN_POINT('Ctrl Pts',(70.2294710222707,219.201001932498,23.8713203435596)) ;
#78697 = CARTESIAN_POINT('Ctrl Pts',(70.2675518310552,219.657324069064,23.8713203435596)) ;
#78698 = CARTESIAN_POINT('Ctrl Pts',(70.2696254029687,219.68217167068,23.8713203435596)) ;
#78699 = CARTESIAN_POINT('Ctrl Pts',(70.2716989748822,219.707019272295,23.8713203435596)) ;
#78700 = CARTESIAN_POINT('Ctrl Pts',(70.3022814706893,218.330941191344,23.9913203435596)) ;
#78701 = CARTESIAN_POINT('Ctrl Pts',(70.2676697182798,217.555757180025,23.9913203435596)) ;
#78702 = CARTESIAN_POINT('Ctrl Pts',(70.2602736675229,216.779393400763,23.9913203435596)) ;
#78703 = CARTESIAN_POINT('Ctrl Pts',(70.2813572214291,216.003852832276,23.9913203435596)) ;
#78704 = CARTESIAN_POINT('Ctrl Pts',(70.3022814706893,218.330941191344,23.9554164275186)) ;
#78705 = CARTESIAN_POINT('Ctrl Pts',(70.2676701188078,217.555766150471,23.9554164275186)) ;
#78706 = CARTESIAN_POINT('Ctrl Pts',(70.2602739227663,216.779384011854,23.9554164275186)) ;
#78707 = CARTESIAN_POINT('Ctrl Pts',(70.2813572214291,216.003852832276,23.9554164275186)) ;
#78708 = CARTESIAN_POINT('Ctrl Pts',(70.2721528923875,218.33228642406,23.8932840614142)) ;
#78709 = CARTESIAN_POINT('Ctrl Pts',(70.2375095501616,217.556394909683,23.8932840614142)) ;
#78710 = CARTESIAN_POINT('Ctrl Pts',(70.2301060791862,216.779314330808,23.8932840614142)) ;
#78711 = CARTESIAN_POINT('Ctrl Pts',(70.2512097642495,216.003033254856,23.8932840614142)) ;
#78712 = CARTESIAN_POINT('Ctrl Pts',(70.2093020433682,218.335092697142,23.8713203435596)) ;
#78713 = CARTESIAN_POINT('Ctrl Pts',(70.1745930291305,217.557730355953,23.8713203435596)) ;
#78714 = CARTESIAN_POINT('Ctrl Pts',(70.1671739965509,216.779144060255,23.8713203435596)) ;
#78715 = CARTESIAN_POINT('Ctrl Pts',(70.1883195322401,216.001323544686,23.8713203435596)) ;
#78716 = CARTESIAN_POINT('Ctrl Pts',(70.1824009080094,218.33629382542,23.8713203435596)) ;
#78717 = CARTESIAN_POINT('Ctrl Pts',(70.14766382781,217.558302903379,23.8713203435596)) ;
#78718 = CARTESIAN_POINT('Ctrl Pts',(70.1402381191435,216.779070181469,23.8713203435596)) ;
#78719 = CARTESIAN_POINT('Ctrl Pts',(70.1614015403524,216.000591762293,23.8713203435596)) ;
#78720 = CARTESIAN_POINT('Origin',(99.3986297236392,223.018122277899,23.8713203435596)) ;
#78721 = CARTESIAN_POINT('Origin',(99.1329946691538,222.962162901338,23.9913203435596)) ;
#78722 = CARTESIAN_POINT('Ctrl Pts',(70.4779346423502,213.258471670562,23.8713203435596)) ;
#78723 = CARTESIAN_POINT('Ctrl Pts',(70.4779346423502,213.258471670562,31.6713203435596)) ;
#78724 = CARTESIAN_POINT('Ctrl Pts',(70.4761055561897,213.274084092013,23.8713203435596)) ;
#78725 = CARTESIAN_POINT('Ctrl Pts',(70.4761055561897,213.274084092013,31.6713203435596)) ;
#78726 = CARTESIAN_POINT('Ctrl Pts',(70.4123720009514,213.821196392358,23.8713203435596)) ;
#78727 = CARTESIAN_POINT('Ctrl Pts',(70.4123720009514,213.821196392358,31.6713203435596)) ;
#78728 = CARTESIAN_POINT('Ctrl Pts',(70.3612615606319,214.369323962879,23.8713203435596)) ;
#78729 = CARTESIAN_POINT('Ctrl Pts',(70.3612615606319,214.369323962879,31.6713203435596)) ;
#78730 = CARTESIAN_POINT('Ctrl Pts',(70.3225171301736,214.918446124758,23.8713203435596)) ;
#78731 = CARTESIAN_POINT('Ctrl Pts',(70.3225171301736,214.918446124758,31.6713203435596)) ;
#78732 = CARTESIAN_POINT('Ctrl Pts',(70.2959099128609,215.468544476001,23.8713203435596)) ;
#78733 = CARTESIAN_POINT('Ctrl Pts',(70.2959099128609,215.468544476001,31.6713203435596)) ;
#78734 = CARTESIAN_POINT('Ctrl Pts',(70.2813572214291,216.003852832275,23.8713203435596)) ;
#78735 = CARTESIAN_POINT('Ctrl Pts',(70.2813572214291,216.003852832275,31.6713203435596)) ;
#78736 = CARTESIAN_POINT('',(70.4779346423502,213.258471670562,23.8713203435596)) ;
#78737 = CARTESIAN_POINT('',(70.2813572214291,216.003852832276,23.8713203435596)) ;
#78738 = CARTESIAN_POINT('Ctrl Pts',(70.2813572214291,216.003852832276,23.8713203435596)) ;
#78739 = CARTESIAN_POINT('Ctrl Pts',(70.2813572214291,216.003852832276,31.6713203435596)) ;
#78740 = CARTESIAN_POINT('Ctrl Pts',(70.2788401464342,216.096441291563,23.8713203435596)) ;
#78741 = CARTESIAN_POINT('Ctrl Pts',(70.2788401464342,216.096441291563,31.6713203435596)) ;
#78742 = CARTESIAN_POINT('Ctrl Pts',(70.2679178621387,216.560643904903,23.8713203435596)) ;
#78743 = CARTESIAN_POINT('Ctrl Pts',(70.2679178621387,216.560643904903,31.6713203435596)) ;
#78744 = CARTESIAN_POINT('Ctrl Pts',(70.2654637030854,217.025527604889,23.8713203435596)) ;
#78745 = CARTESIAN_POINT('Ctrl Pts',(70.2654637030854,217.025527604889,31.6713203435596)) ;
#78746 = CARTESIAN_POINT('Ctrl Pts',(70.2713796878849,217.491084510933,23.8713203435596)) ;
#78747 = CARTESIAN_POINT('Ctrl Pts',(70.2713796878849,217.491084510933,31.6713203435596)) ;
#78748 = CARTESIAN_POINT('Ctrl Pts',(70.2855989071304,217.957309241547,23.8713203435596)) ;
#78749 = CARTESIAN_POINT('Ctrl Pts',(70.2855989071304,217.957309241547,31.6713203435596)) ;
#78750 = CARTESIAN_POINT('Ctrl Pts',(70.3022814706893,218.330941191344,23.8713203435596)) ;
#78751 = CARTESIAN_POINT('Ctrl Pts',(70.3022814706893,218.330941191344,31.6713203435596)) ;
#78752 = CARTESIAN_POINT('',(70.3022814706893,218.330941191344,23.8713203435596)) ;
#78753 = CARTESIAN_POINT('Ctrl Pts',(70.3022814706893,218.330941191344,23.8713203435596)) ;
#78754 = CARTESIAN_POINT('Ctrl Pts',(70.3022814706893,218.330941191344,31.6713203435596)) ;
#78755 = CARTESIAN_POINT('Ctrl Pts',(70.3137968902541,218.588846917257,23.8713203435596)) ;
#78756 = CARTESIAN_POINT('Ctrl Pts',(70.3137968902541,218.588846917257,31.6713203435596)) ;
#78757 = CARTESIAN_POINT('Ctrl Pts',(70.3278377342262,218.846955761663,23.8713203435596)) ;
#78758 = CARTESIAN_POINT('Ctrl Pts',(70.3278377342262,218.846955761663,31.6713203435596)) ;
#78759 = CARTESIAN_POINT('Ctrl Pts',(70.3443973562324,219.105267189998,23.8713203435596)) ;
#78760 = CARTESIAN_POINT('Ctrl Pts',(70.3443973562324,219.105267189998,31.6713203435596)) ;
#78761 = CARTESIAN_POINT('Ctrl Pts',(70.3634723134982,219.363780925362,23.8713203435596)) ;
#78762 = CARTESIAN_POINT('Ctrl Pts',(70.3634723134982,219.363780925362,31.6713203435596)) ;
#78763 = CARTESIAN_POINT('Ctrl Pts',(70.3850625789433,219.622496965577,23.8713203435596)) ;
#78764 = CARTESIAN_POINT('Ctrl Pts',(70.3850625789433,219.622496965577,31.6713203435596)) ;
#78765 = CARTESIAN_POINT('',(70.3850625789433,219.622496965577,23.8713203435596)) ;
#78766 = CARTESIAN_POINT('Origin',(70.3850625789433,219.622496965577,23.8713203435596)) ;
#78767 = CARTESIAN_POINT('',(64.9830939940346,223.650128668,23.8713203435596)) ;
#78768 = CARTESIAN_POINT('',(64.9830939940346,223.650128668,23.8713203435596)) ;
#78769 = CARTESIAN_POINT('',(64.9830939940346,223.650128668,23.8713203435596)) ;
#78770 = CARTESIAN_POINT('Origin',(60.9557289941889,214.062457729594,17.9913203435596)) ;
#78771 = CARTESIAN_POINT('Origin',(60.9557289941889,214.062457729594,17.9913203435596)) ;
#78772 = CARTESIAN_POINT('',(60.8531713625061,214.124762883342,17.9913203435596)) ;
#78773 = CARTESIAN_POINT('Origin',(60.9557289941889,214.062457729594,17.9913203435596)) ;
#78774 = CARTESIAN_POINT('Origin',(60.9557289941889,214.062457729594,17.9913203435596)) ;
#78775 = CARTESIAN_POINT('Origin',(60.9557289910913,214.062457729895,17.9913203435596)) ;
#78776 = CARTESIAN_POINT('Ctrl Pts',(60.9673257563026,214.181896061416,23.7513203435596)) ;
#78777 = CARTESIAN_POINT('Ctrl Pts',(60.9673257563026,214.181896061416,16.8393203435596)) ;
#78778 = CARTESIAN_POINT('Ctrl Pts',(60.9300677412812,214.185513596343,23.7513203435596)) ;
#78779 = CARTESIAN_POINT('Ctrl Pts',(60.9300677412812,214.185513596343,16.8393203435596)) ;
#78780 = CARTESIAN_POINT('Ctrl Pts',(60.8750422973704,214.163785096389,23.7513203435596)) ;
#78781 = CARTESIAN_POINT('Ctrl Pts',(60.8750422973704,214.163785096389,16.8393203435596)) ;
#78782 = CARTESIAN_POINT('Ctrl Pts',(60.8364976384102,214.097504784634,23.7513203435596)) ;
#78783 = CARTESIAN_POINT('Ctrl Pts',(60.8364976384102,214.097504784634,16.8393203435596)) ;
#78784 = CARTESIAN_POINT('Ctrl Pts',(60.8338841153326,214.059085002227,23.7513203435596)) ;
#78785 = CARTESIAN_POINT('Ctrl Pts',(60.8338841153326,214.059085002227,16.8393203435596)) ;
#78786 = CARTESIAN_POINT('Ctrl Pts',(60.8382191089243,214.038138460174,23.7513203435596)) ;
#78787 = CARTESIAN_POINT('Ctrl Pts',(60.8382191089243,214.038138460174,16.8393203435596)) ;
#78788 = CARTESIAN_POINT('Ctrl Pts',(61.1448474062677,212.657605881144,17.9913203435596)) ;
#78789 = CARTESIAN_POINT('Ctrl Pts',(61.0358864187945,213.1162730929,17.9913203435596)) ;
#78790 = CARTESIAN_POINT('Ctrl Pts',(60.9337505575544,213.576533739222,17.9913203435596)) ;
#78791 = CARTESIAN_POINT('Ctrl Pts',(60.8382191077639,214.038138465781,17.9913203435596)) ;
#78792 = CARTESIAN_POINT('Ctrl Pts',(61.1448474062677,212.657605881144,17.9554164275186)) ;
#78793 = CARTESIAN_POINT('Ctrl Pts',(61.0358855397407,213.116276793244,17.9554164275186)) ;
#78794 = CARTESIAN_POINT('Ctrl Pts',(60.9337512988544,213.576530157286,17.9554164275186)) ;
#78795 = CARTESIAN_POINT('Ctrl Pts',(60.8382191077639,214.038138465781,17.9554164275186)) ;
#78796 = CARTESIAN_POINT('Ctrl Pts',(61.1741891643601,212.664576309494,17.8932837582075)) ;
#78797 = CARTESIAN_POINT('Ctrl Pts',(61.0652975082516,213.122951673457,17.8932837582075)) ;
#78798 = CARTESIAN_POINT('Ctrl Pts',(60.9632246192255,213.582928155348,17.8932837582075)) ;
#78799 = CARTESIAN_POINT('Ctrl Pts',(60.8677516360983,214.044250372973,17.8932837582075)) ;
#78800 = CARTESIAN_POINT('Ctrl Pts',(61.2353993963615,212.679117412829,17.8713203435596)) ;
#78801 = CARTESIAN_POINT('Ctrl Pts',(61.1266518731003,213.136886054948,17.8713203435596)) ;
#78802 = CARTESIAN_POINT('Ctrl Pts',(61.0247112733278,213.596265593577,17.8713203435596)) ;
#78803 = CARTESIAN_POINT('Ctrl Pts',(60.9293598364399,214.057000503894,17.8713203435596)) ;
#78804 = CARTESIAN_POINT('Ctrl Pts',(61.2615982170329,212.685341204933,17.8713203435596)) ;
#78805 = CARTESIAN_POINT('Ctrl Pts',(61.1529122911993,213.142850554979,17.8713203435596)) ;
#78806 = CARTESIAN_POINT('Ctrl Pts',(61.0510284852321,213.601973819837,17.8713203435596)) ;
#78807 = CARTESIAN_POINT('Ctrl Pts',(60.9557289930313,214.062457735187,17.8713203435596)) ;
#78808 = CARTESIAN_POINT('Origin',(61.2615982170329,212.685341204933,17.9913203435596)) ;
#78809 = CARTESIAN_POINT('Ctrl Pts',(65.2679705316376,202.055835489823,17.9913203435596)) ;
#78810 = CARTESIAN_POINT('Ctrl Pts',(63.3524709375853,205.346379782453,17.9913203435596)) ;
#78811 = CARTESIAN_POINT('Ctrl Pts',(62.0239099776425,208.957224782185,17.9913203435596)) ;
#78812 = CARTESIAN_POINT('Ctrl Pts',(61.1448474062769,212.657605881106,17.9913203435596)) ;
#78813 = CARTESIAN_POINT('Ctrl Pts',(65.2679705316376,202.055835489823,17.9554164275186)) ;
#78814 = CARTESIAN_POINT('Ctrl Pts',(63.3524488993449,205.346417640882,17.9554164275186)) ;
#78815 = CARTESIAN_POINT('Ctrl Pts',(62.0239170695688,208.957194928986,17.9554164275186)) ;
#78816 = CARTESIAN_POINT('Ctrl Pts',(61.1448474062769,212.657605881106,17.9554164275186)) ;
#78817 = CARTESIAN_POINT('Ctrl Pts',(65.2940343849798,202.071007843105,17.8932837406185)) ;
#78818 = CARTESIAN_POINT('Ctrl Pts',(63.3802729567682,205.358566224537,17.8932837406185)) ;
#78819 = CARTESIAN_POINT('Ctrl Pts',(62.0526923780858,208.966549742266,17.8932837406185)) ;
#78820 = CARTESIAN_POINT('Ctrl Pts',(61.174189150107,212.664576306067,17.8932837406185)) ;
#78821 = CARTESIAN_POINT('Ctrl Pts',(65.3484065753611,202.10265911394,17.8713203435596)) ;
#78822 = CARTESIAN_POINT('Ctrl Pts',(63.4382586169361,205.384010090046,17.8713203435596)) ;
#78823 = CARTESIAN_POINT('Ctrl Pts',(62.1127398064059,208.985985687741,17.8713203435596)) ;
#78824 = CARTESIAN_POINT('Ctrl Pts',(61.2353993963707,212.67911741279,17.8713203435596)) ;
#78825 = CARTESIAN_POINT('Ctrl Pts',(65.3716786148033,202.116206289769,17.8713203435596)) ;
#78826 = CARTESIAN_POINT('Ctrl Pts',(63.4630749292305,205.394904434083,17.8713203435596)) ;
#78827 = CARTESIAN_POINT('Ctrl Pts',(62.1384416786349,208.994301365774,17.8713203435596)) ;
#78828 = CARTESIAN_POINT('Ctrl Pts',(61.2615982170421,212.685341204894,17.8713203435596)) ;
#78829 = CARTESIAN_POINT('Origin',(65.3716786148033,202.116206289769,17.9913203435596)) ;
#78830 = CARTESIAN_POINT('Ctrl Pts',(66.1952689412975,200.555835489821,17.9913203435596)) ;
#78831 = CARTESIAN_POINT('Ctrl Pts',(65.8729833388596,201.047515223108,17.9913203435596)) ;
#78832 = CARTESIAN_POINT('Ctrl Pts',(65.5637332147713,201.547759052751,17.9913203435596)) ;
#78833 = CARTESIAN_POINT('Ctrl Pts',(65.2679705316394,202.05583548982,17.9913203435596)) ;
#78834 = CARTESIAN_POINT('Ctrl Pts',(66.1952689412975,200.555835489821,17.9554164275186)) ;
#78835 = CARTESIAN_POINT('Ctrl Pts',(65.872979631281,201.0475208794,17.9554164275186)) ;
#78836 = CARTESIAN_POINT('Ctrl Pts',(65.5637366175855,201.547753207221,17.9554164275186)) ;
#78837 = CARTESIAN_POINT('Ctrl Pts',(65.2679705316394,202.05583548982,17.9554164275186)) ;
#78838 = CARTESIAN_POINT('Ctrl Pts',(66.2204915925578,200.572368400995,17.893283631872)) ;
#78839 = CARTESIAN_POINT('Ctrl Pts',(65.8984984085001,201.063602020059,17.893283631872)) ;
#78840 = CARTESIAN_POINT('Ctrl Pts',(65.5895286083177,201.563392400006,17.893283631872)) ;
#78841 = CARTESIAN_POINT('Ctrl Pts',(65.2940343066537,202.071007797505,17.893283631872)) ;
#78842 = CARTESIAN_POINT('Ctrl Pts',(66.2731091727483,200.60685810513,17.8713203435596)) ;
#78843 = CARTESIAN_POINT('Ctrl Pts',(65.9517238967264,201.097164298152,17.8713203435596)) ;
#78844 = CARTESIAN_POINT('Ctrl Pts',(65.6433429392842,201.596002170755,17.8713203435596)) ;
#78845 = CARTESIAN_POINT('Ctrl Pts',(65.3484065753628,202.102659113937,17.8713203435596)) ;
#78846 = CARTESIAN_POINT('Ctrl Pts',(66.2956301826422,200.621620147878,17.8713203435596)) ;
#78847 = CARTESIAN_POINT('Ctrl Pts',(65.974504705631,201.111529990869,17.8713203435596)) ;
#78848 = CARTESIAN_POINT('Ctrl Pts',(65.6663765353022,201.609958957032,17.8713203435596)) ;
#78849 = CARTESIAN_POINT('Ctrl Pts',(65.371678614805,202.116206289766,17.8713203435596)) ;
#78850 = CARTESIAN_POINT('Origin',(66.2956301826422,200.621620147878,17.9913203435596)) ;
#78851 = CARTESIAN_POINT('Ctrl Pts',(77.1237619644425,189.518281677405,17.9913203435596)) ;
#78852 = CARTESIAN_POINT('Ctrl Pts',(75.3192709150292,190.827610386593,17.9913203435596)) ;
#78853 = CARTESIAN_POINT('Ctrl Pts',(71.2757417352347,194.115942691271,17.9913203435596)) ;
#78854 = CARTESIAN_POINT('Ctrl Pts',(67.8274231206578,198.065816930128,17.9913203435596)) ;
#78855 = CARTESIAN_POINT('Ctrl Pts',(66.1952689412979,200.55583548982,17.9913203435596)) ;
#78856 = CARTESIAN_POINT('Ctrl Pts',(77.1237619644425,189.518281677405,17.9554164275186)) ;
#78857 = CARTESIAN_POINT('Ctrl Pts',(75.3192591302046,190.827618937596,17.9554164275186)) ;
#78858 = CARTESIAN_POINT('Ctrl Pts',(71.2757353479458,194.115940571234,17.9554164275186)) ;
#78859 = CARTESIAN_POINT('Ctrl Pts',(67.8274418969853,198.065788284915,17.9554164275186)) ;
#78860 = CARTESIAN_POINT('Ctrl Pts',(66.1952689412979,200.55583548982,17.9554164275186)) ;
#78861 = CARTESIAN_POINT('Ctrl Pts',(77.1414733768851,189.542691197338,17.8932836220364)) ;
#78862 = CARTESIAN_POINT('Ctrl Pts',(75.337911801841,190.851345485072,17.8932836220364)) ;
#78863 = CARTESIAN_POINT('Ctrl Pts',(71.2966204784694,194.137907568835,17.8932836220364)) ;
#78864 = CARTESIAN_POINT('Ctrl Pts',(67.8511648677532,198.084609097503,17.8932836220364)) ;
#78865 = CARTESIAN_POINT('Ctrl Pts',(66.2204915857024,200.5723683965,17.8932836220364)) ;
#78866 = CARTESIAN_POINT('Ctrl Pts',(77.1784215957542,189.59361250516,17.8713203435596)) ;
#78867 = CARTESIAN_POINT('Ctrl Pts',(75.3767923032757,190.900864739369,17.8713203435596)) ;
#78868 = CARTESIAN_POINT('Ctrl Pts',(71.340172504427,194.183727838921,17.8713203435596)) ;
#78869 = CARTESIAN_POINT('Ctrl Pts',(67.9007038200928,198.123795579057,17.8713203435596)) ;
#78870 = CARTESIAN_POINT('Ctrl Pts',(66.2731091727487,200.60685810513,17.8713203435596)) ;
#78871 = CARTESIAN_POINT('Ctrl Pts',(77.1942359127805,189.615407485539,17.8713203435596)) ;
#78872 = CARTESIAN_POINT('Ctrl Pts',(75.3934324114903,190.922060530236,17.8713203435596)) ;
#78873 = CARTESIAN_POINT('Ctrl Pts',(71.3588126586277,194.203339283954,17.8713203435596)) ;
#78874 = CARTESIAN_POINT('Ctrl Pts',(67.9219091272743,198.140564861203,17.8713203435596)) ;
#78875 = CARTESIAN_POINT('Ctrl Pts',(66.2956301826426,200.621620147878,17.8713203435596)) ;
#78876 = CARTESIAN_POINT('Origin',(77.1942359127805,189.615407485539,17.9913203435596)) ;
#78877 = CARTESIAN_POINT('Ctrl Pts',(77.1942359127805,189.615407485539,17.8713203435596)) ;
#78878 = CARTESIAN_POINT('Ctrl Pts',(77.3771291752412,189.482701147464,17.8713203435596)) ;
#78879 = CARTESIAN_POINT('Ctrl Pts',(77.602534818386,189.409539758744,17.8713203435596)) ;
#78880 = CARTESIAN_POINT('Ctrl Pts',(77.8285014478222,189.409539758744,17.8713203435596)) ;
#78881 = CARTESIAN_POINT('Ctrl Pts',(77.1731501567454,189.5863475117,17.8713203435596)) ;
#78882 = CARTESIAN_POINT('Ctrl Pts',(77.3621499339522,189.449210320354,17.8713203435596)) ;
#78883 = CARTESIAN_POINT('Ctrl Pts',(77.5949901525182,189.373635842703,17.8713203435596)) ;
#78884 = CARTESIAN_POINT('Ctrl Pts',(77.8285014478222,189.373635842703,17.8713203435596)) ;
#78885 = CARTESIAN_POINT('Ctrl Pts',(77.1366606256317,189.536058358312,17.9014785774642)) ;
#78886 = CARTESIAN_POINT('Ctrl Pts',(77.3361495975408,189.391310265396,17.9014785774642)) ;
#78887 = CARTESIAN_POINT('Ctrl Pts',(77.5820306375505,189.311503042755,17.9014785774642)) ;
#78888 = CARTESIAN_POINT('Ctrl Pts',(77.8285014478223,189.311503042755,17.9014785774642)) ;
#78889 = CARTESIAN_POINT('Ctrl Pts',(77.1237619644425,189.518281677405,17.9643924065289)) ;
#78890 = CARTESIAN_POINT('Ctrl Pts',(77.3269932166768,189.370818206616,17.9643924065289)) ;
#78891 = CARTESIAN_POINT('Ctrl Pts',(77.5774070092107,189.289539758744,17.9643924065289)) ;
#78892 = CARTESIAN_POINT('Ctrl Pts',(77.8285014478222,189.289539758744,17.9643924065289)) ;
#78893 = CARTESIAN_POINT('Ctrl Pts',(77.1237619644425,189.518281677405,17.9913203435596)) ;
#78894 = CARTESIAN_POINT('Ctrl Pts',(77.3269767005103,189.370830190655,17.9913203435596)) ;
#78895 = CARTESIAN_POINT('Ctrl Pts',(77.5774274151154,189.289539758744,17.9913203435596)) ;
#78896 = CARTESIAN_POINT('Ctrl Pts',(77.8285014478222,189.289539758744,17.9913203435596)) ;
#78897 = CARTESIAN_POINT('',(77.8285014478222,189.289539758744,17.9913203435596)) ;
#78898 = CARTESIAN_POINT('Origin',(77.8285014478222,189.409539758744,17.9913203435596)) ;
#78899 = CARTESIAN_POINT('Origin',(77.7368311963088,190.20710947193,17.9913203435596)) ;
#78900 = CARTESIAN_POINT('Origin',(71.6000791389318,189.409539758744,17.9913203435596)) ;
#78901 = CARTESIAN_POINT('',(83.2194473860051,189.289539758744,17.9913203435596)) ;
#78902 = CARTESIAN_POINT('Origin',(83.2194473860051,189.409539758744,17.9913203435596)) ;
#78903 = CARTESIAN_POINT('',(71.6000791389318,189.289539758744,17.9913203435596)) ;
#78904 = CARTESIAN_POINT('Ctrl Pts',(83.2194473860051,189.409539758744,17.8713203435596)) ;
#78905 = CARTESIAN_POINT('Ctrl Pts',(83.3047606779792,189.409539758744,17.8713203435596)) ;
#78906 = CARTESIAN_POINT('Ctrl Pts',(83.4319242412693,189.454563257398,17.8713203435596)) ;
#78907 = CARTESIAN_POINT('Ctrl Pts',(83.5764307889551,189.615888430006,17.8713203435596)) ;
#78908 = CARTESIAN_POINT('Ctrl Pts',(83.6266013556018,189.835500488137,17.8713203435596)) ;
#78909 = CARTESIAN_POINT('Ctrl Pts',(83.5482147548371,189.998322839904,17.8713203435596)) ;
#78910 = CARTESIAN_POINT('Ctrl Pts',(83.4878143389934,190.058573545737,17.8713203435596)) ;
#78911 = CARTESIAN_POINT('Ctrl Pts',(83.2194473860051,189.373635842703,17.8713203435596)) ;
#78912 = CARTESIAN_POINT('Ctrl Pts',(83.3128563436082,189.373635842703,17.8713203435596)) ;
#78913 = CARTESIAN_POINT('Ctrl Pts',(83.452045237747,189.422831326517,17.8713203435596)) ;
#78914 = CARTESIAN_POINT('Ctrl Pts',(83.6102461518883,189.599420760862,17.8713203435596)) ;
#78915 = CARTESIAN_POINT('Ctrl Pts',(83.6651611847245,189.83983301376,17.8713203435596)) ;
#78916 = CARTESIAN_POINT('Ctrl Pts',(83.5793027341283,190.018024833018,17.8713203435596)) ;
#78917 = CARTESIAN_POINT('Ctrl Pts',(83.5131707193836,190.083992931264,17.8713203435596)) ;
#78918 = CARTESIAN_POINT('Ctrl Pts',(83.2194473860052,189.311503153976,17.9014786701593)) ;
#78919 = CARTESIAN_POINT('Ctrl Pts',(83.3267623139629,189.311503153976,17.9014786701593)) ;
#78920 = CARTESIAN_POINT('Ctrl Pts',(83.4867304273842,189.368162111536,17.9014786701593)) ;
#78921 = CARTESIAN_POINT('Ctrl Pts',(83.6685085212826,189.571102519156,17.9014786701593)) ;
#78922 = CARTESIAN_POINT('Ctrl Pts',(83.7316216438234,189.847360366321,17.9014786701593)) ;
#78923 = CARTESIAN_POINT('Ctrl Pts',(83.6330278294468,190.052192963681,17.9014786701593)) ;
#78924 = CARTESIAN_POINT('Ctrl Pts',(83.5570506150538,190.127981859013,17.9014786701593)) ;
#78925 = CARTESIAN_POINT('Ctrl Pts',(83.2194473860051,189.289539758744,17.9643924065289)) ;
#78926 = CARTESIAN_POINT('Ctrl Pts',(83.3317236137326,189.289539758744,17.9643924065289)) ;
#78927 = CARTESIAN_POINT('Ctrl Pts',(83.4990506182369,189.348729786032,17.9643924065289)) ;
#78928 = CARTESIAN_POINT('Ctrl Pts',(83.6892163988353,189.561013301822,17.9643924065289)) ;
#78929 = CARTESIAN_POINT('Ctrl Pts',(83.755232904682,189.850008116062,17.9643924065289)) ;
#78930 = CARTESIAN_POINT('Ctrl Pts',(83.6520515313444,190.064238875503,17.9643924065289)) ;
#78931 = CARTESIAN_POINT('Ctrl Pts',(83.5725617978318,190.143531583735,17.9643924065289)) ;
#78932 = CARTESIAN_POINT('Ctrl Pts',(83.2194473860051,189.289539758744,17.9913203435596)) ;
#78933 = CARTESIAN_POINT('Ctrl Pts',(83.33170171755,189.289539758744,17.9913203435596)) ;
#78934 = CARTESIAN_POINT('Ctrl Pts',(83.4990221955632,189.348781204342,17.9913203435596)) ;
#78935 = CARTESIAN_POINT('Ctrl Pts',(83.6891623898867,189.5610511683,17.9913203435596)) ;
#78936 = CARTESIAN_POINT('Ctrl Pts',(83.7551762933692,189.850014402682,17.9913203435596)) ;
#78937 = CARTESIAN_POINT('Ctrl Pts',(83.6520360292051,190.064254339218,17.9913203435596)) ;
#78938 = CARTESIAN_POINT('Ctrl Pts',(83.5725617978318,190.143531583735,17.9913203435596)) ;
#78939 = CARTESIAN_POINT('',(83.5725617978318,190.143531583735,17.9913203435596)) ;
#78940 = CARTESIAN_POINT('Origin',(83.4878143389934,190.058573545737,17.9913203435596)) ;
#78941 = CARTESIAN_POINT('Ctrl Pts',(83.5725617978318,190.143531583735,17.9913203435596)) ;
#78942 = CARTESIAN_POINT('Ctrl Pts',(83.6520392110072,190.064251165302,17.9913203435596)) ;
#78943 = CARTESIAN_POINT('Ctrl Pts',(83.7551748851088,189.850164868248,17.9913203435596)) ;
#78944 = CARTESIAN_POINT('Ctrl Pts',(83.6762811453293,189.502581007553,17.9913203435596)) ;
#78945 = CARTESIAN_POINT('Ctrl Pts',(83.4441273250624,189.317541444415,17.9913203435596)) ;
#78946 = CARTESIAN_POINT('Ctrl Pts',(83.2755767988648,189.289539758744,17.9913203435596)) ;
#78947 = CARTESIAN_POINT('Ctrl Pts',(83.2194473860051,189.289539758744,17.9913203435596)) ;
#78948 = CARTESIAN_POINT('Ctrl Pts',(74.1761041106884,202.05583548982,17.9913203435596)) ;
#78949 = CARTESIAN_POINT('Ctrl Pts',(75.2361074248711,200.159916764409,17.9913203435596)) ;
#78950 = CARTESIAN_POINT('Ctrl Pts',(78.1041044154073,195.960565221311,17.9913203435596)) ;
#78951 = CARTESIAN_POINT('Ctrl Pts',(81.5183138237629,192.192687846391,17.9913203435596)) ;
#78952 = CARTESIAN_POINT('Ctrl Pts',(83.5725617978318,190.143531583735,17.9913203435596)) ;
#78953 = CARTESIAN_POINT('Ctrl Pts',(74.1761041106884,202.05583548982,17.9554164275186)) ;
#78954 = CARTESIAN_POINT('Ctrl Pts',(75.2360961966516,200.159936847168,17.9554164275186)) ;
#78955 = CARTESIAN_POINT('Ctrl Pts',(78.1040924841332,195.960587192884,17.9554164275186)) ;
#78956 = CARTESIAN_POINT('Ctrl Pts',(81.5183233608015,192.192678332992,17.9554164275186)) ;
#78957 = CARTESIAN_POINT('Ctrl Pts',(83.5725617978318,190.143531583735,17.9554164275186)) ;
#78958 = CARTESIAN_POINT('Ctrl Pts',(74.1497806371692,202.041118103047,17.8932837799342)) ;
#78959 = CARTESIAN_POINT('Ctrl Pts',(75.2106695260217,200.143615441457,17.8932837799342)) ;
#78960 = CARTESIAN_POINT('Ctrl Pts',(78.0806203331662,195.941491968631,17.8932837799342)) ;
#78961 = CARTESIAN_POINT('Ctrl Pts',(81.4962629295466,192.172086546055,17.8932837799342)) ;
#78962 = CARTESIAN_POINT('Ctrl Pts',(83.5512630940976,190.122179957315,17.8932837799342)) ;
#78963 = CARTESIAN_POINT('Ctrl Pts',(74.0948669375562,202.010415993931,17.8713203435596)) ;
#78964 = CARTESIAN_POINT('Ctrl Pts',(75.1575968459697,200.109620490316,17.8713203435596)) ;
#78965 = CARTESIAN_POINT('Ctrl Pts',(78.0316231323412,195.901715537708,17.8713203435596)) ;
#78966 = CARTESIAN_POINT('Ctrl Pts',(81.4502677323176,192.129104525146,17.8713203435596)) ;
#78967 = CARTESIAN_POINT('Ctrl Pts',(83.506831624286,190.077638084882,17.8713203435596)) ;
#78968 = CARTESIAN_POINT('Ctrl Pts',(74.071363112532,201.997275065426,17.8713203435596)) ;
#78969 = CARTESIAN_POINT('Ctrl Pts',(75.1348798094609,200.095072314249,17.8713203435596)) ;
#78970 = CARTESIAN_POINT('Ctrl Pts',(78.0106503827396,195.884693008864,17.8713203435596)) ;
#78971 = CARTESIAN_POINT('Ctrl Pts',(81.4305821636459,192.110706612955,17.8713203435596)) ;
#78972 = CARTESIAN_POINT('Ctrl Pts',(83.4878143389934,190.058573545737,17.8713203435596)) ;
#78973 = CARTESIAN_POINT('',(74.1761041106884,202.05583548982,17.9913203435596)) ;
#78974 = CARTESIAN_POINT('Origin',(74.071363112532,201.997275065426,17.9913203435596)) ;
#78975 = CARTESIAN_POINT('Ctrl Pts',(74.1761041106884,202.05583548982,17.9913203435596)) ;
#78976 = CARTESIAN_POINT('Ctrl Pts',(74.2838092722993,201.863194363147,17.9913203435596)) ;
#78977 = CARTESIAN_POINT('Ctrl Pts',(74.7358054436199,201.068974645156,17.9913203435596)) ;
#78978 = CARTESIAN_POINT('Ctrl Pts',(75.5850166034805,199.677432982293,17.9913203435596)) ;
#78979 = CARTESIAN_POINT('Ctrl Pts',(76.933494947875,197.696777376424,17.9913203435596)) ;
#78980 = CARTESIAN_POINT('Ctrl Pts',(78.784019206408,195.312002858836,17.9913203435596)) ;
#78981 = CARTESIAN_POINT('Ctrl Pts',(80.6886895533707,193.132887074724,17.9913203435596)) ;
#78982 = CARTESIAN_POINT('Ctrl Pts',(82.1803361041117,191.549821741792,17.9913203435596)) ;
#78983 = CARTESIAN_POINT('Ctrl Pts',(83.16020700552,190.554864302944,17.9913203435596)) ;
#78984 = CARTESIAN_POINT('Ctrl Pts',(83.5725617978318,190.143531583735,17.9913203435596)) ;
#78985 = CARTESIAN_POINT('Ctrl Pts',(70.5067868147823,213.020459099211,17.9913203435596)) ;
#78986 = CARTESIAN_POINT('Ctrl Pts',(70.7134450664337,211.371105542151,17.9913203435596)) ;
#78987 = CARTESIAN_POINT('Ctrl Pts',(71.5202034275434,207.561661620558,17.9913203435596)) ;
#78988 = CARTESIAN_POINT('Ctrl Pts',(73.0937605573685,203.991711899461,17.9913203435596)) ;
#78989 = CARTESIAN_POINT('Ctrl Pts',(74.1761041106882,202.05583548982,17.9913203435596)) ;
#78990 = CARTESIAN_POINT('Ctrl Pts',(70.5067868147823,213.020459099211,17.9554164275186)) ;
#78991 = CARTESIAN_POINT('Ctrl Pts',(70.7134424086352,211.371126754222,17.9554164275186)) ;
#78992 = CARTESIAN_POINT('Ctrl Pts',(71.5202054125703,207.561684097306,17.9554164275186)) ;
#78993 = CARTESIAN_POINT('Ctrl Pts',(73.0937720222297,203.991691393444,17.9554164275186)) ;
#78994 = CARTESIAN_POINT('Ctrl Pts',(74.1761041106882,202.05583548982,17.9554164275186)) ;
#78995 = CARTESIAN_POINT('Ctrl Pts',(70.4768623382484,213.016709666608,17.8932838954934)) ;
#78996 = CARTESIAN_POINT('Ctrl Pts',(70.6837302116549,211.365683104068,17.8932838954934)) ;
#78997 = CARTESIAN_POINT('Ctrl Pts',(71.4913439175855,207.552164797002,17.8932838954934)) ;
#78998 = CARTESIAN_POINT('Ctrl Pts',(73.0665327610701,203.978611784322,17.8932838954934)) ;
#78999 = CARTESIAN_POINT('Ctrl Pts',(74.149780553105,202.041118056048,17.8932838954934)) ;
#79000 = CARTESIAN_POINT('Ctrl Pts',(70.4144368399205,213.00888796926,17.8713203435596)) ;
#79001 = CARTESIAN_POINT('Ctrl Pts',(70.6217404956101,211.354383398689,17.8713203435596)) ;
#79002 = CARTESIAN_POINT('Ctrl Pts',(71.4311411755023,207.532366228087,17.8713203435596)) ;
#79003 = CARTESIAN_POINT('Ctrl Pts',(73.0097393253103,203.951271962955,17.8713203435596)) ;
#79004 = CARTESIAN_POINT('Ctrl Pts',(74.0948669375559,202.010415993931,17.8713203435596)) ;
#79005 = CARTESIAN_POINT('Ctrl Pts',(70.3877178199639,213.005540169192,17.8713203435596)) ;
#79006 = CARTESIAN_POINT('Ctrl Pts',(70.5952077140308,211.34954921747,17.8713203435596)) ;
#79007 = CARTESIAN_POINT('Ctrl Pts',(71.4053737386935,207.523894544389,17.8713203435596)) ;
#79008 = CARTESIAN_POINT('Ctrl Pts',(72.9854321297061,203.939567940643,17.8713203435596)) ;
#79009 = CARTESIAN_POINT('Ctrl Pts',(74.0713631125318,201.997275065426,17.8713203435596)) ;
#79010 = CARTESIAN_POINT('Origin',(70.3877178199639,213.005540169192,17.9913203435596)) ;
#79011 = CARTESIAN_POINT('Ctrl Pts',(70.5067868147823,213.020459099211,17.9913203435596)) ;
#79012 = CARTESIAN_POINT('Ctrl Pts',(70.7134450664337,211.371105542151,17.9913203435596)) ;
#79013 = CARTESIAN_POINT('Ctrl Pts',(71.5202034275434,207.561661620558,17.9913203435596)) ;
#79014 = CARTESIAN_POINT('Ctrl Pts',(73.0937605573685,203.991711899461,17.9913203435596)) ;
#79015 = CARTESIAN_POINT('Ctrl Pts',(74.1761041106882,202.05583548982,17.9913203435596)) ;
#79016 = CARTESIAN_POINT('Ctrl Pts',(70.3877178199639,213.005540169192,17.8713203435596)) ;
#79017 = CARTESIAN_POINT('Ctrl Pts',(70.3834041808396,213.039967616326,17.8713203435596)) ;
#79018 = CARTESIAN_POINT('Ctrl Pts',(70.3494702400649,213.117382991064,17.8713203435596)) ;
#79019 = CARTESIAN_POINT('Ctrl Pts',(70.2725551198838,213.157848509207,17.8713203435596)) ;
#79020 = CARTESIAN_POINT('Ctrl Pts',(70.2265094709067,213.162319271896,17.8713203435596)) ;
#79021 = CARTESIAN_POINT('Ctrl Pts',(70.423343179906,213.010003902616,17.8713203435596)) ;
#79022 = CARTESIAN_POINT('Ctrl Pts',(70.4181653875406,213.05132821552,17.8713203435596)) ;
#79023 = CARTESIAN_POINT('Ctrl Pts',(70.3774821996608,213.144204826472,17.8713203435596)) ;
#79024 = CARTESIAN_POINT('Ctrl Pts',(70.2852492082989,213.192688744648,17.8713203435596)) ;
#79025 = CARTESIAN_POINT('Ctrl Pts',(70.2299792140174,213.198055137211,17.8713203435596)) ;
#79026 = CARTESIAN_POINT('Ctrl Pts',(70.4849936629844,213.017728493254,17.9014788019101)) ;
#79027 = CARTESIAN_POINT('Ctrl Pts',(70.4783315097396,213.070899591259,17.9014788019101)) ;
#79028 = CARTESIAN_POINT('Ctrl Pts',(70.425910882421,213.190474327809,17.9014788019101)) ;
#79029 = CARTESIAN_POINT('Ctrl Pts',(70.307098386221,213.252992031279,17.9014788019101)) ;
#79030 = CARTESIAN_POINT('Ctrl Pts',(70.2359836821624,213.259896852312,17.9014788019101)) ;
#79031 = CARTESIAN_POINT('Ctrl Pts',(70.5067868147823,213.020459099211,17.9643924065289)) ;
#79032 = CARTESIAN_POINT('Ctrl Pts',(70.4995950789841,213.077856831581,17.9643924065289)) ;
#79033 = CARTESIAN_POINT('Ctrl Pts',(70.4430506906804,213.206894672446,17.9643924065289)) ;
#79034 = CARTESIAN_POINT('Ctrl Pts',(70.3148739302152,213.274303910178,17.9643924065289)) ;
#79035 = CARTESIAN_POINT('Ctrl Pts',(70.2381062330204,213.281757603718,17.9643924065289)) ;
#79036 = CARTESIAN_POINT('Ctrl Pts',(70.5067868147823,213.020459099211,17.9913203435596)) ;
#79037 = CARTESIAN_POINT('Ctrl Pts',(70.4995974162418,213.077838177768,17.9913203435596)) ;
#79038 = CARTESIAN_POINT('Ctrl Pts',(70.4430408482841,213.206863802331,17.9913203435596)) ;
#79039 = CARTESIAN_POINT('Ctrl Pts',(70.3148489813156,213.27430633257,17.9913203435596)) ;
#79040 = CARTESIAN_POINT('Ctrl Pts',(70.2381062330204,213.281757603718,17.9913203435596)) ;
#79041 = CARTESIAN_POINT('Origin',(70.2265094709067,213.162319271896,17.9913203435596)) ;
#79042 = CARTESIAN_POINT('Origin',(67.5325794977657,213.423884085911,17.9913203435596)) ;
#79043 = CARTESIAN_POINT('Origin',(77.4412221473412,189.289539758744,23.8713203435596)) ;
#79044 = CARTESIAN_POINT('',(77.8285014478222,189.289539758744,17.9913203435596)) ;
#79045 = CARTESIAN_POINT('',(83.2194473860052,189.289539758744,30.2513203435596)) ;
#79046 = CARTESIAN_POINT('Ctrl Pts',(83.5725617978318,190.143531583735,17.9913203435596)) ;
#79047 = CARTESIAN_POINT('Ctrl Pts',(83.5725617978318,190.143531583735,32.7033203435596)) ;
#79048 = CARTESIAN_POINT('Ctrl Pts',(83.6520392110072,190.064251165302,17.9913203435596)) ;
#79049 = CARTESIAN_POINT('Ctrl Pts',(83.6520392110072,190.064251165302,32.7033203435596)) ;
#79050 = CARTESIAN_POINT('Ctrl Pts',(83.7551748851088,189.850164868248,17.9913203435596)) ;
#79051 = CARTESIAN_POINT('Ctrl Pts',(83.7551748851088,189.850164868248,32.7033203435596)) ;
#79052 = CARTESIAN_POINT('Ctrl Pts',(83.6762811453293,189.502581007553,17.9913203435596)) ;
#79053 = CARTESIAN_POINT('Ctrl Pts',(83.6762811453293,189.502581007553,32.7033203435596)) ;
#79054 = CARTESIAN_POINT('Ctrl Pts',(83.4441273250624,189.317541444415,17.9913203435596)) ;
#79055 = CARTESIAN_POINT('Ctrl Pts',(83.4441273250624,189.317541444415,32.7033203435596)) ;
#79056 = CARTESIAN_POINT('Ctrl Pts',(83.2755767988648,189.289539758744,17.9913203435596)) ;
#79057 = CARTESIAN_POINT('Ctrl Pts',(83.2755767988648,189.289539758744,32.7033203435596)) ;
#79058 = CARTESIAN_POINT('Ctrl Pts',(83.2194473860051,189.289539758744,17.9913203435596)) ;
#79059 = CARTESIAN_POINT('Ctrl Pts',(83.2194473860051,189.289539758744,32.7033203435596)) ;
#79060 = CARTESIAN_POINT('',(83.5725617978318,190.143531583735,17.9913203435596)) ;
#79061 = CARTESIAN_POINT('Ctrl Pts',(84.4412221473412,189.289539758744,17.8713203435596)) ;
#79062 = CARTESIAN_POINT('Ctrl Pts',(84.4412221473412,189.289539758744,32.8713203435596)) ;
#79063 = CARTESIAN_POINT('Ctrl Pts',(83.8416464716194,189.870585945118,17.8713203435596)) ;
#79064 = CARTESIAN_POINT('Ctrl Pts',(83.8416464716194,189.870585945118,32.8713203435596)) ;
#79065 = CARTESIAN_POINT('Ctrl Pts',(82.6693997344123,191.034842241154,17.8713203435596)) ;
#79066 = CARTESIAN_POINT('Ctrl Pts',(82.6693997344123,191.034842241154,32.8713203435596)) ;
#79067 = CARTESIAN_POINT('Ctrl Pts',(80.9917381958488,192.787718030768,17.8713203435596)) ;
#79068 = CARTESIAN_POINT('Ctrl Pts',(80.9917381958488,192.787718030768,32.8713203435596)) ;
#79069 = CARTESIAN_POINT('Ctrl Pts',(78.9189744912756,195.138085698398,17.8713203435596)) ;
#79070 = CARTESIAN_POINT('Ctrl Pts',(78.9189744912756,195.138085698398,32.8713203435596)) ;
#79071 = CARTESIAN_POINT('Ctrl Pts',(76.933494947875,197.696777376424,17.8713203435596)) ;
#79072 = CARTESIAN_POINT('Ctrl Pts',(76.933494947875,197.696777376424,32.8713203435596)) ;
#79073 = CARTESIAN_POINT('Ctrl Pts',(75.5850166034805,199.677432982293,17.8713203435596)) ;
#79074 = CARTESIAN_POINT('Ctrl Pts',(75.5850166034805,199.677432982293,32.8713203435596)) ;
#79075 = CARTESIAN_POINT('Ctrl Pts',(74.7358054436199,201.068974645156,17.8713203435596)) ;
#79076 = CARTESIAN_POINT('Ctrl Pts',(74.7358054436199,201.068974645156,32.8713203435596)) ;
#79077 = CARTESIAN_POINT('Ctrl Pts',(74.2838092722993,201.863194363147,17.8713203435596)) ;
#79078 = CARTESIAN_POINT('Ctrl Pts',(74.2838092722993,201.863194363147,32.8713203435596)) ;
#79079 = CARTESIAN_POINT('Ctrl Pts',(74.1761041106884,202.05583548982,17.8713203435596)) ;
#79080 = CARTESIAN_POINT('Ctrl Pts',(74.1761041106884,202.05583548982,32.8713203435596)) ;
#79081 = CARTESIAN_POINT('',(74.1761041106884,202.05583548982,23.8713203435596)) ;
#79082 = CARTESIAN_POINT('Ctrl Pts',(74.1761041106882,202.05583548982,17.8713203435596)) ;
#79083 = CARTESIAN_POINT('Ctrl Pts',(74.1761041106882,202.05583548982,32.8713203435596)) ;
#79084 = CARTESIAN_POINT('Ctrl Pts',(73.9471261103511,202.465384849466,17.8713203435596)) ;
#79085 = CARTESIAN_POINT('Ctrl Pts',(73.9471261103511,202.465384849466,32.8713203435596)) ;
#79086 = CARTESIAN_POINT('Ctrl Pts',(73.4020528825475,203.478780571653,17.8713203435596)) ;
#79087 = CARTESIAN_POINT('Ctrl Pts',(73.4020528825475,203.478780571653,32.8713203435596)) ;
#79088 = CARTESIAN_POINT('Ctrl Pts',(72.6149447082149,205.101979283954,17.8713203435596)) ;
#79089 = CARTESIAN_POINT('Ctrl Pts',(72.6149447082149,205.101979283954,32.8713203435596)) ;
#79090 = CARTESIAN_POINT('Ctrl Pts',(71.7263234125876,207.330523545477,17.8713203435596)) ;
#79091 = CARTESIAN_POINT('Ctrl Pts',(71.7263234125876,207.330523545477,32.8713203435596)) ;
#79092 = CARTESIAN_POINT('Ctrl Pts',(71.0883402872662,209.579226496892,17.8713203435596)) ;
#79093 = CARTESIAN_POINT('Ctrl Pts',(71.0883402872662,209.579226496892,32.8713203435596)) ;
#79094 = CARTESIAN_POINT('Ctrl Pts',(70.7249576044374,211.422049476544,17.8713203435596)) ;
#79095 = CARTESIAN_POINT('Ctrl Pts',(70.7249576044374,211.422049476544,32.8713203435596)) ;
#79096 = CARTESIAN_POINT('Ctrl Pts',(70.5491399848247,212.650688483389,17.8713203435596)) ;
#79097 = CARTESIAN_POINT('Ctrl Pts',(70.5491399848247,212.650688483389,32.8713203435596)) ;
#79098 = CARTESIAN_POINT('Ctrl Pts',(70.4779346423502,213.258471670562,17.8713203435596)) ;
#79099 = CARTESIAN_POINT('Ctrl Pts',(70.4779346423502,213.258471670562,32.8713203435596)) ;
#79100 = CARTESIAN_POINT('Origin',(69.1686691234544,219.464553538579,23.8713203435596)) ;
#79101 = CARTESIAN_POINT('',(68.8712529610467,219.761969700987,23.8713203435596)) ;
#79102 = CARTESIAN_POINT('',(70.8292893218811,217.803933340152,23.8713203435596)) ;
#79103 = CARTESIAN_POINT('',(68.8712529610467,219.761969700987,23.8713203435596)) ;
#79104 = CARTESIAN_POINT('Ctrl Pts',(62.0562434701708,214.076168533126,23.8713203435596)) ;
#79105 = CARTESIAN_POINT('Ctrl Pts',(62.0562434701708,214.076168533126,31.6713203435596)) ;
#79106 = CARTESIAN_POINT('Ctrl Pts',(61.9621987792398,214.520814350555,23.8713203435596)) ;
#79107 = CARTESIAN_POINT('Ctrl Pts',(61.9621987792398,214.520814350555,31.6713203435596)) ;
#79108 = CARTESIAN_POINT('Ctrl Pts',(61.8739898282105,214.96907079501,23.8713203435596)) ;
#79109 = CARTESIAN_POINT('Ctrl Pts',(61.8739898282105,214.96907079501,31.6713203435596)) ;
#79110 = CARTESIAN_POINT('Ctrl Pts',(61.7916108526749,215.420902931566,23.8713203435596)) ;
#79111 = CARTESIAN_POINT('Ctrl Pts',(61.7916108526749,215.420902931566,31.6713203435596)) ;
#79112 = CARTESIAN_POINT('',(61.9703773266185,214.491161471122,30.2513203435596)) ;
#79113 = CARTESIAN_POINT('Ctrl Pts',(61.9703773266185,214.491161471122,26.4913203435596)) ;
#79114 = CARTESIAN_POINT('Ctrl Pts',(61.9703773266185,214.491161471122,31.0033203435596)) ;
#79115 = CARTESIAN_POINT('Ctrl Pts',(61.8515957900547,215.078199641461,26.4913203435596)) ;
#79116 = CARTESIAN_POINT('Ctrl Pts',(61.8515957900547,215.078199641461,31.0033203435596)) ;
#79117 = CARTESIAN_POINT('Ctrl Pts',(61.7916108526749,215.677118589864,26.4913203435596)) ;
#79118 = CARTESIAN_POINT('Ctrl Pts',(61.7916108526749,215.677118589864,31.0033203435596)) ;
#79119 = CARTESIAN_POINT('Ctrl Pts',(61.7916108526749,216.276053366666,26.4913203435596)) ;
#79120 = CARTESIAN_POINT('Ctrl Pts',(61.7916108526749,216.276053366666,31.0033203435596)) ;
#79121 = CARTESIAN_POINT('',(61.7916108526749,216.276053366666,26.4913203435596)) ;
#79122 = CARTESIAN_POINT('Ctrl Pts',(69.2315751790255,211.872432002476,23.4913203435596)) ;
#79123 = CARTESIAN_POINT('Ctrl Pts',(69.2315751790255,211.872432002476,31.6033203435596)) ;
#79124 = CARTESIAN_POINT('Ctrl Pts',(69.305984945383,211.865207250202,23.4913203435596)) ;
#79125 = CARTESIAN_POINT('Ctrl Pts',(69.305984945383,211.865207250202,31.6033203435596)) ;
#79126 = CARTESIAN_POINT('Ctrl Pts',(69.4305433706759,211.801563422573,23.4913203435596)) ;
#79127 = CARTESIAN_POINT('Ctrl Pts',(69.4305433706759,211.801563422573,31.6033203435596)) ;
#79128 = CARTESIAN_POINT('Ctrl Pts',(69.4892247478019,211.678623976047,23.4913203435596)) ;
#79129 = CARTESIAN_POINT('Ctrl Pts',(69.4892247478019,211.678623976047,31.6033203435596)) ;
#79130 = CARTESIAN_POINT('Ctrl Pts',(69.4984736650468,211.623322295552,23.4913203435596)) ;
#79131 = CARTESIAN_POINT('Ctrl Pts',(69.4984736650468,211.623322295552,31.6033203435596)) ;
#79132 = CARTESIAN_POINT('',(69.2315751790255,211.872432002476,30.2513203435596)) ;
#79133 = CARTESIAN_POINT('',(69.4984736650468,211.623322295552,23.4913203435596)) ;
#79134 = CARTESIAN_POINT('Origin',(62.4092970952969,212.53483522599,23.8713203435596)) ;
#79135 = CARTESIAN_POINT('Ctrl Pts',(72.3111547045756,202.05583548982,30.2513203435596)) ;
#79136 = CARTESIAN_POINT('Ctrl Pts',(72.3111547045756,202.05583548982,22.1393203435596)) ;
#79137 = CARTESIAN_POINT('Ctrl Pts',(72.3696846119161,202.05583548982,30.2513203435596)) ;
#79138 = CARTESIAN_POINT('Ctrl Pts',(72.3696846119161,202.05583548982,22.1393203435596)) ;
#79139 = CARTESIAN_POINT('Ctrl Pts',(72.4861965697617,202.091073258586,30.2513203435596)) ;
#79140 = CARTESIAN_POINT('Ctrl Pts',(72.4861965697617,202.091073258586,22.1393203435596)) ;
#79141 = CARTESIAN_POINT('Ctrl Pts',(72.6234348552125,202.255646958551,30.2513203435596)) ;
#79142 = CARTESIAN_POINT('Ctrl Pts',(72.6234348552125,202.255646958551,22.1393203435596)) ;
#79143 = CARTESIAN_POINT('Ctrl Pts',(72.6179307032035,202.415805684798,30.2513203435596)) ;
#79144 = CARTESIAN_POINT('Ctrl Pts',(72.6179307032035,202.415805684798,22.1393203435596)) ;
#79145 = CARTESIAN_POINT('Ctrl Pts',(72.5775641491992,202.49377028534,30.2513203435596)) ;
#79146 = CARTESIAN_POINT('Ctrl Pts',(72.5775641491992,202.49377028534,22.1393203435596)) ;
#79147 = CARTESIAN_POINT('',(72.5775641491992,202.49377028534,30.2513203435596)) ;
#79148 = CARTESIAN_POINT('Ctrl Pts',(73.7436956568153,200.410454788892,30.2513203435596)) ;
#79149 = CARTESIAN_POINT('Ctrl Pts',(73.7436956568153,200.410454788892,22.1393203435596)) ;
#79150 = CARTESIAN_POINT('Ctrl Pts',(73.6906445023934,200.49866288572,30.2513203435596)) ;
#79151 = CARTESIAN_POINT('Ctrl Pts',(73.6906445023934,200.49866288572,22.1393203435596)) ;
#79152 = CARTESIAN_POINT('Ctrl Pts',(73.5895427859729,200.55583548982,30.2513203435596)) ;
#79153 = CARTESIAN_POINT('Ctrl Pts',(73.5895427859729,200.55583548982,22.1393203435596)) ;
#79154 = CARTESIAN_POINT('Ctrl Pts',(73.4866103162092,200.55583548982,30.2513203435596)) ;
#79155 = CARTESIAN_POINT('Ctrl Pts',(73.4866103162092,200.55583548982,22.1393203435596)) ;
#79156 = CARTESIAN_POINT('',(73.4866103162092,200.55583548982,30.2513203435596)) ;
#79157 = CARTESIAN_POINT('Ctrl Pts',(77.8285014478222,189.289539758744,17.9913203435596)) ;
#79158 = CARTESIAN_POINT('Ctrl Pts',(77.8285014478222,189.289539758744,32.7033203435596)) ;
#79159 = CARTESIAN_POINT('Ctrl Pts',(77.5774223547909,189.289539758744,17.9913203435596)) ;
#79160 = CARTESIAN_POINT('Ctrl Pts',(77.5774223547909,189.289539758744,32.7033203435596)) ;
#79161 = CARTESIAN_POINT('Ctrl Pts',(77.3269807962441,189.370827218813,17.9913203435596)) ;
#79162 = CARTESIAN_POINT('Ctrl Pts',(77.3269807962441,189.370827218813,32.7033203435596)) ;
#79163 = CARTESIAN_POINT('Ctrl Pts',(77.1237619644425,189.518281677405,17.9913203435596)) ;
#79164 = CARTESIAN_POINT('Ctrl Pts',(77.1237619644425,189.518281677405,32.7033203435596)) ;
#79165 = CARTESIAN_POINT('Ctrl Pts',(73.6566785252795,200.55583548982,17.854339447693)) ;
#79166 = CARTESIAN_POINT('Ctrl Pts',(73.6566785252795,200.55583548982,32.8747165227329)) ;
#79167 = CARTESIAN_POINT('Ctrl Pts',(75.7001422864503,197.125245060908,17.854339447693)) ;
#79168 = CARTESIAN_POINT('Ctrl Pts',(75.7001422864503,197.125245060908,32.8747165227329)) ;
#79169 = CARTESIAN_POINT('Ctrl Pts',(78.3842768400396,193.78102322923,17.854339447693)) ;
#79170 = CARTESIAN_POINT('Ctrl Pts',(78.3842768400396,193.78102322923,32.8747165227329)) ;
#79171 = CARTESIAN_POINT('Ctrl Pts',(81.5507230003364,190.489539758744,17.854339447693)) ;
#79172 = CARTESIAN_POINT('Ctrl Pts',(81.5507230003364,190.489539758744,32.8747165227329)) ;
#79173 = CARTESIAN_POINT('Origin',(67.6417475736039,200.55583548982,23.8713203435596)) ;
#79174 = CARTESIAN_POINT('Ctrl Pts',(69.4614223697787,211.850115187154,17.854339447693)) ;
#79175 = CARTESIAN_POINT('Ctrl Pts',(69.4614223697787,211.850115187154,32.8747165227329)) ;
#79176 = CARTESIAN_POINT('Ctrl Pts',(69.905975823669,209.06303762573,17.854339447693)) ;
#79177 = CARTESIAN_POINT('Ctrl Pts',(69.905975823669,209.06303762573,32.8747165227329)) ;
#79178 = CARTESIAN_POINT('Ctrl Pts',(70.7494560159525,206.30693385077,17.854339447693)) ;
#79179 = CARTESIAN_POINT('Ctrl Pts',(70.7494560159525,206.30693385077,32.8747165227329)) ;
#79180 = CARTESIAN_POINT('Ctrl Pts',(72.0309081730459,203.597341394065,17.854339447693)) ;
#79181 = CARTESIAN_POINT('Ctrl Pts',(72.0309081730459,203.597341394065,32.8747165227329)) ;
#79182 = CARTESIAN_POINT('Ctrl Pts',(72.2749463865981,203.081329852839,17.854339447693)) ;
#79183 = CARTESIAN_POINT('Ctrl Pts',(72.2749463865981,203.081329852839,32.8747165227329)) ;
#79184 = CARTESIAN_POINT('Ctrl Pts',(72.5341913976221,202.567520362575,17.854339447693)) ;
#79185 = CARTESIAN_POINT('Ctrl Pts',(72.5341913976221,202.567520362575,32.8747165227329)) ;
#79186 = CARTESIAN_POINT('Ctrl Pts',(72.8081914673101,202.05583548982,17.854339447693)) ;
#79187 = CARTESIAN_POINT('Ctrl Pts',(72.8081914673101,202.05583548982,32.8747165227329)) ;
#79188 = CARTESIAN_POINT('Origin',(61.7916108526749,215.420902931566,23.8713203435596)) ;
#79189 = CARTESIAN_POINT('',(61.7916108526749,217.432246240363,23.8713203435596)) ;
#79190 = CARTESIAN_POINT('Origin',(69.6705101448823,217.61928420644,23.8713203435596)) ;
#79191 = CARTESIAN_POINT('Origin',(64.1568347953872,220.146231446812,23.8713203435596)) ;
#79192 = CARTESIAN_POINT('',(69.1892193809281,219.722291984294,23.8713203435596)) ;
#79193 = CARTESIAN_POINT('Origin',(67.7485452644419,219.902067758924,23.8713203435596)) ;
#79194 = CARTESIAN_POINT('',(67.7485452644419,219.902067758924,23.8713203435596)) ;
#79195 = CARTESIAN_POINT('Origin',(64.1568347953872,220.146231446812,23.8713203435596)) ;
#79196 = CARTESIAN_POINT('Origin',(64.1568347953872,220.146231446812,23.8713203435596)) ;
#79197 = CARTESIAN_POINT('',(0.,0.,0.)) ;
#79198 = CARTESIAN_POINT('Ctrl Pts',(49.8966187896629,247.701952531225,31.7413203435596)) ;
#79199 = CARTESIAN_POINT('Ctrl Pts',(49.8969225423282,247.6986843043,31.7413203435596)) ;
#79200 = CARTESIAN_POINT('Ctrl Pts',(49.8972304579647,247.69541527565,31.7413203435597)) ;
#79201 = CARTESIAN_POINT('Ctrl Pts',(49.9067236558174,247.591181597776,31.7413203435597)) ;
#79202 = CARTESIAN_POINT('Ctrl Pts',(49.9177374288024,247.504008411497,31.7413203435597)) ;
#79203 = CARTESIAN_POINT('Ctrl Pts',(49.9804256035652,247.364244651485,31.7413203435597)) ;
#79204 = CARTESIAN_POINT('Ctrl Pts',(50.0370077354619,247.298814470324,31.7413203435597)) ;
#79205 = CARTESIAN_POINT('Ctrl Pts',(50.1086106021864,247.221561922593,31.7413203435597)) ;
#79206 = CARTESIAN_POINT('Ctrl Pts',(50.1123189230203,247.217536513008,31.7413203435596)) ;
#79207 = CARTESIAN_POINT('Ctrl Pts',(50.1160311831359,247.213516656002,31.7413203435596)) ;
#79208 = CARTESIAN_POINT('Ctrl Pts',(49.8966187896629,247.701952531225,31.7054164275186)) ;
#79209 = CARTESIAN_POINT('Ctrl Pts',(49.8969225423282,247.6986843043,31.7054164275186)) ;
#79210 = CARTESIAN_POINT('Ctrl Pts',(49.8972304579647,247.69541527565,31.7054164275186)) ;
#79211 = CARTESIAN_POINT('Ctrl Pts',(49.9067236558174,247.591181597776,31.7054164275186)) ;
#79212 = CARTESIAN_POINT('Ctrl Pts',(49.9177374288024,247.504008411497,31.7054164275186)) ;
#79213 = CARTESIAN_POINT('Ctrl Pts',(49.9804256035652,247.364244651485,31.7054164275186)) ;
#79214 = CARTESIAN_POINT('Ctrl Pts',(50.0370077354619,247.298814470324,31.7054164275186)) ;
#79215 = CARTESIAN_POINT('Ctrl Pts',(50.1086106021864,247.221561922593,31.7054164275186)) ;
#79216 = CARTESIAN_POINT('Ctrl Pts',(50.1123189230203,247.217536513008,31.7054164275186)) ;
#79217 = CARTESIAN_POINT('Ctrl Pts',(50.1160311831359,247.213516656002,31.7054164275186)) ;
#79218 = CARTESIAN_POINT('Ctrl Pts',(49.8665894217931,247.699161568194,31.6432842907294)) ;
#79219 = CARTESIAN_POINT('Ctrl Pts',(49.8668865433394,247.69588922041,31.6432842907294)) ;
#79220 = CARTESIAN_POINT('Ctrl Pts',(49.8672076246043,247.692627717528,31.6432842907294)) ;
#79221 = CARTESIAN_POINT('Ctrl Pts',(49.876579092001,247.588366078285,31.6432842907294)) ;
#79222 = CARTESIAN_POINT('Ctrl Pts',(49.8877086829376,247.497236411322,31.6432842907294)) ;
#79223 = CARTESIAN_POINT('Ctrl Pts',(49.9553609719887,247.346407965604,31.6432842907294)) ;
#79224 = CARTESIAN_POINT('Ctrl Pts',(50.0147608319875,247.278282429423,31.6432842907294)) ;
#79225 = CARTESIAN_POINT('Ctrl Pts',(50.0864627823533,247.201105202407,31.6432842907294)) ;
#79226 = CARTESIAN_POINT('Ctrl Pts',(50.0901533731766,247.197072101885,31.6432842907294)) ;
#79227 = CARTESIAN_POINT('Ctrl Pts',(50.0938748615201,247.193055721962,31.6432842907294)) ;
#79228 = CARTESIAN_POINT('Ctrl Pts',(49.8039461216876,247.693339429828,31.6213203435596)) ;
#79229 = CARTESIAN_POINT('Ctrl Pts',(49.8042459616924,247.69006877141,31.6213203435596)) ;
#79230 = CARTESIAN_POINT('Ctrl Pts',(49.8045604603195,247.686803113285,31.6213203435596)) ;
#79231 = CARTESIAN_POINT('Ctrl Pts',(49.8140384370984,247.582601988406,31.6213203435596)) ;
#79232 = CARTESIAN_POINT('Ctrl Pts',(49.8250164956597,247.48333041954,31.6213203435596)) ;
#79233 = CARTESIAN_POINT('Ctrl Pts',(49.903198192551,247.309016626601,31.6213203435597)) ;
#79234 = CARTESIAN_POINT('Ctrl Pts',(49.9686480743411,247.235639578897,31.6213203435596)) ;
#79235 = CARTESIAN_POINT('Ctrl Pts',(50.0402371297429,247.158420268992,31.6213203435597)) ;
#79236 = CARTESIAN_POINT('Ctrl Pts',(50.0439375652229,247.154390629808,31.6213203435596)) ;
#79237 = CARTESIAN_POINT('Ctrl Pts',(50.0476552704109,247.15037282444,31.6213203435596)) ;
#79238 = CARTESIAN_POINT('Ctrl Pts',(49.777133739023,247.690847456999,31.6213203435596)) ;
#79239 = CARTESIAN_POINT('Ctrl Pts',(49.7774374916883,247.687579230074,31.6213203435596)) ;
#79240 = CARTESIAN_POINT('Ctrl Pts',(49.7777435177816,247.684308495694,31.6213203435596)) ;
#79241 = CARTESIAN_POINT('Ctrl Pts',(49.7873269510022,247.580153011363,31.6213203435596)) ;
#79242 = CARTESIAN_POINT('Ctrl Pts',(49.7981748530167,247.477415105803,31.6213203435596)) ;
#79243 = CARTESIAN_POINT('Ctrl Pts',(49.8808922016941,247.292982144188,31.6213203435597)) ;
#79244 = CARTESIAN_POINT('Ctrl Pts',(49.9489601708937,247.21741901313,31.6213203435596)) ;
#79245 = CARTESIAN_POINT('Ctrl Pts',(50.0204478229115,247.14014860368,31.6213203435597)) ;
#79246 = CARTESIAN_POINT('Ctrl Pts',(50.0241602504257,247.136123685724,31.6213203435596)) ;
#79247 = CARTESIAN_POINT('Ctrl Pts',(50.0278725105414,247.132103828718,31.6213203435596)) ;
#79248 = CARTESIAN_POINT('',(49.777133739023,247.690847456999,31.6213203435596)) ;
#79249 = CARTESIAN_POINT('',(50.0278725105413,247.132103828718,31.6213203435596)) ;
#79250 = CARTESIAN_POINT('Ctrl Pts',(49.777133739023,247.690847456999,31.6213203435596)) ;
#79251 = CARTESIAN_POINT('Ctrl Pts',(49.7774374916883,247.687579230074,31.6213203435596)) ;
#79252 = CARTESIAN_POINT('Ctrl Pts',(49.7777435177816,247.684308495694,31.6213203435596)) ;
#79253 = CARTESIAN_POINT('Ctrl Pts',(49.7873269510022,247.580153011363,31.6213203435596)) ;
#79254 = CARTESIAN_POINT('Ctrl Pts',(49.7981748530167,247.477415105803,31.6213203435596)) ;
#79255 = CARTESIAN_POINT('Ctrl Pts',(49.8808922016941,247.292982144188,31.6213203435597)) ;
#79256 = CARTESIAN_POINT('Ctrl Pts',(49.9489601708937,247.21741901313,31.6213203435596)) ;
#79257 = CARTESIAN_POINT('Ctrl Pts',(50.0204478229115,247.14014860368,31.6213203435597)) ;
#79258 = CARTESIAN_POINT('Ctrl Pts',(50.0241602504257,247.136123685724,31.6213203435596)) ;
#79259 = CARTESIAN_POINT('Ctrl Pts',(50.0278725105414,247.132103828718,31.6213203435596)) ;
#79260 = CARTESIAN_POINT('',(50.1048949947523,247.225574360848,31.7413203435596)) ;
#79261 = CARTESIAN_POINT('Ctrl Pts',(50.0278725105414,247.132103828718,31.6213203435596)) ;
#79262 = CARTESIAN_POINT('Ctrl Pts',(50.0280595512392,247.132330804138,31.6213203435596)) ;
#79263 = CARTESIAN_POINT('Ctrl Pts',(50.0282465911107,247.132557779856,31.6213214458748)) ;
#79264 = CARTESIAN_POINT('Ctrl Pts',(50.038504940272,247.145006504587,31.6214422185109)) ;
#79265 = CARTESIAN_POINT('Ctrl Pts',(50.0485724477496,247.15722379173,31.6247500298547)) ;
#79266 = CARTESIAN_POINT('Ctrl Pts',(50.0656603915231,247.177955014042,31.6359582847072)) ;
#79267 = CARTESIAN_POINT('Ctrl Pts',(50.0742393969475,247.18836221985,31.6438392648492)) ;
#79268 = CARTESIAN_POINT('Ctrl Pts',(50.0891026914623,247.206401264955,31.6671840249628)) ;
#79269 = CARTESIAN_POINT('Ctrl Pts',(50.0946683323572,247.213159727899,31.6801574547695)) ;
#79270 = CARTESIAN_POINT('Ctrl Pts',(50.1006035968679,247.220368116857,31.7016634476284)) ;
#79271 = CARTESIAN_POINT('Ctrl Pts',(50.1021875059769,247.22229201451,31.7093904709062)) ;
#79272 = CARTESIAN_POINT('Ctrl Pts',(50.1043315944804,247.224896338963,31.7251872827606)) ;
#79273 = CARTESIAN_POINT('Ctrl Pts',(50.1048906386302,247.225575402442,31.7332454904375)) ;
#79274 = CARTESIAN_POINT('Ctrl Pts',(50.1048906386303,247.225575402442,31.7413203435596)) ;
#79275 = CARTESIAN_POINT('',(49.8975295575751,247.692147713814,31.7413203435596)) ;
#79276 = CARTESIAN_POINT('Ctrl Pts',(50.1048956053956,247.225574924765,31.7413203435597)) ;
#79277 = CARTESIAN_POINT('Ctrl Pts',(50.092755916046,247.23872050556,31.7413203435597)) ;
#79278 = CARTESIAN_POINT('Ctrl Pts',(50.0808929246769,247.251573001433,31.7413203435597)) ;
#79279 = CARTESIAN_POINT('Ctrl Pts',(50.0694690210685,247.264236937633,31.7413203435597)) ;
#79280 = CARTESIAN_POINT('Ctrl Pts',(50.0573611518781,247.277659081954,31.7413203435597)) ;
#79281 = CARTESIAN_POINT('Ctrl Pts',(50.0457460902749,247.290869219247,31.7413203435597)) ;
#79282 = CARTESIAN_POINT('Ctrl Pts',(50.0347633830109,247.303967779101,31.7413203435597)) ;
#79283 = CARTESIAN_POINT('Ctrl Pts',(50.0225934949892,247.318482233765,31.7413203435597)) ;
#79284 = CARTESIAN_POINT('Ctrl Pts',(50.0111997909391,247.332859565364,31.7413203435597)) ;
#79285 = CARTESIAN_POINT('Ctrl Pts',(50.0007131697972,247.347210090936,31.7413203435597)) ;
#79286 = CARTESIAN_POINT('Ctrl Pts',(49.9892528408923,247.362893097005,31.7413203435597)) ;
#79287 = CARTESIAN_POINT('Ctrl Pts',(49.9788750866055,247.378543740406,31.7413203435597)) ;
#79288 = CARTESIAN_POINT('Ctrl Pts',(49.9696925368555,247.39428001492,31.7413203435597)) ;
#79289 = CARTESIAN_POINT('Ctrl Pts',(49.962085283186,247.407316680693,31.7413203435597)) ;
#79290 = CARTESIAN_POINT('Ctrl Pts',(49.9552968604527,247.420411462331,31.7413203435597)) ;
#79291 = CARTESIAN_POINT('Ctrl Pts',(49.9493716598566,247.433622676736,31.7413203435597)) ;
#79292 = CARTESIAN_POINT('Ctrl Pts',(49.9485345864462,247.435489070306,31.7413203435597)) ;
#79293 = CARTESIAN_POINT('Ctrl Pts',(49.947710735811,247.437366665178,31.7413203435597)) ;
#79294 = CARTESIAN_POINT('Ctrl Pts',(49.9468999191231,247.439255484219,31.7413203435597)) ;
#79295 = CARTESIAN_POINT('Ctrl Pts',(49.9394567849731,247.456594463195,31.7413203435597)) ;
#79296 = CARTESIAN_POINT('Ctrl Pts',(49.9331153249188,247.474880671756,31.7413203435597)) ;
#79297 = CARTESIAN_POINT('Ctrl Pts',(49.9277105050193,247.494120607347,31.7413203435597)) ;
#79298 = CARTESIAN_POINT('Ctrl Pts',(49.9230312826354,247.510777580003,31.7413203435597)) ;
#79299 = CARTESIAN_POINT('Ctrl Pts',(49.9190545065783,247.528149577348,31.7413203435597)) ;
#79300 = CARTESIAN_POINT('Ctrl Pts',(49.9156386352171,247.546225434154,31.7413203435597)) ;
#79301 = CARTESIAN_POINT('Ctrl Pts',(49.9124482520327,247.563108069212,31.7413203435597)) ;
#79302 = CARTESIAN_POINT('Ctrl Pts',(49.9097477074761,247.580604946861,31.7413203435597)) ;
#79303 = CARTESIAN_POINT('Ctrl Pts',(49.9073825196643,247.598689486076,31.7413203435597)) ;
#79304 = CARTESIAN_POINT('Ctrl Pts',(49.9052155686072,247.615258280814,31.7413203435597)) ;
#79305 = CARTESIAN_POINT('Ctrl Pts',(49.9033303248592,247.632320450204,31.7413203435597)) ;
#79306 = CARTESIAN_POINT('Ctrl Pts',(49.9015691997015,247.649838235728,31.7413203435597)) ;
#79307 = CARTESIAN_POINT('Ctrl Pts',(49.9001789372978,247.66366707606,31.7413203435597)) ;
#79308 = CARTESIAN_POINT('Ctrl Pts',(49.8988654497563,247.677779591041,31.7413203435597)) ;
#79309 = CARTESIAN_POINT('Ctrl Pts',(49.897530056052,247.692147760143,31.7413203435597)) ;
#79310 = CARTESIAN_POINT('Ctrl Pts',(49.777133739023,247.690847456999,31.6213203435596)) ;
#79311 = CARTESIAN_POINT('Ctrl Pts',(49.7774262573671,247.690850619957,31.6213203435596)) ;
#79312 = CARTESIAN_POINT('Ctrl Pts',(49.7777187754276,247.690853779499,31.6213214470556)) ;
#79313 = CARTESIAN_POINT('Ctrl Pts',(49.7938052827997,247.691027362574,31.6214426730848)) ;
#79314 = CARTESIAN_POINT('Ctrl Pts',(49.8095865790889,247.691194286689,31.6247713732388)) ;
#79315 = CARTESIAN_POINT('Ctrl Pts',(49.8363324427948,247.691489707221,31.6360317764872)) ;
#79316 = CARTESIAN_POINT('Ctrl Pts',(49.8497322009203,247.691640499545,31.6439353156995)) ;
#79317 = CARTESIAN_POINT('Ctrl Pts',(49.8729530816466,247.691892838565,31.6673317964462)) ;
#79318 = CARTESIAN_POINT('Ctrl Pts',(49.8816380976473,247.69198301369,31.6803265126481)) ;
#79319 = CARTESIAN_POINT('Ctrl Pts',(49.8908743054425,247.69207751469,31.7018134432135)) ;
#79320 = CARTESIAN_POINT('Ctrl Pts',(49.8933328310453,247.692102380517,31.7095135527032)) ;
#79321 = CARTESIAN_POINT('Ctrl Pts',(49.8966608708735,247.692136012753,31.7252506528064)) ;
#79322 = CARTESIAN_POINT('Ctrl Pts',(49.8975283263115,247.692144732519,31.7332777489016)) ;
#79323 = CARTESIAN_POINT('Ctrl Pts',(49.8975283263115,247.692144732519,31.7413203435596)) ;
#79324 = CARTESIAN_POINT('Ctrl Pts',(50.8831605335109,248.366098818484,31.7413203435596)) ;
#79325 = CARTESIAN_POINT('Ctrl Pts',(50.7693177137058,248.364889140804,31.7413203435596)) ;
#79326 = CARTESIAN_POINT('Ctrl Pts',(50.6611870949586,248.363142107183,31.7413203435596)) ;
#79327 = CARTESIAN_POINT('Ctrl Pts',(50.48051672475,248.335752825127,31.7413203435596)) ;
#79328 = CARTESIAN_POINT('Ctrl Pts',(50.3998763353304,248.314886646393,31.7413203435596)) ;
#79329 = CARTESIAN_POINT('Ctrl Pts',(50.31189617328,248.291603218974,31.7413203435597)) ;
#79330 = CARTESIAN_POINT('Ctrl Pts',(50.3087987422526,248.29078568304,31.7413203435596)) ;
#79331 = CARTESIAN_POINT('Ctrl Pts',(50.3057018899657,248.289967396769,31.7413203435596)) ;
#79332 = CARTESIAN_POINT('Ctrl Pts',(50.8831605335109,248.366098818484,31.7054164275186)) ;
#79333 = CARTESIAN_POINT('Ctrl Pts',(50.7693177137058,248.364889140804,31.7054164275186)) ;
#79334 = CARTESIAN_POINT('Ctrl Pts',(50.6611870949586,248.363142107183,31.7054164275186)) ;
#79335 = CARTESIAN_POINT('Ctrl Pts',(50.48051672475,248.335752825127,31.7054164275186)) ;
#79336 = CARTESIAN_POINT('Ctrl Pts',(50.3998763353304,248.314886646393,31.7054164275185)) ;
#79337 = CARTESIAN_POINT('Ctrl Pts',(50.31189617328,248.291603218974,31.7054164275186)) ;
#79338 = CARTESIAN_POINT('Ctrl Pts',(50.3087987422526,248.29078568304,31.7054164275186)) ;
#79339 = CARTESIAN_POINT('Ctrl Pts',(50.3057018899657,248.289967396769,31.7054164275186)) ;
#79340 = CARTESIAN_POINT('Ctrl Pts',(50.8828400884159,248.396255920492,31.6432843121591)) ;
#79341 = CARTESIAN_POINT('Ctrl Pts',(50.7689838795759,248.395080367539,31.6432843121591)) ;
#79342 = CARTESIAN_POINT('Ctrl Pts',(50.6593409446893,248.393370604139,31.6432843121591)) ;
#79343 = CARTESIAN_POINT('Ctrl Pts',(50.4739365108437,248.365260768839,31.6432843121591)) ;
#79344 = CARTESIAN_POINT('Ctrl Pts',(50.3921658146156,248.344058969898,31.6432843121591)) ;
#79345 = CARTESIAN_POINT('Ctrl Pts',(50.3041921025262,248.32076002337,31.6432843121591)) ;
#79346 = CARTESIAN_POINT('Ctrl Pts',(50.3010938281301,248.319945161113,31.6432843121591)) ;
#79347 = CARTESIAN_POINT('Ctrl Pts',(50.297997400334,248.319125488718,31.6432843121591)) ;
#79348 = CARTESIAN_POINT('Ctrl Pts',(50.882171618778,248.459165627568,31.6213203435596)) ;
#79349 = CARTESIAN_POINT('Ctrl Pts',(50.7683209006786,248.457976080325,31.6213203435596)) ;
#79350 = CARTESIAN_POINT('Ctrl Pts',(50.6555070294052,248.456412411503,31.6213203435597)) ;
#79351 = CARTESIAN_POINT('Ctrl Pts',(50.4602045792046,248.426813697693,31.6213203435596)) ;
#79352 = CARTESIAN_POINT('Ctrl Pts',(50.3760989166878,248.404868583297,31.6213203435597)) ;
#79353 = CARTESIAN_POINT('Ctrl Pts',(50.2881197869039,248.381586520614,31.6213203435596)) ;
#79354 = CARTESIAN_POINT('Ctrl Pts',(50.2850219278525,248.380770298768,31.6213203435596)) ;
#79355 = CARTESIAN_POINT('Ctrl Pts',(50.2819253259759,248.379951194812,31.6213203435596)) ;
#79356 = CARTESIAN_POINT('Ctrl Pts',(50.8818855024848,248.486092044526,31.6213203435596)) ;
#79357 = CARTESIAN_POINT('Ctrl Pts',(50.7680426826797,248.484882366845,31.6213203435596)) ;
#79358 = CARTESIAN_POINT('Ctrl Pts',(50.6538689168924,248.483392574996,31.6213203435597)) ;
#79359 = CARTESIAN_POINT('Ctrl Pts',(50.4543262221993,248.453158960515,31.6213203435596)) ;
#79360 = CARTESIAN_POINT('Ctrl Pts',(50.3692249609673,248.430888524762,31.6213203435597)) ;
#79361 = CARTESIAN_POINT('Ctrl Pts',(50.2812403793008,248.407621865807,31.6213203435596)) ;
#79362 = CARTESIAN_POINT('Ctrl Pts',(50.2781430590352,248.406803910429,31.6213203435596)) ;
#79363 = CARTESIAN_POINT('Ctrl Pts',(50.2750462067483,248.405985624158,31.6213203435596)) ;
#79364 = CARTESIAN_POINT('',(50.3149897315107,248.29242201045,31.7413203435596)) ;
#79365 = CARTESIAN_POINT('',(50.8825230540255,248.366092043133,31.7413203435596)) ;
#79366 = CARTESIAN_POINT('Ctrl Pts',(50.3149921209254,248.292422543133,31.7413203435596)) ;
#79367 = CARTESIAN_POINT('Ctrl Pts',(50.3998764650291,248.314886679953,31.7413203435596)) ;
#79368 = CARTESIAN_POINT('Ctrl Pts',(50.4805167880214,248.335752834719,31.7413203435596)) ;
#79369 = CARTESIAN_POINT('Ctrl Pts',(50.6609967037988,248.363113244248,31.7413203435596)) ;
#79370 = CARTESIAN_POINT('Ctrl Pts',(50.7689140351779,248.364882570555,31.7413203435596)) ;
#79371 = CARTESIAN_POINT('Ctrl Pts',(50.8825230540528,248.36609203838,31.7413203435597)) ;
#79372 = CARTESIAN_POINT('',(50.8818855024848,248.486092044526,31.6213203435596)) ;
#79373 = CARTESIAN_POINT('Ctrl Pts',(50.8825230540529,248.366092044717,31.7413203435596)) ;
#79374 = CARTESIAN_POINT('Ctrl Pts',(50.8825534101719,248.366092044717,31.7323443646095)) ;
#79375 = CARTESIAN_POINT('Ctrl Pts',(50.8825723197285,248.367103672931,31.7233637724199)) ;
#79376 = CARTESIAN_POINT('Ctrl Pts',(50.8825808693696,248.369103069156,31.7146074328755)) ;
#79377 = CARTESIAN_POINT('Ctrl Pts',(50.8825893303654,248.371081735008,31.7059418818336)) ;
#79378 = CARTESIAN_POINT('Ctrl Pts',(50.8825876451619,248.374027516586,31.6974967825055)) ;
#79379 = CARTESIAN_POINT('Ctrl Pts',(50.882576866955,248.37786615277,31.6894825551018)) ;
#79380 = CARTESIAN_POINT('Ctrl Pts',(50.8825659193641,248.381765114724,31.6813423807673)) ;
#79381 = CARTESIAN_POINT('Ctrl Pts',(50.8825455907234,248.386584929551,31.6736475899965)) ;
#79382 = CARTESIAN_POINT('Ctrl Pts',(50.8825169846678,248.392198656087,31.6665939655429)) ;
#79383 = CARTESIAN_POINT('Ctrl Pts',(50.8824883786122,248.397812382623,31.6595403410893)) ;
#79384 = CARTESIAN_POINT('Ctrl Pts',(50.8824514951415,248.40421940593,31.6531285618175)) ;
#79385 = CARTESIAN_POINT('Ctrl Pts',(50.8824074378906,248.411251057174,31.6475182829018)) ;
#79386 = CARTESIAN_POINT('Ctrl Pts',(50.8823652042211,248.417991660111,31.642140220023)) ;
#79387 = CARTESIAN_POINT('Ctrl Pts',(50.8823163775403,248.425329993554,31.6374798978438)) ;
#79388 = CARTESIAN_POINT('Ctrl Pts',(50.882263087073,248.433092826769,31.6336584519873)) ;
#79389 = CARTESIAN_POINT('Ctrl Pts',(50.8822098779665,248.440843808143,31.6298428404918)) ;
#79390 = CARTESIAN_POINT('Ctrl Pts',(50.8821522186931,248.449017181676,31.6268640064795)) ;
#79391 = CARTESIAN_POINT('Ctrl Pts',(50.8820922287401,248.457415213738,31.6247972155335)) ;
#79392 = CARTESIAN_POINT('Ctrl Pts',(50.8820322287777,248.465814647027,31.6227300797397)) ;
#79393 = CARTESIAN_POINT('Ctrl Pts',(50.8819698973578,248.474437905681,31.6215755144355)) ;
#79394 = CARTESIAN_POINT('Ctrl Pts',(50.8819073550288,248.483074795671,31.6213582820227)) ;
#79395 = CARTESIAN_POINT('Ctrl Pts',(50.8819000725911,248.48408047637,31.6213329874496)) ;
#79396 = CARTESIAN_POINT('Ctrl Pts',(50.8818927872939,248.485086337244,31.6213203435612)) ;
#79397 = CARTESIAN_POINT('Ctrl Pts',(50.8818855024848,248.486092044526,31.6213203435596)) ;
#79398 = CARTESIAN_POINT('',(50.2750462067483,248.405985624158,31.6213203435596)) ;
#79399 = CARTESIAN_POINT('Ctrl Pts',(50.8818855024848,248.486092044526,31.6213203435596)) ;
#79400 = CARTESIAN_POINT('Ctrl Pts',(50.7680426826797,248.484882366845,31.6213203435596)) ;
#79401 = CARTESIAN_POINT('Ctrl Pts',(50.6538689168924,248.483392574996,31.6213203435597)) ;
#79402 = CARTESIAN_POINT('Ctrl Pts',(50.4543262221993,248.453158960515,31.6213203435596)) ;
#79403 = CARTESIAN_POINT('Ctrl Pts',(50.3692249609673,248.430888524762,31.6213203435597)) ;
#79404 = CARTESIAN_POINT('Ctrl Pts',(50.2812403793008,248.407621865807,31.6213203435596)) ;
#79405 = CARTESIAN_POINT('Ctrl Pts',(50.2781430590352,248.406803910429,31.6213203435596)) ;
#79406 = CARTESIAN_POINT('Ctrl Pts',(50.2750462067483,248.405985624158,31.6213203435596)) ;
#79407 = CARTESIAN_POINT('Ctrl Pts',(50.2750462067483,248.405985624158,31.6213203435597)) ;
#79408 = CARTESIAN_POINT('Ctrl Pts',(50.2751432418492,248.405709761836,31.6213203435597)) ;
#79409 = CARTESIAN_POINT('Ctrl Pts',(50.2752402756055,248.405433899341,31.6213214466179)) ;
#79410 = CARTESIAN_POINT('Ctrl Pts',(50.2805774980751,248.390260268583,31.6214426485925)) ;
#79411 = CARTESIAN_POINT('Ctrl Pts',(50.2858131262488,248.37537442858,31.6247712032253)) ;
#79412 = CARTESIAN_POINT('Ctrl Pts',(50.2946911962445,248.350147654523,31.636032021281)) ;
#79413 = CARTESIAN_POINT('Ctrl Pts',(50.2991400709367,248.337508840197,31.6439361481532)) ;
#79414 = CARTESIAN_POINT('Ctrl Pts',(50.306843750394,248.315602834959,31.667336609376)) ;
#79415 = CARTESIAN_POINT('Ctrl Pts',(50.3097222277476,248.307408665322,31.6803338949418)) ;
#79416 = CARTESIAN_POINT('Ctrl Pts',(50.3127818601181,248.298696206946,31.7018216584692)) ;
#79417 = CARTESIAN_POINT('Ctrl Pts',(50.313595920062,248.296377561573,31.7095201461793)) ;
#79418 = CARTESIAN_POINT('Ctrl Pts',(50.314697907942,248.29323881435,31.7252539715263)) ;
#79419 = CARTESIAN_POINT('Ctrl Pts',(50.3149851263684,248.292420692069,31.7332794168424)) ;
#79420 = CARTESIAN_POINT('Ctrl Pts',(50.3149851263684,248.292420692069,31.7413203435596)) ;
#79421 = CARTESIAN_POINT('Ctrl Pts',(50.090934083219,247.234198089337,31.7413203435596)) ;
#79422 = CARTESIAN_POINT('Ctrl Pts',(50.0955897177682,247.231322397455,31.7413203435596)) ;
#79423 = CARTESIAN_POINT('Ctrl Pts',(50.1002475219359,247.228449453589,31.7413203435596)) ;
#79424 = CARTESIAN_POINT('Ctrl Pts',(50.1974027007021,247.168311194945,31.7413203435596)) ;
#79425 = CARTESIAN_POINT('Ctrl Pts',(50.2828817770592,247.117341800874,31.7413203435594)) ;
#79426 = CARTESIAN_POINT('Ctrl Pts',(50.48239795585,247.050779599937,31.7413203435595)) ;
#79427 = CARTESIAN_POINT('Ctrl Pts',(50.61275116216,247.045540729033,31.7413203435581)) ;
#79428 = CARTESIAN_POINT('Ctrl Pts',(50.754699340979,247.042754795613,31.7413203435597)) ;
#79429 = CARTESIAN_POINT('Ctrl Pts',(50.7551163582219,247.042745762277,31.7413203435596)) ;
#79430 = CARTESIAN_POINT('Ctrl Pts',(50.7555331333966,247.042737076062,31.7413203435596)) ;
#79431 = CARTESIAN_POINT('Ctrl Pts',(50.090934083219,247.234198089337,31.7054164275186)) ;
#79432 = CARTESIAN_POINT('Ctrl Pts',(50.0955897177682,247.231322397455,31.7054164275186)) ;
#79433 = CARTESIAN_POINT('Ctrl Pts',(50.1002475219359,247.228449453589,31.7054164275186)) ;
#79434 = CARTESIAN_POINT('Ctrl Pts',(50.1974027007021,247.168311194945,31.7054164275186)) ;
#79435 = CARTESIAN_POINT('Ctrl Pts',(50.2828817770592,247.117341800874,31.7054164275184)) ;
#79436 = CARTESIAN_POINT('Ctrl Pts',(50.48239795585,247.050779599937,31.7054164275185)) ;
#79437 = CARTESIAN_POINT('Ctrl Pts',(50.61275116216,247.045540729033,31.7054164275171)) ;
#79438 = CARTESIAN_POINT('Ctrl Pts',(50.754699340979,247.042754795613,31.7054164275186)) ;
#79439 = CARTESIAN_POINT('Ctrl Pts',(50.7551163582219,247.042745762277,31.7054164275186)) ;
#79440 = CARTESIAN_POINT('Ctrl Pts',(50.7555331333966,247.042737076062,31.7054164275186)) ;
#79441 = CARTESIAN_POINT('Ctrl Pts',(50.0750852444689,247.208539428997,31.643284293333)) ;
#79442 = CARTESIAN_POINT('Ctrl Pts',(50.079737436052,247.205657852922,31.643284293333)) ;
#79443 = CARTESIAN_POINT('Ctrl Pts',(50.084402484806,247.202796447652,31.643284293333)) ;
#79444 = CARTESIAN_POINT('Ctrl Pts',(50.181499622757,247.142586958144,31.6432842933329)) ;
#79445 = CARTESIAN_POINT('Ctrl Pts',(50.2691603574096,247.090132541043,31.6432842933329)) ;
#79446 = CARTESIAN_POINT('Ctrl Pts',(50.4783018806032,247.020329393151,31.6432842933329)) ;
#79447 = CARTESIAN_POINT('Ctrl Pts',(50.612092332105,247.015290900225,31.6432842933323)) ;
#79448 = CARTESIAN_POINT('Ctrl Pts',(50.7540735388923,247.012605482336,31.6432842933329)) ;
#79449 = CARTESIAN_POINT('Ctrl Pts',(50.7544850390502,247.012590329561,31.6432842933329)) ;
#79450 = CARTESIAN_POINT('Ctrl Pts',(50.7549047158396,247.012584835157,31.643284293333)) ;
#79451 = CARTESIAN_POINT('Ctrl Pts',(50.0420234943591,247.155013727228,31.6213203435596)) ;
#79452 = CARTESIAN_POINT('Ctrl Pts',(50.0466770974599,247.152134563504,31.6213203435596)) ;
#79453 = CARTESIAN_POINT('Ctrl Pts',(50.0513388387582,247.14926712736,31.6213203435596)) ;
#79454 = CARTESIAN_POINT('Ctrl Pts',(50.1484713080158,247.089126522815,31.6213203435596)) ;
#79455 = CARTESIAN_POINT('Ctrl Pts',(50.2404085533977,247.033396611465,31.6213203435596)) ;
#79456 = CARTESIAN_POINT('Ctrl Pts',(50.4699588786217,246.956838370791,31.6213203435596)) ;
#79457 = CARTESIAN_POINT('Ctrl Pts',(50.6108414563099,246.952489795875,31.6213203435594)) ;
#79458 = CARTESIAN_POINT('Ctrl Pts',(50.7527614502915,246.949704550992,31.6213203435596)) ;
#79459 = CARTESIAN_POINT('Ctrl Pts',(50.7531753070812,246.949692023209,31.6213203435596)) ;
#79460 = CARTESIAN_POINT('Ctrl Pts',(50.7535937942914,246.949685220255,31.6213203435596)) ;
#79461 = CARTESIAN_POINT('Ctrl Pts',(50.0278725105413,247.132103828718,31.6213203435596)) ;
#79462 = CARTESIAN_POINT('Ctrl Pts',(50.0325281450905,247.129228136836,31.6213203435596)) ;
#79463 = CARTESIAN_POINT('Ctrl Pts',(50.0371854114367,247.126353120034,31.6213203435596)) ;
#79464 = CARTESIAN_POINT('Ctrl Pts',(50.1343589801246,247.066278119072,31.6213203435596)) ;
#79465 = CARTESIAN_POINT('Ctrl Pts',(50.2280810409672,247.009116738647,31.6213203435596)) ;
#79466 = CARTESIAN_POINT('Ctrl Pts',(50.4664214310973,246.92966815855,31.6213203435596)) ;
#79467 = CARTESIAN_POINT('Ctrl Pts',(50.6103265699945,246.925660041206,31.6213203435594)) ;
#79468 = CARTESIAN_POINT('Ctrl Pts',(50.752198754358,246.922780663952,31.6213203435596)) ;
#79469 = CARTESIAN_POINT('Ctrl Pts',(50.7526159226971,246.922771815846,31.6213203435596)) ;
#79470 = CARTESIAN_POINT('Ctrl Pts',(50.7530326978718,246.922763129631,31.6213203435596)) ;
#79471 = CARTESIAN_POINT('',(50.7530325637488,246.922763132443,31.6213203435596)) ;
#79472 = CARTESIAN_POINT('Ctrl Pts',(50.0278725105413,247.132103828718,31.6213203435596)) ;
#79473 = CARTESIAN_POINT('Ctrl Pts',(50.0325281450905,247.129228136836,31.6213203435596)) ;
#79474 = CARTESIAN_POINT('Ctrl Pts',(50.0371854114367,247.126353120034,31.6213203435596)) ;
#79475 = CARTESIAN_POINT('Ctrl Pts',(50.1343589801246,247.066278119072,31.6213203435596)) ;
#79476 = CARTESIAN_POINT('Ctrl Pts',(50.2280810409672,247.009116738647,31.6213203435596)) ;
#79477 = CARTESIAN_POINT('Ctrl Pts',(50.4664214310973,246.92966815855,31.6213203435596)) ;
#79478 = CARTESIAN_POINT('Ctrl Pts',(50.6103265699945,246.925660041206,31.6213203435594)) ;
#79479 = CARTESIAN_POINT('Ctrl Pts',(50.752198709726,246.922780664858,31.6213203435596)) ;
#79480 = CARTESIAN_POINT('Ctrl Pts',(50.7526158331972,246.922771817744,31.6213203435596)) ;
#79481 = CARTESIAN_POINT('Ctrl Pts',(50.7530325637484,246.922763132426,31.6213203435596)) ;
#79482 = CARTESIAN_POINT('',(50.7542787411678,247.0427631542,31.7413203435596)) ;
#79483 = CARTESIAN_POINT('Ctrl Pts',(50.7530325621815,246.922763132459,31.6213203435596)) ;
#79484 = CARTESIAN_POINT('Ctrl Pts',(50.7527646460474,246.923064784013,31.6213203435596)) ;
#79485 = CARTESIAN_POINT('Ctrl Pts',(50.7525399567633,246.923325470576,31.6213212662913)) ;
#79486 = CARTESIAN_POINT('Ctrl Pts',(50.7496325890277,246.926757551588,31.6213461545782)) ;
#79487 = CARTESIAN_POINT('Ctrl Pts',(50.7470175666196,246.930311340193,31.6214748940474)) ;
#79488 = CARTESIAN_POINT('Ctrl Pts',(50.7435785332281,246.938306579103,31.6222776096934)) ;
#79489 = CARTESIAN_POINT('Ctrl Pts',(50.7426974857717,246.941965162815,31.6228030626945)) ;
#79490 = CARTESIAN_POINT('Ctrl Pts',(50.742015015904,246.951808512294,31.6247263169256)) ;
#79491 = CARTESIAN_POINT('Ctrl Pts',(50.7431812437154,246.957639467861,31.6263476325659)) ;
#79492 = CARTESIAN_POINT('Ctrl Pts',(50.74716434657,246.970554975215,31.630972221387)) ;
#79493 = CARTESIAN_POINT('Ctrl Pts',(50.750429117442,246.977541017359,31.6342831692237)) ;
#79494 = CARTESIAN_POINT('Ctrl Pts',(50.7527478979496,246.985568780879,31.6390534647648)) ;
#79495 = CARTESIAN_POINT('Ctrl Pts',(50.7540558850527,246.99020320561,31.6418509510241)) ;
#79496 = CARTESIAN_POINT('Ctrl Pts',(50.7533210295252,246.999864991888,31.6491953852256)) ;
#79497 = CARTESIAN_POINT('Ctrl Pts',(50.751086767988,247.003933060654,31.6527832509983)) ;
#79498 = CARTESIAN_POINT('Ctrl Pts',(50.7460406591654,247.012784207256,31.6616377388116)) ;
#79499 = CARTESIAN_POINT('Ctrl Pts',(50.7421051714273,247.018704860938,31.6684626416789)) ;
#79500 = CARTESIAN_POINT('Ctrl Pts',(50.7399004608286,247.028197434459,31.6835662597949)) ;
#79501 = CARTESIAN_POINT('Ctrl Pts',(50.7403530673341,247.031356765315,31.6897667463312)) ;
#79502 = CARTESIAN_POINT('Ctrl Pts',(50.7435531726753,247.037095265575,31.7039618703478)) ;
#79503 = CARTESIAN_POINT('Ctrl Pts',(50.7464670059396,247.039184790426,31.7113680720848)) ;
#79504 = CARTESIAN_POINT('Ctrl Pts',(50.7517448065935,247.042040603547,31.7260362201993)) ;
#79505 = CARTESIAN_POINT('Ctrl Pts',(50.7542745642648,247.042763132459,31.7337592180439)) ;
#79506 = CARTESIAN_POINT('Ctrl Pts',(50.7542745642651,247.042763132459,31.7413203435596)) ;
#79507 = CARTESIAN_POINT('Ctrl Pts',(50.7542787425273,247.042763219434,31.7413203435596)) ;
#79508 = CARTESIAN_POINT('Ctrl Pts',(50.7271094895703,247.043329467085,31.7413203435593)) ;
#79509 = CARTESIAN_POINT('Ctrl Pts',(50.7003265960474,247.043892035075,31.7413203435591)) ;
#79510 = CARTESIAN_POINT('Ctrl Pts',(50.6740010884586,247.044750914502,31.741320343559)) ;
#79511 = CARTESIAN_POINT('Ctrl Pts',(50.6460147492917,247.045663979173,31.7413203435589)) ;
#79512 = CARTESIAN_POINT('Ctrl Pts',(50.618545300155,247.046911831848,31.7413203435589)) ;
#79513 = CARTESIAN_POINT('Ctrl Pts',(50.59166023966,247.048796849032,31.7413203435589)) ;
#79514 = CARTESIAN_POINT('Ctrl Pts',(50.5637291844762,247.050755205011,31.7413203435589)) ;
#79515 = CARTESIAN_POINT('Ctrl Pts',(50.536428756022,247.053400881479,31.741320343559)) ;
#79516 = CARTESIAN_POINT('Ctrl Pts',(50.5098172256807,247.057016257844,31.7413203435591)) ;
#79517 = CARTESIAN_POINT('Ctrl Pts',(50.4812755613452,247.060893857416,31.7413203435592)) ;
#79518 = CARTESIAN_POINT('Ctrl Pts',(50.4535262834992,247.065886704076,31.7413203435593)) ;
#79519 = CARTESIAN_POINT('Ctrl Pts',(50.4266229919826,247.072283650437,31.7413203435594)) ;
#79520 = CARTESIAN_POINT('Ctrl Pts',(50.407159438196,247.076911608673,31.7413203435594)) ;
#79521 = CARTESIAN_POINT('Ctrl Pts',(50.3881382694205,247.082273157551,31.7413203435595)) ;
#79522 = CARTESIAN_POINT('Ctrl Pts',(50.369574863394,247.088461667103,31.7413203435594)) ;
#79523 = CARTESIAN_POINT('Ctrl Pts',(50.3695707922032,247.088463024321,31.7413203435594)) ;
#79524 = CARTESIAN_POINT('Ctrl Pts',(50.3695667210145,247.088464381587,31.7413203435594)) ;
#79525 = CARTESIAN_POINT('Ctrl Pts',(50.3695626498277,247.088465738898,31.7413203435594)) ;
#79526 = CARTESIAN_POINT('Ctrl Pts',(50.346746489969,247.096072522687,31.7413203435594)) ;
#79527 = CARTESIAN_POINT('Ctrl Pts',(50.3239939476063,247.105139848513,31.7413203435594)) ;
#79528 = CARTESIAN_POINT('Ctrl Pts',(50.3011789250779,247.115462173694,31.7413203435595)) ;
#79529 = CARTESIAN_POINT('Ctrl Pts',(50.280021321461,247.12503462379,31.7413203435595)) ;
#79530 = CARTESIAN_POINT('Ctrl Pts',(50.2588101814923,247.135686992053,31.7413203435595)) ;
#79531 = CARTESIAN_POINT('Ctrl Pts',(50.2374330483465,247.147216651365,31.7413203435595)) ;
#79532 = CARTESIAN_POINT('Ctrl Pts',(50.2173075360903,247.158071254656,31.7413203435595)) ;
#79533 = CARTESIAN_POINT('Ctrl Pts',(50.19703505635,247.169703937684,31.7413203435596)) ;
#79534 = CARTESIAN_POINT('Ctrl Pts',(50.1765083716673,247.181902012136,31.7413203435596)) ;
#79535 = CARTESIAN_POINT('Ctrl Pts',(50.1573661728375,247.19327734966,31.7413203435596)) ;
#79536 = CARTESIAN_POINT('Ctrl Pts',(50.1380029859063,247.205144648437,31.7413203435596)) ;
#79537 = CARTESIAN_POINT('Ctrl Pts',(50.11831824308,247.217287162085,31.7413203435596)) ;
#79538 = CARTESIAN_POINT('Ctrl Pts',(50.1138614227384,247.220036347192,31.7413203435596)) ;
#79539 = CARTESIAN_POINT('Ctrl Pts',(50.1093880575593,247.222799440314,31.7413203435596)) ;
#79540 = CARTESIAN_POINT('Ctrl Pts',(50.1048968673761,247.225573558217,31.7413203435596)) ;
#79541 = CARTESIAN_POINT('Origin',(50.7706539553668,246.922763132459,31.7413203435596)) ;
#79542 = CARTESIAN_POINT('',(52.1403128398474,246.922763132459,31.6213203435596)) ;
#79543 = CARTESIAN_POINT('',(50.7706539553668,246.922763132459,31.6213203435596)) ;
#79544 = CARTESIAN_POINT('',(52.0203128398474,247.042763132459,31.7413203435596)) ;
#79545 = CARTESIAN_POINT('Origin',(52.1403128398474,246.922763132459,31.7413203435596)) ;
#79546 = CARTESIAN_POINT('',(50.7706539553668,247.042763132459,31.7413203435596)) ;
#79547 = CARTESIAN_POINT('Origin',(52.1403128398474,247.821753594881,31.7413203435596)) ;
#79548 = CARTESIAN_POINT('',(52.0203128398474,248.366092044717,31.7413203435596)) ;
#79549 = CARTESIAN_POINT('',(52.0203128398474,247.821753594881,31.7413203435596)) ;
#79550 = CARTESIAN_POINT('',(52.1403128398474,248.486092044717,31.6213203435596)) ;
#79551 = CARTESIAN_POINT('',(52.1403128398474,247.821753594881,31.6213203435596)) ;
#79552 = CARTESIAN_POINT('Origin',(52.1403128398474,248.486092044717,31.7413203435596)) ;
#79553 = CARTESIAN_POINT('Origin',(51.4036689174439,248.486092044717,31.7413203435596)) ;
#79554 = CARTESIAN_POINT('',(51.4036689174439,248.366092044717,31.7413203435596)) ;
#79555 = CARTESIAN_POINT('',(51.4036689174439,248.486092044717,31.6213203435596)) ;
#79556 = CARTESIAN_POINT('Ctrl Pts',(50.3237735145971,248.296324101873,31.7413203435596)) ;
#79557 = CARTESIAN_POINT('Ctrl Pts',(50.3208460868592,248.295023320436,31.7413203435596)) ;
#79558 = CARTESIAN_POINT('Ctrl Pts',(50.3179187784833,248.293719247106,31.7413203435596)) ;
#79559 = CARTESIAN_POINT('Ctrl Pts',(50.2432348124463,248.260661053439,31.7413203435597)) ;
#79560 = CARTESIAN_POINT('Ctrl Pts',(50.1823953545993,248.2316465172,31.7413203435596)) ;
#79561 = CARTESIAN_POINT('Ctrl Pts',(50.0901995406341,248.158990991578,31.7413203435596)) ;
#79562 = CARTESIAN_POINT('Ctrl Pts',(50.0496571268392,248.110309168465,31.7413203435596)) ;
#79563 = CARTESIAN_POINT('Ctrl Pts',(50.0018795748302,248.049699199696,31.7413203435596)) ;
#79564 = CARTESIAN_POINT('Ctrl Pts',(49.9998104000328,248.04708637804,31.7413203435596)) ;
#79565 = CARTESIAN_POINT('Ctrl Pts',(49.9977443179459,248.04447261808,31.7413203435596)) ;
#79566 = CARTESIAN_POINT('Ctrl Pts',(50.3237735145971,248.296324101873,31.7054164275186)) ;
#79567 = CARTESIAN_POINT('Ctrl Pts',(50.3208460868592,248.295023320436,31.7054164275186)) ;
#79568 = CARTESIAN_POINT('Ctrl Pts',(50.3179187784833,248.293719247106,31.7054164275186)) ;
#79569 = CARTESIAN_POINT('Ctrl Pts',(50.2432348124463,248.260661053439,31.7054164275186)) ;
#79570 = CARTESIAN_POINT('Ctrl Pts',(50.1823953545993,248.2316465172,31.7054164275186)) ;
#79571 = CARTESIAN_POINT('Ctrl Pts',(50.0901995406341,248.158990991578,31.7054164275186)) ;
#79572 = CARTESIAN_POINT('Ctrl Pts',(50.0496571268392,248.110309168465,31.7054164275186)) ;
#79573 = CARTESIAN_POINT('Ctrl Pts',(50.0018795748302,248.049699199696,31.7054164275186)) ;
#79574 = CARTESIAN_POINT('Ctrl Pts',(49.9998104000328,248.04708637804,31.7054164275186)) ;
#79575 = CARTESIAN_POINT('Ctrl Pts',(49.9977443179459,248.04447261808,31.7054164275186)) ;
#79576 = CARTESIAN_POINT('Ctrl Pts',(50.3115272061083,248.323884599068,31.6432843040156)) ;
#79577 = CARTESIAN_POINT('Ctrl Pts',(50.3085977460324,248.322586591314,31.6432843040155)) ;
#79578 = CARTESIAN_POINT('Ctrl Pts',(50.3056742108328,248.321276920664,31.6432843040155)) ;
#79579 = CARTESIAN_POINT('Ctrl Pts',(50.2309743184436,248.288272310817,31.6432843040156)) ;
#79580 = CARTESIAN_POINT('Ctrl Pts',(50.1673000436637,248.258157776563,31.6432843040156)) ;
#79581 = CARTESIAN_POINT('Ctrl Pts',(50.068167766932,248.180033272884,31.6432843040156)) ;
#79582 = CARTESIAN_POINT('Ctrl Pts',(50.0259496726954,248.129031375463,31.6432843040156)) ;
#79583 = CARTESIAN_POINT('Ctrl Pts',(49.9782226660684,248.06839939147,31.6432843040155)) ;
#79584 = CARTESIAN_POINT('Ctrl Pts',(49.976147980735,248.065790714156,31.6432843040156)) ;
#79585 = CARTESIAN_POINT('Ctrl Pts',(49.9740845925537,248.063174769602,31.6432843040155)) ;
#79586 = CARTESIAN_POINT('Ctrl Pts',(50.2859805890603,248.381377636101,31.6213203435597)) ;
#79587 = CARTESIAN_POINT('Ctrl Pts',(50.2830519623244,248.380078491027,31.6213203435596)) ;
#79588 = CARTESIAN_POINT('Ctrl Pts',(50.2801263647861,248.378771734628,31.6213203435596)) ;
#79589 = CARTESIAN_POINT('Ctrl Pts',(50.2054515729317,248.34572107069,31.6213203435597)) ;
#79590 = CARTESIAN_POINT('Ctrl Pts',(50.1358824073971,248.313488625072,31.6213203435596)) ;
#79591 = CARTESIAN_POINT('Ctrl Pts',(50.0221638717514,248.223877898007,31.6213203435597)) ;
#79592 = CARTESIAN_POINT('Ctrl Pts',(49.9766326160923,248.16801950669,31.6213203435597)) ;
#79593 = CARTESIAN_POINT('Ctrl Pts',(49.9288651949389,248.107414681377,31.6213203435596)) ;
#79594 = CARTESIAN_POINT('Ctrl Pts',(49.926793318698,248.104803754981,31.6213203435596)) ;
#79595 = CARTESIAN_POINT('Ctrl Pts',(49.9247288259075,248.102188706199,31.6213203435596)) ;
#79596 = CARTESIAN_POINT('Ctrl Pts',(50.2750462067483,248.405985624158,31.6213203435597)) ;
#79597 = CARTESIAN_POINT('Ctrl Pts',(50.2721187790104,248.40468484272,31.6213203435597)) ;
#79598 = CARTESIAN_POINT('Ctrl Pts',(50.2691906493995,248.403381756314,31.6213203435596)) ;
#79599 = CARTESIAN_POINT('Ctrl Pts',(50.1945362851629,248.370285173624,31.6213203435597)) ;
#79600 = CARTESIAN_POINT('Ctrl Pts',(50.1224471164977,248.337175575328,31.6213203435596)) ;
#79601 = CARTESIAN_POINT('Ctrl Pts',(50.0024661001059,248.242635671415,31.6213203435597)) ;
#79602 = CARTESIAN_POINT('Ctrl Pts',(49.9555470447246,248.184695852018,31.6213203435597)) ;
#79603 = CARTESIAN_POINT('Ctrl Pts',(49.9077381074784,248.124114785998,31.6213203435596)) ;
#79604 = CARTESIAN_POINT('Ctrl Pts',(49.9056698086987,248.121501088032,31.6213203435596)) ;
#79605 = CARTESIAN_POINT('Ctrl Pts',(49.9036037266118,248.118887328072,31.6213203435596)) ;
#79606 = CARTESIAN_POINT('',(50.0039413950685,248.052313607497,31.7413203435596)) ;
#79607 = CARTESIAN_POINT('Ctrl Pts',(50.0039408165155,248.052314063558,31.7413203435596)) ;
#79608 = CARTESIAN_POINT('Ctrl Pts',(50.0496575583587,248.110309686617,31.7413203435596)) ;
#79609 = CARTESIAN_POINT('Ctrl Pts',(50.0901997785078,248.158991179037,31.7413203435596)) ;
#79610 = CARTESIAN_POINT('Ctrl Pts',(50.1823947037638,248.231646004304,31.7413203435596)) ;
#79611 = CARTESIAN_POINT('Ctrl Pts',(50.2432331451607,248.260660258303,31.7413203435597)) ;
#79612 = CARTESIAN_POINT('Ctrl Pts',(50.3149894650065,248.292422612535,31.7413203435596)) ;
#79613 = CARTESIAN_POINT('',(49.9036037266118,248.118887328072,31.6213203435596)) ;
#79614 = CARTESIAN_POINT('Ctrl Pts',(50.2750462067483,248.405985624158,31.6213203435597)) ;
#79615 = CARTESIAN_POINT('Ctrl Pts',(50.2721187790104,248.40468484272,31.6213203435597)) ;
#79616 = CARTESIAN_POINT('Ctrl Pts',(50.2691906493995,248.403381756314,31.6213203435596)) ;
#79617 = CARTESIAN_POINT('Ctrl Pts',(50.1945362851629,248.370285173624,31.6213203435597)) ;
#79618 = CARTESIAN_POINT('Ctrl Pts',(50.1224471164977,248.337175575328,31.6213203435596)) ;
#79619 = CARTESIAN_POINT('Ctrl Pts',(50.0024661001059,248.242635671415,31.6213203435597)) ;
#79620 = CARTESIAN_POINT('Ctrl Pts',(49.9555470447246,248.184695852018,31.6213203435597)) ;
#79621 = CARTESIAN_POINT('Ctrl Pts',(49.9077381074784,248.124114785998,31.6213203435596)) ;
#79622 = CARTESIAN_POINT('Ctrl Pts',(49.9056698086987,248.121501088032,31.6213203435596)) ;
#79623 = CARTESIAN_POINT('Ctrl Pts',(49.9036037266118,248.118887328072,31.6213203435596)) ;
#79624 = CARTESIAN_POINT('Ctrl Pts',(49.9036037266118,248.118887328072,31.6213203435596)) ;
#79625 = CARTESIAN_POINT('Ctrl Pts',(49.9038474528801,248.118725615821,31.6213203435596)) ;
#79626 = CARTESIAN_POINT('Ctrl Pts',(49.9040911791549,248.118563904141,31.6213214465272)) ;
#79627 = CARTESIAN_POINT('Ctrl Pts',(49.9174965285971,248.109669521949,31.6214426327676)) ;
#79628 = CARTESIAN_POINT('Ctrl Pts',(49.9306479955595,248.100944075181,31.6247706510038)) ;
#79629 = CARTESIAN_POINT('Ctrl Pts',(49.9529368794178,248.086154166638,31.6360300282615)) ;
#79630 = CARTESIAN_POINT('Ctrl Pts',(49.9641037850844,248.078743851301,31.6439332011361)) ;
#79631 = CARTESIAN_POINT('Ctrl Pts',(49.9834573384472,248.065902717465,31.6673300848568)) ;
#79632 = CARTESIAN_POINT('Ctrl Pts',(49.9906968210535,248.061100122706,31.6803259746533)) ;
#79633 = CARTESIAN_POINT('Ctrl Pts',(49.9983952806611,248.055993282155,31.7018142049946)) ;
#79634 = CARTESIAN_POINT('Ctrl Pts',(50.0004443425674,248.054634068328,31.7095140383626)) ;
#79635 = CARTESIAN_POINT('Ctrl Pts',(50.0032181564329,248.052794101758,31.725250816951)) ;
#79636 = CARTESIAN_POINT('Ctrl Pts',(50.0039411676504,248.052314509003,31.7332778179758)) ;
#79637 = CARTESIAN_POINT('Ctrl Pts',(50.0039411676504,248.052314509003,31.7413203435596)) ;
#79638 = CARTESIAN_POINT('Ctrl Pts',(50.0087569650634,248.061070406301,31.7413203435596)) ;
#79639 = CARTESIAN_POINT('Ctrl Pts',(50.0071517479483,248.058150953433,31.7413203435596)) ;
#79640 = CARTESIAN_POINT('Ctrl Pts',(50.0055483551771,248.055229229945,31.7413203435596)) ;
#79641 = CARTESIAN_POINT('Ctrl Pts',(49.9690056264369,247.988957027741,31.7413203435597)) ;
#79642 = CARTESIAN_POINT('Ctrl Pts',(49.9400850019578,247.933416217127,31.7413203435596)) ;
#79643 = CARTESIAN_POINT('Ctrl Pts',(49.908310637077,247.825263262329,31.7413203435596)) ;
#79644 = CARTESIAN_POINT('Ctrl Pts',(49.9025264824017,247.763574370657,31.7413203435596)) ;
#79645 = CARTESIAN_POINT('Ctrl Pts',(49.8972996831157,247.688877147303,31.7413203435596)) ;
#79646 = CARTESIAN_POINT('Ctrl Pts',(49.8970639748427,247.685602333175,31.7413203435596)) ;
#79647 = CARTESIAN_POINT('Ctrl Pts',(49.8968309655685,247.682328422,31.7413203435596)) ;
#79648 = CARTESIAN_POINT('Ctrl Pts',(50.0087569650634,248.061070406301,31.7054164275186)) ;
#79649 = CARTESIAN_POINT('Ctrl Pts',(50.0071517479483,248.058150953433,31.7054164275186)) ;
#79650 = CARTESIAN_POINT('Ctrl Pts',(50.0055483551771,248.055229229945,31.7054164275186)) ;
#79651 = CARTESIAN_POINT('Ctrl Pts',(49.9690056264369,247.988957027741,31.7054164275186)) ;
#79652 = CARTESIAN_POINT('Ctrl Pts',(49.9400850019578,247.933416217127,31.7054164275186)) ;
#79653 = CARTESIAN_POINT('Ctrl Pts',(49.908310637077,247.825263262329,31.7054164275186)) ;
#79654 = CARTESIAN_POINT('Ctrl Pts',(49.9025264824017,247.763574370657,31.7054164275186)) ;
#79655 = CARTESIAN_POINT('Ctrl Pts',(49.8972996831157,247.688877147303,31.7054164275186)) ;
#79656 = CARTESIAN_POINT('Ctrl Pts',(49.8970639748427,247.685602333175,31.7054164275186)) ;
#79657 = CARTESIAN_POINT('Ctrl Pts',(49.8968309655685,247.682328422,31.7054164275186)) ;
#79658 = CARTESIAN_POINT('Ctrl Pts',(49.9823295099218,248.075601143813,31.6432842968685)) ;
#79659 = CARTESIAN_POINT('Ctrl Pts',(49.9807217753671,248.072682998912,31.6432842968685)) ;
#79660 = CARTESIAN_POINT('Ctrl Pts',(49.97912328038,248.069758521438,31.6432842968685)) ;
#79661 = CARTESIAN_POINT('Ctrl Pts',(49.9425479159984,248.003516731425,31.6432842968685)) ;
#79662 = CARTESIAN_POINT('Ctrl Pts',(49.9122630644889,247.945726734908,31.6432842968685)) ;
#79663 = CARTESIAN_POINT('Ctrl Pts',(49.8782632727103,247.829997860369,31.6432842968685)) ;
#79664 = CARTESIAN_POINT('Ctrl Pts',(49.8724029099475,247.765706746907,31.6432842968685)) ;
#79665 = CARTESIAN_POINT('Ctrl Pts',(49.867219756094,247.691018175729,31.6432842968685)) ;
#79666 = CARTESIAN_POINT('Ctrl Pts',(49.866978468971,247.687743550218,31.6432842968685)) ;
#79667 = CARTESIAN_POINT('Ctrl Pts',(49.8667482678629,247.684469453685,31.6432842968685)) ;
#79668 = CARTESIAN_POINT('Ctrl Pts',(49.9272000581419,248.105913241166,31.6213203435596)) ;
#79669 = CARTESIAN_POINT('Ctrl Pts',(49.9255933557227,248.102994560006,31.6213203435596)) ;
#79670 = CARTESIAN_POINT('Ctrl Pts',(49.9239922395177,248.100071502154,31.6213203435596)) ;
#79671 = CARTESIAN_POINT('Ctrl Pts',(49.8874505962389,248.033806555933,31.6213203435596)) ;
#79672 = CARTESIAN_POINT('Ctrl Pts',(49.854252009404,247.971446824694,31.6213203435596)) ;
#79673 = CARTESIAN_POINT('Ctrl Pts',(49.8155828998778,247.839827717225,31.6213203435596)) ;
#79674 = CARTESIAN_POINT('Ctrl Pts',(49.8096869765514,247.770175268382,31.6213203435597)) ;
#79675 = CARTESIAN_POINT('Ctrl Pts',(49.8044634272261,247.695484582515,31.6213203435596)) ;
#79676 = CARTESIAN_POINT('Ctrl Pts',(49.8042250862893,247.692209810553,31.6213203435596)) ;
#79677 = CARTESIAN_POINT('Ctrl Pts',(49.8039937338495,247.688935790016,31.6213203435596)) ;
#79678 = CARTESIAN_POINT('Ctrl Pts',(49.9036037266118,248.118887328072,31.6213203435596)) ;
#79679 = CARTESIAN_POINT('Ctrl Pts',(49.9019985094967,248.115967875204,31.6213203435596)) ;
#79680 = CARTESIAN_POINT('Ctrl Pts',(49.900394139303,248.113046614805,31.6213203435596)) ;
#79681 = CARTESIAN_POINT('Ctrl Pts',(49.8638838353781,248.046757375974,31.6213203435596)) ;
#79682 = CARTESIAN_POINT('Ctrl Pts',(49.8294268503797,247.982462018373,31.6213203435596)) ;
#79683 = CARTESIAN_POINT('Ctrl Pts',(49.7887547225882,247.844027283432,31.6213203435596)) ;
#79684 = CARTESIAN_POINT('Ctrl Pts',(49.782864074239,247.772091232065,31.6213203435597)) ;
#79685 = CARTESIAN_POINT('Ctrl Pts',(49.7776014062417,247.697396292484,31.6213203435596)) ;
#79686 = CARTESIAN_POINT('Ctrl Pts',(49.7773667482972,247.694121368174,31.6213203435596)) ;
#79687 = CARTESIAN_POINT('Ctrl Pts',(49.777133739023,247.690847456999,31.6213203435596)) ;
#79688 = CARTESIAN_POINT('Ctrl Pts',(49.8975299240168,247.692149180776,31.7413203435596)) ;
#79689 = CARTESIAN_POINT('Ctrl Pts',(49.8986150818286,247.707396257523,31.7413203435596)) ;
#79690 = CARTESIAN_POINT('Ctrl Pts',(49.8996743511139,247.7222161151,31.7413203435596)) ;
#79691 = CARTESIAN_POINT('Ctrl Pts',(49.9008630958013,247.736607865466,31.7413203435596)) ;
#79692 = CARTESIAN_POINT('Ctrl Pts',(49.9022047500129,247.75285084236,31.7413203435596)) ;
#79693 = CARTESIAN_POINT('Ctrl Pts',(49.9037110345681,247.768548580157,31.7413203435596)) ;
#79694 = CARTESIAN_POINT('Ctrl Pts',(49.9055395786114,247.783719168488,31.7413203435596)) ;
#79695 = CARTESIAN_POINT('Ctrl Pts',(49.907561373165,247.800493067359,31.7413203435596)) ;
#79696 = CARTESIAN_POINT('Ctrl Pts',(49.9099760964081,247.816622813088,31.7413203435596)) ;
#79697 = CARTESIAN_POINT('Ctrl Pts',(49.9129324761923,247.832151816603,31.7413203435596)) ;
#79698 = CARTESIAN_POINT('Ctrl Pts',(49.9160302485486,247.848423514193,31.7413203435596)) ;
#79699 = CARTESIAN_POINT('Ctrl Pts',(49.9197208568293,247.864036184029,31.7413203435596)) ;
#79700 = CARTESIAN_POINT('Ctrl Pts',(49.9241326690729,247.879052359467,31.7413203435596)) ;
#79701 = CARTESIAN_POINT('Ctrl Pts',(49.9246589347965,247.880843573145,31.7413203435596)) ;
#79702 = CARTESIAN_POINT('Ctrl Pts',(49.9251983743351,247.882636314972,31.7413203435596)) ;
#79703 = CARTESIAN_POINT('Ctrl Pts',(49.9257508799616,247.884430785863,31.7413203435596)) ;
#79704 = CARTESIAN_POINT('Ctrl Pts',(49.9305613985087,247.900054763414,31.7413203435596)) ;
#79705 = CARTESIAN_POINT('Ctrl Pts',(49.9363650702522,247.915808958345,31.7413203435596)) ;
#79706 = CARTESIAN_POINT('Ctrl Pts',(49.9430749294362,247.931828632111,31.7413203435596)) ;
#79707 = CARTESIAN_POINT('Ctrl Pts',(49.9489705758089,247.945904386748,31.7413203435596)) ;
#79708 = CARTESIAN_POINT('Ctrl Pts',(49.955566837351,247.960184802822,31.7413203435596)) ;
#79709 = CARTESIAN_POINT('Ctrl Pts',(49.9627697116877,247.974771949686,31.7413203435596)) ;
#79710 = CARTESIAN_POINT('Ctrl Pts',(49.9690514229702,247.987493571743,31.7413203435597)) ;
#79711 = CARTESIAN_POINT('Ctrl Pts',(49.9757948143974,248.000448397417,31.7413203435597)) ;
#79712 = CARTESIAN_POINT('Ctrl Pts',(49.9829015268903,248.013714738828,31.7413203435596)) ;
#79713 = CARTESIAN_POINT('Ctrl Pts',(49.9896302636225,248.026275500058,31.7413203435596)) ;
#79714 = CARTESIAN_POINT('Ctrl Pts',(49.9966853053433,248.039115344112,31.7413203435596)) ;
#79715 = CARTESIAN_POINT('Ctrl Pts',(50.003941798311,248.05231292904,31.7413203435596)) ;
#79716 = CARTESIAN_POINT('Ctrl Pts',(49.9036037266118,248.118887328072,31.6213203435596)) ;
#79717 = CARTESIAN_POINT('Ctrl Pts',(49.9019985094967,248.115967875204,31.6213203435596)) ;
#79718 = CARTESIAN_POINT('Ctrl Pts',(49.900394139303,248.113046614805,31.6213203435596)) ;
#79719 = CARTESIAN_POINT('Ctrl Pts',(49.8638838353781,248.046757375974,31.6213203435596)) ;
#79720 = CARTESIAN_POINT('Ctrl Pts',(49.8294268503797,247.982462018373,31.6213203435596)) ;
#79721 = CARTESIAN_POINT('Ctrl Pts',(49.7887547225882,247.844027283432,31.6213203435596)) ;
#79722 = CARTESIAN_POINT('Ctrl Pts',(49.782864074239,247.772091232065,31.6213203435597)) ;
#79723 = CARTESIAN_POINT('Ctrl Pts',(49.7776014062417,247.697396292484,31.6213203435596)) ;
#79724 = CARTESIAN_POINT('Ctrl Pts',(49.7773667482972,247.694121368174,31.6213203435596)) ;
#79725 = CARTESIAN_POINT('Ctrl Pts',(49.777133739023,247.690847456999,31.6213203435596)) ;
#79726 = CARTESIAN_POINT('Origin',(50.7542829156931,247.042763132459,31.9213203435596)) ;
#79727 = CARTESIAN_POINT('',(52.0203128398474,247.042763132459,31.8013203435596)) ;
#79728 = CARTESIAN_POINT('',(52.0203128398474,247.042763132459,31.9213203435596)) ;
#79729 = CARTESIAN_POINT('',(50.7542829156931,247.042763132459,31.8013203435596)) ;
#79730 = CARTESIAN_POINT('',(52.2271414578465,247.042763132459,31.8013203435596)) ;
#79731 = CARTESIAN_POINT('',(50.7542829156931,247.042763132459,31.9213203435596)) ;
#79732 = CARTESIAN_POINT('Origin',(52.0203128398474,247.042763132459,31.9213203435596)) ;
#79733 = CARTESIAN_POINT('',(52.0203128398474,248.366092044717,31.8013203435596)) ;
#79734 = CARTESIAN_POINT('',(52.0203128398474,248.366092044717,31.9213203435596)) ;
#79735 = CARTESIAN_POINT('',(52.0203128398474,243.213135158824,31.8013203435596)) ;
#79736 = CARTESIAN_POINT('Origin',(52.0203128398474,248.366092044717,31.9213203435596)) ;
#79737 = CARTESIAN_POINT('',(50.8825230539854,248.366092044717,31.8013203435596)) ;
#79738 = CARTESIAN_POINT('',(50.8825230539854,248.366092044717,31.9213203435596)) ;
#79739 = CARTESIAN_POINT('',(52.8601564199237,248.366092044717,31.8013203435596)) ;
#79740 = CARTESIAN_POINT('Ctrl Pts',(50.8825230539854,248.366092044717,31.9213203435596)) ;
#79741 = CARTESIAN_POINT('Ctrl Pts',(50.8825230539854,248.366092044717,31.5613203435596)) ;
#79742 = CARTESIAN_POINT('Ctrl Pts',(50.7740455687365,248.364939378322,31.9213203435596)) ;
#79743 = CARTESIAN_POINT('Ctrl Pts',(50.7740455687365,248.364939378322,31.5613203435596)) ;
#79744 = CARTESIAN_POINT('Ctrl Pts',(50.5817028363738,248.362895571688,31.9213203435596)) ;
#79745 = CARTESIAN_POINT('Ctrl Pts',(50.5817028363738,248.362895571688,31.5613203435596)) ;
#79746 = CARTESIAN_POINT('Ctrl Pts',(50.3959737706177,248.313820081291,31.9213203435596)) ;
#79747 = CARTESIAN_POINT('Ctrl Pts',(50.3959737706177,248.313820081291,31.5613203435596)) ;
#79748 = CARTESIAN_POINT('Ctrl Pts',(50.3149922133501,248.292422193891,31.9213203435596)) ;
#79749 = CARTESIAN_POINT('Ctrl Pts',(50.3149922133501,248.292422193891,31.5613203435596)) ;
#79750 = CARTESIAN_POINT('',(50.3149922133501,248.292422193891,31.8013203435596)) ;
#79751 = CARTESIAN_POINT('',(50.3149922133501,248.292422193891,31.9213203435596)) ;
#79752 = CARTESIAN_POINT('Ctrl Pts',(50.8825230530914,248.366092044866,31.8013203435596)) ;
#79753 = CARTESIAN_POINT('Ctrl Pts',(50.780063617307,248.365003768851,31.8013203435596)) ;
#79754 = CARTESIAN_POINT('Ctrl Pts',(50.6723937595897,248.364790853518,31.8013203435596)) ;
#79755 = CARTESIAN_POINT('Ctrl Pts',(50.471719498392,248.334437936584,31.8013203435596)) ;
#79756 = CARTESIAN_POINT('Ctrl Pts',(50.3915513141507,248.312651528491,31.8013203435596)) ;
#79757 = CARTESIAN_POINT('Ctrl Pts',(50.31499221335,248.292422193891,31.8013203435596)) ;
#79758 = CARTESIAN_POINT('Origin',(50.7870249950405,248.600744057303,31.6213203435596)) ;
#79759 = CARTESIAN_POINT('',(51.4064264123735,248.704482161408,31.6213203435596)) ;
#79760 = CARTESIAN_POINT('',(52.1403128398474,248.704482161408,31.6213203435596)) ;
#79761 = CARTESIAN_POINT('',(51.0967112553384,248.704482161408,31.6213203435596)) ;
#79762 = CARTESIAN_POINT('',(51.086156364446,248.725988135576,31.6213203435596)) ;
#79763 = CARTESIAN_POINT('Ctrl Pts',(51.086156364446,248.725988135576,31.6213203435596)) ;
#79764 = CARTESIAN_POINT('Ctrl Pts',(51.0891401619064,248.72557110151,31.6213203435596)) ;
#79765 = CARTESIAN_POINT('Ctrl Pts',(51.0921240529548,248.725154332015,31.6213203435596)) ;
#79766 = CARTESIAN_POINT('Ctrl Pts',(51.1368100661075,248.718902921604,31.6213203435596)) ;
#79767 = CARTESIAN_POINT('Ctrl Pts',(51.1785415671225,248.713138013086,31.6213203435596)) ;
#79768 = CARTESIAN_POINT('Ctrl Pts',(51.2823351634085,248.704548527333,31.6213203435596)) ;
#79769 = CARTESIAN_POINT('Ctrl Pts',(51.3444132215067,248.704452338598,31.6213203435597)) ;
#79770 = CARTESIAN_POINT('Ctrl Pts',(51.4064264123667,248.70448216142,31.6213203435597)) ;
#79771 = CARTESIAN_POINT('',(50.803890188879,248.850701676295,31.6213203435596)) ;
#79772 = CARTESIAN_POINT('Ctrl Pts',(50.803890188879,248.850701676295,31.6213203435596)) ;
#79773 = CARTESIAN_POINT('Ctrl Pts',(50.8057995745649,248.849549687667,31.6213203435596)) ;
#79774 = CARTESIAN_POINT('Ctrl Pts',(50.807709533127,248.848398088001,31.6213203435596)) ;
#79775 = CARTESIAN_POINT('Ctrl Pts',(50.8526791620758,248.821240949726,31.6213203435597)) ;
#79776 = CARTESIAN_POINT('Ctrl Pts',(50.8960447320484,248.795457119086,31.6213203435597)) ;
#79777 = CARTESIAN_POINT('Ctrl Pts',(50.9859328579063,248.756098193207,31.6213203435597)) ;
#79778 = CARTESIAN_POINT('Ctrl Pts',(51.0317272198324,248.742164050894,31.6213203435597)) ;
#79779 = CARTESIAN_POINT('Ctrl Pts',(51.0803807937155,248.727707582416,31.6213203435597)) ;
#79780 = CARTESIAN_POINT('Ctrl Pts',(51.0832686016586,248.726847429988,31.6213203435597)) ;
#79781 = CARTESIAN_POINT('Ctrl Pts',(51.086156364446,248.725988135576,31.6213203435597)) ;
#79782 = CARTESIAN_POINT('',(50.5065284460866,249.143989702353,31.6213203435597)) ;
#79783 = CARTESIAN_POINT('Ctrl Pts',(50.5065286369161,249.143989458401,31.6213203435597)) ;
#79784 = CARTESIAN_POINT('Ctrl Pts',(50.5069608349978,249.14344985097,31.6213203435597)) ;
#79785 = CARTESIAN_POINT('Ctrl Pts',(50.5073932243977,249.142910226211,31.6213203435597)) ;
#79786 = CARTESIAN_POINT('Ctrl Pts',(50.556272300514,249.081846646474,31.62132034356)) ;
#79787 = CARTESIAN_POINT('Ctrl Pts',(50.6051720569295,249.021342538492,31.6213203435597)) ;
#79788 = CARTESIAN_POINT('Ctrl Pts',(50.7045314789452,248.927144579668,31.6213203435597)) ;
#79789 = CARTESIAN_POINT('Ctrl Pts',(50.7515320882953,248.890838723369,31.6213203435597)) ;
#79790 = CARTESIAN_POINT('Ctrl Pts',(50.8003512733757,248.853416193082,31.6213203435596)) ;
#79791 = CARTESIAN_POINT('Ctrl Pts',(50.8021206938697,248.852058742774,31.6213203435597)) ;
#79792 = CARTESIAN_POINT('Ctrl Pts',(50.803890188879,248.850701676295,31.6213203435597)) ;
#79793 = CARTESIAN_POINT('',(50.1184962383157,249.703743076409,31.6213203435596)) ;
#79794 = CARTESIAN_POINT('Ctrl Pts',(50.1184962401253,249.703743073639,31.6213203435596)) ;
#79795 = CARTESIAN_POINT('Ctrl Pts',(50.1885559277244,249.595500406139,31.6213203435596)) ;
#79796 = CARTESIAN_POINT('Ctrl Pts',(50.2586477088752,249.487244711046,31.6213203435595)) ;
#79797 = CARTESIAN_POINT('Ctrl Pts',(50.3887608735185,249.301944161957,31.6213203435596)) ;
#79798 = CARTESIAN_POINT('Ctrl Pts',(50.4470208542166,249.223788058288,31.6213203435592)) ;
#79799 = CARTESIAN_POINT('Ctrl Pts',(50.5057014968488,249.145098643882,31.6213203435596)) ;
#79800 = CARTESIAN_POINT('Ctrl Pts',(50.5061149650076,249.144544163959,31.6213203435596)) ;
#79801 = CARTESIAN_POINT('Ctrl Pts',(50.5065284346353,249.143989693814,31.6213203435596)) ;
#79802 = CARTESIAN_POINT('',(49.6242728881931,250.480744087106,31.6213203435596)) ;
#79803 = CARTESIAN_POINT('',(50.1997327628534,249.576025797013,31.6213203435596)) ;
#79804 = CARTESIAN_POINT('',(49.2435109302601,250.480744087106,31.6213203435596)) ;
#79805 = CARTESIAN_POINT('',(49.9057153088118,250.480744087106,31.6213203435596)) ;
#79806 = CARTESIAN_POINT('',(49.8203579156189,249.578148362944,31.6213203435596)) ;
#79807 = CARTESIAN_POINT('',(50.182743804609,249.011121144029,31.6213203435596)) ;
#79808 = CARTESIAN_POINT('',(50.2391705625565,249.070003642667,31.6213203435604)) ;
#79809 = CARTESIAN_POINT('Ctrl Pts',(50.2391707426563,249.070004176103,31.6213203435596)) ;
#79810 = CARTESIAN_POINT('Ctrl Pts',(50.1657687234013,249.143332160444,31.6213203435596)) ;
#79811 = CARTESIAN_POINT('Ctrl Pts',(50.0923185561359,249.216754385207,31.6213203435596)) ;
#79812 = CARTESIAN_POINT('Ctrl Pts',(49.9511520237043,249.385651900106,31.6213203435596)) ;
#79813 = CARTESIAN_POINT('Ctrl Pts',(49.885777159574,249.482014947007,31.6213203435596)) ;
#79814 = CARTESIAN_POINT('Ctrl Pts',(49.8203580221144,249.578148200324,31.6213203435596)) ;
#79815 = CARTESIAN_POINT('',(50.8634509060979,248.724567452152,31.6213203435596)) ;
#79816 = CARTESIAN_POINT('Ctrl Pts',(50.8634509060979,248.724567452152,31.6213203435597)) ;
#79817 = CARTESIAN_POINT('Ctrl Pts',(50.752878376055,248.779202490392,31.6213203435597)) ;
#79818 = CARTESIAN_POINT('Ctrl Pts',(50.6422811339546,248.833795616323,31.6213203435596)) ;
#79819 = CARTESIAN_POINT('Ctrl Pts',(50.4731253324676,248.917460196317,31.6213203435596)) ;
#79820 = CARTESIAN_POINT('Ctrl Pts',(50.4140730966128,248.946294536072,31.6213203435596)) ;
#79821 = CARTESIAN_POINT('Ctrl Pts',(50.3173047320902,249.008815217813,31.6213203435596)) ;
#79822 = CARTESIAN_POINT('Ctrl Pts',(50.2782046295083,249.039403431305,31.6213203435596)) ;
#79823 = CARTESIAN_POINT('Ctrl Pts',(50.239170406004,249.070003442965,31.6213203435596)) ;
#79824 = CARTESIAN_POINT('',(49.7134657448932,248.324869300773,31.6213203435596)) ;
#79825 = CARTESIAN_POINT('Ctrl Pts',(49.7134669918129,248.324871302986,31.6213203435596)) ;
#79826 = CARTESIAN_POINT('Ctrl Pts',(49.8135354254198,248.404517214071,31.6213203435596)) ;
#79827 = CARTESIAN_POINT('Ctrl Pts',(49.9140472672828,248.485001685424,31.6213203435596)) ;
#79828 = CARTESIAN_POINT('Ctrl Pts',(50.1766164005556,248.610148341557,31.6213203435597)) ;
#79829 = CARTESIAN_POINT('Ctrl Pts',(50.339328262466,248.63513713406,31.6213203435596)) ;
#79830 = CARTESIAN_POINT('Ctrl Pts',(50.6193644682054,248.68318651908,31.6213203435596)) ;
#79831 = CARTESIAN_POINT('Ctrl Pts',(50.7413810446874,248.703796823408,31.6213203435596)) ;
#79832 = CARTESIAN_POINT('Ctrl Pts',(50.863450906098,248.724567452152,31.6213203435596)) ;
#79833 = CARTESIAN_POINT('',(49.4721211893692,247.691149925186,31.6213203435611)) ;
#79834 = CARTESIAN_POINT('Ctrl Pts',(49.472122022277,247.691150967144,31.6213203435596)) ;
#79835 = CARTESIAN_POINT('Ctrl Pts',(49.4776322982804,247.761009018444,31.6213203435596)) ;
#79836 = CARTESIAN_POINT('Ctrl Pts',(49.4868918774019,247.879515131177,31.6213203435596)) ;
#79837 = CARTESIAN_POINT('Ctrl Pts',(49.5146718619417,247.995378904774,31.6213203435596)) ;
#79838 = CARTESIAN_POINT('Ctrl Pts',(49.549547538703,248.084463228595,31.6213203435596)) ;
#79839 = CARTESIAN_POINT('Ctrl Pts',(49.6044221987356,248.183416394021,31.6213203435596)) ;
#79840 = CARTESIAN_POINT('Ctrl Pts',(49.6732807190579,248.272880146134,31.6213203435596)) ;
#79841 = CARTESIAN_POINT('Ctrl Pts',(49.7134670322841,248.324868305633,31.6213203435596)) ;
#79842 = CARTESIAN_POINT('',(49.6210141597778,247.151691936914,31.6213203435596)) ;
#79843 = CARTESIAN_POINT('Ctrl Pts',(49.6210131682005,247.151692804282,31.6213203435596)) ;
#79844 = CARTESIAN_POINT('Ctrl Pts',(49.5779432602701,247.234817978226,31.6213203435596)) ;
#79845 = CARTESIAN_POINT('Ctrl Pts',(49.5342097952782,247.318188901882,31.6213203435596)) ;
#79846 = CARTESIAN_POINT('Ctrl Pts',(49.4834370857315,247.500442371379,31.6213203435596)) ;
#79847 = CARTESIAN_POINT('Ctrl Pts',(49.478005366162,247.596089312949,31.6213203435596)) ;
#79848 = CARTESIAN_POINT('Ctrl Pts',(49.4721207423776,247.691149897516,31.6213203435596)) ;
#79849 = CARTESIAN_POINT('',(50.0058124410862,246.822526614227,31.6213203435597)) ;
#79850 = CARTESIAN_POINT('Ctrl Pts',(50.005809812189,246.822528105688,31.6213203435597)) ;
#79851 = CARTESIAN_POINT('Ctrl Pts',(49.9776833689163,246.836265985231,31.6213203435597)) ;
#79852 = CARTESIAN_POINT('Ctrl Pts',(49.9026192503807,246.873207876842,31.6213203435597)) ;
#79853 = CARTESIAN_POINT('Ctrl Pts',(49.8301799972564,246.915958463683,31.6213203435596)) ;
#79854 = CARTESIAN_POINT('Ctrl Pts',(49.7621487599861,246.973100389465,31.6213203435596)) ;
#79855 = CARTESIAN_POINT('Ctrl Pts',(49.701845797924,247.037610514595,31.6213203435597)) ;
#79856 = CARTESIAN_POINT('Ctrl Pts',(49.6508881669957,247.109484107848,31.6213203435596)) ;
#79857 = CARTESIAN_POINT('Ctrl Pts',(49.6210149532587,247.151692498505,31.6213203435596)) ;
#79858 = CARTESIAN_POINT('',(50.7765817870421,246.720744026659,31.6213203435596)) ;
#79859 = CARTESIAN_POINT('Ctrl Pts',(50.7765817856215,246.720744025627,31.6213203435596)) ;
#79860 = CARTESIAN_POINT('Ctrl Pts',(50.625471196441,246.721928462813,31.6213203435596)) ;
#79861 = CARTESIAN_POINT('Ctrl Pts',(50.4737979877614,246.722566749351,31.6213203435597)) ;
#79862 = CARTESIAN_POINT('Ctrl Pts',(50.2164851948485,246.763827191512,31.6213203435597)) ;
#79863 = CARTESIAN_POINT('Ctrl Pts',(50.1110650243439,246.793152996729,31.6213203435597)) ;
#79864 = CARTESIAN_POINT('Ctrl Pts',(50.005812342985,246.822526262703,31.6213203435597)) ;
#79865 = CARTESIAN_POINT('',(52.4296443674977,246.720744027501,31.6213203435596)) ;
#79866 = CARTESIAN_POINT('',(51.6683346812691,246.720744027501,31.6213203435596)) ;
#79867 = CARTESIAN_POINT('',(52.4296443674977,250.480744087106,31.6213203435596)) ;
#79868 = CARTESIAN_POINT('',(52.4296443674977,249.600744072205,31.6213203435596)) ;
#79869 = CARTESIAN_POINT('',(52.1403128398474,250.480744087106,31.6213203435596)) ;
#79870 = CARTESIAN_POINT('',(51.4036689174439,250.480744087106,31.6213203435596)) ;
#79871 = CARTESIAN_POINT('',(52.1403128398474,248.712613109356,31.6213203435596)) ;
#79872 = CARTESIAN_POINT('Origin',(50.182743804609,249.011121144029,31.7413203435596)) ;
#79873 = CARTESIAN_POINT('',(49.0244056225832,250.600744087106,31.7413203435596)) ;
#79874 = CARTESIAN_POINT('Origin',(49.2435109302601,250.480744087106,31.7413203435596)) ;
#79875 = CARTESIAN_POINT('',(49.7201766015108,249.512067336446,31.7413203435596)) ;
#79876 = CARTESIAN_POINT('',(50.0816298410385,248.946499426541,31.7413203435596)) ;
#79877 = CARTESIAN_POINT('Ctrl Pts',(49.8203578030133,249.578148522292,31.6213203435596)) ;
#79878 = CARTESIAN_POINT('Ctrl Pts',(49.8201143316048,249.57798792436,31.6213203435596)) ;
#79879 = CARTESIAN_POINT('Ctrl Pts',(49.8198708575707,249.57782732467,31.6213214476887)) ;
#79880 = CARTESIAN_POINT('Ctrl Pts',(49.8120344278958,249.572658275908,31.6213924401153)) ;
#79881 = CARTESIAN_POINT('Ctrl Pts',(49.804486837198,249.567679673608,31.6225275324167)) ;
#79882 = CARTESIAN_POINT('Ctrl Pts',(49.791651457411,249.559212971364,31.6262185924614)) ;
#79883 = CARTESIAN_POINT('Ctrl Pts',(49.786279037641,249.555669070629,31.6283381657329)) ;
#79884 = CARTESIAN_POINT('Ctrl Pts',(49.7740832540178,249.547624217164,31.6345403110037)) ;
#79885 = CARTESIAN_POINT('Ctrl Pts',(49.767470915909,249.54326245926,31.6390055724476)) ;
#79886 = CARTESIAN_POINT('Ctrl Pts',(49.7601937918778,249.538462793976,31.6453557245753)) ;
#79887 = CARTESIAN_POINT('Ctrl Pts',(49.7590266040823,249.537692991468,31.646424002123)) ;
#79888 = CARTESIAN_POINT('Ctrl Pts',(49.7547988343126,249.534904730099,31.6504832283805)) ;
#79889 = CARTESIAN_POINT('Ctrl Pts',(49.7518693497122,249.532972909003,31.6536742656277)) ;
#79890 = CARTESIAN_POINT('Ctrl Pts',(49.7437891211446,249.527644641772,31.663605970272)) ;
#79891 = CARTESIAN_POINT('Ctrl Pts',(49.7391293356128,249.524572046805,31.6708380022079)) ;
#79892 = CARTESIAN_POINT('Ctrl Pts',(49.7323690685834,249.520113636147,31.6841034424277)) ;
#79893 = CARTESIAN_POINT('Ctrl Pts',(49.7299190041598,249.518497551385,31.6898732056734)) ;
#79894 = CARTESIAN_POINT('Ctrl Pts',(49.7249579883231,249.515224496342,31.7042366795402)) ;
#79895 = CARTESIAN_POINT('Ctrl Pts',(49.7228443575224,249.513829279031,31.712944490313)) ;
#79896 = CARTESIAN_POINT('Ctrl Pts',(49.720654622348,249.512383268816,31.7282514461642)) ;
#79897 = CARTESIAN_POINT('Ctrl Pts',(49.7201766015108,249.512067336446,31.7347662286955)) ;
#79898 = CARTESIAN_POINT('Ctrl Pts',(49.7201766015108,249.512067336446,31.7413203435596)) ;
#79899 = CARTESIAN_POINT('Origin',(49.9057153088118,250.480744087106,31.7413203435596)) ;
#79900 = CARTESIAN_POINT('',(49.6901629806574,250.600744087106,31.7413203435596)) ;
#79901 = CARTESIAN_POINT('Origin',(49.6242728881931,250.480744087106,31.7413203435596)) ;
#79902 = CARTESIAN_POINT('',(49.9057153088118,250.600744087106,31.7413203435596)) ;
#79903 = CARTESIAN_POINT('Origin',(50.1997327628534,249.576025797013,31.7413203435596)) ;
#79904 = CARTESIAN_POINT('',(50.2194942457775,249.76854761595,31.7413203435596)) ;
#79905 = CARTESIAN_POINT('Ctrl Pts',(50.1184962360783,249.703743079888,31.6213203435596)) ;
#79906 = CARTESIAN_POINT('Ctrl Pts',(50.1187416948551,249.703900576469,31.6213203435596)) ;
#79907 = CARTESIAN_POINT('Ctrl Pts',(50.1189871559203,249.704058075343,31.6213214476896)) ;
#79908 = CARTESIAN_POINT('Ctrl Pts',(50.1268875814148,249.709127312317,31.6213924404081)) ;
#79909 = CARTESIAN_POINT('Ctrl Pts',(50.134496779585,249.714009714011,31.6225275410102)) ;
#79910 = CARTESIAN_POINT('Ctrl Pts',(50.1474348105249,249.722311369703,31.6262179993372)) ;
#79911 = CARTESIAN_POINT('Ctrl Pts',(50.1528490540415,249.725785419901,31.6283365564217)) ;
#79912 = CARTESIAN_POINT('Ctrl Pts',(50.1651429552605,249.733673783677,31.634536887502)) ;
#79913 = CARTESIAN_POINT('Ctrl Pts',(50.1718096792711,249.73795147265,31.6390018254195)) ;
#79914 = CARTESIAN_POINT('Ctrl Pts',(50.1791479853649,249.742659914759,31.6453529319083)) ;
#79915 = CARTESIAN_POINT('Ctrl Pts',(50.1803262224953,249.743415895318,31.6464225668027)) ;
#79916 = CARTESIAN_POINT('Ctrl Pts',(50.1845881438841,249.746150400814,31.6504816500711)) ;
#79917 = CARTESIAN_POINT('Ctrl Pts',(50.1875398130984,249.748044174978,31.6536708439172)) ;
#79918 = CARTESIAN_POINT('Ctrl Pts',(50.195684363488,249.753269627988,31.6636000631244)) ;
#79919 = CARTESIAN_POINT('Ctrl Pts',(50.2003820835136,249.756283589114,31.6708316856961)) ;
#79920 = CARTESIAN_POINT('Ctrl Pts',(50.2071983400128,249.760656974874,31.684097470937)) ;
#79921 = CARTESIAN_POINT('Ctrl Pts',(50.2096690460319,249.762242278695,31.689868116927)) ;
#79922 = CARTESIAN_POINT('Ctrl Pts',(50.2146716460624,249.765452344316,31.7042327086333)) ;
#79923 = CARTESIAN_POINT('Ctrl Pts',(50.2168031754755,249.766820304159,31.7129407270407)) ;
#79924 = CARTESIAN_POINT('Ctrl Pts',(50.219011933072,249.768237978459,31.7282490558558)) ;
#79925 = CARTESIAN_POINT('Ctrl Pts',(50.2194942440176,249.76854761887,31.7347650345167)) ;
#79926 = CARTESIAN_POINT('Ctrl Pts',(50.2194942440175,249.76854761887,31.7413203435596)) ;
#79927 = CARTESIAN_POINT('',(50.3009858231264,249.640429351149,31.7413203435596)) ;
#79928 = CARTESIAN_POINT('Ctrl Pts',(50.2192360308921,249.768946559407,31.7413203435596)) ;
#79929 = CARTESIAN_POINT('Ctrl Pts',(50.2892957198384,249.660703889824,31.7413203435596)) ;
#79930 = CARTESIAN_POINT('Ctrl Pts',(50.3585729066663,249.55375538464,31.7413203435595)) ;
#79931 = CARTESIAN_POINT('Ctrl Pts',(50.4856696244485,249.372752864996,31.7413203435596)) ;
#79932 = CARTESIAN_POINT('Ctrl Pts',(50.543217787302,249.295522367444,31.7413203435593)) ;
#79933 = CARTESIAN_POINT('Ctrl Pts',(50.6018996488782,249.216833692745,31.7413203435597)) ;
#79934 = CARTESIAN_POINT('Ctrl Pts',(50.6023131730112,249.216279125981,31.7413203435596)) ;
#79935 = CARTESIAN_POINT('Ctrl Pts',(50.6027267043398,249.215724573099,31.7413203435596)) ;
#79936 = CARTESIAN_POINT('Ctrl Pts',(50.2192360308921,249.768946559407,31.7054164275186)) ;
#79937 = CARTESIAN_POINT('Ctrl Pts',(50.2892957198384,249.660703889824,31.7054164275186)) ;
#79938 = CARTESIAN_POINT('Ctrl Pts',(50.3585729066663,249.55375538464,31.7054164275185)) ;
#79939 = CARTESIAN_POINT('Ctrl Pts',(50.4856696244485,249.372752864996,31.7054164275186)) ;
#79940 = CARTESIAN_POINT('Ctrl Pts',(50.543217787302,249.295522367444,31.7054164275182)) ;
#79941 = CARTESIAN_POINT('Ctrl Pts',(50.6018996488782,249.216833692745,31.7054164275186)) ;
#79942 = CARTESIAN_POINT('Ctrl Pts',(50.6023131730112,249.216279125981,31.7054164275186)) ;
#79943 = CARTESIAN_POINT('Ctrl Pts',(50.6027267043398,249.215724573099,31.7054164275186)) ;
#79944 = CARTESIAN_POINT('Ctrl Pts',(50.1939177594495,249.752559396851,31.6432843216851)) ;
#79945 = CARTESIAN_POINT('Ctrl Pts',(50.2639758267822,249.644313855627,31.6432843216851)) ;
#79946 = CARTESIAN_POINT('Ctrl Pts',(50.3334588863795,249.537039133955,31.643284321685)) ;
#79947 = CARTESIAN_POINT('Ctrl Pts',(50.4613142664604,249.354956858061,31.6432843216851)) ;
#79948 = CARTESIAN_POINT('Ctrl Pts',(50.5190399474795,249.277492812335,31.6432843216847)) ;
#79949 = CARTESIAN_POINT('Ctrl Pts',(50.5777228825355,249.198805024834,31.6432843216851)) ;
#79950 = CARTESIAN_POINT('Ctrl Pts',(50.5781362671757,249.198250352243,31.6432843216851)) ;
#79951 = CARTESIAN_POINT('Ctrl Pts',(50.5785498711154,249.197695854323,31.6432843216851)) ;
#79952 = CARTESIAN_POINT('Ctrl Pts',(50.1411021931731,249.718374706478,31.6213203435596)) ;
#79953 = CARTESIAN_POINT('Ctrl Pts',(50.2111609256163,249.610130343067,31.6213203435596)) ;
#79954 = CARTESIAN_POINT('Ctrl Pts',(50.2810705890642,249.502169342483,31.6213203435595)) ;
#79955 = CARTESIAN_POINT('Ctrl Pts',(50.4105071949428,249.31783352678,31.6213203435596)) ;
#79956 = CARTESIAN_POINT('Ctrl Pts',(50.4686066310802,249.239884584998,31.6213203435592)) ;
#79957 = CARTESIAN_POINT('Ctrl Pts',(50.5272883998386,249.161195917641,31.6213203435596)) ;
#79958 = CARTESIAN_POINT('Ctrl Pts',(50.5277018452843,249.160641291024,31.6213203435596)) ;
#79959 = CARTESIAN_POINT('Ctrl Pts',(50.5281154194423,249.160086770561,31.6213203435596)) ;
#79960 = CARTESIAN_POINT('Ctrl Pts',(50.1184962360798,249.703743079889,31.6213203435596)) ;
#79961 = CARTESIAN_POINT('Ctrl Pts',(50.1885559250262,249.595500410306,31.6213203435596)) ;
#79962 = CARTESIAN_POINT('Ctrl Pts',(50.258647707449,249.487244713078,31.6213203435595)) ;
#79963 = CARTESIAN_POINT('Ctrl Pts',(50.3887608735185,249.301944161957,31.6213203435596)) ;
#79964 = CARTESIAN_POINT('Ctrl Pts',(50.4470208542166,249.223788058288,31.6213203435592)) ;
#79965 = CARTESIAN_POINT('Ctrl Pts',(50.5057015585495,249.145098561143,31.6213203435596)) ;
#79966 = CARTESIAN_POINT('Ctrl Pts',(50.506115088408,249.144543998473,31.6213203435596)) ;
#79967 = CARTESIAN_POINT('Ctrl Pts',(50.5065286197366,249.14398944559,31.6213203435596)) ;
#79968 = CARTESIAN_POINT('',(50.6014860873806,249.217388210622,31.7413203435596)) ;
#79969 = CARTESIAN_POINT('Ctrl Pts',(50.5065282662,249.143989955527,31.6213203435597)) ;
#79970 = CARTESIAN_POINT('Ctrl Pts',(50.5067587814614,249.144168655837,31.6213203436138)) ;
#79971 = CARTESIAN_POINT('Ctrl Pts',(50.5069898102017,249.144346708618,31.6213214476891)) ;
#79972 = CARTESIAN_POINT('Ctrl Pts',(50.507220589837,249.144525091037,31.6213236533711)) ;
#79973 = CARTESIAN_POINT('Ctrl Pts',(50.5144175329847,249.150088008785,31.6213924383321)) ;
#79974 = CARTESIAN_POINT('Ctrl Pts',(50.5215715307724,249.155617632913,31.6225274810686)) ;
#79975 = CARTESIAN_POINT('Ctrl Pts',(50.5285466406673,249.161008894249,31.6246435392332)) ;
#79976 = CARTESIAN_POINT('Ctrl Pts',(50.5337389459037,249.165022175028,31.6262187430729)) ;
#79977 = CARTESIAN_POINT('Ctrl Pts',(50.5388325053053,249.168959069177,31.628338843696)) ;
#79978 = CARTESIAN_POINT('Ctrl Pts',(50.5437677752371,249.172773650262,31.6309868527295)) ;
#79979 = CARTESIAN_POINT('Ctrl Pts',(50.5503934802315,249.177894806612,31.634541861254)) ;
#79980 = CARTESIAN_POINT('Ctrl Pts',(50.5566609773773,249.182739119391,31.6390071822895)) ;
#79981 = CARTESIAN_POINT('Ctrl Pts',(50.5624328792937,249.187201020017,31.6443215166813)) ;
#79982 = CARTESIAN_POINT('Ctrl Pts',(50.5635573448131,249.18807027481,31.6453568401965)) ;
#79983 = CARTESIAN_POINT('Ctrl Pts',(50.5646629450614,249.188924974179,31.6464245294253)) ;
#79984 = CARTESIAN_POINT('Ctrl Pts',(50.5657485650742,249.189764263626,31.6475243300193)) ;
#79985 = CARTESIAN_POINT('Ctrl Pts',(50.5686699459928,249.192022774103,31.6504838705877)) ;
#79986 = CARTESIAN_POINT('Ctrl Pts',(50.5714468197053,249.194169827638,31.6536757758731)) ;
#79987 = CARTESIAN_POINT('Ctrl Pts',(50.5740702737092,249.196198328858,31.6570786924021)) ;
#79988 = CARTESIAN_POINT('Ctrl Pts',(50.5791044212708,249.200090821145,31.6636085511004)) ;
#79989 = CARTESIAN_POINT('Ctrl Pts',(50.5835198746397,249.203505131949,31.670840665461)) ;
#79990 = CARTESIAN_POINT('Ctrl Pts',(50.5872694481144,249.206403957949,31.6786045970734)) ;
#79991 = CARTESIAN_POINT('Ctrl Pts',(50.5899263174098,249.208458005388,31.684105956535)) ;
#79992 = CARTESIAN_POINT('Ctrl Pts',(50.5922483559534,249.210252861051,31.6898754635384)) ;
#79993 = CARTESIAN_POINT('Ctrl Pts',(50.5942080262981,249.211767237315,31.6958607981639)) ;
#79994 = CARTESIAN_POINT('Ctrl Pts',(50.5969510272122,249.213886948668,31.7042386247684)) ;
#79995 = CARTESIAN_POINT('Ctrl Pts',(50.5989553811672,249.215434921791,31.7129463762652)) ;
#79996 = CARTESIAN_POINT('Ctrl Pts',(50.6001611416934,249.216365729467,31.7218322584633)) ;
#79997 = CARTESIAN_POINT('Ctrl Pts',(50.6009919855187,249.217007113716,31.7279551827062)) ;
#79998 = CARTESIAN_POINT('Ctrl Pts',(50.601442996467,249.217354970191,31.7341633653977)) ;
#79999 = CARTESIAN_POINT('Ctrl Pts',(50.6014830955948,249.217385899284,31.7404096300915)) ;
#80000 = CARTESIAN_POINT('Ctrl Pts',(50.6014850438655,249.217387402016,31.7407131133612)) ;
#80001 = CARTESIAN_POINT('Ctrl Pts',(50.6014860200994,249.217388154977,31.7410166863487)) ;
#80002 = CARTESIAN_POINT('Ctrl Pts',(50.6014860200994,249.217388154977,31.7413203435596)) ;
#80003 = CARTESIAN_POINT('Ctrl Pts',(50.6014861078465,249.217388225182,31.7413203435596)) ;
#80004 = CARTESIAN_POINT('Ctrl Pts',(50.543217787302,249.295522367444,31.7413203435593)) ;
#80005 = CARTESIAN_POINT('Ctrl Pts',(50.4856696244485,249.372752864996,31.7413203435596)) ;
#80006 = CARTESIAN_POINT('Ctrl Pts',(50.3586618302853,249.553628745657,31.7413203435595)) ;
#80007 = CARTESIAN_POINT('Ctrl Pts',(50.2894659462689,249.660441111302,31.7413203435596)) ;
#80008 = CARTESIAN_POINT('Ctrl Pts',(50.2194942440175,249.76854761887,31.7413203435596)) ;
#80009 = CARTESIAN_POINT('Ctrl Pts',(50.6001891375754,249.219007527002,31.7413203435596)) ;
#80010 = CARTESIAN_POINT('Ctrl Pts',(50.6006214646902,249.218467758338,31.7413203435596)) ;
#80011 = CARTESIAN_POINT('Ctrl Pts',(50.6010540649099,249.217928043864,31.7413203435596)) ;
#80012 = CARTESIAN_POINT('Ctrl Pts',(50.6499195763086,249.156852387871,31.7413203435601)) ;
#80013 = CARTESIAN_POINT('Ctrl Pts',(50.695202994675,249.10133535881,31.7413203435597)) ;
#80014 = CARTESIAN_POINT('Ctrl Pts',(50.7813866081462,249.019639600231,31.7413203435597)) ;
#80015 = CARTESIAN_POINT('Ctrl Pts',(50.8245550336637,248.986049007095,31.7413203435597)) ;
#80016 = CARTESIAN_POINT('Ctrl Pts',(50.8733785425078,248.948637433444,31.7413203435596)) ;
#80017 = CARTESIAN_POINT('Ctrl Pts',(50.8751478527577,248.947279717694,31.7413203435596)) ;
#80018 = CARTESIAN_POINT('Ctrl Pts',(50.876917347767,248.945922651215,31.7413203435596)) ;
#80019 = CARTESIAN_POINT('Ctrl Pts',(50.6001891375754,249.219007527002,31.7054164275186)) ;
#80020 = CARTESIAN_POINT('Ctrl Pts',(50.6006214646902,249.218467758338,31.7054164275186)) ;
#80021 = CARTESIAN_POINT('Ctrl Pts',(50.6010540649099,249.217928043864,31.7054164275186)) ;
#80022 = CARTESIAN_POINT('Ctrl Pts',(50.6499195763086,249.156852387871,31.7054164275191)) ;
#80023 = CARTESIAN_POINT('Ctrl Pts',(50.695202994675,249.10133535881,31.7054164275187)) ;
#80024 = CARTESIAN_POINT('Ctrl Pts',(50.7813866081462,249.019639600231,31.7054164275187)) ;
#80025 = CARTESIAN_POINT('Ctrl Pts',(50.8245550336637,248.986049007095,31.7054164275187)) ;
#80026 = CARTESIAN_POINT('Ctrl Pts',(50.8733785425078,248.948637433444,31.7054164275186)) ;
#80027 = CARTESIAN_POINT('Ctrl Pts',(50.8751478527577,248.947279717694,31.7054164275186)) ;
#80028 = CARTESIAN_POINT('Ctrl Pts',(50.876917347767,248.945922651215,31.7054164275186)) ;
#80029 = CARTESIAN_POINT('Ctrl Pts',(50.5766499626794,249.200153850869,31.6432843195571)) ;
#80030 = CARTESIAN_POINT('Ctrl Pts',(50.5770818425322,249.19961354785,31.6432843195571)) ;
#80031 = CARTESIAN_POINT('Ctrl Pts',(50.5775153094751,249.199074856023,31.6432843195571)) ;
#80032 = CARTESIAN_POINT('Ctrl Pts',(50.6263655239759,249.13798899133,31.6432843195575)) ;
#80033 = CARTESIAN_POINT('Ctrl Pts',(50.6725751704915,249.081223960805,31.6432843195572)) ;
#80034 = CARTESIAN_POINT('Ctrl Pts',(50.7620696300964,248.996395824763,31.6432843195572)) ;
#80035 = CARTESIAN_POINT('Ctrl Pts',(50.8061966649443,248.962103736337,31.6432843195572)) ;
#80036 = CARTESIAN_POINT('Ctrl Pts',(50.8550255073703,248.924707064648,31.6432843195571)) ;
#80037 = CARTESIAN_POINT('Ctrl Pts',(50.8567939979677,248.9233475544,31.6432843195571)) ;
#80038 = CARTESIAN_POINT('Ctrl Pts',(50.8585639123037,248.921991389961,31.6432843195571)) ;
#80039 = CARTESIAN_POINT('Ctrl Pts',(50.5275457036156,249.16082384881,31.6213203435597)) ;
#80040 = CARTESIAN_POINT('Ctrl Pts',(50.5279777669084,249.160283764952,31.6213203435597)) ;
#80041 = CARTESIAN_POINT('Ctrl Pts',(50.5284108272628,249.15974460881,31.6213203435597)) ;
#80042 = CARTESIAN_POINT('Ctrl Pts',(50.5772759064884,249.098670406059,31.62132034356)) ;
#80043 = CARTESIAN_POINT('Ctrl Pts',(50.6253743971568,249.039288562501,31.6213203435597)) ;
#80044 = CARTESIAN_POINT('Ctrl Pts',(50.721776854263,248.947901823281,31.6213203435597)) ;
#80045 = CARTESIAN_POINT('Ctrl Pts',(50.7679148643503,248.912194012504,31.6213203435597)) ;
#80046 = CARTESIAN_POINT('Ctrl Pts',(50.8167388067278,248.874784355228,31.6213203435596)) ;
#80047 = CARTESIAN_POINT('Ctrl Pts',(50.8185077026595,248.873425747502,31.6213203435597)) ;
#80048 = CARTESIAN_POINT('Ctrl Pts',(50.8202774450129,248.8720692131,31.6213203435597)) ;
#80049 = CARTESIAN_POINT('Ctrl Pts',(50.5065282494735,249.14398994213,31.6213203435597)) ;
#80050 = CARTESIAN_POINT('Ctrl Pts',(50.5069605765884,249.143450173467,31.6213203435597)) ;
#80051 = CARTESIAN_POINT('Ctrl Pts',(50.5073930953378,249.142910387443,31.6213203435597)) ;
#80052 = CARTESIAN_POINT('Ctrl Pts',(50.556272300514,249.081846646474,31.62132034356)) ;
#80053 = CARTESIAN_POINT('Ctrl Pts',(50.6051720569295,249.021342538492,31.6213203435597)) ;
#80054 = CARTESIAN_POINT('Ctrl Pts',(50.7045314789452,248.927144579668,31.6213203435597)) ;
#80055 = CARTESIAN_POINT('Ctrl Pts',(50.7515320882953,248.890838723369,31.6213203435597)) ;
#80056 = CARTESIAN_POINT('Ctrl Pts',(50.8003512733757,248.853416193082,31.6213203435596)) ;
#80057 = CARTESIAN_POINT('Ctrl Pts',(50.8021206938697,248.852058742774,31.6213203435597)) ;
#80058 = CARTESIAN_POINT('Ctrl Pts',(50.803890188879,248.850701676295,31.6213203435597)) ;
#80059 = CARTESIAN_POINT('',(50.8716089055848,248.949993517828,31.7413203435596)) ;
#80060 = CARTESIAN_POINT('Ctrl Pts',(50.803890188879,248.850701676295,31.6213203435596)) ;
#80061 = CARTESIAN_POINT('Ctrl Pts',(50.8040547677524,248.850942988537,31.6213203435596)) ;
#80062 = CARTESIAN_POINT('Ctrl Pts',(50.8042193485049,248.85118430314,31.6213214476844)) ;
#80063 = CARTESIAN_POINT('Ctrl Pts',(50.8043839279318,248.851425615335,31.6213236533551)) ;
#80064 = CARTESIAN_POINT('Ctrl Pts',(50.8095148172735,248.858948707318,31.6213924168237)) ;
#80065 = CARTESIAN_POINT('Ctrl Pts',(50.8146154558497,248.866426990874,31.622526772514)) ;
#80066 = CARTESIAN_POINT('Ctrl Pts',(50.8195890325768,248.873718590005,31.6246418150554)) ;
#80067 = CARTESIAN_POINT('Ctrl Pts',(50.8233140073649,248.87917965443,31.6262258823324)) ;
#80068 = CARTESIAN_POINT('Ctrl Pts',(50.8269680033362,248.884536381477,31.6283613268649)) ;
#80069 = CARTESIAN_POINT('Ctrl Pts',(50.8305075891557,248.889725537149,31.6310310265338)) ;
#80070 = CARTESIAN_POINT('Ctrl Pts',(50.8352281370105,248.896646024156,31.634591455829)) ;
#80071 = CARTESIAN_POINT('Ctrl Pts',(50.8396936131263,248.903192690413,31.6390611416434)) ;
#80072 = CARTESIAN_POINT('Ctrl Pts',(50.8438048542172,248.909222926106,31.6443797592907)) ;
#80073 = CARTESIAN_POINT('Ctrl Pts',(50.8445910533297,248.910376097581,31.6453968469247)) ;
#80074 = CARTESIAN_POINT('Ctrl Pts',(50.8453642565382,248.911510329011,31.6464451166949)) ;
#80075 = CARTESIAN_POINT('Ctrl Pts',(50.8461236980812,248.912624528739,31.6475243338418)) ;
#80076 = CARTESIAN_POINT('Ctrl Pts',(50.8482225676657,248.915703843982,31.6505069676805)) ;
#80077 = CARTESIAN_POINT('Ctrl Pts',(50.8502164642029,248.918630336928,31.6537258079622)) ;
#80078 = CARTESIAN_POINT('Ctrl Pts',(50.8520991972097,248.921393981,31.6571590528307)) ;
#80079 = CARTESIAN_POINT('Ctrl Pts',(50.8556826308346,248.926654065705,31.6636935986531)) ;
#80080 = CARTESIAN_POINT('Ctrl Pts',(50.8588251896843,248.931267858224,31.6709300524943)) ;
#80081 = CARTESIAN_POINT('Ctrl Pts',(50.861494385594,248.935184014523,31.6786985561853)) ;
#80082 = CARTESIAN_POINT('Ctrl Pts',(50.8633811693728,248.937952241521,31.6841899053575)) ;
#80083 = CARTESIAN_POINT('Ctrl Pts',(50.8650310448257,248.940371382877,31.6899482287076)) ;
#80084 = CARTESIAN_POINT('Ctrl Pts',(50.8664243752224,248.942412655009,31.695921743135)) ;
#80085 = CARTESIAN_POINT('Ctrl Pts',(50.868377896629,248.9452746243,31.7042969198579)) ;
#80086 = CARTESIAN_POINT('Ctrl Pts',(50.8698066535716,248.947363601716,31.7130016467406)) ;
#80087 = CARTESIAN_POINT('Ctrl Pts',(50.8706661025465,248.948618375692,31.7218846188127)) ;
#80088 = CARTESIAN_POINT('Ctrl Pts',(50.871243897259,248.9494619415,31.7278565082957)) ;
#80089 = CARTESIAN_POINT('Ctrl Pts',(50.8715638860115,248.949927796603,31.73390960257)) ;
#80090 = CARTESIAN_POINT('Ctrl Pts',(50.871604452196,248.949986859998,31.7400001290171)) ;
#80091 = CARTESIAN_POINT('Ctrl Pts',(50.8716073820482,248.949991125793,31.7404400112056)) ;
#80092 = CARTESIAN_POINT('Ctrl Pts',(50.8716088516813,248.949993265221,31.7408800883011)) ;
#80093 = CARTESIAN_POINT('Ctrl Pts',(50.8716088516813,248.949993265221,31.7413203435596)) ;
#80094 = CARTESIAN_POINT('Ctrl Pts',(50.8716089964922,248.949993748075,31.7413203435596)) ;
#80095 = CARTESIAN_POINT('Ctrl Pts',(50.8566479182176,248.961467743602,31.7413203435596)) ;
#80096 = CARTESIAN_POINT('Ctrl Pts',(50.8420547949466,248.972665709568,31.7413203435597)) ;
#80097 = CARTESIAN_POINT('Ctrl Pts',(50.8279269473814,248.983761457176,31.7413203435597)) ;
#80098 = CARTESIAN_POINT('Ctrl Pts',(50.8119753337364,248.996289556601,31.7413203435597)) ;
#80099 = CARTESIAN_POINT('Ctrl Pts',(50.7966166422762,249.008687104005,31.7413203435597)) ;
#80100 = CARTESIAN_POINT('Ctrl Pts',(50.7819399930112,249.021151679859,31.7413203435597)) ;
#80101 = CARTESIAN_POINT('Ctrl Pts',(50.7687471099837,249.032356123616,31.7413203435597)) ;
#80102 = CARTESIAN_POINT('Ctrl Pts',(50.7561040600851,249.043613412057,31.7413203435597)) ;
#80103 = CARTESIAN_POINT('Ctrl Pts',(50.7440508843477,249.055041570073,31.7413203435597)) ;
#80104 = CARTESIAN_POINT('Ctrl Pts',(50.7440503228543,249.05504210245,31.7413203435597)) ;
#80105 = CARTESIAN_POINT('Ctrl Pts',(50.7440497613621,249.055042634828,31.7413203435597)) ;
#80106 = CARTESIAN_POINT('Ctrl Pts',(50.7440491998712,249.055043167206,31.7413203435597)) ;
#80107 = CARTESIAN_POINT('Ctrl Pts',(50.728296029037,249.06997954555,31.7413203435597)) ;
#80108 = CARTESIAN_POINT('Ctrl Pts',(50.7128815963623,249.085842182003,31.7413203435597)) ;
#80109 = CARTESIAN_POINT('Ctrl Pts',(50.6976247786594,249.102536202228,31.7413203435598)) ;
#80110 = CARTESIAN_POINT('Ctrl Pts',(50.6834654512365,249.118029347848,31.7413203435598)) ;
#80111 = CARTESIAN_POINT('Ctrl Pts',(50.6694423288583,249.134239033941,31.7413203435599)) ;
#80112 = CARTESIAN_POINT('Ctrl Pts',(50.6553801487296,249.151057959041,31.7413203435599)) ;
#80113 = CARTESIAN_POINT('Ctrl Pts',(50.6424648114365,249.166505214629,31.7413203435599)) ;
#80114 = CARTESIAN_POINT('Ctrl Pts',(50.6295167370137,249.182466604728,31.7413203435598)) ;
#80115 = CARTESIAN_POINT('Ctrl Pts',(50.6163691801403,249.198827039825,31.7413203435597)) ;
#80116 = CARTESIAN_POINT('Ctrl Pts',(50.6114399261129,249.204960859315,31.7413203435597)) ;
#80117 = CARTESIAN_POINT('Ctrl Pts',(50.6064822852617,249.21115041187,31.7413203435597)) ;
#80118 = CARTESIAN_POINT('Ctrl Pts',(50.6014861116635,249.217388230071,31.7413203435596)) ;
#80119 = CARTESIAN_POINT('Ctrl Pts',(50.7761110306795,246.600744027501,31.7413203435596)) ;
#80120 = CARTESIAN_POINT('Ctrl Pts',(50.6248447035851,246.601930855739,31.7413203435596)) ;
#80121 = CARTESIAN_POINT('Ctrl Pts',(50.4675419277232,246.602054016768,31.7413203435596)) ;
#80122 = CARTESIAN_POINT('Ctrl Pts',(50.1844609819171,246.647423619666,31.7413203435596)) ;
#80123 = CARTESIAN_POINT('Ctrl Pts',(50.0717748712232,246.679540434335,31.7413203435596)) ;
#80124 = CARTESIAN_POINT('Ctrl Pts',(49.963014268976,246.709884602433,31.7413203435596)) ;
#80125 = CARTESIAN_POINT('Ctrl Pts',(50.7761110306795,246.600744027501,31.7054164275186)) ;
#80126 = CARTESIAN_POINT('Ctrl Pts',(50.6248447035851,246.601930855739,31.7054164275186)) ;
#80127 = CARTESIAN_POINT('Ctrl Pts',(50.4675419277232,246.602054016768,31.7054164275186)) ;
#80128 = CARTESIAN_POINT('Ctrl Pts',(50.1844609819171,246.647423619666,31.7054164275186)) ;
#80129 = CARTESIAN_POINT('Ctrl Pts',(50.0717748712232,246.679540434335,31.7054164275186)) ;
#80130 = CARTESIAN_POINT('Ctrl Pts',(49.963014268976,246.709884602433,31.7054164275186)) ;
#80131 = CARTESIAN_POINT('Ctrl Pts',(50.7763476477493,246.630901883472,31.6432842878474)) ;
#80132 = CARTESIAN_POINT('Ctrl Pts',(50.6250864771979,246.632151520329,31.6432842878474)) ;
#80133 = CARTESIAN_POINT('Ctrl Pts',(50.4691644240128,246.632354151178,31.6432842878474)) ;
#80134 = CARTESIAN_POINT('Ctrl Pts',(50.1915979820207,246.67682460216,31.6432842878474)) ;
#80135 = CARTESIAN_POINT('Ctrl Pts',(50.0798957973197,246.708634083591,31.6432842878474)) ;
#80136 = CARTESIAN_POINT('Ctrl Pts',(49.9711190288638,246.738933959252,31.6432842878474)) ;
#80137 = CARTESIAN_POINT('Ctrl Pts',(50.7768412470791,246.693813225893,31.6213203435596)) ;
#80138 = CARTESIAN_POINT('Ctrl Pts',(50.6255779626741,246.695037115223,31.6213203435596)) ;
#80139 = CARTESIAN_POINT('Ctrl Pts',(50.4725210286059,246.695515526414,31.6213203435597)) ;
#80140 = CARTESIAN_POINT('Ctrl Pts',(50.2064980096239,246.738155380204,31.6213203435597)) ;
#80141 = CARTESIAN_POINT('Ctrl Pts',(50.0967962515652,246.769214864176,31.6213203435597)) ;
#80142 = CARTESIAN_POINT('Ctrl Pts',(49.9880261102236,246.799532896911,31.6213203435597)) ;
#80143 = CARTESIAN_POINT('Ctrl Pts',(50.7770525158595,246.720740334135,31.6213203435596)) ;
#80144 = CARTESIAN_POINT('Ctrl Pts',(50.625786188765,246.721927162373,31.6213203435596)) ;
#80145 = CARTESIAN_POINT('Ctrl Pts',(50.4739530550717,246.722541884105,31.6213203435597)) ;
#80146 = CARTESIAN_POINT('Ctrl Pts',(50.2128774242644,246.764405702234,31.6213203435597)) ;
#80147 = CARTESIAN_POINT('Ctrl Pts',(50.1040232264648,246.795126089086,31.6213203435597)) ;
#80148 = CARTESIAN_POINT('Ctrl Pts',(49.9952626242177,246.825470257184,31.6213203435597)) ;
#80149 = CARTESIAN_POINT('',(49.963014268976,246.709884602433,31.7413203435596)) ;
#80150 = CARTESIAN_POINT('',(50.7761110306795,246.600744027501,31.7413203435596)) ;
#80151 = CARTESIAN_POINT('Ctrl Pts',(49.963014268976,246.709884602433,31.7413203435596)) ;
#80152 = CARTESIAN_POINT('Ctrl Pts',(50.0717748712232,246.679540434335,31.7413203435596)) ;
#80153 = CARTESIAN_POINT('Ctrl Pts',(50.1844609819171,246.647423619666,31.7413203435596)) ;
#80154 = CARTESIAN_POINT('Ctrl Pts',(50.4675419277232,246.602054016768,31.7413203435596)) ;
#80155 = CARTESIAN_POINT('Ctrl Pts',(50.6248447035851,246.601930855739,31.7413203435596)) ;
#80156 = CARTESIAN_POINT('Ctrl Pts',(50.7761110306795,246.600744027501,31.7413203435596)) ;
#80157 = CARTESIAN_POINT('Origin',(50.776816088154,246.720741444438,31.7413196030361)) ;
#80158 = CARTESIAN_POINT('Ctrl Pts',(50.0058152416557,246.822525453759,31.6213203435597)) ;
#80159 = CARTESIAN_POINT('Ctrl Pts',(50.0057108572187,246.822251975345,31.6213203435597)) ;
#80160 = CARTESIAN_POINT('Ctrl Pts',(50.0056064783735,246.821978495101,31.6213214466101)) ;
#80161 = CARTESIAN_POINT('Ctrl Pts',(49.9998694926128,246.806946276468,31.6214425632436)) ;
#80162 = CARTESIAN_POINT('Ctrl Pts',(49.9942568463425,246.792192381567,31.6247663677073)) ;
#80163 = CARTESIAN_POINT('Ctrl Pts',(49.9847524089911,246.767174852646,31.6360173172129)) ;
#80164 = CARTESIAN_POINT('Ctrl Pts',(49.9799936655788,246.754633080418,31.6439181882807)) ;
#80165 = CARTESIAN_POINT('Ctrl Pts',(49.9717481869224,246.732896031175,31.6673134404803)) ;
#80166 = CARTESIAN_POINT('Ctrl Pts',(49.9686632968791,246.724764023479,31.6803089503134)) ;
#80167 = CARTESIAN_POINT('Ctrl Pts',(49.96538060094,246.716115506741,31.7018008541679)) ;
#80168 = CARTESIAN_POINT('Ctrl Pts',(49.9645064199671,246.713813311183,31.7095030704103)) ;
#80169 = CARTESIAN_POINT('Ctrl Pts',(49.9633228773224,246.710696906288,31.7252452258737)) ;
#80170 = CARTESIAN_POINT('Ctrl Pts',(49.963014268976,246.709884602433,31.7332749378809)) ;
#80171 = CARTESIAN_POINT('Ctrl Pts',(49.963014268976,246.709884602433,31.7413203435596)) ;
#80172 = CARTESIAN_POINT('Ctrl Pts',(50.8658810352972,248.953449595789,31.7413203435596)) ;
#80173 = CARTESIAN_POINT('Ctrl Pts',(50.8677904209831,248.952297607161,31.7413203435596)) ;
#80174 = CARTESIAN_POINT('Ctrl Pts',(50.8697007917982,248.95114620239,31.7413203435596)) ;
#80175 = CARTESIAN_POINT('Ctrl Pts',(50.9146555099304,248.923982502807,31.7413203435597)) ;
#80176 = CARTESIAN_POINT('Ctrl Pts',(50.9528763911288,248.901570300818,31.7413203435596)) ;
#80177 = CARTESIAN_POINT('Ctrl Pts',(51.0258112433797,248.869636083941,31.7413203435597)) ;
#80178 = CARTESIAN_POINT('Ctrl Pts',(51.0659577418149,248.857165972989,31.7413203435597)) ;
#80179 = CARTESIAN_POINT('Ctrl Pts',(51.1146051981685,248.842724136288,31.7413203435596)) ;
#80180 = CARTESIAN_POINT('Ctrl Pts',(51.1174932228874,248.841863408451,31.7413203435596)) ;
#80181 = CARTESIAN_POINT('Ctrl Pts',(51.1203809856748,248.841004114039,31.7413203435596)) ;
#80182 = CARTESIAN_POINT('Ctrl Pts',(50.8658810352972,248.953449595789,31.7054164275186)) ;
#80183 = CARTESIAN_POINT('Ctrl Pts',(50.8677904209831,248.952297607161,31.7054164275186)) ;
#80184 = CARTESIAN_POINT('Ctrl Pts',(50.8697007917982,248.95114620239,31.7054164275186)) ;
#80185 = CARTESIAN_POINT('Ctrl Pts',(50.9146555099304,248.923982502807,31.7054164275187)) ;
#80186 = CARTESIAN_POINT('Ctrl Pts',(50.9528763911288,248.901570300818,31.7054164275186)) ;
#80187 = CARTESIAN_POINT('Ctrl Pts',(51.0258112433797,248.869636083941,31.7054164275186)) ;
#80188 = CARTESIAN_POINT('Ctrl Pts',(51.0659577418149,248.857165972989,31.7054164275186)) ;
#80189 = CARTESIAN_POINT('Ctrl Pts',(51.1146051981685,248.842724136288,31.7054164275186)) ;
#80190 = CARTESIAN_POINT('Ctrl Pts',(51.1174932228874,248.841863408451,31.7054164275186)) ;
#80191 = CARTESIAN_POINT('Ctrl Pts',(51.1203809856748,248.841004114039,31.7054164275186)) ;
#80192 = CARTESIAN_POINT('Ctrl Pts',(50.8503012828812,248.927626635796,31.6432843213404)) ;
#80193 = CARTESIAN_POINT('Ctrl Pts',(50.8522098095963,248.926474052239,31.6432843213404)) ;
#80194 = CARTESIAN_POINT('Ctrl Pts',(50.8541218808106,248.92532381438,31.6432843213404)) ;
#80195 = CARTESIAN_POINT('Ctrl Pts',(50.8990610907504,248.898152284773,31.6432843213404)) ;
#80196 = CARTESIAN_POINT('Ctrl Pts',(50.9385926468991,248.874899245215,31.6432843213404)) ;
#80197 = CARTESIAN_POINT('Ctrl Pts',(51.0157881375332,248.841100025522,31.6432843213404)) ;
#80198 = CARTESIAN_POINT('Ctrl Pts',(51.0573613312886,248.828244720669,31.6432843213404)) ;
#80199 = CARTESIAN_POINT('Ctrl Pts',(51.1060034495555,248.813819167932,31.6432843213404)) ;
#80200 = CARTESIAN_POINT('Ctrl Pts',(51.108892071156,248.81295593694,31.6432843213404)) ;
#80201 = CARTESIAN_POINT('Ctrl Pts',(51.1117795363305,248.812097903334,31.6432843213404)) ;
#80202 = CARTESIAN_POINT('Ctrl Pts',(50.817800902286,248.873758255513,31.6213203435596)) ;
#80203 = CARTESIAN_POINT('Ctrl Pts',(50.8197097813091,248.872605915967,31.6213203435596)) ;
#80204 = CARTESIAN_POINT('Ctrl Pts',(50.8216208964723,248.871455077228,31.6213203435596)) ;
#80205 = CARTESIAN_POINT('Ctrl Pts',(50.866575821533,248.844290875403,31.6213203435597)) ;
#80206 = CARTESIAN_POINT('Ctrl Pts',(50.9087973628861,248.819267489191,31.6213203435597)) ;
#80207 = CARTESIAN_POINT('Ctrl Pts',(50.9948811142887,248.781575254289,31.6213203435597)) ;
#80208 = CARTESIAN_POINT('Ctrl Pts',(51.0394123778877,248.767959465833,31.6213203435597)) ;
#80209 = CARTESIAN_POINT('Ctrl Pts',(51.088060523457,248.753518054849,31.6213203435597)) ;
#80210 = CARTESIAN_POINT('Ctrl Pts',(51.0909487642498,248.752656211516,31.6213203435597)) ;
#80211 = CARTESIAN_POINT('Ctrl Pts',(51.0938363514906,248.751797660789,31.6213203435597)) ;
#80212 = CARTESIAN_POINT('Ctrl Pts',(50.803890188879,248.850701676295,31.6213203435596)) ;
#80213 = CARTESIAN_POINT('Ctrl Pts',(50.8057995745649,248.849549687667,31.6213203435596)) ;
#80214 = CARTESIAN_POINT('Ctrl Pts',(50.807709533127,248.848398088001,31.6213203435596)) ;
#80215 = CARTESIAN_POINT('Ctrl Pts',(50.8526791620758,248.821240949726,31.6213203435597)) ;
#80216 = CARTESIAN_POINT('Ctrl Pts',(50.8960447320484,248.795457119086,31.6213203435597)) ;
#80217 = CARTESIAN_POINT('Ctrl Pts',(50.9859328579063,248.756098193207,31.6213203435597)) ;
#80218 = CARTESIAN_POINT('Ctrl Pts',(51.0317272198324,248.742164050894,31.6213203435597)) ;
#80219 = CARTESIAN_POINT('Ctrl Pts',(51.0803807937155,248.727707582416,31.6213203435597)) ;
#80220 = CARTESIAN_POINT('Ctrl Pts',(51.0832686016586,248.726847429988,31.6213203435597)) ;
#80221 = CARTESIAN_POINT('Ctrl Pts',(51.086156364446,248.725988135576,31.6213203435597)) ;
#80222 = CARTESIAN_POINT('',(51.1117180549604,248.843581675164,31.7413203435596)) ;
#80223 = CARTESIAN_POINT('Ctrl Pts',(51.086156364446,248.725988135576,31.6213203435596)) ;
#80224 = CARTESIAN_POINT('Ctrl Pts',(51.0862184877469,248.726273926329,31.6213203435596)) ;
#80225 = CARTESIAN_POINT('Ctrl Pts',(51.0862806119271,248.726559719963,31.6213214476805)) ;
#80226 = CARTESIAN_POINT('Ctrl Pts',(51.0863427360275,248.726845510821,31.6213236533421)) ;
#80227 = CARTESIAN_POINT('Ctrl Pts',(51.0882792485619,248.735754091775,31.6213924075178)) ;
#80228 = CARTESIAN_POINT('Ctrl Pts',(51.0902047015119,248.744610062794,31.6225264675735)) ;
#80229 = CARTESIAN_POINT('Ctrl Pts',(51.0920824713405,248.753245454865,31.6246412173916)) ;
#80230 = CARTESIAN_POINT('Ctrl Pts',(51.0934961261605,248.759746498517,31.6262332795432)) ;
#80231 = CARTESIAN_POINT('Ctrl Pts',(51.0948829023365,248.76612299147,31.6283824423936)) ;
#80232 = CARTESIAN_POINT('Ctrl Pts',(51.0962258862543,248.772298724066,31.6310714658467)) ;
#80233 = CARTESIAN_POINT('Ctrl Pts',(51.0980065041998,248.780486923596,31.6346367530796)) ;
#80234 = CARTESIAN_POINT('Ctrl Pts',(51.0996908773251,248.788233065203,31.6391102795551)) ;
#80235 = CARTESIAN_POINT('Ctrl Pts',(51.1012400129114,248.795367565278,31.6444325796703)) ;
#80236 = CARTESIAN_POINT('Ctrl Pts',(51.1015312478744,248.796708839653,31.6454331634095)) ;
#80237 = CARTESIAN_POINT('Ctrl Pts',(51.1018176837993,248.798028431586,31.6464638781034)) ;
#80238 = CARTESIAN_POINT('Ctrl Pts',(51.1020990289973,248.799325104428,31.6475245056918)) ;
#80239 = CARTESIAN_POINT('Ctrl Pts',(51.102895783385,248.802997211799,31.6505281456707)) ;
#80240 = CARTESIAN_POINT('Ctrl Pts',(51.1036517788236,248.806485735886,31.6537715081556)) ;
#80241 = CARTESIAN_POINT('Ctrl Pts',(51.1043651577471,248.809778676875,31.6572323814361)) ;
#80242 = CARTESIAN_POINT('Ctrl Pts',(51.1057129105313,248.81599987327,31.6637708443012)) ;
#80243 = CARTESIAN_POINT('Ctrl Pts',(51.106894374542,248.82145637452,31.6710108132204)) ;
#80244 = CARTESIAN_POINT('Ctrl Pts',(51.1078992539062,248.82608772059,31.6787830171431)) ;
#80245 = CARTESIAN_POINT('Ctrl Pts',(51.1086080932376,248.829354660253,31.6842655098964)) ;
#80246 = CARTESIAN_POINT('Ctrl Pts',(51.1092288843809,248.832210410807,31.6900139551922)) ;
#80247 = CARTESIAN_POINT('Ctrl Pts',(51.1097541934407,248.834620869011,31.6959770540884)) ;
#80248 = CARTESIAN_POINT('Ctrl Pts',(51.1104917883012,248.838005431963,31.7043499367117)) ;
#80249 = CARTESIAN_POINT('Ctrl Pts',(51.111033494853,248.840476230148,31.7130520747481)) ;
#80250 = CARTESIAN_POINT('Ctrl Pts',(51.1113601040974,248.841959524176,31.7219325936276)) ;
#80251 = CARTESIAN_POINT('Ctrl Pts',(51.1115813979812,248.842964529093,31.7279495834929)) ;
#80252 = CARTESIAN_POINT('Ctrl Pts',(51.1117037272201,248.843515379474,31.7340491166042)) ;
#80253 = CARTESIAN_POINT('Ctrl Pts',(51.111717190373,248.843576024758,31.7401863974346)) ;
#80254 = CARTESIAN_POINT('Ctrl Pts',(51.1117180192344,248.843579758396,31.7405642402226)) ;
#80255 = CARTESIAN_POINT('Ctrl Pts',(51.1117184349279,248.843581630191,31.7409422258038)) ;
#80256 = CARTESIAN_POINT('Ctrl Pts',(51.1117184349279,248.843581630191,31.7413203435596)) ;
#80257 = CARTESIAN_POINT('Ctrl Pts',(51.1117179332896,248.843581270679,31.7413203435596)) ;
#80258 = CARTESIAN_POINT('Ctrl Pts',(51.065957488389,248.857166051707,31.7413203435597)) ;
#80259 = CARTESIAN_POINT('Ctrl Pts',(51.0258111312861,248.869636133021,31.7413203435597)) ;
#80260 = CARTESIAN_POINT('Ctrl Pts',(50.9528764837856,248.901570260249,31.7413203435596)) ;
#80261 = CARTESIAN_POINT('Ctrl Pts',(50.914655699209,248.923982391817,31.7413203435597)) ;
#80262 = CARTESIAN_POINT('Ctrl Pts',(50.8716087793554,248.949993308924,31.7413203435596)) ;
#80263 = CARTESIAN_POINT('Origin',(51.0967112553384,248.704482161408,31.7413203435596)) ;
#80264 = CARTESIAN_POINT('',(52.0203128398474,248.824482161408,31.7413203435596)) ;
#80265 = CARTESIAN_POINT('',(51.4063975156363,248.824482161408,31.7413203435596)) ;
#80266 = CARTESIAN_POINT('',(51.0967112553384,248.824482161408,31.7413203435596)) ;
#80267 = CARTESIAN_POINT('Origin',(51.4064119640033,248.704480196061,31.7413223089067)) ;
#80268 = CARTESIAN_POINT('Origin',(52.1403128398474,248.704482161408,31.7413203435596)) ;
#80269 = CARTESIAN_POINT('Ctrl Pts',(51.1027668548594,248.844832957121,31.7413203435596)) ;
#80270 = CARTESIAN_POINT('Ctrl Pts',(51.1057506523197,248.844415923056,31.7413203435596)) ;
#80271 = CARTESIAN_POINT('Ctrl Pts',(51.108734666895,248.843999359902,31.7413203435596)) ;
#80272 = CARTESIAN_POINT('Ctrl Pts',(51.1534179425839,248.837743668557,31.7413203435596)) ;
#80273 = CARTESIAN_POINT('Ctrl Pts',(51.1927045698,248.832377914482,31.7413203435596)) ;
#80274 = CARTESIAN_POINT('Ctrl Pts',(51.2859410141499,248.824656420132,31.7413203435596)) ;
#80275 = CARTESIAN_POINT('Ctrl Pts',(51.3443769229423,248.824452291525,31.7413203435596)) ;
#80276 = CARTESIAN_POINT('Ctrl Pts',(51.4064008275487,248.824482163003,31.7413203435596)) ;
#80277 = CARTESIAN_POINT('Ctrl Pts',(51.1027668548594,248.844832957121,31.7054164275186)) ;
#80278 = CARTESIAN_POINT('Ctrl Pts',(51.1057506523197,248.844415923056,31.7054164275186)) ;
#80279 = CARTESIAN_POINT('Ctrl Pts',(51.108734666895,248.843999359902,31.7054164275186)) ;
#80280 = CARTESIAN_POINT('Ctrl Pts',(51.1534179425839,248.837743668557,31.7054164275186)) ;
#80281 = CARTESIAN_POINT('Ctrl Pts',(51.1927045698,248.832377914482,31.7054164275186)) ;
#80282 = CARTESIAN_POINT('Ctrl Pts',(51.2859410141499,248.824656420132,31.7054164275186)) ;
#80283 = CARTESIAN_POINT('Ctrl Pts',(51.3443769229423,248.824452291525,31.7054164275186)) ;
#80284 = CARTESIAN_POINT('Ctrl Pts',(51.4064008275487,248.824482163003,31.7054164275186)) ;
#80285 = CARTESIAN_POINT('Ctrl Pts',(51.0985922489639,248.814964465564,31.643284324805)) ;
#80286 = CARTESIAN_POINT('Ctrl Pts',(51.1015758214971,248.814546944233,31.643284324805)) ;
#80287 = CARTESIAN_POINT('Ctrl Pts',(51.104560266249,248.81413132837,31.643284324805)) ;
#80288 = CARTESIAN_POINT('Ctrl Pts',(51.1492415021694,248.80787131815,31.643284324805)) ;
#80289 = CARTESIAN_POINT('Ctrl Pts',(51.1891454007169,248.802410297526,31.643284324805)) ;
#80290 = CARTESIAN_POINT('Ctrl Pts',(51.2850366354972,248.794467602977,31.643284324805)) ;
#80291 = CARTESIAN_POINT('Ctrl Pts',(51.3443931112797,248.794282641714,31.643284324805)) ;
#80292 = CARTESIAN_POINT('Ctrl Pts',(51.4064153524046,248.794323351499,31.643284324805)) ;
#80293 = CARTESIAN_POINT('Ctrl Pts',(51.0898837497786,248.752656851168,31.6213203435596)) ;
#80294 = CARTESIAN_POINT('Ctrl Pts',(51.0928674145709,248.7522395297,31.6213203435596)) ;
#80295 = CARTESIAN_POINT('Ctrl Pts',(51.0958516053795,248.751823395832,31.6213203435596)) ;
#80296 = CARTESIAN_POINT('Ctrl Pts',(51.1405353953433,248.745567842801,31.6213203435596)) ;
#80297 = CARTESIAN_POINT('Ctrl Pts',(51.1817199296158,248.739895483147,31.6213203435596)) ;
#80298 = CARTESIAN_POINT('Ctrl Pts',(51.2831521234115,248.731498417485,31.6213203435596)) ;
#80299 = CARTESIAN_POINT('Ctrl Pts',(51.3444227287569,248.73137384663,31.6213203435596)) ;
#80300 = CARTESIAN_POINT('Ctrl Pts',(51.4064456521979,248.731410110828,31.6213203435597)) ;
#80301 = CARTESIAN_POINT('Ctrl Pts',(51.086156364446,248.725988135576,31.6213203435596)) ;
#80302 = CARTESIAN_POINT('Ctrl Pts',(51.0891401619064,248.72557110151,31.6213203435596)) ;
#80303 = CARTESIAN_POINT('Ctrl Pts',(51.0921240529548,248.725154332015,31.6213203435596)) ;
#80304 = CARTESIAN_POINT('Ctrl Pts',(51.1368100661075,248.718902921604,31.6213203435596)) ;
#80305 = CARTESIAN_POINT('Ctrl Pts',(51.1785415671225,248.713138013086,31.6213203435596)) ;
#80306 = CARTESIAN_POINT('Ctrl Pts',(51.2823458655609,248.704547641672,31.6213203435596)) ;
#80307 = CARTESIAN_POINT('Ctrl Pts',(51.3444347164168,248.704452305443,31.6213203435597)) ;
#80308 = CARTESIAN_POINT('Ctrl Pts',(51.4064586210232,248.704482176921,31.6213203435597)) ;
#80309 = CARTESIAN_POINT('Ctrl Pts',(51.4063975156363,248.824482161408,31.7413203435596)) ;
#80310 = CARTESIAN_POINT('Ctrl Pts',(51.3843454600747,248.824471540866,31.7413203435596)) ;
#80311 = CARTESIAN_POINT('Ctrl Pts',(51.3627451413246,248.82446585171,31.7413203435596)) ;
#80312 = CARTESIAN_POINT('Ctrl Pts',(51.3415687668468,248.824692574776,31.7413203435596)) ;
#80313 = CARTESIAN_POINT('Ctrl Pts',(51.3183068802966,248.824941626201,31.7413203435596)) ;
#80314 = CARTESIAN_POINT('Ctrl Pts',(51.2955565276338,248.825470785683,31.7413203435596)) ;
#80315 = CARTESIAN_POINT('Ctrl Pts',(51.2732760199652,248.826515819019,31.7413203435596)) ;
#80316 = CARTESIAN_POINT('Ctrl Pts',(51.2587924657089,248.827195148109,31.7413203435596)) ;
#80317 = CARTESIAN_POINT('Ctrl Pts',(51.2445073560321,248.828091135254,31.7413203435596)) ;
#80318 = CARTESIAN_POINT('Ctrl Pts',(51.2304083944376,248.829257089501,31.7413203435596)) ;
#80319 = CARTESIAN_POINT('Ctrl Pts',(51.2282454160114,248.829435963234,31.7413203435596)) ;
#80320 = CARTESIAN_POINT('Ctrl Pts',(51.2260772117856,248.829621971491,31.7413203435596)) ;
#80321 = CARTESIAN_POINT('Ctrl Pts',(51.223903630718,248.829814863711,31.7413203435596)) ;
#80322 = CARTESIAN_POINT('Ctrl Pts',(51.2060460327205,248.831399617905,31.7413203435596)) ;
#80323 = CARTESIAN_POINT('Ctrl Pts',(51.1878257913053,248.833452870398,31.7413203435596)) ;
#80324 = CARTESIAN_POINT('Ctrl Pts',(51.1691574004514,248.835811237207,31.7413203435596)) ;
#80325 = CARTESIAN_POINT('Ctrl Pts',(51.1521435087056,248.83796059212,31.7413203435596)) ;
#80326 = CARTESIAN_POINT('Ctrl Pts',(51.1347574231604,248.840363925417,31.7413203435596)) ;
#80327 = CARTESIAN_POINT('Ctrl Pts',(51.1169311642445,248.842853457903,31.7413203435596)) ;
#80328 = CARTESIAN_POINT('Ctrl Pts',(51.115197667293,248.843095550032,31.7413203435596)) ;
#80329 = CARTESIAN_POINT('Ctrl Pts',(51.113460004846,248.843338416063,31.7413203435596)) ;
#80330 = CARTESIAN_POINT('Ctrl Pts',(51.1117181123312,248.84358187378,31.7413203435596)) ;
#80331 = CARTESIAN_POINT('Origin',(52.1403128398474,248.712613109356,31.7413203435596)) ;
#80332 = CARTESIAN_POINT('',(52.0203128398474,250.600744087106,31.7413203435596)) ;
#80333 = CARTESIAN_POINT('Origin',(52.1403128398474,250.480744087106,31.7413203435596)) ;
#80334 = CARTESIAN_POINT('',(52.0203128398474,248.712613109356,31.7413203435596)) ;
#80335 = CARTESIAN_POINT('Origin',(51.4036689174439,250.480744087106,31.7413203435596)) ;
#80336 = CARTESIAN_POINT('',(52.5496443674977,250.600744087106,31.7413203435596)) ;
#80337 = CARTESIAN_POINT('',(51.4036689174439,250.600744087106,31.7413203435596)) ;
#80338 = CARTESIAN_POINT('Origin',(52.4296443674977,250.480744087106,31.7413203435596)) ;
#80339 = CARTESIAN_POINT('Origin',(52.4296443674977,249.600744072205,31.7413203435596)) ;
#80340 = CARTESIAN_POINT('',(52.5496443674977,246.600744027501,31.7413203435596)) ;
#80341 = CARTESIAN_POINT('',(52.5496443674977,249.600744072205,31.7413203435596)) ;
#80342 = CARTESIAN_POINT('Origin',(52.4296443674977,246.720744027501,31.7413203435596)) ;
#80343 = CARTESIAN_POINT('Origin',(51.6683346812691,246.720744027501,31.7413203435596)) ;
#80344 = CARTESIAN_POINT('',(51.6683346812691,246.600744027501,31.7413203435596)) ;
#80345 = CARTESIAN_POINT('Ctrl Pts',(49.963014268976,246.709884602433,31.7413203435596)) ;
#80346 = CARTESIAN_POINT('Ctrl Pts',(49.931599450876,246.725215026983,31.7413203435596)) ;
#80347 = CARTESIAN_POINT('Ctrl Pts',(49.8506223616046,246.764832992921,31.7413203435596)) ;
#80348 = CARTESIAN_POINT('Ctrl Pts',(49.7636581126107,246.815285524649,31.7413203435596)) ;
#80349 = CARTESIAN_POINT('Ctrl Pts',(49.6774660851055,246.887582047699,31.7413203435596)) ;
#80350 = CARTESIAN_POINT('Ctrl Pts',(49.6042085555324,246.966699774459,31.7413203435596)) ;
#80351 = CARTESIAN_POINT('Ctrl Pts',(49.5497454158327,247.044683872908,31.7413203435596)) ;
#80352 = CARTESIAN_POINT('Ctrl Pts',(49.5182664633806,247.089148063069,31.7413203435596)) ;
#80353 = CARTESIAN_POINT('Ctrl Pts',(49.963014268976,246.709884602433,31.7054164275186)) ;
#80354 = CARTESIAN_POINT('Ctrl Pts',(49.931599450876,246.725215026983,31.7054164275186)) ;
#80355 = CARTESIAN_POINT('Ctrl Pts',(49.8506223616046,246.764832992921,31.7054164275186)) ;
#80356 = CARTESIAN_POINT('Ctrl Pts',(49.7636581126107,246.815285524649,31.7054164275186)) ;
#80357 = CARTESIAN_POINT('Ctrl Pts',(49.6774660851055,246.887582047699,31.7054164275186)) ;
#80358 = CARTESIAN_POINT('Ctrl Pts',(49.6042085555324,246.966699774459,31.7054164275186)) ;
#80359 = CARTESIAN_POINT('Ctrl Pts',(49.5497454158327,247.044683872908,31.7054164275186)) ;
#80360 = CARTESIAN_POINT('Ctrl Pts',(49.5182664633806,247.089148063069,31.7054164275186)) ;
#80361 = CARTESIAN_POINT('Ctrl Pts',(49.9762408566705,246.736988277557,31.6432842791516)) ;
#80362 = CARTESIAN_POINT('Ctrl Pts',(49.944806126295,246.752294468368,31.6432842791516)) ;
#80363 = CARTESIAN_POINT('Ctrl Pts',(49.86448943937,246.791620886194,31.6432842791516)) ;
#80364 = CARTESIAN_POINT('Ctrl Pts',(49.7803936532232,246.840563126454,31.6432842791516)) ;
#80365 = CARTESIAN_POINT('Ctrl Pts',(49.6987354791454,246.909056370919,31.6432842791516)) ;
#80366 = CARTESIAN_POINT('Ctrl Pts',(49.6282809757044,246.985040051368,31.6432842791516)) ;
#80367 = CARTESIAN_POINT('Ctrl Pts',(49.5743922695998,247.06208594874,31.6432842791516)) ;
#80368 = CARTESIAN_POINT('Ctrl Pts',(49.5428810753553,247.106574270477,31.6432842791516)) ;
#80369 = CARTESIAN_POINT('Ctrl Pts',(50.0038324296295,246.793528410729,31.6213203435597)) ;
#80370 = CARTESIAN_POINT('Ctrl Pts',(49.9724058609042,246.808844534472,31.6213203435597)) ;
#80371 = CARTESIAN_POINT('Ctrl Pts',(49.8934018962093,246.847455485118,31.6213203435597)) ;
#80372 = CARTESIAN_POINT('Ctrl Pts',(49.8152625837333,246.893353442029,31.6213203435596)) ;
#80373 = CARTESIAN_POINT('Ctrl Pts',(49.7431381507101,246.953899251354,31.6213203435596)) ;
#80374 = CARTESIAN_POINT('Ctrl Pts',(49.6784688486474,247.023279651295,31.6213203435597)) ;
#80375 = CARTESIAN_POINT('Ctrl Pts',(49.6257268303213,247.098448108743,31.6213203435596)) ;
#80376 = CARTESIAN_POINT('Ctrl Pts',(49.5942288513534,247.142926539422,31.6213203435596)) ;
#80377 = CARTESIAN_POINT('Ctrl Pts',(50.0156420836194,246.817728531914,31.6213203435597)) ;
#80378 = CARTESIAN_POINT('Ctrl Pts',(49.9842272655194,246.833058956463,31.6213203435597)) ;
#80379 = CARTESIAN_POINT('Ctrl Pts',(49.9057743814449,246.871345851783,31.6213203435597)) ;
#80380 = CARTESIAN_POINT('Ctrl Pts',(49.8301799972564,246.915958463683,31.6213203435596)) ;
#80381 = CARTESIAN_POINT('Ctrl Pts',(49.7621487599861,246.973100389465,31.6213203435596)) ;
#80382 = CARTESIAN_POINT('Ctrl Pts',(49.6999453025556,247.039643602022,31.6213203435597)) ;
#80383 = CARTESIAN_POINT('Ctrl Pts',(49.6476855094111,247.114021727431,31.6213203435596)) ;
#80384 = CARTESIAN_POINT('Ctrl Pts',(49.616206556959,247.158485917592,31.6213203435596)) ;
#80385 = CARTESIAN_POINT('',(49.5182664633806,247.089148063069,31.7413203435596)) ;
#80386 = CARTESIAN_POINT('Ctrl Pts',(49.5182664633806,247.089148063069,31.7413203435596)) ;
#80387 = CARTESIAN_POINT('Ctrl Pts',(49.5497454158327,247.044683872908,31.7413203435596)) ;
#80388 = CARTESIAN_POINT('Ctrl Pts',(49.6042085555324,246.966699774459,31.7413203435596)) ;
#80389 = CARTESIAN_POINT('Ctrl Pts',(49.6774660851055,246.887582047699,31.7413203435596)) ;
#80390 = CARTESIAN_POINT('Ctrl Pts',(49.7636581126107,246.815285524649,31.7413203435596)) ;
#80391 = CARTESIAN_POINT('Ctrl Pts',(49.8506223616046,246.764832992921,31.7413203435596)) ;
#80392 = CARTESIAN_POINT('Ctrl Pts',(49.931599450876,246.725215026983,31.7413203435596)) ;
#80393 = CARTESIAN_POINT('Ctrl Pts',(49.963014268976,246.709884602433,31.7413203435596)) ;
#80394 = CARTESIAN_POINT('Ctrl Pts',(49.6210143583557,247.151690507276,31.6213203435596)) ;
#80395 = CARTESIAN_POINT('Ctrl Pts',(49.6207661365521,247.151539246675,31.6213203435596)) ;
#80396 = CARTESIAN_POINT('Ctrl Pts',(49.6205164447654,247.151387225589,31.6213214399498)) ;
#80397 = CARTESIAN_POINT('Ctrl Pts',(49.6202667549629,247.151235205894,31.6213236426165)) ;
#80398 = CARTESIAN_POINT('Ctrl Pts',(49.6124809300875,247.146494929318,31.6213923261465)) ;
#80399 = CARTESIAN_POINT('Ctrl Pts',(49.6047409010513,247.141782670592,31.6225275482499)) ;
#80400 = CARTESIAN_POINT('Ctrl Pts',(49.5971939561122,247.13718789474,31.6246439453278)) ;
#80401 = CARTESIAN_POINT('Ctrl Pts',(49.5915259656661,247.133737075124,31.6262334253776)) ;
#80402 = CARTESIAN_POINT('Ctrl Pts',(49.585966463366,247.130352225227,31.6283776256885)) ;
#80403 = CARTESIAN_POINT('Ctrl Pts',(49.5805814724203,247.127073844614,31.6310592826868)) ;
#80404 = CARTESIAN_POINT('Ctrl Pts',(49.5734257007315,247.122717413301,31.6346227659724)) ;
#80405 = CARTESIAN_POINT('Ctrl Pts',(49.5666561311895,247.118596395527,31.6390944397671)) ;
#80406 = CARTESIAN_POINT('Ctrl Pts',(49.5604201950558,247.114802652923,31.6444146524314)) ;
#80407 = CARTESIAN_POINT('Ctrl Pts',(49.5592408348075,247.11408516815,31.6454208281193)) ;
#80408 = CARTESIAN_POINT('Ctrl Pts',(49.558080617175,247.113379429088,31.6464574885456)) ;
#80409 = CARTESIAN_POINT('Ctrl Pts',(49.556940634716,247.112686124991,31.6475244112343)) ;
#80410 = CARTESIAN_POINT('Ctrl Pts',(49.556940190168,247.11268585463,31.6475248272918)) ;
#80411 = CARTESIAN_POINT('Ctrl Pts',(49.5569397456231,247.112685584271,31.647525243354)) ;
#80412 = CARTESIAN_POINT('Ctrl Pts',(49.5569393010813,247.112685313913,31.6475256594207)) ;
#80413 = CARTESIAN_POINT('Ctrl Pts',(49.5537377487577,247.110738223408,31.6505221368304)) ;
#80414 = CARTESIAN_POINT('Ctrl Pts',(49.5506956091687,247.108889076253,31.6537571310734)) ;
#80415 = CARTESIAN_POINT('Ctrl Pts',(49.5478235026766,247.107143545382,31.6572085979443)) ;
#80416 = CARTESIAN_POINT('Ctrl Pts',(49.5423838363783,247.103837572752,31.6637455519426)) ;
#80417 = CARTESIAN_POINT('Ctrl Pts',(49.5376124175149,247.10093844266,31.6709841927054)) ;
#80418 = CARTESIAN_POINT('Ctrl Pts',(49.533562965559,247.09847574875,31.678755099518)) ;
#80419 = CARTESIAN_POINT('Ctrl Pts',(49.5307045400923,247.096737383394,31.6842404239951)) ;
#80420 = CARTESIAN_POINT('Ctrl Pts',(49.5282063572055,247.095216848345,31.6899920749716)) ;
#80421 = CARTESIAN_POINT('Ctrl Pts',(49.5260982265622,247.093932318721,31.6959585760797)) ;
#80422 = CARTESIAN_POINT('Ctrl Pts',(49.5231392608972,247.092129356904,31.7043331386219)) ;
#80423 = CARTESIAN_POINT('Ctrl Pts',(49.5209800806778,247.090810247108,31.7130371660676)) ;
#80424 = CARTESIAN_POINT('Ctrl Pts',(49.519684064817,247.090016978543,31.7219195434862)) ;
#80425 = CARTESIAN_POINT('Ctrl Pts',(49.5187514549454,247.089446144406,31.7283112807438)) ;
#80426 = CARTESIAN_POINT('Ctrl Pts',(49.5182664633807,247.089148063069,31.7347961218212)) ;
#80427 = CARTESIAN_POINT('Ctrl Pts',(49.5182664633807,247.089148063069,31.7413203435596)) ;
#80428 = CARTESIAN_POINT('Ctrl Pts',(49.5182664633807,247.089148063069,31.7413203435596)) ;
#80429 = CARTESIAN_POINT('Ctrl Pts',(49.4739778031524,247.174728266885,31.7413203435596)) ;
#80430 = CARTESIAN_POINT('Ctrl Pts',(49.4243564080963,247.265450319237,31.7413203435596)) ;
#80431 = CARTESIAN_POINT('Ctrl Pts',(49.3620432342539,247.48914516309,31.7413203435596)) ;
#80432 = CARTESIAN_POINT('Ctrl Pts',(49.3579333223532,247.594303447023,31.7413203435596)) ;
#80433 = CARTESIAN_POINT('Ctrl Pts',(49.3518273473795,247.692149180776,31.7413203435596)) ;
#80434 = CARTESIAN_POINT('Ctrl Pts',(49.5182664633807,247.089148063069,31.7054164275186)) ;
#80435 = CARTESIAN_POINT('Ctrl Pts',(49.4739778031524,247.174728266885,31.7054164275186)) ;
#80436 = CARTESIAN_POINT('Ctrl Pts',(49.4243564080963,247.265450319237,31.7054164275186)) ;
#80437 = CARTESIAN_POINT('Ctrl Pts',(49.3620432342539,247.48914516309,31.7054164275186)) ;
#80438 = CARTESIAN_POINT('Ctrl Pts',(49.3579333223532,247.594303447023,31.7054164275186)) ;
#80439 = CARTESIAN_POINT('Ctrl Pts',(49.3518273473795,247.692149180776,31.7054164275186)) ;
#80440 = CARTESIAN_POINT('Ctrl Pts',(49.5450510815804,247.103009386154,31.6432842835775)) ;
#80441 = CARTESIAN_POINT('Ctrl Pts',(49.5009087357332,247.188686189581,31.6432842835775)) ;
#80442 = CARTESIAN_POINT('Ctrl Pts',(49.4521809274138,247.278024774281,31.6432842835775)) ;
#80443 = CARTESIAN_POINT('Ctrl Pts',(49.3923857677425,247.492693277404,31.6432842835775)) ;
#80444 = CARTESIAN_POINT('Ctrl Pts',(49.38821128267,247.596175793791,31.6432842835775)) ;
#80445 = CARTESIAN_POINT('Ctrl Pts',(49.3819275757361,247.694027558442,31.6432842835775)) ;
#80446 = CARTESIAN_POINT('Ctrl Pts',(49.6009256299209,247.131925055626,31.6213203435596)) ;
#80447 = CARTESIAN_POINT('Ctrl Pts',(49.5567233085258,247.217562262025,31.6213203435596)) ;
#80448 = CARTESIAN_POINT('Ctrl Pts',(49.5101540874739,247.304273277684,31.6213203435596)) ;
#80449 = CARTESIAN_POINT('Ctrl Pts',(49.4556207812252,247.500038912409,31.6213203435596)) ;
#80450 = CARTESIAN_POINT('Ctrl Pts',(49.4509295670317,247.600096690393,31.6213203435596)) ;
#80451 = CARTESIAN_POINT('Ctrl Pts',(49.4447187139868,247.697945982926,31.6213203435596)) ;
#80452 = CARTESIAN_POINT('Ctrl Pts',(49.6248408710857,247.144301445761,31.6213203435596)) ;
#80453 = CARTESIAN_POINT('Ctrl Pts',(49.5805522108574,247.229881649577,31.6213203435596)) ;
#80454 = CARTESIAN_POINT('Ctrl Pts',(49.5349558256602,247.315510954877,31.6213203435596)) ;
#80455 = CARTESIAN_POINT('Ctrl Pts',(49.4826761929734,247.503173668296,31.6213203435596)) ;
#80456 = CARTESIAN_POINT('Ctrl Pts',(49.4777003462836,247.601777400386,31.6213203435596)) ;
#80457 = CARTESIAN_POINT('Ctrl Pts',(49.4715943713098,247.699623134138,31.6213203435596)) ;
#80458 = CARTESIAN_POINT('',(49.3518273473795,247.692149180776,31.7413203435596)) ;
#80459 = CARTESIAN_POINT('Ctrl Pts',(49.3518273473795,247.692149180776,31.7413203435596)) ;
#80460 = CARTESIAN_POINT('Ctrl Pts',(49.3532388697544,247.669530116159,31.7413203435596)) ;
#80461 = CARTESIAN_POINT('Ctrl Pts',(49.3546686212915,247.646555189823,31.7413203435596)) ;
#80462 = CARTESIAN_POINT('Ctrl Pts',(49.3563472260032,247.623183539353,31.7413203435596)) ;
#80463 = CARTESIAN_POINT('Ctrl Pts',(49.3578189696063,247.602692069958,31.7413203435596)) ;
#80464 = CARTESIAN_POINT('Ctrl Pts',(49.3594818314035,247.581895581421,31.7413203435596)) ;
#80465 = CARTESIAN_POINT('Ctrl Pts',(49.3615296529984,247.560777183086,31.7413203435596)) ;
#80466 = CARTESIAN_POINT('Ctrl Pts',(49.3634663892828,247.540804364933,31.7413203435596)) ;
#80467 = CARTESIAN_POINT('Ctrl Pts',(49.3657469823047,247.520543483475,31.7413203435596)) ;
#80468 = CARTESIAN_POINT('Ctrl Pts',(49.3685771465373,247.499991824908,31.7413203435596)) ;
#80469 = CARTESIAN_POINT('Ctrl Pts',(49.3713415064495,247.479918014202,31.7413203435596)) ;
#80470 = CARTESIAN_POINT('Ctrl Pts',(49.3746294947228,247.459566601333,31.7413203435596)) ;
#80471 = CARTESIAN_POINT('Ctrl Pts',(49.3786823865536,247.438948806417,31.7413203435596)) ;
#80472 = CARTESIAN_POINT('Ctrl Pts',(49.3807088324691,247.428639908959,31.7413203435596)) ;
#80473 = CARTESIAN_POINT('Ctrl Pts',(49.3829273491322,247.418264650282,31.7413203435596)) ;
#80474 = CARTESIAN_POINT('Ctrl Pts',(49.3853737884668,247.407826011524,31.7413203435596)) ;
#80475 = CARTESIAN_POINT('Ctrl Pts',(49.386597008134,247.402606692145,31.7413203435596)) ;
#80476 = CARTESIAN_POINT('Ctrl Pts',(49.3878772728497,247.3973715456,31.7413203435596)) ;
#80477 = CARTESIAN_POINT('Ctrl Pts',(49.3892194719798,247.392121057641,31.7413203435596)) ;
#80478 = CARTESIAN_POINT('Ctrl Pts',(49.3900313620237,247.388945061766,31.7413203435596)) ;
#80479 = CARTESIAN_POINT('Ctrl Pts',(49.3908659191905,247.385763453995,31.7413203435596)) ;
#80480 = CARTESIAN_POINT('Ctrl Pts',(49.3917242773753,247.382576356185,31.7413203435596)) ;
#80481 = CARTESIAN_POINT('Ctrl Pts',(49.3922849384499,247.380494612556,31.7413203435596)) ;
#80482 = CARTESIAN_POINT('Ctrl Pts',(49.3928557558029,247.378410523425,31.7413203435596)) ;
#80483 = CARTESIAN_POINT('Ctrl Pts',(49.393437051874,247.376324135667,31.7413203435596)) ;
#80484 = CARTESIAN_POINT('Ctrl Pts',(49.3988416175673,247.35692606941,31.7413203435596)) ;
#80485 = CARTESIAN_POINT('Ctrl Pts',(49.4049126636213,247.338171165244,31.7413203435596)) ;
#80486 = CARTESIAN_POINT('Ctrl Pts',(49.4114315368304,247.319954022923,31.7413203435596)) ;
#80487 = CARTESIAN_POINT('Ctrl Pts',(49.4182839819689,247.300804706111,31.7413203435596)) ;
#80488 = CARTESIAN_POINT('Ctrl Pts',(49.4256316444079,247.282249701211,31.7413203435596)) ;
#80489 = CARTESIAN_POINT('Ctrl Pts',(49.433276546524,247.264182112204,31.7413203435596)) ;
#80490 = CARTESIAN_POINT('Ctrl Pts',(49.4415958507146,247.244520674208,31.7413203435596)) ;
#80491 = CARTESIAN_POINT('Ctrl Pts',(49.4502673598285,247.225436498998,31.7413203435596)) ;
#80492 = CARTESIAN_POINT('Ctrl Pts',(49.4590962100918,247.206808544484,31.7413203435596)) ;
#80493 = CARTESIAN_POINT('Ctrl Pts',(49.4689135927178,247.186094889642,31.7413203435596)) ;
#80494 = CARTESIAN_POINT('Ctrl Pts',(49.4789257823363,247.165945409405,31.7413203435596)) ;
#80495 = CARTESIAN_POINT('Ctrl Pts',(49.4889328468167,247.146212535825,31.7413203435596)) ;
#80496 = CARTESIAN_POINT('Ctrl Pts',(49.498761731518,247.126831013938,31.7413203435596)) ;
#80497 = CARTESIAN_POINT('Ctrl Pts',(49.5085870880952,247.107851787803,31.7413203435596)) ;
#80498 = CARTESIAN_POINT('Ctrl Pts',(49.5182664633806,247.089148063069,31.7413203435596)) ;
#80499 = CARTESIAN_POINT('Ctrl Pts',(49.4721208157112,247.69114871288,31.6213203435642)) ;
#80500 = CARTESIAN_POINT('Ctrl Pts',(49.4718285538257,247.691151145633,31.6213203461521)) ;
#80501 = CARTESIAN_POINT('Ctrl Pts',(49.4715362875381,247.691153578127,31.6213214522989)) ;
#80502 = CARTESIAN_POINT('Ctrl Pts',(49.4712440226149,247.691156010318,31.6213236594508)) ;
#80503 = CARTESIAN_POINT('Ctrl Pts',(49.4621299528602,247.691231856448,31.6213924878829)) ;
#80504 = CARTESIAN_POINT('Ctrl Pts',(49.453068413761,247.691306946542,31.6225270006307)) ;
#80505 = CARTESIAN_POINT('Ctrl Pts',(49.4442320358178,247.691379867774,31.6246429710497)) ;
#80506 = CARTESIAN_POINT('Ctrl Pts',(49.4375943456525,247.691434644577,31.6262324408676)) ;
#80507 = CARTESIAN_POINT('Ctrl Pts',(49.4310832231964,247.691488164056,31.6283769854049)) ;
#80508 = CARTESIAN_POINT('Ctrl Pts',(49.4247764592481,247.691540106816,31.6310595117001)) ;
#80509 = CARTESIAN_POINT('Ctrl Pts',(49.416396458367,247.691609124838,31.6346238709977)) ;
#80510 = CARTESIAN_POINT('Ctrl Pts',(49.408468612876,247.691674511449,31.639097198746)) ;
#80511 = CARTESIAN_POINT('Ctrl Pts',(49.4011672799356,247.69173678212,31.6444197570069)) ;
#80512 = CARTESIAN_POINT('Ctrl Pts',(49.3997898445836,247.691748529814,31.6454238859751)) ;
#80513 = CARTESIAN_POINT('Ctrl Pts',(49.398434774684,247.691760171008,31.6464583727284)) ;
#80514 = CARTESIAN_POINT('Ctrl Pts',(49.3971033555651,247.691771716554,31.6475229947526)) ;
#80515 = CARTESIAN_POINT('Ctrl Pts',(49.3971027624604,247.691771721697,31.6475234690077)) ;
#80516 = CARTESIAN_POINT('Ctrl Pts',(49.3971021693603,247.69177172684,31.6475239432689)) ;
#80517 = CARTESIAN_POINT('Ctrl Pts',(49.397101576265,247.691771731983,31.647524417536)) ;
#80518 = CARTESIAN_POINT('Ctrl Pts',(49.3933525775546,247.691804242096,31.6505222943044)) ;
#80519 = CARTESIAN_POINT('Ctrl Pts',(49.3897908797355,247.691835977459,31.6537589339136)) ;
#80520 = CARTESIAN_POINT('Ctrl Pts',(49.3864285291373,247.691866160815,31.6572122154329)) ;
#80521 = CARTESIAN_POINT('Ctrl Pts',(49.3800593805917,247.69192333578,31.6637536103066)) ;
#80522 = CARTESIAN_POINT('Ctrl Pts',(49.374473703726,247.691974088573,31.67099741896)) ;
#80523 = CARTESIAN_POINT('Ctrl Pts',(49.3697327311707,247.69201525315,31.6787738331248)) ;
#80524 = CARTESIAN_POINT('Ctrl Pts',(49.366391190525,247.69204426684,31.6842548190841)) ;
#80525 = CARTESIAN_POINT('Ctrl Pts',(49.3634699029181,247.69206856051,31.6900015151129)) ;
#80526 = CARTESIAN_POINT('Ctrl Pts',(49.3610036578803,247.692087865578,31.6959626248072)) ;
#80527 = CARTESIAN_POINT('Ctrl Pts',(49.3575396024612,247.692114981224,31.704335521265)) ;
#80528 = CARTESIAN_POINT('Ctrl Pts',(49.355009880036,247.692131795729,31.7130376254696)) ;
#80529 = CARTESIAN_POINT('Ctrl Pts',(49.3534904620416,247.692140603079,31.7219180382076)) ;
#80530 = CARTESIAN_POINT('Ctrl Pts',(49.3523967698609,247.692146942697,31.7283102475993)) ;
#80531 = CARTESIAN_POINT('Ctrl Pts',(49.3518273473795,247.692149180776,31.7347955926502)) ;
#80532 = CARTESIAN_POINT('Ctrl Pts',(49.3518273473795,247.692149180776,31.7413203435596)) ;
#80533 = CARTESIAN_POINT('Ctrl Pts',(49.3518273473795,247.692149180776,31.7413203435596)) ;
#80534 = CARTESIAN_POINT('Ctrl Pts',(49.3575747933183,247.764817090958,31.7413203435596)) ;
#80535 = CARTESIAN_POINT('Ctrl Pts',(49.3665625013471,247.891107509426,31.7413203435596)) ;
#80536 = CARTESIAN_POINT('Ctrl Pts',(49.3988727594182,248.028724139293,31.7413203435597)) ;
#80537 = CARTESIAN_POINT('Ctrl Pts',(49.4417511608872,248.138252930567,31.7413203435597)) ;
#80538 = CARTESIAN_POINT('Ctrl Pts',(49.5086086325514,248.25752820517,31.7413203435597)) ;
#80539 = CARTESIAN_POINT('Ctrl Pts',(49.5842744886713,248.353930549759,31.7413203435597)) ;
#80540 = CARTESIAN_POINT('Ctrl Pts',(49.6274070383129,248.40974827469,31.7413203435597)) ;
#80541 = CARTESIAN_POINT('Ctrl Pts',(49.3518273473795,247.692149180776,31.7054164275186)) ;
#80542 = CARTESIAN_POINT('Ctrl Pts',(49.3575747933183,247.764817090958,31.7054164275186)) ;
#80543 = CARTESIAN_POINT('Ctrl Pts',(49.3665625013471,247.891107509426,31.7054164275186)) ;
#80544 = CARTESIAN_POINT('Ctrl Pts',(49.3988727594182,248.028724139293,31.7054164275186)) ;
#80545 = CARTESIAN_POINT('Ctrl Pts',(49.4417511608872,248.138252930567,31.7054164275186)) ;
#80546 = CARTESIAN_POINT('Ctrl Pts',(49.5086086325514,248.25752820517,31.7054164275186)) ;
#80547 = CARTESIAN_POINT('Ctrl Pts',(49.5842744886713,248.353930549759,31.7054164275186)) ;
#80548 = CARTESIAN_POINT('Ctrl Pts',(49.6274070383129,248.40974827469,31.7054164275186)) ;
#80549 = CARTESIAN_POINT('Ctrl Pts',(49.3818922493259,247.689771289377,31.6432842964434)) ;
#80550 = CARTESIAN_POINT('Ctrl Pts',(49.3876703792343,247.762477814527,31.6432842964434)) ;
#80551 = CARTESIAN_POINT('Ctrl Pts',(49.3966525635991,247.887497453901,31.6432842964434)) ;
#80552 = CARTESIAN_POINT('Ctrl Pts',(49.4279714952411,248.020314617985,31.6432842964434)) ;
#80553 = CARTESIAN_POINT('Ctrl Pts',(49.468857501104,248.124759718921,31.6432842964434)) ;
#80554 = CARTESIAN_POINT('Ctrl Pts',(49.5332946362515,248.239961500277,31.6432842964434)) ;
#80555 = CARTESIAN_POINT('Ctrl Pts',(49.6081351537844,248.335445899508,31.6432842964434)) ;
#80556 = CARTESIAN_POINT('Ctrl Pts',(49.6512710987205,248.391307577376,31.6432842964434)) ;
#80557 = CARTESIAN_POINT('Ctrl Pts',(49.4446096612768,247.68481084764,31.6213203435596)) ;
#80558 = CARTESIAN_POINT('Ctrl Pts',(49.450375211021,247.757501540984,31.6213203435596)) ;
#80559 = CARTESIAN_POINT('Ctrl Pts',(49.4593850671176,247.879972198323,31.6213203435596)) ;
#80560 = CARTESIAN_POINT('Ctrl Pts',(49.4886840834143,248.002844395605,31.6213203435596)) ;
#80561 = CARTESIAN_POINT('Ctrl Pts',(49.5253667039704,248.096548590802,31.6213203435596)) ;
#80562 = CARTESIAN_POINT('Ctrl Pts',(49.5847592850748,248.203341158271,31.6213203435596)) ;
#80563 = CARTESIAN_POINT('Ctrl Pts',(49.6579185843663,248.296995382265,31.6213203435596)) ;
#80564 = CARTESIAN_POINT('Ctrl Pts',(49.7010531372608,248.352839039806,31.6213203435596)) ;
#80565 = CARTESIAN_POINT('Ctrl Pts',(49.4714537670856,247.682687695253,31.6213203435596)) ;
#80566 = CARTESIAN_POINT('Ctrl Pts',(49.4772012130244,247.755355605436,31.6213203435596)) ;
#80567 = CARTESIAN_POINT('Ctrl Pts',(49.4862294221888,247.876752186485,31.6213203435596)) ;
#80568 = CARTESIAN_POINT('Ctrl Pts',(49.5146718619417,247.995378904774,31.6213203435596)) ;
#80569 = CARTESIAN_POINT('Ctrl Pts',(49.549547538703,248.084463228595,31.6213203435596)) ;
#80570 = CARTESIAN_POINT('Ctrl Pts',(49.6067817018178,248.187671186647,31.6213203435596)) ;
#80571 = CARTESIAN_POINT('Ctrl Pts',(49.6792281363268,248.280556134621,31.6213203435596)) ;
#80572 = CARTESIAN_POINT('Ctrl Pts',(49.7223606859683,248.336373859551,31.6213203435596)) ;
#80573 = CARTESIAN_POINT('',(49.6274070383127,248.40974827469,31.7413203435596)) ;
#80574 = CARTESIAN_POINT('Ctrl Pts',(49.6274070383129,248.40974827469,31.7413203435597)) ;
#80575 = CARTESIAN_POINT('Ctrl Pts',(49.5842744886713,248.353930549759,31.7413203435597)) ;
#80576 = CARTESIAN_POINT('Ctrl Pts',(49.5086086325514,248.25752820517,31.7413203435597)) ;
#80577 = CARTESIAN_POINT('Ctrl Pts',(49.4417511608872,248.138252930567,31.7413203435597)) ;
#80578 = CARTESIAN_POINT('Ctrl Pts',(49.3988727594182,248.028724139293,31.7413203435597)) ;
#80579 = CARTESIAN_POINT('Ctrl Pts',(49.3665625013471,247.891107509426,31.7413203435596)) ;
#80580 = CARTESIAN_POINT('Ctrl Pts',(49.3575747933183,247.764817090958,31.7413203435596)) ;
#80581 = CARTESIAN_POINT('Ctrl Pts',(49.3518273473795,247.692149180776,31.7413203435596)) ;
#80582 = CARTESIAN_POINT('Ctrl Pts',(49.7134632100808,248.324868293052,31.6213203435596)) ;
#80583 = CARTESIAN_POINT('Ctrl Pts',(49.7132559890637,248.325072106525,31.6213203435596)) ;
#80584 = CARTESIAN_POINT('Ctrl Pts',(49.7130468330129,248.325278354732,31.621321434825)) ;
#80585 = CARTESIAN_POINT('Ctrl Pts',(49.712837678588,248.325484601394,31.6213236383315)) ;
#80586 = CARTESIAN_POINT('Ctrl Pts',(49.7063180337272,248.331913607096,31.6213923248027)) ;
#80587 = CARTESIAN_POINT('Ctrl Pts',(49.6998357440119,248.338305723809,31.6225297303056)) ;
#80588 = CARTESIAN_POINT('Ctrl Pts',(49.6935146400323,248.344538332334,31.6246496199846)) ;
#80589 = CARTESIAN_POINT('Ctrl Pts',(49.6886750426664,248.349310175338,31.6262726612349)) ;
#80590 = CARTESIAN_POINT('Ctrl Pts',(49.6839295209328,248.353988818993,31.628472662309)) ;
#80591 = CARTESIAN_POINT('Ctrl Pts',(49.6793363545858,248.358517816042,31.6312289392204)) ;
#80592 = CARTESIAN_POINT('Ctrl Pts',(49.6733673312916,248.364403448488,31.6348108432593)) ;
#80593 = CARTESIAN_POINT('Ctrl Pts',(49.6677194483372,248.36997314875,31.6392916211414)) ;
#80594 = CARTESIAN_POINT('Ctrl Pts',(49.6625123775627,248.375115188156,31.6446092618829)) ;
#80595 = CARTESIAN_POINT('Ctrl Pts',(49.6615906227216,248.376025431155,31.6455505898019)) ;
#80596 = CARTESIAN_POINT('Ctrl Pts',(49.6606827178263,248.376922252148,31.6465182725826)) ;
#80597 = CARTESIAN_POINT('Ctrl Pts',(49.6597893874932,248.377804993748,31.647512135677)) ;
#80598 = CARTESIAN_POINT('Ctrl Pts',(49.6597891089285,248.377805269011,31.6475124455905)) ;
#80599 = CARTESIAN_POINT('Ctrl Pts',(49.6597888303653,248.377805544272,31.6475127555065)) ;
#80600 = CARTESIAN_POINT('Ctrl Pts',(49.6597885518034,248.377805819532,31.6475130654251)) ;
#80601 = CARTESIAN_POINT('Ctrl Pts',(49.657032152052,248.380529548023,31.6505797438691)) ;
#80602 = CARTESIAN_POINT('Ctrl Pts',(49.6544141961377,248.383119520525,31.6538954477906)) ;
#80603 = CARTESIAN_POINT('Ctrl Pts',(49.6519440230935,248.385564616432,31.6574398704136)) ;
#80604 = CARTESIAN_POINT('Ctrl Pts',(49.647394880906,248.390067575838,31.6639673817243)) ;
#80605 = CARTESIAN_POINT('Ctrl Pts',(49.6433948408339,248.39403132537,31.6711969715355)) ;
#80606 = CARTESIAN_POINT('Ctrl Pts',(49.6400004957735,248.397389763697,31.6789765359587)) ;
#80607 = CARTESIAN_POINT('Ctrl Pts',(49.6376234961975,248.399741618425,31.6844244267906)) ;
#80608 = CARTESIAN_POINT('Ctrl Pts',(49.6355443643873,248.401795839926,31.6901429783145)) ;
#80609 = CARTESIAN_POINT('Ctrl Pts',(49.633795270634,248.403518871082,31.6960817822648)) ;
#80610 = CARTESIAN_POINT('Ctrl Pts',(49.6320218954418,248.405265821869,31.7021030304553)) ;
#80611 = CARTESIAN_POINT('Ctrl Pts',(49.630602327527,248.406657503578,31.7083012694437)) ;
#80612 = CARTESIAN_POINT('Ctrl Pts',(49.6295626123056,248.407669693824,31.7146126499384)) ;
#80613 = CARTESIAN_POINT('Ctrl Pts',(49.6291545699323,248.408066933859,31.7170895884534)) ;
#80614 = CARTESIAN_POINT('Ctrl Pts',(49.6288050733612,248.408405673376,31.7195840029885)) ;
#80615 = CARTESIAN_POINT('Ctrl Pts',(49.6285134696779,248.408687250091,31.7220909516336)) ;
#80616 = CARTESIAN_POINT('Ctrl Pts',(49.6277755257932,248.409399819331,31.7284351356344)) ;
#80617 = CARTESIAN_POINT('Ctrl Pts',(49.6274070383132,248.40974827469,31.7348594076613)) ;
#80618 = CARTESIAN_POINT('Ctrl Pts',(49.6274070383132,248.40974827469,31.7413203435596)) ;
#80619 = CARTESIAN_POINT('Ctrl Pts',(49.6274070383123,248.409748274689,31.7413203435596)) ;
#80620 = CARTESIAN_POINT('Ctrl Pts',(49.7312574008403,248.49230944133,31.7413203435596)) ;
#80621 = CARTESIAN_POINT('Ctrl Pts',(49.8396524076077,248.582427489684,31.7413203435597)) ;
#80622 = CARTESIAN_POINT('Ctrl Pts',(50.1474076999394,248.729045342162,31.7413203435597)) ;
#80623 = CARTESIAN_POINT('Ctrl Pts',(50.3192350498477,248.753191697813,31.7413203435597)) ;
#80624 = CARTESIAN_POINT('Ctrl Pts',(50.5991697276986,248.801611100965,31.7413203435596)) ;
#80625 = CARTESIAN_POINT('Ctrl Pts',(50.7212519229577,248.822096521034,31.7413203435596)) ;
#80626 = CARTESIAN_POINT('Ctrl Pts',(50.8433217843682,248.842867149778,31.7413203435596)) ;
#80627 = CARTESIAN_POINT('Ctrl Pts',(49.6274070383123,248.409748274689,31.7323443645494)) ;
#80628 = CARTESIAN_POINT('Ctrl Pts',(49.7312574008403,248.49230944133,31.7323443645494)) ;
#80629 = CARTESIAN_POINT('Ctrl Pts',(49.8396524076077,248.582427489684,31.7323443645494)) ;
#80630 = CARTESIAN_POINT('Ctrl Pts',(50.1474076999394,248.729045342162,31.7323443645494)) ;
#80631 = CARTESIAN_POINT('Ctrl Pts',(50.3192350498477,248.753191697813,31.7323443645494)) ;
#80632 = CARTESIAN_POINT('Ctrl Pts',(50.5991697276986,248.801611100965,31.7323443645494)) ;
#80633 = CARTESIAN_POINT('Ctrl Pts',(50.7212519229577,248.822096521034,31.7323443645494)) ;
#80634 = CARTESIAN_POINT('Ctrl Pts',(50.8433217843682,248.842867149778,31.7323443645494)) ;
#80635 = CARTESIAN_POINT('Ctrl Pts',(49.6298309197071,248.406699372017,31.6964046663919)) ;
#80636 = CARTESIAN_POINT('Ctrl Pts',(49.7337722606661,248.489158151831,31.6964046663919)) ;
#80637 = CARTESIAN_POINT('Ctrl Pts',(49.8419061460976,248.579207835096,31.6964046663919)) ;
#80638 = CARTESIAN_POINT('Ctrl Pts',(50.1484057708637,248.72514366954,31.6964046663919)) ;
#80639 = CARTESIAN_POINT('Ctrl Pts',(50.3199044061097,248.749301688654,31.6964046663919)) ;
#80640 = CARTESIAN_POINT('Ctrl Pts',(50.599825132755,248.797797189828,31.6964046663919)) ;
#80641 = CARTESIAN_POINT('Ctrl Pts',(50.7219148934239,248.818219204104,31.6964046663919)) ;
#80642 = CARTESIAN_POINT('Ctrl Pts',(50.8439751417561,248.839027340845,31.6964046663919)) ;
#80643 = CARTESIAN_POINT('Ctrl Pts',(49.6518601569296,248.378989682767,31.6401779597124)) ;
#80644 = CARTESIAN_POINT('Ctrl Pts',(49.7557604408709,248.461494668013,31.6401779597124)) ;
#80645 = CARTESIAN_POINT('Ctrl Pts',(49.8625658822425,248.549845910284,31.6401779597124)) ;
#80646 = CARTESIAN_POINT('Ctrl Pts',(50.1569996132661,248.690088864524,31.6401779597124)) ;
#80647 = CARTESIAN_POINT('Ctrl Pts',(50.3258240494323,248.714502474362,31.6401779597124)) ;
#80648 = CARTESIAN_POINT('Ctrl Pts',(50.6057825093676,248.762849060457,31.6401779597124)) ;
#80649 = CARTESIAN_POINT('Ctrl Pts',(50.7278485375342,248.783338358162,31.6401779597124)) ;
#80650 = CARTESIAN_POINT('Ctrl Pts',(50.8499131240851,248.804129568182,31.6401779597124)) ;
#80651 = CARTESIAN_POINT('Ctrl Pts',(49.6853263616349,248.336893893275,31.6213203435596)) ;
#80652 = CARTESIAN_POINT('Ctrl Pts',(49.7892736755946,248.419345951094,31.6213203435596)) ;
#80653 = CARTESIAN_POINT('Ctrl Pts',(49.8939292891865,248.505252742644,31.6213203435596)) ;
#80654 = CARTESIAN_POINT('Ctrl Pts',(50.1701152721836,248.636783501172,31.6213203435597)) ;
#80655 = CARTESIAN_POINT('Ctrl Pts',(50.3348376474163,248.661566541191,31.6213203435596)) ;
#80656 = CARTESIAN_POINT('Ctrl Pts',(50.6148326914291,248.709792850834,31.6213203435596)) ;
#80657 = CARTESIAN_POINT('Ctrl Pts',(50.736874324539,248.730303242972,31.6213203435596)) ;
#80658 = CARTESIAN_POINT('Ctrl Pts',(50.8589339417444,248.751113842222,31.6213203435596)) ;
#80659 = CARTESIAN_POINT('Ctrl Pts',(49.7020837842334,248.315815407073,31.6213203435596)) ;
#80660 = CARTESIAN_POINT('Ctrl Pts',(49.8059341467614,248.398376573714,31.6213203435596)) ;
#80661 = CARTESIAN_POINT('Ctrl Pts',(49.9096583356794,248.482909816866,31.6213203435596)) ;
#80662 = CARTESIAN_POINT('Ctrl Pts',(50.1766164005556,248.610148341557,31.6213203435597)) ;
#80663 = CARTESIAN_POINT('Ctrl Pts',(50.339328262466,248.63513713406,31.6213203435596)) ;
#80664 = CARTESIAN_POINT('Ctrl Pts',(50.6193644682054,248.68318651908,31.6213203435596)) ;
#80665 = CARTESIAN_POINT('Ctrl Pts',(50.7413810446874,248.703796823408,31.6213203435596)) ;
#80666 = CARTESIAN_POINT('Ctrl Pts',(50.863450906098,248.724567452152,31.6213203435596)) ;
#80667 = CARTESIAN_POINT('',(50.4787115899697,248.780775843391,31.7413203435597)) ;
#80668 = CARTESIAN_POINT('Ctrl Pts',(50.4787115899697,248.780775843391,31.7413203435597)) ;
#80669 = CARTESIAN_POINT('Ctrl Pts',(50.3192144841703,248.75318880758,31.7413203435597)) ;
#80670 = CARTESIAN_POINT('Ctrl Pts',(50.1473975700188,248.729040516162,31.7413203435597)) ;
#80671 = CARTESIAN_POINT('Ctrl Pts',(49.8396524076077,248.582427489684,31.7413203435597)) ;
#80672 = CARTESIAN_POINT('Ctrl Pts',(49.7312574008403,248.49230944133,31.7413203435596)) ;
#80673 = CARTESIAN_POINT('Ctrl Pts',(49.6274070383123,248.409748274689,31.7413203435596)) ;
#80674 = CARTESIAN_POINT('Ctrl Pts',(50.8634509060979,248.724567452152,31.6213203435596)) ;
#80675 = CARTESIAN_POINT('Ctrl Pts',(50.8626007665065,248.724691643753,31.6213203435596)) ;
#80676 = CARTESIAN_POINT('Ctrl Pts',(50.8617506188712,248.724815832774,31.6213212569625)) ;
#80677 = CARTESIAN_POINT('Ctrl Pts',(50.7857444298763,248.735918471341,31.6214844105417)) ;
#80678 = CARTESIAN_POINT('Ctrl Pts',(50.7110413428426,248.746835358112,31.6287307234378)) ;
#80679 = CARTESIAN_POINT('Ctrl Pts',(50.5933441727746,248.764125424106,31.6532575437195)) ;
#80680 = CARTESIAN_POINT('Ctrl Pts',(50.5540600843127,248.769941046334,31.6679370990345)) ;
#80681 = CARTESIAN_POINT('Ctrl Pts',(50.5153142312762,248.775614320839,31.6899900308231)) ;
#80682 = CARTESIAN_POINT('Ctrl Pts',(50.5011451295166,248.777681686943,31.6993930061635)) ;
#80683 = CARTESIAN_POINT('Ctrl Pts',(50.4874117295432,248.77962254954,31.7157669263666)) ;
#80684 = CARTESIAN_POINT('Ctrl Pts',(50.4841511122824,248.780071069011,31.7207255508811)) ;
#80685 = CARTESIAN_POINT('Ctrl Pts',(50.4799059585844,248.780643053467,31.7309912272279)) ;
#80686 = CARTESIAN_POINT('Ctrl Pts',(50.4787822579947,248.780788066527,31.7360662774667)) ;
#80687 = CARTESIAN_POINT('Ctrl Pts',(50.4787822579947,248.780788066527,31.7413203435596)) ;
#80688 = CARTESIAN_POINT('Ctrl Pts',(50.8102927712973,248.61698393713,31.7413203435596)) ;
#80689 = CARTESIAN_POINT('Ctrl Pts',(50.6997202412544,248.67161897537,31.7413203435596)) ;
#80690 = CARTESIAN_POINT('Ctrl Pts',(50.5890955276099,248.726159041176,31.7413203435596)) ;
#80691 = CARTESIAN_POINT('Ctrl Pts',(50.4199680949566,248.80991384992,31.7413203435596)) ;
#80692 = CARTESIAN_POINT('Ctrl Pts',(50.3572873056676,248.840130404076,31.7413203435596)) ;
#80693 = CARTESIAN_POINT('Ctrl Pts',(50.2435365148802,248.91361297365,31.7413203435596)) ;
#80694 = CARTESIAN_POINT('Ctrl Pts',(50.200394038611,248.947930936924,31.7413203435596)) ;
#80695 = CARTESIAN_POINT('Ctrl Pts',(50.1594670058306,248.980007368928,31.7413203435596)) ;
#80696 = CARTESIAN_POINT('Ctrl Pts',(50.8102927712973,248.61698393713,31.7054164275186)) ;
#80697 = CARTESIAN_POINT('Ctrl Pts',(50.6997202412544,248.67161897537,31.7054164275186)) ;
#80698 = CARTESIAN_POINT('Ctrl Pts',(50.5890955276099,248.726159041176,31.7054164275186)) ;
#80699 = CARTESIAN_POINT('Ctrl Pts',(50.4199680949566,248.80991384992,31.7054164275186)) ;
#80700 = CARTESIAN_POINT('Ctrl Pts',(50.3572873056676,248.840130404076,31.7054164275186)) ;
#80701 = CARTESIAN_POINT('Ctrl Pts',(50.2435365148802,248.91361297365,31.7054164275186)) ;
#80702 = CARTESIAN_POINT('Ctrl Pts',(50.200394038611,248.947930936924,31.7054164275186)) ;
#80703 = CARTESIAN_POINT('Ctrl Pts',(50.1594670058306,248.980007368928,31.7054164275186)) ;
#80704 = CARTESIAN_POINT('Ctrl Pts',(50.8236526539486,248.644022190848,31.6432843149836)) ;
#80705 = CARTESIAN_POINT('Ctrl Pts',(50.7130834685387,248.698667433839,31.6432843149836)) ;
#80706 = CARTESIAN_POINT('Ctrl Pts',(50.6024674717828,248.753214385732,31.6432843149835)) ;
#80707 = CARTESIAN_POINT('Ctrl Pts',(50.4333332648237,248.836947603607,31.6432843149835)) ;
#80708 = CARTESIAN_POINT('Ctrl Pts',(50.3715718870589,248.866830519993,31.6432843149835)) ;
#80709 = CARTESIAN_POINT('Ctrl Pts',(50.2615666635795,248.937859766662,31.6432843149835)) ;
#80710 = CARTESIAN_POINT('Ctrl Pts',(50.2190256737229,248.97169349187,31.6432843149835)) ;
#80711 = CARTESIAN_POINT('Ctrl Pts',(50.1780708772915,249.003744462163,31.6432843149835)) ;
#80712 = CARTESIAN_POINT('Ctrl Pts',(50.8515222485431,248.700425767835,31.6213203435597)) ;
#80713 = CARTESIAN_POINT('Ctrl Pts',(50.7409516914641,248.755066825751,31.6213203435597)) ;
#80714 = CARTESIAN_POINT('Ctrl Pts',(50.6303493540251,248.809644240723,31.6213203435596)) ;
#80715 = CARTESIAN_POINT('Ctrl Pts',(50.4612001281632,248.89332970846,31.6213203435596)) ;
#80716 = CARTESIAN_POINT('Ctrl Pts',(50.401338053989,248.922482324456,31.6213203435596)) ;
#80717 = CARTESIAN_POINT('Ctrl Pts',(50.2991824066269,248.988460164396,31.6213203435596)) ;
#80718 = CARTESIAN_POINT('Ctrl Pts',(50.2578231879838,249.021200188683,31.6213203435596)) ;
#80719 = CARTESIAN_POINT('Ctrl Pts',(50.2168797777163,249.053261601091,31.6213203435596)) ;
#80720 = CARTESIAN_POINT('Ctrl Pts',(50.8634509060979,248.724567452152,31.6213203435597)) ;
#80721 = CARTESIAN_POINT('Ctrl Pts',(50.752878376055,248.779202490392,31.6213203435597)) ;
#80722 = CARTESIAN_POINT('Ctrl Pts',(50.6422811339546,248.833795616323,31.6213203435596)) ;
#80723 = CARTESIAN_POINT('Ctrl Pts',(50.4731253324676,248.917460196317,31.6213203435596)) ;
#80724 = CARTESIAN_POINT('Ctrl Pts',(50.4140730966128,248.946294536072,31.6213203435596)) ;
#80725 = CARTESIAN_POINT('Ctrl Pts',(50.3152831890075,249.010121308417,31.6213203435596)) ;
#80726 = CARTESIAN_POINT('Ctrl Pts',(50.2744176758496,249.042379341516,31.6213203435596)) ;
#80727 = CARTESIAN_POINT('Ctrl Pts',(50.2334906430692,249.07445577352,31.6213203435596)) ;
#80728 = CARTESIAN_POINT('',(50.1594670058306,248.980007368928,31.7413203435597)) ;
#80729 = CARTESIAN_POINT('Ctrl Pts',(50.1594670058306,248.980007368928,31.7413203435596)) ;
#80730 = CARTESIAN_POINT('Ctrl Pts',(50.200394038611,248.947930936924,31.7413203435596)) ;
#80731 = CARTESIAN_POINT('Ctrl Pts',(50.2435365148802,248.91361297365,31.7413203435596)) ;
#80732 = CARTESIAN_POINT('Ctrl Pts',(50.3572882948742,248.840129765052,31.7413203435596)) ;
#80733 = CARTESIAN_POINT('Ctrl Pts',(50.4199700498958,248.809912907504,31.7413203435596)) ;
#80734 = CARTESIAN_POINT('Ctrl Pts',(50.4787034919505,248.780827072781,31.7413203435596)) ;
#80735 = CARTESIAN_POINT('Ctrl Pts',(50.2391706755516,249.070003231659,31.6213203435618)) ;
#80736 = CARTESIAN_POINT('Ctrl Pts',(50.2389769980947,249.069784524285,31.6213203453679)) ;
#80737 = CARTESIAN_POINT('Ctrl Pts',(50.2387833183675,249.069565814233,31.6213214511405)) ;
#80738 = CARTESIAN_POINT('Ctrl Pts',(50.238589640211,249.0693471058,31.6213236583075)) ;
#80739 = CARTESIAN_POINT('Ctrl Pts',(50.2325500741904,249.062527007738,31.6213924855366)) ;
#80740 = CARTESIAN_POINT('Ctrl Pts',(50.2265461170565,249.055746946487,31.6225272947468)) ;
#80741 = CARTESIAN_POINT('Ctrl Pts',(50.2206919611659,249.049135822006,31.6246433236309)) ;
#80742 = CARTESIAN_POINT('Ctrl Pts',(50.2163057580144,249.044182463132,31.6262287499046)) ;
#80743 = CARTESIAN_POINT('Ctrl Pts',(50.2120033490246,249.039323554314,31.6283662815162)) ;
#80744 = CARTESIAN_POINT('Ctrl Pts',(50.2078355499091,249.034616864949,31.6310388202893)) ;
#80745 = CARTESIAN_POINT('Ctrl Pts',(50.202281776799,249.028344997206,31.6346000941325)) ;
#80746 = CARTESIAN_POINT('Ctrl Pts',(50.19702779249,249.02241192312,31.6390704274001)) ;
#80747 = CARTESIAN_POINT('Ctrl Pts',(50.1921876023166,249.016948821135,31.6443896684161)) ;
#80748 = CARTESIAN_POINT('Ctrl Pts',(50.1912650232226,249.01590751005,31.6454035584456)) ;
#80749 = CARTESIAN_POINT('Ctrl Pts',(50.1903575198512,249.014883327718,31.6464484265654)) ;
#80750 = CARTESIAN_POINT('Ctrl Pts',(50.1894659542635,249.013877275703,31.6475240412048)) ;
#80751 = CARTESIAN_POINT('Ctrl Pts',(50.1869901882417,249.011083595204,31.6505108884023)) ;
#80752 = CARTESIAN_POINT('Ctrl Pts',(50.1846371791155,249.008429537609,31.6537346511774)) ;
#80753 = CARTESIAN_POINT('Ctrl Pts',(50.1824152135107,249.00592359253,31.657173440575)) ;
#80754 = CARTESIAN_POINT('Ctrl Pts',(50.1781917651573,249.001160364154,31.6637097926173)) ;
#80755 = CARTESIAN_POINT('Ctrl Pts',(50.1744871031225,248.996983069825,31.6709481856542)) ;
#80756 = CARTESIAN_POINT('Ctrl Pts',(50.171343329535,248.99343577979,31.6787187785384)) ;
#80757 = CARTESIAN_POINT('Ctrl Pts',(50.1691228001679,248.99093023622,31.6842073511783)) ;
#80758 = CARTESIAN_POINT('Ctrl Pts',(50.1671824809342,248.988739496791,31.6899625615029)) ;
#80759 = CARTESIAN_POINT('Ctrl Pts',(50.1655454659138,248.986889652768,31.6959327580786)) ;
#80760 = CARTESIAN_POINT('Ctrl Pts',(50.1632490573667,248.984294687192,31.7043077639729)) ;
#80761 = CARTESIAN_POINT('Ctrl Pts',(50.1615738177969,248.9823977985,31.7130122682104)) ;
#80762 = CARTESIAN_POINT('Ctrl Pts',(50.1605681194369,248.981257369768,31.7218950515951)) ;
#80763 = CARTESIAN_POINT('Ctrl Pts',(50.1598435441663,248.980435725336,31.7282948285366)) ;
#80764 = CARTESIAN_POINT('Ctrl Pts',(50.1594670058305,248.980007368928,31.7347878978623)) ;
#80765 = CARTESIAN_POINT('Ctrl Pts',(50.1594670058305,248.980007368928,31.7413203435596)) ;
#80766 = CARTESIAN_POINT('Ctrl Pts',(50.1594670058305,248.980007368928,31.7413203435596)) ;
#80767 = CARTESIAN_POINT('Ctrl Pts',(50.0843680110922,249.055035615032,31.7413203435596)) ;
#80768 = CARTESIAN_POINT('Ctrl Pts',(50.0065782182602,249.132219046747,31.7413203435596)) ;
#80769 = CARTESIAN_POINT('Ctrl Pts',(49.8534401351876,249.315445306648,31.7413203435596)) ;
#80770 = CARTESIAN_POINT('Ctrl Pts',(49.7859212949379,249.415459142134,31.7413203435596)) ;
#80771 = CARTESIAN_POINT('Ctrl Pts',(49.7201766015107,249.512067336446,31.7413203435596)) ;
#80772 = CARTESIAN_POINT('Ctrl Pts',(50.1594670058305,248.980007368928,31.7054164275186)) ;
#80773 = CARTESIAN_POINT('Ctrl Pts',(50.0843680110922,249.055035615032,31.7054164275186)) ;
#80774 = CARTESIAN_POINT('Ctrl Pts',(50.0065782182602,249.132219046747,31.7054164275186)) ;
#80775 = CARTESIAN_POINT('Ctrl Pts',(49.8534401351876,249.315445306648,31.7054164275186)) ;
#80776 = CARTESIAN_POINT('Ctrl Pts',(49.7859212949379,249.415459142134,31.7054164275186)) ;
#80777 = CARTESIAN_POINT('Ctrl Pts',(49.7201766015107,249.512067336446,31.7054164275186)) ;
#80778 = CARTESIAN_POINT('Ctrl Pts',(50.1807824490313,249.001342911739,31.6432843125428)) ;
#80779 = CARTESIAN_POINT('Ctrl Pts',(50.1057005592276,249.076389407655,31.6432843125428)) ;
#80780 = CARTESIAN_POINT('Ctrl Pts',(50.0285181687661,249.153000953896,31.6432843125428)) ;
#80781 = CARTESIAN_POINT('Ctrl Pts',(49.8779076504796,249.333206669877,31.6432843125428)) ;
#80782 = CARTESIAN_POINT('Ctrl Pts',(49.8108769739463,249.432442440653,31.6432843125428)) ;
#80783 = CARTESIAN_POINT('Ctrl Pts',(49.7451095799621,249.529034955354,31.6432843125428)) ;
#80784 = CARTESIAN_POINT('Ctrl Pts',(50.2252478710253,249.045850262847,31.6213203435596)) ;
#80785 = CARTESIAN_POINT('Ctrl Pts',(50.1501589665769,249.12088927461,31.6213203435596)) ;
#80786 = CARTESIAN_POINT('Ctrl Pts',(50.0742782369067,249.19635189491,31.6213203435596)) ;
#80787 = CARTESIAN_POINT('Ctrl Pts',(49.9289401473877,249.370244565953,31.6213203435596)) ;
#80788 = CARTESIAN_POINT('Ctrl Pts',(49.8628795039616,249.467831583956,31.6213203435596)) ;
#80789 = CARTESIAN_POINT('Ctrl Pts',(49.7971214193578,249.564430528784,31.6213203435596)) ;
#80790 = CARTESIAN_POINT('Ctrl Pts',(50.2442798226044,249.064900160794,31.6213203435596)) ;
#80791 = CARTESIAN_POINT('Ctrl Pts',(50.1691808278661,249.139928406899,31.6213203435596)) ;
#80792 = CARTESIAN_POINT('Ctrl Pts',(50.0938629713761,249.214906582534,31.6213203435596)) ;
#80793 = CARTESIAN_POINT('Ctrl Pts',(49.9507815308594,249.386095173166,31.6213203435596)) ;
#80794 = CARTESIAN_POINT('Ctrl Pts',(49.8851280584615,249.482972237687,31.6213203435596)) ;
#80795 = CARTESIAN_POINT('Ctrl Pts',(49.8193833650344,249.579580431999,31.6213203435596)) ;
#80796 = CARTESIAN_POINT('Ctrl Pts',(49.7201766015108,249.512067336446,31.7413203435596)) ;
#80797 = CARTESIAN_POINT('Ctrl Pts',(49.7412297546283,249.481130891218,31.7413203435596)) ;
#80798 = CARTESIAN_POINT('Ctrl Pts',(49.7624973652352,249.449872249108,31.7413203435596)) ;
#80799 = CARTESIAN_POINT('Ctrl Pts',(49.7842924699231,249.41849608269,31.7413203435596)) ;
#80800 = CARTESIAN_POINT('Ctrl Pts',(49.8052631549654,249.388306748287,31.7413203435596)) ;
#80801 = CARTESIAN_POINT('Ctrl Pts',(49.8267219102803,249.358008385841,31.7413203435596)) ;
#80802 = CARTESIAN_POINT('Ctrl Pts',(49.8489842023975,249.327813735828,31.7413203435596)) ;
#80803 = CARTESIAN_POINT('Ctrl Pts',(49.8624112513967,249.309602446394,31.7413203435596)) ;
#80804 = CARTESIAN_POINT('Ctrl Pts',(49.8761313232906,249.291429485407,31.7413203435596)) ;
#80805 = CARTESIAN_POINT('Ctrl Pts',(49.8902211372196,249.273347763522,31.7413203435596)) ;
#80806 = CARTESIAN_POINT('Ctrl Pts',(49.8972660441841,249.264306902579,31.7413203435596)) ;
#80807 = CARTESIAN_POINT('Ctrl Pts',(49.9044034808366,249.25528892965,31.7413203435596)) ;
#80808 = CARTESIAN_POINT('Ctrl Pts',(49.9116436307471,249.24630095175,31.7413203435596)) ;
#80809 = CARTESIAN_POINT('Ctrl Pts',(49.9156613592195,249.24131331266,31.7413203435596)) ;
#80810 = CARTESIAN_POINT('Ctrl Pts',(49.9197107244713,249.236334916271,31.7413203435596)) ;
#80811 = CARTESIAN_POINT('Ctrl Pts',(49.9237935226235,249.231367023509,31.7413203435596)) ;
#80812 = CARTESIAN_POINT('Ctrl Pts',(49.9265173803749,249.228052670777,31.7413203435596)) ;
#80813 = CARTESIAN_POINT('Ctrl Pts',(49.9292561197825,249.224742993849,31.7413203435596)) ;
#80814 = CARTESIAN_POINT('Ctrl Pts',(49.9320102844097,249.221438375634,31.7413203435596)) ;
#80815 = CARTESIAN_POINT('Ctrl Pts',(49.9325671651966,249.22077019539,31.7413203435596)) ;
#80816 = CARTESIAN_POINT('Ctrl Pts',(49.9331246769457,249.220102221623,31.7413203435596)) ;
#80817 = CARTESIAN_POINT('Ctrl Pts',(49.933682823282,249.219434458619,31.7413203435596)) ;
#80818 = CARTESIAN_POINT('Ctrl Pts',(49.9563305661004,249.192338831929,31.7413203435596)) ;
#80819 = CARTESIAN_POINT('Ctrl Pts',(49.9794784000558,249.166234661918,31.7413203435596)) ;
#80820 = CARTESIAN_POINT('Ctrl Pts',(50.0028581722231,249.140851884011,31.7413203435596)) ;
#80821 = CARTESIAN_POINT('Ctrl Pts',(50.0270883697368,249.114545822612,31.7413203435596)) ;
#80822 = CARTESIAN_POINT('Ctrl Pts',(50.0515679747535,249.089014828443,31.7413203435596)) ;
#80823 = CARTESIAN_POINT('Ctrl Pts',(50.0760422400472,249.063994621682,31.7413203435596)) ;
#80824 = CARTESIAN_POINT('Ctrl Pts',(50.1019094484869,249.037550399732,31.7413203435596)) ;
#80825 = CARTESIAN_POINT('Ctrl Pts',(50.1277709218595,249.011676953172,31.7413203435596)) ;
#80826 = CARTESIAN_POINT('Ctrl Pts',(50.1533699872708,248.986098890802,31.7413203435596)) ;
#80827 = CARTESIAN_POINT('Ctrl Pts',(50.1554040022539,248.98406654465,31.7413203435596)) ;
#80828 = CARTESIAN_POINT('Ctrl Pts',(50.1574363812323,248.982036080532,31.7413203435596)) ;
#80829 = CARTESIAN_POINT('Ctrl Pts',(50.1594670058306,248.980007368928,31.7413203435596)) ;
#80830 = CARTESIAN_POINT('Ctrl Pts',(50.4787029267366,248.780825931436,31.9213203435596)) ;
#80831 = CARTESIAN_POINT('Ctrl Pts',(50.4787029267366,248.780825931436,31.5613203435596)) ;
#80832 = CARTESIAN_POINT('Ctrl Pts',(50.4156447429845,248.811983636512,31.9213203435596)) ;
#80833 = CARTESIAN_POINT('Ctrl Pts',(50.4156447429845,248.811983636512,31.5613203435596)) ;
#80834 = CARTESIAN_POINT('Ctrl Pts',(50.3025555244799,248.867862196722,31.9213203435596)) ;
#80835 = CARTESIAN_POINT('Ctrl Pts',(50.3025555244799,248.867862196722,31.5613203435596)) ;
#80836 = CARTESIAN_POINT('Ctrl Pts',(50.2033540554537,248.945611033121,31.9213203435596)) ;
#80837 = CARTESIAN_POINT('Ctrl Pts',(50.2033540554537,248.945611033121,31.5613203435596)) ;
#80838 = CARTESIAN_POINT('Ctrl Pts',(50.1594670058306,248.980007368928,31.9213203435596)) ;
#80839 = CARTESIAN_POINT('Ctrl Pts',(50.1594670058306,248.980007368928,31.5613203435596)) ;
#80840 = CARTESIAN_POINT('',(50.1594669100106,248.980007221364,31.8013203435596)) ;
#80841 = CARTESIAN_POINT('',(50.1594670058306,248.980007368928,31.9213203435596)) ;
#80842 = CARTESIAN_POINT('',(50.4787029267368,248.780825931436,31.8013203435597)) ;
#80843 = CARTESIAN_POINT('Ctrl Pts',(50.4787029267369,248.780825931436,31.8013203435597)) ;
#80844 = CARTESIAN_POINT('Ctrl Pts',(50.4117018449641,248.813931863473,31.8013203435597)) ;
#80845 = CARTESIAN_POINT('Ctrl Pts',(50.3493334652158,248.845229869203,31.8013203435597)) ;
#80846 = CARTESIAN_POINT('Ctrl Pts',(50.2498264402701,248.909548117546,31.8013203435596)) ;
#80847 = CARTESIAN_POINT('Ctrl Pts',(50.206102738199,248.943426094878,31.8013203435597)) ;
#80848 = CARTESIAN_POINT('Ctrl Pts',(50.1594668438626,248.980007137034,31.8013203435596)) ;
#80849 = CARTESIAN_POINT('',(50.4787029267366,248.780825931436,31.9213203435596)) ;
#80850 = CARTESIAN_POINT('Ctrl Pts',(50.1594670058306,248.980007368928,31.9213203435596)) ;
#80851 = CARTESIAN_POINT('Ctrl Pts',(50.1594670058306,248.980007368928,31.5613203435596)) ;
#80852 = CARTESIAN_POINT('Ctrl Pts',(50.081681528341,249.057719566924,31.9213203435596)) ;
#80853 = CARTESIAN_POINT('Ctrl Pts',(50.081681528341,249.057719566924,31.5613203435596)) ;
#80854 = CARTESIAN_POINT('Ctrl Pts',(49.918276128975,249.220971026696,31.9213203435596)) ;
#80855 = CARTESIAN_POINT('Ctrl Pts',(49.918276128975,249.220971026696,31.5613203435596)) ;
#80856 = CARTESIAN_POINT('Ctrl Pts',(49.7882872096234,249.411982561231,31.9213203435596)) ;
#80857 = CARTESIAN_POINT('Ctrl Pts',(49.7882872096234,249.411982561231,31.5613203435596)) ;
#80858 = CARTESIAN_POINT('Ctrl Pts',(49.7201766015108,249.512067336446,31.9213203435596)) ;
#80859 = CARTESIAN_POINT('Ctrl Pts',(49.7201766015108,249.512067336446,31.5613203435596)) ;
#80860 = CARTESIAN_POINT('',(49.7201769331396,249.512066809238,31.8013203435596)) ;
#80861 = CARTESIAN_POINT('',(49.7201766015108,249.512067336446,31.9213203435596)) ;
#80862 = CARTESIAN_POINT('Ctrl Pts',(50.1594669089399,248.980007271912,31.8013203435596)) ;
#80863 = CARTESIAN_POINT('Ctrl Pts',(50.0792905779469,249.06007991241,31.8013203435597)) ;
#80864 = CARTESIAN_POINT('Ctrl Pts',(50.0018980651231,249.137814436292,31.8013203435595)) ;
#80865 = CARTESIAN_POINT('Ctrl Pts',(49.8585798215644,249.30927447749,31.8013203435596)) ;
#80866 = CARTESIAN_POINT('Ctrl Pts',(49.7903322846594,249.408934973886,31.801320343559)) ;
#80867 = CARTESIAN_POINT('Ctrl Pts',(49.7201769220531,249.512066801696,31.8013203435596)) ;
#80868 = CARTESIAN_POINT('Origin',(49.7201766015108,249.512067336446,31.9213203435596)) ;
#80869 = CARTESIAN_POINT('',(49.0244056225832,250.600744087106,31.8013203435596)) ;
#80870 = CARTESIAN_POINT('',(49.0244056225832,250.600744087106,31.9213203435596)) ;
#80871 = CARTESIAN_POINT('',(52.5952189936417,245.013472390306,31.8013203435596)) ;
#80872 = CARTESIAN_POINT('Origin',(49.0244056225832,250.600744087106,31.9213203435596)) ;
#80873 = CARTESIAN_POINT('',(49.6901629806574,250.600744087106,31.8013203435596)) ;
#80874 = CARTESIAN_POINT('',(49.6901629806574,250.600744087106,31.9213203435596)) ;
#80875 = CARTESIAN_POINT('',(51.3622028112916,250.600744087106,31.8013203435596)) ;
#80876 = CARTESIAN_POINT('Origin',(49.6901629806574,250.600744087106,31.9213203435596)) ;
#80877 = CARTESIAN_POINT('',(50.2194942475374,249.76854761303,31.8013203435596)) ;
#80878 = CARTESIAN_POINT('',(50.2194942475374,249.76854761303,31.9213203435596)) ;
#80879 = CARTESIAN_POINT('',(52.8075349928054,245.69971866274,31.8013203435596)) ;
#80880 = CARTESIAN_POINT('Ctrl Pts',(50.2194942475374,249.76854761303,31.9213203435596)) ;
#80881 = CARTESIAN_POINT('Ctrl Pts',(50.2194942475374,249.76854761303,31.5613203435596)) ;
#80882 = CARTESIAN_POINT('Ctrl Pts',(50.2886676861273,249.661674205943,31.9213203435596)) ;
#80883 = CARTESIAN_POINT('Ctrl Pts',(50.2886676861273,249.661674205943,31.5613203435596)) ;
#80884 = CARTESIAN_POINT('Ctrl Pts',(50.4101984552228,249.473908386807,31.9213203435596)) ;
#80885 = CARTESIAN_POINT('Ctrl Pts',(50.4101984552228,249.473908386807,31.5613203435596)) ;
#80886 = CARTESIAN_POINT('Ctrl Pts',(50.5438898116334,249.294625894933,31.9213203435596)) ;
#80887 = CARTESIAN_POINT('Ctrl Pts',(50.5438898116334,249.294625894933,31.5613203435596)) ;
#80888 = CARTESIAN_POINT('Ctrl Pts',(50.6014861107882,249.217388231164,31.9213203435596)) ;
#80889 = CARTESIAN_POINT('Ctrl Pts',(50.6014861107882,249.217388231164,31.5613203435596)) ;
#80890 = CARTESIAN_POINT('',(50.6014861107881,249.217388231164,31.8013203435596)) ;
#80891 = CARTESIAN_POINT('',(50.6014861107882,249.217388231164,31.9213203435596)) ;
#80892 = CARTESIAN_POINT('Ctrl Pts',(50.2194942475855,249.768547612949,31.8013203435596)) ;
#80893 = CARTESIAN_POINT('Ctrl Pts',(50.2878275213723,249.662972234484,31.8013203435596)) ;
#80894 = CARTESIAN_POINT('Ctrl Pts',(50.3569258709686,249.556106723648,31.8013203435596)) ;
#80895 = CARTESIAN_POINT('Ctrl Pts',(50.4869845254695,249.370877841352,31.8013203435597)) ;
#80896 = CARTESIAN_POINT('Ctrl Pts',(50.5445853180999,249.293693208364,31.8013203435597)) ;
#80897 = CARTESIAN_POINT('Ctrl Pts',(50.6014861107882,249.217388231164,31.8013203435597)) ;
#80898 = CARTESIAN_POINT('Ctrl Pts',(50.6014861107882,249.217388231164,31.9213203435596)) ;
#80899 = CARTESIAN_POINT('Ctrl Pts',(50.6014861107882,249.217388231164,31.5613203435596)) ;
#80900 = CARTESIAN_POINT('Ctrl Pts',(50.6467206773926,249.160912010444,31.9213203435596)) ;
#80901 = CARTESIAN_POINT('Ctrl Pts',(50.6467206773926,249.160912010444,31.5613203435596)) ;
#80902 = CARTESIAN_POINT('Ctrl Pts',(50.7265515411586,249.061241651674,31.9213203435596)) ;
#80903 = CARTESIAN_POINT('Ctrl Pts',(50.7265515411586,249.061241651674,31.5613203435596)) ;
#80904 = CARTESIAN_POINT('Ctrl Pts',(50.8277518319035,248.983628817758,31.9213203435596)) ;
#80905 = CARTESIAN_POINT('Ctrl Pts',(50.8277518319035,248.983628817758,31.5613203435596)) ;
#80906 = CARTESIAN_POINT('Ctrl Pts',(50.8716089964922,248.949993748075,31.9213203435596)) ;
#80907 = CARTESIAN_POINT('Ctrl Pts',(50.8716089964922,248.949993748075,31.5613203435596)) ;
#80908 = CARTESIAN_POINT('',(50.8716089964922,248.949993748075,31.8013203435596)) ;
#80909 = CARTESIAN_POINT('',(50.8716089964922,248.949993748075,31.9213203435596)) ;
#80910 = CARTESIAN_POINT('Ctrl Pts',(50.6014861107882,249.217388231164,31.8013203435596)) ;
#80911 = CARTESIAN_POINT('Ctrl Pts',(50.6431307164356,249.165394145294,31.8013203435596)) ;
#80912 = CARTESIAN_POINT('Ctrl Pts',(50.6869793943593,249.109198386675,31.8013203435596)) ;
#80913 = CARTESIAN_POINT('Ctrl Pts',(50.7876909072677,249.01365071099,31.8013203435596)) ;
#80914 = CARTESIAN_POINT('Ctrl Pts',(50.8311952099577,248.980988011817,31.8013203435596)) ;
#80915 = CARTESIAN_POINT('Ctrl Pts',(50.8716089964922,248.949993748075,31.8013203435596)) ;
#80916 = CARTESIAN_POINT('Ctrl Pts',(50.8716089964922,248.949993748075,31.9213203435596)) ;
#80917 = CARTESIAN_POINT('Ctrl Pts',(50.8716089964922,248.949993748075,31.5613203435596)) ;
#80918 = CARTESIAN_POINT('Ctrl Pts',(50.9103827599137,248.926600394466,31.9213203435596)) ;
#80919 = CARTESIAN_POINT('Ctrl Pts',(50.9103827599137,248.926600394466,31.5613203435596)) ;
#80920 = CARTESIAN_POINT('Ctrl Pts',(50.9859582056058,248.881003501896,31.9213203435596)) ;
#80921 = CARTESIAN_POINT('Ctrl Pts',(50.9859582056058,248.881003501896,31.5613203435596)) ;
#80922 = CARTESIAN_POINT('Ctrl Pts',(51.0705337876061,248.855836848551,31.9213203435596)) ;
#80923 = CARTESIAN_POINT('Ctrl Pts',(51.0705337876061,248.855836848551,31.5613203435596)) ;
#80924 = CARTESIAN_POINT('Ctrl Pts',(51.1117181123312,248.84358187378,31.9213203435596)) ;
#80925 = CARTESIAN_POINT('Ctrl Pts',(51.1117181123312,248.84358187378,31.5613203435596)) ;
#80926 = CARTESIAN_POINT('',(51.1117181123312,248.84358187378,31.8013203435596)) ;
#80927 = CARTESIAN_POINT('',(51.1117181123312,248.84358187378,31.9213203435596)) ;
#80928 = CARTESIAN_POINT('Ctrl Pts',(50.8716089964922,248.949993748075,31.8013203435596)) ;
#80929 = CARTESIAN_POINT('Ctrl Pts',(50.8812952192372,248.944149764571,31.8013203435596)) ;
#80930 = CARTESIAN_POINT('Ctrl Pts',(50.8912297604164,248.938152275578,31.8013203435596)) ;
#80931 = CARTESIAN_POINT('Ctrl Pts',(50.9015589132419,248.93203979987,31.8013203435596)) ;
#80932 = CARTESIAN_POINT('Ctrl Pts',(50.9109223604925,248.926498799091,31.8013203435596)) ;
#80933 = CARTESIAN_POINT('Ctrl Pts',(50.920609761348,248.920862580329,31.8013203435596)) ;
#80934 = CARTESIAN_POINT('Ctrl Pts',(50.9307457548408,248.915195388481,31.8013203435596)) ;
#80935 = CARTESIAN_POINT('Ctrl Pts',(50.93981037248,248.910127219561,31.8013203435596)) ;
#80936 = CARTESIAN_POINT('Ctrl Pts',(50.9492336152923,248.905033946057,31.8013203435596)) ;
#80937 = CARTESIAN_POINT('Ctrl Pts',(50.9591206958319,248.899997988403,31.8013203435596)) ;
#80938 = CARTESIAN_POINT('Ctrl Pts',(50.9640642361016,248.897480009576,31.8013203435596)) ;
#80939 = CARTESIAN_POINT('Ctrl Pts',(50.9691240113763,248.894976985261,31.8013203435596)) ;
#80940 = CARTESIAN_POINT('Ctrl Pts',(50.9743151389776,248.892503680254,31.8013203435596)) ;
#80941 = CARTESIAN_POINT('Ctrl Pts',(50.9769107027783,248.89126702775,31.8013203435596)) ;
#80942 = CARTESIAN_POINT('Ctrl Pts',(50.9795391276914,248.890037857353,31.8013203435596)) ;
#80943 = CARTESIAN_POINT('Ctrl Pts',(50.9822024529822,248.888818354254,31.8013203435596)) ;
#80944 = CARTESIAN_POINT('Ctrl Pts',(50.9838480634011,248.888064849973,31.8013203435596)) ;
#80945 = CARTESIAN_POINT('Ctrl Pts',(50.9855069998973,248.887315041046,31.8013203435596)) ;
#80946 = CARTESIAN_POINT('Ctrl Pts',(50.987179764526,248.886569490637,31.8013203435596)) ;
#80947 = CARTESIAN_POINT('Ctrl Pts',(50.9882142727061,248.886108410827,31.8013203435596)) ;
#80948 = CARTESIAN_POINT('Ctrl Pts',(50.9892540707111,248.885648960224,31.8013203435596)) ;
#80949 = CARTESIAN_POINT('Ctrl Pts',(50.9902992785986,248.885191280252,31.8013203435596)) ;
#80950 = CARTESIAN_POINT('Ctrl Pts',(51.0004197047703,248.880759705994,31.8013203435596)) ;
#80951 = CARTESIAN_POINT('Ctrl Pts',(51.0102980961467,248.876817277561,31.8013203435596)) ;
#80952 = CARTESIAN_POINT('Ctrl Pts',(51.019926996519,248.873209346358,31.8013203435596)) ;
#80953 = CARTESIAN_POINT('Ctrl Pts',(51.0307051781765,248.869170781577,31.8013203435596)) ;
#80954 = CARTESIAN_POINT('Ctrl Pts',(51.0411708920461,248.865551634723,31.8013203435596)) ;
#80955 = CARTESIAN_POINT('Ctrl Pts',(51.0513403827163,248.862195622714,31.8013203435596)) ;
#80956 = CARTESIAN_POINT('Ctrl Pts',(51.0624470976921,248.858530319303,31.8013203435596)) ;
#80957 = CARTESIAN_POINT('Ctrl Pts',(51.0732008410539,248.855179721503,31.8013203435596)) ;
#80958 = CARTESIAN_POINT('Ctrl Pts',(51.0836485698134,248.851998785607,31.8013203435596)) ;
#80959 = CARTESIAN_POINT('Ctrl Pts',(51.0932464252134,248.849076603814,31.8013203435596)) ;
#80960 = CARTESIAN_POINT('Ctrl Pts',(51.1025866694188,248.846299062984,31.8013203435596)) ;
#80961 = CARTESIAN_POINT('Ctrl Pts',(51.1117181123312,248.84358187378,31.8013203435596)) ;
#80962 = CARTESIAN_POINT('Ctrl Pts',(51.1117181123312,248.84358187378,31.9213203435596)) ;
#80963 = CARTESIAN_POINT('Ctrl Pts',(51.1117181123312,248.84358187378,31.5613203435596)) ;
#80964 = CARTESIAN_POINT('Ctrl Pts',(51.1512264477684,248.83805994343,31.9213203435596)) ;
#80965 = CARTESIAN_POINT('Ctrl Pts',(51.1512264477684,248.83805994343,31.5613203435596)) ;
#80966 = CARTESIAN_POINT('Ctrl Pts',(51.2489154900931,248.824406316121,31.9213203435596)) ;
#80967 = CARTESIAN_POINT('Ctrl Pts',(51.2489154900931,248.824406316121,31.5613203435596)) ;
#80968 = CARTESIAN_POINT('Ctrl Pts',(51.3476150025798,248.824453851025,31.9213203435596)) ;
#80969 = CARTESIAN_POINT('Ctrl Pts',(51.3476150025798,248.824453851025,31.5613203435596)) ;
#80970 = CARTESIAN_POINT('Ctrl Pts',(51.4063975156363,248.824482161408,31.9213203435596)) ;
#80971 = CARTESIAN_POINT('Ctrl Pts',(51.4063975156363,248.824482161408,31.5613203435596)) ;
#80972 = CARTESIAN_POINT('',(51.4063975156363,248.824482161408,31.8013203435597)) ;
#80973 = CARTESIAN_POINT('',(51.4063975156363,248.824482161408,31.9213203435596)) ;
#80974 = CARTESIAN_POINT('Ctrl Pts',(51.1117181123309,248.84358187378,31.8013203435596)) ;
#80975 = CARTESIAN_POINT('Ctrl Pts',(51.1489587152535,248.838376895812,31.8013203435596)) ;
#80976 = CARTESIAN_POINT('Ctrl Pts',(51.1881361258901,248.832747914847,31.8013203435596)) ;
#80977 = CARTESIAN_POINT('Ctrl Pts',(51.2926723949292,248.824120149349,31.8013203435596)) ;
#80978 = CARTESIAN_POINT('Ctrl Pts',(51.3510126858065,248.824455380393,31.8013203435596)) ;
#80979 = CARTESIAN_POINT('Ctrl Pts',(51.4063975153673,248.82448216138,31.8013203435596)) ;
#80980 = CARTESIAN_POINT('Origin',(51.4063975156363,248.824482161408,31.9213203435596)) ;
#80981 = CARTESIAN_POINT('',(52.0203128398474,248.824482161408,31.8013203435596)) ;
#80982 = CARTESIAN_POINT('',(52.0203128398474,248.824482161408,31.9213203435596)) ;
#80983 = CARTESIAN_POINT('',(52.5531987578181,248.824482161408,31.8013203435596)) ;
#80984 = CARTESIAN_POINT('Ctrl Pts',(50.3149922133507,248.292422193891,31.8013203435596)) ;
#80985 = CARTESIAN_POINT('Ctrl Pts',(50.2828566975655,248.278143008832,31.8013203435596)) ;
#80986 = CARTESIAN_POINT('Ctrl Pts',(50.2258386057601,248.25332520896,31.8013203435596)) ;
#80987 = CARTESIAN_POINT('Ctrl Pts',(50.1613818919158,248.214949841468,31.8013203435596)) ;
#80988 = CARTESIAN_POINT('Ctrl Pts',(50.0979033745595,248.164702269118,31.8013203435596)) ;
#80989 = CARTESIAN_POINT('Ctrl Pts',(50.0534676836831,248.11466854703,31.8013203435596)) ;
#80990 = CARTESIAN_POINT('Ctrl Pts',(50.0176214060562,248.069618732724,31.8013203435596)) ;
#80991 = CARTESIAN_POINT('Ctrl Pts',(50.003941798311,248.05231292904,31.8013203435596)) ;
#80992 = CARTESIAN_POINT('Ctrl Pts',(50.3149922133507,248.292422193891,31.8372242596007)) ;
#80993 = CARTESIAN_POINT('Ctrl Pts',(50.2828566975655,248.278143008832,31.8372242596007)) ;
#80994 = CARTESIAN_POINT('Ctrl Pts',(50.2258386057601,248.25332520896,31.8372242596007)) ;
#80995 = CARTESIAN_POINT('Ctrl Pts',(50.1613818919158,248.214949841468,31.8372242596007)) ;
#80996 = CARTESIAN_POINT('Ctrl Pts',(50.0979033745595,248.164702269118,31.8372242596007)) ;
#80997 = CARTESIAN_POINT('Ctrl Pts',(50.0534676836831,248.11466854703,31.8372242596007)) ;
#80998 = CARTESIAN_POINT('Ctrl Pts',(50.0176214060562,248.069618732724,31.8372242596007)) ;
#80999 = CARTESIAN_POINT('Ctrl Pts',(50.003941798311,248.05231292904,31.8372242596007)) ;
#81000 = CARTESIAN_POINT('Ctrl Pts',(50.3272385223701,248.264861695502,31.899356381536)) ;
#81001 = CARTESIAN_POINT('Ctrl Pts',(50.2950567106523,248.250556344248,31.899356381536)) ;
#81002 = CARTESIAN_POINT('Ctrl Pts',(50.2389374113449,248.226061625423,31.8993563815361)) ;
#81003 = CARTESIAN_POINT('Ctrl Pts',(50.1779829811741,248.189696416539,31.899356381536)) ;
#81004 = CARTESIAN_POINT('Ctrl Pts',(50.119312163611,248.143252734766,31.8993563815361)) ;
#81005 = CARTESIAN_POINT('Ctrl Pts',(50.0767223473644,248.09547863182,31.899356381536)) ;
#81006 = CARTESIAN_POINT('Ctrl Pts',(50.0412434526266,248.050937221671,31.8993563815361)) ;
#81007 = CARTESIAN_POINT('Ctrl Pts',(50.0276015247282,248.033610776707,31.899356381536)) ;
#81008 = CARTESIAN_POINT('Ctrl Pts',(50.3527851388875,248.207368659663,31.9213203435596)) ;
#81009 = CARTESIAN_POINT('Ctrl Pts',(50.3206223108221,248.19307403786,31.9213203435596)) ;
#81010 = CARTESIAN_POINT('Ctrl Pts',(50.2662434470315,248.169222377751,31.9213203435596)) ;
#81011 = CARTESIAN_POINT('Ctrl Pts',(50.2127147686324,248.136999504271,31.9213203435596)) ;
#81012 = CARTESIAN_POINT('Ctrl Pts',(50.1640396297653,248.098510538817,31.9213203435596)) ;
#81013 = CARTESIAN_POINT('Ctrl Pts',(50.1251782969651,248.055475583572,31.9213203435596)) ;
#81014 = CARTESIAN_POINT('Ctrl Pts',(50.0906146688733,248.011914821926,31.9213203435596)) ;
#81015 = CARTESIAN_POINT('Ctrl Pts',(50.0769572903495,247.994596840921,31.9213203435596)) ;
#81016 = CARTESIAN_POINT('Ctrl Pts',(50.3637195211995,248.182760671606,31.9213203435596)) ;
#81017 = CARTESIAN_POINT('Ctrl Pts',(50.3315840054143,248.168481486547,31.9213203435596)) ;
#81018 = CARTESIAN_POINT('Ctrl Pts',(50.277927744792,248.144899934299,31.9213203435596)) ;
#81019 = CARTESIAN_POINT('Ctrl Pts',(50.2275972966819,248.11444158417,31.9213203435596)) ;
#81020 = CARTESIAN_POINT('Ctrl Pts',(50.1831949139989,248.079360616833,31.9213203435596)) ;
#81021 = CARTESIAN_POINT('Ctrl Pts',(50.1459091564747,248.038358319183,31.9213203435596)) ;
#81022 = CARTESIAN_POINT('Ctrl Pts',(50.1117619973904,247.995204022732,31.9213203435596)) ;
#81023 = CARTESIAN_POINT('Ctrl Pts',(50.0980823896452,247.977898219048,31.9213203435596)) ;
#81024 = CARTESIAN_POINT('',(50.1042746584503,247.985728410081,31.9213203435596)) ;
#81025 = CARTESIAN_POINT('',(50.3549396358571,248.178860256982,31.9213203435596)) ;
#81026 = CARTESIAN_POINT('Ctrl Pts',(50.104281874783,247.985736529947,31.9213203435596)) ;
#81027 = CARTESIAN_POINT('Ctrl Pts',(50.1158999239824,248.000411090002,31.9213203435596)) ;
#81028 = CARTESIAN_POINT('Ctrl Pts',(50.1481620304608,248.040835753353,31.9213203435596)) ;
#81029 = CARTESIAN_POINT('Ctrl Pts',(50.1831949139989,248.079360616833,31.9213203435596)) ;
#81030 = CARTESIAN_POINT('Ctrl Pts',(50.2275972966819,248.11444158417,31.9213203435596)) ;
#81031 = CARTESIAN_POINT('Ctrl Pts',(50.2751776277953,248.143235652944,31.9213203435596)) ;
#81032 = CARTESIAN_POINT('Ctrl Pts',(50.3257302482811,248.165883905264,31.9213203435596)) ;
#81033 = CARTESIAN_POINT('Ctrl Pts',(50.3549394017728,248.178860783873,31.9213203435596)) ;
#81034 = CARTESIAN_POINT('Ctrl Pts',(50.3549344338646,248.178858576757,31.9213203435596)) ;
#81035 = CARTESIAN_POINT('Ctrl Pts',(50.3548372871676,248.179134233402,31.9213203435596)) ;
#81036 = CARTESIAN_POINT('Ctrl Pts',(50.3547401430246,248.17940989064,31.9213192415563)) ;
#81037 = CARTESIAN_POINT('Ctrl Pts',(50.3493944802537,248.194579224157,31.9211981003872)) ;
#81038 = CARTESIAN_POINT('Ctrl Pts',(50.3441572278943,248.209463608499,31.9178698499865)) ;
#81039 = CARTESIAN_POINT('Ctrl Pts',(50.3352855015944,248.234691751609,31.9066093082206)) ;
#81040 = CARTESIAN_POINT('Ctrl Pts',(50.3308425838642,248.247332713497,31.8987051026052)) ;
#81041 = CARTESIAN_POINT('Ctrl Pts',(50.3231419161368,248.269243109216,31.8753017780563)) ;
#81042 = CARTESIAN_POINT('Ctrl Pts',(50.3202611501902,248.277438595027,31.8623013765578)) ;
#81043 = CARTESIAN_POINT('Ctrl Pts',(50.3171983030722,248.286149604156,31.8408116482204)) ;
#81044 = CARTESIAN_POINT('Ctrl Pts',(50.3163832809431,248.288467128432,31.8331147727513)) ;
#81045 = CARTESIAN_POINT('Ctrl Pts',(50.3152798692463,248.291604448919,31.817383920378)) ;
#81046 = CARTESIAN_POINT('Ctrl Pts',(50.3149922133517,248.292422193891,31.8093598799402)) ;
#81047 = CARTESIAN_POINT('Ctrl Pts',(50.3149922133517,248.292422193891,31.8013203435596)) ;
#81048 = CARTESIAN_POINT('',(50.003941798311,248.05231292904,31.8013203435596)) ;
#81049 = CARTESIAN_POINT('Ctrl Pts',(50.3149922133507,248.292422193891,31.8013203435596)) ;
#81050 = CARTESIAN_POINT('Ctrl Pts',(50.2828566975655,248.278143008832,31.8013203435596)) ;
#81051 = CARTESIAN_POINT('Ctrl Pts',(50.2258386057601,248.25332520896,31.8013203435596)) ;
#81052 = CARTESIAN_POINT('Ctrl Pts',(50.1613818919158,248.214949841468,31.8013203435596)) ;
#81053 = CARTESIAN_POINT('Ctrl Pts',(50.0979033745595,248.164702269118,31.8013203435596)) ;
#81054 = CARTESIAN_POINT('Ctrl Pts',(50.0534676836831,248.11466854703,31.8013203435596)) ;
#81055 = CARTESIAN_POINT('Ctrl Pts',(50.0176214060562,248.069618732724,31.8013203435596)) ;
#81056 = CARTESIAN_POINT('Ctrl Pts',(50.003941798311,248.05231292904,31.8013203435596)) ;
#81057 = CARTESIAN_POINT('Ctrl Pts',(50.1042683656432,247.98571946673,31.9213203435596)) ;
#81058 = CARTESIAN_POINT('Ctrl Pts',(50.1040250568153,247.985881647708,31.9213203435596)) ;
#81059 = CARTESIAN_POINT('Ctrl Pts',(50.103781744389,247.986043822761,31.9213192416473)) ;
#81060 = CARTESIAN_POINT('Ctrl Pts',(50.0903945513106,247.994966336622,31.9211981310143)) ;
#81061 = CARTESIAN_POINT('Ctrl Pts',(50.0772500994751,248.003702769267,31.9178712311407)) ;
#81062 = CARTESIAN_POINT('Ctrl Pts',(50.0549619051614,248.018496492087,31.9066113625708)) ;
#81063 = CARTESIAN_POINT('Ctrl Pts',(50.0437921420014,248.025900949602,31.8987080028825)) ;
#81064 = CARTESIAN_POINT('Ctrl Pts',(50.0244291337723,248.038731400036,31.8753079726832)) ;
#81065 = CARTESIAN_POINT('Ctrl Pts',(50.0171854200934,248.043530970201,31.8623083641888)) ;
#81066 = CARTESIAN_POINT('Ctrl Pts',(50.0094860730131,248.048635324575,31.8408181867668)) ;
#81067 = CARTESIAN_POINT('Ctrl Pts',(50.0074375834509,248.04999390866,31.8331201559811)) ;
#81068 = CARTESIAN_POINT('Ctrl Pts',(50.0046645494265,248.051833330652,31.8173867221349)) ;
#81069 = CARTESIAN_POINT('Ctrl Pts',(50.0039417983113,248.05231292904,31.8093613191834)) ;
#81070 = CARTESIAN_POINT('Ctrl Pts',(50.0039417983113,248.05231292904,31.8013203435596)) ;
#81071 = CARTESIAN_POINT('Origin',(52.8601564199237,248.246092044717,31.8013203435596)) ;
#81072 = CARTESIAN_POINT('',(50.8831605673865,248.24609204701,31.9213203435596)) ;
#81073 = CARTESIAN_POINT('Ctrl Pts',(50.8825230539854,248.366092044717,31.8013203435596)) ;
#81074 = CARTESIAN_POINT('Ctrl Pts',(50.8825536510344,248.366092044717,31.8103670376983)) ;
#81075 = CARTESIAN_POINT('Ctrl Pts',(50.8825842480833,248.365064672731,31.8194133382866)) ;
#81076 = CARTESIAN_POINT('Ctrl Pts',(50.8826454342939,248.361007859405,31.8370436695514)) ;
#81077 = CARTESIAN_POINT('Ctrl Pts',(50.8826760234556,248.357979112739,31.8456270529255)) ;
#81078 = CARTESIAN_POINT('Ctrl Pts',(50.8827371951202,248.350074944028,31.8618952684662)) ;
#81079 = CARTESIAN_POINT('Ctrl Pts',(50.8827677776232,248.345200269069,31.8695795901304)) ;
#81080 = CARTESIAN_POINT('Ctrl Pts',(50.8828289657752,248.333847798996,31.8836660555295)) ;
#81081 = CARTESIAN_POINT('Ctrl Pts',(50.8828595714242,248.327369282324,31.8900666073448)) ;
#81082 = CARTESIAN_POINT('Ctrl Pts',(50.8829207658452,248.313144950304,31.9012488492717)) ;
#81083 = CARTESIAN_POINT('Ctrl Pts',(50.8829513546172,248.305400457158,31.9060309476799)) ;
#81084 = CARTESIAN_POINT('Ctrl Pts',(50.8830125480013,248.28903157296,31.9137395592428)) ;
#81085 = CARTESIAN_POINT('Ctrl Pts',(50.8830431526134,248.280407438849,31.9166647706729)) ;
#81086 = CARTESIAN_POINT('Ctrl Pts',(50.8831026946499,248.263203725675,31.9204018086563)) ;
#81087 = CARTESIAN_POINT('Ctrl Pts',(50.8831316320742,248.254648034126,31.9213203435596)) ;
#81088 = CARTESIAN_POINT('Ctrl Pts',(50.8831605694985,248.246092044717,31.9213203435596)) ;
#81089 = CARTESIAN_POINT('',(51.9003128398474,248.246092044717,31.9213203435596)) ;
#81090 = CARTESIAN_POINT('',(52.8601564199237,248.246092044717,31.9213203435596)) ;
#81091 = CARTESIAN_POINT('Origin',(51.9003128398474,248.246092044717,31.8013203435596)) ;
#81092 = CARTESIAN_POINT('Origin',(52.2271414578465,247.162763132459,31.8013203435596)) ;
#81093 = CARTESIAN_POINT('',(51.9003128398474,247.162763132459,31.9213203435596)) ;
#81094 = CARTESIAN_POINT('',(50.7555332764365,247.162763109072,31.9213203435596)) ;
#81095 = CARTESIAN_POINT('',(52.2271414578465,247.162763132459,31.9213203435596)) ;
#81096 = CARTESIAN_POINT('Ctrl Pts',(50.755533264376,247.162763097565,31.9213203435596)) ;
#81097 = CARTESIAN_POINT('Ctrl Pts',(50.7555302176641,247.162471459282,31.9213203435596)) ;
#81098 = CARTESIAN_POINT('Ctrl Pts',(50.7555271710895,247.16217982651,31.9213192375922)) ;
#81099 = CARTESIAN_POINT('Ctrl Pts',(50.7554291239828,247.152793158216,31.9212481256592)) ;
#81100 = CARTESIAN_POINT('Ctrl Pts',(50.7553349634566,247.143760542052,31.9201111028397)) ;
#81101 = CARTESIAN_POINT('Ctrl Pts',(50.7551748602209,247.128400885189,31.9164179948109)) ;
#81102 = CARTESIAN_POINT('Ctrl Pts',(50.755107856334,247.12197273855,31.9142984267547)) ;
#81103 = CARTESIAN_POINT('Ctrl Pts',(50.7549554578127,247.107355434576,31.9080931810874)) ;
#81104 = CARTESIAN_POINT('Ctrl Pts',(50.754872649644,247.099417330385,31.903622605644)) ;
#81105 = CARTESIAN_POINT('Ctrl Pts',(50.7547816212709,247.090676364211,31.8972777600414)) ;
#81106 = CARTESIAN_POINT('Ctrl Pts',(50.7547671299866,247.089284262197,31.8962188977583)) ;
#81107 = CARTESIAN_POINT('Ctrl Pts',(50.7547143583256,247.084211613134,31.892175500388)) ;
#81108 = CARTESIAN_POINT('Ctrl Pts',(50.7546777262954,247.08068424247,31.8889917050932)) ;
#81109 = CARTESIAN_POINT('Ctrl Pts',(50.7545767969812,247.070964671812,31.8791014184334)) ;
#81110 = CARTESIAN_POINT('Ctrl Pts',(50.7545184884795,247.065351409733,31.8719088167943)) ;
#81111 = CARTESIAN_POINT('Ctrl Pts',(50.7544333895888,247.05718990059,31.8586645250675)) ;
#81112 = CARTESIAN_POINT('Ctrl Pts',(50.7544023657846,247.054224758889,31.8528734817062)) ;
#81113 = CARTESIAN_POINT('Ctrl Pts',(50.7543498035961,247.049209302586,31.8407445801303)) ;
#81114 = CARTESIAN_POINT('Ctrl Pts',(50.7543286439786,247.047195500699,31.8344482431042)) ;
#81115 = CARTESIAN_POINT('Ctrl Pts',(50.754292696739,247.043739408648,31.8192922910479)) ;
#81116 = CARTESIAN_POINT('Ctrl Pts',(50.7542829156931,247.042763132459,31.8103264364301)) ;
#81117 = CARTESIAN_POINT('Ctrl Pts',(50.7542829156931,247.042763132459,31.8013203435596)) ;
#81118 = CARTESIAN_POINT('Origin',(51.9003128398474,247.162763132459,31.8013203435596)) ;
#81119 = CARTESIAN_POINT('Ctrl Pts',(50.1048968673761,247.225573558217,31.8013203435596)) ;
#81120 = CARTESIAN_POINT('Ctrl Pts',(50.1817597432473,247.178096904744,31.8013203435596)) ;
#81121 = CARTESIAN_POINT('Ctrl Pts',(50.2633538552322,247.124337723514,31.8013203435596)) ;
#81122 = CARTESIAN_POINT('Ctrl Pts',(50.4250243638207,247.069763631682,31.8013203435596)) ;
#81123 = CARTESIAN_POINT('Ctrl Pts',(50.5610592144137,247.045740326819,31.8013203435596)) ;
#81124 = CARTESIAN_POINT('Ctrl Pts',(50.683716836733,247.044233834523,31.8013203435596)) ;
#81125 = CARTESIAN_POINT('Ctrl Pts',(50.7542829156931,247.042763132459,31.8013203435596)) ;
#81126 = CARTESIAN_POINT('Ctrl Pts',(50.1048968673761,247.225573558217,31.8102963225699)) ;
#81127 = CARTESIAN_POINT('Ctrl Pts',(50.1817597432473,247.178096904744,31.8102963225699)) ;
#81128 = CARTESIAN_POINT('Ctrl Pts',(50.2633538552322,247.124337723514,31.8102963225699)) ;
#81129 = CARTESIAN_POINT('Ctrl Pts',(50.4250243638207,247.069763631682,31.8102963225699)) ;
#81130 = CARTESIAN_POINT('Ctrl Pts',(50.5610592144137,247.045740326819,31.8102963225699)) ;
#81131 = CARTESIAN_POINT('Ctrl Pts',(50.683716836733,247.044233834523,31.8102963225699)) ;
#81132 = CARTESIAN_POINT('Ctrl Pts',(50.7542829156931,247.042763132459,31.8102963225699)) ;
#81133 = CARTESIAN_POINT('Ctrl Pts',(50.106943740414,247.228887366936,31.8462360217477)) ;
#81134 = CARTESIAN_POINT('Ctrl Pts',(50.1839062014652,247.181479943549,31.8462360217477)) ;
#81135 = CARTESIAN_POINT('Ctrl Pts',(50.2652368455491,247.127832547478,31.8462360217477)) ;
#81136 = CARTESIAN_POINT('Ctrl Pts',(50.4259049939851,247.073575134911,31.8462360217477)) ;
#81137 = CARTESIAN_POINT('Ctrl Pts',(50.5613241282129,247.049677198827,31.8462360217477)) ;
#81138 = CARTESIAN_POINT('Ctrl Pts',(50.683758957624,247.048135273327,31.8462360217477)) ;
#81139 = CARTESIAN_POINT('Ctrl Pts',(50.7543640756427,247.046657285836,31.8462360217477)) ;
#81140 = CARTESIAN_POINT('Ctrl Pts',(50.125546565256,247.259004624832,31.9024627370647)) ;
#81141 = CARTESIAN_POINT('Ctrl Pts',(50.2024640642769,247.211565944533,31.9024627370647)) ;
#81142 = CARTESIAN_POINT('Ctrl Pts',(50.2824701436015,247.159314106403,31.9024627370647)) ;
#81143 = CARTESIAN_POINT('Ctrl Pts',(50.4339215284549,247.108239835495,31.9024627370647)) ;
#81144 = CARTESIAN_POINT('Ctrl Pts',(50.563506491025,247.085162762637,31.9024627370647)) ;
#81145 = CARTESIAN_POINT('Ctrl Pts',(50.6845141985273,247.083523653073,31.9024627370647)) ;
#81146 = CARTESIAN_POINT('Ctrl Pts',(50.755101690677,247.082048954903,31.9024627370647)) ;
#81147 = CARTESIAN_POINT('Ctrl Pts',(50.1538074562361,247.304757920327,31.9213203435596)) ;
#81148 = CARTESIAN_POINT('Ctrl Pts',(50.2307764623335,247.257355046955,31.9213203435596)) ;
#81149 = CARTESIAN_POINT('Ctrl Pts',(50.3086353659146,247.207175427604,31.9213203435596)) ;
#81150 = CARTESIAN_POINT('Ctrl Pts',(50.4460983832065,247.160898427981,31.9213203435596)) ;
#81151 = CARTESIAN_POINT('Ctrl Pts',(50.5668502867855,247.139108559787,31.9213203435596)) ;
#81152 = CARTESIAN_POINT('Ctrl Pts',(50.6856145710118,247.137293454578,31.9213203435596)) ;
#81153 = CARTESIAN_POINT('Ctrl Pts',(50.7562222547982,247.135814988266,31.9213203435596)) ;
#81154 = CARTESIAN_POINT('Ctrl Pts',(50.1679584400538,247.327667818836,31.9213203435596)) ;
#81155 = CARTESIAN_POINT('Ctrl Pts',(50.244821315925,247.280191165364,31.9213203435596)) ;
#81156 = CARTESIAN_POINT('Ctrl Pts',(50.3217536426056,247.231101873625,31.9213203435596)) ;
#81157 = CARTESIAN_POINT('Ctrl Pts',(50.4521974658606,247.187269352368,31.9213203435596)) ;
#81158 = CARTESIAN_POINT('Ctrl Pts',(50.5684933320555,247.166079789663,31.9213203435596)) ;
#81159 = CARTESIAN_POINT('Ctrl Pts',(50.6862172722578,247.164207780954,31.9213203435596)) ;
#81160 = CARTESIAN_POINT('Ctrl Pts',(50.7567833512179,247.16273707889,31.9213203435596)) ;
#81161 = CARTESIAN_POINT('',(50.1048968673761,247.225573558217,31.8013203435596)) ;
#81162 = CARTESIAN_POINT('Ctrl Pts',(50.1048968673761,247.225573558217,31.8013203435596)) ;
#81163 = CARTESIAN_POINT('Ctrl Pts',(50.1220003665551,247.215009070557,31.8013203435596)) ;
#81164 = CARTESIAN_POINT('Ctrl Pts',(50.1393793345259,247.204269965481,31.8013203435596)) ;
#81165 = CARTESIAN_POINT('Ctrl Pts',(50.1572105913275,247.193479920427,31.8013203435596)) ;
#81166 = CARTESIAN_POINT('Ctrl Pts',(50.1727805461718,247.184058233771,31.8013203435596)) ;
#81167 = CARTESIAN_POINT('Ctrl Pts',(50.1886952218773,247.174597296923,31.8013203435596)) ;
#81168 = CARTESIAN_POINT('Ctrl Pts',(50.2050843021405,247.165218387481,31.8013203435596)) ;
#81169 = CARTESIAN_POINT('Ctrl Pts',(50.2200254297862,247.156668091742,31.8013203435596)) ;
#81170 = CARTESIAN_POINT('Ctrl Pts',(50.2353607337608,247.148185627256,31.8013203435596)) ;
#81171 = CARTESIAN_POINT('Ctrl Pts',(50.2512006872648,247.13990263557,31.8013203435596)) ;
#81172 = CARTESIAN_POINT('Ctrl Pts',(50.2661930450385,247.132062866674,31.8013203435596)) ;
#81173 = CARTESIAN_POINT('Ctrl Pts',(50.2816373481069,247.124401333234,31.8013203435596)) ;
#81174 = CARTESIAN_POINT('Ctrl Pts',(50.2976405331232,247.117072828458,31.8013203435596)) ;
#81175 = CARTESIAN_POINT('Ctrl Pts',(50.3125234633058,247.110257333617,31.8013203435596)) ;
#81176 = CARTESIAN_POINT('Ctrl Pts',(50.3278897012615,247.103729655485,31.8013203435596)) ;
#81177 = CARTESIAN_POINT('Ctrl Pts',(50.3438384170975,247.097657116859,31.8013203435596)) ;
#81178 = CARTESIAN_POINT('Ctrl Pts',(50.3522456466948,247.094456029888,31.8013203435596)) ;
#81179 = CARTESIAN_POINT('Ctrl Pts',(50.3608149655582,247.091382169327,31.8013203435596)) ;
#81180 = CARTESIAN_POINT('Ctrl Pts',(50.3695626498277,247.088465738898,31.8013203435596)) ;
#81181 = CARTESIAN_POINT('Ctrl Pts',(50.3714498938344,247.087836541995,31.8013203435596)) ;
#81182 = CARTESIAN_POINT('Ctrl Pts',(50.3733365725727,247.08721765027,31.8013203435596)) ;
#81183 = CARTESIAN_POINT('Ctrl Pts',(50.3752217487968,247.086609092803,31.8013203435596)) ;
#81184 = CARTESIAN_POINT('Ctrl Pts',(50.3949270892529,247.080247972865,31.8013203435596)) ;
#81185 = CARTESIAN_POINT('Ctrl Pts',(50.41449862599,247.075000960662,31.8013203435596)) ;
#81186 = CARTESIAN_POINT('Ctrl Pts',(50.4338781015769,247.07059694525,31.8013203435596)) ;
#81187 = CARTESIAN_POINT('Ctrl Pts',(50.4540011902468,247.066023942629,31.8013203435596)) ;
#81188 = CARTESIAN_POINT('Ctrl Pts',(50.4739172837181,247.062360157766,31.8013203435596)) ;
#81189 = CARTESIAN_POINT('Ctrl Pts',(50.4935782017683,247.059357528583,31.8013203435596)) ;
#81190 = CARTESIAN_POINT('Ctrl Pts',(50.5117826362868,247.056577334587,31.8013203435596)) ;
#81191 = CARTESIAN_POINT('Ctrl Pts',(50.5297671997357,247.054365030188,31.8013203435596)) ;
#81192 = CARTESIAN_POINT('Ctrl Pts',(50.5475093978148,247.052559566174,31.8013203435596)) ;
#81193 = CARTESIAN_POINT('Ctrl Pts',(50.5684869881217,247.050424865377,31.8013203435596)) ;
#81194 = CARTESIAN_POINT('Ctrl Pts',(50.5891312305048,247.048857239894,31.8013203435596)) ;
#81195 = CARTESIAN_POINT('Ctrl Pts',(50.6094626803275,247.047643171334,31.8013203435596)) ;
#81196 = CARTESIAN_POINT('Ctrl Pts',(50.6312322488022,247.046343227213,31.8013203435596)) ;
#81197 = CARTESIAN_POINT('Ctrl Pts',(50.6526434341527,247.045449355937,31.8013203435596)) ;
#81198 = CARTESIAN_POINT('Ctrl Pts',(50.673739904065,247.044759445824,31.8013203435596)) ;
#81199 = CARTESIAN_POINT('Ctrl Pts',(50.6977184863756,247.043975283047,31.8013203435596)) ;
#81200 = CARTESIAN_POINT('Ctrl Pts',(50.7212907023591,247.043455310561,31.8013203435596)) ;
#81201 = CARTESIAN_POINT('Ctrl Pts',(50.7445403358891,247.042966742562,31.8013203435596)) ;
#81202 = CARTESIAN_POINT('Ctrl Pts',(50.7477940726226,247.042898368511,31.8013203435596)) ;
#81203 = CARTESIAN_POINT('Ctrl Pts',(50.7510415155772,247.04283068806,31.8013203435596)) ;
#81204 = CARTESIAN_POINT('Ctrl Pts',(50.7542829156931,247.042763132459,31.8013203435596)) ;
#81205 = CARTESIAN_POINT('',(50.1819316941158,247.319027603173,31.9213203435596)) ;
#81206 = CARTESIAN_POINT('Ctrl Pts',(50.7555332761922,247.16276309732,31.9213203435596)) ;
#81207 = CARTESIAN_POINT('Ctrl Pts',(50.6853831050741,247.164221288387,31.9213203435596)) ;
#81208 = CARTESIAN_POINT('Ctrl Pts',(50.568081299126,247.166154863678,31.9213203435596)) ;
#81209 = CARTESIAN_POINT('Ctrl Pts',(50.4521974658606,247.187269352368,31.9213203435596)) ;
#81210 = CARTESIAN_POINT('Ctrl Pts',(50.3269498697332,247.229355806006,31.9213203435596)) ;
#81211 = CARTESIAN_POINT('Ctrl Pts',(50.2541752681168,247.274317645589,31.9213203435596)) ;
#81212 = CARTESIAN_POINT('Ctrl Pts',(50.1819308000888,247.319026158513,31.9213203435596)) ;
#81213 = CARTESIAN_POINT('Ctrl Pts',(50.1819388265444,247.319021191339,31.9213203435596)) ;
#81214 = CARTESIAN_POINT('Ctrl Pts',(50.1817524473267,247.318793998429,31.9213203435596)) ;
#81215 = CARTESIAN_POINT('Ctrl Pts',(50.1815660887041,247.318566789193,31.9213192390868)) ;
#81216 = CARTESIAN_POINT('Ctrl Pts',(50.1714406029608,247.306219582572,31.9211993432478)) ;
#81217 = CARTESIAN_POINT('Ctrl Pts',(50.1615757516659,247.294081074233,31.917946664297)) ;
#81218 = CARTESIAN_POINT('Ctrl Pts',(50.1459828532116,247.275031259232,31.9077738491051)) ;
#81219 = CARTESIAN_POINT('Ctrl Pts',(50.1367511418837,247.263820791132,31.900294136492)) ;
#81220 = CARTESIAN_POINT('Ctrl Pts',(50.1209443533371,247.245047664794,31.8760190448593)) ;
#81221 = CARTESIAN_POINT('Ctrl Pts',(50.1150198743948,247.238012576204,31.8631426108606)) ;
#81222 = CARTESIAN_POINT('Ctrl Pts',(50.1091216557418,247.230422468868,31.8407001619781)) ;
#81223 = CARTESIAN_POINT('Ctrl Pts',(50.1076630070811,247.228494965487,31.8330344212244)) ;
#81224 = CARTESIAN_POINT('Ctrl Pts',(50.1055315058664,247.226090096372,31.8173189025619)) ;
#81225 = CARTESIAN_POINT('Ctrl Pts',(50.1048968673764,247.225573558217,31.8093263718846)) ;
#81226 = CARTESIAN_POINT('Ctrl Pts',(50.1048968673764,247.225573558217,31.8013203435596)) ;
#81227 = CARTESIAN_POINT('Origin',(51.9003128398474,243.213135158824,31.8013203435596)) ;
#81228 = CARTESIAN_POINT('',(51.9003128398474,243.213135158824,31.9213203435596)) ;
#81229 = CARTESIAN_POINT('Ctrl Pts',(49.8975299240168,247.692149180776,31.8013203435596)) ;
#81230 = CARTESIAN_POINT('Ctrl Pts',(49.9003120409242,247.662214992781,31.8013203435596)) ;
#81231 = CARTESIAN_POINT('Ctrl Pts',(49.9080129919011,247.584369229331,31.8013203435596)) ;
#81232 = CARTESIAN_POINT('Ctrl Pts',(49.9228022199243,247.494193108499,31.8013203435597)) ;
#81233 = CARTESIAN_POINT('Ctrl Pts',(49.9584226751439,247.413847381454,31.8013203435597)) ;
#81234 = CARTESIAN_POINT('Ctrl Pts',(49.978378600925,247.378172811915,31.8013203435596)) ;
#81235 = CARTESIAN_POINT('Ctrl Pts',(50.0317423407727,247.303870476782,31.8013203435596)) ;
#81236 = CARTESIAN_POINT('Ctrl Pts',(50.0747869844785,247.258178865285,31.8013203435596)) ;
#81237 = CARTESIAN_POINT('Ctrl Pts',(50.1049315040526,247.225536051252,31.8013203435596)) ;
#81238 = CARTESIAN_POINT('Ctrl Pts',(49.8975299240168,247.692149180776,31.8192723015802)) ;
#81239 = CARTESIAN_POINT('Ctrl Pts',(49.9003120409242,247.662214992781,31.8192723015802)) ;
#81240 = CARTESIAN_POINT('Ctrl Pts',(49.9080129919011,247.584369229331,31.8192723015802)) ;
#81241 = CARTESIAN_POINT('Ctrl Pts',(49.9228022199243,247.494193108499,31.8192723015802)) ;
#81242 = CARTESIAN_POINT('Ctrl Pts',(49.9584226751439,247.413847381454,31.8192723015802)) ;
#81243 = CARTESIAN_POINT('Ctrl Pts',(49.978378600925,247.378172811915,31.8192723015802)) ;
#81244 = CARTESIAN_POINT('Ctrl Pts',(50.0317423407727,247.303870476782,31.8192723015802)) ;
#81245 = CARTESIAN_POINT('Ctrl Pts',(50.0747869844785,247.258178865285,31.8192723015802)) ;
#81246 = CARTESIAN_POINT('Ctrl Pts',(50.1049315040526,247.225536051252,31.8192723015802)) ;
#81247 = CARTESIAN_POINT('Ctrl Pts',(49.9057100722929,247.692909452904,31.8551057858421)) ;
#81248 = CARTESIAN_POINT('Ctrl Pts',(49.9084394091396,247.662972763406,31.8551057858421)) ;
#81249 = CARTESIAN_POINT('Ctrl Pts',(49.9161458757847,247.585340197531,31.8551057858422)) ;
#81250 = CARTESIAN_POINT('Ctrl Pts',(49.9309041124678,247.496274424605,31.8551057858422)) ;
#81251 = CARTESIAN_POINT('Ctrl Pts',(49.9656396859993,247.417640984724,31.8551057858422)) ;
#81252 = CARTESIAN_POINT('Ctrl Pts',(49.9852635362106,247.38264873378,31.8551057858422)) ;
#81253 = CARTESIAN_POINT('Ctrl Pts',(50.0379009729177,247.309294040215,31.8551057858421)) ;
#81254 = CARTESIAN_POINT('Ctrl Pts',(50.0808262047872,247.263810918776,31.8551057858421)) ;
#81255 = CARTESIAN_POINT('Ctrl Pts',(50.1109669912768,247.231109643768,31.8551057858421)) ;
#81256 = CARTESIAN_POINT('Ctrl Pts',(49.9456840251116,247.696624676782,31.9055714461187)) ;
#81257 = CARTESIAN_POINT('Ctrl Pts',(49.9484658983372,247.666690477238,31.9055714461187)) ;
#81258 = CARTESIAN_POINT('Ctrl Pts',(49.9558946167219,247.590135261357,31.9055714461187)) ;
#81259 = CARTESIAN_POINT('Ctrl Pts',(49.9702456835514,247.506232253633,31.9055714461187)) ;
#81260 = CARTESIAN_POINT('Ctrl Pts',(50.0013503310202,247.43618856547,31.9055714461187)) ;
#81261 = CARTESIAN_POINT('Ctrl Pts',(50.0190652052593,247.404431264816,31.9055714461187)) ;
#81262 = CARTESIAN_POINT('Ctrl Pts',(50.0682830773054,247.335769984711,31.9055714461187)) ;
#81263 = CARTESIAN_POINT('Ctrl Pts',(50.1103155648094,247.290990135563,31.9055714461187)) ;
#81264 = CARTESIAN_POINT('Ctrl Pts',(50.1404606488897,247.258346527721,31.9055714461187)) ;
#81265 = CARTESIAN_POINT('Ctrl Pts',(49.9902025919921,247.700762282173,31.9213203435596)) ;
#81266 = CARTESIAN_POINT('Ctrl Pts',(49.9929442461564,247.670826176452,31.9213203435596)) ;
#81267 = CARTESIAN_POINT('Ctrl Pts',(50.0001605373263,247.595459499129,31.9213203435596)) ;
#81268 = CARTESIAN_POINT('Ctrl Pts',(50.0141394662325,247.517389900366,31.9213203435597)) ;
#81269 = CARTESIAN_POINT('Ctrl Pts',(50.0409799368062,247.456841829704,31.9213203435597)) ;
#81270 = CARTESIAN_POINT('Ctrl Pts',(50.0566598259294,247.428718849235,31.9213203435597)) ;
#81271 = CARTESIAN_POINT('Ctrl Pts',(50.1020281310731,247.365264675744,31.9213203435596)) ;
#81272 = CARTESIAN_POINT('Ctrl Pts',(50.143164711757,247.321368403535,31.9213203435596)) ;
#81273 = CARTESIAN_POINT('Ctrl Pts',(50.1733074140605,247.288679830851,31.9213203435596)) ;
#81274 = CARTESIAN_POINT('Ctrl Pts',(50.0170149746567,247.703254255002,31.9213203435596)) ;
#81275 = CARTESIAN_POINT('Ctrl Pts',(50.0197970915642,247.673320067007,31.9213203435596)) ;
#81276 = CARTESIAN_POINT('Ctrl Pts',(50.0268219567888,247.598676615906,31.9213203435596)) ;
#81277 = CARTESIAN_POINT('Ctrl Pts',(50.0405234748466,247.52406549449,31.9213203435597)) ;
#81278 = CARTESIAN_POINT('Ctrl Pts',(50.0649401802121,247.46928270932,31.9213203435597)) ;
#81279 = CARTESIAN_POINT('Ctrl Pts',(50.0793348143422,247.443327888337,31.9213203435597)) ;
#81280 = CARTESIAN_POINT('Ctrl Pts',(50.1224116408749,247.383022857659,31.9213203435596)) ;
#81281 = CARTESIAN_POINT('Ctrl Pts',(50.1629442132913,247.339592992793,31.9213203435596)) ;
#81282 = CARTESIAN_POINT('Ctrl Pts',(50.1930901774771,247.306948877788,31.9213203435596)) ;
#81283 = CARTESIAN_POINT('',(49.8975299240168,247.692149180776,31.8013203435596)) ;
#81284 = CARTESIAN_POINT('Ctrl Pts',(49.8975299240168,247.692149180776,31.8013203435596)) ;
#81285 = CARTESIAN_POINT('Ctrl Pts',(49.8989209824705,247.677182086779,31.8013203435596)) ;
#81286 = CARTESIAN_POINT('Ctrl Pts',(49.9003364541846,247.661913083176,31.8013203435596)) ;
#81287 = CARTESIAN_POINT('Ctrl Pts',(49.9019331250822,247.646242176031,31.8013203435596)) ;
#81288 = CARTESIAN_POINT('Ctrl Pts',(49.9033173765781,247.63265610974,31.8013203435596)) ;
#81289 = CARTESIAN_POINT('Ctrl Pts',(49.9048372301939,247.618767700215,31.8013203435596)) ;
#81290 = CARTESIAN_POINT('Ctrl Pts',(49.9066326956466,247.604528684876,31.8013203435596)) ;
#81291 = CARTESIAN_POINT('Ctrl Pts',(49.9069082176151,247.602343646155,31.8013203435596)) ;
#81292 = CARTESIAN_POINT('Ctrl Pts',(49.9071903212962,247.600150392157,31.8013203435596)) ;
#81293 = CARTESIAN_POINT('Ctrl Pts',(49.907479619698,247.597948796284,31.8013203435596)) ;
#81294 = CARTESIAN_POINT('Ctrl Pts',(49.9091103249136,247.585538932107,31.8013203435596)) ;
#81295 = CARTESIAN_POINT('Ctrl Pts',(49.9109621984763,247.572888414998,31.8013203435596)) ;
#81296 = CARTESIAN_POINT('Ctrl Pts',(49.9131777267516,247.559918931878,31.8013203435596)) ;
#81297 = CARTESIAN_POINT('Ctrl Pts',(49.915073415318,247.548821758741,31.8013203435597)) ;
#81298 = CARTESIAN_POINT('Ctrl Pts',(49.9172352909559,247.537491043414,31.8013203435597)) ;
#81299 = CARTESIAN_POINT('Ctrl Pts',(49.9197895184584,247.525894206826,31.8013203435597)) ;
#81300 = CARTESIAN_POINT('Ctrl Pts',(49.922187758184,247.515005594058,31.8013203435597)) ;
#81301 = CARTESIAN_POINT('Ctrl Pts',(49.9249314068481,247.503882155673,31.8013203435597)) ;
#81302 = CARTESIAN_POINT('Ctrl Pts',(49.928164462093,247.492514588819,31.8013203435597)) ;
#81303 = CARTESIAN_POINT('Ctrl Pts',(49.9311207392,247.482120186279,31.8013203435597)) ;
#81304 = CARTESIAN_POINT('Ctrl Pts',(49.9344860238457,247.471521580022,31.8013203435597)) ;
#81305 = CARTESIAN_POINT('Ctrl Pts',(49.9384087813414,247.460728790724,31.8013203435597)) ;
#81306 = CARTESIAN_POINT('Ctrl Pts',(49.9416467803634,247.451819996023,31.8013203435597)) ;
#81307 = CARTESIAN_POINT('Ctrl Pts',(49.9452650324319,247.442779081571,31.8013203435597)) ;
#81308 = CARTESIAN_POINT('Ctrl Pts',(49.9493716598566,247.433622676736,31.8013203435597)) ;
#81309 = CARTESIAN_POINT('Ctrl Pts',(49.9493749701299,247.433615295934,31.8013203435597)) ;
#81310 = CARTESIAN_POINT('Ctrl Pts',(49.949378280722,247.433607915058,31.8013203435597)) ;
#81311 = CARTESIAN_POINT('Ctrl Pts',(49.9493815916327,247.433600534107,31.8013203435597)) ;
#81312 = CARTESIAN_POINT('Ctrl Pts',(49.9545038625223,247.422181552888,31.8013203435597)) ;
#81313 = CARTESIAN_POINT('Ctrl Pts',(49.9600029742428,247.41143325106,31.8013203435597)) ;
#81314 = CARTESIAN_POINT('Ctrl Pts',(49.9657098706998,247.401244562447,31.8013203435597)) ;
#81315 = CARTESIAN_POINT('Ctrl Pts',(49.9699155343581,247.393736068514,31.8013203435597)) ;
#81316 = CARTESIAN_POINT('Ctrl Pts',(49.974235278962,247.386532044786,31.8013203435596)) ;
#81317 = CARTESIAN_POINT('Ctrl Pts',(49.9786177646995,247.379595326503,31.8013203435596)) ;
#81318 = CARTESIAN_POINT('Ctrl Pts',(49.9849176615277,247.369623677506,31.8013203435596)) ;
#81319 = CARTESIAN_POINT('Ctrl Pts',(49.9913445526255,247.360203543544,31.8013203435596)) ;
#81320 = CARTESIAN_POINT('Ctrl Pts',(49.9978236741791,247.351195483027,31.8013203435596)) ;
#81321 = CARTESIAN_POINT('Ctrl Pts',(50.0019677316018,247.345433911841,31.8013203435596)) ;
#81322 = CARTESIAN_POINT('Ctrl Pts',(50.0061343453035,247.339841446927,31.8013203435596)) ;
#81323 = CARTESIAN_POINT('Ctrl Pts',(50.0103138715769,247.334386031064,31.8013203435596)) ;
#81324 = CARTESIAN_POINT('Ctrl Pts',(50.0187016326063,247.323437726979,31.8013203435596)) ;
#81325 = CARTESIAN_POINT('Ctrl Pts',(50.0271429541399,247.313034619382,31.8013203435596)) ;
#81326 = CARTESIAN_POINT('Ctrl Pts',(50.0355400198878,247.303042575351,31.8013203435596)) ;
#81327 = CARTESIAN_POINT('Ctrl Pts',(50.0446115661329,247.292247936816,31.8013203435596)) ;
#81328 = CARTESIAN_POINT('Ctrl Pts',(50.0536322844746,247.2819334174,31.8013203435596)) ;
#81329 = CARTESIAN_POINT('Ctrl Pts',(50.0625395637957,247.271957006048,31.8013203435596)) ;
#81330 = CARTESIAN_POINT('Ctrl Pts',(50.0729202410483,247.260330346252,31.8013203435596)) ;
#81331 = CARTESIAN_POINT('Ctrl Pts',(50.0831475154001,247.249163200923,31.8013203435596)) ;
#81332 = CARTESIAN_POINT('Ctrl Pts',(50.0931900641649,247.238261049293,31.8013203435596)) ;
#81333 = CARTESIAN_POINT('Ctrl Pts',(50.0971200610123,247.233994660098,31.8013203435596)) ;
#81334 = CARTESIAN_POINT('Ctrl Pts',(50.1010223530526,247.229769113771,31.8013203435596)) ;
#81335 = CARTESIAN_POINT('Ctrl Pts',(50.1048968673761,247.225573558217,31.8013203435596)) ;
#81336 = CARTESIAN_POINT('',(50.0179285595009,247.693448991958,31.9213203435596)) ;
#81337 = CARTESIAN_POINT('Ctrl Pts',(50.1819259253794,247.319035169015,31.9213203435597)) ;
#81338 = CARTESIAN_POINT('Ctrl Pts',(50.1554933071014,247.347673462912,31.9213203435596)) ;
#81339 = CARTESIAN_POINT('Ctrl Pts',(50.1192219147918,247.387488287097,31.9213203435596)) ;
#81340 = CARTESIAN_POINT('Ctrl Pts',(50.0793348143422,247.443327888337,31.9213203435597)) ;
#81341 = CARTESIAN_POINT('Ctrl Pts',(50.0649401802121,247.46928270932,31.9213203435597)) ;
#81342 = CARTESIAN_POINT('Ctrl Pts',(50.0405234748466,247.52406549449,31.9213203435597)) ;
#81343 = CARTESIAN_POINT('Ctrl Pts',(50.0274205901366,247.595416779644,31.9213203435596)) ;
#81344 = CARTESIAN_POINT('Ctrl Pts',(50.0204236837674,247.666797631165,31.9213203435596)) ;
#81345 = CARTESIAN_POINT('Ctrl Pts',(50.0179289780831,247.693447995904,31.9213203435596)) ;
#81346 = CARTESIAN_POINT('Ctrl Pts',(50.017928391634,247.693450066558,31.9213203435596)) ;
#81347 = CARTESIAN_POINT('Ctrl Pts',(50.0176360614229,247.693446884448,31.9213203435596)) ;
#81348 = CARTESIAN_POINT('Ctrl Pts',(50.0173433514854,247.693443731786,31.921319241072)) ;
#81349 = CARTESIAN_POINT('Ctrl Pts',(50.0170506622064,247.693440580217,31.921317036068)) ;
#81350 = CARTESIAN_POINT('Ctrl Pts',(50.0086222481347,247.693349826201,31.9212535397677)) ;
#81351 = CARTESIAN_POINT('Ctrl Pts',(50.0002543434629,247.693260420416,31.9202814000225)) ;
#81352 = CARTESIAN_POINT('Ctrl Pts',(49.9920673812869,247.69317293051,31.9184713729232)) ;
#81353 = CARTESIAN_POINT('Ctrl Pts',(49.9913984237448,247.693165781701,31.9183234754181)) ;
#81354 = CARTESIAN_POINT('Ctrl Pts',(49.9907306748512,247.693158645656,31.9181699552184)) ;
#81355 = CARTESIAN_POINT('Ctrl Pts',(49.9900642015852,247.693151522596,31.9180108360501)) ;
#81356 = CARTESIAN_POINT('Ctrl Pts',(49.9833973538999,247.693080269391,31.9164191394086)) ;
#81357 = CARTESIAN_POINT('Ctrl Pts',(49.976857424647,247.69301028865,31.9142687128406)) ;
#81358 = CARTESIAN_POINT('Ctrl Pts',(49.9705183372566,247.69294212283,31.9115735225365)) ;
#81359 = CARTESIAN_POINT('Ctrl Pts',(49.9621346627971,247.692851971047,31.908009034981)) ;
#81360 = CARTESIAN_POINT('Ctrl Pts',(49.9541926461795,247.692765943363,31.9035316654796)) ;
#81361 = CARTESIAN_POINT('Ctrl Pts',(49.9468699753835,247.69268559923,31.8981932593553)) ;
#81362 = CARTESIAN_POINT('Ctrl Pts',(49.9455102810432,247.692670680703,31.8972020089228)) ;
#81363 = CARTESIAN_POINT('Ctrl Pts',(49.9441720544978,247.69265596149,31.8961809675201)) ;
#81364 = CARTESIAN_POINT('Ctrl Pts',(49.9428566063046,247.692641457862,31.8951303448721)) ;
#81365 = CARTESIAN_POINT('Ctrl Pts',(49.942850731994,247.692641393094,31.8951256531756)) ;
#81366 = CARTESIAN_POINT('Ctrl Pts',(49.9428448581382,247.69264132833,31.8951209608895)) ;
#81367 = CARTESIAN_POINT('Ctrl Pts',(49.9428389847374,247.69264126357,31.8951162680138)) ;
#81368 = CARTESIAN_POINT('Ctrl Pts',(49.9390653822337,247.69259965616,31.8921011413717)) ;
#81369 = CARTESIAN_POINT('Ctrl Pts',(49.9354794429431,247.692559773032,31.8888427091753)) ;
#81370 = CARTESIAN_POINT('Ctrl Pts',(49.932097179084,247.692521650875,31.8853668065556)) ;
#81371 = CARTESIAN_POINT('Ctrl Pts',(49.9257440837398,247.692450043897,31.8788378242911)) ;
#81372 = CARTESIAN_POINT('Ctrl Pts',(49.9201787710645,247.692385036831,31.871618011282)) ;
#81373 = CARTESIAN_POINT('Ctrl Pts',(49.9154588127174,247.692330638236,31.8638856152259)) ;
#81374 = CARTESIAN_POINT('Ctrl Pts',(49.913357124184,247.692306415797,31.8604425576961)) ;
#81375 = CARTESIAN_POINT('Ctrl Pts',(49.9114231698096,247.692284370314,31.8568969998879)) ;
#81376 = CARTESIAN_POINT('Ctrl Pts',(49.9096637197127,247.692265205622,31.8532606519075)) ;
#81377 = CARTESIAN_POINT('Ctrl Pts',(49.9086093688806,247.692253721176,31.8510815696331)) ;
#81378 = CARTESIAN_POINT('Ctrl Pts',(49.9076176957775,247.692243276832,31.8488698077343)) ;
#81379 = CARTESIAN_POINT('Ctrl Pts',(49.9066904861145,247.692233782334,31.8466274426062)) ;
#81380 = CARTESIAN_POINT('Ctrl Pts',(49.9032292440959,247.692198339699,31.8382567701338)) ;
#81381 = CARTESIAN_POINT('Ctrl Pts',(49.9006995749997,247.692176191016,31.8295510379215)) ;
#81382 = CARTESIAN_POINT('Ctrl Pts',(49.899182009376,247.692163157307,31.8206540876558)) ;
#81383 = CARTESIAN_POINT('Ctrl Pts',(49.8980956948875,247.692153827426,31.8142854101992)) ;
#81384 = CARTESIAN_POINT('Ctrl Pts',(49.8975299240168,247.692149180776,31.807818822737)) ;
#81385 = CARTESIAN_POINT('Ctrl Pts',(49.8975299240168,247.692149180776,31.8013203435596)) ;
#81386 = CARTESIAN_POINT('Ctrl Pts',(50.0039417983111,248.05231292904,31.8013203435596)) ;
#81387 = CARTESIAN_POINT('Ctrl Pts',(49.9880262923894,248.023366957204,31.8013203435596)) ;
#81388 = CARTESIAN_POINT('Ctrl Pts',(49.9595768641916,247.972394634097,31.8013203435596)) ;
#81389 = CARTESIAN_POINT('Ctrl Pts',(49.9328199880692,247.908444334476,31.8013203435596)) ;
#81390 = CARTESIAN_POINT('Ctrl Pts',(49.9115183942193,247.835438884033,31.8013203435596)) ;
#81391 = CARTESIAN_POINT('Ctrl Pts',(49.9032281681206,247.770513850496,31.8013203435596)) ;
#81392 = CARTESIAN_POINT('Ctrl Pts',(49.8990770736132,247.713887501579,31.8013203435596)) ;
#81393 = CARTESIAN_POINT('Ctrl Pts',(49.8975299240168,247.692149180776,31.8013203435596)) ;
#81394 = CARTESIAN_POINT('Ctrl Pts',(50.0039417983111,248.05231292904,31.8372242596006)) ;
#81395 = CARTESIAN_POINT('Ctrl Pts',(49.9880262923894,248.023366957204,31.8372242596007)) ;
#81396 = CARTESIAN_POINT('Ctrl Pts',(49.9595768641916,247.972394634097,31.8372242596006)) ;
#81397 = CARTESIAN_POINT('Ctrl Pts',(49.9328199880692,247.908444334476,31.8372242596006)) ;
#81398 = CARTESIAN_POINT('Ctrl Pts',(49.9115183942193,247.835438884033,31.8372242596007)) ;
#81399 = CARTESIAN_POINT('Ctrl Pts',(49.9032281681206,247.770513850496,31.8372242596007)) ;
#81400 = CARTESIAN_POINT('Ctrl Pts',(49.8990770736132,247.713887501579,31.8372242596007)) ;
#81401 = CARTESIAN_POINT('Ctrl Pts',(49.8975299240168,247.692149180776,31.8372242596007)) ;
#81402 = CARTESIAN_POINT('Ctrl Pts',(50.0303692554824,248.037782190411,31.8993563874716)) ;
#81403 = CARTESIAN_POINT('Ctrl Pts',(50.0144401833049,248.008801749279,31.8993563874716)) ;
#81404 = CARTESIAN_POINT('Ctrl Pts',(49.9864587570184,247.958566948592,31.8993563874716)) ;
#81405 = CARTESIAN_POINT('Ctrl Pts',(49.9611065521,247.897853880215,31.8993563874716)) ;
#81406 = CARTESIAN_POINT('Ctrl Pts',(49.9413091559894,247.829989135405,31.8993563874716)) ;
#81407 = CARTESIAN_POINT('Ctrl Pts',(49.9332582787006,247.767775968166,31.8993563874716)) ;
#81408 = CARTESIAN_POINT('Ctrl Pts',(49.9291299338273,247.711745405093,31.8993563874716)) ;
#81409 = CARTESIAN_POINT('Ctrl Pts',(49.9276126240328,247.690008148926,31.8993563874716)) ;
#81410 = CARTESIAN_POINT('Ctrl Pts',(50.0854987052327,248.007470094175,31.9213203435596)) ;
#81411 = CARTESIAN_POINT('Ctrl Pts',(50.0695751953828,247.978503785867,31.9213203435596)) ;
#81412 = CARTESIAN_POINT('Ctrl Pts',(50.0425087956085,247.929736002886,31.9213203435596)) ;
#81413 = CARTESIAN_POINT('Ctrl Pts',(50.0201811280109,247.875790500525,31.9213203435596)) ;
#81414 = CARTESIAN_POINT('Ctrl Pts',(50.0034820155373,247.818649943681,31.9213203435596)) ;
#81415 = CARTESIAN_POINT('Ctrl Pts',(49.9958616134348,247.762060700417,31.9213203435596)) ;
#81416 = CARTESIAN_POINT('Ctrl Pts',(49.9918967002071,247.70727950544,31.9213203435596)) ;
#81417 = CARTESIAN_POINT('Ctrl Pts',(49.9903671557358,247.68554181276,31.9213203435596)) ;
#81418 = CARTESIAN_POINT('Ctrl Pts',(50.1090950367627,247.994496007268,31.9213203435596)) ;
#81419 = CARTESIAN_POINT('Ctrl Pts',(50.0931795308409,247.965550035432,31.9213203435596)) ;
#81420 = CARTESIAN_POINT('Ctrl Pts',(50.0664946055529,247.917398286899,31.9213203435596)) ;
#81421 = CARTESIAN_POINT('Ctrl Pts',(50.0454771499519,247.866351821843,31.9213203435596)) ;
#81422 = CARTESIAN_POINT('Ctrl Pts',(50.0300975833916,247.813801452734,31.9213203435596)) ;
#81423 = CARTESIAN_POINT('Ctrl Pts',(50.0226500033239,247.759613828492,31.9213203435596)) ;
#81424 = CARTESIAN_POINT('Ctrl Pts',(50.0187743001587,247.705368466579,31.9213203435596)) ;
#81425 = CARTESIAN_POINT('Ctrl Pts',(50.0172271505622,247.683630145776,31.9213203435596)) ;
#81426 = CARTESIAN_POINT('Ctrl Pts',(50.003941798311,248.05231292904,31.8013203435596)) ;
#81427 = CARTESIAN_POINT('Ctrl Pts',(49.9973092280089,248.040250089561,31.8013203435596)) ;
#81428 = CARTESIAN_POINT('Ctrl Pts',(49.9905098033151,248.027893411311,31.8013203435596)) ;
#81429 = CARTESIAN_POINT('Ctrl Pts',(49.9836122391022,248.01504026841,31.8013203435596)) ;
#81430 = CARTESIAN_POINT('Ctrl Pts',(49.9781582134433,248.004877061657,31.8013203435596)) ;
#81431 = CARTESIAN_POINT('Ctrl Pts',(49.9726428617977,247.994403438057,31.8013203435596)) ;
#81432 = CARTESIAN_POINT('Ctrl Pts',(49.9671358038039,247.983508719679,31.8013203435596)) ;
#81433 = CARTESIAN_POINT('Ctrl Pts',(49.962297053248,247.973936126715,31.8013203435596)) ;
#81434 = CARTESIAN_POINT('Ctrl Pts',(49.9574646433129,247.964038710708,31.8013203435596)) ;
#81435 = CARTESIAN_POINT('Ctrl Pts',(49.9527177389226,247.953731217489,31.8013203435596)) ;
#81436 = CARTESIAN_POINT('Ctrl Pts',(49.9482194239541,247.943963514746,31.8013203435596)) ;
#81437 = CARTESIAN_POINT('Ctrl Pts',(49.9437957899078,247.93382561916,31.8013203435596)) ;
#81438 = CARTESIAN_POINT('Ctrl Pts',(49.9395411846259,247.923206079714,31.8013203435596)) ;
#81439 = CARTESIAN_POINT('Ctrl Pts',(49.9367748644537,247.916301315525,31.8013203435596)) ;
#81440 = CARTESIAN_POINT('Ctrl Pts',(49.9340808270642,247.909192691924,31.8013203435596)) ;
#81441 = CARTESIAN_POINT('Ctrl Pts',(49.9314977623415,247.901845815823,31.8013203435596)) ;
#81442 = CARTESIAN_POINT('Ctrl Pts',(49.9302062299801,247.898172377772,31.8013203435596)) ;
#81443 = CARTESIAN_POINT('Ctrl Pts',(49.9289426182913,247.894439324299,31.8013203435596)) ;
#81444 = CARTESIAN_POINT('Ctrl Pts',(49.9277129474339,247.890642007448,31.8013203435596)) ;
#81445 = CARTESIAN_POINT('Ctrl Pts',(49.9270587936476,247.888621930952,31.8013203435596)) ;
#81446 = CARTESIAN_POINT('Ctrl Pts',(49.9264142593432,247.886583663888,31.8013203435596)) ;
#81447 = CARTESIAN_POINT('Ctrl Pts',(49.9257803542142,247.884526476061,31.8013203435596)) ;
#81448 = CARTESIAN_POINT('Ctrl Pts',(49.9253459058396,247.883116577534,31.8013203435596)) ;
#81449 = CARTESIAN_POINT('Ctrl Pts',(49.9249164515835,247.88169779133,31.8013203435596)) ;
#81450 = CARTESIAN_POINT('Ctrl Pts',(49.9244923373195,247.88026987625,31.8013203435596)) ;
#81451 = CARTESIAN_POINT('Ctrl Pts',(49.9243720149763,247.879864772949,31.8013203435596)) ;
#81452 = CARTESIAN_POINT('Ctrl Pts',(49.9242521035458,247.879458870193,31.8013203435596)) ;
#81453 = CARTESIAN_POINT('Ctrl Pts',(49.9241326690729,247.879052359467,31.8013203435596)) ;
#81454 = CARTESIAN_POINT('Ctrl Pts',(49.9208603305429,247.867914530669,31.8013203435596)) ;
#81455 = CARTESIAN_POINT('Ctrl Pts',(49.9181591310371,247.857063543614,31.8013203435596)) ;
#81456 = CARTESIAN_POINT('Ctrl Pts',(49.915855507275,247.846490923394,31.8013203435596)) ;
#81457 = CARTESIAN_POINT('Ctrl Pts',(49.9133864593928,247.835159079196,31.8013203435596)) ;
#81458 = CARTESIAN_POINT('Ctrl Pts',(49.9113747091496,247.824146848157,31.8013203435596)) ;
#81459 = CARTESIAN_POINT('Ctrl Pts',(49.9096664176065,247.813426157519,31.8013203435596)) ;
#81460 = CARTESIAN_POINT('Ctrl Pts',(49.9077483672311,247.801389087625,31.8013203435596)) ;
#81461 = CARTESIAN_POINT('Ctrl Pts',(49.9062132415599,247.789719440941,31.8013203435596)) ;
#81462 = CARTESIAN_POINT('Ctrl Pts',(49.9049089271676,247.778358143172,31.8013203435596)) ;
#81463 = CARTESIAN_POINT('Ctrl Pts',(49.9038781189045,247.769379234645,31.8013203435596)) ;
#81464 = CARTESIAN_POINT('Ctrl Pts',(49.9029927564946,247.760589341875,31.8013203435596)) ;
#81465 = CARTESIAN_POINT('Ctrl Pts',(49.9021997298857,247.751964778757,31.8013203435596)) ;
#81466 = CARTESIAN_POINT('Ctrl Pts',(49.9009319351644,247.738176873697,31.8013203435596)) ;
#81467 = CARTESIAN_POINT('Ctrl Pts',(49.8998987096635,247.724820112012,31.8013203435596)) ;
#81468 = CARTESIAN_POINT('Ctrl Pts',(49.8989443625904,247.71181780161,31.8013203435596)) ;
#81469 = CARTESIAN_POINT('Ctrl Pts',(49.8984566596798,247.705173191062,31.8013203435596)) ;
#81470 = CARTESIAN_POINT('Ctrl Pts',(49.8979905234979,247.698620862186,31.8013203435596)) ;
#81471 = CARTESIAN_POINT('Ctrl Pts',(49.8975299240168,247.692149180776,31.8013203435596)) ;
#81472 = CARTESIAN_POINT('Ctrl Pts',(50.0179283156872,247.693449009475,31.9213203435596)) ;
#81473 = CARTESIAN_POINT('Ctrl Pts',(50.0192542126488,247.711903817022,31.9213203435596)) ;
#81474 = CARTESIAN_POINT('Ctrl Pts',(50.0230986509543,247.762878130318,31.9213203435596)) ;
#81475 = CARTESIAN_POINT('Ctrl Pts',(50.0300975833916,247.813801452734,31.9213203435596)) ;
#81476 = CARTESIAN_POINT('Ctrl Pts',(50.0454771499519,247.866351821843,31.9213203435596)) ;
#81477 = CARTESIAN_POINT('Ctrl Pts',(50.0652213925075,247.914305951343,31.9213203435596)) ;
#81478 = CARTESIAN_POINT('Ctrl Pts',(50.0899672457456,247.959705458432,31.9213203435596)) ;
#81479 = CARTESIAN_POINT('Ctrl Pts',(50.1042736016154,247.985728991073,31.9213203435596)) ;
#81480 = CARTESIAN_POINT('Ctrl Pts',(50.8825961108042,248.366092821008,31.8013203435596)) ;
#81481 = CARTESIAN_POINT('Ctrl Pts',(50.7801147995828,248.365003869109,31.8013203435596)) ;
#81482 = CARTESIAN_POINT('Ctrl Pts',(50.6724206638963,248.36479492292,31.8013203435596)) ;
#81483 = CARTESIAN_POINT('Ctrl Pts',(50.471719498392,248.334437936584,31.8013203435596)) ;
#81484 = CARTESIAN_POINT('Ctrl Pts',(50.3915513141507,248.312651528491,31.8013203435596)) ;
#81485 = CARTESIAN_POINT('Ctrl Pts',(50.31499221335,248.292422193891,31.8013203435596)) ;
#81486 = CARTESIAN_POINT('Ctrl Pts',(50.8825961108042,248.366092821008,31.8372242596007)) ;
#81487 = CARTESIAN_POINT('Ctrl Pts',(50.7801147995828,248.365003869109,31.8372242596007)) ;
#81488 = CARTESIAN_POINT('Ctrl Pts',(50.6724206638963,248.36479492292,31.8372242596007)) ;
#81489 = CARTESIAN_POINT('Ctrl Pts',(50.471719498392,248.334437936584,31.8372242596007)) ;
#81490 = CARTESIAN_POINT('Ctrl Pts',(50.3915513141507,248.312651528491,31.8372242596007)) ;
#81491 = CARTESIAN_POINT('Ctrl Pts',(50.31499221335,248.292422193891,31.8372242596007)) ;
#81492 = CARTESIAN_POINT('Ctrl Pts',(50.8829165559117,248.335935717821,31.8993563735458)) ;
#81493 = CARTESIAN_POINT('Ctrl Pts',(50.7804359845514,248.334789190028,31.8993563735458)) ;
#81494 = CARTESIAN_POINT('Ctrl Pts',(50.6739766272416,248.334513975409,31.8993563735458)) ;
#81495 = CARTESIAN_POINT('Ctrl Pts',(50.4785264203756,248.304964355459,31.8993563735458)) ;
#81496 = CARTESIAN_POINT('Ctrl Pts',(50.3992728553965,248.283451733373,31.8993563735458)) ;
#81497 = CARTESIAN_POINT('Ctrl Pts',(50.3226967032828,248.263264100802,31.8993563735458)) ;
#81498 = CARTESIAN_POINT('Ctrl Pts',(50.8835850255371,248.273026011925,31.9213203435596)) ;
#81499 = CARTESIAN_POINT('Ctrl Pts',(50.7811041507587,248.271903096087,31.9213203435596)) ;
#81500 = CARTESIAN_POINT('Ctrl Pts',(50.6772024747733,248.271387553944,31.9213203435596)) ;
#81501 = CARTESIAN_POINT('Ctrl Pts',(50.4927328800327,248.243483059088,31.9213203435596)) ;
#81502 = CARTESIAN_POINT('Ctrl Pts',(50.4153379366858,248.22264313048,31.9213203435596)) ;
#81503 = CARTESIAN_POINT('Ctrl Pts',(50.3387687773397,248.202438395848,31.9213203435596)) ;
#81504 = CARTESIAN_POINT('Ctrl Pts',(50.8838711418303,248.246099594967,31.9213203435596)) ;
#81505 = CARTESIAN_POINT('Ctrl Pts',(50.7813898306089,248.245010643067,31.9213203435596)) ;
#81506 = CARTESIAN_POINT('Ctrl Pts',(50.678579872875,248.244375290024,31.9213203435596)) ;
#81507 = CARTESIAN_POINT('Ctrl Pts',(50.4988146088647,248.217168446757,31.9213203435596)) ;
#81508 = CARTESIAN_POINT('Ctrl Pts',(50.4222069973681,248.196633301102,31.9213203435596)) ;
#81509 = CARTESIAN_POINT('Ctrl Pts',(50.3456478965673,248.176403966502,31.9213203435596)) ;
#81510 = CARTESIAN_POINT('Ctrl Pts',(50.3549449524769,248.178861357243,31.9213203435596)) ;
#81511 = CARTESIAN_POINT('Ctrl Pts',(50.4284115903355,248.198281497898,31.9213203435596)) ;
#81512 = CARTESIAN_POINT('Ctrl Pts',(50.5019861952148,248.217648455246,31.9213203435596)) ;
#81513 = CARTESIAN_POINT('Ctrl Pts',(50.6783454900482,248.244339817004,31.9213203435596)) ;
#81514 = CARTESIAN_POINT('Ctrl Pts',(50.7809146033543,248.245007627582,31.9213203435596)) ;
#81515 = CARTESIAN_POINT('Ctrl Pts',(50.8831605632216,248.246092051596,31.9213203435596)) ;
#81516 = CARTESIAN_POINT('Origin',(53.7,239.383507185188,31.9213203435596)) ;
#81517 = CARTESIAN_POINT('Origin',(68.7473528137424,242.977647186258,31.7413203435596)) ;
#81518 = CARTESIAN_POINT('',(68.3897056274848,242.62,31.6213203435596)) ;
#81519 = CARTESIAN_POINT('',(69.6,243.830294372515,31.6213203435596)) ;
#81520 = CARTESIAN_POINT('',(68.7473528137424,242.977647186258,31.6213203435596)) ;
#81521 = CARTESIAN_POINT('',(69.6,244.,31.7413203435596)) ;
#81522 = CARTESIAN_POINT('Origin',(69.6,243.830294372515,31.7413203435596)) ;
#81523 = CARTESIAN_POINT('',(68.1,242.5,31.7413203435596)) ;
#81524 = CARTESIAN_POINT('',(68.6625,243.0625,31.7413203435596)) ;
#81525 = CARTESIAN_POINT('Origin',(68.3897056274848,242.62,31.7413203435596)) ;
#81526 = CARTESIAN_POINT('Origin',(69.7026471862576,243.727647186258,31.7413203435596)) ;
#81527 = CARTESIAN_POINT('',(71.1,242.5,31.7413203435596)) ;
#81528 = CARTESIAN_POINT('',(69.7875,243.8125,31.7413203435596)) ;
#81529 = CARTESIAN_POINT('',(70.8102943725152,242.62,31.6213203435596)) ;
#81530 = CARTESIAN_POINT('',(69.7026471862576,243.727647186258,31.6213203435596)) ;
#81531 = CARTESIAN_POINT('Origin',(70.8102943725152,242.62,31.7413203435596)) ;
#81532 = CARTESIAN_POINT('Origin',(70.35,242.62,31.7413203435596)) ;
#81533 = CARTESIAN_POINT('',(70.35,242.5,31.7413203435596)) ;
#81534 = CARTESIAN_POINT('',(70.35,242.62,31.6213203435596)) ;
#81535 = CARTESIAN_POINT('Origin',(71.1,242.5,31.9213203435596)) ;
#81536 = CARTESIAN_POINT('',(68.1,242.5,31.8013203435596)) ;
#81537 = CARTESIAN_POINT('',(68.1,242.5,31.9213203435596)) ;
#81538 = CARTESIAN_POINT('',(71.1,242.5,31.8013203435596)) ;
#81539 = CARTESIAN_POINT('',(62.4,242.5,31.8013203435596)) ;
#81540 = CARTESIAN_POINT('',(71.1,242.5,31.9213203435596)) ;
#81541 = CARTESIAN_POINT('Origin',(68.1,242.5,31.9213203435596)) ;
#81542 = CARTESIAN_POINT('',(69.6,244.,31.8013203435596)) ;
#81543 = CARTESIAN_POINT('',(69.6,244.,31.9213203435596)) ;
#81544 = CARTESIAN_POINT('',(63.720876796297,238.120876796297,31.8013203435596)) ;
#81545 = CARTESIAN_POINT('Origin',(69.6,243.25,31.6213203435596)) ;
#81546 = CARTESIAN_POINT('Origin',(68.22,240.125,31.7413203435596)) ;
#81547 = CARTESIAN_POINT('',(68.22,240.12,31.6213203435596)) ;
#81548 = CARTESIAN_POINT('',(68.22,240.38,31.6213203435596)) ;
#81549 = CARTESIAN_POINT('',(68.22,240.125,31.6213203435596)) ;
#81550 = CARTESIAN_POINT('',(68.1,240.5,31.7413203435596)) ;
#81551 = CARTESIAN_POINT('Origin',(68.22,240.38,31.7413203435596)) ;
#81552 = CARTESIAN_POINT('',(68.1,240.,31.7413203435596)) ;
#81553 = CARTESIAN_POINT('',(68.1,240.125,31.7413203435596)) ;
#81554 = CARTESIAN_POINT('Origin',(68.22,240.12,31.7413203435596)) ;
#81555 = CARTESIAN_POINT('Origin',(68.85,240.38,31.7413203435596)) ;
#81556 = CARTESIAN_POINT('',(71.1,240.5,31.7413203435596)) ;
#81557 = CARTESIAN_POINT('',(68.85,240.5,31.7413203435596)) ;
#81558 = CARTESIAN_POINT('',(70.98,240.38,31.6213203435596)) ;
#81559 = CARTESIAN_POINT('',(68.85,240.38,31.6213203435596)) ;
#81560 = CARTESIAN_POINT('Origin',(70.98,240.38,31.7413203435596)) ;
#81561 = CARTESIAN_POINT('Origin',(70.98,240.375,31.7413203435596)) ;
#81562 = CARTESIAN_POINT('',(71.1,240.,31.7413203435596)) ;
#81563 = CARTESIAN_POINT('',(71.1,240.375,31.7413203435596)) ;
#81564 = CARTESIAN_POINT('',(70.98,240.12,31.6213203435596)) ;
#81565 = CARTESIAN_POINT('',(70.98,240.375,31.6213203435596)) ;
#81566 = CARTESIAN_POINT('Origin',(70.98,240.12,31.7413203435596)) ;
#81567 = CARTESIAN_POINT('Origin',(70.35,240.12,31.7413203435596)) ;
#81568 = CARTESIAN_POINT('',(70.35,240.,31.7413203435596)) ;
#81569 = CARTESIAN_POINT('',(70.35,240.12,31.6213203435596)) ;
#81570 = CARTESIAN_POINT('Origin',(71.1,240.,31.9213203435596)) ;
#81571 = CARTESIAN_POINT('',(68.1,240.,31.8013203435596)) ;
#81572 = CARTESIAN_POINT('',(68.1,240.,31.9213203435596)) ;
#81573 = CARTESIAN_POINT('',(71.1,240.,31.8013203435596)) ;
#81574 = CARTESIAN_POINT('',(62.4,240.,31.8013203435596)) ;
#81575 = CARTESIAN_POINT('',(71.1,240.,31.9213203435596)) ;
#81576 = CARTESIAN_POINT('Origin',(68.1,240.,31.9213203435596)) ;
#81577 = CARTESIAN_POINT('',(68.1,240.5,31.8013203435596)) ;
#81578 = CARTESIAN_POINT('',(68.1,240.5,31.9213203435596)) ;
#81579 = CARTESIAN_POINT('',(68.1,239.691753592594,31.8013203435596)) ;
#81580 = CARTESIAN_POINT('Origin',(69.6,240.25,31.6213203435596)) ;
#81581 = CARTESIAN_POINT('Origin',(69.4973528137424,236.772352813742,31.7413203435596)) ;
#81582 = CARTESIAN_POINT('',(69.6,236.669705627485,31.6213203435596)) ;
#81583 = CARTESIAN_POINT('',(68.3897056274848,237.88,31.6213203435596)) ;
#81584 = CARTESIAN_POINT('',(69.4973528137424,236.772352813742,31.6213203435596)) ;
#81585 = CARTESIAN_POINT('',(68.1,238.,31.7413203435596)) ;
#81586 = CARTESIAN_POINT('Origin',(68.3897056274848,237.88,31.7413203435596)) ;
#81587 = CARTESIAN_POINT('',(69.6,236.5,31.7413203435596)) ;
#81588 = CARTESIAN_POINT('',(69.4125,236.6875,31.7413203435596)) ;
#81589 = CARTESIAN_POINT('Origin',(69.6,236.669705627485,31.7413203435596)) ;
#81590 = CARTESIAN_POINT('Origin',(68.85,237.88,31.7413203435596)) ;
#81591 = CARTESIAN_POINT('',(71.1,238.,31.7413203435596)) ;
#81592 = CARTESIAN_POINT('',(68.85,238.,31.7413203435596)) ;
#81593 = CARTESIAN_POINT('',(70.8102943725152,237.88,31.6213203435596)) ;
#81594 = CARTESIAN_POINT('',(68.85,237.88,31.6213203435596)) ;
#81595 = CARTESIAN_POINT('Origin',(70.8102943725152,237.88,31.7413203435596)) ;
#81596 = CARTESIAN_POINT('Origin',(70.4526471862576,237.522352813742,31.7413203435596)) ;
#81597 = CARTESIAN_POINT('',(70.5375,237.4375,31.7413203435596)) ;
#81598 = CARTESIAN_POINT('',(70.4526471862576,237.522352813742,31.6213203435596)) ;
#81599 = CARTESIAN_POINT('Origin',(71.1,238.,31.9213203435596)) ;
#81600 = CARTESIAN_POINT('',(69.6,236.5,31.8013203435596)) ;
#81601 = CARTESIAN_POINT('',(69.6,236.5,31.9213203435596)) ;
#81602 = CARTESIAN_POINT('',(71.1,238.,31.8013203435596)) ;
#81603 = CARTESIAN_POINT('',(67.095876796297,233.995876796297,31.8013203435596)) ;
#81604 = CARTESIAN_POINT('',(71.1,238.,31.9213203435596)) ;
#81605 = CARTESIAN_POINT('Origin',(69.6,236.5,31.9213203435596)) ;
#81606 = CARTESIAN_POINT('',(68.1,238.,31.8013203435596)) ;
#81607 = CARTESIAN_POINT('',(68.1,238.,31.9213203435596)) ;
#81608 = CARTESIAN_POINT('',(64.9041232037029,241.195876796297,31.8013203435596)) ;
#81609 = CARTESIAN_POINT('Origin',(69.6,237.25,31.6213203435596)) ;
#81610 = CARTESIAN_POINT('Origin',(52.4941050300712,244.948850672818,31.8013203435596)) ;
#81611 = CARTESIAN_POINT('',(48.8053003149063,250.720744087106,31.9213203435596)) ;
#81612 = CARTESIAN_POINT('',(49.61999553422,249.445986003055,31.9213203435596)) ;
#81613 = CARTESIAN_POINT('',(52.4941050300712,244.948850672818,31.9213203435596)) ;
#81614 = CARTESIAN_POINT('Ctrl Pts',(49.619995533665,249.445986166465,31.9213203435595)) ;
#81615 = CARTESIAN_POINT('Ctrl Pts',(49.6203404723475,249.445987337983,31.9213203432281)) ;
#81616 = CARTESIAN_POINT('Ctrl Pts',(49.6206841195624,249.445991847541,31.9213192876678)) ;
#81617 = CARTESIAN_POINT('Ctrl Pts',(49.6271977972035,249.44614280716,31.9212785208871)) ;
#81618 = CARTESIAN_POINT('Ctrl Pts',(49.6317059524695,249.447345115284,31.9208773504705)) ;
#81619 = CARTESIAN_POINT('Ctrl Pts',(49.6380743219538,249.44937032073,31.9201693929286)) ;
#81620 = CARTESIAN_POINT('Ctrl Pts',(49.641690337665,249.451131784247,31.9195319535847)) ;
#81621 = CARTESIAN_POINT('Ctrl Pts',(49.6518044956798,249.45763877911,31.9169593737309)) ;
#81622 = CARTESIAN_POINT('Ctrl Pts',(49.6572528688844,249.463335401781,31.9144710691175)) ;
#81623 = CARTESIAN_POINT('Ctrl Pts',(49.666878845865,249.473896545401,31.9084510815192)) ;
#81624 = CARTESIAN_POINT('Ctrl Pts',(49.6712115535048,249.478917613583,31.9049863994144)) ;
#81625 = CARTESIAN_POINT('Ctrl Pts',(49.6783494210367,249.484542782463,31.8989002966151)) ;
#81626 = CARTESIAN_POINT('Ctrl Pts',(49.6834227994079,249.487937662943,31.894992295344)) ;
#81627 = CARTESIAN_POINT('Ctrl Pts',(49.6989702717527,249.491136363809,31.880164499323)) ;
#81628 = CARTESIAN_POINT('Ctrl Pts',(49.7070380162235,249.492141350405,31.8716282984031)) ;
#81629 = CARTESIAN_POINT('Ctrl Pts',(49.7162040167626,249.497712159108,31.8523734086746)) ;
#81630 = CARTESIAN_POINT('Ctrl Pts',(49.7184485652111,249.500582089905,31.8446052087515)) ;
#81631 = CARTESIAN_POINT('Ctrl Pts',(49.7208851754006,249.508221113742,31.8235840752159)) ;
#81632 = CARTESIAN_POINT('Ctrl Pts',(49.7201772727542,249.512066286148,31.812221963213)) ;
#81633 = CARTESIAN_POINT('Ctrl Pts',(49.7201772727542,249.512066286148,31.8013203435596)) ;
#81634 = CARTESIAN_POINT('Origin',(48.8053003149063,250.720744087106,31.8013203435596)) ;
#81635 = CARTESIAN_POINT('Ctrl Pts',(50.1645741624171,248.974905023649,31.8013203435596)) ;
#81636 = CARTESIAN_POINT('Ctrl Pts',(50.1628717618181,248.976605820465,31.8013203435596)) ;
#81637 = CARTESIAN_POINT('Ctrl Pts',(50.161169441236,248.978306941473,31.8013203435596)) ;
#81638 = CARTESIAN_POINT('Ctrl Pts',(50.0792906217163,249.060079868447,31.8013203435597)) ;
#81639 = CARTESIAN_POINT('Ctrl Pts',(50.0018980844143,249.137814413213,31.8013203435595)) ;
#81640 = CARTESIAN_POINT('Ctrl Pts',(49.8585796911378,249.309274633528,31.8013203435596)) ;
#81641 = CARTESIAN_POINT('Ctrl Pts',(49.7903320475991,249.408935320061,31.801320343559)) ;
#81642 = CARTESIAN_POINT('Ctrl Pts',(49.719851873712,249.512544638728,31.8013203435596)) ;
#81643 = CARTESIAN_POINT('Ctrl Pts',(49.7195269576717,249.513021952172,31.8013203435596)) ;
#81644 = CARTESIAN_POINT('Ctrl Pts',(49.7192021347817,249.513499261461,31.8013203435596)) ;
#81645 = CARTESIAN_POINT('Ctrl Pts',(50.1645741624171,248.974905023649,31.8372242596007)) ;
#81646 = CARTESIAN_POINT('Ctrl Pts',(50.1628717618181,248.976605820465,31.8372242596007)) ;
#81647 = CARTESIAN_POINT('Ctrl Pts',(50.161169441236,248.978306941473,31.8372242596007)) ;
#81648 = CARTESIAN_POINT('Ctrl Pts',(50.0792906217163,249.060079868447,31.8372242596007)) ;
#81649 = CARTESIAN_POINT('Ctrl Pts',(50.0018980844143,249.137814413213,31.8372242596006)) ;
#81650 = CARTESIAN_POINT('Ctrl Pts',(49.8585796911378,249.309274633528,31.8372242596006)) ;
#81651 = CARTESIAN_POINT('Ctrl Pts',(49.7903320475991,249.408935320061,31.8372242596001)) ;
#81652 = CARTESIAN_POINT('Ctrl Pts',(49.719851873712,249.512544638728,31.8372242596007)) ;
#81653 = CARTESIAN_POINT('Ctrl Pts',(49.7195269576717,249.513021952172,31.8372242596007)) ;
#81654 = CARTESIAN_POINT('Ctrl Pts',(49.7192021347817,249.513499261461,31.8372242596007)) ;
#81655 = CARTESIAN_POINT('Ctrl Pts',(50.1432587188193,248.953569480441,31.8993563739025)) ;
#81656 = CARTESIAN_POINT('Ctrl Pts',(50.1415558219281,248.95526983324,31.8993563739025)) ;
#81657 = CARTESIAN_POINT('Ctrl Pts',(50.1398544635708,248.956971826313,31.8993563739025)) ;
#81658 = CARTESIAN_POINT('Ctrl Pts',(50.057967123475,249.038735748406,31.8993563739025)) ;
#81659 = CARTESIAN_POINT('Ctrl Pts',(49.9798830936785,249.117126688483,31.8993563739025)) ;
#81660 = CARTESIAN_POINT('Ctrl Pts',(49.8341996896905,249.291413887079,31.8993563739025)) ;
#81661 = CARTESIAN_POINT('Ctrl Pts',(49.7653887727712,249.391960366771,31.8993563739023)) ;
#81662 = CARTESIAN_POINT('Ctrl Pts',(49.6949192354727,249.495577339479,31.8993563739025)) ;
#81663 = CARTESIAN_POINT('Ctrl Pts',(49.6945936096815,249.496053982978,31.8993563739025)) ;
#81664 = CARTESIAN_POINT('Ctrl Pts',(49.6942691558659,249.496531642236,31.8993563739025)) ;
#81665 = CARTESIAN_POINT('Ctrl Pts',(50.0987932972223,248.90906212973,31.9213203435596)) ;
#81666 = CARTESIAN_POINT('Ctrl Pts',(50.0970906038601,248.91076266462,31.9213203435596)) ;
#81667 = CARTESIAN_POINT('Ctrl Pts',(50.095388780737,248.912464241265,31.9213203435596)) ;
#81668 = CARTESIAN_POINT('Ctrl Pts',(50.0135099010427,248.994236060385,31.9213203435596)) ;
#81669 = CARTESIAN_POINT('Ctrl Pts',(49.9339632706332,249.073967528443,31.9213203435596)) ;
#81670 = CARTESIAN_POINT('Ctrl Pts',(49.7833426499648,249.254164571414,31.9213203435596)) ;
#81671 = CARTESIAN_POINT('Ctrl Pts',(49.713386826283,249.356572966886,31.9213203435597)) ;
#81672 = CARTESIAN_POINT('Ctrl Pts',(49.6429072391231,249.460181618977,31.9213203435596)) ;
#81673 = CARTESIAN_POINT('Ctrl Pts',(49.6425819221073,249.460658553386,31.9213203435596)) ;
#81674 = CARTESIAN_POINT('Ctrl Pts',(49.6422573169346,249.461136069123,31.9213203435596)) ;
#81675 = CARTESIAN_POINT('Ctrl Pts',(50.0797613456432,248.890012231782,31.9213203435596)) ;
#81676 = CARTESIAN_POINT('Ctrl Pts',(50.0780589450442,248.891713028598,31.9213203435596)) ;
#81677 = CARTESIAN_POINT('Ctrl Pts',(50.0763565126285,248.893414055885,31.9213203435596)) ;
#81678 = CARTESIAN_POINT('Ctrl Pts',(49.9944856092052,248.975193684333,31.9213203435596)) ;
#81679 = CARTESIAN_POINT('Ctrl Pts',(49.9143096240871,249.055494147431,31.9213203435596)) ;
#81680 = CARTESIAN_POINT('Ctrl Pts',(49.761575185646,249.238222792144,31.9213203435596)) ;
#81681 = CARTESIAN_POINT('Ctrl Pts',(49.6911343223267,249.341430458474,31.9213203435597)) ;
#81682 = CARTESIAN_POINT('Ctrl Pts',(49.6206450819629,249.445031517405,31.9213203435597)) ;
#81683 = CARTESIAN_POINT('Ctrl Pts',(49.620320194148,249.445508856619,31.9213203435596)) ;
#81684 = CARTESIAN_POINT('Ctrl Pts',(49.619995371258,249.445986165908,31.9213203435596)) ;
#81685 = CARTESIAN_POINT('',(50.0797613456432,248.890012231782,31.9213203435596)) ;
#81686 = CARTESIAN_POINT('Ctrl Pts',(49.6199955742298,249.445985867652,31.9213203435596)) ;
#81687 = CARTESIAN_POINT('Ctrl Pts',(49.6203203294896,249.445508657769,31.9213203435596)) ;
#81688 = CARTESIAN_POINT('Ctrl Pts',(49.6206451495996,249.445031417996,31.9213203435597)) ;
#81689 = CARTESIAN_POINT('Ctrl Pts',(49.6911343223267,249.341430458474,31.9213203435597)) ;
#81690 = CARTESIAN_POINT('Ctrl Pts',(49.761575185646,249.238222792144,31.9213203435596)) ;
#81691 = CARTESIAN_POINT('Ctrl Pts',(49.9143096240871,249.055494147431,31.9213203435596)) ;
#81692 = CARTESIAN_POINT('Ctrl Pts',(49.9944856092052,248.975193684333,31.9213203435596)) ;
#81693 = CARTESIAN_POINT('Ctrl Pts',(50.0763565126285,248.893414055885,31.9213203435596)) ;
#81694 = CARTESIAN_POINT('Ctrl Pts',(50.0780589450442,248.891713028598,31.9213203435596)) ;
#81695 = CARTESIAN_POINT('Ctrl Pts',(50.0797613456432,248.890012231782,31.9213203435596)) ;
#81696 = CARTESIAN_POINT('Ctrl Pts',(50.0797613456432,248.890012231782,31.9213203435596)) ;
#81697 = CARTESIAN_POINT('Ctrl Pts',(50.0799550565321,248.890230949474,31.9213203435596)) ;
#81698 = CARTESIAN_POINT('Ctrl Pts',(50.0801487695989,248.890449669304,31.9213192394347)) ;
#81699 = CARTESIAN_POINT('Ctrl Pts',(50.0803424810526,248.890668386944,31.921317033763)) ;
#81700 = CARTESIAN_POINT('Ctrl Pts',(50.0863819669867,248.897487509339,31.9212482658966)) ;
#81701 = CARTESIAN_POINT('Ctrl Pts',(50.0923858427197,248.904266041468,31.920113765387)) ;
#81702 = CARTESIAN_POINT('Ctrl Pts',(50.098240144254,248.910875306167,31.9179984115576)) ;
#81703 = CARTESIAN_POINT('Ctrl Pts',(50.1026283517431,248.915829411226,31.9164128062617)) ;
#81704 = CARTESIAN_POINT('Ctrl Pts',(50.1069328634758,248.920688757015,31.9142748253259)) ;
#81705 = CARTESIAN_POINT('Ctrl Pts',(50.1111024611988,248.925395931222,31.9116016099452)) ;
#81706 = CARTESIAN_POINT('Ctrl Pts',(50.1166571287938,248.93166674912,31.9080403976087)) ;
#81707 = CARTESIAN_POINT('Ctrl Pts',(50.1219117234167,248.937598907753,31.9035702316688)) ;
#81708 = CARTESIAN_POINT('Ctrl Pts',(50.1267497978321,248.943063509505,31.8982512360342)) ;
#81709 = CARTESIAN_POINT('Ctrl Pts',(50.1276721474668,248.944105302788,31.8972372016769)) ;
#81710 = CARTESIAN_POINT('Ctrl Pts',(50.1285793102163,248.945130054085,31.8961921802598)) ;
#81711 = CARTESIAN_POINT('Ctrl Pts',(50.1294703957101,248.946136786457,31.8951164031763)) ;
#81712 = CARTESIAN_POINT('Ctrl Pts',(50.1319444308956,248.948931906936,31.8921295849925)) ;
#81713 = CARTESIAN_POINT('Ctrl Pts',(50.1342946961643,248.951588289624,31.8889058568381)) ;
#81714 = CARTESIAN_POINT('Ctrl Pts',(50.1365137723335,248.954096684356,31.8854671010793)) ;
#81715 = CARTESIAN_POINT('Ctrl Pts',(50.1407310642358,248.958863818055,31.8789318423909)) ;
#81716 = CARTESIAN_POINT('Ctrl Pts',(50.1444295692805,248.963045335349,31.8716947525886)) ;
#81717 = CARTESIAN_POINT('Ctrl Pts',(50.1475706336284,248.966594182085,31.8639255828771)) ;
#81718 = CARTESIAN_POINT('Ctrl Pts',(50.1497901014565,248.969101787879,31.8584359079403)) ;
#81719 = CARTESIAN_POINT('Ctrl Pts',(50.1517308057983,248.971293070318,31.8526794530798)) ;
#81720 = CARTESIAN_POINT('Ctrl Pts',(50.1533696323212,248.973141935655,31.8467079120488)) ;
#81721 = CARTESIAN_POINT('Ctrl Pts',(50.1556680971207,248.97573498125,31.8383327871238)) ;
#81722 = CARTESIAN_POINT('Ctrl Pts',(50.1573486404184,248.977627070085,31.8296281500221)) ;
#81723 = CARTESIAN_POINT('Ctrl Pts',(50.1583591663423,248.978763132081,31.8207452397396)) ;
#81724 = CARTESIAN_POINT('Ctrl Pts',(50.1590537646987,248.979544019316,31.8146394538937)) ;
#81725 = CARTESIAN_POINT('Ctrl Pts',(50.1594312220891,248.979967107938,31.8084487630574)) ;
#81726 = CARTESIAN_POINT('Ctrl Pts',(50.1594644902513,248.980004403535,31.80221996166)) ;
#81727 = CARTESIAN_POINT('Ctrl Pts',(50.1594660914167,248.980006198537,31.8019201752897)) ;
#81728 = CARTESIAN_POINT('Ctrl Pts',(50.1594668937473,248.980007097905,31.8016203008231)) ;
#81729 = CARTESIAN_POINT('Ctrl Pts',(50.1594668937473,248.980007097905,31.8013203435596)) ;
#81730 = CARTESIAN_POINT('Ctrl Pts',(50.4787029267369,248.780825931436,31.8013203435597)) ;
#81731 = CARTESIAN_POINT('Ctrl Pts',(50.4117018449641,248.813931863473,31.8013203435597)) ;
#81732 = CARTESIAN_POINT('Ctrl Pts',(50.3493334652158,248.845229869203,31.8013203435597)) ;
#81733 = CARTESIAN_POINT('Ctrl Pts',(50.2498263991114,248.90954814415,31.8013203435596)) ;
#81734 = CARTESIAN_POINT('Ctrl Pts',(50.2061026564305,248.943426158234,31.8013203435597)) ;
#81735 = CARTESIAN_POINT('Ctrl Pts',(50.1575737020552,248.981492111274,31.8013203435596)) ;
#81736 = CARTESIAN_POINT('Ctrl Pts',(50.1556790282941,248.982976184296,31.8013203435596)) ;
#81737 = CARTESIAN_POINT('Ctrl Pts',(50.1537849828817,248.984460636374,31.8013203435596)) ;
#81738 = CARTESIAN_POINT('Ctrl Pts',(50.4787029267369,248.780825931436,31.8372242596007)) ;
#81739 = CARTESIAN_POINT('Ctrl Pts',(50.4117018449641,248.813931863473,31.8372242596007)) ;
#81740 = CARTESIAN_POINT('Ctrl Pts',(50.3493334652158,248.845229869203,31.8372242596007)) ;
#81741 = CARTESIAN_POINT('Ctrl Pts',(50.2498263991114,248.90954814415,31.8372242596007)) ;
#81742 = CARTESIAN_POINT('Ctrl Pts',(50.2061026564305,248.943426158234,31.8372242596007)) ;
#81743 = CARTESIAN_POINT('Ctrl Pts',(50.1575737020552,248.981492111274,31.8372242596007)) ;
#81744 = CARTESIAN_POINT('Ctrl Pts',(50.1556790282941,248.982976184296,31.8372242596007)) ;
#81745 = CARTESIAN_POINT('Ctrl Pts',(50.1537849828817,248.984460636374,31.8372242596007)) ;
#81746 = CARTESIAN_POINT('Ctrl Pts',(50.4653430446037,248.753787678766,31.8993563735393)) ;
#81747 = CARTESIAN_POINT('Ctrl Pts',(50.3983338831863,248.786874129495,31.8993563735393)) ;
#81748 = CARTESIAN_POINT('Ctrl Pts',(50.3347981036532,248.818711381287,31.8993563735393)) ;
#81749 = CARTESIAN_POINT('Ctrl Pts',(50.2320023038783,248.885156890167,31.8993563735392)) ;
#81750 = CARTESIAN_POINT('Ctrl Pts',(50.1874911512665,248.919683104852,31.8993563735392)) ;
#81751 = CARTESIAN_POINT('Ctrl Pts',(50.1389704723505,248.957755600037,31.8993563735392)) ;
#81752 = CARTESIAN_POINT('Ctrl Pts',(50.1370744698898,248.959238465174,31.8993563735392)) ;
#81753 = CARTESIAN_POINT('Ctrl Pts',(50.1351811121424,248.96072354406,31.8993563735392)) ;
#81754 = CARTESIAN_POINT('Ctrl Pts',(50.4374734494912,248.697384100731,31.9213203435597)) ;
#81755 = CARTESIAN_POINT('Ctrl Pts',(50.3704676015478,248.730478540772,31.9213203435597)) ;
#81756 = CARTESIAN_POINT('Ctrl Pts',(50.3044864917679,248.763398175418,31.9213203435596)) ;
#81757 = CARTESIAN_POINT('Ctrl Pts',(50.1948178799082,248.834278555724,31.9213203435596)) ;
#81758 = CARTESIAN_POINT('Ctrl Pts',(50.1486909620483,248.870172693384,31.9213203435596)) ;
#81759 = CARTESIAN_POINT('Ctrl Pts',(50.100161151985,248.908238097848,31.9213203435596)) ;
#81760 = CARTESIAN_POINT('Ctrl Pts',(50.0982658507559,248.90972158238,31.9213203435596)) ;
#81761 = CARTESIAN_POINT('Ctrl Pts',(50.0963722109961,248.911206404212,31.9213203435596)) ;
#81762 = CARTESIAN_POINT('Ctrl Pts',(50.4255447919364,248.673242416413,31.9213203435597)) ;
#81763 = CARTESIAN_POINT('Ctrl Pts',(50.3585437101636,248.706348348451,31.9213203435597)) ;
#81764 = CARTESIAN_POINT('Ctrl Pts',(50.2915142881931,248.739724202851,31.9213203435596)) ;
#81765 = CARTESIAN_POINT('Ctrl Pts',(50.1789019553601,248.812502338361,31.9213203435596)) ;
#81766 = CARTESIAN_POINT('Ctrl Pts',(50.1320879154728,248.848984582,31.9213203435596)) ;
#81767 = CARTESIAN_POINT('Ctrl Pts',(50.0835498156237,248.88704350896,31.9213203435596)) ;
#81768 = CARTESIAN_POINT('Ctrl Pts',(50.0816553910555,248.888527779704,31.9213203435596)) ;
#81769 = CARTESIAN_POINT('Ctrl Pts',(50.0797613456432,248.890012231782,31.9213203435596)) ;
#81770 = CARTESIAN_POINT('',(50.1488121427117,248.836580765127,31.9213203435596)) ;
#81771 = CARTESIAN_POINT('Ctrl Pts',(50.0797613456432,248.890012231782,31.9213203435596)) ;
#81772 = CARTESIAN_POINT('Ctrl Pts',(50.0816553910555,248.888527779704,31.9213203435596)) ;
#81773 = CARTESIAN_POINT('Ctrl Pts',(50.0835498156237,248.88704350896,31.9213203435596)) ;
#81774 = CARTESIAN_POINT('Ctrl Pts',(50.1064328415097,248.869100832722,31.9213203435596)) ;
#81775 = CARTESIAN_POINT('Ctrl Pts',(50.1274567829485,248.852661400565,31.9213203435596)) ;
#81776 = CARTESIAN_POINT('Ctrl Pts',(50.1487729722068,248.836622996822,31.9213203435596)) ;
#81777 = CARTESIAN_POINT('Ctrl Pts',(50.1488635747438,248.836554830776,31.9213203435596)) ;
#81778 = CARTESIAN_POINT('Ctrl Pts',(50.1494762260617,248.836435221396,31.9213203435596)) ;
#81779 = CARTESIAN_POINT('Ctrl Pts',(50.1500888768936,248.836315582823,31.9213193779744)) ;
#81780 = CARTESIAN_POINT('Ctrl Pts',(50.2199516118796,248.822669804373,31.9210999975431)) ;
#81781 = CARTESIAN_POINT('Ctrl Pts',(50.2932276038533,248.809136345474,31.9086382258559)) ;
#81782 = CARTESIAN_POINT('Ctrl Pts',(50.3849253203238,248.794641665557,31.8816049009698)) ;
#81783 = CARTESIAN_POINT('Ctrl Pts',(50.4175915222911,248.789807511013,31.8682131659955)) ;
#81784 = CARTESIAN_POINT('Ctrl Pts',(50.4513376409524,248.784832870319,31.845780337943)) ;
#81785 = CARTESIAN_POINT('Ctrl Pts',(50.4615810717974,248.783331501165,31.8374718315758)) ;
#81786 = CARTESIAN_POINT('Ctrl Pts',(50.4718249633557,248.7818318897,31.8237615537037)) ;
#81787 = CARTESIAN_POINT('Ctrl Pts',(50.4744069643523,248.781454197681,31.8193773446321)) ;
#81788 = CARTESIAN_POINT('Ctrl Pts',(50.4777976781207,248.780958284954,31.8103794553702)) ;
#81789 = CARTESIAN_POINT('Ctrl Pts',(50.4787029267369,248.780825931436,31.8059165081512)) ;
#81790 = CARTESIAN_POINT('Ctrl Pts',(50.4787029267369,248.780825931436,31.8013203435597)) ;
#81791 = CARTESIAN_POINT('Origin',(52.9087880530785,245.764122216876,31.8013203435596)) ;
#81792 = CARTESIAN_POINT('',(50.3204922629989,249.833352139877,31.9213203435596)) ;
#81793 = CARTESIAN_POINT('Origin',(50.3206219211603,249.83315301197,31.8013178123873)) ;
#81794 = CARTESIAN_POINT('',(49.7560530731217,250.720744087106,31.9213203435596)) ;
#81795 = CARTESIAN_POINT('',(52.9087880530785,245.764122216876,31.9213203435596)) ;
#81796 = CARTESIAN_POINT('Origin',(49.7560530731217,250.720744087106,31.8013203435596)) ;
#81797 = CARTESIAN_POINT('Ctrl Pts',(49.6160227907477,248.400697783797,31.8013203435596)) ;
#81798 = CARTESIAN_POINT('Ctrl Pts',(49.6198183561661,248.403715262998,31.8013203435596)) ;
#81799 = CARTESIAN_POINT('Ctrl Pts',(49.6236165574443,248.406731398897,31.8013203435596)) ;
#81800 = CARTESIAN_POINT('Ctrl Pts',(49.7452792733463,248.503611247398,31.8013203435596)) ;
#81801 = CARTESIAN_POINT('Ctrl Pts',(49.8575493060997,248.591032492834,31.8013203435596)) ;
#81802 = CARTESIAN_POINT('Ctrl Pts',(50.1251937816473,248.718765363451,31.8013203435596)) ;
#81803 = CARTESIAN_POINT('Ctrl Pts',(50.2970303169916,248.749913679334,31.8013203435596)) ;
#81804 = CARTESIAN_POINT('Ctrl Pts',(50.4787029267368,248.780825931436,31.8013203435596)) ;
#81805 = CARTESIAN_POINT('Ctrl Pts',(49.6160227907477,248.400697783797,31.8372242596007)) ;
#81806 = CARTESIAN_POINT('Ctrl Pts',(49.6198183561661,248.403715262998,31.8372242596007)) ;
#81807 = CARTESIAN_POINT('Ctrl Pts',(49.6236165574443,248.406731398897,31.8372242596007)) ;
#81808 = CARTESIAN_POINT('Ctrl Pts',(49.7452792733463,248.503611247398,31.8372242596006)) ;
#81809 = CARTESIAN_POINT('Ctrl Pts',(49.8575493060997,248.591032492834,31.8372242596006)) ;
#81810 = CARTESIAN_POINT('Ctrl Pts',(50.1251937816473,248.718765363451,31.8372242596007)) ;
#81811 = CARTESIAN_POINT('Ctrl Pts',(50.2970303169916,248.749913679334,31.8372242596006)) ;
#81812 = CARTESIAN_POINT('Ctrl Pts',(50.4787029267368,248.780825931436,31.8372242596007)) ;
#81813 = CARTESIAN_POINT('Ctrl Pts',(49.5972547773324,248.424305311118,31.8993563712368)) ;
#81814 = CARTESIAN_POINT('Ctrl Pts',(49.6010468963673,248.427328920395,31.8993563712368)) ;
#81815 = CARTESIAN_POINT('Ctrl Pts',(49.6048519513673,248.430333346679,31.8993563712368)) ;
#81816 = CARTESIAN_POINT('Ctrl Pts',(49.7264624062265,248.527276869617,31.8993563712368)) ;
#81817 = CARTESIAN_POINT('Ctrl Pts',(49.8405567586885,248.61634984787,31.8993563712368)) ;
#81818 = CARTESIAN_POINT('Ctrl Pts',(50.1170880290107,248.748336416003,31.8993563712368)) ;
#81819 = CARTESIAN_POINT('Ctrl Pts',(50.2918849936094,248.779783116107,31.8993563712368)) ;
#81820 = CARTESIAN_POINT('Ctrl Pts',(50.4736440074975,248.810557413234,31.8993563712368)) ;
#81821 = CARTESIAN_POINT('Ctrl Pts',(49.5581034674252,248.473552165211,31.9213203435596)) ;
#81822 = CARTESIAN_POINT('Ctrl Pts',(49.5618969998779,248.476573260445,31.9213203435596)) ;
#81823 = CARTESIAN_POINT('Ctrl Pts',(49.5656988002261,248.479583622788,31.9213203435596)) ;
#81824 = CARTESIAN_POINT('Ctrl Pts',(49.6873510258597,248.576449789539,31.9213203435596)) ;
#81825 = CARTESIAN_POINT('Ctrl Pts',(49.8050378320701,248.669116635466,31.9213203435596)) ;
#81826 = CARTESIAN_POINT('Ctrl Pts',(50.1003231440839,248.810000534578,31.9213203435596)) ;
#81827 = CARTESIAN_POINT('Ctrl Pts',(50.2813671912147,248.841748364289,31.9213203435596)) ;
#81828 = CARTESIAN_POINT('Ctrl Pts',(50.4630907693605,248.872579238991,31.9213203435596)) ;
#81829 = CARTESIAN_POINT('Ctrl Pts',(49.5413460448266,248.494630651413,31.9213203435596)) ;
#81830 = CARTESIAN_POINT('Ctrl Pts',(49.545141610245,248.497648130615,31.9213203435596)) ;
#81831 = CARTESIAN_POINT('Ctrl Pts',(49.5489391040554,248.500666073732,31.9213203435596)) ;
#81832 = CARTESIAN_POINT('Ctrl Pts',(49.6706342383944,248.597464241588,31.9213203435596)) ;
#81833 = CARTESIAN_POINT('Ctrl Pts',(49.7898232864642,248.691693931079,31.9213203435596)) ;
#81834 = CARTESIAN_POINT('Ctrl Pts',(50.0931714339411,248.836389995259,31.9213203435596)) ;
#81835 = CARTESIAN_POINT('Ctrl Pts',(50.2769011952618,248.86821337696,31.9213203435596)) ;
#81836 = CARTESIAN_POINT('Ctrl Pts',(50.458573805007,248.899125629062,31.9213203435596)) ;
#81837 = CARTESIAN_POINT('',(49.5413460448267,248.494630651413,31.9213203435596)) ;
#81838 = CARTESIAN_POINT('Ctrl Pts',(50.1487803566378,248.836532728787,31.9213203435596)) ;
#81839 = CARTESIAN_POINT('Ctrl Pts',(50.0725213308391,248.816277003213,31.9213203435596)) ;
#81840 = CARTESIAN_POINT('Ctrl Pts',(49.997874147536,248.790933504476,31.9213203435596)) ;
#81841 = CARTESIAN_POINT('Ctrl Pts',(49.7898232864642,248.691693931079,31.9213203435596)) ;
#81842 = CARTESIAN_POINT('Ctrl Pts',(49.6706342383944,248.597464241588,31.9213203435596)) ;
#81843 = CARTESIAN_POINT('Ctrl Pts',(49.5489391040554,248.500666073732,31.9213203435596)) ;
#81844 = CARTESIAN_POINT('Ctrl Pts',(49.545141610245,248.497648130615,31.9213203435596)) ;
#81845 = CARTESIAN_POINT('Ctrl Pts',(49.5413460448266,248.494630651413,31.9213203435596)) ;
#81846 = CARTESIAN_POINT('',(49.6274057472066,248.409748472578,31.8013203435596)) ;
#81847 = CARTESIAN_POINT('Ctrl Pts',(49.5413460448268,248.494630651413,31.9213203435596)) ;
#81848 = CARTESIAN_POINT('Ctrl Pts',(49.5415551337113,248.494424426691,31.9213203435596)) ;
#81849 = CARTESIAN_POINT('Ctrl Pts',(49.5417642221659,248.494218201969,31.9213192401467)) ;
#81850 = CARTESIAN_POINT('Ctrl Pts',(49.5532375457974,248.482901999561,31.9211982874866)) ;
#81851 = CARTESIAN_POINT('Ctrl Pts',(49.564495812884,248.471797885886,31.9178840333569)) ;
#81852 = CARTESIAN_POINT('Ctrl Pts',(49.5835952095543,248.452961415427,31.9066597394761)) ;
#81853 = CARTESIAN_POINT('Ctrl Pts',(49.59317857724,248.443510005046,31.8987710966051)) ;
#81854 = CARTESIAN_POINT('Ctrl Pts',(49.6097840808936,248.42713046638,31.875408144021)) ;
#81855 = CARTESIAN_POINT('Ctrl Pts',(49.6160001139493,248.420998029143,31.8624282825602)) ;
#81856 = CARTESIAN_POINT('Ctrl Pts',(49.6226237280662,248.41446363332,31.8409288459213)) ;
#81857 = CARTESIAN_POINT('Ctrl Pts',(49.6243900313392,248.412721148843,31.8332103472442)) ;
#81858 = CARTESIAN_POINT('Ctrl Pts',(49.6267809902568,248.410362500334,31.8174327379094)) ;
#81859 = CARTESIAN_POINT('Ctrl Pts',(49.6274043438977,248.40974760789,31.8093846732346)) ;
#81860 = CARTESIAN_POINT('Ctrl Pts',(49.6274043438977,248.40974760789,31.8013203435596)) ;
#81861 = CARTESIAN_POINT('Ctrl Pts',(49.6274063177084,248.409749179632,31.8013203435596)) ;
#81862 = CARTESIAN_POINT('Ctrl Pts',(49.7452798059519,248.503611662122,31.8013203435596)) ;
#81863 = CARTESIAN_POINT('Ctrl Pts',(49.8575495917875,248.591032629178,31.8013203435596)) ;
#81864 = CARTESIAN_POINT('Ctrl Pts',(50.1251937816473,248.718765363451,31.8013203435596)) ;
#81865 = CARTESIAN_POINT('Ctrl Pts',(50.2970303169916,248.749913679334,31.8013203435596)) ;
#81866 = CARTESIAN_POINT('Ctrl Pts',(50.4787029267368,248.780825931436,31.8013203435596)) ;
#81867 = CARTESIAN_POINT('Ctrl Pts',(49.3511580123827,247.683686434724,31.8013203435596)) ;
#81868 = CARTESIAN_POINT('Ctrl Pts',(49.3513811606149,247.686507812404,31.8013203435596)) ;
#81869 = CARTESIAN_POINT('Ctrl Pts',(49.351606496417,247.689330023121,31.8013203435596)) ;
#81870 = CARTESIAN_POINT('Ctrl Pts',(49.3630909791246,247.836615729966,31.8013203435595)) ;
#81871 = CARTESIAN_POINT('Ctrl Pts',(49.3759860107092,247.970275925653,31.8013203435596)) ;
#81872 = CARTESIAN_POINT('Ctrl Pts',(49.4638970144239,248.194828827023,31.8013203435596)) ;
#81873 = CARTESIAN_POINT('Ctrl Pts',(49.5415374649235,248.298874984898,31.8013203435596)) ;
#81874 = CARTESIAN_POINT('Ctrl Pts',(49.6303717987922,248.413579230883,31.8013203435596)) ;
#81875 = CARTESIAN_POINT('Ctrl Pts',(49.6333346667356,248.41741920385,31.8013203435596)) ;
#81876 = CARTESIAN_POINT('Ctrl Pts',(49.6362996924823,248.421256236275,31.8013203435596)) ;
#81877 = CARTESIAN_POINT('Ctrl Pts',(49.3511580123827,247.683686434724,31.8372242596007)) ;
#81878 = CARTESIAN_POINT('Ctrl Pts',(49.3513811606149,247.686507812404,31.8372242596007)) ;
#81879 = CARTESIAN_POINT('Ctrl Pts',(49.351606496417,247.689330023121,31.8372242596007)) ;
#81880 = CARTESIAN_POINT('Ctrl Pts',(49.3630909791246,247.836615729966,31.8372242596006)) ;
#81881 = CARTESIAN_POINT('Ctrl Pts',(49.3759860107092,247.970275925653,31.8372242596006)) ;
#81882 = CARTESIAN_POINT('Ctrl Pts',(49.4638970144239,248.194828827023,31.8372242596006)) ;
#81883 = CARTESIAN_POINT('Ctrl Pts',(49.5415374649235,248.298874984898,31.8372242596006)) ;
#81884 = CARTESIAN_POINT('Ctrl Pts',(49.6303717987922,248.413579230883,31.8372242596007)) ;
#81885 = CARTESIAN_POINT('Ctrl Pts',(49.6333346667356,248.41741920385,31.8372242596007)) ;
#81886 = CARTESIAN_POINT('Ctrl Pts',(49.6362996924823,248.421256236275,31.8372242596007)) ;
#81887 = CARTESIAN_POINT('Ctrl Pts',(49.3210931084848,247.686064326277,31.899356388327)) ;
#81888 = CARTESIAN_POINT('Ctrl Pts',(49.3213103584176,247.688889074995,31.899356388327)) ;
#81889 = CARTESIAN_POINT('Ctrl Pts',(49.3215472229959,247.69170499457,31.899356388327)) ;
#81890 = CARTESIAN_POINT('Ctrl Pts',(49.3329108418495,247.839022547426,31.8993563883269)) ;
#81891 = CARTESIAN_POINT('Ctrl Pts',(49.3458237475767,247.975989259365,31.899356388327)) ;
#81892 = CARTESIAN_POINT('Ctrl Pts',(49.4378098065694,248.210938101463,31.899356388327)) ;
#81893 = CARTESIAN_POINT('Ctrl Pts',(49.5175746100229,248.31737546829,31.899356388327)) ;
#81894 = CARTESIAN_POINT('Ctrl Pts',(49.6065149484319,248.432017131571,31.899356388327)) ;
#81895 = CARTESIAN_POINT('Ctrl Pts',(49.609462878417,248.435862398147,31.899356388327)) ;
#81896 = CARTESIAN_POINT('Ctrl Pts',(49.6124356305256,248.439696934785,31.899356388327)) ;
#81897 = CARTESIAN_POINT('Ctrl Pts',(49.2583756984854,247.69102476786,31.9213203435596)) ;
#81898 = CARTESIAN_POINT('Ctrl Pts',(49.2585953667594,247.69384813443,31.9213203435596)) ;
#81899 = CARTESIAN_POINT('Ctrl Pts',(49.2588267189017,247.696667220839,31.9213203435596)) ;
#81900 = CARTESIAN_POINT('Ctrl Pts',(49.2703008601906,247.843927023218,31.9213203435596)) ;
#81901 = CARTESIAN_POINT('Ctrl Pts',(49.2828807770222,247.987714515527,31.9213203435596)) ;
#81902 = CARTESIAN_POINT('Ctrl Pts',(49.3834849539174,248.244699535025,31.9213203435596)) ;
#81903 = CARTESIAN_POINT('Ctrl Pts',(49.4679013933208,248.355809221579,31.9213203435596)) ;
#81904 = CARTESIAN_POINT('Ctrl Pts',(49.5567283655309,248.470487025677,31.9213203435596)) ;
#81905 = CARTESIAN_POINT('Ctrl Pts',(49.5596840092843,248.474329911232,31.9213203435596)) ;
#81906 = CARTESIAN_POINT('Ctrl Pts',(49.5626535935343,248.478165471159,31.9213203435596)) ;
#81907 = CARTESIAN_POINT('Ctrl Pts',(49.2315315926766,247.693147920246,31.9213203435596)) ;
#81908 = CARTESIAN_POINT('Ctrl Pts',(49.2317547409087,247.695969297926,31.9213203435596)) ;
#81909 = CARTESIAN_POINT('Ctrl Pts',(49.2319788244617,247.698792445045,31.9213203435596)) ;
#81910 = CARTESIAN_POINT('Ctrl Pts',(49.2435604941406,247.846006907065,31.9213203435596)) ;
#81911 = CARTESIAN_POINT('Ctrl Pts',(49.2559363973039,247.992701048677,31.9213203435596)) ;
#81912 = CARTESIAN_POINT('Ctrl Pts',(49.3602487491191,248.259175969039,31.9213203435596)) ;
#81913 = CARTESIAN_POINT('Ctrl Pts',(49.4466927160512,248.372233027417,31.9213203435596)) ;
#81914 = CARTESIAN_POINT('Ctrl Pts',(49.5354156179722,248.486953981746,31.9213203435596)) ;
#81915 = CARTESIAN_POINT('Ctrl Pts',(49.53838101908,248.490793618988,31.9213203435596)) ;
#81916 = CARTESIAN_POINT('Ctrl Pts',(49.5413460448267,248.494630651413,31.9213203435596)) ;
#81917 = CARTESIAN_POINT('',(49.2315315926766,247.693147920246,31.9213203435596)) ;
#81918 = CARTESIAN_POINT('Ctrl Pts',(49.5413460448267,248.494630651413,31.9213203435596)) ;
#81919 = CARTESIAN_POINT('Ctrl Pts',(49.53838101908,248.490793618988,31.9213203435596)) ;
#81920 = CARTESIAN_POINT('Ctrl Pts',(49.5354156179722,248.486953981746,31.9213203435596)) ;
#81921 = CARTESIAN_POINT('Ctrl Pts',(49.4466927160512,248.372233027417,31.9213203435596)) ;
#81922 = CARTESIAN_POINT('Ctrl Pts',(49.3602487491191,248.259175969039,31.9213203435596)) ;
#81923 = CARTESIAN_POINT('Ctrl Pts',(49.2559363973039,247.992701048677,31.9213203435596)) ;
#81924 = CARTESIAN_POINT('Ctrl Pts',(49.2435604941406,247.846006907065,31.9213203435596)) ;
#81925 = CARTESIAN_POINT('Ctrl Pts',(49.2319788244617,247.698792445045,31.9213203435596)) ;
#81926 = CARTESIAN_POINT('Ctrl Pts',(49.2317547409087,247.695969297926,31.9213203435596)) ;
#81927 = CARTESIAN_POINT('Ctrl Pts',(49.2315315926766,247.693147920246,31.9213203435596)) ;
#81928 = CARTESIAN_POINT('',(49.3518267393442,247.692149029454,31.8013203435596)) ;
#81929 = CARTESIAN_POINT('Ctrl Pts',(49.2315315926766,247.693147920246,31.9213203435596)) ;
#81930 = CARTESIAN_POINT('Ctrl Pts',(49.2318239505491,247.693145492984,31.9213203435596)) ;
#81931 = CARTESIAN_POINT('Ctrl Pts',(49.2321163107771,247.693143065995,31.9213192394382)) ;
#81932 = CARTESIAN_POINT('Ctrl Pts',(49.2324086676693,247.693140639281,31.9213170337815)) ;
#81933 = CARTESIAN_POINT('Ctrl Pts',(49.2415098317031,247.693065094895,31.9212483709802)) ;
#81934 = CARTESIAN_POINT('Ctrl Pts',(49.2505568709384,247.692990108873,31.9201172490698)) ;
#81935 = CARTESIAN_POINT('Ctrl Pts',(49.2593794714521,247.692916421526,31.9180080056539)) ;
#81936 = CARTESIAN_POINT('Ctrl Pts',(49.2660335770399,247.692860845691,31.9164171902953)) ;
#81937 = CARTESIAN_POINT('Ctrl Pts',(49.2725604492711,247.692806003611,31.9142686983227)) ;
#81938 = CARTESIAN_POINT('Ctrl Pts',(49.2788818911616,247.692752877869,31.9115798250687)) ;
#81939 = CARTESIAN_POINT('Ctrl Pts',(49.2872630385297,247.692682442251,31.9080148404676)) ;
#81940 = CARTESIAN_POINT('Ctrl Pts',(49.2951916702454,247.692615698676,31.9035408183158)) ;
#81941 = CARTESIAN_POINT('Ctrl Pts',(49.3024934133583,247.692556314186,31.8982175686063)) ;
#81942 = CARTESIAN_POINT('Ctrl Pts',(49.3038700446628,247.692545118154,31.8972139517879)) ;
#81943 = CARTESIAN_POINT('Ctrl Pts',(49.305224326051,247.692534188902,31.8961800157529)) ;
#81944 = CARTESIAN_POINT('Ctrl Pts',(49.3065549752602,247.692523559636,31.8951159825132)) ;
#81945 = CARTESIAN_POINT('Ctrl Pts',(49.3103044615355,247.692493608626,31.8921177632971)) ;
#81946 = CARTESIAN_POINT('Ctrl Pts',(49.3138665421931,247.69246602184,31.8888807508021)) ;
#81947 = CARTESIAN_POINT('Ctrl Pts',(49.3172291832474,247.692440227635,31.8854270573049)) ;
#81948 = CARTESIAN_POINT('Ctrl Pts',(49.3235962748799,247.692391386839,31.8788875597455)) ;
#81949 = CARTESIAN_POINT('Ctrl Pts',(49.3291801942726,247.692349272201,31.8716460920431)) ;
#81950 = CARTESIAN_POINT('Ctrl Pts',(49.333919892969,247.692311699374,31.863872181942)) ;
#81951 = CARTESIAN_POINT('Ctrl Pts',(49.3372625857124,247.692285200977,31.85838959865)) ;
#81952 = CARTESIAN_POINT('Ctrl Pts',(49.3401847505064,247.692261008218,31.8526410625285)) ;
#81953 = CARTESIAN_POINT('Ctrl Pts',(49.3426515861621,247.692239389276,31.8466779100469)) ;
#81954 = CARTESIAN_POINT('Ctrl Pts',(49.3461145160436,247.692209040727,31.8383068704645)) ;
#81955 = CARTESIAN_POINT('Ctrl Pts',(49.3486435722209,247.692183923337,31.8296066607461)) ;
#81956 = CARTESIAN_POINT('Ctrl Pts',(49.3501628732842,247.69216754168,31.8207281380371)) ;
#81957 = CARTESIAN_POINT('Ctrl Pts',(49.3511547437465,247.692156846971,31.8149318250899)) ;
#81958 = CARTESIAN_POINT('Ctrl Pts',(49.3517153955676,247.692149915258,31.8090589132011)) ;
#81959 = CARTESIAN_POINT('Ctrl Pts',(49.3518117389559,247.692148725188,31.8031494394816)) ;
#81960 = CARTESIAN_POINT('Ctrl Pts',(49.3518216729152,247.69214860248,31.8025401141059)) ;
#81961 = CARTESIAN_POINT('Ctrl Pts',(49.3518266612828,247.692148540243,31.8019304006143)) ;
#81962 = CARTESIAN_POINT('Ctrl Pts',(49.3518266612828,247.692148540243,31.8013203435596)) ;
#81963 = CARTESIAN_POINT('Ctrl Pts',(49.351826324154,247.69214926056,31.8013203435596)) ;
#81964 = CARTESIAN_POINT('Ctrl Pts',(49.363091023437,247.836616189274,31.8013203435595)) ;
#81965 = CARTESIAN_POINT('Ctrl Pts',(49.3759860874712,247.970276121727,31.8013203435596)) ;
#81966 = CARTESIAN_POINT('Ctrl Pts',(49.4638968212056,248.194828333482,31.8013203435596)) ;
#81967 = CARTESIAN_POINT('Ctrl Pts',(49.5415367709703,248.298874054929,31.8013203435596)) ;
#81968 = CARTESIAN_POINT('Ctrl Pts',(49.6274052886232,248.409748827735,31.8013203435596)) ;
#81969 = CARTESIAN_POINT('Ctrl Pts',(49.5220917256399,247.081756402944,31.8013203435596)) ;
#81970 = CARTESIAN_POINT('Ctrl Pts',(49.5208165737813,247.08422041417,31.8013203435596)) ;
#81971 = CARTESIAN_POINT('Ctrl Pts',(49.5195423275549,247.086685824071,31.8013203435596)) ;
#81972 = CARTESIAN_POINT('Ctrl Pts',(49.4663642430865,247.189248746888,31.8013203435597)) ;
#81973 = CARTESIAN_POINT('Ctrl Pts',(49.4195138367936,247.282633469367,31.8013203435596)) ;
#81974 = CARTESIAN_POINT('Ctrl Pts',(49.3668547913298,247.471629570943,31.8013203435596)) ;
#81975 = CARTESIAN_POINT('Ctrl Pts',(49.3588813375332,247.577652626811,31.8013203435597)) ;
#81976 = CARTESIAN_POINT('Ctrl Pts',(49.3516526720405,247.694972349092,31.8013203435596)) ;
#81977 = CARTESIAN_POINT('Ctrl Pts',(49.3514748692129,247.697797498201,31.8013203435596)) ;
#81978 = CARTESIAN_POINT('Ctrl Pts',(49.3512986166069,247.700621873608,31.8013203435596)) ;
#81979 = CARTESIAN_POINT('Ctrl Pts',(49.5220917256399,247.081756402944,31.8372242596007)) ;
#81980 = CARTESIAN_POINT('Ctrl Pts',(49.5208165737813,247.08422041417,31.8372242596007)) ;
#81981 = CARTESIAN_POINT('Ctrl Pts',(49.5195423275549,247.086685824071,31.8372242596007)) ;
#81982 = CARTESIAN_POINT('Ctrl Pts',(49.4663642430865,247.189248746888,31.8372242596007)) ;
#81983 = CARTESIAN_POINT('Ctrl Pts',(49.4195138367936,247.282633469367,31.8372242596007)) ;
#81984 = CARTESIAN_POINT('Ctrl Pts',(49.3668547913298,247.471629570943,31.8372242596007)) ;
#81985 = CARTESIAN_POINT('Ctrl Pts',(49.3588813375332,247.577652626811,31.8372242596007)) ;
#81986 = CARTESIAN_POINT('Ctrl Pts',(49.3516526720405,247.694972349092,31.8372242596007)) ;
#81987 = CARTESIAN_POINT('Ctrl Pts',(49.3514748692129,247.697797498201,31.8372242596007)) ;
#81988 = CARTESIAN_POINT('Ctrl Pts',(49.3512986166069,247.700621873608,31.8372242596007)) ;
#81989 = CARTESIAN_POINT('Ctrl Pts',(49.4953071063915,247.067895079317,31.899356402125)) ;
#81990 = CARTESIAN_POINT('Ctrl Pts',(49.4940289586876,247.070358373031,31.899356402125)) ;
#81991 = CARTESIAN_POINT('Ctrl Pts',(49.4927605208449,247.072825291279,31.899356402125)) ;
#81992 = CARTESIAN_POINT('Ctrl Pts',(49.4395322856787,247.175364270832,31.8993564021251)) ;
#81993 = CARTESIAN_POINT('Ctrl Pts',(49.3915127800559,247.27075119156,31.899356402125)) ;
#81994 = CARTESIAN_POINT('Ctrl Pts',(49.3367241123045,247.467386546691,31.899356402125)) ;
#81995 = CARTESIAN_POINT('Ctrl Pts',(49.3287281528714,247.575768514214,31.8993564021251)) ;
#81996 = CARTESIAN_POINT('Ctrl Pts',(49.3215552662865,247.69309484099,31.899356402125)) ;
#81997 = CARTESIAN_POINT('Ctrl Pts',(49.3213716917485,247.695918082734,31.899356402125)) ;
#81998 = CARTESIAN_POINT('Ctrl Pts',(49.3211983870719,247.698743495868,31.899356402125)) ;
#81999 = CARTESIAN_POINT('Ctrl Pts',(49.4394325590996,247.038979410387,31.9213203435596)) ;
#82000 = CARTESIAN_POINT('Ctrl Pts',(49.4381556394463,247.041442998223,31.9213203435596)) ;
#82001 = CARTESIAN_POINT('Ctrl Pts',(49.436884323614,247.043909228964,31.9213203435596)) ;
#82002 = CARTESIAN_POINT('Ctrl Pts',(49.3837071618505,247.146462634709,31.9213203435596)) ;
#82003 = CARTESIAN_POINT('Ctrl Pts',(49.3331330179417,247.245909737314,31.9213203435597)) ;
#82004 = CARTESIAN_POINT('Ctrl Pts',(49.2738726758569,247.45860094103,31.9213203435596)) ;
#82005 = CARTESIAN_POINT('Ctrl Pts',(49.2659876314173,247.571865092995,31.9213203435597)) ;
#82006 = CARTESIAN_POINT('Ctrl Pts',(49.2587624951247,247.689175844789,31.9213203435596)) ;
#82007 = CARTESIAN_POINT('Ctrl Pts',(49.2585817630851,247.692000083707,31.9213203435596)) ;
#82008 = CARTESIAN_POINT('Ctrl Pts',(49.2584072499996,247.694825071459,31.9213203435596)) ;
#82009 = CARTESIAN_POINT('Ctrl Pts',(49.4155173179348,247.026603020253,31.9213203435596)) ;
#82010 = CARTESIAN_POINT('Ctrl Pts',(49.4142421660762,247.029067031478,31.9213203435596)) ;
#82011 = CARTESIAN_POINT('Ctrl Pts',(49.4129671275179,247.031532331052,31.9213203435596)) ;
#82012 = CARTESIAN_POINT('Ctrl Pts',(49.3598376892698,247.134102605098,31.9213203435596)) ;
#82013 = CARTESIAN_POINT('Ctrl Pts',(49.3081508780161,247.235268173893,31.9213203435597)) ;
#82014 = CARTESIAN_POINT('Ctrl Pts',(49.2469717443521,247.454851457692,31.9213203435596)) ;
#82015 = CARTESIAN_POINT('Ctrl Pts',(49.2391603974573,247.570198843043,31.9213203435597)) ;
#82016 = CARTESIAN_POINT('Ctrl Pts',(49.231884888391,247.687498052493,31.9213203435596)) ;
#82017 = CARTESIAN_POINT('Ctrl Pts',(49.2317078452825,247.690323544838,31.9213203435596)) ;
#82018 = CARTESIAN_POINT('Ctrl Pts',(49.2315315926766,247.693147920246,31.9213203435596)) ;
#82019 = CARTESIAN_POINT('',(49.4155173179349,247.026603020253,31.9213203435596)) ;
#82020 = CARTESIAN_POINT('Ctrl Pts',(49.2315315926766,247.693147920246,31.9213203435596)) ;
#82021 = CARTESIAN_POINT('Ctrl Pts',(49.2317078452825,247.690323544838,31.9213203435596)) ;
#82022 = CARTESIAN_POINT('Ctrl Pts',(49.231884888391,247.687498052493,31.9213203435596)) ;
#82023 = CARTESIAN_POINT('Ctrl Pts',(49.2391603974573,247.570198843043,31.9213203435597)) ;
#82024 = CARTESIAN_POINT('Ctrl Pts',(49.2469717443521,247.454851457692,31.9213203435596)) ;
#82025 = CARTESIAN_POINT('Ctrl Pts',(49.3081508780161,247.235268173893,31.9213203435597)) ;
#82026 = CARTESIAN_POINT('Ctrl Pts',(49.3598376892698,247.134102605098,31.9213203435596)) ;
#82027 = CARTESIAN_POINT('Ctrl Pts',(49.4129671275179,247.031532331052,31.9213203435596)) ;
#82028 = CARTESIAN_POINT('Ctrl Pts',(49.4142421660762,247.029067031478,31.9213203435596)) ;
#82029 = CARTESIAN_POINT('Ctrl Pts',(49.4155173179348,247.026603020253,31.9213203435596)) ;
#82030 = CARTESIAN_POINT('',(49.5182659490466,247.089147608782,31.8013203435596)) ;
#82031 = CARTESIAN_POINT('Ctrl Pts',(49.4155173179349,247.026603020253,31.9213203435597)) ;
#82032 = CARTESIAN_POINT('Ctrl Pts',(49.4157670319329,247.026755025144,31.9213203435597)) ;
#82033 = CARTESIAN_POINT('Ctrl Pts',(49.4160167483516,247.026907031361,31.9213192394375)) ;
#82034 = CARTESIAN_POINT('Ctrl Pts',(49.4162664622726,247.027059035989,31.9213170337681)) ;
#82035 = CARTESIAN_POINT('Ctrl Pts',(49.4240469768085,247.031795152474,31.9212483101556)) ;
#82036 = CARTESIAN_POINT('Ctrl Pts',(49.4317814689462,247.036503062995,31.9201152014319)) ;
#82037 = CARTESIAN_POINT('Ctrl Pts',(49.4393237342447,247.04109353787,31.9180023530773)) ;
#82038 = CARTESIAN_POINT('Ctrl Pts',(49.4449984731521,247.044547373733,31.9164126632045)) ;
#82039 = CARTESIAN_POINT('Ctrl Pts',(49.4505648075892,247.047934953336,31.9142670803829)) ;
#82040 = CARTESIAN_POINT('Ctrl Pts',(49.4559561497916,247.051216117542,31.9115828535184)) ;
#82041 = CARTESIAN_POINT('Ctrl Pts',(49.4631144221162,247.05557263324,31.9080189122668)) ;
#82042 = CARTESIAN_POINT('Ctrl Pts',(49.4698862001626,247.059693958133,31.9035462640003)) ;
#82043 = CARTESIAN_POINT('Ctrl Pts',(49.4761217118301,247.063491285742,31.898224590158)) ;
#82044 = CARTESIAN_POINT('Ctrl Pts',(49.4773000339027,247.064208865177,31.8972189556431)) ;
#82045 = CARTESIAN_POINT('Ctrl Pts',(49.4784591456912,247.064914843391,31.8961828689005)) ;
#82046 = CARTESIAN_POINT('Ctrl Pts',(49.4795979337044,247.065608567612,31.8951165526276)) ;
#82047 = CARTESIAN_POINT('Ctrl Pts',(49.4827981454019,247.067558065098,31.8921200003544)) ;
#82048 = CARTESIAN_POINT('Ctrl Pts',(49.4858380622011,247.069410896474,31.8888848938609)) ;
#82049 = CARTESIAN_POINT('Ctrl Pts',(49.4887077644748,247.071160240999,31.8854333041442)) ;
#82050 = CARTESIAN_POINT('Ctrl Pts',(49.4941434979626,247.074473814921,31.8788953709304)) ;
#82051 = CARTESIAN_POINT('Ctrl Pts',(49.4989104717773,247.077380441405,31.8716555617629)) ;
#82052 = CARTESIAN_POINT('Ctrl Pts',(49.5029578808311,247.079846150381,31.8638834627152)) ;
#82053 = CARTESIAN_POINT('Ctrl Pts',(49.5058141003531,247.081586178636,31.8583987635578)) ;
#82054 = CARTESIAN_POINT('Ctrl Pts',(49.5083114220383,247.083106343917,31.852647864799)) ;
#82055 = CARTESIAN_POINT('Ctrl Pts',(49.5104201017535,247.084388545671,31.8466822212965)) ;
#82056 = CARTESIAN_POINT('Ctrl Pts',(49.5133796477241,247.08618812434,31.8383094010603)) ;
#82057 = CARTESIAN_POINT('Ctrl Pts',(49.5155424607875,247.087499817604,31.8296073353928)) ;
#82058 = CARTESIAN_POINT('Ctrl Pts',(49.51684226662,247.088286631527,31.8207269964985)) ;
#82059 = CARTESIAN_POINT('Ctrl Pts',(49.5176934522641,247.088801881343,31.8149116533194)) ;
#82060 = CARTESIAN_POINT('Ctrl Pts',(49.5181738049218,247.089091627686,31.8090192524275)) ;
#82061 = CARTESIAN_POINT('Ctrl Pts',(49.5182538948739,247.08913993916,31.8030902043847)) ;
#82062 = CARTESIAN_POINT('Ctrl Pts',(49.518261859298,247.089144743421,31.8025005991682)) ;
#82063 = CARTESIAN_POINT('Ctrl Pts',(49.5182658583933,247.089147155091,31.8019106321131)) ;
#82064 = CARTESIAN_POINT('Ctrl Pts',(49.5182658583933,247.089147155091,31.8013203435596)) ;
#82065 = CARTESIAN_POINT('Ctrl Pts',(49.5182658425303,247.089147741163,31.8013203435596)) ;
#82066 = CARTESIAN_POINT('Ctrl Pts',(49.4663641066775,247.189249018786,31.8013203435597)) ;
#82067 = CARTESIAN_POINT('Ctrl Pts',(49.4195137987933,247.282633605752,31.8013203435596)) ;
#82068 = CARTESIAN_POINT('Ctrl Pts',(49.3668548399605,247.471629396404,31.8013203435596)) ;
#82069 = CARTESIAN_POINT('Ctrl Pts',(49.3588813667358,247.577652238505,31.8013203435597)) ;
#82070 = CARTESIAN_POINT('Ctrl Pts',(49.3518266315492,247.692149022813,31.8013203435596)) ;
#82071 = CARTESIAN_POINT('Ctrl Pts',(49.9728509295514,246.705084314165,31.8013203435596)) ;
#82072 = CARTESIAN_POINT('Ctrl Pts',(49.9695706917073,246.706685069535,31.8013203435596)) ;
#82073 = CARTESIAN_POINT('Ctrl Pts',(49.966291605231,246.708288233407,31.8013203435596)) ;
#82074 = CARTESIAN_POINT('Ctrl Pts',(49.8668375731075,246.756687889626,31.8013203435596)) ;
#82075 = CARTESIAN_POINT('Ctrl Pts',(49.7804572807525,246.80081678555,31.8013203435596)) ;
#82076 = CARTESIAN_POINT('Ctrl Pts',(49.6421980930019,246.917171131134,31.8013203435596)) ;
#82077 = CARTESIAN_POINT('Ctrl Pts',(49.5823727945931,246.998379121351,31.8013203435596)) ;
#82078 = CARTESIAN_POINT('Ctrl Pts',(49.5166663659865,247.091411852008,31.8013203435596)) ;
#82079 = CARTESIAN_POINT('Ctrl Pts',(49.5150609156944,247.09367591647,31.8013203435596)) ;
#82080 = CARTESIAN_POINT('Ctrl Pts',(49.5134574115132,247.095940874776,31.8013203435596)) ;
#82081 = CARTESIAN_POINT('Ctrl Pts',(49.9728509295514,246.705084314165,31.8372242596007)) ;
#82082 = CARTESIAN_POINT('Ctrl Pts',(49.9695706917073,246.706685069535,31.8372242596007)) ;
#82083 = CARTESIAN_POINT('Ctrl Pts',(49.966291605231,246.708288233407,31.8372242596007)) ;
#82084 = CARTESIAN_POINT('Ctrl Pts',(49.8668375731075,246.756687889626,31.8372242596006)) ;
#82085 = CARTESIAN_POINT('Ctrl Pts',(49.7804572807525,246.80081678555,31.8372242596007)) ;
#82086 = CARTESIAN_POINT('Ctrl Pts',(49.6421980930019,246.917171131134,31.8372242596007)) ;
#82087 = CARTESIAN_POINT('Ctrl Pts',(49.5823727945931,246.998379121351,31.8372242596007)) ;
#82088 = CARTESIAN_POINT('Ctrl Pts',(49.5166663659865,247.091411852008,31.8372242596007)) ;
#82089 = CARTESIAN_POINT('Ctrl Pts',(49.5150609156944,247.09367591647,31.8372242596007)) ;
#82090 = CARTESIAN_POINT('Ctrl Pts',(49.5134574115132,247.095940874776,31.8372242596007)) ;
#82091 = CARTESIAN_POINT('Ctrl Pts',(49.9596243415484,246.677980638409,31.8993564071237)) ;
#82092 = CARTESIAN_POINT('Ctrl Pts',(49.9563408931928,246.679577731124,31.8993564071237)) ;
#82093 = CARTESIAN_POINT('Ctrl Pts',(49.953067881515,246.681188239656,31.8993564071237)) ;
#82094 = CARTESIAN_POINT('Ctrl Pts',(49.8535780165042,246.729519028743,31.8993564071237)) ;
#82095 = CARTESIAN_POINT('Ctrl Pts',(49.76458783128,246.77474795192,31.8993564071237)) ;
#82096 = CARTESIAN_POINT('Ctrl Pts',(49.6190805221059,246.8971980461,31.8993564071237)) ;
#82097 = CARTESIAN_POINT('Ctrl Pts',(49.5577004345458,246.98090485912,31.8993564071237)) ;
#82098 = CARTESIAN_POINT('Ctrl Pts',(49.4920542320471,247.073989023636,31.8993564071237)) ;
#82099 = CARTESIAN_POINT('Ctrl Pts',(49.4904438528122,247.076245990223,31.8993564071237)) ;
#82100 = CARTESIAN_POINT('Ctrl Pts',(49.4888427989645,247.078514666962,31.8993564071237)) ;
#82101 = CARTESIAN_POINT('Ctrl Pts',(49.9320327688979,246.621440505869,31.9213203435596)) ;
#82102 = CARTESIAN_POINT('Ctrl Pts',(49.9287506364852,246.623039099855,31.9213203435596)) ;
#82103 = CARTESIAN_POINT('Ctrl Pts',(49.9254744022225,246.624645982205,31.9213203435597)) ;
#82104 = CARTESIAN_POINT('Ctrl Pts',(49.826031455862,246.673033136406,31.9213203435596)) ;
#82105 = CARTESIAN_POINT('Ctrl Pts',(49.7315757026825,246.720314831074,31.9213203435597)) ;
#82106 = CARTESIAN_POINT('Ctrl Pts',(49.5707926314164,246.855628276461,31.9213203435597)) ;
#82107 = CARTESIAN_POINT('Ctrl Pts',(49.5063980993641,246.944612608217,31.9213203435597)) ;
#82108 = CARTESIAN_POINT('Ctrl Pts',(49.4407050846512,247.037634688339,31.9213203435597)) ;
#82109 = CARTESIAN_POINT('Ctrl Pts',(49.4390970817449,247.039895245817,31.9213203435597)) ;
#82110 = CARTESIAN_POINT('Ctrl Pts',(49.4374950235404,247.042162398423,31.9213203435597)) ;
#82111 = CARTESIAN_POINT('Ctrl Pts',(49.920223114908,246.597240384684,31.9213203435596)) ;
#82112 = CARTESIAN_POINT('Ctrl Pts',(49.9169428770639,246.598841140054,31.9213203435596)) ;
#82113 = CARTESIAN_POINT('Ctrl Pts',(49.9136626226905,246.600443322388,31.9213203435597)) ;
#82114 = CARTESIAN_POINT('Ctrl Pts',(49.8142599722259,246.648887834106,31.9213203435596)) ;
#82115 = CARTESIAN_POINT('Ctrl Pts',(49.7174613505083,246.697007950007,31.9213203435597)) ;
#82116 = CARTESIAN_POINT('Ctrl Pts',(49.5501141329755,246.837851580331,31.9213203435597)) ;
#82117 = CARTESIAN_POINT('Ctrl Pts',(49.4844674063744,246.929105544499,31.9213203435597)) ;
#82118 = CARTESIAN_POINT('Ctrl Pts',(49.4187257048484,247.02207291095,31.9213203435597)) ;
#82119 = CARTESIAN_POINT('Ctrl Pts',(49.4171208221161,247.024338061946,31.9213203435597)) ;
#82120 = CARTESIAN_POINT('Ctrl Pts',(49.4155173179349,247.026603020253,31.9213203435597)) ;
#82121 = CARTESIAN_POINT('',(49.920223114908,246.597240384684,31.9213203435596)) ;
#82122 = CARTESIAN_POINT('Ctrl Pts',(49.4155173179349,247.026603020253,31.9213203435597)) ;
#82123 = CARTESIAN_POINT('Ctrl Pts',(49.4171208221161,247.024338061946,31.9213203435597)) ;
#82124 = CARTESIAN_POINT('Ctrl Pts',(49.4187257048484,247.02207291095,31.9213203435597)) ;
#82125 = CARTESIAN_POINT('Ctrl Pts',(49.4844674063744,246.929105544499,31.9213203435597)) ;
#82126 = CARTESIAN_POINT('Ctrl Pts',(49.5501141329755,246.837851580331,31.9213203435597)) ;
#82127 = CARTESIAN_POINT('Ctrl Pts',(49.7174613505083,246.697007950007,31.9213203435597)) ;
#82128 = CARTESIAN_POINT('Ctrl Pts',(49.8142599722259,246.648887834106,31.9213203435596)) ;
#82129 = CARTESIAN_POINT('Ctrl Pts',(49.9136626226905,246.600443322388,31.9213203435597)) ;
#82130 = CARTESIAN_POINT('Ctrl Pts',(49.9169428770639,246.598841140054,31.9213203435596)) ;
#82131 = CARTESIAN_POINT('Ctrl Pts',(49.920223114908,246.597240384684,31.9213203435596)) ;
#82132 = CARTESIAN_POINT('',(49.9630124011287,246.709884790551,31.8013203435596)) ;
#82133 = CARTESIAN_POINT('Ctrl Pts',(49.920223114908,246.597240384684,31.9213203435596)) ;
#82134 = CARTESIAN_POINT('Ctrl Pts',(49.9203270795018,246.597514062031,31.9213203435596)) ;
#82135 = CARTESIAN_POINT('Ctrl Pts',(49.9204310420858,246.597787739813,31.9213192401161)) ;
#82136 = CARTESIAN_POINT('Ctrl Pts',(49.9261452162948,246.612830383777,31.9211980829694)) ;
#82137 = CARTESIAN_POINT('Ctrl Pts',(49.9317497593604,246.627588945362,31.9178730678895)) ;
#82138 = CARTESIAN_POINT('Ctrl Pts',(49.9412579376298,246.652605293149,31.9066209866904)) ;
#82139 = CARTESIAN_POINT('Ctrl Pts',(49.9460250235365,246.665143275588,31.8987201940233)) ;
#82140 = CARTESIAN_POINT('Ctrl Pts',(49.9542795629539,246.686873772146,31.8753276927662)) ;
#82141 = CARTESIAN_POINT('Ctrl Pts',(49.9573645028934,246.695004030452,31.8623344826963)) ;
#82142 = CARTESIAN_POINT('Ctrl Pts',(49.9606452939414,246.703653016984,31.8408440931569)) ;
#82143 = CARTESIAN_POINT('Ctrl Pts',(49.9615186214591,246.705955875339,31.8331409754495)) ;
#82144 = CARTESIAN_POINT('Ctrl Pts',(49.9627008150583,246.70907318093,31.8173971266666)) ;
#82145 = CARTESIAN_POINT('Ctrl Pts',(49.9630089487856,246.70988574977,31.8093665682248)) ;
#82146 = CARTESIAN_POINT('Ctrl Pts',(49.9630089487856,246.70988574977,31.8013203435596)) ;
#82147 = CARTESIAN_POINT('Ctrl Pts',(49.9630121174873,246.709884207708,31.8013203435596)) ;
#82148 = CARTESIAN_POINT('Ctrl Pts',(49.8668361976932,246.756688592282,31.8013203435596)) ;
#82149 = CARTESIAN_POINT('Ctrl Pts',(49.7804567409035,246.80081723987,31.8013203435596)) ;
#82150 = CARTESIAN_POINT('Ctrl Pts',(49.6421982418782,246.917171005845,31.8013203435596)) ;
#82151 = CARTESIAN_POINT('Ctrl Pts',(49.582373047438,246.998378778135,31.8013203435596)) ;
#82152 = CARTESIAN_POINT('Ctrl Pts',(49.5182656747761,247.089147415072,31.8013203435596)) ;
#82153 = CARTESIAN_POINT('Ctrl Pts',(50.776581773269,246.600740334078,31.8013203435596)) ;
#82154 = CARTESIAN_POINT('Ctrl Pts',(50.6130596458297,246.602023320729,31.8013203435596)) ;
#82155 = CARTESIAN_POINT('Ctrl Pts',(50.4553670282039,246.603946729355,31.8013203435597)) ;
#82156 = CARTESIAN_POINT('Ctrl Pts',(50.1936350043753,246.645974976166,31.8013203435596)) ;
#82157 = CARTESIAN_POINT('Ctrl Pts',(50.0804419933617,246.677083602446,31.8013203435597)) ;
#82158 = CARTESIAN_POINT('Ctrl Pts',(49.9595007821451,246.710865673262,31.8013203435596)) ;
#82159 = CARTESIAN_POINT('Ctrl Pts',(49.9559857966182,246.711845543641,31.8013203435596)) ;
#82160 = CARTESIAN_POINT('Ctrl Pts',(49.9524714701496,246.712826039435,31.8013203435596)) ;
#82161 = CARTESIAN_POINT('Ctrl Pts',(50.776581773269,246.600740334078,31.8372242596007)) ;
#82162 = CARTESIAN_POINT('Ctrl Pts',(50.6130596458297,246.602023320729,31.8372242596007)) ;
#82163 = CARTESIAN_POINT('Ctrl Pts',(50.4553670282039,246.603946729355,31.8372242596007)) ;
#82164 = CARTESIAN_POINT('Ctrl Pts',(50.1936350043753,246.645974976166,31.8372242596007)) ;
#82165 = CARTESIAN_POINT('Ctrl Pts',(50.0804419933617,246.677083602446,31.8372242596007)) ;
#82166 = CARTESIAN_POINT('Ctrl Pts',(49.9595007821451,246.710865673262,31.8372242596007)) ;
#82167 = CARTESIAN_POINT('Ctrl Pts',(49.9559857966182,246.711845543641,31.8372242596007)) ;
#82168 = CARTESIAN_POINT('Ctrl Pts',(49.9524714701496,246.712826039435,31.8372242596007)) ;
#82169 = CARTESIAN_POINT('Ctrl Pts',(50.77634515619,246.570582476921,31.8993563978491)) ;
#82170 = CARTESIAN_POINT('Ctrl Pts',(50.6128091505364,246.571822761431,31.8993563978491)) ;
#82171 = CARTESIAN_POINT('Ctrl Pts',(50.4535114513267,246.573692836958,31.8993563978491)) ;
#82172 = CARTESIAN_POINT('Ctrl Pts',(50.1866740839135,246.616546092373,31.8993563978491)) ;
#82173 = CARTESIAN_POINT('Ctrl Pts',(50.0723303628448,246.648016517864,31.8993563978492)) ;
#82174 = CARTESIAN_POINT('Ctrl Pts',(49.951396476224,246.681817835341,31.8993563978491)) ;
#82175 = CARTESIAN_POINT('Ctrl Pts',(49.9478805798078,246.682794550961,31.8993563978491)) ;
#82176 = CARTESIAN_POINT('Ctrl Pts',(49.9443667099431,246.683776681474,31.8993563978491)) ;
#82177 = CARTESIAN_POINT('Ctrl Pts',(50.7758515568694,246.507671135686,31.9213203435597)) ;
#82178 = CARTESIAN_POINT('Ctrl Pts',(50.6123212405251,246.508928925739,31.9213203435597)) ;
#82179 = CARTESIAN_POINT('Ctrl Pts',(50.449664371721,246.510603924041,31.9213203435597)) ;
#82180 = CARTESIAN_POINT('Ctrl Pts',(50.1721428735797,246.555157055951,31.9213203435597)) ;
#82181 = CARTESIAN_POINT('Ctrl Pts',(50.0554285869099,246.587437349141,31.9213203435597)) ;
#82182 = CARTESIAN_POINT('Ctrl Pts',(49.9344891569417,246.621218012807,31.9213203435596)) ;
#82183 = CARTESIAN_POINT('Ctrl Pts',(49.9309736859494,246.62219628459,31.9213203435596)) ;
#82184 = CARTESIAN_POINT('Ctrl Pts',(49.927459628902,246.623177744958,31.9213203435596)) ;
#82185 = CARTESIAN_POINT('Ctrl Pts',(50.7756402880891,246.480744027444,31.9213203435597)) ;
#82186 = CARTESIAN_POINT('Ctrl Pts',(50.6121181606498,246.482027014095,31.9213203435597)) ;
#82187 = CARTESIAN_POINT('Ctrl Pts',(50.4480217070699,246.483604593335,31.9213203435597)) ;
#82188 = CARTESIAN_POINT('Ctrl Pts',(50.1659215683921,246.52888178823,31.9213203435597)) ;
#82189 = CARTESIAN_POINT('Ctrl Pts',(50.0481976053291,246.561517875523,31.9213203435597)) ;
#82190 = CARTESIAN_POINT('Ctrl Pts',(49.9272523439948,246.595279599443,31.9213203435596)) ;
#82191 = CARTESIAN_POINT('Ctrl Pts',(49.9237374413766,246.59625988889,31.9213203435596)) ;
#82192 = CARTESIAN_POINT('Ctrl Pts',(49.920223114908,246.597240384684,31.9213203435596)) ;
#82193 = CARTESIAN_POINT('',(50.77564028487,246.480744027482,31.9213203435597)) ;
#82194 = CARTESIAN_POINT('Ctrl Pts',(49.920223114908,246.597240384684,31.9213203435596)) ;
#82195 = CARTESIAN_POINT('Ctrl Pts',(49.9237374413766,246.59625988889,31.9213203435596)) ;
#82196 = CARTESIAN_POINT('Ctrl Pts',(49.9272523439948,246.595279599443,31.9213203435596)) ;
#82197 = CARTESIAN_POINT('Ctrl Pts',(50.0481976053291,246.561517875523,31.9213203435597)) ;
#82198 = CARTESIAN_POINT('Ctrl Pts',(50.1659215683921,246.52888178823,31.9213203435597)) ;
#82199 = CARTESIAN_POINT('Ctrl Pts',(50.4480217070699,246.483604593335,31.9213203435597)) ;
#82200 = CARTESIAN_POINT('Ctrl Pts',(50.6121181606498,246.482027014095,31.9213203435597)) ;
#82201 = CARTESIAN_POINT('Ctrl Pts',(50.7756402880891,246.480744027444,31.9213203435597)) ;
#82202 = CARTESIAN_POINT('',(50.7761110356061,246.600744027949,31.8013203435596)) ;
#82203 = CARTESIAN_POINT('Ctrl Pts',(50.7756402808459,246.480744027501,31.9213203435597)) ;
#82204 = CARTESIAN_POINT('Ctrl Pts',(50.7756414249247,246.481035667445,31.9213203435597)) ;
#82205 = CARTESIAN_POINT('Ctrl Pts',(50.7756425689877,246.481327310518,31.9213192394314)) ;
#82206 = CARTESIAN_POINT('Ctrl Pts',(50.7756793939496,246.490714130495,31.9212482468609)) ;
#82207 = CARTESIAN_POINT('Ctrl Pts',(50.7757148772581,246.499754942601,31.9201131493261)) ;
#82208 = CARTESIAN_POINT('Ctrl Pts',(50.7757752384286,246.515127192197,31.9164226980159)) ;
#82209 = CARTESIAN_POINT('Ctrl Pts',(50.7758005091845,246.521560106118,31.9143041430243)) ;
#82210 = CARTESIAN_POINT('Ctrl Pts',(50.7758578779052,246.536167028899,31.90810382497)) ;
#82211 = CARTESIAN_POINT('Ctrl Pts',(50.7758889840361,246.544088046079,31.903638902298)) ;
#82212 = CARTESIAN_POINT('Ctrl Pts',(50.7759230860527,246.552806936408,31.8972878004598)) ;
#82213 = CARTESIAN_POINT('Ctrl Pts',(50.7759285564978,246.554206855326,31.8962181513507)) ;
#82214 = CARTESIAN_POINT('Ctrl Pts',(50.7759483201422,246.559270573818,31.8921590556894)) ;
#82215 = CARTESIAN_POINT('Ctrl Pts',(50.7759619611503,246.562777498341,31.8889698646365)) ;
#82216 = CARTESIAN_POINT('Ctrl Pts',(50.7759995646949,246.57245412009,31.8790406793499)) ;
#82217 = CARTESIAN_POINT('Ctrl Pts',(50.7760212186874,246.578035503319,31.871809093448)) ;
#82218 = CARTESIAN_POINT('Ctrl Pts',(50.77605281931,246.586134096496,31.8585433129843)) ;
#82219 = CARTESIAN_POINT('Ctrl Pts',(50.7760643339462,246.589069672085,31.8527726268368)) ;
#82220 = CARTESIAN_POINT('Ctrl Pts',(50.7760878139232,246.595013606618,31.8384079767118)) ;
#82221 = CARTESIAN_POINT('Ctrl Pts',(50.7760979872128,246.597546326518,31.8296999420229)) ;
#82222 = CARTESIAN_POINT('Ctrl Pts',(50.7761086558584,246.600170884711,31.8143916078104)) ;
#82223 = CARTESIAN_POINT('Ctrl Pts',(50.776111046444,246.600744029292,31.8078756404829)) ;
#82224 = CARTESIAN_POINT('Ctrl Pts',(50.776111046444,246.600744029292,31.8013203435596)) ;
#82225 = CARTESIAN_POINT('Ctrl Pts',(50.7761110306795,246.600744027501,31.8013203435596)) ;
#82226 = CARTESIAN_POINT('Ctrl Pts',(50.7318115553004,246.601091599028,31.8013203435596)) ;
#82227 = CARTESIAN_POINT('Ctrl Pts',(50.6879330968571,246.601440518035,31.8013203435596)) ;
#82228 = CARTESIAN_POINT('Ctrl Pts',(50.6445235118033,246.602281618153,31.8013203435596)) ;
#82229 = CARTESIAN_POINT('Ctrl Pts',(50.5998048884608,246.603148082076,31.8013203435596)) ;
#82230 = CARTESIAN_POINT('Ctrl Pts',(50.5555837981124,246.604536553163,31.8013203435596)) ;
#82231 = CARTESIAN_POINT('Ctrl Pts',(50.5119042411479,246.606927166115,31.8013203435597)) ;
#82232 = CARTESIAN_POINT('Ctrl Pts',(50.4659508748484,246.609442226255,31.8013203435597)) ;
#82233 = CARTESIAN_POINT('Ctrl Pts',(50.4205968622638,246.613066290501,31.8013203435597)) ;
#82234 = CARTESIAN_POINT('Ctrl Pts',(50.3758849022658,246.618300500973,31.8013203435597)) ;
#82235 = CARTESIAN_POINT('Ctrl Pts',(50.3522226439638,246.621070525821,31.8013203435597)) ;
#82236 = CARTESIAN_POINT('Ctrl Pts',(50.3287400670188,246.624290568393,31.8013203435597)) ;
#82237 = CARTESIAN_POINT('Ctrl Pts',(50.3054426551874,246.628029171234,31.8013203435596)) ;
#82238 = CARTESIAN_POINT('Ctrl Pts',(50.300772904059,246.62877853966,31.8013203435596)) ;
#82239 = CARTESIAN_POINT('Ctrl Pts',(50.296100662629,246.629550323865,31.8013203435596)) ;
#82240 = CARTESIAN_POINT('Ctrl Pts',(50.2914257404912,246.630343819124,31.8013203435596)) ;
#82241 = CARTESIAN_POINT('Ctrl Pts',(50.2534216693473,246.636794418593,31.8013203435596)) ;
#82242 = CARTESIAN_POINT('Ctrl Pts',(50.2152410381834,246.644683702373,31.8013203435596)) ;
#82243 = CARTESIAN_POINT('Ctrl Pts',(50.1767784263017,246.653607486108,31.8013203435596)) ;
#82244 = CARTESIAN_POINT('Ctrl Pts',(50.1411378791258,246.661876517243,31.8013203435596)) ;
#82245 = CARTESIAN_POINT('Ctrl Pts',(50.1052552397161,246.671033999744,31.8013203435597)) ;
#82246 = CARTESIAN_POINT('Ctrl Pts',(50.06904036106,246.680715789108,31.8013203435596)) ;
#82247 = CARTESIAN_POINT('Ctrl Pts',(50.0340380172689,246.690073415929,31.8013203435596)) ;
#82248 = CARTESIAN_POINT('Ctrl Pts',(49.9987253672562,246.699921219123,31.8013203435596)) ;
#82249 = CARTESIAN_POINT('Ctrl Pts',(49.963014268976,246.709884602433,31.8013203435596)) ;
#82250 = CARTESIAN_POINT('Origin',(51.9003128398474,244.103994673298,31.8013203435596)) ;
#82251 = CARTESIAN_POINT('',(52.0203128398474,250.600744087106,31.8013203435596)) ;
#82252 = CARTESIAN_POINT('',(52.0203128398474,244.103994673298,31.8013203435596)) ;
#82253 = CARTESIAN_POINT('',(51.9003128398474,250.720744087106,31.9213203435596)) ;
#82254 = CARTESIAN_POINT('Origin',(51.9003128398474,250.720744087106,31.8013203435596)) ;
#82255 = CARTESIAN_POINT('',(51.9003128398474,248.944482161408,31.9213203435596)) ;
#82256 = CARTESIAN_POINT('',(51.9003128398474,244.103994673298,31.9213203435596)) ;
#82257 = CARTESIAN_POINT('Origin',(51.9003128398474,248.944482161408,31.8013203435596)) ;
#82258 = CARTESIAN_POINT('Origin',(53.1248221837489,246.480744027501,31.8013203435596)) ;
#82259 = CARTESIAN_POINT('',(52.6696443674977,246.480744027501,31.9213203435596)) ;
#82260 = CARTESIAN_POINT('',(53.1248221837489,246.480744027501,31.9213203435596)) ;
#82261 = CARTESIAN_POINT('',(52.5496443674977,246.600744027501,31.8013203435596)) ;
#82262 = CARTESIAN_POINT('Origin',(52.6696443674977,246.480744027501,31.8013203435596)) ;
#82263 = CARTESIAN_POINT('',(53.1248221837489,246.600744027501,31.8013203435596)) ;
#82264 = CARTESIAN_POINT('Origin',(52.6696443674977,244.992125636147,31.8013203435596)) ;
#82265 = CARTESIAN_POINT('',(52.6696443674977,250.720744087106,31.9213203435596)) ;
#82266 = CARTESIAN_POINT('',(52.6696443674977,244.992125636147,31.9213203435596)) ;
#82267 = CARTESIAN_POINT('',(52.5496443674977,250.600744087106,31.8013203435596)) ;
#82268 = CARTESIAN_POINT('Origin',(52.6696443674977,250.720744087106,31.8013203435596)) ;
#82269 = CARTESIAN_POINT('',(52.5496443674977,244.992125636147,31.8013203435596)) ;
#82270 = CARTESIAN_POINT('Origin',(52.8601564199237,250.720744087106,31.8013203435596)) ;
#82271 = CARTESIAN_POINT('',(52.8601564199237,250.600744087106,31.8013203435596)) ;
#82272 = CARTESIAN_POINT('',(52.8601564199237,250.720744087106,31.9213203435596)) ;
#82273 = CARTESIAN_POINT('Ctrl Pts',(51.1117181123309,248.84358187378,31.8013203435596)) ;
#82274 = CARTESIAN_POINT('Ctrl Pts',(51.1489587152535,248.838376895812,31.8013203435596)) ;
#82275 = CARTESIAN_POINT('Ctrl Pts',(51.1881361258901,248.832747914847,31.8013203435596)) ;
#82276 = CARTESIAN_POINT('Ctrl Pts',(51.2926832236002,248.824119255618,31.8013203435596)) ;
#82277 = CARTESIAN_POINT('Ctrl Pts',(51.3510329785516,248.824455497164,31.8013203435596)) ;
#82278 = CARTESIAN_POINT('Ctrl Pts',(51.4064264123703,248.824482175325,31.8013203435596)) ;
#82279 = CARTESIAN_POINT('Ctrl Pts',(51.1117181123309,248.84358187378,31.8372242596007)) ;
#82280 = CARTESIAN_POINT('Ctrl Pts',(51.1489587152535,248.838376895812,31.8372242596006)) ;
#82281 = CARTESIAN_POINT('Ctrl Pts',(51.1881361258901,248.832747914847,31.8372242596007)) ;
#82282 = CARTESIAN_POINT('Ctrl Pts',(51.2926832236002,248.824119255618,31.8372242596007)) ;
#82283 = CARTESIAN_POINT('Ctrl Pts',(51.3510329785516,248.824455497164,31.8372242596007)) ;
#82284 = CARTESIAN_POINT('Ctrl Pts',(51.4064264123703,248.824482175325,31.8372242596007)) ;
#82285 = CARTESIAN_POINT('Ctrl Pts',(51.1158927186706,248.873450368516,31.8993563584643)) ;
#82286 = CARTESIAN_POINT('Ctrl Pts',(51.1531387365592,248.86825773829,31.8993563584643)) ;
#82287 = CARTESIAN_POINT('Ctrl Pts',(51.191825566714,248.862704407547,31.8993563584643)) ;
#82288 = CARTESIAN_POINT('Ctrl Pts',(51.2933967401955,248.854327364572,31.8993563584643)) ;
#82289 = CARTESIAN_POINT('Ctrl Pts',(51.3510153287493,248.854633525484,31.8993563584643)) ;
#82290 = CARTESIAN_POINT('Ctrl Pts',(51.4064118875128,248.854640990038,31.8993563584643)) ;
#82291 = CARTESIAN_POINT('Ctrl Pts',(51.1246012174117,248.935757979734,31.9213203435596)) ;
#82292 = CARTESIAN_POINT('Ctrl Pts',(51.1618450140909,248.930560284486,31.9213203435596)) ;
#82293 = CARTESIAN_POINT('Ctrl Pts',(51.1995213578042,248.925197579428,31.9213203435596)) ;
#82294 = CARTESIAN_POINT('Ctrl Pts',(51.294882734956,248.917325960997,31.9213203435596)) ;
#82295 = CARTESIAN_POINT('Ctrl Pts',(51.3509863108044,248.917538881559,31.9213203435596)) ;
#82296 = CARTESIAN_POINT('Ctrl Pts',(51.4063815877211,248.917554227501,31.9213203435596)) ;
#82297 = CARTESIAN_POINT('Ctrl Pts',(51.1283286027442,248.962426695326,31.9213203435596)) ;
#82298 = CARTESIAN_POINT('Ctrl Pts',(51.1655692056668,248.957221717357,31.9213203435596)) ;
#82299 = CARTESIAN_POINT('Ctrl Pts',(51.2028151840149,248.951946048557,31.9213203435596)) ;
#82300 = CARTESIAN_POINT('Ctrl Pts',(51.2955183598921,248.944287530684,31.9213203435596)) ;
#82301 = CARTESIAN_POINT('Ctrl Pts',(51.3509751850771,248.944455483247,31.9213203435596)) ;
#82302 = CARTESIAN_POINT('Ctrl Pts',(51.4063686188957,248.944482161408,31.9213203435596)) ;
#82303 = CARTESIAN_POINT('',(51.4063686188957,248.944482161408,31.9213203435596)) ;
#82304 = CARTESIAN_POINT('Origin',(51.4063542356917,248.944482151675,31.80132034635)) ;
#82305 = CARTESIAN_POINT('',(51.1372712358084,248.961175922748,31.9213203435596)) ;
#82306 = CARTESIAN_POINT('Ctrl Pts',(51.4063686188957,248.944482161408,31.9213203435596)) ;
#82307 = CARTESIAN_POINT('Ctrl Pts',(51.3509751850771,248.944455483247,31.9213203435596)) ;
#82308 = CARTESIAN_POINT('Ctrl Pts',(51.2955183598921,248.944287530684,31.9213203435596)) ;
#82309 = CARTESIAN_POINT('Ctrl Pts',(51.2058202898626,248.951697786762,31.9213203435596)) ;
#82310 = CARTESIAN_POINT('Ctrl Pts',(51.1715427561408,248.956389821489,31.9213203435596)) ;
#82311 = CARTESIAN_POINT('Ctrl Pts',(51.1372855628255,248.961174642356,31.9213203435596)) ;
#82312 = CARTESIAN_POINT('Ctrl Pts',(51.137257201749,248.961178603667,31.9213203435596)) ;
#82313 = CARTESIAN_POINT('Ctrl Pts',(51.1371956772459,248.960893312062,31.9213203435596)) ;
#82314 = CARTESIAN_POINT('Ctrl Pts',(51.1371341474076,248.960608021905,31.9213192437131)) ;
#82315 = CARTESIAN_POINT('Ctrl Pts',(51.1337432017254,248.944886937038,31.9211981723136)) ;
#82316 = CARTESIAN_POINT('Ctrl Pts',(51.130400973083,248.929466879524,31.9178672689546)) ;
#82317 = CARTESIAN_POINT('Ctrl Pts',(51.1247267558731,248.903341551515,31.9066018385777)) ;
#82318 = CARTESIAN_POINT('Ctrl Pts',(51.1218791521258,248.890256390852,31.8986969526448)) ;
#82319 = CARTESIAN_POINT('Ctrl Pts',(51.1169394944018,248.867572728553,31.8752907032164)) ;
#82320 = CARTESIAN_POINT('Ctrl Pts',(51.1150914688031,248.859087608765,31.8622865674932)) ;
#82321 = CARTESIAN_POINT('Ctrl Pts',(51.1131294333774,248.85007188772,31.8407965086607)) ;
#82322 = CARTESIAN_POINT('Ctrl Pts',(51.1126079113899,248.847674181376,31.8331028074907)) ;
#82323 = CARTESIAN_POINT('Ctrl Pts',(51.1119020158497,248.844428030261,31.8173781185803)) ;
#82324 = CARTESIAN_POINT('Ctrl Pts',(51.1117181123326,248.84358187378,31.8093569350819)) ;
#82325 = CARTESIAN_POINT('Ctrl Pts',(51.1117181123326,248.84358187378,31.8013203435596)) ;
#82326 = CARTESIAN_POINT('Origin',(52.5531987578181,248.944482161408,31.8013203435596)) ;
#82327 = CARTESIAN_POINT('',(52.5531987578181,248.944482161408,31.9213203435596)) ;
#82328 = CARTESIAN_POINT('Ctrl Pts',(50.8716089964921,248.949993748075,31.8013203435596)) ;
#82329 = CARTESIAN_POINT('Ctrl Pts',(50.9057808422561,248.929376866944,31.8013203435596)) ;
#82330 = CARTESIAN_POINT('Ctrl Pts',(50.9426967052446,248.906058928819,31.8013203435596)) ;
#82331 = CARTESIAN_POINT('Ctrl Pts',(51.0354893826749,248.865415252228,31.8013203435596)) ;
#82332 = CARTESIAN_POINT('Ctrl Pts',(51.0754146033954,248.854384493201,31.8013203435596)) ;
#82333 = CARTESIAN_POINT('Ctrl Pts',(51.1117181123318,248.84358187378,31.8013203435596)) ;
#82334 = CARTESIAN_POINT('Ctrl Pts',(50.8716089964921,248.949993748075,31.8372242596007)) ;
#82335 = CARTESIAN_POINT('Ctrl Pts',(50.9057808422561,248.929376866944,31.8372242596006)) ;
#82336 = CARTESIAN_POINT('Ctrl Pts',(50.9426967052446,248.906058928819,31.8372242596006)) ;
#82337 = CARTESIAN_POINT('Ctrl Pts',(51.0354893826749,248.865415252228,31.8372242596006)) ;
#82338 = CARTESIAN_POINT('Ctrl Pts',(51.0754146033954,248.854384493201,31.8372242596007)) ;
#82339 = CARTESIAN_POINT('Ctrl Pts',(51.1117181123318,248.84358187378,31.8372242596007)) ;
#82340 = CARTESIAN_POINT('Ctrl Pts',(50.8871887506966,248.975816711032,31.8993563616251)) ;
#82341 = CARTESIAN_POINT('Ctrl Pts',(50.9214287856237,248.95524472293,31.8993563616251)) ;
#82342 = CARTESIAN_POINT('Ctrl Pts',(50.9575760093834,248.932477758779,31.8993563616251)) ;
#82343 = CARTESIAN_POINT('Ctrl Pts',(51.0449515126423,248.894201916256,31.8993563616251)) ;
#82344 = CARTESIAN_POINT('Ctrl Pts',(51.0840029923614,248.883367857674,31.8993563616251)) ;
#82345 = CARTESIAN_POINT('Ctrl Pts',(51.1203195626634,248.872488087803,31.8993563616251)) ;
#82346 = CARTESIAN_POINT('Ctrl Pts',(50.9196891295034,249.02968508835,31.9213203435596)) ;
#82347 = CARTESIAN_POINT('Ctrl Pts',(50.95390119474,249.009094686119,31.9213203435596)) ;
#82348 = CARTESIAN_POINT('Ctrl Pts',(50.9885819797057,248.987566509174,31.9213203435596)) ;
#82349 = CARTESIAN_POINT('Ctrl Pts',(51.0647020317792,248.954225167441,31.9213203435596)) ;
#82350 = CARTESIAN_POINT('Ctrl Pts',(51.1019515336979,248.943636451488,31.9213203435596)) ;
#82351 = CARTESIAN_POINT('Ctrl Pts',(51.1382627465158,248.93278832703,31.9213203435596)) ;
#82352 = CARTESIAN_POINT('Ctrl Pts',(50.9335998429103,249.052741667569,31.9213203435596)) ;
#82353 = CARTESIAN_POINT('Ctrl Pts',(50.9677716886743,249.032124786438,31.9213203435596)) ;
#82354 = CARTESIAN_POINT('Ctrl Pts',(51.0018475472828,249.0111416709,31.9213203435596)) ;
#82355 = CARTESIAN_POINT('Ctrl Pts',(51.0731575641017,248.97991155694,31.9213203435596)) ;
#82356 = CARTESIAN_POINT('Ctrl Pts',(51.109639224624,248.969400471664,31.9213203435596)) ;
#82357 = CARTESIAN_POINT('Ctrl Pts',(51.1459427335603,248.958597852243,31.9213203435596)) ;
#82358 = CARTESIAN_POINT('',(50.9393246912647,249.049285590905,31.9213203435556)) ;
#82359 = CARTESIAN_POINT('Ctrl Pts',(51.1372708297894,248.961174555801,31.9213203435596)) ;
#82360 = CARTESIAN_POINT('Ctrl Pts',(51.1038423419625,248.97110363352,31.9213203435596)) ;
#82361 = CARTESIAN_POINT('Ctrl Pts',(51.0703935287813,248.981122062026,31.9213203435596)) ;
#82362 = CARTESIAN_POINT('Ctrl Pts',(51.0038907454527,249.010246855353,31.9213203435596)) ;
#82363 = CARTESIAN_POINT('Ctrl Pts',(50.9715854655917,249.02979664263,31.9213203435596)) ;
#82364 = CARTESIAN_POINT('Ctrl Pts',(50.9393243991729,249.049285107378,31.9213203435596)) ;
#82365 = CARTESIAN_POINT('Ctrl Pts',(50.9393250687946,249.049284702869,31.9213203435485)) ;
#82366 = CARTESIAN_POINT('Ctrl Pts',(50.9391605620508,249.049043427891,31.9213203395065)) ;
#82367 = CARTESIAN_POINT('Ctrl Pts',(50.9389960528488,249.048802149732,31.9213192316299)) ;
#82368 = CARTESIAN_POINT('Ctrl Pts',(50.9388315444401,249.048560873149,31.9213170224859)) ;
#82369 = CARTESIAN_POINT('Ctrl Pts',(50.9337013545053,249.041036669922,31.9212481303927)) ;
#82370 = CARTESIAN_POINT('Ctrl Pts',(50.928600939845,249.033556486928,31.9201132752162)) ;
#82371 = CARTESIAN_POINT('Ctrl Pts',(50.9236275213475,249.02626262057,31.9179971542262)) ;
#82372 = CARTESIAN_POINT('Ctrl Pts',(50.9199052479004,249.020803646007,31.9164133782025)) ;
#82373 = CARTESIAN_POINT('Ctrl Pts',(50.9162538645725,249.015448621153,31.9142786664762)) ;
#82374 = CARTESIAN_POINT('Ctrl Pts',(50.9127164446231,249.010261058044,31.9116100684325)) ;
#82375 = CARTESIAN_POINT('Ctrl Pts',(50.9079966071706,249.003339500807,31.9080494651758)) ;
#82376 = CARTESIAN_POINT('Ctrl Pts',(50.9035313617411,248.996791787699,31.9035793945282)) ;
#82377 = CARTESIAN_POINT('Ctrl Pts',(50.8994175635233,248.990762394863,31.898260203771)) ;
#82378 = CARTESIAN_POINT('Ctrl Pts',(50.8986312567895,248.989609943543,31.8972434996719)) ;
#82379 = CARTESIAN_POINT('Ctrl Pts',(50.8978578245792,248.988476487402,31.8961956369672)) ;
#82380 = CARTESIAN_POINT('Ctrl Pts',(50.8970980036519,248.987363137245,31.8951168504373)) ;
#82381 = CARTESIAN_POINT('Ctrl Pts',(50.8949972230907,248.984284906199,31.8921341821659)) ;
#82382 = CARTESIAN_POINT('Ctrl Pts',(50.8930003769272,248.98136017739,31.8889152931147)) ;
#82383 = CARTESIAN_POINT('Ctrl Pts',(50.8911145493636,248.978598394777,31.8854819951251)) ;
#82384 = CARTESIAN_POINT('Ctrl Pts',(50.8875237702891,248.973339721393,31.8789446982823)) ;
#82385 = CARTESIAN_POINT('Ctrl Pts',(50.8843740883763,248.968727964332,31.8717049222366)) ;
#82386 = CARTESIAN_POINT('Ctrl Pts',(50.8817015988867,248.964812183075,31.8639327628133)) ;
#82387 = CARTESIAN_POINT('Ctrl Pts',(50.8798143452646,248.962046944002,31.8584442338293)) ;
#82388 = CARTESIAN_POINT('Ctrl Pts',(50.8781653794535,248.959629320532,31.852689084534)) ;
#82389 = CARTESIAN_POINT('Ctrl Pts',(50.8767742851082,248.95758806856,31.8467190011286)) ;
#82390 = CARTESIAN_POINT('Ctrl Pts',(50.8748228640619,248.954724609246,31.8383441943121)) ;
#82391 = CARTESIAN_POINT('Ctrl Pts',(50.8733995571067,248.952631836735,31.8296398838193)) ;
#82392 = CARTESIAN_POINT('Ctrl Pts',(50.8725450425081,248.95137357103,31.8207573318203)) ;
#82393 = CARTESIAN_POINT('Ctrl Pts',(50.8719290057467,248.950466461975,31.8143537214259)) ;
#82394 = CARTESIAN_POINT('Ctrl Pts',(50.8716089964922,248.949993748075,31.8078567218145)) ;
#82395 = CARTESIAN_POINT('Ctrl Pts',(50.8716089964922,248.949993748075,31.8013203435596)) ;
#82396 = CARTESIAN_POINT('Ctrl Pts',(50.6014861107882,249.217388231164,31.8013203435596)) ;
#82397 = CARTESIAN_POINT('Ctrl Pts',(50.6431307164356,249.165394145294,31.8013203435596)) ;
#82398 = CARTESIAN_POINT('Ctrl Pts',(50.6869793943593,249.109198386675,31.8013203435596)) ;
#82399 = CARTESIAN_POINT('Ctrl Pts',(50.7876909072677,249.01365071099,31.8013203435596)) ;
#82400 = CARTESIAN_POINT('Ctrl Pts',(50.8311952099577,248.980988011817,31.8013203435596)) ;
#82401 = CARTESIAN_POINT('Ctrl Pts',(50.8716089964922,248.949993748075,31.8013203435596)) ;
#82402 = CARTESIAN_POINT('Ctrl Pts',(50.6014861107882,249.217388231164,31.8372242596007)) ;
#82403 = CARTESIAN_POINT('Ctrl Pts',(50.6431307164356,249.165394145294,31.8372242596006)) ;
#82404 = CARTESIAN_POINT('Ctrl Pts',(50.6869793943593,249.109198386675,31.8372242596007)) ;
#82405 = CARTESIAN_POINT('Ctrl Pts',(50.7876909072677,249.01365071099,31.8372242596007)) ;
#82406 = CARTESIAN_POINT('Ctrl Pts',(50.8311952099577,248.980988011817,31.8372242596007)) ;
#82407 = CARTESIAN_POINT('Ctrl Pts',(50.8716089964922,248.949993748075,31.8372242596007)) ;
#82408 = CARTESIAN_POINT('Ctrl Pts',(50.6250252885878,249.236241909622,31.8993563630984)) ;
#82409 = CARTESIAN_POINT('Ctrl Pts',(50.6667241194215,249.184277969696,31.8993563630984)) ;
#82410 = CARTESIAN_POINT('Ctrl Pts',(50.7099286886098,249.129019052297,31.8993563630984)) ;
#82411 = CARTESIAN_POINT('Ctrl Pts',(50.8067675034066,249.037124248324,31.8993563630984)) ;
#82412 = CARTESIAN_POINT('Ctrl Pts',(50.8495672969953,249.004964549531,31.8993563630984)) ;
#82413 = CARTESIAN_POINT('Ctrl Pts',(50.8899624342195,248.97392501228,31.8993563630984)) ;
#82414 = CARTESIAN_POINT('Ctrl Pts',(50.6741295447479,249.275571909355,31.9213203435596)) ;
#82415 = CARTESIAN_POINT('Ctrl Pts',(50.7158061341191,249.223595604513,31.9213203435596)) ;
#82416 = CARTESIAN_POINT('Ctrl Pts',(50.7577733526272,249.170327174966,31.9213203435596)) ;
#82417 = CARTESIAN_POINT('Ctrl Pts',(50.8465626123779,249.086092192121,31.9213203435596)) ;
#82418 = CARTESIAN_POINT('Ctrl Pts',(50.8878461126627,249.054868153674,31.9213203435596)) ;
#82419 = CARTESIAN_POINT('Ctrl Pts',(50.9282488992462,249.023847186189,31.9213203435596)) ;
#82420 = CARTESIAN_POINT('Ctrl Pts',(50.69514699889,249.292405816036,31.9213203435596)) ;
#82421 = CARTESIAN_POINT('Ctrl Pts',(50.7367916045374,249.240411730166,31.9213203435596)) ;
#82422 = CARTESIAN_POINT('Ctrl Pts',(50.7782468577583,249.18800126692,31.9213203435596)) ;
#82423 = CARTESIAN_POINT('Ctrl Pts',(50.8635956083774,249.107051404809,31.9213203435596)) ;
#82424 = CARTESIAN_POINT('Ctrl Pts',(50.9042223688458,249.076208986737,31.9213203435596)) ;
#82425 = CARTESIAN_POINT('Ctrl Pts',(50.9446361553801,249.045214722995,31.9213203435596)) ;
#82426 = CARTESIAN_POINT('',(50.6964442987387,249.290785955645,31.9213203435596)) ;
#82427 = CARTESIAN_POINT('Ctrl Pts',(50.939324907591,249.049286844368,31.9213203435596)) ;
#82428 = CARTESIAN_POINT('Ctrl Pts',(50.9006704775887,249.078918887735,31.9213203435596)) ;
#82429 = CARTESIAN_POINT('Ctrl Pts',(50.8619758937283,249.108587639102,31.9213203435596)) ;
#82430 = CARTESIAN_POINT('Ctrl Pts',(50.7787491279644,249.187524883802,31.9213203435596)) ;
#82431 = CARTESIAN_POINT('Ctrl Pts',(50.7376533076475,249.239323955441,31.9213203435596)) ;
#82432 = CARTESIAN_POINT('Ctrl Pts',(50.6964442808212,249.290785941297,31.9213203435596)) ;
#82433 = CARTESIAN_POINT('Ctrl Pts',(50.6964442909169,249.290785882339,31.9213203435596)) ;
#82434 = CARTESIAN_POINT('Ctrl Pts',(50.6962133562336,249.290607729158,31.9213203434865)) ;
#82435 = CARTESIAN_POINT('Ctrl Pts',(50.69598224445,249.290429791841,31.9213192393805)) ;
#82436 = CARTESIAN_POINT('Ctrl Pts',(50.6957514762923,249.290251414378,31.9213170336782)) ;
#82437 = CARTESIAN_POINT('Ctrl Pts',(50.6885546406468,249.284688457595,31.9212482456927)) ;
#82438 = CARTESIAN_POINT('Ctrl Pts',(50.6814006814086,249.27915858507,31.9201131362439)) ;
#82439 = CARTESIAN_POINT('Ctrl Pts',(50.6744256288717,249.273766936644,31.9179969379934)) ;
#82440 = CARTESIAN_POINT('Ctrl Pts',(50.6692337901446,249.269753695316,31.9164217584556)) ;
#82441 = CARTESIAN_POINT('Ctrl Pts',(50.6641407016877,249.265816738188,31.914301727067)) ;
#82442 = CARTESIAN_POINT('Ctrl Pts',(50.6592058288327,249.262002122443,31.9116538260208)) ;
#82443 = CARTESIAN_POINT('Ctrl Pts',(50.6525801029015,249.256880491309,31.9080986652011)) ;
#82444 = CARTESIAN_POINT('Ctrl Pts',(50.6463125394723,249.25203575774,31.9036331060502)) ;
#82445 = CARTESIAN_POINT('Ctrl Pts',(50.6405399600747,249.247574290001,31.8983184908323)) ;
#82446 = CARTESIAN_POINT('Ctrl Pts',(50.6394156172124,249.246705316348,31.8972833470474)) ;
#82447 = CARTESIAN_POINT('Ctrl Pts',(50.6383101062439,249.245850925699,31.896215850627)) ;
#82448 = CARTESIAN_POINT('Ctrl Pts',(50.6372245343117,249.2450119811,31.895116256076)) ;
#82449 = CARTESIAN_POINT('Ctrl Pts',(50.6343027290264,249.242753970654,31.8921567090614)) ;
#82450 = CARTESIAN_POINT('Ctrl Pts',(50.6315251916768,249.240607714716,31.8889648053869)) ;
#82451 = CARTESIAN_POINT('Ctrl Pts',(50.6289010358486,249.238580050955,31.8855618965884)) ;
#82452 = CARTESIAN_POINT('Ctrl Pts',(50.6238651781714,249.234688884888,31.8790315815006)) ;
#82453 = CARTESIAN_POINT('Ctrl Pts',(50.6194480456435,249.231276008718,31.8717989312328)) ;
#82454 = CARTESIAN_POINT('Ctrl Pts',(50.6156976656245,249.228377709018,31.86403439033)) ;
#82455 = CARTESIAN_POINT('Ctrl Pts',(50.6130406872218,249.226324391843,31.8585335564466)) ;
#82456 = CARTESIAN_POINT('Ctrl Pts',(50.6107188488196,249.224529738816,31.8527646307448)) ;
#82457 = CARTESIAN_POINT('Ctrl Pts',(50.6087596898981,249.223015035295,31.8467799131912)) ;
#82458 = CARTESIAN_POINT('Ctrl Pts',(50.6060171944983,249.220894703253,31.8384023077914)) ;
#82459 = CARTESIAN_POINT('Ctrl Pts',(50.6040141086399,249.219345101931,31.8296947779775)) ;
#82460 = CARTESIAN_POINT('Ctrl Pts',(50.6028094856611,249.218412789161,31.8208091193525)) ;
#82461 = CARTESIAN_POINT('Ctrl Pts',(50.6019390438936,249.217739114501,31.8143884810815)) ;
#82462 = CARTESIAN_POINT('Ctrl Pts',(50.6014861107882,249.217388231164,31.8078740801924)) ;
#82463 = CARTESIAN_POINT('Ctrl Pts',(50.6014861107882,249.217388231164,31.8013203435596)) ;
#82464 = CARTESIAN_POINT('Ctrl Pts',(50.2194532543318,249.768610947797,31.8013199480773)) ;
#82465 = CARTESIAN_POINT('Ctrl Pts',(50.2877998866917,249.663014973847,31.8013199480773)) ;
#82466 = CARTESIAN_POINT('Ctrl Pts',(50.3569110677109,249.556127806374,31.8013199480773)) ;
#82467 = CARTESIAN_POINT('Ctrl Pts',(50.4869845254701,249.370877841352,31.8013199480774)) ;
#82468 = CARTESIAN_POINT('Ctrl Pts',(50.5445853181005,249.293693208364,31.8013199480774)) ;
#82469 = CARTESIAN_POINT('Ctrl Pts',(50.6014861107887,249.217388231164,31.8013199480774)) ;
#82470 = CARTESIAN_POINT('Ctrl Pts',(50.2194531480909,249.768610879033,31.837223998882)) ;
#82471 = CARTESIAN_POINT('Ctrl Pts',(50.2877997804396,249.663014905074,31.837223998882)) ;
#82472 = CARTESIAN_POINT('Ctrl Pts',(50.356910962284,249.556127736288,31.837223998882)) ;
#82473 = CARTESIAN_POINT('Ctrl Pts',(50.4869844233015,249.37087776663,31.837223998882)) ;
#82474 = CARTESIAN_POINT('Ctrl Pts',(50.5445852166412,249.293693132706,31.837223998882)) ;
#82475 = CARTESIAN_POINT('Ctrl Pts',(50.6014860093375,249.217388155512,31.837223998882)) ;
#82476 = CARTESIAN_POINT('Ctrl Pts',(50.2447714707482,249.784998074696,31.8993564452671)) ;
#82477 = CARTESIAN_POINT('Ctrl Pts',(50.3131207689826,249.679404050894,31.8993564452672)) ;
#82478 = CARTESIAN_POINT('Ctrl Pts',(50.3820352831163,249.572830004009,31.8993564452671)) ;
#82479 = CARTESIAN_POINT('Ctrl Pts',(50.5113322522005,249.388684776835,31.8993564452672)) ;
#82480 = CARTESIAN_POINT('Ctrl Pts',(50.5687640133161,249.311723393403,31.8993564452671)) ;
#82481 = CARTESIAN_POINT('Ctrl Pts',(50.6256628918907,249.235416911072,31.8993564452672)) ;
#82482 = CARTESIAN_POINT('Ctrl Pts',(50.2975873134094,249.819182943984,31.9213204357249)) ;
#82483 = CARTESIAN_POINT('Ctrl Pts',(50.3659355722092,249.713588032968,31.9213204357249)) ;
#82484 = CARTESIAN_POINT('Ctrl Pts',(50.4344445902855,249.607670461033,31.9213204357248)) ;
#82485 = CARTESIAN_POINT('Ctrl Pts',(50.562123374562,249.425831480274,31.9213204357248)) ;
#82486 = CARTESIAN_POINT('Ctrl Pts',(50.6191979436028,249.349332056466,31.9213204357248)) ;
#82487 = CARTESIAN_POINT('Ctrl Pts',(50.676097607319,249.273026191517,31.9213204357248)) ;
#82488 = CARTESIAN_POINT('Ctrl Pts',(50.3201933811436,249.833814642216,31.921320343559)) ;
#82489 = CARTESIAN_POINT('Ctrl Pts',(50.3885400996636,249.728218529107,31.921320343559)) ;
#82490 = CARTESIAN_POINT('Ctrl Pts',(50.4568763496929,249.622582483817,31.9213203435589)) ;
#82491 = CARTESIAN_POINT('Ctrl Pts',(50.5838627947292,249.441730893079,31.9213203435589)) ;
#82492 = CARTESIAN_POINT('Ctrl Pts',(50.6407837197257,249.365428572277,31.9213203435589)) ;
#82493 = CARTESIAN_POINT('Ctrl Pts',(50.6976845124305,249.28912359509,31.9213203435589)) ;
#82494 = CARTESIAN_POINT('Ctrl Pts',(50.6964443401006,249.290786023789,31.9213203435596)) ;
#82495 = CARTESIAN_POINT('Ctrl Pts',(50.6399566587065,249.366536825083,31.9213203435596)) ;
#82496 = CARTESIAN_POINT('Ctrl Pts',(50.5834651712519,249.442296492374,31.9213203435596)) ;
#82497 = CARTESIAN_POINT('Ctrl Pts',(50.4569815065016,249.622432033364,31.9213203435596)) ;
#82498 = CARTESIAN_POINT('Ctrl Pts',(50.3887392215019,249.727910011782,31.9213203435597)) ;
#82499 = CARTESIAN_POINT('Ctrl Pts',(50.3204922630187,249.833352139651,31.9213203435597)) ;
#82500 = CARTESIAN_POINT('Origin',(51.3622028112916,250.720744087106,31.8013203435596)) ;
#82501 = CARTESIAN_POINT('',(51.3622028112916,250.720744087106,31.9213203435596)) ;
#82502 = CARTESIAN_POINT('Ctrl Pts',(49.3518273473795,247.692149180776,31.9213203435596)) ;
#82503 = CARTESIAN_POINT('Ctrl Pts',(49.3518273473795,247.692149180776,31.5613203435596)) ;
#82504 = CARTESIAN_POINT('Ctrl Pts',(49.3625435679673,247.827639860195,31.9213203435596)) ;
#82505 = CARTESIAN_POINT('Ctrl Pts',(49.3625435679673,247.827639860195,31.5613203435596)) ;
#82506 = CARTESIAN_POINT('Ctrl Pts',(49.3836326934911,248.094280502961,31.9213203435596)) ;
#82507 = CARTESIAN_POINT('Ctrl Pts',(49.3836326934911,248.094280502961,31.5613203435596)) ;
#82508 = CARTESIAN_POINT('Ctrl Pts',(49.5470356170248,248.305739818825,31.9213203435596)) ;
#82509 = CARTESIAN_POINT('Ctrl Pts',(49.5470356170248,248.305739818825,31.5613203435596)) ;
#82510 = CARTESIAN_POINT('Ctrl Pts',(49.6274070383127,248.40974827469,31.9213203435596)) ;
#82511 = CARTESIAN_POINT('Ctrl Pts',(49.6274070383127,248.40974827469,31.5613203435596)) ;
#82512 = CARTESIAN_POINT('',(49.6274070383127,248.40974827469,31.9213203435596)) ;
#82513 = CARTESIAN_POINT('',(49.3518273473795,247.692149180776,31.9213203435596)) ;
#82514 = CARTESIAN_POINT('Ctrl Pts',(49.5182664633806,247.089148063069,31.9213203435596)) ;
#82515 = CARTESIAN_POINT('Ctrl Pts',(49.5182664633806,247.089148063069,31.5613203435596)) ;
#82516 = CARTESIAN_POINT('Ctrl Pts',(49.4697226969388,247.182950526379,31.9213203435596)) ;
#82517 = CARTESIAN_POINT('Ctrl Pts',(49.4697226969388,247.182950526379,31.5613203435596)) ;
#82518 = CARTESIAN_POINT('Ctrl Pts',(49.3717947762919,247.372179357529,31.9213203435596)) ;
#82519 = CARTESIAN_POINT('Ctrl Pts',(49.3717947762919,247.372179357529,31.5613203435596)) ;
#82520 = CARTESIAN_POINT('Ctrl Pts',(49.3585211271629,247.58488411708,31.9213203435596)) ;
#82521 = CARTESIAN_POINT('Ctrl Pts',(49.3585211271629,247.58488411708,31.5613203435596)) ;
#82522 = CARTESIAN_POINT('Ctrl Pts',(49.3518273473795,247.692149180776,31.9213203435596)) ;
#82523 = CARTESIAN_POINT('Ctrl Pts',(49.3518273473795,247.692149180776,31.5613203435596)) ;
#82524 = CARTESIAN_POINT('',(49.5182664633806,247.089148063069,31.9213203435596)) ;
#82525 = CARTESIAN_POINT('Ctrl Pts',(49.963014268976,246.709884602433,31.9213203435596)) ;
#82526 = CARTESIAN_POINT('Ctrl Pts',(49.963014268976,246.709884602433,31.5613203435596)) ;
#82527 = CARTESIAN_POINT('Ctrl Pts',(49.8744014403106,246.75312764397,31.9213203435596)) ;
#82528 = CARTESIAN_POINT('Ctrl Pts',(49.8744014403106,246.75312764397,31.5613203435596)) ;
#82529 = CARTESIAN_POINT('Ctrl Pts',(49.6937403867375,246.841290199679,31.9213203435596)) ;
#82530 = CARTESIAN_POINT('Ctrl Pts',(49.6937403867375,246.841290199679,31.5613203435596)) ;
#82531 = CARTESIAN_POINT('Ctrl Pts',(49.5774946027845,247.005487996637,31.9213203435596)) ;
#82532 = CARTESIAN_POINT('Ctrl Pts',(49.5774946027845,247.005487996637,31.5613203435596)) ;
#82533 = CARTESIAN_POINT('Ctrl Pts',(49.5182664633806,247.089148063069,31.9213203435596)) ;
#82534 = CARTESIAN_POINT('Ctrl Pts',(49.5182664633806,247.089148063069,31.5613203435596)) ;
#82535 = CARTESIAN_POINT('',(49.963014268976,246.709884602433,31.9213203435596)) ;
#82536 = CARTESIAN_POINT('Ctrl Pts',(50.7761110306795,246.600744027501,31.9213203435596)) ;
#82537 = CARTESIAN_POINT('Ctrl Pts',(50.7761110306795,246.600744027501,31.5613203435596)) ;
#82538 = CARTESIAN_POINT('Ctrl Pts',(50.618064325309,246.601984054257,31.9213203435596)) ;
#82539 = CARTESIAN_POINT('Ctrl Pts',(50.618064325309,246.601984054257,31.5613203435596)) ;
#82540 = CARTESIAN_POINT('Ctrl Pts',(50.341991448014,246.604150108612,31.9213203435596)) ;
#82541 = CARTESIAN_POINT('Ctrl Pts',(50.341991448014,246.604150108612,31.5613203435596)) ;
#82542 = CARTESIAN_POINT('Ctrl Pts',(50.0765116899345,246.678218863653,31.9213203435596)) ;
#82543 = CARTESIAN_POINT('Ctrl Pts',(50.0765116899345,246.678218863653,31.5613203435596)) ;
#82544 = CARTESIAN_POINT('Ctrl Pts',(49.963014268976,246.709884602433,31.9213203435596)) ;
#82545 = CARTESIAN_POINT('Ctrl Pts',(49.963014268976,246.709884602433,31.5613203435596)) ;
#82546 = CARTESIAN_POINT('',(50.7761110306795,246.600744027501,31.9213203435596)) ;
#82547 = CARTESIAN_POINT('Origin',(52.5496443674977,246.600744027501,31.9213203435596)) ;
#82548 = CARTESIAN_POINT('',(52.5496443674977,246.600744027501,31.9213203435596)) ;
#82549 = CARTESIAN_POINT('Origin',(52.5496443674977,250.600744087106,31.9213203435596)) ;
#82550 = CARTESIAN_POINT('',(52.5496443674977,250.600744087106,31.9213203435596)) ;
#82551 = CARTESIAN_POINT('Origin',(52.0203128398474,250.600744087106,31.9213203435596)) ;
#82552 = CARTESIAN_POINT('',(52.0203128398474,250.600744087106,31.9213203435596)) ;
#82553 = CARTESIAN_POINT('Origin',(52.0203128398474,248.824482161408,31.9213203435596)) ;
#82554 = CARTESIAN_POINT('Origin',(53.7,239.383507185188,31.9213203435596)) ;
#82555 = CARTESIAN_POINT('',(79.0999999999999,263.8,31.9213203435596)) ;
#82556 = CARTESIAN_POINT('',(79.0999999999999,259.648528137424,31.9213203435596)) ;
#82557 = CARTESIAN_POINT('',(79.0999999999999,249.391753592594,31.9213203435596)) ;
#82558 = CARTESIAN_POINT('',(78.2,263.8,31.9213203435596)) ;
#82559 = CARTESIAN_POINT('',(66.4499999999999,263.8,31.9213203435596)) ;
#82560 = CARTESIAN_POINT('',(78.2,263.763591785235,31.9213203435596)) ;
#82561 = CARTESIAN_POINT('',(78.2,252.191753592594,31.9213203435596)) ;
#82562 = CARTESIAN_POINT('',(76.5,262.026327083856,31.9213203435596)) ;
#82563 = CARTESIAN_POINT('Origin',(76.5,263.763591785235,31.9213203435596)) ;
#82564 = CARTESIAN_POINT('',(69.9,262.026327083856,31.9213203435596)) ;
#82565 = CARTESIAN_POINT('',(64.4,262.026327083856,31.9213203435596)) ;
#82566 = CARTESIAN_POINT('',(68.2,263.763591785235,31.9213203435596)) ;
#82567 = CARTESIAN_POINT('Origin',(69.9,263.763591785235,31.9213203435596)) ;
#82568 = CARTESIAN_POINT('',(68.2,263.8,31.9213203435596)) ;
#82569 = CARTESIAN_POINT('',(68.2,251.191753592594,31.9213203435596)) ;
#82570 = CARTESIAN_POINT('',(61.5,263.8,31.9213203435596)) ;
#82571 = CARTESIAN_POINT('',(66.4499999999999,263.8,31.9213203435596)) ;
#82572 = CARTESIAN_POINT('',(64.1,261.2,31.9213203435596)) ;
#82573 = CARTESIAN_POINT('Origin',(61.5,261.2,31.9213203435596)) ;
#82574 = CARTESIAN_POINT('Origin',(61.5,261.2,31.9213203435596)) ;
#82575 = CARTESIAN_POINT('',(56.2,263.8,31.9213203435596)) ;
#82576 = CARTESIAN_POINT('',(66.4499999999999,263.8,31.9213203435596)) ;
#82577 = CARTESIAN_POINT('',(56.2,263.763591785235,31.9213203435596)) ;
#82578 = CARTESIAN_POINT('',(56.2,252.191753592594,31.9213203435596)) ;
#82579 = CARTESIAN_POINT('',(54.5,262.026327083856,31.9213203435596)) ;
#82580 = CARTESIAN_POINT('Origin',(54.5,263.763591785235,31.9213203435596)) ;
#82581 = CARTESIAN_POINT('',(47.9,262.026327083856,31.9213203435596)) ;
#82582 = CARTESIAN_POINT('',(53.4,262.026327083856,31.9213203435596)) ;
#82583 = CARTESIAN_POINT('',(46.2,263.763591785235,31.9213203435596)) ;
#82584 = CARTESIAN_POINT('Origin',(47.9,263.763591785235,31.9213203435596)) ;
#82585 = CARTESIAN_POINT('',(46.2,263.8,31.9213203435596)) ;
#82586 = CARTESIAN_POINT('',(46.2,251.191753592594,31.9213203435596)) ;
#82587 = CARTESIAN_POINT('',(26.3,263.8,31.9213203435596)) ;
#82588 = CARTESIAN_POINT('',(66.4499999999999,263.8,31.9213203435596)) ;
#82589 = CARTESIAN_POINT('',(26.3,245.6,31.9213203435596)) ;
#82590 = CARTESIAN_POINT('',(26.3,252.191753592594,31.9213203435596)) ;
#82591 = CARTESIAN_POINT('',(26.8,245.1,31.9213203435596)) ;
#82592 = CARTESIAN_POINT('Origin',(26.8,245.6,31.9213203435596)) ;
#82593 = CARTESIAN_POINT('',(33.6,245.1,31.9213203435596)) ;
#82594 = CARTESIAN_POINT('',(39.95,245.1,31.9213203435596)) ;
#82595 = CARTESIAN_POINT('',(34.1,245.6,31.9213203435596)) ;
#82596 = CARTESIAN_POINT('Origin',(33.6,245.6,31.9213203435596)) ;
#82597 = CARTESIAN_POINT('',(34.1,248.9,31.9213203435596)) ;
#82598 = CARTESIAN_POINT('',(34.1000000000001,244.191753592594,31.9213203435596)) ;
#82599 = CARTESIAN_POINT('',(34.3,249.1,31.9213203435596)) ;
#82600 = CARTESIAN_POINT('Origin',(34.3,248.9,31.9213203435596)) ;
#82601 = CARTESIAN_POINT('',(46.1,249.1,31.9213203435596)) ;
#82602 = CARTESIAN_POINT('',(49.95,249.1,31.9213203435596)) ;
#82603 = CARTESIAN_POINT('',(46.3,248.9,31.9213203435596)) ;
#82604 = CARTESIAN_POINT('Origin',(46.1,248.9,31.9213203435596)) ;
#82605 = CARTESIAN_POINT('',(46.2999999999999,245.6,31.9213203435596)) ;
#82606 = CARTESIAN_POINT('',(46.2999999999999,242.191753592594,31.9213203435596)) ;
#82607 = CARTESIAN_POINT('',(46.8,245.1,31.9213203435596)) ;
#82608 = CARTESIAN_POINT('Origin',(46.8,245.6,31.9213203435596)) ;
#82609 = CARTESIAN_POINT('',(55.3573593128808,245.1,31.9213203435596)) ;
#82610 = CARTESIAN_POINT('',(39.95,245.1,31.9213203435596)) ;
#82611 = CARTESIAN_POINT('',(56.0573593128807,244.4,31.9213203435596)) ;
#82612 = CARTESIAN_POINT('Origin',(55.3573593128808,244.4,31.9213203435596)) ;
#82613 = CARTESIAN_POINT('',(56.0573593128808,226.261195155516,31.9213203435596)) ;
#82614 = CARTESIAN_POINT('',(56.0573593128807,242.191753592594,31.9213203435596)) ;
#82615 = CARTESIAN_POINT('',(56.7626663401537,224.024247053747,31.9213203435596)) ;
#82616 = CARTESIAN_POINT('Origin',(59.9573593128808,226.261195155516,31.9213203435596)) ;
#82617 = CARTESIAN_POINT('',(61.2884174438392,217.560804636007,31.9213203435596)) ;
#82618 = CARTESIAN_POINT('',(52.2889313872861,230.413402709377,31.9213203435596)) ;
#82619 = CARTESIAN_POINT('',(63.8058825236653,215.957002501029,31.9213203435596)) ;
#82620 = CARTESIAN_POINT('Origin',(64.4831104165663,219.797752737776,31.9213203435596)) ;
#82621 = CARTESIAN_POINT('',(75.3227721070991,213.926264133629,31.9213203435596)) ;
#82622 = CARTESIAN_POINT('',(56.086380506565,217.318158984277,31.9213203435596)) ;
#82623 = CARTESIAN_POINT('',(79.9000000000001,217.767014370377,31.9213203435596)) ;
#82624 = CARTESIAN_POINT('Origin',(76.0000000000001,217.767014370377,31.9213203435596)) ;
#82625 = CARTESIAN_POINT('',(79.9000000000001,224.305309236676,31.9213203435596)) ;
#82626 = CARTESIAN_POINT('',(79.9,228.575260777783,31.9213203435596)) ;
#82627 = CARTESIAN_POINT('',(80.1050252531695,224.800283983507,31.9213203435596)) ;
#82628 = CARTESIAN_POINT('Origin',(80.6000000000001,224.305309236676,31.9213203435596)) ;
#82629 = CARTESIAN_POINT('',(80.9535533905933,225.64881212093,31.9213203435596)) ;
#82630 = CARTESIAN_POINT('',(77.061706774654,221.756965504991,31.9213203435596)) ;
#82631 = CARTESIAN_POINT('',(81.1,226.002365511524,31.9213203435596)) ;
#82632 = CARTESIAN_POINT('Origin',(80.6,226.002365511524,31.9213203435596)) ;
#82633 = CARTESIAN_POINT('',(81.1,236.901613323034,31.9213203435596)) ;
#82634 = CARTESIAN_POINT('',(81.1,232.568672279644,31.9213203435596)) ;
#82635 = CARTESIAN_POINT('',(80.616129032258,237.401353109641,31.9213203435596)) ;
#82636 = CARTESIAN_POINT('Origin',(80.6,236.901613323034,31.9213203435596)) ;
#82637 = CARTESIAN_POINT('',(78.0999999999999,240.,31.9213203435596)) ;
#82638 = CARTESIAN_POINT('Origin',(80.6999999999999,240.,31.9213203435596)) ;
#82639 = CARTESIAN_POINT('',(78.0999999999999,244.,31.9213203435596)) ;
#82640 = CARTESIAN_POINT('',(78.0999999999999,239.691753592594,31.9213203435596)) ;
#82641 = CARTESIAN_POINT('',(80.616129032258,246.598646890358,31.9213203435596)) ;
#82642 = CARTESIAN_POINT('Origin',(80.6999999999999,244.,31.9213203435596)) ;
#82643 = CARTESIAN_POINT('',(81.1,247.098386676966,31.9213203435596)) ;
#82644 = CARTESIAN_POINT('Origin',(80.6,247.098386676966,31.9213203435596)) ;
#82645 = CARTESIAN_POINT('',(81.1,257.151471862576,31.9213203435596)) ;
#82646 = CARTESIAN_POINT('',(81.1,242.941753592594,31.9213203435596)) ;
#82647 = CARTESIAN_POINT('',(80.9535533905932,257.50502525317,31.9213203435596)) ;
#82648 = CARTESIAN_POINT('Origin',(80.6,257.151471862576,31.9213203435596)) ;
#82649 = CARTESIAN_POINT('',(79.3050252531694,259.153553390593,31.9213203435596)) ;
#82650 = CARTESIAN_POINT('',(78.758412525583,259.70016611818,31.9213203435596)) ;
#82651 = CARTESIAN_POINT('Origin',(79.7999999999999,259.648528137424,31.9213203435596)) ;
#82652 = CARTESIAN_POINT('',(69.6,244.169705627485,31.9213203435596)) ;
#82653 = CARTESIAN_POINT('',(67.8102943725152,242.38,31.9213203435596)) ;
#82654 = CARTESIAN_POINT('',(63.6360239825547,238.20572961004,31.9213203435596)) ;
#82655 = CARTESIAN_POINT('',(71.3897056274848,242.38,31.9213203435596)) ;
#82656 = CARTESIAN_POINT('',(66.8639760174453,246.90572961004,31.9213203435596)) ;
#82657 = CARTESIAN_POINT('',(62.4,242.38,31.9213203435596)) ;
#82658 = CARTESIAN_POINT('',(67.8102943725152,238.12,31.9213203435596)) ;
#82659 = CARTESIAN_POINT('',(69.6,236.330294372515,31.9213203435596)) ;
#82660 = CARTESIAN_POINT('',(64.8192703899605,241.111023982555,31.9213203435596)) ;
#82661 = CARTESIAN_POINT('',(71.3897056274848,238.12,31.9213203435596)) ;
#82662 = CARTESIAN_POINT('',(60.9,238.12,31.9213203435596)) ;
#82663 = CARTESIAN_POINT('',(67.1807296100394,233.911023982555,31.9213203435596)) ;
#82664 = CARTESIAN_POINT('',(67.3,247.9,31.9213203435596)) ;
#82665 = CARTESIAN_POINT('',(67.5,248.1,31.9213203435596)) ;
#82666 = CARTESIAN_POINT('Origin',(67.3,248.1,31.9213203435596)) ;
#82667 = CARTESIAN_POINT('',(64.4999999999999,247.9,31.9213203435596)) ;
#82668 = CARTESIAN_POINT('',(59.05,247.9,31.9213203435596)) ;
#82669 = CARTESIAN_POINT('',(64.3,248.1,31.9213203435596)) ;
#82670 = CARTESIAN_POINT('Origin',(64.4999999999999,248.1,31.9213203435596)) ;
#82671 = CARTESIAN_POINT('',(64.3,250.9,31.9213203435596)) ;
#82672 = CARTESIAN_POINT('',(64.3,245.191753592594,31.9213203435596)) ;
#82673 = CARTESIAN_POINT('',(64.5,251.1,31.9213203435596)) ;
#82674 = CARTESIAN_POINT('Origin',(64.5,250.9,31.9213203435596)) ;
#82675 = CARTESIAN_POINT('',(64.6,251.1,31.9213203435596)) ;
#82676 = CARTESIAN_POINT('',(59.2,251.1,31.9213203435596)) ;
#82677 = CARTESIAN_POINT('',(64.6,256.9,31.9213203435596)) ;
#82678 = CARTESIAN_POINT('',(64.6,248.191753592594,31.9213203435596)) ;
#82679 = CARTESIAN_POINT('',(64.8,257.1,31.9213203435596)) ;
#82680 = CARTESIAN_POINT('Origin',(64.8,256.9,31.9213203435596)) ;
#82681 = CARTESIAN_POINT('',(67.,257.1,31.9213203435596)) ;
#82682 = CARTESIAN_POINT('',(60.4,257.1,31.9213203435596)) ;
#82683 = CARTESIAN_POINT('',(67.2,256.9,31.9213203435596)) ;
#82684 = CARTESIAN_POINT('Origin',(67.,256.9,31.9213203435596)) ;
#82685 = CARTESIAN_POINT('',(67.2,251.1,31.9213203435596)) ;
#82686 = CARTESIAN_POINT('',(67.2,245.191753592594,31.9213203435596)) ;
#82687 = CARTESIAN_POINT('',(67.3,251.1,31.9213203435596)) ;
#82688 = CARTESIAN_POINT('',(60.55,251.1,31.9213203435596)) ;
#82689 = CARTESIAN_POINT('',(67.5,250.9,31.9213203435596)) ;
#82690 = CARTESIAN_POINT('Origin',(67.3,250.9,31.9213203435596)) ;
#82691 = CARTESIAN_POINT('',(67.5,243.691753592594,31.9213203435596)) ;
#82692 = CARTESIAN_POINT('',(80.299999999999,230.4,31.9213203435596)) ;
#82693 = CARTESIAN_POINT('',(80.299999999999,229.3,31.9213203435596)) ;
#82694 = CARTESIAN_POINT('',(80.299999999999,232.441753592594,31.9213203435596)) ;
#82695 = CARTESIAN_POINT('',(80.1999999999999,229.3,31.9213203435596)) ;
#82696 = CARTESIAN_POINT('',(66.9499999999995,229.3,31.9213203435596)) ;
#82697 = CARTESIAN_POINT('',(80.1999999999999,226.7,31.9213203435596)) ;
#82698 = CARTESIAN_POINT('',(80.1999999999999,234.391753592594,31.9213203435596)) ;
#82699 = CARTESIAN_POINT('',(80.299999999999,226.7,31.9213203435596)) ;
#82700 = CARTESIAN_POINT('',(66.4499999999997,226.700000000001,31.9213203435596)) ;
#82701 = CARTESIAN_POINT('',(80.2999999999989,225.6,31.9213203435596)) ;
#82702 = CARTESIAN_POINT('',(80.299999999999,232.441753592594,31.9213203435596)) ;
#82703 = CARTESIAN_POINT('',(80.0999999999989,225.4,31.9213203435596)) ;
#82704 = CARTESIAN_POINT('Origin',(80.0999999999989,225.6,31.9213203435596)) ;
#82705 = CARTESIAN_POINT('',(76.0414213562366,225.4,31.9213203435596)) ;
#82706 = CARTESIAN_POINT('',(64.4499999999996,225.4,31.9213203435596)) ;
#82707 = CARTESIAN_POINT('',(75.8999999999993,225.458578643763,31.9213203435596)) ;
#82708 = CARTESIAN_POINT('Origin',(76.0414213562366,225.6,31.9213203435596)) ;
#82709 = CARTESIAN_POINT('',(75.158578643762,226.2,31.9213203435596)) ;
#82710 = CARTESIAN_POINT('',(66.6834125255838,234.675166118178,31.9213203435596)) ;
#82711 = CARTESIAN_POINT('',(75.0999999999993,226.341421356237,31.9213203435596)) ;
#82712 = CARTESIAN_POINT('Origin',(75.2999999999993,226.341421356237,31.9213203435596)) ;
#82713 = CARTESIAN_POINT('',(75.0999999999994,229.658578643763,31.9213203435596)) ;
#82714 = CARTESIAN_POINT('',(75.0999999999996,234.941753592594,31.9213203435596)) ;
#82715 = CARTESIAN_POINT('',(75.1585786437621,229.8,31.9213203435596)) ;
#82716 = CARTESIAN_POINT('Origin',(75.2999999999994,229.658578643763,31.9213203435596)) ;
#82717 = CARTESIAN_POINT('',(75.8999999999994,230.541421356237,31.9213203435596)) ;
#82718 = CARTESIAN_POINT('',(72.3751661181778,227.016587474416,31.9213203435596)) ;
#82719 = CARTESIAN_POINT('',(76.0414213562367,230.6,31.9213203435596)) ;
#82720 = CARTESIAN_POINT('Origin',(76.0414213562367,230.4,31.9213203435596)) ;
#82721 = CARTESIAN_POINT('',(80.099999999999,230.6,31.9213203435596)) ;
#82722 = CARTESIAN_POINT('',(66.9499999999995,230.6,31.9213203435596)) ;
#82723 = CARTESIAN_POINT('Origin',(80.099999999999,230.4,31.9213203435596)) ;
#82724 = CARTESIAN_POINT('',(71.5999999999999,226.1,31.9213203435596)) ;
#82725 = CARTESIAN_POINT('',(71.3999999999999,225.9,31.9213203435596)) ;
#82726 = CARTESIAN_POINT('Origin',(71.5999999999999,225.9,31.9213203435596)) ;
#82727 = CARTESIAN_POINT('',(71.6999999999999,226.1,31.9213203435596)) ;
#82728 = CARTESIAN_POINT('',(62.75,226.1,31.9213203435596)) ;
#82729 = CARTESIAN_POINT('',(71.6999999999999,231.9,31.9213203435596)) ;
#82730 = CARTESIAN_POINT('',(71.6999999999999,235.691753592594,31.9213203435596)) ;
#82731 = CARTESIAN_POINT('',(71.8999999999999,232.1,31.9213203435596)) ;
#82732 = CARTESIAN_POINT('Origin',(71.8999999999999,231.9,31.9213203435596)) ;
#82733 = CARTESIAN_POINT('',(74.0999999999999,232.1,31.9213203435596)) ;
#82734 = CARTESIAN_POINT('',(63.95,232.1,31.9213203435596)) ;
#82735 = CARTESIAN_POINT('',(74.2999999999999,231.9,31.9213203435596)) ;
#82736 = CARTESIAN_POINT('Origin',(74.0999999999999,231.9,31.9213203435596)) ;
#82737 = CARTESIAN_POINT('',(74.2999999999999,226.1,31.9213203435596)) ;
#82738 = CARTESIAN_POINT('',(74.2999999999999,232.691753592594,31.9213203435596)) ;
#82739 = CARTESIAN_POINT('',(74.3999999999999,226.1,31.9213203435596)) ;
#82740 = CARTESIAN_POINT('',(64.1,226.1,31.9213203435596)) ;
#82741 = CARTESIAN_POINT('',(74.5999999999999,225.9,31.9213203435596)) ;
#82742 = CARTESIAN_POINT('Origin',(74.3999999999999,225.9,31.9213203435596)) ;
#82743 = CARTESIAN_POINT('',(74.5999999999999,223.1,31.9213203435596)) ;
#82744 = CARTESIAN_POINT('',(74.5999999999999,231.191753592594,31.9213203435596)) ;
#82745 = CARTESIAN_POINT('',(74.3999999999999,222.9,31.9213203435596)) ;
#82746 = CARTESIAN_POINT('Origin',(74.3999999999999,223.1,31.9213203435596)) ;
#82747 = CARTESIAN_POINT('',(71.5999999999999,222.9,31.9213203435596)) ;
#82748 = CARTESIAN_POINT('',(62.6,222.9,31.9213203435596)) ;
#82749 = CARTESIAN_POINT('',(71.3999999999999,223.1,31.9213203435596)) ;
#82750 = CARTESIAN_POINT('Origin',(71.5999999999999,223.1,31.9213203435596)) ;
#82751 = CARTESIAN_POINT('',(71.3999999999999,232.691753592594,31.9213203435596)) ;
#82752 = CARTESIAN_POINT('',(59.7573593128808,230.1,31.9213203435596)) ;
#82753 = CARTESIAN_POINT('',(59.5573593128808,229.9,31.9213203435596)) ;
#82754 = CARTESIAN_POINT('Origin',(59.7573593128808,229.9,31.9213203435596)) ;
#82755 = CARTESIAN_POINT('',(59.8573593128808,230.1,31.9213203435596)) ;
#82756 = CARTESIAN_POINT('',(56.8286796564404,230.1,31.9213203435596)) ;
#82757 = CARTESIAN_POINT('',(59.8573593128808,235.9,31.9213203435596)) ;
#82758 = CARTESIAN_POINT('',(59.8573593128808,237.691753592594,31.9213203435596)) ;
#82759 = CARTESIAN_POINT('',(60.0573593128808,236.1,31.9213203435596)) ;
#82760 = CARTESIAN_POINT('Origin',(60.0573593128808,235.9,31.9213203435596)) ;
#82761 = CARTESIAN_POINT('',(62.2573593128808,236.1,31.9213203435596)) ;
#82762 = CARTESIAN_POINT('',(58.0286796564404,236.1,31.9213203435596)) ;
#82763 = CARTESIAN_POINT('',(62.4573593128808,235.9,31.9213203435596)) ;
#82764 = CARTESIAN_POINT('Origin',(62.2573593128808,235.9,31.9213203435596)) ;
#82765 = CARTESIAN_POINT('',(62.4573593128808,230.1,31.9213203435596)) ;
#82766 = CARTESIAN_POINT('',(62.4573593128808,234.691753592594,31.9213203435596)) ;
#82767 = CARTESIAN_POINT('',(62.5573593128808,230.1,31.9213203435596)) ;
#82768 = CARTESIAN_POINT('',(58.1786796564404,230.1,31.9213203435596)) ;
#82769 = CARTESIAN_POINT('',(62.7573593128808,229.9,31.9213203435596)) ;
#82770 = CARTESIAN_POINT('Origin',(62.5573593128808,229.9,31.9213203435596)) ;
#82771 = CARTESIAN_POINT('',(62.7573593128808,227.1,31.9213203435596)) ;
#82772 = CARTESIAN_POINT('',(62.7573593128808,233.191753592594,31.9213203435596)) ;
#82773 = CARTESIAN_POINT('',(62.5573593128808,226.9,31.9213203435596)) ;
#82774 = CARTESIAN_POINT('Origin',(62.5573593128808,227.1,31.9213203435596)) ;
#82775 = CARTESIAN_POINT('',(59.7573593128808,226.9,31.9213203435596)) ;
#82776 = CARTESIAN_POINT('',(56.6786796564404,226.9,31.9213203435596)) ;
#82777 = CARTESIAN_POINT('',(59.5573593128808,227.1,31.9213203435596)) ;
#82778 = CARTESIAN_POINT('Origin',(59.7573593128808,227.1,31.9213203435596)) ;
#82779 = CARTESIAN_POINT('',(59.5573593128808,234.691753592594,31.9213203435596)) ;
#82780 = CARTESIAN_POINT('',(80.299999999999,253.6,31.9213203435596)) ;
#82781 = CARTESIAN_POINT('',(80.299999999999,252.3,31.9213203435596)) ;
#82782 = CARTESIAN_POINT('',(80.2999999999989,243.941753592594,31.9213203435596)) ;
#82783 = CARTESIAN_POINT('',(80.1999999999999,252.3,31.9213203435596)) ;
#82784 = CARTESIAN_POINT('',(66.9499999999999,252.3,31.9213203435596)) ;
#82785 = CARTESIAN_POINT('',(80.1999999999999,249.7,31.9213203435596)) ;
#82786 = CARTESIAN_POINT('',(80.1999999999999,245.891753592594,31.9213203435596)) ;
#82787 = CARTESIAN_POINT('',(80.2999999999989,249.7,31.9213203435596)) ;
#82788 = CARTESIAN_POINT('',(66.4500000000001,249.700000000001,31.9213203435596)) ;
#82789 = CARTESIAN_POINT('',(80.2999999999989,248.4,31.9213203435596)) ;
#82790 = CARTESIAN_POINT('',(80.2999999999989,243.941753592594,31.9213203435596)) ;
#82791 = CARTESIAN_POINT('',(76.0414213562365,248.4,31.9213203435596)) ;
#82792 = CARTESIAN_POINT('',(64.4499999999996,248.4,31.9213203435596)) ;
#82793 = CARTESIAN_POINT('',(75.8999999999992,248.458578643763,31.9213203435596)) ;
#82794 = CARTESIAN_POINT('Origin',(76.0414213562365,248.6,31.9213203435596)) ;
#82795 = CARTESIAN_POINT('',(75.158578643762,249.2,31.9213203435596)) ;
#82796 = CARTESIAN_POINT('',(72.4334125255833,251.925166118179,31.9213203435596)) ;
#82797 = CARTESIAN_POINT('',(75.0999999999993,249.341421356237,31.9213203435596)) ;
#82798 = CARTESIAN_POINT('Origin',(75.2999999999993,249.341421356237,31.9213203435596)) ;
#82799 = CARTESIAN_POINT('',(75.0999999999994,252.658578643763,31.9213203435596)) ;
#82800 = CARTESIAN_POINT('',(75.0999999999992,246.441753592594,31.9213203435596)) ;
#82801 = CARTESIAN_POINT('',(75.1585786437621,252.8,31.9213203435596)) ;
#82802 = CARTESIAN_POINT('Origin',(75.2999999999994,252.658578643763,31.9213203435596)) ;
#82803 = CARTESIAN_POINT('',(75.8999999999994,253.541421356237,31.9213203435596)) ;
#82804 = CARTESIAN_POINT('',(66.6251661181778,244.266587474416,31.9213203435596)) ;
#82805 = CARTESIAN_POINT('',(76.0414213562367,253.6,31.9213203435596)) ;
#82806 = CARTESIAN_POINT('Origin',(76.0414213562367,253.4,31.9213203435596)) ;
#82807 = CARTESIAN_POINT('',(66.9499999999995,253.6,31.9213203435596)) ;
#82808 = CARTESIAN_POINT('',(33.3,254.8,31.9213203435596)) ;
#82809 = CARTESIAN_POINT('Origin',(30.6999999999999,254.8,31.9213203435596)) ;
#82810 = CARTESIAN_POINT('',(28.1,262.2,31.9213203435596)) ;
#82811 = CARTESIAN_POINT('',(28.1,263.3,31.9213203435596)) ;
#82812 = CARTESIAN_POINT('',(28.1,251.391753592594,31.9213203435596)) ;
#82813 = CARTESIAN_POINT('',(28.2999999999999,263.5,31.9213203435596)) ;
#82814 = CARTESIAN_POINT('Origin',(28.2999999999999,263.3,31.9213203435596)) ;
#82815 = CARTESIAN_POINT('',(32.3585786437627,263.5,31.9213203435596)) ;
#82816 = CARTESIAN_POINT('',(43.45,263.5,31.9213203435596)) ;
#82817 = CARTESIAN_POINT('',(32.5,263.441421356237,31.9213203435596)) ;
#82818 = CARTESIAN_POINT('Origin',(32.3585786437627,263.3,31.9213203435596)) ;
#82819 = CARTESIAN_POINT('',(33.2414213562373,262.7,31.9213203435596)) ;
#82820 = CARTESIAN_POINT('',(43.9998338818216,251.941587474416,31.9213203435596)) ;
#82821 = CARTESIAN_POINT('',(33.2999999999999,262.558578643763,31.9213203435596)) ;
#82822 = CARTESIAN_POINT('Origin',(33.1,262.558578643763,31.9213203435596)) ;
#82823 = CARTESIAN_POINT('',(33.2999999999999,259.241421356237,31.9213203435596)) ;
#82824 = CARTESIAN_POINT('',(33.2999999999999,248.891753592594,31.9213203435596)) ;
#82825 = CARTESIAN_POINT('',(33.2414213562373,259.1,31.9213203435596)) ;
#82826 = CARTESIAN_POINT('Origin',(33.1,259.241421356237,31.9213203435596)) ;
#82827 = CARTESIAN_POINT('',(32.5,258.358578643763,31.9213203435596)) ;
#82828 = CARTESIAN_POINT('',(33.2415874744158,259.100166118179,31.9213203435596)) ;
#82829 = CARTESIAN_POINT('',(32.3585786437627,258.3,31.9213203435596)) ;
#82830 = CARTESIAN_POINT('Origin',(32.3585786437627,258.5,31.9213203435596)) ;
#82831 = CARTESIAN_POINT('',(28.1,258.3,31.9213203435596)) ;
#82832 = CARTESIAN_POINT('',(40.95,258.3,31.9213203435596)) ;
#82833 = CARTESIAN_POINT('',(28.1,259.6,31.9213203435596)) ;
#82834 = CARTESIAN_POINT('',(28.1,251.391753592594,31.9213203435596)) ;
#82835 = CARTESIAN_POINT('',(28.1999999999999,259.6,31.9213203435596)) ;
#82836 = CARTESIAN_POINT('',(40.9499999999996,259.6,31.9213203435596)) ;
#82837 = CARTESIAN_POINT('',(28.1999999999999,262.2,31.9213203435596)) ;
#82838 = CARTESIAN_POINT('',(28.1999999999999,249.441753592594,31.9213203435596)) ;
#82839 = CARTESIAN_POINT('',(41.45,262.2,31.9213203435596)) ;
#82840 = CARTESIAN_POINT('',(55.2649110640673,257.,31.9213203435596)) ;
#82841 = CARTESIAN_POINT('Origin',(51.2,257.,31.9213203435596)) ;
#82842 = CARTESIAN_POINT('',(79.8149110640674,218.,31.9213203435596)) ;
#82843 = CARTESIAN_POINT('Origin',(75.7500000000001,218.,31.9213203435596)) ;
#82844 = CARTESIAN_POINT('',(57.8573593128808,241.8,31.9213203435596)) ;
#82845 = CARTESIAN_POINT('',(57.9573593128808,241.8,31.9213203435596)) ;
#82846 = CARTESIAN_POINT('',(56.3286796564404,241.8,31.9213203435596)) ;
#82847 = CARTESIAN_POINT('',(57.8573593128808,243.1,31.9213203435596)) ;
#82848 = CARTESIAN_POINT('',(57.8573593128808,241.191753592594,31.9213203435596)) ;
#82849 = CARTESIAN_POINT('',(62.1159379566435,243.1,31.9213203435596)) ;
#82850 = CARTESIAN_POINT('',(58.3286796564404,243.1,31.9213203435596)) ;
#82851 = CARTESIAN_POINT('',(62.2573593128808,243.041421356237,31.9213203435596)) ;
#82852 = CARTESIAN_POINT('Origin',(62.1159379566435,242.9,31.9213203435596)) ;
#82853 = CARTESIAN_POINT('',(62.9987806691181,242.3,31.9213203435596)) ;
#82854 = CARTESIAN_POINT('',(61.2178533664821,244.080927302636,31.9213203435596)) ;
#82855 = CARTESIAN_POINT('',(63.0573593128807,242.158578643763,31.9213203435596)) ;
#82856 = CARTESIAN_POINT('Origin',(62.8573593128808,242.158578643763,31.9213203435596)) ;
#82857 = CARTESIAN_POINT('',(63.0573593128807,238.841421356237,31.9213203435596)) ;
#82858 = CARTESIAN_POINT('',(63.0573593128807,238.691753592594,31.9213203435596)) ;
#82859 = CARTESIAN_POINT('',(62.998780669118,238.7,31.9213203435596)) ;
#82860 = CARTESIAN_POINT('Origin',(62.8573593128808,238.841421356237,31.9213203435596)) ;
#82861 = CARTESIAN_POINT('',(62.2573593128808,237.958578643763,31.9213203435596)) ;
#82862 = CARTESIAN_POINT('',(60.6596069590762,236.360826289958,31.9213203435596)) ;
#82863 = CARTESIAN_POINT('',(62.1159379566435,237.9,31.9213203435596)) ;
#82864 = CARTESIAN_POINT('Origin',(62.1159379566435,238.1,31.9213203435596)) ;
#82865 = CARTESIAN_POINT('',(57.8573593128808,237.9,31.9213203435596)) ;
#82866 = CARTESIAN_POINT('',(55.8286796564404,237.9,31.9213203435596)) ;
#82867 = CARTESIAN_POINT('',(57.8573593128808,239.2,31.9213203435596)) ;
#82868 = CARTESIAN_POINT('',(57.8573593128808,241.191753592594,31.9213203435596)) ;
#82869 = CARTESIAN_POINT('',(57.9573593128808,239.2,31.9213203435596)) ;
#82870 = CARTESIAN_POINT('',(55.8286796564404,239.2,31.9213203435596)) ;
#82871 = CARTESIAN_POINT('',(57.9573593128808,239.241753592594,31.9213203435596)) ;
#82872 = CARTESIAN_POINT('',(77.2649110640673,257.,31.9213203435596)) ;
#82873 = CARTESIAN_POINT('Origin',(73.2,257.,31.9213203435596)) ;
#82874 = CARTESIAN_POINT('',(66.2568347953872,220.146231446812,31.9213203435596)) ;
#82875 = CARTESIAN_POINT('Origin',(64.1568347953873,220.146231446812,31.9213203435596)) ;
#82876 = CARTESIAN_POINT('',(37.2999999999999,260.1,31.9213203435596)) ;
#82877 = CARTESIAN_POINT('',(37.0999999999999,259.9,31.9213203435596)) ;
#82878 = CARTESIAN_POINT('Origin',(37.2999999999999,259.9,31.9213203435596)) ;
#82879 = CARTESIAN_POINT('',(43.0999999999999,260.1,31.9213203435596)) ;
#82880 = CARTESIAN_POINT('',(48.4499999999999,260.1,31.9213203435596)) ;
#82881 = CARTESIAN_POINT('',(43.2999999999999,259.9,31.9213203435596)) ;
#82882 = CARTESIAN_POINT('Origin',(43.0999999999999,259.9,31.9213203435596)) ;
#82883 = CARTESIAN_POINT('',(43.2999999999999,252.1,31.9213203435596)) ;
#82884 = CARTESIAN_POINT('',(43.2999999999999,245.691753592594,31.9213203435596)) ;
#82885 = CARTESIAN_POINT('',(43.0999999999999,251.9,31.9213203435596)) ;
#82886 = CARTESIAN_POINT('Origin',(43.0999999999999,252.1,31.9213203435596)) ;
#82887 = CARTESIAN_POINT('',(37.2999999999999,251.9,31.9213203435596)) ;
#82888 = CARTESIAN_POINT('',(45.4499999999999,251.9,31.9213203435596)) ;
#82889 = CARTESIAN_POINT('',(37.0999999999999,252.1,31.9213203435596)) ;
#82890 = CARTESIAN_POINT('Origin',(37.2999999999999,252.1,31.9213203435596)) ;
#82891 = CARTESIAN_POINT('',(37.0999999999999,249.691753592594,31.9213203435596)) ;
#82892 = CARTESIAN_POINT('',(59.3,247.9,31.9213203435596)) ;
#82893 = CARTESIAN_POINT('',(59.5,248.1,31.9213203435596)) ;
#82894 = CARTESIAN_POINT('Origin',(59.3,248.1,31.9213203435596)) ;
#82895 = CARTESIAN_POINT('',(56.5,247.9,31.9213203435596)) ;
#82896 = CARTESIAN_POINT('',(55.05,247.9,31.9213203435596)) ;
#82897 = CARTESIAN_POINT('',(56.3,248.1,31.9213203435596)) ;
#82898 = CARTESIAN_POINT('Origin',(56.5,248.1,31.9213203435596)) ;
#82899 = CARTESIAN_POINT('',(56.3,250.9,31.9213203435596)) ;
#82900 = CARTESIAN_POINT('',(56.3,245.191753592594,31.9213203435596)) ;
#82901 = CARTESIAN_POINT('',(56.5,251.1,31.9213203435596)) ;
#82902 = CARTESIAN_POINT('Origin',(56.5,250.9,31.9213203435596)) ;
#82903 = CARTESIAN_POINT('',(56.6,251.1,31.9213203435596)) ;
#82904 = CARTESIAN_POINT('',(55.2,251.1,31.9213203435596)) ;
#82905 = CARTESIAN_POINT('',(56.6,256.9,31.9213203435596)) ;
#82906 = CARTESIAN_POINT('',(56.6,248.191753592594,31.9213203435596)) ;
#82907 = CARTESIAN_POINT('',(56.8,257.1,31.9213203435596)) ;
#82908 = CARTESIAN_POINT('Origin',(56.8,256.9,31.9213203435596)) ;
#82909 = CARTESIAN_POINT('',(59.,257.1,31.9213203435596)) ;
#82910 = CARTESIAN_POINT('',(56.4,257.1,31.9213203435596)) ;
#82911 = CARTESIAN_POINT('',(59.2,256.9,31.9213203435596)) ;
#82912 = CARTESIAN_POINT('Origin',(59.,256.9,31.9213203435596)) ;
#82913 = CARTESIAN_POINT('',(59.2,251.1,31.9213203435596)) ;
#82914 = CARTESIAN_POINT('',(59.2,245.191753592594,31.9213203435596)) ;
#82915 = CARTESIAN_POINT('',(59.3,251.1,31.9213203435596)) ;
#82916 = CARTESIAN_POINT('',(56.55,251.1,31.9213203435596)) ;
#82917 = CARTESIAN_POINT('',(59.5,250.9,31.9213203435596)) ;
#82918 = CARTESIAN_POINT('Origin',(59.3,250.9,31.9213203435596)) ;
#82919 = CARTESIAN_POINT('',(59.5,243.691753592594,31.9213203435596)) ;
#82920 = CARTESIAN_POINT('',(67.98,240.62,31.9213203435596)) ;
#82921 = CARTESIAN_POINT('',(67.98,239.88,31.9213203435596)) ;
#82922 = CARTESIAN_POINT('',(67.98,239.691753592594,31.9213203435596)) ;
#82923 = CARTESIAN_POINT('',(71.22,240.62,31.9213203435596)) ;
#82924 = CARTESIAN_POINT('',(60.9,240.62,31.9213203435596)) ;
#82925 = CARTESIAN_POINT('',(71.22,239.88,31.9213203435596)) ;
#82926 = CARTESIAN_POINT('',(71.22,239.941753592594,31.9213203435596)) ;
#82927 = CARTESIAN_POINT('',(62.4,239.88,31.9213203435596)) ;
#82928 = CARTESIAN_POINT('Origin',(63.6360239825547,238.20572961004,31.8013203435596)) ;
#82929 = CARTESIAN_POINT('Origin',(67.8102943725152,242.38,31.8013203435596)) ;
#82930 = CARTESIAN_POINT('Origin',(69.6,244.169705627485,31.8013203435596)) ;
#82931 = CARTESIAN_POINT('Origin',(62.4,242.38,31.8013203435596)) ;
#82932 = CARTESIAN_POINT('Origin',(71.3897056274848,242.38,31.8013203435596)) ;
#82933 = CARTESIAN_POINT('Origin',(66.8639760174453,246.90572961004,31.8013203435596)) ;
#82934 = CARTESIAN_POINT('',(66.7791232037029,246.820876796297,31.8013203435596)) ;
#82935 = CARTESIAN_POINT('Origin',(69.6,244.,31.9213203435596)) ;
#82936 = CARTESIAN_POINT('Origin',(67.98,239.691753592594,31.8013203435596)) ;
#82937 = CARTESIAN_POINT('Origin',(67.98,239.88,31.8013203435596)) ;
#82938 = CARTESIAN_POINT('Origin',(67.98,240.62,31.8013203435596)) ;
#82939 = CARTESIAN_POINT('Origin',(62.4,239.88,31.8013203435596)) ;
#82940 = CARTESIAN_POINT('Origin',(71.22,239.88,31.8013203435596)) ;
#82941 = CARTESIAN_POINT('Origin',(71.22,239.941753592594,31.8013203435596)) ;
#82942 = CARTESIAN_POINT('',(71.1,240.5,31.8013203435596)) ;
#82943 = CARTESIAN_POINT('',(71.1,239.941753592594,31.8013203435596)) ;
#82944 = CARTESIAN_POINT('Origin',(71.22,240.62,31.8013203435596)) ;
#82945 = CARTESIAN_POINT('Origin',(60.9,240.62,31.8013203435596)) ;
#82946 = CARTESIAN_POINT('',(60.9,240.5,31.8013203435596)) ;
#82947 = CARTESIAN_POINT('Origin',(68.1,240.5,31.9213203435596)) ;
#82948 = CARTESIAN_POINT('',(71.1,240.5,31.9213203435596)) ;
#82949 = CARTESIAN_POINT('Origin',(64.8192703899605,241.111023982555,31.8013203435596)) ;
#82950 = CARTESIAN_POINT('Origin',(69.6,236.330294372515,31.8013203435596)) ;
#82951 = CARTESIAN_POINT('Origin',(67.8102943725152,238.12,31.8013203435596)) ;
#82952 = CARTESIAN_POINT('Origin',(67.1807296100394,233.911023982555,31.8013203435596)) ;
#82953 = CARTESIAN_POINT('Origin',(71.3897056274848,238.12,31.8013203435596)) ;
#82954 = CARTESIAN_POINT('Origin',(60.9,238.12,31.8013203435596)) ;
#82955 = CARTESIAN_POINT('',(60.9,238.,31.8013203435596)) ;
#82956 = CARTESIAN_POINT('Origin',(68.1,238.,31.9213203435596)) ;
#82957 = CARTESIAN_POINT('Origin',(71.1,240.5,31.9213203435596)) ;
#82958 = CARTESIAN_POINT('Ctrl Pts',(50.1048968673761,247.225573558217,31.9213203435596)) ;
#82959 = CARTESIAN_POINT('Ctrl Pts',(50.1048968673761,247.225573558217,31.5613203435596)) ;
#82960 = CARTESIAN_POINT('Ctrl Pts',(50.1908486902686,247.172482844858,31.9213203435596)) ;
#82961 = CARTESIAN_POINT('Ctrl Pts',(50.1908486902686,247.172482844858,31.5613203435596)) ;
#82962 = CARTESIAN_POINT('Ctrl Pts',(50.3885184489928,247.05038620808,31.9213203435596)) ;
#82963 = CARTESIAN_POINT('Ctrl Pts',(50.3885184489928,247.05038620808,31.5613203435596)) ;
#82964 = CARTESIAN_POINT('Ctrl Pts',(50.6222076847147,247.045515776756,31.9213203435596)) ;
#82965 = CARTESIAN_POINT('Ctrl Pts',(50.6222076847147,247.045515776756,31.5613203435596)) ;
#82966 = CARTESIAN_POINT('Ctrl Pts',(50.7542829156931,247.042763132459,31.9213203435596)) ;
#82967 = CARTESIAN_POINT('Ctrl Pts',(50.7542829156931,247.042763132459,31.5613203435596)) ;
#82968 = CARTESIAN_POINT('',(50.1048968673761,247.225573558217,31.9213203435596)) ;
#82969 = CARTESIAN_POINT('Ctrl Pts',(49.8975299240168,247.692149180776,31.9213203435596)) ;
#82970 = CARTESIAN_POINT('Ctrl Pts',(49.8975299240168,247.692149180776,31.5613203435596)) ;
#82971 = CARTESIAN_POINT('Ctrl Pts',(49.9059085609628,247.601999233154,31.9213203435596)) ;
#82972 = CARTESIAN_POINT('Ctrl Pts',(49.9059085609628,247.601999233154,31.5613203435596)) ;
#82973 = CARTESIAN_POINT('Ctrl Pts',(49.9225413218171,247.423039035993,31.9213203435596)) ;
#82974 = CARTESIAN_POINT('Ctrl Pts',(49.9225413218171,247.423039035993,31.5613203435596)) ;
#82975 = CARTESIAN_POINT('Ctrl Pts',(50.044415803444,247.291066067091,31.9213203435596)) ;
#82976 = CARTESIAN_POINT('Ctrl Pts',(50.044415803444,247.291066067091,31.5613203435596)) ;
#82977 = CARTESIAN_POINT('Ctrl Pts',(50.1048968673761,247.225573558217,31.9213203435596)) ;
#82978 = CARTESIAN_POINT('Ctrl Pts',(50.1048968673761,247.225573558217,31.5613203435596)) ;
#82979 = CARTESIAN_POINT('',(49.8975299240168,247.692149180776,31.9213203435596)) ;
#82980 = CARTESIAN_POINT('Ctrl Pts',(50.003941798311,248.05231292904,31.9213203435596)) ;
#82981 = CARTESIAN_POINT('Ctrl Pts',(50.003941798311,248.05231292904,31.5613203435596)) ;
#82982 = CARTESIAN_POINT('Ctrl Pts',(49.9729051299706,247.995865679917,31.9213203435596)) ;
#82983 = CARTESIAN_POINT('Ctrl Pts',(49.9729051299706,247.995865679917,31.5613203435596)) ;
#82984 = CARTESIAN_POINT('Ctrl Pts',(49.9111525355836,247.883554524574,31.9213203435596)) ;
#82985 = CARTESIAN_POINT('Ctrl Pts',(49.9111525355836,247.883554524574,31.5613203435596)) ;
#82986 = CARTESIAN_POINT('Ctrl Pts',(49.9020550437817,247.755729655054,31.9213203435596)) ;
#82987 = CARTESIAN_POINT('Ctrl Pts',(49.9020550437817,247.755729655054,31.5613203435596)) ;
#82988 = CARTESIAN_POINT('Ctrl Pts',(49.8975299240168,247.692149180776,31.9213203435596)) ;
#82989 = CARTESIAN_POINT('Ctrl Pts',(49.8975299240168,247.692149180776,31.5613203435596)) ;
#82990 = CARTESIAN_POINT('',(50.003941798311,248.05231292904,31.9213203435596)) ;
#82991 = CARTESIAN_POINT('Ctrl Pts',(50.3149922133501,248.292422193891,31.9213203435596)) ;
#82992 = CARTESIAN_POINT('Ctrl Pts',(50.3149922133501,248.292422193891,31.5613203435596)) ;
#82993 = CARTESIAN_POINT('Ctrl Pts',(50.2514495790856,248.264187481871,31.9213203435596)) ;
#82994 = CARTESIAN_POINT('Ctrl Pts',(50.2514495790856,248.264187481871,31.5613203435596)) ;
#82995 = CARTESIAN_POINT('Ctrl Pts',(50.1280938441034,248.20937524921,31.9213203435596)) ;
#82996 = CARTESIAN_POINT('Ctrl Pts',(50.1280938441034,248.20937524921,31.5613203435596)) ;
#82997 = CARTESIAN_POINT('Ctrl Pts',(50.044483186211,248.103601044398,31.9213203435596)) ;
#82998 = CARTESIAN_POINT('Ctrl Pts',(50.044483186211,248.103601044398,31.5613203435596)) ;
#82999 = CARTESIAN_POINT('Ctrl Pts',(50.003941798311,248.05231292904,31.9213203435596)) ;
#83000 = CARTESIAN_POINT('Ctrl Pts',(50.003941798311,248.05231292904,31.5613203435596)) ;
#83001 = CARTESIAN_POINT('Ctrl Pts',(49.6274070383127,248.40974827469,31.9213203435596)) ;
#83002 = CARTESIAN_POINT('Ctrl Pts',(49.6274070383127,248.40974827469,31.5613203435596)) ;
#83003 = CARTESIAN_POINT('Ctrl Pts',(49.7398143320343,248.499112212212,31.9213203435596)) ;
#83004 = CARTESIAN_POINT('Ctrl Pts',(49.7398143320343,248.499112212212,31.5613203435596)) ;
#83005 = CARTESIAN_POINT('Ctrl Pts',(49.9894578389715,248.697579108959,31.9213203435596)) ;
#83006 = CARTESIAN_POINT('Ctrl Pts',(49.9894578389715,248.697579108959,31.5613203435596)) ;
#83007 = CARTESIAN_POINT('Ctrl Pts',(50.3051550779305,248.751296136815,31.9213203435596)) ;
#83008 = CARTESIAN_POINT('Ctrl Pts',(50.3051550779305,248.751296136815,31.5613203435596)) ;
#83009 = CARTESIAN_POINT('Ctrl Pts',(50.4787029267366,248.780825931436,31.9213203435596)) ;
#83010 = CARTESIAN_POINT('Ctrl Pts',(50.4787029267366,248.780825931436,31.5613203435596)) ;
#83011 = CARTESIAN_POINT('Origin',(75.7500000000001,218.,29.7213203435596)) ;
#83012 = CARTESIAN_POINT('',(73.7500000000001,218.,29.7213203435596)) ;
#83013 = CARTESIAN_POINT('',(77.7500000000001,218.,29.7213203435596)) ;
#83014 = CARTESIAN_POINT('Origin',(75.7500000000001,218.,29.7213203435596)) ;
#83015 = CARTESIAN_POINT('',(77.8500000000001,218.,29.6213203435596)) ;
#83016 = CARTESIAN_POINT('Origin',(77.8500000000001,218.,29.7213203435596)) ;
#83017 = CARTESIAN_POINT('Origin',(75.7500000000001,218.,29.6213203435596)) ;
#83018 = CARTESIAN_POINT('Origin',(75.7500000000001,218.,29.7213203435596)) ;
#83019 = CARTESIAN_POINT('Origin',(75.7500000000001,218.,29.6213203435596)) ;
#83020 = CARTESIAN_POINT('',(72.8500000000001,218.,29.6213203435596)) ;
#83021 = CARTESIAN_POINT('Origin',(75.7500000000001,218.,29.6213203435596)) ;
#83022 = CARTESIAN_POINT('Origin',(75.7500000000001,218.,19.9213203435596)) ;
#83023 = CARTESIAN_POINT('',(73.7500000000001,218.,30.1213203435596)) ;
#83024 = CARTESIAN_POINT('',(73.7500000000001,218.,19.9213203435596)) ;
#83025 = CARTESIAN_POINT('Origin',(75.7500000000001,218.,30.1213203435596)) ;
#83026 = CARTESIAN_POINT('Origin',(75.7500000000001,218.,29.7213203435596)) ;
#83027 = CARTESIAN_POINT('',(72.7500000000001,218.,29.7213203435596)) ;
#83028 = CARTESIAN_POINT('Origin',(75.7500000000001,218.,29.7213203435596)) ;
#83029 = CARTESIAN_POINT('Origin',(72.8500000000001,218.,29.7213203435596)) ;
#83030 = CARTESIAN_POINT('Origin',(75.7500000000001,218.,28.9213203435596)) ;
#83031 = CARTESIAN_POINT('',(72.7500000000001,218.,30.6213203435596)) ;
#83032 = CARTESIAN_POINT('Origin',(75.7500000000001,218.,30.6213203435596)) ;
#83033 = CARTESIAN_POINT('',(72.7500000000001,218.,28.9213203435596)) ;
#83034 = CARTESIAN_POINT('Origin',(75.7500000000001,218.,30.6213203435596)) ;
#83035 = CARTESIAN_POINT('',(72.6500000000001,218.,30.7213203435596)) ;
#83036 = CARTESIAN_POINT('Origin',(75.7500000000001,218.,30.7213203435596)) ;
#83037 = CARTESIAN_POINT('Origin',(72.6500000000001,218.,30.6213203435596)) ;
#83038 = CARTESIAN_POINT('Origin',(53.7,239.383507185188,30.7213203435596)) ;
#83039 = CARTESIAN_POINT('',(28.1267949192431,263.4,30.7213203435596)) ;
#83040 = CARTESIAN_POINT('',(26.3,263.4,30.7213203435596)) ;
#83041 = CARTESIAN_POINT('',(66.4499999999999,263.4,30.7213203435596)) ;
#83042 = CARTESIAN_POINT('',(28.1,263.3,30.7213203435596)) ;
#83043 = CARTESIAN_POINT('Origin',(28.3,263.3,30.7213203435596)) ;
#83044 = CARTESIAN_POINT('',(28.1,262.3,30.7213203435596)) ;
#83045 = CARTESIAN_POINT('',(28.1,251.391753592594,30.7213203435596)) ;
#83046 = CARTESIAN_POINT('',(28.2,262.3,30.7213203435596)) ;
#83047 = CARTESIAN_POINT('',(41.45,262.3,30.7213203435596)) ;
#83048 = CARTESIAN_POINT('',(28.1999999999999,259.5,30.7213203435596)) ;
#83049 = CARTESIAN_POINT('',(28.1999999999999,251.391753592594,30.7213203435596)) ;
#83050 = CARTESIAN_POINT('',(28.1999999999999,258.3,30.7213203435596)) ;
#83051 = CARTESIAN_POINT('',(28.1999999999999,251.391753592594,30.7213203435596)) ;
#83052 = CARTESIAN_POINT('',(32.3585786437627,258.3,30.7213203435596)) ;
#83053 = CARTESIAN_POINT('',(40.95,258.3,30.7213203435596)) ;
#83054 = CARTESIAN_POINT('',(32.5,258.358578643763,30.7213203435596)) ;
#83055 = CARTESIAN_POINT('Origin',(32.3585786437627,258.5,30.7213203435596)) ;
#83056 = CARTESIAN_POINT('',(33.2414213562373,259.1,30.7213203435596)) ;
#83057 = CARTESIAN_POINT('',(33.2415874744158,259.100166118179,30.7213203435596)) ;
#83058 = CARTESIAN_POINT('',(33.3,259.241421356237,30.7213203435596)) ;
#83059 = CARTESIAN_POINT('Origin',(33.1,259.241421356237,30.7213203435596)) ;
#83060 = CARTESIAN_POINT('',(33.2999999999999,262.558578643763,30.7213203435596)) ;
#83061 = CARTESIAN_POINT('',(33.2999999999999,248.891753592594,30.7213203435596)) ;
#83062 = CARTESIAN_POINT('',(33.2414213562373,262.7,30.7213203435596)) ;
#83063 = CARTESIAN_POINT('Origin',(33.1,262.558578643763,30.7213203435596)) ;
#83064 = CARTESIAN_POINT('',(32.5414213562372,263.4,30.7213203435596)) ;
#83065 = CARTESIAN_POINT('',(43.9998338818216,251.941587474416,30.7213203435596)) ;
#83066 = CARTESIAN_POINT('',(46.2376487793589,263.4,30.7213203435596)) ;
#83067 = CARTESIAN_POINT('',(66.4499999999999,263.4,30.7213203435596)) ;
#83068 = CARTESIAN_POINT('',(47.9,262.026327083856,30.7213203435596)) ;
#83069 = CARTESIAN_POINT('Origin',(47.9,263.763591785235,30.7213203435596)) ;
#83070 = CARTESIAN_POINT('',(54.5,262.026327083856,30.7213203435596)) ;
#83071 = CARTESIAN_POINT('',(53.4,262.026327083856,30.7213203435596)) ;
#83072 = CARTESIAN_POINT('',(56.2,263.763591785235,30.7213203435596)) ;
#83073 = CARTESIAN_POINT('Origin',(54.5,263.763591785235,30.7213203435596)) ;
#83074 = CARTESIAN_POINT('',(56.2,263.8,30.7213203435596)) ;
#83075 = CARTESIAN_POINT('',(56.2,252.191753592594,30.7213203435596)) ;
#83076 = CARTESIAN_POINT('',(68.2,263.8,30.7213203435596)) ;
#83077 = CARTESIAN_POINT('',(66.4499999999999,263.8,30.7213203435596)) ;
#83078 = CARTESIAN_POINT('',(68.2,263.763591785235,30.7213203435596)) ;
#83079 = CARTESIAN_POINT('',(68.2,251.191753592594,30.7213203435596)) ;
#83080 = CARTESIAN_POINT('',(69.9,262.026327083856,30.7213203435596)) ;
#83081 = CARTESIAN_POINT('Origin',(69.9,263.763591785235,30.7213203435596)) ;
#83082 = CARTESIAN_POINT('',(76.5,262.026327083856,30.7213203435596)) ;
#83083 = CARTESIAN_POINT('',(64.4,262.026327083856,30.7213203435596)) ;
#83084 = CARTESIAN_POINT('',(78.162351220641,263.4,30.7213203435596)) ;
#83085 = CARTESIAN_POINT('Origin',(76.5,263.763591785235,30.7213203435596)) ;
#83086 = CARTESIAN_POINT('',(79.0999999999999,263.4,30.7213203435596)) ;
#83087 = CARTESIAN_POINT('',(66.4499999999999,263.4,30.7213203435596)) ;
#83088 = CARTESIAN_POINT('',(79.0999999999999,259.648528137424,30.7213203435596)) ;
#83089 = CARTESIAN_POINT('',(79.0999999999999,249.391753592594,30.7213203435596)) ;
#83090 = CARTESIAN_POINT('',(79.3050252531694,259.153553390593,30.7213203435596)) ;
#83091 = CARTESIAN_POINT('Origin',(79.7999999999999,259.648528137424,30.7213203435596)) ;
#83092 = CARTESIAN_POINT('',(80.9535533905932,257.50502525317,30.7213203435596)) ;
#83093 = CARTESIAN_POINT('',(78.758412525583,259.70016611818,30.7213203435596)) ;
#83094 = CARTESIAN_POINT('',(81.1,257.151471862576,30.7213203435596)) ;
#83095 = CARTESIAN_POINT('Origin',(80.6,257.151471862576,30.7213203435596)) ;
#83096 = CARTESIAN_POINT('',(81.1,247.098386676966,30.7213203435596)) ;
#83097 = CARTESIAN_POINT('',(81.1,242.941753592594,30.7213203435596)) ;
#83098 = CARTESIAN_POINT('',(80.616129032258,246.598646890358,30.7213203435596)) ;
#83099 = CARTESIAN_POINT('Origin',(80.6,247.098386676966,30.7213203435596)) ;
#83100 = CARTESIAN_POINT('',(78.0999999999999,244.,30.7213203435596)) ;
#83101 = CARTESIAN_POINT('Origin',(80.6999999999999,244.,30.7213203435596)) ;
#83102 = CARTESIAN_POINT('',(78.1,240.,30.7213203435596)) ;
#83103 = CARTESIAN_POINT('',(78.1,239.691753592594,30.7213203435596)) ;
#83104 = CARTESIAN_POINT('',(80.616129032258,237.401353109641,30.7213203435596)) ;
#83105 = CARTESIAN_POINT('Origin',(80.6999999999999,240.,30.7213203435596)) ;
#83106 = CARTESIAN_POINT('',(81.1,236.901613323034,30.7213203435596)) ;
#83107 = CARTESIAN_POINT('Origin',(80.6,236.901613323034,30.7213203435596)) ;
#83108 = CARTESIAN_POINT('',(81.1,226.002365511524,30.7213203435596)) ;
#83109 = CARTESIAN_POINT('',(81.1,232.568672279644,30.7213203435596)) ;
#83110 = CARTESIAN_POINT('',(80.9535533905933,225.64881212093,30.7213203435596)) ;
#83111 = CARTESIAN_POINT('Origin',(80.6,226.002365511524,30.7213203435596)) ;
#83112 = CARTESIAN_POINT('',(80.1050252531695,224.800283983507,30.7213203435596)) ;
#83113 = CARTESIAN_POINT('',(77.061706774654,221.756965504991,30.7213203435596)) ;
#83114 = CARTESIAN_POINT('',(79.9000000000001,224.305309236676,30.7213203435596)) ;
#83115 = CARTESIAN_POINT('Origin',(80.6000000000001,224.305309236676,30.7213203435596)) ;
#83116 = CARTESIAN_POINT('',(79.9000000000001,217.767014370377,30.7213203435596)) ;
#83117 = CARTESIAN_POINT('',(79.9,228.575260777783,30.7213203435596)) ;
#83118 = CARTESIAN_POINT('',(75.3227721070991,213.926264133629,30.7213203435596)) ;
#83119 = CARTESIAN_POINT('Origin',(76.0000000000001,217.767014370377,30.7213203435596)) ;
#83120 = CARTESIAN_POINT('',(63.8058825236653,215.957002501029,30.7213203435596)) ;
#83121 = CARTESIAN_POINT('',(56.086380506565,217.318158984277,30.7213203435596)) ;
#83122 = CARTESIAN_POINT('',(61.2884174438392,217.560804636007,30.7213203435596)) ;
#83123 = CARTESIAN_POINT('Origin',(64.4831104165663,219.797752737776,30.7213203435596)) ;
#83124 = CARTESIAN_POINT('',(56.7626663401537,224.024247053747,30.7213203435596)) ;
#83125 = CARTESIAN_POINT('',(52.288931387286,230.413402709377,30.7213203435596)) ;
#83126 = CARTESIAN_POINT('',(56.0573593128808,226.261195155516,30.7213203435596)) ;
#83127 = CARTESIAN_POINT('Origin',(59.9573593128808,226.261195155516,30.7213203435596)) ;
#83128 = CARTESIAN_POINT('',(56.0573593128807,244.4,30.7213203435596)) ;
#83129 = CARTESIAN_POINT('',(56.0573593128807,242.191753592594,30.7213203435596)) ;
#83130 = CARTESIAN_POINT('',(55.3573593128808,245.1,30.7213203435596)) ;
#83131 = CARTESIAN_POINT('Origin',(55.3573593128808,244.4,30.7213203435596)) ;
#83132 = CARTESIAN_POINT('',(46.8,245.1,30.7213203435596)) ;
#83133 = CARTESIAN_POINT('',(39.95,245.1,30.7213203435596)) ;
#83134 = CARTESIAN_POINT('',(46.2999999999999,245.6,30.7213203435596)) ;
#83135 = CARTESIAN_POINT('Origin',(46.8,245.6,30.7213203435596)) ;
#83136 = CARTESIAN_POINT('',(46.3,248.9,30.7213203435596)) ;
#83137 = CARTESIAN_POINT('',(46.2999999999999,242.191753592594,30.7213203435596)) ;
#83138 = CARTESIAN_POINT('',(46.1267949192431,249.,30.7213203435596)) ;
#83139 = CARTESIAN_POINT('Ctrl Pts',(46.1267949192431,249.,30.7213203435596)) ;
#83140 = CARTESIAN_POINT('Ctrl Pts',(46.1522826614307,249.,30.7213203435596)) ;
#83141 = CARTESIAN_POINT('Ctrl Pts',(46.1815269526849,248.99104280001,30.7213203435596)) ;
#83142 = CARTESIAN_POINT('Ctrl Pts',(46.2384776727796,248.960391271619,30.7213203435596)) ;
#83143 = CARTESIAN_POINT('Ctrl Pts',(46.2722901777919,248.927709822208,30.7213203435596)) ;
#83144 = CARTESIAN_POINT('Ctrl Pts',(46.3,248.9,30.7213203435596)) ;
#83145 = CARTESIAN_POINT('',(34.2732050807569,249.,30.7213203435596)) ;
#83146 = CARTESIAN_POINT('',(49.95,249.,30.7213203435596)) ;
#83147 = CARTESIAN_POINT('',(34.1,248.9,30.7213203435596)) ;
#83148 = CARTESIAN_POINT('Ctrl Pts',(34.1,248.9,30.7213203435596)) ;
#83149 = CARTESIAN_POINT('Ctrl Pts',(34.1277098222081,248.927709822208,30.7213203435596)) ;
#83150 = CARTESIAN_POINT('Ctrl Pts',(34.1615223272204,248.960391271619,30.7213203435596)) ;
#83151 = CARTESIAN_POINT('Ctrl Pts',(34.2184730473151,248.99104280001,30.7213203435596)) ;
#83152 = CARTESIAN_POINT('Ctrl Pts',(34.2477173385693,249.,30.7213203435596)) ;
#83153 = CARTESIAN_POINT('Ctrl Pts',(34.2732050807569,249.,30.7213203435596)) ;
#83154 = CARTESIAN_POINT('',(34.1,245.6,30.7213203435596)) ;
#83155 = CARTESIAN_POINT('',(34.1000000000001,244.191753592594,30.7213203435596)) ;
#83156 = CARTESIAN_POINT('',(33.6,245.1,30.7213203435596)) ;
#83157 = CARTESIAN_POINT('Origin',(33.6,245.6,30.7213203435596)) ;
#83158 = CARTESIAN_POINT('',(26.8,245.1,30.7213203435596)) ;
#83159 = CARTESIAN_POINT('',(39.95,245.1,30.7213203435596)) ;
#83160 = CARTESIAN_POINT('',(26.3,245.6,30.7213203435596)) ;
#83161 = CARTESIAN_POINT('Origin',(26.8,245.6,30.7213203435596)) ;
#83162 = CARTESIAN_POINT('',(26.3,252.191753592594,30.7213203435596)) ;
#83163 = CARTESIAN_POINT('',(69.2,257.,30.7213203435596)) ;
#83164 = CARTESIAN_POINT('Origin',(73.2,257.,30.7213203435596)) ;
#83165 = CARTESIAN_POINT('',(74.2999999999999,226.1,30.7213203435596)) ;
#83166 = CARTESIAN_POINT('',(74.3999999999999,226.1,30.7213203435596)) ;
#83167 = CARTESIAN_POINT('',(64.1,226.1,30.7213203435596)) ;
#83168 = CARTESIAN_POINT('',(74.2999999999999,231.9,30.7213203435596)) ;
#83169 = CARTESIAN_POINT('',(74.2999999999999,232.691753592594,30.7213203435596)) ;
#83170 = CARTESIAN_POINT('',(74.0999999999999,232.1,30.7213203435596)) ;
#83171 = CARTESIAN_POINT('Origin',(74.0999999999999,231.9,30.7213203435596)) ;
#83172 = CARTESIAN_POINT('',(71.8999999999999,232.1,30.7213203435596)) ;
#83173 = CARTESIAN_POINT('',(63.95,232.1,30.7213203435596)) ;
#83174 = CARTESIAN_POINT('',(71.6999999999999,231.9,30.7213203435596)) ;
#83175 = CARTESIAN_POINT('Origin',(71.8999999999999,231.9,30.7213203435596)) ;
#83176 = CARTESIAN_POINT('',(71.6999999999999,226.1,30.7213203435596)) ;
#83177 = CARTESIAN_POINT('',(71.6999999999999,235.691753592594,30.7213203435596)) ;
#83178 = CARTESIAN_POINT('',(71.5999999999999,226.1,30.7213203435596)) ;
#83179 = CARTESIAN_POINT('',(62.75,226.1,30.7213203435596)) ;
#83180 = CARTESIAN_POINT('',(71.3999999999999,225.9,30.7213203435596)) ;
#83181 = CARTESIAN_POINT('Origin',(71.5999999999999,225.9,30.7213203435596)) ;
#83182 = CARTESIAN_POINT('',(71.3999999999999,223.1,30.7213203435596)) ;
#83183 = CARTESIAN_POINT('',(71.3999999999999,232.691753592594,30.7213203435596)) ;
#83184 = CARTESIAN_POINT('',(71.5999999999999,222.9,30.7213203435596)) ;
#83185 = CARTESIAN_POINT('Origin',(71.5999999999999,223.1,30.7213203435596)) ;
#83186 = CARTESIAN_POINT('',(74.3999999999999,222.9,30.7213203435596)) ;
#83187 = CARTESIAN_POINT('',(62.6,222.9,30.7213203435596)) ;
#83188 = CARTESIAN_POINT('',(74.5999999999999,223.1,30.7213203435596)) ;
#83189 = CARTESIAN_POINT('Origin',(74.3999999999999,223.1,30.7213203435596)) ;
#83190 = CARTESIAN_POINT('',(74.6,225.9,30.7213203435596)) ;
#83191 = CARTESIAN_POINT('',(74.5999999999999,231.191753592594,30.7213203435596)) ;
#83192 = CARTESIAN_POINT('Origin',(74.3999999999999,225.9,30.7213203435596)) ;
#83193 = CARTESIAN_POINT('',(28.1,254.8,30.7213203435596)) ;
#83194 = CARTESIAN_POINT('Origin',(30.7,254.8,30.7213203435596)) ;
#83195 = CARTESIAN_POINT('',(59.,261.2,30.7213203435596)) ;
#83196 = CARTESIAN_POINT('Origin',(61.5,261.2,30.7213203435596)) ;
#83197 = CARTESIAN_POINT('',(80.299999999999,252.4,30.7213203435596)) ;
#83198 = CARTESIAN_POINT('',(80.199999999999,252.4,30.7213203435596)) ;
#83199 = CARTESIAN_POINT('',(66.9499999999999,252.4,30.7213203435596)) ;
#83200 = CARTESIAN_POINT('',(80.299999999999,253.4,30.7213203435596)) ;
#83201 = CARTESIAN_POINT('',(80.2999999999989,243.941753592594,30.7213203435596)) ;
#83202 = CARTESIAN_POINT('',(80.099999999999,253.6,30.7213203435596)) ;
#83203 = CARTESIAN_POINT('Origin',(80.099999999999,253.4,30.7213203435596)) ;
#83204 = CARTESIAN_POINT('',(76.0414213562367,253.6,30.7213203435596)) ;
#83205 = CARTESIAN_POINT('',(66.9499999999995,253.6,30.7213203435596)) ;
#83206 = CARTESIAN_POINT('',(75.8999999999994,253.541421356237,30.7213203435596)) ;
#83207 = CARTESIAN_POINT('Origin',(76.0414213562367,253.4,30.7213203435596)) ;
#83208 = CARTESIAN_POINT('',(75.1585786437621,252.8,30.7213203435596)) ;
#83209 = CARTESIAN_POINT('',(66.6251661181778,244.266587474416,30.7213203435596)) ;
#83210 = CARTESIAN_POINT('',(75.0999999999994,252.658578643763,30.7213203435596)) ;
#83211 = CARTESIAN_POINT('Origin',(75.2999999999994,252.658578643763,30.7213203435596)) ;
#83212 = CARTESIAN_POINT('',(75.0999999999993,249.341421356237,30.7213203435596)) ;
#83213 = CARTESIAN_POINT('',(75.0999999999992,246.441753592594,30.7213203435596)) ;
#83214 = CARTESIAN_POINT('',(75.158578643762,249.2,30.7213203435596)) ;
#83215 = CARTESIAN_POINT('Origin',(75.2999999999993,249.341421356237,30.7213203435596)) ;
#83216 = CARTESIAN_POINT('',(75.8999999999992,248.458578643763,30.7213203435596)) ;
#83217 = CARTESIAN_POINT('',(72.4334125255833,251.925166118179,30.7213203435596)) ;
#83218 = CARTESIAN_POINT('',(76.0414213562365,248.4,30.7213203435596)) ;
#83219 = CARTESIAN_POINT('Origin',(76.0414213562365,248.6,30.7213203435596)) ;
#83220 = CARTESIAN_POINT('',(80.0999999999989,248.4,30.7213203435596)) ;
#83221 = CARTESIAN_POINT('',(64.4499999999996,248.4,30.7213203435596)) ;
#83222 = CARTESIAN_POINT('',(80.2999999999989,248.6,30.7213203435596)) ;
#83223 = CARTESIAN_POINT('Origin',(80.0999999999989,248.6,30.7213203435596)) ;
#83224 = CARTESIAN_POINT('',(80.2999999999989,249.6,30.7213203435596)) ;
#83225 = CARTESIAN_POINT('',(80.2999999999989,243.941753592594,30.7213203435596)) ;
#83226 = CARTESIAN_POINT('',(80.1999999999999,249.6,30.7213203435596)) ;
#83227 = CARTESIAN_POINT('',(66.4500000000001,249.6,30.7213203435596)) ;
#83228 = CARTESIAN_POINT('',(80.1999999999989,243.941753592594,30.7213203435596)) ;
#83229 = CARTESIAN_POINT('',(62.1568347953873,220.146231446812,30.7213203435596)) ;
#83230 = CARTESIAN_POINT('Origin',(64.1568347953873,220.146231446812,30.7213203435596)) ;
#83231 = CARTESIAN_POINT('',(80.099999999999,230.5,30.7213203435596)) ;
#83232 = CARTESIAN_POINT('',(76.0414213562367,230.5,30.7213203435596)) ;
#83233 = CARTESIAN_POINT('',(66.9499999999995,230.5,30.7213203435596)) ;
#83234 = CARTESIAN_POINT('',(75.9707106781181,230.470710678119,30.7213203435596)) ;
#83235 = CARTESIAN_POINT('Origin',(76.0414213562367,230.4,30.7213203435596)) ;
#83236 = CARTESIAN_POINT('',(75.2292893218808,229.729289321881,30.7213203435596)) ;
#83237 = CARTESIAN_POINT('',(72.4458767962964,226.945876796297,30.7213203435596)) ;
#83238 = CARTESIAN_POINT('',(75.1999999999994,229.658578643763,30.7213203435596)) ;
#83239 = CARTESIAN_POINT('Origin',(75.2999999999994,229.658578643763,30.7213203435596)) ;
#83240 = CARTESIAN_POINT('',(75.1999999999993,226.341421356237,30.7213203435596)) ;
#83241 = CARTESIAN_POINT('',(75.1999999999996,234.941753592594,30.7213203435596)) ;
#83242 = CARTESIAN_POINT('',(75.2292893218806,226.270710678119,30.7213203435596)) ;
#83243 = CARTESIAN_POINT('Origin',(75.2999999999993,226.341421356237,30.7213203435596)) ;
#83244 = CARTESIAN_POINT('',(75.9707106781179,225.529289321881,30.7213203435596)) ;
#83245 = CARTESIAN_POINT('',(66.7541232037024,234.745876796297,30.7213203435596)) ;
#83246 = CARTESIAN_POINT('',(76.0414213562366,225.5,30.7213203435596)) ;
#83247 = CARTESIAN_POINT('Origin',(76.0414213562366,225.6,30.7213203435596)) ;
#83248 = CARTESIAN_POINT('',(80.0999999999989,225.5,30.7213203435596)) ;
#83249 = CARTESIAN_POINT('',(64.4499999999996,225.5,30.7213203435596)) ;
#83250 = CARTESIAN_POINT('',(80.199999999999,225.6,30.7213203435596)) ;
#83251 = CARTESIAN_POINT('Origin',(80.0999999999989,225.6,30.7213203435596)) ;
#83252 = CARTESIAN_POINT('',(80.199999999999,226.6,30.7213203435596)) ;
#83253 = CARTESIAN_POINT('',(80.199999999999,232.441753592594,30.7213203435596)) ;
#83254 = CARTESIAN_POINT('',(80.199999999999,229.4,30.7213203435596)) ;
#83255 = CARTESIAN_POINT('',(80.199999999999,232.441753592594,30.7213203435596)) ;
#83256 = CARTESIAN_POINT('',(80.199999999999,230.4,30.7213203435596)) ;
#83257 = CARTESIAN_POINT('',(80.199999999999,232.441753592594,30.7213203435596)) ;
#83258 = CARTESIAN_POINT('Origin',(80.099999999999,230.4,30.7213203435596)) ;
#83259 = CARTESIAN_POINT('',(37.0999999999999,259.9,30.7213203435596)) ;
#83260 = CARTESIAN_POINT('',(37.2999999999999,260.1,30.7213203435596)) ;
#83261 = CARTESIAN_POINT('Origin',(37.2999999999999,259.9,30.7213203435596)) ;
#83262 = CARTESIAN_POINT('',(37.0999999999999,252.1,30.7213203435596)) ;
#83263 = CARTESIAN_POINT('',(37.0999999999999,249.691753592594,30.7213203435596)) ;
#83264 = CARTESIAN_POINT('',(37.2999999999999,251.9,30.7213203435596)) ;
#83265 = CARTESIAN_POINT('Origin',(37.2999999999999,252.1,30.7213203435596)) ;
#83266 = CARTESIAN_POINT('',(43.0999999999999,251.9,30.7213203435596)) ;
#83267 = CARTESIAN_POINT('',(45.4499999999999,251.9,30.7213203435596)) ;
#83268 = CARTESIAN_POINT('',(43.2999999999999,252.1,30.7213203435596)) ;
#83269 = CARTESIAN_POINT('Origin',(43.0999999999999,252.1,30.7213203435596)) ;
#83270 = CARTESIAN_POINT('',(43.2999999999999,259.9,30.7213203435596)) ;
#83271 = CARTESIAN_POINT('',(43.2999999999999,245.691753592594,30.7213203435596)) ;
#83272 = CARTESIAN_POINT('',(43.0999999999999,260.1,30.7213203435596)) ;
#83273 = CARTESIAN_POINT('Origin',(43.0999999999999,259.9,30.7213203435596)) ;
#83274 = CARTESIAN_POINT('',(48.4499999999999,260.1,30.7213203435596)) ;
#83275 = CARTESIAN_POINT('',(57.9573593128807,242.926794919243,30.7213203435596)) ;
#83276 = CARTESIAN_POINT('',(57.9573593128807,241.9,30.7213203435596)) ;
#83277 = CARTESIAN_POINT('',(57.9573593128807,241.191753592594,30.7213203435596)) ;
#83278 = CARTESIAN_POINT('',(57.9573593128807,239.1,30.7213203435596)) ;
#83279 = CARTESIAN_POINT('',(57.9573593128807,241.191753592594,30.7213203435596)) ;
#83280 = CARTESIAN_POINT('',(57.9573593128807,238.073205080757,30.7213203435596)) ;
#83281 = CARTESIAN_POINT('',(57.9573593128807,241.191753592594,30.7213203435596)) ;
#83282 = CARTESIAN_POINT('',(58.0573593128808,237.9,30.7213203435596)) ;
#83283 = CARTESIAN_POINT('Ctrl Pts',(58.0573593128808,237.9,30.7213203435596)) ;
#83284 = CARTESIAN_POINT('Ctrl Pts',(58.0296494906727,237.927709822208,30.7213203435596)) ;
#83285 = CARTESIAN_POINT('Ctrl Pts',(57.9969680412619,237.96152232722,30.7213203435596)) ;
#83286 = CARTESIAN_POINT('Ctrl Pts',(57.9663165128706,238.018473047315,30.7213203435596)) ;
#83287 = CARTESIAN_POINT('Ctrl Pts',(57.9573593128808,238.047717338569,30.7213203435596)) ;
#83288 = CARTESIAN_POINT('Ctrl Pts',(57.9573593128808,238.073205080757,30.7213203435596)) ;
#83289 = CARTESIAN_POINT('',(62.1159379566435,237.9,30.7213203435596)) ;
#83290 = CARTESIAN_POINT('',(55.8286796564404,237.9,30.7213203435596)) ;
#83291 = CARTESIAN_POINT('',(62.2573593128808,237.958578643763,30.7213203435596)) ;
#83292 = CARTESIAN_POINT('Origin',(62.1159379566435,238.1,30.7213203435596)) ;
#83293 = CARTESIAN_POINT('',(62.998780669118,238.7,30.7213203435596)) ;
#83294 = CARTESIAN_POINT('',(60.6596069590762,236.360826289958,30.7213203435596)) ;
#83295 = CARTESIAN_POINT('',(63.0573593128808,238.841421356237,30.7213203435596)) ;
#83296 = CARTESIAN_POINT('Origin',(62.8573593128807,238.841421356237,30.7213203435596)) ;
#83297 = CARTESIAN_POINT('',(63.0573593128807,242.158578643763,30.7213203435596)) ;
#83298 = CARTESIAN_POINT('',(63.0573593128807,238.691753592594,30.7213203435596)) ;
#83299 = CARTESIAN_POINT('',(62.9987806691181,242.3,30.7213203435596)) ;
#83300 = CARTESIAN_POINT('Origin',(62.8573593128807,242.158578643763,30.7213203435596)) ;
#83301 = CARTESIAN_POINT('',(62.2573593128808,243.041421356237,30.7213203435596)) ;
#83302 = CARTESIAN_POINT('',(61.2178533664821,244.080927302636,30.7213203435596)) ;
#83303 = CARTESIAN_POINT('',(62.1159379566435,243.1,30.7213203435596)) ;
#83304 = CARTESIAN_POINT('Origin',(62.1159379566435,242.9,30.7213203435596)) ;
#83305 = CARTESIAN_POINT('',(58.0573593128808,243.1,30.7213203435596)) ;
#83306 = CARTESIAN_POINT('',(58.3286796564404,243.1,30.7213203435596)) ;
#83307 = CARTESIAN_POINT('Ctrl Pts',(57.9573593128808,242.926794919243,30.7213203435596)) ;
#83308 = CARTESIAN_POINT('Ctrl Pts',(57.9573593128808,242.952282661431,30.7213203435596)) ;
#83309 = CARTESIAN_POINT('Ctrl Pts',(57.9663165128706,242.981526952685,30.7213203435596)) ;
#83310 = CARTESIAN_POINT('Ctrl Pts',(57.9969680412619,243.03847767278,30.7213203435596)) ;
#83311 = CARTESIAN_POINT('Ctrl Pts',(58.0296494906727,243.072290177792,30.7213203435596)) ;
#83312 = CARTESIAN_POINT('Ctrl Pts',(58.0573593128808,243.1,30.7213203435596)) ;
#83313 = CARTESIAN_POINT('',(62.2841542321239,236.,30.7213203435596)) ;
#83314 = CARTESIAN_POINT('',(60.0305643936376,236.,30.7213203435596)) ;
#83315 = CARTESIAN_POINT('',(58.0286796564404,236.,30.7213203435596)) ;
#83316 = CARTESIAN_POINT('',(59.8573593128808,235.9,30.7213203435596)) ;
#83317 = CARTESIAN_POINT('Ctrl Pts',(59.8573593128808,235.9,30.7213203435596)) ;
#83318 = CARTESIAN_POINT('Ctrl Pts',(59.8850691350889,235.927709822208,30.7213203435596)) ;
#83319 = CARTESIAN_POINT('Ctrl Pts',(59.9188816401012,235.960391271619,30.7213203435596)) ;
#83320 = CARTESIAN_POINT('Ctrl Pts',(59.9758323601959,235.99104280001,30.7213203435596)) ;
#83321 = CARTESIAN_POINT('Ctrl Pts',(60.0050766514501,236.,30.7213203435596)) ;
#83322 = CARTESIAN_POINT('Ctrl Pts',(60.0305643936377,236.,30.7213203435596)) ;
#83323 = CARTESIAN_POINT('',(59.8573593128808,230.1,30.7213203435596)) ;
#83324 = CARTESIAN_POINT('',(59.8573593128808,237.691753592594,30.7213203435596)) ;
#83325 = CARTESIAN_POINT('',(59.7573593128808,230.1,30.7213203435596)) ;
#83326 = CARTESIAN_POINT('',(56.8286796564404,230.1,30.7213203435596)) ;
#83327 = CARTESIAN_POINT('',(59.5573593128808,229.9,30.7213203435596)) ;
#83328 = CARTESIAN_POINT('Origin',(59.7573593128808,229.9,30.7213203435596)) ;
#83329 = CARTESIAN_POINT('',(59.5573593128808,227.1,30.7213203435596)) ;
#83330 = CARTESIAN_POINT('',(59.5573593128808,234.691753592594,30.7213203435596)) ;
#83331 = CARTESIAN_POINT('',(59.7573593128808,226.9,30.7213203435596)) ;
#83332 = CARTESIAN_POINT('Origin',(59.7573593128808,227.1,30.7213203435596)) ;
#83333 = CARTESIAN_POINT('',(62.5573593128808,226.9,30.7213203435596)) ;
#83334 = CARTESIAN_POINT('',(56.6786796564404,226.9,30.7213203435596)) ;
#83335 = CARTESIAN_POINT('',(62.7573593128808,227.1,30.7213203435596)) ;
#83336 = CARTESIAN_POINT('Origin',(62.5573593128808,227.1,30.7213203435596)) ;
#83337 = CARTESIAN_POINT('',(62.7573593128808,229.9,30.7213203435596)) ;
#83338 = CARTESIAN_POINT('',(62.7573593128808,233.191753592594,30.7213203435596)) ;
#83339 = CARTESIAN_POINT('',(62.5573593128808,230.1,30.7213203435596)) ;
#83340 = CARTESIAN_POINT('Origin',(62.5573593128808,229.9,30.7213203435596)) ;
#83341 = CARTESIAN_POINT('',(62.4573593128808,230.1,30.7213203435596)) ;
#83342 = CARTESIAN_POINT('',(58.1786796564404,230.1,30.7213203435596)) ;
#83343 = CARTESIAN_POINT('',(62.4573593128808,235.9,30.7213203435596)) ;
#83344 = CARTESIAN_POINT('',(62.4573593128808,234.691753592594,30.7213203435596)) ;
#83345 = CARTESIAN_POINT('Ctrl Pts',(62.2841542321239,236.,30.7213203435596)) ;
#83346 = CARTESIAN_POINT('Ctrl Pts',(62.3096419743115,236.,30.7213203435596)) ;
#83347 = CARTESIAN_POINT('Ctrl Pts',(62.3388862655657,235.99104280001,30.7213203435596)) ;
#83348 = CARTESIAN_POINT('Ctrl Pts',(62.3958369856604,235.960391271619,30.7213203435596)) ;
#83349 = CARTESIAN_POINT('Ctrl Pts',(62.4296494906727,235.927709822208,30.7213203435596)) ;
#83350 = CARTESIAN_POINT('Ctrl Pts',(62.4573593128808,235.9,30.7213203435596)) ;
#83351 = CARTESIAN_POINT('',(56.3,250.9,30.7213203435596)) ;
#83352 = CARTESIAN_POINT('',(56.5,251.1,30.7213203435596)) ;
#83353 = CARTESIAN_POINT('Origin',(56.5,250.9,30.7213203435596)) ;
#83354 = CARTESIAN_POINT('',(56.3,248.1,30.7213203435596)) ;
#83355 = CARTESIAN_POINT('',(56.3,245.191753592594,30.7213203435596)) ;
#83356 = CARTESIAN_POINT('',(56.5,247.9,30.7213203435596)) ;
#83357 = CARTESIAN_POINT('Origin',(56.5,248.1,30.7213203435596)) ;
#83358 = CARTESIAN_POINT('',(59.3,247.9,30.7213203435596)) ;
#83359 = CARTESIAN_POINT('',(55.05,247.9,30.7213203435596)) ;
#83360 = CARTESIAN_POINT('',(59.5,248.1,30.7213203435596)) ;
#83361 = CARTESIAN_POINT('Origin',(59.3,248.1,30.7213203435596)) ;
#83362 = CARTESIAN_POINT('',(59.5,250.9,30.7213203435596)) ;
#83363 = CARTESIAN_POINT('',(59.5,243.691753592594,30.7213203435596)) ;
#83364 = CARTESIAN_POINT('',(59.3,251.1,30.7213203435596)) ;
#83365 = CARTESIAN_POINT('Origin',(59.3,250.9,30.7213203435596)) ;
#83366 = CARTESIAN_POINT('',(59.2,251.1,30.7213203435596)) ;
#83367 = CARTESIAN_POINT('',(56.55,251.1,30.7213203435596)) ;
#83368 = CARTESIAN_POINT('',(59.2,256.9,30.7213203435596)) ;
#83369 = CARTESIAN_POINT('',(59.2,245.191753592594,30.7213203435596)) ;
#83370 = CARTESIAN_POINT('',(59.,257.1,30.7213203435596)) ;
#83371 = CARTESIAN_POINT('Origin',(59.,256.9,30.7213203435596)) ;
#83372 = CARTESIAN_POINT('',(56.8,257.1,30.7213203435596)) ;
#83373 = CARTESIAN_POINT('',(56.4,257.1,30.7213203435596)) ;
#83374 = CARTESIAN_POINT('',(56.6,256.9,30.7213203435596)) ;
#83375 = CARTESIAN_POINT('Origin',(56.8,256.9,30.7213203435596)) ;
#83376 = CARTESIAN_POINT('',(56.6,251.1,30.7213203435596)) ;
#83377 = CARTESIAN_POINT('',(56.6,248.191753592594,30.7213203435596)) ;
#83378 = CARTESIAN_POINT('',(55.2,251.1,30.7213203435596)) ;
#83379 = CARTESIAN_POINT('',(64.3,250.9,30.7213203435596)) ;
#83380 = CARTESIAN_POINT('',(64.4999999999999,251.1,30.7213203435596)) ;
#83381 = CARTESIAN_POINT('Origin',(64.4999999999999,250.9,30.7213203435596)) ;
#83382 = CARTESIAN_POINT('',(64.3,248.1,30.7213203435596)) ;
#83383 = CARTESIAN_POINT('',(64.3,245.191753592594,30.7213203435596)) ;
#83384 = CARTESIAN_POINT('',(64.4999999999999,247.9,30.7213203435596)) ;
#83385 = CARTESIAN_POINT('Origin',(64.4999999999999,248.1,30.7213203435596)) ;
#83386 = CARTESIAN_POINT('',(67.3,247.9,30.7213203435596)) ;
#83387 = CARTESIAN_POINT('',(59.05,247.9,30.7213203435596)) ;
#83388 = CARTESIAN_POINT('',(67.5,248.1,30.7213203435596)) ;
#83389 = CARTESIAN_POINT('Origin',(67.3,248.1,30.7213203435596)) ;
#83390 = CARTESIAN_POINT('',(67.5,250.9,30.7213203435596)) ;
#83391 = CARTESIAN_POINT('',(67.5,243.691753592594,30.7213203435596)) ;
#83392 = CARTESIAN_POINT('',(67.3,251.1,30.7213203435596)) ;
#83393 = CARTESIAN_POINT('Origin',(67.3,250.9,30.7213203435596)) ;
#83394 = CARTESIAN_POINT('',(67.2,251.1,30.7213203435596)) ;
#83395 = CARTESIAN_POINT('',(60.55,251.1,30.7213203435596)) ;
#83396 = CARTESIAN_POINT('',(67.2,256.9,30.7213203435596)) ;
#83397 = CARTESIAN_POINT('',(67.2,245.191753592594,30.7213203435596)) ;
#83398 = CARTESIAN_POINT('',(67.,257.1,30.7213203435596)) ;
#83399 = CARTESIAN_POINT('Origin',(67.,256.9,30.7213203435596)) ;
#83400 = CARTESIAN_POINT('',(64.8,257.1,30.7213203435596)) ;
#83401 = CARTESIAN_POINT('',(60.4,257.1,30.7213203435596)) ;
#83402 = CARTESIAN_POINT('',(64.6,256.9,30.7213203435596)) ;
#83403 = CARTESIAN_POINT('Origin',(64.8,256.9,30.7213203435596)) ;
#83404 = CARTESIAN_POINT('',(64.6,251.1,30.7213203435596)) ;
#83405 = CARTESIAN_POINT('',(64.6,248.191753592594,30.7213203435596)) ;
#83406 = CARTESIAN_POINT('',(59.2,251.1,30.7213203435596)) ;
#83407 = CARTESIAN_POINT('',(47.2001799037401,256.996752829339,30.7213203435596)) ;
#83408 = CARTESIAN_POINT('Ctrl Pts',(47.2001799037401,256.996752829339,30.7213203435596)) ;
#83409 = CARTESIAN_POINT('Ctrl Pts',(47.1996958934101,257.592950087367,30.7213203435596)) ;
#83410 = CARTESIAN_POINT('Ctrl Pts',(47.4713258041952,258.790688157784,30.7213203435596)) ;
#83411 = CARTESIAN_POINT('Ctrl Pts',(48.6193980168863,260.233005722467,30.7213203435596)) ;
#83412 = CARTESIAN_POINT('Ctrl Pts',(50.2789716629066,261.032977199702,30.7213203435596)) ;
#83413 = CARTESIAN_POINT('Ctrl Pts',(52.1193940511311,261.033737473045,30.7213203435596)) ;
#83414 = CARTESIAN_POINT('Ctrl Pts',(53.7785648155242,260.233461912991,30.7213203435596)) ;
#83415 = CARTESIAN_POINT('Ctrl Pts',(55.0559915567595,258.636262470822,30.7213203435596)) ;
#83416 = CARTESIAN_POINT('Ctrl Pts',(55.305635860734,256.985238068826,30.7213203435596)) ;
#83417 = CARTESIAN_POINT('Ctrl Pts',(55.0373399291364,255.821578804573,30.7213203435596)) ;
#83418 = CARTESIAN_POINT('Ctrl Pts',(54.6764928726381,254.892517415637,30.7213203435596)) ;
#83419 = CARTESIAN_POINT('Ctrl Pts',(53.7849806154459,253.771240925762,30.7213203435596)) ;
#83420 = CARTESIAN_POINT('Ctrl Pts',(52.1281196619292,252.969136511964,30.7213203435596)) ;
#83421 = CARTESIAN_POINT('Ctrl Pts',(50.2846657419234,252.967612937877,30.7213203435596)) ;
#83422 = CARTESIAN_POINT('Ctrl Pts',(48.6260586034358,253.762867831118,30.7213203435596)) ;
#83423 = CARTESIAN_POINT('Ctrl Pts',(47.4744091088858,255.204607859147,30.7213203435596)) ;
#83424 = CARTESIAN_POINT('Ctrl Pts',(47.2006639140701,256.40055557131,30.7213203435596)) ;
#83425 = CARTESIAN_POINT('Ctrl Pts',(47.2001799037401,256.996752829339,30.7213203435596)) ;
#83426 = CARTESIAN_POINT('Origin',(26.3,263.4,30.3213203435596)) ;
#83427 = CARTESIAN_POINT('',(26.2,263.9,30.3213203435596)) ;
#83428 = CARTESIAN_POINT('',(26.3,263.8,30.3213203435596)) ;
#83429 = CARTESIAN_POINT('Origin',(26.3,263.9,30.3213203435596)) ;
#83430 = CARTESIAN_POINT('Origin',(26.3,263.4,30.3213203435596)) ;
#83431 = CARTESIAN_POINT('',(26.2,263.4,30.8213203435596)) ;
#83432 = CARTESIAN_POINT('Origin',(26.3,263.4,30.8213203435596)) ;
#83433 = CARTESIAN_POINT('Origin',(26.2,263.4,30.3213203435596)) ;
#83434 = CARTESIAN_POINT('Origin',(26.3,263.9,19.9213203435596)) ;
#83435 = CARTESIAN_POINT('',(26.2,263.9,21.9213203435596)) ;
#83436 = CARTESIAN_POINT('',(26.3,263.8,21.9213203435596)) ;
#83437 = CARTESIAN_POINT('Origin',(26.3,263.9,21.9213203435596)) ;
#83438 = CARTESIAN_POINT('',(26.3,263.8,19.9213203435596)) ;
#83439 = CARTESIAN_POINT('',(26.2,263.9,19.9213203435596)) ;
#83440 = CARTESIAN_POINT('Origin',(28.2,263.9,21.9213203435596)) ;
#83441 = CARTESIAN_POINT('',(28.2,263.9,19.9213203435596)) ;
#83442 = CARTESIAN_POINT('',(28.2,263.8,20.0213203435596)) ;
#83443 = CARTESIAN_POINT('Origin',(28.2,263.9,20.0213203435596)) ;
#83444 = CARTESIAN_POINT('Origin',(28.2,263.8,21.9213203435596)) ;
#83445 = CARTESIAN_POINT('Origin',(28.2,263.9,21.9213203435596)) ;
#83446 = CARTESIAN_POINT('Origin',(66.4499999999999,263.9,20.0213203435596)) ;
#83447 = CARTESIAN_POINT('',(35.6,263.9,19.9213203435596)) ;
#83448 = CARTESIAN_POINT('',(35.6,263.8,20.0213203435596)) ;
#83449 = CARTESIAN_POINT('Origin',(35.6,263.9,20.0213203435596)) ;
#83450 = CARTESIAN_POINT('',(66.4499999999999,263.8,20.0213203435596)) ;
#83451 = CARTESIAN_POINT('',(66.4499999999999,263.9,19.9213203435596)) ;
#83452 = CARTESIAN_POINT('Origin',(35.6,263.9,21.9213203435596)) ;
#83453 = CARTESIAN_POINT('',(37.6,263.9,21.9213203435596)) ;
#83454 = CARTESIAN_POINT('',(37.5,263.8,21.9213203435596)) ;
#83455 = CARTESIAN_POINT('Origin',(37.5,263.9,21.9213203435596)) ;
#83456 = CARTESIAN_POINT('Origin',(35.6,263.8,21.9213203435596)) ;
#83457 = CARTESIAN_POINT('Origin',(35.6,263.9,21.9213203435596)) ;
#83458 = CARTESIAN_POINT('Origin',(37.5,263.9,22.4713203435596)) ;
#83459 = CARTESIAN_POINT('',(37.6,263.9,25.0213203435596)) ;
#83460 = CARTESIAN_POINT('',(37.5,263.8,25.0213203435596)) ;
#83461 = CARTESIAN_POINT('Origin',(37.5,263.9,25.0213203435596)) ;
#83462 = CARTESIAN_POINT('',(37.5,263.8,22.4713203435596)) ;
#83463 = CARTESIAN_POINT('',(37.6,263.9,22.4713203435596)) ;
#83464 = CARTESIAN_POINT('Origin',(40.2,263.9,25.0213203435596)) ;
#83465 = CARTESIAN_POINT('',(42.8,263.9,25.0213203435596)) ;
#83466 = CARTESIAN_POINT('',(42.9,263.8,25.0213203435596)) ;
#83467 = CARTESIAN_POINT('Origin',(42.9,263.9,25.0213203435596)) ;
#83468 = CARTESIAN_POINT('Origin',(40.2,263.8,25.0213203435596)) ;
#83469 = CARTESIAN_POINT('Origin',(40.2,263.9,25.0213203435596)) ;
#83470 = CARTESIAN_POINT('Origin',(42.9,263.9,19.9213203435596)) ;
#83471 = CARTESIAN_POINT('',(42.8,263.9,21.9213203435596)) ;
#83472 = CARTESIAN_POINT('',(42.9,263.8,21.9213203435596)) ;
#83473 = CARTESIAN_POINT('Origin',(42.9,263.9,21.9213203435596)) ;
#83474 = CARTESIAN_POINT('',(42.9,263.8,19.9213203435596)) ;
#83475 = CARTESIAN_POINT('',(42.8,263.9,19.9213203435596)) ;
#83476 = CARTESIAN_POINT('Origin',(44.8,263.9,21.9213203435596)) ;
#83477 = CARTESIAN_POINT('',(44.8,263.9,19.9213203435596)) ;
#83478 = CARTESIAN_POINT('',(44.8,263.8,20.0213203435596)) ;
#83479 = CARTESIAN_POINT('Origin',(44.8,263.9,20.0213203435596)) ;
#83480 = CARTESIAN_POINT('Origin',(44.8,263.8,21.9213203435596)) ;
#83481 = CARTESIAN_POINT('Origin',(44.8,263.9,21.9213203435596)) ;
#83482 = CARTESIAN_POINT('Origin',(66.4499999999999,263.9,20.0213203435596)) ;
#83483 = CARTESIAN_POINT('',(77.1999999999999,263.9,19.9213203435596)) ;
#83484 = CARTESIAN_POINT('',(77.1999999999999,263.8,20.0213203435596)) ;
#83485 = CARTESIAN_POINT('Origin',(77.1999999999999,263.9,20.0213203435596)) ;
#83486 = CARTESIAN_POINT('',(66.4499999999999,263.8,20.0213203435596)) ;
#83487 = CARTESIAN_POINT('',(66.4499999999999,263.9,19.9213203435596)) ;
#83488 = CARTESIAN_POINT('Origin',(77.1999999999999,263.9,21.9213203435596)) ;
#83489 = CARTESIAN_POINT('',(79.1999999999999,263.9,21.9213203435596)) ;
#83490 = CARTESIAN_POINT('',(79.0999999999999,263.8,21.9213203435596)) ;
#83491 = CARTESIAN_POINT('Origin',(79.0999999999999,263.9,21.9213203435596)) ;
#83492 = CARTESIAN_POINT('Origin',(77.1999999999999,263.8,21.9213203435596)) ;
#83493 = CARTESIAN_POINT('Origin',(77.1999999999999,263.9,21.9213203435596)) ;
#83494 = CARTESIAN_POINT('Origin',(79.0999999999999,263.9,19.9213203435596)) ;
#83495 = CARTESIAN_POINT('',(79.1999999999999,263.9,30.3213203435596)) ;
#83496 = CARTESIAN_POINT('',(79.0999999999999,263.8,30.3213203435596)) ;
#83497 = CARTESIAN_POINT('Origin',(79.0999999999999,263.9,30.3213203435596)) ;
#83498 = CARTESIAN_POINT('',(79.0999999999999,263.8,19.9213203435596)) ;
#83499 = CARTESIAN_POINT('',(79.1999999999999,263.9,19.9213203435596)) ;
#83500 = CARTESIAN_POINT('Origin',(79.0999999999999,263.4,30.3213203435596)) ;
#83501 = CARTESIAN_POINT('',(79.1999999999999,263.4,30.8213203435596)) ;
#83502 = CARTESIAN_POINT('Origin',(79.1999999999999,263.4,30.3213203435596)) ;
#83503 = CARTESIAN_POINT('Origin',(79.0999999999999,263.4,30.8213203435596)) ;
#83504 = CARTESIAN_POINT('Origin',(79.0999999999999,263.4,30.3213203435596)) ;
#83505 = CARTESIAN_POINT('Origin',(79.1999999999999,259.4,19.9213203435596)) ;
#83506 = CARTESIAN_POINT('',(79.1999999999999,264.9,21.9213203435596)) ;
#83507 = CARTESIAN_POINT('',(79.1999999999999,249.391753592594,21.9213203435596)) ;
#83508 = CARTESIAN_POINT('',(79.1999999999999,264.9,30.7213203435596)) ;
#83509 = CARTESIAN_POINT('',(79.1999999999999,264.9,19.9213203435596)) ;
#83510 = CARTESIAN_POINT('',(79.1999999999999,263.8,31.8213203435596)) ;
#83511 = CARTESIAN_POINT('Origin',(79.1999999999999,263.8,30.7213203435596)) ;
#83512 = CARTESIAN_POINT('',(79.1999999999999,259.648528137424,31.8213203435596)) ;
#83513 = CARTESIAN_POINT('',(79.1999999999999,249.391753592594,31.8213203435596)) ;
#83514 = CARTESIAN_POINT('',(79.1999999999999,259.648528137424,30.8213203435596)) ;
#83515 = CARTESIAN_POINT('',(79.1999999999999,259.648528137424,19.9213203435596)) ;
#83516 = CARTESIAN_POINT('',(79.1999999999999,249.391753592594,30.8213203435596)) ;
#83517 = CARTESIAN_POINT('Origin',(77.1999999999999,249.391753592594,21.9213203435596)) ;
#83518 = CARTESIAN_POINT('',(77.1999999999999,264.9,19.9213203435596)) ;
#83519 = CARTESIAN_POINT('',(77.1999999999999,249.391753592594,19.9213203435596)) ;
#83520 = CARTESIAN_POINT('Origin',(77.1999999999999,264.9,21.9213203435596)) ;
#83521 = CARTESIAN_POINT('Origin',(53.7,239.383507185188,19.9213203435596)) ;
#83522 = CARTESIAN_POINT('',(44.8,264.9,19.9213203435596)) ;
#83523 = CARTESIAN_POINT('',(44.8,252.191753592594,19.9213203435596)) ;
#83524 = CARTESIAN_POINT('',(66.4499999999999,264.9,19.9213203435596)) ;
#83525 = CARTESIAN_POINT('Origin',(44.8,252.191753592594,21.9213203435596)) ;
#83526 = CARTESIAN_POINT('',(42.8,264.9,21.9213203435596)) ;
#83527 = CARTESIAN_POINT('',(42.8,252.191753592594,21.9213203435596)) ;
#83528 = CARTESIAN_POINT('Origin',(44.8,264.9,21.9213203435596)) ;
#83529 = CARTESIAN_POINT('Origin',(42.8,265.,19.9213203435596)) ;
#83530 = CARTESIAN_POINT('',(42.8,264.9,25.0213203435596)) ;
#83531 = CARTESIAN_POINT('',(42.8,265.,25.0213203435596)) ;
#83532 = CARTESIAN_POINT('',(42.8,264.9,19.9213203435596)) ;
#83533 = CARTESIAN_POINT('Origin',(40.2,265.,25.0213203435596)) ;
#83534 = CARTESIAN_POINT('',(37.6,264.9,25.0213203435596)) ;
#83535 = CARTESIAN_POINT('',(37.6,265.,25.0213203435596)) ;
#83536 = CARTESIAN_POINT('Origin',(40.2,264.9,25.0213203435596)) ;
#83537 = CARTESIAN_POINT('Origin',(37.6,265.,25.0213203435596)) ;
#83538 = CARTESIAN_POINT('',(37.6,264.9,21.9213203435596)) ;
#83539 = CARTESIAN_POINT('',(37.6,252.191753592594,21.9213203435596)) ;
#83540 = CARTESIAN_POINT('',(37.6,264.9,22.4713203435596)) ;
#83541 = CARTESIAN_POINT('Origin',(35.6,252.191753592594,21.9213203435596)) ;
#83542 = CARTESIAN_POINT('',(35.6,264.9,19.9213203435596)) ;
#83543 = CARTESIAN_POINT('',(35.6,252.191753592594,19.9213203435596)) ;
#83544 = CARTESIAN_POINT('Origin',(35.6,264.9,21.9213203435596)) ;
#83545 = CARTESIAN_POINT('Origin',(53.7,239.383507185188,19.9213203435596)) ;
#83546 = CARTESIAN_POINT('',(28.2,264.9,19.9213203435596)) ;
#83547 = CARTESIAN_POINT('',(28.2,252.191753592594,19.9213203435596)) ;
#83548 = CARTESIAN_POINT('',(66.4499999999999,264.9,19.9213203435596)) ;
#83549 = CARTESIAN_POINT('Origin',(28.2,252.191753592594,21.9213203435596)) ;
#83550 = CARTESIAN_POINT('',(26.2,264.9,21.9213203435596)) ;
#83551 = CARTESIAN_POINT('',(26.2,252.191753592594,21.9213203435596)) ;
#83552 = CARTESIAN_POINT('Origin',(28.2,264.9,21.9213203435596)) ;
#83553 = CARTESIAN_POINT('Origin',(26.2,265.,19.9213203435596)) ;
#83554 = CARTESIAN_POINT('',(26.2,245.6,30.8213203435596)) ;
#83555 = CARTESIAN_POINT('',(26.2,252.191753592594,30.8213203435596)) ;
#83556 = CARTESIAN_POINT('',(26.2,245.6,31.8213203435596)) ;
#83557 = CARTESIAN_POINT('',(26.2,245.6,19.9213203435596)) ;
#83558 = CARTESIAN_POINT('',(26.2,263.8,31.8213203435596)) ;
#83559 = CARTESIAN_POINT('',(26.2,252.191753592594,31.8213203435596)) ;
#83560 = CARTESIAN_POINT('',(26.2,264.9,30.7213203435596)) ;
#83561 = CARTESIAN_POINT('Origin',(26.2,263.8,30.7213203435596)) ;
#83562 = CARTESIAN_POINT('',(26.2,264.9,19.9213203435596)) ;
#83563 = CARTESIAN_POINT('Origin',(73.2,257.,29.7213203435596)) ;
#83564 = CARTESIAN_POINT('',(70.2,257.,29.7213203435596)) ;
#83565 = CARTESIAN_POINT('Origin',(69.2,257.,29.7213203435596)) ;
#83566 = CARTESIAN_POINT('Origin',(73.2,257.,29.7213203435596)) ;
#83567 = CARTESIAN_POINT('Origin',(73.2,257.,28.9213203435596)) ;
#83568 = CARTESIAN_POINT('',(70.2,257.,29.6213203435596)) ;
#83569 = CARTESIAN_POINT('',(70.2,257.,28.9213203435596)) ;
#83570 = CARTESIAN_POINT('Origin',(73.2,257.,29.6213203435596)) ;
#83571 = CARTESIAN_POINT('Ctrl Pts',(48.2000201227716,256.997564528802,29.7391774864168)) ;
#83572 = CARTESIAN_POINT('Ctrl Pts',(48.1996571011318,257.444729584704,29.7391774864168)) ;
#83573 = CARTESIAN_POINT('Ctrl Pts',(48.4033873306915,258.343067515653,29.7391774864168)) ;
#83574 = CARTESIAN_POINT('Ctrl Pts',(49.2644744428091,259.424847087356,29.7391774864168)) ;
#83575 = CARTESIAN_POINT('Ctrl Pts',(50.5092023113187,260.024848656503,29.7391774864168)) ;
#83576 = CARTESIAN_POINT('Ctrl Pts',(51.8895719273014,260.025418883332,29.7391774864168)) ;
#83577 = CARTESIAN_POINT('Ctrl Pts',(53.1339976230268,259.425189243343,29.7391774864168)) ;
#83578 = CARTESIAN_POINT('Ctrl Pts',(54.0921043443573,258.227243818021,29.7391774864167)) ;
#83579 = CARTESIAN_POINT('Ctrl Pts',(54.2793447377661,256.988928127914,29.7391774864167)) ;
#83580 = CARTESIAN_POINT('Ctrl Pts',(54.0781150882907,256.116150279737,29.7391774864167)) ;
#83581 = CARTESIAN_POINT('Ctrl Pts',(53.8074694386866,255.419327571605,29.7391774864167)) ;
#83582 = CARTESIAN_POINT('Ctrl Pts',(53.138809657118,254.578338020705,29.7391774864167)) ;
#83583 = CARTESIAN_POINT('Ctrl Pts',(51.8961163858473,253.976736687915,29.7391774864168)) ;
#83584 = CARTESIAN_POINT('Ctrl Pts',(50.5134730340159,253.975593963619,29.7391774864168)) ;
#83585 = CARTESIAN_POINT('Ctrl Pts',(49.2694700738971,254.572057959393,29.7391774864168)) ;
#83586 = CARTESIAN_POINT('Ctrl Pts',(48.4056998977081,255.653404362029,29.7391774864168)) ;
#83587 = CARTESIAN_POINT('Ctrl Pts',(48.2003831444115,256.550399472899,29.7391774864168)) ;
#83588 = CARTESIAN_POINT('Ctrl Pts',(48.2000201227716,256.997564528802,29.7391774864168)) ;
#83589 = CARTESIAN_POINT('Ctrl Pts',(48.1947380216729,256.997560240638,30.0349280800261)) ;
#83590 = CARTESIAN_POINT('Ctrl Pts',(48.1943747281785,257.445060163369,30.0349280800261)) ;
#83591 = CARTESIAN_POINT('Ctrl Pts',(48.3987531591452,258.34442732955,30.0349280800261)) ;
#83592 = CARTESIAN_POINT('Ctrl Pts',(49.2614119341439,259.427283390293,30.0349280800261)) ;
#83593 = CARTESIAN_POINT('Ctrl Pts',(50.5074335198535,260.027951447571,30.0349280800261)) ;
#83594 = CARTESIAN_POINT('Ctrl Pts',(51.889675953912,260.028326821561,30.0349280800261)) ;
#83595 = CARTESIAN_POINT('Ctrl Pts',(53.1358585454785,259.427468823063,30.0349280800261)) ;
#83596 = CARTESIAN_POINT('Ctrl Pts',(54.0948641455133,258.228316050248,30.0349280800261)) ;
#83597 = CARTESIAN_POINT('Ctrl Pts',(54.2823703564133,256.988738847751,30.0349280800261)) ;
#83598 = CARTESIAN_POINT('Ctrl Pts',(54.0809503109861,256.115159784954,30.0349280800261)) ;
#83599 = CARTESIAN_POINT('Ctrl Pts',(53.8099967208346,255.41769815285,30.0349280800261)) ;
#83600 = CARTESIAN_POINT('Ctrl Pts',(53.1404967730488,254.575643430502,30.0349280800261)) ;
#83601 = CARTESIAN_POINT('Ctrl Pts',(51.8964734498615,253.973593813523,30.0349280800261)) ;
#83602 = CARTESIAN_POINT('Ctrl Pts',(50.5123829163539,253.972292508993,30.0349280800261)) ;
#83603 = CARTESIAN_POINT('Ctrl Pts',(49.2664516588918,254.569603468298,30.0349280800261)) ;
#83604 = CARTESIAN_POINT('Ctrl Pts',(48.4011338558011,255.652030289862,30.0349280800261)) ;
#83605 = CARTESIAN_POINT('Ctrl Pts',(48.1951013151674,256.550060317907,30.0349280800261)) ;
#83606 = CARTESIAN_POINT('Ctrl Pts',(48.1947380216729,256.997560240638,30.0349280800261)) ;
#83607 = CARTESIAN_POINT('Ctrl Pts',(47.9403271495437,256.997353702469,30.5426019839815)) ;
#83608 = CARTESIAN_POINT('Ctrl Pts',(47.9399326186896,257.483331374468,30.5426019839815)) ;
#83609 = CARTESIAN_POINT('Ctrl Pts',(48.1612323137361,258.459560607115,30.5426019839815)) ;
#83610 = CARTESIAN_POINT('Ctrl Pts',(49.0968466073856,259.63517435474,30.5426019839815)) ;
#83611 = CARTESIAN_POINT('Ctrl Pts',(50.4495302427206,260.287204473252,30.5426019839815)) ;
#83612 = CARTESIAN_POINT('Ctrl Pts',(51.9495193659296,260.287869000223,30.5426019839815)) ;
#83613 = CARTESIAN_POINT('Ctrl Pts',(53.3017682744996,259.635582227122,30.5426019839815)) ;
#83614 = CARTESIAN_POINT('Ctrl Pts',(54.3429942328016,258.333729835107,30.5426019839814)) ;
#83615 = CARTESIAN_POINT('Ctrl Pts',(54.5464577252491,256.988008648977,30.5426019839814)) ;
#83616 = CARTESIAN_POINT('Ctrl Pts',(54.3277710414745,256.039510112854,30.5426019839814)) ;
#83617 = CARTESIAN_POINT('Ctrl Pts',(54.0336582949932,255.282232103612,30.5426019839814)) ;
#83618 = CARTESIAN_POINT('Ctrl Pts',(53.3070386850274,254.368347021547,30.5426019839814)) ;
#83619 = CARTESIAN_POINT('Ctrl Pts',(51.9565749304451,253.714527943762,30.5426019839815)) ;
#83620 = CARTESIAN_POINT('Ctrl Pts',(50.4540166666556,253.713322223552,30.5426019839815)) ;
#83621 = CARTESIAN_POINT('Ctrl Pts',(49.1022665858778,254.361465700547,30.5426019839815)) ;
#83622 = CARTESIAN_POINT('Ctrl Pts',(48.163730370093,255.536607705174,30.5426019839815)) ;
#83623 = CARTESIAN_POINT('Ctrl Pts',(47.9407216803977,256.511376030469,30.5426019839815)) ;
#83624 = CARTESIAN_POINT('Ctrl Pts',(47.9403271495437,256.997353702469,30.5426019839815)) ;
#83625 = CARTESIAN_POINT('Ctrl Pts',(47.4220281498853,256.996932932218,30.7213203435596)) ;
#83626 = CARTESIAN_POINT('Ctrl Pts',(47.4215709320604,257.560127551602,30.7213203435596)) ;
#83627 = CARTESIAN_POINT('Ctrl Pts',(47.6780933089332,258.691513196809,30.7213203435596)) ;
#83628 = CARTESIAN_POINT('Ctrl Pts',(48.7624802059068,260.053952562978,30.7213203435596)) ;
#83629 = CARTESIAN_POINT('Ctrl Pts',(50.3301356783258,260.809610148858,30.7213203435596)) ;
#83630 = CARTESIAN_POINT('Ctrl Pts',(52.0685601808136,260.810356467353,30.7213203435596)) ;
#83631 = CARTESIAN_POINT('Ctrl Pts',(53.6357683192668,260.054406114016,30.7213203435596)) ;
#83632 = CARTESIAN_POINT('Ctrl Pts',(54.8424566758268,258.545664711818,30.7213203435596)) ;
#83633 = CARTESIAN_POINT('Ctrl Pts',(55.0782637682426,256.986081290598,30.7213203435596)) ;
#83634 = CARTESIAN_POINT('Ctrl Pts',(54.824825139774,255.886857921965,30.7213203435596)) ;
#83635 = CARTESIAN_POINT('Ctrl Pts',(54.4839680197378,255.009241811416,30.7213203435596)) ;
#83636 = CARTESIAN_POINT('Ctrl Pts',(53.6418545271852,253.950096561179,30.7213203435596)) ;
#83637 = CARTESIAN_POINT('Ctrl Pts',(52.0767670390764,253.192392502866,30.7213203435596)) ;
#83638 = CARTESIAN_POINT('Ctrl Pts',(50.3354172573281,253.19097598695,30.7213203435596)) ;
#83639 = CARTESIAN_POINT('Ctrl Pts',(48.7687662812976,253.942151697168,30.7213203435596)) ;
#83640 = CARTESIAN_POINT('Ctrl Pts',(47.6809963718967,255.304044883527,30.7213203435596)) ;
#83641 = CARTESIAN_POINT('Ctrl Pts',(47.4224853677104,256.433738312834,30.7213203435596)) ;
#83642 = CARTESIAN_POINT('Ctrl Pts',(47.4220281498854,256.996932932218,30.7213203435596)) ;
#83643 = CARTESIAN_POINT('Ctrl Pts',(47.2001799037401,256.996752829339,30.7213203435596)) ;
#83644 = CARTESIAN_POINT('Ctrl Pts',(47.1996958934101,257.592950087367,30.7213203435596)) ;
#83645 = CARTESIAN_POINT('Ctrl Pts',(47.4713258041952,258.790688157784,30.7213203435596)) ;
#83646 = CARTESIAN_POINT('Ctrl Pts',(48.6193980168863,260.233005722467,30.7213203435596)) ;
#83647 = CARTESIAN_POINT('Ctrl Pts',(50.2789716629066,261.032977199702,30.7213203435596)) ;
#83648 = CARTESIAN_POINT('Ctrl Pts',(52.1193940511311,261.033737473045,30.7213203435596)) ;
#83649 = CARTESIAN_POINT('Ctrl Pts',(53.7785648155242,260.233461912991,30.7213203435596)) ;
#83650 = CARTESIAN_POINT('Ctrl Pts',(55.0559915567595,258.636262470822,30.7213203435596)) ;
#83651 = CARTESIAN_POINT('Ctrl Pts',(55.305635860734,256.985238068826,30.7213203435596)) ;
#83652 = CARTESIAN_POINT('Ctrl Pts',(55.0373399291364,255.821578804573,30.7213203435596)) ;
#83653 = CARTESIAN_POINT('Ctrl Pts',(54.6764928726381,254.892517415637,30.7213203435596)) ;
#83654 = CARTESIAN_POINT('Ctrl Pts',(53.7849806154459,253.771240925762,30.7213203435596)) ;
#83655 = CARTESIAN_POINT('Ctrl Pts',(52.1281196619292,252.969136511964,30.7213203435596)) ;
#83656 = CARTESIAN_POINT('Ctrl Pts',(50.2846657419234,252.967612937877,30.7213203435596)) ;
#83657 = CARTESIAN_POINT('Ctrl Pts',(48.6260586034358,253.762867831118,30.7213203435596)) ;
#83658 = CARTESIAN_POINT('Ctrl Pts',(47.4744091088858,255.204607859147,30.7213203435596)) ;
#83659 = CARTESIAN_POINT('Ctrl Pts',(47.2006639140701,256.40055557131,30.7213203435596)) ;
#83660 = CARTESIAN_POINT('Ctrl Pts',(47.2001799037401,256.996752829339,30.7213203435596)) ;
#83661 = CARTESIAN_POINT('',(48.2000203746466,256.99756452918,29.7391774849179)) ;
#83662 = CARTESIAN_POINT('Ctrl Pts',(47.2001799037401,256.996752829339,30.7213203435596)) ;
#83663 = CARTESIAN_POINT('Ctrl Pts',(47.4220281498853,256.996932932218,30.7213203435596)) ;
#83664 = CARTESIAN_POINT('Ctrl Pts',(47.9403271495437,256.997353702469,30.5426019839815)) ;
#83665 = CARTESIAN_POINT('Ctrl Pts',(48.1947380216729,256.997560240638,30.0349280800261)) ;
#83666 = CARTESIAN_POINT('Ctrl Pts',(48.2000201227716,256.997564528802,29.7391774864168)) ;
#83667 = CARTESIAN_POINT('',(48.2000195339838,256.999999959719,29.7391774864168)) ;
#83668 = CARTESIAN_POINT('Ctrl Pts',(48.2000208783164,256.997564529727,29.7391774864168)) ;
#83669 = CARTESIAN_POINT('Ctrl Pts',(48.2005690937809,256.549587458459,29.7391774864168)) ;
#83670 = CARTESIAN_POINT('Ctrl Pts',(48.4059605550267,255.653078047389,29.7391774864168)) ;
#83671 = CARTESIAN_POINT('Ctrl Pts',(49.2694700738971,254.572057959393,29.7391774864168)) ;
#83672 = CARTESIAN_POINT('Ctrl Pts',(50.5134730340159,253.975593963619,29.7391774864168)) ;
#83673 = CARTESIAN_POINT('Ctrl Pts',(51.8961163858473,253.976736687915,29.7391774864168)) ;
#83674 = CARTESIAN_POINT('Ctrl Pts',(53.138809657118,254.578338020705,29.7391774864167)) ;
#83675 = CARTESIAN_POINT('Ctrl Pts',(53.8074694386866,255.419327571605,29.7391774864167)) ;
#83676 = CARTESIAN_POINT('Ctrl Pts',(54.0781150882907,256.116150279737,29.7391774864167)) ;
#83677 = CARTESIAN_POINT('Ctrl Pts',(54.2793447377661,256.988928127914,29.7391774864167)) ;
#83678 = CARTESIAN_POINT('Ctrl Pts',(54.0921043443573,258.227243818021,29.7391774864167)) ;
#83679 = CARTESIAN_POINT('Ctrl Pts',(53.1339976230268,259.425189243343,29.7391774864168)) ;
#83680 = CARTESIAN_POINT('Ctrl Pts',(51.8895719273014,260.025418883332,29.7391774864168)) ;
#83681 = CARTESIAN_POINT('Ctrl Pts',(50.5092023113187,260.024848656503,29.7391774864168)) ;
#83682 = CARTESIAN_POINT('Ctrl Pts',(49.2644744428091,259.424847087356,29.7391774864168)) ;
#83683 = CARTESIAN_POINT('Ctrl Pts',(48.4041682584632,258.344048591433,29.7391774864168)) ;
#83684 = CARTESIAN_POINT('Ctrl Pts',(48.200212080878,257.447173389509,29.7391774864168)) ;
#83685 = CARTESIAN_POINT('Ctrl Pts',(48.2000199116081,256.999999959709,29.7391774864168)) ;
#83686 = CARTESIAN_POINT('',(48.2000191563594,256.999999960043,29.7391774864168)) ;
#83687 = CARTESIAN_POINT('Origin',(51.2,257.,29.7413203435596)) ;
#83688 = CARTESIAN_POINT('',(48.32,257.,29.6213203435596)) ;
#83689 = CARTESIAN_POINT('Origin',(48.32,257.,29.7413203435596)) ;
#83690 = CARTESIAN_POINT('Origin',(51.2,257.,29.6213203435596)) ;
#83691 = CARTESIAN_POINT('Origin',(51.2,257.,29.6213203435596)) ;
#83692 = CARTESIAN_POINT('',(53.32,257.,29.6213203435596)) ;
#83693 = CARTESIAN_POINT('Origin',(51.2,257.,29.6213203435596)) ;
#83694 = CARTESIAN_POINT('Origin',(51.2,257.,29.7413203435596)) ;
#83695 = CARTESIAN_POINT('',(49.2,257.,29.7413203435596)) ;
#83696 = CARTESIAN_POINT('',(53.2,257.,29.7413203435596)) ;
#83697 = CARTESIAN_POINT('Origin',(51.2,257.,29.7413203435596)) ;
#83698 = CARTESIAN_POINT('Origin',(53.32,257.,29.7413203435596)) ;
#83699 = CARTESIAN_POINT('Origin',(51.2,257.,29.7413203435596)) ;
#83700 = CARTESIAN_POINT('Origin',(51.2,257.,19.9213203435596)) ;
#83701 = CARTESIAN_POINT('',(49.2,257.,30.1213203435596)) ;
#83702 = CARTESIAN_POINT('',(49.2,257.,19.9213203435596)) ;
#83703 = CARTESIAN_POINT('Origin',(51.2,257.,30.1213203435596)) ;
#83704 = CARTESIAN_POINT('Origin',(73.1999999999999,263.88342319271,27.1425655430194)) ;
#83705 = CARTESIAN_POINT('',(73.1999999999999,263.59500851924,29.0950298771693)) ;
#83706 = CARTESIAN_POINT('Origin',(73.1999999999999,264.000849166908,27.1672868007454)) ;
#83707 = CARTESIAN_POINT('',(73.1999999999999,263.502303802768,28.9528826452449)) ;
#83708 = CARTESIAN_POINT('Origin',(73.1999999999999,263.477582545042,29.0703086194433)) ;
#83709 = CARTESIAN_POINT('',(75.0499999999999,263.88342319271,27.1425655430194)) ;
#83710 = CARTESIAN_POINT('Origin',(73.1999999999999,263.88342319271,27.1425655430194)) ;
#83711 = CARTESIAN_POINT('Origin',(73.1999999999999,263.88342319271,27.1425655430194)) ;
#83712 = CARTESIAN_POINT('Origin',(73.1999999999999,264.000849166908,27.1672868007454)) ;
#83713 = CARTESIAN_POINT('',(75.0499999999999,262.944015399123,26.9447954812117)) ;
#83714 = CARTESIAN_POINT('',(75.0499999999999,264.000849166908,27.1672868007454)) ;
#83715 = CARTESIAN_POINT('',(73.1999999999999,263.325134789065,25.134478378986)) ;
#83716 = CARTESIAN_POINT('Origin',(73.1999999999999,262.944015399123,26.9447954812115)) ;
#83717 = CARTESIAN_POINT('Origin',(73.1999999999999,262.944015399123,26.9447954812115)) ;
#83718 = CARTESIAN_POINT('Origin',(75.1,264.,27.1713203435596)) ;
#83719 = CARTESIAN_POINT('',(76.5,263.20058682584,30.9685329208194)) ;
#83720 = CARTESIAN_POINT('',(69.9,263.20058682584,30.9685329208194)) ;
#83721 = CARTESIAN_POINT('',(64.4,263.20058682584,30.9685329208194)) ;
#83722 = CARTESIAN_POINT('',(76.5,264.010725107507,27.120376082903)) ;
#83723 = CARTESIAN_POINT('',(76.5,264.75198938992,23.5993707414376)) ;
#83724 = CARTESIAN_POINT('',(77.3539593550092,265.,22.4213203435597)) ;
#83725 = CARTESIAN_POINT('Origin',(77.5,264.010725107507,27.1203760829029)) ;
#83726 = CARTESIAN_POINT('',(69.0460404446207,265.,22.4213203435596)) ;
#83727 = CARTESIAN_POINT('',(26.2,265.,22.4213203435596)) ;
#83728 = CARTESIAN_POINT('',(69.9,264.010725107507,27.1203760829029)) ;
#83729 = CARTESIAN_POINT('Origin',(68.8999999999999,264.010725107507,27.1203760829029)) ;
#83730 = CARTESIAN_POINT('',(69.9,264.709549071618,23.8009622533739)) ;
#83731 = CARTESIAN_POINT('Origin',(73.1999999999999,262.944015399123,26.9447954812115)) ;
#83732 = CARTESIAN_POINT('',(73.1999999999999,263.232430072592,24.9923311470616)) ;
#83733 = CARTESIAN_POINT('Origin',(73.1999999999999,262.826589424924,26.9200742234855)) ;
#83734 = CARTESIAN_POINT('Origin',(73.1999999999999,263.349856046791,25.0170524047876)) ;
#83735 = CARTESIAN_POINT('Origin',(75.1,262.825740258016,26.9241077662998)) ;
#83736 = CARTESIAN_POINT('',(77.2325869638084,263.799952628918,22.2965990045162)) ;
#83737 = CARTESIAN_POINT('',(76.5,262.836465365522,26.8731635056432)) ;
#83738 = CARTESIAN_POINT('Ctrl Pts',(77.2324172913864,263.799905257836,22.2968240171558)) ;
#83739 = CARTESIAN_POINT('Ctrl Pts',(77.0709872482774,263.754804582325,22.5110522258322)) ;
#83740 = CARTESIAN_POINT('Ctrl Pts',(76.6823307971632,263.532544066078,23.5667896780028)) ;
#83741 = CARTESIAN_POINT('Ctrl Pts',(76.4999999999999,263.102238319793,25.6107419728579)) ;
#83742 = CARTESIAN_POINT('Ctrl Pts',(76.5,262.836465365523,26.8731635056432)) ;
#83743 = CARTESIAN_POINT('',(76.5,263.577729647936,23.3521581641778)) ;
#83744 = CARTESIAN_POINT('',(69.9,262.836465365522,26.8731635056431)) ;
#83745 = CARTESIAN_POINT('',(69.9,263.535289329634,23.5537496761141)) ;
#83746 = CARTESIAN_POINT('',(69.1671450699313,263.79990527434,22.2968239387601)) ;
#83747 = CARTESIAN_POINT('Ctrl Pts',(69.8999999999999,262.836465365523,26.8731635056431)) ;
#83748 = CARTESIAN_POINT('Ctrl Pts',(69.9,263.036041279363,25.9251779149008)) ;
#83749 = CARTESIAN_POINT('Ctrl Pts',(69.766510541265,263.46977838237,23.8649266756155)) ;
#83750 = CARTESIAN_POINT('Ctrl Pts',(69.3922529932014,263.736480055353,22.598093728948)) ;
#83751 = CARTESIAN_POINT('Ctrl Pts',(69.1674817299058,263.79981054868,22.2972738856443)) ;
#83752 = CARTESIAN_POINT('',(77.1499999999999,263.8,22.2963739918749)) ;
#83753 = CARTESIAN_POINT('Origin',(51.1999999999999,263.88342319271,27.1425655430194)) ;
#83754 = CARTESIAN_POINT('',(51.1999999999999,263.59500851924,29.0950298771693)) ;
#83755 = CARTESIAN_POINT('Origin',(51.1999999999999,264.000849166908,27.1672868007454)) ;
#83756 = CARTESIAN_POINT('',(51.1999999999999,263.502303802768,28.9528826452449)) ;
#83757 = CARTESIAN_POINT('Origin',(51.1999999999999,263.477582545042,29.0703086194433)) ;
#83758 = CARTESIAN_POINT('',(53.0499999999999,263.88342319271,27.1425655430194)) ;
#83759 = CARTESIAN_POINT('Origin',(51.1999999999999,263.88342319271,27.1425655430194)) ;
#83760 = CARTESIAN_POINT('Origin',(51.1999999999999,263.88342319271,27.1425655430194)) ;
#83761 = CARTESIAN_POINT('Origin',(51.1999999999999,264.000849166908,27.1672868007454)) ;
#83762 = CARTESIAN_POINT('',(53.0499999999999,262.944015399123,26.9447954812117)) ;
#83763 = CARTESIAN_POINT('',(53.0499999999999,264.000849166908,27.1672868007454)) ;
#83764 = CARTESIAN_POINT('',(51.1999999999999,263.325134789065,25.134478378986)) ;
#83765 = CARTESIAN_POINT('Origin',(51.1999999999999,262.944015399123,26.9447954812115)) ;
#83766 = CARTESIAN_POINT('Origin',(51.1999999999999,262.944015399123,26.9447954812115)) ;
#83767 = CARTESIAN_POINT('Origin',(53.1,264.,27.1713203435596)) ;
#83768 = CARTESIAN_POINT('',(54.5,263.20058682584,30.9685329208194)) ;
#83769 = CARTESIAN_POINT('',(47.9,263.20058682584,30.9685329208194)) ;
#83770 = CARTESIAN_POINT('',(53.4,263.20058682584,30.9685329208194)) ;
#83771 = CARTESIAN_POINT('',(54.5,264.010725107507,27.120376082903)) ;
#83772 = CARTESIAN_POINT('',(54.5,264.75198938992,23.5993707414376)) ;
#83773 = CARTESIAN_POINT('',(55.3539343055938,265.,22.4213203435596)) ;
#83774 = CARTESIAN_POINT('Origin',(55.5,264.010725107507,27.1203760829029)) ;
#83775 = CARTESIAN_POINT('',(47.0460398203948,265.,22.4213203435596)) ;
#83776 = CARTESIAN_POINT('',(26.2,265.,22.4213203435596)) ;
#83777 = CARTESIAN_POINT('',(47.9,264.010725107507,27.1203760829029)) ;
#83778 = CARTESIAN_POINT('Origin',(46.9,264.010725107507,27.1203760829029)) ;
#83779 = CARTESIAN_POINT('',(47.9,264.709549071618,23.8009622533739)) ;
#83780 = CARTESIAN_POINT('Origin',(51.1999999999999,262.944015399123,26.9447954812115)) ;
#83781 = CARTESIAN_POINT('',(51.1999999999999,263.232430072592,24.9923311470617)) ;
#83782 = CARTESIAN_POINT('Origin',(51.1999999999999,262.826589424924,26.9200742234856)) ;
#83783 = CARTESIAN_POINT('Origin',(51.1999999999999,263.349856046791,25.0170524047876)) ;
#83784 = CARTESIAN_POINT('Origin',(53.1,262.825740258016,26.9241077662998)) ;
#83785 = CARTESIAN_POINT('',(47.9,262.836465365522,26.8731635056431)) ;
#83786 = CARTESIAN_POINT('',(47.1671452090265,263.799905296423,22.2968238338636)) ;
#83787 = CARTESIAN_POINT('Ctrl Pts',(47.9,262.836465365523,26.8731635056431)) ;
#83788 = CARTESIAN_POINT('Ctrl Pts',(47.9,263.036041279363,25.925177914903)) ;
#83789 = CARTESIAN_POINT('Ctrl Pts',(47.7665130315213,263.469780156239,23.8649182497395)) ;
#83790 = CARTESIAN_POINT('Ctrl Pts',(47.3922533394392,263.736480301986,22.5980925574409)) ;
#83791 = CARTESIAN_POINT('Ctrl Pts',(47.1674817919091,263.799810592846,22.2972736758538)) ;
#83792 = CARTESIAN_POINT('',(55.2325867846313,263.799952660996,22.2965988521424)) ;
#83793 = CARTESIAN_POINT('',(66.1499999999999,263.8,22.2963739918749)) ;
#83794 = CARTESIAN_POINT('',(54.5,262.836465365522,26.8731635056432)) ;
#83795 = CARTESIAN_POINT('Ctrl Pts',(55.2324172261571,263.799905321993,22.2968237124103)) ;
#83796 = CARTESIAN_POINT('Ctrl Pts',(55.0709869664947,263.754804859476,22.511050909364)) ;
#83797 = CARTESIAN_POINT('Ctrl Pts',(54.6823287364216,263.532546092952,23.5667800503536)) ;
#83798 = CARTESIAN_POINT('Ctrl Pts',(54.4999999999999,263.102238319793,25.6107419728589)) ;
#83799 = CARTESIAN_POINT('Ctrl Pts',(54.5,262.836465365523,26.8731635056432)) ;
#83800 = CARTESIAN_POINT('',(54.5,263.577729647936,23.3521581641778)) ;
#83801 = CARTESIAN_POINT('',(47.9,263.535289329634,23.5537496761141)) ;
#83802 = CARTESIAN_POINT('Origin',(35.6,264.9,21.9213203435596)) ;
#83803 = CARTESIAN_POINT('',(35.6,265.,20.0213203435596)) ;
#83804 = CARTESIAN_POINT('Origin',(35.6,264.9,20.0213203435596)) ;
#83805 = CARTESIAN_POINT('',(37.5,265.,21.9213203435596)) ;
#83806 = CARTESIAN_POINT('Origin',(35.6,265.,21.9213203435596)) ;
#83807 = CARTESIAN_POINT('Origin',(37.5,264.9,21.9213203435596)) ;
#83808 = CARTESIAN_POINT('Origin',(37.5,264.9,22.4713203435596)) ;
#83809 = CARTESIAN_POINT('',(37.5,265.,25.0213203435596)) ;
#83810 = CARTESIAN_POINT('Origin',(37.5,264.9,25.0213203435596)) ;
#83811 = CARTESIAN_POINT('',(37.5,265.,22.4713203435596)) ;
#83812 = CARTESIAN_POINT('Origin',(40.2,264.9,25.0213203435596)) ;
#83813 = CARTESIAN_POINT('',(42.9,265.,25.0213203435596)) ;
#83814 = CARTESIAN_POINT('Origin',(42.9,264.9,25.0213203435596)) ;
#83815 = CARTESIAN_POINT('Origin',(40.2,265.,25.0213203435596)) ;
#83816 = CARTESIAN_POINT('Origin',(42.9,264.9,19.9213203435596)) ;
#83817 = CARTESIAN_POINT('',(42.9,265.,21.9213203435596)) ;
#83818 = CARTESIAN_POINT('Origin',(42.9,264.9,21.9213203435596)) ;
#83819 = CARTESIAN_POINT('',(42.9,265.,19.9213203435596)) ;
#83820 = CARTESIAN_POINT('Origin',(44.8,264.9,21.9213203435596)) ;
#83821 = CARTESIAN_POINT('',(44.8,265.,20.0213203435596)) ;
#83822 = CARTESIAN_POINT('Origin',(44.8,264.9,20.0213203435596)) ;
#83823 = CARTESIAN_POINT('Origin',(44.8,265.,21.9213203435596)) ;
#83824 = CARTESIAN_POINT('Origin',(79.1999999999999,265.,19.9213203435596)) ;
#83825 = CARTESIAN_POINT('',(28.2,265.,20.0213203435596)) ;
#83826 = CARTESIAN_POINT('',(66.4499999999999,265.,20.0213203435596)) ;
#83827 = CARTESIAN_POINT('',(26.3,265.,21.9213203435596)) ;
#83828 = CARTESIAN_POINT('Origin',(28.2,265.,21.9213203435596)) ;
#83829 = CARTESIAN_POINT('',(26.3,265.,30.7213203435596)) ;
#83830 = CARTESIAN_POINT('',(26.3,265.,19.9213203435596)) ;
#83831 = CARTESIAN_POINT('',(46.9,265.,30.7213203435596)) ;
#83832 = CARTESIAN_POINT('',(66.4499999999999,265.,30.7213203435596)) ;
#83833 = CARTESIAN_POINT('',(46.9,265.,22.4733813234278)) ;
#83834 = CARTESIAN_POINT('',(46.9,265.,19.9213203435596)) ;
#83835 = CARTESIAN_POINT('Ctrl Pts',(47.0453687118714,265.,22.4213203435611)) ;
#83836 = CARTESIAN_POINT('Ctrl Pts',(47.0190922729071,265.,22.4214536264379)) ;
#83837 = CARTESIAN_POINT('Ctrl Pts',(46.992447726076,265.,22.424830164787)) ;
#83838 = CARTESIAN_POINT('Ctrl Pts',(46.9546773758358,265.,22.4371420104603)) ;
#83839 = CARTESIAN_POINT('Ctrl Pts',(46.9423422478844,265.,22.4425803610722)) ;
#83840 = CARTESIAN_POINT('Ctrl Pts',(46.9197422382574,265.,22.4560226634585)) ;
#83841 = CARTESIAN_POINT('Ctrl Pts',(46.9095834753162,265.,22.4637992160125)) ;
#83842 = CARTESIAN_POINT('Ctrl Pts',(46.9003152423108,265.,22.4730640569009)) ;
#83843 = CARTESIAN_POINT('Ctrl Pts',(46.9001574429778,265.,22.4732225117743)) ;
#83844 = CARTESIAN_POINT('Ctrl Pts',(46.9,265.,22.4733813234278)) ;
#83845 = CARTESIAN_POINT('',(55.5,265.,22.4733813234278)) ;
#83846 = CARTESIAN_POINT('Ctrl Pts',(55.5,265.,22.4733813234278)) ;
#83847 = CARTESIAN_POINT('Ctrl Pts',(55.4998440576649,265.,22.4732225009103)) ;
#83848 = CARTESIAN_POINT('Ctrl Pts',(55.4996877611835,265.,22.4730640154298)) ;
#83849 = CARTESIAN_POINT('Ctrl Pts',(55.4908833110416,265.,22.464175452815)) ;
#83850 = CARTESIAN_POINT('Ctrl Pts',(55.4813394787527,265.,22.4566715159258)) ;
#83851 = CARTESIAN_POINT('Ctrl Pts',(55.4600552303074,265.,22.4435953221648)) ;
#83852 = CARTESIAN_POINT('Ctrl Pts',(55.448466273445,265.,22.4382495306549)) ;
#83853 = CARTESIAN_POINT('Ctrl Pts',(55.4106891852956,265.,22.425086339052)) ;
#83854 = CARTESIAN_POINT('Ctrl Pts',(55.3829804661023,265.,22.4213867240657)) ;
#83855 = CARTESIAN_POINT('Ctrl Pts',(55.3555997571232,265.,22.421320343561)) ;
#83856 = CARTESIAN_POINT('',(55.5,265.,30.7213203435596)) ;
#83857 = CARTESIAN_POINT('',(55.5,265.,19.9213203435596)) ;
#83858 = CARTESIAN_POINT('',(68.9,265.,30.7213203435596)) ;
#83859 = CARTESIAN_POINT('',(66.4499999999999,265.,30.7213203435596)) ;
#83860 = CARTESIAN_POINT('',(68.8999999999999,265.,22.4733813234278)) ;
#83861 = CARTESIAN_POINT('',(68.8999999999999,265.,19.9213203435596)) ;
#83862 = CARTESIAN_POINT('Ctrl Pts',(69.0453678447016,265.,22.4213203435607)) ;
#83863 = CARTESIAN_POINT('Ctrl Pts',(69.0190920820314,265.,22.4214543901977)) ;
#83864 = CARTESIAN_POINT('Ctrl Pts',(68.9924474326331,265.,22.4248305985132)) ;
#83865 = CARTESIAN_POINT('Ctrl Pts',(68.9546771660397,265.,22.4371420488168)) ;
#83866 = CARTESIAN_POINT('Ctrl Pts',(68.9423421942767,265.,22.4425803275581)) ;
#83867 = CARTESIAN_POINT('Ctrl Pts',(68.9197422336765,265.,22.4560226169246)) ;
#83868 = CARTESIAN_POINT('Ctrl Pts',(68.9095834355294,265.,22.4637992057439)) ;
#83869 = CARTESIAN_POINT('Ctrl Pts',(68.9003152401964,265.,22.4730640573226)) ;
#83870 = CARTESIAN_POINT('Ctrl Pts',(68.9001574425991,265.,22.4732225112997)) ;
#83871 = CARTESIAN_POINT('Ctrl Pts',(68.8999999999999,265.,22.4733813234278)) ;
#83872 = CARTESIAN_POINT('',(77.5,265.,22.4733813234278)) ;
#83873 = CARTESIAN_POINT('Ctrl Pts',(77.5,265.,22.4733813234278)) ;
#83874 = CARTESIAN_POINT('Ctrl Pts',(77.4998425562135,265.,22.4732225098274)) ;
#83875 = CARTESIAN_POINT('Ctrl Pts',(77.4996847618097,265.,22.4730640587698)) ;
#83876 = CARTESIAN_POINT('Ctrl Pts',(77.4908533994486,265.,22.4642358680099)) ;
#83877 = CARTESIAN_POINT('Ctrl Pts',(77.4812280995991,265.,22.4567689285165)) ;
#83878 = CARTESIAN_POINT('Ctrl Pts',(77.4599504800949,265.,22.4437921170525)) ;
#83879 = CARTESIAN_POINT('Ctrl Pts',(77.4483957267967,265.,22.438461808421)) ;
#83880 = CARTESIAN_POINT('Ctrl Pts',(77.4103406428432,265.,22.4251907142037)) ;
#83881 = CARTESIAN_POINT('Ctrl Pts',(77.3822743638663,265.,22.4214616185286)) ;
#83882 = CARTESIAN_POINT('Ctrl Pts',(77.3546324333372,265.,22.4213203435609)) ;
#83883 = CARTESIAN_POINT('',(77.5,265.,30.7213203435596)) ;
#83884 = CARTESIAN_POINT('',(77.5,265.,19.9213203435596)) ;
#83885 = CARTESIAN_POINT('',(79.0999999999999,265.,30.7213203435596)) ;
#83886 = CARTESIAN_POINT('',(66.4499999999999,265.,30.7213203435596)) ;
#83887 = CARTESIAN_POINT('',(79.0999999999999,265.,21.9213203435596)) ;
#83888 = CARTESIAN_POINT('',(79.0999999999999,265.,19.9213203435596)) ;
#83889 = CARTESIAN_POINT('',(77.1999999999999,265.,20.0213203435596)) ;
#83890 = CARTESIAN_POINT('Origin',(77.1999999999999,265.,21.9213203435596)) ;
#83891 = CARTESIAN_POINT('',(66.4499999999999,265.,20.0213203435596)) ;
#83892 = CARTESIAN_POINT('Origin',(66.4499999999999,264.9,20.0213203435596)) ;
#83893 = CARTESIAN_POINT('Origin',(28.2,264.9,20.0213203435596)) ;
#83894 = CARTESIAN_POINT('Origin',(79.1999999999999,263.8,19.9213203435596)) ;
#83895 = CARTESIAN_POINT('',(78.1993563245317,263.8,30.3213203435596)) ;
#83896 = CARTESIAN_POINT('',(66.4499999999999,263.8,30.3213203435596)) ;
#83897 = CARTESIAN_POINT('',(78.0420937034656,263.800015547414,27.0760161755151)) ;
#83898 = CARTESIAN_POINT('Origin',(76.5,263.8,30.548381323428)) ;
#83899 = CARTESIAN_POINT('Ctrl Pts',(78.0420863446217,263.8,27.0760132984819)) ;
#83900 = CARTESIAN_POINT('Ctrl Pts',(77.9385797424837,263.8,25.9938609841148)) ;
#83901 = CARTESIAN_POINT('Ctrl Pts',(77.847161300073,263.800000000028,24.8253075196437)) ;
#83902 = CARTESIAN_POINT('Ctrl Pts',(77.6881616771047,263.800000000028,23.2254574982112)) ;
#83903 = CARTESIAN_POINT('Ctrl Pts',(77.6338781282738,263.800000000004,22.806209746512)) ;
#83904 = CARTESIAN_POINT('Ctrl Pts',(77.5731133611966,263.800000000004,22.5633014256337)) ;
#83905 = CARTESIAN_POINT('Ctrl Pts',(77.5656436952132,263.8,22.5362571159244)) ;
#83906 = CARTESIAN_POINT('Ctrl Pts',(77.5525252044025,263.8,22.4970249872318)) ;
#83907 = CARTESIAN_POINT('Ctrl Pts',(77.5472664241076,263.8,22.4827534614122)) ;
#83908 = CARTESIAN_POINT('Ctrl Pts',(77.5345309823458,263.8,22.4531152552685)) ;
#83909 = CARTESIAN_POINT('Ctrl Pts',(77.5266242104818,263.8,22.4374841446812)) ;
#83910 = CARTESIAN_POINT('Ctrl Pts',(77.5042152651784,263.8,22.4030141768054)) ;
#83911 = CARTESIAN_POINT('Ctrl Pts',(77.4839496773601,263.8,22.3779632317415)) ;
#83912 = CARTESIAN_POINT('Ctrl Pts',(77.4178853473915,263.8,22.3331581295801)) ;
#83913 = CARTESIAN_POINT('Ctrl Pts',(77.3812322693006,263.8,22.3183191618849)) ;
#83914 = CARTESIAN_POINT('Ctrl Pts',(77.307381732694,263.8,22.300232389935)) ;
#83915 = CARTESIAN_POINT('Ctrl Pts',(77.2699691807084,263.8,22.2963944605413)) ;
#83916 = CARTESIAN_POINT('Ctrl Pts',(77.2327566362305,263.8,22.2963739918766)) ;
#83917 = CARTESIAN_POINT('',(68.3578850163,263.800011090529,27.0760152372235)) ;
#83918 = CARTESIAN_POINT('Ctrl Pts',(69.1668084099568,263.8,22.296373991876)) ;
#83919 = CARTESIAN_POINT('Ctrl Pts',(69.1071461813465,263.8,22.2964240616732)) ;
#83920 = CARTESIAN_POINT('Ctrl Pts',(69.0549431451098,263.8,22.3062923346873)) ;
#83921 = CARTESIAN_POINT('Ctrl Pts',(68.9802386686246,263.8,22.3351722086986)) ;
#83922 = CARTESIAN_POINT('Ctrl Pts',(68.9509341582604,263.8,22.3516916978657)) ;
#83923 = CARTESIAN_POINT('Ctrl Pts',(68.9022365717782,263.8,22.3939701968917)) ;
#83924 = CARTESIAN_POINT('Ctrl Pts',(68.8864566236587,263.8,22.4156208414979)) ;
#83925 = CARTESIAN_POINT('Ctrl Pts',(68.8666952618675,263.8,22.4504498771856)) ;
#83926 = CARTESIAN_POINT('Ctrl Pts',(68.8598414559823,263.8,22.4654710745531)) ;
#83927 = CARTESIAN_POINT('Ctrl Pts',(68.8477759615529,263.8,22.4957554711451)) ;
#83928 = CARTESIAN_POINT('Ctrl Pts',(68.8423101798017,263.8,22.511735034006)) ;
#83929 = CARTESIAN_POINT('Ctrl Pts',(68.8256553266128,263.8,22.5652106127884)) ;
#83930 = CARTESIAN_POINT('Ctrl Pts',(68.8153865038261,263.8,22.6074723643896)) ;
#83931 = CARTESIAN_POINT('Ctrl Pts',(68.7300038445153,263.8,22.9981158670073)) ;
#83932 = CARTESIAN_POINT('Ctrl Pts',(68.657295336473,263.799999999949,23.7292165741023)) ;
#83933 = CARTESIAN_POINT('Ctrl Pts',(68.5036810339554,263.799999999949,25.4440967856073)) ;
#83934 = CARTESIAN_POINT('Ctrl Pts',(68.4331437753965,263.8,26.2891604408503)) ;
#83935 = CARTESIAN_POINT('Ctrl Pts',(68.3578902629937,263.8,27.0760131853556)) ;
#83936 = CARTESIAN_POINT('',(68.2,263.8,30.5483813234279)) ;
#83937 = CARTESIAN_POINT('Origin',(69.9,263.8,30.5483813234279)) ;
#83938 = CARTESIAN_POINT('',(68.2,263.8,19.9213203435596)) ;
#83939 = CARTESIAN_POINT('',(56.2,263.8,30.548381323428)) ;
#83940 = CARTESIAN_POINT('',(56.2,263.8,19.9213203435596)) ;
#83941 = CARTESIAN_POINT('',(56.0420937198539,263.800015543961,27.0760161747882)) ;
#83942 = CARTESIAN_POINT('Origin',(54.5,263.8,30.548381323428)) ;
#83943 = CARTESIAN_POINT('Ctrl Pts',(56.0420863626506,263.8,27.0760132983946)) ;
#83944 = CARTESIAN_POINT('Ctrl Pts',(55.9385805509996,263.8,25.9938693510034)) ;
#83945 = CARTESIAN_POINT('Ctrl Pts',(55.8471616308305,263.800000000026,24.825314711562)) ;
#83946 = CARTESIAN_POINT('Ctrl Pts',(55.6881591543513,263.800000000026,23.2254385528796)) ;
#83947 = CARTESIAN_POINT('Ctrl Pts',(55.6338760138876,263.800000000004,22.8061998855569)) ;
#83948 = CARTESIAN_POINT('Ctrl Pts',(55.5731125109262,263.800000000004,22.5632984759483)) ;
#83949 = CARTESIAN_POINT('Ctrl Pts',(55.5656430417995,263.8,22.536255083441)) ;
#83950 = CARTESIAN_POINT('Ctrl Pts',(55.5525248140369,263.8,22.4970239295753)) ;
#83951 = CARTESIAN_POINT('Ctrl Pts',(55.5472660822281,263.8,22.4827526087893)) ;
#83952 = CARTESIAN_POINT('Ctrl Pts',(55.534530691983,263.8,22.4531146554099)) ;
#83953 = CARTESIAN_POINT('Ctrl Pts',(55.5266239224689,263.8,22.4374836332353)) ;
#83954 = CARTESIAN_POINT('Ctrl Pts',(55.5042149314907,263.8,22.4030137503595)) ;
#83955 = CARTESIAN_POINT('Ctrl Pts',(55.4839492743427,263.8,22.3779628455479)) ;
#83956 = CARTESIAN_POINT('Ctrl Pts',(55.4178847304879,263.8,22.3331578097732)) ;
#83957 = CARTESIAN_POINT('Ctrl Pts',(55.3812314093916,263.8,22.3183188321358)) ;
#83958 = CARTESIAN_POINT('Ctrl Pts',(55.3073810167929,263.8,22.3002321949928)) ;
#83959 = CARTESIAN_POINT('Ctrl Pts',(55.2699686939412,263.8,22.2963942886275)) ;
#83960 = CARTESIAN_POINT('Ctrl Pts',(55.2327563431054,263.8,22.2963739918746)) ;
#83961 = CARTESIAN_POINT('',(46.3578850044002,263.800011088028,27.0760152366969)) ;
#83962 = CARTESIAN_POINT('Ctrl Pts',(47.166808626144,263.8,22.2963739918735)) ;
#83963 = CARTESIAN_POINT('Ctrl Pts',(47.1071458919983,263.8,22.296423758252)) ;
#83964 = CARTESIAN_POINT('Ctrl Pts',(47.0549411454493,263.8,22.3062924794497)) ;
#83965 = CARTESIAN_POINT('Ctrl Pts',(46.9802357268767,263.8,22.3351737363304)) ;
#83966 = CARTESIAN_POINT('Ctrl Pts',(46.9509317672401,263.8,22.3516933245359)) ;
#83967 = CARTESIAN_POINT('Ctrl Pts',(46.902235607331,263.8,22.3939714478775)) ;
#83968 = CARTESIAN_POINT('Ctrl Pts',(46.8864560566414,263.8,22.4156216929879)) ;
#83969 = CARTESIAN_POINT('Ctrl Pts',(46.8666949613237,263.8,22.450450502502)) ;
#83970 = CARTESIAN_POINT('Ctrl Pts',(46.8598412387473,263.8,22.4654715721611)) ;
#83971 = CARTESIAN_POINT('Ctrl Pts',(46.8477758406621,263.8,22.4957558005747)) ;
#83972 = CARTESIAN_POINT('Ctrl Pts',(46.8423100875593,263.8,22.5117353108167)) ;
#83973 = CARTESIAN_POINT('Ctrl Pts',(46.8256552051007,263.8,22.5652110982458)) ;
#83974 = CARTESIAN_POINT('Ctrl Pts',(46.8153863576338,263.8,22.6074731645702)) ;
#83975 = CARTESIAN_POINT('Ctrl Pts',(46.7300045475566,263.8,22.9981150219511)) ;
#83976 = CARTESIAN_POINT('Ctrl Pts',(46.6572960858892,263.799999999947,23.7292172541206)) ;
#83977 = CARTESIAN_POINT('Ctrl Pts',(46.5036802672985,263.799999999947,25.4441081278137)) ;
#83978 = CARTESIAN_POINT('Ctrl Pts',(46.4331431886047,263.8,26.2891665072701)) ;
#83979 = CARTESIAN_POINT('Ctrl Pts',(46.3578902499069,263.8,27.0760131852921)) ;
#83980 = CARTESIAN_POINT('',(46.2006436754682,263.8,30.3213203435596)) ;
#83981 = CARTESIAN_POINT('Origin',(47.9,263.8,30.5483813234279)) ;
#83982 = CARTESIAN_POINT('',(32.5414213562372,263.8,30.3213203435596)) ;
#83983 = CARTESIAN_POINT('',(66.4499999999999,263.8,30.3213203435596)) ;
#83984 = CARTESIAN_POINT('',(32.4585786437627,263.8,30.3247636574754)) ;
#83985 = CARTESIAN_POINT('Origin',(32.5414213562372,263.8,30.8213203435596)) ;
#83986 = CARTESIAN_POINT('',(32.3585786437627,263.8,30.331422395003)) ;
#83987 = CARTESIAN_POINT('Ctrl Pts',(32.3585786437627,263.8,30.331422395003)) ;
#83988 = CARTESIAN_POINT('Ctrl Pts',(32.3919863317222,263.8,30.331422395003)) ;
#83989 = CARTESIAN_POINT('Ctrl Pts',(32.4252483895324,263.8,30.3275439731426)) ;
#83990 = CARTESIAN_POINT('Ctrl Pts',(32.4585786437628,263.8,30.3247636574754)) ;
#83991 = CARTESIAN_POINT('',(28.3,263.8,30.331422395003)) ;
#83992 = CARTESIAN_POINT('',(43.45,263.8,30.331422395003)) ;
#83993 = CARTESIAN_POINT('',(28.1267949192431,263.8,30.3213203435596)) ;
#83994 = CARTESIAN_POINT('Ctrl Pts',(28.1267949192431,263.8,30.3213203435596)) ;
#83995 = CARTESIAN_POINT('Ctrl Pts',(28.1557233556092,263.8,30.3213203435596)) ;
#83996 = CARTESIAN_POINT('Ctrl Pts',(28.2134628330395,263.8,30.3254695601432)) ;
#83997 = CARTESIAN_POINT('Ctrl Pts',(28.2710715636338,263.8,30.331422395003)) ;
#83998 = CARTESIAN_POINT('Ctrl Pts',(28.2999999999999,263.8,30.331422395003)) ;
#83999 = CARTESIAN_POINT('',(66.4499999999999,263.8,30.3213203435596)) ;
#84000 = CARTESIAN_POINT('Origin',(66.4499999999999,264.9,20.0213203435596)) ;
#84001 = CARTESIAN_POINT('Origin',(77.1999999999999,264.9,20.0213203435596)) ;
#84002 = CARTESIAN_POINT('Origin',(66.4499999999999,263.4,30.3213203435596)) ;
#84003 = CARTESIAN_POINT('Ctrl Pts',(46.2376487793589,263.4,30.7213203435596)) ;
#84004 = CARTESIAN_POINT('Ctrl Pts',(46.2326137620506,263.424040519058,30.7213203435596)) ;
#84005 = CARTESIAN_POINT('Ctrl Pts',(46.2281249082703,263.448476883063,30.71912697103)) ;
#84006 = CARTESIAN_POINT('Ctrl Pts',(46.2158136627296,263.525131463702,30.7049856843152)) ;
#84007 = CARTESIAN_POINT('Ctrl Pts',(46.2103971054,263.576067017857,30.6840778621322)) ;
#84008 = CARTESIAN_POINT('Ctrl Pts',(46.2038518923002,263.660659692702,30.6288392064935)) ;
#84009 = CARTESIAN_POINT('Ctrl Pts',(46.2022098218577,263.700010832306,30.591200326939)) ;
#84010 = CARTESIAN_POINT('Ctrl Pts',(46.2005618251513,263.760218076329,30.5032121921945)) ;
#84011 = CARTESIAN_POINT('Ctrl Pts',(46.2004291717567,263.781074440706,30.4528655341031)) ;
#84012 = CARTESIAN_POINT('Ctrl Pts',(46.2004291717567,263.791419913995,30.4037245359795)) ;
#84013 = CARTESIAN_POINT('Ctrl Pts',(46.2004291717567,263.796960438797,30.3774070431671)) ;
#84014 = CARTESIAN_POINT('Ctrl Pts',(46.2004835410982,263.8,30.3495592495545)) ;
#84015 = CARTESIAN_POINT('Ctrl Pts',(46.2006436754682,263.8,30.3213203435596)) ;
#84016 = CARTESIAN_POINT('Origin',(32.5414213562372,263.4,30.3213203435596)) ;
#84017 = CARTESIAN_POINT('Ctrl Pts',(32.5414213562372,263.8,30.3213203435596)) ;
#84018 = CARTESIAN_POINT('Ctrl Pts',(32.5137435539536,263.8,30.3213203435596)) ;
#84019 = CARTESIAN_POINT('Ctrl Pts',(32.4860658393229,263.8,30.3224707532589)) ;
#84020 = CARTESIAN_POINT('Ctrl Pts',(32.4585786437627,263.8,30.3247636574754)) ;
#84021 = CARTESIAN_POINT('Ctrl Pts',(32.5414213562372,263.8,30.4260400986793)) ;
#84022 = CARTESIAN_POINT('Ctrl Pts',(32.516647311045,263.799939841784,30.4241767924342)) ;
#84023 = CARTESIAN_POINT('Ctrl Pts',(32.4917066372636,263.800050776884,30.4233947555209)) ;
#84024 = CARTESIAN_POINT('Ctrl Pts',(32.4668242027051,263.8,30.4236109139464)) ;
#84025 = CARTESIAN_POINT('Ctrl Pts',(32.5414213562372,263.713177767049,30.6344981106088)) ;
#84026 = CARTESIAN_POINT('Ctrl Pts',(32.5224039013355,263.716415820393,30.6290758165712)) ;
#84027 = CARTESIAN_POINT('Ctrl Pts',(32.5029543565148,263.719507392095,30.6243705183387)) ;
#84028 = CARTESIAN_POINT('Ctrl Pts',(32.4832538801415,263.722531687981,30.6205688825484)) ;
#84029 = CARTESIAN_POINT('Ctrl Pts',(32.5414213562372,263.50471975512,30.7213203435597)) ;
#84030 = CARTESIAN_POINT('Ctrl Pts',(32.5248379622831,263.513950857204,30.7183564282524)) ;
#84031 = CARTESIAN_POINT('Ctrl Pts',(32.5079533734914,263.523051108391,30.7159641292369)) ;
#84032 = CARTESIAN_POINT('Ctrl Pts',(32.4910326442839,263.531986701662,30.7138202314961)) ;
#84033 = CARTESIAN_POINT('Ctrl Pts',(32.5414213562372,263.4,30.7213203435596)) ;
#84034 = CARTESIAN_POINT('Ctrl Pts',(32.524814674867,263.411071120913,30.7213203435596)) ;
#84035 = CARTESIAN_POINT('Ctrl Pts',(32.5082080460886,263.422142206766,30.7215504254995)) ;
#84036 = CARTESIAN_POINT('Ctrl Pts',(32.4917157287525,263.43313708499,30.7220090063428)) ;
#84037 = CARTESIAN_POINT('',(32.4917157287525,263.43313708499,30.7220090063428)) ;
#84038 = CARTESIAN_POINT('Origin',(32.4585786437627,263.4,30.3247636574754)) ;
#84039 = CARTESIAN_POINT('Origin',(32.5414213562372,263.4,30.8213203435596)) ;
#84040 = CARTESIAN_POINT('Ctrl Pts',(32.4661974061031,263.8,30.3241495482157)) ;
#84041 = CARTESIAN_POINT('Ctrl Pts',(32.427775427709,263.8,30.3271273965861)) ;
#84042 = CARTESIAN_POINT('Ctrl Pts',(32.3894656419897,263.8,30.3320669171698)) ;
#84043 = CARTESIAN_POINT('Ctrl Pts',(32.35094083609,263.8,30.331352667432)) ;
#84044 = CARTESIAN_POINT('Ctrl Pts',(32.4739550747079,263.800023048002,30.4237405302309)) ;
#84045 = CARTESIAN_POINT('Ctrl Pts',(32.4384840003436,263.799890383199,30.4230691207513)) ;
#84046 = CARTESIAN_POINT('Ctrl Pts',(32.3956007239745,263.800015403833,30.4226634961011)) ;
#84047 = CARTESIAN_POINT('Ctrl Pts',(32.3494742105276,263.799998368455,30.4227242881205)) ;
#84048 = CARTESIAN_POINT('Ctrl Pts',(32.489423057882,263.721324324522,30.6222814519142)) ;
#84049 = CARTESIAN_POINT('Ctrl Pts',(32.4598454616252,263.726901760206,30.614607325942)) ;
#84050 = CARTESIAN_POINT('Ctrl Pts',(32.4078143613243,263.735991513718,30.6035180183888)) ;
#84051 = CARTESIAN_POINT('Ctrl Pts',(32.3465538177013,263.734676655515,30.605126476162)) ;
#84052 = CARTESIAN_POINT('Ctrl Pts',(32.4966185134649,263.528321623589,30.7148404386893)) ;
#84053 = CARTESIAN_POINT('Ctrl Pts',(32.4704413404425,263.544604892099,30.7105178580992)) ;
#84054 = CARTESIAN_POINT('Ctrl Pts',(32.4147657809408,263.57288534838,30.7044385729834)) ;
#84055 = CARTESIAN_POINT('Ctrl Pts',(32.3449157225414,263.56879986086,30.7053209268799)) ;
#84056 = CARTESIAN_POINT('Ctrl Pts',(32.4971643394536,263.428547221079,30.7219188515075)) ;
#84057 = CARTESIAN_POINT('Ctrl Pts',(32.4716769894707,263.448435108365,30.722537008849)) ;
#84058 = CARTESIAN_POINT('Ctrl Pts',(32.4160802382908,263.484256591046,30.7235573712385)) ;
#84059 = CARTESIAN_POINT('Ctrl Pts',(32.3446178057178,263.479085396975,30.7234098127246)) ;
#84060 = CARTESIAN_POINT('',(32.3585786437627,263.48,30.7233407538483)) ;
#84061 = CARTESIAN_POINT('Origin',(32.3585786437627,263.4,30.331422395003)) ;
#84062 = CARTESIAN_POINT('Ctrl Pts',(32.4917157287525,263.43313708499,30.7220090063427)) ;
#84063 = CARTESIAN_POINT('Ctrl Pts',(32.4862531044155,263.437172850683,30.7221280308607)) ;
#84064 = CARTESIAN_POINT('Ctrl Pts',(32.4799268910377,263.441637838602,30.7222567124468)) ;
#84065 = CARTESIAN_POINT('Ctrl Pts',(32.4726883818981,263.446171330639,30.7223863480612)) ;
#84066 = CARTESIAN_POINT('Ctrl Pts',(32.4660437256829,263.450332891461,30.7225053482689)) ;
#84067 = CARTESIAN_POINT('Ctrl Pts',(32.4586288871471,263.454550717319,30.7226250788745)) ;
#84068 = CARTESIAN_POINT('Ctrl Pts',(32.4504481493401,263.458527237894,30.7227376232999)) ;
#84069 = CARTESIAN_POINT('Ctrl Pts',(32.4429648306756,263.462164754625,30.7228405731583)) ;
#84070 = CARTESIAN_POINT('Ctrl Pts',(32.4348405192778,263.46559929887,30.7229374604874)) ;
#84071 = CARTESIAN_POINT('Ctrl Pts',(32.4261242620743,263.468603798031,30.7230220080826)) ;
#84072 = CARTESIAN_POINT('Ctrl Pts',(32.4176398736902,263.471528371869,30.7231043065529)) ;
#84073 = CARTESIAN_POINT('Ctrl Pts',(32.4085946242033,263.474044542166,30.7231748710841)) ;
#84074 = CARTESIAN_POINT('Ctrl Pts',(32.3990802048924,263.475957726272,30.7232283375603)) ;
#84075 = CARTESIAN_POINT('Ctrl Pts',(32.3897735748965,263.477829127564,30.7232806363602)) ;
#84076 = CARTESIAN_POINT('Ctrl Pts',(32.3800184348618,263.479122788557,30.7233165339942)) ;
#84077 = CARTESIAN_POINT('Ctrl Pts',(32.3699426275149,263.479683772191,30.7233320336986)) ;
#84078 = CARTESIAN_POINT('Ctrl Pts',(32.3661959536449,263.479892373115,30.7233377972404)) ;
#84079 = CARTESIAN_POINT('Ctrl Pts',(32.3624053322483,263.48,30.7233407538483)) ;
#84080 = CARTESIAN_POINT('Ctrl Pts',(32.3585786437627,263.48,30.7233407538483)) ;
#84081 = CARTESIAN_POINT('Origin',(43.45,263.4,30.331422395003)) ;
#84082 = CARTESIAN_POINT('',(28.3,263.48,30.7233407538483)) ;
#84083 = CARTESIAN_POINT('Origin',(28.3,263.4,30.331422395003)) ;
#84084 = CARTESIAN_POINT('',(43.45,263.48,30.7233407538483)) ;
#84085 = CARTESIAN_POINT('Ctrl Pts',(28.2999999999999,263.8,30.331422395003)) ;
#84086 = CARTESIAN_POINT('Ctrl Pts',(28.2710715636338,263.8,30.331422395003)) ;
#84087 = CARTESIAN_POINT('Ctrl Pts',(28.2134628330395,263.8,30.3254695601432)) ;
#84088 = CARTESIAN_POINT('Ctrl Pts',(28.1557233556092,263.8,30.3213203435596)) ;
#84089 = CARTESIAN_POINT('Ctrl Pts',(28.1267949192431,263.8,30.3213203435596)) ;
#84090 = CARTESIAN_POINT('Ctrl Pts',(28.2999999999999,263.8,30.4227182887366)) ;
#84091 = CARTESIAN_POINT('Ctrl Pts',(28.2656750347894,263.8,30.4227182887366)) ;
#84092 = CARTESIAN_POINT('Ctrl Pts',(28.201063490636,263.79998336013,30.4232854950333)) ;
#84093 = CARTESIAN_POINT('Ctrl Pts',(28.1511709085951,263.799945547361,30.4243535136987)) ;
#84094 = CARTESIAN_POINT('Ctrl Pts',(28.1267949192431,263.8,30.4260400986793)) ;
#84095 = CARTESIAN_POINT('Ctrl Pts',(28.2999999999999,263.734854968624,30.6048303319916)) ;
#84096 = CARTESIAN_POINT('Ctrl Pts',(28.2549355475455,263.734854968624,30.6048303319916)) ;
#84097 = CARTESIAN_POINT('Ctrl Pts',(28.1764296104343,263.723817492061,30.6182710292689)) ;
#84098 = CARTESIAN_POINT('Ctrl Pts',(28.1421458519343,263.716108985329,30.6295903534867)) ;
#84099 = CARTESIAN_POINT('Ctrl Pts',(28.1267949192431,263.713178038174,30.634498381734)) ;
#84100 = CARTESIAN_POINT('Ctrl Pts',(28.3,263.569451342103,30.7050815751016)) ;
#84101 = CARTESIAN_POINT('Ctrl Pts',(28.2489802156405,263.569451342103,30.7050815751016)) ;
#84102 = CARTESIAN_POINT('Ctrl Pts',(28.1644027263672,263.535328707411,30.7126199315049)) ;
#84103 = CARTESIAN_POINT('Ctrl Pts',(28.1383297842868,263.513075353224,30.7186375344111)) ;
#84104 = CARTESIAN_POINT('Ctrl Pts',(28.1267949192431,263.50471975512,30.7213203435596)) ;
#84105 = CARTESIAN_POINT('Ctrl Pts',(28.3,263.48,30.7233407538483)) ;
#84106 = CARTESIAN_POINT('Ctrl Pts',(28.2479288145409,263.48,30.7233407538483)) ;
#84107 = CARTESIAN_POINT('Ctrl Pts',(28.1632911232526,263.436809028867,30.7221501868763)) ;
#84108 = CARTESIAN_POINT('Ctrl Pts',(28.1383662937896,263.410021104314,30.7213203435596)) ;
#84109 = CARTESIAN_POINT('Ctrl Pts',(28.1267949192431,263.4,30.7213203435596)) ;
#84110 = CARTESIAN_POINT('Origin',(28.1267949192431,263.4,30.3213203435596)) ;
#84111 = CARTESIAN_POINT('Ctrl Pts',(28.3,263.48,30.7233407538483)) ;
#84112 = CARTESIAN_POINT('Ctrl Pts',(28.2479288145409,263.48,30.7233407538483)) ;
#84113 = CARTESIAN_POINT('Ctrl Pts',(28.1632911232526,263.436809028867,30.7221501868763)) ;
#84114 = CARTESIAN_POINT('Ctrl Pts',(28.1383662937896,263.410021104314,30.7213203435596)) ;
#84115 = CARTESIAN_POINT('Ctrl Pts',(28.1267949192431,263.4,30.7213203435596)) ;
#84116 = CARTESIAN_POINT('Origin',(66.4499999999999,263.4,30.3213203435596)) ;
#84117 = CARTESIAN_POINT('Origin',(26.3,252.191753592594,30.8213203435596)) ;
#84118 = CARTESIAN_POINT('Origin',(26.3,245.6,30.8213203435596)) ;
#84119 = CARTESIAN_POINT('Origin',(28.3,263.3,30.8213203435596)) ;
#84120 = CARTESIAN_POINT('',(28.3,263.4,30.8213203435596)) ;
#84121 = CARTESIAN_POINT('Origin',(28.3,263.5,30.8213203435596)) ;
#84122 = CARTESIAN_POINT('',(28.2,263.3,30.8213203435596)) ;
#84123 = CARTESIAN_POINT('Origin',(28.3,263.3,30.8213203435596)) ;
#84124 = CARTESIAN_POINT('Origin',(28.1,263.3,30.8213203435596)) ;
#84125 = CARTESIAN_POINT('Origin',(43.45,263.5,30.8213203435596)) ;
#84126 = CARTESIAN_POINT('',(32.3585786437627,263.4,30.8213203435596)) ;
#84127 = CARTESIAN_POINT('Origin',(32.3585786437627,263.5,30.8213203435596)) ;
#84128 = CARTESIAN_POINT('',(43.45,263.4,30.8213203435596)) ;
#84129 = CARTESIAN_POINT('Origin',(32.3585786437627,263.3,30.8213203435596)) ;
#84130 = CARTESIAN_POINT('',(32.4292893218813,263.370710678119,30.8213203435596)) ;
#84131 = CARTESIAN_POINT('Origin',(32.5,263.441421356237,30.8213203435596)) ;
#84132 = CARTESIAN_POINT('Origin',(32.3585786437627,263.3,30.8213203435596)) ;
#84133 = CARTESIAN_POINT('Origin',(43.9998338818216,251.941587474416,30.8213203435596)) ;
#84134 = CARTESIAN_POINT('',(33.1707106781186,262.629289321881,30.8213203435596)) ;
#84135 = CARTESIAN_POINT('Origin',(33.2414213562373,262.7,30.8213203435596)) ;
#84136 = CARTESIAN_POINT('',(43.929123203703,251.870876796297,30.8213203435596)) ;
#84137 = CARTESIAN_POINT('Origin',(66.4499999999999,263.4,30.3213203435596)) ;
#84138 = CARTESIAN_POINT('Ctrl Pts',(78.1993563245318,263.8,30.3213203435596)) ;
#84139 = CARTESIAN_POINT('Ctrl Pts',(78.1995164589018,263.8,30.3495592495545)) ;
#84140 = CARTESIAN_POINT('Ctrl Pts',(78.1995708282433,263.796960438797,30.3774070431671)) ;
#84141 = CARTESIAN_POINT('Ctrl Pts',(78.1995708282433,263.781074440706,30.4528655341031)) ;
#84142 = CARTESIAN_POINT('Ctrl Pts',(78.1994381748487,263.760218076329,30.5032121921945)) ;
#84143 = CARTESIAN_POINT('Ctrl Pts',(78.1977901781423,263.700010832306,30.591200326939)) ;
#84144 = CARTESIAN_POINT('Ctrl Pts',(78.1961481076998,263.660659692702,30.6288392064935)) ;
#84145 = CARTESIAN_POINT('Ctrl Pts',(78.1896028945999,263.576067017857,30.6840778621322)) ;
#84146 = CARTESIAN_POINT('Ctrl Pts',(78.1841863372704,263.525131463702,30.7049856843151)) ;
#84147 = CARTESIAN_POINT('Ctrl Pts',(78.1718750917296,263.448476883063,30.71912697103)) ;
#84148 = CARTESIAN_POINT('Ctrl Pts',(78.1673862379493,263.424040519058,30.7213203435596)) ;
#84149 = CARTESIAN_POINT('Ctrl Pts',(78.162351220641,263.4,30.7213203435596)) ;
#84150 = CARTESIAN_POINT('Origin',(76.5,265.241264282414,23.7023759819625)) ;
#84151 = CARTESIAN_POINT('Ctrl Pts',(78.0420937034656,263.800015547414,27.0760161755151)) ;
#84152 = CARTESIAN_POINT('Ctrl Pts',(77.9130621118948,263.528796412695,27.018917410311)) ;
#84153 = CARTESIAN_POINT('Ctrl Pts',(77.4812575809273,263.030548349122,26.9140230811377)) ;
#84154 = CARTESIAN_POINT('Ctrl Pts',(76.8382263221145,262.836465365523,26.8731635056432)) ;
#84155 = CARTESIAN_POINT('Ctrl Pts',(76.5,262.836465365523,26.8731635056432)) ;
#84156 = CARTESIAN_POINT('Origin',(59.8573593128808,230.1,31.8213203435596)) ;
#84157 = CARTESIAN_POINT('',(59.9573593128808,230.1,31.8213203435596)) ;
#84158 = CARTESIAN_POINT('Origin',(59.8573593128808,230.1,31.8213203435596)) ;
#84159 = CARTESIAN_POINT('',(59.8573593128808,230.,31.8213203435596)) ;
#84160 = CARTESIAN_POINT('Origin',(59.8573593128808,230.1,31.8213203435596)) ;
#84161 = CARTESIAN_POINT('Origin',(59.8573593128808,230.1,31.8213203435596)) ;
#84162 = CARTESIAN_POINT('Origin',(56.8286796564404,230.1,31.8213203435596)) ;
#84163 = CARTESIAN_POINT('',(59.7573593128808,230.,31.8213203435596)) ;
#84164 = CARTESIAN_POINT('Origin',(59.7573593128808,230.1,31.8213203435596)) ;
#84165 = CARTESIAN_POINT('',(56.8286796564404,230.,31.8213203435596)) ;
#84166 = CARTESIAN_POINT('Origin',(59.7573593128808,229.9,31.8213203435596)) ;
#84167 = CARTESIAN_POINT('',(59.6573593128808,229.9,31.8213203435596)) ;
#84168 = CARTESIAN_POINT('Origin',(59.5573593128808,229.9,31.8213203435596)) ;
#84169 = CARTESIAN_POINT('Origin',(59.7573593128808,229.9,31.8213203435596)) ;
#84170 = CARTESIAN_POINT('Origin',(59.8573593128808,230.1,30.8213203435596)) ;
#84171 = CARTESIAN_POINT('',(59.9573593128808,230.1,30.8213203435596)) ;
#84172 = CARTESIAN_POINT('',(59.8573593128808,230.,30.8213203435596)) ;
#84173 = CARTESIAN_POINT('Origin',(59.8573593128808,230.1,30.8213203435596)) ;
#84174 = CARTESIAN_POINT('Origin',(59.8573593128808,230.1,30.8213203435596)) ;
#84175 = CARTESIAN_POINT('Origin',(59.8573593128808,230.1,30.8213203435596)) ;
#84176 = CARTESIAN_POINT('Origin',(59.8573593128808,230.1,19.9213203435596)) ;
#84177 = CARTESIAN_POINT('',(59.9573593128808,230.1,19.9213203435596)) ;
#84178 = CARTESIAN_POINT('',(59.8573593128808,230.,19.9213203435596)) ;
#84179 = CARTESIAN_POINT('Origin',(62.2573593128808,235.9,31.8213203435596)) ;
#84180 = CARTESIAN_POINT('',(62.2573593128808,236.,31.8213203435596)) ;
#84181 = CARTESIAN_POINT('Origin',(62.2573593128808,236.1,31.8213203435596)) ;
#84182 = CARTESIAN_POINT('',(62.3573593128808,235.9,31.8213203435596)) ;
#84183 = CARTESIAN_POINT('Origin',(62.2573593128808,235.9,31.8213203435596)) ;
#84184 = CARTESIAN_POINT('Origin',(62.4573593128808,235.9,31.8213203435596)) ;
#84185 = CARTESIAN_POINT('Origin',(60.0573593128808,235.9,31.8213203435596)) ;
#84186 = CARTESIAN_POINT('',(60.0573593128808,236.,31.8213203435596)) ;
#84187 = CARTESIAN_POINT('',(59.9573593128808,235.9,31.8213203435596)) ;
#84188 = CARTESIAN_POINT('Origin',(60.0573593128808,235.9,31.8213203435596)) ;
#84189 = CARTESIAN_POINT('Origin',(60.0573593128808,236.1,31.8213203435596)) ;
#84190 = CARTESIAN_POINT('Origin',(59.8573593128808,235.9,31.8213203435596)) ;
#84191 = CARTESIAN_POINT('Origin',(58.0286796564404,236.1,31.8213203435596)) ;
#84192 = CARTESIAN_POINT('',(58.0286796564404,236.,31.8213203435596)) ;
#84193 = CARTESIAN_POINT('Origin',(59.8573593128808,237.691753592594,31.8213203435596)) ;
#84194 = CARTESIAN_POINT('',(59.9573593128808,237.691753592594,31.8213203435596)) ;
#84195 = CARTESIAN_POINT('Origin',(59.8573593128808,235.9,30.8213203435596)) ;
#84196 = CARTESIAN_POINT('',(60.0573593128808,236.,30.8213203435596)) ;
#84197 = CARTESIAN_POINT('',(59.9573593128808,235.9,30.8213203435596)) ;
#84198 = CARTESIAN_POINT('Origin',(60.0573593128808,235.9,30.8213203435596)) ;
#84199 = CARTESIAN_POINT('Origin',(59.8573593128808,235.9,30.8213203435596)) ;
#84200 = CARTESIAN_POINT('Origin',(59.8573593128808,236.,30.8213203435596)) ;
#84201 = CARTESIAN_POINT('Origin',(60.0573593128808,235.9,19.9213203435596)) ;
#84202 = CARTESIAN_POINT('',(59.9573593128808,235.9,19.9213203435596)) ;
#84203 = CARTESIAN_POINT('',(60.0573593128808,236.,19.9213203435596)) ;
#84204 = CARTESIAN_POINT('Origin',(62.2573593128808,235.9,19.9213203435596)) ;
#84205 = CARTESIAN_POINT('',(62.2573593128808,236.,30.8213203435596)) ;
#84206 = CARTESIAN_POINT('',(62.3573593128808,235.9,30.8213203435596)) ;
#84207 = CARTESIAN_POINT('Origin',(62.2573593128808,235.9,30.8213203435596)) ;
#84208 = CARTESIAN_POINT('',(62.3573593128808,235.9,19.9213203435596)) ;
#84209 = CARTESIAN_POINT('',(62.2573593128808,236.,19.9213203435596)) ;
#84210 = CARTESIAN_POINT('Origin',(62.4573593128808,235.9,30.8213203435596)) ;
#84211 = CARTESIAN_POINT('Origin',(62.4573593128808,235.9,30.8213203435596)) ;
#84212 = CARTESIAN_POINT('Origin',(62.4573593128808,236.,30.8213203435596)) ;
#84213 = CARTESIAN_POINT('Origin',(62.4573593128808,234.691753592594,31.8213203435596)) ;
#84214 = CARTESIAN_POINT('',(62.3573593128808,230.1,31.8213203435596)) ;
#84215 = CARTESIAN_POINT('Origin',(62.4573593128808,230.1,31.8213203435596)) ;
#84216 = CARTESIAN_POINT('',(62.3573593128808,234.691753592594,31.8213203435596)) ;
#84217 = CARTESIAN_POINT('Origin',(62.4573593128808,230.1,31.8213203435596)) ;
#84218 = CARTESIAN_POINT('',(62.4573593128808,230.,31.8213203435596)) ;
#84219 = CARTESIAN_POINT('Origin',(62.4573593128808,230.1,31.8213203435596)) ;
#84220 = CARTESIAN_POINT('Origin',(62.4573593128808,230.1,31.8213203435596)) ;
#84221 = CARTESIAN_POINT('Origin',(56.8286796564404,230.1,30.8213203435596)) ;
#84222 = CARTESIAN_POINT('',(59.7573593128808,230.,30.8213203435596)) ;
#84223 = CARTESIAN_POINT('',(56.8286796564404,230.,30.8213203435596)) ;
#84224 = CARTESIAN_POINT('Origin',(59.7573593128808,230.1,30.8213203435596)) ;
#84225 = CARTESIAN_POINT('Origin',(59.9573593128808,230.,19.9213203435596)) ;
#84226 = CARTESIAN_POINT('',(59.7573593128808,230.,19.9213203435596)) ;
#84227 = CARTESIAN_POINT('Origin',(58.1786796564404,230.1,31.8213203435596)) ;
#84228 = CARTESIAN_POINT('',(62.5573593128808,230.,31.8213203435596)) ;
#84229 = CARTESIAN_POINT('',(58.1786796564404,230.,31.8213203435596)) ;
#84230 = CARTESIAN_POINT('Origin',(62.5573593128808,230.1,31.8213203435596)) ;
#84231 = CARTESIAN_POINT('Origin',(62.4573593128808,230.1,19.9213203435596)) ;
#84232 = CARTESIAN_POINT('',(62.3573593128808,230.1,30.8213203435596)) ;
#84233 = CARTESIAN_POINT('',(62.3573593128808,230.1,19.9213203435596)) ;
#84234 = CARTESIAN_POINT('',(62.4573593128808,230.,30.8213203435596)) ;
#84235 = CARTESIAN_POINT('Origin',(62.4573593128808,230.1,30.8213203435596)) ;
#84236 = CARTESIAN_POINT('',(62.4573593128808,230.,19.9213203435596)) ;
#84237 = CARTESIAN_POINT('Origin',(62.3573593128808,230.,19.9213203435596)) ;
#84238 = CARTESIAN_POINT('',(62.3573593128808,234.691753592594,30.8213203435596)) ;
#84239 = CARTESIAN_POINT('Origin',(58.0573593128808,237.9,30.8213203435596)) ;
#84240 = CARTESIAN_POINT('',(57.9573593128808,238.1,30.8213203435596)) ;
#84241 = CARTESIAN_POINT('',(58.0573593128808,238.,30.8213203435596)) ;
#84242 = CARTESIAN_POINT('Origin',(58.0573593128808,238.1,30.8213203435596)) ;
#84243 = CARTESIAN_POINT('Origin',(58.0573593128808,237.9,30.8213203435596)) ;
#84244 = CARTESIAN_POINT('Origin',(57.9573593128808,237.9,30.8213203435596)) ;
#84245 = CARTESIAN_POINT('Origin',(58.0573593128808,238.1,19.9213203435596)) ;
#84246 = CARTESIAN_POINT('',(57.9573593128808,238.1,31.8213203435596)) ;
#84247 = CARTESIAN_POINT('',(58.0573593128808,238.,31.8213203435596)) ;
#84248 = CARTESIAN_POINT('Origin',(58.0573593128808,238.1,31.8213203435596)) ;
#84249 = CARTESIAN_POINT('',(58.0573593128808,238.,19.9213203435596)) ;
#84250 = CARTESIAN_POINT('',(57.9573593128808,238.1,19.9213203435596)) ;
#84251 = CARTESIAN_POINT('Ctrl Pts',(58.0573593128808,238.,31.8213203435596)) ;
#84252 = CARTESIAN_POINT('Ctrl Pts',(58.0573593128808,238.,31.8736802211195)) ;
#84253 = CARTESIAN_POINT('Ctrl Pts',(57.9620790680004,237.95235987756,31.9213203435596)) ;
#84254 = CARTESIAN_POINT('Ctrl Pts',(57.8573593128808,237.9,31.9213203435596)) ;
#84255 = CARTESIAN_POINT('Ctrl Pts',(58.0274393828466,238.,31.8213203435596)) ;
#84256 = CARTESIAN_POINT('Ctrl Pts',(58.0274393828466,238.,31.8577789708945)) ;
#84257 = CARTESIAN_POINT('Ctrl Pts',(57.952105757989,237.962333187571,31.9213203435596)) ;
#84258 = CARTESIAN_POINT('Ctrl Pts',(57.8573593128808,237.9,31.9213203435596)) ;
#84259 = CARTESIAN_POINT('Ctrl Pts',(57.975662586397,238.025132309007,31.8213203435596)) ;
#84260 = CARTESIAN_POINT('Ctrl Pts',(57.975662586397,238.025132309007,31.8441177712024)) ;
#84261 = CARTESIAN_POINT('Ctrl Pts',(57.9346524654691,237.979786480091,31.9213203435596)) ;
#84262 = CARTESIAN_POINT('Ctrl Pts',(57.8573593128808,237.9,31.9213203435596)) ;
#84263 = CARTESIAN_POINT('Ctrl Pts',(57.9573593128808,238.077560052474,31.8213203435596)) ;
#84264 = CARTESIAN_POINT('Ctrl Pts',(57.9573593128808,238.077560052474,31.8619121713414)) ;
#84265 = CARTESIAN_POINT('Ctrl Pts',(57.9171991729491,237.997239772611,31.9213203435596)) ;
#84266 = CARTESIAN_POINT('Ctrl Pts',(57.8573593128808,237.9,31.9213203435596)) ;
#84267 = CARTESIAN_POINT('Ctrl Pts',(57.9573593128808,238.1,31.8213203435596)) ;
#84268 = CARTESIAN_POINT('Ctrl Pts',(57.9573593128808,238.1,31.8736802211195)) ;
#84269 = CARTESIAN_POINT('Ctrl Pts',(57.9097191904406,238.00471975512,31.9213203435596)) ;
#84270 = CARTESIAN_POINT('Ctrl Pts',(57.8573593128808,237.9,31.9213203435596)) ;
#84271 = CARTESIAN_POINT('Origin',(57.8573593128808,237.9,31.8213203435596)) ;
#84272 = CARTESIAN_POINT('Origin',(57.8573593128808,237.9,31.8213203435596)) ;
#84273 = CARTESIAN_POINT('Origin',(57.8573593128808,241.191753592594,31.8213203435596)) ;
#84274 = CARTESIAN_POINT('',(57.9573593128808,239.1,31.8213203435596)) ;
#84275 = CARTESIAN_POINT('',(57.9573593128808,241.191753592594,31.8213203435596)) ;
#84276 = CARTESIAN_POINT('Origin',(57.8573593128808,239.2,31.8213203435596)) ;
#84277 = CARTESIAN_POINT('Origin',(57.9573593128808,243.,19.9213203435596)) ;
#84278 = CARTESIAN_POINT('',(57.9573593128808,239.1,22.9213203435596)) ;
#84279 = CARTESIAN_POINT('Ctrl Pts',(57.9573593128808,242.9,31.8213203435596)) ;
#84280 = CARTESIAN_POINT('Ctrl Pts',(57.9573593128808,242.9,31.8736802211195)) ;
#84281 = CARTESIAN_POINT('Ctrl Pts',(57.9097191904406,242.99528024488,31.9213203435596)) ;
#84282 = CARTESIAN_POINT('Ctrl Pts',(57.8573593128808,243.1,31.9213203435596)) ;
#84283 = CARTESIAN_POINT('Ctrl Pts',(57.9573593128808,242.929919930034,31.8213203435596)) ;
#84284 = CARTESIAN_POINT('Ctrl Pts',(57.9573593128808,242.929919930034,31.8577789708945)) ;
#84285 = CARTESIAN_POINT('Ctrl Pts',(57.919692500452,243.005253554892,31.9213203435596)) ;
#84286 = CARTESIAN_POINT('Ctrl Pts',(57.8573593128808,243.1,31.9213203435596)) ;
#84287 = CARTESIAN_POINT('Ctrl Pts',(57.9824916671412,242.981696672186,31.8213203435596)) ;
#84288 = CARTESIAN_POINT('Ctrl Pts',(57.9824916671412,242.981696672186,31.8441177712024)) ;
#84289 = CARTESIAN_POINT('Ctrl Pts',(57.9371457929719,243.022706847412,31.9213203435596)) ;
#84290 = CARTESIAN_POINT('Ctrl Pts',(57.8573593128808,243.1,31.9213203435596)) ;
#84291 = CARTESIAN_POINT('Ctrl Pts',(58.0349193653551,243.,31.8213203435596)) ;
#84292 = CARTESIAN_POINT('Ctrl Pts',(58.0349193653551,243.,31.8619121713414)) ;
#84293 = CARTESIAN_POINT('Ctrl Pts',(57.9545990854919,243.040160139932,31.9213203435596)) ;
#84294 = CARTESIAN_POINT('Ctrl Pts',(57.8573593128808,243.1,31.9213203435596)) ;
#84295 = CARTESIAN_POINT('Ctrl Pts',(58.0573593128808,243.,31.8213203435596)) ;
#84296 = CARTESIAN_POINT('Ctrl Pts',(58.0573593128808,243.,31.8736802211195)) ;
#84297 = CARTESIAN_POINT('Ctrl Pts',(57.9620790680004,243.04764012244,31.9213203435596)) ;
#84298 = CARTESIAN_POINT('Ctrl Pts',(57.8573593128808,243.1,31.9213203435596)) ;
#84299 = CARTESIAN_POINT('',(57.9573593128808,242.9,31.8213203435596)) ;
#84300 = CARTESIAN_POINT('',(58.0573593128808,243.,31.8213203435596)) ;
#84301 = CARTESIAN_POINT('Origin',(58.0573593128808,242.9,31.8213203435596)) ;
#84302 = CARTESIAN_POINT('Origin',(57.8573593128808,243.1,31.8213203435596)) ;
#84303 = CARTESIAN_POINT('Origin',(57.8573593128808,243.1,31.8213203435596)) ;
#84304 = CARTESIAN_POINT('Origin',(58.0573593128808,242.9,19.9213203435596)) ;
#84305 = CARTESIAN_POINT('',(57.9573593128808,242.9,30.8213203435596)) ;
#84306 = CARTESIAN_POINT('',(58.0573593128808,243.,30.8213203435596)) ;
#84307 = CARTESIAN_POINT('Origin',(58.0573593128808,242.9,30.8213203435596)) ;
#84308 = CARTESIAN_POINT('',(58.0573593128808,243.,19.9213203435596)) ;
#84309 = CARTESIAN_POINT('',(57.9573593128808,242.9,19.9213203435596)) ;
#84310 = CARTESIAN_POINT('Origin',(58.0573593128808,243.1,30.8213203435596)) ;
#84311 = CARTESIAN_POINT('Origin',(58.0573593128808,243.1,30.8213203435596)) ;
#84312 = CARTESIAN_POINT('Origin',(57.9573593128808,243.1,30.8213203435596)) ;
#84313 = CARTESIAN_POINT('Origin',(57.9573593128808,243.,19.9213203435596)) ;
#84314 = CARTESIAN_POINT('',(57.9573593128808,241.9,31.8213203435596)) ;
#84315 = CARTESIAN_POINT('',(57.9573593128808,241.191753592594,31.8213203435596)) ;
#84316 = CARTESIAN_POINT('',(57.9573593128808,241.9,22.9213203435596)) ;
#84317 = CARTESIAN_POINT('Origin',(57.8573593128808,241.191753592594,31.8213203435596)) ;
#84318 = CARTESIAN_POINT('Origin',(57.8573593128807,241.8,31.8213203435596)) ;
#84319 = CARTESIAN_POINT('Origin',(40.95,258.3,30.8213203435596)) ;
#84320 = CARTESIAN_POINT('',(32.3585786437627,258.4,30.8213203435596)) ;
#84321 = CARTESIAN_POINT('Origin',(32.3585786437627,258.3,30.8213203435596)) ;
#84322 = CARTESIAN_POINT('',(28.2,258.4,30.8213203435596)) ;
#84323 = CARTESIAN_POINT('Origin',(28.1999999999999,258.3,30.8213203435596)) ;
#84324 = CARTESIAN_POINT('',(40.95,258.4,30.8213203435596)) ;
#84325 = CARTESIAN_POINT('Origin',(32.3585786437627,258.5,30.8213203435596)) ;
#84326 = CARTESIAN_POINT('',(32.4292893218813,258.429289321881,30.8213203435596)) ;
#84327 = CARTESIAN_POINT('Origin',(32.5,258.358578643763,30.8213203435596)) ;
#84328 = CARTESIAN_POINT('Origin',(32.3585786437627,258.5,30.8213203435596)) ;
#84329 = CARTESIAN_POINT('Origin',(33.2415874744158,259.100166118179,30.8213203435596)) ;
#84330 = CARTESIAN_POINT('',(33.1707106781186,259.170710678119,30.8213203435596)) ;
#84331 = CARTESIAN_POINT('Origin',(33.2414213562373,259.1,30.8213203435596)) ;
#84332 = CARTESIAN_POINT('',(33.1708767962972,259.170876796297,30.8213203435596)) ;
#84333 = CARTESIAN_POINT('Origin',(33.1,259.241421356237,30.8213203435596)) ;
#84334 = CARTESIAN_POINT('',(33.2,259.241421356237,30.8213203435596)) ;
#84335 = CARTESIAN_POINT('Origin',(33.3,259.241421356237,30.8213203435596)) ;
#84336 = CARTESIAN_POINT('Origin',(33.1,259.241421356237,30.8213203435596)) ;
#84337 = CARTESIAN_POINT('Origin',(33.2999999999999,248.891753592594,30.8213203435596)) ;
#84338 = CARTESIAN_POINT('',(33.2,262.558578643763,30.8213203435596)) ;
#84339 = CARTESIAN_POINT('Origin',(33.2999999999999,262.558578643763,30.8213203435596)) ;
#84340 = CARTESIAN_POINT('',(33.2,248.891753592594,30.8213203435596)) ;
#84341 = CARTESIAN_POINT('Origin',(33.1,262.558578643763,30.8213203435596)) ;
#84342 = CARTESIAN_POINT('Origin',(33.1,262.558578643763,30.8213203435596)) ;
#84343 = CARTESIAN_POINT('Origin',(28.1,251.391753592594,30.8213203435596)) ;
#84344 = CARTESIAN_POINT('',(28.2,262.3,30.8213203435596)) ;
#84345 = CARTESIAN_POINT('Origin',(28.1,262.3,30.8213203435596)) ;
#84346 = CARTESIAN_POINT('',(28.2,251.391753592594,30.8213203435596)) ;
#84347 = CARTESIAN_POINT('Origin',(28.2,263.4,19.9213203435596)) ;
#84348 = CARTESIAN_POINT('',(28.1999999999999,263.3,31.8213203435596)) ;
#84349 = CARTESIAN_POINT('',(28.2,263.3,19.9213203435596)) ;
#84350 = CARTESIAN_POINT('',(28.2,262.3,31.8213203435596)) ;
#84351 = CARTESIAN_POINT('',(28.1999999999999,251.391753592594,31.8213203435596)) ;
#84352 = CARTESIAN_POINT('',(28.2,262.3,22.9213203435596)) ;
#84353 = CARTESIAN_POINT('Origin',(28.3,263.3,19.9213203435596)) ;
#84354 = CARTESIAN_POINT('',(28.2999999999999,263.4,31.8213203435596)) ;
#84355 = CARTESIAN_POINT('',(28.3,263.4,19.9213203435596)) ;
#84356 = CARTESIAN_POINT('Origin',(28.2999999999999,263.3,31.8213203435596)) ;
#84357 = CARTESIAN_POINT('Origin',(33.2,263.4,19.9213203435596)) ;
#84358 = CARTESIAN_POINT('',(32.3585786437627,263.4,31.8213203435596)) ;
#84359 = CARTESIAN_POINT('',(32.3585786437627,263.4,19.9213203435596)) ;
#84360 = CARTESIAN_POINT('',(43.45,263.4,31.8213203435596)) ;
#84361 = CARTESIAN_POINT('Origin',(32.3585786437627,263.3,19.9213203435596)) ;
#84362 = CARTESIAN_POINT('',(32.4292893218813,263.370710678119,31.8213203435596)) ;
#84363 = CARTESIAN_POINT('',(32.4292893218813,263.370710678119,19.9213203435596)) ;
#84364 = CARTESIAN_POINT('Origin',(32.3585786437627,263.3,31.8213203435596)) ;
#84365 = CARTESIAN_POINT('Origin',(32.8,263.,19.9213203435596)) ;
#84366 = CARTESIAN_POINT('',(33.1707106781186,262.629289321881,31.8213203435596)) ;
#84367 = CARTESIAN_POINT('',(33.1707106781186,262.629289321881,19.9213203435596)) ;
#84368 = CARTESIAN_POINT('',(43.929123203703,251.870876796297,31.8213203435596)) ;
#84369 = CARTESIAN_POINT('Origin',(33.1,262.558578643763,19.9213203435596)) ;
#84370 = CARTESIAN_POINT('',(33.1999999999999,262.558578643763,31.8213203435596)) ;
#84371 = CARTESIAN_POINT('',(33.2,262.558578643763,19.9213203435596)) ;
#84372 = CARTESIAN_POINT('Origin',(33.1,262.558578643763,31.8213203435596)) ;
#84373 = CARTESIAN_POINT('Origin',(33.2,258.4,19.9213203435596)) ;
#84374 = CARTESIAN_POINT('',(33.1999999999999,259.241421356237,31.8213203435596)) ;
#84375 = CARTESIAN_POINT('',(33.2,259.241421356237,19.9213203435596)) ;
#84376 = CARTESIAN_POINT('',(33.1999999999999,248.891753592594,31.8213203435596)) ;
#84377 = CARTESIAN_POINT('Origin',(33.1,259.241421356237,19.9213203435596)) ;
#84378 = CARTESIAN_POINT('',(33.1707106781186,259.170710678119,31.8213203435596)) ;
#84379 = CARTESIAN_POINT('',(33.1707106781186,259.170710678119,19.9213203435596)) ;
#84380 = CARTESIAN_POINT('Origin',(33.1,259.241421356237,31.8213203435596)) ;
#84381 = CARTESIAN_POINT('Origin',(32.8,258.8,19.9213203435596)) ;
#84382 = CARTESIAN_POINT('',(32.4292893218813,258.429289321881,31.8213203435596)) ;
#84383 = CARTESIAN_POINT('',(32.4292893218813,258.429289321881,19.9213203435596)) ;
#84384 = CARTESIAN_POINT('',(33.1708767962972,259.170876796297,31.8213203435596)) ;
#84385 = CARTESIAN_POINT('Origin',(32.3585786437627,258.5,19.9213203435596)) ;
#84386 = CARTESIAN_POINT('',(32.3585786437627,258.4,31.8213203435596)) ;
#84387 = CARTESIAN_POINT('',(32.3585786437627,258.4,19.9213203435596)) ;
#84388 = CARTESIAN_POINT('Origin',(32.3585786437627,258.5,31.8213203435596)) ;
#84389 = CARTESIAN_POINT('Origin',(28.2,258.4,19.9213203435596)) ;
#84390 = CARTESIAN_POINT('',(28.1999999999999,258.4,31.8213203435596)) ;
#84391 = CARTESIAN_POINT('',(28.2,258.4,19.9213203435596)) ;
#84392 = CARTESIAN_POINT('',(40.95,258.4,31.8213203435596)) ;
#84393 = CARTESIAN_POINT('Origin',(64.1,226.1,30.8213203435596)) ;
#84394 = CARTESIAN_POINT('',(74.3999999999999,226.,30.8213203435596)) ;
#84395 = CARTESIAN_POINT('Origin',(74.3999999999999,226.1,30.8213203435596)) ;
#84396 = CARTESIAN_POINT('',(74.2999999999999,226.,30.8213203435596)) ;
#84397 = CARTESIAN_POINT('',(64.1,226.,30.8213203435596)) ;
#84398 = CARTESIAN_POINT('Origin',(74.2999999999999,226.1,30.8213203435596)) ;
#84399 = CARTESIAN_POINT('Origin',(74.3999999999999,225.9,30.8213203435596)) ;
#84400 = CARTESIAN_POINT('',(74.4999999999999,225.9,30.8213203435596)) ;
#84401 = CARTESIAN_POINT('Origin',(74.6,225.9,30.8213203435596)) ;
#84402 = CARTESIAN_POINT('Origin',(74.3999999999999,225.9,30.8213203435596)) ;
#84403 = CARTESIAN_POINT('Origin',(74.5999999999999,231.191753592594,30.8213203435596)) ;
#84404 = CARTESIAN_POINT('',(74.4999999999999,223.1,30.8213203435596)) ;
#84405 = CARTESIAN_POINT('Origin',(74.5999999999999,223.1,30.8213203435596)) ;
#84406 = CARTESIAN_POINT('',(74.4999999999999,231.191753592594,30.8213203435596)) ;
#84407 = CARTESIAN_POINT('Origin',(74.3999999999999,223.1,30.8213203435596)) ;
#84408 = CARTESIAN_POINT('',(74.3999999999999,223.,30.8213203435596)) ;
#84409 = CARTESIAN_POINT('Origin',(74.3999999999999,222.9,30.8213203435596)) ;
#84410 = CARTESIAN_POINT('Origin',(74.3999999999999,223.1,30.8213203435596)) ;
#84411 = CARTESIAN_POINT('Origin',(62.6,222.9,30.8213203435596)) ;
#84412 = CARTESIAN_POINT('',(71.5999999999999,223.,30.8213203435596)) ;
#84413 = CARTESIAN_POINT('Origin',(71.5999999999999,222.9,30.8213203435596)) ;
#84414 = CARTESIAN_POINT('',(62.6,223.,30.8213203435596)) ;
#84415 = CARTESIAN_POINT('Origin',(71.5999999999999,223.1,30.8213203435596)) ;
#84416 = CARTESIAN_POINT('',(71.4999999999999,223.1,30.8213203435596)) ;
#84417 = CARTESIAN_POINT('Origin',(71.3999999999999,223.1,30.8213203435596)) ;
#84418 = CARTESIAN_POINT('Origin',(71.5999999999999,223.1,30.8213203435596)) ;
#84419 = CARTESIAN_POINT('Origin',(71.3999999999999,232.691753592594,30.8213203435596)) ;
#84420 = CARTESIAN_POINT('',(71.4999999999999,225.9,30.8213203435596)) ;
#84421 = CARTESIAN_POINT('Origin',(71.3999999999999,225.9,30.8213203435596)) ;
#84422 = CARTESIAN_POINT('',(71.4999999999999,232.691753592594,30.8213203435596)) ;
#84423 = CARTESIAN_POINT('Origin',(71.5999999999999,225.9,30.8213203435596)) ;
#84424 = CARTESIAN_POINT('',(71.5999999999999,226.,30.8213203435596)) ;
#84425 = CARTESIAN_POINT('Origin',(71.5999999999999,226.1,30.8213203435596)) ;
#84426 = CARTESIAN_POINT('Origin',(71.5999999999999,225.9,30.8213203435596)) ;
#84427 = CARTESIAN_POINT('Origin',(62.75,226.1,30.8213203435596)) ;
#84428 = CARTESIAN_POINT('',(71.6999999999999,226.,30.8213203435596)) ;
#84429 = CARTESIAN_POINT('Origin',(71.6999999999999,226.1,30.8213203435596)) ;
#84430 = CARTESIAN_POINT('',(62.75,226.,30.8213203435596)) ;
#84431 = CARTESIAN_POINT('Origin',(71.6999999999999,235.691753592594,30.8213203435596)) ;
#84432 = CARTESIAN_POINT('',(71.7999999999999,231.9,30.8213203435596)) ;
#84433 = CARTESIAN_POINT('Origin',(71.6999999999999,231.9,30.8213203435596)) ;
#84434 = CARTESIAN_POINT('',(71.7999999999999,226.1,30.8213203435596)) ;
#84435 = CARTESIAN_POINT('',(71.7999999999999,235.691753592594,30.8213203435596)) ;
#84436 = CARTESIAN_POINT('Origin',(71.6999999999999,226.1,30.8213203435596)) ;
#84437 = CARTESIAN_POINT('Origin',(71.8999999999999,231.9,30.8213203435596)) ;
#84438 = CARTESIAN_POINT('',(71.8999999999999,232.,30.8213203435596)) ;
#84439 = CARTESIAN_POINT('Origin',(71.8999999999999,232.1,30.8213203435596)) ;
#84440 = CARTESIAN_POINT('Origin',(71.8999999999999,231.9,30.8213203435596)) ;
#84441 = CARTESIAN_POINT('Origin',(63.95,232.1,30.8213203435596)) ;
#84442 = CARTESIAN_POINT('',(74.0999999999999,232.,30.8213203435596)) ;
#84443 = CARTESIAN_POINT('Origin',(74.0999999999999,232.1,30.8213203435596)) ;
#84444 = CARTESIAN_POINT('',(63.95,232.,30.8213203435596)) ;
#84445 = CARTESIAN_POINT('Origin',(74.0999999999999,231.9,30.8213203435596)) ;
#84446 = CARTESIAN_POINT('',(74.1999999999999,231.9,30.8213203435596)) ;
#84447 = CARTESIAN_POINT('Origin',(74.2999999999999,231.9,30.8213203435596)) ;
#84448 = CARTESIAN_POINT('Origin',(74.0999999999999,231.9,30.8213203435596)) ;
#84449 = CARTESIAN_POINT('Origin',(74.2999999999999,232.691753592594,30.8213203435596)) ;
#84450 = CARTESIAN_POINT('',(74.1999999999999,226.1,30.8213203435596)) ;
#84451 = CARTESIAN_POINT('Origin',(74.2999999999999,226.1,30.8213203435596)) ;
#84452 = CARTESIAN_POINT('',(74.1999999999999,232.691753592594,30.8213203435596)) ;
#84453 = CARTESIAN_POINT('Origin',(71.6999999999999,226.1,30.8213203435596)) ;
#84454 = CARTESIAN_POINT('Origin',(71.6999999999999,226.1,30.8213203435596)) ;
#84455 = CARTESIAN_POINT('Origin',(74.2999999999999,226.1,30.8213203435596)) ;
#84456 = CARTESIAN_POINT('Origin',(74.2999999999999,226.1,30.8213203435596)) ;
#84457 = CARTESIAN_POINT('Origin',(74.3999999999999,223.1,19.9213203435596)) ;
#84458 = CARTESIAN_POINT('',(74.3999999999999,223.,31.8213203435596)) ;
#84459 = CARTESIAN_POINT('',(74.3999999999999,223.,19.9213203435596)) ;
#84460 = CARTESIAN_POINT('',(74.4999999999999,223.1,31.8213203435596)) ;
#84461 = CARTESIAN_POINT('Origin',(74.3999999999999,223.1,31.8213203435596)) ;
#84462 = CARTESIAN_POINT('',(74.4999999999999,223.1,19.9213203435596)) ;
#84463 = CARTESIAN_POINT('Origin',(71.4999999999999,223.,19.9213203435596)) ;
#84464 = CARTESIAN_POINT('',(71.5999999999999,223.,31.8213203435596)) ;
#84465 = CARTESIAN_POINT('',(71.5999999999999,223.,19.9213203435596)) ;
#84466 = CARTESIAN_POINT('',(62.6,223.,31.8213203435596)) ;
#84467 = CARTESIAN_POINT('Origin',(71.5999999999999,223.1,19.9213203435596)) ;
#84468 = CARTESIAN_POINT('',(71.4999999999999,223.1,31.8213203435596)) ;
#84469 = CARTESIAN_POINT('',(71.4999999999999,223.1,19.9213203435596)) ;
#84470 = CARTESIAN_POINT('Origin',(71.5999999999999,223.1,31.8213203435596)) ;
#84471 = CARTESIAN_POINT('Origin',(71.4999999999999,226.,19.9213203435596)) ;
#84472 = CARTESIAN_POINT('',(71.4999999999999,225.9,31.8213203435596)) ;
#84473 = CARTESIAN_POINT('',(71.4999999999999,225.9,19.9213203435596)) ;
#84474 = CARTESIAN_POINT('',(71.4999999999999,232.691753592594,31.8213203435596)) ;
#84475 = CARTESIAN_POINT('Origin',(71.5999999999999,225.9,19.9213203435596)) ;
#84476 = CARTESIAN_POINT('',(71.5999999999999,226.,31.8213203435596)) ;
#84477 = CARTESIAN_POINT('',(71.5999999999999,226.,19.9213203435596)) ;
#84478 = CARTESIAN_POINT('Origin',(71.5999999999999,225.9,31.8213203435596)) ;
#84479 = CARTESIAN_POINT('Origin',(71.7999999999999,226.,19.9213203435596)) ;
#84480 = CARTESIAN_POINT('',(71.6999999999999,226.,31.8213203435596)) ;
#84481 = CARTESIAN_POINT('',(71.6999999999999,226.,19.9213203435596)) ;
#84482 = CARTESIAN_POINT('',(62.75,226.,31.8213203435596)) ;
#84483 = CARTESIAN_POINT('Origin',(71.6999999999999,226.1,19.9213203435596)) ;
#84484 = CARTESIAN_POINT('',(71.7999999999999,226.1,31.8213203435596)) ;
#84485 = CARTESIAN_POINT('',(71.7999999999999,226.1,19.9213203435596)) ;
#84486 = CARTESIAN_POINT('Origin',(71.6999999999999,226.1,31.8213203435596)) ;
#84487 = CARTESIAN_POINT('Origin',(71.7999999999999,232.,19.9213203435596)) ;
#84488 = CARTESIAN_POINT('',(71.7999999999999,231.9,31.8213203435596)) ;
#84489 = CARTESIAN_POINT('',(71.7999999999999,231.9,19.9213203435596)) ;
#84490 = CARTESIAN_POINT('',(71.7999999999999,235.691753592594,31.8213203435596)) ;
#84491 = CARTESIAN_POINT('Origin',(80.0999999999989,248.6,30.8213203435596)) ;
#84492 = CARTESIAN_POINT('',(80.0999999999989,248.5,30.8213203435596)) ;
#84493 = CARTESIAN_POINT('Origin',(80.0999999999989,248.4,30.8213203435596)) ;
#84494 = CARTESIAN_POINT('',(80.199999999999,248.6,30.8213203435596)) ;
#84495 = CARTESIAN_POINT('Origin',(80.0999999999989,248.6,30.8213203435596)) ;
#84496 = CARTESIAN_POINT('Origin',(80.2999999999989,248.6,30.8213203435596)) ;
#84497 = CARTESIAN_POINT('Origin',(80.099999999999,253.4,30.8213203435596)) ;
#84498 = CARTESIAN_POINT('',(80.099999999999,253.5,30.8213203435596)) ;
#84499 = CARTESIAN_POINT('',(80.199999999999,253.4,30.8213203435596)) ;
#84500 = CARTESIAN_POINT('Origin',(80.099999999999,253.4,30.8213203435596)) ;
#84501 = CARTESIAN_POINT('Origin',(80.099999999999,253.6,30.8213203435596)) ;
#84502 = CARTESIAN_POINT('Origin',(80.299999999999,253.4,30.8213203435596)) ;
#84503 = CARTESIAN_POINT('Origin',(66.9499999999995,253.6,30.8213203435596)) ;
#84504 = CARTESIAN_POINT('',(76.0414213562367,253.5,30.8213203435596)) ;
#84505 = CARTESIAN_POINT('Origin',(76.0414213562367,253.6,30.8213203435596)) ;
#84506 = CARTESIAN_POINT('',(66.9499999999995,253.5,30.8213203435596)) ;
#84507 = CARTESIAN_POINT('Origin',(76.0414213562367,253.4,30.8213203435596)) ;
#84508 = CARTESIAN_POINT('',(75.9707106781181,253.470710678119,30.8213203435596)) ;
#84509 = CARTESIAN_POINT('Origin',(75.8999999999994,253.541421356237,30.8213203435596)) ;
#84510 = CARTESIAN_POINT('Origin',(76.0414213562367,253.4,30.8213203435596)) ;
#84511 = CARTESIAN_POINT('Origin',(66.6251661181778,244.266587474416,30.8213203435596)) ;
#84512 = CARTESIAN_POINT('',(75.2292893218808,252.729289321881,30.8213203435596)) ;
#84513 = CARTESIAN_POINT('Origin',(75.1585786437621,252.8,30.8213203435596)) ;
#84514 = CARTESIAN_POINT('',(66.6958767962964,244.195876796297,30.8213203435596)) ;
#84515 = CARTESIAN_POINT('Origin',(75.2999999999994,252.658578643763,30.8213203435596)) ;
#84516 = CARTESIAN_POINT('',(75.1999999999994,252.658578643763,30.8213203435596)) ;
#84517 = CARTESIAN_POINT('Origin',(75.0999999999994,252.658578643763,30.8213203435596)) ;
#84518 = CARTESIAN_POINT('Origin',(75.2999999999994,252.658578643763,30.8213203435596)) ;
#84519 = CARTESIAN_POINT('Origin',(75.0999999999992,246.441753592594,30.8213203435596)) ;
#84520 = CARTESIAN_POINT('',(75.1999999999993,249.341421356237,30.8213203435596)) ;
#84521 = CARTESIAN_POINT('Origin',(75.0999999999993,249.341421356237,30.8213203435596)) ;
#84522 = CARTESIAN_POINT('',(75.1999999999992,246.441753592594,30.8213203435596)) ;
#84523 = CARTESIAN_POINT('Origin',(75.2999999999993,249.341421356237,30.8213203435596)) ;
#84524 = CARTESIAN_POINT('',(75.2292893218807,249.270710678119,30.8213203435596)) ;
#84525 = CARTESIAN_POINT('Origin',(75.158578643762,249.2,30.8213203435596)) ;
#84526 = CARTESIAN_POINT('Origin',(75.2999999999993,249.341421356237,30.8213203435596)) ;
#84527 = CARTESIAN_POINT('Origin',(72.4334125255833,251.925166118179,30.8213203435596)) ;
#84528 = CARTESIAN_POINT('',(75.9707106781179,248.529289321881,30.8213203435596)) ;
#84529 = CARTESIAN_POINT('Origin',(75.8999999999992,248.458578643763,30.8213203435596)) ;
#84530 = CARTESIAN_POINT('',(72.504123203702,251.995876796297,30.8213203435596)) ;
#84531 = CARTESIAN_POINT('Origin',(76.0414213562365,248.6,30.8213203435596)) ;
#84532 = CARTESIAN_POINT('',(76.0414213562365,248.5,30.8213203435596)) ;
#84533 = CARTESIAN_POINT('Origin',(76.0414213562365,248.4,30.8213203435596)) ;
#84534 = CARTESIAN_POINT('Origin',(76.0414213562365,248.6,30.8213203435596)) ;
#84535 = CARTESIAN_POINT('Origin',(64.4499999999996,248.4,30.8213203435596)) ;
#84536 = CARTESIAN_POINT('',(64.4499999999996,248.5,30.8213203435596)) ;
#84537 = CARTESIAN_POINT('Origin',(80.2999999999989,243.941753592594,30.8213203435596)) ;
#84538 = CARTESIAN_POINT('',(80.199999999999,252.4,30.8213203435596)) ;
#84539 = CARTESIAN_POINT('Origin',(80.299999999999,252.4,30.8213203435596)) ;
#84540 = CARTESIAN_POINT('',(80.1999999999989,243.941753592594,30.8213203435596)) ;
#84541 = CARTESIAN_POINT('Origin',(80.099999999999,253.4,19.9213203435596)) ;
#84542 = CARTESIAN_POINT('',(80.199999999999,253.4,31.8213203435596)) ;
#84543 = CARTESIAN_POINT('',(80.099999999999,253.5,31.8213203435596)) ;
#84544 = CARTESIAN_POINT('Origin',(80.099999999999,253.4,31.8213203435596)) ;
#84545 = CARTESIAN_POINT('',(80.099999999999,253.5,19.9213203435596)) ;
#84546 = CARTESIAN_POINT('',(80.199999999999,253.4,19.9213203435596)) ;
#84547 = CARTESIAN_POINT('Ctrl Pts',(80.099999999999,253.5,31.8213203435596)) ;
#84548 = CARTESIAN_POINT('Ctrl Pts',(80.099999999999,253.5,31.8736802211195)) ;
#84549 = CARTESIAN_POINT('Ctrl Pts',(80.1952802448793,253.54764012244,31.9213203435596)) ;
#84550 = CARTESIAN_POINT('Ctrl Pts',(80.299999999999,253.6,31.9213203435596)) ;
#84551 = CARTESIAN_POINT('Ctrl Pts',(80.1299199300332,253.5,31.8213203435596)) ;
#84552 = CARTESIAN_POINT('Ctrl Pts',(80.1299199300331,253.5,31.8577789708945)) ;
#84553 = CARTESIAN_POINT('Ctrl Pts',(80.2052535548907,253.537666812429,31.9213203435596)) ;
#84554 = CARTESIAN_POINT('Ctrl Pts',(80.299999999999,253.6,31.9213203435596)) ;
#84555 = CARTESIAN_POINT('Ctrl Pts',(80.1816963524867,253.474867379293,31.8213203435596)) ;
#84556 = CARTESIAN_POINT('Ctrl Pts',(80.1816963524867,253.474867379293,31.8441177712024)) ;
#84557 = CARTESIAN_POINT('Ctrl Pts',(80.2227068474107,253.520213519909,31.9213203435596)) ;
#84558 = CARTESIAN_POINT('Ctrl Pts',(80.299999999999,253.6,31.9213203435596)) ;
#84559 = CARTESIAN_POINT('Ctrl Pts',(80.199999999999,253.422439947526,31.8213203435596)) ;
#84560 = CARTESIAN_POINT('Ctrl Pts',(80.199999999999,253.422439947526,31.8619121713415)) ;
#84561 = CARTESIAN_POINT('Ctrl Pts',(80.2401601399306,253.502760227389,31.9213203435596)) ;
#84562 = CARTESIAN_POINT('Ctrl Pts',(80.299999999999,253.6,31.9213203435596)) ;
#84563 = CARTESIAN_POINT('Ctrl Pts',(80.199999999999,253.4,31.8213203435596)) ;
#84564 = CARTESIAN_POINT('Ctrl Pts',(80.199999999999,253.4,31.8736802211195)) ;
#84565 = CARTESIAN_POINT('Ctrl Pts',(80.2476401224392,253.49528024488,31.9213203435596)) ;
#84566 = CARTESIAN_POINT('Ctrl Pts',(80.299999999999,253.6,31.9213203435596)) ;
#84567 = CARTESIAN_POINT('Origin',(80.299999999999,253.6,31.8213203435596)) ;
#84568 = CARTESIAN_POINT('Origin',(80.299999999999,253.6,31.8213203435596)) ;
#84569 = CARTESIAN_POINT('Origin',(80.0999999999989,248.6,19.9213203435596)) ;
#84570 = CARTESIAN_POINT('',(80.0999999999989,248.5,31.8213203435596)) ;
#84571 = CARTESIAN_POINT('',(80.199999999999,248.6,31.8213203435596)) ;
#84572 = CARTESIAN_POINT('Origin',(80.0999999999989,248.6,31.8213203435596)) ;
#84573 = CARTESIAN_POINT('',(80.199999999999,248.6,19.9213203435596)) ;
#84574 = CARTESIAN_POINT('',(80.0999999999989,248.5,19.9213203435596)) ;
#84575 = CARTESIAN_POINT('Ctrl Pts',(80.299999999999,248.4,31.9213203435596)) ;
#84576 = CARTESIAN_POINT('Ctrl Pts',(80.1952802448793,248.45235987756,31.9213203435597)) ;
#84577 = CARTESIAN_POINT('Ctrl Pts',(80.0999999999989,248.5,31.8736802211194)) ;
#84578 = CARTESIAN_POINT('Ctrl Pts',(80.0999999999989,248.5,31.8213203435596)) ;
#84579 = CARTESIAN_POINT('Ctrl Pts',(80.299999999999,248.4,31.9213203435596)) ;
#84580 = CARTESIAN_POINT('Ctrl Pts',(80.2052535548907,248.462333187571,31.9213203435597)) ;
#84581 = CARTESIAN_POINT('Ctrl Pts',(80.1299199300331,248.5,31.8577789708944)) ;
#84582 = CARTESIAN_POINT('Ctrl Pts',(80.1299199300331,248.5,31.8213203435596)) ;
#84583 = CARTESIAN_POINT('Ctrl Pts',(80.299999999999,248.4,31.9213203435596)) ;
#84584 = CARTESIAN_POINT('Ctrl Pts',(80.2227068474107,248.479786480091,31.9213203435597)) ;
#84585 = CARTESIAN_POINT('Ctrl Pts',(80.1816963988781,248.525132582043,31.8441177712024)) ;
#84586 = CARTESIAN_POINT('Ctrl Pts',(80.1816963988781,248.525132582043,31.8213203435596)) ;
#84587 = CARTESIAN_POINT('Ctrl Pts',(80.299999999999,248.4,31.9213203435596)) ;
#84588 = CARTESIAN_POINT('Ctrl Pts',(80.2401601399306,248.497239772611,31.9213203435597)) ;
#84589 = CARTESIAN_POINT('Ctrl Pts',(80.1999999999989,248.577560052474,31.8619121713414)) ;
#84590 = CARTESIAN_POINT('Ctrl Pts',(80.1999999999989,248.577560052474,31.8213203435596)) ;
#84591 = CARTESIAN_POINT('Ctrl Pts',(80.299999999999,248.4,31.9213203435596)) ;
#84592 = CARTESIAN_POINT('Ctrl Pts',(80.2476401224392,248.50471975512,31.9213203435597)) ;
#84593 = CARTESIAN_POINT('Ctrl Pts',(80.1999999999989,248.6,31.8736802211195)) ;
#84594 = CARTESIAN_POINT('Ctrl Pts',(80.1999999999989,248.6,31.8213203435596)) ;
#84595 = CARTESIAN_POINT('Origin',(80.2999999999989,248.4,31.8213203435596)) ;
#84596 = CARTESIAN_POINT('Origin',(80.2999999999989,248.4,31.8213203435596)) ;
#84597 = CARTESIAN_POINT('Origin',(80.2999999999989,243.941753592594,30.8213203435596)) ;
#84598 = CARTESIAN_POINT('',(80.199999999999,249.6,30.8213203435596)) ;
#84599 = CARTESIAN_POINT('Origin',(80.2999999999989,249.6,30.8213203435596)) ;
#84600 = CARTESIAN_POINT('',(80.1999999999989,243.941753592594,30.8213203435596)) ;
#84601 = CARTESIAN_POINT('Origin',(80.199999999999,248.5,19.9213203435596)) ;
#84602 = CARTESIAN_POINT('',(80.199999999999,252.4,31.8213203435596)) ;
#84603 = CARTESIAN_POINT('',(80.199999999999,252.4,22.9213203435596)) ;
#84604 = CARTESIAN_POINT('',(80.1999999999989,243.941753592594,31.8213203435596)) ;
#84605 = CARTESIAN_POINT('Origin',(64.4999999999999,250.9,30.8213203435596)) ;
#84606 = CARTESIAN_POINT('',(64.4999999999999,251.,30.8213203435596)) ;
#84607 = CARTESIAN_POINT('Origin',(64.4999999999999,251.1,30.8213203435596)) ;
#84608 = CARTESIAN_POINT('',(64.3999999999999,250.9,30.8213203435596)) ;
#84609 = CARTESIAN_POINT('Origin',(64.4999999999999,250.9,30.8213203435596)) ;
#84610 = CARTESIAN_POINT('Origin',(64.3,250.9,30.8213203435596)) ;
#84611 = CARTESIAN_POINT('Origin',(59.2,251.1,30.8213203435596)) ;
#84612 = CARTESIAN_POINT('',(64.6,251.,30.8213203435596)) ;
#84613 = CARTESIAN_POINT('Origin',(64.6,251.1,30.8213203435596)) ;
#84614 = CARTESIAN_POINT('',(59.2,251.,30.8213203435596)) ;
#84615 = CARTESIAN_POINT('Origin',(64.6,248.191753592594,30.8213203435596)) ;
#84616 = CARTESIAN_POINT('',(64.7,256.9,30.8213203435596)) ;
#84617 = CARTESIAN_POINT('Origin',(64.6,256.9,30.8213203435596)) ;
#84618 = CARTESIAN_POINT('',(64.7,251.1,30.8213203435596)) ;
#84619 = CARTESIAN_POINT('',(64.7,248.191753592594,30.8213203435596)) ;
#84620 = CARTESIAN_POINT('Origin',(64.6,251.1,30.8213203435596)) ;
#84621 = CARTESIAN_POINT('Origin',(64.8,256.9,30.8213203435596)) ;
#84622 = CARTESIAN_POINT('',(64.8,257.,30.8213203435596)) ;
#84623 = CARTESIAN_POINT('Origin',(64.8,257.1,30.8213203435596)) ;
#84624 = CARTESIAN_POINT('Origin',(64.8,256.9,30.8213203435596)) ;
#84625 = CARTESIAN_POINT('Origin',(60.4,257.1,30.8213203435596)) ;
#84626 = CARTESIAN_POINT('',(67.,257.,30.8213203435596)) ;
#84627 = CARTESIAN_POINT('Origin',(67.,257.1,30.8213203435596)) ;
#84628 = CARTESIAN_POINT('',(60.4,257.,30.8213203435596)) ;
#84629 = CARTESIAN_POINT('Origin',(67.,256.9,30.8213203435596)) ;
#84630 = CARTESIAN_POINT('',(67.1,256.9,30.8213203435596)) ;
#84631 = CARTESIAN_POINT('Origin',(67.2,256.9,30.8213203435596)) ;
#84632 = CARTESIAN_POINT('Origin',(67.,256.9,30.8213203435596)) ;
#84633 = CARTESIAN_POINT('Origin',(67.2,245.191753592594,30.8213203435596)) ;
#84634 = CARTESIAN_POINT('',(67.1,251.1,30.8213203435596)) ;
#84635 = CARTESIAN_POINT('Origin',(67.2,251.1,30.8213203435596)) ;
#84636 = CARTESIAN_POINT('',(67.1,245.191753592594,30.8213203435596)) ;
#84637 = CARTESIAN_POINT('Origin',(64.6,251.1,30.8213203435596)) ;
#84638 = CARTESIAN_POINT('Origin',(64.6,251.1,30.8213203435596)) ;
#84639 = CARTESIAN_POINT('Origin',(60.55,251.1,30.8213203435596)) ;
#84640 = CARTESIAN_POINT('',(67.3,251.,30.8213203435596)) ;
#84641 = CARTESIAN_POINT('Origin',(67.3,251.1,30.8213203435596)) ;
#84642 = CARTESIAN_POINT('',(67.2,251.,30.8213203435596)) ;
#84643 = CARTESIAN_POINT('',(60.55,251.,30.8213203435596)) ;
#84644 = CARTESIAN_POINT('Origin',(67.2,251.1,30.8213203435596)) ;
#84645 = CARTESIAN_POINT('Origin',(67.3,250.9,30.8213203435596)) ;
#84646 = CARTESIAN_POINT('',(67.4,250.9,30.8213203435596)) ;
#84647 = CARTESIAN_POINT('Origin',(67.5,250.9,30.8213203435596)) ;
#84648 = CARTESIAN_POINT('Origin',(67.3,250.9,30.8213203435596)) ;
#84649 = CARTESIAN_POINT('Origin',(67.2,251.1,30.8213203435596)) ;
#84650 = CARTESIAN_POINT('Origin',(67.2,251.1,30.8213203435596)) ;
#84651 = CARTESIAN_POINT('Origin',(64.7,251.,19.9213203435596)) ;
#84652 = CARTESIAN_POINT('',(64.6,251.,31.8213203435596)) ;
#84653 = CARTESIAN_POINT('',(64.6,251.,19.9213203435596)) ;
#84654 = CARTESIAN_POINT('',(64.5,251.,31.8213203435596)) ;
#84655 = CARTESIAN_POINT('',(59.2,251.,31.8213203435596)) ;
#84656 = CARTESIAN_POINT('',(64.5,251.,19.9213203435596)) ;
#84657 = CARTESIAN_POINT('Origin',(64.6,251.1,19.9213203435596)) ;
#84658 = CARTESIAN_POINT('',(64.7,251.1,31.8213203435596)) ;
#84659 = CARTESIAN_POINT('',(64.7,251.1,19.9213203435596)) ;
#84660 = CARTESIAN_POINT('Origin',(64.6,251.1,31.8213203435596)) ;
#84661 = CARTESIAN_POINT('Origin',(64.7,257.,19.9213203435596)) ;
#84662 = CARTESIAN_POINT('',(64.7,256.9,31.8213203435596)) ;
#84663 = CARTESIAN_POINT('',(64.7,256.9,19.9213203435596)) ;
#84664 = CARTESIAN_POINT('',(64.7,248.191753592594,31.8213203435596)) ;
#84665 = CARTESIAN_POINT('Origin',(64.8,256.9,19.9213203435596)) ;
#84666 = CARTESIAN_POINT('',(64.8,257.,31.8213203435596)) ;
#84667 = CARTESIAN_POINT('',(64.8,257.,19.9213203435596)) ;
#84668 = CARTESIAN_POINT('Origin',(64.8,256.9,31.8213203435596)) ;
#84669 = CARTESIAN_POINT('Origin',(67.1,257.,19.9213203435596)) ;
#84670 = CARTESIAN_POINT('',(67.,257.,31.8213203435596)) ;
#84671 = CARTESIAN_POINT('',(67.,257.,19.9213203435596)) ;
#84672 = CARTESIAN_POINT('',(60.4,257.,31.8213203435596)) ;
#84673 = CARTESIAN_POINT('Origin',(67.,256.9,19.9213203435596)) ;
#84674 = CARTESIAN_POINT('',(67.1,256.9,31.8213203435596)) ;
#84675 = CARTESIAN_POINT('',(67.1,256.9,19.9213203435596)) ;
#84676 = CARTESIAN_POINT('Origin',(67.,256.9,31.8213203435596)) ;
#84677 = CARTESIAN_POINT('Origin',(67.1,251.,19.9213203435596)) ;
#84678 = CARTESIAN_POINT('',(67.1,251.1,31.8213203435596)) ;
#84679 = CARTESIAN_POINT('',(67.1,251.1,19.9213203435596)) ;
#84680 = CARTESIAN_POINT('',(67.1,245.191753592594,31.8213203435596)) ;
#84681 = CARTESIAN_POINT('Origin',(67.2,251.1,19.9213203435596)) ;
#84682 = CARTESIAN_POINT('',(67.2,251.,31.8213203435596)) ;
#84683 = CARTESIAN_POINT('',(67.2,251.,19.9213203435596)) ;
#84684 = CARTESIAN_POINT('Origin',(67.2,251.1,31.8213203435596)) ;
#84685 = CARTESIAN_POINT('Origin',(67.4,251.,19.9213203435596)) ;
#84686 = CARTESIAN_POINT('',(67.3,251.,31.8213203435596)) ;
#84687 = CARTESIAN_POINT('',(67.3,251.,19.9213203435596)) ;
#84688 = CARTESIAN_POINT('',(60.55,251.,31.8213203435596)) ;
#84689 = CARTESIAN_POINT('Origin',(56.5,250.9,30.8213203435596)) ;
#84690 = CARTESIAN_POINT('',(56.5,251.,30.8213203435596)) ;
#84691 = CARTESIAN_POINT('Origin',(56.5,251.1,30.8213203435596)) ;
#84692 = CARTESIAN_POINT('',(56.3999999999999,250.9,30.8213203435596)) ;
#84693 = CARTESIAN_POINT('Origin',(56.5,250.9,30.8213203435596)) ;
#84694 = CARTESIAN_POINT('Origin',(56.3,250.9,30.8213203435596)) ;
#84695 = CARTESIAN_POINT('Origin',(55.2,251.1,30.8213203435596)) ;
#84696 = CARTESIAN_POINT('',(56.6,251.,30.8213203435596)) ;
#84697 = CARTESIAN_POINT('Origin',(56.6,251.1,30.8213203435596)) ;
#84698 = CARTESIAN_POINT('',(55.2,251.,30.8213203435596)) ;
#84699 = CARTESIAN_POINT('Origin',(56.6,248.191753592594,30.8213203435596)) ;
#84700 = CARTESIAN_POINT('',(56.7,256.9,30.8213203435596)) ;
#84701 = CARTESIAN_POINT('Origin',(56.6,256.9,30.8213203435596)) ;
#84702 = CARTESIAN_POINT('',(56.7,251.1,30.8213203435596)) ;
#84703 = CARTESIAN_POINT('',(56.7,248.191753592594,30.8213203435596)) ;
#84704 = CARTESIAN_POINT('Origin',(56.6,251.1,30.8213203435596)) ;
#84705 = CARTESIAN_POINT('Origin',(56.8,256.9,30.8213203435596)) ;
#84706 = CARTESIAN_POINT('',(56.8,257.,30.8213203435596)) ;
#84707 = CARTESIAN_POINT('Origin',(56.8,257.1,30.8213203435596)) ;
#84708 = CARTESIAN_POINT('Origin',(56.8,256.9,30.8213203435596)) ;
#84709 = CARTESIAN_POINT('Origin',(56.4,257.1,30.8213203435596)) ;
#84710 = CARTESIAN_POINT('',(59.,257.,30.8213203435596)) ;
#84711 = CARTESIAN_POINT('Origin',(59.,257.1,30.8213203435596)) ;
#84712 = CARTESIAN_POINT('',(56.4,257.,30.8213203435596)) ;
#84713 = CARTESIAN_POINT('Origin',(59.,256.9,30.8213203435596)) ;
#84714 = CARTESIAN_POINT('',(59.1,256.9,30.8213203435596)) ;
#84715 = CARTESIAN_POINT('Origin',(59.2,256.9,30.8213203435596)) ;
#84716 = CARTESIAN_POINT('Origin',(59.,256.9,30.8213203435596)) ;
#84717 = CARTESIAN_POINT('Origin',(59.2,245.191753592594,30.8213203435596)) ;
#84718 = CARTESIAN_POINT('',(59.1,251.1,30.8213203435596)) ;
#84719 = CARTESIAN_POINT('Origin',(59.2,251.1,30.8213203435596)) ;
#84720 = CARTESIAN_POINT('',(59.1,245.191753592594,30.8213203435596)) ;
#84721 = CARTESIAN_POINT('Origin',(56.6,251.1,30.8213203435596)) ;
#84722 = CARTESIAN_POINT('Origin',(56.6,251.1,30.8213203435596)) ;
#84723 = CARTESIAN_POINT('Origin',(56.55,251.1,30.8213203435596)) ;
#84724 = CARTESIAN_POINT('',(59.3,251.,30.8213203435596)) ;
#84725 = CARTESIAN_POINT('Origin',(59.3,251.1,30.8213203435596)) ;
#84726 = CARTESIAN_POINT('',(59.2,251.,30.8213203435596)) ;
#84727 = CARTESIAN_POINT('',(56.55,251.,30.8213203435596)) ;
#84728 = CARTESIAN_POINT('Origin',(59.2,251.1,30.8213203435596)) ;
#84729 = CARTESIAN_POINT('Origin',(59.3,250.9,30.8213203435596)) ;
#84730 = CARTESIAN_POINT('',(59.4,250.9,30.8213203435596)) ;
#84731 = CARTESIAN_POINT('Origin',(59.5,250.9,30.8213203435596)) ;
#84732 = CARTESIAN_POINT('Origin',(59.3,250.9,30.8213203435596)) ;
#84733 = CARTESIAN_POINT('Origin',(59.2,251.1,30.8213203435596)) ;
#84734 = CARTESIAN_POINT('Origin',(59.2,251.1,30.8213203435596)) ;
#84735 = CARTESIAN_POINT('Origin',(56.7,251.,19.9213203435596)) ;
#84736 = CARTESIAN_POINT('',(56.6,251.,31.8213203435596)) ;
#84737 = CARTESIAN_POINT('',(56.6,251.,19.9213203435596)) ;
#84738 = CARTESIAN_POINT('',(56.5,251.,31.8213203435596)) ;
#84739 = CARTESIAN_POINT('',(55.2,251.,31.8213203435596)) ;
#84740 = CARTESIAN_POINT('',(56.5,251.,19.9213203435596)) ;
#84741 = CARTESIAN_POINT('Origin',(56.6,251.1,19.9213203435596)) ;
#84742 = CARTESIAN_POINT('',(56.7,251.1,31.8213203435596)) ;
#84743 = CARTESIAN_POINT('',(56.7,251.1,19.9213203435596)) ;
#84744 = CARTESIAN_POINT('Origin',(56.6,251.1,31.8213203435596)) ;
#84745 = CARTESIAN_POINT('Origin',(56.7,257.,19.9213203435596)) ;
#84746 = CARTESIAN_POINT('',(56.7,256.9,31.8213203435596)) ;
#84747 = CARTESIAN_POINT('',(56.7,256.9,19.9213203435596)) ;
#84748 = CARTESIAN_POINT('',(56.7,248.191753592594,31.8213203435596)) ;
#84749 = CARTESIAN_POINT('Origin',(56.8,256.9,19.9213203435596)) ;
#84750 = CARTESIAN_POINT('',(56.8,257.,31.8213203435596)) ;
#84751 = CARTESIAN_POINT('',(56.8,257.,19.9213203435596)) ;
#84752 = CARTESIAN_POINT('Origin',(56.8,256.9,31.8213203435596)) ;
#84753 = CARTESIAN_POINT('Origin',(59.1,257.,19.9213203435596)) ;
#84754 = CARTESIAN_POINT('',(59.,257.,31.8213203435596)) ;
#84755 = CARTESIAN_POINT('',(59.,257.,19.9213203435596)) ;
#84756 = CARTESIAN_POINT('',(56.4,257.,31.8213203435596)) ;
#84757 = CARTESIAN_POINT('Origin',(59.,256.9,19.9213203435596)) ;
#84758 = CARTESIAN_POINT('',(59.1,256.9,31.8213203435596)) ;
#84759 = CARTESIAN_POINT('',(59.1,256.9,19.9213203435596)) ;
#84760 = CARTESIAN_POINT('Origin',(59.,256.9,31.8213203435596)) ;
#84761 = CARTESIAN_POINT('Origin',(59.1,251.,19.9213203435596)) ;
#84762 = CARTESIAN_POINT('',(59.1,251.1,31.8213203435596)) ;
#84763 = CARTESIAN_POINT('',(59.1,251.1,19.9213203435596)) ;
#84764 = CARTESIAN_POINT('',(59.1,245.191753592594,31.8213203435596)) ;
#84765 = CARTESIAN_POINT('Origin',(59.2,251.1,19.9213203435596)) ;
#84766 = CARTESIAN_POINT('',(59.2,251.,31.8213203435596)) ;
#84767 = CARTESIAN_POINT('',(59.2,251.,19.9213203435596)) ;
#84768 = CARTESIAN_POINT('Origin',(59.2,251.1,31.8213203435596)) ;
#84769 = CARTESIAN_POINT('Origin',(59.4,251.,19.9213203435596)) ;
#84770 = CARTESIAN_POINT('',(59.3,251.,31.8213203435596)) ;
#84771 = CARTESIAN_POINT('',(59.3,251.,19.9213203435596)) ;
#84772 = CARTESIAN_POINT('',(56.55,251.,31.8213203435596)) ;
#84773 = CARTESIAN_POINT('Origin',(62.4573593128808,234.691753592594,30.8213203435596)) ;
#84774 = CARTESIAN_POINT('Origin',(62.4573593128808,230.1,30.8213203435596)) ;
#84775 = CARTESIAN_POINT('Origin',(58.1786796564404,230.1,30.8213203435596)) ;
#84776 = CARTESIAN_POINT('',(62.5573593128808,230.,30.8213203435596)) ;
#84777 = CARTESIAN_POINT('Origin',(62.5573593128808,230.1,30.8213203435596)) ;
#84778 = CARTESIAN_POINT('',(58.1786796564404,230.,30.8213203435596)) ;
#84779 = CARTESIAN_POINT('Origin',(62.4573593128808,230.1,30.8213203435596)) ;
#84780 = CARTESIAN_POINT('Origin',(62.5573593128808,229.9,30.8213203435596)) ;
#84781 = CARTESIAN_POINT('',(62.6573593128808,229.9,30.8213203435596)) ;
#84782 = CARTESIAN_POINT('Origin',(62.7573593128808,229.9,30.8213203435596)) ;
#84783 = CARTESIAN_POINT('Origin',(62.5573593128808,229.9,30.8213203435596)) ;
#84784 = CARTESIAN_POINT('Origin',(62.4573593128808,230.1,30.8213203435596)) ;
#84785 = CARTESIAN_POINT('Origin',(62.6573593128808,230.,19.9213203435596)) ;
#84786 = CARTESIAN_POINT('',(62.5573593128808,230.,19.9213203435596)) ;
#84787 = CARTESIAN_POINT('Origin',(59.8573593128808,237.691753592594,30.8213203435596)) ;
#84788 = CARTESIAN_POINT('',(59.9573593128808,237.691753592594,30.8213203435596)) ;
#84789 = CARTESIAN_POINT('Origin',(59.7573593128808,229.9,30.8213203435596)) ;
#84790 = CARTESIAN_POINT('',(59.6573593128808,229.9,30.8213203435596)) ;
#84791 = CARTESIAN_POINT('Origin',(59.7573593128808,229.9,30.8213203435596)) ;
#84792 = CARTESIAN_POINT('Origin',(59.5573593128808,229.9,30.8213203435596)) ;
#84793 = CARTESIAN_POINT('Origin',(59.9573593128808,236.,19.9213203435596)) ;
#84794 = CARTESIAN_POINT('Origin',(55.8286796564404,237.9,30.8213203435596)) ;
#84795 = CARTESIAN_POINT('',(62.1159379566435,238.,30.8213203435596)) ;
#84796 = CARTESIAN_POINT('',(55.8286796564404,238.,30.8213203435596)) ;
#84797 = CARTESIAN_POINT('Origin',(62.1159379566435,237.9,30.8213203435596)) ;
#84798 = CARTESIAN_POINT('Origin',(62.1159379566435,238.1,30.8213203435596)) ;
#84799 = CARTESIAN_POINT('',(62.1866486347621,238.029289321881,30.8213203435596)) ;
#84800 = CARTESIAN_POINT('Origin',(62.2573593128808,237.958578643763,30.8213203435596)) ;
#84801 = CARTESIAN_POINT('Origin',(62.1159379566435,238.1,30.8213203435596)) ;
#84802 = CARTESIAN_POINT('Origin',(60.6596069590762,236.360826289958,30.8213203435596)) ;
#84803 = CARTESIAN_POINT('',(62.9280699909994,238.770710678119,30.8213203435596)) ;
#84804 = CARTESIAN_POINT('Origin',(62.998780669118,238.7,30.8213203435596)) ;
#84805 = CARTESIAN_POINT('',(60.5888962809576,236.431536968077,30.8213203435596)) ;
#84806 = CARTESIAN_POINT('Origin',(62.8573593128807,238.841421356237,30.8213203435596)) ;
#84807 = CARTESIAN_POINT('',(62.9573593128807,238.841421356237,30.8213203435596)) ;
#84808 = CARTESIAN_POINT('Origin',(63.0573593128808,238.841421356237,30.8213203435596)) ;
#84809 = CARTESIAN_POINT('Origin',(62.8573593128807,238.841421356237,30.8213203435596)) ;
#84810 = CARTESIAN_POINT('Origin',(63.0573593128807,238.691753592594,30.8213203435596)) ;
#84811 = CARTESIAN_POINT('',(62.9573593128807,242.158578643763,30.8213203435596)) ;
#84812 = CARTESIAN_POINT('Origin',(63.0573593128807,242.158578643763,30.8213203435596)) ;
#84813 = CARTESIAN_POINT('',(62.9573593128807,238.691753592594,30.8213203435596)) ;
#84814 = CARTESIAN_POINT('Origin',(62.8573593128807,242.158578643763,30.8213203435596)) ;
#84815 = CARTESIAN_POINT('',(62.9280699909994,242.229289321881,30.8213203435596)) ;
#84816 = CARTESIAN_POINT('Origin',(62.9987806691181,242.3,30.8213203435596)) ;
#84817 = CARTESIAN_POINT('Origin',(62.8573593128807,242.158578643763,30.8213203435596)) ;
#84818 = CARTESIAN_POINT('Origin',(61.2178533664821,244.080927302636,30.8213203435596)) ;
#84819 = CARTESIAN_POINT('',(62.1866486347621,242.970710678119,30.8213203435596)) ;
#84820 = CARTESIAN_POINT('Origin',(62.2573593128808,243.041421356237,30.8213203435596)) ;
#84821 = CARTESIAN_POINT('',(61.1471426883634,244.010216624517,30.8213203435596)) ;
#84822 = CARTESIAN_POINT('Origin',(62.1159379566435,242.9,30.8213203435596)) ;
#84823 = CARTESIAN_POINT('',(62.1159379566435,243.,30.8213203435596)) ;
#84824 = CARTESIAN_POINT('Origin',(62.1159379566435,243.1,30.8213203435596)) ;
#84825 = CARTESIAN_POINT('Origin',(62.1159379566435,242.9,30.8213203435596)) ;
#84826 = CARTESIAN_POINT('Origin',(58.3286796564404,243.1,30.8213203435596)) ;
#84827 = CARTESIAN_POINT('',(58.3286796564404,243.,30.8213203435596)) ;
#84828 = CARTESIAN_POINT('Origin',(62.9573593128807,243.,19.9213203435596)) ;
#84829 = CARTESIAN_POINT('',(62.1159379566435,243.,31.8213203435596)) ;
#84830 = CARTESIAN_POINT('',(62.1159379566435,243.,19.9213203435596)) ;
#84831 = CARTESIAN_POINT('',(58.3286796564404,243.,31.8213203435596)) ;
#84832 = CARTESIAN_POINT('Origin',(62.1159379566435,242.9,19.9213203435596)) ;
#84833 = CARTESIAN_POINT('',(62.1866486347621,242.970710678119,31.8213203435596)) ;
#84834 = CARTESIAN_POINT('',(62.1866486347621,242.970710678119,19.9213203435596)) ;
#84835 = CARTESIAN_POINT('Origin',(62.1159379566435,242.9,31.8213203435596)) ;
#84836 = CARTESIAN_POINT('Origin',(62.5573593128807,242.6,19.9213203435596)) ;
#84837 = CARTESIAN_POINT('',(62.9280699909994,242.229289321881,31.8213203435596)) ;
#84838 = CARTESIAN_POINT('',(62.9280699909994,242.229289321881,19.9213203435596)) ;
#84839 = CARTESIAN_POINT('',(61.1471426883634,244.010216624517,31.8213203435596)) ;
#84840 = CARTESIAN_POINT('Origin',(62.8573593128807,242.158578643763,19.9213203435596)) ;
#84841 = CARTESIAN_POINT('',(62.9573593128807,242.158578643763,31.8213203435596)) ;
#84842 = CARTESIAN_POINT('',(62.9573593128807,242.158578643763,19.9213203435596)) ;
#84843 = CARTESIAN_POINT('Origin',(62.8573593128807,242.158578643763,31.8213203435596)) ;
#84844 = CARTESIAN_POINT('Origin',(62.9573593128807,238.,19.9213203435596)) ;
#84845 = CARTESIAN_POINT('',(62.9573593128807,238.841421356237,31.8213203435596)) ;
#84846 = CARTESIAN_POINT('',(62.9573593128807,238.841421356237,19.9213203435596)) ;
#84847 = CARTESIAN_POINT('',(62.9573593128807,238.691753592594,31.8213203435596)) ;
#84848 = CARTESIAN_POINT('Origin',(62.8573593128807,238.841421356237,19.9213203435596)) ;
#84849 = CARTESIAN_POINT('',(62.9280699909994,238.770710678119,31.8213203435596)) ;
#84850 = CARTESIAN_POINT('',(62.9280699909994,238.770710678119,19.9213203435596)) ;
#84851 = CARTESIAN_POINT('Origin',(62.8573593128807,238.841421356237,31.8213203435596)) ;
#84852 = CARTESIAN_POINT('Origin',(62.5573593128807,238.4,19.9213203435596)) ;
#84853 = CARTESIAN_POINT('',(62.1866486347621,238.029289321881,31.8213203435596)) ;
#84854 = CARTESIAN_POINT('',(62.1866486347621,238.029289321881,19.9213203435596)) ;
#84855 = CARTESIAN_POINT('',(60.5888962809576,236.431536968077,31.8213203435596)) ;
#84856 = CARTESIAN_POINT('Origin',(62.1159379566435,238.1,19.9213203435596)) ;
#84857 = CARTESIAN_POINT('',(62.1159379566435,238.,31.8213203435596)) ;
#84858 = CARTESIAN_POINT('',(62.1159379566435,238.,19.9213203435596)) ;
#84859 = CARTESIAN_POINT('Origin',(62.1159379566435,238.1,31.8213203435596)) ;
#84860 = CARTESIAN_POINT('Origin',(57.9573593128808,238.,19.9213203435596)) ;
#84861 = CARTESIAN_POINT('',(55.8286796564404,238.,31.8213203435596)) ;
#84862 = CARTESIAN_POINT('Origin',(59.7573593128808,229.9,19.9213203435596)) ;
#84863 = CARTESIAN_POINT('',(59.6573593128808,229.9,19.9213203435596)) ;
#84864 = CARTESIAN_POINT('Origin',(62.5573593128808,227.1,30.8213203435596)) ;
#84865 = CARTESIAN_POINT('',(62.5573593128808,227.,30.8213203435596)) ;
#84866 = CARTESIAN_POINT('Origin',(62.5573593128808,226.9,30.8213203435596)) ;
#84867 = CARTESIAN_POINT('',(62.6573593128808,227.1,30.8213203435596)) ;
#84868 = CARTESIAN_POINT('Origin',(62.5573593128808,227.1,30.8213203435596)) ;
#84869 = CARTESIAN_POINT('Origin',(62.7573593128808,227.1,30.8213203435596)) ;
#84870 = CARTESIAN_POINT('Origin',(59.6573593128808,227.,19.9213203435596)) ;
#84871 = CARTESIAN_POINT('',(59.7573593128808,227.,30.8213203435596)) ;
#84872 = CARTESIAN_POINT('',(56.6786796564404,227.,30.8213203435596)) ;
#84873 = CARTESIAN_POINT('',(59.7573593128808,227.,31.8213203435596)) ;
#84874 = CARTESIAN_POINT('',(59.7573593128808,227.,19.9213203435596)) ;
#84875 = CARTESIAN_POINT('',(62.5573593128808,227.,31.8213203435596)) ;
#84876 = CARTESIAN_POINT('',(56.6786796564404,227.,31.8213203435596)) ;
#84877 = CARTESIAN_POINT('',(62.5573593128808,227.,19.9213203435596)) ;
#84878 = CARTESIAN_POINT('Origin',(62.5573593128808,229.9,31.8213203435596)) ;
#84879 = CARTESIAN_POINT('',(62.6573593128808,229.9,31.8213203435596)) ;
#84880 = CARTESIAN_POINT('Origin',(62.5573593128808,229.9,31.8213203435596)) ;
#84881 = CARTESIAN_POINT('Origin',(62.7573593128808,229.9,31.8213203435596)) ;
#84882 = CARTESIAN_POINT('Origin',(62.5573593128808,229.9,19.9213203435596)) ;
#84883 = CARTESIAN_POINT('',(62.6573593128808,229.9,19.9213203435596)) ;
#84884 = CARTESIAN_POINT('Origin',(59.7573593128808,227.1,31.8213203435596)) ;
#84885 = CARTESIAN_POINT('Origin',(59.7573593128808,226.9,31.8213203435596)) ;
#84886 = CARTESIAN_POINT('',(59.6573593128808,227.1,31.8213203435596)) ;
#84887 = CARTESIAN_POINT('Origin',(59.7573593128808,227.1,31.8213203435596)) ;
#84888 = CARTESIAN_POINT('Origin',(59.5573593128808,227.1,31.8213203435596)) ;
#84889 = CARTESIAN_POINT('Origin',(62.5573593128808,227.1,31.8213203435596)) ;
#84890 = CARTESIAN_POINT('',(62.6573593128808,227.1,31.8213203435596)) ;
#84891 = CARTESIAN_POINT('Origin',(62.7573593128808,227.1,31.8213203435596)) ;
#84892 = CARTESIAN_POINT('Origin',(62.5573593128808,227.1,31.8213203435596)) ;
#84893 = CARTESIAN_POINT('Origin',(62.5573593128808,226.9,31.8213203435596)) ;
#84894 = CARTESIAN_POINT('Origin',(62.7573593128808,233.191753592594,31.8213203435596)) ;
#84895 = CARTESIAN_POINT('',(62.6573593128808,233.191753592594,31.8213203435596)) ;
#84896 = CARTESIAN_POINT('Origin',(62.5573593128808,227.1,19.9213203435596)) ;
#84897 = CARTESIAN_POINT('',(62.6573593128808,227.1,19.9213203435596)) ;
#84898 = CARTESIAN_POINT('Origin',(56.6786796564404,226.9,31.8213203435596)) ;
#84899 = CARTESIAN_POINT('Origin',(59.7573593128808,227.1,30.8213203435596)) ;
#84900 = CARTESIAN_POINT('',(59.6573593128808,227.1,30.8213203435596)) ;
#84901 = CARTESIAN_POINT('Origin',(59.7573593128808,227.1,30.8213203435596)) ;
#84902 = CARTESIAN_POINT('Origin',(59.7573593128808,226.9,30.8213203435596)) ;
#84903 = CARTESIAN_POINT('Origin',(59.5573593128808,227.1,30.8213203435596)) ;
#84904 = CARTESIAN_POINT('Origin',(56.6786796564404,226.9,30.8213203435596)) ;
#84905 = CARTESIAN_POINT('Origin',(59.5573593128808,234.691753592594,30.8213203435596)) ;
#84906 = CARTESIAN_POINT('',(59.6573593128808,234.691753592594,30.8213203435596)) ;
#84907 = CARTESIAN_POINT('Origin',(59.7573593128808,227.1,19.9213203435596)) ;
#84908 = CARTESIAN_POINT('',(59.6573593128808,227.1,19.9213203435596)) ;
#84909 = CARTESIAN_POINT('Origin',(59.5573593128808,234.691753592594,31.8213203435596)) ;
#84910 = CARTESIAN_POINT('',(59.6573593128808,234.691753592594,31.8213203435596)) ;
#84911 = CARTESIAN_POINT('Origin',(62.6573593128808,227.,19.9213203435596)) ;
#84912 = CARTESIAN_POINT('',(62.6573593128808,233.191753592594,30.8213203435596)) ;
#84913 = CARTESIAN_POINT('Origin',(62.7573593128808,233.191753592594,30.8213203435596)) ;
#84914 = CARTESIAN_POINT('Origin',(64.4999999999999,248.1,30.8213203435596)) ;
#84915 = CARTESIAN_POINT('',(64.4999999999999,248.,30.8213203435596)) ;
#84916 = CARTESIAN_POINT('Origin',(64.4999999999999,247.9,30.8213203435596)) ;
#84917 = CARTESIAN_POINT('',(64.3999999999999,248.1,30.8213203435596)) ;
#84918 = CARTESIAN_POINT('Origin',(64.3,248.1,30.8213203435596)) ;
#84919 = CARTESIAN_POINT('Origin',(64.4999999999999,248.1,30.8213203435596)) ;
#84920 = CARTESIAN_POINT('Origin',(67.3,248.1,30.8213203435596)) ;
#84921 = CARTESIAN_POINT('',(67.3,248.,30.8213203435596)) ;
#84922 = CARTESIAN_POINT('Origin',(67.3,247.9,30.8213203435596)) ;
#84923 = CARTESIAN_POINT('',(67.4,248.1,30.8213203435596)) ;
#84924 = CARTESIAN_POINT('Origin',(67.3,248.1,30.8213203435596)) ;
#84925 = CARTESIAN_POINT('Origin',(67.5,248.1,30.8213203435596)) ;
#84926 = CARTESIAN_POINT('Origin',(64.3999999999999,248.,19.9213203435596)) ;
#84927 = CARTESIAN_POINT('',(59.05,248.,30.8213203435596)) ;
#84928 = CARTESIAN_POINT('',(64.4999999999999,248.,31.8213203435596)) ;
#84929 = CARTESIAN_POINT('',(64.4999999999999,248.,19.9213203435596)) ;
#84930 = CARTESIAN_POINT('',(67.3,248.,31.8213203435596)) ;
#84931 = CARTESIAN_POINT('',(59.05,248.,31.8213203435596)) ;
#84932 = CARTESIAN_POINT('',(67.3,248.,19.9213203435596)) ;
#84933 = CARTESIAN_POINT('Origin',(64.8,256.9,31.8213203435596)) ;
#84934 = CARTESIAN_POINT('Origin',(64.8,257.1,31.8213203435596)) ;
#84935 = CARTESIAN_POINT('Origin',(64.6,256.9,31.8213203435596)) ;
#84936 = CARTESIAN_POINT('Origin',(67.,256.9,31.8213203435596)) ;
#84937 = CARTESIAN_POINT('Origin',(67.,257.1,31.8213203435596)) ;
#84938 = CARTESIAN_POINT('Origin',(67.2,256.9,31.8213203435596)) ;
#84939 = CARTESIAN_POINT('Origin',(60.4,257.1,31.8213203435596)) ;
#84940 = CARTESIAN_POINT('Origin',(64.6,251.1,31.8213203435596)) ;
#84941 = CARTESIAN_POINT('Origin',(64.6,251.1,31.8213203435596)) ;
#84942 = CARTESIAN_POINT('Origin',(64.6,251.1,31.8213203435596)) ;
#84943 = CARTESIAN_POINT('Origin',(67.2,251.1,31.8213203435596)) ;
#84944 = CARTESIAN_POINT('Origin',(67.2,251.1,31.8213203435596)) ;
#84945 = CARTESIAN_POINT('Origin',(67.2,251.1,31.8213203435596)) ;
#84946 = CARTESIAN_POINT('Origin',(67.2,245.191753592594,31.8213203435596)) ;
#84947 = CARTESIAN_POINT('Origin',(64.5,250.9,31.8213203435596)) ;
#84948 = CARTESIAN_POINT('',(64.3999999999999,250.9,31.8213203435596)) ;
#84949 = CARTESIAN_POINT('Origin',(64.3,250.9,31.8213203435596)) ;
#84950 = CARTESIAN_POINT('Origin',(64.5,250.9,31.8213203435596)) ;
#84951 = CARTESIAN_POINT('Origin',(64.5,251.1,31.8213203435596)) ;
#84952 = CARTESIAN_POINT('Origin',(67.3,250.9,31.8213203435596)) ;
#84953 = CARTESIAN_POINT('Origin',(67.3,251.1,31.8213203435596)) ;
#84954 = CARTESIAN_POINT('',(67.4,250.9,31.8213203435596)) ;
#84955 = CARTESIAN_POINT('Origin',(67.3,250.9,31.8213203435596)) ;
#84956 = CARTESIAN_POINT('Origin',(67.5,250.9,31.8213203435596)) ;
#84957 = CARTESIAN_POINT('Origin',(60.55,251.1,31.8213203435596)) ;
#84958 = CARTESIAN_POINT('Origin',(67.3,250.9,19.9213203435596)) ;
#84959 = CARTESIAN_POINT('',(67.4,250.9,19.9213203435596)) ;
#84960 = CARTESIAN_POINT('Origin',(64.4999999999999,248.1,31.8213203435596)) ;
#84961 = CARTESIAN_POINT('Origin',(64.4999999999999,247.9,31.8213203435596)) ;
#84962 = CARTESIAN_POINT('',(64.3999999999999,248.1,31.8213203435596)) ;
#84963 = CARTESIAN_POINT('Origin',(64.4999999999999,248.1,31.8213203435596)) ;
#84964 = CARTESIAN_POINT('Origin',(64.3,248.1,31.8213203435596)) ;
#84965 = CARTESIAN_POINT('Origin',(67.3,248.1,31.8213203435596)) ;
#84966 = CARTESIAN_POINT('',(67.4,248.1,31.8213203435596)) ;
#84967 = CARTESIAN_POINT('Origin',(67.5,248.1,31.8213203435596)) ;
#84968 = CARTESIAN_POINT('Origin',(67.3,248.1,31.8213203435596)) ;
#84969 = CARTESIAN_POINT('Origin',(67.3,247.9,31.8213203435596)) ;
#84970 = CARTESIAN_POINT('Origin',(67.5,243.691753592594,31.8213203435596)) ;
#84971 = CARTESIAN_POINT('',(67.4,243.691753592594,31.8213203435596)) ;
#84972 = CARTESIAN_POINT('Origin',(67.3,248.1,19.9213203435596)) ;
#84973 = CARTESIAN_POINT('',(67.4,248.1,19.9213203435596)) ;
#84974 = CARTESIAN_POINT('Origin',(59.05,247.9,31.8213203435596)) ;
#84975 = CARTESIAN_POINT('Origin',(64.4999999999999,248.1,19.9213203435596)) ;
#84976 = CARTESIAN_POINT('',(64.3999999999999,248.1,19.9213203435596)) ;
#84977 = CARTESIAN_POINT('Origin',(64.3,245.191753592594,31.8213203435596)) ;
#84978 = CARTESIAN_POINT('',(64.3999999999999,245.191753592594,31.8213203435596)) ;
#84979 = CARTESIAN_POINT('Origin',(64.5,250.9,19.9213203435596)) ;
#84980 = CARTESIAN_POINT('',(64.3999999999999,250.9,19.9213203435596)) ;
#84981 = CARTESIAN_POINT('Origin',(59.2,251.1,31.8213203435596)) ;
#84982 = CARTESIAN_POINT('Origin',(64.6,248.191753592594,31.8213203435596)) ;
#84983 = CARTESIAN_POINT('Origin',(59.05,247.9,30.8213203435596)) ;
#84984 = CARTESIAN_POINT('Origin',(67.4,248.,19.9213203435596)) ;
#84985 = CARTESIAN_POINT('',(67.4,243.691753592594,30.8213203435596)) ;
#84986 = CARTESIAN_POINT('Origin',(67.5,243.691753592594,30.8213203435596)) ;
#84987 = CARTESIAN_POINT('Origin',(56.5,248.1,30.8213203435596)) ;
#84988 = CARTESIAN_POINT('',(56.5,248.,30.8213203435596)) ;
#84989 = CARTESIAN_POINT('Origin',(56.5,247.9,30.8213203435596)) ;
#84990 = CARTESIAN_POINT('',(56.3999999999999,248.1,30.8213203435596)) ;
#84991 = CARTESIAN_POINT('Origin',(56.3,248.1,30.8213203435596)) ;
#84992 = CARTESIAN_POINT('Origin',(56.5,248.1,30.8213203435596)) ;
#84993 = CARTESIAN_POINT('Origin',(59.3,248.1,30.8213203435596)) ;
#84994 = CARTESIAN_POINT('',(59.3,248.,30.8213203435596)) ;
#84995 = CARTESIAN_POINT('Origin',(59.3,247.9,30.8213203435596)) ;
#84996 = CARTESIAN_POINT('',(59.4,248.1,30.8213203435596)) ;
#84997 = CARTESIAN_POINT('Origin',(59.3,248.1,30.8213203435596)) ;
#84998 = CARTESIAN_POINT('Origin',(59.5,248.1,30.8213203435596)) ;
#84999 = CARTESIAN_POINT('Origin',(56.3999999999999,248.,19.9213203435596)) ;
#85000 = CARTESIAN_POINT('',(55.05,248.,30.8213203435596)) ;
#85001 = CARTESIAN_POINT('',(56.5,248.,31.8213203435596)) ;
#85002 = CARTESIAN_POINT('',(56.5,248.,19.9213203435596)) ;
#85003 = CARTESIAN_POINT('',(59.3,248.,31.8213203435596)) ;
#85004 = CARTESIAN_POINT('',(55.05,248.,31.8213203435596)) ;
#85005 = CARTESIAN_POINT('',(59.3,248.,19.9213203435596)) ;
#85006 = CARTESIAN_POINT('Origin',(56.8,256.9,31.8213203435596)) ;
#85007 = CARTESIAN_POINT('Origin',(56.6,256.9,31.8213203435596)) ;
#85008 = CARTESIAN_POINT('Origin',(56.8,257.1,31.8213203435596)) ;
#85009 = CARTESIAN_POINT('Origin',(56.6,251.1,31.8213203435596)) ;
#85010 = CARTESIAN_POINT('Origin',(56.6,251.1,31.8213203435596)) ;
#85011 = CARTESIAN_POINT('Origin',(56.6,251.1,31.8213203435596)) ;
#85012 = CARTESIAN_POINT('Origin',(56.6,248.191753592594,31.8213203435596)) ;
#85013 = CARTESIAN_POINT('Origin',(59.,256.9,31.8213203435596)) ;
#85014 = CARTESIAN_POINT('Origin',(59.,257.1,31.8213203435596)) ;
#85015 = CARTESIAN_POINT('Origin',(59.2,256.9,31.8213203435596)) ;
#85016 = CARTESIAN_POINT('Origin',(56.4,257.1,31.8213203435596)) ;
#85017 = CARTESIAN_POINT('Origin',(56.5,250.9,31.8213203435596)) ;
#85018 = CARTESIAN_POINT('',(56.3999999999999,250.9,31.8213203435596)) ;
#85019 = CARTESIAN_POINT('Origin',(56.3,250.9,31.8213203435596)) ;
#85020 = CARTESIAN_POINT('Origin',(56.5,250.9,31.8213203435596)) ;
#85021 = CARTESIAN_POINT('Origin',(56.5,251.1,31.8213203435596)) ;
#85022 = CARTESIAN_POINT('Origin',(59.2,251.1,31.8213203435596)) ;
#85023 = CARTESIAN_POINT('Origin',(59.2,251.1,31.8213203435596)) ;
#85024 = CARTESIAN_POINT('Origin',(59.2,251.1,31.8213203435596)) ;
#85025 = CARTESIAN_POINT('Origin',(59.2,245.191753592594,31.8213203435596)) ;
#85026 = CARTESIAN_POINT('Origin',(56.5,248.1,31.8213203435596)) ;
#85027 = CARTESIAN_POINT('Origin',(56.5,247.9,31.8213203435596)) ;
#85028 = CARTESIAN_POINT('',(56.3999999999999,248.1,31.8213203435596)) ;
#85029 = CARTESIAN_POINT('Origin',(56.5,248.1,31.8213203435596)) ;
#85030 = CARTESIAN_POINT('Origin',(56.3,248.1,31.8213203435596)) ;
#85031 = CARTESIAN_POINT('Origin',(59.3,250.9,31.8213203435596)) ;
#85032 = CARTESIAN_POINT('Origin',(59.3,251.1,31.8213203435596)) ;
#85033 = CARTESIAN_POINT('',(59.4,250.9,31.8213203435596)) ;
#85034 = CARTESIAN_POINT('Origin',(59.3,250.9,31.8213203435596)) ;
#85035 = CARTESIAN_POINT('Origin',(59.5,250.9,31.8213203435596)) ;
#85036 = CARTESIAN_POINT('Origin',(56.55,251.1,31.8213203435596)) ;
#85037 = CARTESIAN_POINT('Origin',(59.3,250.9,19.9213203435596)) ;
#85038 = CARTESIAN_POINT('',(59.4,250.9,19.9213203435596)) ;
#85039 = CARTESIAN_POINT('Origin',(59.3,248.1,31.8213203435596)) ;
#85040 = CARTESIAN_POINT('',(59.4,248.1,31.8213203435596)) ;
#85041 = CARTESIAN_POINT('Origin',(59.5,248.1,31.8213203435596)) ;
#85042 = CARTESIAN_POINT('Origin',(59.3,248.1,31.8213203435596)) ;
#85043 = CARTESIAN_POINT('Origin',(59.3,247.9,31.8213203435596)) ;
#85044 = CARTESIAN_POINT('Origin',(59.5,243.691753592594,31.8213203435596)) ;
#85045 = CARTESIAN_POINT('',(59.4,243.691753592594,31.8213203435596)) ;
#85046 = CARTESIAN_POINT('Origin',(59.3,248.1,19.9213203435596)) ;
#85047 = CARTESIAN_POINT('',(59.4,248.1,19.9213203435596)) ;
#85048 = CARTESIAN_POINT('Origin',(55.05,247.9,31.8213203435596)) ;
#85049 = CARTESIAN_POINT('Origin',(56.5,248.1,19.9213203435596)) ;
#85050 = CARTESIAN_POINT('',(56.3999999999999,248.1,19.9213203435596)) ;
#85051 = CARTESIAN_POINT('Origin',(56.3,245.191753592594,31.8213203435596)) ;
#85052 = CARTESIAN_POINT('',(56.3999999999999,245.191753592594,31.8213203435596)) ;
#85053 = CARTESIAN_POINT('Origin',(56.5,250.9,19.9213203435596)) ;
#85054 = CARTESIAN_POINT('',(56.3999999999999,250.9,19.9213203435596)) ;
#85055 = CARTESIAN_POINT('Origin',(55.2,251.1,31.8213203435596)) ;
#85056 = CARTESIAN_POINT('Origin',(55.05,247.9,30.8213203435596)) ;
#85057 = CARTESIAN_POINT('Origin',(59.4,248.,19.9213203435596)) ;
#85058 = CARTESIAN_POINT('',(59.4,243.691753592594,30.8213203435596)) ;
#85059 = CARTESIAN_POINT('Origin',(59.5,243.691753592594,30.8213203435596)) ;
#85060 = CARTESIAN_POINT('Origin',(46.1,248.9,31.8213203435596)) ;
#85061 = CARTESIAN_POINT('',(46.1,249.,31.8213203435596)) ;
#85062 = CARTESIAN_POINT('Origin',(46.1,249.1,31.8213203435596)) ;
#85063 = CARTESIAN_POINT('',(46.2,248.9,31.8213203435596)) ;
#85064 = CARTESIAN_POINT('Origin',(46.1,248.9,31.8213203435596)) ;
#85065 = CARTESIAN_POINT('Origin',(46.3,248.9,31.8213203435596)) ;
#85066 = CARTESIAN_POINT('Origin',(34.3,248.9,31.8213203435596)) ;
#85067 = CARTESIAN_POINT('',(34.2,248.9,31.8213203435596)) ;
#85068 = CARTESIAN_POINT('Origin',(34.1,248.9,31.8213203435596)) ;
#85069 = CARTESIAN_POINT('',(34.3,249.,31.8213203435596)) ;
#85070 = CARTESIAN_POINT('Origin',(34.3,248.9,31.8213203435596)) ;
#85071 = CARTESIAN_POINT('Origin',(34.3,249.1,31.8213203435596)) ;
#85072 = CARTESIAN_POINT('Origin',(26.3,264.9,19.9213203435596)) ;
#85073 = CARTESIAN_POINT('Origin',(26.3,264.9,21.9213203435596)) ;
#85074 = CARTESIAN_POINT('Origin',(26.3,264.9,30.7213203435596)) ;
#85075 = CARTESIAN_POINT('Origin',(26.3,263.8,30.7213203435596)) ;
#85076 = CARTESIAN_POINT('Origin',(26.3,263.8,31.8213203435596)) ;
#85077 = CARTESIAN_POINT('Origin',(26.3,263.8,30.7213203435596)) ;
#85078 = CARTESIAN_POINT('Origin',(26.3,252.191753592594,31.8213203435596)) ;
#85079 = CARTESIAN_POINT('Origin',(26.3,245.6,31.8213203435596)) ;
#85080 = CARTESIAN_POINT('Origin',(26.8,245.6,31.8213203435596)) ;
#85081 = CARTESIAN_POINT('',(26.8,245.,31.8213203435596)) ;
#85082 = CARTESIAN_POINT('Origin',(26.8,245.1,31.8213203435596)) ;
#85083 = CARTESIAN_POINT('Origin',(26.8,245.6,31.8213203435596)) ;
#85084 = CARTESIAN_POINT('Origin',(39.95,245.1,31.8213203435596)) ;
#85085 = CARTESIAN_POINT('',(33.6,245.,31.8213203435596)) ;
#85086 = CARTESIAN_POINT('Origin',(33.6,245.1,31.8213203435596)) ;
#85087 = CARTESIAN_POINT('',(39.95,245.,31.8213203435596)) ;
#85088 = CARTESIAN_POINT('Origin',(33.6,245.6,31.8213203435596)) ;
#85089 = CARTESIAN_POINT('',(34.2,245.6,31.8213203435596)) ;
#85090 = CARTESIAN_POINT('Origin',(34.1,245.6,31.8213203435596)) ;
#85091 = CARTESIAN_POINT('Origin',(33.6,245.6,31.8213203435596)) ;
#85092 = CARTESIAN_POINT('Origin',(34.1000000000001,244.191753592594,31.8213203435596)) ;
#85093 = CARTESIAN_POINT('',(34.2000000000001,244.191753592594,31.8213203435596)) ;
#85094 = CARTESIAN_POINT('Origin',(28.2,264.9,21.9213203435596)) ;
#85095 = CARTESIAN_POINT('Origin',(77.1999999999999,264.9,21.9213203435596)) ;
#85096 = CARTESIAN_POINT('Origin',(79.0999999999999,264.9,21.9213203435596)) ;
#85097 = CARTESIAN_POINT('Origin',(79.0999999999999,264.9,19.9213203435596)) ;
#85098 = CARTESIAN_POINT('Origin',(79.0999999999999,264.9,30.7213203435596)) ;
#85099 = CARTESIAN_POINT('Origin',(79.0999999999999,263.8,30.7213203435596)) ;
#85100 = CARTESIAN_POINT('Origin',(79.0999999999999,263.8,31.8213203435596)) ;
#85101 = CARTESIAN_POINT('Origin',(79.0999999999999,263.8,30.7213203435596)) ;
#85102 = CARTESIAN_POINT('Origin',(79.0999999999999,249.391753592594,31.8213203435596)) ;
#85103 = CARTESIAN_POINT('Origin',(79.0999999999999,259.648528137424,31.8213203435596)) ;
#85104 = CARTESIAN_POINT('Origin',(79.7999999999999,259.648528137424,31.8213203435596)) ;
#85105 = CARTESIAN_POINT('',(79.375735931288,259.224264068712,31.8213203435596)) ;
#85106 = CARTESIAN_POINT('Origin',(79.3050252531694,259.153553390593,31.8213203435596)) ;
#85107 = CARTESIAN_POINT('Origin',(79.7999999999999,259.648528137424,31.8213203435596)) ;
#85108 = CARTESIAN_POINT('Origin',(78.758412525583,259.70016611818,31.8213203435596)) ;
#85109 = CARTESIAN_POINT('',(81.0242640687119,257.575735931288,31.8213203435596)) ;
#85110 = CARTESIAN_POINT('Origin',(80.9535533905932,257.50502525317,31.8213203435596)) ;
#85111 = CARTESIAN_POINT('',(78.8291232037016,259.770876796298,31.8213203435596)) ;
#85112 = CARTESIAN_POINT('Origin',(80.6,257.151471862576,31.8213203435596)) ;
#85113 = CARTESIAN_POINT('',(81.2,257.151471862576,31.8213203435596)) ;
#85114 = CARTESIAN_POINT('Origin',(81.1,257.151471862576,31.8213203435596)) ;
#85115 = CARTESIAN_POINT('Origin',(80.6,257.151471862576,31.8213203435596)) ;
#85116 = CARTESIAN_POINT('Origin',(81.1,242.941753592594,31.8213203435596)) ;
#85117 = CARTESIAN_POINT('',(81.2,247.098386676966,31.8213203435596)) ;
#85118 = CARTESIAN_POINT('Origin',(81.1,247.098386676966,31.8213203435596)) ;
#85119 = CARTESIAN_POINT('',(81.2,242.941753592594,31.8213203435596)) ;
#85120 = CARTESIAN_POINT('Origin',(80.6,247.098386676966,31.8213203435596)) ;
#85121 = CARTESIAN_POINT('',(80.6193548387097,246.498698933037,31.8213203435596)) ;
#85122 = CARTESIAN_POINT('Origin',(80.616129032258,246.598646890358,31.8213203435596)) ;
#85123 = CARTESIAN_POINT('Origin',(80.6,247.098386676966,31.8213203435596)) ;
#85124 = CARTESIAN_POINT('Origin',(80.6999999999999,244.,31.8213203435596)) ;
#85125 = CARTESIAN_POINT('',(78.1999999999999,244.,31.8213203435596)) ;
#85126 = CARTESIAN_POINT('Origin',(78.0999999999999,244.,31.8213203435596)) ;
#85127 = CARTESIAN_POINT('Origin',(80.6999999999999,244.,31.8213203435596)) ;
#85128 = CARTESIAN_POINT('Origin',(78.0999999999999,239.691753592594,31.8213203435596)) ;
#85129 = CARTESIAN_POINT('',(78.1999999999999,240.,31.8213203435596)) ;
#85130 = CARTESIAN_POINT('Origin',(78.0999999999999,240.,31.8213203435596)) ;
#85131 = CARTESIAN_POINT('',(78.1999999999999,239.691753592594,31.8213203435596)) ;
#85132 = CARTESIAN_POINT('Origin',(80.6999999999999,240.,31.8213203435596)) ;
#85133 = CARTESIAN_POINT('',(80.6193548387097,237.501301066963,31.8213203435596)) ;
#85134 = CARTESIAN_POINT('Origin',(80.616129032258,237.401353109641,31.8213203435596)) ;
#85135 = CARTESIAN_POINT('Origin',(80.6999999999999,240.,31.8213203435596)) ;
#85136 = CARTESIAN_POINT('Origin',(80.6,236.901613323034,31.8213203435596)) ;
#85137 = CARTESIAN_POINT('',(81.2,236.901613323034,31.8213203435596)) ;
#85138 = CARTESIAN_POINT('Origin',(81.1,236.901613323034,31.8213203435596)) ;
#85139 = CARTESIAN_POINT('Origin',(80.6,236.901613323034,31.8213203435596)) ;
#85140 = CARTESIAN_POINT('Origin',(81.1,232.568672279644,31.8213203435596)) ;
#85141 = CARTESIAN_POINT('',(81.2,226.002365511524,31.8213203435596)) ;
#85142 = CARTESIAN_POINT('Origin',(81.1,226.002365511524,31.8213203435596)) ;
#85143 = CARTESIAN_POINT('',(81.2,232.568672279644,31.8213203435596)) ;
#85144 = CARTESIAN_POINT('Origin',(80.6,226.002365511524,31.8213203435596)) ;
#85145 = CARTESIAN_POINT('',(81.0242640687119,225.578101442812,31.8213203435596)) ;
#85146 = CARTESIAN_POINT('Origin',(80.9535533905933,225.64881212093,31.8213203435596)) ;
#85147 = CARTESIAN_POINT('Origin',(80.6,226.002365511524,31.8213203435596)) ;
#85148 = CARTESIAN_POINT('Origin',(77.061706774654,221.756965504991,31.8213203435596)) ;
#85149 = CARTESIAN_POINT('',(80.1757359312881,224.729573305388,31.8213203435596)) ;
#85150 = CARTESIAN_POINT('Origin',(80.1050252531695,224.800283983507,31.8213203435596)) ;
#85151 = CARTESIAN_POINT('',(77.1324174527726,221.686254826872,31.8213203435596)) ;
#85152 = CARTESIAN_POINT('Origin',(80.6000000000001,224.305309236676,31.8213203435596)) ;
#85153 = CARTESIAN_POINT('',(80.0000000000001,224.305309236676,31.8213203435596)) ;
#85154 = CARTESIAN_POINT('Origin',(79.9000000000001,224.305309236676,31.8213203435596)) ;
#85155 = CARTESIAN_POINT('Origin',(80.6000000000001,224.305309236676,31.8213203435596)) ;
#85156 = CARTESIAN_POINT('Origin',(79.9,228.575260777783,31.8213203435596)) ;
#85157 = CARTESIAN_POINT('',(80.0000000000001,217.767014370377,31.8213203435596)) ;
#85158 = CARTESIAN_POINT('Origin',(79.9000000000001,217.767014370377,31.8213203435596)) ;
#85159 = CARTESIAN_POINT('',(80.,228.575260777783,31.8213203435596)) ;
#85160 = CARTESIAN_POINT('Origin',(76.0000000000001,217.767014370377,31.8213203435596)) ;
#85161 = CARTESIAN_POINT('',(75.3054072893324,213.827783358328,31.8213203435596)) ;
#85162 = CARTESIAN_POINT('Origin',(75.3227721070991,213.926264133629,31.8213203435596)) ;
#85163 = CARTESIAN_POINT('Origin',(76.0000000000001,217.767014370377,31.8213203435596)) ;
#85164 = CARTESIAN_POINT('Origin',(56.086380506565,217.318158984277,31.8213203435596)) ;
#85165 = CARTESIAN_POINT('',(63.7885177058986,215.858521725728,31.8213203435596)) ;
#85166 = CARTESIAN_POINT('Origin',(63.8058825236653,215.957002501029,31.8213203435596)) ;
#85167 = CARTESIAN_POINT('',(56.0690156887983,217.219678208976,31.8213203435596)) ;
#85168 = CARTESIAN_POINT('Origin',(64.4831104165663,219.797752737776,31.8213203435596)) ;
#85169 = CARTESIAN_POINT('',(61.2065022394103,217.503446992372,31.8213203435596)) ;
#85170 = CARTESIAN_POINT('Origin',(61.2884174438392,217.560804636007,31.8213203435596)) ;
#85171 = CARTESIAN_POINT('Origin',(64.4831104165663,219.797752737776,31.8213203435596)) ;
#85172 = CARTESIAN_POINT('Origin',(52.2889313872861,230.413402709377,31.8213203435596)) ;
#85173 = CARTESIAN_POINT('',(56.6807511357248,223.966889410112,31.8213203435596)) ;
#85174 = CARTESIAN_POINT('Origin',(56.7626663401537,224.024247053747,31.8213203435596)) ;
#85175 = CARTESIAN_POINT('',(52.2070161828572,230.356045065742,31.8213203435596)) ;
#85176 = CARTESIAN_POINT('Origin',(59.9573593128808,226.261195155516,31.8213203435596)) ;
#85177 = CARTESIAN_POINT('',(55.9573593128808,226.261195155516,31.8213203435596)) ;
#85178 = CARTESIAN_POINT('Origin',(56.0573593128808,226.261195155516,31.8213203435596)) ;
#85179 = CARTESIAN_POINT('Origin',(59.9573593128808,226.261195155516,31.8213203435596)) ;
#85180 = CARTESIAN_POINT('Origin',(56.0573593128807,242.191753592594,31.8213203435596)) ;
#85181 = CARTESIAN_POINT('',(55.9573593128808,244.4,31.8213203435596)) ;
#85182 = CARTESIAN_POINT('Origin',(56.0573593128807,244.4,31.8213203435596)) ;
#85183 = CARTESIAN_POINT('',(55.9573593128808,242.191753592594,31.8213203435596)) ;
#85184 = CARTESIAN_POINT('Origin',(55.3573593128808,244.4,31.8213203435596)) ;
#85185 = CARTESIAN_POINT('',(55.3573593128808,245.,31.8213203435596)) ;
#85186 = CARTESIAN_POINT('Origin',(55.3573593128808,245.1,31.8213203435596)) ;
#85187 = CARTESIAN_POINT('Origin',(55.3573593128808,244.4,31.8213203435596)) ;
#85188 = CARTESIAN_POINT('Origin',(39.95,245.1,31.8213203435596)) ;
#85189 = CARTESIAN_POINT('',(46.8,245.,31.8213203435596)) ;
#85190 = CARTESIAN_POINT('Origin',(46.8,245.1,31.8213203435596)) ;
#85191 = CARTESIAN_POINT('',(39.95,245.,31.8213203435596)) ;
#85192 = CARTESIAN_POINT('Origin',(46.8,245.6,31.8213203435596)) ;
#85193 = CARTESIAN_POINT('',(46.2,245.6,31.8213203435596)) ;
#85194 = CARTESIAN_POINT('Origin',(46.2999999999999,245.6,31.8213203435596)) ;
#85195 = CARTESIAN_POINT('Origin',(46.8,245.6,31.8213203435596)) ;
#85196 = CARTESIAN_POINT('Origin',(46.2999999999999,242.191753592594,31.8213203435596)) ;
#85197 = CARTESIAN_POINT('',(46.1999999999999,242.191753592594,31.8213203435596)) ;
#85198 = CARTESIAN_POINT('Origin',(34.1,248.9,30.8213203435596)) ;
#85199 = CARTESIAN_POINT('',(34.3,249.,30.8213203435596)) ;
#85200 = CARTESIAN_POINT('',(34.2,248.9,30.8213203435596)) ;
#85201 = CARTESIAN_POINT('Origin',(34.3,248.9,30.8213203435596)) ;
#85202 = CARTESIAN_POINT('Origin',(34.1,248.9,30.8213203435596)) ;
#85203 = CARTESIAN_POINT('Origin',(34.1,249.,30.8213203435596)) ;
#85204 = CARTESIAN_POINT('Origin',(34.3,248.9,19.9213203435596)) ;
#85205 = CARTESIAN_POINT('',(34.2,248.9,19.9213203435596)) ;
#85206 = CARTESIAN_POINT('',(34.3,249.,19.9213203435596)) ;
#85207 = CARTESIAN_POINT('Origin',(49.95,249.1,31.8213203435596)) ;
#85208 = CARTESIAN_POINT('',(49.95,249.,31.8213203435596)) ;
#85209 = CARTESIAN_POINT('Origin',(46.1,248.9,19.9213203435596)) ;
#85210 = CARTESIAN_POINT('',(46.1,249.,30.8213203435596)) ;
#85211 = CARTESIAN_POINT('',(46.2,248.9,30.8213203435596)) ;
#85212 = CARTESIAN_POINT('Origin',(46.1,248.9,30.8213203435596)) ;
#85213 = CARTESIAN_POINT('',(46.2,248.9,19.9213203435596)) ;
#85214 = CARTESIAN_POINT('',(46.1,249.,19.9213203435596)) ;
#85215 = CARTESIAN_POINT('Origin',(46.3,248.9,30.8213203435596)) ;
#85216 = CARTESIAN_POINT('Origin',(46.3,248.9,30.8213203435596)) ;
#85217 = CARTESIAN_POINT('Origin',(46.3,249.,30.8213203435596)) ;
#85218 = CARTESIAN_POINT('Origin',(66.4499999999999,263.8,30.7213203435596)) ;
#85219 = CARTESIAN_POINT('',(77.7056259120663,264.647498436458,31.5708769339063)) ;
#85220 = CARTESIAN_POINT('Origin',(78.2,263.8,30.7213203435596)) ;
#85221 = CARTESIAN_POINT('Origin',(78.2,263.8,30.7213203435596)) ;
#85222 = CARTESIAN_POINT('Origin',(81.2,257.4,19.9213203435596)) ;
#85223 = CARTESIAN_POINT('',(81.0242640687119,257.575735931288,30.8213203435596)) ;
#85224 = CARTESIAN_POINT('',(81.0242640687119,257.575735931288,19.9213203435596)) ;
#85225 = CARTESIAN_POINT('',(79.375735931288,259.224264068712,30.8213203435596)) ;
#85226 = CARTESIAN_POINT('',(78.8291232037016,259.770876796298,30.8213203435596)) ;
#85227 = CARTESIAN_POINT('',(79.375735931288,259.224264068712,19.9213203435596)) ;
#85228 = CARTESIAN_POINT('Origin',(80.6,257.151471862576,19.9213203435596)) ;
#85229 = CARTESIAN_POINT('',(81.2,257.151471862576,30.8213203435596)) ;
#85230 = CARTESIAN_POINT('',(81.2,257.151471862576,19.9213203435596)) ;
#85231 = CARTESIAN_POINT('Origin',(80.6,257.151471862576,30.8213203435596)) ;
#85232 = CARTESIAN_POINT('Origin',(81.2,246.5,19.9213203435596)) ;
#85233 = CARTESIAN_POINT('',(81.2,247.098386676966,30.8213203435596)) ;
#85234 = CARTESIAN_POINT('',(81.2,247.098386676966,19.9213203435596)) ;
#85235 = CARTESIAN_POINT('',(81.2,242.941753592594,30.8213203435596)) ;
#85236 = CARTESIAN_POINT('Origin',(80.6,247.098386676966,19.9213203435596)) ;
#85237 = CARTESIAN_POINT('',(80.6193548387097,246.498698933037,30.8213203435596)) ;
#85238 = CARTESIAN_POINT('',(80.6193548387097,246.498698933037,19.9213203435596)) ;
#85239 = CARTESIAN_POINT('Origin',(80.6,247.098386676966,30.8213203435596)) ;
#85240 = CARTESIAN_POINT('Origin',(80.6999999999999,244.,19.9213203435596)) ;
#85241 = CARTESIAN_POINT('',(78.1999999999999,244.,30.8213203435596)) ;
#85242 = CARTESIAN_POINT('',(78.1999999999999,244.,19.9213203435596)) ;
#85243 = CARTESIAN_POINT('Origin',(80.6999999999999,244.,30.8213203435596)) ;
#85244 = CARTESIAN_POINT('Origin',(78.1999999999999,240.,19.9213203435596)) ;
#85245 = CARTESIAN_POINT('',(78.1999999999999,240.,30.8213203435596)) ;
#85246 = CARTESIAN_POINT('',(78.1999999999999,240.,19.9213203435596)) ;
#85247 = CARTESIAN_POINT('',(78.1999999999999,239.691753592594,30.8213203435596)) ;
#85248 = CARTESIAN_POINT('Origin',(80.6999999999999,240.,19.9213203435596)) ;
#85249 = CARTESIAN_POINT('',(80.6193548387097,237.501301066963,30.8213203435596)) ;
#85250 = CARTESIAN_POINT('',(80.6193548387097,237.501301066963,19.9213203435596)) ;
#85251 = CARTESIAN_POINT('Origin',(80.6999999999999,240.,30.8213203435596)) ;
#85252 = CARTESIAN_POINT('Origin',(80.6,236.901613323034,19.9213203435596)) ;
#85253 = CARTESIAN_POINT('',(81.2,236.901613323034,30.8213203435596)) ;
#85254 = CARTESIAN_POINT('',(81.2,236.901613323034,19.9213203435596)) ;
#85255 = CARTESIAN_POINT('Origin',(80.6,236.901613323034,30.8213203435596)) ;
#85256 = CARTESIAN_POINT('Origin',(81.2,225.7538373741,19.9213203435596)) ;
#85257 = CARTESIAN_POINT('',(81.2,226.002365511524,30.8213203435596)) ;
#85258 = CARTESIAN_POINT('',(81.2,226.002365511524,19.9213203435596)) ;
#85259 = CARTESIAN_POINT('',(81.2,232.568672279644,30.8213203435596)) ;
#85260 = CARTESIAN_POINT('Origin',(80.6,226.002365511524,19.9213203435596)) ;
#85261 = CARTESIAN_POINT('',(81.0242640687119,225.578101442812,30.8213203435596)) ;
#85262 = CARTESIAN_POINT('',(81.0242640687119,225.578101442812,19.9213203435596)) ;
#85263 = CARTESIAN_POINT('Origin',(80.6,226.002365511524,30.8213203435596)) ;
#85264 = CARTESIAN_POINT('Origin',(80.0000000000001,224.5538373741,19.9213203435596)) ;
#85265 = CARTESIAN_POINT('',(80.1757359312881,224.729573305388,30.8213203435596)) ;
#85266 = CARTESIAN_POINT('',(80.1757359312881,224.729573305388,19.9213203435596)) ;
#85267 = CARTESIAN_POINT('',(77.1324174527726,221.686254826872,30.8213203435596)) ;
#85268 = CARTESIAN_POINT('Origin',(80.6000000000001,224.305309236676,19.9213203435596)) ;
#85269 = CARTESIAN_POINT('',(80.0000000000001,224.305309236676,30.8213203435596)) ;
#85270 = CARTESIAN_POINT('',(80.0000000000001,224.305309236676,19.9213203435596)) ;
#85271 = CARTESIAN_POINT('Origin',(80.6000000000001,224.305309236676,30.8213203435596)) ;
#85272 = CARTESIAN_POINT('Origin',(80.0000000000001,217.767014370377,19.9213203435596)) ;
#85273 = CARTESIAN_POINT('',(80.0000000000001,217.767014370377,30.8213203435596)) ;
#85274 = CARTESIAN_POINT('',(80.0000000000001,217.767014370377,19.9213203435596)) ;
#85275 = CARTESIAN_POINT('',(80.,228.575260777783,30.8213203435596)) ;
#85276 = CARTESIAN_POINT('Origin',(76.0000000000001,217.767014370377,19.9213203435596)) ;
#85277 = CARTESIAN_POINT('',(75.3054072893324,213.827783358328,30.8213203435596)) ;
#85278 = CARTESIAN_POINT('',(75.3054072893324,213.827783358328,19.9213203435596)) ;
#85279 = CARTESIAN_POINT('Origin',(76.0000000000001,217.767014370377,30.8213203435596)) ;
#85280 = CARTESIAN_POINT('Origin',(62.1568347953873,216.146231446812,19.9213203435596)) ;
#85281 = CARTESIAN_POINT('',(63.7885177058986,215.858521725728,30.8213203435596)) ;
#85282 = CARTESIAN_POINT('',(63.7885177058986,215.858521725728,19.9213203435596)) ;
#85283 = CARTESIAN_POINT('',(56.0690156887983,217.219678208976,30.8213203435596)) ;
#85284 = CARTESIAN_POINT('Origin',(64.4831104165663,219.797752737776,19.9213203435596)) ;
#85285 = CARTESIAN_POINT('',(61.2065022394103,217.503446992372,30.8213203435596)) ;
#85286 = CARTESIAN_POINT('',(61.2065022394103,217.503446992372,19.9213203435596)) ;
#85287 = CARTESIAN_POINT('Origin',(64.4831104165663,219.797752737776,30.8213203435596)) ;
#85288 = CARTESIAN_POINT('Origin',(55.9573593128808,225.,19.9213203435596)) ;
#85289 = CARTESIAN_POINT('',(56.6807511357248,223.966889410112,30.8213203435596)) ;
#85290 = CARTESIAN_POINT('',(56.6807511357248,223.966889410112,19.9213203435596)) ;
#85291 = CARTESIAN_POINT('',(52.2070161828572,230.356045065742,30.8213203435596)) ;
#85292 = CARTESIAN_POINT('Origin',(59.9573593128808,226.261195155516,19.9213203435596)) ;
#85293 = CARTESIAN_POINT('',(55.9573593128808,226.261195155516,30.8213203435596)) ;
#85294 = CARTESIAN_POINT('',(55.9573593128808,226.261195155516,19.9213203435596)) ;
#85295 = CARTESIAN_POINT('Origin',(59.9573593128808,226.261195155516,30.8213203435596)) ;
#85296 = CARTESIAN_POINT('Origin',(55.9573593128808,245.,19.9213203435596)) ;
#85297 = CARTESIAN_POINT('',(55.9573593128808,244.4,30.8213203435596)) ;
#85298 = CARTESIAN_POINT('',(55.9573593128808,244.4,19.9213203435596)) ;
#85299 = CARTESIAN_POINT('',(55.9573593128808,242.191753592594,30.8213203435596)) ;
#85300 = CARTESIAN_POINT('Origin',(55.3573593128808,244.4,19.9213203435596)) ;
#85301 = CARTESIAN_POINT('',(55.3573593128808,245.,30.8213203435596)) ;
#85302 = CARTESIAN_POINT('',(55.3573593128808,245.,19.9213203435596)) ;
#85303 = CARTESIAN_POINT('Origin',(55.3573593128808,244.4,30.8213203435596)) ;
#85304 = CARTESIAN_POINT('Origin',(26.2,245.,19.9213203435596)) ;
#85305 = CARTESIAN_POINT('',(46.8,245.,30.8213203435596)) ;
#85306 = CARTESIAN_POINT('',(46.8,245.,19.9213203435596)) ;
#85307 = CARTESIAN_POINT('',(39.95,245.,30.8213203435596)) ;
#85308 = CARTESIAN_POINT('Origin',(46.8,245.6,19.9213203435596)) ;
#85309 = CARTESIAN_POINT('',(46.2,245.6,30.8213203435596)) ;
#85310 = CARTESIAN_POINT('',(46.2,245.6,19.9213203435596)) ;
#85311 = CARTESIAN_POINT('Origin',(46.8,245.6,30.8213203435596)) ;
#85312 = CARTESIAN_POINT('Origin',(46.2,245.,19.9213203435596)) ;
#85313 = CARTESIAN_POINT('',(46.1999999999999,242.191753592594,30.8213203435596)) ;
#85314 = CARTESIAN_POINT('Origin',(46.2999999999999,242.191753592594,30.8213203435596)) ;
#85315 = CARTESIAN_POINT('Origin',(46.2999999999999,245.6,30.8213203435596)) ;
#85316 = CARTESIAN_POINT('Origin',(79.2999999999999,229.3,25.9213203435596)) ;
#85317 = CARTESIAN_POINT('',(79.2999999999999,229.4,25.9213203435596)) ;
#85318 = CARTESIAN_POINT('',(79.1999999999999,229.3,25.9213203435596)) ;
#85319 = CARTESIAN_POINT('Origin',(79.2999999999999,229.3,25.9213203435596)) ;
#85320 = CARTESIAN_POINT('',(79.1999999999999,229.3,30.9213203435596)) ;
#85321 = CARTESIAN_POINT('',(79.1999999999999,229.3,25.9213203435596)) ;
#85322 = CARTESIAN_POINT('',(79.2999999999999,229.4,30.9213203435596)) ;
#85323 = CARTESIAN_POINT('Origin',(79.2999999999999,229.3,30.9213203435596)) ;
#85324 = CARTESIAN_POINT('',(79.2999999999999,229.4,25.9213203435596)) ;
#85325 = CARTESIAN_POINT('Origin',(80.1999999999999,229.3,30.9213203435596)) ;
#85326 = CARTESIAN_POINT('',(80.199999999999,229.4,31.8213203435596)) ;
#85327 = CARTESIAN_POINT('Origin',(80.1999999999999,229.3,31.8213203435596)) ;
#85328 = CARTESIAN_POINT('Origin',(80.1999999999999,229.4,30.9213203435596)) ;
#85329 = CARTESIAN_POINT('Origin',(80.1999999999999,229.3,30.9213203435596)) ;
#85330 = CARTESIAN_POINT('Origin',(66.9499999999995,229.3,31.8213203435596)) ;
#85331 = CARTESIAN_POINT('Origin',(80.299999999999,229.3,31.8213203435596)) ;
#85332 = CARTESIAN_POINT('Origin',(80.1999999999999,234.391753592594,30.9213203435596)) ;
#85333 = CARTESIAN_POINT('',(79.1999999999999,226.7,30.9213203435596)) ;
#85334 = CARTESIAN_POINT('',(79.1999999999999,234.391753592594,30.9213203435596)) ;
#85335 = CARTESIAN_POINT('Origin',(80.1999999999999,226.7,30.9213203435596)) ;
#85336 = CARTESIAN_POINT('Origin',(79.1999999999999,229.4,25.9213203435596)) ;
#85337 = CARTESIAN_POINT('',(79.1999999999999,226.7,25.9213203435596)) ;
#85338 = CARTESIAN_POINT('',(79.1999999999999,226.6,25.9213203435596)) ;
#85339 = CARTESIAN_POINT('',(79.1999999999999,226.7,25.9213203435596)) ;
#85340 = CARTESIAN_POINT('Origin',(79.6999999999999,228.,25.9213203435596)) ;
#85341 = CARTESIAN_POINT('',(80.199999999999,229.4,25.9213203435596)) ;
#85342 = CARTESIAN_POINT('',(79.1999999999999,229.4,25.9213203435596)) ;
#85343 = CARTESIAN_POINT('',(80.199999999999,226.6,25.9213203435596)) ;
#85344 = CARTESIAN_POINT('',(80.199999999999,230.5,25.9213203435596)) ;
#85345 = CARTESIAN_POINT('',(79.2999999999999,226.6,25.9213203435596)) ;
#85346 = CARTESIAN_POINT('',(80.1999999999999,226.6,25.9213203435596)) ;
#85347 = CARTESIAN_POINT('Origin',(79.2999999999999,226.7,25.9213203435596)) ;
#85348 = CARTESIAN_POINT('Origin',(79.2999999999999,226.7,25.9213203435596)) ;
#85349 = CARTESIAN_POINT('',(79.2999999999999,226.6,30.9213203435596)) ;
#85350 = CARTESIAN_POINT('',(79.2999999999999,226.6,25.9213203435596)) ;
#85351 = CARTESIAN_POINT('Origin',(79.2999999999999,226.7,30.9213203435596)) ;
#85352 = CARTESIAN_POINT('Origin',(80.1999999999999,226.7,30.9213203435596)) ;
#85353 = CARTESIAN_POINT('',(80.199999999999,226.6,31.8213203435596)) ;
#85354 = CARTESIAN_POINT('Origin',(80.199999999999,226.7,31.8213203435596)) ;
#85355 = CARTESIAN_POINT('Origin',(80.1999999999999,226.6,30.9213203435596)) ;
#85356 = CARTESIAN_POINT('Origin',(66.4499999999997,226.700000000001,31.8213203435596)) ;
#85357 = CARTESIAN_POINT('Origin',(80.299999999999,226.7,31.8213203435596)) ;
#85358 = CARTESIAN_POINT('Origin',(79.1999999999999,226.6,25.9213203435596)) ;
#85359 = CARTESIAN_POINT('',(80.199999999999,226.6,25.9213203435596)) ;
#85360 = CARTESIAN_POINT('',(80.199999999999,226.6,22.9213203435596)) ;
#85361 = CARTESIAN_POINT('Origin',(80.099999999999,230.4,31.8213203435596)) ;
#85362 = CARTESIAN_POINT('',(80.099999999999,230.5,31.8213203435596)) ;
#85363 = CARTESIAN_POINT('Origin',(80.099999999999,230.6,31.8213203435596)) ;
#85364 = CARTESIAN_POINT('',(80.199999999999,230.4,31.8213203435596)) ;
#85365 = CARTESIAN_POINT('Origin',(80.099999999999,230.4,31.8213203435596)) ;
#85366 = CARTESIAN_POINT('Origin',(80.299999999999,230.4,31.8213203435596)) ;
#85367 = CARTESIAN_POINT('Origin',(76.0414213562367,230.4,31.8213203435596)) ;
#85368 = CARTESIAN_POINT('',(76.0414213562367,230.5,31.8213203435596)) ;
#85369 = CARTESIAN_POINT('',(75.9707106781181,230.470710678119,31.8213203435596)) ;
#85370 = CARTESIAN_POINT('Origin',(76.0414213562367,230.4,31.8213203435596)) ;
#85371 = CARTESIAN_POINT('Origin',(76.0414213562367,230.6,31.8213203435596)) ;
#85372 = CARTESIAN_POINT('Origin',(75.8999999999994,230.541421356237,31.8213203435596)) ;
#85373 = CARTESIAN_POINT('Origin',(66.9499999999995,230.6,31.8213203435596)) ;
#85374 = CARTESIAN_POINT('',(66.9499999999995,230.5,31.8213203435596)) ;
#85375 = CARTESIAN_POINT('Origin',(75.2999999999994,229.658578643763,31.8213203435596)) ;
#85376 = CARTESIAN_POINT('',(75.2292893218808,229.729289321881,31.8213203435596)) ;
#85377 = CARTESIAN_POINT('',(75.1999999999994,229.658578643763,31.8213203435596)) ;
#85378 = CARTESIAN_POINT('Origin',(75.2999999999994,229.658578643763,31.8213203435596)) ;
#85379 = CARTESIAN_POINT('Origin',(75.1585786437621,229.8,31.8213203435596)) ;
#85380 = CARTESIAN_POINT('Origin',(75.0999999999994,229.658578643763,31.8213203435596)) ;
#85381 = CARTESIAN_POINT('Origin',(72.3751661181778,227.016587474416,31.8213203435596)) ;
#85382 = CARTESIAN_POINT('',(72.4458767962964,226.945876796297,31.8213203435596)) ;
#85383 = CARTESIAN_POINT('Origin',(75.2999999999993,226.341421356237,31.8213203435596)) ;
#85384 = CARTESIAN_POINT('',(75.1999999999993,226.341421356237,31.8213203435596)) ;
#85385 = CARTESIAN_POINT('',(75.2292893218806,226.270710678119,31.8213203435596)) ;
#85386 = CARTESIAN_POINT('Origin',(75.2999999999993,226.341421356237,31.8213203435596)) ;
#85387 = CARTESIAN_POINT('Origin',(75.0999999999993,226.341421356237,31.8213203435596)) ;
#85388 = CARTESIAN_POINT('Origin',(75.158578643762,226.2,31.8213203435596)) ;
#85389 = CARTESIAN_POINT('Origin',(75.0999999999996,234.941753592594,31.8213203435596)) ;
#85390 = CARTESIAN_POINT('',(75.1999999999996,234.941753592594,31.8213203435596)) ;
#85391 = CARTESIAN_POINT('Origin',(76.0414213562366,225.6,31.8213203435596)) ;
#85392 = CARTESIAN_POINT('',(75.9707106781179,225.529289321881,31.8213203435596)) ;
#85393 = CARTESIAN_POINT('',(76.0414213562366,225.5,31.8213203435596)) ;
#85394 = CARTESIAN_POINT('Origin',(76.0414213562366,225.6,31.8213203435596)) ;
#85395 = CARTESIAN_POINT('Origin',(75.8999999999993,225.458578643763,31.8213203435596)) ;
#85396 = CARTESIAN_POINT('Origin',(76.0414213562366,225.4,31.8213203435596)) ;
#85397 = CARTESIAN_POINT('Origin',(66.6834125255838,234.675166118178,31.8213203435596)) ;
#85398 = CARTESIAN_POINT('',(66.7541232037024,234.745876796297,31.8213203435596)) ;
#85399 = CARTESIAN_POINT('Origin',(80.0999999999989,225.6,31.8213203435596)) ;
#85400 = CARTESIAN_POINT('',(80.199999999999,225.6,31.8213203435596)) ;
#85401 = CARTESIAN_POINT('Origin',(80.2999999999989,225.6,31.8213203435596)) ;
#85402 = CARTESIAN_POINT('',(80.0999999999989,225.5,31.8213203435596)) ;
#85403 = CARTESIAN_POINT('Origin',(80.0999999999989,225.6,31.8213203435596)) ;
#85404 = CARTESIAN_POINT('Origin',(80.0999999999989,225.4,31.8213203435596)) ;
#85405 = CARTESIAN_POINT('Origin',(80.299999999999,232.441753592594,31.8213203435596)) ;
#85406 = CARTESIAN_POINT('',(80.199999999999,232.441753592594,31.8213203435596)) ;
#85407 = CARTESIAN_POINT('Origin',(80.0999999999989,225.6,19.9213203435596)) ;
#85408 = CARTESIAN_POINT('',(80.0999999999989,225.5,19.9213203435596)) ;
#85409 = CARTESIAN_POINT('',(80.199999999999,225.6,19.9213203435596)) ;
#85410 = CARTESIAN_POINT('Origin',(64.4499999999996,225.4,31.8213203435596)) ;
#85411 = CARTESIAN_POINT('',(64.4499999999996,225.5,31.8213203435596)) ;
#85412 = CARTESIAN_POINT('Origin',(76.0414213562366,225.6,19.9213203435596)) ;
#85413 = CARTESIAN_POINT('',(75.9707106781179,225.529289321881,19.9213203435596)) ;
#85414 = CARTESIAN_POINT('',(76.0414213562366,225.5,19.9213203435596)) ;
#85415 = CARTESIAN_POINT('Origin',(75.2999999999993,226.341421356237,19.9213203435596)) ;
#85416 = CARTESIAN_POINT('',(75.1999999999993,226.341421356237,19.9213203435596)) ;
#85417 = CARTESIAN_POINT('',(75.2292893218806,226.270710678119,19.9213203435596)) ;
#85418 = CARTESIAN_POINT('Origin',(75.2999999999994,229.658578643763,19.9213203435596)) ;
#85419 = CARTESIAN_POINT('',(75.2292893218808,229.729289321881,19.9213203435596)) ;
#85420 = CARTESIAN_POINT('',(75.1999999999994,229.658578643763,19.9213203435596)) ;
#85421 = CARTESIAN_POINT('Origin',(76.0414213562367,230.4,19.9213203435596)) ;
#85422 = CARTESIAN_POINT('',(76.0414213562367,230.5,19.9213203435596)) ;
#85423 = CARTESIAN_POINT('',(75.9707106781181,230.470710678119,19.9213203435596)) ;
#85424 = CARTESIAN_POINT('Origin',(80.099999999999,230.4,19.9213203435596)) ;
#85425 = CARTESIAN_POINT('',(80.199999999999,230.4,19.9213203435596)) ;
#85426 = CARTESIAN_POINT('',(80.099999999999,230.5,19.9213203435596)) ;
#85427 = CARTESIAN_POINT('Origin',(80.299999999999,232.441753592594,31.8213203435596)) ;
#85428 = CARTESIAN_POINT('',(80.199999999999,232.441753592594,31.8213203435596)) ;
#85429 = CARTESIAN_POINT('Origin',(75.1999999999993,225.5,19.9213203435596)) ;
#85430 = CARTESIAN_POINT('Origin',(80.199999999999,225.5,19.9213203435596)) ;
#85431 = CARTESIAN_POINT('Origin',(74.2999999999999,226.1,31.8213203435596)) ;
#85432 = CARTESIAN_POINT('',(74.2999999999999,226.,31.8213203435596)) ;
#85433 = CARTESIAN_POINT('Origin',(74.2999999999999,226.1,31.8213203435596)) ;
#85434 = CARTESIAN_POINT('',(74.1999999999999,226.1,31.8213203435596)) ;
#85435 = CARTESIAN_POINT('Origin',(74.2999999999999,226.1,31.8213203435596)) ;
#85436 = CARTESIAN_POINT('Origin',(74.2999999999999,226.1,31.8213203435596)) ;
#85437 = CARTESIAN_POINT('Origin',(74.3999999999999,225.9,31.8213203435596)) ;
#85438 = CARTESIAN_POINT('',(74.3999999999999,226.,31.8213203435596)) ;
#85439 = CARTESIAN_POINT('Origin',(74.3999999999999,226.1,31.8213203435596)) ;
#85440 = CARTESIAN_POINT('',(74.4999999999999,225.9,31.8213203435596)) ;
#85441 = CARTESIAN_POINT('Origin',(74.3999999999999,225.9,31.8213203435596)) ;
#85442 = CARTESIAN_POINT('Origin',(74.5999999999999,225.9,31.8213203435596)) ;
#85443 = CARTESIAN_POINT('Origin',(64.1,226.1,31.8213203435596)) ;
#85444 = CARTESIAN_POINT('',(64.1,226.,31.8213203435596)) ;
#85445 = CARTESIAN_POINT('Origin',(74.3999999999999,225.9,19.9213203435596)) ;
#85446 = CARTESIAN_POINT('',(74.4999999999999,225.9,19.9213203435596)) ;
#85447 = CARTESIAN_POINT('',(74.3999999999999,226.,19.9213203435596)) ;
#85448 = CARTESIAN_POINT('Origin',(74.0999999999999,231.9,31.8213203435596)) ;
#85449 = CARTESIAN_POINT('',(74.0999999999999,232.,31.8213203435596)) ;
#85450 = CARTESIAN_POINT('Origin',(74.0999999999999,232.1,31.8213203435596)) ;
#85451 = CARTESIAN_POINT('',(74.1999999999999,231.9,31.8213203435596)) ;
#85452 = CARTESIAN_POINT('Origin',(74.0999999999999,231.9,31.8213203435596)) ;
#85453 = CARTESIAN_POINT('Origin',(74.2999999999999,231.9,31.8213203435596)) ;
#85454 = CARTESIAN_POINT('Origin',(74.3999999999999,223.1,31.8213203435596)) ;
#85455 = CARTESIAN_POINT('Origin',(74.5999999999999,223.1,31.8213203435596)) ;
#85456 = CARTESIAN_POINT('Origin',(74.3999999999999,222.9,31.8213203435596)) ;
#85457 = CARTESIAN_POINT('Origin',(74.5999999999999,231.191753592594,31.8213203435596)) ;
#85458 = CARTESIAN_POINT('',(74.4999999999999,231.191753592594,31.8213203435596)) ;
#85459 = CARTESIAN_POINT('Origin',(71.8999999999999,231.9,31.8213203435596)) ;
#85460 = CARTESIAN_POINT('',(71.8999999999999,232.,31.8213203435596)) ;
#85461 = CARTESIAN_POINT('Origin',(71.8999999999999,231.9,31.8213203435596)) ;
#85462 = CARTESIAN_POINT('Origin',(71.8999999999999,232.1,31.8213203435596)) ;
#85463 = CARTESIAN_POINT('Origin',(71.6999999999999,231.9,31.8213203435596)) ;
#85464 = CARTESIAN_POINT('Origin',(63.95,232.1,31.8213203435596)) ;
#85465 = CARTESIAN_POINT('',(63.95,232.,31.8213203435596)) ;
#85466 = CARTESIAN_POINT('Origin',(71.5999999999999,223.1,31.8213203435596)) ;
#85467 = CARTESIAN_POINT('Origin',(71.5999999999999,222.9,31.8213203435596)) ;
#85468 = CARTESIAN_POINT('Origin',(71.3999999999999,223.1,31.8213203435596)) ;
#85469 = CARTESIAN_POINT('Origin',(62.6,222.9,31.8213203435596)) ;
#85470 = CARTESIAN_POINT('Origin',(71.6999999999999,226.1,31.8213203435596)) ;
#85471 = CARTESIAN_POINT('Origin',(71.6999999999999,226.1,31.8213203435596)) ;
#85472 = CARTESIAN_POINT('Origin',(71.6999999999999,226.1,31.8213203435596)) ;
#85473 = CARTESIAN_POINT('Origin',(71.5999999999999,225.9,31.8213203435596)) ;
#85474 = CARTESIAN_POINT('Origin',(71.3999999999999,225.9,31.8213203435596)) ;
#85475 = CARTESIAN_POINT('Origin',(71.5999999999999,226.1,31.8213203435596)) ;
#85476 = CARTESIAN_POINT('Origin',(71.3999999999999,232.691753592594,31.8213203435596)) ;
#85477 = CARTESIAN_POINT('Origin',(62.75,226.1,31.8213203435596)) ;
#85478 = CARTESIAN_POINT('Origin',(71.6999999999999,235.691753592594,31.8213203435596)) ;
#85479 = CARTESIAN_POINT('Origin',(71.8999999999999,231.9,19.9213203435596)) ;
#85480 = CARTESIAN_POINT('',(71.8999999999999,232.,19.9213203435596)) ;
#85481 = CARTESIAN_POINT('Origin',(74.0999999999999,231.9,19.9213203435596)) ;
#85482 = CARTESIAN_POINT('',(74.1999999999999,231.9,19.9213203435596)) ;
#85483 = CARTESIAN_POINT('',(74.0999999999999,232.,19.9213203435596)) ;
#85484 = CARTESIAN_POINT('Origin',(74.2999999999999,232.691753592594,31.8213203435596)) ;
#85485 = CARTESIAN_POINT('',(74.1999999999999,232.691753592594,31.8213203435596)) ;
#85486 = CARTESIAN_POINT('Origin',(74.2999999999999,226.1,19.9213203435596)) ;
#85487 = CARTESIAN_POINT('',(74.2999999999999,226.,19.9213203435596)) ;
#85488 = CARTESIAN_POINT('',(74.1999999999999,226.1,19.9213203435596)) ;
#85489 = CARTESIAN_POINT('Origin',(74.4999999999999,223.,19.9213203435596)) ;
#85490 = CARTESIAN_POINT('Origin',(74.4999999999999,226.,19.9213203435596)) ;
#85491 = CARTESIAN_POINT('Origin',(58.8573593128808,241.8,25.9213203435596)) ;
#85492 = CARTESIAN_POINT('',(58.9573593128808,241.8,25.9213203435596)) ;
#85493 = CARTESIAN_POINT('',(58.8573593128808,241.9,25.9213203435596)) ;
#85494 = CARTESIAN_POINT('Origin',(58.8573593128808,241.8,25.9213203435596)) ;
#85495 = CARTESIAN_POINT('',(58.8573593128808,241.9,30.9213203435596)) ;
#85496 = CARTESIAN_POINT('',(58.8573593128808,241.9,25.9213203435596)) ;
#85497 = CARTESIAN_POINT('',(58.9573593128808,241.8,30.9213203435596)) ;
#85498 = CARTESIAN_POINT('Origin',(58.8573593128808,241.8,30.9213203435596)) ;
#85499 = CARTESIAN_POINT('',(58.9573593128808,241.8,25.9213203435596)) ;
#85500 = CARTESIAN_POINT('Origin',(57.9573593128808,241.8,30.9213203435596)) ;
#85501 = CARTESIAN_POINT('Origin',(57.9573593128808,241.8,31.8213203435596)) ;
#85502 = CARTESIAN_POINT('Origin',(57.9573593128808,241.8,30.9213203435596)) ;
#85503 = CARTESIAN_POINT('Origin',(57.9573593128808,241.9,30.9213203435596)) ;
#85504 = CARTESIAN_POINT('Origin',(56.3286796564404,241.8,31.8213203435596)) ;
#85505 = CARTESIAN_POINT('Origin',(58.9573593128808,241.9,25.9213203435596)) ;
#85506 = CARTESIAN_POINT('',(57.9573593128808,241.9,25.9213203435596)) ;
#85507 = CARTESIAN_POINT('',(57.9573593128808,241.9,25.9213203435596)) ;
#85508 = CARTESIAN_POINT('',(57.9573593128808,241.9,25.9213203435596)) ;
#85509 = CARTESIAN_POINT('Origin',(58.8573593128808,239.2,25.9213203435596)) ;
#85510 = CARTESIAN_POINT('',(58.8573593128808,239.1,25.9213203435596)) ;
#85511 = CARTESIAN_POINT('',(58.9573593128808,239.2,25.9213203435596)) ;
#85512 = CARTESIAN_POINT('Origin',(58.8573593128808,239.2,25.9213203435596)) ;
#85513 = CARTESIAN_POINT('',(58.9573593128808,239.2,30.9213203435596)) ;
#85514 = CARTESIAN_POINT('',(58.9573593128808,239.2,25.9213203435596)) ;
#85515 = CARTESIAN_POINT('',(58.8573593128808,239.1,30.9213203435596)) ;
#85516 = CARTESIAN_POINT('Origin',(58.8573593128808,239.2,30.9213203435596)) ;
#85517 = CARTESIAN_POINT('',(58.8573593128808,239.1,25.9213203435596)) ;
#85518 = CARTESIAN_POINT('Origin',(57.9573593128808,239.2,30.9213203435596)) ;
#85519 = CARTESIAN_POINT('Origin',(57.9573593128808,239.2,31.8213203435596)) ;
#85520 = CARTESIAN_POINT('Origin',(57.9573593128808,239.1,30.9213203435596)) ;
#85521 = CARTESIAN_POINT('Origin',(57.9573593128808,239.2,30.9213203435596)) ;
#85522 = CARTESIAN_POINT('Origin',(55.8286796564404,239.2,31.8213203435596)) ;
#85523 = CARTESIAN_POINT('Origin',(57.9573593128808,239.241753592594,30.9213203435596)) ;
#85524 = CARTESIAN_POINT('',(58.9573593128808,239.241753592594,30.9213203435596)) ;
#85525 = CARTESIAN_POINT('Origin',(58.9573593128808,239.1,25.9213203435596)) ;
#85526 = CARTESIAN_POINT('',(58.9573593128808,241.9,25.9213203435596)) ;
#85527 = CARTESIAN_POINT('Origin',(62.1159379566435,238.1,31.8213203435596)) ;
#85528 = CARTESIAN_POINT('Origin',(62.1159379566435,237.9,31.8213203435596)) ;
#85529 = CARTESIAN_POINT('Origin',(62.2573593128808,237.958578643763,31.8213203435596)) ;
#85530 = CARTESIAN_POINT('Origin',(55.8286796564404,237.9,31.8213203435596)) ;
#85531 = CARTESIAN_POINT('Origin',(62.8573593128808,238.841421356237,31.8213203435596)) ;
#85532 = CARTESIAN_POINT('Origin',(62.998780669118,238.7,31.8213203435596)) ;
#85533 = CARTESIAN_POINT('Origin',(63.0573593128807,238.841421356237,31.8213203435596)) ;
#85534 = CARTESIAN_POINT('Origin',(60.6596069590762,236.360826289958,31.8213203435596)) ;
#85535 = CARTESIAN_POINT('Origin',(62.8573593128808,242.158578643763,31.8213203435596)) ;
#85536 = CARTESIAN_POINT('Origin',(63.0573593128807,242.158578643763,31.8213203435596)) ;
#85537 = CARTESIAN_POINT('Origin',(62.9987806691181,242.3,31.8213203435596)) ;
#85538 = CARTESIAN_POINT('Origin',(63.0573593128807,238.691753592594,31.8213203435596)) ;
#85539 = CARTESIAN_POINT('Origin',(62.1159379566435,242.9,31.8213203435596)) ;
#85540 = CARTESIAN_POINT('Origin',(62.2573593128808,243.041421356237,31.8213203435596)) ;
#85541 = CARTESIAN_POINT('Origin',(62.1159379566435,243.1,31.8213203435596)) ;
#85542 = CARTESIAN_POINT('Origin',(61.2178533664821,244.080927302636,31.8213203435596)) ;
#85543 = CARTESIAN_POINT('Origin',(58.3286796564404,243.1,31.8213203435596)) ;
#85544 = CARTESIAN_POINT('Origin',(79.2999999999999,252.3,25.9213203435596)) ;
#85545 = CARTESIAN_POINT('',(79.2999999999999,252.4,25.9213203435596)) ;
#85546 = CARTESIAN_POINT('',(79.1999999999999,252.3,25.9213203435596)) ;
#85547 = CARTESIAN_POINT('Origin',(79.2999999999999,252.3,25.9213203435596)) ;
#85548 = CARTESIAN_POINT('',(79.1999999999999,252.3,30.9213203435596)) ;
#85549 = CARTESIAN_POINT('',(79.1999999999999,252.3,25.9213203435596)) ;
#85550 = CARTESIAN_POINT('',(79.2999999999999,252.4,30.9213203435596)) ;
#85551 = CARTESIAN_POINT('Origin',(79.2999999999999,252.3,30.9213203435596)) ;
#85552 = CARTESIAN_POINT('',(79.2999999999999,252.4,25.9213203435596)) ;
#85553 = CARTESIAN_POINT('Origin',(80.1999999999999,252.3,30.9213203435596)) ;
#85554 = CARTESIAN_POINT('Origin',(80.1999999999999,252.3,31.8213203435596)) ;
#85555 = CARTESIAN_POINT('Origin',(80.1999999999999,252.4,30.9213203435596)) ;
#85556 = CARTESIAN_POINT('Origin',(80.1999999999999,252.3,30.9213203435596)) ;
#85557 = CARTESIAN_POINT('Origin',(66.9499999999999,252.3,31.8213203435596)) ;
#85558 = CARTESIAN_POINT('Origin',(80.299999999999,252.3,31.8213203435596)) ;
#85559 = CARTESIAN_POINT('Origin',(80.1999999999999,245.891753592594,30.9213203435596)) ;
#85560 = CARTESIAN_POINT('',(79.1999999999999,249.7,30.9213203435596)) ;
#85561 = CARTESIAN_POINT('',(79.1999999999999,245.891753592594,30.9213203435596)) ;
#85562 = CARTESIAN_POINT('Origin',(80.1999999999999,249.7,30.9213203435596)) ;
#85563 = CARTESIAN_POINT('Origin',(79.1999999999999,252.4,25.9213203435596)) ;
#85564 = CARTESIAN_POINT('',(79.1999999999999,249.7,25.9213203435596)) ;
#85565 = CARTESIAN_POINT('',(79.1999999999999,249.6,25.9213203435596)) ;
#85566 = CARTESIAN_POINT('',(79.1999999999999,249.7,25.9213203435596)) ;
#85567 = CARTESIAN_POINT('Origin',(79.6999999999999,251.,25.9213203435596)) ;
#85568 = CARTESIAN_POINT('',(80.1999999999999,252.4,25.9213203435596)) ;
#85569 = CARTESIAN_POINT('',(79.1999999999999,252.4,25.9213203435596)) ;
#85570 = CARTESIAN_POINT('',(80.1999999999999,249.6,25.9213203435596)) ;
#85571 = CARTESIAN_POINT('',(80.1999999999999,252.4,25.9213203435596)) ;
#85572 = CARTESIAN_POINT('',(79.2999999999999,249.6,25.9213203435596)) ;
#85573 = CARTESIAN_POINT('',(80.1999999999999,249.6,25.9213203435596)) ;
#85574 = CARTESIAN_POINT('Origin',(79.2999999999999,249.7,25.9213203435596)) ;
#85575 = CARTESIAN_POINT('Origin',(79.2999999999999,249.7,25.9213203435596)) ;
#85576 = CARTESIAN_POINT('',(79.2999999999999,249.6,30.9213203435596)) ;
#85577 = CARTESIAN_POINT('',(79.2999999999999,249.6,25.9213203435596)) ;
#85578 = CARTESIAN_POINT('Origin',(79.2999999999999,249.7,30.9213203435596)) ;
#85579 = CARTESIAN_POINT('Origin',(80.1999999999999,249.7,30.9213203435596)) ;
#85580 = CARTESIAN_POINT('',(80.199999999999,249.6,31.8213203435596)) ;
#85581 = CARTESIAN_POINT('Origin',(80.199999999999,249.7,31.8213203435596)) ;
#85582 = CARTESIAN_POINT('Origin',(80.1999999999999,249.6,30.9213203435596)) ;
#85583 = CARTESIAN_POINT('Origin',(66.4500000000001,249.700000000001,31.8213203435596)) ;
#85584 = CARTESIAN_POINT('Origin',(80.2999999999989,249.7,31.8213203435596)) ;
#85585 = CARTESIAN_POINT('Origin',(79.1999999999999,249.6,25.9213203435596)) ;
#85586 = CARTESIAN_POINT('',(80.1999999999999,249.6,25.9213203435596)) ;
#85587 = CARTESIAN_POINT('',(80.199999999999,249.6,22.9213203435596)) ;
#85588 = CARTESIAN_POINT('Origin',(76.0414213562365,248.6,31.8213203435596)) ;
#85589 = CARTESIAN_POINT('',(75.9707106781179,248.529289321881,31.8213203435596)) ;
#85590 = CARTESIAN_POINT('',(76.0414213562365,248.5,31.8213203435596)) ;
#85591 = CARTESIAN_POINT('Origin',(76.0414213562365,248.6,31.8213203435596)) ;
#85592 = CARTESIAN_POINT('Origin',(75.8999999999992,248.458578643763,31.8213203435596)) ;
#85593 = CARTESIAN_POINT('Origin',(76.0414213562365,248.4,31.8213203435596)) ;
#85594 = CARTESIAN_POINT('Origin',(75.2999999999993,249.341421356237,31.8213203435596)) ;
#85595 = CARTESIAN_POINT('',(75.1999999999993,249.341421356237,31.8213203435596)) ;
#85596 = CARTESIAN_POINT('',(75.2292893218807,249.270710678119,31.8213203435596)) ;
#85597 = CARTESIAN_POINT('Origin',(75.2999999999993,249.341421356237,31.8213203435596)) ;
#85598 = CARTESIAN_POINT('Origin',(75.0999999999993,249.341421356237,31.8213203435596)) ;
#85599 = CARTESIAN_POINT('Origin',(75.158578643762,249.2,31.8213203435596)) ;
#85600 = CARTESIAN_POINT('Origin',(75.2999999999994,252.658578643763,31.8213203435596)) ;
#85601 = CARTESIAN_POINT('',(75.2292893218808,252.729289321881,31.8213203435596)) ;
#85602 = CARTESIAN_POINT('',(75.1999999999994,252.658578643763,31.8213203435596)) ;
#85603 = CARTESIAN_POINT('Origin',(75.2999999999994,252.658578643763,31.8213203435596)) ;
#85604 = CARTESIAN_POINT('Origin',(75.1585786437621,252.8,31.8213203435596)) ;
#85605 = CARTESIAN_POINT('Origin',(75.0999999999994,252.658578643763,31.8213203435596)) ;
#85606 = CARTESIAN_POINT('Origin',(76.0414213562367,253.4,31.8213203435596)) ;
#85607 = CARTESIAN_POINT('',(76.0414213562367,253.5,31.8213203435596)) ;
#85608 = CARTESIAN_POINT('',(75.9707106781181,253.470710678119,31.8213203435596)) ;
#85609 = CARTESIAN_POINT('Origin',(76.0414213562367,253.4,31.8213203435596)) ;
#85610 = CARTESIAN_POINT('Origin',(76.0414213562367,253.6,31.8213203435596)) ;
#85611 = CARTESIAN_POINT('Origin',(75.8999999999994,253.541421356237,31.8213203435596)) ;
#85612 = CARTESIAN_POINT('Origin',(66.9499999999995,253.6,31.8213203435596)) ;
#85613 = CARTESIAN_POINT('',(66.9499999999995,253.5,31.8213203435596)) ;
#85614 = CARTESIAN_POINT('Origin',(80.2999999999989,243.941753592594,31.8213203435596)) ;
#85615 = CARTESIAN_POINT('Origin',(66.6251661181778,244.266587474416,31.8213203435596)) ;
#85616 = CARTESIAN_POINT('',(66.6958767962964,244.195876796297,31.8213203435596)) ;
#85617 = CARTESIAN_POINT('Origin',(76.0414213562367,253.4,19.9213203435596)) ;
#85618 = CARTESIAN_POINT('',(76.0414213562367,253.5,19.9213203435596)) ;
#85619 = CARTESIAN_POINT('',(75.9707106781181,253.470710678119,19.9213203435596)) ;
#85620 = CARTESIAN_POINT('Origin',(75.0999999999992,246.441753592594,31.8213203435596)) ;
#85621 = CARTESIAN_POINT('',(75.1999999999992,246.441753592594,31.8213203435596)) ;
#85622 = CARTESIAN_POINT('Origin',(75.2999999999994,252.658578643763,19.9213203435596)) ;
#85623 = CARTESIAN_POINT('',(75.2292893218808,252.729289321881,19.9213203435596)) ;
#85624 = CARTESIAN_POINT('',(75.1999999999994,252.658578643763,19.9213203435596)) ;
#85625 = CARTESIAN_POINT('Origin',(72.4334125255833,251.925166118179,31.8213203435596)) ;
#85626 = CARTESIAN_POINT('',(72.504123203702,251.995876796297,31.8213203435596)) ;
#85627 = CARTESIAN_POINT('Origin',(75.2999999999993,249.341421356237,19.9213203435596)) ;
#85628 = CARTESIAN_POINT('',(75.1999999999993,249.341421356237,19.9213203435596)) ;
#85629 = CARTESIAN_POINT('',(75.2292893218807,249.270710678119,19.9213203435596)) ;
#85630 = CARTESIAN_POINT('Origin',(64.4499999999996,248.4,31.8213203435596)) ;
#85631 = CARTESIAN_POINT('',(64.4499999999996,248.5,31.8213203435596)) ;
#85632 = CARTESIAN_POINT('Origin',(76.0414213562365,248.6,19.9213203435596)) ;
#85633 = CARTESIAN_POINT('',(75.9707106781179,248.529289321881,19.9213203435596)) ;
#85634 = CARTESIAN_POINT('',(76.0414213562365,248.5,19.9213203435596)) ;
#85635 = CARTESIAN_POINT('Origin',(80.2999999999989,243.941753592594,31.8213203435596)) ;
#85636 = CARTESIAN_POINT('',(80.1999999999989,243.941753592594,31.8213203435596)) ;
#85637 = CARTESIAN_POINT('Origin',(75.5999999999994,253.1,19.9213203435596)) ;
#85638 = CARTESIAN_POINT('Origin',(75.1999999999994,253.5,19.9213203435596)) ;
#85639 = CARTESIAN_POINT('Origin',(75.5999999999993,248.9,19.9213203435596)) ;
#85640 = CARTESIAN_POINT('Origin',(75.1999999999993,248.5,19.9213203435596)) ;
#85641 = CARTESIAN_POINT('Origin',(80.199999999999,248.5,19.9213203435596)) ;
#85642 = CARTESIAN_POINT('Origin',(64.3,245.191753592594,30.8213203435596)) ;
#85643 = CARTESIAN_POINT('',(64.3999999999999,245.191753592594,30.8213203435596)) ;
#85644 = CARTESIAN_POINT('Origin',(64.3999999999999,251.,19.9213203435596)) ;
#85645 = CARTESIAN_POINT('Origin',(56.3,245.191753592594,30.8213203435596)) ;
#85646 = CARTESIAN_POINT('',(56.3999999999999,245.191753592594,30.8213203435596)) ;
#85647 = CARTESIAN_POINT('Origin',(56.3999999999999,251.,19.9213203435596)) ;
#85648 = CARTESIAN_POINT('Origin',(43.0999999999999,252.1,31.8213203435596)) ;
#85649 = CARTESIAN_POINT('',(43.1999999999999,252.1,31.8213203435596)) ;
#85650 = CARTESIAN_POINT('Origin',(43.2999999999999,252.1,31.8213203435596)) ;
#85651 = CARTESIAN_POINT('',(43.0999999999999,252.,31.8213203435596)) ;
#85652 = CARTESIAN_POINT('Origin',(43.0999999999999,252.1,31.8213203435596)) ;
#85653 = CARTESIAN_POINT('Origin',(43.0999999999999,251.9,31.8213203435596)) ;
#85654 = CARTESIAN_POINT('Origin',(43.0999999999999,252.1,30.8213203435596)) ;
#85655 = CARTESIAN_POINT('',(43.1999999999999,252.1,30.8213203435596)) ;
#85656 = CARTESIAN_POINT('',(43.0999999999999,252.,30.8213203435596)) ;
#85657 = CARTESIAN_POINT('Origin',(43.0999999999999,252.1,30.8213203435596)) ;
#85658 = CARTESIAN_POINT('Origin',(43.2999999999999,252.1,30.8213203435596)) ;
#85659 = CARTESIAN_POINT('Origin',(43.0999999999999,251.9,30.8213203435596)) ;
#85660 = CARTESIAN_POINT('Origin',(43.0999999999999,259.9,31.8213203435596)) ;
#85661 = CARTESIAN_POINT('',(43.0999999999999,260.,31.8213203435596)) ;
#85662 = CARTESIAN_POINT('Origin',(43.0999999999999,260.1,31.8213203435596)) ;
#85663 = CARTESIAN_POINT('',(43.1999999999999,259.9,31.8213203435596)) ;
#85664 = CARTESIAN_POINT('Origin',(43.0999999999999,259.9,31.8213203435596)) ;
#85665 = CARTESIAN_POINT('Origin',(43.2999999999999,259.9,31.8213203435596)) ;
#85666 = CARTESIAN_POINT('Origin',(37.2999999999999,252.1,31.8213203435596)) ;
#85667 = CARTESIAN_POINT('',(37.1999999999999,252.1,31.8213203435596)) ;
#85668 = CARTESIAN_POINT('',(37.2999999999999,252.,31.8213203435596)) ;
#85669 = CARTESIAN_POINT('Origin',(37.2999999999999,252.1,31.8213203435596)) ;
#85670 = CARTESIAN_POINT('Origin',(37.0999999999999,252.1,31.8213203435596)) ;
#85671 = CARTESIAN_POINT('Origin',(37.2999999999999,251.9,31.8213203435596)) ;
#85672 = CARTESIAN_POINT('Origin',(37.2999999999999,252.1,30.8213203435596)) ;
#85673 = CARTESIAN_POINT('',(37.1999999999999,252.1,30.8213203435596)) ;
#85674 = CARTESIAN_POINT('Origin',(37.0999999999999,252.1,30.8213203435596)) ;
#85675 = CARTESIAN_POINT('',(37.2999999999999,252.,30.8213203435596)) ;
#85676 = CARTESIAN_POINT('Origin',(37.2999999999999,252.1,30.8213203435596)) ;
#85677 = CARTESIAN_POINT('Origin',(37.2999999999999,251.9,30.8213203435596)) ;
#85678 = CARTESIAN_POINT('Origin',(43.0999999999999,259.9,30.8213203435596)) ;
#85679 = CARTESIAN_POINT('',(43.0999999999999,260.,30.8213203435596)) ;
#85680 = CARTESIAN_POINT('',(43.1999999999999,259.9,30.8213203435596)) ;
#85681 = CARTESIAN_POINT('Origin',(43.0999999999999,259.9,30.8213203435596)) ;
#85682 = CARTESIAN_POINT('Origin',(43.0999999999999,260.1,30.8213203435596)) ;
#85683 = CARTESIAN_POINT('Origin',(43.2999999999999,259.9,30.8213203435596)) ;
#85684 = CARTESIAN_POINT('Origin',(37.2999999999999,259.9,31.8213203435596)) ;
#85685 = CARTESIAN_POINT('',(37.1999999999999,259.9,31.8213203435596)) ;
#85686 = CARTESIAN_POINT('Origin',(37.0999999999999,259.9,31.8213203435596)) ;
#85687 = CARTESIAN_POINT('',(37.2999999999999,260.,31.8213203435596)) ;
#85688 = CARTESIAN_POINT('Origin',(37.2999999999999,259.9,31.8213203435596)) ;
#85689 = CARTESIAN_POINT('Origin',(37.2999999999999,260.1,31.8213203435596)) ;
#85690 = CARTESIAN_POINT('Origin',(37.0999999999999,249.691753592594,31.8213203435596)) ;
#85691 = CARTESIAN_POINT('',(37.1999999999999,249.691753592594,31.8213203435596)) ;
#85692 = CARTESIAN_POINT('Origin',(37.2999999999999,259.9,30.8213203435596)) ;
#85693 = CARTESIAN_POINT('',(37.1999999999999,259.9,30.8213203435596)) ;
#85694 = CARTESIAN_POINT('',(37.2999999999999,260.,30.8213203435596)) ;
#85695 = CARTESIAN_POINT('Origin',(37.2999999999999,259.9,30.8213203435596)) ;
#85696 = CARTESIAN_POINT('Origin',(37.0999999999999,259.9,30.8213203435596)) ;
#85697 = CARTESIAN_POINT('Origin',(37.2999999999999,260.1,30.8213203435596)) ;
#85698 = CARTESIAN_POINT('Origin',(37.0999999999999,249.691753592594,30.8213203435596)) ;
#85699 = CARTESIAN_POINT('',(37.1999999999999,249.691753592594,30.8213203435596)) ;
#85700 = CARTESIAN_POINT('Origin',(48.4499999999999,260.1,30.8213203435596)) ;
#85701 = CARTESIAN_POINT('',(48.4499999999999,260.,30.8213203435596)) ;
#85702 = CARTESIAN_POINT('Origin',(37.2999999999999,259.9,19.9213203435596)) ;
#85703 = CARTESIAN_POINT('',(37.1999999999999,259.9,19.9213203435596)) ;
#85704 = CARTESIAN_POINT('',(37.2999999999999,260.,19.9213203435596)) ;
#85705 = CARTESIAN_POINT('Origin',(48.4499999999999,260.1,31.8213203435596)) ;
#85706 = CARTESIAN_POINT('',(48.4499999999999,260.,31.8213203435596)) ;
#85707 = CARTESIAN_POINT('Origin',(43.2999999999999,245.691753592594,30.8213203435596)) ;
#85708 = CARTESIAN_POINT('',(43.1999999999999,245.691753592594,30.8213203435596)) ;
#85709 = CARTESIAN_POINT('Origin',(43.0999999999999,259.9,19.9213203435596)) ;
#85710 = CARTESIAN_POINT('',(43.0999999999999,260.,19.9213203435596)) ;
#85711 = CARTESIAN_POINT('',(43.1999999999999,259.9,19.9213203435596)) ;
#85712 = CARTESIAN_POINT('Origin',(37.2999999999999,252.1,19.9213203435596)) ;
#85713 = CARTESIAN_POINT('',(37.2999999999999,252.,19.9213203435596)) ;
#85714 = CARTESIAN_POINT('',(37.1999999999999,252.1,19.9213203435596)) ;
#85715 = CARTESIAN_POINT('Origin',(45.4499999999999,251.9,30.8213203435596)) ;
#85716 = CARTESIAN_POINT('',(45.4499999999999,252.,30.8213203435596)) ;
#85717 = CARTESIAN_POINT('Origin',(45.4499999999999,251.9,31.8213203435596)) ;
#85718 = CARTESIAN_POINT('',(45.4499999999999,252.,31.8213203435596)) ;
#85719 = CARTESIAN_POINT('Origin',(43.2999999999999,245.691753592594,31.8213203435596)) ;
#85720 = CARTESIAN_POINT('',(43.1999999999999,245.691753592594,31.8213203435596)) ;
#85721 = CARTESIAN_POINT('Origin',(43.0999999999999,252.1,19.9213203435596)) ;
#85722 = CARTESIAN_POINT('',(43.1999999999999,252.1,19.9213203435596)) ;
#85723 = CARTESIAN_POINT('',(43.0999999999999,252.,19.9213203435596)) ;
#85724 = CARTESIAN_POINT('Origin',(37.1999999999999,260.,19.9213203435596)) ;
#85725 = CARTESIAN_POINT('Origin',(43.1999999999999,260.,19.9213203435596)) ;
#85726 = CARTESIAN_POINT('Origin',(43.1999999999999,252.,19.9213203435596)) ;
#85727 = CARTESIAN_POINT('Origin',(37.1999999999999,252.,19.9213203435596)) ;
#85728 = CARTESIAN_POINT('Origin',(30.7,254.8,30.8213203435596)) ;
#85729 = CARTESIAN_POINT('',(28.1999999999999,254.8,30.8213203435596)) ;
#85730 = CARTESIAN_POINT('Origin',(28.1,254.8,30.8213203435596)) ;
#85731 = CARTESIAN_POINT('Origin',(30.7,254.8,30.8213203435596)) ;
#85732 = CARTESIAN_POINT('Origin',(30.7,254.8,19.9213203435596)) ;
#85733 = CARTESIAN_POINT('',(28.2,254.8,31.8213203435596)) ;
#85734 = CARTESIAN_POINT('',(28.2,254.8,19.9213203435596)) ;
#85735 = CARTESIAN_POINT('',(33.1999999999999,254.8,31.8213203435596)) ;
#85736 = CARTESIAN_POINT('Origin',(30.6999999999999,254.8,31.8213203435596)) ;
#85737 = CARTESIAN_POINT('Origin',(30.6999999999999,254.8,31.8213203435596)) ;
#85738 = CARTESIAN_POINT('Origin',(30.6999999999999,254.8,31.8213203435596)) ;
#85739 = CARTESIAN_POINT('Origin',(33.2999999999999,254.8,31.8213203435596)) ;
#85740 = CARTESIAN_POINT('Origin',(29.1,262.2,25.9213203435596)) ;
#85741 = CARTESIAN_POINT('',(29.1999999999999,262.2,25.9213203435596)) ;
#85742 = CARTESIAN_POINT('',(29.1,262.3,25.9213203435596)) ;
#85743 = CARTESIAN_POINT('Origin',(29.1,262.2,25.9213203435596)) ;
#85744 = CARTESIAN_POINT('',(29.1,262.3,30.9213203435596)) ;
#85745 = CARTESIAN_POINT('',(29.1,262.3,25.9213203435596)) ;
#85746 = CARTESIAN_POINT('',(29.1999999999999,262.2,30.9213203435596)) ;
#85747 = CARTESIAN_POINT('Origin',(29.1,262.2,30.9213203435596)) ;
#85748 = CARTESIAN_POINT('',(29.1999999999999,262.2,25.9213203435596)) ;
#85749 = CARTESIAN_POINT('Origin',(28.1999999999999,262.2,30.9213203435596)) ;
#85750 = CARTESIAN_POINT('Origin',(28.2,262.2,31.8213203435596)) ;
#85751 = CARTESIAN_POINT('Origin',(28.1999999999999,262.2,30.9213203435596)) ;
#85752 = CARTESIAN_POINT('Origin',(28.1999999999999,262.3,30.9213203435596)) ;
#85753 = CARTESIAN_POINT('Origin',(41.45,262.2,31.8213203435596)) ;
#85754 = CARTESIAN_POINT('Origin',(28.1,262.2,31.8213203435596)) ;
#85755 = CARTESIAN_POINT('Origin',(29.1999999999999,262.3,25.9213203435596)) ;
#85756 = CARTESIAN_POINT('',(28.2,262.3,25.9213203435596)) ;
#85757 = CARTESIAN_POINT('',(28.2,262.3,25.9213203435596)) ;
#85758 = CARTESIAN_POINT('',(28.2,262.3,25.9213203435596)) ;
#85759 = CARTESIAN_POINT('Origin',(28.7,260.9,25.9213203435596)) ;
#85760 = CARTESIAN_POINT('',(29.1999999999999,259.6,25.9213203435596)) ;
#85761 = CARTESIAN_POINT('',(29.1999999999999,262.3,25.9213203435596)) ;
#85762 = CARTESIAN_POINT('',(29.1,259.5,25.9213203435596)) ;
#85763 = CARTESIAN_POINT('Origin',(29.1,259.6,25.9213203435596)) ;
#85764 = CARTESIAN_POINT('',(28.2,259.5,25.9213203435596)) ;
#85765 = CARTESIAN_POINT('',(29.1999999999999,259.5,25.9213203435596)) ;
#85766 = CARTESIAN_POINT('',(28.2,259.5,25.9213203435596)) ;
#85767 = CARTESIAN_POINT('Origin',(29.1999999999999,259.5,25.9213203435596)) ;
#85768 = CARTESIAN_POINT('',(29.1999999999999,259.6,30.9213203435596)) ;
#85769 = CARTESIAN_POINT('',(29.1999999999999,249.441753592594,30.9213203435596)) ;
#85770 = CARTESIAN_POINT('',(29.1999999999999,259.6,25.9213203435596)) ;
#85771 = CARTESIAN_POINT('Origin',(29.1,259.6,25.9213203435596)) ;
#85772 = CARTESIAN_POINT('',(29.1,259.5,30.9213203435596)) ;
#85773 = CARTESIAN_POINT('Origin',(29.1,259.6,30.9213203435596)) ;
#85774 = CARTESIAN_POINT('',(29.1,259.5,25.9213203435596)) ;
#85775 = CARTESIAN_POINT('Origin',(28.1999999999999,259.6,30.9213203435596)) ;
#85776 = CARTESIAN_POINT('',(28.2,259.5,31.8213203435596)) ;
#85777 = CARTESIAN_POINT('Origin',(28.1999999999999,259.6,31.8213203435596)) ;
#85778 = CARTESIAN_POINT('Origin',(28.2,259.5,30.9213203435596)) ;
#85779 = CARTESIAN_POINT('Origin',(28.1999999999999,259.6,30.9213203435596)) ;
#85780 = CARTESIAN_POINT('Origin',(40.9499999999996,259.6,31.8213203435596)) ;
#85781 = CARTESIAN_POINT('Origin',(28.0999999999999,259.6,31.8213203435596)) ;
#85782 = CARTESIAN_POINT('Origin',(28.1999999999999,249.441753592594,30.9213203435596)) ;
#85783 = CARTESIAN_POINT('Origin',(32.3585786437627,258.5,31.8213203435596)) ;
#85784 = CARTESIAN_POINT('Origin',(32.3585786437627,258.3,31.8213203435596)) ;
#85785 = CARTESIAN_POINT('Origin',(32.5,258.358578643763,31.8213203435596)) ;
#85786 = CARTESIAN_POINT('Origin',(40.95,258.3,31.8213203435596)) ;
#85787 = CARTESIAN_POINT('Origin',(28.1,258.3,31.8213203435596)) ;
#85788 = CARTESIAN_POINT('Origin',(33.1,259.241421356237,31.8213203435596)) ;
#85789 = CARTESIAN_POINT('Origin',(33.2414213562373,259.1,31.8213203435596)) ;
#85790 = CARTESIAN_POINT('Origin',(33.2999999999999,259.241421356237,31.8213203435596)) ;
#85791 = CARTESIAN_POINT('Origin',(33.2415874744158,259.100166118179,31.8213203435596)) ;
#85792 = CARTESIAN_POINT('Origin',(33.1,262.558578643763,31.8213203435596)) ;
#85793 = CARTESIAN_POINT('Origin',(33.2999999999999,262.558578643763,31.8213203435596)) ;
#85794 = CARTESIAN_POINT('Origin',(33.2414213562373,262.7,31.8213203435596)) ;
#85795 = CARTESIAN_POINT('Origin',(33.2999999999999,248.891753592594,31.8213203435596)) ;
#85796 = CARTESIAN_POINT('Origin',(32.3585786437627,263.3,31.8213203435596)) ;
#85797 = CARTESIAN_POINT('Origin',(32.5,263.441421356237,31.8213203435596)) ;
#85798 = CARTESIAN_POINT('Origin',(32.3585786437627,263.5,31.8213203435596)) ;
#85799 = CARTESIAN_POINT('Origin',(43.9998338818216,251.941587474416,31.8213203435596)) ;
#85800 = CARTESIAN_POINT('Origin',(28.2999999999999,263.3,31.8213203435596)) ;
#85801 = CARTESIAN_POINT('Origin',(28.2999999999999,263.5,31.8213203435596)) ;
#85802 = CARTESIAN_POINT('Origin',(28.1,263.3,31.8213203435596)) ;
#85803 = CARTESIAN_POINT('Origin',(43.45,263.5,31.8213203435596)) ;
#85804 = CARTESIAN_POINT('Origin',(28.1,251.391753592594,31.8213203435596)) ;
#85805 = CARTESIAN_POINT('Origin',(28.1,251.391753592594,31.8213203435596)) ;
#85806 = CARTESIAN_POINT('',(28.1999999999999,251.391753592594,31.8213203435596)) ;
#85807 = CARTESIAN_POINT('Origin',(61.5,261.2,31.8213203435596)) ;
#85808 = CARTESIAN_POINT('',(64.,261.2,31.8213203435596)) ;
#85809 = CARTESIAN_POINT('Origin',(64.1,261.2,31.8213203435596)) ;
#85810 = CARTESIAN_POINT('',(59.,261.2,31.8213203435596)) ;
#85811 = CARTESIAN_POINT('Origin',(61.5,261.2,31.8213203435596)) ;
#85812 = CARTESIAN_POINT('Origin',(61.5,261.2,31.8213203435596)) ;
#85813 = CARTESIAN_POINT('Origin',(61.5,261.2,19.9213203435596)) ;
#85814 = CARTESIAN_POINT('',(59.,261.2,19.9213203435596)) ;
#85815 = CARTESIAN_POINT('Origin',(64.1568347953873,220.146231446812,31.8213203435596)) ;
#85816 = CARTESIAN_POINT('',(66.1568347953873,220.146231446812,31.8213203435596)) ;
#85817 = CARTESIAN_POINT('Origin',(66.2568347953873,220.146231446812,31.8213203435596)) ;
#85818 = CARTESIAN_POINT('',(62.1568347953873,220.146231446812,31.8213203435596)) ;
#85819 = CARTESIAN_POINT('Origin',(64.1568347953873,220.146231446812,31.8213203435596)) ;
#85820 = CARTESIAN_POINT('Origin',(64.1568347953873,220.146231446812,31.8213203435596)) ;
#85821 = CARTESIAN_POINT('Origin',(64.1568347953873,220.146231446812,19.9213203435596)) ;
#85822 = CARTESIAN_POINT('',(62.1568347953873,220.146231446812,19.9213203435596)) ;
#85823 = CARTESIAN_POINT('Origin',(79.0999999999999,249.391753592594,30.8213203435596)) ;
#85824 = CARTESIAN_POINT('Origin',(79.0999999999999,259.648528137424,30.8213203435596)) ;
#85825 = CARTESIAN_POINT('Origin',(79.7999999999999,259.648528137424,30.8213203435596)) ;
#85826 = CARTESIAN_POINT('Origin',(79.3050252531694,259.153553390593,30.8213203435596)) ;
#85827 = CARTESIAN_POINT('Origin',(79.7999999999999,259.648528137424,30.8213203435596)) ;
#85828 = CARTESIAN_POINT('Origin',(78.758412525583,259.70016611818,30.8213203435596)) ;
#85829 = CARTESIAN_POINT('Origin',(80.9535533905932,257.50502525317,30.8213203435596)) ;
#85830 = CARTESIAN_POINT('Origin',(80.6,257.151471862576,30.8213203435596)) ;
#85831 = CARTESIAN_POINT('Origin',(81.1,257.151471862576,30.8213203435596)) ;
#85832 = CARTESIAN_POINT('Origin',(81.1,242.941753592594,30.8213203435596)) ;
#85833 = CARTESIAN_POINT('Origin',(81.1,247.098386676966,30.8213203435596)) ;
#85834 = CARTESIAN_POINT('Origin',(80.6,247.098386676966,30.8213203435596)) ;
#85835 = CARTESIAN_POINT('Origin',(80.616129032258,246.598646890358,30.8213203435596)) ;
#85836 = CARTESIAN_POINT('Origin',(80.6999999999999,244.,30.8213203435596)) ;
#85837 = CARTESIAN_POINT('Origin',(78.0999999999999,244.,30.8213203435596)) ;
#85838 = CARTESIAN_POINT('Origin',(78.1,239.691753592594,30.8213203435596)) ;
#85839 = CARTESIAN_POINT('Origin',(78.1,240.,30.8213203435596)) ;
#85840 = CARTESIAN_POINT('Origin',(80.6999999999999,240.,30.8213203435596)) ;
#85841 = CARTESIAN_POINT('Origin',(80.616129032258,237.401353109641,30.8213203435596)) ;
#85842 = CARTESIAN_POINT('Origin',(80.6,236.901613323034,30.8213203435596)) ;
#85843 = CARTESIAN_POINT('Origin',(81.1,236.901613323034,30.8213203435596)) ;
#85844 = CARTESIAN_POINT('Origin',(81.1,232.568672279644,30.8213203435596)) ;
#85845 = CARTESIAN_POINT('Origin',(81.1,226.002365511524,30.8213203435596)) ;
#85846 = CARTESIAN_POINT('Origin',(80.6,226.002365511524,30.8213203435596)) ;
#85847 = CARTESIAN_POINT('Origin',(80.9535533905933,225.64881212093,30.8213203435596)) ;
#85848 = CARTESIAN_POINT('Origin',(77.061706774654,221.756965504991,30.8213203435596)) ;
#85849 = CARTESIAN_POINT('Origin',(80.1050252531695,224.800283983507,30.8213203435596)) ;
#85850 = CARTESIAN_POINT('Origin',(80.6000000000001,224.305309236676,30.8213203435596)) ;
#85851 = CARTESIAN_POINT('Origin',(79.9000000000001,224.305309236676,30.8213203435596)) ;
#85852 = CARTESIAN_POINT('Origin',(79.9,228.575260777783,30.8213203435596)) ;
#85853 = CARTESIAN_POINT('Origin',(79.9000000000001,217.767014370377,30.8213203435596)) ;
#85854 = CARTESIAN_POINT('Origin',(76.0000000000001,217.767014370377,30.8213203435596)) ;
#85855 = CARTESIAN_POINT('Origin',(75.3227721070991,213.926264133629,30.8213203435596)) ;
#85856 = CARTESIAN_POINT('Origin',(56.086380506565,217.318158984277,30.8213203435596)) ;
#85857 = CARTESIAN_POINT('Origin',(63.8058825236653,215.957002501029,30.8213203435596)) ;
#85858 = CARTESIAN_POINT('Origin',(64.4831104165663,219.797752737776,30.8213203435596)) ;
#85859 = CARTESIAN_POINT('Origin',(61.2884174438392,217.560804636007,30.8213203435596)) ;
#85860 = CARTESIAN_POINT('Origin',(52.288931387286,230.413402709377,30.8213203435596)) ;
#85861 = CARTESIAN_POINT('Origin',(56.7626663401537,224.024247053747,30.8213203435596)) ;
#85862 = CARTESIAN_POINT('Origin',(59.9573593128808,226.261195155516,30.8213203435596)) ;
#85863 = CARTESIAN_POINT('Origin',(56.0573593128808,226.261195155516,30.8213203435596)) ;
#85864 = CARTESIAN_POINT('Origin',(56.0573593128807,242.191753592594,30.8213203435596)) ;
#85865 = CARTESIAN_POINT('Origin',(56.0573593128807,244.4,30.8213203435596)) ;
#85866 = CARTESIAN_POINT('Origin',(55.3573593128808,244.4,30.8213203435596)) ;
#85867 = CARTESIAN_POINT('Origin',(55.3573593128808,245.1,30.8213203435596)) ;
#85868 = CARTESIAN_POINT('Origin',(39.95,245.1,30.8213203435596)) ;
#85869 = CARTESIAN_POINT('Origin',(46.8,245.1,30.8213203435596)) ;
#85870 = CARTESIAN_POINT('Origin',(46.8,245.6,30.8213203435596)) ;
#85871 = CARTESIAN_POINT('Origin',(79.7999999999999,259.648528137424,19.9213203435596)) ;
#85872 = CARTESIAN_POINT('Origin',(26.8,245.6,30.8213203435596)) ;
#85873 = CARTESIAN_POINT('',(26.8,245.,30.8213203435596)) ;
#85874 = CARTESIAN_POINT('Origin',(26.8,245.1,30.8213203435596)) ;
#85875 = CARTESIAN_POINT('Origin',(26.8,245.6,30.8213203435596)) ;
#85876 = CARTESIAN_POINT('Origin',(39.95,245.1,30.8213203435596)) ;
#85877 = CARTESIAN_POINT('',(33.6,245.,30.8213203435596)) ;
#85878 = CARTESIAN_POINT('Origin',(33.6,245.1,30.8213203435596)) ;
#85879 = CARTESIAN_POINT('',(39.95,245.,30.8213203435596)) ;
#85880 = CARTESIAN_POINT('Origin',(33.6,245.6,30.8213203435596)) ;
#85881 = CARTESIAN_POINT('',(34.2,245.6,30.8213203435596)) ;
#85882 = CARTESIAN_POINT('Origin',(34.1,245.6,30.8213203435596)) ;
#85883 = CARTESIAN_POINT('Origin',(33.6,245.6,30.8213203435596)) ;
#85884 = CARTESIAN_POINT('Origin',(34.1000000000001,244.191753592594,30.8213203435596)) ;
#85885 = CARTESIAN_POINT('',(34.2000000000001,244.191753592594,30.8213203435596)) ;
#85886 = CARTESIAN_POINT('Origin',(51.2,257.,30.1213203435596)) ;
#85887 = CARTESIAN_POINT('',(49.,257.,30.3213203435596)) ;
#85888 = CARTESIAN_POINT('Origin',(49.,257.,30.1213203435596)) ;
#85889 = CARTESIAN_POINT('Origin',(51.2,257.,30.3213203435596)) ;
#85890 = CARTESIAN_POINT('Origin',(51.2,257.,30.3213203435596)) ;
#85891 = CARTESIAN_POINT('',(53.8,257.,30.3213203435596)) ;
#85892 = CARTESIAN_POINT('Origin',(51.2,257.,30.3213203435596)) ;
#85893 = CARTESIAN_POINT('Origin',(51.2,257.,30.5213203435596)) ;
#85894 = CARTESIAN_POINT('',(48.4,257.,30.5213203435596)) ;
#85895 = CARTESIAN_POINT('',(54.,257.,30.5213203435596)) ;
#85896 = CARTESIAN_POINT('Origin',(51.2,257.,30.5213203435596)) ;
#85897 = CARTESIAN_POINT('Origin',(53.8,257.,30.5213203435596)) ;
#85898 = CARTESIAN_POINT('Origin',(51.2,257.,30.5213203435596)) ;
#85899 = CARTESIAN_POINT('Origin',(51.2,257.,30.9213203435596)) ;
#85900 = CARTESIAN_POINT('',(48.4,257.,30.8969367901425)) ;
#85901 = CARTESIAN_POINT('Origin',(51.2,257.,30.8969367901425)) ;
#85902 = CARTESIAN_POINT('',(48.4,257.,30.9213203435596)) ;
#85903 = CARTESIAN_POINT('Origin',(51.2,257.,30.8969367901425)) ;
#85904 = CARTESIAN_POINT('',(48.3936201934668,257.,30.9470488713393)) ;
#85905 = CARTESIAN_POINT('Origin',(48.2,257.,30.8969367901425)) ;
#85906 = CARTESIAN_POINT('',(54.0063798065332,257.,30.9470488713393)) ;
#85907 = CARTESIAN_POINT('Origin',(51.2,257.,30.9470488713393)) ;
#85908 = CARTESIAN_POINT('Origin',(51.2,257.,30.9470488713393)) ;
#85909 = CARTESIAN_POINT('Origin',(73.2,257.,30.8969367901425)) ;
#85910 = CARTESIAN_POINT('',(70.3999999999999,257.,30.8969367901425)) ;
#85911 = CARTESIAN_POINT('Origin',(73.2,257.,30.8969367901425)) ;
#85912 = CARTESIAN_POINT('',(70.3936201934668,257.,30.9470488713393)) ;
#85913 = CARTESIAN_POINT('Origin',(70.2,257.,30.8969367901425)) ;
#85914 = CARTESIAN_POINT('',(76.0063798065332,257.,30.9470488713393)) ;
#85915 = CARTESIAN_POINT('Origin',(73.2,257.,30.9470488713393)) ;
#85916 = CARTESIAN_POINT('Origin',(73.2,257.,30.9470488713393)) ;
#85917 = CARTESIAN_POINT('Origin',(73.2,257.,30.9213203435596)) ;
#85918 = CARTESIAN_POINT('',(70.4,257.,30.5213203435596)) ;
#85919 = CARTESIAN_POINT('',(70.4,257.,30.9213203435596)) ;
#85920 = CARTESIAN_POINT('',(76.,257.,30.5213203435596)) ;
#85921 = CARTESIAN_POINT('Origin',(73.2,257.,30.5213203435596)) ;
#85922 = CARTESIAN_POINT('Origin',(73.2,257.,30.5213203435596)) ;
#85923 = CARTESIAN_POINT('Origin',(73.2,257.,30.5213203435596)) ;
#85924 = CARTESIAN_POINT('',(75.8,257.,30.3213203435596)) ;
#85925 = CARTESIAN_POINT('Origin',(75.8,257.,30.5213203435596)) ;
#85926 = CARTESIAN_POINT('Origin',(73.2,257.,30.3213203435596)) ;
#85927 = CARTESIAN_POINT('Origin',(73.2,257.,30.3213203435596)) ;
#85928 = CARTESIAN_POINT('',(71.,257.,30.3213203435596)) ;
#85929 = CARTESIAN_POINT('Origin',(73.2,257.,30.3213203435596)) ;
#85930 = CARTESIAN_POINT('Origin',(73.2,257.,30.1213203435596)) ;
#85931 = CARTESIAN_POINT('',(71.2,257.,30.1213203435596)) ;
#85932 = CARTESIAN_POINT('Origin',(73.2,257.,30.1213203435596)) ;
#85933 = CARTESIAN_POINT('Origin',(71.,257.,30.1213203435596)) ;
#85934 = CARTESIAN_POINT('Origin',(73.2,257.,19.9213203435596)) ;
#85935 = CARTESIAN_POINT('',(71.2,257.,29.6213203435596)) ;
#85936 = CARTESIAN_POINT('Origin',(73.2,257.,29.6213203435596)) ;
#85937 = CARTESIAN_POINT('',(71.2,257.,19.9213203435596)) ;
#85938 = CARTESIAN_POINT('Origin',(75.7500000000001,218.,30.8969367901425)) ;
#85939 = CARTESIAN_POINT('',(72.9500000000001,218.,30.8969367901425)) ;
#85940 = CARTESIAN_POINT('Origin',(75.7500000000001,218.,30.8969367901425)) ;
#85941 = CARTESIAN_POINT('',(72.9436201934669,218.,30.9470488713393)) ;
#85942 = CARTESIAN_POINT('Origin',(72.7500000000001,218.,30.8969367901425)) ;
#85943 = CARTESIAN_POINT('',(78.5563798065333,218.,30.9470488713393)) ;
#85944 = CARTESIAN_POINT('Origin',(75.7500000000001,218.,30.9470488713393)) ;
#85945 = CARTESIAN_POINT('Origin',(75.7500000000001,218.,30.9470488713393)) ;
#85946 = CARTESIAN_POINT('Origin',(75.7500000000001,218.,30.9213203435596)) ;
#85947 = CARTESIAN_POINT('',(72.9500000000001,218.,30.5213203435596)) ;
#85948 = CARTESIAN_POINT('',(72.9500000000001,218.,30.9213203435596)) ;
#85949 = CARTESIAN_POINT('',(78.5500000000001,218.,30.5213203435596)) ;
#85950 = CARTESIAN_POINT('Origin',(75.7500000000001,218.,30.5213203435596)) ;
#85951 = CARTESIAN_POINT('Origin',(75.7500000000001,218.,30.5213203435596)) ;
#85952 = CARTESIAN_POINT('Origin',(75.7500000000001,218.,30.1213203435596)) ;
#85953 = CARTESIAN_POINT('',(73.5500000000001,218.,30.3213203435596)) ;
#85954 = CARTESIAN_POINT('Origin',(73.5500000000001,218.,30.1213203435596)) ;
#85955 = CARTESIAN_POINT('Origin',(75.7500000000001,218.,30.3213203435596)) ;
#85956 = CARTESIAN_POINT('Origin',(75.7500000000001,218.,30.3213203435596)) ;
#85957 = CARTESIAN_POINT('',(78.3500000000001,218.,30.3213203435596)) ;
#85958 = CARTESIAN_POINT('Origin',(75.7500000000001,218.,30.3213203435596)) ;
#85959 = CARTESIAN_POINT('Origin',(75.7500000000001,218.,30.5213203435596)) ;
#85960 = CARTESIAN_POINT('Origin',(78.3500000000001,218.,30.5213203435596)) ;
#85961 = CARTESIAN_POINT('Origin',(51.2,257.,30.6213203435596)) ;
#85962 = CARTESIAN_POINT('Origin',(55.2649110640674,257.,30.6213203435596)) ;
#85963 = CARTESIAN_POINT('Origin',(73.2,257.,30.6213203435596)) ;
#85964 = CARTESIAN_POINT('Origin',(77.2649110640674,257.,30.6213203435596)) ;
#85965 = CARTESIAN_POINT('Origin',(75.7500000000001,218.,30.6213203435596)) ;
#85966 = CARTESIAN_POINT('Origin',(79.8149110640674,218.,30.6213203435596)) ;
#85967 = CARTESIAN_POINT('Origin',(73.2,257.,29.6213203435596)) ;
#85968 = CARTESIAN_POINT('Origin',(33.6,245.6,19.9213203435596)) ;
#85969 = CARTESIAN_POINT('',(33.6,245.,19.9213203435596)) ;
#85970 = CARTESIAN_POINT('',(34.2,245.6,19.9213203435596)) ;
#85971 = CARTESIAN_POINT('Origin',(26.2,245.,19.9213203435596)) ;
#85972 = CARTESIAN_POINT('',(26.8,245.,19.9213203435596)) ;
#85973 = CARTESIAN_POINT('Origin',(26.8,245.6,19.9213203435596)) ;
#85974 = CARTESIAN_POINT('Origin',(75.5999999999993,225.9,19.9213203435596)) ;
#85975 = CARTESIAN_POINT('Origin',(75.1999999999994,230.5,19.9213203435596)) ;
#85976 = CARTESIAN_POINT('Origin',(75.5999999999994,230.1,19.9213203435596)) ;
#85977 = CARTESIAN_POINT('Origin',(80.199999999999,230.5,19.9213203435596)) ;
#85978 = CARTESIAN_POINT('Origin',(80.199999999999,253.5,19.9213203435596)) ;
#85979 = CARTESIAN_POINT('Ctrl Pts',(46.8995772828086,264.999999634466,30.7206748684131)) ;
#85980 = CARTESIAN_POINT('Ctrl Pts',(46.8996347166691,265.000098160446,30.900346512201)) ;
#85981 = CARTESIAN_POINT('Ctrl Pts',(46.8518142718604,264.918063685094,31.2588421307007)) ;
#85982 = CARTESIAN_POINT('Ctrl Pts',(46.6177377231473,264.516555192435,31.7637752135733)) ;
#85983 = CARTESIAN_POINT('Ctrl Pts',(46.3570192595451,264.069339743442,31.9213203435596)) ;
#85984 = CARTESIAN_POINT('Ctrl Pts',(46.2,263.8,31.9213203435596)) ;
#85985 = CARTESIAN_POINT('Ctrl Pts',(47.0306190770353,265.00011652697,30.7206035829153)) ;
#85986 = CARTESIAN_POINT('Ctrl Pts',(47.0307043719217,265.0002417701,30.9201211188153)) ;
#85987 = CARTESIAN_POINT('Ctrl Pts',(46.9596768730597,264.895948135418,31.3129265397466)) ;
#85988 = CARTESIAN_POINT('Ctrl Pts',(46.6673261574499,264.467185432906,31.790097128723)) ;
#85989 = CARTESIAN_POINT('Ctrl Pts',(46.3757393401946,264.050619662792,31.9213203435596)) ;
#85990 = CARTESIAN_POINT('Ctrl Pts',(46.2,263.8,31.9213203435596)) ;
#85991 = CARTESIAN_POINT('Ctrl Pts',(47.2915525808353,264.891552580839,30.7205226506387)) ;
#85992 = CARTESIAN_POINT('Ctrl Pts',(47.2916923685089,264.891692368513,30.9425726727612)) ;
#85993 = CARTESIAN_POINT('Ctrl Pts',(47.175274965989,264.775274965993,31.372780469797)) ;
#85994 = CARTESIAN_POINT('Ctrl Pts',(46.7673172266825,264.367317226684,31.8157593328667)) ;
#85995 = CARTESIAN_POINT('Ctrl Pts',(46.4131795014931,264.013179501493,31.9213203435596)) ;
#85996 = CARTESIAN_POINT('Ctrl Pts',(46.2,263.8,31.9213203435596)) ;
#85997 = CARTESIAN_POINT('Ctrl Pts',(47.400116526968,264.630619077042,30.7206035829153)) ;
#85998 = CARTESIAN_POINT('Ctrl Pts',(47.4002417700975,264.630704371928,30.9201211188158)) ;
#85999 = CARTESIAN_POINT('Ctrl Pts',(47.295948135415,264.559676873064,31.3129265397479)) ;
#86000 = CARTESIAN_POINT('Ctrl Pts',(46.8671854329034,264.267326157452,31.7900971287236)) ;
#86001 = CARTESIAN_POINT('Ctrl Pts',(46.4506196627917,263.975739340196,31.9213203435596)) ;
#86002 = CARTESIAN_POINT('Ctrl Pts',(46.2,263.8,31.9213203435596)) ;
#86003 = CARTESIAN_POINT('Ctrl Pts',(47.3999996344655,264.499577282817,30.7206748684131)) ;
#86004 = CARTESIAN_POINT('Ctrl Pts',(47.4000981604458,264.499634716678,30.9003465122023)) ;
#86005 = CARTESIAN_POINT('Ctrl Pts',(47.3180636850924,264.451814271868,31.2588421307041)) ;
#86006 = CARTESIAN_POINT('Ctrl Pts',(46.9165551924319,264.21773772315,31.763775213575)) ;
#86007 = CARTESIAN_POINT('Ctrl Pts',(46.4693397434408,263.957019259546,31.9213203435596)) ;
#86008 = CARTESIAN_POINT('Ctrl Pts',(46.2,263.8,31.9213203435596)) ;
#86009 = CARTESIAN_POINT('Origin',(46.2,263.8,30.7213203435596)) ;
#86010 = CARTESIAN_POINT('',(47.4,264.5,30.7213203435596)) ;
#86011 = CARTESIAN_POINT('Origin',(46.2,263.8,30.7213203435596)) ;
#86012 = CARTESIAN_POINT('Origin',(46.9,264.5,30.7213203435596)) ;
#86013 = CARTESIAN_POINT('Ctrl Pts',(55.0000127765018,264.497506774224,30.717524648916)) ;
#86014 = CARTESIAN_POINT('Ctrl Pts',(54.99912644432,264.498021883759,30.9874956561826)) ;
#86015 = CARTESIAN_POINT('Ctrl Pts',(55.2172274582073,264.371268236017,31.6180363905289)) ;
#86016 = CARTESIAN_POINT('Ctrl Pts',(55.8404866413515,264.008965312001,31.9213203435596)) ;
#86017 = CARTESIAN_POINT('Ctrl Pts',(56.2,263.8,31.9213203435596)) ;
#86018 = CARTESIAN_POINT('Ctrl Pts',(54.9993214128065,264.629240949551,30.7170995183319)) ;
#86019 = CARTESIAN_POINT('Ctrl Pts',(54.9981949105548,264.629996957963,31.0173898959233)) ;
#86020 = CARTESIAN_POINT('Ctrl Pts',(55.2755991661809,264.443841808721,31.6781435477989)) ;
#86021 = CARTESIAN_POINT('Ctrl Pts',(55.8655779824594,264.034056653109,31.9213203435596)) ;
#86022 = CARTESIAN_POINT('Ctrl Pts',(56.2,263.8,31.9213203435596)) ;
#86023 = CARTESIAN_POINT('Ctrl Pts',(55.1080548223873,264.891945177613,30.7166163696442)) ;
#86024 = CARTESIAN_POINT('Ctrl Pts',(55.1068252095724,264.893174790428,31.0513754562231)) ;
#86025 = CARTESIAN_POINT('Ctrl Pts',(55.4097601276945,264.590239872305,31.7407074319743)) ;
#86026 = CARTESIAN_POINT('Ctrl Pts',(55.9157606646752,264.084239335325,31.9213203435596)) ;
#86027 = CARTESIAN_POINT('Ctrl Pts',(56.2,263.8,31.9213203435596)) ;
#86028 = CARTESIAN_POINT('Ctrl Pts',(55.3707590504493,265.000678587193,30.7170995183319)) ;
#86029 = CARTESIAN_POINT('Ctrl Pts',(55.3700030420373,265.001805089445,31.0173898959233)) ;
#86030 = CARTESIAN_POINT('Ctrl Pts',(55.5561581912784,264.724400833819,31.6781435477988)) ;
#86031 = CARTESIAN_POINT('Ctrl Pts',(55.965943346891,264.134422017541,31.9213203435596)) ;
#86032 = CARTESIAN_POINT('Ctrl Pts',(56.2,263.8,31.9213203435596)) ;
#86033 = CARTESIAN_POINT('Ctrl Pts',(55.5024932257763,264.999987223498,30.7175246489159)) ;
#86034 = CARTESIAN_POINT('Ctrl Pts',(55.5019781162411,265.00087355568,30.9874956561826)) ;
#86035 = CARTESIAN_POINT('Ctrl Pts',(55.6287317639835,264.782772541792,31.6180363905288)) ;
#86036 = CARTESIAN_POINT('Ctrl Pts',(55.9910346879988,264.159513358648,31.9213203435596)) ;
#86037 = CARTESIAN_POINT('Ctrl Pts',(56.2,263.8,31.9213203435596)) ;
#86038 = CARTESIAN_POINT('',(55.,264.5,30.7213203435596)) ;
#86039 = CARTESIAN_POINT('',(55.3522605104815,264.294514702219,31.5706363965757)) ;
#86040 = CARTESIAN_POINT('Origin',(56.2,263.8,30.7213203435596)) ;
#86041 = CARTESIAN_POINT('Origin',(56.2,263.8,30.7213203435596)) ;
#86042 = CARTESIAN_POINT('',(55.7054852977724,264.647739489533,31.5706363965612)) ;
#86043 = CARTESIAN_POINT('Origin',(56.2,263.8,30.7213203435596)) ;
#86044 = CARTESIAN_POINT('Origin',(56.2,263.8,30.7213203435596)) ;
#86045 = CARTESIAN_POINT('Origin',(55.5,264.5,30.7213203435596)) ;
#86046 = CARTESIAN_POINT('Ctrl Pts',(68.8975058001088,264.999987213392,30.7175231713329)) ;
#86047 = CARTESIAN_POINT('Ctrl Pts',(68.8980211176555,265.000873904652,30.9874944556892)) ;
#86048 = CARTESIAN_POINT('Ctrl Pts',(68.7712660652602,264.782770188553,31.618033084322)) ;
#86049 = CARTESIAN_POINT('Ctrl Pts',(68.4089651270207,264.159513543629,31.9213203435596)) ;
#86050 = CARTESIAN_POINT('Ctrl Pts',(68.2,263.8,31.9213203435596)) ;
#86051 = CARTESIAN_POINT('Ctrl Pts',(69.0292403053076,265.000678853629,30.7170978723306)) ;
#86052 = CARTESIAN_POINT('Ctrl Pts',(69.0299966176013,265.001805816084,31.0173888110261)) ;
#86053 = CARTESIAN_POINT('Ctrl Pts',(68.8438397072984,264.72439710198,31.678134090218)) ;
#86054 = CARTESIAN_POINT('Ctrl Pts',(68.4340565297887,264.134422140861,31.9213203435596)) ;
#86055 = CARTESIAN_POINT('Ctrl Pts',(68.2,263.8,31.9213203435596)) ;
#86056 = CARTESIAN_POINT('Ctrl Pts',(69.2919444837221,264.891944483736,30.7166145318953)) ;
#86057 = CARTESIAN_POINT('Ctrl Pts',(69.293174578849,264.893174578863,31.0513745401012)) ;
#86058 = CARTESIAN_POINT('Ctrl Pts',(68.990239681009,264.590239681019,31.7406867780937)) ;
#86059 = CARTESIAN_POINT('Ctrl Pts',(68.4842393353228,264.084239335327,31.9213203435596)) ;
#86060 = CARTESIAN_POINT('Ctrl Pts',(68.2,263.8,31.9213203435596)) ;
#86061 = CARTESIAN_POINT('Ctrl Pts',(69.400678853621,264.629240305328,30.7170978723306)) ;
#86062 = CARTESIAN_POINT('Ctrl Pts',(69.4018058160759,264.629996617621,31.0173888110287)) ;
#86063 = CARTESIAN_POINT('Ctrl Pts',(69.12439710197,264.443839707309,31.6781340902227)) ;
#86064 = CARTESIAN_POINT('Ctrl Pts',(68.5344221408571,264.034056529793,31.9213203435596)) ;
#86065 = CARTESIAN_POINT('Ctrl Pts',(68.2,263.8,31.9213203435596)) ;
#86066 = CARTESIAN_POINT('Ctrl Pts',(69.3999872133923,264.497505800138,30.7175231713328)) ;
#86067 = CARTESIAN_POINT('Ctrl Pts',(69.4008739046523,264.498021117685,30.9874944556959)) ;
#86068 = CARTESIAN_POINT('Ctrl Pts',(69.1827701885397,264.371266065276,31.6180330843354)) ;
#86069 = CARTESIAN_POINT('Ctrl Pts',(68.5595135436233,264.008965127026,31.9213203435596)) ;
#86070 = CARTESIAN_POINT('Ctrl Pts',(68.2,263.8,31.9213203435596)) ;
#86071 = CARTESIAN_POINT('',(68.694428877676,264.64759236173,31.570783225819)) ;
#86072 = CARTESIAN_POINT('Origin',(68.2,263.8,30.7213203435596)) ;
#86073 = CARTESIAN_POINT('Origin',(68.2,263.8,30.7213203435596)) ;
#86074 = CARTESIAN_POINT('',(69.0475923616046,264.294428877603,31.5707832259444)) ;
#86075 = CARTESIAN_POINT('Origin',(68.2,263.8,30.7213203435596)) ;
#86076 = CARTESIAN_POINT('',(69.4,264.5,30.7213203435596)) ;
#86077 = CARTESIAN_POINT('Origin',(68.2,263.8,30.7213203435596)) ;
#86078 = CARTESIAN_POINT('Origin',(68.9,264.5,30.7213203435596)) ;
#86079 = CARTESIAN_POINT('Ctrl Pts',(77.0000127930585,264.497505178544,30.7175222285172)) ;
#86080 = CARTESIAN_POINT('Ctrl Pts',(76.999125872671,264.498020628823,30.9874936896829)) ;
#86081 = CARTESIAN_POINT('Ctrl Pts',(77.2172313133203,264.371264679952,31.6180309744835)) ;
#86082 = CARTESIAN_POINT('Ctrl Pts',(77.8404863383386,264.008965008988,31.9213203435596)) ;
#86083 = CARTESIAN_POINT('Ctrl Pts',(78.2,263.8,31.9213203435596)) ;
#86084 = CARTESIAN_POINT('Ctrl Pts',(76.999320976368,264.629239894225,30.7170968220494)) ;
#86085 = CARTESIAN_POINT('Ctrl Pts',(76.9981937202562,264.629996400424,31.0173881187927)) ;
#86086 = CARTESIAN_POINT('Ctrl Pts',(77.2756052796858,264.44383836622,31.6781280546311)) ;
#86087 = CARTESIAN_POINT('Ctrl Pts',(77.8655777804508,264.034056451101,31.9213203435596)) ;
#86088 = CARTESIAN_POINT('Ctrl Pts',(78.2,263.8,31.9213203435596)) ;
#86089 = CARTESIAN_POINT('Ctrl Pts',(77.1080559582206,264.891944041766,30.7166133592621)) ;
#86090 = CARTESIAN_POINT('Ctrl Pts',(77.1068255553296,264.893174444657,31.0513739555782)) ;
#86091 = CARTESIAN_POINT('Ctrl Pts',(77.4097604424929,264.590239557496,31.7406735987709)) ;
#86092 = CARTESIAN_POINT('Ctrl Pts',(77.9157606646733,264.084239335323,31.9213203435596)) ;
#86093 = CARTESIAN_POINT('Ctrl Pts',(78.2,263.8,31.9213203435596)) ;
#86094 = CARTESIAN_POINT('Ctrl Pts',(77.370760105756,265.000679023624,30.7170968220493)) ;
#86095 = CARTESIAN_POINT('Ctrl Pts',(77.3700035995569,265.001806279736,31.0173881187952)) ;
#86096 = CARTESIAN_POINT('Ctrl Pts',(77.5561616337687,264.724394720305,31.6781280546357)) ;
#86097 = CARTESIAN_POINT('Ctrl Pts',(77.965943548896,264.134422219546,31.9213203435596)) ;
#86098 = CARTESIAN_POINT('Ctrl Pts',(78.2,263.8,31.9213203435596)) ;
#86099 = CARTESIAN_POINT('Ctrl Pts',(77.5024948214269,264.999987206942,30.7175222285171)) ;
#86100 = CARTESIAN_POINT('Ctrl Pts',(77.5019793711485,265.000874127329,30.9874936896894)) ;
#86101 = CARTESIAN_POINT('Ctrl Pts',(77.6287353200318,264.782768686667,31.6180309744965)) ;
#86102 = CARTESIAN_POINT('Ctrl Pts',(77.9910349910063,264.159513661656,31.9213203435596)) ;
#86103 = CARTESIAN_POINT('Ctrl Pts',(78.2,263.8,31.9213203435596)) ;
#86104 = CARTESIAN_POINT('',(77.,264.5,30.7213203435596)) ;
#86105 = CARTESIAN_POINT('',(77.3525015634302,264.294374087999,31.5708769337946)) ;
#86106 = CARTESIAN_POINT('Origin',(78.2,263.8,30.7213203435596)) ;
#86107 = CARTESIAN_POINT('Origin',(78.2,263.8,30.7213203435596)) ;
#86108 = CARTESIAN_POINT('Origin',(77.5,264.5,30.7213203435596)) ;
#86109 = CARTESIAN_POINT('Origin',(78.2,252.191753592594,30.7213203435596)) ;
#86110 = CARTESIAN_POINT('',(77.,263.763591785235,30.7213203435596)) ;
#86111 = CARTESIAN_POINT('',(77.,252.191753592594,30.7213203435596)) ;
#86112 = CARTESIAN_POINT('Origin',(78.2,263.763591785235,30.7213203435596)) ;
#86113 = CARTESIAN_POINT('Ctrl Pts',(76.4995190226377,262.026327156306,31.9213203435596)) ;
#86114 = CARTESIAN_POINT('Ctrl Pts',(76.8811596225238,262.026212180825,31.9213203435596)) ;
#86115 = CARTESIAN_POINT('Ctrl Pts',(77.5148352095089,262.254066418952,31.9213203435596)) ;
#86116 = CARTESIAN_POINT('Ctrl Pts',(78.0836688954258,262.984975488253,31.9213203435596)) ;
#86117 = CARTESIAN_POINT('Ctrl Pts',(78.2000733801637,263.504024694381,31.9213203435596)) ;
#86118 = CARTESIAN_POINT('Ctrl Pts',(78.1999999305895,263.764083305616,31.9213203435596)) ;
#86119 = CARTESIAN_POINT('Ctrl Pts',(76.4996093403379,262.337938596679,31.9213203432719)) ;
#86120 = CARTESIAN_POINT('Ctrl Pts',(76.8095855113217,262.337841295896,31.9213207998724)) ;
#86121 = CARTESIAN_POINT('Ctrl Pts',(77.3248206408524,262.530669626882,31.9204156081284)) ;
#86122 = CARTESIAN_POINT('Ctrl Pts',(77.7690289165673,263.136266572609,31.9210372315204)) ;
#86123 = CARTESIAN_POINT('Ctrl Pts',(77.848207800611,263.556750307023,31.9210300573126)) ;
#86124 = CARTESIAN_POINT('Ctrl Pts',(77.8409471725199,263.763983467654,31.9213208928997)) ;
#86125 = CARTESIAN_POINT('Ctrl Pts',(76.4997657781298,262.879952924587,31.697544092197)) ;
#86126 = CARTESIAN_POINT('Ctrl Pts',(76.685613962614,262.879887256888,31.6975487112581)) ;
#86127 = CARTESIAN_POINT('Ctrl Pts',(76.9925944092368,263.010027791412,31.6883950616448)) ;
#86128 = CARTESIAN_POINT('Ctrl Pts',(77.2228704336,263.397819282277,31.6563868166324)) ;
#86129 = CARTESIAN_POINT('Ctrl Pts',(77.238135214489,263.647341999612,31.6322498913161)) ;
#86130 = CARTESIAN_POINT('Ctrl Pts',(77.2194335073132,263.763811927863,31.6196189939447)) ;
#86131 = CARTESIAN_POINT('Ctrl Pts',(76.4998448149111,263.152594688376,31.1969452376454)) ;
#86132 = CARTESIAN_POINT('Ctrl Pts',(76.6229793650612,263.152550698014,31.1969584257997)) ;
#86133 = CARTESIAN_POINT('Ctrl Pts',(76.8274272241081,263.23973060012,31.1708228417253)) ;
#86134 = CARTESIAN_POINT('Ctrl Pts',(76.9892209015336,263.503877433016,31.0845228152707)) ;
#86135 = CARTESIAN_POINT('Ctrl Pts',(77.0082592674544,263.679638279009,31.0219906010643)) ;
#86136 = CARTESIAN_POINT('Ctrl Pts',(76.9998598913761,263.763750765635,30.99018357636)) ;
#86137 = CARTESIAN_POINT('Ctrl Pts',(76.4998585633068,263.20068211308,30.9680799623059)) ;
#86138 = CARTESIAN_POINT('Ctrl Pts',(76.6120841869172,263.200644865691,30.968096329597)) ;
#86139 = CARTESIAN_POINT('Ctrl Pts',(76.7984234856098,263.27446038894,30.9356602252213)) ;
#86140 = CARTESIAN_POINT('Ctrl Pts',(76.9657383928732,263.511275997684,30.831616819832)) ;
#86141 = CARTESIAN_POINT('Ctrl Pts',(77.0000051280261,263.679472135069,30.7577337022785)) ;
#86142 = CARTESIAN_POINT('Ctrl Pts',(77.0000001340552,263.763751075536,30.720717075604)) ;
#86143 = CARTESIAN_POINT('Origin',(76.5,262.026327083856,30.7213203435596)) ;
#86144 = CARTESIAN_POINT('Origin',(76.5,263.763591785235,30.7213203435596)) ;
#86145 = CARTESIAN_POINT('Origin',(64.4,262.026327083856,30.7213203435596)) ;
#86146 = CARTESIAN_POINT('Origin',(69.9,262.026327083856,30.7213203435596)) ;
#86147 = CARTESIAN_POINT('Ctrl Pts',(68.1983125112596,263.765148977383,31.9213190650864)) ;
#86148 = CARTESIAN_POINT('Ctrl Pts',(68.1980077983924,263.374417823647,31.9213212039938)) ;
#86149 = CARTESIAN_POINT('Ctrl Pts',(68.5095269157522,262.461458547847,31.9213224688896)) ;
#86150 = CARTESIAN_POINT('Ctrl Pts',(69.3919168992797,262.024364125748,31.9213193980855)) ;
#86151 = CARTESIAN_POINT('Ctrl Pts',(69.9015236996613,262.024862823348,31.9213194015866)) ;
#86152 = CARTESIAN_POINT('Ctrl Pts',(68.5579695947186,263.764832436952,31.9218621048563)) ;
#86153 = CARTESIAN_POINT('Ctrl Pts',(68.5469047154847,263.45353874313,31.9213904806212)) ;
#86154 = CARTESIAN_POINT('Ctrl Pts',(68.7720647452498,262.70680443246,31.9210845767404)) ;
#86155 = CARTESIAN_POINT('Ctrl Pts',(69.4873911960094,262.336546050699,31.9217215128341)) ;
#86156 = CARTESIAN_POINT('Ctrl Pts',(69.901237377907,262.336968483875,31.9217207866612)) ;
#86157 = CARTESIAN_POINT('Ctrl Pts',(69.1805657273697,263.764288546693,31.6200744602099)) ;
#86158 = CARTESIAN_POINT('Ctrl Pts',(69.1523633773431,263.589485112743,31.6390141732535)) ;
#86159 = CARTESIAN_POINT('Ctrl Pts',(69.2295848925071,263.131551068329,31.6803391920196)) ;
#86160 = CARTESIAN_POINT('Ctrl Pts',(69.6527467734552,262.879525187827,31.6979704437927)) ;
#86161 = CARTESIAN_POINT('Ctrl Pts',(69.9007414815215,262.879812711463,31.6979503261674)) ;
#86162 = CARTESIAN_POINT('Ctrl Pts',(69.4002579350921,263.764094862603,30.9898143483238)) ;
#86163 = CARTESIAN_POINT('Ctrl Pts',(69.3875802847056,263.637875419481,31.0375709322432)) ;
#86164 = CARTESIAN_POINT('Ctrl Pts',(69.4541887094701,263.320310298445,31.1465777171764)) ;
#86165 = CARTESIAN_POINT('Ctrl Pts',(69.7362429697597,263.152507028698,31.196812365578)) ;
#86166 = CARTESIAN_POINT('Ctrl Pts',(69.900491089929,263.152698471114,31.1967550496367)) ;
#86167 = CARTESIAN_POINT('Ctrl Pts',(69.3999996982701,263.764095954884,30.7202075564157)) ;
#86168 = CARTESIAN_POINT('Ctrl Pts',(69.3999369107821,263.63758951881,30.7757813606872)) ;
#86169 = CARTESIAN_POINT('Ctrl Pts',(69.4915234368195,263.342047582185,30.9056533534648)) ;
#86170 = CARTESIAN_POINT('Ctrl Pts',(69.7507436235131,263.200584779449,30.9678467447103)) ;
#86171 = CARTESIAN_POINT('Ctrl Pts',(69.9004476076753,263.200746179747,30.9677757859222)) ;
#86172 = CARTESIAN_POINT('',(69.4,263.763591785235,30.7213203435597)) ;
#86173 = CARTESIAN_POINT('Origin',(68.2,263.763591785235,30.7213203435596)) ;
#86174 = CARTESIAN_POINT('Origin',(69.9,263.763591785235,30.7213203435596)) ;
#86175 = CARTESIAN_POINT('Origin',(68.2,251.191753592594,30.7213203435596)) ;
#86176 = CARTESIAN_POINT('',(69.4,251.191753592594,30.7213203435596)) ;
#86177 = CARTESIAN_POINT('Origin',(66.4499999999999,263.8,30.7213203435596)) ;
#86178 = CARTESIAN_POINT('Origin',(56.2,252.191753592594,30.7213203435596)) ;
#86179 = CARTESIAN_POINT('',(55.,263.763591785235,30.7213203435596)) ;
#86180 = CARTESIAN_POINT('',(55.,252.191753592594,30.7213203435596)) ;
#86181 = CARTESIAN_POINT('Origin',(56.2,263.763591785235,30.7213203435596)) ;
#86182 = CARTESIAN_POINT('Ctrl Pts',(54.4995191990323,262.026327156252,31.9213203435596)) ;
#86183 = CARTESIAN_POINT('Ctrl Pts',(54.8811597389274,262.026212224654,31.9213203435596)) ;
#86184 = CARTESIAN_POINT('Ctrl Pts',(55.5148367741968,262.25406310381,31.9213203435596)) ;
#86185 = CARTESIAN_POINT('Ctrl Pts',(56.0836704564179,262.98497327714,31.9213203435596)) ;
#86186 = CARTESIAN_POINT('Ctrl Pts',(56.2000733522523,263.50402457578,31.9213203435596)) ;
#86187 = CARTESIAN_POINT('Ctrl Pts',(56.1999999306414,263.764083125354,31.9213203435596)) ;
#86188 = CARTESIAN_POINT('Ctrl Pts',(54.4996094836088,262.337938596633,31.9213203432732)) ;
#86189 = CARTESIAN_POINT('Ctrl Pts',(54.8095856066388,262.337841334075,31.9213207980662)) ;
#86190 = CARTESIAN_POINT('Ctrl Pts',(55.324820581982,262.530664663494,31.9204188586157)) ;
#86191 = CARTESIAN_POINT('Ctrl Pts',(55.7690292246145,263.136262709219,31.9210399847418)) ;
#86192 = CARTESIAN_POINT('Ctrl Pts',(55.8482077820982,263.556750212249,31.9210300555789)) ;
#86193 = CARTESIAN_POINT('Ctrl Pts',(55.8409471775529,263.763983324007,31.9213208926998)) ;
#86194 = CARTESIAN_POINT('Ctrl Pts',(54.4997658640126,262.87995410944,31.6975454235242)) ;
#86195 = CARTESIAN_POINT('Ctrl Pts',(54.6856140321838,262.879888467203,31.6975500409814)) ;
#86196 = CARTESIAN_POINT('Ctrl Pts',(54.9925945661554,263.010026293502,31.6883962107278)) ;
#86197 = CARTESIAN_POINT('Ctrl Pts',(55.222870433538,263.397818932101,31.6563880739499)) ;
#86198 = CARTESIAN_POINT('Ctrl Pts',(55.2381328918591,263.647341932731,31.6322519116531)) ;
#86199 = CARTESIAN_POINT('Ctrl Pts',(55.2194312038371,263.763811847149,31.6196210183214)) ;
#86200 = CARTESIAN_POINT('Ctrl Pts',(54.4998448718075,263.15259463109,31.1969453407673)) ;
#86201 = CARTESIAN_POINT('Ctrl Pts',(54.6229794158692,263.152550658295,31.196958524294)) ;
#86202 = CARTESIAN_POINT('Ctrl Pts',(54.8274272512656,263.239727731085,31.1708225203607)) ;
#86203 = CARTESIAN_POINT('Ctrl Pts',(54.9892211600963,263.503875278608,31.0845224833632)) ;
#86204 = CARTESIAN_POINT('Ctrl Pts',(55.0082593119534,263.67963823302,31.0219907412878)) ;
#86205 = CARTESIAN_POINT('Ctrl Pts',(54.9998599440985,263.763750707344,30.9901837278691)) ;
#86206 = CARTESIAN_POINT('Ctrl Pts',(54.4998586151676,263.200682078159,30.9680801284357)) ;
#86207 = CARTESIAN_POINT('Ctrl Pts',(54.6120842290547,263.20064484498,30.9680964894767)) ;
#86208 = CARTESIAN_POINT('Ctrl Pts',(54.7984239677902,263.274459292836,30.9356608694408)) ;
#86209 = CARTESIAN_POINT('Ctrl Pts',(54.9657388695267,263.511275278549,30.8316173195593)) ;
#86210 = CARTESIAN_POINT('Ctrl Pts',(55.0000051257995,263.679472096755,30.7577339109711)) ;
#86211 = CARTESIAN_POINT('Ctrl Pts',(55.0000001339559,263.763751017118,30.7207172968552)) ;
#86212 = CARTESIAN_POINT('Origin',(54.5,262.026327083856,30.7213203435596)) ;
#86213 = CARTESIAN_POINT('Origin',(54.5,263.763591785235,30.7213203435596)) ;
#86214 = CARTESIAN_POINT('Origin',(53.4,262.026327083856,30.7213203435596)) ;
#86215 = CARTESIAN_POINT('Origin',(47.9,262.026327083856,30.7213203435596)) ;
#86216 = CARTESIAN_POINT('Ctrl Pts',(46.1983076282625,263.76515348891,31.9213190576818)) ;
#86217 = CARTESIAN_POINT('Ctrl Pts',(46.1980020403729,263.374419766008,31.9213212030712)) ;
#86218 = CARTESIAN_POINT('Ctrl Pts',(46.5095143637924,262.461447593742,31.9213224512428)) ;
#86219 = CARTESIAN_POINT('Ctrl Pts',(47.3919185200641,262.024358451223,31.9213193926338)) ;
#86220 = CARTESIAN_POINT('Ctrl Pts',(47.9015281138921,262.024858587217,31.9213193961311)) ;
#86221 = CARTESIAN_POINT('Ctrl Pts',(46.5579664947406,263.764836030645,31.921863668865)) ;
#86222 = CARTESIAN_POINT('Ctrl Pts',(46.5469008415638,263.453540510638,31.9213919346374)) ;
#86223 = CARTESIAN_POINT('Ctrl Pts',(46.7720552690258,262.706793116683,31.9210902454287)) ;
#86224 = CARTESIAN_POINT('Ctrl Pts',(47.4873927052263,262.336542026587,31.9217226657269)) ;
#86225 = CARTESIAN_POINT('Ctrl Pts',(47.9012409620629,262.33696567494,31.921721942615)) ;
#86226 = CARTESIAN_POINT('Ctrl Pts',(47.1805678274021,263.764290563759,31.6200780451729)) ;
#86227 = CARTESIAN_POINT('Ctrl Pts',(47.1523648718258,263.589486462611,31.639017761761)) ;
#86228 = CARTESIAN_POINT('Ctrl Pts',(47.229577444136,263.131548511894,31.6803418390727)) ;
#86229 = CARTESIAN_POINT('Ctrl Pts',(47.6527479151927,262.879524817036,31.6979732378616)) ;
#86230 = CARTESIAN_POINT('Ctrl Pts',(47.9007436285402,262.879813170893,31.6979530617955)) ;
#86231 = CARTESIAN_POINT('Ctrl Pts',(47.4002579617035,263.764096318685,30.9898141318404)) ;
#86232 = CARTESIAN_POINT('Ctrl Pts',(47.387579941251,263.637876445166,31.0375708922236)) ;
#86233 = CARTESIAN_POINT('Ctrl Pts',(47.4541847095435,263.32030586019,31.1465778444696)) ;
#86234 = CARTESIAN_POINT('Ctrl Pts',(47.7362438590021,263.152506333287,31.1968127976388)) ;
#86235 = CARTESIAN_POINT('Ctrl Pts',(47.9004925115266,263.152698325886,31.1967553153352)) ;
#86236 = CARTESIAN_POINT('Ctrl Pts',(47.3999996994773,263.764097414176,30.7202074191205)) ;
#86237 = CARTESIAN_POINT('Ctrl Pts',(47.3999365884846,263.637590496111,30.7757814206139)) ;
#86238 = CARTESIAN_POINT('Ctrl Pts',(47.4915207311276,263.342045075793,30.9056548931698)) ;
#86239 = CARTESIAN_POINT('Ctrl Pts',(47.750744453621,263.200584225821,30.9678473764369)) ;
#86240 = CARTESIAN_POINT('Ctrl Pts',(47.9004489033514,263.200746091367,30.9677762131617)) ;
#86241 = CARTESIAN_POINT('',(47.4,263.763591785235,30.7213203435596)) ;
#86242 = CARTESIAN_POINT('Origin',(46.2,263.763591785235,30.7213203435596)) ;
#86243 = CARTESIAN_POINT('Origin',(47.9,263.763591785235,30.7213203435596)) ;
#86244 = CARTESIAN_POINT('Origin',(46.2,251.191753592594,30.7213203435596)) ;
#86245 = CARTESIAN_POINT('',(47.4,251.191753592594,30.7213203435596)) ;
#86246 = CARTESIAN_POINT('Origin',(66.4499999999999,263.8,30.7213203435596)) ;
#86247 = CARTESIAN_POINT('Origin',(47.9,265.198823964111,23.9039674938989)) ;
#86248 = CARTESIAN_POINT('',(47.4,264.5,27.2233813234278)) ;
#86249 = CARTESIAN_POINT('Origin',(47.9,264.5,27.2233813234278)) ;
#86250 = CARTESIAN_POINT('',(47.4,265.198823964111,23.9039674938989)) ;
#86251 = CARTESIAN_POINT('Origin',(54.5,265.241264282414,23.7023759819625)) ;
#86252 = CARTESIAN_POINT('',(55.,264.5,27.2233813234279)) ;
#86253 = CARTESIAN_POINT('',(55.,265.241264282414,23.7023759819625)) ;
#86254 = CARTESIAN_POINT('Origin',(54.5,264.5,27.2233813234279)) ;
#86255 = CARTESIAN_POINT('Origin',(55.,265.,19.9213203435596)) ;
#86256 = CARTESIAN_POINT('',(55.,264.5,19.9213203435596)) ;
#86257 = CARTESIAN_POINT('Origin',(55.5,264.5,19.9213203435596)) ;
#86258 = CARTESIAN_POINT('Origin',(55.5,264.5,27.2233813234279)) ;
#86259 = CARTESIAN_POINT('Origin',(68.8999999999999,264.5,19.9213203435596)) ;
#86260 = CARTESIAN_POINT('',(69.4,264.5,27.2233813234278)) ;
#86261 = CARTESIAN_POINT('',(69.4,264.5,19.9213203435596)) ;
#86262 = CARTESIAN_POINT('Origin',(68.8999999999999,264.5,27.2233813234279)) ;
#86263 = CARTESIAN_POINT('Origin',(69.4,263.,19.9213203435596)) ;
#86264 = CARTESIAN_POINT('',(69.4,265.198823964111,23.9039674938989)) ;
#86265 = CARTESIAN_POINT('Origin',(69.9,265.198823964111,23.9039674938989)) ;
#86266 = CARTESIAN_POINT('Origin',(69.9,264.5,27.2233813234278)) ;
#86267 = CARTESIAN_POINT('Origin',(76.5,265.241264282414,23.7023759819625)) ;
#86268 = CARTESIAN_POINT('',(77.,264.5,27.2233813234279)) ;
#86269 = CARTESIAN_POINT('',(77.,265.241264282414,23.7023759819625)) ;
#86270 = CARTESIAN_POINT('Origin',(76.5,264.5,27.2233813234279)) ;
#86271 = CARTESIAN_POINT('Origin',(77.,265.,19.9213203435596)) ;
#86272 = CARTESIAN_POINT('',(77.,264.5,19.9213203435596)) ;
#86273 = CARTESIAN_POINT('Origin',(77.5,264.5,19.9213203435596)) ;
#86274 = CARTESIAN_POINT('Origin',(77.5,264.5,27.2233813234279)) ;
#86275 = CARTESIAN_POINT('Origin',(57.9573593128808,239.1,25.9213203435596)) ;
#86276 = CARTESIAN_POINT('',(57.9573593128808,239.1,25.9213203435596)) ;
#86277 = CARTESIAN_POINT('',(57.9573593128808,239.1,25.9213203435596)) ;
#86278 = CARTESIAN_POINT('',(58.9573593128808,239.1,25.9213203435596)) ;
#86279 = CARTESIAN_POINT('Origin',(57.9573593128808,241.9,25.9213203435596)) ;
#86280 = CARTESIAN_POINT('',(57.9573593128808,238.,25.9213203435596)) ;
#86281 = CARTESIAN_POINT('Origin',(58.4573593128808,240.5,25.9213203435596)) ;
#86282 = CARTESIAN_POINT('Origin',(28.2,259.5,25.9213203435596)) ;
#86283 = CARTESIAN_POINT('',(28.2,259.5,22.9213203435596)) ;
#86284 = CARTESIAN_POINT('',(28.2,259.5,25.9213203435596)) ;
#86285 = CARTESIAN_POINT('Origin',(28.2,262.3,25.9213203435596)) ;
#86286 = CARTESIAN_POINT('Origin',(28.2,263.4,19.9213203435596)) ;
#86287 = CARTESIAN_POINT('Origin',(80.199999999999,229.4,25.9213203435596)) ;
#86288 = CARTESIAN_POINT('',(80.199999999999,229.4,22.9213203435596)) ;
#86289 = CARTESIAN_POINT('',(80.199999999999,229.4,25.9213203435596)) ;
#86290 = CARTESIAN_POINT('Origin',(80.199999999999,226.6,25.9213203435596)) ;
#86291 = CARTESIAN_POINT('Origin',(80.199999999999,225.5,19.9213203435596)) ;
#86292 = CARTESIAN_POINT('Origin',(80.1999999999999,252.4,25.9213203435596)) ;
#86293 = CARTESIAN_POINT('',(80.1999999999999,252.4,25.9213203435596)) ;
#86294 = CARTESIAN_POINT('Origin',(80.1999999999999,249.6,25.9213203435596)) ;
#86295 = CARTESIAN_POINT('Origin',(62.3573593128808,236.,19.9213203435596)) ;
#86296 = CARTESIAN_POINT('Origin',(59.6573593128808,230.,19.9213203435596)) ;
#86297 = CARTESIAN_POINT('Origin',(74.1999999999999,226.,19.9213203435596)) ;
#86298 = CARTESIAN_POINT('Origin',(74.1999999999999,232.,19.9213203435596)) ;
#86299 = CARTESIAN_POINT('Origin',(46.2,249.,19.9213203435596)) ;
#86300 = CARTESIAN_POINT('Origin',(34.2,249.,19.9213203435596)) ;
#86301 = CARTESIAN_POINT('Origin',(47.9,265.198823964111,23.9039674938989)) ;
#86302 = CARTESIAN_POINT('Ctrl Pts',(47.9,262.836465365523,26.8731635056431)) ;
#86303 = CARTESIAN_POINT('Ctrl Pts',(47.5643828957836,262.836465365523,26.8731635056431)) ;
#86304 = CARTESIAN_POINT('Ctrl Pts',(46.9213179685814,263.028957632654,26.9136881934604)) ;
#86305 = CARTESIAN_POINT('Ctrl Pts',(46.4879676042577,263.526449023177,27.0184232230439)) ;
#86306 = CARTESIAN_POINT('Ctrl Pts',(46.3578850044002,263.800011088028,27.0760152366969)) ;
#86307 = CARTESIAN_POINT('Origin',(69.9,265.198823964111,23.9039674938989)) ;
#86308 = CARTESIAN_POINT('Ctrl Pts',(69.8999999999999,262.836465365523,26.8731635056431)) ;
#86309 = CARTESIAN_POINT('Ctrl Pts',(69.5643828957837,262.836465365523,26.8731635056431)) ;
#86310 = CARTESIAN_POINT('Ctrl Pts',(68.9213187664228,263.028958787238,26.9136884365308)) ;
#86311 = CARTESIAN_POINT('Ctrl Pts',(68.4879676731616,263.526449111869,27.018423241716)) ;
#86312 = CARTESIAN_POINT('Ctrl Pts',(68.3578850163,263.800011090529,27.0760152372235)) ;
#86313 = CARTESIAN_POINT('',(68.2,265.198823964111,23.9039674938989)) ;
#86314 = CARTESIAN_POINT('Origin',(54.5,265.241264282414,23.7023759819625)) ;
#86315 = CARTESIAN_POINT('',(56.2,265.241264282414,23.7023759819625)) ;
#86316 = CARTESIAN_POINT('Ctrl Pts',(56.0420937198538,263.800015543961,27.0760161747882)) ;
#86317 = CARTESIAN_POINT('Ctrl Pts',(55.9130621935296,263.528796310769,27.0189173888531)) ;
#86318 = CARTESIAN_POINT('Ctrl Pts',(55.4812583733538,263.030547215847,26.9140228425536)) ;
#86319 = CARTESIAN_POINT('Ctrl Pts',(54.8382263221145,262.836465365523,26.8731635056432)) ;
#86320 = CARTESIAN_POINT('Ctrl Pts',(54.5,262.836465365523,26.8731635056432)) ;
#86321 = CARTESIAN_POINT('Ctrl Pts',(77.5537622727767,263.802136938942,22.4624560909017)) ;
#86322 = CARTESIAN_POINT('Ctrl Pts',(77.6160771412392,263.802537425212,22.6256558820165)) ;
#86323 = CARTESIAN_POINT('Ctrl Pts',(77.7667803184966,263.803782273667,23.6750632252419)) ;
#86324 = CARTESIAN_POINT('Ctrl Pts',(77.9665329974434,263.843280570403,25.8555842488501)) ;
#86325 = CARTESIAN_POINT('Ctrl Pts',(78.0877270051615,263.90548764331,27.0982208272828)) ;
#86326 = CARTESIAN_POINT('Ctrl Pts',(77.5161760774539,263.799312868747,22.4167726468286)) ;
#86327 = CARTESIAN_POINT('Ctrl Pts',(77.5360130337711,263.788191358363,22.5795333003453)) ;
#86328 = CARTESIAN_POINT('Ctrl Pts',(77.5967692029986,263.715444795543,23.6261104468405)) ;
#86329 = CARTESIAN_POINT('Ctrl Pts',(77.7986137416006,263.605995170056,25.7988034515835)) ;
#86330 = CARTESIAN_POINT('Ctrl Pts',(77.9646212448201,263.590301235021,27.0318657939587)) ;
#86331 = CARTESIAN_POINT('Ctrl Pts',(77.4409019362984,263.799793835359,22.326574012864)) ;
#86332 = CARTESIAN_POINT('Ctrl Pts',(77.3748831483453,263.771443558149,22.4887490503241)) ;
#86333 = CARTESIAN_POINT('Ctrl Pts',(77.2452754678601,263.588475046809,23.5314907130649)) ;
#86334 = CARTESIAN_POINT('Ctrl Pts',(77.3522662402912,263.226007627549,25.6938646863724)) ;
#86335 = CARTESIAN_POINT('Ctrl Pts',(77.5202253706355,263.042309806729,26.9164991774763)) ;
#86336 = CARTESIAN_POINT('Ctrl Pts',(77.3648210667925,263.812301985206,22.2379396633952)) ;
#86337 = CARTESIAN_POINT('Ctrl Pts',(77.2112621247156,263.777968352196,22.4010107034791)) ;
#86338 = CARTESIAN_POINT('Ctrl Pts',(76.8778016563596,263.557546258392,23.4497540555238)) ;
#86339 = CARTESIAN_POINT('Ctrl Pts',(76.7820603106784,263.099191795812,25.6290359143092)) ;
#86340 = CARTESIAN_POINT('Ctrl Pts',(76.8382263221145,262.836465365523,26.8731635056432)) ;
#86341 = CARTESIAN_POINT('Ctrl Pts',(77.3271465306621,263.821412870453,22.1946628572268)) ;
#86342 = CARTESIAN_POINT('Ctrl Pts',(77.1302379764753,263.786866856953,22.3587564213473)) ;
#86343 = CARTESIAN_POINT('Ctrl Pts',(76.6959586099435,263.564706082808,23.4140200985382)) ;
#86344 = CARTESIAN_POINT('Ctrl Pts',(76.4999999999999,263.102238319793,25.6107419728579)) ;
#86345 = CARTESIAN_POINT('Ctrl Pts',(76.5,262.836465365523,26.8731635056432)) ;
#86346 = CARTESIAN_POINT('Ctrl Pts',(46.3089246998894,263.914167397861,27.1000481440303)) ;
#86347 = CARTESIAN_POINT('Ctrl Pts',(46.398964552187,263.865836783231,26.1667163497985)) ;
#86348 = CARTESIAN_POINT('Ctrl Pts',(46.6032252577224,263.805761093415,23.9724961226782)) ;
#86349 = CARTESIAN_POINT('Ctrl Pts',(46.7606927309181,263.803165448826,22.6811011432147)) ;
#86350 = CARTESIAN_POINT('Ctrl Pts',(46.8451922840736,263.802215511675,22.4637434724043)) ;
#86351 = CARTESIAN_POINT('Ctrl Pts',(46.4320964795723,263.592931328567,27.0324194978629)) ;
#86352 = CARTESIAN_POINT('Ctrl Pts',(46.5570399219172,263.604010070467,26.1064695432228)) ;
#86353 = CARTESIAN_POINT('Ctrl Pts',(46.7855269650946,263.693914392471,23.922291785831)) ;
#86354 = CARTESIAN_POINT('Ctrl Pts',(46.8563738086724,263.784563059776,22.6340524722874)) ;
#86355 = CARTESIAN_POINT('Ctrl Pts',(46.8834079801304,263.7992846537,22.417292856026)) ;
#86356 = CARTESIAN_POINT('Ctrl Pts',(46.8791957179207,263.041566324535,26.9163426549089)) ;
#86357 = CARTESIAN_POINT('Ctrl Pts',(47.005410100848,263.179715009613,25.9983019039964)) ;
#86358 = CARTESIAN_POINT('Ctrl Pts',(47.1632040825922,263.535554931216,23.8263510090413)) ;
#86359 = CARTESIAN_POINT('Ctrl Pts',(47.0468280440546,263.761973579305,22.5426416146634)) ;
#86360 = CARTESIAN_POINT('Ctrl Pts',(46.9590496239828,263.799755056779,22.3266718772418)) ;
#86361 = CARTESIAN_POINT('Ctrl Pts',(47.5643828957836,262.836465365523,26.8731635056431)) ;
#86362 = CARTESIAN_POINT('Ctrl Pts',(47.60623000954,263.033757813591,25.9388062619286)) ;
#86363 = CARTESIAN_POINT('Ctrl Pts',(47.5618573951966,263.495689639793,23.7452082892501)) ;
#86364 = CARTESIAN_POINT('Ctrl Pts',(47.2403381174637,263.766640803451,22.4548184438463)) ;
#86365 = CARTESIAN_POINT('Ctrl Pts',(47.035499525566,263.812365610051,22.2376373441309)) ;
#86366 = CARTESIAN_POINT('Ctrl Pts',(47.9,262.836465365523,26.8731635056431)) ;
#86367 = CARTESIAN_POINT('Ctrl Pts',(47.9,263.036041279363,25.925177914903)) ;
#86368 = CARTESIAN_POINT('Ctrl Pts',(47.7565399119583,263.502185788995,23.7109914941486)) ;
#86369 = CARTESIAN_POINT('Ctrl Pts',(47.3349857520721,263.775399470748,22.4132265058195)) ;
#86370 = CARTESIAN_POINT('Ctrl Pts',(47.0728917988203,263.821406189075,22.1946945937677)) ;
#86371 = CARTESIAN_POINT('Ctrl Pts',(68.3089238972751,263.914169501419,27.1000485868847)) ;
#86372 = CARTESIAN_POINT('Ctrl Pts',(68.3989635214134,263.86583849844,26.1667167443968)) ;
#86373 = CARTESIAN_POINT('Ctrl Pts',(68.6032220468531,263.805761123684,23.9725059876743)) ;
#86374 = CARTESIAN_POINT('Ctrl Pts',(68.7606921054679,263.803165570431,22.6811014507584)) ;
#86375 = CARTESIAN_POINT('Ctrl Pts',(68.8451920342653,263.802215530838,22.4637437760421)) ;
#86376 = CARTESIAN_POINT('Ctrl Pts',(68.4320954464358,263.59293250129,27.0324197447521)) ;
#86377 = CARTESIAN_POINT('Ctrl Pts',(68.5570388859512,263.60401096028,26.1064697725006)) ;
#86378 = CARTESIAN_POINT('Ctrl Pts',(68.7855276207896,263.693915243154,23.9223023915977)) ;
#86379 = CARTESIAN_POINT('Ctrl Pts',(68.856373384639,263.784563110008,22.6340526757915)) ;
#86380 = CARTESIAN_POINT('Ctrl Pts',(68.8834078117171,263.799284652591,22.4172930577749)) ;
#86381 = CARTESIAN_POINT('Ctrl Pts',(68.8791958017697,263.041567784116,26.9163429621891)) ;
#86382 = CARTESIAN_POINT('Ctrl Pts',(69.0054102786155,263.179716403355,25.998302229438)) ;
#86383 = CARTESIAN_POINT('Ctrl Pts',(69.1631998752088,263.535551916632,23.8263609376104)) ;
#86384 = CARTESIAN_POINT('Ctrl Pts',(69.0468278287294,263.761973575494,22.5426417126032)) ;
#86385 = CARTESIAN_POINT('Ctrl Pts',(68.9590495389693,263.799755044124,22.3266719765335)) ;
#86386 = CARTESIAN_POINT('Ctrl Pts',(69.5643828957837,262.836465365523,26.8731635056431)) ;
#86387 = CARTESIAN_POINT('Ctrl Pts',(69.6062300095402,263.033757813591,25.9388062619264)) ;
#86388 = CARTESIAN_POINT('Ctrl Pts',(69.5618553916678,263.495691690019,23.7452185551853)) ;
#86389 = CARTESIAN_POINT('Ctrl Pts',(69.2403381174618,263.766640803452,22.4548184438401)) ;
#86390 = CARTESIAN_POINT('Ctrl Pts',(69.0354995255635,263.812365610052,22.2376373441282)) ;
#86391 = CARTESIAN_POINT('Ctrl Pts',(69.8999999999999,262.836465365523,26.8731635056431)) ;
#86392 = CARTESIAN_POINT('Ctrl Pts',(69.9,263.036041279363,25.9251779149008)) ;
#86393 = CARTESIAN_POINT('Ctrl Pts',(69.7565372356489,263.502183882598,23.7110005495361)) ;
#86394 = CARTESIAN_POINT('Ctrl Pts',(69.3349857520697,263.77539947075,22.4132265058132)) ;
#86395 = CARTESIAN_POINT('Ctrl Pts',(69.0728917988171,263.821406189076,22.194694593765)) ;
#86396 = CARTESIAN_POINT('Origin',(68.2,263.,19.9213203435596)) ;
#86397 = CARTESIAN_POINT('Ctrl Pts',(55.5537620469059,263.802136922676,22.4624558020398)) ;
#86398 = CARTESIAN_POINT('Ctrl Pts',(55.6160766782539,263.80253734094,22.6256555955562)) ;
#86399 = CARTESIAN_POINT('Ctrl Pts',(55.7667779370375,263.803782509322,23.6750521597127)) ;
#86400 = CARTESIAN_POINT('Ctrl Pts',(55.9665320341884,263.843279207882,25.8555839228286)) ;
#86401 = CARTESIAN_POINT('Ctrl Pts',(56.0877262991014,263.905485833697,27.0982204463116)) ;
#86402 = CARTESIAN_POINT('Ctrl Pts',(55.5161759288423,263.799312871516,22.4167724460066)) ;
#86403 = CARTESIAN_POINT('Ctrl Pts',(55.5360127177972,263.788191328469,22.5795331048077)) ;
#86404 = CARTESIAN_POINT('Ctrl Pts',(55.5967692807576,263.715444932713,23.6260989147318)) ;
#86405 = CARTESIAN_POINT('Ctrl Pts',(55.7986128632549,263.605994459492,25.798803253818)) ;
#86406 = CARTESIAN_POINT('Ctrl Pts',(55.9646203702438,263.59030019996,27.0318655760511)) ;
#86407 = CARTESIAN_POINT('Ctrl Pts',(55.4409018736246,263.799793850706,22.326573900578)) ;
#86408 = CARTESIAN_POINT('Ctrl Pts',(55.3748830042504,263.771443563708,22.4887489443983)) ;
#86409 = CARTESIAN_POINT('Ctrl Pts',(55.2452720253742,263.588478145295,23.5314796807535)) ;
#86410 = CARTESIAN_POINT('Ctrl Pts',(55.3522665253084,263.226006301692,25.693864370421)) ;
#86411 = CARTESIAN_POINT('Ctrl Pts',(55.5202255476893,263.042308404551,26.9164988822807)) ;
#86412 = CARTESIAN_POINT('Ctrl Pts',(55.3648210917583,263.812301990784,22.2379396367372)) ;
#86413 = CARTESIAN_POINT('Ctrl Pts',(55.2112621445889,263.777968364114,22.4010106829945)) ;
#86414 = CARTESIAN_POINT('Ctrl Pts',(54.8777999382771,263.557545614509,23.449742781627)) ;
#86415 = CARTESIAN_POINT('Ctrl Pts',(54.7820603106785,263.099191795812,25.6290359143101)) ;
#86416 = CARTESIAN_POINT('Ctrl Pts',(54.8382263221145,262.836465365523,26.8731635056432)) ;
#86417 = CARTESIAN_POINT('Ctrl Pts',(55.3271465626755,263.821412876097,22.1946628304122)) ;
#86418 = CARTESIAN_POINT('Ctrl Pts',(55.1302380022922,263.786866861796,22.3587563983465)) ;
#86419 = CARTESIAN_POINT('Ctrl Pts',(54.6959563997398,263.564708271942,23.4140097001504)) ;
#86420 = CARTESIAN_POINT('Ctrl Pts',(54.4999999999999,263.102238319793,25.6107419728589)) ;
#86421 = CARTESIAN_POINT('Ctrl Pts',(54.5,262.836465365523,26.8731635056432)) ;
#86422 = CARTESIAN_POINT('Origin',(56.2,265.,19.9213203435596)) ;
#86423 = CARTESIAN_POINT('Ctrl Pts',(47.4008246626337,264.507291217703,27.3512671439807)) ;
#86424 = CARTESIAN_POINT('Ctrl Pts',(47.3989076166213,264.621171941884,26.2435524495949)) ;
#86425 = CARTESIAN_POINT('Ctrl Pts',(47.3293899330196,264.805875369694,24.4171429924089)) ;
#86426 = CARTESIAN_POINT('Ctrl Pts',(47.1149669351868,264.970247820277,22.7745888050877)) ;
#86427 = CARTESIAN_POINT('Ctrl Pts',(46.9644226373298,265.001836362709,22.4577371313621)) ;
#86428 = CARTESIAN_POINT('Ctrl Pts',(46.8873229985597,264.999843640625,22.477722172732)) ;
#86429 = CARTESIAN_POINT('Ctrl Pts',(47.3909631887125,264.370604282734,27.3224308638185)) ;
#86430 = CARTESIAN_POINT('Ctrl Pts',(47.4243488309635,264.501610595782,26.2190423498724)) ;
#86431 = CARTESIAN_POINT('Ctrl Pts',(47.385851610773,264.73667771661,24.3962605702668)) ;
#86432 = CARTESIAN_POINT('Ctrl Pts',(47.1535711617938,264.958837275192,22.7560844475633)) ;
#86433 = CARTESIAN_POINT('Ctrl Pts',(46.9758145805122,265.0024310584,22.4395657325186)) ;
#86434 = CARTESIAN_POINT('Ctrl Pts',(46.8850787413281,264.999683369079,22.4595294432364)) ;
#86435 = CARTESIAN_POINT('Ctrl Pts',(47.4952139876938,264.097493346775,27.2655157277541)) ;
#86436 = CARTESIAN_POINT('Ctrl Pts',(47.5582348223583,264.292430830159,26.170510089975)) ;
#86437 = CARTESIAN_POINT('Ctrl Pts',(47.5249447211539,264.631611270102,24.3552106906146)) ;
#86438 = CARTESIAN_POINT('Ctrl Pts',(47.228614625003,264.944153638504,22.7198228985961)) ;
#86439 = CARTESIAN_POINT('Ctrl Pts',(46.9983903760502,265.005190448574,22.4040660373099)) ;
#86440 = CARTESIAN_POINT('Ctrl Pts',(46.8806381671158,265.00134258216,22.4239812708368)) ;
#86441 = CARTESIAN_POINT('Ctrl Pts',(47.7673957205814,263.984449147131,27.2432031080418)) ;
#86442 = CARTESIAN_POINT('Ctrl Pts',(47.7928204242151,264.216965605649,26.1426034533423)) ;
#86443 = CARTESIAN_POINT('Ctrl Pts',(47.6940585839927,264.599716436459,24.3229037323166)) ;
#86444 = CARTESIAN_POINT('Ctrl Pts',(47.3047276552285,264.944752851235,22.6850560291216)) ;
#86445 = CARTESIAN_POINT('Ctrl Pts',(47.0211912224739,265.011015887813,22.3688906832847)) ;
#86446 = CARTESIAN_POINT('Ctrl Pts',(46.8761507816279,265.006835652272,22.3888318545834)) ;
#86447 = CARTESIAN_POINT('Ctrl Pts',(47.900839428631,263.984703728653,27.2439881395081)) ;
#86448 = CARTESIAN_POINT('Ctrl Pts',(47.9070163405631,264.21777726175,26.1368564584777)) ;
#86449 = CARTESIAN_POINT('Ctrl Pts',(47.7764900567607,264.602186299455,24.3109308810781)) ;
#86450 = CARTESIAN_POINT('Ctrl Pts',(47.3417200484268,264.947919455522,22.6686907100956)) ;
#86451 = CARTESIAN_POINT('Ctrl Pts',(47.0323284790502,265.014618545435,22.3518830915824)) ;
#86452 = CARTESIAN_POINT('Ctrl Pts',(46.873959871809,265.010411597039,22.3718653109223)) ;
#86453 = CARTESIAN_POINT('Origin',(46.9,264.5,27.2233813234279)) ;
#86454 = CARTESIAN_POINT('Ctrl Pts',(55.5255673610189,264.999356809564,22.4862307209618)) ;
#86455 = CARTESIAN_POINT('Ctrl Pts',(55.4109671059889,265.005425204665,22.4210492449598)) ;
#86456 = CARTESIAN_POINT('Ctrl Pts',(55.1416818286438,264.924461110078,23.2918898343867)) ;
#86457 = CARTESIAN_POINT('Ctrl Pts',(55.0024976411188,264.667616273681,25.9804497446043)) ;
#86458 = CARTESIAN_POINT('Ctrl Pts',(54.9963300104537,264.515694422742,27.4891456859497)) ;
#86459 = CARTESIAN_POINT('Ctrl Pts',(55.5304587903673,264.998833446453,22.4670625659595)) ;
#86460 = CARTESIAN_POINT('Ctrl Pts',(55.3940129026723,265.007685061672,22.4019652735408)) ;
#86461 = CARTESIAN_POINT('Ctrl Pts',(55.0701232396585,264.889109282959,23.2716945070135)) ;
#86462 = CARTESIAN_POINT('Ctrl Pts',(54.9691052398483,264.542596400602,25.9559962065829)) ;
#86463 = CARTESIAN_POINT('Ctrl Pts',(55.01870636833,264.370339661709,27.4582800755484)) ;
#86464 = CARTESIAN_POINT('Ctrl Pts',(55.5399297326649,265.000117029878,22.4304757432437)) ;
#86465 = CARTESIAN_POINT('Ctrl Pts',(55.3610526986339,265.012656016268,22.3655583950824)) ;
#86466 = CARTESIAN_POINT('Ctrl Pts',(54.9363638397547,264.844925871569,23.2329126197646)) ;
#86467 = CARTESIAN_POINT('Ctrl Pts',(54.823337890213,264.339857688415,25.9080805918787)) ;
#86468 = CARTESIAN_POINT('Ctrl Pts',(54.9202367438694,264.076965070082,27.3976744897227)) ;
#86469 = CARTESIAN_POINT('Ctrl Pts',(55.5495146369683,265.005673339809,22.3943346542401)) ;
#86470 = CARTESIAN_POINT('Ctrl Pts',(55.3276395741456,265.019340477166,22.3293242824278)) ;
#86471 = CARTESIAN_POINT('Ctrl Pts',(54.8035926044541,264.836747727878,23.1979076932162)) ;
#86472 = CARTESIAN_POINT('Ctrl Pts',(54.5910965086588,264.272804860473,25.8777147035963)) ;
#86473 = CARTESIAN_POINT('Ctrl Pts',(54.6354515551578,263.956212815122,27.3754759866893)) ;
#86474 = CARTESIAN_POINT('Ctrl Pts',(55.5540753127105,265.009258937202,22.3773405899133)) ;
#86475 = CARTESIAN_POINT('Ctrl Pts',(55.3117363898015,265.022976994424,22.3121815465214)) ;
#86476 = CARTESIAN_POINT('Ctrl Pts',(54.7405444818452,264.839699472842,23.1827259708804)) ;
#86477 = CARTESIAN_POINT('Ctrl Pts',(54.4812488421695,264.273919304648,25.8701523185663)) ;
#86478 = CARTESIAN_POINT('Ctrl Pts',(54.4993596409889,263.956681652816,27.3771201355784)) ;
#86479 = CARTESIAN_POINT('Ctrl Pts',(77.5126870873055,264.999843389651,22.4777270870555)) ;
#86480 = CARTESIAN_POINT('Ctrl Pts',(77.4355856076841,265.001837775216,22.4577244733426)) ;
#86481 = CARTESIAN_POINT('Ctrl Pts',(77.2850416233415,264.970250830608,22.774574270844)) ;
#86482 = CARTESIAN_POINT('Ctrl Pts',(77.070616045939,264.805880890583,24.4171737852644)) ;
#86483 = CARTESIAN_POINT('Ctrl Pts',(77.0010927930105,264.621179637214,26.2436227267522)) ;
#86484 = CARTESIAN_POINT('Ctrl Pts',(76.9991739635825,264.507297407404,27.3513716626615)) ;
#86485 = CARTESIAN_POINT('Ctrl Pts',(77.5149332535848,264.999682929536,22.4595336213756)) ;
#86486 = CARTESIAN_POINT('Ctrl Pts',(77.4241945868893,265.002432970266,22.4395523417571)) ;
#86487 = CARTESIAN_POINT('Ctrl Pts',(77.2464340770455,264.958840455122,22.7560694393853)) ;
#86488 = CARTESIAN_POINT('Ctrl Pts',(77.014150140122,264.736678453386,24.3962909120826)) ;
#86489 = CARTESIAN_POINT('Ctrl Pts',(76.9756554398609,264.5016104682,26.2191114851833)) ;
#86490 = CARTESIAN_POINT('Ctrl Pts',(77.0090442725839,264.370603528154,27.3225338245482)) ;
#86491 = CARTESIAN_POINT('Ctrl Pts',(77.5193774902576,265.001341919645,22.4239852672336)) ;
#86492 = CARTESIAN_POINT('Ctrl Pts',(77.4016209356984,265.005193167249,22.4040525055347)) ;
#86493 = CARTESIAN_POINT('Ctrl Pts',(77.1713939672703,264.944156713126,22.7198077925902)) ;
#86494 = CARTESIAN_POINT('Ctrl Pts',(76.8750612211273,264.631607422865,24.3552406151253)) ;
#86495 = CARTESIAN_POINT('Ctrl Pts',(76.8417685764965,264.292425394558,26.1705787621317)) ;
#86496 = CARTESIAN_POINT('Ctrl Pts',(76.904797000281,264.097484288593,27.2656173880932)) ;
#86497 = CARTESIAN_POINT('Ctrl Pts',(77.523868555885,265.006834920525,22.3888356841188)) ;
#86498 = CARTESIAN_POINT('Ctrl Pts',(77.3788224880676,265.011018690996,22.3688769443209)) ;
#86499 = CARTESIAN_POINT('Ctrl Pts',(77.0952809873972,264.944758364116,22.6850409999854)) ;
#86500 = CARTESIAN_POINT('Ctrl Pts',(76.7059440140755,264.599714552233,24.3229338911505)) ;
#86501 = CARTESIAN_POINT('Ctrl Pts',(76.6071833141231,264.216953764414,26.1426713565531)) ;
#86502 = CARTESIAN_POINT('Ctrl Pts',(76.6326153072635,263.984431556749,27.2433041953422)) ;
#86503 = CARTESIAN_POINT('Ctrl Pts',(77.5260611861056,265.010410675423,22.3718696861525)) ;
#86504 = CARTESIAN_POINT('Ctrl Pts',(77.3676867570225,265.014621321342,22.3518699016325)) ;
#86505 = CARTESIAN_POINT('Ctrl Pts',(77.0582908870455,264.947922650659,22.6686755732325)) ;
#86506 = CARTESIAN_POINT('Ctrl Pts',(76.623515455463,264.602180068614,24.3109603652938)) ;
#86507 = CARTESIAN_POINT('Ctrl Pts',(76.4929898959272,264.217763018292,26.1369243071539)) ;
#86508 = CARTESIAN_POINT('Ctrl Pts',(76.4991742481055,263.984682447818,27.2440890311872)) ;
#86509 = CARTESIAN_POINT('Ctrl Pts',(69.4008257028231,264.507295904801,27.3513462902868)) ;
#86510 = CARTESIAN_POINT('Ctrl Pts',(69.3989073063844,264.621177769096,26.2436056666157)) ;
#86511 = CARTESIAN_POINT('Ctrl Pts',(69.3293854049881,264.805879550229,24.4171663113135)) ;
#86512 = CARTESIAN_POINT('Ctrl Pts',(69.1149604545227,264.970250099837,22.7745777990922)) ;
#86513 = CARTESIAN_POINT('Ctrl Pts',(68.9644163937797,265.001837432337,22.4577275461148)) ;
#86514 = CARTESIAN_POINT('Ctrl Pts',(68.8873153610441,264.999843450594,22.4777258938723)) ;
#86515 = CARTESIAN_POINT('Ctrl Pts',(69.3909575385873,264.370603711185,27.3225088303552)) ;
#86516 = CARTESIAN_POINT('Ctrl Pts',(69.4243455968175,264.501610499055,26.2190947022126)) ;
#86517 = CARTESIAN_POINT('Ctrl Pts',(69.3858502849074,264.736678274293,24.3962835477298)) ;
#86518 = CARTESIAN_POINT('Ctrl Pts',(69.1535671948623,264.958839683308,22.7560730826454)) ;
#86519 = CARTESIAN_POINT('Ctrl Pts',(68.9758076385222,265.002432506156,22.4395555924098)) ;
#86520 = CARTESIAN_POINT('Ctrl Pts',(68.8850696582037,264.999683036264,22.4595326069041)) ;
#86521 = CARTESIAN_POINT('Ctrl Pts',(69.4952056691767,264.097486489153,27.2655927099579)) ;
#86522 = CARTESIAN_POINT('Ctrl Pts',(69.5582322508228,264.292426715909,26.1705620920024)) ;
#86523 = CARTESIAN_POINT('Ctrl Pts',(69.5249402193863,264.63160835578,24.3552333518857)) ;
#86524 = CARTESIAN_POINT('Ctrl Pts',(69.2286081188304,264.944155966591,22.7198114595033)) ;
#86525 = CARTESIAN_POINT('Ctrl Pts',(68.9983818102557,265.005192507295,22.4040557903944)) ;
#86526 = CARTESIAN_POINT('Ctrl Pts',(68.8806263106136,265.001342080515,22.4239842968519)) ;
#86527 = CARTESIAN_POINT('Ctrl Pts',(69.7673873702777,263.98443582666,27.24327965592)) ;
#86528 = CARTESIAN_POINT('Ctrl Pts',(69.7928175937792,264.21695663877,26.1426548726517)) ;
#86529 = CARTESIAN_POINT('Ctrl Pts',(69.6940566161564,264.599715009964,24.3229265712649)) ;
#86530 = CARTESIAN_POINT('Ctrl Pts',(69.3047211111121,264.944757025772,22.6850446482569)) ;
#86531 = CARTESIAN_POINT('Ctrl Pts',(69.0211808402246,265.011018010547,22.3688802794475)) ;
#86532 = CARTESIAN_POINT('Ctrl Pts',(68.8761361383546,265.006835098209,22.3888347542145)) ;
#86533 = CARTESIAN_POINT('Ctrl Pts',(69.9008290727288,263.984687613801,27.2440645392984)) ;
#86534 = CARTESIAN_POINT('Ctrl Pts',(69.9070116186382,264.217766475947,26.1369078365147)) ;
#86535 = CARTESIAN_POINT('Ctrl Pts',(69.7764858821136,264.602181580875,24.3109532089491)) ;
#86536 = CARTESIAN_POINT('Ctrl Pts',(69.3417117681599,264.947921875006,22.6686792476652)) ;
#86537 = CARTESIAN_POINT('Ctrl Pts',(69.0323169416041,265.014620647502,22.3518731034479)) ;
#86538 = CARTESIAN_POINT('Ctrl Pts',(68.8739439257557,265.01041089921,22.3718686237511)) ;
#86539 = CARTESIAN_POINT('Origin',(46.9,264.5,19.9213203435596)) ;
#86540 = CARTESIAN_POINT('',(47.4,264.5,19.9213203435596)) ;
#86541 = CARTESIAN_POINT('Origin',(47.4,263.,19.9213203435596)) ;
#86542 = CARTESIAN_POINT('',(0.,0.,0.)) ;
#86543 = CARTESIAN_POINT('Origin',(75.3,227.275,30.6213203435596)) ;
#86544 = CARTESIAN_POINT('',(75.2,229.7,30.6213203435596)) ;
#86545 = CARTESIAN_POINT('',(75.1999999999999,226.3,30.6213203435596)) ;
#86546 = CARTESIAN_POINT('',(75.1999999999999,227.275,30.6213203435596)) ;
#86547 = CARTESIAN_POINT('',(75.2999999999999,226.2,30.7213203435596)) ;
#86548 = CARTESIAN_POINT('Origin',(75.2999999999999,226.2,30.6213203435596)) ;
#86549 = CARTESIAN_POINT('',(75.3,229.658578643763,30.7213203435596)) ;
#86550 = CARTESIAN_POINT('',(75.3,227.275,30.7213203435596)) ;
#86551 = CARTESIAN_POINT('Origin',(75.3,229.658578643763,30.6213203435596)) ;
#86552 = CARTESIAN_POINT('Origin',(75.4082106781188,229.766789321882,30.6213203435596)) ;
#86553 = CARTESIAN_POINT('',(76.0414213562373,230.4,30.7213203435596)) ;
#86554 = CARTESIAN_POINT('',(75.4082106781188,229.766789321882,30.7213203435596)) ;
#86555 = CARTESIAN_POINT('',(76.,230.5,30.6213203435596)) ;
#86556 = CARTESIAN_POINT('Origin',(76.0414213562373,230.4,30.6213203435596)) ;
#86557 = CARTESIAN_POINT('',(75.3375000000001,229.8375,30.6213203435596)) ;
#86558 = CARTESIAN_POINT('Origin',(76.6,230.4,30.6213203435596)) ;
#86559 = CARTESIAN_POINT('',(79.1,230.4,30.7213203435596)) ;
#86560 = CARTESIAN_POINT('',(76.6,230.4,30.7213203435596)) ;
#86561 = CARTESIAN_POINT('',(79.2,230.5,30.6213203435596)) ;
#86562 = CARTESIAN_POINT('Origin',(79.1,230.4,30.6213203435596)) ;
#86563 = CARTESIAN_POINT('',(76.6,230.5,30.6213203435596)) ;
#86564 = CARTESIAN_POINT('Origin',(79.1,226.100000000001,30.6213203435596)) ;
#86565 = CARTESIAN_POINT('',(79.1,226.100000000001,30.7213203435596)) ;
#86566 = CARTESIAN_POINT('',(79.2,226.100000000001,30.6213203435596)) ;
#86567 = CARTESIAN_POINT('Origin',(79.1,226.100000000001,30.6213203435596)) ;
#86568 = CARTESIAN_POINT('',(79.1,226.000000000001,30.6213203435596)) ;
#86569 = CARTESIAN_POINT('Origin',(79.1,226.100000000001,30.6213203435596)) ;
#86570 = CARTESIAN_POINT('Origin',(79.1,226.100000000001,30.6213203435596)) ;
#86571 = CARTESIAN_POINT('Origin',(78.2,226.100000000001,30.6213203435596)) ;
#86572 = CARTESIAN_POINT('',(75.3999999999987,226.100000000001,30.7213203435596)) ;
#86573 = CARTESIAN_POINT('',(75.4999999999987,226.000000000001,30.6213203435596)) ;
#86574 = CARTESIAN_POINT('Origin',(75.3999999999987,226.100000000001,30.6213203435596)) ;
#86575 = CARTESIAN_POINT('',(78.2,226.000000000001,30.6213203435596)) ;
#86576 = CARTESIAN_POINT('',(78.2,226.100000000001,30.7213203435596)) ;
#86577 = CARTESIAN_POINT('Origin',(79.1,226.100000000001,30.7213203435596)) ;
#86578 = CARTESIAN_POINT('',(79.1,226.000000000001,29.5213203435596)) ;
#86579 = CARTESIAN_POINT('',(79.2,226.100000000001,29.5213203435596)) ;
#86580 = CARTESIAN_POINT('Origin',(79.1,226.100000000001,29.5213203435596)) ;
#86581 = CARTESIAN_POINT('',(79.2,226.100000000001,30.7213203435596)) ;
#86582 = CARTESIAN_POINT('',(79.1,226.000000000001,30.7213203435596)) ;
#86583 = CARTESIAN_POINT('Origin',(79.1,229.375,30.6213203435596)) ;
#86584 = CARTESIAN_POINT('',(79.1,229.375,30.7213203435596)) ;
#86585 = CARTESIAN_POINT('',(79.2,229.375,30.6213203435596)) ;
#86586 = CARTESIAN_POINT('Origin',(75.1999999999999,226.3,30.7213203435596)) ;
#86587 = CARTESIAN_POINT('',(75.2,229.7,29.5213203435596)) ;
#86588 = CARTESIAN_POINT('',(75.2,229.7,30.7213203435596)) ;
#86589 = CARTESIAN_POINT('',(75.1999999999999,226.3,29.5213203435596)) ;
#86590 = CARTESIAN_POINT('',(75.2,229.7,29.5213203435596)) ;
#86591 = CARTESIAN_POINT('',(75.1999999999999,226.3,30.7213203435596)) ;
#86592 = CARTESIAN_POINT('Origin',(75.4999999999987,226.000000000001,30.7213203435596)) ;
#86593 = CARTESIAN_POINT('',(75.4999999999987,226.000000000001,29.5213203435596)) ;
#86594 = CARTESIAN_POINT('',(75.1999999999999,226.3,29.5213203435596)) ;
#86595 = CARTESIAN_POINT('',(75.4999999999987,226.000000000001,30.7213203435596)) ;
#86596 = CARTESIAN_POINT('',(75.1999999999999,226.3,30.7213203435596)) ;
#86597 = CARTESIAN_POINT('Origin',(75.2,229.7,30.7213203435596)) ;
#86598 = CARTESIAN_POINT('',(76.,230.5,29.5213203435596)) ;
#86599 = CARTESIAN_POINT('',(76.,230.5,30.7213203435596)) ;
#86600 = CARTESIAN_POINT('',(76.,230.5,29.5213203435596)) ;
#86601 = CARTESIAN_POINT('Origin',(76.,230.5,30.7213203435596)) ;
#86602 = CARTESIAN_POINT('',(79.2,230.5,29.5213203435596)) ;
#86603 = CARTESIAN_POINT('',(79.2,230.5,30.7213203435596)) ;
#86604 = CARTESIAN_POINT('',(80.2,230.5,29.5213203435596)) ;
#86605 = CARTESIAN_POINT('Origin',(79.2,230.5,30.7213203435596)) ;
#86606 = CARTESIAN_POINT('',(79.2,226.000000000001,29.5213203435596)) ;
#86607 = CARTESIAN_POINT('Origin',(79.2,226.000000000001,30.7213203435596)) ;
#86608 = CARTESIAN_POINT('',(74.7,226.000000000001,29.5213203435596)) ;
#86609 = CARTESIAN_POINT('Origin',(77.2,228.250000000001,29.5213203435596)) ;
#86610 = CARTESIAN_POINT('Origin',(77.2,228.250000000001,30.7213203435596)) ;
#86611 = CARTESIAN_POINT('',(0.,0.,0.)) ;
#86612 = CARTESIAN_POINT('Origin',(71.0296384056928,220.462610236549,30.6213203435596)) ;
#86613 = CARTESIAN_POINT('',(66.535890167043,220.462610236549,30.7213203435596)) ;
#86614 = CARTESIAN_POINT('',(66.5470607720161,220.362610236549,30.6213203435596)) ;
#86615 = CARTESIAN_POINT('Ctrl Pts',(66.535890167043,220.462610236549,30.7213203435596)) ;
#86616 = CARTESIAN_POINT('Ctrl Pts',(66.5375573265241,220.450073793375,30.7213203435596)) ;
#86617 = CARTESIAN_POINT('Ctrl Pts',(66.5392266719142,220.436678341659,30.7188189533562)) ;
#86618 = CARTESIAN_POINT('Ctrl Pts',(66.5421069063706,220.412004111391,30.7085970880789)) ;
#86619 = CARTESIAN_POINT('Ctrl Pts',(66.5433203105337,220.400725238479,30.700877549635)) ;
#86620 = CARTESIAN_POINT('Ctrl Pts',(66.5451460630584,220.382976586378,30.6830871681797)) ;
#86621 = CARTESIAN_POINT('Ctrl Pts',(66.5458826827361,220.375300527803,30.6718610783706)) ;
#86622 = CARTESIAN_POINT('Ctrl Pts',(66.5468387755779,220.365117510381,30.6472522185807)) ;
#86623 = CARTESIAN_POINT('Ctrl Pts',(66.5470607720162,220.362610236549,30.633869677038)) ;
#86624 = CARTESIAN_POINT('Ctrl Pts',(66.5470607720162,220.362610236549,30.6213203435596)) ;
#86625 = CARTESIAN_POINT('',(72.0450953968557,220.362610236549,30.6213203435596)) ;
#86626 = CARTESIAN_POINT('',(71.0296384056928,220.362610236549,30.6213203435596)) ;
#86627 = CARTESIAN_POINT('',(72.0450953968557,220.462610236549,30.7213203435596)) ;
#86628 = CARTESIAN_POINT('Origin',(72.0450953968557,220.462610236549,30.6213203435596)) ;
#86629 = CARTESIAN_POINT('',(71.0296384056928,220.462610236549,30.7213203435596)) ;
#86630 = CARTESIAN_POINT('Origin',(72.0450953968556,220.462610236549,30.7213203435596)) ;
#86631 = CARTESIAN_POINT('',(72.1450953968557,220.462610236549,30.6213203435596)) ;
#86632 = CARTESIAN_POINT('Origin',(72.0450953968556,220.462610236549,30.6213203435596)) ;
#86633 = CARTESIAN_POINT('',(72.0450953968556,220.362610236549,29.6213203435596)) ;
#86634 = CARTESIAN_POINT('',(72.0450953968556,220.362610236549,30.7213203435596)) ;
#86635 = CARTESIAN_POINT('',(72.1450953968557,220.462610236549,29.6213203435596)) ;
#86636 = CARTESIAN_POINT('Origin',(72.0450953968556,220.462610236549,29.6213203435596)) ;
#86637 = CARTESIAN_POINT('',(72.1450953968557,220.462610236549,30.7213203435596)) ;
#86638 = CARTESIAN_POINT('Origin',(71.0296384056928,220.462610236549,29.6213203435596)) ;
#86639 = CARTESIAN_POINT('',(66.5470607720161,220.362610236549,29.6213203435596)) ;
#86640 = CARTESIAN_POINT('',(66.535890167043,220.462610236549,29.5213203435596)) ;
#86641 = CARTESIAN_POINT('Ctrl Pts',(66.5470607720162,220.362610236549,29.6213203435596)) ;
#86642 = CARTESIAN_POINT('Ctrl Pts',(66.5470607720162,220.362610236549,29.6087513069564)) ;
#86643 = CARTESIAN_POINT('Ctrl Pts',(66.5468380955723,220.365125326392,29.5953491152596)) ;
#86644 = CARTESIAN_POINT('Ctrl Pts',(66.5458791440598,220.37533771967,29.5707102872029)) ;
#86645 = CARTESIAN_POINT('Ctrl Pts',(66.5451403289395,220.383035341946,29.559473881925)) ;
#86646 = CARTESIAN_POINT('Ctrl Pts',(66.5433118191149,220.400804731032,29.5417044928395)) ;
#86647 = CARTESIAN_POINT('Ctrl Pts',(66.5420991240993,220.412073206815,29.5340065426202)) ;
#86648 = CARTESIAN_POINT('Ctrl Pts',(66.5392218285232,220.436717456405,29.5238140042625)) ;
#86649 = CARTESIAN_POINT('Ctrl Pts',(66.5375547295074,220.450093322012,29.5213203435596)) ;
#86650 = CARTESIAN_POINT('Ctrl Pts',(66.535890167043,220.462610236549,29.5213203435596)) ;
#86651 = CARTESIAN_POINT('',(72.0450953968557,220.462610236549,29.5213203435596)) ;
#86652 = CARTESIAN_POINT('',(71.0296384056928,220.462610236549,29.5213203435596)) ;
#86653 = CARTESIAN_POINT('Origin',(72.0450953968557,220.462610236549,29.6213203435596)) ;
#86654 = CARTESIAN_POINT('',(71.0296384056928,220.362610236549,29.6213203435596)) ;
#86655 = CARTESIAN_POINT('Origin',(72.0450953968557,220.462610236549,29.6213203435596)) ;
#86656 = CARTESIAN_POINT('Origin',(72.0450953968557,220.462610236549,29.6213203435596)) ;
#86657 = CARTESIAN_POINT('Origin',(72.0450953968557,220.462610236549,30.6213203435596)) ;
#86658 = CARTESIAN_POINT('Origin',(72.0450953968557,220.462610236549,30.6213203435596)) ;
#86659 = CARTESIAN_POINT('Origin',(69.9141814145298,238.377312217409,30.7213203435596)) ;
#86660 = CARTESIAN_POINT('',(72.0450953968556,223.000000000001,30.7213203435596)) ;
#86661 = CARTESIAN_POINT('',(72.0450953968556,230.688656108705,30.7213203435596)) ;
#86662 = CARTESIAN_POINT('',(74.7,226.067880390059,30.7213203435596)) ;
#86663 = CARTESIAN_POINT('Origin',(75.1450953968556,223.000000000001,30.7213203435596)) ;
#86664 = CARTESIAN_POINT('',(74.7,231.000000000001,30.7213203435596)) ;
#86665 = CARTESIAN_POINT('',(74.7,231.000000000001,30.7213203435596)) ;
#86666 = CARTESIAN_POINT('',(79.0976680713511,231.000000000001,30.7213203435596)) ;
#86667 = CARTESIAN_POINT('',(79.2,231.000000000001,30.7213203435596)) ;
#86668 = CARTESIAN_POINT('',(80.1000000000001,235.614468918958,30.7213203435596)) ;
#86669 = CARTESIAN_POINT('',(80.1582163984138,235.882481693345,30.7213203435596)) ;
#86670 = CARTESIAN_POINT('',(80.1000000000001,238.703733341287,30.7213203435596)) ;
#86671 = CARTESIAN_POINT('',(80.1000000000001,238.490522779348,30.7213203435596)) ;
#86672 = CARTESIAN_POINT('',(82.1067384683691,238.703733341287,30.7213203435596)) ;
#86673 = CARTESIAN_POINT('',(76.057090707265,238.703733341287,30.7213203435596)) ;
#86674 = CARTESIAN_POINT('',(82.183342912681,238.739454580319,30.7213203435596)) ;
#86675 = CARTESIAN_POINT('Origin',(82.1067384683691,238.803733341287,30.7213203435596)) ;
#86676 = CARTESIAN_POINT('',(83.9347806063073,240.826736743903,30.7213203435596)) ;
#86677 = CARTESIAN_POINT('',(80.4937295064186,236.72585173331,30.7213203435596)) ;
#86678 = CARTESIAN_POINT('',(84.0283628290597,241.083851787777,30.7213203435596)) ;
#86679 = CARTESIAN_POINT('Origin',(83.6283628290597,241.083851787777,30.7213203435596)) ;
#86680 = CARTESIAN_POINT('',(84.0283628290597,244.119881553511,30.7213203435596)) ;
#86681 = CARTESIAN_POINT('',(84.0283628290597,241.339589444027,30.7213203435596)) ;
#86682 = CARTESIAN_POINT('',(83.9347806063073,244.376996597386,30.7213203435596)) ;
#86683 = CARTESIAN_POINT('Origin',(83.6283628290597,244.119881553511,30.7213203435596)) ;
#86684 = CARTESIAN_POINT('',(82.2732639481701,246.357115043876,30.7213203435596)) ;
#86685 = CARTESIAN_POINT('',(81.6097350811727,247.14787795491,30.7213203435596)) ;
#86686 = CARTESIAN_POINT('',(81.9668461709225,246.500000000001,30.7213203435596)) ;
#86687 = CARTESIAN_POINT('Origin',(81.9668461709225,246.100000000001,30.7213203435596)) ;
#86688 = CARTESIAN_POINT('',(79.1,246.500000000001,30.7213203435596)) ;
#86689 = CARTESIAN_POINT('',(74.5570907072649,246.500000000001,30.7213203435596)) ;
#86690 = CARTESIAN_POINT('',(79.1,253.900000000001,30.7213203435596)) ;
#86691 = CARTESIAN_POINT('',(79.1,246.138656108705,30.7213203435596)) ;
#86692 = CARTESIAN_POINT('',(67.6,253.900000000001,30.7213203435596)) ;
#86693 = CARTESIAN_POINT('',(67.6,253.900000000001,30.7213203435596)) ;
#86694 = CARTESIAN_POINT('',(67.6,257.5,30.7213203435596)) ;
#86695 = CARTESIAN_POINT('',(67.6,257.5,30.7213203435596)) ;
#86696 = CARTESIAN_POINT('',(55.7,257.5,30.7213203435596)) ;
#86697 = CARTESIAN_POINT('',(55.7,257.5,30.7213203435596)) ;
#86698 = CARTESIAN_POINT('',(55.7,245.9,30.7213203435596)) ;
#86699 = CARTESIAN_POINT('',(55.7,245.9,30.7213203435596)) ;
#86700 = CARTESIAN_POINT('',(58.9573593128807,245.9,30.7213203435596)) ;
#86701 = CARTESIAN_POINT('',(58.9573593128807,245.9,30.7213203435596)) ;
#86702 = CARTESIAN_POINT('',(58.9573593128807,226.1,30.7213203435596)) ;
#86703 = CARTESIAN_POINT('',(58.9573593128807,239.1,30.7213203435596)) ;
#86704 = CARTESIAN_POINT('',(61.775147916658,220.442149698512,30.7213203435596)) ;
#86705 = CARTESIAN_POINT('',(58.9573593128807,226.1,30.7213203435596)) ;
#86706 = CARTESIAN_POINT('Origin',(64.1568347953872,220.146231446812,30.7213203435596)) ;
#86707 = CARTESIAN_POINT('',(75.3756995384723,242.900000000001,30.7213203435596)) ;
#86708 = CARTESIAN_POINT('',(75.3756995384723,240.900000000001,30.7213203435596)) ;
#86709 = CARTESIAN_POINT('',(75.3756995384723,240.638656108705,30.7213203435596)) ;
#86710 = CARTESIAN_POINT('',(78.481026119647,242.900000000001,30.7213203435596)) ;
#86711 = CARTESIAN_POINT('Origin',(76.9283628290597,242.900000000001,30.7213203435596)) ;
#86712 = CARTESIAN_POINT('',(78.481026119647,240.900000000001,30.7213203435596)) ;
#86713 = CARTESIAN_POINT('',(78.481026119647,239.638656108705,30.7213203435596)) ;
#86714 = CARTESIAN_POINT('Origin',(76.9283628290597,240.900000000001,30.7213203435596)) ;
#86715 = CARTESIAN_POINT('',(73.9,229.6,30.7213203435596)) ;
#86716 = CARTESIAN_POINT('',(74.2,229.90139888331,30.7213203435596)) ;
#86717 = CARTESIAN_POINT('Ctrl Pts',(74.2,229.90139888331,30.7213203435596)) ;
#86718 = CARTESIAN_POINT('Ctrl Pts',(74.2,229.864103877398,30.7213203435596)) ;
#86719 = CARTESIAN_POINT('Ctrl Pts',(74.1913108545003,229.820201486786,30.7213203435596)) ;
#86720 = CARTESIAN_POINT('Ctrl Pts',(74.1628856418395,229.751400609842,30.7213203435596)) ;
#86721 = CARTESIAN_POINT('Ctrl Pts',(74.1381754797833,229.714300461156,30.7213203435596)) ;
#86722 = CARTESIAN_POINT('Ctrl Pts',(74.0857759852183,229.661783948368,30.7213203435596)) ;
#86723 = CARTESIAN_POINT('Ctrl Pts',(74.0488482525377,229.637045411928,30.7213203435596)) ;
#86724 = CARTESIAN_POINT('Ctrl Pts',(73.9804869087102,229.608675189374,30.7213203435596)) ;
#86725 = CARTESIAN_POINT('Ctrl Pts',(73.9369742156035,229.6,30.7213203435596)) ;
#86726 = CARTESIAN_POINT('Ctrl Pts',(73.9,229.6,30.7213203435596)) ;
#86727 = CARTESIAN_POINT('',(72.1,229.6,30.7213203435596)) ;
#86728 = CARTESIAN_POINT('',(74.2,229.6,30.7213203435596)) ;
#86729 = CARTESIAN_POINT('',(71.8,229.90139888331,30.7213203435596)) ;
#86730 = CARTESIAN_POINT('Ctrl Pts',(72.1,229.6,30.7213203435596)) ;
#86731 = CARTESIAN_POINT('Ctrl Pts',(72.0630257843965,229.6,30.7213203435596)) ;
#86732 = CARTESIAN_POINT('Ctrl Pts',(72.0195130912898,229.608675189374,30.7213203435596)) ;
#86733 = CARTESIAN_POINT('Ctrl Pts',(71.9511517474623,229.637045411928,30.7213203435596)) ;
#86734 = CARTESIAN_POINT('Ctrl Pts',(71.9142240147817,229.661783948368,30.7213203435596)) ;
#86735 = CARTESIAN_POINT('Ctrl Pts',(71.8618245202167,229.714300461156,30.7213203435596)) ;
#86736 = CARTESIAN_POINT('Ctrl Pts',(71.8371143581605,229.751400609842,30.7213203435596)) ;
#86737 = CARTESIAN_POINT('Ctrl Pts',(71.8086891454997,229.820201486786,30.7213203435596)) ;
#86738 = CARTESIAN_POINT('Ctrl Pts',(71.8,229.864103877398,30.7213203435596)) ;
#86739 = CARTESIAN_POINT('Ctrl Pts',(71.8,229.90139888331,30.7213203435596)) ;
#86740 = CARTESIAN_POINT('',(71.8,231.69860111669,30.7213203435596)) ;
#86741 = CARTESIAN_POINT('',(71.8,229.6,30.7213203435596)) ;
#86742 = CARTESIAN_POINT('',(72.1,232.,30.7213203435596)) ;
#86743 = CARTESIAN_POINT('Ctrl Pts',(71.8,231.69860111669,30.7213203435596)) ;
#86744 = CARTESIAN_POINT('Ctrl Pts',(71.8,231.735896122602,30.7213203435596)) ;
#86745 = CARTESIAN_POINT('Ctrl Pts',(71.8086891454997,231.779798513214,30.7213203435596)) ;
#86746 = CARTESIAN_POINT('Ctrl Pts',(71.8371143581605,231.848599390158,30.7213203435596)) ;
#86747 = CARTESIAN_POINT('Ctrl Pts',(71.8618245202167,231.885699538844,30.7213203435596)) ;
#86748 = CARTESIAN_POINT('Ctrl Pts',(71.9142240147817,231.938216051632,30.7213203435596)) ;
#86749 = CARTESIAN_POINT('Ctrl Pts',(71.9511517474623,231.962954588072,30.7213203435596)) ;
#86750 = CARTESIAN_POINT('Ctrl Pts',(72.0195130912898,231.991324810626,30.7213203435596)) ;
#86751 = CARTESIAN_POINT('Ctrl Pts',(72.0630257843965,232.,30.7213203435596)) ;
#86752 = CARTESIAN_POINT('Ctrl Pts',(72.1,232.,30.7213203435596)) ;
#86753 = CARTESIAN_POINT('',(73.9,232.,30.7213203435596)) ;
#86754 = CARTESIAN_POINT('',(71.8,232.,30.7213203435596)) ;
#86755 = CARTESIAN_POINT('',(74.2,231.69860111669,30.7213203435596)) ;
#86756 = CARTESIAN_POINT('Ctrl Pts',(73.9,232.,30.7213203435596)) ;
#86757 = CARTESIAN_POINT('Ctrl Pts',(73.9369742156035,232.,30.7213203435596)) ;
#86758 = CARTESIAN_POINT('Ctrl Pts',(73.9804869087102,231.991324810626,30.7213203435596)) ;
#86759 = CARTESIAN_POINT('Ctrl Pts',(74.0488482525377,231.962954588072,30.7213203435596)) ;
#86760 = CARTESIAN_POINT('Ctrl Pts',(74.0857759852183,231.938216051632,30.7213203435596)) ;
#86761 = CARTESIAN_POINT('Ctrl Pts',(74.1381754797833,231.885699538844,30.7213203435596)) ;
#86762 = CARTESIAN_POINT('Ctrl Pts',(74.1628856418395,231.848599390158,30.7213203435596)) ;
#86763 = CARTESIAN_POINT('Ctrl Pts',(74.1913108545003,231.779798513214,30.7213203435596)) ;
#86764 = CARTESIAN_POINT('Ctrl Pts',(74.2,231.735896122602,30.7213203435596)) ;
#86765 = CARTESIAN_POINT('Ctrl Pts',(74.2,231.69860111669,30.7213203435596)) ;
#86766 = CARTESIAN_POINT('',(74.2,232.,30.7213203435596)) ;
#86767 = CARTESIAN_POINT('',(66.8,254.6,30.7213203435596)) ;
#86768 = CARTESIAN_POINT('',(65.,254.6,30.7213203435596)) ;
#86769 = CARTESIAN_POINT('',(67.3070907072649,254.6,30.7213203435596)) ;
#86770 = CARTESIAN_POINT('',(64.7,254.90139888331,30.7213203435596)) ;
#86771 = CARTESIAN_POINT('Ctrl Pts',(65.,254.6,30.7213203435596)) ;
#86772 = CARTESIAN_POINT('Ctrl Pts',(64.9630257843965,254.6,30.7213203435596)) ;
#86773 = CARTESIAN_POINT('Ctrl Pts',(64.9195130912898,254.608675189374,30.7213203435596)) ;
#86774 = CARTESIAN_POINT('Ctrl Pts',(64.8511517474623,254.637045411928,30.7213203435596)) ;
#86775 = CARTESIAN_POINT('Ctrl Pts',(64.8142240147817,254.661783948368,30.7213203435596)) ;
#86776 = CARTESIAN_POINT('Ctrl Pts',(64.7618245202167,254.714300461156,30.7213203435596)) ;
#86777 = CARTESIAN_POINT('Ctrl Pts',(64.7371143581605,254.751400609842,30.7213203435596)) ;
#86778 = CARTESIAN_POINT('Ctrl Pts',(64.7086891454997,254.820201486786,30.7213203435596)) ;
#86779 = CARTESIAN_POINT('Ctrl Pts',(64.7,254.864103877398,30.7213203435596)) ;
#86780 = CARTESIAN_POINT('Ctrl Pts',(64.7,254.90139888331,30.7213203435596)) ;
#86781 = CARTESIAN_POINT('',(64.7,256.69860111669,30.7213203435596)) ;
#86782 = CARTESIAN_POINT('',(64.7,247.688656108704,30.7213203435596)) ;
#86783 = CARTESIAN_POINT('',(65.,257.,30.7213203435596)) ;
#86784 = CARTESIAN_POINT('Ctrl Pts',(64.7,256.69860111669,30.7213203435596)) ;
#86785 = CARTESIAN_POINT('Ctrl Pts',(64.7,256.735896122602,30.7213203435596)) ;
#86786 = CARTESIAN_POINT('Ctrl Pts',(64.7086891454997,256.779798513214,30.7213203435596)) ;
#86787 = CARTESIAN_POINT('Ctrl Pts',(64.7371143581605,256.848599390158,30.7213203435596)) ;
#86788 = CARTESIAN_POINT('Ctrl Pts',(64.7618245202167,256.885699538844,30.7213203435596)) ;
#86789 = CARTESIAN_POINT('Ctrl Pts',(64.8142240147817,256.938216051632,30.7213203435596)) ;
#86790 = CARTESIAN_POINT('Ctrl Pts',(64.8511517474623,256.962954588072,30.7213203435596)) ;
#86791 = CARTESIAN_POINT('Ctrl Pts',(64.9195130912898,256.991324810626,30.7213203435596)) ;
#86792 = CARTESIAN_POINT('Ctrl Pts',(64.9630257843965,257.,30.7213203435596)) ;
#86793 = CARTESIAN_POINT('Ctrl Pts',(65.,257.,30.7213203435596)) ;
#86794 = CARTESIAN_POINT('',(66.8,257.,30.7213203435596)) ;
#86795 = CARTESIAN_POINT('',(68.5070907072649,257.,30.7213203435596)) ;
#86796 = CARTESIAN_POINT('',(67.1,256.69860111669,30.7213203435596)) ;
#86797 = CARTESIAN_POINT('Ctrl Pts',(66.8,257.,30.7213203435596)) ;
#86798 = CARTESIAN_POINT('Ctrl Pts',(66.8369742156035,257.,30.7213203435596)) ;
#86799 = CARTESIAN_POINT('Ctrl Pts',(66.8804869087102,256.991324810626,30.7213203435596)) ;
#86800 = CARTESIAN_POINT('Ctrl Pts',(66.9488482525377,256.962954588072,30.7213203435596)) ;
#86801 = CARTESIAN_POINT('Ctrl Pts',(66.9857759852183,256.938216051632,30.7213203435596)) ;
#86802 = CARTESIAN_POINT('Ctrl Pts',(67.0381754797833,256.885699538844,30.7213203435596)) ;
#86803 = CARTESIAN_POINT('Ctrl Pts',(67.0628856418395,256.848599390158,30.7213203435596)) ;
#86804 = CARTESIAN_POINT('Ctrl Pts',(67.0913108545003,256.779798513214,30.7213203435596)) ;
#86805 = CARTESIAN_POINT('Ctrl Pts',(67.1,256.735896122602,30.7213203435596)) ;
#86806 = CARTESIAN_POINT('Ctrl Pts',(67.1,256.69860111669,30.7213203435596)) ;
#86807 = CARTESIAN_POINT('',(67.1,254.90139888331,30.7213203435596)) ;
#86808 = CARTESIAN_POINT('',(67.1,246.488656108704,30.7213203435596)) ;
#86809 = CARTESIAN_POINT('Ctrl Pts',(67.1,254.90139888331,30.7213203435596)) ;
#86810 = CARTESIAN_POINT('Ctrl Pts',(67.1,254.864103877398,30.7213203435596)) ;
#86811 = CARTESIAN_POINT('Ctrl Pts',(67.0913108545003,254.820201486786,30.7213203435596)) ;
#86812 = CARTESIAN_POINT('Ctrl Pts',(67.0628856418395,254.751400609842,30.7213203435596)) ;
#86813 = CARTESIAN_POINT('Ctrl Pts',(67.0381754797833,254.714300461156,30.7213203435596)) ;
#86814 = CARTESIAN_POINT('Ctrl Pts',(66.9857759852183,254.661783948368,30.7213203435596)) ;
#86815 = CARTESIAN_POINT('Ctrl Pts',(66.9488482525377,254.637045411928,30.7213203435596)) ;
#86816 = CARTESIAN_POINT('Ctrl Pts',(66.8804869087102,254.608675189374,30.7213203435596)) ;
#86817 = CARTESIAN_POINT('Ctrl Pts',(66.8369742156035,254.6,30.7213203435596)) ;
#86818 = CARTESIAN_POINT('Ctrl Pts',(66.8,254.6,30.7213203435596)) ;
#86819 = CARTESIAN_POINT('',(62.0573593128807,233.6,30.7213203435596)) ;
#86820 = CARTESIAN_POINT('',(60.2573593128808,233.6,30.7213203435596)) ;
#86821 = CARTESIAN_POINT('',(64.9357703637053,233.6,30.7213203435596)) ;
#86822 = CARTESIAN_POINT('',(59.9573593128807,233.90139888331,30.7213203435596)) ;
#86823 = CARTESIAN_POINT('Ctrl Pts',(60.2573593128808,233.6,30.7213203435596)) ;
#86824 = CARTESIAN_POINT('Ctrl Pts',(60.2203850972773,233.6,30.7213203435596)) ;
#86825 = CARTESIAN_POINT('Ctrl Pts',(60.1768724041706,233.608675189374,30.7213203435596)) ;
#86826 = CARTESIAN_POINT('Ctrl Pts',(60.1085110603431,233.637045411928,30.7213203435596)) ;
#86827 = CARTESIAN_POINT('Ctrl Pts',(60.0715833276625,233.661783948368,30.7213203435596)) ;
#86828 = CARTESIAN_POINT('Ctrl Pts',(60.0191838330975,233.714300461156,30.7213203435596)) ;
#86829 = CARTESIAN_POINT('Ctrl Pts',(59.9944736710413,233.751400609842,30.7213203435596)) ;
#86830 = CARTESIAN_POINT('Ctrl Pts',(59.9660484583805,233.820201486786,30.7213203435596)) ;
#86831 = CARTESIAN_POINT('Ctrl Pts',(59.9573593128808,233.864103877398,30.7213203435596)) ;
#86832 = CARTESIAN_POINT('Ctrl Pts',(59.9573593128808,233.90139888331,30.7213203435596)) ;
#86833 = CARTESIAN_POINT('',(59.9573593128807,235.69860111669,30.7213203435596)) ;
#86834 = CARTESIAN_POINT('',(59.9573593128807,237.188656108704,30.7213203435596)) ;
#86835 = CARTESIAN_POINT('',(60.2573593128808,236.,30.7213203435596)) ;
#86836 = CARTESIAN_POINT('Ctrl Pts',(59.9573593128808,235.69860111669,30.7213203435596)) ;
#86837 = CARTESIAN_POINT('Ctrl Pts',(59.9573593128808,235.735896122602,30.7213203435596)) ;
#86838 = CARTESIAN_POINT('Ctrl Pts',(59.9660484583805,235.779798513214,30.7213203435596)) ;
#86839 = CARTESIAN_POINT('Ctrl Pts',(59.9944736710413,235.848599390158,30.7213203435596)) ;
#86840 = CARTESIAN_POINT('Ctrl Pts',(60.0191838330975,235.885699538844,30.7213203435596)) ;
#86841 = CARTESIAN_POINT('Ctrl Pts',(60.0715833276625,235.938216051632,30.7213203435596)) ;
#86842 = CARTESIAN_POINT('Ctrl Pts',(60.1085110603431,235.962954588072,30.7213203435596)) ;
#86843 = CARTESIAN_POINT('Ctrl Pts',(60.1768724041706,235.991324810626,30.7213203435596)) ;
#86844 = CARTESIAN_POINT('Ctrl Pts',(60.2203850972773,236.,30.7213203435596)) ;
#86845 = CARTESIAN_POINT('Ctrl Pts',(60.2573593128808,236.,30.7213203435596)) ;
#86846 = CARTESIAN_POINT('',(62.0573593128807,236.,30.7213203435596)) ;
#86847 = CARTESIAN_POINT('',(66.1357703637053,236.,30.7213203435596)) ;
#86848 = CARTESIAN_POINT('',(62.3573593128808,235.69860111669,30.7213203435596)) ;
#86849 = CARTESIAN_POINT('Ctrl Pts',(62.0573593128807,236.,30.7213203435596)) ;
#86850 = CARTESIAN_POINT('Ctrl Pts',(62.0943335284842,236.,30.7213203435596)) ;
#86851 = CARTESIAN_POINT('Ctrl Pts',(62.1378462215909,235.991324810626,30.7213203435596)) ;
#86852 = CARTESIAN_POINT('Ctrl Pts',(62.2062075654184,235.962954588072,30.7213203435596)) ;
#86853 = CARTESIAN_POINT('Ctrl Pts',(62.243135298099,235.938216051632,30.7213203435596)) ;
#86854 = CARTESIAN_POINT('Ctrl Pts',(62.295534792664,235.885699538844,30.7213203435596)) ;
#86855 = CARTESIAN_POINT('Ctrl Pts',(62.3202449547202,235.848599390158,30.7213203435596)) ;
#86856 = CARTESIAN_POINT('Ctrl Pts',(62.348670167381,235.779798513214,30.7213203435596)) ;
#86857 = CARTESIAN_POINT('Ctrl Pts',(62.3573593128807,235.735896122602,30.7213203435596)) ;
#86858 = CARTESIAN_POINT('Ctrl Pts',(62.3573593128807,235.69860111669,30.7213203435596)) ;
#86859 = CARTESIAN_POINT('',(62.3573593128808,233.90139888331,30.7213203435596)) ;
#86860 = CARTESIAN_POINT('',(62.3573593128808,235.988656108704,30.7213203435596)) ;
#86861 = CARTESIAN_POINT('Ctrl Pts',(62.3573593128807,233.90139888331,30.7213203435596)) ;
#86862 = CARTESIAN_POINT('Ctrl Pts',(62.3573593128807,233.864103877398,30.7213203435596)) ;
#86863 = CARTESIAN_POINT('Ctrl Pts',(62.348670167381,233.820201486786,30.7213203435596)) ;
#86864 = CARTESIAN_POINT('Ctrl Pts',(62.3202449547202,233.751400609842,30.7213203435596)) ;
#86865 = CARTESIAN_POINT('Ctrl Pts',(62.295534792664,233.714300461156,30.7213203435596)) ;
#86866 = CARTESIAN_POINT('Ctrl Pts',(62.243135298099,233.661783948368,30.7213203435596)) ;
#86867 = CARTESIAN_POINT('Ctrl Pts',(62.2062075654184,233.637045411928,30.7213203435596)) ;
#86868 = CARTESIAN_POINT('Ctrl Pts',(62.1378462215909,233.608675189374,30.7213203435596)) ;
#86869 = CARTESIAN_POINT('Ctrl Pts',(62.0943335284842,233.6,30.7213203435596)) ;
#86870 = CARTESIAN_POINT('Ctrl Pts',(62.0573593128807,233.6,30.7213203435596)) ;
#86871 = CARTESIAN_POINT('',(58.8,254.6,30.7213203435596)) ;
#86872 = CARTESIAN_POINT('',(57.,254.6,30.7213203435596)) ;
#86873 = CARTESIAN_POINT('',(63.3070907072649,254.6,30.7213203435596)) ;
#86874 = CARTESIAN_POINT('',(56.7,254.90139888331,30.7213203435596)) ;
#86875 = CARTESIAN_POINT('Ctrl Pts',(57.,254.6,30.7213203435596)) ;
#86876 = CARTESIAN_POINT('Ctrl Pts',(56.9630257843965,254.6,30.7213203435596)) ;
#86877 = CARTESIAN_POINT('Ctrl Pts',(56.9195130912898,254.608675189374,30.7213203435596)) ;
#86878 = CARTESIAN_POINT('Ctrl Pts',(56.8511517474623,254.637045411928,30.7213203435596)) ;
#86879 = CARTESIAN_POINT('Ctrl Pts',(56.8142240147817,254.661783948368,30.7213203435596)) ;
#86880 = CARTESIAN_POINT('Ctrl Pts',(56.7618245202167,254.714300461156,30.7213203435596)) ;
#86881 = CARTESIAN_POINT('Ctrl Pts',(56.7371143581605,254.751400609842,30.7213203435596)) ;
#86882 = CARTESIAN_POINT('Ctrl Pts',(56.7086891454997,254.820201486786,30.7213203435596)) ;
#86883 = CARTESIAN_POINT('Ctrl Pts',(56.7,254.864103877398,30.7213203435596)) ;
#86884 = CARTESIAN_POINT('Ctrl Pts',(56.7,254.90139888331,30.7213203435596)) ;
#86885 = CARTESIAN_POINT('',(56.7,256.69860111669,30.7213203435596)) ;
#86886 = CARTESIAN_POINT('',(56.7,247.688656108704,30.7213203435596)) ;
#86887 = CARTESIAN_POINT('',(57.,257.,30.7213203435596)) ;
#86888 = CARTESIAN_POINT('Ctrl Pts',(56.7,256.69860111669,30.7213203435596)) ;
#86889 = CARTESIAN_POINT('Ctrl Pts',(56.7,256.735896122602,30.7213203435596)) ;
#86890 = CARTESIAN_POINT('Ctrl Pts',(56.7086891454997,256.779798513214,30.7213203435596)) ;
#86891 = CARTESIAN_POINT('Ctrl Pts',(56.7371143581605,256.848599390158,30.7213203435596)) ;
#86892 = CARTESIAN_POINT('Ctrl Pts',(56.7618245202167,256.885699538844,30.7213203435596)) ;
#86893 = CARTESIAN_POINT('Ctrl Pts',(56.8142240147817,256.938216051632,30.7213203435596)) ;
#86894 = CARTESIAN_POINT('Ctrl Pts',(56.8511517474623,256.962954588072,30.7213203435596)) ;
#86895 = CARTESIAN_POINT('Ctrl Pts',(56.9195130912898,256.991324810626,30.7213203435596)) ;
#86896 = CARTESIAN_POINT('Ctrl Pts',(56.9630257843965,257.,30.7213203435596)) ;
#86897 = CARTESIAN_POINT('Ctrl Pts',(57.,257.,30.7213203435596)) ;
#86898 = CARTESIAN_POINT('',(58.8,257.,30.7213203435596)) ;
#86899 = CARTESIAN_POINT('',(64.5070907072649,257.,30.7213203435596)) ;
#86900 = CARTESIAN_POINT('',(59.1,256.69860111669,30.7213203435596)) ;
#86901 = CARTESIAN_POINT('Ctrl Pts',(58.8,257.,30.7213203435596)) ;
#86902 = CARTESIAN_POINT('Ctrl Pts',(58.8369742156035,257.,30.7213203435596)) ;
#86903 = CARTESIAN_POINT('Ctrl Pts',(58.8804869087102,256.991324810626,30.7213203435596)) ;
#86904 = CARTESIAN_POINT('Ctrl Pts',(58.9488482525377,256.962954588072,30.7213203435596)) ;
#86905 = CARTESIAN_POINT('Ctrl Pts',(58.9857759852183,256.938216051632,30.7213203435596)) ;
#86906 = CARTESIAN_POINT('Ctrl Pts',(59.0381754797833,256.885699538844,30.7213203435596)) ;
#86907 = CARTESIAN_POINT('Ctrl Pts',(59.0628856418395,256.848599390158,30.7213203435596)) ;
#86908 = CARTESIAN_POINT('Ctrl Pts',(59.0913108545003,256.779798513214,30.7213203435596)) ;
#86909 = CARTESIAN_POINT('Ctrl Pts',(59.1,256.735896122602,30.7213203435596)) ;
#86910 = CARTESIAN_POINT('Ctrl Pts',(59.1,256.69860111669,30.7213203435596)) ;
#86911 = CARTESIAN_POINT('',(59.1,254.90139888331,30.7213203435596)) ;
#86912 = CARTESIAN_POINT('',(59.1,246.488656108705,30.7213203435596)) ;
#86913 = CARTESIAN_POINT('Ctrl Pts',(59.1,254.90139888331,30.7213203435596)) ;
#86914 = CARTESIAN_POINT('Ctrl Pts',(59.1,254.864103877398,30.7213203435596)) ;
#86915 = CARTESIAN_POINT('Ctrl Pts',(59.0913108545003,254.820201486786,30.7213203435596)) ;
#86916 = CARTESIAN_POINT('Ctrl Pts',(59.0628856418395,254.751400609842,30.7213203435596)) ;
#86917 = CARTESIAN_POINT('Ctrl Pts',(59.0381754797833,254.714300461156,30.7213203435596)) ;
#86918 = CARTESIAN_POINT('Ctrl Pts',(58.9857759852183,254.661783948368,30.7213203435596)) ;
#86919 = CARTESIAN_POINT('Ctrl Pts',(58.9488482525377,254.637045411928,30.7213203435596)) ;
#86920 = CARTESIAN_POINT('Ctrl Pts',(58.8804869087102,254.608675189374,30.7213203435596)) ;
#86921 = CARTESIAN_POINT('Ctrl Pts',(58.8369742156035,254.6,30.7213203435596)) ;
#86922 = CARTESIAN_POINT('Ctrl Pts',(58.8,254.6,30.7213203435596)) ;
#86923 = CARTESIAN_POINT('Origin',(72.0450953968556,230.688656108705,30.6213203435596)) ;
#86924 = CARTESIAN_POINT('',(72.1450953968556,223.000000000001,30.6213203435596)) ;
#86925 = CARTESIAN_POINT('',(72.1450953968556,230.688656108705,30.6213203435596)) ;
#86926 = CARTESIAN_POINT('Origin',(72.0450953968556,223.000000000001,30.6213203435596)) ;
#86927 = CARTESIAN_POINT('Origin',(72.1450953968556,223.000000000001,30.7213203435596)) ;
#86928 = CARTESIAN_POINT('',(72.1450953968556,223.000000000001,29.6213203435596)) ;
#86929 = CARTESIAN_POINT('',(72.1450953968556,230.688656108705,29.6213203435596)) ;
#86930 = CARTESIAN_POINT('',(72.1450953968556,223.000000000001,30.7213203435596)) ;
#86931 = CARTESIAN_POINT('Origin',(72.0450953968556,230.688656108705,29.6213203435596)) ;
#86932 = CARTESIAN_POINT('',(72.0450953968556,223.000000000001,29.5213203435596)) ;
#86933 = CARTESIAN_POINT('',(72.0450953968556,230.688656108705,29.5213203435596)) ;
#86934 = CARTESIAN_POINT('Origin',(72.0450953968556,223.000000000001,29.6213203435596)) ;
#86935 = CARTESIAN_POINT('Origin',(69.9141814145298,238.377312217409,29.5213203435596)) ;
#86936 = CARTESIAN_POINT('',(61.775147916658,220.442149698512,29.5213203435596)) ;
#86937 = CARTESIAN_POINT('Origin',(64.1568347953872,220.146231446812,29.5213203435596)) ;
#86938 = CARTESIAN_POINT('',(58.9573593128807,226.1,29.5213203435596)) ;
#86939 = CARTESIAN_POINT('',(58.9573593128807,226.1,29.5213203435596)) ;
#86940 = CARTESIAN_POINT('',(58.9573593128807,245.9,29.5213203435596)) ;
#86941 = CARTESIAN_POINT('',(58.9573593128807,239.1,29.5213203435596)) ;
#86942 = CARTESIAN_POINT('',(55.7,245.9,29.5213203435596)) ;
#86943 = CARTESIAN_POINT('',(58.9573593128807,245.9,29.5213203435596)) ;
#86944 = CARTESIAN_POINT('',(55.7,257.5,29.5213203435596)) ;
#86945 = CARTESIAN_POINT('',(55.7,245.9,29.5213203435596)) ;
#86946 = CARTESIAN_POINT('',(67.6,257.5,29.5213203435596)) ;
#86947 = CARTESIAN_POINT('',(55.7,257.5,29.5213203435596)) ;
#86948 = CARTESIAN_POINT('',(67.6,253.900000000001,29.5213203435596)) ;
#86949 = CARTESIAN_POINT('',(67.6,257.5,29.5213203435596)) ;
#86950 = CARTESIAN_POINT('',(79.1,253.900000000001,29.5213203435596)) ;
#86951 = CARTESIAN_POINT('',(67.6,253.900000000001,29.5213203435596)) ;
#86952 = CARTESIAN_POINT('',(79.1,246.500000000001,29.5213203435596)) ;
#86953 = CARTESIAN_POINT('',(79.1,246.138656108705,29.5213203435596)) ;
#86954 = CARTESIAN_POINT('',(81.9668461709225,246.500000000001,29.5213203435596)) ;
#86955 = CARTESIAN_POINT('',(74.5570907072649,246.500000000001,29.5213203435596)) ;
#86956 = CARTESIAN_POINT('',(82.2732639481701,246.357115043876,29.5213203435596)) ;
#86957 = CARTESIAN_POINT('Origin',(81.9668461709225,246.100000000001,29.5213203435596)) ;
#86958 = CARTESIAN_POINT('',(83.9347806063073,244.376996597386,29.5213203435596)) ;
#86959 = CARTESIAN_POINT('',(81.6097350811727,247.14787795491,29.5213203435596)) ;
#86960 = CARTESIAN_POINT('',(84.0283628290597,244.119881553511,29.5213203435596)) ;
#86961 = CARTESIAN_POINT('Origin',(83.6283628290597,244.119881553511,29.5213203435596)) ;
#86962 = CARTESIAN_POINT('',(84.0283628290597,241.083851787777,29.5213203435596)) ;
#86963 = CARTESIAN_POINT('',(84.0283628290597,241.339589444027,29.5213203435596)) ;
#86964 = CARTESIAN_POINT('',(83.9347806063073,240.826736743903,29.5213203435596)) ;
#86965 = CARTESIAN_POINT('Origin',(83.6283628290597,241.083851787777,29.5213203435596)) ;
#86966 = CARTESIAN_POINT('',(82.183342912681,238.739454580319,29.5213203435596)) ;
#86967 = CARTESIAN_POINT('',(80.4937295064186,236.72585173331,29.5213203435596)) ;
#86968 = CARTESIAN_POINT('',(82.1067384683691,238.703733341287,29.5213203435596)) ;
#86969 = CARTESIAN_POINT('Origin',(82.1067384683691,238.803733341287,29.5213203435596)) ;
#86970 = CARTESIAN_POINT('',(80.1000000000001,238.703733341287,29.5213203435596)) ;
#86971 = CARTESIAN_POINT('',(76.057090707265,238.703733341287,29.5213203435596)) ;
#86972 = CARTESIAN_POINT('',(80.1000000000001,235.614468918958,29.5213203435596)) ;
#86973 = CARTESIAN_POINT('',(80.1000000000001,238.490522779348,29.5213203435596)) ;
#86974 = CARTESIAN_POINT('',(79.0976680713511,231.000000000001,29.5213203435596)) ;
#86975 = CARTESIAN_POINT('',(80.1582163984138,235.882481693345,29.5213203435596)) ;
#86976 = CARTESIAN_POINT('',(74.7,231.000000000001,29.5213203435596)) ;
#86977 = CARTESIAN_POINT('',(79.2,231.000000000001,29.5213203435596)) ;
#86978 = CARTESIAN_POINT('',(74.7,226.067880390059,29.5213203435596)) ;
#86979 = CARTESIAN_POINT('',(74.7,231.000000000001,29.5213203435596)) ;
#86980 = CARTESIAN_POINT('Origin',(75.1450953968556,223.000000000001,29.5213203435596)) ;
#86981 = CARTESIAN_POINT('',(78.381026119647,242.900000000001,29.5213203435596)) ;
#86982 = CARTESIAN_POINT('',(75.4756995384723,242.900000000001,29.5213203435596)) ;
#86983 = CARTESIAN_POINT('Origin',(76.9283628290597,242.900000000001,29.5213203435596)) ;
#86984 = CARTESIAN_POINT('',(75.4756995384723,240.900000000001,29.5213203435596)) ;
#86985 = CARTESIAN_POINT('',(75.4756995384723,240.900000000001,29.5213203435596)) ;
#86986 = CARTESIAN_POINT('',(78.381026119647,240.900000000001,29.5213203435596)) ;
#86987 = CARTESIAN_POINT('Origin',(76.9283628290597,240.900000000001,29.5213203435596)) ;
#86988 = CARTESIAN_POINT('',(78.381026119647,242.900000000001,29.5213203435596)) ;
#86989 = CARTESIAN_POINT('',(74.2,229.6,29.5213203435596)) ;
#86990 = CARTESIAN_POINT('',(74.2,232.,29.5213203435596)) ;
#86991 = CARTESIAN_POINT('',(74.2,232.,29.5213203435596)) ;
#86992 = CARTESIAN_POINT('',(71.8,232.,29.5213203435596)) ;
#86993 = CARTESIAN_POINT('',(71.8,232.,29.5213203435596)) ;
#86994 = CARTESIAN_POINT('',(71.8,229.6,29.5213203435596)) ;
#86995 = CARTESIAN_POINT('',(71.8,229.6,29.5213203435596)) ;
#86996 = CARTESIAN_POINT('',(74.2,229.6,29.5213203435596)) ;
#86997 = CARTESIAN_POINT('Origin',(79.1,246.138656108705,29.6213203435596)) ;
#86998 = CARTESIAN_POINT('',(79.2,253.900000000001,29.6213203435596)) ;
#86999 = CARTESIAN_POINT('Origin',(79.1,253.900000000001,29.6213203435596)) ;
#87000 = CARTESIAN_POINT('',(79.2,246.600000000001,29.6213203435596)) ;
#87001 = CARTESIAN_POINT('',(79.2,246.138656108705,29.6213203435596)) ;
#87002 = CARTESIAN_POINT('Origin',(79.1,246.500000000001,29.6213203435596)) ;
#87003 = CARTESIAN_POINT('Origin',(79.1,246.138656108705,30.6213203435596)) ;
#87004 = CARTESIAN_POINT('',(79.2,253.900000000001,30.6213203435596)) ;
#87005 = CARTESIAN_POINT('Origin',(79.1,253.900000000001,30.6213203435596)) ;
#87006 = CARTESIAN_POINT('',(79.2,246.600000000001,30.6213203435596)) ;
#87007 = CARTESIAN_POINT('Origin',(79.1,246.500000000001,30.6213203435596)) ;
#87008 = CARTESIAN_POINT('',(79.2,246.138656108705,30.6213203435596)) ;
#87009 = CARTESIAN_POINT('Origin',(79.2,253.900000000001,30.7213203435596)) ;
#87010 = CARTESIAN_POINT('',(79.2,253.900000000001,30.7213203435596)) ;
#87011 = CARTESIAN_POINT('',(79.2,246.600000000001,30.7213203435596)) ;
#87012 = CARTESIAN_POINT('Origin',(83.6283628290597,244.119881553511,29.6213203435596)) ;
#87013 = CARTESIAN_POINT('',(84.1283628290597,244.119881553511,29.6213203435596)) ;
#87014 = CARTESIAN_POINT('Origin',(84.0283628290597,244.119881553511,29.6213203435596)) ;
#87015 = CARTESIAN_POINT('',(84.0113850506192,244.441275358355,29.6213203435596)) ;
#87016 = CARTESIAN_POINT('Origin',(83.9347806063073,244.376996597386,29.6213203435596)) ;
#87017 = CARTESIAN_POINT('Origin',(83.6283628290597,244.119881553511,29.6213203435596)) ;
#87018 = CARTESIAN_POINT('Origin',(83.6283628290597,244.119881553511,30.6213203435596)) ;
#87019 = CARTESIAN_POINT('',(84.1283628290597,244.119881553511,30.6213203435596)) ;
#87020 = CARTESIAN_POINT('Origin',(84.0283628290597,244.119881553511,30.6213203435596)) ;
#87021 = CARTESIAN_POINT('',(84.0113850506192,244.441275358355,30.6213203435596)) ;
#87022 = CARTESIAN_POINT('Origin',(83.6283628290597,244.119881553511,30.6213203435596)) ;
#87023 = CARTESIAN_POINT('Origin',(83.9347806063073,244.376996597386,30.6213203435596)) ;
#87024 = CARTESIAN_POINT('Origin',(83.6283628290597,244.119881553511,30.7213203435596)) ;
#87025 = CARTESIAN_POINT('',(84.1283628290597,244.119881553511,30.7213203435596)) ;
#87026 = CARTESIAN_POINT('',(84.0113850506192,244.441275358355,30.7213203435596)) ;
#87027 = CARTESIAN_POINT('Origin',(84.1283628290597,244.301866670644,30.7213203435596)) ;
#87028 = CARTESIAN_POINT('',(84.1283628290596,241.083851787777,30.6213203435596)) ;
#87029 = CARTESIAN_POINT('',(84.1283628290597,241.339589444027,30.6213203435596)) ;
#87030 = CARTESIAN_POINT('',(84.1283628290596,241.083851787777,29.6213203435596)) ;
#87031 = CARTESIAN_POINT('',(84.1283628290597,241.083851787777,30.7213203435596)) ;
#87032 = CARTESIAN_POINT('',(84.1283628290597,241.339589444027,29.6213203435596)) ;
#87033 = CARTESIAN_POINT('Origin',(84.0283628290597,241.339589444027,30.6213203435596)) ;
#87034 = CARTESIAN_POINT('Origin',(84.0283628290596,241.083851787777,30.6213203435596)) ;
#87035 = CARTESIAN_POINT('Origin',(81.6097350811727,247.14787795491,30.6213203435596)) ;
#87036 = CARTESIAN_POINT('',(82.349868392482,246.421393804845,30.6213203435596)) ;
#87037 = CARTESIAN_POINT('',(81.6863395254846,247.212156715879,30.6213203435596)) ;
#87038 = CARTESIAN_POINT('Origin',(82.2732639481701,246.357115043876,30.6213203435596)) ;
#87039 = CARTESIAN_POINT('Origin',(81.9668461709225,246.100000000001,29.6213203435596)) ;
#87040 = CARTESIAN_POINT('',(82.349868392482,246.421393804845,29.6213203435596)) ;
#87041 = CARTESIAN_POINT('Origin',(82.2732639481701,246.357115043876,29.6213203435596)) ;
#87042 = CARTESIAN_POINT('',(81.9668461709225,246.600000000001,29.6213203435596)) ;
#87043 = CARTESIAN_POINT('Origin',(81.9668461709225,246.500000000001,29.6213203435596)) ;
#87044 = CARTESIAN_POINT('Origin',(81.9668461709225,246.100000000001,29.6213203435596)) ;
#87045 = CARTESIAN_POINT('Origin',(81.9668461709225,246.100000000001,30.6213203435596)) ;
#87046 = CARTESIAN_POINT('',(81.9668461709225,246.600000000001,30.6213203435596)) ;
#87047 = CARTESIAN_POINT('Origin',(81.9668461709225,246.100000000001,30.6213203435596)) ;
#87048 = CARTESIAN_POINT('Origin',(81.9668461709225,246.500000000001,30.6213203435596)) ;
#87049 = CARTESIAN_POINT('Origin',(81.9668461709225,246.100000000001,30.7213203435596)) ;
#87050 = CARTESIAN_POINT('',(82.349868392482,246.421393804845,30.7213203435596)) ;
#87051 = CARTESIAN_POINT('',(81.9668461709225,246.600000000001,30.7213203435596)) ;
#87052 = CARTESIAN_POINT('Origin',(81.6097350811727,247.14787795491,29.6213203435596)) ;
#87053 = CARTESIAN_POINT('',(81.6863395254846,247.212156715879,29.6213203435596)) ;
#87054 = CARTESIAN_POINT('Origin',(82.2,246.600000000001,30.7213203435596)) ;
#87055 = CARTESIAN_POINT('Origin',(83.6283628290597,241.083851787777,29.6213203435596)) ;
#87056 = CARTESIAN_POINT('',(84.0113850506191,240.762457982934,29.6213203435596)) ;
#87057 = CARTESIAN_POINT('Origin',(83.9347806063072,240.826736743903,29.6213203435596)) ;
#87058 = CARTESIAN_POINT('Origin',(84.0283628290596,241.083851787777,29.6213203435596)) ;
#87059 = CARTESIAN_POINT('Origin',(83.6283628290597,241.083851787777,29.6213203435596)) ;
#87060 = CARTESIAN_POINT('Origin',(83.6283628290597,241.083851787777,30.6213203435596)) ;
#87061 = CARTESIAN_POINT('',(84.0113850506191,240.762457982934,30.6213203435596)) ;
#87062 = CARTESIAN_POINT('Origin',(83.9347806063072,240.826736743903,30.6213203435596)) ;
#87063 = CARTESIAN_POINT('Origin',(83.6283628290597,241.083851787777,30.6213203435596)) ;
#87064 = CARTESIAN_POINT('Origin',(83.6283628290597,241.083851787777,30.7213203435596)) ;
#87065 = CARTESIAN_POINT('',(84.0113850506192,240.762457982934,30.7213203435596)) ;
#87066 = CARTESIAN_POINT('Origin',(80.4937295064186,236.72585173331,29.6213203435596)) ;
#87067 = CARTESIAN_POINT('',(82.2599473569929,238.67517581935,29.6213203435596)) ;
#87068 = CARTESIAN_POINT('',(80.5703339507305,236.661572972341,29.6213203435596)) ;
#87069 = CARTESIAN_POINT('Origin',(82.183342912681,238.739454580319,29.6213203435596)) ;
#87070 = CARTESIAN_POINT('Origin',(84.1283628290597,240.901866670644,30.7213203435596)) ;
#87071 = CARTESIAN_POINT('',(82.2599473569929,238.67517581935,30.6213203435596)) ;
#87072 = CARTESIAN_POINT('',(80.5703339507305,236.661572972341,30.6213203435596)) ;
#87073 = CARTESIAN_POINT('',(82.2599473569929,238.67517581935,30.7213203435596)) ;
#87074 = CARTESIAN_POINT('Origin',(80.4937295064186,236.72585173331,30.6213203435596)) ;
#87075 = CARTESIAN_POINT('Origin',(82.183342912681,238.739454580319,30.6213203435596)) ;
#87076 = CARTESIAN_POINT('Ctrl Pts',(80.1000000000001,238.703733341287,30.7213203435596)) ;
#87077 = CARTESIAN_POINT('Ctrl Pts',(80.1673349911517,238.681308542337,30.7213203435596)) ;
#87078 = CARTESIAN_POINT('Ctrl Pts',(80.3246968018175,238.628902299152,30.70305597993)) ;
#87079 = CARTESIAN_POINT('Ctrl Pts',(80.4001384593499,238.603722491233,30.6512500569856)) ;
#87080 = CARTESIAN_POINT('Ctrl Pts',(80.4001060221343,238.603733317644,30.621286553673)) ;
#87081 = CARTESIAN_POINT('Ctrl Pts',(80.1000000000001,238.703733341287,30.7213203435596)) ;
#87082 = CARTESIAN_POINT('Ctrl Pts',(80.1598499591183,238.673823510303,30.7213203435596)) ;
#87083 = CARTESIAN_POINT('Ctrl Pts',(80.3006804267155,238.603362191114,30.6841188443569)) ;
#87084 = CARTESIAN_POINT('Ctrl Pts',(80.3477306429498,238.603762877822,30.635414869881)) ;
#87085 = CARTESIAN_POINT('Ctrl Pts',(80.3477104110672,238.603762708834,30.6213044253022)) ;
#87086 = CARTESIAN_POINT('Ctrl Pts',(80.1000000000001,238.703733341287,30.7213203435596)) ;
#87087 = CARTESIAN_POINT('Ctrl Pts',(80.1448798950513,238.658853446236,30.7213203435596)) ;
#87088 = CARTESIAN_POINT('Ctrl Pts',(80.2522646492235,238.551468692064,30.664890088409)) ;
#87089 = CARTESIAN_POINT('Ctrl Pts',(80.2434889907335,238.560244350553,30.6174238570621)) ;
#87090 = CARTESIAN_POINT('Ctrl Pts',(80.2434927581474,238.560240583139,30.6213247294469)) ;
#87091 = CARTESIAN_POINT('Ctrl Pts',(80.1000000000001,238.703733341287,30.7213203435596)) ;
#87092 = CARTESIAN_POINT('Ctrl Pts',(80.1299098309844,238.643883382169,30.7213203435596)) ;
#87093 = CARTESIAN_POINT('Ctrl Pts',(80.2003711501734,238.503052914572,30.684118844357)) ;
#87094 = CARTESIAN_POINT('Ctrl Pts',(80.1999704634652,238.456002698337,30.6354148698811)) ;
#87095 = CARTESIAN_POINT('Ctrl Pts',(80.1999706324531,238.45602293022,30.6213044253022)) ;
#87096 = CARTESIAN_POINT('Ctrl Pts',(80.1000000000001,238.703733341287,30.7213203435596)) ;
#87097 = CARTESIAN_POINT('Ctrl Pts',(80.1224247989508,238.636398350136,30.7213203435596)) ;
#87098 = CARTESIAN_POINT('Ctrl Pts',(80.1748310421352,238.479036539469,30.7030559799303)) ;
#87099 = CARTESIAN_POINT('Ctrl Pts',(80.2000108500545,238.403594881936,30.6512500569859)) ;
#87100 = CARTESIAN_POINT('Ctrl Pts',(80.2000000236427,238.403627319152,30.621286553673)) ;
#87101 = CARTESIAN_POINT('',(80.2000000000001,238.403733341287,30.6213203435596)) ;
#87102 = CARTESIAN_POINT('',(80.4000000000001,238.603733341287,30.6213203435596)) ;
#87103 = CARTESIAN_POINT('Origin',(80.4000000000001,238.403733341287,30.6213203435596)) ;
#87104 = CARTESIAN_POINT('',(80.2871000903541,238.641366644502,30.6994893600058)) ;
#87105 = CARTESIAN_POINT('Origin',(80.1000000000001,238.703733341287,30.6213203435596)) ;
#87106 = CARTESIAN_POINT('Origin',(80.1000000000001,238.703733341287,30.6213203435596)) ;
#87107 = CARTESIAN_POINT('',(80.1623666967849,238.516633250933,30.6994893600057)) ;
#87108 = CARTESIAN_POINT('Origin',(80.1000000000001,238.703733341287,30.6213203435596)) ;
#87109 = CARTESIAN_POINT('Origin',(80.1000000000001,238.703733341287,30.6213203435596)) ;
#87110 = CARTESIAN_POINT('Origin',(80.4000000000001,238.403733341287,30.7213203435596)) ;
#87111 = CARTESIAN_POINT('',(80.2000000000001,238.403733341287,29.6213203435596)) ;
#87112 = CARTESIAN_POINT('',(80.2000000000001,238.403733341287,30.7213203435596)) ;
#87113 = CARTESIAN_POINT('',(80.4000000000001,238.603733341287,29.6213203435596)) ;
#87114 = CARTESIAN_POINT('Origin',(80.4000000000001,238.403733341287,29.6213203435596)) ;
#87115 = CARTESIAN_POINT('',(80.4000000000001,238.603733341287,30.7213203435596)) ;
#87116 = CARTESIAN_POINT('Ctrl Pts',(80.1000000000001,238.703733341287,29.5213203435596)) ;
#87117 = CARTESIAN_POINT('Ctrl Pts',(80.12242479571,238.636398346894,29.5213203435596)) ;
#87118 = CARTESIAN_POINT('Ctrl Pts',(80.1748310522054,238.479036465714,29.539584677183)) ;
#87119 = CARTESIAN_POINT('Ctrl Pts',(80.2000108523797,238.40359485233,29.5913906280511)) ;
#87120 = CARTESIAN_POINT('Ctrl Pts',(80.2000000236528,238.403627296473,29.6213541406864)) ;
#87121 = CARTESIAN_POINT('Ctrl Pts',(80.1000000000001,238.703733341287,29.5213203435596)) ;
#87122 = CARTESIAN_POINT('Ctrl Pts',(80.1299098288238,238.643883380009,29.5213203435596)) ;
#87123 = CARTESIAN_POINT('Ctrl Pts',(80.2003711613395,238.503052837057,29.5585219149689)) ;
#87124 = CARTESIAN_POINT('Ctrl Pts',(80.1999704571707,238.456002678962,29.6072258190892)) ;
#87125 = CARTESIAN_POINT('Ctrl Pts',(80.1999706262014,238.456022915153,29.6213362652259)) ;
#87126 = CARTESIAN_POINT('Ctrl Pts',(80.1000000000001,238.703733341287,29.5213203435596)) ;
#87127 = CARTESIAN_POINT('Ctrl Pts',(80.1448798950518,238.658853446236,29.5213203435596)) ;
#87128 = CARTESIAN_POINT('Ctrl Pts',(80.2522647587334,238.551468582557,29.5777508728895)) ;
#87129 = CARTESIAN_POINT('Ctrl Pts',(80.2434889412482,238.560244400044,29.6252168369043)) ;
#87130 = CARTESIAN_POINT('Ctrl Pts',(80.2434927095359,238.560240631756,29.6213159567278)) ;
#87131 = CARTESIAN_POINT('Ctrl Pts',(80.1000000000001,238.703733341287,29.5213203435596)) ;
#87132 = CARTESIAN_POINT('Ctrl Pts',(80.15984996128,238.673823512465,29.5213203435596)) ;
#87133 = CARTESIAN_POINT('Ctrl Pts',(80.300680504234,238.603362179951,29.5585219149676)) ;
#87134 = CARTESIAN_POINT('Ctrl Pts',(80.3477306623321,238.603762884119,29.607225819088)) ;
#87135 = CARTESIAN_POINT('Ctrl Pts',(80.3477104261414,238.603762715089,29.6213362652259)) ;
#87136 = CARTESIAN_POINT('Ctrl Pts',(80.1000000000001,238.703733341287,29.5213203435596)) ;
#87137 = CARTESIAN_POINT('Ctrl Pts',(80.1673349943943,238.681308545579,29.5213203435596)) ;
#87138 = CARTESIAN_POINT('Ctrl Pts',(80.3246968755785,238.628902289088,29.5395846771792)) ;
#87139 = CARTESIAN_POINT('Ctrl Pts',(80.4001384889675,238.603722488907,29.5913906280479)) ;
#87140 = CARTESIAN_POINT('Ctrl Pts',(80.4001060448247,238.603733317634,29.6213541406864)) ;
#87141 = CARTESIAN_POINT('',(80.1623667045681,238.516633227583,29.5431513333233)) ;
#87142 = CARTESIAN_POINT('Origin',(80.1000000000001,238.703733341287,29.6213203435596)) ;
#87143 = CARTESIAN_POINT('Origin',(80.1000000000001,238.703733341287,29.6213203435596)) ;
#87144 = CARTESIAN_POINT('',(80.2871001137062,238.641366636718,29.5431513333238)) ;
#87145 = CARTESIAN_POINT('Origin',(80.1000000000001,238.703733341287,29.6213203435596)) ;
#87146 = CARTESIAN_POINT('Origin',(80.1000000000001,238.703733341287,29.6213203435596)) ;
#87147 = CARTESIAN_POINT('Origin',(80.2000000000001,238.603733341287,30.7213203435596)) ;
#87148 = CARTESIAN_POINT('',(80.2000000000001,235.603733341287,30.6213203435596)) ;
#87149 = CARTESIAN_POINT('',(80.2000000000001,238.490522779348,30.6213203435596)) ;
#87150 = CARTESIAN_POINT('',(80.2000000000001,235.603733341287,29.6213203435596)) ;
#87151 = CARTESIAN_POINT('',(80.2000000000001,235.603733341287,30.7213203435596)) ;
#87152 = CARTESIAN_POINT('',(80.2000000000001,238.490522779348,29.6213203435596)) ;
#87153 = CARTESIAN_POINT('Origin',(80.1000000000001,238.490522779348,30.6213203435596)) ;
#87154 = CARTESIAN_POINT('Origin',(80.1000000000001,235.614468918958,30.6213203435596)) ;
#87155 = CARTESIAN_POINT('Origin',(76.057090707265,238.703733341287,30.6213203435596)) ;
#87156 = CARTESIAN_POINT('',(82.1067384683691,238.603733341287,30.6213203435596)) ;
#87157 = CARTESIAN_POINT('',(76.057090707265,238.603733341287,30.6213203435596)) ;
#87158 = CARTESIAN_POINT('Origin',(82.1067384683691,238.703733341287,30.6213203435596)) ;
#87159 = CARTESIAN_POINT('Ctrl Pts',(82.2599473569933,238.67517581935,29.6213203435597)) ;
#87160 = CARTESIAN_POINT('Ctrl Pts',(82.1999999999999,238.603733341287,29.6213203435598)) ;
#87161 = CARTESIAN_POINT('Ctrl Pts',(82.106738468368,238.603733341287,29.6213203435596)) ;
#87162 = CARTESIAN_POINT('Ctrl Pts',(82.2599473569934,238.67517581935,29.5213203435594)) ;
#87163 = CARTESIAN_POINT('Ctrl Pts',(82.2,238.603733341287,29.5213203435595)) ;
#87164 = CARTESIAN_POINT('Ctrl Pts',(82.1067384683682,238.603733341287,29.5213203435592)) ;
#87165 = CARTESIAN_POINT('Ctrl Pts',(82.183342912681,238.739454580319,29.5213203435596)) ;
#87166 = CARTESIAN_POINT('Ctrl Pts',(82.1533692341843,238.703733341287,29.5213203435597)) ;
#87167 = CARTESIAN_POINT('Ctrl Pts',(82.1067384683682,238.703733341287,29.5213203435596)) ;
#87168 = CARTESIAN_POINT('',(82.1067384683691,238.603733341287,29.6213203435596)) ;
#87169 = CARTESIAN_POINT('Origin',(82.1067384683691,238.703733341287,29.6213203435596)) ;
#87170 = CARTESIAN_POINT('Origin',(82.1067384683691,238.803733341287,29.6213203435596)) ;
#87171 = CARTESIAN_POINT('Ctrl Pts',(82.183342912681,238.739454580319,30.7213203435596)) ;
#87172 = CARTESIAN_POINT('Ctrl Pts',(82.1533692341851,238.703733341287,30.7213203435595)) ;
#87173 = CARTESIAN_POINT('Ctrl Pts',(82.1067384683691,238.703733341287,30.7213203435597)) ;
#87174 = CARTESIAN_POINT('Ctrl Pts',(82.2599473569944,238.675175819352,30.7213203435596)) ;
#87175 = CARTESIAN_POINT('Ctrl Pts',(82.2000000000015,238.603733341286,30.7213203435595)) ;
#87176 = CARTESIAN_POINT('Ctrl Pts',(82.1067384683677,238.603733341287,30.7213203435597)) ;
#87177 = CARTESIAN_POINT('Ctrl Pts',(82.2599473569945,238.675175819352,30.6213203435595)) ;
#87178 = CARTESIAN_POINT('Ctrl Pts',(82.2000000000014,238.603733341286,30.6213203435594)) ;
#87179 = CARTESIAN_POINT('Ctrl Pts',(82.1067384683674,238.603733341287,30.6213203435596)) ;
#87180 = CARTESIAN_POINT('Origin',(82.1067384683691,238.803733341287,30.6213203435596)) ;
#87181 = CARTESIAN_POINT('Origin',(82.1067384683691,238.803733341287,30.7213203435596)) ;
#87182 = CARTESIAN_POINT('',(82.1067384683691,238.603733341287,30.7213203435596)) ;
#87183 = CARTESIAN_POINT('Origin',(76.057090707265,238.703733341287,29.6213203435596)) ;
#87184 = CARTESIAN_POINT('',(76.057090707265,238.603733341287,29.6213203435596)) ;
#87185 = CARTESIAN_POINT('Origin',(82.2000000000001,238.603733341287,30.7213203435596)) ;
#87186 = CARTESIAN_POINT('Origin',(75.3756995384723,240.638656108705,30.6213203435596)) ;
#87187 = CARTESIAN_POINT('',(75.4756995384723,242.900000000001,30.6213203435596)) ;
#87188 = CARTESIAN_POINT('Origin',(75.3756995384723,242.900000000001,30.6213203435596)) ;
#87189 = CARTESIAN_POINT('',(75.4756995384723,240.900000000001,30.6213203435596)) ;
#87190 = CARTESIAN_POINT('Origin',(75.3756995384723,240.900000000001,30.6213203435596)) ;
#87191 = CARTESIAN_POINT('',(75.4756995384723,240.638656108705,30.6213203435596)) ;
#87192 = CARTESIAN_POINT('Origin',(76.9283628290597,240.900000000001,30.6213203435596)) ;
#87193 = CARTESIAN_POINT('',(78.381026119647,240.900000000001,30.6213203435596)) ;
#87194 = CARTESIAN_POINT('Origin',(78.481026119647,240.900000000001,30.6213203435596)) ;
#87195 = CARTESIAN_POINT('Origin',(76.9283628290597,240.900000000001,30.6213203435596)) ;
#87196 = CARTESIAN_POINT('Origin',(78.481026119647,239.638656108705,30.6213203435596)) ;
#87197 = CARTESIAN_POINT('',(78.381026119647,242.900000000001,30.6213203435596)) ;
#87198 = CARTESIAN_POINT('Origin',(78.481026119647,242.900000000001,30.6213203435596)) ;
#87199 = CARTESIAN_POINT('',(78.381026119647,239.638656108705,30.6213203435596)) ;
#87200 = CARTESIAN_POINT('Origin',(76.9283628290597,242.900000000001,30.6213203435596)) ;
#87201 = CARTESIAN_POINT('Origin',(76.9283628290597,242.900000000001,30.6213203435596)) ;
#87202 = CARTESIAN_POINT('Origin',(76.9283628290597,242.900000000001,30.7213203435596)) ;
#87203 = CARTESIAN_POINT('',(75.4756995384723,242.900000000001,30.7213203435596)) ;
#87204 = CARTESIAN_POINT('',(78.381026119647,242.900000000001,30.7213203435596)) ;
#87205 = CARTESIAN_POINT('Origin',(75.4756995384723,242.900000000001,30.7213203435596)) ;
#87206 = CARTESIAN_POINT('',(75.4756995384723,240.900000000001,30.7213203435596)) ;
#87207 = CARTESIAN_POINT('Origin',(75.1450953968556,223.000000000001,30.6213203435596)) ;
#87208 = CARTESIAN_POINT('',(74.7,226.000000000001,30.6954104575527)) ;
#87209 = CARTESIAN_POINT('Ctrl Pts',(74.7,226.000000000001,30.6954104575527)) ;
#87210 = CARTESIAN_POINT('Ctrl Pts',(74.7,226.008355406754,30.7029024804683)) ;
#87211 = CARTESIAN_POINT('Ctrl Pts',(74.7,226.019099007153,30.709548142939)) ;
#87212 = CARTESIAN_POINT('Ctrl Pts',(74.7,226.040633652905,30.7184120613473)) ;
#87213 = CARTESIAN_POINT('Ctrl Pts',(74.7,226.055366277592,30.7213203435596)) ;
#87214 = CARTESIAN_POINT('Ctrl Pts',(74.7,226.067880390058,30.7213203435596)) ;
#87215 = CARTESIAN_POINT('',(75.1450953968557,226.000000000001,30.6213203435596)) ;
#87216 = CARTESIAN_POINT('Origin',(75.1450953968556,223.000000000001,30.6213203435596)) ;
#87217 = CARTESIAN_POINT('Ctrl Pts',(75.1450953968556,226.000000000001,30.6213203435596)) ;
#87218 = CARTESIAN_POINT('Ctrl Pts',(75.0066828077914,226.000000000001,30.6465909093173)) ;
#87219 = CARTESIAN_POINT('Ctrl Pts',(74.8525909945362,226.000000000001,30.6751106345129)) ;
#87220 = CARTESIAN_POINT('Ctrl Pts',(74.7,226.000000000001,30.6954104575527)) ;
#87221 = CARTESIAN_POINT('Origin',(74.7,226.000000000001,30.7213203435596)) ;
#87222 = CARTESIAN_POINT('',(75.1450953968557,226.000000000001,29.6213203435596)) ;
#87223 = CARTESIAN_POINT('',(75.1450953968557,226.000000000001,30.7213203435596)) ;
#87224 = CARTESIAN_POINT('',(74.7,226.000000000001,29.5472302295665)) ;
#87225 = CARTESIAN_POINT('Ctrl Pts',(74.7,226.000000000001,29.5472302295665)) ;
#87226 = CARTESIAN_POINT('Ctrl Pts',(74.8525909945361,226.000000000001,29.5675300526063)) ;
#87227 = CARTESIAN_POINT('Ctrl Pts',(75.0066828077914,226.000000000001,29.5960497778019)) ;
#87228 = CARTESIAN_POINT('Ctrl Pts',(75.1450953968556,226.000000000001,29.6213203435596)) ;
#87229 = CARTESIAN_POINT('',(74.7,226.000000000001,30.7213203435596)) ;
#87230 = CARTESIAN_POINT('Origin',(75.1450953968556,223.000000000001,30.7213203435596)) ;
#87231 = CARTESIAN_POINT('Origin',(75.1450953968556,223.000000000001,29.6213203435596)) ;
#87232 = CARTESIAN_POINT('Origin',(72.1450953968557,220.362610236549,30.7213203435596)) ;
#87233 = CARTESIAN_POINT('',(66.5470607720161,220.362610236549,30.7213203435596)) ;
#87234 = CARTESIAN_POINT('Origin',(75.1450953968556,223.000000000001,29.6213203435596)) ;
#87235 = CARTESIAN_POINT('Ctrl Pts',(74.7,226.067880390058,29.5213203435596)) ;
#87236 = CARTESIAN_POINT('Ctrl Pts',(74.7,226.055366277592,29.5213203435595)) ;
#87237 = CARTESIAN_POINT('Ctrl Pts',(74.7,226.040633652905,29.5242286257719)) ;
#87238 = CARTESIAN_POINT('Ctrl Pts',(74.7,226.019099007153,29.5330925441802)) ;
#87239 = CARTESIAN_POINT('Ctrl Pts',(74.7,226.008355406754,29.5397382066508)) ;
#87240 = CARTESIAN_POINT('Ctrl Pts',(74.7,226.000000000001,29.5472302295665)) ;
#87241 = CARTESIAN_POINT('Origin',(74.7,231.000000000001,30.7213203435596)) ;
#87242 = CARTESIAN_POINT('',(74.7,231.000000000001,30.7213203435596)) ;
#87243 = CARTESIAN_POINT('Origin',(80.1582163984138,235.882481693345,29.6213203435596)) ;
#87244 = CARTESIAN_POINT('',(79.2,231.000000000001,29.6213203435596)) ;
#87245 = CARTESIAN_POINT('',(80.2559376094964,235.861255179157,29.6213203435596)) ;
#87246 = CARTESIAN_POINT('Origin',(79.0976680713511,231.000000000001,29.6213203435596)) ;
#87247 = CARTESIAN_POINT('Origin',(80.1000000000001,235.614468918958,29.6213203435596)) ;
#87248 = CARTESIAN_POINT('Origin',(80.1000000000001,238.490522779348,29.6213203435596)) ;
#87249 = CARTESIAN_POINT('Origin',(84.0283628290597,241.339589444027,29.6213203435596)) ;
#87250 = CARTESIAN_POINT('Origin',(74.5570907072649,246.500000000001,29.6213203435596)) ;
#87251 = CARTESIAN_POINT('',(74.5570907072649,246.600000000001,29.6213203435596)) ;
#87252 = CARTESIAN_POINT('Origin',(79.2,231.000000000001,30.7213203435596)) ;
#87253 = CARTESIAN_POINT('',(79.2,231.000000000001,30.6213203435596)) ;
#87254 = CARTESIAN_POINT('',(79.2,231.000000000001,30.7213203435596)) ;
#87255 = CARTESIAN_POINT('Origin',(79.0976680713511,231.000000000001,30.6213203435596)) ;
#87256 = CARTESIAN_POINT('Origin',(80.2000000000001,235.603733341287,30.7213203435596)) ;
#87257 = CARTESIAN_POINT('',(80.2559376094964,235.861255179157,30.6213203435596)) ;
#87258 = CARTESIAN_POINT('Origin',(79.2,246.600000000001,30.7213203435596)) ;
#87259 = CARTESIAN_POINT('',(74.5570907072649,246.600000000001,30.6213203435596)) ;
#87260 = CARTESIAN_POINT('Origin',(74.5570907072649,246.500000000001,30.6213203435596)) ;
#87261 = CARTESIAN_POINT('Origin',(80.1582163984138,235.882481693345,30.6213203435596)) ;
#87262 = CARTESIAN_POINT('Origin',(57.,255.80417392569,30.6213203435596)) ;
#87263 = CARTESIAN_POINT('',(56.7,255.80417392569,31.5213203435596)) ;
#87264 = CARTESIAN_POINT('',(57.,255.80417392569,31.8213203435596)) ;
#87265 = CARTESIAN_POINT('Origin',(57.,255.80417392569,31.5213203435596)) ;
#87266 = CARTESIAN_POINT('Origin',(57.,255.80417392569,30.6213203435596)) ;
#87267 = CARTESIAN_POINT('Origin',(56.7,255.80417392569,30.6213203435596)) ;
#87268 = CARTESIAN_POINT('Origin',(57.,256.4,31.5213203435596)) ;
#87269 = CARTESIAN_POINT('',(56.7,255.79582607431,31.5213203435596)) ;
#87270 = CARTESIAN_POINT('',(57.,255.79582607431,31.8213203435596)) ;
#87271 = CARTESIAN_POINT('Origin',(57.,255.79582607431,31.5213203435596)) ;
#87272 = CARTESIAN_POINT('',(57.,256.4,31.8213203435596)) ;
#87273 = CARTESIAN_POINT('',(56.7,256.4,31.5213203435596)) ;
#87274 = CARTESIAN_POINT('Origin',(57.,255.79582607431,30.6213203435596)) ;
#87275 = CARTESIAN_POINT('Origin',(57.,255.79582607431,30.6213203435596)) ;
#87276 = CARTESIAN_POINT('Origin',(56.7,255.79582607431,30.6213203435596)) ;
#87277 = CARTESIAN_POINT('Origin',(56.7,257.,30.2213203435596)) ;
#87278 = CARTESIAN_POINT('Origin',(58.8,255.79582607431,30.6213203435596)) ;
#87279 = CARTESIAN_POINT('',(59.1,255.79582607431,31.5213203435596)) ;
#87280 = CARTESIAN_POINT('',(58.8,255.79582607431,31.8213203435596)) ;
#87281 = CARTESIAN_POINT('Origin',(58.8,255.79582607431,31.5213203435596)) ;
#87282 = CARTESIAN_POINT('Origin',(58.8,255.79582607431,30.6213203435596)) ;
#87283 = CARTESIAN_POINT('Origin',(59.1,255.79582607431,30.6213203435596)) ;
#87284 = CARTESIAN_POINT('Origin',(58.8,255.2,31.5213203435596)) ;
#87285 = CARTESIAN_POINT('',(59.1,255.80417392569,31.5213203435596)) ;
#87286 = CARTESIAN_POINT('',(58.8,255.80417392569,31.8213203435596)) ;
#87287 = CARTESIAN_POINT('Origin',(58.8,255.80417392569,31.5213203435596)) ;
#87288 = CARTESIAN_POINT('',(58.8,255.2,31.8213203435596)) ;
#87289 = CARTESIAN_POINT('',(59.1,255.2,31.5213203435596)) ;
#87290 = CARTESIAN_POINT('Origin',(58.8,255.80417392569,30.6213203435596)) ;
#87291 = CARTESIAN_POINT('Origin',(58.8,255.80417392569,30.6213203435596)) ;
#87292 = CARTESIAN_POINT('Origin',(59.1,255.80417392569,30.6213203435596)) ;
#87293 = CARTESIAN_POINT('Origin',(59.1,254.6,30.2213203435596)) ;
#87294 = CARTESIAN_POINT('Origin',(66.8,255.79582607431,30.6213203435596)) ;
#87295 = CARTESIAN_POINT('',(67.1,255.79582607431,31.5213203435596)) ;
#87296 = CARTESIAN_POINT('',(66.8,255.79582607431,31.8213203435596)) ;
#87297 = CARTESIAN_POINT('Origin',(66.8,255.79582607431,31.5213203435596)) ;
#87298 = CARTESIAN_POINT('Origin',(66.8,255.79582607431,30.6213203435596)) ;
#87299 = CARTESIAN_POINT('Origin',(67.1,255.79582607431,30.6213203435596)) ;
#87300 = CARTESIAN_POINT('Origin',(66.8,255.2,31.5213203435596)) ;
#87301 = CARTESIAN_POINT('',(67.1,255.80417392569,31.5213203435596)) ;
#87302 = CARTESIAN_POINT('',(66.8,255.80417392569,31.8213203435596)) ;
#87303 = CARTESIAN_POINT('Origin',(66.8,255.80417392569,31.5213203435596)) ;
#87304 = CARTESIAN_POINT('',(66.8,255.2,31.8213203435596)) ;
#87305 = CARTESIAN_POINT('',(67.1,255.2,31.5213203435596)) ;
#87306 = CARTESIAN_POINT('Origin',(66.8,255.80417392569,30.6213203435596)) ;
#87307 = CARTESIAN_POINT('Origin',(66.8,255.80417392569,30.6213203435596)) ;
#87308 = CARTESIAN_POINT('Origin',(67.1,255.80417392569,30.6213203435596)) ;
#87309 = CARTESIAN_POINT('Origin',(67.1,254.6,30.2213203435596)) ;
#87310 = CARTESIAN_POINT('Origin',(65.,255.80417392569,30.6213203435596)) ;
#87311 = CARTESIAN_POINT('',(64.7,255.80417392569,31.5213203435596)) ;
#87312 = CARTESIAN_POINT('',(65.,255.80417392569,31.8213203435596)) ;
#87313 = CARTESIAN_POINT('Origin',(65.,255.80417392569,31.5213203435596)) ;
#87314 = CARTESIAN_POINT('Origin',(65.,255.80417392569,30.6213203435596)) ;
#87315 = CARTESIAN_POINT('Origin',(64.7,255.80417392569,30.6213203435596)) ;
#87316 = CARTESIAN_POINT('Origin',(65.,256.4,31.5213203435596)) ;
#87317 = CARTESIAN_POINT('',(64.7,255.79582607431,31.5213203435596)) ;
#87318 = CARTESIAN_POINT('',(65.,255.79582607431,31.8213203435596)) ;
#87319 = CARTESIAN_POINT('Origin',(65.,255.79582607431,31.5213203435596)) ;
#87320 = CARTESIAN_POINT('',(65.,256.4,31.8213203435596)) ;
#87321 = CARTESIAN_POINT('',(64.7,256.4,31.5213203435596)) ;
#87322 = CARTESIAN_POINT('Origin',(65.,255.79582607431,30.6213203435596)) ;
#87323 = CARTESIAN_POINT('Origin',(65.,255.79582607431,30.6213203435596)) ;
#87324 = CARTESIAN_POINT('Origin',(64.7,255.79582607431,30.6213203435596)) ;
#87325 = CARTESIAN_POINT('Origin',(64.7,257.,30.2213203435596)) ;
#87326 = CARTESIAN_POINT('Origin',(62.0573593128807,234.79582607431,30.6213203435596)) ;
#87327 = CARTESIAN_POINT('',(62.3573593128808,234.79582607431,31.5213203435596)) ;
#87328 = CARTESIAN_POINT('',(62.0573593128807,234.79582607431,31.8213203435596)) ;
#87329 = CARTESIAN_POINT('Origin',(62.0573593128807,234.79582607431,31.5213203435596)) ;
#87330 = CARTESIAN_POINT('Origin',(62.0573593128807,234.79582607431,30.6213203435596)) ;
#87331 = CARTESIAN_POINT('Origin',(62.3573593128808,234.79582607431,30.6213203435596)) ;
#87332 = CARTESIAN_POINT('Origin',(62.0573593128807,234.2,31.5213203435596)) ;
#87333 = CARTESIAN_POINT('',(62.3573593128808,234.80417392569,31.5213203435596)) ;
#87334 = CARTESIAN_POINT('',(62.0573593128807,234.80417392569,31.8213203435596)) ;
#87335 = CARTESIAN_POINT('Origin',(62.0573593128807,234.80417392569,31.5213203435596)) ;
#87336 = CARTESIAN_POINT('',(62.0573593128807,234.2,31.8213203435596)) ;
#87337 = CARTESIAN_POINT('',(62.3573593128808,234.2,31.5213203435596)) ;
#87338 = CARTESIAN_POINT('Origin',(62.0573593128807,234.80417392569,30.6213203435596)) ;
#87339 = CARTESIAN_POINT('Origin',(62.0573593128807,234.80417392569,30.6213203435596)) ;
#87340 = CARTESIAN_POINT('Origin',(62.3573593128808,234.80417392569,30.6213203435596)) ;
#87341 = CARTESIAN_POINT('Origin',(62.3573593128808,233.6,30.2213203435596)) ;
#87342 = CARTESIAN_POINT('Origin',(60.2573593128808,234.80417392569,30.6213203435596)) ;
#87343 = CARTESIAN_POINT('',(59.9573593128807,234.80417392569,31.5213203435596)) ;
#87344 = CARTESIAN_POINT('',(60.2573593128808,234.80417392569,31.8213203435596)) ;
#87345 = CARTESIAN_POINT('Origin',(60.2573593128808,234.80417392569,31.5213203435596)) ;
#87346 = CARTESIAN_POINT('Origin',(60.2573593128808,234.80417392569,30.6213203435596)) ;
#87347 = CARTESIAN_POINT('Origin',(59.9573593128807,234.80417392569,30.6213203435596)) ;
#87348 = CARTESIAN_POINT('Origin',(60.2573593128808,235.4,31.5213203435596)) ;
#87349 = CARTESIAN_POINT('',(59.9573593128807,234.79582607431,31.5213203435596)) ;
#87350 = CARTESIAN_POINT('',(60.2573593128808,234.79582607431,31.8213203435596)) ;
#87351 = CARTESIAN_POINT('Origin',(60.2573593128808,234.79582607431,31.5213203435596)) ;
#87352 = CARTESIAN_POINT('',(60.2573593128808,235.4,31.8213203435596)) ;
#87353 = CARTESIAN_POINT('',(59.9573593128807,235.4,31.5213203435596)) ;
#87354 = CARTESIAN_POINT('Origin',(60.2573593128808,234.79582607431,30.6213203435596)) ;
#87355 = CARTESIAN_POINT('Origin',(60.2573593128808,234.79582607431,30.6213203435596)) ;
#87356 = CARTESIAN_POINT('Origin',(59.9573593128807,234.79582607431,30.6213203435596)) ;
#87357 = CARTESIAN_POINT('Origin',(59.9573593128807,236.,30.2213203435596)) ;
#87358 = CARTESIAN_POINT('Origin',(73.9,230.79582607431,30.6213203435596)) ;
#87359 = CARTESIAN_POINT('',(74.2,230.79582607431,31.5213203435596)) ;
#87360 = CARTESIAN_POINT('',(73.9,230.79582607431,31.8213203435596)) ;
#87361 = CARTESIAN_POINT('Origin',(73.9,230.79582607431,31.5213203435596)) ;
#87362 = CARTESIAN_POINT('Origin',(73.9,230.79582607431,30.6213203435596)) ;
#87363 = CARTESIAN_POINT('Origin',(74.2,230.79582607431,30.6213203435596)) ;
#87364 = CARTESIAN_POINT('Origin',(73.9,230.2,31.5213203435596)) ;
#87365 = CARTESIAN_POINT('',(74.2,230.80417392569,31.5213203435596)) ;
#87366 = CARTESIAN_POINT('',(73.9,230.80417392569,31.8213203435596)) ;
#87367 = CARTESIAN_POINT('Origin',(73.9,230.80417392569,31.5213203435596)) ;
#87368 = CARTESIAN_POINT('',(73.9,230.2,31.8213203435596)) ;
#87369 = CARTESIAN_POINT('',(74.2,230.2,31.5213203435596)) ;
#87370 = CARTESIAN_POINT('Origin',(73.9,230.80417392569,30.6213203435596)) ;
#87371 = CARTESIAN_POINT('Origin',(73.9,230.80417392569,30.6213203435596)) ;
#87372 = CARTESIAN_POINT('Origin',(74.2,230.80417392569,30.6213203435596)) ;
#87373 = CARTESIAN_POINT('Origin',(74.2,229.6,30.2213203435596)) ;
#87374 = CARTESIAN_POINT('Origin',(72.1,230.80417392569,30.6213203435596)) ;
#87375 = CARTESIAN_POINT('',(71.8,230.80417392569,31.5213203435596)) ;
#87376 = CARTESIAN_POINT('',(72.1,230.80417392569,31.8213203435596)) ;
#87377 = CARTESIAN_POINT('Origin',(72.1,230.80417392569,31.5213203435596)) ;
#87378 = CARTESIAN_POINT('Origin',(72.1,230.80417392569,30.6213203435596)) ;
#87379 = CARTESIAN_POINT('Origin',(71.8,230.80417392569,30.6213203435596)) ;
#87380 = CARTESIAN_POINT('Origin',(72.1,231.4,31.5213203435596)) ;
#87381 = CARTESIAN_POINT('',(71.8,230.79582607431,31.5213203435596)) ;
#87382 = CARTESIAN_POINT('',(72.1,230.79582607431,31.8213203435596)) ;
#87383 = CARTESIAN_POINT('Origin',(72.1,230.79582607431,31.5213203435596)) ;
#87384 = CARTESIAN_POINT('',(72.1,231.4,31.8213203435596)) ;
#87385 = CARTESIAN_POINT('',(71.8,231.4,31.5213203435596)) ;
#87386 = CARTESIAN_POINT('Origin',(72.1,230.79582607431,30.6213203435596)) ;
#87387 = CARTESIAN_POINT('Origin',(72.1,230.79582607431,30.6213203435596)) ;
#87388 = CARTESIAN_POINT('Origin',(71.8,230.79582607431,30.6213203435596)) ;
#87389 = CARTESIAN_POINT('Origin',(71.8,232.,30.2213203435596)) ;
#87390 = CARTESIAN_POINT('Origin',(71.8,230.80417392569,30.6213203435596)) ;
#87391 = CARTESIAN_POINT('',(71.8,230.80417392569,31.8213203435596)) ;
#87392 = CARTESIAN_POINT('Origin',(73.,230.8,31.8213203435596)) ;
#87393 = CARTESIAN_POINT('',(74.2,230.79582607431,31.8213203435596)) ;
#87394 = CARTESIAN_POINT('Origin',(74.2,230.79582607431,30.6213203435596)) ;
#87395 = CARTESIAN_POINT('Origin',(66.1357703637053,234.80417392569,30.6213203435596)) ;
#87396 = CARTESIAN_POINT('',(66.1357703637053,234.80417392569,31.8213203435596)) ;
#87397 = CARTESIAN_POINT('Origin',(61.1573593128808,234.8,31.8213203435596)) ;
#87398 = CARTESIAN_POINT('',(64.9357703637053,234.79582607431,31.8213203435596)) ;
#87399 = CARTESIAN_POINT('Origin',(64.9357703637053,234.79582607431,30.6213203435596)) ;
#87400 = CARTESIAN_POINT('Origin',(67.3070907072649,255.79582607431,30.6213203435596)) ;
#87401 = CARTESIAN_POINT('',(67.3070907072649,255.79582607431,31.8213203435596)) ;
#87402 = CARTESIAN_POINT('Origin',(65.9,255.8,31.8213203435596)) ;
#87403 = CARTESIAN_POINT('',(68.5070907072649,255.80417392569,31.8213203435596)) ;
#87404 = CARTESIAN_POINT('Origin',(68.5070907072649,255.80417392569,30.6213203435596)) ;
#87405 = CARTESIAN_POINT('Origin',(64.5070907072649,255.80417392569,30.6213203435596)) ;
#87406 = CARTESIAN_POINT('',(64.5070907072649,255.80417392569,31.8213203435596)) ;
#87407 = CARTESIAN_POINT('Origin',(57.9,255.8,31.8213203435596)) ;
#87408 = CARTESIAN_POINT('',(63.3070907072649,255.79582607431,31.8213203435596)) ;
#87409 = CARTESIAN_POINT('Origin',(63.3070907072649,255.79582607431,30.6213203435596)) ;
#87410 = CARTESIAN_POINT('Origin',(73.,230.8,30.2213203435596)) ;
#87411 = CARTESIAN_POINT('',(74.2,229.6,30.2213203435596)) ;
#87412 = CARTESIAN_POINT('',(74.2,232.,30.2213203435596)) ;
#87413 = CARTESIAN_POINT('',(74.2,230.2,30.2213203435596)) ;
#87414 = CARTESIAN_POINT('',(71.8,229.6,30.2213203435596)) ;
#87415 = CARTESIAN_POINT('',(72.4,229.6,30.2213203435596)) ;
#87416 = CARTESIAN_POINT('',(71.8,232.,30.2213203435596)) ;
#87417 = CARTESIAN_POINT('',(71.8,231.4,30.2213203435596)) ;
#87418 = CARTESIAN_POINT('',(73.6,232.,30.2213203435596)) ;
#87419 = CARTESIAN_POINT('Origin',(74.2,232.,30.7213203435596)) ;
#87420 = CARTESIAN_POINT('',(71.8,232.,30.7213203435596)) ;
#87421 = CARTESIAN_POINT('',(74.2,232.,30.7213203435596)) ;
#87422 = CARTESIAN_POINT('Origin',(71.8,232.,30.7213203435596)) ;
#87423 = CARTESIAN_POINT('',(71.8,229.6,30.7213203435596)) ;
#87424 = CARTESIAN_POINT('Origin',(64.1568347953872,220.146231446812,30.7213203435596)) ;
#87425 = CARTESIAN_POINT('',(61.775147916658,220.442149698512,30.7213203435596)) ;
#87426 = CARTESIAN_POINT('Origin',(62.3665731005048,219.254624434818,30.7213203435596)) ;
#87427 = CARTESIAN_POINT('',(58.9573593128807,226.1,30.7213203435596)) ;
#87428 = CARTESIAN_POINT('Origin',(78.381026119647,240.900000000001,30.7213203435596)) ;
#87429 = CARTESIAN_POINT('',(78.381026119647,240.900000000001,30.7213203435596)) ;
#87430 = CARTESIAN_POINT('Origin',(76.9283628290597,240.900000000001,30.7213203435596)) ;
#87431 = CARTESIAN_POINT('Origin',(71.8,229.6,30.7213203435596)) ;
#87432 = CARTESIAN_POINT('',(74.2,229.6,30.7213203435596)) ;
#87433 = CARTESIAN_POINT('Origin',(74.2,229.6,30.7213203435596)) ;
#87434 = CARTESIAN_POINT('Origin',(67.6,253.900000000001,30.7213203435596)) ;
#87435 = CARTESIAN_POINT('',(67.6,253.900000000001,30.7213203435596)) ;
#87436 = CARTESIAN_POINT('Origin',(67.6,257.5,30.7213203435596)) ;
#87437 = CARTESIAN_POINT('',(67.6,257.5,30.7213203435596)) ;
#87438 = CARTESIAN_POINT('Origin',(55.7,257.5,30.7213203435596)) ;
#87439 = CARTESIAN_POINT('',(55.7,257.5,30.7213203435596)) ;
#87440 = CARTESIAN_POINT('Origin',(55.7,245.9,30.7213203435596)) ;
#87441 = CARTESIAN_POINT('',(55.7,245.9,30.7213203435596)) ;
#87442 = CARTESIAN_POINT('Origin',(58.9573593128807,245.9,30.7213203435596)) ;
#87443 = CARTESIAN_POINT('',(58.9573593128807,245.9,30.7213203435596)) ;
#87444 = CARTESIAN_POINT('Origin',(58.9573593128807,226.1,30.7213203435596)) ;
#87445 = CARTESIAN_POINT('',(0.,0.,0.)) ;
#87446 = CARTESIAN_POINT('Origin',(34.2,257.9,30.7213203435596)) ;
#87447 = CARTESIAN_POINT('',(34.2,257.9,30.7213203435596)) ;
#87448 = CARTESIAN_POINT('',(29.2,257.9,30.7213203435596)) ;
#87449 = CARTESIAN_POINT('',(34.2,257.9,30.7213203435596)) ;
#87450 = CARTESIAN_POINT('',(29.2,257.9,29.5213203435596)) ;
#87451 = CARTESIAN_POINT('',(29.2,257.9,30.7213203435596)) ;
#87452 = CARTESIAN_POINT('',(34.2,257.9,29.5213203435596)) ;
#87453 = CARTESIAN_POINT('',(34.2,257.9,29.5213203435596)) ;
#87454 = CARTESIAN_POINT('',(34.2,257.9,30.7213203435596)) ;
#87455 = CARTESIAN_POINT('Origin',(34.2,263.8,30.7213203435596)) ;
#87456 = CARTESIAN_POINT('',(34.2,263.8,30.7213203435596)) ;
#87457 = CARTESIAN_POINT('',(34.2,263.8,30.7213203435596)) ;
#87458 = CARTESIAN_POINT('',(34.2,263.8,29.5213203435596)) ;
#87459 = CARTESIAN_POINT('',(34.2,263.8,29.5213203435596)) ;
#87460 = CARTESIAN_POINT('',(34.2,263.8,30.7213203435596)) ;
#87461 = CARTESIAN_POINT('Origin',(29.2,263.8,30.7213203435596)) ;
#87462 = CARTESIAN_POINT('',(29.2,263.8,30.7213203435596)) ;
#87463 = CARTESIAN_POINT('',(29.2,263.8,30.7213203435596)) ;
#87464 = CARTESIAN_POINT('',(29.2,263.8,29.5213203435596)) ;
#87465 = CARTESIAN_POINT('',(29.2,263.8,29.5213203435596)) ;
#87466 = CARTESIAN_POINT('',(29.2,263.8,30.7213203435596)) ;
#87467 = CARTESIAN_POINT('Origin',(29.2,257.9,30.7213203435596)) ;
#87468 = CARTESIAN_POINT('',(29.2,257.9,30.7213203435596)) ;
#87469 = CARTESIAN_POINT('',(29.2,257.9,29.5213203435596)) ;
#87470 = CARTESIAN_POINT('Origin',(31.7,260.85,29.5213203435596)) ;
#87471 = CARTESIAN_POINT('Origin',(31.7,260.85,30.7213203435596)) ;
#87472 = CARTESIAN_POINT('',(0.,0.,0.)) ;
#87473 = CARTESIAN_POINT('Origin',(64.1568347953872,220.146231446812,30.2741067480597)) ;
#87474 = CARTESIAN_POINT('',(62.1568347953872,220.146231446812,30.2741067480597)) ;
#87475 = CARTESIAN_POINT('',(66.1568347953872,220.146231446812,30.2741067480597)) ;
#87476 = CARTESIAN_POINT('Origin',(64.1568347953872,220.146231446812,30.2741067480597)) ;
#87477 = CARTESIAN_POINT('',(66.5568347953872,220.146231446812,30.7213203435596)) ;
#87478 = CARTESIAN_POINT('Origin',(66.6068347953872,220.146231446812,30.2741067480597)) ;
#87479 = CARTESIAN_POINT('',(61.7568347953872,220.146231446812,30.7213203435596)) ;
#87480 = CARTESIAN_POINT('Origin',(64.1568347953872,220.146231446812,30.7213203435596)) ;
#87481 = CARTESIAN_POINT('Origin',(64.1568347953872,220.146231446812,30.7213203435596)) ;
#87482 = CARTESIAN_POINT('Origin',(64.1568347953872,220.146231446812,30.2741067480597)) ;
#87483 = CARTESIAN_POINT('Origin',(64.1568347953872,220.146231446812,30.7213203435596)) ;
#87484 = CARTESIAN_POINT('',(62.1568347953872,220.146231446812,28.7213203435596)) ;
#87485 = CARTESIAN_POINT('',(62.1568347953872,220.146231446812,30.7213203435596)) ;
#87486 = CARTESIAN_POINT('Origin',(64.1568347953872,220.146231446812,28.7213203435596)) ;
#87487 = CARTESIAN_POINT('Origin',(64.1568347953872,220.146231446812,30.7213203435596)) ;
#87488 = CARTESIAN_POINT('',(61.7568347953872,220.146231446812,28.7213203435596)) ;
#87489 = CARTESIAN_POINT('Origin',(64.1568347953872,220.146231446812,28.7213203435596)) ;
#87490 = CARTESIAN_POINT('',(61.7568347953872,220.146231446812,30.7213203435596)) ;
#87491 = CARTESIAN_POINT('Origin',(64.1568347953872,220.146231446812,28.7213203435596)) ;
#87492 = CARTESIAN_POINT('',(0.,0.,0.)) ;
#87493 = CARTESIAN_POINT('Origin',(61.5,261.2,30.3471546048822)) ;
#87494 = CARTESIAN_POINT('',(59.,261.2,30.3471546048822)) ;
#87495 = CARTESIAN_POINT('',(64.,261.2,30.3471546048822)) ;
#87496 = CARTESIAN_POINT('Origin',(61.5,261.2,30.3471546048822)) ;
#87497 = CARTESIAN_POINT('',(64.2,261.2,30.7213203435596)) ;
#87498 = CARTESIAN_POINT('Origin',(64.45,261.2,30.3471546048822)) ;
#87499 = CARTESIAN_POINT('',(58.8,261.2,30.7213203435596)) ;
#87500 = CARTESIAN_POINT('Origin',(61.5,261.2,30.7213203435596)) ;
#87501 = CARTESIAN_POINT('Origin',(61.5,261.2,30.7213203435596)) ;
#87502 = CARTESIAN_POINT('Origin',(61.5,261.2,30.3471546048822)) ;
#87503 = CARTESIAN_POINT('Origin',(61.5,261.2,30.7213203435596)) ;
#87504 = CARTESIAN_POINT('',(59.,261.2,28.7213203435596)) ;
#87505 = CARTESIAN_POINT('',(59.,261.2,30.7213203435596)) ;
#87506 = CARTESIAN_POINT('Origin',(61.5,261.2,28.7213203435596)) ;
#87507 = CARTESIAN_POINT('Origin',(61.5,261.2,30.7213203435596)) ;
#87508 = CARTESIAN_POINT('',(58.8,261.2,28.7213203435596)) ;
#87509 = CARTESIAN_POINT('Origin',(61.5,261.2,28.7213203435596)) ;
#87510 = CARTESIAN_POINT('',(58.8,261.2,30.7213203435596)) ;
#87511 = CARTESIAN_POINT('Origin',(61.5,261.2,28.7213203435596)) ;
#87512 = CARTESIAN_POINT('',(0.,0.,0.)) ;
#87513 = CARTESIAN_POINT('Origin',(30.7,254.8,30.2713203435596)) ;
#87514 = CARTESIAN_POINT('',(28.2,254.8,30.2713203435596)) ;
#87515 = CARTESIAN_POINT('Origin',(30.7,254.8,30.2713203435596)) ;
#87516 = CARTESIAN_POINT('',(27.75,254.8,30.7213203435596)) ;
#87517 = CARTESIAN_POINT('Origin',(27.75,254.8,30.2713203435596)) ;
#87518 = CARTESIAN_POINT('Origin',(30.7,254.8,30.7213203435596)) ;
#87519 = CARTESIAN_POINT('Origin',(30.7,254.8,30.7213203435596)) ;
#87520 = CARTESIAN_POINT('',(28.2,254.8,28.7213203435596)) ;
#87521 = CARTESIAN_POINT('',(28.2,254.8,30.7213203435596)) ;
#87522 = CARTESIAN_POINT('Origin',(30.7,254.8,28.7213203435596)) ;
#87523 = CARTESIAN_POINT('Origin',(30.7,254.8,30.7213203435596)) ;
#87524 = CARTESIAN_POINT('',(27.7,254.8,30.7213203435596)) ;
#87525 = CARTESIAN_POINT('Origin',(30.7,254.8,30.7213203435596)) ;
#87526 = CARTESIAN_POINT('Origin',(30.7,254.8,30.7213203435596)) ;
#87527 = CARTESIAN_POINT('',(27.7,254.8,28.7213203435596)) ;
#87528 = CARTESIAN_POINT('Origin',(30.7,254.8,28.7213203435596)) ;
#87529 = CARTESIAN_POINT('',(27.7,254.8,30.7213203435596)) ;
#87530 = CARTESIAN_POINT('Origin',(30.7,254.8,28.7213203435596)) ;
#87531 = CARTESIAN_POINT('',(0.,0.,0.)) ;
#87532 = CARTESIAN_POINT('Origin',(82.08,243.620000000001,31.5013203435596)) ;
#87533 = CARTESIAN_POINT('',(82.2,243.620000000001,31.5013203435596)) ;
#87534 = CARTESIAN_POINT('',(82.32,243.620000000001,31.6213203435596)) ;
#87535 = CARTESIAN_POINT('Origin',(82.32,243.620000000001,31.5013203435596)) ;
#87536 = CARTESIAN_POINT('',(82.08,243.500000000001,31.5013203435596)) ;
#87537 = CARTESIAN_POINT('Origin',(82.08,243.620000000001,31.5013203435596)) ;
#87538 = CARTESIAN_POINT('',(82.08,243.380000000001,31.6213203435596)) ;
#87539 = CARTESIAN_POINT('Origin',(82.08,243.380000000001,31.5013203435596)) ;
#87540 = CARTESIAN_POINT('Origin',(82.08,243.620000000001,31.6213203435596)) ;
#87541 = CARTESIAN_POINT('Ctrl Pts',(81.95,243.750000000001,30.9213203435596)) ;
#87542 = CARTESIAN_POINT('Ctrl Pts',(82.0831487735147,243.68224032658,30.9213203435596)) ;
#87543 = CARTESIAN_POINT('Ctrl Pts',(82.2022655046152,243.621718901757,31.0443420434627)) ;
#87544 = CARTESIAN_POINT('Ctrl Pts',(82.1999288862301,243.62290611287,31.1751079336016)) ;
#87545 = CARTESIAN_POINT('Ctrl Pts',(81.95,243.750000000001,30.9213203435596)) ;
#87546 = CARTESIAN_POINT('Ctrl Pts',(82.0707400003391,243.669831553405,30.9213203435596)) ;
#87547 = CARTESIAN_POINT('Ctrl Pts',(82.2034801642546,243.58435864747,31.023821296679)) ;
#87548 = CARTESIAN_POINT('Ctrl Pts',(82.2008789356986,243.586033838743,31.1757084682768)) ;
#87549 = CARTESIAN_POINT('Ctrl Pts',(81.95,243.750000000001,30.9213203435596)) ;
#87550 = CARTESIAN_POINT('Ctrl Pts',(82.0489448986456,243.648036451712,30.9213203435596)) ;
#87551 = CARTESIAN_POINT('Ctrl Pts',(82.1727418948934,243.51884959129,31.0059874513795)) ;
#87552 = CARTESIAN_POINT('Ctrl Pts',(82.17031722008,243.521379708731,31.1762303714321)) ;
#87553 = CARTESIAN_POINT('Ctrl Pts',(81.95,243.750000000001,30.9213203435596)) ;
#87554 = CARTESIAN_POINT('Ctrl Pts',(82.027149796952,243.626241350018,30.9213203435596)) ;
#87555 = CARTESIAN_POINT('Ctrl Pts',(82.1065333928586,243.496839168867,31.0290306789701)) ;
#87556 = CARTESIAN_POINT('Ctrl Pts',(82.1049772902892,243.499375561169,31.1755560169681)) ;
#87557 = CARTESIAN_POINT('Ctrl Pts',(81.95,243.750000000001,30.9213203435596)) ;
#87558 = CARTESIAN_POINT('Ctrl Pts',(82.0177634684342,243.6168550215,30.9213203435596)) ;
#87559 = CARTESIAN_POINT('Ctrl Pts',(82.0782935637655,243.497733002078,31.0443131727587)) ;
#87560 = CARTESIAN_POINT('Ctrl Pts',(82.0771061831309,243.500069723277,31.1751087784957)) ;
#87561 = CARTESIAN_POINT('',(82.08,243.500000000001,31.1713203435596)) ;
#87562 = CARTESIAN_POINT('',(82.2,243.620000000001,31.1713203435596)) ;
#87563 = CARTESIAN_POINT('Origin',(82.08,243.620000000001,31.1713203435596)) ;
#87564 = CARTESIAN_POINT('',(81.95,243.750000000001,30.9213203435596)) ;
#87565 = CARTESIAN_POINT('Origin',(81.95,243.750000000001,31.1713203435596)) ;
#87566 = CARTESIAN_POINT('Origin',(81.95,243.750000000001,31.1713203435596)) ;
#87567 = CARTESIAN_POINT('Origin',(82.08,243.620000000001,30.7213203435596)) ;
#87568 = CARTESIAN_POINT('',(82.08,243.500000000001,30.7213203435596)) ;
#87569 = CARTESIAN_POINT('',(82.2,243.620000000001,30.7213203435596)) ;
#87570 = CARTESIAN_POINT('Origin',(81.22,243.380000000001,31.5013203435596)) ;
#87571 = CARTESIAN_POINT('',(81.22,243.500000000001,31.5013203435596)) ;
#87572 = CARTESIAN_POINT('',(81.22,243.380000000001,31.6213203435596)) ;
#87573 = CARTESIAN_POINT('Origin',(81.22,243.380000000001,31.5013203435596)) ;
#87574 = CARTESIAN_POINT('',(81.1,243.380000000001,31.5013203435596)) ;
#87575 = CARTESIAN_POINT('Origin',(81.22,243.380000000001,31.5013203435596)) ;
#87576 = CARTESIAN_POINT('Origin',(81.22,243.380000000001,31.5013203435596)) ;
#87577 = CARTESIAN_POINT('Ctrl Pts',(80.85,243.750000000001,30.9213203435596)) ;
#87578 = CARTESIAN_POINT('Ctrl Pts',(80.9060690286283,243.66694135397,30.9213203435596)) ;
#87579 = CARTESIAN_POINT('Ctrl Pts',(81.0371686448867,243.472735445585,30.9670228859097)) ;
#87580 = CARTESIAN_POINT('Ctrl Pts',(81.1000922423061,243.379647960366,31.096644359925)) ;
#87581 = CARTESIAN_POINT('Ctrl Pts',(81.1000000308994,243.379784375592,31.1716078849273)) ;
#87582 = CARTESIAN_POINT('Ctrl Pts',(80.85,243.750000000001,30.9213203435596)) ;
#87583 = CARTESIAN_POINT('Ctrl Pts',(80.9112084395532,243.672080764895,30.9213203435596)) ;
#87584 = CARTESIAN_POINT('Ctrl Pts',(81.0547714042485,243.489170469053,30.9800563984678)) ;
#87585 = CARTESIAN_POINT('Ctrl Pts',(81.0999971368146,243.415654001957,31.1075891712013)) ;
#87586 = CARTESIAN_POINT('Ctrl Pts',(81.0999308343166,243.415761752623,31.1715657892914)) ;
#87587 = CARTESIAN_POINT('Ctrl Pts',(80.85,243.750000000001,30.9213203435596)) ;
#87588 = CARTESIAN_POINT('Ctrl Pts',(80.9202050132824,243.681077338625,30.9213203435596)) ;
#87589 = CARTESIAN_POINT('Ctrl Pts',(81.0858811028462,243.518463497089,30.9900089508676)) ;
#87590 = CARTESIAN_POINT('Ctrl Pts',(81.1301864568706,243.478022835174,31.117002321391)) ;
#87591 = CARTESIAN_POINT('Ctrl Pts',(81.1301214902666,243.478082140937,31.1715295882239)) ;
#87592 = CARTESIAN_POINT('Ctrl Pts',(80.85,243.750000000001,30.9213203435596)) ;
#87593 = CARTESIAN_POINT('Ctrl Pts',(80.9292015870114,243.690073912354,30.9213203435596)) ;
#87594 = CARTESIAN_POINT('Ctrl Pts',(81.114823358716,243.549738586775,30.9767972196575)) ;
#87595 = CARTESIAN_POINT('Ctrl Pts',(81.1933315389235,243.499977625037,31.1047490010866)) ;
#87596 = CARTESIAN_POINT('Ctrl Pts',(81.1932164772698,243.500050566896,31.1715767127306)) ;
#87597 = CARTESIAN_POINT('Ctrl Pts',(80.8500000000001,243.750000000001,30.9213203435596)) ;
#87598 = CARTESIAN_POINT('Ctrl Pts',(80.9330587498157,243.693931075158,30.9213203435596)) ;
#87599 = CARTESIAN_POINT('Ctrl Pts',(81.1272657467482,243.562830762151,30.9670226804587)) ;
#87600 = CARTESIAN_POINT('Ctrl Pts',(81.2203527598548,243.499907763237,31.0966450170891)) ;
#87601 = CARTESIAN_POINT('Ctrl Pts',(81.2202163453198,243.499999973768,31.1716078824025)) ;
#87602 = CARTESIAN_POINT('',(81.1,243.380000000001,31.1713203435596)) ;
#87603 = CARTESIAN_POINT('',(81.22,243.500000000001,31.1713203435596)) ;
#87604 = CARTESIAN_POINT('Origin',(81.22,243.380000000001,31.1713203435596)) ;
#87605 = CARTESIAN_POINT('',(81.0807585144051,243.594082084862,30.9758987384622)) ;
#87606 = CARTESIAN_POINT('Origin',(80.85,243.750000000001,31.1713203435596)) ;
#87607 = CARTESIAN_POINT('',(80.85,243.750000000001,30.9213203435596)) ;
#87608 = CARTESIAN_POINT('Origin',(80.85,243.750000000001,31.1713203435596)) ;
#87609 = CARTESIAN_POINT('',(81.0059179151387,243.519241485596,30.9758987384623)) ;
#87610 = CARTESIAN_POINT('Origin',(80.85,243.750000000001,31.1713203435596)) ;
#87611 = CARTESIAN_POINT('Origin',(80.85,243.750000000001,31.1713203435596)) ;
#87612 = CARTESIAN_POINT('Origin',(81.22,243.380000000001,30.7213203435596)) ;
#87613 = CARTESIAN_POINT('',(81.1,243.380000000001,30.7213203435596)) ;
#87614 = CARTESIAN_POINT('',(81.22,243.500000000001,30.7213203435596)) ;
#87615 = CARTESIAN_POINT('Origin',(82.08,243.980000000001,31.5013203435596)) ;
#87616 = CARTESIAN_POINT('',(82.08,244.100000000001,31.5013203435596)) ;
#87617 = CARTESIAN_POINT('',(82.08,244.220000000001,31.6213203435596)) ;
#87618 = CARTESIAN_POINT('Origin',(82.08,244.220000000001,31.5013203435596)) ;
#87619 = CARTESIAN_POINT('',(82.2,243.980000000001,31.5013203435596)) ;
#87620 = CARTESIAN_POINT('Origin',(82.08,243.980000000001,31.5013203435596)) ;
#87621 = CARTESIAN_POINT('',(82.32,243.980000000001,31.6213203435596)) ;
#87622 = CARTESIAN_POINT('Origin',(82.32,243.980000000001,31.5013203435596)) ;
#87623 = CARTESIAN_POINT('Origin',(82.08,243.980000000001,31.6213203435596)) ;
#87624 = CARTESIAN_POINT('Ctrl Pts',(81.95,243.850000000001,30.9213203435596)) ;
#87625 = CARTESIAN_POINT('Ctrl Pts',(82.0177596734215,243.983148773511,30.9213203435596)) ;
#87626 = CARTESIAN_POINT('Ctrl Pts',(82.078281098242,244.102265504606,31.0443420434537)) ;
#87627 = CARTESIAN_POINT('Ctrl Pts',(82.0770938871316,244.099928886226,31.175107933593)) ;
#87628 = CARTESIAN_POINT('Ctrl Pts',(81.95,243.850000000001,30.9213203435596)) ;
#87629 = CARTESIAN_POINT('Ctrl Pts',(82.030168446596,243.970740000336,30.9213203435596)) ;
#87630 = CARTESIAN_POINT('Ctrl Pts',(82.1156413526764,244.103480164368,31.0238212966733)) ;
#87631 = CARTESIAN_POINT('Ctrl Pts',(82.1139661614044,244.100878935816,31.1757084682668)) ;
#87632 = CARTESIAN_POINT('Ctrl Pts',(81.95,243.850000000001,30.9213203435596)) ;
#87633 = CARTESIAN_POINT('Ctrl Pts',(82.0519635482869,243.948944898645,30.9213203435596)) ;
#87634 = CARTESIAN_POINT('Ctrl Pts',(82.1811504039019,244.072741890888,31.0059874513777)) ;
#87635 = CARTESIAN_POINT('Ctrl Pts',(82.1786202865599,244.070317216158,31.1762303714208)) ;
#87636 = CARTESIAN_POINT('Ctrl Pts',(81.95,243.850000000001,30.9213203435596)) ;
#87637 = CARTESIAN_POINT('Ctrl Pts',(82.0737586499778,243.927149796954,30.9213203435596)) ;
#87638 = CARTESIAN_POINT('Ctrl Pts',(82.20316083127,244.006533392985,31.0290306789624)) ;
#87639 = CARTESIAN_POINT('Ctrl Pts',(82.2006244389709,244.004977290417,31.1755560169585)) ;
#87640 = CARTESIAN_POINT('Ctrl Pts',(81.95,243.850000000001,30.9213203435596)) ;
#87641 = CARTESIAN_POINT('Ctrl Pts',(82.0831449784942,243.917763468438,30.9213203435596)) ;
#87642 = CARTESIAN_POINT('Ctrl Pts',(82.20226699791,243.97829356377,31.0443131727465)) ;
#87643 = CARTESIAN_POINT('Ctrl Pts',(82.1999302767171,243.977106183138,31.1751087784873)) ;
#87644 = CARTESIAN_POINT('',(82.2,243.980000000001,31.1713203435596)) ;
#87645 = CARTESIAN_POINT('',(82.08,244.100000000001,31.1713203435596)) ;
#87646 = CARTESIAN_POINT('Origin',(82.08,243.980000000001,31.1713203435596)) ;
#87647 = CARTESIAN_POINT('',(81.95,243.850000000001,30.9213203435596)) ;
#87648 = CARTESIAN_POINT('Origin',(81.95,243.850000000001,31.1713203435596)) ;
#87649 = CARTESIAN_POINT('Origin',(81.95,243.850000000001,31.1713203435596)) ;
#87650 = CARTESIAN_POINT('Origin',(82.08,243.980000000001,30.7213203435596)) ;
#87651 = CARTESIAN_POINT('',(82.2,243.980000000001,30.7213203435596)) ;
#87652 = CARTESIAN_POINT('',(82.08,244.100000000001,30.7213203435596)) ;
#87653 = CARTESIAN_POINT('Origin',(82.32,243.950000000001,31.5013203435596)) ;
#87654 = CARTESIAN_POINT('',(82.32,243.950000000001,31.6213203435596)) ;
#87655 = CARTESIAN_POINT('',(82.2,243.950000000001,31.5013203435596)) ;
#87656 = CARTESIAN_POINT('Origin',(80.98,242.520000000001,31.5013203435596)) ;
#87657 = CARTESIAN_POINT('',(81.1,242.520000000001,31.5013203435596)) ;
#87658 = CARTESIAN_POINT('',(81.22,242.520000000001,31.6213203435596)) ;
#87659 = CARTESIAN_POINT('Origin',(81.22,242.520000000001,31.5013203435596)) ;
#87660 = CARTESIAN_POINT('',(80.98,242.400000000001,31.5013203435596)) ;
#87661 = CARTESIAN_POINT('Origin',(80.98,242.520000000001,31.5013203435596)) ;
#87662 = CARTESIAN_POINT('',(80.98,242.280000000001,31.6213203435596)) ;
#87663 = CARTESIAN_POINT('Origin',(80.98,242.280000000001,31.5013203435596)) ;
#87664 = CARTESIAN_POINT('Origin',(80.98,242.520000000001,31.6213203435596)) ;
#87665 = CARTESIAN_POINT('Ctrl Pts',(80.85,242.650000000001,30.9213203435596)) ;
#87666 = CARTESIAN_POINT('Ctrl Pts',(80.9831487735423,242.582240326584,30.9213203435596)) ;
#87667 = CARTESIAN_POINT('Ctrl Pts',(81.1022655046685,242.521718901747,31.0443420435114)) ;
#87668 = CARTESIAN_POINT('Ctrl Pts',(81.0999288862541,242.522906112875,31.1751079336474)) ;
#87669 = CARTESIAN_POINT('Ctrl Pts',(80.85,242.650000000001,30.9213203435596)) ;
#87670 = CARTESIAN_POINT('Ctrl Pts',(80.9707400003613,242.569831553404,30.9213203435596)) ;
#87671 = CARTESIAN_POINT('Ctrl Pts',(81.1034801636441,242.484358648257,31.0238212967098)) ;
#87672 = CARTESIAN_POINT('Ctrl Pts',(81.1008789350685,242.486033839536,31.1757084683305)) ;
#87673 = CARTESIAN_POINT('Ctrl Pts',(80.85,242.650000000001,30.9213203435596)) ;
#87674 = CARTESIAN_POINT('Ctrl Pts',(80.9489448986537,242.548036451696,30.9213203435596)) ;
#87675 = CARTESIAN_POINT('Ctrl Pts',(81.0727419165628,242.418849565278,31.0059874513892)) ;
#87676 = CARTESIAN_POINT('Ctrl Pts',(81.070317241297,242.421379683257,31.1762303714928)) ;
#87677 = CARTESIAN_POINT('Ctrl Pts',(80.85,242.650000000001,30.9213203435596)) ;
#87678 = CARTESIAN_POINT('Ctrl Pts',(80.9271497969463,242.526241349989,30.9213203435596)) ;
#87679 = CARTESIAN_POINT('Ctrl Pts',(81.0065333921819,242.396839169602,31.0290306790113)) ;
#87680 = CARTESIAN_POINT('Ctrl Pts',(81.0049772896065,242.39937556192,31.1755560170196)) ;
#87681 = CARTESIAN_POINT('Ctrl Pts',(80.8500000000001,242.650000000001,30.9213203435596)) ;
#87682 = CARTESIAN_POINT('Ctrl Pts',(80.9177634684198,242.516855021462,30.9213203435596)) ;
#87683 = CARTESIAN_POINT('Ctrl Pts',(80.9782935637477,242.39773300201,31.0443131728241)) ;
#87684 = CARTESIAN_POINT('Ctrl Pts',(80.9771061830986,242.400069723238,31.175108778541)) ;
#87685 = CARTESIAN_POINT('',(80.98,242.400000000001,31.1713203435596)) ;
#87686 = CARTESIAN_POINT('',(81.1,242.520000000001,31.1713203435596)) ;
#87687 = CARTESIAN_POINT('Origin',(80.98,242.520000000001,31.1713203435596)) ;
#87688 = CARTESIAN_POINT('',(80.85,242.650000000001,30.9213203435596)) ;
#87689 = CARTESIAN_POINT('Origin',(80.85,242.650000000001,31.1713203435596)) ;
#87690 = CARTESIAN_POINT('Origin',(80.85,242.650000000001,31.1713203435596)) ;
#87691 = CARTESIAN_POINT('Origin',(80.98,242.520000000001,30.7213203435596)) ;
#87692 = CARTESIAN_POINT('',(80.98,242.400000000001,30.7213203435596)) ;
#87693 = CARTESIAN_POINT('',(81.1,242.520000000001,30.7213203435596)) ;
#87694 = CARTESIAN_POINT('Origin',(81.22,244.220000000001,31.5013203435596)) ;
#87695 = CARTESIAN_POINT('',(81.1,244.220000000001,31.5013203435596)) ;
#87696 = CARTESIAN_POINT('',(81.22,244.220000000001,31.6213203435596)) ;
#87697 = CARTESIAN_POINT('Origin',(81.22,244.220000000001,31.5013203435596)) ;
#87698 = CARTESIAN_POINT('',(81.22,244.100000000001,31.5013203435596)) ;
#87699 = CARTESIAN_POINT('Origin',(81.22,244.220000000001,31.5013203435596)) ;
#87700 = CARTESIAN_POINT('Origin',(81.22,244.220000000001,31.5013203435596)) ;
#87701 = CARTESIAN_POINT('Ctrl Pts',(80.85,243.850000000001,30.9213203435596)) ;
#87702 = CARTESIAN_POINT('Ctrl Pts',(80.933058642349,243.906069032311,30.9213203435596)) ;
#87703 = CARTESIAN_POINT('Ctrl Pts',(81.1272644866058,244.037168619611,30.9670229231865)) ;
#87704 = CARTESIAN_POINT('Ctrl Pts',(81.2203519977101,244.100092231335,31.0966443451774)) ;
#87705 = CARTESIAN_POINT('Ctrl Pts',(81.2202155986979,244.100000030893,31.1716078506955)) ;
#87706 = CARTESIAN_POINT('Ctrl Pts',(80.85,243.850000000001,30.9213203435596)) ;
#87707 = CARTESIAN_POINT('Ctrl Pts',(80.9279192326513,243.911208442009,30.9213203435596)) ;
#87708 = CARTESIAN_POINT('Ctrl Pts',(81.1108294721138,244.05477138239,30.9800563956)) ;
#87709 = CARTESIAN_POINT('Ctrl Pts',(81.1843459682786,244.0999971372,31.1075891515919)) ;
#87710 = CARTESIAN_POINT('Ctrl Pts',(81.1842382304091,244.099930842572,31.1715657600926)) ;
#87711 = CARTESIAN_POINT('Ctrl Pts',(80.85,243.850000000001,30.9213203435596)) ;
#87712 = CARTESIAN_POINT('Ctrl Pts',(80.9189226613762,243.920205013284,30.9213203435596)) ;
#87713 = CARTESIAN_POINT('Ctrl Pts',(81.0815364284407,244.085881025253,30.9900088723548)) ;
#87714 = CARTESIAN_POINT('Ctrl Pts',(81.1219771701419,244.130186459382,31.1170022964528)) ;
#87715 = CARTESIAN_POINT('Ctrl Pts',(81.1219178713322,244.130121500405,31.1715295633574)) ;
#87716 = CARTESIAN_POINT('Ctrl Pts',(80.85,243.850000000001,30.9213203435596)) ;
#87717 = CARTESIAN_POINT('Ctrl Pts',(80.9099260901013,243.929201584559,30.9213203435596)) ;
#87718 = CARTESIAN_POINT('Ctrl Pts',(81.0502613754307,244.114823285899,30.9767972170891)) ;
#87719 = CARTESIAN_POINT('Ctrl Pts',(81.1000223723327,244.193331508108,31.1047489821795)) ;
#87720 = CARTESIAN_POINT('Ctrl Pts',(81.099949439114,244.193216460102,31.1715766822281)) ;
#87721 = CARTESIAN_POINT('Ctrl Pts',(80.85,243.850000000001,30.9213203435596)) ;
#87722 = CARTESIAN_POINT('Ctrl Pts',(80.9060689285239,243.933058746136,30.9213203435596)) ;
#87723 = CARTESIAN_POINT('Ctrl Pts',(81.0371692125707,244.127265678943,30.9670227177986)) ;
#87724 = CARTESIAN_POINT('Ctrl Pts',(81.1000922257932,244.220352717941,31.0966450022337)) ;
#87725 = CARTESIAN_POINT('Ctrl Pts',(81.1000000262267,244.220216319619,31.1716078481715)) ;
#87726 = CARTESIAN_POINT('',(81.22,244.100000000001,31.1713203435596)) ;
#87727 = CARTESIAN_POINT('',(81.1,244.220000000001,31.1713203435596)) ;
#87728 = CARTESIAN_POINT('Origin',(81.22,244.220000000001,31.1713203435596)) ;
#87729 = CARTESIAN_POINT('',(81.00591790761,244.080758503264,30.9758987324555)) ;
#87730 = CARTESIAN_POINT('Origin',(80.85,243.850000000001,31.1713203435596)) ;
#87731 = CARTESIAN_POINT('',(80.85,243.850000000001,30.9213203435596)) ;
#87732 = CARTESIAN_POINT('Origin',(80.85,243.850000000001,31.1713203435596)) ;
#87733 = CARTESIAN_POINT('',(81.0807585032626,244.005917907611,30.9758987324554)) ;
#87734 = CARTESIAN_POINT('Origin',(80.85,243.850000000001,31.1713203435596)) ;
#87735 = CARTESIAN_POINT('Origin',(80.85,243.850000000001,31.1713203435596)) ;
#87736 = CARTESIAN_POINT('Origin',(81.22,244.220000000001,30.7213203435596)) ;
#87737 = CARTESIAN_POINT('',(81.22,244.100000000001,30.7213203435596)) ;
#87738 = CARTESIAN_POINT('',(81.1,244.220000000001,30.7213203435596)) ;
#87739 = CARTESIAN_POINT('Origin',(80.95,244.220000000001,31.5013203435596)) ;
#87740 = CARTESIAN_POINT('',(80.95,244.220000000001,31.6213203435596)) ;
#87741 = CARTESIAN_POINT('',(80.95,244.100000000001,31.5013203435596)) ;
#87742 = CARTESIAN_POINT('Origin',(80.62,242.520000000001,31.5013203435596)) ;
#87743 = CARTESIAN_POINT('',(80.62,242.400000000001,31.5013203435596)) ;
#87744 = CARTESIAN_POINT('',(80.62,242.280000000001,31.6213203435596)) ;
#87745 = CARTESIAN_POINT('Origin',(80.62,242.280000000001,31.5013203435596)) ;
#87746 = CARTESIAN_POINT('',(80.5,242.520000000001,31.5013203435596)) ;
#87747 = CARTESIAN_POINT('Origin',(80.62,242.520000000001,31.5013203435596)) ;
#87748 = CARTESIAN_POINT('',(80.38,242.520000000001,31.6213203435596)) ;
#87749 = CARTESIAN_POINT('Origin',(80.38,242.520000000001,31.5013203435596)) ;
#87750 = CARTESIAN_POINT('Origin',(80.62,242.520000000001,31.6213203435596)) ;
#87751 = CARTESIAN_POINT('Ctrl Pts',(80.75,242.650000000001,30.9213203435596)) ;
#87752 = CARTESIAN_POINT('Ctrl Pts',(80.682240326584,242.516851226453,30.9213203435596)) ;
#87753 = CARTESIAN_POINT('Ctrl Pts',(80.6217189017438,242.397734495321,31.0443420435221)) ;
#87754 = CARTESIAN_POINT('Ctrl Pts',(80.6229061128752,242.400071113742,31.1751079336573)) ;
#87755 = CARTESIAN_POINT('Ctrl Pts',(80.75,242.650000000001,30.9213203435596)) ;
#87756 = CARTESIAN_POINT('Ctrl Pts',(80.6698315534017,242.529259999635,30.9213203435596)) ;
#87757 = CARTESIAN_POINT('Ctrl Pts',(80.5843586484258,242.396519836488,31.0238212967164)) ;
#87758 = CARTESIAN_POINT('Ctrl Pts',(80.5860338397051,242.399121065068,31.1757084683422)) ;
#87759 = CARTESIAN_POINT('Ctrl Pts',(80.75,242.650000000001,30.9213203435596)) ;
#87760 = CARTESIAN_POINT('Ctrl Pts',(80.6480364516902,242.551055101347,30.9213203435596)) ;
#87761 = CARTESIAN_POINT('Ctrl Pts',(80.5188495596748,242.427258078776,31.0059874513904)) ;
#87762 = CARTESIAN_POINT('Ctrl Pts',(80.5213796777706,242.42968275414,31.176230371506)) ;
#87763 = CARTESIAN_POINT('Ctrl Pts',(80.75,242.650000000001,30.9213203435596)) ;
#87764 = CARTESIAN_POINT('Ctrl Pts',(80.6262413499785,242.572850203058,30.9213203435596)) ;
#87765 = CARTESIAN_POINT('Ctrl Pts',(80.4968391697564,242.493466607971,31.0290306790226)) ;
#87766 = CARTESIAN_POINT('Ctrl Pts',(80.4993755620784,242.495022710548,31.1755560170308)) ;
#87767 = CARTESIAN_POINT('Ctrl Pts',(80.75,242.650000000001,30.9213203435596)) ;
#87768 = CARTESIAN_POINT('Ctrl Pts',(80.616855021449,242.582236531587,30.9213203435596)) ;
#87769 = CARTESIAN_POINT('Ctrl Pts',(80.497733001995,242.521706436267,31.0443131728438)) ;
#87770 = CARTESIAN_POINT('Ctrl Pts',(80.5000697232289,242.522893816919,31.1751087785507)) ;
#87771 = CARTESIAN_POINT('',(80.5,242.520000000001,31.1713203435596)) ;
#87772 = CARTESIAN_POINT('',(80.62,242.400000000001,31.1713203435596)) ;
#87773 = CARTESIAN_POINT('Origin',(80.62,242.520000000001,31.1713203435596)) ;
#87774 = CARTESIAN_POINT('',(80.75,242.650000000001,30.9213203435596)) ;
#87775 = CARTESIAN_POINT('Origin',(80.75,242.650000000001,31.1713203435596)) ;
#87776 = CARTESIAN_POINT('Origin',(80.75,242.650000000001,31.1713203435596)) ;
#87777 = CARTESIAN_POINT('Origin',(80.62,242.520000000001,30.7213203435596)) ;
#87778 = CARTESIAN_POINT('',(80.5,242.520000000001,30.7213203435596)) ;
#87779 = CARTESIAN_POINT('',(80.62,242.400000000001,30.7213203435596)) ;
#87780 = CARTESIAN_POINT('Origin',(80.98,245.080000000001,31.5013203435596)) ;
#87781 = CARTESIAN_POINT('',(80.98,245.200000000001,31.5013203435596)) ;
#87782 = CARTESIAN_POINT('',(80.98,245.320000000001,31.6213203435596)) ;
#87783 = CARTESIAN_POINT('Origin',(80.98,245.320000000001,31.5013203435596)) ;
#87784 = CARTESIAN_POINT('',(81.1,245.080000000001,31.5013203435596)) ;
#87785 = CARTESIAN_POINT('Origin',(80.98,245.080000000001,31.5013203435596)) ;
#87786 = CARTESIAN_POINT('',(81.22,245.080000000001,31.6213203435596)) ;
#87787 = CARTESIAN_POINT('Origin',(81.22,245.080000000001,31.5013203435596)) ;
#87788 = CARTESIAN_POINT('Origin',(80.98,245.080000000001,31.6213203435596)) ;
#87789 = CARTESIAN_POINT('Ctrl Pts',(80.85,244.950000000001,30.9213203435596)) ;
#87790 = CARTESIAN_POINT('Ctrl Pts',(80.9177596734216,245.083148773511,30.9213203435596)) ;
#87791 = CARTESIAN_POINT('Ctrl Pts',(80.9782810982421,245.202265504606,31.0443420434537)) ;
#87792 = CARTESIAN_POINT('Ctrl Pts',(80.9770938871316,245.199928886227,31.175107933593)) ;
#87793 = CARTESIAN_POINT('Ctrl Pts',(80.85,244.950000000001,30.9213203435596)) ;
#87794 = CARTESIAN_POINT('Ctrl Pts',(80.9301684465961,245.070740000336,30.9213203435596)) ;
#87795 = CARTESIAN_POINT('Ctrl Pts',(81.0156413526763,245.203480164368,31.0238212966733)) ;
#87796 = CARTESIAN_POINT('Ctrl Pts',(81.0139661614043,245.200878935816,31.1757084682668)) ;
#87797 = CARTESIAN_POINT('Ctrl Pts',(80.85,244.950000000001,30.9213203435596)) ;
#87798 = CARTESIAN_POINT('Ctrl Pts',(80.9519635482881,245.048944898644,30.9213203435596)) ;
#87799 = CARTESIAN_POINT('Ctrl Pts',(81.0811504039054,245.172741890886,31.0059874513767)) ;
#87800 = CARTESIAN_POINT('Ctrl Pts',(81.0786202865633,245.170317216156,31.1762303714209)) ;
#87801 = CARTESIAN_POINT('Ctrl Pts',(80.85,244.950000000001,30.9213203435596)) ;
#87802 = CARTESIAN_POINT('Ctrl Pts',(80.9737586499801,245.027149796952,30.9213203435596)) ;
#87803 = CARTESIAN_POINT('Ctrl Pts',(81.1031608312723,245.106533392978,31.0290306789648)) ;
#87804 = CARTESIAN_POINT('Ctrl Pts',(81.1006244389731,245.10497729041,31.1755560169585)) ;
#87805 = CARTESIAN_POINT('Ctrl Pts',(80.8499999999999,244.950000000001,30.9213203435596)) ;
#87806 = CARTESIAN_POINT('Ctrl Pts',(80.9831449784976,245.017763468435,30.9213203435596)) ;
#87807 = CARTESIAN_POINT('Ctrl Pts',(81.1022669979097,245.07829356376,31.0443131727521)) ;
#87808 = CARTESIAN_POINT('Ctrl Pts',(81.0999302767169,245.077106183128,31.1751087784871)) ;
#87809 = CARTESIAN_POINT('',(81.1,245.080000000001,31.1713203435596)) ;
#87810 = CARTESIAN_POINT('',(80.98,245.200000000001,31.1713203435596)) ;
#87811 = CARTESIAN_POINT('Origin',(80.98,245.080000000001,31.1713203435596)) ;
#87812 = CARTESIAN_POINT('',(80.85,244.950000000001,30.9213203435596)) ;
#87813 = CARTESIAN_POINT('Origin',(80.85,244.950000000001,31.1713203435596)) ;
#87814 = CARTESIAN_POINT('Origin',(80.85,244.950000000001,31.1713203435596)) ;
#87815 = CARTESIAN_POINT('Origin',(80.98,245.080000000001,30.7213203435596)) ;
#87816 = CARTESIAN_POINT('',(81.1,245.080000000001,30.7213203435596)) ;
#87817 = CARTESIAN_POINT('',(80.98,245.200000000001,30.7213203435596)) ;
#87818 = CARTESIAN_POINT('Origin',(81.22,244.500000000001,31.5013203435596)) ;
#87819 = CARTESIAN_POINT('',(81.22,244.500000000001,31.6213203435596)) ;
#87820 = CARTESIAN_POINT('',(81.1,244.500000000001,31.5013203435596)) ;
#87821 = CARTESIAN_POINT('Origin',(80.38,243.380000000001,31.5013203435596)) ;
#87822 = CARTESIAN_POINT('',(80.5,243.380000000001,31.5013203435596)) ;
#87823 = CARTESIAN_POINT('',(80.38,243.380000000001,31.6213203435596)) ;
#87824 = CARTESIAN_POINT('Origin',(80.38,243.380000000001,31.5013203435596)) ;
#87825 = CARTESIAN_POINT('',(80.38,243.500000000001,31.5013203435596)) ;
#87826 = CARTESIAN_POINT('Origin',(80.38,243.380000000001,31.5013203435596)) ;
#87827 = CARTESIAN_POINT('Origin',(80.38,243.380000000001,31.5013203435596)) ;
#87828 = CARTESIAN_POINT('Ctrl Pts',(80.75,243.750000000001,30.9213203435596)) ;
#87829 = CARTESIAN_POINT('Ctrl Pts',(80.6669413510771,243.693930974265,30.9213203435596)) ;
#87830 = CARTESIAN_POINT('Ctrl Pts',(80.4727353923176,243.56283133526,30.9670228566277)) ;
#87831 = CARTESIAN_POINT('Ctrl Pts',(80.3796479274324,243.499907749076,31.0966443715092)) ;
#87832 = CARTESIAN_POINT('Ctrl Pts',(80.379784355394,243.499999969096,31.1716079118165)) ;
#87833 = CARTESIAN_POINT('Ctrl Pts',(80.75,243.750000000001,30.9213203435596)) ;
#87834 = CARTESIAN_POINT('Ctrl Pts',(80.6720807629661,243.688791562376,30.9213203435596)) ;
#87835 = CARTESIAN_POINT('Ctrl Pts',(80.4891704228372,243.545228578582,30.9800564007202)) ;
#87836 = CARTESIAN_POINT('Ctrl Pts',(80.4156539785755,243.500002863489,31.1075891866046)) ;
#87837 = CARTESIAN_POINT('Ctrl Pts',(80.4157617392922,243.500069172168,31.1715658122273)) ;
#87838 = CARTESIAN_POINT('Ctrl Pts',(80.75,243.750000000001,30.9213203435596)) ;
#87839 = CARTESIAN_POINT('Ctrl Pts',(80.6810773386231,243.679794986719,30.9213203435596)) ;
#87840 = CARTESIAN_POINT('Ctrl Pts',(80.5184634385883,243.514118836202,30.9900090125417)) ;
#87841 = CARTESIAN_POINT('Ctrl Pts',(80.4780228393493,243.469813545103,31.1170023409801)) ;
#87842 = CARTESIAN_POINT('Ctrl Pts',(80.4780821505742,243.469878517698,31.1715296077568)) ;
#87843 = CARTESIAN_POINT('Ctrl Pts',(80.75,243.750000000001,30.9213203435596)) ;
#87844 = CARTESIAN_POINT('Ctrl Pts',(80.69007391428,243.670798411063,30.9213203435596)) ;
#87845 = CARTESIAN_POINT('Ctrl Pts',(80.5497385570857,243.485176584085,30.9767972216749)) ;
#87846 = CARTESIAN_POINT('Ctrl Pts',(80.4999776229693,243.406668436871,31.1047490159384)) ;
#87847 = CARTESIAN_POINT('Ctrl Pts',(80.5000505716157,243.406783509245,31.1715767366906)) ;
#87848 = CARTESIAN_POINT('Ctrl Pts',(80.75,243.750000000001,30.9213203435596)) ;
#87849 = CARTESIAN_POINT('Ctrl Pts',(80.6939310780478,243.666941247294,30.9213203435596)) ;
#87850 = CARTESIAN_POINT('Ctrl Pts',(80.5628307422909,243.47273419999,30.9670226511274)) ;
#87851 = CARTESIAN_POINT('Ctrl Pts',(80.499907754619,243.379647207222,31.0966450287582)) ;
#87852 = CARTESIAN_POINT('Ctrl Pts',(80.4999999737621,243.379783634492,31.1716079092912)) ;
#87853 = CARTESIAN_POINT('',(80.38,243.500000000001,31.1713203435596)) ;
#87854 = CARTESIAN_POINT('',(80.5,243.380000000001,31.1713203435596)) ;
#87855 = CARTESIAN_POINT('Origin',(80.38,243.380000000001,31.1713203435596)) ;
#87856 = CARTESIAN_POINT('',(80.5940820789473,243.519241476843,30.9758987431808)) ;
#87857 = CARTESIAN_POINT('Origin',(80.75,243.750000000001,31.1713203435596)) ;
#87858 = CARTESIAN_POINT('',(80.75,243.750000000001,30.9213203435596)) ;
#87859 = CARTESIAN_POINT('Origin',(80.75,243.750000000001,31.1713203435596)) ;
#87860 = CARTESIAN_POINT('',(80.5192414768421,243.594082078948,30.9758987431808)) ;
#87861 = CARTESIAN_POINT('Origin',(80.75,243.750000000001,31.1713203435596)) ;
#87862 = CARTESIAN_POINT('Origin',(80.75,243.750000000001,31.1713203435596)) ;
#87863 = CARTESIAN_POINT('Origin',(80.38,243.380000000001,30.7213203435596)) ;
#87864 = CARTESIAN_POINT('',(80.38,243.500000000001,30.7213203435596)) ;
#87865 = CARTESIAN_POINT('',(80.5,243.380000000001,30.7213203435596)) ;
#87866 = CARTESIAN_POINT('Origin',(80.62,245.080000000001,31.5013203435596)) ;
#87867 = CARTESIAN_POINT('',(80.5,245.080000000001,31.5013203435596)) ;
#87868 = CARTESIAN_POINT('',(80.38,245.080000000001,31.6213203435596)) ;
#87869 = CARTESIAN_POINT('Origin',(80.38,245.080000000001,31.5013203435596)) ;
#87870 = CARTESIAN_POINT('',(80.62,245.200000000001,31.5013203435596)) ;
#87871 = CARTESIAN_POINT('Origin',(80.62,245.080000000001,31.5013203435596)) ;
#87872 = CARTESIAN_POINT('',(80.62,245.320000000001,31.6213203435596)) ;
#87873 = CARTESIAN_POINT('Origin',(80.62,245.320000000001,31.5013203435596)) ;
#87874 = CARTESIAN_POINT('Origin',(80.62,245.080000000001,31.6213203435596)) ;
#87875 = CARTESIAN_POINT('Ctrl Pts',(80.75,244.950000000001,30.9213203435596)) ;
#87876 = CARTESIAN_POINT('Ctrl Pts',(80.6168512264854,245.017759673422,30.9213203435596)) ;
#87877 = CARTESIAN_POINT('Ctrl Pts',(80.497734495385,245.078281098245,31.0443420434625)) ;
#87878 = CARTESIAN_POINT('Ctrl Pts',(80.50007111377,245.077093887132,31.1751079336014)) ;
#87879 = CARTESIAN_POINT('Ctrl Pts',(80.75,244.950000000001,30.9213203435596)) ;
#87880 = CARTESIAN_POINT('Ctrl Pts',(80.6292599996609,245.030168446598,30.9213203435596)) ;
#87881 = CARTESIAN_POINT('Ctrl Pts',(80.4965198357456,245.115641352532,31.023821296679)) ;
#87882 = CARTESIAN_POINT('Ctrl Pts',(80.4991210643014,245.113966161259,31.1757084682767)) ;
#87883 = CARTESIAN_POINT('Ctrl Pts',(80.75,244.950000000001,30.9213203435596)) ;
#87884 = CARTESIAN_POINT('Ctrl Pts',(80.6510551013544,245.051963548291,30.9213203435596)) ;
#87885 = CARTESIAN_POINT('Ctrl Pts',(80.5272581051066,245.181150408713,31.0059874513795)) ;
#87886 = CARTESIAN_POINT('Ctrl Pts',(80.52968277992,245.178620291272,31.176230371432)) ;
#87887 = CARTESIAN_POINT('Ctrl Pts',(80.75,244.950000000001,30.9213203435596)) ;
#87888 = CARTESIAN_POINT('Ctrl Pts',(80.6728502030479,245.073758649985,30.9213203435596)) ;
#87889 = CARTESIAN_POINT('Ctrl Pts',(80.593466607141,245.203160831135,31.0290306789699)) ;
#87890 = CARTESIAN_POINT('Ctrl Pts',(80.5950227097103,245.200624438833,31.175556016968)) ;
#87891 = CARTESIAN_POINT('Ctrl Pts',(80.75,244.950000000001,30.9213203435596)) ;
#87892 = CARTESIAN_POINT('Ctrl Pts',(80.6822365315657,245.083144978503,30.9213203435596)) ;
#87893 = CARTESIAN_POINT('Ctrl Pts',(80.6217064362341,245.202266997924,31.0443131727584)) ;
#87894 = CARTESIAN_POINT('Ctrl Pts',(80.6228938168687,245.199930276725,31.1751087784956)) ;
#87895 = CARTESIAN_POINT('',(80.62,245.200000000001,31.1713203435596)) ;
#87896 = CARTESIAN_POINT('',(80.5,245.080000000001,31.1713203435596)) ;
#87897 = CARTESIAN_POINT('Origin',(80.62,245.080000000001,31.1713203435596)) ;
#87898 = CARTESIAN_POINT('',(80.75,244.950000000001,30.9213203435596)) ;
#87899 = CARTESIAN_POINT('Origin',(80.75,244.950000000001,31.1713203435596)) ;
#87900 = CARTESIAN_POINT('Origin',(80.75,244.950000000001,31.1713203435596)) ;
#87901 = CARTESIAN_POINT('Origin',(80.62,245.080000000001,30.7213203435596)) ;
#87902 = CARTESIAN_POINT('',(80.62,245.200000000001,30.7213203435596)) ;
#87903 = CARTESIAN_POINT('',(80.5,245.080000000001,30.7213203435596)) ;
#87904 = CARTESIAN_POINT('Origin',(80.65,245.320000000001,31.5013203435596)) ;
#87905 = CARTESIAN_POINT('',(80.65,245.320000000001,31.6213203435596)) ;
#87906 = CARTESIAN_POINT('',(80.65,245.200000000001,31.5013203435596)) ;
#87907 = CARTESIAN_POINT('Origin',(79.52,243.620000000001,31.5013203435596)) ;
#87908 = CARTESIAN_POINT('',(79.52,243.500000000001,31.5013203435596)) ;
#87909 = CARTESIAN_POINT('',(79.52,243.380000000001,31.6213203435596)) ;
#87910 = CARTESIAN_POINT('Origin',(79.52,243.380000000001,31.5013203435596)) ;
#87911 = CARTESIAN_POINT('',(79.4,243.620000000001,31.5013203435596)) ;
#87912 = CARTESIAN_POINT('Origin',(79.52,243.620000000001,31.5013203435596)) ;
#87913 = CARTESIAN_POINT('',(79.28,243.620000000001,31.6213203435596)) ;
#87914 = CARTESIAN_POINT('Origin',(79.28,243.620000000001,31.5013203435596)) ;
#87915 = CARTESIAN_POINT('Origin',(79.52,243.620000000001,31.6213203435596)) ;
#87916 = CARTESIAN_POINT('Ctrl Pts',(79.65,243.750000000001,30.9213203435596)) ;
#87917 = CARTESIAN_POINT('Ctrl Pts',(79.582240326584,243.616851226453,30.9213203435596)) ;
#87918 = CARTESIAN_POINT('Ctrl Pts',(79.5217189017439,243.497734495321,31.0443420435221)) ;
#87919 = CARTESIAN_POINT('Ctrl Pts',(79.5229061128752,243.500071113742,31.1751079336573)) ;
#87920 = CARTESIAN_POINT('Ctrl Pts',(79.65,243.750000000001,30.9213203435596)) ;
#87921 = CARTESIAN_POINT('Ctrl Pts',(79.5698315534018,243.629259999635,30.9213203435596)) ;
#87922 = CARTESIAN_POINT('Ctrl Pts',(79.4843586484258,243.496519836488,31.0238212967164)) ;
#87923 = CARTESIAN_POINT('Ctrl Pts',(79.4860338397051,243.499121065068,31.1757084683421)) ;
#87924 = CARTESIAN_POINT('Ctrl Pts',(79.65,243.750000000001,30.9213203435596)) ;
#87925 = CARTESIAN_POINT('Ctrl Pts',(79.5480364516901,243.651055101347,30.9213203435596)) ;
#87926 = CARTESIAN_POINT('Ctrl Pts',(79.4188495596745,243.527258078776,31.0059874513903)) ;
#87927 = CARTESIAN_POINT('Ctrl Pts',(79.4213796777703,243.52968275414,31.176230371506)) ;
#87928 = CARTESIAN_POINT('Ctrl Pts',(79.65,243.750000000001,30.9213203435596)) ;
#87929 = CARTESIAN_POINT('Ctrl Pts',(79.5262413499783,243.672850203058,30.9213203435596)) ;
#87930 = CARTESIAN_POINT('Ctrl Pts',(79.3968391697563,243.593466607972,31.0290306790228)) ;
#87931 = CARTESIAN_POINT('Ctrl Pts',(79.3993755620783,243.595022710549,31.1755560170307)) ;
#87932 = CARTESIAN_POINT('Ctrl Pts',(79.65,243.750000000001,30.9213203435596)) ;
#87933 = CARTESIAN_POINT('Ctrl Pts',(79.5168550214487,243.682236531589,30.9213203435596)) ;
#87934 = CARTESIAN_POINT('Ctrl Pts',(79.3977330019951,243.621706436268,31.0443131728442)) ;
#87935 = CARTESIAN_POINT('Ctrl Pts',(79.4000697232289,243.62289381692,31.1751087785507)) ;
#87936 = CARTESIAN_POINT('',(79.4,243.620000000001,31.1713203435596)) ;
#87937 = CARTESIAN_POINT('',(79.52,243.500000000001,31.1713203435596)) ;
#87938 = CARTESIAN_POINT('Origin',(79.52,243.620000000001,31.1713203435596)) ;
#87939 = CARTESIAN_POINT('',(79.65,243.750000000001,30.9213203435596)) ;
#87940 = CARTESIAN_POINT('Origin',(79.65,243.750000000001,31.1713203435596)) ;
#87941 = CARTESIAN_POINT('Origin',(79.65,243.750000000001,31.1713203435596)) ;
#87942 = CARTESIAN_POINT('Origin',(79.52,243.620000000001,30.7213203435596)) ;
#87943 = CARTESIAN_POINT('',(79.4,243.620000000001,30.7213203435596)) ;
#87944 = CARTESIAN_POINT('',(79.52,243.500000000001,30.7213203435596)) ;
#87945 = CARTESIAN_POINT('Origin',(80.38,244.220000000001,31.5013203435596)) ;
#87946 = CARTESIAN_POINT('',(80.38,244.100000000001,31.5013203435596)) ;
#87947 = CARTESIAN_POINT('',(80.38,244.220000000001,31.6213203435596)) ;
#87948 = CARTESIAN_POINT('Origin',(80.38,244.220000000001,31.5013203435596)) ;
#87949 = CARTESIAN_POINT('',(80.5,244.220000000001,31.5013203435596)) ;
#87950 = CARTESIAN_POINT('Origin',(80.38,244.220000000001,31.5013203435596)) ;
#87951 = CARTESIAN_POINT('Origin',(80.38,244.220000000001,31.5013203435596)) ;
#87952 = CARTESIAN_POINT('Ctrl Pts',(80.7500000000001,243.850000000001,30.9213203435596)) ;
#87953 = CARTESIAN_POINT('Ctrl Pts',(80.6939309713718,243.933058646032,30.9213203435596)) ;
#87954 = CARTESIAN_POINT('Ctrl Pts',(80.5628313551136,244.127264554417,30.9670228859096)) ;
#87955 = CARTESIAN_POINT('Ctrl Pts',(80.4999077576942,244.220352039636,31.0966443599245)) ;
#87956 = CARTESIAN_POINT('Ctrl Pts',(80.4999999691007,244.22021562441,31.1716078849265)) ;
#87957 = CARTESIAN_POINT('Ctrl Pts',(80.75,243.850000000001,30.9213203435596)) ;
#87958 = CARTESIAN_POINT('Ctrl Pts',(80.6887915604468,243.927919235107,30.9213203435596)) ;
#87959 = CARTESIAN_POINT('Ctrl Pts',(80.5452285957518,244.110829530948,30.9800563984677)) ;
#87960 = CARTESIAN_POINT('Ctrl Pts',(80.5000028631856,244.184345998044,31.1075891712008)) ;
#87961 = CARTESIAN_POINT('Ctrl Pts',(80.5000691656834,244.184238247379,31.1715657892908)) ;
#87962 = CARTESIAN_POINT('Ctrl Pts',(80.75,243.850000000001,30.9213203435596)) ;
#87963 = CARTESIAN_POINT('Ctrl Pts',(80.6797949867176,243.918922661378,30.9213203435596)) ;
#87964 = CARTESIAN_POINT('Ctrl Pts',(80.5141188971542,244.081536502913,30.9900089508675)) ;
#87965 = CARTESIAN_POINT('Ctrl Pts',(80.4698135431297,244.121977164828,31.1170023213905)) ;
#87966 = CARTESIAN_POINT('Ctrl Pts',(80.4698785097335,244.121917859065,31.1715295882234)) ;
#87967 = CARTESIAN_POINT('Ctrl Pts',(80.75,243.850000000001,30.9213203435596)) ;
#87968 = CARTESIAN_POINT('Ctrl Pts',(80.6707984129886,243.909926087649,30.9213203435596)) ;
#87969 = CARTESIAN_POINT('Ctrl Pts',(80.4851766412845,244.050261413227,30.9767972196575)) ;
#87970 = CARTESIAN_POINT('Ctrl Pts',(80.4066684610771,244.100022374965,31.1047490010863)) ;
#87971 = CARTESIAN_POINT('Ctrl Pts',(80.4067835227305,244.099949433106,31.17157671273)) ;
#87972 = CARTESIAN_POINT('Ctrl Pts',(80.75,243.850000000001,30.9213203435596)) ;
#87973 = CARTESIAN_POINT('Ctrl Pts',(80.6669412501844,243.906068924844,30.9213203435596)) ;
#87974 = CARTESIAN_POINT('Ctrl Pts',(80.4727342532524,244.037169237852,30.9670226804588)) ;
#87975 = CARTESIAN_POINT('Ctrl Pts',(80.3796472401461,244.100092236764,31.0966450170888)) ;
#87976 = CARTESIAN_POINT('Ctrl Pts',(80.3797836546807,244.100000026234,31.1716078824018)) ;
#87977 = CARTESIAN_POINT('',(80.5,244.220000000001,31.1713203435596)) ;
#87978 = CARTESIAN_POINT('',(80.38,244.100000000001,31.1713203435596)) ;
#87979 = CARTESIAN_POINT('Origin',(80.38,244.220000000001,31.1713203435596)) ;
#87980 = CARTESIAN_POINT('',(80.5192414855947,244.00591791514,30.9758987384623)) ;
#87981 = CARTESIAN_POINT('Origin',(80.75,243.850000000001,31.1713203435596)) ;
#87982 = CARTESIAN_POINT('',(80.75,243.850000000001,30.9213203435596)) ;
#87983 = CARTESIAN_POINT('Origin',(80.75,243.850000000001,31.1713203435596)) ;
#87984 = CARTESIAN_POINT('',(80.5940820848613,244.080758514406,30.9758987384623)) ;
#87985 = CARTESIAN_POINT('Origin',(80.75,243.850000000001,31.1713203435596)) ;
#87986 = CARTESIAN_POINT('Origin',(80.75,243.850000000001,31.1713203435596)) ;
#87987 = CARTESIAN_POINT('Origin',(80.38,244.220000000001,30.7213203435596)) ;
#87988 = CARTESIAN_POINT('',(80.5,244.220000000001,30.7213203435596)) ;
#87989 = CARTESIAN_POINT('',(80.38,244.100000000001,30.7213203435596)) ;
#87990 = CARTESIAN_POINT('Origin',(80.38,243.950000000001,31.5013203435596)) ;
#87991 = CARTESIAN_POINT('',(80.38,243.950000000001,31.6213203435596)) ;
#87992 = CARTESIAN_POINT('',(80.5,243.950000000001,31.5013203435596)) ;
#87993 = CARTESIAN_POINT('Origin',(79.52,243.980000000001,31.5013203435596)) ;
#87994 = CARTESIAN_POINT('',(79.4,243.980000000001,31.5013203435596)) ;
#87995 = CARTESIAN_POINT('',(79.28,243.980000000001,31.6213203435596)) ;
#87996 = CARTESIAN_POINT('Origin',(79.28,243.980000000001,31.5013203435596)) ;
#87997 = CARTESIAN_POINT('',(79.52,244.100000000001,31.5013203435596)) ;
#87998 = CARTESIAN_POINT('Origin',(79.52,243.980000000001,31.5013203435596)) ;
#87999 = CARTESIAN_POINT('',(79.52,244.220000000001,31.6213203435596)) ;
#88000 = CARTESIAN_POINT('Origin',(79.52,244.220000000001,31.5013203435596)) ;
#88001 = CARTESIAN_POINT('Origin',(79.52,243.980000000001,31.6213203435596)) ;
#88002 = CARTESIAN_POINT('Ctrl Pts',(79.65,243.850000000001,30.9213203435596)) ;
#88003 = CARTESIAN_POINT('Ctrl Pts',(79.5168512264577,243.917759673418,30.9213203435596)) ;
#88004 = CARTESIAN_POINT('Ctrl Pts',(79.3977344953316,243.978281098255,31.0443420435113)) ;
#88005 = CARTESIAN_POINT('Ctrl Pts',(79.4000711137459,243.977093887127,31.1751079336473)) ;
#88006 = CARTESIAN_POINT('Ctrl Pts',(79.65,243.850000000001,30.9213203435596)) ;
#88007 = CARTESIAN_POINT('Ctrl Pts',(79.5292599996388,243.930168446599,30.9213203435596)) ;
#88008 = CARTESIAN_POINT('Ctrl Pts',(79.396519836356,244.015641351745,31.0238212967097)) ;
#88009 = CARTESIAN_POINT('Ctrl Pts',(79.3991210649315,244.013966160467,31.1757084683304)) ;
#88010 = CARTESIAN_POINT('Ctrl Pts',(79.65,243.850000000001,30.9213203435596)) ;
#88011 = CARTESIAN_POINT('Ctrl Pts',(79.5510551013474,243.951963548308,30.9213203435596)) ;
#88012 = CARTESIAN_POINT('Ctrl Pts',(79.427258083439,244.081150434729,31.0059874513882)) ;
#88013 = CARTESIAN_POINT('Ctrl Pts',(79.4296827587047,244.078620316749,31.1762303714927)) ;
#88014 = CARTESIAN_POINT('Ctrl Pts',(79.65,243.850000000001,30.9213203435596)) ;
#88015 = CARTESIAN_POINT('Ctrl Pts',(79.5728502030561,243.973758650017,30.9213203435596)) ;
#88016 = CARTESIAN_POINT('Ctrl Pts',(79.4934666078253,244.103160830403,31.0290306790137)) ;
#88017 = CARTESIAN_POINT('Ctrl Pts',(79.4950227104005,244.100624438084,31.1755560170194)) ;
#88018 = CARTESIAN_POINT('Ctrl Pts',(79.65,243.850000000001,30.9213203435596)) ;
#88019 = CARTESIAN_POINT('Ctrl Pts',(79.5822365315838,243.983144978544,30.9213203435596)) ;
#88020 = CARTESIAN_POINT('Ctrl Pts',(79.5217064362629,244.102266997991,31.0443131728297)) ;
#88021 = CARTESIAN_POINT('Ctrl Pts',(79.5228938169118,244.099930276764,31.1751087785408)) ;
#88022 = CARTESIAN_POINT('',(79.52,244.100000000001,31.1713203435596)) ;
#88023 = CARTESIAN_POINT('',(79.4,243.980000000001,31.1713203435596)) ;
#88024 = CARTESIAN_POINT('Origin',(79.52,243.980000000001,31.1713203435596)) ;
#88025 = CARTESIAN_POINT('',(79.65,243.850000000001,30.9213203435596)) ;
#88026 = CARTESIAN_POINT('Origin',(79.65,243.850000000001,31.1713203435596)) ;
#88027 = CARTESIAN_POINT('Origin',(79.65,243.850000000001,31.1713203435596)) ;
#88028 = CARTESIAN_POINT('Origin',(79.52,243.980000000001,30.7213203435596)) ;
#88029 = CARTESIAN_POINT('',(79.52,244.100000000001,30.7213203435596)) ;
#88030 = CARTESIAN_POINT('',(79.4,243.980000000001,30.7213203435596)) ;
#88031 = CARTESIAN_POINT('Origin',(80.1,244.220000000001,31.5013203435596)) ;
#88032 = CARTESIAN_POINT('',(80.1,244.220000000001,31.6213203435596)) ;
#88033 = CARTESIAN_POINT('',(80.1,244.100000000001,31.5013203435596)) ;
#88034 = CARTESIAN_POINT('Origin',(79.28,243.650000000001,31.5013203435596)) ;
#88035 = CARTESIAN_POINT('',(79.28,243.650000000001,31.6213203435596)) ;
#88036 = CARTESIAN_POINT('',(79.4,243.650000000001,31.5013203435596)) ;
#88037 = CARTESIAN_POINT('Origin',(80.65,243.380000000001,31.5013203435596)) ;
#88038 = CARTESIAN_POINT('',(80.65,243.380000000001,31.6213203435596)) ;
#88039 = CARTESIAN_POINT('',(80.65,243.500000000001,31.5013203435596)) ;
#88040 = CARTESIAN_POINT('Origin',(80.38,243.100000000001,31.5013203435596)) ;
#88041 = CARTESIAN_POINT('',(80.38,243.100000000001,31.6213203435596)) ;
#88042 = CARTESIAN_POINT('',(80.5,243.100000000001,31.5013203435596)) ;
#88043 = CARTESIAN_POINT('Origin',(80.95,242.280000000001,31.5013203435596)) ;
#88044 = CARTESIAN_POINT('',(80.95,242.280000000001,31.6213203435596)) ;
#88045 = CARTESIAN_POINT('',(80.95,242.400000000001,31.5013203435596)) ;
#88046 = CARTESIAN_POINT('Origin',(81.22,243.650000000001,31.5013203435596)) ;
#88047 = CARTESIAN_POINT('',(81.22,243.650000000001,31.6213203435596)) ;
#88048 = CARTESIAN_POINT('',(81.1,243.650000000001,31.5013203435596)) ;
#88049 = CARTESIAN_POINT('Origin',(81.5,243.380000000001,31.5013203435596)) ;
#88050 = CARTESIAN_POINT('',(81.5,243.380000000001,31.6213203435596)) ;
#88051 = CARTESIAN_POINT('',(81.5,243.500000000001,31.5013203435596)) ;
#88052 = CARTESIAN_POINT('Origin',(82.2,244.100000000001,30.7213203435596)) ;
#88053 = CARTESIAN_POINT('',(82.2,243.950000000001,31.1713203435596)) ;
#88054 = CARTESIAN_POINT('Origin',(81.1,244.100000000001,30.7213203435596)) ;
#88055 = CARTESIAN_POINT('',(80.95,244.100000000001,31.1713203435596)) ;
#88056 = CARTESIAN_POINT('Origin',(80.95,243.850000000001,31.1713203435596)) ;
#88057 = CARTESIAN_POINT('',(80.95,243.850000000001,30.9213203435596)) ;
#88058 = CARTESIAN_POINT('Origin',(81.1,245.200000000001,30.7213203435596)) ;
#88059 = CARTESIAN_POINT('',(81.1,244.500000000001,31.1713203435596)) ;
#88060 = CARTESIAN_POINT('Origin',(80.85,244.500000000001,31.1713203435596)) ;
#88061 = CARTESIAN_POINT('',(80.85,244.500000000001,30.9213203435596)) ;
#88062 = CARTESIAN_POINT('Origin',(80.5,245.200000000001,30.7213203435596)) ;
#88063 = CARTESIAN_POINT('',(80.65,245.200000000001,31.1713203435596)) ;
#88064 = CARTESIAN_POINT('Origin',(80.65,244.950000000001,31.1713203435596)) ;
#88065 = CARTESIAN_POINT('',(80.65,244.950000000001,30.9213203435596)) ;
#88066 = CARTESIAN_POINT('Origin',(80.5,244.100000000001,30.7213203435596)) ;
#88067 = CARTESIAN_POINT('',(80.5,243.950000000001,31.1713203435596)) ;
#88068 = CARTESIAN_POINT('Origin',(80.75,243.950000000001,31.1713203435596)) ;
#88069 = CARTESIAN_POINT('',(80.75,243.950000000001,30.9213203435596)) ;
#88070 = CARTESIAN_POINT('Origin',(79.4,244.100000000001,30.7213203435596)) ;
#88071 = CARTESIAN_POINT('',(80.1,244.100000000001,31.1713203435596)) ;
#88072 = CARTESIAN_POINT('Origin',(80.1,243.850000000001,31.1713203435596)) ;
#88073 = CARTESIAN_POINT('',(80.1,243.850000000001,30.9213203435596)) ;
#88074 = CARTESIAN_POINT('Origin',(80.8,243.800000000001,31.6213203435596)) ;
#88075 = CARTESIAN_POINT('',(79.05,243.800000000001,31.6213203435596)) ;
#88076 = CARTESIAN_POINT('Origin',(80.8,243.800000000001,31.6213203435596)) ;
#88077 = CARTESIAN_POINT('Origin',(80.65,243.750000000001,31.1713203435596)) ;
#88078 = CARTESIAN_POINT('',(80.65,243.750000000001,30.9213203435596)) ;
#88079 = CARTESIAN_POINT('',(80.65,243.500000000001,31.1713203435596)) ;
#88080 = CARTESIAN_POINT('Origin',(79.65,243.650000000001,31.1713203435596)) ;
#88081 = CARTESIAN_POINT('',(79.65,243.650000000001,30.9213203435596)) ;
#88082 = CARTESIAN_POINT('',(79.4,243.650000000001,31.1713203435596)) ;
#88083 = CARTESIAN_POINT('Origin',(81.95,243.950000000001,31.1713203435596)) ;
#88084 = CARTESIAN_POINT('',(81.95,243.950000000001,30.9213203435596)) ;
#88085 = CARTESIAN_POINT('Origin',(81.5,243.750000000001,31.1713203435596)) ;
#88086 = CARTESIAN_POINT('',(81.5,243.750000000001,30.9213203435596)) ;
#88087 = CARTESIAN_POINT('',(81.5,243.500000000001,31.1713203435596)) ;
#88088 = CARTESIAN_POINT('Origin',(80.85,243.650000000001,31.1713203435596)) ;
#88089 = CARTESIAN_POINT('',(80.85,243.650000000001,30.9213203435596)) ;
#88090 = CARTESIAN_POINT('',(81.1,243.650000000001,31.1713203435596)) ;
#88091 = CARTESIAN_POINT('Origin',(80.95,242.650000000001,31.1713203435596)) ;
#88092 = CARTESIAN_POINT('',(80.95,242.650000000001,30.9213203435596)) ;
#88093 = CARTESIAN_POINT('',(80.95,242.400000000001,31.1713203435596)) ;
#88094 = CARTESIAN_POINT('Origin',(80.75,243.100000000001,31.1713203435596)) ;
#88095 = CARTESIAN_POINT('',(80.75,243.100000000001,30.9213203435596)) ;
#88096 = CARTESIAN_POINT('',(80.5,243.100000000001,31.1713203435596)) ;
#88097 = CARTESIAN_POINT('Origin',(82.2,243.500000000001,30.7213203435596)) ;
#88098 = CARTESIAN_POINT('Origin',(81.1,243.500000000001,30.7213203435596)) ;
#88099 = CARTESIAN_POINT('Origin',(81.1,242.400000000001,30.7213203435596)) ;
#88100 = CARTESIAN_POINT('Origin',(80.5,242.400000000001,30.7213203435596)) ;
#88101 = CARTESIAN_POINT('Origin',(80.5,243.500000000001,30.7213203435596)) ;
#88102 = CARTESIAN_POINT('Origin',(80.8,243.800000000001,30.9213203435596)) ;
#88103 = CARTESIAN_POINT('Origin',(80.8,243.800000000001,31.3713203435596)) ;
#88104 = CARTESIAN_POINT('',(78.8,243.800000000001,31.3713203435596)) ;
#88105 = CARTESIAN_POINT('Origin',(79.05,243.800000000001,31.3713203435596)) ;
#88106 = CARTESIAN_POINT('Origin',(80.8,243.800000000001,31.3713203435596)) ;
#88107 = CARTESIAN_POINT('Origin',(80.8,243.800000000001,30.7213203435596)) ;
#88108 = CARTESIAN_POINT('',(78.8,243.800000000001,30.9713203435596)) ;
#88109 = CARTESIAN_POINT('',(78.8,243.800000000001,30.7213203435596)) ;
#88110 = CARTESIAN_POINT('',(82.8,243.800000000001,30.9713203435596)) ;
#88111 = CARTESIAN_POINT('Origin',(80.8,243.800000000001,30.9713203435596)) ;
#88112 = CARTESIAN_POINT('Origin',(80.8,243.800000000001,30.9713203435596)) ;
#88113 = CARTESIAN_POINT('Origin',(80.8,243.800000000001,30.9713203435596)) ;
#88114 = CARTESIAN_POINT('',(82.55,243.800000000001,30.7213203435596)) ;
#88115 = CARTESIAN_POINT('Origin',(80.8,243.800000000001,30.7213203435596)) ;
#88116 = CARTESIAN_POINT('Origin',(82.55,243.800000000001,30.9713203435596)) ;
#88117 = CARTESIAN_POINT('Origin',(80.8,243.800000000001,30.7213203435596)) ;
#88118 = CARTESIAN_POINT('Origin',(79.4,243.500000000001,30.7213203435596)) ;
#88119 = CARTESIAN_POINT('',(0.,0.,0.)) ;
#88120 = CARTESIAN_POINT('Origin',(28.,248.1,26.6213203435596)) ;
#88121 = CARTESIAN_POINT('',(28.,248.2,26.6213203435596)) ;
#88122 = CARTESIAN_POINT('',(28.1,248.1,26.6213203435596)) ;
#88123 = CARTESIAN_POINT('Origin',(28.,248.1,26.6213203435596)) ;
#88124 = CARTESIAN_POINT('',(28.,248.1,26.7213203435596)) ;
#88125 = CARTESIAN_POINT('Origin',(28.,248.1,26.6213203435596)) ;
#88126 = CARTESIAN_POINT('Origin',(28.,248.1,26.6213203435596)) ;
#88127 = CARTESIAN_POINT('Origin',(28.,248.1,26.1213203435596)) ;
#88128 = CARTESIAN_POINT('',(28.,248.1,26.0213203435596)) ;
#88129 = CARTESIAN_POINT('',(28.1,248.1,26.1213203435596)) ;
#88130 = CARTESIAN_POINT('Origin',(28.,248.1,26.1213203435596)) ;
#88131 = CARTESIAN_POINT('',(28.,248.2,26.1213203435596)) ;
#88132 = CARTESIAN_POINT('Origin',(28.,248.1,26.1213203435596)) ;
#88133 = CARTESIAN_POINT('Origin',(28.,248.1,26.1213203435596)) ;
#88134 = CARTESIAN_POINT('Origin',(26.4,248.1,26.1213203435596)) ;
#88135 = CARTESIAN_POINT('',(26.3,248.1,26.1213203435596)) ;
#88136 = CARTESIAN_POINT('',(26.4,248.1,26.0213203435596)) ;
#88137 = CARTESIAN_POINT('Origin',(26.4,248.1,26.1213203435596)) ;
#88138 = CARTESIAN_POINT('',(26.4,248.2,26.1213203435596)) ;
#88139 = CARTESIAN_POINT('Origin',(26.4,248.1,26.1213203435596)) ;
#88140 = CARTESIAN_POINT('Origin',(26.4,248.1,26.1213203435596)) ;
#88141 = CARTESIAN_POINT('Origin',(26.4,248.1,26.1963203435596)) ;
#88142 = CARTESIAN_POINT('',(26.4,248.2,26.6213203435596)) ;
#88143 = CARTESIAN_POINT('',(26.4,248.2,26.1963203435596)) ;
#88144 = CARTESIAN_POINT('',(26.3,248.1,26.7213203435596)) ;
#88145 = CARTESIAN_POINT('',(26.3,248.1,26.1963203435596)) ;
#88146 = CARTESIAN_POINT('Origin',(26.4,248.1,26.6213203435596)) ;
#88147 = CARTESIAN_POINT('Origin',(26.3,248.1,26.1213203435596)) ;
#88148 = CARTESIAN_POINT('',(26.3,248.1,26.0213203435596)) ;
#88149 = CARTESIAN_POINT('',(26.3,248.2,26.1213203435596)) ;
#88150 = CARTESIAN_POINT('Origin',(28.,246.5,26.1213203435596)) ;
#88151 = CARTESIAN_POINT('',(28.,246.4,26.1213203435596)) ;
#88152 = CARTESIAN_POINT('',(28.1,246.5,26.1213203435596)) ;
#88153 = CARTESIAN_POINT('Origin',(28.,246.5,26.1213203435596)) ;
#88154 = CARTESIAN_POINT('',(28.,246.5,26.0213203435596)) ;
#88155 = CARTESIAN_POINT('Origin',(28.,246.5,26.1213203435596)) ;
#88156 = CARTESIAN_POINT('Origin',(28.,246.5,26.1213203435596)) ;
#88157 = CARTESIAN_POINT('Origin',(26.4,246.5,26.1213203435596)) ;
#88158 = CARTESIAN_POINT('',(26.3,246.5,26.1213203435596)) ;
#88159 = CARTESIAN_POINT('',(26.4,246.4,26.1213203435596)) ;
#88160 = CARTESIAN_POINT('Origin',(26.4,246.5,26.1213203435596)) ;
#88161 = CARTESIAN_POINT('',(26.4,246.5,26.0213203435596)) ;
#88162 = CARTESIAN_POINT('Origin',(26.4,246.5,26.1213203435596)) ;
#88163 = CARTESIAN_POINT('Origin',(26.4,246.5,26.1213203435596)) ;
#88164 = CARTESIAN_POINT('Origin',(26.4,246.85,26.1213203435596)) ;
#88165 = CARTESIAN_POINT('',(26.3,246.85,26.1213203435596)) ;
#88166 = CARTESIAN_POINT('',(26.4,246.85,26.0213203435596)) ;
#88167 = CARTESIAN_POINT('Origin',(26.3,246.5,26.1213203435596)) ;
#88168 = CARTESIAN_POINT('',(26.3,246.4,26.1213203435596)) ;
#88169 = CARTESIAN_POINT('',(26.3,246.5,26.0213203435596)) ;
#88170 = CARTESIAN_POINT('Origin',(26.4,246.5,26.5463203435596)) ;
#88171 = CARTESIAN_POINT('',(26.4,246.4,26.7213203435596)) ;
#88172 = CARTESIAN_POINT('',(26.3,246.5,26.7213203435596)) ;
#88173 = CARTESIAN_POINT('Origin',(26.4,246.5,26.7213203435596)) ;
#88174 = CARTESIAN_POINT('',(26.3,246.5,26.5463203435596)) ;
#88175 = CARTESIAN_POINT('',(26.4,246.4,26.5463203435596)) ;
#88176 = CARTESIAN_POINT('Origin',(28.,246.85,26.1213203435596)) ;
#88177 = CARTESIAN_POINT('',(28.1,246.85,26.1213203435596)) ;
#88178 = CARTESIAN_POINT('',(28.,246.85,26.0213203435596)) ;
#88179 = CARTESIAN_POINT('Origin',(28.,246.5,26.5463203435596)) ;
#88180 = CARTESIAN_POINT('',(28.,246.4,26.7213203435596)) ;
#88181 = CARTESIAN_POINT('',(28.,246.4,26.5463203435596)) ;
#88182 = CARTESIAN_POINT('',(28.1,246.5,26.6213203435596)) ;
#88183 = CARTESIAN_POINT('',(28.1,246.5,26.5463203435596)) ;
#88184 = CARTESIAN_POINT('Origin',(28.,246.5,26.6213203435596)) ;
#88185 = CARTESIAN_POINT('Origin',(28.,248.1,26.1963203435596)) ;
#88186 = CARTESIAN_POINT('',(28.1,248.1,26.1963203435596)) ;
#88187 = CARTESIAN_POINT('',(28.,248.2,26.1963203435596)) ;
#88188 = CARTESIAN_POINT('Origin',(28.,247.75,26.6213203435596)) ;
#88189 = CARTESIAN_POINT('',(28.1,247.75,26.6213203435596)) ;
#88190 = CARTESIAN_POINT('',(28.,247.75,26.7213203435596)) ;
#88191 = CARTESIAN_POINT('Origin',(26.3,248.1,26.6213203435596)) ;
#88192 = CARTESIAN_POINT('',(26.3,248.1,26.7213203435596)) ;
#88193 = CARTESIAN_POINT('',(26.3,248.2,26.6213203435596)) ;
#88194 = CARTESIAN_POINT('Origin',(26.3,247.3,26.3713203435596)) ;
#88195 = CARTESIAN_POINT('',(26.3,247.7,26.7213203435596)) ;
#88196 = CARTESIAN_POINT('Origin',(26.3,246.4,26.7213203435596)) ;
#88197 = CARTESIAN_POINT('',(26.3,246.4,26.7213203435596)) ;
#88198 = CARTESIAN_POINT('Origin',(26.3,248.2,26.0213203435596)) ;
#88199 = CARTESIAN_POINT('Origin',(26.3,246.4,26.0213203435596)) ;
#88200 = CARTESIAN_POINT('Origin',(28.1,247.3,26.3713203435596)) ;
#88201 = CARTESIAN_POINT('Origin',(26.3,248.2,26.7213203435596)) ;
#88202 = CARTESIAN_POINT('',(0.,0.,0.)) ;
#88203 = CARTESIAN_POINT('Origin',(64.1568347953872,220.146231446812,28.8213203435596)) ;
#88204 = CARTESIAN_POINT('',(66.0568347953872,220.146231446812,28.7213203435596)) ;
#88205 = CARTESIAN_POINT('Origin',(64.1568347953872,220.146231446812,28.7213203435596)) ;
#88206 = CARTESIAN_POINT('',(66.1568347953872,220.146231446812,28.8213203435596)) ;
#88207 = CARTESIAN_POINT('Origin',(66.0568347953872,220.146231446812,28.8213203435596)) ;
#88208 = CARTESIAN_POINT('',(62.1568347953872,220.146231446812,28.8213203435596)) ;
#88209 = CARTESIAN_POINT('Origin',(64.1568347953872,220.146231446812,28.8213203435596)) ;
#88210 = CARTESIAN_POINT('Origin',(64.1568347953872,220.146231446812,28.8213203435596)) ;
#88211 = CARTESIAN_POINT('Origin',(64.1568347953872,220.146231446812,30.2213203435596)) ;
#88212 = CARTESIAN_POINT('',(62.1568347953872,220.146231446812,30.0213203435596)) ;
#88213 = CARTESIAN_POINT('',(62.1568347953872,220.146231446812,30.2213203435596)) ;
#88214 = CARTESIAN_POINT('',(66.1568347953872,220.146231446812,30.0213203435596)) ;
#88215 = CARTESIAN_POINT('Origin',(64.1568347953872,220.146231446812,30.0213203435596)) ;
#88216 = CARTESIAN_POINT('Origin',(64.1568347953872,220.146231446812,30.0213203435596)) ;
#88217 = CARTESIAN_POINT('Origin',(64.1568347953872,220.146231446812,28.7213203435596)) ;
#88218 = CARTESIAN_POINT('Origin',(64.3068347953872,218.546231446812,30.1213203435596)) ;
#88219 = CARTESIAN_POINT('',(63.7568347953872,218.546231446812,30.2213203435596)) ;
#88220 = CARTESIAN_POINT('',(64.5568347953872,218.546231446812,30.2213203435596)) ;
#88221 = CARTESIAN_POINT('',(64.3068347953872,218.546231446812,30.2213203435596)) ;
#88222 = CARTESIAN_POINT('',(64.4568347953872,218.646231446812,30.1213203435596)) ;
#88223 = CARTESIAN_POINT('Origin',(64.5568347953872,218.546231446812,30.1213203435596)) ;
#88224 = CARTESIAN_POINT('',(63.8568347953872,218.646231446812,30.1213203435596)) ;
#88225 = CARTESIAN_POINT('',(64.3068347953872,218.646231446812,30.1213203435596)) ;
#88226 = CARTESIAN_POINT('Origin',(63.7568347953872,218.546231446812,30.1213203435596)) ;
#88227 = CARTESIAN_POINT('Origin',(64.5568347953872,219.996231446812,30.1213203435596)) ;
#88228 = CARTESIAN_POINT('',(64.5568347953872,219.746231446812,30.2213203435596)) ;
#88229 = CARTESIAN_POINT('',(64.5568347953872,219.996231446812,30.2213203435596)) ;
#88230 = CARTESIAN_POINT('',(64.4568347953872,219.846231446812,30.1213203435596)) ;
#88231 = CARTESIAN_POINT('Origin',(64.5568347953872,219.746231446812,30.1213203435596)) ;
#88232 = CARTESIAN_POINT('',(64.4568347953872,219.996231446812,30.1213203435596)) ;
#88233 = CARTESIAN_POINT('Origin',(64.9068347953872,219.746231446812,30.1213203435596)) ;
#88234 = CARTESIAN_POINT('',(65.7568347953872,219.746231446812,30.2213203435596)) ;
#88235 = CARTESIAN_POINT('',(64.9068347953872,219.746231446812,30.2213203435596)) ;
#88236 = CARTESIAN_POINT('',(65.6568347953872,219.846231446812,30.1213203435596)) ;
#88237 = CARTESIAN_POINT('Origin',(65.7568347953872,219.746231446812,30.1213203435596)) ;
#88238 = CARTESIAN_POINT('',(64.9068347953872,219.846231446812,30.1213203435596)) ;
#88239 = CARTESIAN_POINT('Origin',(65.7568347953872,220.296231446812,30.1213203435596)) ;
#88240 = CARTESIAN_POINT('',(65.7568347953872,220.546231446812,30.2213203435596)) ;
#88241 = CARTESIAN_POINT('',(65.7568347953872,220.296231446812,30.2213203435596)) ;
#88242 = CARTESIAN_POINT('',(65.6568347953872,220.446231446812,30.1213203435596)) ;
#88243 = CARTESIAN_POINT('Origin',(65.7568347953872,220.546231446812,30.1213203435596)) ;
#88244 = CARTESIAN_POINT('',(65.6568347953872,220.296231446812,30.1213203435596)) ;
#88245 = CARTESIAN_POINT('Origin',(64.3068347953872,220.546231446812,30.1213203435596)) ;
#88246 = CARTESIAN_POINT('',(64.5568347953872,220.546231446812,30.2213203435596)) ;
#88247 = CARTESIAN_POINT('',(64.3068347953872,220.546231446812,30.2213203435596)) ;
#88248 = CARTESIAN_POINT('',(64.4568347953872,220.446231446812,30.1213203435596)) ;
#88249 = CARTESIAN_POINT('Origin',(64.5568347953872,220.546231446812,30.1213203435596)) ;
#88250 = CARTESIAN_POINT('',(64.3068347953872,220.446231446812,30.1213203435596)) ;
#88251 = CARTESIAN_POINT('Origin',(64.0068347953872,221.746231446812,30.1213203435596)) ;
#88252 = CARTESIAN_POINT('',(64.5568347953872,221.746231446812,30.2213203435596)) ;
#88253 = CARTESIAN_POINT('',(63.7568347953872,221.746231446812,30.2213203435596)) ;
#88254 = CARTESIAN_POINT('',(64.0068347953872,221.746231446812,30.2213203435596)) ;
#88255 = CARTESIAN_POINT('',(63.8568347953872,221.646231446812,30.1213203435596)) ;
#88256 = CARTESIAN_POINT('Origin',(63.7568347953872,221.746231446812,30.1213203435596)) ;
#88257 = CARTESIAN_POINT('',(64.4568347953872,221.646231446812,30.1213203435596)) ;
#88258 = CARTESIAN_POINT('',(64.0068347953872,221.646231446812,30.1213203435596)) ;
#88259 = CARTESIAN_POINT('Origin',(64.5568347953872,221.746231446812,30.1213203435596)) ;
#88260 = CARTESIAN_POINT('Origin',(63.7568347953872,220.296231446812,30.1213203435596)) ;
#88261 = CARTESIAN_POINT('',(63.8568347953872,220.446231446812,30.1213203435596)) ;
#88262 = CARTESIAN_POINT('',(63.8568347953872,220.296231446812,30.1213203435596)) ;
#88263 = CARTESIAN_POINT('',(63.7568347953872,220.546231446812,30.2213203435596)) ;
#88264 = CARTESIAN_POINT('',(63.7568347953872,220.296231446812,30.2213203435596)) ;
#88265 = CARTESIAN_POINT('Origin',(63.7568347953872,220.546231446812,30.1213203435596)) ;
#88266 = CARTESIAN_POINT('Origin',(64.5568347953872,220.896231446812,30.1213203435596)) ;
#88267 = CARTESIAN_POINT('',(64.5568347953872,220.896231446812,30.2213203435596)) ;
#88268 = CARTESIAN_POINT('',(64.4568347953872,220.896231446812,30.1213203435596)) ;
#88269 = CARTESIAN_POINT('Origin',(63.4068347953872,220.546231446812,30.1213203435596)) ;
#88270 = CARTESIAN_POINT('',(62.6568347953872,220.446231446812,30.1213203435596)) ;
#88271 = CARTESIAN_POINT('',(63.4068347953872,220.446231446812,30.1213203435596)) ;
#88272 = CARTESIAN_POINT('',(62.5568347953872,220.546231446812,30.2213203435596)) ;
#88273 = CARTESIAN_POINT('',(63.4068347953872,220.546231446812,30.2213203435596)) ;
#88274 = CARTESIAN_POINT('Origin',(62.5568347953872,220.546231446812,30.1213203435596)) ;
#88275 = CARTESIAN_POINT('Origin',(62.5568347953872,219.996231446812,30.1213203435596)) ;
#88276 = CARTESIAN_POINT('',(62.6568347953872,219.846231446812,30.1213203435596)) ;
#88277 = CARTESIAN_POINT('',(62.6568347953872,219.996231446812,30.1213203435596)) ;
#88278 = CARTESIAN_POINT('',(62.5568347953872,219.746231446812,30.2213203435596)) ;
#88279 = CARTESIAN_POINT('',(62.5568347953872,219.996231446812,30.2213203435596)) ;
#88280 = CARTESIAN_POINT('Origin',(62.5568347953872,219.746231446812,30.1213203435596)) ;
#88281 = CARTESIAN_POINT('Origin',(64.0068347953872,219.746231446812,30.1213203435596)) ;
#88282 = CARTESIAN_POINT('',(63.8568347953872,219.846231446812,30.1213203435596)) ;
#88283 = CARTESIAN_POINT('',(64.0068347953872,219.846231446812,30.1213203435596)) ;
#88284 = CARTESIAN_POINT('',(63.7568347953872,219.746231446812,30.2213203435596)) ;
#88285 = CARTESIAN_POINT('',(64.0068347953872,219.746231446812,30.2213203435596)) ;
#88286 = CARTESIAN_POINT('Origin',(63.7568347953872,219.746231446812,30.1213203435596)) ;
#88287 = CARTESIAN_POINT('Origin',(63.7568347953872,219.396231446812,30.1213203435596)) ;
#88288 = CARTESIAN_POINT('',(63.8568347953872,219.396231446812,30.1213203435596)) ;
#88289 = CARTESIAN_POINT('',(63.7568347953872,219.396231446812,30.2213203435596)) ;
#88290 = CARTESIAN_POINT('Origin',(64.4568347953872,219.846231446812,30.7213203435596)) ;
#88291 = CARTESIAN_POINT('',(64.4568347953872,219.846231446812,30.0213203435596)) ;
#88292 = CARTESIAN_POINT('',(64.4568347953872,219.846231446812,30.7213203435596)) ;
#88293 = CARTESIAN_POINT('',(64.4568347953872,218.646231446812,30.0213203435596)) ;
#88294 = CARTESIAN_POINT('',(64.4568347953872,219.996231446812,30.0213203435596)) ;
#88295 = CARTESIAN_POINT('',(64.4568347953872,218.646231446812,30.7213203435596)) ;
#88296 = CARTESIAN_POINT('Origin',(65.6568347953872,219.846231446812,30.7213203435596)) ;
#88297 = CARTESIAN_POINT('',(65.6568347953872,219.846231446812,30.0213203435596)) ;
#88298 = CARTESIAN_POINT('',(65.6568347953872,219.846231446812,30.7213203435596)) ;
#88299 = CARTESIAN_POINT('',(64.9068347953872,219.846231446812,30.0213203435596)) ;
#88300 = CARTESIAN_POINT('Origin',(65.6568347953872,220.446231446812,30.7213203435596)) ;
#88301 = CARTESIAN_POINT('',(65.6568347953872,220.446231446812,30.0213203435596)) ;
#88302 = CARTESIAN_POINT('',(65.6568347953872,220.446231446812,30.7213203435596)) ;
#88303 = CARTESIAN_POINT('',(65.6568347953872,220.296231446812,30.0213203435596)) ;
#88304 = CARTESIAN_POINT('Origin',(64.4568347953872,220.446231446812,30.7213203435596)) ;
#88305 = CARTESIAN_POINT('',(64.4568347953872,220.446231446812,30.0213203435596)) ;
#88306 = CARTESIAN_POINT('',(64.4568347953872,220.446231446812,30.7213203435596)) ;
#88307 = CARTESIAN_POINT('',(64.3068347953872,220.446231446812,30.0213203435596)) ;
#88308 = CARTESIAN_POINT('Origin',(64.4568347953872,221.646231446812,30.7213203435596)) ;
#88309 = CARTESIAN_POINT('',(64.4568347953872,221.646231446812,30.0213203435596)) ;
#88310 = CARTESIAN_POINT('',(64.4568347953872,221.646231446812,30.7213203435596)) ;
#88311 = CARTESIAN_POINT('',(64.4568347953872,220.896231446812,30.0213203435596)) ;
#88312 = CARTESIAN_POINT('Origin',(63.8568347953872,221.646231446812,30.7213203435596)) ;
#88313 = CARTESIAN_POINT('',(63.8568347953872,221.646231446812,30.0213203435596)) ;
#88314 = CARTESIAN_POINT('',(63.8568347953872,221.646231446812,30.7213203435596)) ;
#88315 = CARTESIAN_POINT('',(64.0068347953872,221.646231446812,30.0213203435596)) ;
#88316 = CARTESIAN_POINT('Origin',(64.1568347953872,220.146231446812,30.2213203435596)) ;
#88317 = CARTESIAN_POINT('',(65.9568347953872,220.146231446812,30.2213203435596)) ;
#88318 = CARTESIAN_POINT('Origin',(64.1568347953872,220.146231446812,30.2213203435596)) ;
#88319 = CARTESIAN_POINT('Origin',(64.0068347953872,219.946231446812,30.0213203435596)) ;
#88320 = CARTESIAN_POINT('',(63.9568347953872,219.946231446812,29.9213203435596)) ;
#88321 = CARTESIAN_POINT('',(62.7568347953872,219.946231446812,29.9213203435596)) ;
#88322 = CARTESIAN_POINT('',(64.0068347953872,219.946231446812,29.9213203435596)) ;
#88323 = CARTESIAN_POINT('',(62.6568347953872,219.846231446812,30.0213203435596)) ;
#88324 = CARTESIAN_POINT('Origin',(62.7568347953872,219.946231446812,30.0213203435596)) ;
#88325 = CARTESIAN_POINT('',(63.8568347953872,219.846231446812,30.0213203435596)) ;
#88326 = CARTESIAN_POINT('',(64.0068347953872,219.846231446812,30.0213203435596)) ;
#88327 = CARTESIAN_POINT('Origin',(63.9568347953872,219.946231446812,30.0213203435596)) ;
#88328 = CARTESIAN_POINT('Origin',(62.7568347953872,219.996231446812,30.0213203435596)) ;
#88329 = CARTESIAN_POINT('',(62.7568347953872,220.346231446812,29.9213203435596)) ;
#88330 = CARTESIAN_POINT('',(62.7568347953872,219.996231446812,29.9213203435596)) ;
#88331 = CARTESIAN_POINT('',(62.6568347953872,220.446231446812,30.0213203435596)) ;
#88332 = CARTESIAN_POINT('Origin',(62.7568347953872,220.346231446812,30.0213203435596)) ;
#88333 = CARTESIAN_POINT('',(62.6568347953872,219.996231446812,30.0213203435596)) ;
#88334 = CARTESIAN_POINT('Origin',(63.4068347953872,220.346231446812,30.0213203435596)) ;
#88335 = CARTESIAN_POINT('',(63.9568347953872,220.346231446812,29.9213203435596)) ;
#88336 = CARTESIAN_POINT('',(63.4068347953872,220.346231446812,29.9213203435596)) ;
#88337 = CARTESIAN_POINT('',(63.8568347953872,220.446231446812,30.0213203435596)) ;
#88338 = CARTESIAN_POINT('Origin',(63.9568347953872,220.346231446812,30.0213203435596)) ;
#88339 = CARTESIAN_POINT('',(63.4068347953872,220.446231446812,30.0213203435596)) ;
#88340 = CARTESIAN_POINT('Origin',(63.9568347953872,220.296231446812,30.0213203435596)) ;
#88341 = CARTESIAN_POINT('',(63.9568347953872,221.546231446812,29.9213203435596)) ;
#88342 = CARTESIAN_POINT('',(63.9568347953872,220.296231446812,29.9213203435596)) ;
#88343 = CARTESIAN_POINT('Origin',(63.9568347953872,221.546231446812,30.0213203435596)) ;
#88344 = CARTESIAN_POINT('',(63.8568347953872,220.296231446812,30.0213203435596)) ;
#88345 = CARTESIAN_POINT('Origin',(64.0068347953872,221.546231446812,30.0213203435596)) ;
#88346 = CARTESIAN_POINT('',(64.3568347953872,221.546231446812,29.9213203435596)) ;
#88347 = CARTESIAN_POINT('',(64.0068347953872,221.546231446812,29.9213203435596)) ;
#88348 = CARTESIAN_POINT('Origin',(64.3568347953872,221.546231446812,30.0213203435596)) ;
#88349 = CARTESIAN_POINT('Origin',(64.3568347953872,220.896231446812,30.0213203435596)) ;
#88350 = CARTESIAN_POINT('',(64.3568347953872,220.346231446812,29.9213203435596)) ;
#88351 = CARTESIAN_POINT('',(64.3568347953872,220.896231446812,29.9213203435596)) ;
#88352 = CARTESIAN_POINT('Origin',(64.3568347953872,220.346231446812,30.0213203435596)) ;
#88353 = CARTESIAN_POINT('Origin',(64.3068347953872,220.346231446812,30.0213203435596)) ;
#88354 = CARTESIAN_POINT('',(65.5568347953872,220.346231446812,29.9213203435596)) ;
#88355 = CARTESIAN_POINT('',(64.3068347953872,220.346231446812,29.9213203435596)) ;
#88356 = CARTESIAN_POINT('Origin',(65.5568347953872,220.346231446812,30.0213203435596)) ;
#88357 = CARTESIAN_POINT('Origin',(65.5568347953872,220.296231446812,30.0213203435596)) ;
#88358 = CARTESIAN_POINT('',(65.5568347953872,219.946231446812,29.9213203435596)) ;
#88359 = CARTESIAN_POINT('',(65.5568347953872,220.296231446812,29.9213203435596)) ;
#88360 = CARTESIAN_POINT('Origin',(65.5568347953872,219.946231446812,30.0213203435596)) ;
#88361 = CARTESIAN_POINT('Origin',(64.9068347953872,219.946231446812,30.0213203435596)) ;
#88362 = CARTESIAN_POINT('',(64.3568347953872,219.946231446812,29.9213203435596)) ;
#88363 = CARTESIAN_POINT('',(64.9068347953872,219.946231446812,29.9213203435596)) ;
#88364 = CARTESIAN_POINT('Origin',(64.3568347953872,219.946231446812,30.0213203435596)) ;
#88365 = CARTESIAN_POINT('Origin',(64.3568347953872,219.996231446812,30.0213203435596)) ;
#88366 = CARTESIAN_POINT('',(64.3568347953872,218.746231446812,29.9213203435596)) ;
#88367 = CARTESIAN_POINT('',(64.3568347953872,219.996231446812,29.9213203435596)) ;
#88368 = CARTESIAN_POINT('Origin',(64.3568347953872,218.746231446812,30.0213203435596)) ;
#88369 = CARTESIAN_POINT('Origin',(64.3068347953872,218.746231446812,30.0213203435596)) ;
#88370 = CARTESIAN_POINT('',(63.8568347953872,218.646231446812,30.0213203435596)) ;
#88371 = CARTESIAN_POINT('',(64.3068347953872,218.646231446812,30.0213203435596)) ;
#88372 = CARTESIAN_POINT('',(63.9568347953872,218.746231446812,29.9213203435596)) ;
#88373 = CARTESIAN_POINT('',(64.3068347953872,218.746231446812,29.9213203435596)) ;
#88374 = CARTESIAN_POINT('Origin',(63.9568347953872,218.746231446812,30.0213203435596)) ;
#88375 = CARTESIAN_POINT('Origin',(63.9568347953872,219.396231446812,30.0213203435596)) ;
#88376 = CARTESIAN_POINT('',(63.8568347953872,219.396231446812,30.0213203435596)) ;
#88377 = CARTESIAN_POINT('',(63.9568347953872,219.396231446812,29.9213203435596)) ;
#88378 = CARTESIAN_POINT('Origin',(64.4568347953872,218.646231446812,30.7213203435596)) ;
#88379 = CARTESIAN_POINT('',(63.8568347953872,218.646231446812,30.7213203435596)) ;
#88380 = CARTESIAN_POINT('Origin',(63.8568347953872,218.646231446812,30.7213203435596)) ;
#88381 = CARTESIAN_POINT('',(63.8568347953872,219.846231446812,30.7213203435596)) ;
#88382 = CARTESIAN_POINT('Origin',(63.8568347953872,219.846231446812,30.7213203435596)) ;
#88383 = CARTESIAN_POINT('',(62.6568347953872,219.846231446812,30.7213203435596)) ;
#88384 = CARTESIAN_POINT('Origin',(64.1568347953872,220.146231446812,29.9213203435596)) ;
#88385 = CARTESIAN_POINT('Origin',(64.1568347953872,220.146231446812,30.0213203435596)) ;
#88386 = CARTESIAN_POINT('Origin',(65.9568347953872,220.146231446812,30.0213203435596)) ;
#88387 = CARTESIAN_POINT('Origin',(62.6568347953872,219.846231446812,30.7213203435596)) ;
#88388 = CARTESIAN_POINT('',(62.6568347953872,220.446231446812,30.7213203435596)) ;
#88389 = CARTESIAN_POINT('Origin',(62.6568347953872,220.446231446812,30.7213203435596)) ;
#88390 = CARTESIAN_POINT('',(63.8568347953872,220.446231446812,30.7213203435596)) ;
#88391 = CARTESIAN_POINT('Origin',(63.8568347953872,220.446231446812,30.7213203435596)) ;
#88392 = CARTESIAN_POINT('',(0.,0.,0.)) ;
#88393 = CARTESIAN_POINT('Origin',(61.35,261.,30.0213203435596)) ;
#88394 = CARTESIAN_POINT('',(61.3,261.,29.9213203435596)) ;
#88395 = CARTESIAN_POINT('',(60.1,261.,29.9213203435596)) ;
#88396 = CARTESIAN_POINT('',(61.35,261.,29.9213203435596)) ;
#88397 = CARTESIAN_POINT('',(60.,260.9,30.0213203435596)) ;
#88398 = CARTESIAN_POINT('Origin',(60.1,261.,30.0213203435596)) ;
#88399 = CARTESIAN_POINT('',(61.2,260.9,30.0213203435596)) ;
#88400 = CARTESIAN_POINT('',(61.35,260.9,30.0213203435596)) ;
#88401 = CARTESIAN_POINT('Origin',(61.3,261.,30.0213203435596)) ;
#88402 = CARTESIAN_POINT('Origin',(60.1,261.05,30.0213203435596)) ;
#88403 = CARTESIAN_POINT('',(60.1,261.4,29.9213203435596)) ;
#88404 = CARTESIAN_POINT('',(60.1,261.05,29.9213203435596)) ;
#88405 = CARTESIAN_POINT('',(60.,261.5,30.0213203435596)) ;
#88406 = CARTESIAN_POINT('Origin',(60.1,261.4,30.0213203435596)) ;
#88407 = CARTESIAN_POINT('',(60.,261.05,30.0213203435596)) ;
#88408 = CARTESIAN_POINT('Origin',(60.75,261.4,30.0213203435596)) ;
#88409 = CARTESIAN_POINT('',(61.3,261.4,29.9213203435596)) ;
#88410 = CARTESIAN_POINT('',(60.75,261.4,29.9213203435596)) ;
#88411 = CARTESIAN_POINT('',(61.2,261.5,30.0213203435596)) ;
#88412 = CARTESIAN_POINT('Origin',(61.3,261.4,30.0213203435596)) ;
#88413 = CARTESIAN_POINT('',(60.75,261.5,30.0213203435596)) ;
#88414 = CARTESIAN_POINT('Origin',(61.3,261.35,30.0213203435596)) ;
#88415 = CARTESIAN_POINT('',(61.3,262.6,29.9213203435596)) ;
#88416 = CARTESIAN_POINT('',(61.3,261.35,29.9213203435596)) ;
#88417 = CARTESIAN_POINT('',(61.2,262.7,30.0213203435596)) ;
#88418 = CARTESIAN_POINT('Origin',(61.3,262.6,30.0213203435596)) ;
#88419 = CARTESIAN_POINT('',(61.2,261.35,30.0213203435596)) ;
#88420 = CARTESIAN_POINT('Origin',(61.35,262.6,30.0213203435596)) ;
#88421 = CARTESIAN_POINT('',(61.7,262.6,29.9213203435596)) ;
#88422 = CARTESIAN_POINT('',(61.35,262.6,29.9213203435596)) ;
#88423 = CARTESIAN_POINT('',(61.8,262.7,30.0213203435596)) ;
#88424 = CARTESIAN_POINT('Origin',(61.7,262.6,30.0213203435596)) ;
#88425 = CARTESIAN_POINT('',(61.35,262.7,30.0213203435596)) ;
#88426 = CARTESIAN_POINT('Origin',(61.7,261.95,30.0213203435596)) ;
#88427 = CARTESIAN_POINT('',(61.8,261.5,30.0213203435596)) ;
#88428 = CARTESIAN_POINT('',(61.8,261.95,30.0213203435596)) ;
#88429 = CARTESIAN_POINT('',(61.7,261.4,29.9213203435596)) ;
#88430 = CARTESIAN_POINT('',(61.7,261.95,29.9213203435596)) ;
#88431 = CARTESIAN_POINT('Origin',(61.7,261.4,30.0213203435596)) ;
#88432 = CARTESIAN_POINT('Origin',(61.65,261.4,30.0213203435596)) ;
#88433 = CARTESIAN_POINT('',(63.,261.5,30.0213203435596)) ;
#88434 = CARTESIAN_POINT('',(61.65,261.5,30.0213203435596)) ;
#88435 = CARTESIAN_POINT('',(62.9,261.4,29.9213203435596)) ;
#88436 = CARTESIAN_POINT('',(61.65,261.4,29.9213203435596)) ;
#88437 = CARTESIAN_POINT('Origin',(62.9,261.4,30.0213203435596)) ;
#88438 = CARTESIAN_POINT('Origin',(62.9,261.35,30.0213203435596)) ;
#88439 = CARTESIAN_POINT('',(63.,260.9,30.0213203435596)) ;
#88440 = CARTESIAN_POINT('',(63.,261.35,30.0213203435596)) ;
#88441 = CARTESIAN_POINT('',(62.9,261.,29.9213203435596)) ;
#88442 = CARTESIAN_POINT('',(62.9,261.35,29.9213203435596)) ;
#88443 = CARTESIAN_POINT('Origin',(62.9,261.,30.0213203435596)) ;
#88444 = CARTESIAN_POINT('Origin',(62.25,261.,30.0213203435596)) ;
#88445 = CARTESIAN_POINT('',(61.8,260.9,30.0213203435596)) ;
#88446 = CARTESIAN_POINT('',(62.25,260.9,30.0213203435596)) ;
#88447 = CARTESIAN_POINT('',(61.7,261.,29.9213203435596)) ;
#88448 = CARTESIAN_POINT('',(62.25,261.,29.9213203435596)) ;
#88449 = CARTESIAN_POINT('Origin',(61.7,261.,30.0213203435596)) ;
#88450 = CARTESIAN_POINT('Origin',(61.7,261.05,30.0213203435596)) ;
#88451 = CARTESIAN_POINT('',(61.8,259.7,30.0213203435596)) ;
#88452 = CARTESIAN_POINT('',(61.8,261.05,30.0213203435596)) ;
#88453 = CARTESIAN_POINT('',(61.7,259.8,29.9213203435596)) ;
#88454 = CARTESIAN_POINT('',(61.7,261.05,29.9213203435596)) ;
#88455 = CARTESIAN_POINT('Origin',(61.7,259.8,30.0213203435596)) ;
#88456 = CARTESIAN_POINT('Origin',(61.65,259.8,30.0213203435596)) ;
#88457 = CARTESIAN_POINT('',(61.2,259.7,30.0213203435596)) ;
#88458 = CARTESIAN_POINT('',(61.65,259.7,30.0213203435596)) ;
#88459 = CARTESIAN_POINT('',(61.3,259.8,29.9213203435596)) ;
#88460 = CARTESIAN_POINT('',(61.65,259.8,29.9213203435596)) ;
#88461 = CARTESIAN_POINT('Origin',(61.3,259.8,30.0213203435596)) ;
#88462 = CARTESIAN_POINT('Origin',(61.3,260.45,30.0213203435596)) ;
#88463 = CARTESIAN_POINT('',(61.2,260.45,30.0213203435596)) ;
#88464 = CARTESIAN_POINT('',(61.3,260.45,29.9213203435596)) ;
#88465 = CARTESIAN_POINT('Origin',(63.,261.5,30.7213203435596)) ;
#88466 = CARTESIAN_POINT('',(63.,260.9,30.1213203435596)) ;
#88467 = CARTESIAN_POINT('',(63.,260.9,30.7213203435596)) ;
#88468 = CARTESIAN_POINT('',(63.,261.5,30.1213203435596)) ;
#88469 = CARTESIAN_POINT('',(63.,261.35,30.1213203435596)) ;
#88470 = CARTESIAN_POINT('',(63.,261.5,30.7213203435596)) ;
#88471 = CARTESIAN_POINT('Origin',(63.,260.9,30.7213203435596)) ;
#88472 = CARTESIAN_POINT('',(61.8,260.9,30.1213203435596)) ;
#88473 = CARTESIAN_POINT('',(61.8,260.9,30.7213203435596)) ;
#88474 = CARTESIAN_POINT('',(62.25,260.9,30.1213203435596)) ;
#88475 = CARTESIAN_POINT('Origin',(61.8,260.9,30.7213203435596)) ;
#88476 = CARTESIAN_POINT('',(61.8,259.7,30.1213203435596)) ;
#88477 = CARTESIAN_POINT('',(61.8,259.7,30.7213203435596)) ;
#88478 = CARTESIAN_POINT('',(61.8,261.05,30.1213203435596)) ;
#88479 = CARTESIAN_POINT('Origin',(61.8,259.7,30.7213203435596)) ;
#88480 = CARTESIAN_POINT('',(61.2,259.7,30.1213203435596)) ;
#88481 = CARTESIAN_POINT('',(61.2,259.7,30.7213203435596)) ;
#88482 = CARTESIAN_POINT('',(61.65,259.7,30.1213203435596)) ;
#88483 = CARTESIAN_POINT('Origin',(61.2,259.7,30.7213203435596)) ;
#88484 = CARTESIAN_POINT('',(61.2,260.9,30.1213203435596)) ;
#88485 = CARTESIAN_POINT('',(61.2,260.9,30.7213203435596)) ;
#88486 = CARTESIAN_POINT('',(61.2,260.45,30.1213203435596)) ;
#88487 = CARTESIAN_POINT('Origin',(61.2,260.9,30.7213203435596)) ;
#88488 = CARTESIAN_POINT('',(60.,260.9,30.1213203435596)) ;
#88489 = CARTESIAN_POINT('',(60.,260.9,30.7213203435596)) ;
#88490 = CARTESIAN_POINT('',(61.35,260.9,30.1213203435596)) ;
#88491 = CARTESIAN_POINT('Origin',(61.5,261.2,29.9213203435596)) ;
#88492 = CARTESIAN_POINT('Origin',(61.5,261.2,28.8213203435596)) ;
#88493 = CARTESIAN_POINT('',(63.9,261.2,28.7213203435596)) ;
#88494 = CARTESIAN_POINT('Origin',(61.5,261.2,28.7213203435596)) ;
#88495 = CARTESIAN_POINT('',(64.,261.2,28.8213203435596)) ;
#88496 = CARTESIAN_POINT('Origin',(63.9,261.2,28.8213203435596)) ;
#88497 = CARTESIAN_POINT('',(59.,261.2,28.8213203435596)) ;
#88498 = CARTESIAN_POINT('Origin',(61.5,261.2,28.8213203435596)) ;
#88499 = CARTESIAN_POINT('Origin',(61.5,261.2,28.8213203435596)) ;
#88500 = CARTESIAN_POINT('Origin',(61.5,261.2,30.2213203435596)) ;
#88501 = CARTESIAN_POINT('',(59.,261.2,30.0213203435596)) ;
#88502 = CARTESIAN_POINT('',(59.,261.2,30.2213203435596)) ;
#88503 = CARTESIAN_POINT('',(64.,261.2,30.0213203435596)) ;
#88504 = CARTESIAN_POINT('Origin',(61.5,261.2,30.0213203435596)) ;
#88505 = CARTESIAN_POINT('Origin',(61.5,261.2,30.0213203435596)) ;
#88506 = CARTESIAN_POINT('Origin',(61.5,261.2,28.7213203435596)) ;
#88507 = CARTESIAN_POINT('Origin',(61.65,259.6,30.1213203435596)) ;
#88508 = CARTESIAN_POINT('',(61.1,259.6,30.2213203435596)) ;
#88509 = CARTESIAN_POINT('',(61.9,259.6,30.2213203435596)) ;
#88510 = CARTESIAN_POINT('',(61.65,259.6,30.2213203435596)) ;
#88511 = CARTESIAN_POINT('Origin',(61.9,259.6,30.1213203435596)) ;
#88512 = CARTESIAN_POINT('Origin',(61.1,259.6,30.1213203435596)) ;
#88513 = CARTESIAN_POINT('Origin',(61.9,261.05,30.1213203435596)) ;
#88514 = CARTESIAN_POINT('',(61.9,260.8,30.2213203435596)) ;
#88515 = CARTESIAN_POINT('',(61.9,261.05,30.2213203435596)) ;
#88516 = CARTESIAN_POINT('Origin',(61.9,260.8,30.1213203435596)) ;
#88517 = CARTESIAN_POINT('Origin',(62.25,260.8,30.1213203435596)) ;
#88518 = CARTESIAN_POINT('',(63.1,260.8,30.2213203435596)) ;
#88519 = CARTESIAN_POINT('',(62.25,260.8,30.2213203435596)) ;
#88520 = CARTESIAN_POINT('Origin',(63.1,260.8,30.1213203435596)) ;
#88521 = CARTESIAN_POINT('Origin',(63.1,261.35,30.1213203435596)) ;
#88522 = CARTESIAN_POINT('',(63.1,261.6,30.2213203435596)) ;
#88523 = CARTESIAN_POINT('',(63.1,261.35,30.2213203435596)) ;
#88524 = CARTESIAN_POINT('Origin',(63.1,261.6,30.1213203435596)) ;
#88525 = CARTESIAN_POINT('Origin',(61.65,261.6,30.1213203435596)) ;
#88526 = CARTESIAN_POINT('',(61.9,261.6,30.2213203435596)) ;
#88527 = CARTESIAN_POINT('',(61.65,261.6,30.2213203435596)) ;
#88528 = CARTESIAN_POINT('',(61.8,261.5,30.1213203435596)) ;
#88529 = CARTESIAN_POINT('Origin',(61.9,261.6,30.1213203435596)) ;
#88530 = CARTESIAN_POINT('',(61.65,261.5,30.1213203435596)) ;
#88531 = CARTESIAN_POINT('Origin',(61.35,262.8,30.1213203435596)) ;
#88532 = CARTESIAN_POINT('',(61.9,262.8,30.2213203435596)) ;
#88533 = CARTESIAN_POINT('',(61.1,262.8,30.2213203435596)) ;
#88534 = CARTESIAN_POINT('',(61.35,262.8,30.2213203435596)) ;
#88535 = CARTESIAN_POINT('',(61.2,262.7,30.1213203435596)) ;
#88536 = CARTESIAN_POINT('Origin',(61.1,262.8,30.1213203435596)) ;
#88537 = CARTESIAN_POINT('',(61.8,262.7,30.1213203435596)) ;
#88538 = CARTESIAN_POINT('',(61.35,262.7,30.1213203435596)) ;
#88539 = CARTESIAN_POINT('Origin',(61.9,262.8,30.1213203435596)) ;
#88540 = CARTESIAN_POINT('Origin',(61.1,261.35,30.1213203435596)) ;
#88541 = CARTESIAN_POINT('',(61.2,261.5,30.1213203435596)) ;
#88542 = CARTESIAN_POINT('',(61.2,261.35,30.1213203435596)) ;
#88543 = CARTESIAN_POINT('',(61.1,261.6,30.2213203435596)) ;
#88544 = CARTESIAN_POINT('',(61.1,261.35,30.2213203435596)) ;
#88545 = CARTESIAN_POINT('Origin',(61.1,261.6,30.1213203435596)) ;
#88546 = CARTESIAN_POINT('Origin',(61.9,261.95,30.1213203435596)) ;
#88547 = CARTESIAN_POINT('',(61.9,261.95,30.2213203435596)) ;
#88548 = CARTESIAN_POINT('',(61.8,261.95,30.1213203435596)) ;
#88549 = CARTESIAN_POINT('Origin',(60.75,261.6,30.1213203435596)) ;
#88550 = CARTESIAN_POINT('',(60.,261.5,30.1213203435596)) ;
#88551 = CARTESIAN_POINT('',(60.75,261.5,30.1213203435596)) ;
#88552 = CARTESIAN_POINT('',(59.9,261.6,30.2213203435596)) ;
#88553 = CARTESIAN_POINT('',(60.75,261.6,30.2213203435596)) ;
#88554 = CARTESIAN_POINT('Origin',(59.9,261.6,30.1213203435596)) ;
#88555 = CARTESIAN_POINT('Origin',(59.9,261.05,30.1213203435596)) ;
#88556 = CARTESIAN_POINT('',(60.,261.05,30.1213203435596)) ;
#88557 = CARTESIAN_POINT('',(59.9,260.8,30.2213203435596)) ;
#88558 = CARTESIAN_POINT('',(59.9,261.05,30.2213203435596)) ;
#88559 = CARTESIAN_POINT('Origin',(59.9,260.8,30.1213203435596)) ;
#88560 = CARTESIAN_POINT('Origin',(61.35,260.8,30.1213203435596)) ;
#88561 = CARTESIAN_POINT('',(61.1,260.8,30.2213203435596)) ;
#88562 = CARTESIAN_POINT('',(61.35,260.8,30.2213203435596)) ;
#88563 = CARTESIAN_POINT('Origin',(61.1,260.8,30.1213203435596)) ;
#88564 = CARTESIAN_POINT('Origin',(61.1,260.45,30.1213203435596)) ;
#88565 = CARTESIAN_POINT('',(61.1,260.45,30.2213203435596)) ;
#88566 = CARTESIAN_POINT('Origin',(61.8,261.5,30.7213203435596)) ;
#88567 = CARTESIAN_POINT('',(61.8,261.5,30.7213203435596)) ;
#88568 = CARTESIAN_POINT('Origin',(61.8,262.7,30.7213203435596)) ;
#88569 = CARTESIAN_POINT('',(61.8,262.7,30.7213203435596)) ;
#88570 = CARTESIAN_POINT('Origin',(61.2,262.7,30.7213203435596)) ;
#88571 = CARTESIAN_POINT('',(61.2,262.7,30.7213203435596)) ;
#88572 = CARTESIAN_POINT('Origin',(61.5,261.2,30.2213203435596)) ;
#88573 = CARTESIAN_POINT('',(63.8,261.2,30.2213203435596)) ;
#88574 = CARTESIAN_POINT('Origin',(61.5,261.2,30.2213203435596)) ;
#88575 = CARTESIAN_POINT('Origin',(61.5,261.2,30.0213203435596)) ;
#88576 = CARTESIAN_POINT('Origin',(63.8,261.2,30.0213203435596)) ;
#88577 = CARTESIAN_POINT('Origin',(60.,260.9,30.7213203435596)) ;
#88578 = CARTESIAN_POINT('',(60.,261.5,30.7213203435596)) ;
#88579 = CARTESIAN_POINT('Origin',(60.,261.5,30.7213203435596)) ;
#88580 = CARTESIAN_POINT('',(61.2,261.5,30.7213203435596)) ;
#88581 = CARTESIAN_POINT('Origin',(61.2,261.5,30.7213203435596)) ;
#88582 = CARTESIAN_POINT('',(0.,0.,0.)) ;
#88583 = CARTESIAN_POINT('Origin',(30.55,254.6,30.0213203435596)) ;
#88584 = CARTESIAN_POINT('',(30.5,254.6,29.9213203435596)) ;
#88585 = CARTESIAN_POINT('',(29.3,254.6,29.9213203435596)) ;
#88586 = CARTESIAN_POINT('',(30.55,254.6,29.9213203435596)) ;
#88587 = CARTESIAN_POINT('',(29.2,254.5,30.0213203435596)) ;
#88588 = CARTESIAN_POINT('Origin',(29.3,254.6,30.0213203435596)) ;
#88589 = CARTESIAN_POINT('',(30.4,254.5,30.0213203435596)) ;
#88590 = CARTESIAN_POINT('',(30.55,254.5,30.0213203435596)) ;
#88591 = CARTESIAN_POINT('Origin',(30.5,254.6,30.0213203435596)) ;
#88592 = CARTESIAN_POINT('Origin',(29.3,254.65,30.0213203435596)) ;
#88593 = CARTESIAN_POINT('',(29.3,255.,29.9213203435596)) ;
#88594 = CARTESIAN_POINT('',(29.3,254.65,29.9213203435596)) ;
#88595 = CARTESIAN_POINT('',(29.2,255.1,30.0213203435596)) ;
#88596 = CARTESIAN_POINT('Origin',(29.3,255.,30.0213203435596)) ;
#88597 = CARTESIAN_POINT('',(29.2,254.65,30.0213203435596)) ;
#88598 = CARTESIAN_POINT('Origin',(29.95,255.,30.0213203435596)) ;
#88599 = CARTESIAN_POINT('',(30.5,255.,29.9213203435596)) ;
#88600 = CARTESIAN_POINT('',(29.95,255.,29.9213203435596)) ;
#88601 = CARTESIAN_POINT('',(30.4,255.1,30.0213203435596)) ;
#88602 = CARTESIAN_POINT('Origin',(30.5,255.,30.0213203435596)) ;
#88603 = CARTESIAN_POINT('',(29.95,255.1,30.0213203435596)) ;
#88604 = CARTESIAN_POINT('Origin',(30.5,254.95,30.0213203435596)) ;
#88605 = CARTESIAN_POINT('',(30.5,256.2,29.9213203435596)) ;
#88606 = CARTESIAN_POINT('',(30.5,254.95,29.9213203435596)) ;
#88607 = CARTESIAN_POINT('',(30.4,256.3,30.0213203435596)) ;
#88608 = CARTESIAN_POINT('Origin',(30.5,256.2,30.0213203435596)) ;
#88609 = CARTESIAN_POINT('',(30.4,254.95,30.0213203435596)) ;
#88610 = CARTESIAN_POINT('Origin',(30.55,256.2,30.0213203435596)) ;
#88611 = CARTESIAN_POINT('',(30.9,256.2,29.9213203435596)) ;
#88612 = CARTESIAN_POINT('',(30.55,256.2,29.9213203435596)) ;
#88613 = CARTESIAN_POINT('',(31.,256.3,30.0213203435596)) ;
#88614 = CARTESIAN_POINT('Origin',(30.9,256.2,30.0213203435596)) ;
#88615 = CARTESIAN_POINT('',(30.55,256.3,30.0213203435596)) ;
#88616 = CARTESIAN_POINT('Origin',(30.9,255.55,30.0213203435596)) ;
#88617 = CARTESIAN_POINT('',(31.,255.1,30.0213203435596)) ;
#88618 = CARTESIAN_POINT('',(31.,255.55,30.0213203435596)) ;
#88619 = CARTESIAN_POINT('',(30.9,255.,29.9213203435596)) ;
#88620 = CARTESIAN_POINT('',(30.9,255.55,29.9213203435596)) ;
#88621 = CARTESIAN_POINT('Origin',(30.9,255.,30.0213203435596)) ;
#88622 = CARTESIAN_POINT('Origin',(30.85,255.,30.0213203435596)) ;
#88623 = CARTESIAN_POINT('',(32.2,255.1,30.0213203435596)) ;
#88624 = CARTESIAN_POINT('',(30.85,255.1,30.0213203435596)) ;
#88625 = CARTESIAN_POINT('',(32.1,255.,29.9213203435596)) ;
#88626 = CARTESIAN_POINT('',(30.85,255.,29.9213203435596)) ;
#88627 = CARTESIAN_POINT('Origin',(32.1,255.,30.0213203435596)) ;
#88628 = CARTESIAN_POINT('Origin',(32.1,254.95,30.0213203435596)) ;
#88629 = CARTESIAN_POINT('',(32.2,254.5,30.0213203435596)) ;
#88630 = CARTESIAN_POINT('',(32.2,254.95,30.0213203435596)) ;
#88631 = CARTESIAN_POINT('',(32.1,254.6,29.9213203435596)) ;
#88632 = CARTESIAN_POINT('',(32.1,254.95,29.9213203435596)) ;
#88633 = CARTESIAN_POINT('Origin',(32.1,254.6,30.0213203435596)) ;
#88634 = CARTESIAN_POINT('Origin',(31.45,254.6,30.0213203435596)) ;
#88635 = CARTESIAN_POINT('',(31.,254.5,30.0213203435596)) ;
#88636 = CARTESIAN_POINT('',(31.45,254.5,30.0213203435596)) ;
#88637 = CARTESIAN_POINT('',(30.9,254.6,29.9213203435596)) ;
#88638 = CARTESIAN_POINT('',(31.45,254.6,29.9213203435596)) ;
#88639 = CARTESIAN_POINT('Origin',(30.9,254.6,30.0213203435596)) ;
#88640 = CARTESIAN_POINT('Origin',(30.9,254.65,30.0213203435596)) ;
#88641 = CARTESIAN_POINT('',(31.,253.3,30.0213203435596)) ;
#88642 = CARTESIAN_POINT('',(31.,254.65,30.0213203435596)) ;
#88643 = CARTESIAN_POINT('',(30.9,253.4,29.9213203435596)) ;
#88644 = CARTESIAN_POINT('',(30.9,254.65,29.9213203435596)) ;
#88645 = CARTESIAN_POINT('Origin',(30.9,253.4,30.0213203435596)) ;
#88646 = CARTESIAN_POINT('Origin',(30.85,253.4,30.0213203435596)) ;
#88647 = CARTESIAN_POINT('',(30.4,253.3,30.0213203435596)) ;
#88648 = CARTESIAN_POINT('',(30.85,253.3,30.0213203435596)) ;
#88649 = CARTESIAN_POINT('',(30.5,253.4,29.9213203435596)) ;
#88650 = CARTESIAN_POINT('',(30.85,253.4,29.9213203435596)) ;
#88651 = CARTESIAN_POINT('Origin',(30.5,253.4,30.0213203435596)) ;
#88652 = CARTESIAN_POINT('Origin',(30.5,254.05,30.0213203435596)) ;
#88653 = CARTESIAN_POINT('',(30.4,254.05,30.0213203435596)) ;
#88654 = CARTESIAN_POINT('',(30.5,254.05,29.9213203435596)) ;
#88655 = CARTESIAN_POINT('Origin',(32.2,255.1,30.7213203435596)) ;
#88656 = CARTESIAN_POINT('',(32.2,254.5,30.1213203435596)) ;
#88657 = CARTESIAN_POINT('',(32.2,254.5,30.7213203435596)) ;
#88658 = CARTESIAN_POINT('',(32.2,255.1,30.1213203435596)) ;
#88659 = CARTESIAN_POINT('',(32.2,254.95,30.1213203435596)) ;
#88660 = CARTESIAN_POINT('',(32.2,255.1,30.7213203435596)) ;
#88661 = CARTESIAN_POINT('Origin',(32.2,254.5,30.7213203435596)) ;
#88662 = CARTESIAN_POINT('',(31.,254.5,30.1213203435596)) ;
#88663 = CARTESIAN_POINT('',(31.,254.5,30.7213203435596)) ;
#88664 = CARTESIAN_POINT('',(31.45,254.5,30.1213203435596)) ;
#88665 = CARTESIAN_POINT('Origin',(31.,254.5,30.7213203435596)) ;
#88666 = CARTESIAN_POINT('',(31.,253.3,30.1213203435596)) ;
#88667 = CARTESIAN_POINT('',(31.,253.3,30.7213203435596)) ;
#88668 = CARTESIAN_POINT('',(31.,254.65,30.1213203435596)) ;
#88669 = CARTESIAN_POINT('Origin',(31.,253.3,30.7213203435596)) ;
#88670 = CARTESIAN_POINT('',(30.4,253.3,30.1213203435596)) ;
#88671 = CARTESIAN_POINT('',(30.4,253.3,30.7213203435596)) ;
#88672 = CARTESIAN_POINT('',(30.85,253.3,30.1213203435596)) ;
#88673 = CARTESIAN_POINT('Origin',(30.4,253.3,30.7213203435596)) ;
#88674 = CARTESIAN_POINT('',(30.4,254.5,30.1213203435596)) ;
#88675 = CARTESIAN_POINT('',(30.4,254.5,30.7213203435596)) ;
#88676 = CARTESIAN_POINT('',(30.4,254.05,30.1213203435596)) ;
#88677 = CARTESIAN_POINT('Origin',(30.4,254.5,30.7213203435596)) ;
#88678 = CARTESIAN_POINT('',(29.2,254.5,30.1213203435596)) ;
#88679 = CARTESIAN_POINT('',(29.2,254.5,30.7213203435596)) ;
#88680 = CARTESIAN_POINT('',(30.55,254.5,30.1213203435596)) ;
#88681 = CARTESIAN_POINT('Origin',(30.7,254.8,29.9213203435596)) ;
#88682 = CARTESIAN_POINT('Origin',(30.7,254.8,28.8213203435596)) ;
#88683 = CARTESIAN_POINT('',(33.1,254.8,28.7213203435596)) ;
#88684 = CARTESIAN_POINT('Origin',(30.7,254.8,28.7213203435596)) ;
#88685 = CARTESIAN_POINT('',(33.2,254.8,28.8213203435596)) ;
#88686 = CARTESIAN_POINT('Origin',(33.1,254.8,28.8213203435596)) ;
#88687 = CARTESIAN_POINT('',(28.2,254.8,28.8213203435596)) ;
#88688 = CARTESIAN_POINT('Origin',(30.7,254.8,28.8213203435596)) ;
#88689 = CARTESIAN_POINT('Origin',(30.7,254.8,28.8213203435596)) ;
#88690 = CARTESIAN_POINT('Origin',(30.7,254.8,30.2213203435596)) ;
#88691 = CARTESIAN_POINT('',(28.2,254.8,30.0213203435596)) ;
#88692 = CARTESIAN_POINT('',(28.2,254.8,30.2213203435596)) ;
#88693 = CARTESIAN_POINT('',(33.2,254.8,30.0213203435596)) ;
#88694 = CARTESIAN_POINT('Origin',(30.7,254.8,30.0213203435596)) ;
#88695 = CARTESIAN_POINT('Origin',(30.7,254.8,30.0213203435596)) ;
#88696 = CARTESIAN_POINT('Origin',(30.7,254.8,28.7213203435596)) ;
#88697 = CARTESIAN_POINT('Origin',(30.85,253.2,30.1213203435596)) ;
#88698 = CARTESIAN_POINT('',(30.3,253.2,30.2213203435596)) ;
#88699 = CARTESIAN_POINT('',(31.1,253.2,30.2213203435596)) ;
#88700 = CARTESIAN_POINT('',(30.85,253.2,30.2213203435596)) ;
#88701 = CARTESIAN_POINT('Origin',(31.1,253.2,30.1213203435596)) ;
#88702 = CARTESIAN_POINT('Origin',(30.3,253.2,30.1213203435596)) ;
#88703 = CARTESIAN_POINT('Origin',(31.1,254.65,30.1213203435596)) ;
#88704 = CARTESIAN_POINT('',(31.1,254.4,30.2213203435596)) ;
#88705 = CARTESIAN_POINT('',(31.1,254.65,30.2213203435596)) ;
#88706 = CARTESIAN_POINT('Origin',(31.1,254.4,30.1213203435596)) ;
#88707 = CARTESIAN_POINT('Origin',(31.45,254.4,30.1213203435596)) ;
#88708 = CARTESIAN_POINT('',(32.3,254.4,30.2213203435596)) ;
#88709 = CARTESIAN_POINT('',(31.45,254.4,30.2213203435596)) ;
#88710 = CARTESIAN_POINT('Origin',(32.3,254.4,30.1213203435596)) ;
#88711 = CARTESIAN_POINT('Origin',(32.3,254.95,30.1213203435596)) ;
#88712 = CARTESIAN_POINT('',(32.3,255.2,30.2213203435596)) ;
#88713 = CARTESIAN_POINT('',(32.3,254.95,30.2213203435596)) ;
#88714 = CARTESIAN_POINT('Origin',(32.3,255.2,30.1213203435596)) ;
#88715 = CARTESIAN_POINT('Origin',(30.85,255.2,30.1213203435596)) ;
#88716 = CARTESIAN_POINT('',(31.1,255.2,30.2213203435596)) ;
#88717 = CARTESIAN_POINT('',(30.85,255.2,30.2213203435596)) ;
#88718 = CARTESIAN_POINT('',(31.,255.1,30.1213203435596)) ;
#88719 = CARTESIAN_POINT('Origin',(31.1,255.2,30.1213203435596)) ;
#88720 = CARTESIAN_POINT('',(30.85,255.1,30.1213203435596)) ;
#88721 = CARTESIAN_POINT('Origin',(30.55,256.4,30.1213203435596)) ;
#88722 = CARTESIAN_POINT('',(31.1,256.4,30.2213203435596)) ;
#88723 = CARTESIAN_POINT('',(30.3,256.4,30.2213203435596)) ;
#88724 = CARTESIAN_POINT('',(30.55,256.4,30.2213203435596)) ;
#88725 = CARTESIAN_POINT('',(30.4,256.3,30.1213203435596)) ;
#88726 = CARTESIAN_POINT('Origin',(30.3,256.4,30.1213203435596)) ;
#88727 = CARTESIAN_POINT('',(31.,256.3,30.1213203435596)) ;
#88728 = CARTESIAN_POINT('',(30.55,256.3,30.1213203435596)) ;
#88729 = CARTESIAN_POINT('Origin',(31.1,256.4,30.1213203435596)) ;
#88730 = CARTESIAN_POINT('Origin',(30.3,254.95,30.1213203435596)) ;
#88731 = CARTESIAN_POINT('',(30.4,255.1,30.1213203435596)) ;
#88732 = CARTESIAN_POINT('',(30.4,254.95,30.1213203435596)) ;
#88733 = CARTESIAN_POINT('',(30.3,255.2,30.2213203435596)) ;
#88734 = CARTESIAN_POINT('',(30.3,254.95,30.2213203435596)) ;
#88735 = CARTESIAN_POINT('Origin',(30.3,255.2,30.1213203435596)) ;
#88736 = CARTESIAN_POINT('Origin',(31.1,255.55,30.1213203435596)) ;
#88737 = CARTESIAN_POINT('',(31.1,255.55,30.2213203435596)) ;
#88738 = CARTESIAN_POINT('',(31.,255.55,30.1213203435596)) ;
#88739 = CARTESIAN_POINT('Origin',(29.95,255.2,30.1213203435596)) ;
#88740 = CARTESIAN_POINT('',(29.2,255.1,30.1213203435596)) ;
#88741 = CARTESIAN_POINT('',(29.95,255.1,30.1213203435596)) ;
#88742 = CARTESIAN_POINT('',(29.1,255.2,30.2213203435596)) ;
#88743 = CARTESIAN_POINT('',(29.95,255.2,30.2213203435596)) ;
#88744 = CARTESIAN_POINT('Origin',(29.1,255.2,30.1213203435596)) ;
#88745 = CARTESIAN_POINT('Origin',(29.1,254.65,30.1213203435596)) ;
#88746 = CARTESIAN_POINT('',(29.2,254.65,30.1213203435596)) ;
#88747 = CARTESIAN_POINT('',(29.1,254.4,30.2213203435596)) ;
#88748 = CARTESIAN_POINT('',(29.1,254.65,30.2213203435596)) ;
#88749 = CARTESIAN_POINT('Origin',(29.1,254.4,30.1213203435596)) ;
#88750 = CARTESIAN_POINT('Origin',(30.55,254.4,30.1213203435596)) ;
#88751 = CARTESIAN_POINT('',(30.3,254.4,30.2213203435596)) ;
#88752 = CARTESIAN_POINT('',(30.55,254.4,30.2213203435596)) ;
#88753 = CARTESIAN_POINT('Origin',(30.3,254.4,30.1213203435596)) ;
#88754 = CARTESIAN_POINT('Origin',(30.3,254.05,30.1213203435596)) ;
#88755 = CARTESIAN_POINT('',(30.3,254.05,30.2213203435596)) ;
#88756 = CARTESIAN_POINT('Origin',(31.,255.1,30.7213203435596)) ;
#88757 = CARTESIAN_POINT('',(31.,255.1,30.7213203435596)) ;
#88758 = CARTESIAN_POINT('Origin',(31.,256.3,30.7213203435596)) ;
#88759 = CARTESIAN_POINT('',(31.,256.3,30.7213203435596)) ;
#88760 = CARTESIAN_POINT('Origin',(30.4,256.3,30.7213203435596)) ;
#88761 = CARTESIAN_POINT('',(30.4,256.3,30.7213203435596)) ;
#88762 = CARTESIAN_POINT('Origin',(30.7,254.8,30.2213203435596)) ;
#88763 = CARTESIAN_POINT('',(33.,254.8,30.2213203435596)) ;
#88764 = CARTESIAN_POINT('Origin',(30.7,254.8,30.2213203435596)) ;
#88765 = CARTESIAN_POINT('Origin',(30.7,254.8,30.0213203435596)) ;
#88766 = CARTESIAN_POINT('Origin',(33.,254.8,30.0213203435596)) ;
#88767 = CARTESIAN_POINT('Origin',(29.2,254.5,30.7213203435596)) ;
#88768 = CARTESIAN_POINT('',(29.2,255.1,30.7213203435596)) ;
#88769 = CARTESIAN_POINT('Origin',(29.2,255.1,30.7213203435596)) ;
#88770 = CARTESIAN_POINT('',(30.4,255.1,30.7213203435596)) ;
#88771 = CARTESIAN_POINT('Origin',(30.4,255.1,30.7213203435596)) ;
#88772 = CARTESIAN_POINT('',(0.,0.,0.)) ;
#88773 = CARTESIAN_POINT('Origin',(45.05,247.85,28.7713203435596)) ;
#88774 = CARTESIAN_POINT('',(45.05,247.9,28.7713203435596)) ;
#88775 = CARTESIAN_POINT('',(45.1,247.85,28.7713203435596)) ;
#88776 = CARTESIAN_POINT('Origin',(45.05,247.85,28.7713203435596)) ;
#88777 = CARTESIAN_POINT('',(45.05,247.85,28.7213203435596)) ;
#88778 = CARTESIAN_POINT('Origin',(45.05,247.85,28.7713203435596)) ;
#88779 = CARTESIAN_POINT('Origin',(45.05,247.85,28.7713203435596)) ;
#88780 = CARTESIAN_POINT('Origin',(45.05,246.91625919068,28.7713203435596)) ;
#88781 = CARTESIAN_POINT('',(45.1,246.91625919068,28.7713203435596)) ;
#88782 = CARTESIAN_POINT('',(45.05,246.886850605796,28.7308835393444)) ;
#88783 = CARTESIAN_POINT('Origin',(45.05,246.91625919068,28.7713203435596)) ;
#88784 = CARTESIAN_POINT('',(45.05,246.91625919068,28.7213203435596)) ;
#88785 = CARTESIAN_POINT('Origin',(45.05,246.91625919068,28.7713203435596)) ;
#88786 = CARTESIAN_POINT('Origin',(45.05,246.91625919068,28.7713203435596)) ;
#88787 = CARTESIAN_POINT('Origin',(45.05,247.15,28.7713203435596)) ;
#88788 = CARTESIAN_POINT('',(45.1,247.15,28.7713203435596)) ;
#88789 = CARTESIAN_POINT('',(45.05,247.15,28.7213203435596)) ;
#88790 = CARTESIAN_POINT('Origin',(35.35,247.85,28.7713203435596)) ;
#88791 = CARTESIAN_POINT('',(35.35,247.85,28.7213203435596)) ;
#88792 = CARTESIAN_POINT('',(35.3,247.85,28.7713203435596)) ;
#88793 = CARTESIAN_POINT('Origin',(35.35,247.85,28.7713203435596)) ;
#88794 = CARTESIAN_POINT('',(35.35,247.9,28.7713203435596)) ;
#88795 = CARTESIAN_POINT('Origin',(35.35,247.85,28.7713203435596)) ;
#88796 = CARTESIAN_POINT('Origin',(35.35,247.85,28.7713203435596)) ;
#88797 = CARTESIAN_POINT('Origin',(42.65,247.85,28.7713203435596)) ;
#88798 = CARTESIAN_POINT('',(42.65,247.9,28.7713203435596)) ;
#88799 = CARTESIAN_POINT('',(42.65,247.85,28.7213203435596)) ;
#88800 = CARTESIAN_POINT('Origin',(45.05,247.85,31.8713203435596)) ;
#88801 = CARTESIAN_POINT('',(45.1,247.85,31.8713203435596)) ;
#88802 = CARTESIAN_POINT('',(45.05,247.9,31.8713203435596)) ;
#88803 = CARTESIAN_POINT('Origin',(45.05,247.85,31.8713203435596)) ;
#88804 = CARTESIAN_POINT('',(45.15,247.85,31.9213203435596)) ;
#88805 = CARTESIAN_POINT('Origin',(45.15,247.85,31.8713203435596)) ;
#88806 = CARTESIAN_POINT('',(45.05,247.95,31.9213203435596)) ;
#88807 = CARTESIAN_POINT('Origin',(45.05,247.85,31.9213203435596)) ;
#88808 = CARTESIAN_POINT('Origin',(45.05,247.95,31.8713203435596)) ;
#88809 = CARTESIAN_POINT('Ctrl Pts',(45.100000736089,242.654130216336,31.8710061164266)) ;
#88810 = CARTESIAN_POINT('Ctrl Pts',(45.0999925613464,242.62245247665,31.8801399127304)) ;
#88811 = CARTESIAN_POINT('Ctrl Pts',(45.093399397134,242.569918655277,31.8953123581957)) ;
#88812 = CARTESIAN_POINT('Ctrl Pts',(45.0723245052974,242.522754591895,31.9089495529807)) ;
#88813 = CARTESIAN_POINT('Ctrl Pts',(45.0573753277667,242.51316005143,31.9117246086577)) ;
#88814 = CARTESIAN_POINT('Ctrl Pts',(45.0498683683397,242.513216942934,31.9117081537903)) ;
#88815 = CARTESIAN_POINT('Ctrl Pts',(45.0999007385685,242.654129809016,31.8860569433972)) ;
#88816 = CARTESIAN_POINT('Ctrl Pts',(45.1027420250355,242.622491185791,31.8934562217455)) ;
#88817 = CARTESIAN_POINT('Ctrl Pts',(45.0988440451183,242.5681700861,31.9044544950197)) ;
#88818 = CARTESIAN_POINT('Ctrl Pts',(45.0760540091005,242.518481086614,31.9134709137417)) ;
#88819 = CARTESIAN_POINT('Ctrl Pts',(45.0585961298263,242.508297013843,31.9152655724638)) ;
#88820 = CARTESIAN_POINT('Ctrl Pts',(45.0498465782584,242.508357399168,31.9152549299434)) ;
#88821 = CARTESIAN_POINT('Ctrl Pts',(45.1124458017577,242.654149588799,31.9121185269271)) ;
#88822 = CARTESIAN_POINT('Ctrl Pts',(45.1168400062175,242.620824309685,31.9143468692785)) ;
#88823 = CARTESIAN_POINT('Ctrl Pts',(45.1124356980016,242.56280158586,31.9172670990625)) ;
#88824 = CARTESIAN_POINT('Ctrl Pts',(45.0833001042428,242.509598931222,31.9194845333789)) ;
#88825 = CARTESIAN_POINT('Ctrl Pts',(45.0610143823453,242.498676245984,31.9198998020343)) ;
#88826 = CARTESIAN_POINT('Ctrl Pts',(45.0498034221959,242.498741010382,31.9198973387953)) ;
#88827 = CARTESIAN_POINT('Ctrl Pts',(45.138764565538,242.654190410765,31.9213206201139)) ;
#88828 = CARTESIAN_POINT('Ctrl Pts',(45.1401144780131,242.617375310913,31.9212968863911)) ;
#88829 = CARTESIAN_POINT('Ctrl Pts',(45.129606976681,242.55548089994,31.9213095444323)) ;
#88830 = CARTESIAN_POINT('Ctrl Pts',(45.091319078717,242.499569893145,31.9213068206852)) ;
#88831 = CARTESIAN_POINT('Ctrl Pts',(45.0636555557442,242.488165179893,31.9213204231679)) ;
#88832 = CARTESIAN_POINT('Ctrl Pts',(45.0497562823574,242.488232804192,31.9213203428565)) ;
#88833 = CARTESIAN_POINT('Ctrl Pts',(45.1499996370486,242.654207810581,31.9213203435596)) ;
#88834 = CARTESIAN_POINT('Ctrl Pts',(45.1500616220573,242.615905236523,31.9213203435596)) ;
#88835 = CARTESIAN_POINT('Ctrl Pts',(45.1369492436899,242.552354124405,31.9213203435596)) ;
#88836 = CARTESIAN_POINT('Ctrl Pts',(45.094751916561,242.495283622616,31.9213203435596)) ;
#88837 = CARTESIAN_POINT('Ctrl Pts',(45.0647843437491,242.483672564324,31.9213203435596)) ;
#88838 = CARTESIAN_POINT('Ctrl Pts',(45.049736135378,242.483741412881,31.9213203435596)) ;
#88839 = CARTESIAN_POINT('',(45.05,242.48374080932,31.9213203435596)) ;
#88840 = CARTESIAN_POINT('',(45.15,242.653759190679,31.9213203435596)) ;
#88841 = CARTESIAN_POINT('Origin',(45.05,242.653759190679,31.9213203435596)) ;
#88842 = CARTESIAN_POINT('',(45.1,242.653759190679,31.8713203435596)) ;
#88843 = CARTESIAN_POINT('Origin',(45.15,242.653759190679,31.8713203435596)) ;
#88844 = CARTESIAN_POINT('',(45.05,242.513149394204,31.9117571477748)) ;
#88845 = CARTESIAN_POINT('Origin',(45.05,242.653759190679,31.8713203435596)) ;
#88846 = CARTESIAN_POINT('Origin',(45.05,242.48374080932,31.8713203435596)) ;
#88847 = CARTESIAN_POINT('Origin',(45.15,246.025,31.8713203435596)) ;
#88848 = CARTESIAN_POINT('',(45.15,246.025,31.9213203435596)) ;
#88849 = CARTESIAN_POINT('',(45.1,246.025,31.8713203435596)) ;
#88850 = CARTESIAN_POINT('Origin',(45.05,245.187246422722,30.0287841748018)) ;
#88851 = CARTESIAN_POINT('',(45.05,245.157837837838,29.9883473705867)) ;
#88852 = CARTESIAN_POINT('',(45.1,245.187246422722,30.0287841748018)) ;
#88853 = CARTESIAN_POINT('Origin',(35.35,246.91625919068,28.7713203435596)) ;
#88854 = CARTESIAN_POINT('',(35.35,246.886850605796,28.7308835393445)) ;
#88855 = CARTESIAN_POINT('',(35.3,246.91625919068,28.7713203435596)) ;
#88856 = CARTESIAN_POINT('Origin',(35.35,246.91625919068,28.7713203435596)) ;
#88857 = CARTESIAN_POINT('',(35.35,246.91625919068,28.7213203435596)) ;
#88858 = CARTESIAN_POINT('Origin',(35.35,246.91625919068,28.7713203435596)) ;
#88859 = CARTESIAN_POINT('Origin',(35.35,246.91625919068,28.7713203435596)) ;
#88860 = CARTESIAN_POINT('Origin',(38.975,246.91625919068,28.7713203435596)) ;
#88861 = CARTESIAN_POINT('',(38.975,246.91625919068,28.7213203435596)) ;
#88862 = CARTESIAN_POINT('',(38.975,246.886850605796,28.7308835393445)) ;
#88863 = CARTESIAN_POINT('Origin',(35.35,247.65,28.7713203435596)) ;
#88864 = CARTESIAN_POINT('',(35.3,247.65,28.7713203435596)) ;
#88865 = CARTESIAN_POINT('',(35.35,247.65,28.7213203435596)) ;
#88866 = CARTESIAN_POINT('Origin',(35.35,247.85,31.8713203435596)) ;
#88867 = CARTESIAN_POINT('',(35.35,247.95,31.9213203435596)) ;
#88868 = CARTESIAN_POINT('',(35.25,247.85,31.9213203435596)) ;
#88869 = CARTESIAN_POINT('Origin',(35.35,247.85,31.9213203435596)) ;
#88870 = CARTESIAN_POINT('',(35.3,247.85,31.8713203435596)) ;
#88871 = CARTESIAN_POINT('Origin',(35.25,247.85,31.8713203435596)) ;
#88872 = CARTESIAN_POINT('',(35.35,247.9,31.8713203435596)) ;
#88873 = CARTESIAN_POINT('Origin',(35.35,247.85,31.8713203435596)) ;
#88874 = CARTESIAN_POINT('Origin',(35.35,247.95,31.8713203435596)) ;
#88875 = CARTESIAN_POINT('Ctrl Pts',(35.3502565731995,242.513282235284,31.9116610526359)) ;
#88876 = CARTESIAN_POINT('Ctrl Pts',(35.3390013657597,242.513112238919,31.9117105145564)) ;
#88877 = CARTESIAN_POINT('Ctrl Pts',(35.3126883604354,242.538810184974,31.9042333955065)) ;
#88878 = CARTESIAN_POINT('Ctrl Pts',(35.3000170639085,242.612165533139,31.8829377134629)) ;
#88879 = CARTESIAN_POINT('Ctrl Pts',(35.299997199836,242.654484026663,31.8707059635828)) ;
#88880 = CARTESIAN_POINT('Ctrl Pts',(35.3502992712021,242.508407184294,31.9152313508883)) ;
#88881 = CARTESIAN_POINT('Ctrl Pts',(35.3371713310074,242.508226354371,31.9152624722717)) ;
#88882 = CARTESIAN_POINT('Ctrl Pts',(35.3063767609757,242.535564204124,31.9105601570622)) ;
#88883 = CARTESIAN_POINT('Ctrl Pts',(35.2963540554806,242.612239454015,31.8957701050313)) ;
#88884 = CARTESIAN_POINT('Ctrl Pts',(35.3001940210199,242.654482933999,31.8858430843487)) ;
#88885 = CARTESIAN_POINT('Ctrl Pts',(35.3503840040175,242.498741118317,31.9199072049728)) ;
#88886 = CARTESIAN_POINT('Ctrl Pts',(35.3335389864695,242.498547467106,31.9199143760934)) ;
#88887 = CARTESIAN_POINT('Ctrl Pts',(35.2940728826173,242.527823493039,31.9188313538683)) ;
#88888 = CARTESIAN_POINT('Ctrl Pts',(35.2816723512703,242.610023632475,31.9151151694671)) ;
#88889 = CARTESIAN_POINT('Ctrl Pts',(35.287633530646,242.654521639855,31.9121464449948)) ;
#88890 = CARTESIAN_POINT('Ctrl Pts',(35.3504766155513,242.488173521915,31.921328574714)) ;
#88891 = CARTESIAN_POINT('Ctrl Pts',(35.3295687857424,242.487971244137,31.9213286024899)) ;
#88892 = CARTESIAN_POINT('Ctrl Pts',(35.2806653372481,242.518549809002,31.9213243830799)) ;
#88893 = CARTESIAN_POINT('Ctrl Pts',(35.2592374640768,242.605399085081,31.9213249653989)) ;
#88894 = CARTESIAN_POINT('Ctrl Pts',(35.2610978069887,242.654602031267,31.9213742951207)) ;
#88895 = CARTESIAN_POINT('Ctrl Pts',(35.3505162409945,242.483651681807,31.921320259465)) ;
#88896 = CARTESIAN_POINT('Ctrl Pts',(35.3278700899377,242.483445705528,31.9213202584698)) ;
#88897 = CARTESIAN_POINT('Ctrl Pts',(35.2749216409559,242.514582707583,31.92132040927)) ;
#88898 = CARTESIAN_POINT('Ctrl Pts',(35.2496412591386,242.603428347186,31.9213206187124)) ;
#88899 = CARTESIAN_POINT('Ctrl Pts',(35.2497723113216,242.654636290699,31.921319786846)) ;
#88900 = CARTESIAN_POINT('',(35.25,242.653759190679,31.9213203435596)) ;
#88901 = CARTESIAN_POINT('',(35.35,242.48374080932,31.9213203435596)) ;
#88902 = CARTESIAN_POINT('Origin',(35.35,242.65375919068,31.9213203435596)) ;
#88903 = CARTESIAN_POINT('',(35.35,242.513149394204,31.9117571477748)) ;
#88904 = CARTESIAN_POINT('Origin',(35.35,242.48374080932,31.8713203435596)) ;
#88905 = CARTESIAN_POINT('',(35.3,242.653759190679,31.8713203435596)) ;
#88906 = CARTESIAN_POINT('Origin',(35.35,242.65375919068,31.8713203435596)) ;
#88907 = CARTESIAN_POINT('Origin',(35.25,242.653759190679,31.8713203435596)) ;
#88908 = CARTESIAN_POINT('Origin',(35.25,246.525,31.8713203435596)) ;
#88909 = CARTESIAN_POINT('',(35.25,246.525,31.9213203435596)) ;
#88910 = CARTESIAN_POINT('',(35.3,246.525,31.8713203435596)) ;
#88911 = CARTESIAN_POINT('Origin',(38.975,242.48374080932,31.8713203435596)) ;
#88912 = CARTESIAN_POINT('',(38.975,242.513149394204,31.9117571477748)) ;
#88913 = CARTESIAN_POINT('',(38.975,242.48374080932,31.9213203435596)) ;
#88914 = CARTESIAN_POINT('Origin',(35.35,245.514273449749,29.790946336964)) ;
#88915 = CARTESIAN_POINT('',(35.35,245.484864864865,29.7505095327488)) ;
#88916 = CARTESIAN_POINT('',(35.3,245.514273449749,29.790946336964)) ;
#88917 = CARTESIAN_POINT('Origin',(35.35,247.85,31.4213203435596)) ;
#88918 = CARTESIAN_POINT('',(35.3,247.85,31.4213203435596)) ;
#88919 = CARTESIAN_POINT('',(35.35,247.9,31.4213203435596)) ;
#88920 = CARTESIAN_POINT('Origin',(42.65,247.95,31.8713203435596)) ;
#88921 = CARTESIAN_POINT('',(42.65,247.95,31.9213203435596)) ;
#88922 = CARTESIAN_POINT('',(42.65,247.9,31.8713203435596)) ;
#88923 = CARTESIAN_POINT('Origin',(45.05,247.85,31.4213203435596)) ;
#88924 = CARTESIAN_POINT('',(45.05,247.9,31.4213203435596)) ;
#88925 = CARTESIAN_POINT('',(45.1,247.85,31.4213203435596)) ;
#88926 = CARTESIAN_POINT('Origin',(40.2,247.4,28.7213203435596)) ;
#88927 = CARTESIAN_POINT('Origin',(45.1,247.9,31.4213203435596)) ;
#88928 = CARTESIAN_POINT('Origin',(45.1,246.9,31.4213203435596)) ;
#88929 = CARTESIAN_POINT('Origin',(37.75,244.7,30.3213203435596)) ;
#88930 = CARTESIAN_POINT('Origin',(35.3,247.9,31.4213203435596)) ;
#88931 = CARTESIAN_POINT('Origin',(34.35,248.85,31.8713203435596)) ;
#88932 = CARTESIAN_POINT('',(34.3,248.85,31.8713203435596)) ;
#88933 = CARTESIAN_POINT('',(34.35,248.9,31.8713203435596)) ;
#88934 = CARTESIAN_POINT('Origin',(34.35,248.85,31.8713203435596)) ;
#88935 = CARTESIAN_POINT('',(34.35,248.85,31.9213203435596)) ;
#88936 = CARTESIAN_POINT('Origin',(34.35,248.85,31.8713203435596)) ;
#88937 = CARTESIAN_POINT('Origin',(34.35,248.85,31.8713203435596)) ;
#88938 = CARTESIAN_POINT('Origin',(46.05,248.85,31.8713203435596)) ;
#88939 = CARTESIAN_POINT('',(46.05,248.9,31.8713203435596)) ;
#88940 = CARTESIAN_POINT('',(46.1,248.85,31.8713203435596)) ;
#88941 = CARTESIAN_POINT('Origin',(46.05,248.85,31.8713203435596)) ;
#88942 = CARTESIAN_POINT('',(46.05,248.85,31.9213203435596)) ;
#88943 = CARTESIAN_POINT('Origin',(46.05,248.85,31.8713203435596)) ;
#88944 = CARTESIAN_POINT('Origin',(46.05,248.85,31.8713203435596)) ;
#88945 = CARTESIAN_POINT('Origin',(37.25,248.85,31.8713203435596)) ;
#88946 = CARTESIAN_POINT('',(37.25,248.9,31.8713203435596)) ;
#88947 = CARTESIAN_POINT('',(37.25,248.85,31.9213203435596)) ;
#88948 = CARTESIAN_POINT('Origin',(34.35,243.275,31.8713203435596)) ;
#88949 = CARTESIAN_POINT('',(34.35,241.578968906908,31.9213203435596)) ;
#88950 = CARTESIAN_POINT('',(34.35,243.275,31.9213203435596)) ;
#88951 = CARTESIAN_POINT('',(34.3,241.528968906908,31.8713203435596)) ;
#88952 = CARTESIAN_POINT('',(34.3,243.275,31.8713203435596)) ;
#88953 = CARTESIAN_POINT('Origin',(34.35,241.578968906908,31.8713203435596)) ;
#88954 = CARTESIAN_POINT('Origin',(46.05,241.578968906908,31.8713203435596)) ;
#88955 = CARTESIAN_POINT('',(46.1,241.578968906908,31.8713203435596)) ;
#88956 = CARTESIAN_POINT('',(46.05,241.553053821103,31.8285604519819)) ;
#88957 = CARTESIAN_POINT('Origin',(46.05,241.578968906908,31.8713203435596)) ;
#88958 = CARTESIAN_POINT('',(46.05,241.578968906908,31.9213203435596)) ;
#88959 = CARTESIAN_POINT('Origin',(46.05,241.578968906908,31.8713203435596)) ;
#88960 = CARTESIAN_POINT('Origin',(46.05,241.578968906908,31.8713203435596)) ;
#88961 = CARTESIAN_POINT('Origin',(46.05,247.025,31.8713203435596)) ;
#88962 = CARTESIAN_POINT('',(46.1,247.025,31.8713203435596)) ;
#88963 = CARTESIAN_POINT('',(46.05,247.025,31.9213203435596)) ;
#88964 = CARTESIAN_POINT('Origin',(41.675,241.578968906908,31.8713203435596)) ;
#88965 = CARTESIAN_POINT('',(34.3,241.553053821103,31.8285604519819)) ;
#88966 = CARTESIAN_POINT('',(41.675,241.553053821103,31.8285604519819)) ;
#88967 = CARTESIAN_POINT('',(41.675,241.578968906908,31.9213203435596)) ;
#88968 = CARTESIAN_POINT('Origin',(34.3,241.578968906908,31.8713203435596)) ;
#88969 = CARTESIAN_POINT('Origin',(46.05,245.81852757741,29.3018908462858)) ;
#88970 = CARTESIAN_POINT('',(46.05,248.,27.9213203435596)) ;
#88971 = CARTESIAN_POINT('',(46.1,248.096468906908,27.9213203435596)) ;
#88972 = CARTESIAN_POINT('Origin',(46.05,248.096468906908,27.9213203435596)) ;
#88973 = CARTESIAN_POINT('',(46.1,245.81852757741,29.3018908462858)) ;
#88974 = CARTESIAN_POINT('',(46.05,245.792612491605,29.2591309547081)) ;
#88975 = CARTESIAN_POINT('Origin',(46.05,248.85,31.9213203435596)) ;
#88976 = CARTESIAN_POINT('',(46.1,248.85,27.9213203435596)) ;
#88977 = CARTESIAN_POINT('',(46.05,248.9,27.9213203435596)) ;
#88978 = CARTESIAN_POINT('Origin',(46.05,248.85,27.9213203435596)) ;
#88979 = CARTESIAN_POINT('',(46.05,248.9,31.9213203435596)) ;
#88980 = CARTESIAN_POINT('',(46.1,248.85,31.9213203435596)) ;
#88981 = CARTESIAN_POINT('Origin',(34.35,248.85,31.9213203435596)) ;
#88982 = CARTESIAN_POINT('',(34.35,248.9,27.9213203435596)) ;
#88983 = CARTESIAN_POINT('',(34.3,248.85,27.9213203435596)) ;
#88984 = CARTESIAN_POINT('Origin',(34.35,248.85,27.9213203435596)) ;
#88985 = CARTESIAN_POINT('',(34.3,248.85,31.9213203435596)) ;
#88986 = CARTESIAN_POINT('',(34.35,248.9,31.9213203435596)) ;
#88987 = CARTESIAN_POINT('Origin',(46.1,248.9,31.9213203435596)) ;
#88988 = CARTESIAN_POINT('',(46.1,248.9,27.9213203435596)) ;
#88989 = CARTESIAN_POINT('Origin',(40.2,245.15,27.9213203435596)) ;
#88990 = CARTESIAN_POINT('',(34.3,248.,27.9213203435596)) ;
#88991 = CARTESIAN_POINT('',(43.15,248.,27.9213203435596)) ;
#88992 = CARTESIAN_POINT('',(34.3,241.4,27.9213203435596)) ;
#88993 = CARTESIAN_POINT('',(34.3,248.9,27.9213203435596)) ;
#88994 = CARTESIAN_POINT('Origin',(43.15,244.7,29.9213203435596)) ;
#88995 = CARTESIAN_POINT('',(34.3,243.05,30.9213203435596)) ;
#88996 = CARTESIAN_POINT('Origin',(40.2,245.15,31.9213203435596)) ;
#88997 = CARTESIAN_POINT('Origin',(34.3,241.4,31.9213203435596)) ;
#88998 = CARTESIAN_POINT('Origin',(34.3,248.9,31.9213203435596)) ;
#88999 = CARTESIAN_POINT('',(0.,0.,0.)) ;
#89000 = CARTESIAN_POINT('Ctrl Pts',(55.5095145719656,261.79455482774,20.2277364888237)) ;
#89001 = CARTESIAN_POINT('Ctrl Pts',(55.5235850209285,261.795524155342,20.2176307773862)) ;
#89002 = CARTESIAN_POINT('Ctrl Pts',(55.5532287114159,261.797064527402,20.1984257565318)) ;
#89003 = CARTESIAN_POINT('Ctrl Pts',(55.6031763483208,261.798222507439,20.1723029608032)) ;
#89004 = CARTESIAN_POINT('Ctrl Pts',(55.6599047282381,261.79814256388,20.1486416834275)) ;
#89005 = CARTESIAN_POINT('Ctrl Pts',(55.7252078119995,261.796555096217,20.1272203634637)) ;
#89006 = CARTESIAN_POINT('Ctrl Pts',(55.8010086453308,261.793278462298,20.1080994112902)) ;
#89007 = CARTESIAN_POINT('Ctrl Pts',(55.8886521902875,261.788562905801,20.0918367827122)) ;
#89008 = CARTESIAN_POINT('Ctrl Pts',(55.9864294144668,261.783244910011,20.0795560745166)) ;
#89009 = CARTESIAN_POINT('Ctrl Pts',(56.0870864420511,261.778692438248,20.0723692404909)) ;
#89010 = CARTESIAN_POINT('Ctrl Pts',(56.1809390611363,261.776355954665,20.0702679342639)) ;
#89011 = CARTESIAN_POINT('Ctrl Pts',(56.2391336395509,261.776281941501,20.0706687254062)) ;
#89012 = CARTESIAN_POINT('Ctrl Pts',(56.2695111541429,261.776281941501,20.0706687254062)) ;
#89013 = CARTESIAN_POINT('Ctrl Pts',(55.5318704226011,261.835587804427,20.2336372451564)) ;
#89014 = CARTESIAN_POINT('Ctrl Pts',(55.5459583366965,261.834973203121,20.2238071455774)) ;
#89015 = CARTESIAN_POINT('Ctrl Pts',(55.5756021232183,261.833526932472,20.2050383428634)) ;
#89016 = CARTESIAN_POINT('Ctrl Pts',(55.6253962312584,261.83064540612,20.1793520028903)) ;
#89017 = CARTESIAN_POINT('Ctrl Pts',(55.6817877740942,261.826937340059,20.1560071692871)) ;
#89018 = CARTESIAN_POINT('Ctrl Pts',(55.7465198445918,261.822171831918,20.1348521511824)) ;
#89019 = CARTESIAN_POINT('Ctrl Pts',(55.8213429131526,261.816334347102,20.116044324121)) ;
#89020 = CARTESIAN_POINT('Ctrl Pts',(55.9069737675768,261.809885023379,20.1002538676655)) ;
#89021 = CARTESIAN_POINT('Ctrl Pts',(56.0006863128197,261.803760509541,20.0886458821796)) ;
#89022 = CARTESIAN_POINT('Ctrl Pts',(56.0954683537023,261.799281373801,20.0821480955844)) ;
#89023 = CARTESIAN_POINT('Ctrl Pts',(56.1840401677701,261.79765282798,20.0805472862567)) ;
#89024 = CARTESIAN_POINT('Ctrl Pts',(56.2401954718791,261.798341867179,20.0812712738205)) ;
#89025 = CARTESIAN_POINT('Ctrl Pts',(56.2695111541429,261.798715764224,20.0814509780309)) ;
#89026 = CARTESIAN_POINT('Ctrl Pts',(55.5809822967928,261.905784092892,20.2463148514966)) ;
#89027 = CARTESIAN_POINT('Ctrl Pts',(55.595241405465,261.902637928269,20.236906103947)) ;
#89028 = CARTESIAN_POINT('Ctrl Pts',(55.6251695278679,261.896295106137,20.2188443093641)) ;
#89029 = CARTESIAN_POINT('Ctrl Pts',(55.6752360499304,261.886680755071,20.1939945267448)) ;
#89030 = CARTESIAN_POINT('Ctrl Pts',(55.7317648353249,261.877030049387,20.1714245134235)) ;
#89031 = CARTESIAN_POINT('Ctrl Pts',(55.7963490542379,261.867339871692,20.151107208204)) ;
#89032 = CARTESIAN_POINT('Ctrl Pts',(55.869636711629,261.857869603308,20.1333948641784)) ;
#89033 = CARTESIAN_POINT('Ctrl Pts',(55.9501532362832,261.849298162689,20.1191525070167)) ;
#89034 = CARTESIAN_POINT('Ctrl Pts',(56.0337736489394,261.842781264602,20.1094881093263)) ;
#89035 = CARTESIAN_POINT('Ctrl Pts',(56.1152086370634,261.839299967236,20.1047811880335)) ;
#89036 = CARTESIAN_POINT('Ctrl Pts',(56.1919043895799,261.839370541405,20.1044512199224)) ;
#89037 = CARTESIAN_POINT('Ctrl Pts',(56.2427773792535,261.841154112132,20.1058420373569)) ;
#89038 = CARTESIAN_POINT('Ctrl Pts',(56.2695111541429,261.841969944151,20.1063719286696)) ;
#89039 = CARTESIAN_POINT('Ctrl Pts',(55.7142947487837,261.996615667805,20.2848817332965)) ;
#89040 = CARTESIAN_POINT('Ctrl Pts',(55.727431023685,261.989690475884,20.2750630800784)) ;
#89041 = CARTESIAN_POINT('Ctrl Pts',(55.7551316099311,261.976322682396,20.256254734585)) ;
#89042 = CARTESIAN_POINT('Ctrl Pts',(55.801119679589,261.957993605918,20.2308429035396)) ;
#89043 = CARTESIAN_POINT('Ctrl Pts',(55.8516376794038,261.941560611499,20.208427342522)) ;
#89044 = CARTESIAN_POINT('Ctrl Pts',(55.9066495299668,261.92699687125,20.1889543815959)) ;
#89045 = CARTESIAN_POINT('Ctrl Pts',(55.9650620575114,261.914742356923,20.1729029806023)) ;
#89046 = CARTESIAN_POINT('Ctrl Pts',(56.0249859995935,261.905548305835,20.1610377158358)) ;
#89047 = CARTESIAN_POINT('Ctrl Pts',(56.0846095008272,261.899969669763,20.1538028301126)) ;
#89048 = CARTESIAN_POINT('Ctrl Pts',(56.1437294140665,261.897823268871,20.1507219087426)) ;
#89049 = CARTESIAN_POINT('Ctrl Pts',(56.2045341748838,261.898451408471,20.1509202634277)) ;
#89050 = CARTESIAN_POINT('Ctrl Pts',(56.2477208775326,261.899867602781,20.1523151226862)) ;
#89051 = CARTESIAN_POINT('Ctrl Pts',(56.2695111541429,261.900567313948,20.1529909710202)) ;
#89052 = CARTESIAN_POINT('Ctrl Pts',(55.8167520150608,262.046133815589,20.3289876130455)) ;
#89053 = CARTESIAN_POINT('Ctrl Pts',(55.8272233753503,262.037515709941,20.3182149809853)) ;
#89054 = CARTESIAN_POINT('Ctrl Pts',(55.8493213988809,262.02109949769,20.2976947156725)) ;
#89055 = CARTESIAN_POINT('Ctrl Pts',(55.885680659634,261.999411922698,20.2705852469321)) ;
#89056 = CARTESIAN_POINT('Ctrl Pts',(55.9253732866277,261.980738298363,20.2472432165129)) ;
#89057 = CARTESIAN_POINT('Ctrl Pts',(55.9686042187112,261.964920001218,20.2274703450816)) ;
#89058 = CARTESIAN_POINT('Ctrl Pts',(56.0147532633608,261.952242450621,20.2116234068352)) ;
#89059 = CARTESIAN_POINT('Ctrl Pts',(56.062891123676,261.943048307455,20.2001307278784)) ;
#89060 = CARTESIAN_POINT('Ctrl Pts',(56.1123369473664,261.937285799675,20.1929275931536)) ;
#89061 = CARTESIAN_POINT('Ctrl Pts',(56.1631175051399,261.934403034741,20.1893241369859)) ;
#89062 = CARTESIAN_POINT('Ctrl Pts',(56.2154844879084,261.933798091816,20.1885679583302)) ;
#89063 = CARTESIAN_POINT('Ctrl Pts',(56.2514427323094,261.934313905503,20.1892127254389)) ;
#89064 = CARTESIAN_POINT('Ctrl Pts',(56.2695111541429,261.934573054282,20.1895366614117)) ;
#89065 = CARTESIAN_POINT('Ctrl Pts',(55.8638558727399,262.066371572297,20.3542848089307)) ;
#89066 = CARTESIAN_POINT('Ctrl Pts',(55.872989551448,262.057390488197,20.343058453806)) ;
#89067 = CARTESIAN_POINT('Ctrl Pts',(55.8924334380602,262.040313031316,20.321711632704)) ;
#89068 = CARTESIAN_POINT('Ctrl Pts',(55.9246856684865,262.017918820106,20.2937188686917)) ;
#89069 = CARTESIAN_POINT('Ctrl Pts',(55.960120463602,261.998755165223,20.2697643000883)) ;
#89070 = CARTESIAN_POINT('Ctrl Pts',(55.9988335935537,261.982652502899,20.2496359721834)) ;
#89071 = CARTESIAN_POINT('Ctrl Pts',(56.0401450285716,261.969868594253,20.2336560863755)) ;
#89072 = CARTESIAN_POINT('Ctrl Pts',(56.0832318051021,261.960620595462,20.222096087887)) ;
#89073 = CARTESIAN_POINT('Ctrl Pts',(56.1276386228793,261.954662126184,20.2146480012896)) ;
#89074 = CARTESIAN_POINT('Ctrl Pts',(56.1734770209332,261.951373074562,20.2105366867623)) ;
#89075 = CARTESIAN_POINT('Ctrl Pts',(56.2208605753121,261.950134902533,20.2089889717264)) ;
#89076 = CARTESIAN_POINT('Ctrl Pts',(56.2532834268155,261.950121980978,20.2089728197824)) ;
#89077 = CARTESIAN_POINT('Ctrl Pts',(56.2695111541429,261.950121980978,20.2089728197824)) ;
#89078 = CARTESIAN_POINT('',(55.5095145719656,261.79455482774,20.2277364888237)) ;
#89079 = CARTESIAN_POINT('',(56.2695111541429,261.776281941501,20.0706687254062)) ;
#89080 = CARTESIAN_POINT('Ctrl Pts',(55.5095145719656,261.79455482774,20.2277364888237)) ;
#89081 = CARTESIAN_POINT('Ctrl Pts',(55.5235850209285,261.795524155342,20.2176307773862)) ;
#89082 = CARTESIAN_POINT('Ctrl Pts',(55.5532287114159,261.797064527402,20.1984257565318)) ;
#89083 = CARTESIAN_POINT('Ctrl Pts',(55.6031763483208,261.79822250744,20.1723029608032)) ;
#89084 = CARTESIAN_POINT('Ctrl Pts',(55.6599047282381,261.79814256388,20.1486416834275)) ;
#89085 = CARTESIAN_POINT('Ctrl Pts',(55.7252078119995,261.796555096218,20.1272203634636)) ;
#89086 = CARTESIAN_POINT('Ctrl Pts',(55.8010086453309,261.793278462297,20.1080994112902)) ;
#89087 = CARTESIAN_POINT('Ctrl Pts',(55.8886521902874,261.788562905802,20.0918367827122)) ;
#89088 = CARTESIAN_POINT('Ctrl Pts',(55.9864294144668,261.78324491001,20.0795560745165)) ;
#89089 = CARTESIAN_POINT('Ctrl Pts',(56.0870864420511,261.778692438249,20.0723692404909)) ;
#89090 = CARTESIAN_POINT('Ctrl Pts',(56.1809390611364,261.776355954664,20.0702679342639)) ;
#89091 = CARTESIAN_POINT('Ctrl Pts',(56.2391336395509,261.776281941501,20.0706687254062)) ;
#89092 = CARTESIAN_POINT('Ctrl Pts',(56.2695111541429,261.776281941501,20.0706687254062)) ;
#89093 = CARTESIAN_POINT('',(55.8638558727399,262.066371572297,20.3542848089307)) ;
#89094 = CARTESIAN_POINT('Ctrl Pts',(55.5095145719656,261.79455482774,20.2277364888237)) ;
#89095 = CARTESIAN_POINT('Ctrl Pts',(55.5318704226011,261.835587804427,20.2336372451564)) ;
#89096 = CARTESIAN_POINT('Ctrl Pts',(55.5809822967928,261.905784092892,20.2463148514966)) ;
#89097 = CARTESIAN_POINT('Ctrl Pts',(55.7142947487837,261.996615667805,20.2848817332965)) ;
#89098 = CARTESIAN_POINT('Ctrl Pts',(55.8167520150608,262.046133815589,20.3289876130455)) ;
#89099 = CARTESIAN_POINT('Ctrl Pts',(55.8638558727399,262.066371572297,20.3542848089307)) ;
#89100 = CARTESIAN_POINT('',(56.2695111541429,261.950121980978,20.2089728197824)) ;
#89101 = CARTESIAN_POINT('Ctrl Pts',(55.8638558727399,262.066371572297,20.3542848089307)) ;
#89102 = CARTESIAN_POINT('Ctrl Pts',(55.8713330463535,262.05901931838,20.345094491535)) ;
#89103 = CARTESIAN_POINT('Ctrl Pts',(55.8792039017644,262.051963652932,20.336274909725)) ;
#89104 = CARTESIAN_POINT('Ctrl Pts',(55.8874289902313,262.045256409105,20.3278908549412)) ;
#89105 = CARTESIAN_POINT('Ctrl Pts',(55.8892510844872,262.043770561203,20.3260335450625)) ;
#89106 = CARTESIAN_POINT('Ctrl Pts',(55.8910908387747,262.04230150103,20.3241972198463)) ;
#89107 = CARTESIAN_POINT('Ctrl Pts',(55.8929476782012,262.040849955509,20.3223827879453)) ;
#89108 = CARTESIAN_POINT('Ctrl Pts',(55.8986519339602,262.036390772459,20.3168088091333)) ;
#89109 = CARTESIAN_POINT('Ctrl Pts',(55.9045175213531,262.0320969714,20.3114415578101)) ;
#89110 = CARTESIAN_POINT('Ctrl Pts',(55.9105424868196,262.027972712684,20.3062862344144)) ;
#89111 = CARTESIAN_POINT('Ctrl Pts',(55.9153320522155,262.024694120144,20.3021879937394)) ;
#89112 = CARTESIAN_POINT('Ctrl Pts',(55.920221933305,262.021522772665,20.2982238093905)) ;
#89113 = CARTESIAN_POINT('Ctrl Pts',(55.9252155779456,262.018456999749,20.2943915932464)) ;
#89114 = CARTESIAN_POINT('Ctrl Pts',(55.9321214893699,262.014217219444,20.2890918678644)) ;
#89115 = CARTESIAN_POINT('Ctrl Pts',(55.9392257846889,262.010179296389,20.2840444640455)) ;
#89116 = CARTESIAN_POINT('Ctrl Pts',(55.9465389364433,262.006333296846,20.2792369646175)) ;
#89117 = CARTESIAN_POINT('Ctrl Pts',(55.9511666186691,262.003899590515,20.2761948317038)) ;
#89118 = CARTESIAN_POINT('Ctrl Pts',(55.9558757446086,262.001543949715,20.2732502807027)) ;
#89119 = CARTESIAN_POINT('Ctrl Pts',(55.9606665897011,261.99926519383,20.2704018358466)) ;
#89120 = CARTESIAN_POINT('Ctrl Pts',(55.9656406070482,261.996899312428,20.2674444840949)) ;
#89121 = CARTESIAN_POINT('Ctrl Pts',(55.9707027113969,261.994616308741,20.2645907294863)) ;
#89122 = CARTESIAN_POINT('Ctrl Pts',(55.9758446315117,261.992419381877,20.2618445709062)) ;
#89123 = CARTESIAN_POINT('Ctrl Pts',(55.9834806996654,261.989156810136,20.2577663562296)) ;
#89124 = CARTESIAN_POINT('Ctrl Pts',(55.9912961311385,261.986082334998,20.253923262308)) ;
#89125 = CARTESIAN_POINT('Ctrl Pts',(55.9992662548239,261.983205399202,20.2503270925619)) ;
#89126 = CARTESIAN_POINT('Ctrl Pts',(56.0062869640403,261.980671168811,20.2471593045731)) ;
#89127 = CARTESIAN_POINT('Ctrl Pts',(56.0134277031511,261.978290217307,20.244183115193)) ;
#89128 = CARTESIAN_POINT('Ctrl Pts',(56.0206680705166,261.976067940801,20.2414052695604)) ;
#89129 = CARTESIAN_POINT('Ctrl Pts',(56.0271821933992,261.974068569566,20.2389060555169)) ;
#89130 = CARTESIAN_POINT('Ctrl Pts',(56.0337779379306,261.972197164793,20.2365667995501)) ;
#89131 = CARTESIAN_POINT('Ctrl Pts',(56.0404403335848,261.970457505536,20.23439222548)) ;
#89132 = CARTESIAN_POINT('Ctrl Pts',(56.0445887481694,261.969374287395,20.2330382028047)) ;
#89133 = CARTESIAN_POINT('Ctrl Pts',(56.0487630052482,261.96834214749,20.2317480279244)) ;
#89134 = CARTESIAN_POINT('Ctrl Pts',(56.0529610797319,261.967360010175,20.2305203562874)) ;
#89135 = CARTESIAN_POINT('Ctrl Pts',(56.0629996414285,261.965011493953,20.2275847110245)) ;
#89136 = CARTESIAN_POINT('Ctrl Pts',(56.0731702750401,261.962953857029,20.2250126648544)) ;
#89137 = CARTESIAN_POINT('Ctrl Pts',(56.083450668956,261.961167864353,20.2227801740048)) ;
#89138 = CARTESIAN_POINT('Ctrl Pts',(56.0834769606655,261.961163296746,20.2227744644958)) ;
#89139 = CARTESIAN_POINT('Ctrl Pts',(56.0835032530946,261.961158730916,20.2227687572091)) ;
#89140 = CARTESIAN_POINT('Ctrl Pts',(56.0835295462434,261.961154166864,20.2227630521437)) ;
#89141 = CARTESIAN_POINT('Ctrl Pts',(56.0980833454394,261.958627869948,20.2196051809913)) ;
#89142 = CARTESIAN_POINT('Ctrl Pts',(56.1128624571979,261.956645585289,20.2171273251705)) ;
#89143 = CARTESIAN_POINT('Ctrl Pts',(56.1278768193434,261.955106576005,20.215203563567)) ;
#89144 = CARTESIAN_POINT('Ctrl Pts',(56.1299108979432,261.954898077914,20.2149429409531)) ;
#89145 = CARTESIAN_POINT('Ctrl Pts',(56.1319492921022,261.954697711593,20.2146924830527)) ;
#89146 = CARTESIAN_POINT('Ctrl Pts',(56.1339920253113,261.954505223791,20.2144518733006)) ;
#89147 = CARTESIAN_POINT('Ctrl Pts',(56.1470546902204,261.953274322151,20.2129132462534)) ;
#89148 = CARTESIAN_POINT('Ctrl Pts',(56.1602993589054,261.952367232026,20.2117793835923)) ;
#89149 = CARTESIAN_POINT('Ctrl Pts',(56.1737344620585,261.951714748922,20.2109637797128)) ;
#89150 = CARTESIAN_POINT('Ctrl Pts',(56.1744674056311,261.951679153118,20.210919284958)) ;
#89151 = CARTESIAN_POINT('Ctrl Pts',(56.1752009165622,261.951644315065,20.210875737391)) ;
#89152 = CARTESIAN_POINT('Ctrl Pts',(56.1759349892867,261.951610219791,20.210833118299)) ;
#89153 = CARTESIAN_POINT('Ctrl Pts',(56.1882999108463,261.951035909686,20.2101152306677)) ;
#89154 = CARTESIAN_POINT('Ctrl Pts',(56.2008266725393,261.950673148754,20.2096617795031)) ;
#89155 = CARTESIAN_POINT('Ctrl Pts',(56.2134912420145,261.950453035381,20.2093866377862)) ;
#89156 = CARTESIAN_POINT('Ctrl Pts',(56.2160120270313,261.950409223509,20.2093318729464)) ;
#89157 = CARTESIAN_POINT('Ctrl Pts',(56.218537945353,261.950370958144,20.2092840412407)) ;
#89158 = CARTESIAN_POINT('Ctrl Pts',(56.221068929131,261.950337727748,20.2092425032449)) ;
#89159 = CARTESIAN_POINT('Ctrl Pts',(56.2299314802775,261.950221367424,20.2090970528413)) ;
#89160 = CARTESIAN_POINT('Ctrl Pts',(56.2388562189851,261.95016674229,20.2090287714307)) ;
#89161 = CARTESIAN_POINT('Ctrl Pts',(56.2478153214656,261.950142093806,20.2089979608233)) ;
#89162 = CARTESIAN_POINT('Ctrl Pts',(56.2550320831194,261.950122238889,20.2089731421754)) ;
#89163 = CARTESIAN_POINT('Ctrl Pts',(56.2622712892624,261.950121980978,20.2089728197824)) ;
#89164 = CARTESIAN_POINT('Ctrl Pts',(56.2695111541429,261.950121980978,20.2089728197824)) ;
#89165 = CARTESIAN_POINT('Origin',(56.2695111541429,261.559687576257,20.5213203435596)) ;
#89166 = CARTESIAN_POINT('Ctrl Pts',(55.5095145719656,261.79455482774,20.2277364888237)) ;
#89167 = CARTESIAN_POINT('Ctrl Pts',(55.5318704226011,261.835587804427,20.2336372451564)) ;
#89168 = CARTESIAN_POINT('Ctrl Pts',(55.5809822967928,261.905784092892,20.2463148514966)) ;
#89169 = CARTESIAN_POINT('Ctrl Pts',(55.7142947487837,261.996615667805,20.2848817332965)) ;
#89170 = CARTESIAN_POINT('Ctrl Pts',(55.8167520150608,262.046133815589,20.3289876130455)) ;
#89171 = CARTESIAN_POINT('Ctrl Pts',(55.8638558727399,262.066371572297,20.3542848089307)) ;
#89172 = CARTESIAN_POINT('Ctrl Pts',(55.5021508781933,261.805895393144,20.239612427161)) ;
#89173 = CARTESIAN_POINT('Ctrl Pts',(55.5245129486454,261.845948338582,20.2451930175294)) ;
#89174 = CARTESIAN_POINT('Ctrl Pts',(55.5734190414891,261.915123351253,20.2575607551273)) ;
#89175 = CARTESIAN_POINT('Ctrl Pts',(55.7070692316063,262.006295891711,20.2968962781282)) ;
#89176 = CARTESIAN_POINT('Ctrl Pts',(55.8078507833606,262.055426513127,20.3406034849686)) ;
#89177 = CARTESIAN_POINT('Ctrl Pts',(55.8547221940317,262.075352656397,20.3655111640554)) ;
#89178 = CARTESIAN_POINT('Ctrl Pts',(55.4880735456019,261.829072700441,20.2645630186822)) ;
#89179 = CARTESIAN_POINT('Ctrl Pts',(55.5104117488909,261.867380393505,20.2695523766429)) ;
#89180 = CARTESIAN_POINT('Ctrl Pts',(55.559902068292,261.934673156301,20.2813591433882)) ;
#89181 = CARTESIAN_POINT('Ctrl Pts',(55.6936488281965,262.02682092658,20.3223088243929)) ;
#89182 = CARTESIAN_POINT('Ctrl Pts',(55.7912089494402,262.074940512162,20.3649959837617)) ;
#89183 = CARTESIAN_POINT('Ctrl Pts',(55.8376310823803,262.094199248694,20.3890694044266)) ;
#89184 = CARTESIAN_POINT('Ctrl Pts',(55.4699650328212,261.866144293726,20.3064310132397)) ;
#89185 = CARTESIAN_POINT('Ctrl Pts',(55.4929957908261,261.902377349883,20.3106523286683)) ;
#89186 = CARTESIAN_POINT('Ctrl Pts',(55.546126482402,261.967512823357,20.3217909930518)) ;
#89187 = CARTESIAN_POINT('Ctrl Pts',(55.6762898619748,262.061105323079,20.3645153425193)) ;
#89188 = CARTESIAN_POINT('Ctrl Pts',(55.7702332408511,262.106446960815,20.4043790445782)) ;
#89189 = CARTESIAN_POINT('Ctrl Pts',(55.816111301075,262.12434494673,20.4267515269718)) ;
#89190 = CARTESIAN_POINT('Ctrl Pts',(55.4520758007103,261.906852049728,20.3536557306369)) ;
#89191 = CARTESIAN_POINT('Ctrl Pts',(55.4739718660818,261.941532580139,20.3569670015285)) ;
#89192 = CARTESIAN_POINT('Ctrl Pts',(55.5356402846097,262.004945670765,20.3676331273513)) ;
#89193 = CARTESIAN_POINT('Ctrl Pts',(55.6630577627351,262.098567808436,20.4105259197655)) ;
#89194 = CARTESIAN_POINT('Ctrl Pts',(55.7537573949811,262.139559060658,20.4457691693816)) ;
#89195 = CARTESIAN_POINT('Ctrl Pts',(55.7992124503129,262.155600230362,20.4658206315121)) ;
#89196 = CARTESIAN_POINT('Ctrl Pts',(55.4413189890535,261.951943447046,20.4076656249392)) ;
#89197 = CARTESIAN_POINT('Ctrl Pts',(55.4685727933187,261.985027606168,20.4101150870237)) ;
#89198 = CARTESIAN_POINT('Ctrl Pts',(55.5256447361003,262.048195315495,20.4196062026645)) ;
#89199 = CARTESIAN_POINT('Ctrl Pts',(55.655240746667,262.138550523405,20.4597488079456)) ;
#89200 = CARTESIAN_POINT('Ctrl Pts',(55.7421185070325,262.173732522086,20.488485996167)) ;
#89201 = CARTESIAN_POINT('Ctrl Pts',(55.7871294431314,262.187426540391,20.5056035190482)) ;
#89202 = CARTESIAN_POINT('Ctrl Pts',(55.4339566679902,262.003588608482,20.4698817737906)) ;
#89203 = CARTESIAN_POINT('Ctrl Pts',(55.4606880082801,262.035663654577,20.4708390649677)) ;
#89204 = CARTESIAN_POINT('Ctrl Pts',(55.5235568044765,262.097388906199,20.4785782506978)) ;
#89205 = CARTESIAN_POINT('Ctrl Pts',(55.6508626693057,262.180531558113,20.5114075592019)) ;
#89206 = CARTESIAN_POINT('Ctrl Pts',(55.7350394275834,262.208890877721,20.5324339407107)) ;
#89207 = CARTESIAN_POINT('Ctrl Pts',(55.7793466606563,262.219881088534,20.5461717042271)) ;
#89208 = CARTESIAN_POINT('Ctrl Pts',(55.4320069322682,262.063615725155,20.5417594331499)) ;
#89209 = CARTESIAN_POINT('Ctrl Pts',(55.4607036186458,262.094102965218,20.5405796731094)) ;
#89210 = CARTESIAN_POINT('Ctrl Pts',(55.5260165932096,262.152758635894,20.5442555742965)) ;
#89211 = CARTESIAN_POINT('Ctrl Pts',(55.6506170754938,262.223658860309,20.564760989951)) ;
#89212 = CARTESIAN_POINT('Ctrl Pts',(55.7321897267531,262.244956725749,20.5775162507453)) ;
#89213 = CARTESIAN_POINT('Ctrl Pts',(55.7755030403665,262.252890970876,20.5874340571549)) ;
#89214 = CARTESIAN_POINT('Ctrl Pts',(55.4372381689899,262.132341396724,20.6226948020985)) ;
#89215 = CARTESIAN_POINT('Ctrl Pts',(55.4672574673095,262.160051164332,20.6179839815041)) ;
#89216 = CARTESIAN_POINT('Ctrl Pts',(55.535055068772,262.211948592104,20.6140283051287)) ;
#89217 = CARTESIAN_POINT('Ctrl Pts',(55.6545305697442,262.266520428154,20.6180877115192)) ;
#89218 = CARTESIAN_POINT('Ctrl Pts',(55.7339304470145,262.281174467558,20.6227884280072)) ;
#89219 = CARTESIAN_POINT('Ctrl Pts',(55.7758592437434,262.285802712839,20.6285737346079)) ;
#89220 = CARTESIAN_POINT('Ctrl Pts',(55.4523935735627,262.206184157921,20.7072597357073)) ;
#89221 = CARTESIAN_POINT('Ctrl Pts',(55.4830627961843,262.229306963324,20.6976358460879)) ;
#89222 = CARTESIAN_POINT('Ctrl Pts',(55.5507543239758,262.270631714132,20.6830746334434)) ;
#89223 = CARTESIAN_POINT('Ctrl Pts',(55.6635699821141,262.307900047814,20.6697105532676)) ;
#89224 = CARTESIAN_POINT('Ctrl Pts',(55.7406360766256,262.316640091316,20.6671204577043)) ;
#89225 = CARTESIAN_POINT('Ctrl Pts',(55.7806429509047,262.317878574873,20.6686685621508)) ;
#89226 = CARTESIAN_POINT('Ctrl Pts',(55.4781604356767,262.278168118765,20.7871118425305)) ;
#89227 = CARTESIAN_POINT('Ctrl Pts',(55.5080300138342,262.295736009422,20.772627604968)) ;
#89228 = CARTESIAN_POINT('Ctrl Pts',(55.5728717758892,262.325199710388,20.7472936904588)) ;
#89229 = CARTESIAN_POINT('Ctrl Pts',(55.678507170532,262.34810030968,20.7195478001993)) ;
#89230 = CARTESIAN_POINT('Ctrl Pts',(55.7521512287222,262.350721354057,20.7097220361308)) ;
#89231 = CARTESIAN_POINT('Ctrl Pts',(55.789593096855,262.34862473989,20.7071012684221)) ;
#89232 = CARTESIAN_POINT('Ctrl Pts',(55.5008488901186,262.323452680659,20.8366594790575)) ;
#89233 = CARTESIAN_POINT('Ctrl Pts',(55.5294141416451,262.337477501983,20.8194278639549)) ;
#89234 = CARTESIAN_POINT('Ctrl Pts',(55.5909766067113,262.35982539795,20.7880695269394)) ;
#89235 = CARTESIAN_POINT('Ctrl Pts',(55.691882974598,262.375012422702,20.7524880639786)) ;
#89236 = CARTESIAN_POINT('Ctrl Pts',(55.762148436109,262.372604836401,20.7370763890607)) ;
#89237 = CARTESIAN_POINT('Ctrl Pts',(55.7975023182572,262.368314961946,20.7317140459925)) ;
#89238 = CARTESIAN_POINT('Ctrl Pts',(55.5133169212987,262.347205304054,20.8621241336292)) ;
#89239 = CARTESIAN_POINT('Ctrl Pts',(55.5408880083649,262.359266249537,20.8435414012517)) ;
#89240 = CARTESIAN_POINT('Ctrl Pts',(55.6003710788384,262.377970841319,20.8093031768376)) ;
#89241 = CARTESIAN_POINT('Ctrl Pts',(55.6986198286852,262.388518764252,20.7690288804046)) ;
#89242 = CARTESIAN_POINT('Ctrl Pts',(55.7671947747017,262.3835623992,20.7507733425594)) ;
#89243 = CARTESIAN_POINT('Ctrl Pts',(55.8014829417656,262.378142623667,20.743998623144)) ;
#89244 = CARTESIAN_POINT('',(55.5133169212987,262.347205304054,20.8621241336292)) ;
#89245 = CARTESIAN_POINT('Ctrl Pts',(55.5095145719656,261.79455482774,20.2277364888237)) ;
#89246 = CARTESIAN_POINT('Ctrl Pts',(55.5021508781933,261.805895393144,20.239612427161)) ;
#89247 = CARTESIAN_POINT('Ctrl Pts',(55.4880735456018,261.829072700441,20.2645630186821)) ;
#89248 = CARTESIAN_POINT('Ctrl Pts',(55.4699650328212,261.866144293726,20.3064310132397)) ;
#89249 = CARTESIAN_POINT('Ctrl Pts',(55.4520758007103,261.906852049728,20.3536557306369)) ;
#89250 = CARTESIAN_POINT('Ctrl Pts',(55.4413189890535,261.951943447046,20.4076656249392)) ;
#89251 = CARTESIAN_POINT('Ctrl Pts',(55.4339566679903,262.003588608482,20.4698817737906)) ;
#89252 = CARTESIAN_POINT('Ctrl Pts',(55.4320069322682,262.063615725155,20.5417594331499)) ;
#89253 = CARTESIAN_POINT('Ctrl Pts',(55.4372381689898,262.132341396724,20.6226948020985)) ;
#89254 = CARTESIAN_POINT('Ctrl Pts',(55.4523935735627,262.206184157921,20.7072597357073)) ;
#89255 = CARTESIAN_POINT('Ctrl Pts',(55.4781604356767,262.278168118765,20.7871118425305)) ;
#89256 = CARTESIAN_POINT('Ctrl Pts',(55.5008488901186,262.323452680659,20.8366594790575)) ;
#89257 = CARTESIAN_POINT('Ctrl Pts',(55.5133169212987,262.347205304054,20.8621241336292)) ;
#89258 = CARTESIAN_POINT('',(55.8014829417656,262.378142623667,20.743998623144)) ;
#89259 = CARTESIAN_POINT('Origin',(55.8014829417656,261.987708218946,21.0563461469212)) ;
#89260 = CARTESIAN_POINT('Ctrl Pts',(55.8014829417656,262.378142623667,20.743998623144)) ;
#89261 = CARTESIAN_POINT('Ctrl Pts',(55.7991573587302,262.372401049934,20.7368216559782)) ;
#89262 = CARTESIAN_POINT('Ctrl Pts',(55.7968348028396,262.366657445889,20.7296421510009)) ;
#89263 = CARTESIAN_POINT('Ctrl Pts',(55.7946197225382,262.360866471452,20.7224034329287)) ;
#89264 = CARTESIAN_POINT('Ctrl Pts',(55.7930432612197,262.356745064571,20.7172516743091)) ;
#89265 = CARTESIAN_POINT('Ctrl Pts',(55.7915186399541,262.352601013753,20.7120716107602)) ;
#89266 = CARTESIAN_POINT('Ctrl Pts',(55.7900769583761,262.348423032613,20.7068491343307)) ;
#89267 = CARTESIAN_POINT('Ctrl Pts',(55.7893457597689,262.346304025173,20.7042003750277)) ;
#89268 = CARTESIAN_POINT('Ctrl Pts',(55.7886358870253,262.344176285044,20.7015406998662)) ;
#89269 = CARTESIAN_POINT('Ctrl Pts',(55.7879489827639,262.342039856916,20.6988701647101)) ;
#89270 = CARTESIAN_POINT('Ctrl Pts',(55.7857762248067,262.33528208662,20.6904229518515)) ;
#89271 = CARTESIAN_POINT('Ctrl Pts',(55.7838412913505,262.328431054561,20.6818591617716)) ;
#89272 = CARTESIAN_POINT('Ctrl Pts',(55.7822046176232,262.3214814517,20.673172158189)) ;
#89273 = CARTESIAN_POINT('Ctrl Pts',(55.7819051330084,262.320209787654,20.6715825781292)) ;
#89274 = CARTESIAN_POINT('Ctrl Pts',(55.7816155233921,262.318934967357,20.6699890527579)) ;
#89275 = CARTESIAN_POINT('Ctrl Pts',(55.7813361907946,262.317656922226,20.6683914963437)) ;
#89276 = CARTESIAN_POINT('Ctrl Pts',(55.7799457578442,262.311295201187,20.6604393450441)) ;
#89277 = CARTESIAN_POINT('Ctrl Pts',(55.7788098142623,262.304853533795,20.6523872608128)) ;
#89278 = CARTESIAN_POINT('Ctrl Pts',(55.7779419835549,262.298346676154,20.6442536887576)) ;
#89279 = CARTESIAN_POINT('Ctrl Pts',(55.7773814313783,262.294143744426,20.6390000240963)) ;
#89280 = CARTESIAN_POINT('Ctrl Pts',(55.7769320002345,262.289914226983,20.6337131272905)) ;
#89281 = CARTESIAN_POINT('Ctrl Pts',(55.7765961607768,262.285663289202,20.6283994550628)) ;
#89282 = CARTESIAN_POINT('Ctrl Pts',(55.7761841937201,262.280448755037,20.6218812873552)) ;
#89283 = CARTESIAN_POINT('Ctrl Pts',(55.7759431555174,262.275201990712,20.615322831949)) ;
#89284 = CARTESIAN_POINT('Ctrl Pts',(55.7758684038679,262.26993703184,20.608741633359)) ;
#89285 = CARTESIAN_POINT('Ctrl Pts',(55.7757878800543,262.264265523994,20.6016522485523)) ;
#89286 = CARTESIAN_POINT('Ctrl Pts',(55.7759011734486,262.258572201006,20.594535594817)) ;
#89287 = CARTESIAN_POINT('Ctrl Pts',(55.7762026881147,262.252874555225,20.5874135375915)) ;
#89288 = CARTESIAN_POINT('Ctrl Pts',(55.7764544426288,262.248117214352,20.5814668614997)) ;
#89289 = CARTESIAN_POINT('Ctrl Pts',(55.7768374163714,262.243356859504,20.5755164179393)) ;
#89290 = CARTESIAN_POINT('Ctrl Pts',(55.7773478415344,262.238602506964,20.5695734772651)) ;
#89291 = CARTESIAN_POINT('Ctrl Pts',(55.7780162384643,262.23237672722,20.5617912525844)) ;
#89292 = CARTESIAN_POINT('Ctrl Pts',(55.7789034723116,262.226161192034,20.5540218336032)) ;
#89293 = CARTESIAN_POINT('Ctrl Pts',(55.7800025150514,262.219973478099,20.5462871911838)) ;
#89294 = CARTESIAN_POINT('Ctrl Pts',(55.7803506975784,262.218013177743,20.5438368157386)) ;
#89295 = CARTESIAN_POINT('Ctrl Pts',(55.7807201433493,262.216055670913,20.5413899322016)) ;
#89296 = CARTESIAN_POINT('Ctrl Pts',(55.7811112438686,262.214100958861,20.5389465421364)) ;
#89297 = CARTESIAN_POINT('Ctrl Pts',(55.7826261697489,262.206529391629,20.529482083096)) ;
#89298 = CARTESIAN_POINT('Ctrl Pts',(55.7844636665024,262.199005975118,20.5200778124559)) ;
#89299 = CARTESIAN_POINT('Ctrl Pts',(55.78664185792,262.191537798588,20.5107425917956)) ;
#89300 = CARTESIAN_POINT('Ctrl Pts',(55.7870318798326,262.190200564188,20.5090710487957)) ;
#89301 = CARTESIAN_POINT('Ctrl Pts',(55.7874328447887,262.188864923484,20.507401497916)) ;
#89302 = CARTESIAN_POINT('Ctrl Pts',(55.7878449073235,262.187530870786,20.5057339320444)) ;
#89303 = CARTESIAN_POINT('Ctrl Pts',(55.7898993187327,262.180879712646,20.4974199843724)) ;
#89304 = CARTESIAN_POINT('Ctrl Pts',(55.7922294437967,262.174267976547,20.4891553142605)) ;
#89305 = CARTESIAN_POINT('Ctrl Pts',(55.7948616136521,262.167690167664,20.4809330531478)) ;
#89306 = CARTESIAN_POINT('Ctrl Pts',(55.7964672004132,262.163677796335,20.4759175889817)) ;
#89307 = CARTESIAN_POINT('Ctrl Pts',(55.7981833380746,262.159679471643,20.4709196831148)) ;
#89308 = CARTESIAN_POINT('Ctrl Pts',(55.8000143657964,262.155695146818,20.4659392770827)) ;
#89309 = CARTESIAN_POINT('Ctrl Pts',(55.801824812773,262.15175560579,20.4610148507967)) ;
#89310 = CARTESIAN_POINT('Ctrl Pts',(55.8037475810324,262.147829752407,20.4561075340681)) ;
#89311 = CARTESIAN_POINT('Ctrl Pts',(55.8057805190409,262.143922743729,20.4512237732206)) ;
#89312 = CARTESIAN_POINT('Ctrl Pts',(55.8091738951825,262.137401172497,20.4430718091804)) ;
#89313 = CARTESIAN_POINT('Ctrl Pts',(55.8128771536114,262.130929204255,20.4349818488788)) ;
#89314 = CARTESIAN_POINT('Ctrl Pts',(55.8168812880823,262.124529812421,20.4269826090862)) ;
#89315 = CARTESIAN_POINT('Ctrl Pts',(55.8185339153892,262.121888590013,20.4236810810753)) ;
#89316 = CARTESIAN_POINT('Ctrl Pts',(55.8202377903298,262.11925972928,20.4203950051593)) ;
#89317 = CARTESIAN_POINT('Ctrl Pts',(55.8219913716022,262.116645490428,20.4171272065948)) ;
#89318 = CARTESIAN_POINT('Ctrl Pts',(55.8270320588606,262.109130834177,20.4077338862809)) ;
#89319 = CARTESIAN_POINT('Ctrl Pts',(55.8324856267513,262.101735225616,20.3984893755799)) ;
#89320 = CARTESIAN_POINT('Ctrl Pts',(55.83831695648,262.094511770528,20.3894600567187)) ;
#89321 = CARTESIAN_POINT('Ctrl Pts',(55.8429762944998,262.088740099143,20.3822454674877)) ;
#89322 = CARTESIAN_POINT('Ctrl Pts',(55.8478767960498,262.083078335888,20.3751682634189)) ;
#89323 = CARTESIAN_POINT('Ctrl Pts',(55.8529974353104,262.077553870314,20.368262681452)) ;
#89324 = CARTESIAN_POINT('Ctrl Pts',(55.8565149891311,262.073758913474,20.3635189854023)) ;
#89325 = CARTESIAN_POINT('Ctrl Pts',(55.8601365537588,262.070028753333,20.3588562852258)) ;
#89326 = CARTESIAN_POINT('Ctrl Pts',(55.8638558727399,262.066371572297,20.3542848089307)) ;
#89327 = CARTESIAN_POINT('Ctrl Pts',(55.5095145719656,261.79455482774,20.2277364888237)) ;
#89328 = CARTESIAN_POINT('Ctrl Pts',(55.5021508781933,261.805895393144,20.239612427161)) ;
#89329 = CARTESIAN_POINT('Ctrl Pts',(55.4880735456018,261.829072700441,20.2645630186821)) ;
#89330 = CARTESIAN_POINT('Ctrl Pts',(55.4699650328212,261.866144293726,20.3064310132397)) ;
#89331 = CARTESIAN_POINT('Ctrl Pts',(55.4520758007103,261.906852049728,20.3536557306369)) ;
#89332 = CARTESIAN_POINT('Ctrl Pts',(55.4413189890535,261.951943447046,20.4076656249392)) ;
#89333 = CARTESIAN_POINT('Ctrl Pts',(55.4339566679903,262.003588608482,20.4698817737906)) ;
#89334 = CARTESIAN_POINT('Ctrl Pts',(55.4320069322682,262.063615725155,20.5417594331499)) ;
#89335 = CARTESIAN_POINT('Ctrl Pts',(55.4372381689898,262.132341396724,20.6226948020985)) ;
#89336 = CARTESIAN_POINT('Ctrl Pts',(55.4523935735627,262.206184157921,20.7072597357073)) ;
#89337 = CARTESIAN_POINT('Ctrl Pts',(55.4781604356767,262.278168118765,20.7871118425305)) ;
#89338 = CARTESIAN_POINT('Ctrl Pts',(55.5008488901186,262.323452680659,20.8366594790575)) ;
#89339 = CARTESIAN_POINT('Ctrl Pts',(55.5133169212987,262.347205304054,20.8621241336292)) ;
#89340 = CARTESIAN_POINT('Ctrl Pts',(55.4626130754224,261.791323735734,20.2614221936152)) ;
#89341 = CARTESIAN_POINT('Ctrl Pts',(55.456933189044,261.80292645307,20.2736403319025)) ;
#89342 = CARTESIAN_POINT('Ctrl Pts',(55.4459364134233,261.82662567018,20.299221698274)) ;
#89343 = CARTESIAN_POINT('Ctrl Pts',(55.4318517617125,261.864376559775,20.3418755777896)) ;
#89344 = CARTESIAN_POINT('Ctrl Pts',(55.4170849015297,261.905634161402,20.3897054228805)) ;
#89345 = CARTESIAN_POINT('Ctrl Pts',(55.4094946332789,261.951022937766,20.4441389408264)) ;
#89346 = CARTESIAN_POINT('Ctrl Pts',(55.4043163979937,262.002731372621,20.5064211995693)) ;
#89347 = CARTESIAN_POINT('Ctrl Pts',(55.4041907996858,262.06216052464,20.5774476075643)) ;
#89348 = CARTESIAN_POINT('Ctrl Pts',(55.410843827055,262.128931911869,20.65558394842)) ;
#89349 = CARTESIAN_POINT('Ctrl Pts',(55.4267179821464,262.199434726762,20.7352219757316)) ;
#89350 = CARTESIAN_POINT('Ctrl Pts',(55.4519739561487,262.268120582844,20.8098095523395)) ;
#89351 = CARTESIAN_POINT('Ctrl Pts',(55.4736689753899,262.312067039713,20.8567205002237)) ;
#89352 = CARTESIAN_POINT('Ctrl Pts',(55.4857458342326,262.33514435857,20.8807068660068)) ;
#89353 = CARTESIAN_POINT('Ctrl Pts',(55.3860532767111,261.781008579942,20.3361055438638)) ;
#89354 = CARTESIAN_POINT('Ctrl Pts',(55.3825955021332,261.793201335109,20.3488988744911)) ;
#89355 = CARTESIAN_POINT('Ctrl Pts',(55.3757040049108,261.818043148829,20.3756388327424)) ;
#89356 = CARTESIAN_POINT('Ctrl Pts',(55.3669780343311,261.857372312824,20.4202275315097)) ;
#89357 = CARTESIAN_POINT('Ctrl Pts',(55.3559877265066,261.900120114085,20.4701859646172)) ;
#89358 = CARTESIAN_POINT('Ctrl Pts',(55.3525696678913,261.946639790849,20.5267824467788)) ;
#89359 = CARTESIAN_POINT('Ctrl Pts',(55.3501888273653,261.998688786346,20.5899899103179)) ;
#89360 = CARTESIAN_POINT('Ctrl Pts',(55.353194091183,262.056267188396,20.6585894493622)) ;
#89361 = CARTESIAN_POINT('Ctrl Pts',(55.3625023028779,262.118055719835,20.7292468247288)) ;
#89362 = CARTESIAN_POINT('Ctrl Pts',(55.3795168054528,262.181156991198,20.7971576993123)) ;
#89363 = CARTESIAN_POINT('Ctrl Pts',(55.4035892741016,262.242857727496,20.8596399172166)) ;
#89364 = CARTESIAN_POINT('Ctrl Pts',(55.42361623327,262.283862452034,20.9001120203024)) ;
#89365 = CARTESIAN_POINT('Ctrl Pts',(55.4349467887998,262.305606144961,20.9207980665079)) ;
#89366 = CARTESIAN_POINT('Ctrl Pts',(55.2919386084249,261.742010571783,20.5272717802442)) ;
#89367 = CARTESIAN_POINT('Ctrl Pts',(55.2905609388079,261.756084194904,20.5407912325947)) ;
#89368 = CARTESIAN_POINT('Ctrl Pts',(55.2875844799747,261.784514567651,20.568652899067)) ;
#89369 = CARTESIAN_POINT('Ctrl Pts',(55.2843693955679,261.828488818617,20.613161965571)) ;
#89370 = CARTESIAN_POINT('Ctrl Pts',(55.2787014910525,261.874606326743,20.6598246389281)) ;
#89371 = CARTESIAN_POINT('Ctrl Pts',(55.282339584292,261.922376601744,20.7084339193678)) ;
#89372 = CARTESIAN_POINT('Ctrl Pts',(55.2867532550598,261.972820267034,20.7571463593862)) ;
#89373 = CARTESIAN_POINT('Ctrl Pts',(55.2961707426459,262.025232807302,20.8049516990132)) ;
#89374 = CARTESIAN_POINT('Ctrl Pts',(55.3097166755623,262.078984671258,20.8509463776884)) ;
#89375 = CARTESIAN_POINT('Ctrl Pts',(55.3274619515341,262.133564899343,20.895158309429)) ;
#89376 = CARTESIAN_POINT('Ctrl Pts',(55.3488908311421,262.189257575911,20.9398889939635)) ;
#89377 = CARTESIAN_POINT('Ctrl Pts',(55.3657889087667,262.227536454716,20.9716659960487)) ;
#89378 = CARTESIAN_POINT('Ctrl Pts',(55.3751920600054,262.247035598335,20.9870170813929)) ;
#89379 = CARTESIAN_POINT('Ctrl Pts',(55.2649157169606,261.69184073163,20.6679797590307)) ;
#89380 = CARTESIAN_POINT('Ctrl Pts',(55.2649086000589,261.708286029276,20.6789611373507)) ;
#89381 = CARTESIAN_POINT('Ctrl Pts',(55.2648440073611,261.741176973179,20.7012707802754)) ;
#89382 = CARTESIAN_POINT('Ctrl Pts',(55.2650501911457,261.790617905123,20.7359777828176)) ;
#89383 = CARTESIAN_POINT('Ctrl Pts',(55.2647071106602,261.840419413326,20.7716773112338)) ;
#89384 = CARTESIAN_POINT('Ctrl Pts',(55.2685704487611,261.890478004158,20.8085365763669)) ;
#89385 = CARTESIAN_POINT('Ctrl Pts',(55.2743403282809,261.941338432843,20.8457412040926)) ;
#89386 = CARTESIAN_POINT('Ctrl Pts',(55.2830463917309,261.992700907183,20.883401123301)) ;
#89387 = CARTESIAN_POINT('Ctrl Pts',(55.2945926429713,262.04449713072,20.9211540604301)) ;
#89388 = CARTESIAN_POINT('Ctrl Pts',(55.3091555672942,262.096549677205,20.9587162447594)) ;
#89389 = CARTESIAN_POINT('Ctrl Pts',(55.326770477828,262.148491465379,20.9961671298381)) ;
#89390 = CARTESIAN_POINT('Ctrl Pts',(55.3405568610208,262.182853784487,21.0212206455135)) ;
#89391 = CARTESIAN_POINT('Ctrl Pts',(55.3481064294777,262.200232606203,21.0332361465525)) ;
#89392 = CARTESIAN_POINT('Ctrl Pts',(55.2649122781271,261.665580342705,20.7284379454282)) ;
#89393 = CARTESIAN_POINT('Ctrl Pts',(55.2649104802532,261.683350669897,20.7386049292427)) ;
#89394 = CARTESIAN_POINT('Ctrl Pts',(55.264874404684,261.718678953952,20.7593137062813)) ;
#89395 = CARTESIAN_POINT('Ctrl Pts',(55.2650136524204,261.771002970452,20.7914811683607)) ;
#89396 = CARTESIAN_POINT('Ctrl Pts',(55.2646380837014,261.822823681129,20.8244650422272)) ;
#89397 = CARTESIAN_POINT('Ctrl Pts',(55.267246242196,261.87415188769,20.8581387118653)) ;
#89398 = CARTESIAN_POINT('Ctrl Pts',(55.2723439409786,261.925296254531,20.8917898342268)) ;
#89399 = CARTESIAN_POINT('Ctrl Pts',(55.2800868920873,261.97606891941,20.9255063012982)) ;
#89400 = CARTESIAN_POINT('Ctrl Pts',(55.2904575118652,262.026562708551,20.9589320611357)) ;
#89401 = CARTESIAN_POINT('Ctrl Pts',(55.3034984602722,262.076742149292,20.9918978037114)) ;
#89402 = CARTESIAN_POINT('Ctrl Pts',(55.3191977410406,262.126387158599,21.0245040383623)) ;
#89403 = CARTESIAN_POINT('Ctrl Pts',(55.3314042901508,262.158997112573,21.0460840685968)) ;
#89404 = CARTESIAN_POINT('Ctrl Pts',(55.3380548194638,262.175416437892,21.0563461469212)) ;
#89405 = CARTESIAN_POINT('',(55.2649122781606,261.665580028629,20.7284377450722)) ;
#89406 = CARTESIAN_POINT('Ctrl Pts',(55.5095145719656,261.79455482774,20.2277364888237)) ;
#89407 = CARTESIAN_POINT('Ctrl Pts',(55.4626130754224,261.791323735734,20.2614221936152)) ;
#89408 = CARTESIAN_POINT('Ctrl Pts',(55.3860532767111,261.781008579942,20.3361055438638)) ;
#89409 = CARTESIAN_POINT('Ctrl Pts',(55.2919386177282,261.742010575638,20.5272717613472)) ;
#89410 = CARTESIAN_POINT('Ctrl Pts',(55.2649157249743,261.691840746508,20.6679797173033)) ;
#89411 = CARTESIAN_POINT('Ctrl Pts',(55.2649122781302,261.665580366068,20.728437891641)) ;
#89412 = CARTESIAN_POINT('',(55.2648833765136,261.800000087205,20.8099471270963)) ;
#89413 = CARTESIAN_POINT('Ctrl Pts',(55.264912278126,261.665580353186,20.728437951425)) ;
#89414 = CARTESIAN_POINT('Ctrl Pts',(55.2649116845233,261.67144754861,20.7317947653228)) ;
#89415 = CARTESIAN_POINT('Ctrl Pts',(55.2649094006061,261.6771004327,20.7350471228012)) ;
#89416 = CARTESIAN_POINT('Ctrl Pts',(55.2649071885691,261.682520862898,20.7381870921931)) ;
#89417 = CARTESIAN_POINT('Ctrl Pts',(55.2649051367789,261.687548620226,20.7410995924083)) ;
#89418 = CARTESIAN_POINT('Ctrl Pts',(55.2649031330562,261.692375204843,20.7439171417652)) ;
#89419 = CARTESIAN_POINT('Ctrl Pts',(55.2649020653765,261.697026581304,20.7466532077635)) ;
#89420 = CARTESIAN_POINT('Ctrl Pts',(55.2649007202167,261.702886807363,20.7501003519362)) ;
#89421 = CARTESIAN_POINT('Ctrl Pts',(55.2649008325002,261.708468494965,20.7534180622178)) ;
#89422 = CARTESIAN_POINT('Ctrl Pts',(55.2649035864154,261.713918696501,20.7566853863074)) ;
#89423 = CARTESIAN_POINT('Ctrl Pts',(55.2649043754765,261.715480306677,20.7576215510556)) ;
#89424 = CARTESIAN_POINT('Ctrl Pts',(55.2649053808284,261.717031475024,20.7585537601388)) ;
#89425 = CARTESIAN_POINT('Ctrl Pts',(55.2649066286006,261.718573526866,20.7594824355829)) ;
#89426 = CARTESIAN_POINT('Ctrl Pts',(55.264908727046,261.721166878015,20.7610442388023)) ;
#89427 = CARTESIAN_POINT('Ctrl Pts',(55.2649115070367,261.723734449957,20.7625960412854)) ;
#89428 = CARTESIAN_POINT('Ctrl Pts',(55.264914577773,261.726282582634,20.7641397963417)) ;
#89429 = CARTESIAN_POINT('Ctrl Pts',(55.2649199956029,261.730778360887,20.7668635086787)) ;
#89430 = CARTESIAN_POINT('Ctrl Pts',(55.2649263016323,261.735213563686,20.7695605656014)) ;
#89431 = CARTESIAN_POINT('Ctrl Pts',(55.2649315558431,261.739564585578,20.7722202638766)) ;
#89432 = CARTESIAN_POINT('Ctrl Pts',(55.264939501443,261.746144351901,20.776242351924)) ;
#89433 = CARTESIAN_POINT('Ctrl Pts',(55.2649447892793,261.752531922181,20.7801795081595)) ;
#89434 = CARTESIAN_POINT('Ctrl Pts',(55.2649429787217,261.758523548692,20.7838956325582)) ;
#89435 = CARTESIAN_POINT('Ctrl Pts',(55.2649417450228,261.762606193293,20.7864277688969)) ;
#89436 = CARTESIAN_POINT('Ctrl Pts',(55.2649372853029,261.766502858534,20.788855812778)) ;
#89437 = CARTESIAN_POINT('Ctrl Pts',(55.2649295433275,261.770147948255,20.791134949254)) ;
#89438 = CARTESIAN_POINT('Ctrl Pts',(55.2649289946744,261.770406265999,20.7912964655502)) ;
#89439 = CARTESIAN_POINT('Ctrl Pts',(55.2649284300825,261.770663330091,20.7914571915746)) ;
#89440 = CARTESIAN_POINT('Ctrl Pts',(55.2649278497419,261.770919127213,20.7916171217019)) ;
#89441 = CARTESIAN_POINT('Ctrl Pts',(55.2649207517931,261.774047694601,20.7935731725673)) ;
#89442 = CARTESIAN_POINT('Ctrl Pts',(55.2649114923583,261.776986718916,20.7954101797538)) ;
#89443 = CARTESIAN_POINT('Ctrl Pts',(55.2649033675045,261.779711801583,20.797117915298)) ;
#89444 = CARTESIAN_POINT('Ctrl Pts',(55.2648952021657,261.782450462998,20.7988341602765)) ;
#89445 = CARTESIAN_POINT('Ctrl Pts',(55.2648881394329,261.78497238351,20.8004196374816)) ;
#89446 = CARTESIAN_POINT('Ctrl Pts',(55.2648833749291,261.7872887411,20.8018804120226)) ;
#89447 = CARTESIAN_POINT('Ctrl Pts',(55.2648788571325,261.78948515714,20.8032655473092)) ;
#89448 = CARTESIAN_POINT('Ctrl Pts',(55.2648763284609,261.79149632143,20.804538307404)) ;
#89449 = CARTESIAN_POINT('Ctrl Pts',(55.2648758168632,261.793370917429,20.8057280000853)) ;
#89450 = CARTESIAN_POINT('Ctrl Pts',(55.2648753337915,261.795140988699,20.806851357244)) ;
#89451 = CARTESIAN_POINT('Ctrl Pts',(55.2648765899003,261.796789100496,20.8079005374401)) ;
#89452 = CARTESIAN_POINT('Ctrl Pts',(55.2648796573053,261.798396281414,20.8089247864228)) ;
#89453 = CARTESIAN_POINT('Ctrl Pts',(55.2648806830266,261.798933712801,20.8092672889662)) ;
#89454 = CARTESIAN_POINT('Ctrl Pts',(55.264881915461,261.799466926199,20.8096072235845)) ;
#89455 = CARTESIAN_POINT('Ctrl Pts',(55.2648833765136,261.800000087205,20.8099471270963)) ;
#89456 = CARTESIAN_POINT('',(55.3380548194639,262.175416437892,21.0563461469212)) ;
#89457 = CARTESIAN_POINT('Ctrl Pts',(55.2648833765465,261.800000099193,20.8099471347392)) ;
#89458 = CARTESIAN_POINT('Ctrl Pts',(55.264887076765,261.801350363729,20.810807962245)) ;
#89459 = CARTESIAN_POINT('Ctrl Pts',(55.2648921382654,261.802704527689,20.8116713360936)) ;
#89460 = CARTESIAN_POINT('Ctrl Pts',(55.2648999326208,261.804196001596,20.8126249318168)) ;
#89461 = CARTESIAN_POINT('Ctrl Pts',(55.2649079852912,261.805736904873,20.8136101309332)) ;
#89462 = CARTESIAN_POINT('Ctrl Pts',(55.2649188903312,261.807424217338,20.8146915320592)) ;
#89463 = CARTESIAN_POINT('Ctrl Pts',(55.2649360911695,261.809356367705,20.8159340062698)) ;
#89464 = CARTESIAN_POINT('Ctrl Pts',(55.2649539728193,261.811364992857,20.8172256577855)) ;
#89465 = CARTESIAN_POINT('Ctrl Pts',(55.2649785312904,261.813638039835,20.818691266036)) ;
#89466 = CARTESIAN_POINT('Ctrl Pts',(55.2650171871798,261.816236845546,20.8203715342793)) ;
#89467 = CARTESIAN_POINT('Ctrl Pts',(55.2650465915238,261.818213676981,20.8216496625624)) ;
#89468 = CARTESIAN_POINT('Ctrl Pts',(55.265084237455,261.820379398754,20.8230503908865)) ;
#89469 = CARTESIAN_POINT('Ctrl Pts',(55.2651353764379,261.822741913237,20.8245790678812)) ;
#89470 = CARTESIAN_POINT('Ctrl Pts',(55.2651547797991,261.823638308109,20.8251590847361)) ;
#89471 = CARTESIAN_POINT('Ctrl Pts',(55.2651761513239,261.824563031671,20.8257575242165)) ;
#89472 = CARTESIAN_POINT('Ctrl Pts',(55.2651997562632,261.825516516964,20.8263746705597)) ;
#89473 = CARTESIAN_POINT('Ctrl Pts',(55.2653002299749,261.829574998343,20.8290015353458)) ;
#89474 = CARTESIAN_POINT('Ctrl Pts',(55.2654410724233,261.834152612198,20.8319735604999)) ;
#89475 = CARTESIAN_POINT('Ctrl Pts',(55.2656422570234,261.839211915542,20.8352701409018)) ;
#89476 = CARTESIAN_POINT('Ctrl Pts',(55.2658245152904,261.843795267643,20.8382565972742)) ;
#89477 = CARTESIAN_POINT('Ctrl Pts',(55.2660564623741,261.848770288387,20.8415071128075)) ;
#89478 = CARTESIAN_POINT('Ctrl Pts',(55.2663498860856,261.854070559063,20.8449782174637)) ;
#89479 = CARTESIAN_POINT('Ctrl Pts',(55.2666975191413,261.860350042343,20.8490906005828)) ;
#89480 = CARTESIAN_POINT('Ctrl Pts',(55.2671320468463,261.867085104201,20.8535121626097)) ;
#89481 = CARTESIAN_POINT('Ctrl Pts',(55.2676612201599,261.874121981231,20.8581327504047)) ;
#89482 = CARTESIAN_POINT('Ctrl Pts',(55.2677194642485,261.87489650345,20.8586413208826)) ;
#89483 = CARTESIAN_POINT('Ctrl Pts',(55.2677788417528,261.875674684992,20.8591522975341)) ;
#89484 = CARTESIAN_POINT('Ctrl Pts',(55.2678393634794,261.876456315003,20.8596655428744)) ;
#89485 = CARTESIAN_POINT('Ctrl Pts',(55.2684840368388,261.884782185273,20.8651325976987)) ;
#89486 = CARTESIAN_POINT('Ctrl Pts',(55.2692600300963,261.893493152603,20.870860923632)) ;
#89487 = CARTESIAN_POINT('Ctrl Pts',(55.2701660419482,261.902315938472,20.8766742798029)) ;
#89488 = CARTESIAN_POINT('Ctrl Pts',(55.2708959763049,261.90942407344,20.8813578481106)) ;
#89489 = CARTESIAN_POINT('Ctrl Pts',(55.2717096489056,261.916603394402,20.8860956655889)) ;
#89490 = CARTESIAN_POINT('Ctrl Pts',(55.2725968069079,261.923732793028,20.8908074049882)) ;
#89491 = CARTESIAN_POINT('Ctrl Pts',(55.2726591307255,261.924233641061,20.8911384098222)) ;
#89492 = CARTESIAN_POINT('Ctrl Pts',(55.2727218125129,261.924734239028,20.8914692811339)) ;
#89493 = CARTESIAN_POINT('Ctrl Pts',(55.2727848485094,261.925234558655,20.8918000022097)) ;
#89494 = CARTESIAN_POINT('Ctrl Pts',(55.273563027158,261.931410998673,20.89588275007)) ;
#89495 = CARTESIAN_POINT('Ctrl Pts',(55.2743955029591,261.937544984512,20.899942595275)) ;
#89496 = CARTESIAN_POINT('Ctrl Pts',(55.2752717329007,261.943585821033,20.9039445402612)) ;
#89497 = CARTESIAN_POINT('Ctrl Pts',(55.2761597409042,261.949707856956,20.9080002783828)) ;
#89498 = CARTESIAN_POINT('Ctrl Pts',(55.2770923617596,261.955733783538,20.9119962627578)) ;
#89499 = CARTESIAN_POINT('Ctrl Pts',(55.2780621179994,261.961651586864,20.9159220749311)) ;
#89500 = CARTESIAN_POINT('Ctrl Pts',(55.2788579412695,261.966507988299,20.9191437635918)) ;
#89501 = CARTESIAN_POINT('Ctrl Pts',(55.2796785979965,261.971291439717,20.9223180969199)) ;
#89502 = CARTESIAN_POINT('Ctrl Pts',(55.2805249392995,261.976023013032,20.9254564121947)) ;
#89503 = CARTESIAN_POINT('Ctrl Pts',(55.2806454561434,261.976696777009,20.9259033002888)) ;
#89504 = CARTESIAN_POINT('Ctrl Pts',(55.2807664959025,261.977369488772,20.9263494583211)) ;
#89505 = CARTESIAN_POINT('Ctrl Pts',(55.2808880637497,261.978041207549,20.9267949212353)) ;
#89506 = CARTESIAN_POINT('Ctrl Pts',(55.2819528718817,261.983924766677,20.9306967138914)) ;
#89507 = CARTESIAN_POINT('Ctrl Pts',(55.2830575310507,261.989731884693,20.9345442358035)) ;
#89508 = CARTESIAN_POINT('Ctrl Pts',(55.2842204372246,261.995563383192,20.9384046930442)) ;
#89509 = CARTESIAN_POINT('Ctrl Pts',(55.2852766754412,262.000859985544,20.9419110485546)) ;
#89510 = CARTESIAN_POINT('Ctrl Pts',(55.2863822704946,262.00618208714,20.9454316325777)) ;
#89511 = CARTESIAN_POINT('Ctrl Pts',(55.2875502546595,262.011577672918,20.948997216028)) ;
#89512 = CARTESIAN_POINT('Ctrl Pts',(55.288614318678,262.016493192202,20.9522455554906)) ;
#89513 = CARTESIAN_POINT('Ctrl Pts',(55.2897303147452,262.021469464214,20.9555310700184)) ;
#89514 = CARTESIAN_POINT('Ctrl Pts',(55.2909026141373,262.026510521406,20.9588549641176)) ;
#89515 = CARTESIAN_POINT('Ctrl Pts',(55.2910848557811,262.027294186871,20.9593716852969)) ;
#89516 = CARTESIAN_POINT('Ctrl Pts',(55.2912684588985,262.028079417904,20.9598893337448)) ;
#89517 = CARTESIAN_POINT('Ctrl Pts',(55.2914534398696,262.028866226384,20.960407918366)) ;
#89518 = CARTESIAN_POINT('Ctrl Pts',(55.2929248551374,262.035124826947,20.9645329552543)) ;
#89519 = CARTESIAN_POINT('Ctrl Pts',(55.2944836292958,262.041482818636,20.9687171431804)) ;
#89520 = CARTESIAN_POINT('Ctrl Pts',(55.296124351784,262.047894905047,20.9729342442153)) ;
#89521 = CARTESIAN_POINT('Ctrl Pts',(55.2979374574581,262.054980679965,20.9775944167121)) ;
#89522 = CARTESIAN_POINT('Ctrl Pts',(55.2998509444912,262.062131742623,20.9822943552114)) ;
#89523 = CARTESIAN_POINT('Ctrl Pts',(55.3018372142892,262.069236566269,20.9869636166808)) ;
#89524 = CARTESIAN_POINT('Ctrl Pts',(55.30253052279,262.071716508639,20.9885934248127)) ;
#89525 = CARTESIAN_POINT('Ctrl Pts',(55.3032326176547,262.074190840947,20.9902192244433)) ;
#89526 = CARTESIAN_POINT('Ctrl Pts',(55.3039416337351,262.076653487504,20.9918372019887)) ;
#89527 = CARTESIAN_POINT('Ctrl Pts',(55.3058169380262,262.083167037455,20.9961166539192)) ;
#89528 = CARTESIAN_POINT('Ctrl Pts',(55.3077412820762,262.089598675218,21.0003413330951)) ;
#89529 = CARTESIAN_POINT('Ctrl Pts',(55.3096736304775,262.095837693835,21.0044415123092)) ;
#89530 = CARTESIAN_POINT('Ctrl Pts',(55.3120993978905,262.103669825991,21.0095886592308)) ;
#89531 = CARTESIAN_POINT('Ctrl Pts',(55.3145368697036,262.111194113669,21.014537052505)) ;
#89532 = CARTESIAN_POINT('Ctrl Pts',(55.3168878208236,262.118199499406,21.0191481320322)) ;
#89533 = CARTESIAN_POINT('Ctrl Pts',(55.3178189202186,262.120973997934,21.0209743602858)) ;
#89534 = CARTESIAN_POINT('Ctrl Pts',(55.3187365177371,262.123667968671,21.0227460251729)) ;
#89535 = CARTESIAN_POINT('Ctrl Pts',(55.3196347281987,262.126270973828,21.0244576618027)) ;
#89536 = CARTESIAN_POINT('Ctrl Pts',(55.3206354767496,262.129171133369,21.026364695789)) ;
#89537 = CARTESIAN_POINT('Ctrl Pts',(55.3216121837815,262.131958428654,21.0281971101326)) ;
#89538 = CARTESIAN_POINT('Ctrl Pts',(55.3225568950698,262.134619639904,21.0299450085362)) ;
#89539 = CARTESIAN_POINT('Ctrl Pts',(55.3241929769073,262.139228412388,21.0329720760301)) ;
#89540 = CARTESIAN_POINT('Ctrl Pts',(55.325732568719,262.143457850253,21.0357467867831)) ;
#89541 = CARTESIAN_POINT('Ctrl Pts',(55.3271454351735,262.147273177299,21.0382438986209)) ;
#89542 = CARTESIAN_POINT('Ctrl Pts',(55.3285114456696,262.15096197377,21.0406581968508)) ;
#89543 = CARTESIAN_POINT('Ctrl Pts',(55.3297585882148,262.154263201759,21.0428126342237)) ;
#89544 = CARTESIAN_POINT('Ctrl Pts',(55.330876560063,262.157186132183,21.0447119352508)) ;
#89545 = CARTESIAN_POINT('Ctrl Pts',(55.3318939799478,262.159846170126,21.0464404104672)) ;
#89546 = CARTESIAN_POINT('Ctrl Pts',(55.3328043988932,262.162192988628,21.0479576178318)) ;
#89547 = CARTESIAN_POINT('Ctrl Pts',(55.3336172586244,262.164270659442,21.0492908720446)) ;
#89548 = CARTESIAN_POINT('Ctrl Pts',(55.3344062793214,262.166287397645,21.0505850254241)) ;
#89549 = CARTESIAN_POINT('Ctrl Pts',(55.3351032841592,262.168050305835,21.0517057696937)) ;
#89550 = CARTESIAN_POINT('Ctrl Pts',(55.3357328885529,262.169632717654,21.0527075249679)) ;
#89551 = CARTESIAN_POINT('Ctrl Pts',(55.3363397180733,262.171157888403,21.0536730434406)) ;
#89552 = CARTESIAN_POINT('Ctrl Pts',(55.3368838676364,262.172515205813,21.0545279586057)) ;
#89553 = CARTESIAN_POINT('Ctrl Pts',(55.3374067785918,262.173812572095,21.0553418454806)) ;
#89554 = CARTESIAN_POINT('Ctrl Pts',(55.3376249049078,262.174353753581,21.0556813490688)) ;
#89555 = CARTESIAN_POINT('Ctrl Pts',(55.3378395674669,262.174885007626,21.0560140030048)) ;
#89556 = CARTESIAN_POINT('Ctrl Pts',(55.3380548194638,262.175416437892,21.0563461469212)) ;
#89557 = CARTESIAN_POINT('Origin',(55.8014829417656,261.987708218946,21.0563461469212)) ;
#89558 = CARTESIAN_POINT('Ctrl Pts',(55.5095145719656,261.79455482774,20.2277364888237)) ;
#89559 = CARTESIAN_POINT('Ctrl Pts',(55.4626130754224,261.791323735734,20.2614221936152)) ;
#89560 = CARTESIAN_POINT('Ctrl Pts',(55.3860532767111,261.781008579942,20.3361055438638)) ;
#89561 = CARTESIAN_POINT('Ctrl Pts',(55.2919386084249,261.742010571783,20.5272717802442)) ;
#89562 = CARTESIAN_POINT('Ctrl Pts',(55.2649157169606,261.69184073163,20.6679797590307)) ;
#89563 = CARTESIAN_POINT('Ctrl Pts',(55.2649122781271,261.665580342705,20.7284379454282)) ;
#89564 = CARTESIAN_POINT('Ctrl Pts',(55.5011311279772,261.779167461482,20.2255237051989)) ;
#89565 = CARTESIAN_POINT('Ctrl Pts',(55.456175278049,261.775186015806,20.2587821206896)) ;
#89566 = CARTESIAN_POINT('Ctrl Pts',(55.382237274109,261.763499950179,20.3326971182674)) ;
#89567 = CARTESIAN_POINT('Ctrl Pts',(55.29093472858,261.721392635792,20.5208133734021)) ;
#89568 = CARTESIAN_POINT('Ctrl Pts',(55.2649244698029,261.670189926701,20.6567721272306)) ;
#89569 = CARTESIAN_POINT('Ctrl Pts',(55.2649145254694,261.643367433716,20.71572921566)) ;
#89570 = CARTESIAN_POINT('Ctrl Pts',(55.4854302237238,261.746721466304,20.2213211965547)) ;
#89571 = CARTESIAN_POINT('Ctrl Pts',(55.4440536435622,261.74140119116,20.2537866714569)) ;
#89572 = CARTESIAN_POINT('Ctrl Pts',(55.3749045745113,261.727021754684,20.3263522718821)) ;
#89573 = CARTESIAN_POINT('Ctrl Pts',(55.2887959933571,261.678997151227,20.5082350012948)) ;
#89574 = CARTESIAN_POINT('Ctrl Pts',(55.2649030138605,261.626302482539,20.6346570484583)) ;
#89575 = CARTESIAN_POINT('Ctrl Pts',(55.26490889801,261.59862630945,20.690861256424)) ;
#89576 = CARTESIAN_POINT('Ctrl Pts',(55.4649411121345,261.691374789118,20.2150379267643)) ;
#89577 = CARTESIAN_POINT('Ctrl Pts',(55.428041263659,261.684353823492,20.2464932932028)) ;
#89578 = CARTESIAN_POINT('Ctrl Pts',(55.3646008444798,261.665909068801,20.3175416220631)) ;
#89579 = CARTESIAN_POINT('Ctrl Pts',(55.2856017188784,261.610888438487,20.4888635693427)) ;
#89580 = CARTESIAN_POINT('Ctrl Pts',(55.2649132810963,261.558540491237,20.6020448190387)) ;
#89581 = CARTESIAN_POINT('Ctrl Pts',(55.2649116963883,261.530698564893,20.6550488940796)) ;
#89582 = CARTESIAN_POINT('Ctrl Pts',(55.4472141017732,261.626342713257,20.2085985316935)) ;
#89583 = CARTESIAN_POINT('Ctrl Pts',(55.413733637549,261.617728456411,20.2392888290324)) ;
#89584 = CARTESIAN_POINT('Ctrl Pts',(55.3548941740118,261.595684496215,20.3093684675433)) ;
#89585 = CARTESIAN_POINT('Ctrl Pts',(55.2825837342738,261.536726216894,20.4692014769607)) ;
#89586 = CARTESIAN_POINT('Ctrl Pts',(55.2649106528737,261.487796504572,20.5717207979694)) ;
#89587 = CARTESIAN_POINT('Ctrl Pts',(55.2649109321867,261.461146834667,20.6224699580307)) ;
#89588 = CARTESIAN_POINT('Ctrl Pts',(55.4320883309197,261.54761255968,20.2014661968594)) ;
#89589 = CARTESIAN_POINT('Ctrl Pts',(55.4011858995745,261.538027697824,20.2316047928881)) ;
#89590 = CARTESIAN_POINT('Ctrl Pts',(55.3459211189135,261.513570807188,20.300979608063)) ;
#89591 = CARTESIAN_POINT('Ctrl Pts',(55.280186364588,261.456674374888,20.4483155522099)) ;
#89592 = CARTESIAN_POINT('Ctrl Pts',(55.2649110500436,261.414367237008,20.5433352405049)) ;
#89593 = CARTESIAN_POINT('Ctrl Pts',(55.2649110664895,261.390495196763,20.5924091979401)) ;
#89594 = CARTESIAN_POINT('Ctrl Pts',(55.4201855327187,261.451485192532,20.1924774356911)) ;
#89595 = CARTESIAN_POINT('Ctrl Pts',(55.3910693268253,261.442295282441,20.2221606966266)) ;
#89596 = CARTESIAN_POINT('Ctrl Pts',(55.338286157701,261.418483405646,20.2905621884509)) ;
#89597 = CARTESIAN_POINT('Ctrl Pts',(55.2788123134952,261.372468306853,20.4254128007512)) ;
#89598 = CARTESIAN_POINT('Ctrl Pts',(55.2649111022978,261.338665106617,20.5164805332069)) ;
#89599 = CARTESIAN_POINT('Ctrl Pts',(55.2649110733168,261.319006701877,20.5643405753509)) ;
#89600 = CARTESIAN_POINT('Ctrl Pts',(55.4127834941959,261.337382234005,20.1809091598321)) ;
#89601 = CARTESIAN_POINT('Ctrl Pts',(55.3844119930881,261.330754075371,20.2102651168952)) ;
#89602 = CARTESIAN_POINT('Ctrl Pts',(55.332911951351,261.313654500188,20.2776533346949)) ;
#89603 = CARTESIAN_POINT('Ctrl Pts',(55.2783408443739,261.285115029417,20.4035536370883)) ;
#89604 = CARTESIAN_POINT('Ctrl Pts',(55.2649110495544,261.259955288591,20.4941009157673)) ;
#89605 = CARTESIAN_POINT('Ctrl Pts',(55.2649110604085,261.245647194609,20.5412687298936)) ;
#89606 = CARTESIAN_POINT('Ctrl Pts',(55.4106967194038,261.2145920902,20.1714615566787)) ;
#89607 = CARTESIAN_POINT('Ctrl Pts',(55.3817726165835,261.212391231516,20.201117086952)) ;
#89608 = CARTESIAN_POINT('Ctrl Pts',(55.3298548129479,261.205827465748,20.2688848493694)) ;
#89609 = CARTESIAN_POINT('Ctrl Pts',(55.2778619848215,261.193338034809,20.3908691572262)) ;
#89610 = CARTESIAN_POINT('Ctrl Pts',(55.2649110678744,261.177942527005,20.4808836390622)) ;
#89611 = CARTESIAN_POINT('Ctrl Pts',(55.2649110649601,261.170167353101,20.5266939931165)) ;
#89612 = CARTESIAN_POINT('Ctrl Pts',(55.4113576734741,261.13534727522,20.1677669529664)) ;
#89613 = CARTESIAN_POINT('Ctrl Pts',(55.3811470979398,261.134705739364,20.1979775285007)) ;
#89614 = CARTESIAN_POINT('Ctrl Pts',(55.3280699815944,261.132719886408,20.2666239963843)) ;
#89615 = CARTESIAN_POINT('Ctrl Pts',(55.2768787444733,261.127286640832,20.3883249095729)) ;
#89616 = CARTESIAN_POINT('Ctrl Pts',(55.2649110640675,261.121858235112,20.4767780866077)) ;
#89617 = CARTESIAN_POINT('Ctrl Pts',(55.2649110640675,261.119141720484,20.5213203435597)) ;
#89618 = CARTESIAN_POINT('Ctrl Pts',(55.4113576734741,261.093548013806,20.1677669529664)) ;
#89619 = CARTESIAN_POINT('Ctrl Pts',(55.3805043197369,261.093548013806,20.1986203067036)) ;
#89620 = CARTESIAN_POINT('Ctrl Pts',(55.3269240548999,261.093548013806,20.2684476752798)) ;
#89621 = CARTESIAN_POINT('Ctrl Pts',(55.276399501296,261.093548013806,20.3904247378231)) ;
#89622 = CARTESIAN_POINT('Ctrl Pts',(55.2649110640673,261.093548013806,20.4776871122598)) ;
#89623 = CARTESIAN_POINT('Ctrl Pts',(55.2649110640673,261.093548013806,20.5213203435596)) ;
#89624 = CARTESIAN_POINT('',(55.4113576734741,261.093548013806,20.1677669529664)) ;
#89625 = CARTESIAN_POINT('Ctrl Pts',(55.5095145719656,261.79455482774,20.2277364888237)) ;
#89626 = CARTESIAN_POINT('Ctrl Pts',(55.5011311279772,261.779167461482,20.2255237051989)) ;
#89627 = CARTESIAN_POINT('Ctrl Pts',(55.4854302237238,261.746721466304,20.2213211965547)) ;
#89628 = CARTESIAN_POINT('Ctrl Pts',(55.4649411121345,261.691374789118,20.2150379267643)) ;
#89629 = CARTESIAN_POINT('Ctrl Pts',(55.4472141017732,261.626342713257,20.2085985316935)) ;
#89630 = CARTESIAN_POINT('Ctrl Pts',(55.4320883309197,261.54761255968,20.2014661968594)) ;
#89631 = CARTESIAN_POINT('Ctrl Pts',(55.4201855327187,261.451485192532,20.1924774356911)) ;
#89632 = CARTESIAN_POINT('Ctrl Pts',(55.4127834941959,261.337382234005,20.1809091598321)) ;
#89633 = CARTESIAN_POINT('Ctrl Pts',(55.4106967194038,261.2145920902,20.1714615566787)) ;
#89634 = CARTESIAN_POINT('Ctrl Pts',(55.4113576734741,261.13534727522,20.1677669529664)) ;
#89635 = CARTESIAN_POINT('Ctrl Pts',(55.4113576734741,261.093548013806,20.1677669529664)) ;
#89636 = CARTESIAN_POINT('',(55.2649110640674,261.093548013806,20.5213203435596)) ;
#89637 = CARTESIAN_POINT('Origin',(55.7649110640674,261.093548013806,20.5213203435596)) ;
#89638 = CARTESIAN_POINT('Ctrl Pts',(55.2649110640673,261.093548013806,20.5213203435596)) ;
#89639 = CARTESIAN_POINT('Ctrl Pts',(55.2649110640673,261.095953574552,20.5213203435596)) ;
#89640 = CARTESIAN_POINT('Ctrl Pts',(55.2649110641555,261.098363829073,20.5213210869593)) ;
#89641 = CARTESIAN_POINT('Ctrl Pts',(55.2649110658753,261.100914479524,20.5213508933325)) ;
#89642 = CARTESIAN_POINT('Ctrl Pts',(55.264911067669,261.103574764907,20.5213819808768)) ;
#89643 = CARTESIAN_POINT('Ctrl Pts',(55.2649110708674,261.106387547156,20.5214446439697)) ;
#89644 = CARTESIAN_POINT('Ctrl Pts',(55.2649110723512,261.109447355915,20.5215616301146)) ;
#89645 = CARTESIAN_POINT('Ctrl Pts',(55.2649110739158,261.112673890933,20.5216849907304)) ;
#89646 = CARTESIAN_POINT('Ctrl Pts',(55.2649110731951,261.116174814157,20.5218687043635)) ;
#89647 = CARTESIAN_POINT('Ctrl Pts',(55.2649110711966,261.120000151541,20.5221299119106)) ;
#89648 = CARTESIAN_POINT('Ctrl Pts',(55.2649110690495,261.12410979266,20.522410532721)) ;
#89649 = CARTESIAN_POINT('Ctrl Pts',(55.2649110661775,261.128593453019,20.5227805212708)) ;
#89650 = CARTESIAN_POINT('Ctrl Pts',(55.264911065038,261.133450022732,20.5232513519634)) ;
#89651 = CARTESIAN_POINT('Ctrl Pts',(55.2649110637655,261.138872992704,20.5237770935586)) ;
#89652 = CARTESIAN_POINT('Ctrl Pts',(55.2649110642511,261.144761660323,20.5244152470584)) ;
#89653 = CARTESIAN_POINT('Ctrl Pts',(55.2649110642177,261.151044919855,20.5251897158003)) ;
#89654 = CARTESIAN_POINT('Ctrl Pts',(55.2649110641858,261.157035609164,20.5259281226079)) ;
#89655 = CARTESIAN_POINT('Ctrl Pts',(55.264911064118,261.163382857385,20.5267957767956)) ;
#89656 = CARTESIAN_POINT('Ctrl Pts',(55.2649110639784,261.169990918531,20.5277797035235)) ;
#89657 = CARTESIAN_POINT('Ctrl Pts',(55.2649110637722,261.179745146691,20.5292320880557)) ;
#89658 = CARTESIAN_POINT('Ctrl Pts',(55.2649110633954,261.190066022824,20.5309359022516)) ;
#89659 = CARTESIAN_POINT('Ctrl Pts',(55.2649110631044,261.200632533083,20.5329114013934)) ;
#89660 = CARTESIAN_POINT('Ctrl Pts',(55.2649110630817,261.201457066028,20.5330655548542)) ;
#89661 = CARTESIAN_POINT('Ctrl Pts',(55.2649110630596,261.202283112817,20.5332213503105)) ;
#89662 = CARTESIAN_POINT('Ctrl Pts',(55.2649110630382,261.203110526522,20.5333787899727)) ;
#89663 = CARTESIAN_POINT('Ctrl Pts',(55.2649110628502,261.210386142706,20.5347631887907)) ;
#89664 = CARTESIAN_POINT('Ctrl Pts',(55.2649110626976,261.217766083194,20.5362748858767)) ;
#89665 = CARTESIAN_POINT('Ctrl Pts',(55.2649110627707,261.225190406921,20.5379151796448)) ;
#89666 = CARTESIAN_POINT('Ctrl Pts',(55.2649110628364,261.231859050926,20.5393885172316)) ;
#89667 = CARTESIAN_POINT('Ctrl Pts',(55.2649110632121,261.238564598798,20.5409601923757)) ;
#89668 = CARTESIAN_POINT('Ctrl Pts',(55.264911064521,261.245304154603,20.5426504023542)) ;
#89669 = CARTESIAN_POINT('Ctrl Pts',(55.2649110645244,261.245322028108,20.542654884842)) ;
#89670 = CARTESIAN_POINT('Ctrl Pts',(55.2649110645279,261.245339901851,20.5426593681642)) ;
#89671 = CARTESIAN_POINT('Ctrl Pts',(55.2649110645314,261.245357775832,20.542663852321)) ;
#89672 = CARTESIAN_POINT('Ctrl Pts',(55.2649110657567,261.251646693871,20.5442415922823)) ;
#89673 = CARTESIAN_POINT('Ctrl Pts',(55.2649110678177,261.25796485254,20.5459225583356)) ;
#89674 = CARTESIAN_POINT('Ctrl Pts',(55.2649110689405,261.264356178618,20.5477254079163)) ;
#89675 = CARTESIAN_POINT('Ctrl Pts',(55.2649110702031,261.271542625449,20.5497525432083)) ;
#89676 = CARTESIAN_POINT('Ctrl Pts',(55.2649110698206,261.278827235558,20.5519354804463)) ;
#89677 = CARTESIAN_POINT('Ctrl Pts',(55.2649110692137,261.286323385524,20.5543065199875)) ;
#89678 = CARTESIAN_POINT('Ctrl Pts',(55.2649110686365,261.293453221298,20.5565616939928)) ;
#89679 = CARTESIAN_POINT('Ctrl Pts',(55.2649110688686,261.300774597955,20.5589870012318)) ;
#89680 = CARTESIAN_POINT('Ctrl Pts',(55.2649110694204,261.308334792425,20.5615715880227)) ;
#89681 = CARTESIAN_POINT('Ctrl Pts',(55.2649110696691,261.311741518433,20.5627362378311)) ;
#89682 = CARTESIAN_POINT('Ctrl Pts',(55.2649110698818,261.315195489647,20.5639367060361)) ;
#89683 = CARTESIAN_POINT('Ctrl Pts',(55.2649110700281,261.318695106674,20.5651727800032)) ;
#89684 = CARTESIAN_POINT('Ctrl Pts',(55.2649110702299,261.323522550396,20.5668778458623)) ;
#89685 = CARTESIAN_POINT('Ctrl Pts',(55.2649110703085,261.328436825461,20.5686506966079)) ;
#89686 = CARTESIAN_POINT('Ctrl Pts',(55.2649110700846,261.333434936416,20.570490540775)) ;
#89687 = CARTESIAN_POINT('Ctrl Pts',(55.2649110696552,261.343017284311,20.574017878811)) ;
#89688 = CARTESIAN_POINT('Ctrl Pts',(55.264911068135,261.352905770516,20.5777922330151)) ;
#89689 = CARTESIAN_POINT('Ctrl Pts',(55.2649110639489,261.363017322083,20.5817650271008)) ;
#89690 = CARTESIAN_POINT('Ctrl Pts',(55.2649110602374,261.371982469125,20.5852874027631)) ;
#89691 = CARTESIAN_POINT('Ctrl Pts',(55.264911054406,261.381123415544,20.5889627139288)) ;
#89692 = CARTESIAN_POINT('Ctrl Pts',(55.2649110452715,261.39035843418,20.5927355771868)) ;
#89693 = CARTESIAN_POINT('Ctrl Pts',(55.2649110415572,261.394113550621,20.5942696878808)) ;
#89694 = CARTESIAN_POINT('Ctrl Pts',(55.2649110372937,261.397884266899,20.5958197960011)) ;
#89695 = CARTESIAN_POINT('Ctrl Pts',(55.2649110331729,261.401664355739,20.5973841568064)) ;
#89696 = CARTESIAN_POINT('Ctrl Pts',(55.2649110199599,261.413784923579,20.6024001609441)) ;
#89697 = CARTESIAN_POINT('Ctrl Pts',(55.2649110079949,261.425990648584,20.6075720219529)) ;
#89698 = CARTESIAN_POINT('Ctrl Pts',(55.2649110211286,261.438076897157,20.6128139199388)) ;
#89699 = CARTESIAN_POINT('Ctrl Pts',(55.2649110294867,261.445768305083,20.6161497420901)) ;
#89700 = CARTESIAN_POINT('Ctrl Pts',(55.2649110480021,261.453410324451,20.619513524549)) ;
#89701 = CARTESIAN_POINT('Ctrl Pts',(55.2649110819384,261.460963759829,20.622889185544)) ;
#89702 = CARTESIAN_POINT('Ctrl Pts',(55.2649110946635,261.463796083617,20.6241549625655)) ;
#89703 = CARTESIAN_POINT('Ctrl Pts',(55.2649111095407,261.466615960681,20.6254223899507)) ;
#89704 = CARTESIAN_POINT('Ctrl Pts',(55.2649111252154,261.469421281671,20.6266906002001)) ;
#89705 = CARTESIAN_POINT('Ctrl Pts',(55.2649111755076,261.478422182194,20.6307596655011)) ;
#89706 = CARTESIAN_POINT('Ctrl Pts',(55.2649112334233,261.487272197075,20.6348384842092)) ;
#89707 = CARTESIAN_POINT('Ctrl Pts',(55.2649112590157,261.49594352396,20.6389157230749)) ;
#89708 = CARTESIAN_POINT('Ctrl Pts',(55.2649112823866,261.503862131913,20.6426390351511)) ;
#89709 = CARTESIAN_POINT('Ctrl Pts',(55.2649112790021,261.511631875597,20.6463603736446)) ;
#89710 = CARTESIAN_POINT('Ctrl Pts',(55.2649112238241,261.519270955283,20.6500882567231)) ;
#89711 = CARTESIAN_POINT('Ctrl Pts',(55.2649111967476,261.523019534116,20.6519175691757)) ;
#89712 = CARTESIAN_POINT('Ctrl Pts',(55.2649111572818,261.526736725872,20.6537480972418)) ;
#89713 = CARTESIAN_POINT('Ctrl Pts',(55.2649111026463,261.53042995632,20.6555838410976)) ;
#89714 = CARTESIAN_POINT('Ctrl Pts',(55.2649110493035,261.534035797492,20.6573761475535)) ;
#89715 = CARTESIAN_POINT('Ctrl Pts',(55.2649109815467,261.537618800964,20.6591734205906)) ;
#89716 = CARTESIAN_POINT('Ctrl Pts',(55.2649109089552,261.541186632215,20.6609780166873)) ;
#89717 = CARTESIAN_POINT('Ctrl Pts',(55.2649107770721,261.547668610221,20.6642565776356)) ;
#89718 = CARTESIAN_POINT('Ctrl Pts',(55.2649106289493,261.55410517783,20.66756295349)) ;
#89719 = CARTESIAN_POINT('Ctrl Pts',(55.2649105198908,261.560555098686,20.6709200241745)) ;
#89720 = CARTESIAN_POINT('Ctrl Pts',(55.2649104085869,261.567137817086,20.6743462136518)) ;
#89721 = CARTESIAN_POINT('Ctrl Pts',(55.2649103378208,261.573734394714,20.6778251286652)) ;
#89722 = CARTESIAN_POINT('Ctrl Pts',(55.264910370993,261.580353065022,20.6813531377929)) ;
#89723 = CARTESIAN_POINT('Ctrl Pts',(55.264910401248,261.586389691437,20.6845708948508)) ;
#89724 = CARTESIAN_POINT('Ctrl Pts',(55.264910518443,261.592444179297,20.6878294094783)) ;
#89725 = CARTESIAN_POINT('Ctrl Pts',(55.2649107712449,261.598491907439,20.6911062231953)) ;
#89726 = CARTESIAN_POINT('Ctrl Pts',(55.2649108250096,261.599778107717,20.6918031193877)) ;
#89727 = CARTESIAN_POINT('Ctrl Pts',(55.2649108848975,261.601064003873,20.6925008394558)) ;
#89728 = CARTESIAN_POINT('Ctrl Pts',(55.2649109496009,261.602349332226,20.693199220935)) ;
#89729 = CARTESIAN_POINT('Ctrl Pts',(55.2649114635442,261.612558765541,20.6987465031727)) ;
#89730 = CARTESIAN_POINT('Ctrl Pts',(55.2649122753921,261.622729303273,20.7043377443707)) ;
#89731 = CARTESIAN_POINT('Ctrl Pts',(55.264912743211,261.632628552867,20.7098463844237)) ;
#89732 = CARTESIAN_POINT('Ctrl Pts',(55.2649131534803,261.641310030782,20.7146773705005)) ;
#89733 = CARTESIAN_POINT('Ctrl Pts',(55.2649132915559,261.649777221039,20.7194414819695)) ;
#89734 = CARTESIAN_POINT('Ctrl Pts',(55.2649128645567,261.657885102421,20.7240497636966)) ;
#89735 = CARTESIAN_POINT('Ctrl Pts',(55.2649127275021,261.660487501128,20.7255288907142)) ;
#89736 = CARTESIAN_POINT('Ctrl Pts',(55.2649125337714,261.663053367234,20.7269921815504)) ;
#89737 = CARTESIAN_POINT('Ctrl Pts',(55.2649122782257,261.665579368428,20.7284373880131)) ;
#89738 = CARTESIAN_POINT('Ctrl Pts',(55.5095145719656,261.79455482774,20.2277364888237)) ;
#89739 = CARTESIAN_POINT('Ctrl Pts',(55.5011311279772,261.779167461482,20.2255237051989)) ;
#89740 = CARTESIAN_POINT('Ctrl Pts',(55.4854302237238,261.746721466304,20.2213211965547)) ;
#89741 = CARTESIAN_POINT('Ctrl Pts',(55.4649411121345,261.691374789118,20.2150379267643)) ;
#89742 = CARTESIAN_POINT('Ctrl Pts',(55.4472141017732,261.626342713257,20.2085985316935)) ;
#89743 = CARTESIAN_POINT('Ctrl Pts',(55.4320883309197,261.54761255968,20.2014661968594)) ;
#89744 = CARTESIAN_POINT('Ctrl Pts',(55.4201855327187,261.451485192532,20.1924774356911)) ;
#89745 = CARTESIAN_POINT('Ctrl Pts',(55.4127834941959,261.337382234005,20.1809091598321)) ;
#89746 = CARTESIAN_POINT('Ctrl Pts',(55.4106967194038,261.2145920902,20.1714615566787)) ;
#89747 = CARTESIAN_POINT('Ctrl Pts',(55.4113576734741,261.13534727522,20.1677669529664)) ;
#89748 = CARTESIAN_POINT('Ctrl Pts',(55.4113576734741,261.093548013806,20.1677669529664)) ;
#89749 = CARTESIAN_POINT('Ctrl Pts',(55.5340602178732,261.756752943059,20.1881500276994)) ;
#89750 = CARTESIAN_POINT('Ctrl Pts',(55.525623721009,261.742330395001,20.1868005704375)) ;
#89751 = CARTESIAN_POINT('Ctrl Pts',(55.5097976144326,261.711615750798,20.1840390520077)) ;
#89752 = CARTESIAN_POINT('Ctrl Pts',(55.4892611883365,261.658349413846,20.1793261680185)) ;
#89753 = CARTESIAN_POINT('Ctrl Pts',(55.4716399351109,261.594887926556,20.1742186050668)) ;
#89754 = CARTESIAN_POINT('Ctrl Pts',(55.4570261046371,261.517912475163,20.1677768004166)) ;
#89755 = CARTESIAN_POINT('Ctrl Pts',(55.4461750352641,261.4248025452,20.1591893941808)) ;
#89756 = CARTESIAN_POINT('Ctrl Pts',(55.4403075481406,261.316741549714,20.1490460444848)) ;
#89757 = CARTESIAN_POINT('Ctrl Pts',(55.4397672990167,261.203533325761,20.1411593374996)) ;
#89758 = CARTESIAN_POINT('Ctrl Pts',(55.4415682490085,261.131344448697,20.137556377432)) ;
#89759 = CARTESIAN_POINT('Ctrl Pts',(55.4422110272113,261.093548013806,20.1369135992292)) ;
#89760 = CARTESIAN_POINT('Ctrl Pts',(55.5890667713761,261.688545713664,20.1225709708889)) ;
#89761 = CARTESIAN_POINT('Ctrl Pts',(55.5804415216983,261.674930230812,20.1219461679195)) ;
#89762 = CARTESIAN_POINT('Ctrl Pts',(55.5643715025921,261.645549687186,20.1205101639258)) ;
#89763 = CARTESIAN_POINT('Ctrl Pts',(55.5440004208549,261.593366839832,20.1174753224289)) ;
#89764 = CARTESIAN_POINT('Ctrl Pts',(55.5275077045974,261.53074866982,20.1128786169289)) ;
#89765 = CARTESIAN_POINT('Ctrl Pts',(55.5149582126142,261.455358101747,20.1065866956058)) ;
#89766 = CARTESIAN_POINT('Ctrl Pts',(55.507071095585,261.367892543992,20.0991563518021)) ;
#89767 = CARTESIAN_POINT('Ctrl Pts',(55.5044282154051,261.273712249443,20.0923731576416)) ;
#89768 = CARTESIAN_POINT('Ctrl Pts',(55.5065870370321,261.181367979666,20.0871845682348)) ;
#89769 = CARTESIAN_POINT('Ctrl Pts',(55.5102147168921,261.123669597378,20.0844792610867)) ;
#89770 = CARTESIAN_POINT('Ctrl Pts',(55.5120383957876,261.093548013806,20.0833333343921)) ;
#89771 = CARTESIAN_POINT('Ctrl Pts',(55.735413453564,261.557876251656,20.0417117307531)) ;
#89772 = CARTESIAN_POINT('Ctrl Pts',(55.7249293160056,261.543907787696,20.0414514566473)) ;
#89773 = CARTESIAN_POINT('Ctrl Pts',(55.7054852264464,261.513984623845,20.0407144700406)) ;
#89774 = CARTESIAN_POINT('Ctrl Pts',(55.6810670160264,261.463017852386,20.0390718220181)) ;
#89775 = CARTESIAN_POINT('Ctrl Pts',(55.6607837910255,261.405540716534,20.037276875508)) ;
#89776 = CARTESIAN_POINT('Ctrl Pts',(55.644455495605,261.342979538332,20.0357888764937)) ;
#89777 = CARTESIAN_POINT('Ctrl Pts',(55.6330565896902,261.279282393762,20.0349679385755)) ;
#89778 = CARTESIAN_POINT('Ctrl Pts',(55.6274098727185,261.216744008419,20.0346779991369)) ;
#89779 = CARTESIAN_POINT('Ctrl Pts',(55.6277776422459,261.155243093917,20.0342048062941)) ;
#89780 = CARTESIAN_POINT('Ctrl Pts',(55.6319156300806,261.114107180235,20.0332880239655)) ;
#89781 = CARTESIAN_POINT('Ctrl Pts',(55.6340154583308,261.093548013806,20.0328087807883)) ;
#89782 = CARTESIAN_POINT('Ctrl Pts',(55.8502255851785,261.475529765423,20.0213203435596)) ;
#89783 = CARTESIAN_POINT('Ctrl Pts',(55.8372875489689,261.46314325178,20.0213203435596)) ;
#89784 = CARTESIAN_POINT('Ctrl Pts',(55.8129913200325,261.436965535865,20.0213203435596)) ;
#89785 = CARTESIAN_POINT('Ctrl Pts',(55.782270802112,261.393871982293,20.0213203435596)) ;
#89786 = CARTESIAN_POINT('Ctrl Pts',(55.757059342802,261.346599890857,20.0213203435596)) ;
#89787 = CARTESIAN_POINT('Ctrl Pts',(55.7377798655275,261.296394503685,20.0213203435596)) ;
#89788 = CARTESIAN_POINT('Ctrl Pts',(55.7253576978104,261.245518369142,20.0213203435596)) ;
#89789 = CARTESIAN_POINT('Ctrl Pts',(55.7194104036995,261.194000747696,20.0213203435596)) ;
#89790 = CARTESIAN_POINT('Ctrl Pts',(55.7186325494572,261.142659830188,20.0213203435596)) ;
#89791 = CARTESIAN_POINT('Ctrl Pts',(55.7203688071154,261.109892648291,20.0213203435596)) ;
#89792 = CARTESIAN_POINT('Ctrl Pts',(55.7212778327675,261.093548013806,20.0213203435596)) ;
#89793 = CARTESIAN_POINT('Ctrl Pts',(55.9002853073786,261.439128427997,20.0213203435596)) ;
#89794 = CARTESIAN_POINT('Ctrl Pts',(55.8870982395572,261.427398724874,20.0213203435596)) ;
#89795 = CARTESIAN_POINT('Ctrl Pts',(55.8624074372275,261.402653034435,20.0213203435596)) ;
#89796 = CARTESIAN_POINT('Ctrl Pts',(55.8314994101313,261.362343578996,20.0213203435596)) ;
#89797 = CARTESIAN_POINT('Ctrl Pts',(55.8063264068976,261.318668579119,20.0213203435596)) ;
#89798 = CARTESIAN_POINT('Ctrl Pts',(55.7871994190772,261.273156234995,20.0213203435596)) ;
#89799 = CARTESIAN_POINT('Ctrl Pts',(55.7746083733825,261.227740270089,20.0213203435596)) ;
#89800 = CARTESIAN_POINT('Ctrl Pts',(55.7676584903403,261.18196002793,20.0213203435596)) ;
#89801 = CARTESIAN_POINT('Ctrl Pts',(55.7649476045566,261.136640551767,20.0213203435596)) ;
#89802 = CARTESIAN_POINT('Ctrl Pts',(55.7649110640674,261.107859578892,20.0213203435596)) ;
#89803 = CARTESIAN_POINT('Ctrl Pts',(55.7649110640674,261.093548013806,20.0213203435596)) ;
#89804 = CARTESIAN_POINT('',(55.9002853073786,261.439128427997,20.0213203435596)) ;
#89805 = CARTESIAN_POINT('Ctrl Pts',(55.5095145719656,261.79455482774,20.2277364888237)) ;
#89806 = CARTESIAN_POINT('Ctrl Pts',(55.5340602178732,261.756752943059,20.1881500276994)) ;
#89807 = CARTESIAN_POINT('Ctrl Pts',(55.5890667713761,261.688545713664,20.1225709708889)) ;
#89808 = CARTESIAN_POINT('Ctrl Pts',(55.735413453564,261.557876251656,20.0417117307531)) ;
#89809 = CARTESIAN_POINT('Ctrl Pts',(55.8502255851785,261.475529765423,20.0213203435596)) ;
#89810 = CARTESIAN_POINT('Ctrl Pts',(55.9002853073786,261.439128427997,20.0213203435596)) ;
#89811 = CARTESIAN_POINT('',(55.7649110640674,261.093548013806,20.0213203435596)) ;
#89812 = CARTESIAN_POINT('Ctrl Pts',(55.9002853073786,261.439128427997,20.0213203435596)) ;
#89813 = CARTESIAN_POINT('Ctrl Pts',(55.8911225255332,261.430978268137,20.0213203435596)) ;
#89814 = CARTESIAN_POINT('Ctrl Pts',(55.8823626842497,261.422515001751,20.0213203435599)) ;
#89815 = CARTESIAN_POINT('Ctrl Pts',(55.8740745391944,261.413782365245,20.0213203435597)) ;
#89816 = CARTESIAN_POINT('Ctrl Pts',(55.8704346856053,261.409947307084,20.0213203435596)) ;
#89817 = CARTESIAN_POINT('Ctrl Pts',(55.8668841554711,261.40605928624,20.0213203435596)) ;
#89818 = CARTESIAN_POINT('Ctrl Pts',(55.8634283117518,261.402121551956,20.0213203435599)) ;
#89819 = CARTESIAN_POINT('Ctrl Pts',(55.8597986175688,261.397985725112,20.0213203435603)) ;
#89820 = CARTESIAN_POINT('Ctrl Pts',(55.8562733770184,261.393795057419,20.0213203435611)) ;
#89821 = CARTESIAN_POINT('Ctrl Pts',(55.8528506936904,261.389548714247,20.0213203435638)) ;
#89822 = CARTESIAN_POINT('Ctrl Pts',(55.8459105310129,261.380938419465,20.0213203435691)) ;
#89823 = CARTESIAN_POINT('Ctrl Pts',(55.8393976147825,261.372099983805,20.0213203435612)) ;
#89824 = CARTESIAN_POINT('Ctrl Pts',(55.8332886371026,261.36302684571,20.0213203435601)) ;
#89825 = CARTESIAN_POINT('Ctrl Pts',(55.8330098051664,261.362612720664,20.0213203435601)) ;
#89826 = CARTESIAN_POINT('Ctrl Pts',(55.8327318195274,261.362198112044,20.02132034356)) ;
#89827 = CARTESIAN_POINT('Ctrl Pts',(55.8324546776944,261.361783017971,20.02132034356)) ;
#89828 = CARTESIAN_POINT('Ctrl Pts',(55.8266846684896,261.353140884826,20.0213203435592)) ;
#89829 = CARTESIAN_POINT('Ctrl Pts',(55.8212801248487,261.34428846144,20.0213203435596)) ;
#89830 = CARTESIAN_POINT('Ctrl Pts',(55.816247995365,261.335274645693,20.0213203435596)) ;
#89831 = CARTESIAN_POINT('Ctrl Pts',(55.8131313863721,261.329692011281,20.0213203435596)) ;
#89832 = CARTESIAN_POINT('Ctrl Pts',(55.8101586733848,261.324049540243,20.0213203435596)) ;
#89833 = CARTESIAN_POINT('Ctrl Pts',(55.8073336503441,261.318362594802,20.0213203435598)) ;
#89834 = CARTESIAN_POINT('Ctrl Pts',(55.8037773390003,261.311203520949,20.0213203435601)) ;
#89835 = CARTESIAN_POINT('Ctrl Pts',(55.8004550995969,261.303973971199,20.0213203435606)) ;
#89836 = CARTESIAN_POINT('Ctrl Pts',(55.797377237718,261.296712332345,20.0213203435605)) ;
#89837 = CARTESIAN_POINT('Ctrl Pts',(55.7940628302853,261.288892608544,20.0213203435603)) ;
#89838 = CARTESIAN_POINT('Ctrl Pts',(55.7910310881517,261.281034638102,20.0213203435596)) ;
#89839 = CARTESIAN_POINT('Ctrl Pts',(55.7882882555811,261.27317252627,20.0213203435598)) ;
#89840 = CARTESIAN_POINT('Ctrl Pts',(55.7878705140813,261.271975103423,20.0213203435599)) ;
#89841 = CARTESIAN_POINT('Ctrl Pts',(55.7874594806918,261.270777584212,20.0213203435599)) ;
#89842 = CARTESIAN_POINT('Ctrl Pts',(55.7870550706068,261.26957989208,20.0213203435601)) ;
#89843 = CARTESIAN_POINT('Ctrl Pts',(55.7842121766762,261.261160439104,20.0213203435609)) ;
#89844 = CARTESIAN_POINT('Ctrl Pts',(55.7816995351282,261.252741436658,20.0213203435728)) ;
#89845 = CARTESIAN_POINT('Ctrl Pts',(55.7795007628783,261.244326782953,20.0213203435689)) ;
#89846 = CARTESIAN_POINT('Ctrl Pts',(55.7780513827448,261.238780036622,20.0213203435663)) ;
#89847 = CARTESIAN_POINT('Ctrl Pts',(55.7767370713497,261.233234004934,20.0213203435613)) ;
#89848 = CARTESIAN_POINT('Ctrl Pts',(55.7755477954306,261.227679835847,20.0213203435602)) ;
#89849 = CARTESIAN_POINT('Ctrl Pts',(55.7748608844637,261.224471816921,20.0213203435595)) ;
#89850 = CARTESIAN_POINT('Ctrl Pts',(55.7742157070453,261.221261079339,20.0213203435596)) ;
#89851 = CARTESIAN_POINT('Ctrl Pts',(55.7736096920963,261.218047898293,20.0213203435596)) ;
#89852 = CARTESIAN_POINT('Ctrl Pts',(55.7717399027023,261.2081339979,20.0213203435596)) ;
#89853 = CARTESIAN_POINT('Ctrl Pts',(55.7702454216534,261.19819023561,20.0213203435596)) ;
#89854 = CARTESIAN_POINT('Ctrl Pts',(55.7690653662697,261.188266727098,20.0213203435596)) ;
#89855 = CARTESIAN_POINT('Ctrl Pts',(55.7688182504891,261.186188641962,20.0213203435596)) ;
#89856 = CARTESIAN_POINT('Ctrl Pts',(55.7685848703948,261.184111917233,20.0213203435596)) ;
#89857 = CARTESIAN_POINT('Ctrl Pts',(55.7683646635995,261.182036903631,20.0213203435597)) ;
#89858 = CARTESIAN_POINT('Ctrl Pts',(55.76742212904,261.173155379204,20.0213203435601)) ;
#89859 = CARTESIAN_POINT('Ctrl Pts',(55.7667209439631,261.164305165404,20.0213203435655)) ;
#89860 = CARTESIAN_POINT('Ctrl Pts',(55.7662109000418,261.155542863057,20.021320343563)) ;
#89861 = CARTESIAN_POINT('Ctrl Pts',(55.7658483474578,261.149314388948,20.0213203435611)) ;
#89862 = CARTESIAN_POINT('Ctrl Pts',(55.765581273064,261.143128087237,20.0213203435599)) ;
#89863 = CARTESIAN_POINT('Ctrl Pts',(55.7653895517551,261.136998650066,20.0213203435601)) ;
#89864 = CARTESIAN_POINT('Ctrl Pts',(55.765319811409,261.134769012308,20.0213203435602)) ;
#89865 = CARTESIAN_POINT('Ctrl Pts',(55.7652600481747,261.132546901807,20.0213203435604)) ;
#89866 = CARTESIAN_POINT('Ctrl Pts',(55.7652087553039,261.130331096701,20.0213203435613)) ;
#89867 = CARTESIAN_POINT('Ctrl Pts',(55.7650413523549,261.123099442408,20.0213203435642)) ;
#89868 = CARTESIAN_POINT('Ctrl Pts',(55.7649659237062,261.1159466348,20.0213203435738)) ;
#89869 = CARTESIAN_POINT('Ctrl Pts',(55.7649342294194,261.108847738531,20.0213203435675)) ;
#89870 = CARTESIAN_POINT('Ctrl Pts',(55.7649113765851,261.10372915356,20.0213203435629)) ;
#89871 = CARTESIAN_POINT('Ctrl Pts',(55.7649110640674,261.098637903367,20.0213203435596)) ;
#89872 = CARTESIAN_POINT('Ctrl Pts',(55.7649110640674,261.093548013806,20.0213203435596)) ;
#89873 = CARTESIAN_POINT('Origin',(55.7649110640674,261.093548013806,20.5213203435596)) ;
#89874 = CARTESIAN_POINT('Origin',(65.2229283731508,226.843027476095,16.0213203435596)) ;
#89875 = CARTESIAN_POINT('',(65.2229283731508,226.843027476095,16.0213203435596)) ;
#89876 = CARTESIAN_POINT('',(63.9568984489966,226.843027476095,16.0213203435596)) ;
#89877 = CARTESIAN_POINT('',(67.6578947220605,226.843027476095,16.0213203435596)) ;
#89878 = CARTESIAN_POINT('',(65.2229283731508,226.843027476095,16.3213203435596)) ;
#89879 = CARTESIAN_POINT('',(65.2229283731508,226.843027476095,16.0213203435596)) ;
#89880 = CARTESIAN_POINT('',(63.9568984489966,226.843027476095,16.3213203435596)) ;
#89881 = CARTESIAN_POINT('',(65.2229283731508,226.843027476095,16.3213203435596)) ;
#89882 = CARTESIAN_POINT('',(63.9568984489966,226.843027476095,16.0213203435596)) ;
#89883 = CARTESIAN_POINT('Ctrl Pts',(65.8723144214678,227.025837901854,16.0213203435596)) ;
#89884 = CARTESIAN_POINT('Ctrl Pts',(65.8723144214678,227.025837901854,16.3813203435596)) ;
#89885 = CARTESIAN_POINT('Ctrl Pts',(65.7863625985753,226.972747188495,16.0213203435596)) ;
#89886 = CARTESIAN_POINT('Ctrl Pts',(65.7863625985753,226.972747188495,16.3813203435596)) ;
#89887 = CARTESIAN_POINT('Ctrl Pts',(65.5886928398511,226.850650551717,16.0213203435596)) ;
#89888 = CARTESIAN_POINT('Ctrl Pts',(65.5886928398511,226.850650551717,16.3813203435596)) ;
#89889 = CARTESIAN_POINT('Ctrl Pts',(65.3550036041292,226.845780120393,16.0213203435596)) ;
#89890 = CARTESIAN_POINT('Ctrl Pts',(65.3550036041292,226.845780120393,16.3813203435596)) ;
#89891 = CARTESIAN_POINT('Ctrl Pts',(65.2229283731508,226.843027476095,16.0213203435596)) ;
#89892 = CARTESIAN_POINT('Ctrl Pts',(65.2229283731508,226.843027476095,16.3813203435596)) ;
#89893 = CARTESIAN_POINT('',(65.8723144214678,227.025837901854,16.0213203435596)) ;
#89894 = CARTESIAN_POINT('Ctrl Pts',(65.8723144214678,227.025837901854,16.0213203435596)) ;
#89895 = CARTESIAN_POINT('Ctrl Pts',(65.7863625985753,226.972747188495,16.0213203435596)) ;
#89896 = CARTESIAN_POINT('Ctrl Pts',(65.5886928398511,226.850650551717,16.0213203435596)) ;
#89897 = CARTESIAN_POINT('Ctrl Pts',(65.3550036041292,226.845780120393,16.0213203435596)) ;
#89898 = CARTESIAN_POINT('Ctrl Pts',(65.2229283731508,226.843027476095,16.0213203435596)) ;
#89899 = CARTESIAN_POINT('',(65.8723144214678,227.025837901854,16.3213203435596)) ;
#89900 = CARTESIAN_POINT('',(65.8723144214678,227.025837901854,16.0213203435596)) ;
#89901 = CARTESIAN_POINT('Ctrl Pts',(65.8723144214678,227.025837901854,16.3213203435596)) ;
#89902 = CARTESIAN_POINT('Ctrl Pts',(65.7863625985753,226.972747188495,16.3213203435596)) ;
#89903 = CARTESIAN_POINT('Ctrl Pts',(65.5886928398511,226.850650551717,16.3213203435596)) ;
#89904 = CARTESIAN_POINT('Ctrl Pts',(65.3550036041292,226.845780120393,16.3213203435596)) ;
#89905 = CARTESIAN_POINT('Ctrl Pts',(65.2229283731508,226.843027476095,16.3213203435596)) ;
#89906 = CARTESIAN_POINT('Ctrl Pts',(66.0796813648272,227.492413524412,16.0213203435596)) ;
#89907 = CARTESIAN_POINT('Ctrl Pts',(66.0796813648272,227.492413524412,16.3813203435596)) ;
#89908 = CARTESIAN_POINT('Ctrl Pts',(66.0713027278811,227.402263576791,16.0213203435596)) ;
#89909 = CARTESIAN_POINT('Ctrl Pts',(66.0713027278811,227.402263576791,16.3813203435596)) ;
#89910 = CARTESIAN_POINT('Ctrl Pts',(66.0546699670268,227.22330337963,16.0213203435596)) ;
#89911 = CARTESIAN_POINT('Ctrl Pts',(66.0546699670268,227.22330337963,16.3813203435596)) ;
#89912 = CARTESIAN_POINT('Ctrl Pts',(65.9327954854,227.091330410728,16.0213203435596)) ;
#89913 = CARTESIAN_POINT('Ctrl Pts',(65.9327954854,227.091330410728,16.3813203435596)) ;
#89914 = CARTESIAN_POINT('Ctrl Pts',(65.8723144214678,227.025837901854,16.0213203435596)) ;
#89915 = CARTESIAN_POINT('Ctrl Pts',(65.8723144214678,227.025837901854,16.3813203435596)) ;
#89916 = CARTESIAN_POINT('',(66.0796813648272,227.492413524412,16.0213203435596)) ;
#89917 = CARTESIAN_POINT('Ctrl Pts',(66.0796813648272,227.492413524412,16.0213203435596)) ;
#89918 = CARTESIAN_POINT('Ctrl Pts',(66.0713027278811,227.402263576791,16.0213203435596)) ;
#89919 = CARTESIAN_POINT('Ctrl Pts',(66.0546699670268,227.22330337963,16.0213203435596)) ;
#89920 = CARTESIAN_POINT('Ctrl Pts',(65.9327954854,227.091330410728,16.0213203435596)) ;
#89921 = CARTESIAN_POINT('Ctrl Pts',(65.8723144214678,227.025837901854,16.0213203435596)) ;
#89922 = CARTESIAN_POINT('',(66.0796813648272,227.492413524412,16.3213203435596)) ;
#89923 = CARTESIAN_POINT('',(66.0796813648272,227.492413524412,16.0213203435596)) ;
#89924 = CARTESIAN_POINT('Ctrl Pts',(66.0796813648272,227.492413524412,16.3213203435596)) ;
#89925 = CARTESIAN_POINT('Ctrl Pts',(66.0713027278811,227.402263576791,16.3213203435596)) ;
#89926 = CARTESIAN_POINT('Ctrl Pts',(66.0546699670268,227.22330337963,16.3213203435596)) ;
#89927 = CARTESIAN_POINT('Ctrl Pts',(65.9327954854,227.091330410728,16.3213203435596)) ;
#89928 = CARTESIAN_POINT('Ctrl Pts',(65.8723144214678,227.025837901854,16.3213203435596)) ;
#89929 = CARTESIAN_POINT('Ctrl Pts',(65.9732694905329,227.852577272677,16.0213203435596)) ;
#89930 = CARTESIAN_POINT('Ctrl Pts',(65.9732694905329,227.852577272677,16.3813203435596)) ;
#89931 = CARTESIAN_POINT('Ctrl Pts',(66.0043061588733,227.796130023554,16.0213203435596)) ;
#89932 = CARTESIAN_POINT('Ctrl Pts',(66.0043061588733,227.796130023554,16.3813203435596)) ;
#89933 = CARTESIAN_POINT('Ctrl Pts',(66.0660587532603,227.68381886821,16.0213203435596)) ;
#89934 = CARTESIAN_POINT('Ctrl Pts',(66.0660587532603,227.68381886821,16.3813203435596)) ;
#89935 = CARTESIAN_POINT('Ctrl Pts',(66.0751562450622,227.555993998691,16.0213203435596)) ;
#89936 = CARTESIAN_POINT('Ctrl Pts',(66.0751562450622,227.555993998691,16.3813203435596)) ;
#89937 = CARTESIAN_POINT('Ctrl Pts',(66.0796813648272,227.492413524412,16.0213203435596)) ;
#89938 = CARTESIAN_POINT('Ctrl Pts',(66.0796813648272,227.492413524412,16.3813203435596)) ;
#89939 = CARTESIAN_POINT('',(65.9732694905329,227.852577272677,16.0213203435596)) ;
#89940 = CARTESIAN_POINT('Ctrl Pts',(65.9732694905329,227.852577272677,16.0213203435596)) ;
#89941 = CARTESIAN_POINT('Ctrl Pts',(66.0043061588733,227.796130023554,16.0213203435596)) ;
#89942 = CARTESIAN_POINT('Ctrl Pts',(66.0660587532603,227.68381886821,16.0213203435596)) ;
#89943 = CARTESIAN_POINT('Ctrl Pts',(66.0751562450622,227.555993998691,16.0213203435596)) ;
#89944 = CARTESIAN_POINT('Ctrl Pts',(66.0796813648272,227.492413524412,16.0213203435596)) ;
#89945 = CARTESIAN_POINT('',(65.9732694905329,227.852577272677,16.3213203435596)) ;
#89946 = CARTESIAN_POINT('',(65.9732694905329,227.852577272677,16.0213203435596)) ;
#89947 = CARTESIAN_POINT('Ctrl Pts',(65.9732694905329,227.852577272677,16.3213203435596)) ;
#89948 = CARTESIAN_POINT('Ctrl Pts',(66.0043061588733,227.796130023554,16.3213203435596)) ;
#89949 = CARTESIAN_POINT('Ctrl Pts',(66.0660587532603,227.68381886821,16.3213203435596)) ;
#89950 = CARTESIAN_POINT('Ctrl Pts',(66.0751562450622,227.555993998691,16.3213203435596)) ;
#89951 = CARTESIAN_POINT('Ctrl Pts',(66.0796813648272,227.492413524412,16.3213203435596)) ;
#89952 = CARTESIAN_POINT('Ctrl Pts',(65.6622190754938,228.092686537527,16.0213203435596)) ;
#89953 = CARTESIAN_POINT('Ctrl Pts',(65.6622190754938,228.092686537527,16.3813203435596)) ;
#89954 = CARTESIAN_POINT('Ctrl Pts',(65.7257617097583,228.064451825508,16.0213203435596)) ;
#89955 = CARTESIAN_POINT('Ctrl Pts',(65.7257617097583,228.064451825508,16.3813203435596)) ;
#89956 = CARTESIAN_POINT('Ctrl Pts',(65.8491174447405,228.009639592847,16.0213203435596)) ;
#89957 = CARTESIAN_POINT('Ctrl Pts',(65.8491174447405,228.009639592847,16.3813203435596)) ;
#89958 = CARTESIAN_POINT('Ctrl Pts',(65.932728102633,227.903865388034,16.0213203435596)) ;
#89959 = CARTESIAN_POINT('Ctrl Pts',(65.932728102633,227.903865388034,16.3813203435596)) ;
#89960 = CARTESIAN_POINT('Ctrl Pts',(65.9732694905329,227.852577272677,16.0213203435596)) ;
#89961 = CARTESIAN_POINT('Ctrl Pts',(65.9732694905329,227.852577272677,16.3813203435596)) ;
#89962 = CARTESIAN_POINT('',(65.6622190754938,228.092686537527,16.0213203435596)) ;
#89963 = CARTESIAN_POINT('Ctrl Pts',(65.6622190754938,228.092686537527,16.0213203435596)) ;
#89964 = CARTESIAN_POINT('Ctrl Pts',(65.7257617097583,228.064451825508,16.0213203435596)) ;
#89965 = CARTESIAN_POINT('Ctrl Pts',(65.8491174447405,228.009639592847,16.0213203435596)) ;
#89966 = CARTESIAN_POINT('Ctrl Pts',(65.932728102633,227.903865388034,16.0213203435596)) ;
#89967 = CARTESIAN_POINT('Ctrl Pts',(65.9732694905329,227.852577272677,16.0213203435596)) ;
#89968 = CARTESIAN_POINT('',(65.6622190754938,228.092686537527,16.3213203435596)) ;
#89969 = CARTESIAN_POINT('',(65.6622190754938,228.092686537527,16.0213203435596)) ;
#89970 = CARTESIAN_POINT('Ctrl Pts',(65.6622190754938,228.092686537527,16.3213203435596)) ;
#89971 = CARTESIAN_POINT('Ctrl Pts',(65.7257617097583,228.064451825508,16.3213203435596)) ;
#89972 = CARTESIAN_POINT('Ctrl Pts',(65.8491174447405,228.009639592847,16.3213203435596)) ;
#89973 = CARTESIAN_POINT('Ctrl Pts',(65.932728102633,227.903865388034,16.3213203435596)) ;
#89974 = CARTESIAN_POINT('Ctrl Pts',(65.9732694905329,227.852577272677,16.3213203435596)) ;
#89975 = CARTESIAN_POINT('Ctrl Pts',(65.0946882348585,228.166356388354,16.0213203435596)) ;
#89976 = CARTESIAN_POINT('Ctrl Pts',(65.0946882348585,228.166356388354,16.3813203435596)) ;
#89977 = CARTESIAN_POINT('Ctrl Pts',(65.2031657201074,228.165203721958,16.0213203435596)) ;
#89978 = CARTESIAN_POINT('Ctrl Pts',(65.2031657201074,228.165203721958,16.3813203435596)) ;
#89979 = CARTESIAN_POINT('Ctrl Pts',(65.3955084524701,228.163159915324,16.0213203435596)) ;
#89980 = CARTESIAN_POINT('Ctrl Pts',(65.3955084524701,228.163159915324,16.3813203435596)) ;
#89981 = CARTESIAN_POINT('Ctrl Pts',(65.5812375182262,228.114084424928,16.0213203435596)) ;
#89982 = CARTESIAN_POINT('Ctrl Pts',(65.5812375182262,228.114084424928,16.3813203435596)) ;
#89983 = CARTESIAN_POINT('Ctrl Pts',(65.6622190754938,228.092686537527,16.0213203435596)) ;
#89984 = CARTESIAN_POINT('Ctrl Pts',(65.6622190754938,228.092686537527,16.3813203435596)) ;
#89985 = CARTESIAN_POINT('',(65.0946882348585,228.166356388354,16.0213203435596)) ;
#89986 = CARTESIAN_POINT('Ctrl Pts',(65.0946882348585,228.166356388354,16.0213203435596)) ;
#89987 = CARTESIAN_POINT('Ctrl Pts',(65.2031657201074,228.165203721958,16.0213203435596)) ;
#89988 = CARTESIAN_POINT('Ctrl Pts',(65.3955084524701,228.163159915324,16.0213203435596)) ;
#89989 = CARTESIAN_POINT('Ctrl Pts',(65.5812375182262,228.114084424928,16.0213203435596)) ;
#89990 = CARTESIAN_POINT('Ctrl Pts',(65.6622190754938,228.092686537527,16.0213203435596)) ;
#89991 = CARTESIAN_POINT('',(65.0946882348585,228.166356388354,16.3213203435596)) ;
#89992 = CARTESIAN_POINT('',(65.0946882348585,228.166356388354,16.0213203435596)) ;
#89993 = CARTESIAN_POINT('Ctrl Pts',(65.0946882348585,228.166356388354,16.3213203435596)) ;
#89994 = CARTESIAN_POINT('Ctrl Pts',(65.2031657201074,228.165203721958,16.3213203435596)) ;
#89995 = CARTESIAN_POINT('Ctrl Pts',(65.3955084524701,228.163159915324,16.3213203435596)) ;
#89996 = CARTESIAN_POINT('Ctrl Pts',(65.5812375182262,228.114084424928,16.3213203435596)) ;
#89997 = CARTESIAN_POINT('Ctrl Pts',(65.6622190754938,228.092686537527,16.3213203435596)) ;
#89998 = CARTESIAN_POINT('Origin',(63.9568984489966,228.166356388354,16.0213203435596)) ;
#89999 = CARTESIAN_POINT('',(63.9568984489966,228.166356388354,16.0213203435596)) ;
#90000 = CARTESIAN_POINT('',(67.0248797599834,228.166356388354,16.0213203435596)) ;
#90001 = CARTESIAN_POINT('',(63.9568984489966,228.166356388354,16.3213203435596)) ;
#90002 = CARTESIAN_POINT('',(63.9568984489966,228.166356388354,16.0213203435596)) ;
#90003 = CARTESIAN_POINT('',(63.9568984489966,228.166356388354,16.3213203435596)) ;
#90004 = CARTESIAN_POINT('Origin',(63.9568984489966,226.843027476095,16.0213203435596)) ;
#90005 = CARTESIAN_POINT('',(63.9568984489966,228.43789484464,16.0213203435596)) ;
#90006 = CARTESIAN_POINT('',(63.9568984489966,226.843027476095,16.3213203435596)) ;
#90007 = CARTESIAN_POINT('Origin',(63.9568984489966,228.624746505045,16.0213203435596)) ;
#90008 = CARTESIAN_POINT('',(63.9568984489966,228.624746505045,16.0213203435596)) ;
#90009 = CARTESIAN_POINT('',(63.9568984489966,230.401008430742,16.0213203435596)) ;
#90010 = CARTESIAN_POINT('',(63.9568984489966,229.328754359115,16.0213203435596)) ;
#90011 = CARTESIAN_POINT('',(63.9568984489966,228.624746505045,16.3213203435596)) ;
#90012 = CARTESIAN_POINT('',(63.9568984489966,228.624746505045,16.0213203435596)) ;
#90013 = CARTESIAN_POINT('',(63.9568984489966,230.401008430742,16.3213203435596)) ;
#90014 = CARTESIAN_POINT('',(63.9568984489966,228.624746505045,16.3213203435596)) ;
#90015 = CARTESIAN_POINT('',(63.9568984489966,230.401008430742,16.0213203435596)) ;
#90016 = CARTESIAN_POINT('Origin',(64.5708137732077,228.624746505045,16.0213203435596)) ;
#90017 = CARTESIAN_POINT('',(64.5708137732077,228.624746505045,16.0213203435596)) ;
#90018 = CARTESIAN_POINT('',(67.3318374220889,228.624746505045,16.0213203435596)) ;
#90019 = CARTESIAN_POINT('',(64.5708137732077,228.624746505045,16.3213203435596)) ;
#90020 = CARTESIAN_POINT('',(64.5708137732077,228.624746505045,16.0213203435596)) ;
#90021 = CARTESIAN_POINT('',(64.5708137732077,228.624746505045,16.3213203435596)) ;
#90022 = CARTESIAN_POINT('Ctrl Pts',(64.8654931765127,228.643846217417,16.0213203435596)) ;
#90023 = CARTESIAN_POINT('Ctrl Pts',(64.8654931765127,228.643846217417,16.3813203435596)) ;
#90024 = CARTESIAN_POINT('Ctrl Pts',(64.8259848410755,228.638324287067,16.0213203435596)) ;
#90025 = CARTESIAN_POINT('Ctrl Pts',(64.8259848410755,228.638324287067,16.3813203435596)) ;
#90026 = CARTESIAN_POINT('Ctrl Pts',(64.7282957987508,228.624670659758,16.0213203435596)) ;
#90027 = CARTESIAN_POINT('Ctrl Pts',(64.7282957987508,228.624670659758,16.3813203435596)) ;
#90028 = CARTESIAN_POINT('Ctrl Pts',(64.6295962862642,228.624718194661,16.0213203435596)) ;
#90029 = CARTESIAN_POINT('Ctrl Pts',(64.6295962862642,228.624718194661,16.3813203435596)) ;
#90030 = CARTESIAN_POINT('Ctrl Pts',(64.5708137732077,228.624746505045,16.0213203435596)) ;
#90031 = CARTESIAN_POINT('Ctrl Pts',(64.5708137732077,228.624746505045,16.3813203435596)) ;
#90032 = CARTESIAN_POINT('',(64.8654931765127,228.643846217417,16.0213203435596)) ;
#90033 = CARTESIAN_POINT('Ctrl Pts',(64.8654931765127,228.643846217417,16.0213203435596)) ;
#90034 = CARTESIAN_POINT('Ctrl Pts',(64.8259848410755,228.638324287067,16.0213203435596)) ;
#90035 = CARTESIAN_POINT('Ctrl Pts',(64.7282957987508,228.624670659758,16.0213203435596)) ;
#90036 = CARTESIAN_POINT('Ctrl Pts',(64.6295962862642,228.624718194661,16.0213203435596)) ;
#90037 = CARTESIAN_POINT('Ctrl Pts',(64.5708137732077,228.624746505045,16.0213203435596)) ;
#90038 = CARTESIAN_POINT('',(64.8654931765127,228.643846217417,16.3213203435596)) ;
#90039 = CARTESIAN_POINT('',(64.8654931765127,228.643846217417,16.0213203435596)) ;
#90040 = CARTESIAN_POINT('Ctrl Pts',(64.8654931765127,228.643846217417,16.3213203435596)) ;
#90041 = CARTESIAN_POINT('Ctrl Pts',(64.8259848410755,228.638324287067,16.3213203435596)) ;
#90042 = CARTESIAN_POINT('Ctrl Pts',(64.7282957987508,228.624670659758,16.3213203435596)) ;
#90043 = CARTESIAN_POINT('Ctrl Pts',(64.6295962862642,228.624718194661,16.3213203435596)) ;
#90044 = CARTESIAN_POINT('Ctrl Pts',(64.5708137732077,228.624746505045,16.3213203435596)) ;
#90045 = CARTESIAN_POINT('Ctrl Pts',(65.1056022923517,228.750258091711,16.0213203435596)) ;
#90046 = CARTESIAN_POINT('Ctrl Pts',(65.1056022923517,228.750258091711,16.3813203435596)) ;
#90047 = CARTESIAN_POINT('Ctrl Pts',(65.0668285289302,228.726864738102,16.0213203435596)) ;
#90048 = CARTESIAN_POINT('Ctrl Pts',(65.0668285289302,228.726864738102,16.3813203435596)) ;
#90049 = CARTESIAN_POINT('Ctrl Pts',(64.9912530832381,228.681267845533,16.0213203435596)) ;
#90050 = CARTESIAN_POINT('Ctrl Pts',(64.9912530832381,228.681267845533,16.3813203435596)) ;
#90051 = CARTESIAN_POINT('Ctrl Pts',(64.9066775012378,228.656101192188,16.0213203435596)) ;
#90052 = CARTESIAN_POINT('Ctrl Pts',(64.9066775012378,228.656101192188,16.3813203435596)) ;
#90053 = CARTESIAN_POINT('Ctrl Pts',(64.8654931765127,228.643846217417,16.0213203435596)) ;
#90054 = CARTESIAN_POINT('Ctrl Pts',(64.8654931765127,228.643846217417,16.3813203435596)) ;
#90055 = CARTESIAN_POINT('',(65.1056022923517,228.750258091711,16.0213203435596)) ;
#90056 = CARTESIAN_POINT('Ctrl Pts',(65.1056022923517,228.750258091711,16.0213203435596)) ;
#90057 = CARTESIAN_POINT('Ctrl Pts',(65.0668285289302,228.726864738102,16.0213203435596)) ;
#90058 = CARTESIAN_POINT('Ctrl Pts',(64.9912530832381,228.681267845533,16.0213203435596)) ;
#90059 = CARTESIAN_POINT('Ctrl Pts',(64.9066775012378,228.656101192188,16.0213203435596)) ;
#90060 = CARTESIAN_POINT('Ctrl Pts',(64.8654931765127,228.643846217417,16.0213203435596)) ;
#90061 = CARTESIAN_POINT('',(65.1056022923517,228.750258091711,16.3213203435596)) ;
#90062 = CARTESIAN_POINT('',(65.1056022923517,228.750258091711,16.0213203435596)) ;
#90063 = CARTESIAN_POINT('Ctrl Pts',(65.1056022923517,228.750258091711,16.3213203435596)) ;
#90064 = CARTESIAN_POINT('Ctrl Pts',(65.0668285289302,228.726864738102,16.3213203435596)) ;
#90065 = CARTESIAN_POINT('Ctrl Pts',(64.9912530832381,228.681267845533,16.3213203435596)) ;
#90066 = CARTESIAN_POINT('Ctrl Pts',(64.9066775012378,228.656101192188,16.3213203435596)) ;
#90067 = CARTESIAN_POINT('Ctrl Pts',(64.8654931765127,228.643846217417,16.3213203435596)) ;
#90068 = CARTESIAN_POINT('Ctrl Pts',(65.3757251780558,229.017652574801,16.0213203435596)) ;
#90069 = CARTESIAN_POINT('Ctrl Pts',(65.3757251780558,229.017652574801,16.3813203435596)) ;
#90070 = CARTESIAN_POINT('Ctrl Pts',(65.3304906114513,228.961176354081,16.0213203435596)) ;
#90071 = CARTESIAN_POINT('Ctrl Pts',(65.3304906114513,228.961176354081,16.3813203435596)) ;
#90072 = CARTESIAN_POINT('Ctrl Pts',(65.2506597476853,228.861505995311,16.0213203435596)) ;
#90073 = CARTESIAN_POINT('Ctrl Pts',(65.2506597476853,228.861505995311,16.3813203435596)) ;
#90074 = CARTESIAN_POINT('Ctrl Pts',(65.1494594569405,228.783893161395,16.0213203435596)) ;
#90075 = CARTESIAN_POINT('Ctrl Pts',(65.1494594569405,228.783893161395,16.3813203435596)) ;
#90076 = CARTESIAN_POINT('Ctrl Pts',(65.1056022923517,228.750258091711,16.0213203435596)) ;
#90077 = CARTESIAN_POINT('Ctrl Pts',(65.1056022923517,228.750258091711,16.3813203435596)) ;
#90078 = CARTESIAN_POINT('',(65.3757251780558,229.017652574801,16.0213203435596)) ;
#90079 = CARTESIAN_POINT('Ctrl Pts',(65.3757251780558,229.017652574801,16.0213203435596)) ;
#90080 = CARTESIAN_POINT('Ctrl Pts',(65.3304906114513,228.961176354081,16.0213203435596)) ;
#90081 = CARTESIAN_POINT('Ctrl Pts',(65.2506597476853,228.861505995311,16.0213203435596)) ;
#90082 = CARTESIAN_POINT('Ctrl Pts',(65.1494594569405,228.783893161395,16.0213203435596)) ;
#90083 = CARTESIAN_POINT('Ctrl Pts',(65.1056022923517,228.750258091711,16.0213203435596)) ;
#90084 = CARTESIAN_POINT('',(65.3757251780558,229.017652574801,16.3213203435596)) ;
#90085 = CARTESIAN_POINT('',(65.3757251780558,229.017652574801,16.0213203435596)) ;
#90086 = CARTESIAN_POINT('Ctrl Pts',(65.3757251780558,229.017652574801,16.3213203435596)) ;
#90087 = CARTESIAN_POINT('Ctrl Pts',(65.3304906114513,228.961176354081,16.3213203435596)) ;
#90088 = CARTESIAN_POINT('Ctrl Pts',(65.2506597476853,228.861505995311,16.3213203435596)) ;
#90089 = CARTESIAN_POINT('Ctrl Pts',(65.1494594569405,228.783893161395,16.3213203435596)) ;
#90090 = CARTESIAN_POINT('Ctrl Pts',(65.1056022923517,228.750258091711,16.3213203435596)) ;
#90091 = CARTESIAN_POINT('Ctrl Pts',(65.7577170413065,229.568811956667,16.0213203435596)) ;
#90092 = CARTESIAN_POINT('Ctrl Pts',(65.7577170413065,229.568811956667,16.3813203435596)) ;
#90093 = CARTESIAN_POINT('Ctrl Pts',(65.6885436027166,229.461938549579,16.0213203435596)) ;
#90094 = CARTESIAN_POINT('Ctrl Pts',(65.6885436027166,229.461938549579,16.3813203435596)) ;
#90095 = CARTESIAN_POINT('Ctrl Pts',(65.5670128336211,229.274172730444,16.0213203435596)) ;
#90096 = CARTESIAN_POINT('Ctrl Pts',(65.5670128336211,229.274172730444,16.3813203435596)) ;
#90097 = CARTESIAN_POINT('Ctrl Pts',(65.4333214772105,229.094890238569,16.0213203435596)) ;
#90098 = CARTESIAN_POINT('Ctrl Pts',(65.4333214772105,229.094890238569,16.3813203435596)) ;
#90099 = CARTESIAN_POINT('Ctrl Pts',(65.3757251780558,229.017652574801,16.0213203435596)) ;
#90100 = CARTESIAN_POINT('Ctrl Pts',(65.3757251780558,229.017652574801,16.3813203435596)) ;
#90101 = CARTESIAN_POINT('',(65.7577170413065,229.568811956667,16.0213203435596)) ;
#90102 = CARTESIAN_POINT('Ctrl Pts',(65.7577170413065,229.568811956667,16.0213203435596)) ;
#90103 = CARTESIAN_POINT('Ctrl Pts',(65.6885436027166,229.461938549579,16.0213203435596)) ;
#90104 = CARTESIAN_POINT('Ctrl Pts',(65.5670128336211,229.274172730444,16.0213203435596)) ;
#90105 = CARTESIAN_POINT('Ctrl Pts',(65.4333214772105,229.094890238569,16.0213203435596)) ;
#90106 = CARTESIAN_POINT('Ctrl Pts',(65.3757251780558,229.017652574801,16.0213203435596)) ;
#90107 = CARTESIAN_POINT('',(65.7577170413065,229.568811956667,16.3213203435596)) ;
#90108 = CARTESIAN_POINT('',(65.7577170413065,229.568811956667,16.0213203435596)) ;
#90109 = CARTESIAN_POINT('Ctrl Pts',(65.7577170413065,229.568811956667,16.3213203435596)) ;
#90110 = CARTESIAN_POINT('Ctrl Pts',(65.6885436027166,229.461938549579,16.3213203435596)) ;
#90111 = CARTESIAN_POINT('Ctrl Pts',(65.5670128336211,229.274172730444,16.3213203435596)) ;
#90112 = CARTESIAN_POINT('Ctrl Pts',(65.4333214772105,229.094890238569,16.3213203435596)) ;
#90113 = CARTESIAN_POINT('Ctrl Pts',(65.3757251780558,229.017652574801,16.3213203435596)) ;
#90114 = CARTESIAN_POINT('Origin',(66.2870483081865,230.401008430742,16.0213203435596)) ;
#90115 = CARTESIAN_POINT('',(66.2870483081865,230.401008430742,16.0213203435596)) ;
#90116 = CARTESIAN_POINT('',(66.7517866175368,231.131654071021,16.0213203435596)) ;
#90117 = CARTESIAN_POINT('',(66.2870483081865,230.401008430742,16.3213203435596)) ;
#90118 = CARTESIAN_POINT('',(66.2870483081865,230.401008430742,16.0213203435596)) ;
#90119 = CARTESIAN_POINT('',(66.2870483081865,230.401008430742,16.3213203435596)) ;
#90120 = CARTESIAN_POINT('Origin',(66.9528056662607,230.401008430742,16.0213203435596)) ;
#90121 = CARTESIAN_POINT('',(66.9528056662607,230.401008430742,16.0213203435596)) ;
#90122 = CARTESIAN_POINT('',(68.5228333686155,230.401008430742,16.0213203435596)) ;
#90123 = CARTESIAN_POINT('',(66.9528056662607,230.401008430742,16.3213203435596)) ;
#90124 = CARTESIAN_POINT('',(66.9528056662607,230.401008430742,16.0213203435596)) ;
#90125 = CARTESIAN_POINT('',(66.9528056662607,230.401008430742,16.3213203435596)) ;
#90126 = CARTESIAN_POINT('Origin',(66.2570346873331,229.312331680082,16.0213203435596)) ;
#90127 = CARTESIAN_POINT('',(66.2570346873331,229.312331680082,16.0213203435596)) ;
#90128 = CARTESIAN_POINT('',(66.976676663234,230.438359513508,16.0213203435596)) ;
#90129 = CARTESIAN_POINT('',(66.2570346873331,229.312331680082,16.3213203435596)) ;
#90130 = CARTESIAN_POINT('',(66.2570346873331,229.312331680082,16.0213203435596)) ;
#90131 = CARTESIAN_POINT('',(66.2570346873331,229.312331680082,16.3213203435596)) ;
#90132 = CARTESIAN_POINT('Ctrl Pts',(65.8177442830134,228.780271712565,16.0213203435596)) ;
#90133 = CARTESIAN_POINT('Ctrl Pts',(65.8177442830134,228.780271712565,16.3813203435596)) ;
#90134 = CARTESIAN_POINT('Ctrl Pts',(65.8955297605029,228.857983910561,16.0213203435596)) ;
#90135 = CARTESIAN_POINT('Ctrl Pts',(65.8955297605029,228.857983910561,16.3813203435596)) ;
#90136 = CARTESIAN_POINT('Ctrl Pts',(66.0589351598689,229.021235370333,16.0213203435596)) ;
#90137 = CARTESIAN_POINT('Ctrl Pts',(66.0589351598689,229.021235370333,16.3813203435596)) ;
#90138 = CARTESIAN_POINT('Ctrl Pts',(66.1889240792206,229.212246904868,16.0213203435596)) ;
#90139 = CARTESIAN_POINT('Ctrl Pts',(66.1889240792206,229.212246904868,16.3813203435596)) ;
#90140 = CARTESIAN_POINT('Ctrl Pts',(66.2570346873331,229.312331680082,16.0213203435596)) ;
#90141 = CARTESIAN_POINT('Ctrl Pts',(66.2570346873331,229.312331680082,16.3813203435596)) ;
#90142 = CARTESIAN_POINT('',(65.8177442830134,228.780271712565,16.0213203435596)) ;
#90143 = CARTESIAN_POINT('Ctrl Pts',(65.8177442830134,228.780271712565,16.0213203435596)) ;
#90144 = CARTESIAN_POINT('Ctrl Pts',(65.8955297605029,228.857983910561,16.0213203435596)) ;
#90145 = CARTESIAN_POINT('Ctrl Pts',(66.0589351598689,229.021235370333,16.0213203435596)) ;
#90146 = CARTESIAN_POINT('Ctrl Pts',(66.1889240792206,229.212246904868,16.0213203435596)) ;
#90147 = CARTESIAN_POINT('Ctrl Pts',(66.2570346873331,229.312331680082,16.0213203435596)) ;
#90148 = CARTESIAN_POINT('',(65.8177442830134,228.780271712565,16.3213203435596)) ;
#90149 = CARTESIAN_POINT('',(65.8177442830134,228.780271712565,16.0213203435596)) ;
#90150 = CARTESIAN_POINT('Ctrl Pts',(65.8177442830134,228.780271712565,16.3213203435596)) ;
#90151 = CARTESIAN_POINT('Ctrl Pts',(65.8955297605029,228.857983910561,16.3213203435596)) ;
#90152 = CARTESIAN_POINT('Ctrl Pts',(66.0589351598689,229.021235370333,16.3213203435596)) ;
#90153 = CARTESIAN_POINT('Ctrl Pts',(66.1889240792206,229.212246904868,16.3213203435596)) ;
#90154 = CARTESIAN_POINT('Ctrl Pts',(66.2570346873331,229.312331680082,16.3213203435596)) ;
#90155 = CARTESIAN_POINT('Ctrl Pts',(65.4985083621073,228.581090275072,16.0213203435596)) ;
#90156 = CARTESIAN_POINT('Ctrl Pts',(65.4985083621073,228.581090275072,16.3813203435596)) ;
#90157 = CARTESIAN_POINT('Ctrl Pts',(65.5615665458594,228.612247980149,16.0213203435596)) ;
#90158 = CARTESIAN_POINT('Ctrl Pts',(65.5615665458594,228.612247980149,16.3813203435596)) ;
#90159 = CARTESIAN_POINT('Ctrl Pts',(65.674655764364,228.668126540359,16.0213203435596)) ;
#90160 = CARTESIAN_POINT('Ctrl Pts',(65.674655764364,228.668126540359,16.3813203435596)) ;
#90161 = CARTESIAN_POINT('Ctrl Pts',(65.7738572333903,228.745875376758,16.0213203435596)) ;
#90162 = CARTESIAN_POINT('Ctrl Pts',(65.7738572333903,228.745875376758,16.3813203435596)) ;
#90163 = CARTESIAN_POINT('Ctrl Pts',(65.8177442830134,228.780271712565,16.0213203435596)) ;
#90164 = CARTESIAN_POINT('Ctrl Pts',(65.8177442830134,228.780271712565,16.3813203435596)) ;
#90165 = CARTESIAN_POINT('',(65.4985083621073,228.581090275072,16.0213203435596)) ;
#90166 = CARTESIAN_POINT('Ctrl Pts',(65.4985083621073,228.581090275072,16.0213203435596)) ;
#90167 = CARTESIAN_POINT('Ctrl Pts',(65.5615665458594,228.612247980149,16.0213203435596)) ;
#90168 = CARTESIAN_POINT('Ctrl Pts',(65.674655764364,228.668126540359,16.0213203435596)) ;
#90169 = CARTESIAN_POINT('Ctrl Pts',(65.7738572333903,228.745875376758,16.0213203435596)) ;
#90170 = CARTESIAN_POINT('Ctrl Pts',(65.8177442830134,228.780271712565,16.0213203435596)) ;
#90171 = CARTESIAN_POINT('',(65.4985083621073,228.581090275072,16.3213203435596)) ;
#90172 = CARTESIAN_POINT('',(65.4985083621073,228.581090275072,16.0213203435596)) ;
#90173 = CARTESIAN_POINT('Ctrl Pts',(65.4985083621073,228.581090275072,16.3213203435596)) ;
#90174 = CARTESIAN_POINT('Ctrl Pts',(65.5615665458594,228.612247980149,16.3213203435596)) ;
#90175 = CARTESIAN_POINT('Ctrl Pts',(65.674655764364,228.668126540359,16.3213203435596)) ;
#90176 = CARTESIAN_POINT('Ctrl Pts',(65.7738572333903,228.745875376758,16.3213203435596)) ;
#90177 = CARTESIAN_POINT('Ctrl Pts',(65.8177442830134,228.780271712565,16.3213203435596)) ;
#90178 = CARTESIAN_POINT('Ctrl Pts',(66.3498042505312,228.210012618326,16.0213203435596)) ;
#90179 = CARTESIAN_POINT('Ctrl Pts',(66.3498042505312,228.210012618326,16.3813203435596)) ;
#90180 = CARTESIAN_POINT('Ctrl Pts',(66.2373969568096,228.299376555848,16.0213203435596)) ;
#90181 = CARTESIAN_POINT('Ctrl Pts',(66.2373969568096,228.299376555848,16.3813203435596)) ;
#90182 = CARTESIAN_POINT('Ctrl Pts',(65.9877534498724,228.497843452596,16.0213203435596)) ;
#90183 = CARTESIAN_POINT('Ctrl Pts',(65.9877534498724,228.497843452596,16.3813203435596)) ;
#90184 = CARTESIAN_POINT('Ctrl Pts',(65.6720562109134,228.551560480452,16.0213203435596)) ;
#90185 = CARTESIAN_POINT('Ctrl Pts',(65.6720562109134,228.551560480452,16.3813203435596)) ;
#90186 = CARTESIAN_POINT('Ctrl Pts',(65.4985083621073,228.581090275072,16.0213203435596)) ;
#90187 = CARTESIAN_POINT('Ctrl Pts',(65.4985083621073,228.581090275072,16.3813203435596)) ;
#90188 = CARTESIAN_POINT('',(66.3498042505312,228.210012618326,16.0213203435596)) ;
#90189 = CARTESIAN_POINT('Ctrl Pts',(66.3498042505312,228.210012618326,16.0213203435596)) ;
#90190 = CARTESIAN_POINT('Ctrl Pts',(66.2373969568096,228.299376555848,16.0213203435596)) ;
#90191 = CARTESIAN_POINT('Ctrl Pts',(65.9877534498724,228.497843452596,16.0213203435596)) ;
#90192 = CARTESIAN_POINT('Ctrl Pts',(65.6720562109134,228.551560480452,16.0213203435596)) ;
#90193 = CARTESIAN_POINT('Ctrl Pts',(65.4985083621073,228.581090275072,16.0213203435596)) ;
#90194 = CARTESIAN_POINT('',(66.3498042505312,228.210012618326,16.3213203435596)) ;
#90195 = CARTESIAN_POINT('',(66.3498042505312,228.210012618326,16.0213203435596)) ;
#90196 = CARTESIAN_POINT('Ctrl Pts',(66.3498042505312,228.210012618326,16.3213203435596)) ;
#90197 = CARTESIAN_POINT('Ctrl Pts',(66.2373969568096,228.299376555848,16.3213203435596)) ;
#90198 = CARTESIAN_POINT('Ctrl Pts',(65.9877534498724,228.497843452596,16.3213203435596)) ;
#90199 = CARTESIAN_POINT('Ctrl Pts',(65.6720562109134,228.551560480452,16.3213203435596)) ;
#90200 = CARTESIAN_POINT('Ctrl Pts',(65.4985083621073,228.581090275072,16.3213203435596)) ;
#90201 = CARTESIAN_POINT('Ctrl Pts',(66.6253839414644,227.492413524412,16.0213203435596)) ;
#90202 = CARTESIAN_POINT('Ctrl Pts',(66.6253839414644,227.492413524412,16.3813203435596)) ;
#90203 = CARTESIAN_POINT('Ctrl Pts',(66.6146677208766,227.627904203831,16.0213203435596)) ;
#90204 = CARTESIAN_POINT('Ctrl Pts',(66.6146677208766,227.627904203831,16.3813203435596)) ;
#90205 = CARTESIAN_POINT('Ctrl Pts',(66.5935785953528,227.894544846597,16.0213203435596)) ;
#90206 = CARTESIAN_POINT('Ctrl Pts',(66.5935785953528,227.894544846597,16.3813203435596)) ;
#90207 = CARTESIAN_POINT('Ctrl Pts',(66.4301756718191,228.106004162461,16.0213203435596)) ;
#90208 = CARTESIAN_POINT('Ctrl Pts',(66.4301756718191,228.106004162461,16.3813203435596)) ;
#90209 = CARTESIAN_POINT('Ctrl Pts',(66.3498042505312,228.210012618326,16.0213203435596)) ;
#90210 = CARTESIAN_POINT('Ctrl Pts',(66.3498042505312,228.210012618326,16.3813203435596)) ;
#90211 = CARTESIAN_POINT('',(66.6253839414644,227.492413524412,16.0213203435596)) ;
#90212 = CARTESIAN_POINT('Ctrl Pts',(66.6253839414644,227.492413524412,16.0213203435596)) ;
#90213 = CARTESIAN_POINT('Ctrl Pts',(66.6146677208766,227.627904203831,16.0213203435596)) ;
#90214 = CARTESIAN_POINT('Ctrl Pts',(66.5935785953528,227.894544846597,16.0213203435596)) ;
#90215 = CARTESIAN_POINT('Ctrl Pts',(66.4301756718191,228.106004162461,16.0213203435596)) ;
#90216 = CARTESIAN_POINT('Ctrl Pts',(66.3498042505312,228.210012618326,16.0213203435596)) ;
#90217 = CARTESIAN_POINT('',(66.6253839414644,227.492413524412,16.3213203435596)) ;
#90218 = CARTESIAN_POINT('',(66.6253839414644,227.492413524412,16.0213203435596)) ;
#90219 = CARTESIAN_POINT('Ctrl Pts',(66.6253839414644,227.492413524412,16.3213203435596)) ;
#90220 = CARTESIAN_POINT('Ctrl Pts',(66.6146677208766,227.627904203831,16.3213203435596)) ;
#90221 = CARTESIAN_POINT('Ctrl Pts',(66.5935785953528,227.894544846597,16.3213203435596)) ;
#90222 = CARTESIAN_POINT('Ctrl Pts',(66.4301756718191,228.106004162461,16.3213203435596)) ;
#90223 = CARTESIAN_POINT('Ctrl Pts',(66.3498042505312,228.210012618326,16.3213203435596)) ;
#90224 = CARTESIAN_POINT('Ctrl Pts',(66.4589448254633,226.889412406706,16.0213203435596)) ;
#90225 = CARTESIAN_POINT('Ctrl Pts',(66.4589448254633,226.889412406706,16.3813203435596)) ;
#90226 = CARTESIAN_POINT('Ctrl Pts',(66.5074885919051,226.983214870015,16.0213203435596)) ;
#90227 = CARTESIAN_POINT('Ctrl Pts',(66.5074885919051,226.983214870015,16.3813203435596)) ;
#90228 = CARTESIAN_POINT('Ctrl Pts',(66.605416512552,227.172443701166,16.0213203435596)) ;
#90229 = CARTESIAN_POINT('Ctrl Pts',(66.605416512552,227.172443701166,16.3813203435596)) ;
#90230 = CARTESIAN_POINT('Ctrl Pts',(66.6186901616811,227.385148460716,16.0213203435596)) ;
#90231 = CARTESIAN_POINT('Ctrl Pts',(66.6186901616811,227.385148460716,16.3813203435596)) ;
#90232 = CARTESIAN_POINT('Ctrl Pts',(66.6253839414644,227.492413524412,16.0213203435596)) ;
#90233 = CARTESIAN_POINT('Ctrl Pts',(66.6253839414644,227.492413524412,16.3813203435596)) ;
#90234 = CARTESIAN_POINT('',(66.4589448254633,226.889412406706,16.0213203435596)) ;
#90235 = CARTESIAN_POINT('Ctrl Pts',(66.4589448254633,226.889412406706,16.0213203435596)) ;
#90236 = CARTESIAN_POINT('Ctrl Pts',(66.5074885919051,226.983214870015,16.0213203435596)) ;
#90237 = CARTESIAN_POINT('Ctrl Pts',(66.605416512552,227.172443701166,16.0213203435596)) ;
#90238 = CARTESIAN_POINT('Ctrl Pts',(66.6186901616811,227.385148460716,16.0213203435596)) ;
#90239 = CARTESIAN_POINT('Ctrl Pts',(66.6253839414644,227.492413524412,16.0213203435596)) ;
#90240 = CARTESIAN_POINT('',(66.4589448254633,226.889412406706,16.3213203435596)) ;
#90241 = CARTESIAN_POINT('',(66.4589448254633,226.889412406706,16.0213203435596)) ;
#90242 = CARTESIAN_POINT('Ctrl Pts',(66.4589448254633,226.889412406706,16.3213203435596)) ;
#90243 = CARTESIAN_POINT('Ctrl Pts',(66.5074885919051,226.983214870015,16.3213203435596)) ;
#90244 = CARTESIAN_POINT('Ctrl Pts',(66.605416512552,227.172443701166,16.3213203435596)) ;
#90245 = CARTESIAN_POINT('Ctrl Pts',(66.6186901616811,227.385148460716,16.3213203435596)) ;
#90246 = CARTESIAN_POINT('Ctrl Pts',(66.6253839414644,227.492413524412,16.3213203435596)) ;
#90247 = CARTESIAN_POINT('Ctrl Pts',(66.0141970198679,226.51014894607,16.0213203435596)) ;
#90248 = CARTESIAN_POINT('Ctrl Pts',(66.0141970198679,226.51014894607,16.3813203435596)) ;
#90249 = CARTESIAN_POINT('Ctrl Pts',(66.1028098485333,226.553391987607,16.0213203435596)) ;
#90250 = CARTESIAN_POINT('Ctrl Pts',(66.1028098485333,226.553391987607,16.3813203435596)) ;
#90251 = CARTESIAN_POINT('Ctrl Pts',(66.2834709021064,226.641554543316,16.0213203435596)) ;
#90252 = CARTESIAN_POINT('Ctrl Pts',(66.2834709021064,226.641554543316,16.3813203435596)) ;
#90253 = CARTESIAN_POINT('Ctrl Pts',(66.3997166860594,226.805752340273,16.0213203435596)) ;
#90254 = CARTESIAN_POINT('Ctrl Pts',(66.3997166860594,226.805752340273,16.3813203435596)) ;
#90255 = CARTESIAN_POINT('Ctrl Pts',(66.4589448254633,226.889412406706,16.0213203435596)) ;
#90256 = CARTESIAN_POINT('Ctrl Pts',(66.4589448254633,226.889412406706,16.3813203435596)) ;
#90257 = CARTESIAN_POINT('',(66.0141970198679,226.51014894607,16.0213203435596)) ;
#90258 = CARTESIAN_POINT('Ctrl Pts',(66.0141970198679,226.51014894607,16.0213203435596)) ;
#90259 = CARTESIAN_POINT('Ctrl Pts',(66.1028098485333,226.553391987607,16.0213203435596)) ;
#90260 = CARTESIAN_POINT('Ctrl Pts',(66.2834709021064,226.641554543316,16.0213203435596)) ;
#90261 = CARTESIAN_POINT('Ctrl Pts',(66.3997166860594,226.805752340273,16.0213203435596)) ;
#90262 = CARTESIAN_POINT('Ctrl Pts',(66.4589448254633,226.889412406706,16.0213203435596)) ;
#90263 = CARTESIAN_POINT('',(66.0141970198679,226.51014894607,16.3213203435596)) ;
#90264 = CARTESIAN_POINT('',(66.0141970198679,226.51014894607,16.0213203435596)) ;
#90265 = CARTESIAN_POINT('Ctrl Pts',(66.0141970198679,226.51014894607,16.3213203435596)) ;
#90266 = CARTESIAN_POINT('Ctrl Pts',(66.1028098485333,226.553391987607,16.3213203435596)) ;
#90267 = CARTESIAN_POINT('Ctrl Pts',(66.2834709021064,226.641554543316,16.3213203435596)) ;
#90268 = CARTESIAN_POINT('Ctrl Pts',(66.3997166860594,226.805752340273,16.3213203435596)) ;
#90269 = CARTESIAN_POINT('Ctrl Pts',(66.4589448254633,226.889412406706,16.3213203435596)) ;
#90270 = CARTESIAN_POINT('Ctrl Pts',(65.2011002581644,226.401008371138,16.0213203435596)) ;
#90271 = CARTESIAN_POINT('Ctrl Pts',(65.2011002581644,226.401008371138,16.3813203435596)) ;
#90272 = CARTESIAN_POINT('Ctrl Pts',(65.3591469635349,226.402248397894,16.0213203435596)) ;
#90273 = CARTESIAN_POINT('Ctrl Pts',(65.3591469635349,226.402248397894,16.3813203435596)) ;
#90274 = CARTESIAN_POINT('Ctrl Pts',(65.6352198408299,226.404414452249,16.0213203435596)) ;
#90275 = CARTESIAN_POINT('Ctrl Pts',(65.6352198408299,226.404414452249,16.3813203435596)) ;
#90276 = CARTESIAN_POINT('Ctrl Pts',(65.9006995989094,226.47848320729,16.0213203435596)) ;
#90277 = CARTESIAN_POINT('Ctrl Pts',(65.9006995989094,226.47848320729,16.3813203435596)) ;
#90278 = CARTESIAN_POINT('Ctrl Pts',(66.0141970198679,226.51014894607,16.0213203435596)) ;
#90279 = CARTESIAN_POINT('Ctrl Pts',(66.0141970198679,226.51014894607,16.3813203435596)) ;
#90280 = CARTESIAN_POINT('',(65.2011002581644,226.401008371138,16.0213203435596)) ;
#90281 = CARTESIAN_POINT('Ctrl Pts',(65.2011002581644,226.401008371138,16.0213203435596)) ;
#90282 = CARTESIAN_POINT('Ctrl Pts',(65.3591469635349,226.402248397894,16.0213203435596)) ;
#90283 = CARTESIAN_POINT('Ctrl Pts',(65.6352198408299,226.404414452249,16.0213203435596)) ;
#90284 = CARTESIAN_POINT('Ctrl Pts',(65.9006995989094,226.47848320729,16.0213203435596)) ;
#90285 = CARTESIAN_POINT('Ctrl Pts',(66.0141970198679,226.51014894607,16.0213203435596)) ;
#90286 = CARTESIAN_POINT('',(65.2011002581644,226.401008371138,16.3213203435596)) ;
#90287 = CARTESIAN_POINT('',(65.2011002581644,226.401008371138,16.0213203435596)) ;
#90288 = CARTESIAN_POINT('Ctrl Pts',(65.2011002581644,226.401008371138,16.3213203435596)) ;
#90289 = CARTESIAN_POINT('Ctrl Pts',(65.3591469635349,226.402248397894,16.3213203435596)) ;
#90290 = CARTESIAN_POINT('Ctrl Pts',(65.6352198408299,226.404414452249,16.3213203435596)) ;
#90291 = CARTESIAN_POINT('Ctrl Pts',(65.9006995989094,226.47848320729,16.3213203435596)) ;
#90292 = CARTESIAN_POINT('Ctrl Pts',(66.0141970198679,226.51014894607,16.3213203435596)) ;
#90293 = CARTESIAN_POINT('Origin',(63.4275669213462,226.401008371138,16.0213203435596)) ;
#90294 = CARTESIAN_POINT('',(63.4275669213462,226.401008371138,16.0213203435596)) ;
#90295 = CARTESIAN_POINT('',(66.7602139961582,226.401008371138,16.0213203435596)) ;
#90296 = CARTESIAN_POINT('',(63.4275669213462,226.401008371138,16.3213203435596)) ;
#90297 = CARTESIAN_POINT('',(63.4275669213462,226.401008371138,16.0213203435596)) ;
#90298 = CARTESIAN_POINT('',(63.4275669213462,226.401008371138,16.3213203435596)) ;
#90299 = CARTESIAN_POINT('Origin',(63.4275669213462,230.401008430742,16.0213203435596)) ;
#90300 = CARTESIAN_POINT('',(63.4275669213462,230.401008430742,16.0213203435596)) ;
#90301 = CARTESIAN_POINT('',(63.4275669213462,230.216885321963,16.0213203435596)) ;
#90302 = CARTESIAN_POINT('',(63.4275669213462,230.401008430742,16.3213203435596)) ;
#90303 = CARTESIAN_POINT('',(63.4275669213462,230.401008430742,16.0213203435596)) ;
#90304 = CARTESIAN_POINT('',(63.4275669213462,230.401008430742,16.3213203435596)) ;
#90305 = CARTESIAN_POINT('Origin',(63.9568984489966,230.401008430742,16.0213203435596)) ;
#90306 = CARTESIAN_POINT('',(67.0248797599834,230.401008430742,16.0213203435596)) ;
#90307 = CARTESIAN_POINT('',(63.9568984489966,230.401008430742,16.3213203435596)) ;
#90308 = CARTESIAN_POINT('Origin',(65.1901862938035,228.40100840094,16.3213203435596)) ;
#90309 = CARTESIAN_POINT('Origin',(70.0928610709702,230.032762213184,16.0213203435596)) ;
#90310 = CARTESIAN_POINT('',(56.1573593128808,238.278291754874,16.0213203435596)) ;
#90311 = CARTESIAN_POINT('',(56.1573593128808,226.261195155516,16.0213203435596)) ;
#90312 = CARTESIAN_POINT('',(56.1573593128808,228.14697868435,16.0213203435596)) ;
#90313 = CARTESIAN_POINT('',(68.4815231079478,238.278291754874,16.0213203435596)) ;
#90314 = CARTESIAN_POINT('',(69.2696458032277,238.278291754874,16.0213203435596)) ;
#90315 = CARTESIAN_POINT('',(80.5752025501715,238.278291754874,16.0213203435596)) ;
#90316 = CARTESIAN_POINT('Origin',(74.5283628290597,239.4,16.0213203435596)) ;
#90317 = CARTESIAN_POINT('',(81.3283036990481,238.278291755028,16.0213203435596)) ;
#90318 = CARTESIAN_POINT('',(69.2696458032277,238.278291754874,16.0213203435596)) ;
#90319 = CARTESIAN_POINT('',(81.1,237.60736287746,16.0213203435596)) ;
#90320 = CARTESIAN_POINT('Origin',(82.2,237.60736287746,16.0213203435596)) ;
#90321 = CARTESIAN_POINT('',(81.1,226.002365511524,16.0213203435596)) ;
#90322 = CARTESIAN_POINT('',(81.1,234.318247777236,16.0213203435596)) ;
#90323 = CARTESIAN_POINT('',(80.9535533905933,225.648812120931,16.0213203435596)) ;
#90324 = CARTESIAN_POINT('Origin',(80.5999999999999,226.002365511524,16.0213203435596)) ;
#90325 = CARTESIAN_POINT('',(80.1050252531694,224.800283983507,16.0213203435596)) ;
#90326 = CARTESIAN_POINT('',(79.3343678337509,224.029626564088,16.0213203435596)) ;
#90327 = CARTESIAN_POINT('',(80.0535626751402,224.742809236676,16.0213203435596)) ;
#90328 = CARTESIAN_POINT('Origin',(80.6000000000002,224.305309236676,16.0213203435596)) ;
#90329 = CARTESIAN_POINT('',(79.3510004003203,224.405309236676,16.0213203435596)) ;
#90330 = CARTESIAN_POINT('Origin',(79.3510004003203,225.305309236676,16.0213203435596)) ;
#90331 = CARTESIAN_POINT('',(75.,224.405309236676,16.0213203435596)) ;
#90332 = CARTESIAN_POINT('',(75.046430535485,224.405309236676,16.0213203435596)) ;
#90333 = CARTESIAN_POINT('',(70.8999999999999,220.305309236676,16.0213203435596)) ;
#90334 = CARTESIAN_POINT('Origin',(74.9999999999998,220.305309236676,16.0213203435596)) ;
#90335 = CARTESIAN_POINT('',(70.8999999999998,217.165524426368,16.0213203435596)) ;
#90336 = CARTESIAN_POINT('',(70.9000000000001,225.16903572493,16.0213203435596)) ;
#90337 = CARTESIAN_POINT('',(69.4079308494226,215.768555109772,16.0213203435596)) ;
#90338 = CARTESIAN_POINT('Origin',(69.4999999999997,217.165524426368,16.0213203435596)) ;
#90339 = CARTESIAN_POINT('',(63.3614933659285,216.167053742856,16.0213203435596)) ;
#90340 = CARTESIAN_POINT('',(69.2808968287545,215.776927458569,16.0213203435596)) ;
#90341 = CARTESIAN_POINT('',(61.3703326482681,217.618162279643,16.0213203435596)) ;
#90342 = CARTESIAN_POINT('Origin',(64.4831104165663,219.797752737776,16.0213203435596)) ;
#90343 = CARTESIAN_POINT('',(56.8445815445825,224.081604697382,16.0213203435596)) ;
#90344 = CARTESIAN_POINT('',(59.3765805603019,220.465535350009,16.0213203435596)) ;
#90345 = CARTESIAN_POINT('Origin',(59.9573593128806,226.261195155516,16.0213203435596)) ;
#90346 = CARTESIAN_POINT('',(65.4568347953872,218.760590800757,16.0213203435596)) ;
#90347 = CARTESIAN_POINT('',(65.4568347953872,216.846231446812,16.0213203435596)) ;
#90348 = CARTESIAN_POINT('',(65.4568347953872,224.289496829998,16.0213203435596)) ;
#90349 = CARTESIAN_POINT('',(62.8568347953872,218.760590800757,16.0213203435596)) ;
#90350 = CARTESIAN_POINT('Origin',(64.1568347953872,220.146231446812,16.0213203435596)) ;
#90351 = CARTESIAN_POINT('',(62.8568347953872,216.846231446812,16.0213203435596)) ;
#90352 = CARTESIAN_POINT('',(62.8568347953872,223.489496829998,16.0213203435596)) ;
#90353 = CARTESIAN_POINT('',(67.7248479331787,216.846231446812,16.0213203435596)) ;
#90354 = CARTESIAN_POINT('Ctrl Pts',(62.4573593128808,235.849044700347,29.5213203435596)) ;
#90355 = CARTESIAN_POINT('Ctrl Pts',(62.4573593128808,235.849044700347,24.9613203435596)) ;
#90356 = CARTESIAN_POINT('Ctrl Pts',(62.4573593128808,235.882800482314,29.5213203435596)) ;
#90357 = CARTESIAN_POINT('Ctrl Pts',(62.4573593128808,235.882800482314,24.9613203435596)) ;
#90358 = CARTESIAN_POINT('Ctrl Pts',(62.4423298065164,235.916280466737,29.5213203435596)) ;
#90359 = CARTESIAN_POINT('Ctrl Pts',(62.4423298065164,235.916280466737,24.9613203435596)) ;
#90360 = CARTESIAN_POINT('Ctrl Pts',(62.4171062395287,235.938713132308,29.5213203435596)) ;
#90361 = CARTESIAN_POINT('Ctrl Pts',(62.4171062395287,235.938713132308,24.9613203435596)) ;
#90362 = CARTESIAN_POINT('',(62.4573593128808,235.849044700347,25.7213203435596)) ;
#90363 = CARTESIAN_POINT('',(62.4169327150641,235.938516599365,25.7213203435596)) ;
#90364 = CARTESIAN_POINT('Origin',(62.3640981990777,235.86104805899,25.7213203435596)) ;
#90365 = CARTESIAN_POINT('',(62.4573593128808,235.849044700347,29.5213203435596)) ;
#90366 = CARTESIAN_POINT('',(62.4573593128808,235.849044700347,25.7213203435596)) ;
#90367 = CARTESIAN_POINT('',(62.4169327150641,235.938516599365,29.5213203435596)) ;
#90368 = CARTESIAN_POINT('Origin',(62.3640981990903,235.861048058995,29.5213203435596)) ;
#90369 = CARTESIAN_POINT('',(62.4169327140377,235.938516598221,29.5213203435596)) ;
#90370 = CARTESIAN_POINT('Ctrl Pts',(62.4573593128808,235.9,29.5213203435596)) ;
#90371 = CARTESIAN_POINT('Ctrl Pts',(62.4573593128808,235.9,18.1213203435596)) ;
#90372 = CARTESIAN_POINT('Ctrl Pts',(62.4296494906727,235.927709822208,29.5213203435596)) ;
#90373 = CARTESIAN_POINT('Ctrl Pts',(62.4296494906727,235.927709822208,18.1213203435596)) ;
#90374 = CARTESIAN_POINT('Ctrl Pts',(62.3958369856604,235.960391271619,29.5213203435596)) ;
#90375 = CARTESIAN_POINT('Ctrl Pts',(62.3958369856604,235.960391271619,18.1213203435596)) ;
#90376 = CARTESIAN_POINT('Ctrl Pts',(62.3388862655657,235.99104280001,29.5213203435596)) ;
#90377 = CARTESIAN_POINT('Ctrl Pts',(62.3388862655657,235.99104280001,18.1213203435596)) ;
#90378 = CARTESIAN_POINT('Ctrl Pts',(62.3096419743114,236.,29.5213203435596)) ;
#90379 = CARTESIAN_POINT('Ctrl Pts',(62.3096419743114,236.,18.1213203435596)) ;
#90380 = CARTESIAN_POINT('Ctrl Pts',(62.2841542321239,236.,29.5213203435596)) ;
#90381 = CARTESIAN_POINT('Ctrl Pts',(62.2841542321239,236.,18.1213203435596)) ;
#90382 = CARTESIAN_POINT('',(62.2841542321239,236.,29.5213203435596)) ;
#90383 = CARTESIAN_POINT('Ctrl Pts',(62.4169327140379,235.938516598221,29.5213203435596)) ;
#90384 = CARTESIAN_POINT('Ctrl Pts',(62.3992166438732,235.954158616459,29.5213203435596)) ;
#90385 = CARTESIAN_POINT('Ctrl Pts',(62.3803790823931,235.968710891811,29.5213203435596)) ;
#90386 = CARTESIAN_POINT('Ctrl Pts',(62.3388862655657,235.99104280001,29.5213203435596)) ;
#90387 = CARTESIAN_POINT('Ctrl Pts',(62.3096419743114,236.,29.5213203435596)) ;
#90388 = CARTESIAN_POINT('Ctrl Pts',(62.2841542321239,236.,29.5213203435596)) ;
#90389 = CARTESIAN_POINT('',(62.2841542321239,236.,25.7213203435596)) ;
#90390 = CARTESIAN_POINT('',(62.2841542321239,236.,29.5213203435596)) ;
#90391 = CARTESIAN_POINT('Ctrl Pts',(62.2841542321239,236.,25.7213203435596)) ;
#90392 = CARTESIAN_POINT('Ctrl Pts',(62.3096419743114,236.,25.7213203435596)) ;
#90393 = CARTESIAN_POINT('Ctrl Pts',(62.3388862655657,235.99104280001,25.7213203435596)) ;
#90394 = CARTESIAN_POINT('Ctrl Pts',(62.3803790823931,235.968710891811,25.7213203435596)) ;
#90395 = CARTESIAN_POINT('Ctrl Pts',(62.3992166438732,235.954158616459,25.7213203435596)) ;
#90396 = CARTESIAN_POINT('Ctrl Pts',(62.4169327140379,235.938516598221,25.7213203435596)) ;
#90397 = CARTESIAN_POINT('Origin',(66.56,251.44,19.7813203435596)) ;
#90398 = CARTESIAN_POINT('',(66.56,251.2,20.2613203435596)) ;
#90399 = CARTESIAN_POINT('',(66.56,251.44,20.0213203435596)) ;
#90400 = CARTESIAN_POINT('Origin',(66.56,251.44,20.2613203435596)) ;
#90401 = CARTESIAN_POINT('',(66.8,251.44,19.7813203435596)) ;
#90402 = CARTESIAN_POINT('Origin',(66.56,251.44,19.7813203435596)) ;
#90403 = CARTESIAN_POINT('',(66.8,251.2,20.1970125373762)) ;
#90404 = CARTESIAN_POINT('Ctrl Pts',(66.8,251.2,20.1970125373761)) ;
#90405 = CARTESIAN_POINT('Ctrl Pts',(66.8,251.2,20.1634772824134)) ;
#90406 = CARTESIAN_POINT('Ctrl Pts',(66.8,251.206626505453,20.123784303008)) ;
#90407 = CARTESIAN_POINT('Ctrl Pts',(66.8,251.228274899711,20.0539974766885)) ;
#90408 = CARTESIAN_POINT('Ctrl Pts',(66.8,251.249130360957,20.011389083393)) ;
#90409 = CARTESIAN_POINT('Ctrl Pts',(66.8,251.313969023646,19.9090950900013)) ;
#90410 = CARTESIAN_POINT('Ctrl Pts',(66.8,251.382314385242,19.8390059583173)) ;
#90411 = CARTESIAN_POINT('Ctrl Pts',(66.8,251.44,19.7813203435596)) ;
#90412 = CARTESIAN_POINT('Origin',(66.56,251.2,19.7813203435596)) ;
#90413 = CARTESIAN_POINT('Origin',(65.975,251.44,20.2613203435596)) ;
#90414 = CARTESIAN_POINT('',(66.1,251.2,20.2613203435596)) ;
#90415 = CARTESIAN_POINT('',(66.1,251.44,20.0213203435596)) ;
#90416 = CARTESIAN_POINT('Origin',(66.1,251.44,20.2613203435596)) ;
#90417 = CARTESIAN_POINT('',(65.975,251.44,20.0213203435596)) ;
#90418 = CARTESIAN_POINT('',(65.975,251.2,20.2613203435596)) ;
#90419 = CARTESIAN_POINT('Ctrl Pts',(65.9400000000002,251.6,20.0213203435596)) ;
#90420 = CARTESIAN_POINT('Ctrl Pts',(65.9400000000003,251.44,20.0213203435596)) ;
#90421 = CARTESIAN_POINT('Ctrl Pts',(66.1000000000004,251.44,20.0213203435596)) ;
#90422 = CARTESIAN_POINT('Ctrl Pts',(65.7,251.6,20.0213203435594)) ;
#90423 = CARTESIAN_POINT('Ctrl Pts',(65.7000000000003,251.2,20.0213203435594)) ;
#90424 = CARTESIAN_POINT('Ctrl Pts',(66.1000000000004,251.2,20.0213203435594)) ;
#90425 = CARTESIAN_POINT('Ctrl Pts',(65.7,251.6,20.2613203435596)) ;
#90426 = CARTESIAN_POINT('Ctrl Pts',(65.7000000000003,251.2,20.2613203435596)) ;
#90427 = CARTESIAN_POINT('Ctrl Pts',(66.1000000000004,251.2,20.2613203435596)) ;
#90428 = CARTESIAN_POINT('',(65.7,251.6,20.2613203435596)) ;
#90429 = CARTESIAN_POINT('',(65.94,251.6,20.0213203435596)) ;
#90430 = CARTESIAN_POINT('Origin',(65.94,251.6,20.2613203435596)) ;
#90431 = CARTESIAN_POINT('Origin',(66.1,251.6,20.0213203435596)) ;
#90432 = CARTESIAN_POINT('Origin',(66.1,251.6,20.2613203435596)) ;
#90433 = CARTESIAN_POINT('Origin',(65.94,252.4,20.2613203435596)) ;
#90434 = CARTESIAN_POINT('',(65.7,253.055933015586,20.2613203435596)) ;
#90435 = CARTESIAN_POINT('',(65.9396674027608,253.055812426285,20.0212455719998)) ;
#90436 = CARTESIAN_POINT('Origin',(65.94,253.055933015586,20.2613203435596)) ;
#90437 = CARTESIAN_POINT('',(65.94,253.053504693378,20.0213203435596)) ;
#90438 = CARTESIAN_POINT('Ctrl Pts',(65.9396674027608,253.055812426285,20.0213203435596)) ;
#90439 = CARTESIAN_POINT('Ctrl Pts',(65.9397782685072,253.055043181982,20.0213203435596)) ;
#90440 = CARTESIAN_POINT('Ctrl Pts',(65.9398891342536,253.05427393768,20.0213203435596)) ;
#90441 = CARTESIAN_POINT('Ctrl Pts',(65.94,253.053504693378,20.0213203435596)) ;
#90442 = CARTESIAN_POINT('',(65.94,252.4,20.0213203435596)) ;
#90443 = CARTESIAN_POINT('',(65.7,252.4,20.2613203435596)) ;
#90444 = CARTESIAN_POINT('Ctrl Pts',(65.8787223053518,253.200000000043,20.0213203435596)) ;
#90445 = CARTESIAN_POINT('Ctrl Pts',(65.8988550182207,253.152091884828,20.0213203435596)) ;
#90446 = CARTESIAN_POINT('Ctrl Pts',(65.9192601391554,253.103601946723,20.0213203435596)) ;
#90447 = CARTESIAN_POINT('Ctrl Pts',(65.9400000000004,253.055933015586,20.0213203435596)) ;
#90448 = CARTESIAN_POINT('Ctrl Pts',(65.8279579835555,253.201487684761,20.0346431984532)) ;
#90449 = CARTESIAN_POINT('Ctrl Pts',(65.8435615888772,253.152668920777,20.0311364548328)) ;
#90450 = CARTESIAN_POINT('Ctrl Pts',(65.8598723347433,253.10358309864,20.0268717600141)) ;
#90451 = CARTESIAN_POINT('Ctrl Pts',(65.8771681469285,253.055933015586,20.0213203435595)) ;
#90452 = CARTESIAN_POINT('Ctrl Pts',(65.735859111132,253.208302568615,20.0956734070701)) ;
#90453 = CARTESIAN_POINT('Ctrl Pts',(65.740788844418,253.156930054594,20.091034868245)) ;
#90454 = CARTESIAN_POINT('Ctrl Pts',(65.7461509033861,253.105566496234,20.0836957459916)) ;
#90455 = CARTESIAN_POINT('Ctrl Pts',(65.752215309716,253.055933015586,20.0735356532753)) ;
#90456 = CARTESIAN_POINT('Ctrl Pts',(65.6999999999998,253.219924430328,20.1997521646846)) ;
#90457 = CARTESIAN_POINT('Ctrl Pts',(65.6999351060341,253.165238884986,20.2023526749646)) ;
#90458 = CARTESIAN_POINT('Ctrl Pts',(65.7001128677229,253.11025926159,20.2019758599767)) ;
#90459 = CARTESIAN_POINT('Ctrl Pts',(65.7,253.055933015586,20.1984884904878)) ;
#90460 = CARTESIAN_POINT('Ctrl Pts',(65.6999999999998,253.225751090982,20.2519324105771)) ;
#90461 = CARTESIAN_POINT('Ctrl Pts',(65.6999999999998,253.16940880829,20.2582238213609)) ;
#90462 = CARTESIAN_POINT('Ctrl Pts',(65.7,253.112625472478,20.2613203435597)) ;
#90463 = CARTESIAN_POINT('Ctrl Pts',(65.7,253.055933015586,20.2613203435596)) ;
#90464 = CARTESIAN_POINT('',(65.8787220969437,253.199999911797,20.021320809239)) ;
#90465 = CARTESIAN_POINT('',(65.6999999999999,253.200000001188,20.2545830286245)) ;
#90466 = CARTESIAN_POINT('Ctrl Pts',(65.8787219951101,253.2,20.0213204260013)) ;
#90467 = CARTESIAN_POINT('Ctrl Pts',(65.8637513393088,253.2,20.0252984157073)) ;
#90468 = CARTESIAN_POINT('Ctrl Pts',(65.8492674755271,253.2,20.0307646764352)) ;
#90469 = CARTESIAN_POINT('Ctrl Pts',(65.8354281636608,253.2,20.0375555002856)) ;
#90470 = CARTESIAN_POINT('Ctrl Pts',(65.8215887561901,253.2,20.0443463710483)) ;
#90471 = CARTESIAN_POINT('Ctrl Pts',(65.8083925033119,253.2,20.0524630322388)) ;
#90472 = CARTESIAN_POINT('Ctrl Pts',(65.7960263435029,253.2,20.0617902565927)) ;
#90473 = CARTESIAN_POINT('Ctrl Pts',(65.7841216235844,253.2,20.0707694381062)) ;
#90474 = CARTESIAN_POINT('Ctrl Pts',(65.7730938774418,253.2,20.0807890097741)) ;
#90475 = CARTESIAN_POINT('Ctrl Pts',(65.7630914752968,253.2,20.0917318564667)) ;
#90476 = CARTESIAN_POINT('Ctrl Pts',(65.7589082319733,253.2,20.0963084161475)) ;
#90477 = CARTESIAN_POINT('Ctrl Pts',(65.7549047310405,253.2,20.101046950744)) ;
#90478 = CARTESIAN_POINT('Ctrl Pts',(65.7510938065472,253.2,20.1059407077756)) ;
#90479 = CARTESIAN_POINT('Ctrl Pts',(65.7448220996584,253.2,20.1139944516221)) ;
#90480 = CARTESIAN_POINT('Ctrl Pts',(65.7390714447429,253.2,20.1224685139581)) ;
#90481 = CARTESIAN_POINT('Ctrl Pts',(65.7338649261578,253.2,20.1313038355597)) ;
#90482 = CARTESIAN_POINT('Ctrl Pts',(65.7261735242395,253.2,20.1443559371521)) ;
#90483 = CARTESIAN_POINT('Ctrl Pts',(65.7197244243772,253.2,20.1580982486252)) ;
#90484 = CARTESIAN_POINT('Ctrl Pts',(65.714572824113,253.2,20.1723335497224)) ;
#90485 = CARTESIAN_POINT('Ctrl Pts',(65.7124421681154,253.2,20.1782211435001)) ;
#90486 = CARTESIAN_POINT('Ctrl Pts',(65.7105340250227,253.2,20.1841933262792)) ;
#90487 = CARTESIAN_POINT('Ctrl Pts',(65.7088547698819,253.2,20.1902368435495)) ;
#90488 = CARTESIAN_POINT('Ctrl Pts',(65.7048015662676,253.2,20.2048240289322)) ;
#90489 = CARTESIAN_POINT('Ctrl Pts',(65.7021029059883,253.2,20.2197377335324)) ;
#90490 = CARTESIAN_POINT('Ctrl Pts',(65.7008336869791,253.2,20.2347908075204)) ;
#90491 = CARTESIAN_POINT('Ctrl Pts',(65.7002792381749,253.2,20.2413666299846)) ;
#90492 = CARTESIAN_POINT('Ctrl Pts',(65.6999982168404,253.2,20.247969183683)) ;
#90493 = CARTESIAN_POINT('Ctrl Pts',(65.6999999999998,253.2,20.2545830064533)) ;
#90494 = CARTESIAN_POINT('',(65.9054141138738,253.136644520473,20.0212807249742)) ;
#90495 = CARTESIAN_POINT('Ctrl Pts',(65.8787223180024,253.200000004773,20.0213211815297)) ;
#90496 = CARTESIAN_POINT('Ctrl Pts',(65.8875660862203,253.178955523856,20.0213256058334)) ;
#90497 = CARTESIAN_POINT('Ctrl Pts',(65.8964675487447,253.157798296395,20.0213194598004)) ;
#90498 = CARTESIAN_POINT('Ctrl Pts',(65.9054141138738,253.136644520473,20.0212807249742)) ;
#90499 = CARTESIAN_POINT('Ctrl Pts',(65.9054141138738,253.136644520473,20.0212807249742)) ;
#90500 = CARTESIAN_POINT('Ctrl Pts',(65.9147761239318,253.114508442539,20.0212401914478)) ;
#90501 = CARTESIAN_POINT('Ctrl Pts',(65.9241869890751,253.09237636557,20.0211639482418)) ;
#90502 = CARTESIAN_POINT('Ctrl Pts',(65.93365196153,253.07038006692,20.0210779520608)) ;
#90503 = CARTESIAN_POINT('Ctrl Pts',(65.935730195249,253.065550317043,20.021059069791)) ;
#90504 = CARTESIAN_POINT('Ctrl Pts',(65.9378111246201,253.060727099485,20.0210398990018)) ;
#90505 = CARTESIAN_POINT('Ctrl Pts',(65.9398949529419,253.055911779844,20.0210210022763)) ;
#90506 = CARTESIAN_POINT('Origin',(65.6999999999758,253.056278660127,18.7250135059453)) ;
#90507 = CARTESIAN_POINT('Origin',(65.7,253.,24.0213203435596)) ;
#90508 = CARTESIAN_POINT('',(65.7,251.6,23.0213203435596)) ;
#90509 = CARTESIAN_POINT('',(65.7,251.6,20.0213203435596)) ;
#90510 = CARTESIAN_POINT('',(65.7,253.1,23.0213203435596)) ;
#90511 = CARTESIAN_POINT('',(65.7,252.4,23.0213203435596)) ;
#90512 = CARTESIAN_POINT('',(65.7,253.1,24.0213203435596)) ;
#90513 = CARTESIAN_POINT('',(65.7,253.1,24.0213203435596)) ;
#90514 = CARTESIAN_POINT('',(65.7,253.2,24.0213203435596)) ;
#90515 = CARTESIAN_POINT('',(65.7,253.,24.0213203435596)) ;
#90516 = CARTESIAN_POINT('',(65.7,253.2,24.0213203435596)) ;
#90517 = CARTESIAN_POINT('Origin',(66.1,251.6,20.0213203435596)) ;
#90518 = CARTESIAN_POINT('',(66.1,251.2,23.0213203435596)) ;
#90519 = CARTESIAN_POINT('',(66.1,251.2,20.0213203435596)) ;
#90520 = CARTESIAN_POINT('Origin',(66.1,251.6,23.0213203435596)) ;
#90521 = CARTESIAN_POINT('Origin',(65.7,251.2,20.0213203435596)) ;
#90522 = CARTESIAN_POINT('',(66.8,251.2,23.0213203435596)) ;
#90523 = CARTESIAN_POINT('',(66.8,251.2,22.0213203435596)) ;
#90524 = CARTESIAN_POINT('',(65.975,251.2,23.0213203435596)) ;
#90525 = CARTESIAN_POINT('Ctrl Pts',(59.4599709502105,252.66176631391,20.0213203406956)) ;
#90526 = CARTESIAN_POINT('Ctrl Pts',(59.4862791845716,252.73300766342,20.0213255280724)) ;
#90527 = CARTESIAN_POINT('Ctrl Pts',(59.5476801368282,252.899278293364,20.0048984182032)) ;
#90528 = CARTESIAN_POINT('Ctrl Pts',(59.5942467666672,253.025378338935,19.9538218787239)) ;
#90529 = CARTESIAN_POINT('Ctrl Pts',(59.6112632622918,253.071458136446,19.9183779157918)) ;
#90530 = CARTESIAN_POINT('Ctrl Pts',(59.5228076267856,252.661766373174,20.0213125642804)) ;
#90531 = CARTESIAN_POINT('Ctrl Pts',(59.5447480140858,252.732953219279,20.0283608967158)) ;
#90532 = CARTESIAN_POINT('Ctrl Pts',(59.5931584269531,252.904373903459,20.0244169597432)) ;
#90533 = CARTESIAN_POINT('Ctrl Pts',(59.6267463142549,253.039426939223,19.9717522594694)) ;
#90534 = CARTESIAN_POINT('Ctrl Pts',(59.6388683863242,253.088950591174,19.9323854375313)) ;
#90535 = CARTESIAN_POINT('Ctrl Pts',(59.6477975268572,252.661760233233,20.0735298372816)) ;
#90536 = CARTESIAN_POINT('Ctrl Pts',(59.6554884901573,252.738506902787,20.0864278965363)) ;
#90537 = CARTESIAN_POINT('Ctrl Pts',(59.6711001024041,252.927116008415,20.0875757744157)) ;
#90538 = CARTESIAN_POINT('Ctrl Pts',(59.6805415396398,253.078232351583,20.0199472449724)) ;
#90539 = CARTESIAN_POINT('Ctrl Pts',(59.6839102088974,253.133679100257,19.9682029127294)) ;
#90540 = CARTESIAN_POINT('Ctrl Pts',(59.7000176946533,252.661745701756,20.1985255688626)) ;
#90541 = CARTESIAN_POINT('Ctrl Pts',(59.6998718034678,252.75165343376,20.2029571135977)) ;
#90542 = CARTESIAN_POINT('Ctrl Pts',(59.6998122444854,252.964737640422,20.1793702220234)) ;
#90543 = CARTESIAN_POINT('Ctrl Pts',(59.7000270806329,253.129051719149,20.0818652291328)) ;
#90544 = CARTESIAN_POINT('Ctrl Pts',(59.7000054052531,253.189168023934,20.012637059726)) ;
#90545 = CARTESIAN_POINT('Ctrl Pts',(59.6999999910052,252.66173837404,20.2613836458743)) ;
#90546 = CARTESIAN_POINT('Ctrl Pts',(59.7000001367147,252.758282786987,20.2613906018571)) ;
#90547 = CARTESIAN_POINT('Ctrl Pts',(59.7000001940885,252.983605119967,20.2252383047188)) ;
#90548 = CARTESIAN_POINT('Ctrl Pts',(59.699999976005,253.154487386442,20.1128549327947)) ;
#90549 = CARTESIAN_POINT('Ctrl Pts',(59.6999999972766,253.216931543521,20.0348693941943)) ;
#90550 = CARTESIAN_POINT('',(59.7,253.2,20.0547106776782)) ;
#90551 = CARTESIAN_POINT('',(59.6989357893727,253.198893220947,20.0213203435596)) ;
#90552 = CARTESIAN_POINT('Ctrl Pts',(59.7,253.2,20.0546787338963)) ;
#90553 = CARTESIAN_POINT('Ctrl Pts',(59.7000002277722,253.2,20.0491133758029)) ;
#90554 = CARTESIAN_POINT('Ctrl Pts',(59.6999115519515,253.2,20.0435500952352)) ;
#90555 = CARTESIAN_POINT('Ctrl Pts',(59.6995747351395,253.2,20.0324243353057)) ;
#90556 = CARTESIAN_POINT('Ctrl Pts',(59.6993268096966,253.2,20.0268679068488)) ;
#90557 = CARTESIAN_POINT('Ctrl Pts',(59.6990088056403,253.2,20.021311332408)) ;
#90558 = CARTESIAN_POINT('',(59.7,252.66184497925,20.2613203435596)) ;
#90559 = CARTESIAN_POINT('Origin',(59.7,252.66184497925,19.8213203435596)) ;
#90560 = CARTESIAN_POINT('',(59.46,252.66184497925,20.0213203435596)) ;
#90561 = CARTESIAN_POINT('Origin',(59.46,252.66184497925,20.2613203435596)) ;
#90562 = CARTESIAN_POINT('',(59.542455661465,252.885254883942,19.9972444447401)) ;
#90563 = CARTESIAN_POINT('Origin',(59.46,252.66184497925,19.8213203435596)) ;
#90564 = CARTESIAN_POINT('',(59.6074881670737,252.973767115183,19.9952481069197)) ;
#90565 = CARTESIAN_POINT('Ctrl Pts',(59.5424456954486,252.885275820812,19.9972326388961)) ;
#90566 = CARTESIAN_POINT('Ctrl Pts',(59.542916942341,252.885870023412,19.9971914059271)) ;
#90567 = CARTESIAN_POINT('Ctrl Pts',(59.5433878129887,252.886464556907,19.9971507181093)) ;
#90568 = CARTESIAN_POINT('Ctrl Pts',(59.5438575843988,252.887058515381,19.9971106340598)) ;
#90569 = CARTESIAN_POINT('Ctrl Pts',(59.5530969190852,252.898740327019,19.996322272015)) ;
#90570 = CARTESIAN_POINT('Ctrl Pts',(59.5624673714554,252.910908714203,19.9957195274863)) ;
#90571 = CARTESIAN_POINT('Ctrl Pts',(59.571742193056,252.923362468785,19.995356358669)) ;
#90572 = CARTESIAN_POINT('Ctrl Pts',(59.5806730652746,252.935354385784,19.9950066576785)) ;
#90573 = CARTESIAN_POINT('Ctrl Pts',(59.5895141940076,252.947611011629,19.9948775133271)) ;
#90574 = CARTESIAN_POINT('Ctrl Pts',(59.5980894303711,252.95998930852,19.9950028035369)) ;
#90575 = CARTESIAN_POINT('Ctrl Pts',(59.6012608458573,252.964567225768,19.9950491401386)) ;
#90576 = CARTESIAN_POINT('Ctrl Pts',(59.6043962457373,252.969162147482,19.9951302491092)) ;
#90577 = CARTESIAN_POINT('Ctrl Pts',(59.6074880869828,252.97376808314,19.9952479713636)) ;
#90578 = CARTESIAN_POINT('',(59.6445121748197,252.999999508894,20.021320114607)) ;
#90579 = CARTESIAN_POINT('Ctrl Pts',(59.6075096705789,252.973853981228,19.9951743247871)) ;
#90580 = CARTESIAN_POINT('Ctrl Pts',(59.6142809805769,252.977720686039,19.9990410295982)) ;
#90581 = CARTESIAN_POINT('Ctrl Pts',(59.6207622195018,252.981841745709,20.0031620892954)) ;
#90582 = CARTESIAN_POINT('Ctrl Pts',(59.6331221952063,252.990570656193,20.0118909997797)) ;
#90583 = CARTESIAN_POINT('Ctrl Pts',(59.6389969882328,252.99518214824,20.0165024917991)) ;
#90584 = CARTESIAN_POINT('Ctrl Pts',(59.6445120247841,252.999999313142,20.0213196567018)) ;
#90585 = CARTESIAN_POINT('Ctrl Pts',(59.6445125319219,252.999999354438,20.0213203435596)) ;
#90586 = CARTESIAN_POINT('Ctrl Pts',(59.6583065581309,253.031891118753,20.0213203435596)) ;
#90587 = CARTESIAN_POINT('Ctrl Pts',(59.6707567119401,253.064944388245,20.021320344362)) ;
#90588 = CARTESIAN_POINT('Ctrl Pts',(59.6896400105539,253.131227832493,20.021320344362)) ;
#90589 = CARTESIAN_POINT('Ctrl Pts',(59.6964171938951,253.164990946491,20.0213203435596)) ;
#90590 = CARTESIAN_POINT('Ctrl Pts',(59.6989291504472,253.198897505808,20.0213203435596)) ;
#90591 = CARTESIAN_POINT('Origin',(59.46,251.2,20.2613203435596)) ;
#90592 = CARTESIAN_POINT('',(59.7,251.6,20.2613203435596)) ;
#90593 = CARTESIAN_POINT('',(59.46,251.6,20.0213203435596)) ;
#90594 = CARTESIAN_POINT('Origin',(59.46,251.6,20.2613203435596)) ;
#90595 = CARTESIAN_POINT('',(59.46,251.2,20.0213203435596)) ;
#90596 = CARTESIAN_POINT('',(59.7,251.2,20.2613203435596)) ;
#90597 = CARTESIAN_POINT('Ctrl Pts',(59.2999999999997,251.44,20.0213203435596)) ;
#90598 = CARTESIAN_POINT('Ctrl Pts',(59.4599999999999,251.44,20.0213203435596)) ;
#90599 = CARTESIAN_POINT('Ctrl Pts',(59.46,251.6,20.0213203435596)) ;
#90600 = CARTESIAN_POINT('Ctrl Pts',(59.2999999999997,251.2,20.0213203435595)) ;
#90601 = CARTESIAN_POINT('Ctrl Pts',(59.6999999999999,251.2,20.0213203435594)) ;
#90602 = CARTESIAN_POINT('Ctrl Pts',(59.7000000000001,251.6,20.0213203435595)) ;
#90603 = CARTESIAN_POINT('Ctrl Pts',(59.2999999999998,251.2,20.2613203435596)) ;
#90604 = CARTESIAN_POINT('Ctrl Pts',(59.6999999999999,251.2,20.2613203435595)) ;
#90605 = CARTESIAN_POINT('Ctrl Pts',(59.7000000000001,251.6,20.2613203435596)) ;
#90606 = CARTESIAN_POINT('',(59.3,251.2,20.2613203435596)) ;
#90607 = CARTESIAN_POINT('',(59.3,251.44,20.0213203435596)) ;
#90608 = CARTESIAN_POINT('Origin',(59.3,251.44,20.2613203435596)) ;
#90609 = CARTESIAN_POINT('Origin',(59.3,251.6,20.0213203435596)) ;
#90610 = CARTESIAN_POINT('Origin',(59.3,251.6,20.2613203435596)) ;
#90611 = CARTESIAN_POINT('Origin',(65.975,251.44,20.2613203435596)) ;
#90612 = CARTESIAN_POINT('',(58.84,251.2,20.2613203435596)) ;
#90613 = CARTESIAN_POINT('',(58.84,251.44,20.0213203435596)) ;
#90614 = CARTESIAN_POINT('Origin',(58.84,251.44,20.2613203435596)) ;
#90615 = CARTESIAN_POINT('',(65.975,251.44,20.0213203435596)) ;
#90616 = CARTESIAN_POINT('',(65.975,251.2,20.2613203435596)) ;
#90617 = CARTESIAN_POINT('Origin',(58.84,251.44,19.7813203435596)) ;
#90618 = CARTESIAN_POINT('',(58.6,251.2,20.1970125373762)) ;
#90619 = CARTESIAN_POINT('',(58.6,251.44,19.7813203435596)) ;
#90620 = CARTESIAN_POINT('Ctrl Pts',(58.6000000000001,251.44,19.7813203435596)) ;
#90621 = CARTESIAN_POINT('Ctrl Pts',(58.6000000000001,251.373496426701,19.847823916859)) ;
#90622 = CARTESIAN_POINT('Ctrl Pts',(58.6000000000001,251.295060948115,19.9289739288886)) ;
#90623 = CARTESIAN_POINT('Ctrl Pts',(58.6000000000001,251.221497279975,20.0656556571159)) ;
#90624 = CARTESIAN_POINT('Ctrl Pts',(58.6000000000001,251.2,20.135841956126)) ;
#90625 = CARTESIAN_POINT('Ctrl Pts',(58.6000000000001,251.2,20.1970125373762)) ;
#90626 = CARTESIAN_POINT('Origin',(58.84,251.44,19.7813203435596)) ;
#90627 = CARTESIAN_POINT('Origin',(58.84,251.2,19.7813203435596)) ;
#90628 = CARTESIAN_POINT('Origin',(65.7,251.2,20.0213203435596)) ;
#90629 = CARTESIAN_POINT('',(59.3,251.2,23.0213203435596)) ;
#90630 = CARTESIAN_POINT('',(59.3,251.2,20.0213203435596)) ;
#90631 = CARTESIAN_POINT('',(58.6,251.2,23.0213203435596)) ;
#90632 = CARTESIAN_POINT('',(65.975,251.2,23.0213203435596)) ;
#90633 = CARTESIAN_POINT('',(58.6,251.2,22.0213203435596)) ;
#90634 = CARTESIAN_POINT('Origin',(59.3,251.6,20.0213203435596)) ;
#90635 = CARTESIAN_POINT('',(59.7,251.6,23.0213203435596)) ;
#90636 = CARTESIAN_POINT('',(59.7,251.6,20.0213203435596)) ;
#90637 = CARTESIAN_POINT('Origin',(59.3,251.6,23.0213203435596)) ;
#90638 = CARTESIAN_POINT('Origin',(59.7,250.6,20.0213203435596)) ;
#90639 = CARTESIAN_POINT('',(59.7,253.2,23.0213203435596)) ;
#90640 = CARTESIAN_POINT('',(59.7,253.2,22.0213203435596)) ;
#90641 = CARTESIAN_POINT('',(59.7,242.,23.0213203435596)) ;
#90642 = CARTESIAN_POINT('Ctrl Pts',(59.6983561413947,253.201132335348,20.0213068391943)) ;
#90643 = CARTESIAN_POINT('Ctrl Pts',(59.6405833573623,253.138206691657,20.0213203435596)) ;
#90644 = CARTESIAN_POINT('Ctrl Pts',(59.5229242400133,253.015841209614,20.0213203435596)) ;
#90645 = CARTESIAN_POINT('Ctrl Pts',(59.3615012183121,252.847961267045,20.0213203435596)) ;
#90646 = CARTESIAN_POINT('Ctrl Pts',(59.2467429329946,252.728612650314,20.0213203435596)) ;
#90647 = CARTESIAN_POINT('Ctrl Pts',(59.1766245450661,252.655689526869,20.0213203435596)) ;
#90648 = CARTESIAN_POINT('Ctrl Pts',(59.1427392883506,252.620448859885,20.0213203435596)) ;
#90649 = CARTESIAN_POINT('Ctrl Pts',(59.1198396721444,252.59663325903,20.0213203435596)) ;
#90650 = CARTESIAN_POINT('Ctrl Pts',(59.1070160194856,252.583296660265,20.0213203435596)) ;
#90651 = CARTESIAN_POINT('Ctrl Pts',(59.100742188597,252.576771876141,20.0213203435596)) ;
#90652 = CARTESIAN_POINT('Ctrl Pts',(59.0976481299957,252.573554055196,20.0213203435596)) ;
#90653 = CARTESIAN_POINT('Ctrl Pts',(59.6983561413947,253.201132335348,20.0213068391943)) ;
#90654 = CARTESIAN_POINT('Ctrl Pts',(59.6387389889223,253.141348443802,20.0212943049799)) ;
#90655 = CARTESIAN_POINT('Ctrl Pts',(59.5177887613006,253.024552101869,20.0188009859938)) ;
#90656 = CARTESIAN_POINT('Ctrl Pts',(59.3547417480892,252.862674067239,20.0094198699614)) ;
#90657 = CARTESIAN_POINT('Ctrl Pts',(59.2436260334543,252.74520130829,19.9993245938688)) ;
#90658 = CARTESIAN_POINT('Ctrl Pts',(59.1797745588704,252.672296794036,19.9930704302621)) ;
#90659 = CARTESIAN_POINT('Ctrl Pts',(59.150461980661,252.636868221831,19.990450276081)) ;
#90660 = CARTESIAN_POINT('Ctrl Pts',(59.1317791109331,252.612984832977,19.9893039012676)) ;
#90661 = CARTESIAN_POINT('Ctrl Pts',(59.1217337199043,252.599697553955,19.9889950808986)) ;
#90662 = CARTESIAN_POINT('Ctrl Pts',(59.1169697132597,252.593243019353,19.9889876151247)) ;
#90663 = CARTESIAN_POINT('Ctrl Pts',(59.114661714354,252.590077279297,19.9890311381653)) ;
#90664 = CARTESIAN_POINT('Ctrl Pts',(59.6983561413947,253.201132335348,20.0213068391943)) ;
#90665 = CARTESIAN_POINT('Ctrl Pts',(59.6350498031855,253.147632380457,20.0212422231911)) ;
#90666 = CARTESIAN_POINT('Ctrl Pts',(59.5075447508945,253.041891485879,20.0149253757923)) ;
#90667 = CARTESIAN_POINT('Ctrl Pts',(59.3390921011038,252.89406358936,19.9902535879186)) ;
#90668 = CARTESIAN_POINT('Ctrl Pts',(59.2306666331395,252.784723922575,19.9617875770576)) ;
#90669 = CARTESIAN_POINT('Ctrl Pts',(59.174826300634,252.71614725735,19.942028468966)) ;
#90670 = CARTESIAN_POINT('Ctrl Pts',(59.151995644535,252.682857965521,19.9327134222409)) ;
#90671 = CARTESIAN_POINT('Ctrl Pts',(59.1397130985584,252.660746974676,19.9274872737863)) ;
#90672 = CARTESIAN_POINT('Ctrl Pts',(59.1340298579112,252.648674214786,19.9252363474521)) ;
#90673 = CARTESIAN_POINT('Ctrl Pts',(59.1316869209399,252.642917043708,19.9244431805881)) ;
#90674 = CARTESIAN_POINT('Ctrl Pts',(59.1306535459891,252.640131701431,19.9241575626337)) ;
#90675 = CARTESIAN_POINT('Ctrl Pts',(59.6983561413947,253.201132335348,20.0213068391943)) ;
#90676 = CARTESIAN_POINT('Ctrl Pts',(59.6250143371155,253.164724381672,20.0211005575757)) ;
#90677 = CARTESIAN_POINT('Ctrl Pts',(59.479716487384,253.089447846023,20.0098769411972)) ;
#90678 = CARTESIAN_POINT('Ctrl Pts',(59.2877528595915,252.985613790057,19.9648062300671)) ;
#90679 = CARTESIAN_POINT('Ctrl Pts',(59.1649824243651,252.911156238581,19.9083610107024)) ;
#90680 = CARTESIAN_POINT('Ctrl Pts',(59.1038826177998,252.866722375844,19.8630066618772)) ;
#90681 = CARTESIAN_POINT('Ctrl Pts',(59.0801924624728,252.846166525223,19.8385056723018)) ;
#90682 = CARTESIAN_POINT('Ctrl Pts',(59.0688119787604,252.833471233285,19.8212764972742)) ;
#90683 = CARTESIAN_POINT('Ctrl Pts',(59.0642587414283,252.826989190829,19.8117477346005)) ;
#90684 = CARTESIAN_POINT('Ctrl Pts',(59.0627109533308,252.824088799222,19.8072083560344)) ;
#90685 = CARTESIAN_POINT('Ctrl Pts',(59.0621414351439,252.822747469555,19.8050299254675)) ;
#90686 = CARTESIAN_POINT('Ctrl Pts',(59.6983561413947,253.201132335348,20.0213068391943)) ;
#90687 = CARTESIAN_POINT('Ctrl Pts',(59.6168230991084,253.17867209478,20.0209849428196)) ;
#90688 = CARTESIAN_POINT('Ctrl Pts',(59.4566744266614,253.127543443304,20.0173244896171)) ;
#90689 = CARTESIAN_POINT('Ctrl Pts',(59.235417471757,253.058718839497,19.9973837843722)) ;
#90690 = CARTESIAN_POINT('Ctrl Pts',(59.0741608580319,253.010488324297,19.9709643752037)) ;
#90691 = CARTESIAN_POINT('Ctrl Pts',(58.970763369431,252.979409797583,19.944956093994)) ;
#90692 = CARTESIAN_POINT('Ctrl Pts',(58.9186367041767,252.963112203106,19.928060513653)) ;
#90693 = CARTESIAN_POINT('Ctrl Pts',(58.8817163868829,252.950491410093,19.9126774778034)) ;
#90694 = CARTESIAN_POINT('Ctrl Pts',(58.8604121341276,252.942597577878,19.9022589536899)) ;
#90695 = CARTESIAN_POINT('Ctrl Pts',(58.8497660624433,252.938375656177,19.8964295097095)) ;
#90696 = CARTESIAN_POINT('Ctrl Pts',(58.8444584671265,252.936177800295,19.8933199111082)) ;
#90697 = CARTESIAN_POINT('Ctrl Pts',(59.6983561413947,253.201132335348,20.0213068391943)) ;
#90698 = CARTESIAN_POINT('Ctrl Pts',(59.6104804032961,253.18947021835,20.0208954293076)) ;
#90699 = CARTESIAN_POINT('Ctrl Pts',(59.4409767120307,253.161409042463,20.0226915082758)) ;
#90700 = CARTESIAN_POINT('Ctrl Pts',(59.2056496041379,253.099665034983,20.0428866978387)) ;
#90701 = CARTESIAN_POINT('Ctrl Pts',(59.0351181159364,253.021807165115,20.0645075503816)) ;
#90702 = CARTESIAN_POINT('Ctrl Pts',(58.9263998406049,252.945184792316,20.0751016605283)) ;
#90703 = CARTESIAN_POINT('Ctrl Pts',(58.8717548724627,252.896835253805,20.0775118985888)) ;
#90704 = CARTESIAN_POINT('Ctrl Pts',(58.8331279718619,252.855453382999,20.0755760868657)) ;
#90705 = CARTESIAN_POINT('Ctrl Pts',(58.8108414175582,252.828814232857,20.0726724433716)) ;
#90706 = CARTESIAN_POINT('Ctrl Pts',(58.7997165407889,252.814483766437,20.0704334854542)) ;
#90707 = CARTESIAN_POINT('Ctrl Pts',(58.7941662396937,252.80702403625,20.069077982382)) ;
#90708 = CARTESIAN_POINT('',(59.5076923076923,253.,20.0213203435596)) ;
#90709 = CARTESIAN_POINT('',(58.5931591083782,252.048885472713,20.0213203435596)) ;
#90710 = CARTESIAN_POINT('',(58.9535270326722,252.853553390409,19.8748737339686)) ;
#90711 = CARTESIAN_POINT('Ctrl Pts',(58.9535270332697,252.853553390621,19.8748737341804)) ;
#90712 = CARTESIAN_POINT('Ctrl Pts',(58.9544812639864,252.853959618843,19.8752799624022)) ;
#90713 = CARTESIAN_POINT('Ctrl Pts',(58.9554377472264,252.854363438162,19.8756837817213)) ;
#90714 = CARTESIAN_POINT('Ctrl Pts',(59.0080837204097,252.876415266471,19.8977356100307)) ;
#90715 = CARTESIAN_POINT('Ctrl Pts',(59.0819911038653,252.898174251807,19.9194945953742)) ;
#90716 = CARTESIAN_POINT('Ctrl Pts',(59.2187094508916,252.931982805319,19.9533031488854)) ;
#90717 = CARTESIAN_POINT('Ctrl Pts',(59.2544798933849,252.940439100737,19.9617594442965)) ;
#90718 = CARTESIAN_POINT('Ctrl Pts',(59.3184078361109,252.955441546707,19.9767618902667)) ;
#90719 = CARTESIAN_POINT('Ctrl Pts',(59.3580711003919,252.964683338623,19.9860036821827)) ;
#90720 = CARTESIAN_POINT('Ctrl Pts',(59.430373614325,252.981655902742,20.0029762463013)) ;
#90721 = CARTESIAN_POINT('Ctrl Pts',(59.4733907178604,252.991778140936,20.0130984844959)) ;
#90722 = CARTESIAN_POINT('Ctrl Pts',(59.5076923076922,253.,20.0213203435596)) ;
#90723 = CARTESIAN_POINT('',(59.6906222915952,253.199677791956,20.0212702067469)) ;
#90724 = CARTESIAN_POINT('Ctrl Pts',(58.9535270325137,252.853553390013,19.8748737335726)) ;
#90725 = CARTESIAN_POINT('Ctrl Pts',(58.9565617584117,252.855892584028,19.8772129275957)) ;
#90726 = CARTESIAN_POINT('Ctrl Pts',(58.9596988881571,252.858222716888,19.8794965005046)) ;
#90727 = CARTESIAN_POINT('Ctrl Pts',(58.9629217338132,252.860543300927,19.8817279974797)) ;
#90728 = CARTESIAN_POINT('Ctrl Pts',(58.9661445794694,252.862863884965,19.8839594944547)) ;
#90729 = CARTESIAN_POINT('Ctrl Pts',(58.9694531410364,252.865174920183,19.8861389154958)) ;
#90730 = CARTESIAN_POINT('Ctrl Pts',(58.9728284392491,252.867471315475,19.8882643714541)) ;
#90731 = CARTESIAN_POINT('Ctrl Pts',(58.9795790356745,252.872064106058,19.8925152833706)) ;
#90732 = CARTESIAN_POINT('Ctrl Pts',(58.9865965786828,252.876598336938,19.8965503349557)) ;
#90733 = CARTESIAN_POINT('Ctrl Pts',(58.9938251766377,252.881099271588,19.9004208018149)) ;
#90734 = CARTESIAN_POINT('Ctrl Pts',(59.0082823725472,252.890101140888,19.9081617355332)) ;
#90735 = CARTESIAN_POINT('Ctrl Pts',(59.0235837882427,252.898969825267,19.9152443303478)) ;
#90736 = CARTESIAN_POINT('Ctrl Pts',(59.0394887827122,252.907759632436,19.9218109468869)) ;
#90737 = CARTESIAN_POINT('Ctrl Pts',(59.0553937771816,252.916549439604,19.9283775634259)) ;
#90738 = CARTESIAN_POINT('Ctrl Pts',(59.071902350425,252.925260369562,19.9344282016893)) ;
#90739 = CARTESIAN_POINT('Ctrl Pts',(59.0887153135157,252.933877010233,19.940052639116)) ;
#90740 = CARTESIAN_POINT('Ctrl Pts',(59.1391542027878,252.959726932244,19.9569259513962)) ;
#90741 = CARTESIAN_POINT('Ctrl Pts',(59.1923326006852,252.984728250665,19.9699634561467)) ;
#90742 = CARTESIAN_POINT('Ctrl Pts',(59.2467899675908,253.009457808401,19.980592445341)) ;
#90743 = CARTESIAN_POINT('Ctrl Pts',(59.3193997901315,253.042430552049,19.9947644309334)) ;
#90744 = CARTESIAN_POINT('Ctrl Pts',(59.3942833353535,253.074920165588,20.0046546110925)) ;
#90745 = CARTESIAN_POINT('Ctrl Pts',(59.4697367320825,253.107111524934,20.0112252313073)) ;
#90746 = CARTESIAN_POINT('Ctrl Pts',(59.4792622083269,253.111175464293,20.0120547272542)) ;
#90747 = CARTESIAN_POINT('Ctrl Pts',(59.4887968912323,253.115234454755,20.0128312408816)) ;
#90748 = CARTESIAN_POINT('Ctrl Pts',(59.4983287695347,253.119280138962,20.01355466622)) ;
#90749 = CARTESIAN_POINT('Ctrl Pts',(59.5618746248842,253.146251367004,20.0183775018095)) ;
#90750 = CARTESIAN_POINT('Ctrl Pts',(59.6258593253504,253.172858346708,20.0208838985848)) ;
#90751 = CARTESIAN_POINT('Ctrl Pts',(59.6906214872845,253.198122842305,20.0212707200625)) ;
#90752 = CARTESIAN_POINT('Origin',(59.695235655795,253.2,20.1326604265405)) ;
#90753 = CARTESIAN_POINT('Origin',(66.25,251.8,20.0213203435596)) ;
#90754 = CARTESIAN_POINT('',(57.7535453536325,253.,20.0213203435596)) ;
#90755 = CARTESIAN_POINT('Origin',(49.257090707265,252.,19.0213203435596)) ;
#90756 = CARTESIAN_POINT('',(59.4538479685896,252.944303048062,19.965623391622)) ;
#90757 = CARTESIAN_POINT('Ctrl Pts',(59.4538479685897,252.944303048062,19.965623391622)) ;
#90758 = CARTESIAN_POINT('Ctrl Pts',(59.4795957437549,252.949199657807,19.9705200013664)) ;
#90759 = CARTESIAN_POINT('Ctrl Pts',(59.5039155081045,252.953845010205,19.9751653550366)) ;
#90760 = CARTESIAN_POINT('Ctrl Pts',(59.5551459406205,252.9637107836,19.9850311284307)) ;
#90761 = CARTESIAN_POINT('Ctrl Pts',(59.5822031562559,252.968956670847,19.9902770144069)) ;
#90762 = CARTESIAN_POINT('Ctrl Pts',(59.60747650753,252.973908029254,19.9952283728131)) ;
#90763 = CARTESIAN_POINT('',(59.0238256449734,252.853553390593,19.8748737341529)) ;
#90764 = CARTESIAN_POINT('Ctrl Pts',(59.4538479685896,252.944303048062,19.965623391622)) ;
#90765 = CARTESIAN_POINT('Ctrl Pts',(59.3652369852379,252.927451362751,19.9487717063111)) ;
#90766 = CARTESIAN_POINT('Ctrl Pts',(59.3092068635467,252.917036967626,19.9383573111849)) ;
#90767 = CARTESIAN_POINT('Ctrl Pts',(59.1694500968853,252.888903295121,19.91022363868)) ;
#90768 = CARTESIAN_POINT('Ctrl Pts',(59.096657519322,252.8730579694,19.8943783129598)) ;
#90769 = CARTESIAN_POINT('Ctrl Pts',(59.0254737954579,252.853996221768,19.8753165653275)) ;
#90770 = CARTESIAN_POINT('Ctrl Pts',(59.0246496511332,252.853775036505,19.8750953800646)) ;
#90771 = CARTESIAN_POINT('Ctrl Pts',(59.0238256449756,252.853553390593,19.874873734153)) ;
#90772 = CARTESIAN_POINT('',(58.7659637180533,252.658578643763,19.6798989873223)) ;
#90773 = CARTESIAN_POINT('Origin',(59.3208772194954,252.658578643763,19.6798989873223)) ;
#90774 = CARTESIAN_POINT('',(58.508445556536,252.390759755785,19.4120800993443)) ;
#90775 = CARTESIAN_POINT('',(57.5854307313793,251.430824337622,18.4521446811814)) ;
#90776 = CARTESIAN_POINT('',(58.3670916964374,252.229977120843,19.2512974644025)) ;
#90777 = CARTESIAN_POINT('Ctrl Pts',(58.3670916964374,252.229977120843,19.2512974644025)) ;
#90778 = CARTESIAN_POINT('Ctrl Pts',(58.3959491235504,252.259719824999,19.2810401685591)) ;
#90779 = CARTESIAN_POINT('Ctrl Pts',(58.4427197527521,252.313512630762,19.3348329743217)) ;
#90780 = CARTESIAN_POINT('Ctrl Pts',(58.4869349700687,252.368388745859,19.3897090894184)) ;
#90781 = CARTESIAN_POINT('Ctrl Pts',(58.508445556536,252.390759755785,19.4120800993443)) ;
#90782 = CARTESIAN_POINT('',(57.3882337581722,251.21966991411,18.2409902576697)) ;
#90783 = CARTESIAN_POINT('Origin',(62.771739895016,256.247475826304,23.2687961698638)) ;
#90784 = CARTESIAN_POINT('',(46.,251.21966991411,18.2409902576697)) ;
#90785 = CARTESIAN_POINT('',(52.2356360608974,251.21966991411,18.2409902576697)) ;
#90786 = CARTESIAN_POINT('',(46.,252.270294372515,19.2916147160749)) ;
#90787 = CARTESIAN_POINT('',(46.,249.975,16.9963203435596)) ;
#90788 = CARTESIAN_POINT('',(43.4,252.270294372515,19.2916147160749)) ;
#90789 = CARTESIAN_POINT('',(44.7285453536325,252.270294372515,19.2916147160749)) ;
#90790 = CARTESIAN_POINT('',(43.4,252.670710678119,19.6920310216783)) ;
#90791 = CARTESIAN_POINT('',(43.4,254.65,21.6713203435596)) ;
#90792 = CARTESIAN_POINT('',(43.4621585770309,252.85355339061,19.8748737341699)) ;
#90793 = CARTESIAN_POINT('Origin',(43.7,252.670710678119,19.6920310216783)) ;
#90794 = CARTESIAN_POINT('',(47.7791083033805,252.853553390593,19.8748737341529)) ;
#90795 = CARTESIAN_POINT('',(52.2356360608974,252.853553390593,19.8748737341529)) ;
#90796 = CARTESIAN_POINT('',(54.6208916966195,252.853553390593,19.8748737341529)) ;
#90797 = CARTESIAN_POINT('Origin',(51.2,255.853553390593,22.8748737341529)) ;
#90798 = CARTESIAN_POINT('',(52.2356360608974,252.853553390593,19.8748737341529)) ;
#90799 = CARTESIAN_POINT('Ctrl Pts',(34.7000000219136,245.200029079685,18.9812108522455)) ;
#90800 = CARTESIAN_POINT('Ctrl Pts',(34.7000093384897,245.17006613755,18.9811792211247)) ;
#90801 = CARTESIAN_POINT('Ctrl Pts',(34.6748288409442,245.118261285358,19.0666706061063)) ;
#90802 = CARTESIAN_POINT('Ctrl Pts',(34.6224243037673,245.1,19.2450088782142)) ;
#90803 = CARTESIAN_POINT('Ctrl Pts',(34.6,245.1,19.3213203435596)) ;
#90804 = CARTESIAN_POINT('Ctrl Pts',(34.6999696741166,245.200010627956,19.0440796070764)) ;
#90805 = CARTESIAN_POINT('Ctrl Pts',(34.6999676399907,245.18906525137,19.0440605781652)) ;
#90806 = CARTESIAN_POINT('Ctrl Pts',(34.7054733072358,245.140987432299,19.095486456445)) ;
#90807 = CARTESIAN_POINT('Ctrl Pts',(34.6314054973637,245.1,19.2539900718105)) ;
#90808 = CARTESIAN_POINT('Ctrl Pts',(34.6,245.1,19.3213203435596)) ;
#90809 = CARTESIAN_POINT('Ctrl Pts',(34.7521917241297,245.199989665103,19.16912861943)) ;
#90810 = CARTESIAN_POINT('Ctrl Pts',(34.7521859728801,245.210650489643,19.1691343706795)) ;
#90811 = CARTESIAN_POINT('Ctrl Pts',(34.7677441747257,245.164070188481,19.153576168834)) ;
#90812 = CARTESIAN_POINT('Ctrl Pts',(34.6493678845564,245.1,19.2719524590032)) ;
#90813 = CARTESIAN_POINT('Ctrl Pts',(34.6,245.1,19.3213203435596)) ;
#90814 = CARTESIAN_POINT('Ctrl Pts',(34.8772407364833,245.200010627956,19.221350669443)) ;
#90815 = CARTESIAN_POINT('Ctrl Pts',(34.8772597653945,245.18906525137,19.2213527035689)) ;
#90816 = CARTESIAN_POINT('Ctrl Pts',(34.8258338871147,245.140987432298,19.2158470363238)) ;
#90817 = CARTESIAN_POINT('Ctrl Pts',(34.6673302717491,245.1,19.2899148461959)) ;
#90818 = CARTESIAN_POINT('Ctrl Pts',(34.6,245.1,19.3213203435596)) ;
#90819 = CARTESIAN_POINT('Ctrl Pts',(34.9401094913142,245.200029079685,19.2213203216461)) ;
#90820 = CARTESIAN_POINT('Ctrl Pts',(34.940141122435,245.17006613755,19.2213110050699)) ;
#90821 = CARTESIAN_POINT('Ctrl Pts',(34.8546497374533,245.118261285358,19.2464915026154)) ;
#90822 = CARTESIAN_POINT('Ctrl Pts',(34.6763114653455,245.1,19.2988960397923)) ;
#90823 = CARTESIAN_POINT('Ctrl Pts',(34.6,245.1,19.3213203435596)) ;
#90824 = CARTESIAN_POINT('',(34.7,245.2,18.9813203435596)) ;
#90825 = CARTESIAN_POINT('',(34.94,245.2,19.2213203435596)) ;
#90826 = CARTESIAN_POINT('Origin',(34.94,245.2,18.9813203435596)) ;
#90827 = CARTESIAN_POINT('',(34.812048130896,245.121831303122,19.2589532462372)) ;
#90828 = CARTESIAN_POINT('Origin',(34.6,245.2,19.3213203435596)) ;
#90829 = CARTESIAN_POINT('',(34.6,245.1,19.3213203435596)) ;
#90830 = CARTESIAN_POINT('Origin',(34.6,245.2,19.3213203435596)) ;
#90831 = CARTESIAN_POINT('',(34.6623670973224,245.121831303122,19.1092722126636)) ;
#90832 = CARTESIAN_POINT('Origin',(34.6,245.2,19.3213203435596)) ;
#90833 = CARTESIAN_POINT('Origin',(34.6,245.2,19.3213203435596)) ;
#90834 = CARTESIAN_POINT('Origin',(34.94,252.4,18.9813203435596)) ;
#90835 = CARTESIAN_POINT('',(34.7,251.535735931288,18.9813203435596)) ;
#90836 = CARTESIAN_POINT('',(34.94,251.535735931288,19.2213203435596)) ;
#90837 = CARTESIAN_POINT('Origin',(34.94,251.535735931288,18.9813203435596)) ;
#90838 = CARTESIAN_POINT('',(34.94,252.4,19.2213203435596)) ;
#90839 = CARTESIAN_POINT('',(34.7,252.4,18.9813203435596)) ;
#90840 = CARTESIAN_POINT('Ctrl Pts',(34.6017339105327,251.97522832562,19.1067953741799)) ;
#90841 = CARTESIAN_POINT('Ctrl Pts',(34.6634134588563,251.864241814735,19.0750536538863)) ;
#90842 = CARTESIAN_POINT('Ctrl Pts',(34.7000061973417,251.700474278475,19.028221281181)) ;
#90843 = CARTESIAN_POINT('Ctrl Pts',(34.7000001095966,251.535435370687,18.9810436611381)) ;
#90844 = CARTESIAN_POINT('Ctrl Pts',(34.6185891138952,251.988340545982,19.1416152707518)) ;
#90845 = CARTESIAN_POINT('Ctrl Pts',(34.6820644896349,251.871454352969,19.118504383798)) ;
#90846 = CARTESIAN_POINT('Ctrl Pts',(34.7125874913099,251.700356151572,19.0833081167134)) ;
#90847 = CARTESIAN_POINT('Ctrl Pts',(34.6999241628191,251.535435577959,19.0439540541464)) ;
#90848 = CARTESIAN_POINT('Ctrl Pts',(34.6666204996312,252.025705917447,19.1999857849512)) ;
#90849 = CARTESIAN_POINT('Ctrl Pts',(34.7426835812045,251.897727354795,19.1933392410231)) ;
#90850 = CARTESIAN_POINT('Ctrl Pts',(34.7752829676017,251.710693056027,19.1828544398397)) ;
#90851 = CARTESIAN_POINT('Ctrl Pts',(34.752107940643,251.535416712293,19.1690554827065)) ;
#90852 = CARTESIAN_POINT('Ctrl Pts',(34.7310058064877,252.075793529964,19.2213202461027)) ;
#90853 = CARTESIAN_POINT('Ctrl Pts',(34.8303563319875,251.937975750104,19.2213739807519)) ;
#90854 = CARTESIAN_POINT('Ctrl Pts',(34.8851586497759,251.735194021102,19.2210635103389)) ;
#90855 = CARTESIAN_POINT('Ctrl Pts',(34.8771536379644,251.535372020486,19.2213208115184)) ;
#90856 = CARTESIAN_POINT('Ctrl Pts',(34.7632130987747,252.100848735699,19.2213203435596)) ;
#90857 = CARTESIAN_POINT('Ctrl Pts',(34.8742461148383,251.958128788049,19.2213203435596)) ;
#90858 = CARTESIAN_POINT('Ctrl Pts',(34.9400799458861,251.747541937871,19.2213203435596)) ;
#90859 = CARTESIAN_POINT('Ctrl Pts',(34.9399999271389,251.535349497,19.2213203435596)) ;
#90860 = CARTESIAN_POINT('',(34.6018973652929,251.975065897532,19.1068431910579)) ;
#90861 = CARTESIAN_POINT('',(34.7634152575273,252.100588745031,19.2213203435596)) ;
#90862 = CARTESIAN_POINT('Origin',(34.7634152575273,252.100588745031,18.9813203435596)) ;
#90863 = CARTESIAN_POINT('Origin',(34.4,251.535735931288,19.2213203435596)) ;
#90864 = CARTESIAN_POINT('Origin',(34.4,251.535735931288,18.9813203435596)) ;
#90865 = CARTESIAN_POINT('Ctrl Pts',(34.7634152575273,252.100588745031,19.2213203435596)) ;
#90866 = CARTESIAN_POINT('Ctrl Pts',(34.6573341599048,252.168839249362,19.2213203435596)) ;
#90867 = CARTESIAN_POINT('Ctrl Pts',(34.528261189473,252.227295182387,19.2491278924933)) ;
#90868 = CARTESIAN_POINT('Ctrl Pts',(34.4017755136714,252.269701879201,19.2910234275852)) ;
#90869 = CARTESIAN_POINT('Ctrl Pts',(34.4008872944232,252.269998607705,19.2913189512647)) ;
#90870 = CARTESIAN_POINT('Ctrl Pts',(34.4,252.270294372515,19.2916147160749)) ;
#90871 = CARTESIAN_POINT('Ctrl Pts',(34.6989581230585,252.050496195232,19.2213203435596)) ;
#90872 = CARTESIAN_POINT('Ctrl Pts',(34.6197281326642,252.126885662221,19.2061907587185)) ;
#90873 = CARTESIAN_POINT('Ctrl Pts',(34.5092623007076,252.213208210922,19.2345935259517)) ;
#90874 = CARTESIAN_POINT('Ctrl Pts',(34.401512470054,252.269502550543,19.2908287731336)) ;
#90875 = CARTESIAN_POINT('Ctrl Pts',(34.4007558433964,252.269900019436,19.2912203629956)) ;
#90876 = CARTESIAN_POINT('Ctrl Pts',(34.4,252.270294372515,19.2916147160749)) ;
#90877 = CARTESIAN_POINT('Ctrl Pts',(34.6356092113767,252.001264895404,19.1764212743414)) ;
#90878 = CARTESIAN_POINT('Ctrl Pts',(34.5811287956459,252.097389804567,19.177622597453)) ;
#90879 = CARTESIAN_POINT('Ctrl Pts',(34.4903264917909,252.198996115397,19.2204192832181)) ;
#90880 = CARTESIAN_POINT('Ctrl Pts',(34.4012491049424,252.269305008193,19.290631181609)) ;
#90881 = CARTESIAN_POINT('Ctrl Pts',(34.4006243923697,252.269801431167,19.2911217747264)) ;
#90882 = CARTESIAN_POINT('Ctrl Pts',(34.4,252.270294372515,19.2916147160749)) ;
#90883 = CARTESIAN_POINT('Ctrl Pts',(34.6018973652929,251.975065897532,19.106843191058)) ;
#90884 = CARTESIAN_POINT('Ctrl Pts',(34.5429634221693,252.081233348715,19.1371767485388)) ;
#90885 = CARTESIAN_POINT('Ctrl Pts',(34.4712562163731,252.184523710722,19.2064133504464)) ;
#90886 = CARTESIAN_POINT('Ctrl Pts',(34.4009863964841,252.269109921364,19.2904316036179)) ;
#90887 = CARTESIAN_POINT('Ctrl Pts',(34.4004929413429,252.269702842897,19.2910231864568)) ;
#90888 = CARTESIAN_POINT('Ctrl Pts',(34.4,252.270294372515,19.2916147160749)) ;
#90889 = CARTESIAN_POINT('',(34.4,252.270294372515,19.2916147160749)) ;
#90890 = CARTESIAN_POINT('Ctrl Pts',(34.6018973652929,251.975065897532,19.106843191058)) ;
#90891 = CARTESIAN_POINT('Ctrl Pts',(34.5429634221693,252.081233348715,19.1371767485388)) ;
#90892 = CARTESIAN_POINT('Ctrl Pts',(34.4712562163731,252.184523710722,19.2064133504464)) ;
#90893 = CARTESIAN_POINT('Ctrl Pts',(34.4009863964841,252.269109921364,19.2904316036179)) ;
#90894 = CARTESIAN_POINT('Ctrl Pts',(34.4004929413429,252.269702842897,19.2910231864568)) ;
#90895 = CARTESIAN_POINT('Ctrl Pts',(34.4,252.270294372515,19.2916147160749)) ;
#90896 = CARTESIAN_POINT('Ctrl Pts',(34.4,252.270294372515,19.2916147160749)) ;
#90897 = CARTESIAN_POINT('Ctrl Pts',(34.4008872944232,252.269998607705,19.2913189512647)) ;
#90898 = CARTESIAN_POINT('Ctrl Pts',(34.4017755136714,252.269701879201,19.2910234275852)) ;
#90899 = CARTESIAN_POINT('Ctrl Pts',(34.528261189473,252.227295182387,19.2491278924933)) ;
#90900 = CARTESIAN_POINT('Ctrl Pts',(34.6573341599048,252.168839249362,19.2213203435596)) ;
#90901 = CARTESIAN_POINT('Ctrl Pts',(34.7634152575273,252.100588745031,19.2213203435596)) ;
#90902 = CARTESIAN_POINT('Origin',(34.4,252.262867965644,19.7084523779156)) ;
#90903 = CARTESIAN_POINT('',(34.7,251.007537879754,18.4531222920257)) ;
#90904 = CARTESIAN_POINT('',(34.7,252.262867965644,19.7084523779156)) ;
#90905 = CARTESIAN_POINT('',(34.4,251.21966991411,18.2409902576697)) ;
#90906 = CARTESIAN_POINT('Origin',(34.4,251.007537879754,18.4531222920257)) ;
#90907 = CARTESIAN_POINT('',(34.4,252.475,19.4963203435596)) ;
#90908 = CARTESIAN_POINT('Origin',(34.7,254.9,18.0213203435596)) ;
#90909 = CARTESIAN_POINT('',(34.7,245.2,18.3213203435596)) ;
#90910 = CARTESIAN_POINT('',(34.7,245.2,23.7713203435596)) ;
#90911 = CARTESIAN_POINT('',(34.7,250.68933982822,18.3213203435596)) ;
#90912 = CARTESIAN_POINT('',(34.7,251.975,18.3213203435596)) ;
#90913 = CARTESIAN_POINT('Origin',(34.7,250.68933982822,18.7713203435596)) ;
#90914 = CARTESIAN_POINT('Origin',(34.6,245.2,23.7713203435596)) ;
#90915 = CARTESIAN_POINT('',(34.6,245.1,18.3213203435596)) ;
#90916 = CARTESIAN_POINT('',(34.6,245.1,23.7713203435596)) ;
#90917 = CARTESIAN_POINT('Origin',(34.6,245.2,18.3213203435596)) ;
#90918 = CARTESIAN_POINT('Ctrl Pts',(45.8,245.1,19.3213203435596)) ;
#90919 = CARTESIAN_POINT('Ctrl Pts',(45.7701101736509,245.1,19.2195624777583)) ;
#90920 = CARTESIAN_POINT('Ctrl Pts',(45.7183540340142,245.125062832338,19.0433988064518)) ;
#90921 = CARTESIAN_POINT('Ctrl Pts',(45.6999901429942,245.177552241659,18.9811290612227)) ;
#90922 = CARTESIAN_POINT('Ctrl Pts',(45.6999999540947,245.200041989469,18.9811623295317)) ;
#90923 = CARTESIAN_POINT('Ctrl Pts',(45.8,245.1,19.3213203435596)) ;
#90924 = CARTESIAN_POINT('Ctrl Pts',(45.7581321670755,245.1,19.2315404843337)) ;
#90925 = CARTESIAN_POINT('Ctrl Pts',(45.6904763225037,245.153565681928,19.0780179164569)) ;
#90926 = CARTESIAN_POINT('Ctrl Pts',(45.7000488684854,245.19180184345,19.0440292695842)) ;
#90927 = CARTESIAN_POINT('Ctrl Pts',(45.7000437609983,245.200015344509,19.0440474324887)) ;
#90928 = CARTESIAN_POINT('Ctrl Pts',(45.8,245.1,19.3213203435596)) ;
#90929 = CARTESIAN_POINT('Ctrl Pts',(45.7341761539248,245.1,19.2554964974844)) ;
#90930 = CARTESIAN_POINT('Ctrl Pts',(45.6263979131407,245.183234588789,19.1477182567004)) ;
#90931 = CARTESIAN_POINT('Ctrl Pts',(45.6478283493969,245.207992331203,19.1691486929565)) ;
#90932 = CARTESIAN_POINT('Ctrl Pts',(45.6478169119502,245.199985071692,19.1691372555099)) ;
#90933 = CARTESIAN_POINT('Ctrl Pts',(45.8,245.1,19.3213203435596)) ;
#90934 = CARTESIAN_POINT('Ctrl Pts',(45.710220140774,245.1,19.2794525106351)) ;
#90935 = CARTESIAN_POINT('Ctrl Pts',(45.5566975728973,245.153565681928,19.2117966660634)) ;
#90936 = CARTESIAN_POINT('Ctrl Pts',(45.5227089260246,245.19180184345,19.221369212045)) ;
#90937 = CARTESIAN_POINT('Ctrl Pts',(45.522727088929,245.200015344509,19.2213641045579)) ;
#90938 = CARTESIAN_POINT('Ctrl Pts',(45.8,245.1,19.3213203435596)) ;
#90939 = CARTESIAN_POINT('Ctrl Pts',(45.6982421341987,245.1,19.2914305172105)) ;
#90940 = CARTESIAN_POINT('Ctrl Pts',(45.5220784628922,245.125062832338,19.2396743775738)) ;
#90941 = CARTESIAN_POINT('Ctrl Pts',(45.4598087176631,245.177552241659,19.2213104865538)) ;
#90942 = CARTESIAN_POINT('Ctrl Pts',(45.459841985972,245.200041989469,19.2213202976544)) ;
#90943 = CARTESIAN_POINT('',(45.46,245.2,19.2213203435596)) ;
#90944 = CARTESIAN_POINT('',(45.7,245.2,18.9813203435596)) ;
#90945 = CARTESIAN_POINT('Origin',(45.46,245.2,18.9813203435596)) ;
#90946 = CARTESIAN_POINT('',(45.7337685111545,245.125077440745,19.0961332814849)) ;
#90947 = CARTESIAN_POINT('Origin',(45.8,245.2,19.3213203435596)) ;
#90948 = CARTESIAN_POINT('',(45.8,245.1,19.3213203435596)) ;
#90949 = CARTESIAN_POINT('Origin',(45.8,245.2,19.3213203435596)) ;
#90950 = CARTESIAN_POINT('',(45.5748129379279,245.125077440744,19.2550888547148)) ;
#90951 = CARTESIAN_POINT('Origin',(45.8,245.2,19.3213203435596)) ;
#90952 = CARTESIAN_POINT('Origin',(45.8,245.2,19.3213203435596)) ;
#90953 = CARTESIAN_POINT('Origin',(45.46,247.4,18.9813203435596)) ;
#90954 = CARTESIAN_POINT('',(45.46,251.535735931288,19.2213203435596)) ;
#90955 = CARTESIAN_POINT('',(45.7,251.535735931288,18.9813203435596)) ;
#90956 = CARTESIAN_POINT('Origin',(45.46,251.535735931288,18.9813203435596)) ;
#90957 = CARTESIAN_POINT('',(45.7,247.4,18.9813203435596)) ;
#90958 = CARTESIAN_POINT('',(45.46,247.4,19.2213203435596)) ;
#90959 = CARTESIAN_POINT('Ctrl Pts',(45.6999998904024,251.535435370679,18.9810436611296)) ;
#90960 = CARTESIAN_POINT('Ctrl Pts',(45.699993802657,251.700474278472,19.0282212811746)) ;
#90961 = CARTESIAN_POINT('Ctrl Pts',(45.7365865411453,251.864241814738,19.0750536538836)) ;
#90962 = CARTESIAN_POINT('Ctrl Pts',(45.7982660894715,251.975228325624,19.1067953741784)) ;
#90963 = CARTESIAN_POINT('Ctrl Pts',(45.7000758378912,251.535435577951,19.0439540548493)) ;
#90964 = CARTESIAN_POINT('Ctrl Pts',(45.6874125093996,251.700356151569,19.083308117419)) ;
#90965 = CARTESIAN_POINT('Ctrl Pts',(45.7179355104384,251.871454352916,19.1185043839603)) ;
#90966 = CARTESIAN_POINT('Ctrl Pts',(45.7814108861818,251.98834054593,19.1416152709156)) ;
#90967 = CARTESIAN_POINT('Ctrl Pts',(45.647891359541,251.535416712284,19.1690547828863)) ;
#90968 = CARTESIAN_POINT('Ctrl Pts',(45.6247163318147,251.710693055956,19.1828537393655)) ;
#90969 = CARTESIAN_POINT('Ctrl Pts',(45.6573163478517,251.897727410595,19.1933390793962)) ;
#90970 = CARTESIAN_POINT('Ctrl Pts',(45.7333794286637,252.025705973181,19.1999856226698)) ;
#90971 = CARTESIAN_POINT('Ctrl Pts',(45.522846362036,251.535372020476,19.2213208115184)) ;
#90972 = CARTESIAN_POINT('Ctrl Pts',(45.5148413502221,251.735194021099,19.2210635103388)) ;
#90973 = CARTESIAN_POINT('Ctrl Pts',(45.5696436680127,251.937975750109,19.2213739807519)) ;
#90974 = CARTESIAN_POINT('Ctrl Pts',(45.6689941935172,252.075793529971,19.2213202461027)) ;
#90975 = CARTESIAN_POINT('Ctrl Pts',(45.4600000728611,251.535349496989,19.2213203435596)) ;
#90976 = CARTESIAN_POINT('Ctrl Pts',(45.4599200541118,251.747541937868,19.2213203435596)) ;
#90977 = CARTESIAN_POINT('Ctrl Pts',(45.525753885162,251.958128788054,19.2213203435596)) ;
#90978 = CARTESIAN_POINT('Ctrl Pts',(45.6367869012307,252.100848735706,19.2213203435596)) ;
#90979 = CARTESIAN_POINT('',(45.6365847424727,252.100588745031,19.2213203435596)) ;
#90980 = CARTESIAN_POINT('',(45.798102634707,251.975065897532,19.1068431910579)) ;
#90981 = CARTESIAN_POINT('Origin',(45.6365847424727,252.100588745031,18.9813203435596)) ;
#90982 = CARTESIAN_POINT('Origin',(46.,251.535735931288,18.9813203435596)) ;
#90983 = CARTESIAN_POINT('Origin',(46.,251.535735931288,19.2213203435596)) ;
#90984 = CARTESIAN_POINT('Ctrl Pts',(46.,252.270294372515,19.2916147160749)) ;
#90985 = CARTESIAN_POINT('Ctrl Pts',(45.9991127055774,252.269998607706,19.2913189512654)) ;
#90986 = CARTESIAN_POINT('Ctrl Pts',(45.9982244863323,252.269701879202,19.2910234275873)) ;
#90987 = CARTESIAN_POINT('Ctrl Pts',(45.87173880933,252.22729518208,19.2491278919541)) ;
#90988 = CARTESIAN_POINT('Ctrl Pts',(45.7426658400944,252.168839249362,19.2213203435596)) ;
#90989 = CARTESIAN_POINT('Ctrl Pts',(45.6365847424727,252.100588745031,19.2213203435596)) ;
#90990 = CARTESIAN_POINT('Ctrl Pts',(46.,252.270294372515,19.2916147160749)) ;
#90991 = CARTESIAN_POINT('Ctrl Pts',(45.9992432480265,252.269899128634,19.2912194721931)) ;
#90992 = CARTESIAN_POINT('Ctrl Pts',(45.9984881400231,252.269484042833,19.2908487161059)) ;
#90993 = CARTESIAN_POINT('Ctrl Pts',(45.8908075064141,252.213536269908,19.2342664523398)) ;
#90994 = CARTESIAN_POINT('Ctrl Pts',(45.7804734503348,252.127653985431,19.205962938089)) ;
#90995 = CARTESIAN_POINT('Ctrl Pts',(45.7010418769414,252.050496195232,19.2213203435596)) ;
#90996 = CARTESIAN_POINT('Ctrl Pts',(46.,252.270294372515,19.2916147160749)) ;
#90997 = CARTESIAN_POINT('Ctrl Pts',(45.9993751441279,252.269800058411,19.2911204019704)) ;
#90998 = CARTESIAN_POINT('Ctrl Pts',(45.9987511914088,252.269287284606,19.290651085124)) ;
#90999 = CARTESIAN_POINT('Ctrl Pts',(45.9096857659592,252.199356446256,19.2201402522094)) ;
#91000 = CARTESIAN_POINT('Ctrl Pts',(45.8192755842025,252.09797381701,19.1772675246916)) ;
#91001 = CARTESIAN_POINT('Ctrl Pts',(45.7643907886233,252.001264895404,19.1764212743414)) ;
#91002 = CARTESIAN_POINT('Ctrl Pts',(46.,252.270294372515,19.2916147160749)) ;
#91003 = CARTESIAN_POINT('Ctrl Pts',(45.9995070586569,252.269702842898,19.2910231864577)) ;
#91004 = CARTESIAN_POINT('Ctrl Pts',(45.999013603518,252.269109921366,19.2904316036215)) ;
#91005 = CARTESIAN_POINT('Ctrl Pts',(45.9287437829605,252.184523710006,19.2064133494711)) ;
#91006 = CARTESIAN_POINT('Ctrl Pts',(45.8570365778302,252.081233348715,19.1371767485386)) ;
#91007 = CARTESIAN_POINT('Ctrl Pts',(45.798102634707,251.975065897532,19.106843191058)) ;
#91008 = CARTESIAN_POINT('',(45.9943955116219,252.2684153652,19.2897579022715)) ;
#91009 = CARTESIAN_POINT('Ctrl Pts',(45.6365847424727,252.100588745031,19.2213203435596)) ;
#91010 = CARTESIAN_POINT('Ctrl Pts',(45.7418374703499,252.168306292463,19.2213203435596)) ;
#91011 = CARTESIAN_POINT('Ctrl Pts',(45.8697243923924,252.226381639409,19.2486952985084)) ;
#91012 = CARTESIAN_POINT('Ctrl Pts',(45.9943955116219,252.2684153652,19.2897579022714)) ;
#91013 = CARTESIAN_POINT('Ctrl Pts',(45.9943955116219,252.2684153652,19.2897579022714)) ;
#91014 = CARTESIAN_POINT('Ctrl Pts',(45.9953767097843,252.268746182913,19.2900810769698)) ;
#91015 = CARTESIAN_POINT('Ctrl Pts',(45.996357708755,252.269076006983,19.2904050995018)) ;
#91016 = CARTESIAN_POINT('Ctrl Pts',(45.9982244863323,252.269701879202,19.2910234275873)) ;
#91017 = CARTESIAN_POINT('Ctrl Pts',(45.9991127055774,252.269998607706,19.2913189512654)) ;
#91018 = CARTESIAN_POINT('Ctrl Pts',(46.,252.270294372515,19.2916147160749)) ;
#91019 = CARTESIAN_POINT('',(45.996886678812,252.266546563962,19.287891562564)) ;
#91020 = CARTESIAN_POINT('Ctrl Pts',(46.,252.270294372515,19.2916147160749)) ;
#91021 = CARTESIAN_POINT('Ctrl Pts',(45.9995070586569,252.269702842898,19.2910231864577)) ;
#91022 = CARTESIAN_POINT('Ctrl Pts',(45.999013603518,252.269109921366,19.2904316036215)) ;
#91023 = CARTESIAN_POINT('Ctrl Pts',(45.9979765993132,252.267861643568,19.2891917074307)) ;
#91024 = CARTESIAN_POINT('Ctrl Pts',(45.9974316943751,252.267204687989,19.2885411965337)) ;
#91025 = CARTESIAN_POINT('Ctrl Pts',(45.996886678812,252.266546563962,19.287891562564)) ;
#91026 = CARTESIAN_POINT('Ctrl Pts',(45.996886678812,252.266546563962,19.287891562564)) ;
#91027 = CARTESIAN_POINT('Ctrl Pts',(45.9276248562919,252.182910659558,19.20533459398)) ;
#91028 = CARTESIAN_POINT('Ctrl Pts',(45.8565764521882,252.080404448356,19.1369399198645)) ;
#91029 = CARTESIAN_POINT('Ctrl Pts',(45.798102634707,251.975065897532,19.106843191058)) ;
#91030 = CARTESIAN_POINT('Origin',(40.2,249.9,19.2213203435596)) ;
#91031 = CARTESIAN_POINT('',(37.,252.100588745031,19.2213203435596)) ;
#91032 = CARTESIAN_POINT('',(44.7285453536325,252.100588745031,19.2213203435596)) ;
#91033 = CARTESIAN_POINT('',(37.,252.1,19.2213203435596)) ;
#91034 = CARTESIAN_POINT('',(37.,254.9,19.2213203435596)) ;
#91035 = CARTESIAN_POINT('',(37.3,251.8,19.2213203435596)) ;
#91036 = CARTESIAN_POINT('Origin',(37.3,252.1,19.2213203435596)) ;
#91037 = CARTESIAN_POINT('',(43.1,251.8,19.2213203435596)) ;
#91038 = CARTESIAN_POINT('',(38.75,251.8,19.2213203435596)) ;
#91039 = CARTESIAN_POINT('',(43.4,252.1,19.2213203435596)) ;
#91040 = CARTESIAN_POINT('Origin',(43.1,252.1,19.2213203435596)) ;
#91041 = CARTESIAN_POINT('',(43.4,252.100588745031,19.2213203435596)) ;
#91042 = CARTESIAN_POINT('',(43.4,251.,19.2213203435596)) ;
#91043 = CARTESIAN_POINT('',(44.7285453536325,252.100588745031,19.2213203435596)) ;
#91044 = CARTESIAN_POINT('',(41.6,245.2,19.2213203435596)) ;
#91045 = CARTESIAN_POINT('',(47.7786796564403,245.2,19.2213203435596)) ;
#91046 = CARTESIAN_POINT('',(41.6000000000001,242.9,19.2213203435596)) ;
#91047 = CARTESIAN_POINT('',(41.6,246.4,19.2213203435596)) ;
#91048 = CARTESIAN_POINT('',(38.8,242.9,19.2213203435596)) ;
#91049 = CARTESIAN_POINT('Origin',(40.2,242.9,19.2213203435596)) ;
#91050 = CARTESIAN_POINT('',(38.8,245.2,19.2213203435596)) ;
#91051 = CARTESIAN_POINT('',(38.8,247.5,19.2213203435596)) ;
#91052 = CARTESIAN_POINT('',(47.7786796564403,245.2,19.2213203435596)) ;
#91053 = CARTESIAN_POINT('Origin',(47.7786796564403,245.2,19.3213203435596)) ;
#91054 = CARTESIAN_POINT('',(41.7,245.1,19.3213203435596)) ;
#91055 = CARTESIAN_POINT('',(47.7786796564403,245.1,19.3213203435596)) ;
#91056 = CARTESIAN_POINT('Origin',(41.6,245.2,19.3213203435596)) ;
#91057 = CARTESIAN_POINT('Origin',(45.8,245.2,23.7713203435596)) ;
#91058 = CARTESIAN_POINT('',(45.7,245.2,18.3213203435596)) ;
#91059 = CARTESIAN_POINT('',(45.7,245.2,23.7713203435596)) ;
#91060 = CARTESIAN_POINT('',(45.8,245.1,18.3213203435596)) ;
#91061 = CARTESIAN_POINT('Origin',(45.8,245.2,18.3213203435596)) ;
#91062 = CARTESIAN_POINT('',(45.8,245.1,23.7713203435596)) ;
#91063 = CARTESIAN_POINT('Ctrl Pts',(79.19990306123,263.55551337303,30.6183190664329)) ;
#91064 = CARTESIAN_POINT('Ctrl Pts',(79.2026802545332,263.681247332211,30.6199053561371)) ;
#91065 = CARTESIAN_POINT('Ctrl Pts',(79.088180181727,263.8,30.5545045090528)) ;
#91066 = CARTESIAN_POINT('Ctrl Pts',(78.96,263.8,30.4813203435596)) ;
#91067 = CARTESIAN_POINT('Ctrl Pts',(79.2008868874385,263.554884893925,30.6492315412213)) ;
#91068 = CARTESIAN_POINT('Ctrl Pts',(79.203944249311,263.698638059625,30.6513250951561)) ;
#91069 = CARTESIAN_POINT('Ctrl Pts',(79.0777524976478,263.8,30.564932193132)) ;
#91070 = CARTESIAN_POINT('Ctrl Pts',(78.96,263.8,30.4813203435596)) ;
#91071 = CARTESIAN_POINT('Ctrl Pts',(79.1753437943954,263.554337258733,30.7036056868826)) ;
#91072 = CARTESIAN_POINT('Ctrl Pts',(79.178220382535,263.713791744552,30.7065917747161)) ;
#91073 = CARTESIAN_POINT('Ctrl Pts',(79.0594215416058,263.8,30.5832631491739)) ;
#91074 = CARTESIAN_POINT('Ctrl Pts',(78.96,263.8,30.4813203435596)) ;
#91075 = CARTESIAN_POINT('Ctrl Pts',(79.1204172721867,263.555043591858,30.7219456941975)) ;
#91076 = CARTESIAN_POINT('Ctrl Pts',(79.122387689755,263.694246708396,30.7249347311953)) ;
#91077 = CARTESIAN_POINT('Ctrl Pts',(79.0410905855638,263.8,30.6015941052159)) ;
#91078 = CARTESIAN_POINT('Ctrl Pts',(78.96,263.8,30.4813203435596)) ;
#91079 = CARTESIAN_POINT('Ctrl Pts',(79.0970093616256,263.555512320864,30.7212251114454)) ;
#91080 = CARTESIAN_POINT('Ctrl Pts',(79.0985958367215,263.681276446828,30.7240024241314)) ;
#91081 = CARTESIAN_POINT('Ctrl Pts',(79.0331873136011,263.8,30.6094973771787)) ;
#91082 = CARTESIAN_POINT('Ctrl Pts',(78.96,263.8,30.4813203435596)) ;
#91083 = CARTESIAN_POINT('',(79.2,263.56,30.6213203435596)) ;
#91084 = CARTESIAN_POINT('',(78.96,263.8,30.4813203435596)) ;
#91085 = CARTESIAN_POINT('Origin',(78.96,263.56,30.4813203435596)) ;
#91086 = CARTESIAN_POINT('',(79.1,263.56,30.7213203435596)) ;
#91087 = CARTESIAN_POINT('Origin',(78.96,263.56,30.4813203435596)) ;
#91088 = CARTESIAN_POINT('Origin',(79.1,263.56,30.6213203435596)) ;
#91089 = CARTESIAN_POINT('Origin',(80.5421241520375,263.56,30.4813203435596)) ;
#91090 = CARTESIAN_POINT('',(78.7,263.8,30.4813203435596)) ;
#91091 = CARTESIAN_POINT('',(80.5421241520375,263.8,30.4813203435596)) ;
#91092 = CARTESIAN_POINT('',(78.7,263.56,30.7213203435596)) ;
#91093 = CARTESIAN_POINT('Origin',(78.7,263.56,30.4813203435596)) ;
#91094 = CARTESIAN_POINT('',(80.5421241520375,263.56,30.7213203435596)) ;
#91095 = CARTESIAN_POINT('Origin',(78.96,263.56,30.1213203435596)) ;
#91096 = CARTESIAN_POINT('',(79.2,263.56,22.4577516938163)) ;
#91097 = CARTESIAN_POINT('',(79.2,263.56,30.1213203435596)) ;
#91098 = CARTESIAN_POINT('',(79.1755756290597,263.665485298291,22.6717108729184)) ;
#91099 = CARTESIAN_POINT('Ctrl Pts',(79.2,263.56,22.4577516938161)) ;
#91100 = CARTESIAN_POINT('Ctrl Pts',(79.2,263.560387113803,22.4580922726939)) ;
#91101 = CARTESIAN_POINT('Ctrl Pts',(79.1999990633892,263.560773655608,22.458433496925)) ;
#91102 = CARTESIAN_POINT('Ctrl Pts',(79.1998704864085,263.587384235686,22.4820045990841)) ;
#91103 = CARTESIAN_POINT('Ctrl Pts',(79.1954682388742,263.609945987182,22.5073822183424)) ;
#91104 = CARTESIAN_POINT('Ctrl Pts',(79.1861715042083,263.641598026275,22.5602671403111)) ;
#91105 = CARTESIAN_POINT('Ctrl Pts',(79.1817919077629,263.651962524966,22.5853229810386)) ;
#91106 = CARTESIAN_POINT('Ctrl Pts',(79.176825633249,263.663019660801,22.6314067110977)) ;
#91107 = CARTESIAN_POINT('Ctrl Pts',(79.1755756290598,263.665485298291,22.6515196535244)) ;
#91108 = CARTESIAN_POINT('Ctrl Pts',(79.1755756290598,263.665485298291,22.6717108732387)) ;
#91109 = CARTESIAN_POINT('',(79.1755756290598,263.665485298291,25.7213203435596)) ;
#91110 = CARTESIAN_POINT('',(79.1755756290598,263.665485298291,30.1213203435596)) ;
#91111 = CARTESIAN_POINT('',(78.96,263.8,25.7213203435596)) ;
#91112 = CARTESIAN_POINT('Origin',(78.96,263.56,25.7213203435596)) ;
#91113 = CARTESIAN_POINT('',(78.96,263.8,30.1213203435596)) ;
#91114 = CARTESIAN_POINT('Origin',(78.7,258.202943725152,30.7213203435596)) ;
#91115 = CARTESIAN_POINT('',(78.7,263.8,25.7213203435596)) ;
#91116 = CARTESIAN_POINT('',(78.7,263.8,30.7213203435596)) ;
#91117 = CARTESIAN_POINT('',(78.7,263.425,25.7213203435596)) ;
#91118 = CARTESIAN_POINT('',(78.7,263.8,25.7213203435596)) ;
#91119 = CARTESIAN_POINT('',(78.7,263.425,29.5213203435596)) ;
#91120 = CARTESIAN_POINT('',(78.7,263.425,30.1213203435596)) ;
#91121 = CARTESIAN_POINT('',(78.7,258.061522368915,29.5213203435596)) ;
#91122 = CARTESIAN_POINT('',(78.7000000000001,249.459777528085,29.5213203435596)) ;
#91123 = CARTESIAN_POINT('',(78.7,258.202943725152,29.6213203435596)) ;
#91124 = CARTESIAN_POINT('Origin',(78.7,258.061522368915,29.6213203435596)) ;
#91125 = CARTESIAN_POINT('',(78.7,258.202943725152,30.6213203435596)) ;
#91126 = CARTESIAN_POINT('',(78.7,258.202943725152,30.7213203435596)) ;
#91127 = CARTESIAN_POINT('',(78.7,258.34436508139,30.7213203435596)) ;
#91128 = CARTESIAN_POINT('Origin',(78.7,258.34436508139,30.6213203435596)) ;
#91129 = CARTESIAN_POINT('',(78.7,263.8,30.7213203435596)) ;
#91130 = CARTESIAN_POINT('Origin',(78.7,263.8,30.7213203435596)) ;
#91131 = CARTESIAN_POINT('',(77.2,263.8,25.7213203435596)) ;
#91132 = CARTESIAN_POINT('Origin',(79.95,259.751471862576,25.7213203435596)) ;
#91133 = CARTESIAN_POINT('',(79.04,263.68,25.7213203435596)) ;
#91134 = CARTESIAN_POINT('Origin',(79.1,263.6,25.7213203435596)) ;
#91135 = CARTESIAN_POINT('',(77.9683532470183,262.876264935264,25.7213203435596)) ;
#91136 = CARTESIAN_POINT('Origin',(79.1,263.6,29.5213203435596)) ;
#91137 = CARTESIAN_POINT('',(79.04,263.68,22.6717108732387)) ;
#91138 = CARTESIAN_POINT('Origin',(79.1,263.6,22.6717108732387)) ;
#91139 = CARTESIAN_POINT('',(79.04,263.68,29.5213203435596)) ;
#91140 = CARTESIAN_POINT('Origin',(66.56,251.2,19.7813203435596)) ;
#91141 = CARTESIAN_POINT('',(66.56,252.24,20.0213203435596)) ;
#91142 = CARTESIAN_POINT('',(66.56,251.2,20.0213203435596)) ;
#91143 = CARTESIAN_POINT('',(66.8,252.,19.7813203435596)) ;
#91144 = CARTESIAN_POINT('Origin',(66.56,252.24,19.7813203435596)) ;
#91145 = CARTESIAN_POINT('',(66.8,251.2,19.7813203435596)) ;
#91146 = CARTESIAN_POINT('Origin',(66.25,251.8,20.0213203435596)) ;
#91147 = CARTESIAN_POINT('',(66.2242118694392,252.575788130571,20.0213203435597)) ;
#91148 = CARTESIAN_POINT('Ctrl Pts',(65.94,253.053504693378,20.0213203435596)) ;
#91149 = CARTESIAN_POINT('Ctrl Pts',(65.9767477884387,252.96763867409,20.0213203435596)) ;
#91150 = CARTESIAN_POINT('Ctrl Pts',(66.0176818440557,252.879704923853,20.0213203435596)) ;
#91151 = CARTESIAN_POINT('Ctrl Pts',(66.1031725049829,252.727882430291,20.0213203435596)) ;
#91152 = CARTESIAN_POINT('Ctrl Pts',(66.1572502182071,252.642747715263,20.0213203435596)) ;
#91153 = CARTESIAN_POINT('Ctrl Pts',(66.2242112157523,252.575788784279,20.0213203435596)) ;
#91154 = CARTESIAN_POINT('',(66.7875,252.0125,20.0213203435596)) ;
#91155 = CARTESIAN_POINT('Ctrl Pts',(58.600000056816,251.975444989098,19.7811597661928)) ;
#91156 = CARTESIAN_POINT('Ctrl Pts',(58.5999555541213,251.975437275298,19.8440457155357)) ;
#91157 = CARTESIAN_POINT('Ctrl Pts',(58.6521580208533,251.984485702865,19.9691623227064)) ;
#91158 = CARTESIAN_POINT('Ctrl Pts',(58.777274628024,252.006172581441,20.0213647894384)) ;
#91159 = CARTESIAN_POINT('Ctrl Pts',(58.840160577367,252.01707281266,20.0213202867436)) ;
#91160 = CARTESIAN_POINT('Ctrl Pts',(58.6000000433271,252.000971418317,19.7811775148673)) ;
#91161 = CARTESIAN_POINT('Ctrl Pts',(58.5999661067172,252.000962555144,19.8371125691419)) ;
#91162 = CARTESIAN_POINT('Ctrl Pts',(58.6397724916797,252.011358835424,19.9486050783821)) ;
#91163 = CARTESIAN_POINT('Ctrl Pts',(58.7439794071885,252.03806921914,20.0112711346708)) ;
#91164 = CARTESIAN_POINT('Ctrl Pts',(58.8024064475807,252.053375145924,20.0213461160323)) ;
#91165 = CARTESIAN_POINT('Ctrl Pts',(58.6099157004014,252.052043043932,19.7812197015128)) ;
#91166 = CARTESIAN_POINT('Ctrl Pts',(58.6098983376034,252.052031828423,19.8206333831451)) ;
#91167 = CARTESIAN_POINT('Ctrl Pts',(58.630263078444,252.065186724936,19.8994186791738)) ;
#91168 = CARTESIAN_POINT('Ctrl Pts',(58.6891074359545,252.101875712154,19.9593347509465)) ;
#91169 = CARTESIAN_POINT('Ctrl Pts',(58.727245689281,252.125616817957,19.9778261025138)) ;
#91170 = CARTESIAN_POINT('Ctrl Pts',(58.6381785959941,252.095724858518,19.7812690036197)) ;
#91171 = CARTESIAN_POINT('Ctrl Pts',(58.6381689240718,252.095714970455,19.8013749227895)) ;
#91172 = CARTESIAN_POINT('Ctrl Pts',(58.6495137915443,252.107313265173,19.8414536032633)) ;
#91173 = CARTESIAN_POINT('Ctrl Pts',(58.6789249290458,252.137847807203,19.8672326888626)) ;
#91174 = CARTESIAN_POINT('Ctrl Pts',(58.6958346094131,252.155752774615,19.8735570199477)) ;
#91175 = CARTESIAN_POINT('Ctrl Pts',(58.6559044410999,252.114140580344,19.7812936795923)) ;
#91176 = CARTESIAN_POINT('Ctrl Pts',(58.6558970330687,252.114132875287,19.7917359290227)) ;
#91177 = CARTESIAN_POINT('Ctrl Pts',(58.6645867897606,252.123171048738,19.8125113086305)) ;
#91178 = CARTESIAN_POINT('Ctrl Pts',(58.6854050755849,252.144822345019,19.821142975253)) ;
#91179 = CARTESIAN_POINT('Ctrl Pts',(58.6958601680558,252.155694402978,19.8211100731203)) ;
#91180 = CARTESIAN_POINT('',(58.6958333870197,252.1556667225,19.8213203435596)) ;
#91181 = CARTESIAN_POINT('',(58.8400000000001,252.01704497925,20.0213203435596)) ;
#91182 = CARTESIAN_POINT('Origin',(58.84,252.01704497925,19.8213203435596)) ;
#91183 = CARTESIAN_POINT('',(58.6,251.97544497925,19.7813203435596)) ;
#91184 = CARTESIAN_POINT('Origin',(58.84,252.01704497925,19.7813203435596)) ;
#91185 = CARTESIAN_POINT('',(58.6558333870196,252.1140667225,19.7813203435596)) ;
#91186 = CARTESIAN_POINT('Origin',(58.8,251.97544497925,19.7813203435596)) ;
#91187 = CARTESIAN_POINT('Origin',(58.6958333870196,252.1556667225,19.7813203435596)) ;
#91188 = CARTESIAN_POINT('Origin',(58.84,248.1,19.7813203435596)) ;
#91189 = CARTESIAN_POINT('',(58.6,248.1,19.7813203435596)) ;
#91190 = CARTESIAN_POINT('',(58.84,248.1,20.0213203435596)) ;
#91191 = CARTESIAN_POINT('Origin',(58.45,251.9,24.0213203435596)) ;
#91192 = CARTESIAN_POINT('',(58.6558333870196,252.1140667225,19.6041630560343)) ;
#91193 = CARTESIAN_POINT('',(58.6558333870196,252.1140667225,24.0213203435596)) ;
#91194 = CARTESIAN_POINT('',(58.6524986843825,252.11059862929,19.5535233690183)) ;
#91195 = CARTESIAN_POINT('Origin',(58.2558333870196,251.6980667225,19.6041630560343)) ;
#91196 = CARTESIAN_POINT('',(58.9101303310336,252.378535544275,19.8213203435596)) ;
#91197 = CARTESIAN_POINT('',(57.7295973443597,251.150781238134,18.5935660374187)) ;
#91198 = CARTESIAN_POINT('',(60.2985780169101,253.822521137587,19.8213203435596)) ;
#91199 = CARTESIAN_POINT('Origin',(58.8,251.97544497925,24.0213203435596)) ;
#91200 = CARTESIAN_POINT('',(58.6,251.97544497925,19.6041630560343)) ;
#91201 = CARTESIAN_POINT('',(58.6,251.97544497925,24.0213203435596)) ;
#91202 = CARTESIAN_POINT('Origin',(58.8,251.97544497925,19.6041630560343)) ;
#91203 = CARTESIAN_POINT('Origin',(58.6000000000001,244.4,24.0213203435596)) ;
#91204 = CARTESIAN_POINT('',(58.6,252.056,23.0213203435596)) ;
#91205 = CARTESIAN_POINT('',(58.6,248.1,23.0213203435596)) ;
#91206 = CARTESIAN_POINT('',(58.6,252.056,24.0213203435596)) ;
#91207 = CARTESIAN_POINT('',(58.6,252.056,24.0213203435596)) ;
#91208 = CARTESIAN_POINT('',(58.6,245.4,24.0213203435596)) ;
#91209 = CARTESIAN_POINT('',(58.6,250.6,24.0213203435596)) ;
#91210 = CARTESIAN_POINT('',(58.6,245.4,19.6041630560343)) ;
#91211 = CARTESIAN_POINT('',(58.6,245.4,24.0213203435596)) ;
#91212 = CARTESIAN_POINT('',(58.6,245.5625,19.6041630560343)) ;
#91213 = CARTESIAN_POINT('Origin',(37.,252.100588745031,19.4613203435596)) ;
#91214 = CARTESIAN_POINT('',(37.1,252.100588745031,19.3213203435596)) ;
#91215 = CARTESIAN_POINT('Origin',(37.,252.100588745031,19.3213203435596)) ;
#91216 = CARTESIAN_POINT('',(37.,252.270294372515,19.2916147160749)) ;
#91217 = CARTESIAN_POINT('Origin',(37.,252.100588745031,19.4613203435596)) ;
#91218 = CARTESIAN_POINT('',(37.1,252.199583694397,19.3623253941935)) ;
#91219 = CARTESIAN_POINT('Origin',(37.,252.199583694397,19.3623253941935)) ;
#91220 = CARTESIAN_POINT('Origin',(37.1,252.100588745031,19.4613203435596)) ;
#91221 = CARTESIAN_POINT('Origin',(44.7285453536325,252.100588745031,19.4613203435596)) ;
#91222 = CARTESIAN_POINT('',(44.7285453536325,252.270294372515,19.2916147160749)) ;
#91223 = CARTESIAN_POINT('Origin',(37.,256.529289321881,23.6920310216783)) ;
#91224 = CARTESIAN_POINT('',(37.,252.670710678119,19.6920310216783)) ;
#91225 = CARTESIAN_POINT('',(37.,256.6,23.6213203435596)) ;
#91226 = CARTESIAN_POINT('',(37.1,252.6,19.7627416997969)) ;
#91227 = CARTESIAN_POINT('Origin',(37.,252.6,19.7627416997969)) ;
#91228 = CARTESIAN_POINT('',(37.1,256.529289321881,23.6920310216783)) ;
#91229 = CARTESIAN_POINT('Origin',(49.257090707265,252.,19.0213203435596)) ;
#91230 = CARTESIAN_POINT('',(26.4,251.21966991411,18.2409902576697)) ;
#91231 = CARTESIAN_POINT('',(52.2356360608974,251.21966991411,18.2409902576697)) ;
#91232 = CARTESIAN_POINT('',(26.4,252.853553390593,19.8748737341529)) ;
#91233 = CARTESIAN_POINT('',(26.4,253.025,20.0463203435596)) ;
#91234 = CARTESIAN_POINT('',(36.9378414229691,252.85355339061,19.8748737341699)) ;
#91235 = CARTESIAN_POINT('',(52.2356360608974,252.853553390593,19.8748737341529)) ;
#91236 = CARTESIAN_POINT('Origin',(36.7,252.670710678119,19.6920310216783)) ;
#91237 = CARTESIAN_POINT('Origin',(43.4,252.100588745031,19.4613203435596)) ;
#91238 = CARTESIAN_POINT('',(43.3,252.100588745031,19.3213203435596)) ;
#91239 = CARTESIAN_POINT('Origin',(43.4,252.100588745031,19.3213203435596)) ;
#91240 = CARTESIAN_POINT('',(43.3,252.199583694397,19.3623253941935)) ;
#91241 = CARTESIAN_POINT('Origin',(43.3,252.100588745031,19.4613203435596)) ;
#91242 = CARTESIAN_POINT('Origin',(43.4,252.199583694397,19.3623253941935)) ;
#91243 = CARTESIAN_POINT('Origin',(43.4,252.100588745031,19.4613203435596)) ;
#91244 = CARTESIAN_POINT('Origin',(44.7285453536325,252.100588745031,19.4613203435596)) ;
#91245 = CARTESIAN_POINT('Origin',(43.4,251.,19.3213203435596)) ;
#91246 = CARTESIAN_POINT('',(43.3,252.1,19.3213203435596)) ;
#91247 = CARTESIAN_POINT('Origin',(43.4,252.1,19.3213203435596)) ;
#91248 = CARTESIAN_POINT('',(43.3,251.,19.3213203435596)) ;
#91249 = CARTESIAN_POINT('Origin',(34.4,245.2,18.3213203435596)) ;
#91250 = CARTESIAN_POINT('',(34.4,245.1,18.1213203435596)) ;
#91251 = CARTESIAN_POINT('Origin',(34.4,245.1,18.3213203435596)) ;
#91252 = CARTESIAN_POINT('',(34.4,245.2,18.0213203435596)) ;
#91253 = CARTESIAN_POINT('Origin',(34.4,245.2,18.1213203435596)) ;
#91254 = CARTESIAN_POINT('Origin',(34.4,245.2,18.3213203435596)) ;
#91255 = CARTESIAN_POINT('Origin',(34.4,250.68933982822,18.7713203435596)) ;
#91256 = CARTESIAN_POINT('',(34.4,250.68933982822,18.0213203435596)) ;
#91257 = CARTESIAN_POINT('Origin',(34.4,250.68933982822,18.3213203435596)) ;
#91258 = CARTESIAN_POINT('Origin',(34.4,250.68933982822,18.7713203435596)) ;
#91259 = CARTESIAN_POINT('Origin',(34.4,251.975,18.3213203435596)) ;
#91260 = CARTESIAN_POINT('',(34.4,251.975,18.0213203435596)) ;
#91261 = CARTESIAN_POINT('Origin',(46.,245.2,18.3213203435596)) ;
#91262 = CARTESIAN_POINT('',(46.,245.2,18.0213203435596)) ;
#91263 = CARTESIAN_POINT('Origin',(46.,245.2,18.3213203435596)) ;
#91264 = CARTESIAN_POINT('',(46.,245.1,18.1213203435596)) ;
#91265 = CARTESIAN_POINT('Origin',(46.,245.2,18.1213203435596)) ;
#91266 = CARTESIAN_POINT('Origin',(46.,245.1,18.3213203435596)) ;
#91267 = CARTESIAN_POINT('Origin',(46.,246.975,18.3213203435596)) ;
#91268 = CARTESIAN_POINT('',(45.7,250.68933982822,18.3213203435596)) ;
#91269 = CARTESIAN_POINT('',(46.,250.68933982822,18.0213203435596)) ;
#91270 = CARTESIAN_POINT('Origin',(46.,250.68933982822,18.3213203435596)) ;
#91271 = CARTESIAN_POINT('',(46.,246.975,18.0213203435596)) ;
#91272 = CARTESIAN_POINT('',(45.7,246.975,18.3213203435596)) ;
#91273 = CARTESIAN_POINT('Origin',(46.,250.68933982822,18.7713203435596)) ;
#91274 = CARTESIAN_POINT('',(45.7,251.007537879754,18.4531222920257)) ;
#91275 = CARTESIAN_POINT('Origin',(46.,251.007537879754,18.4531222920257)) ;
#91276 = CARTESIAN_POINT('Origin',(46.,250.68933982822,18.7713203435596)) ;
#91277 = CARTESIAN_POINT('Origin',(45.7,250.68933982822,18.7713203435596)) ;
#91278 = CARTESIAN_POINT('Origin',(46.,249.762867965644,17.2084523779156)) ;
#91279 = CARTESIAN_POINT('',(45.7,249.762867965644,17.2084523779156)) ;
#91280 = CARTESIAN_POINT('Origin',(55.3573593128808,245.1,29.5213203435596)) ;
#91281 = CARTESIAN_POINT('',(55.3573593128808,245.1,18.1213203435596)) ;
#91282 = CARTESIAN_POINT('',(55.2857703637053,245.1,18.1213203435596)) ;
#91283 = CARTESIAN_POINT('',(55.3573593128808,245.1,30.7213203435596)) ;
#91284 = CARTESIAN_POINT('',(55.3573593128808,245.1,29.5213203435596)) ;
#91285 = CARTESIAN_POINT('',(46.8,245.1,30.7213203435596)) ;
#91286 = CARTESIAN_POINT('',(55.3573593128808,245.1,30.7213203435596)) ;
#91287 = CARTESIAN_POINT('',(46.8,245.1,20.0213203435596)) ;
#91288 = CARTESIAN_POINT('',(46.8,245.1,29.5213203435596)) ;
#91289 = CARTESIAN_POINT('',(41.7,245.1,20.0213203435596)) ;
#91290 = CARTESIAN_POINT('',(55.3573593128808,245.1,20.0213203435596)) ;
#91291 = CARTESIAN_POINT('',(41.7,245.1,24.3713203435596)) ;
#91292 = CARTESIAN_POINT('Origin',(55.2857703637053,245.2,18.1213203435596)) ;
#91293 = CARTESIAN_POINT('',(55.3573593128808,245.2,18.0213203435596)) ;
#91294 = CARTESIAN_POINT('',(55.2857703637053,245.2,18.0213203435596)) ;
#91295 = CARTESIAN_POINT('Origin',(55.3573593128808,245.2,18.1213203435596)) ;
#91296 = CARTESIAN_POINT('Origin',(55.2141814145299,249.05,18.0213203435596)) ;
#91297 = CARTESIAN_POINT('',(57.0469450846408,250.68933982822,18.0213203435596)) ;
#91298 = CARTESIAN_POINT('',(52.2356360608974,250.68933982822,18.0213203435596)) ;
#91299 = CARTESIAN_POINT('',(57.0171572875254,250.6,18.0213203435596)) ;
#91300 = CARTESIAN_POINT('Origin',(57.36141013588,250.588334274672,18.0213203435596)) ;
#91301 = CARTESIAN_POINT('',(57.0171572875254,244.208722493294,18.0213203435596)) ;
#91302 = CARTESIAN_POINT('',(57.0171572875254,247.8875,18.0213203435596)) ;
#91303 = CARTESIAN_POINT('',(56.1573593128807,244.208722493294,18.0213203435596)) ;
#91304 = CARTESIAN_POINT('',(64.0732152677426,244.208722493294,18.0213203435596)) ;
#91305 = CARTESIAN_POINT('',(56.1573593128807,244.4,18.0213203435596)) ;
#91306 = CARTESIAN_POINT('',(56.1573593128808,237.655597577758,18.0213203435596)) ;
#91307 = CARTESIAN_POINT('Origin',(55.3573593128808,244.4,18.0213203435596)) ;
#91308 = CARTESIAN_POINT('Origin',(52.2356360608974,250.68933982822,18.7713203435596)) ;
#91309 = CARTESIAN_POINT('',(57.1201778296089,250.775348215898,18.0261270789701)) ;
#91310 = CARTESIAN_POINT('Ctrl Pts',(57.1201105354923,250.775384372087,18.0260789875623)) ;
#91311 = CARTESIAN_POINT('Ctrl Pts',(57.1531938341603,250.850775222355,18.0345331819805)) ;
#91312 = CARTESIAN_POINT('Ctrl Pts',(57.2453556003495,251.012930443534,18.0800899809205)) ;
#91313 = CARTESIAN_POINT('Ctrl Pts',(57.3390787831373,251.150386903953,18.1717072475128)) ;
#91314 = CARTESIAN_POINT('Ctrl Pts',(57.3882337581722,251.21966991411,18.2409902576698)) ;
#91315 = CARTESIAN_POINT('Ctrl Pts',(57.046945084641,250.68933982822,18.0213203435596)) ;
#91316 = CARTESIAN_POINT('Ctrl Pts',(57.0658007810727,250.725754870646,18.0213203435596)) ;
#91317 = CARTESIAN_POINT('Ctrl Pts',(57.0917499983331,250.753564280112,18.0236645927849)) ;
#91318 = CARTESIAN_POINT('Ctrl Pts',(57.1202270585269,250.775323946388,18.0262024909521)) ;
#91319 = CARTESIAN_POINT('Origin',(81.1,238.503733341287,30.6213203435596)) ;
#91320 = CARTESIAN_POINT('',(81.1,238.603733341287,30.6213203435596)) ;
#91321 = CARTESIAN_POINT('',(81.2,238.503733341287,30.6213203435596)) ;
#91322 = CARTESIAN_POINT('Origin',(81.1,238.503733341287,30.6213203435596)) ;
#91323 = CARTESIAN_POINT('',(81.1,238.503733341287,30.7213203435596)) ;
#91324 = CARTESIAN_POINT('Origin',(81.1,238.503733341287,30.6213203435596)) ;
#91325 = CARTESIAN_POINT('Origin',(81.1,238.503733341287,30.6213203435596)) ;
#91326 = CARTESIAN_POINT('Origin',(77.925,238.503733341287,30.6213203435596)) ;
#91327 = CARTESIAN_POINT('',(80.,238.603733341287,30.6213203435596)) ;
#91328 = CARTESIAN_POINT('',(80.1,238.503733341287,30.7213203435596)) ;
#91329 = CARTESIAN_POINT('Origin',(80.1,238.503733341287,30.6213203435596)) ;
#91330 = CARTESIAN_POINT('',(77.925,238.503733341287,30.7213203435596)) ;
#91331 = CARTESIAN_POINT('',(77.925,238.603733341287,30.6213203435596)) ;
#91332 = CARTESIAN_POINT('Origin',(74.9999999999998,220.305309236676,30.6213203435596)) ;
#91333 = CARTESIAN_POINT('',(72.3072410949819,223.397080489445,30.7213203435596)) ;
#91334 = CARTESIAN_POINT('',(72.4472638847366,223.384844644141,30.6213203435596)) ;
#91335 = CARTESIAN_POINT('Ctrl Pts',(72.3072410949819,223.397080489445,30.7213203435596)) ;
#91336 = CARTESIAN_POINT('Ctrl Pts',(72.3101340243119,223.393675929465,30.7213203435596)) ;
#91337 = CARTESIAN_POINT('Ctrl Pts',(72.3132391000724,223.390484046919,30.7210210006498)) ;
#91338 = CARTESIAN_POINT('Ctrl Pts',(72.3212552465528,223.38326583681,30.7195830340118)) ;
#91339 = CARTESIAN_POINT('Ctrl Pts',(72.3262847482039,223.379552566922,30.7181499124324)) ;
#91340 = CARTESIAN_POINT('Ctrl Pts',(72.3418384928136,223.37010049032,30.7123855270563)) ;
#91341 = CARTESIAN_POINT('Ctrl Pts',(72.3526461080447,223.366083274383,30.7067053729914)) ;
#91342 = CARTESIAN_POINT('Ctrl Pts',(72.3744712399842,223.361576323922,30.6928428900762)) ;
#91343 = CARTESIAN_POINT('Ctrl Pts',(72.3854649216459,223.361319212967,30.6845254783462)) ;
#91344 = CARTESIAN_POINT('Ctrl Pts',(72.4056828300951,223.363823007051,30.6672585994799)) ;
#91345 = CARTESIAN_POINT('Ctrl Pts',(72.4150882865401,223.366503475073,30.6582230647311)) ;
#91346 = CARTESIAN_POINT('Ctrl Pts',(72.4320205436683,223.373954425398,30.6402375869053)) ;
#91347 = CARTESIAN_POINT('Ctrl Pts',(72.4396999602672,223.378679872843,30.631199149209)) ;
#91348 = CARTESIAN_POINT('Ctrl Pts',(72.446817075448,223.384475902764,30.6219068564245)) ;
#91349 = CARTESIAN_POINT('Ctrl Pts',(72.4470408822559,223.384659789476,30.6216135992287)) ;
#91350 = CARTESIAN_POINT('Ctrl Pts',(72.4472638847366,223.384844644141,30.6213203435596)) ;
#91351 = CARTESIAN_POINT('',(75.,224.305309236676,30.6213203435596)) ;
#91352 = CARTESIAN_POINT('Origin',(74.9999999999998,220.305309236676,30.6213203435596)) ;
#91353 = CARTESIAN_POINT('',(75.,224.405309236676,30.7213203435596)) ;
#91354 = CARTESIAN_POINT('Origin',(75.,224.405309236676,30.6213203435596)) ;
#91355 = CARTESIAN_POINT('Origin',(74.9999999999998,220.305309236676,30.7213203435596)) ;
#91356 = CARTESIAN_POINT('Origin',(77.9249999999999,224.405309236676,30.6213203435596)) ;
#91357 = CARTESIAN_POINT('',(79.3510004003203,224.305309236676,30.6213203435596)) ;
#91358 = CARTESIAN_POINT('',(79.3510004003203,224.405309236676,30.7213203435596)) ;
#91359 = CARTESIAN_POINT('Origin',(79.3510004003203,224.405309236676,30.6213203435596)) ;
#91360 = CARTESIAN_POINT('',(77.9249999999999,224.405309236676,30.7213203435596)) ;
#91361 = CARTESIAN_POINT('',(77.9249999999999,224.305309236676,30.6213203435596)) ;
#91362 = CARTESIAN_POINT('Origin',(79.3510004003203,225.305309236676,30.6213203435596)) ;
#91363 = CARTESIAN_POINT('',(80.1316251501201,224.680309236676,30.6213203435596)) ;
#91364 = CARTESIAN_POINT('',(80.0535626751402,224.742809236676,30.7213203435596)) ;
#91365 = CARTESIAN_POINT('Origin',(80.0535626751402,224.742809236676,30.6213203435596)) ;
#91366 = CARTESIAN_POINT('Origin',(79.3510004003203,225.305309236676,30.7213203435596)) ;
#91367 = CARTESIAN_POINT('Origin',(79.3510004003203,225.305309236676,30.6213203435596)) ;
#91368 = CARTESIAN_POINT('Origin',(80.6000000000002,224.305309236676,30.6213203435596)) ;
#91369 = CARTESIAN_POINT('',(80.1757359312881,224.729573305388,30.6213203435596)) ;
#91370 = CARTESIAN_POINT('',(80.1050252531694,224.800283983507,30.7213203435596)) ;
#91371 = CARTESIAN_POINT('Origin',(80.1050252531694,224.800283983507,30.6213203435596)) ;
#91372 = CARTESIAN_POINT('Origin',(80.6000000000002,224.305309236676,30.7213203435596)) ;
#91373 = CARTESIAN_POINT('Origin',(80.6000000000002,224.305309236676,30.6213203435596)) ;
#91374 = CARTESIAN_POINT('Origin',(80.2950815131274,224.990340243465,30.6213203435596)) ;
#91375 = CARTESIAN_POINT('',(81.024264068712,225.578101442812,30.6213203435596)) ;
#91376 = CARTESIAN_POINT('',(80.9535533905933,225.648812120931,30.7213203435596)) ;
#91377 = CARTESIAN_POINT('Origin',(80.9535533905933,225.648812120931,30.6213203435596)) ;
#91378 = CARTESIAN_POINT('',(80.2950815131274,224.990340243465,30.7213203435596)) ;
#91379 = CARTESIAN_POINT('',(80.3657921912461,224.919629565346,30.6213203435596)) ;
#91380 = CARTESIAN_POINT('Origin',(80.5999999999999,226.002365511524,30.6213203435596)) ;
#91381 = CARTESIAN_POINT('',(81.2,226.002365511524,30.6213203435596)) ;
#91382 = CARTESIAN_POINT('',(81.1,226.002365511524,30.7213203435596)) ;
#91383 = CARTESIAN_POINT('Origin',(81.1,226.002365511524,30.6213203435596)) ;
#91384 = CARTESIAN_POINT('Origin',(80.5999999999999,226.002365511524,30.7213203435596)) ;
#91385 = CARTESIAN_POINT('Origin',(80.5999999999999,226.002365511524,30.6213203435596)) ;
#91386 = CARTESIAN_POINT('Origin',(81.1,233.361105671474,30.6213203435596)) ;
#91387 = CARTESIAN_POINT('',(81.1,233.361105671474,30.7213203435596)) ;
#91388 = CARTESIAN_POINT('',(81.2,233.361105671474,30.6213203435596)) ;
#91389 = CARTESIAN_POINT('Origin',(81.1,238.503733341287,30.1213203435596)) ;
#91390 = CARTESIAN_POINT('',(81.2,238.503733341287,29.6213203435596)) ;
#91391 = CARTESIAN_POINT('',(81.1,238.603733341287,29.6213203435596)) ;
#91392 = CARTESIAN_POINT('Origin',(81.1,238.503733341287,29.6213203435596)) ;
#91393 = CARTESIAN_POINT('',(81.1,238.603733341287,30.1213203435596)) ;
#91394 = CARTESIAN_POINT('',(81.2,238.503733341287,30.1213203435596)) ;
#91395 = CARTESIAN_POINT('Origin',(81.3,238.503733341287,29.6213203435596)) ;
#91396 = CARTESIAN_POINT('',(81.3,238.503733341287,29.5213203435596)) ;
#91397 = CARTESIAN_POINT('',(81.1267949192431,238.603733341287,29.5213203435596)) ;
#91398 = CARTESIAN_POINT('Ctrl Pts',(81.1267949192431,238.603733341287,29.5213203435596)) ;
#91399 = CARTESIAN_POINT('Ctrl Pts',(81.1522826614307,238.603733341287,29.5213203435596)) ;
#91400 = CARTESIAN_POINT('Ctrl Pts',(81.1815269526849,238.594776141297,29.5213203435596)) ;
#91401 = CARTESIAN_POINT('Ctrl Pts',(81.2384776727796,238.564124612906,29.5213203435596)) ;
#91402 = CARTESIAN_POINT('Ctrl Pts',(81.2722901777919,238.531443163495,29.5213203435596)) ;
#91403 = CARTESIAN_POINT('Ctrl Pts',(81.3,238.503733341287,29.5213203435596)) ;
#91404 = CARTESIAN_POINT('Origin',(81.3,238.603733341287,29.6213203435596)) ;
#91405 = CARTESIAN_POINT('Origin',(81.3,238.503733341287,29.6213203435596)) ;
#91406 = CARTESIAN_POINT('Origin',(75.8499999999999,228.11847800166,30.7213203435596)) ;
#91407 = CARTESIAN_POINT('',(80.1,230.5,30.7213203435596)) ;
#91408 = CARTESIAN_POINT('',(80.1,229.30923900083,30.7213203435596)) ;
#91409 = CARTESIAN_POINT('',(80.2,230.4,30.7213203435596)) ;
#91410 = CARTESIAN_POINT('Origin',(80.1,230.4,30.7213203435596)) ;
#91411 = CARTESIAN_POINT('',(80.1999999999999,225.6,30.7213203435596)) ;
#91412 = CARTESIAN_POINT('',(80.1999999999999,225.6,30.7213203435596)) ;
#91413 = CARTESIAN_POINT('',(80.0999999999999,225.5,30.7213203435596)) ;
#91414 = CARTESIAN_POINT('Origin',(80.0999999999999,225.6,30.7213203435596)) ;
#91415 = CARTESIAN_POINT('',(80.,225.5,30.7213203435596)) ;
#91416 = CARTESIAN_POINT('',(76.0414213562372,225.5,30.7213203435596)) ;
#91417 = CARTESIAN_POINT('',(80.,224.805309236676,30.7213203435596)) ;
#91418 = CARTESIAN_POINT('',(80.,224.305309236676,30.7213203435596)) ;
#91419 = CARTESIAN_POINT('',(75.,224.805309236676,30.7213203435596)) ;
#91420 = CARTESIAN_POINT('',(80.,224.805309236676,30.7213203435596)) ;
#91421 = CARTESIAN_POINT('',(72.4201780792821,223.992383802967,30.7213203435596)) ;
#91422 = CARTESIAN_POINT('Origin',(74.9999999999998,220.305309236676,30.7213203435596)) ;
#91423 = CARTESIAN_POINT('',(72.2848151277479,223.47832706609,30.7213203435596)) ;
#91424 = CARTESIAN_POINT('Origin',(75.1450953968556,223.000000000001,30.7213203435596)) ;
#91425 = CARTESIAN_POINT('Origin',(72.383445481855,223.461833029328,30.7213203435596)) ;
#91426 = CARTESIAN_POINT('Origin',(80.1,229.30923900083,30.6213203435596)) ;
#91427 = CARTESIAN_POINT('',(80.,230.5,30.6213203435596)) ;
#91428 = CARTESIAN_POINT('',(80.,229.30923900083,30.6213203435596)) ;
#91429 = CARTESIAN_POINT('Origin',(80.1,230.5,30.6213203435596)) ;
#91430 = CARTESIAN_POINT('Origin',(80.,238.603733341287,30.7213203435596)) ;
#91431 = CARTESIAN_POINT('',(80.,238.603733341287,29.5213203435596)) ;
#91432 = CARTESIAN_POINT('',(67.607090707265,238.603733341287,29.5213203435596)) ;
#91433 = CARTESIAN_POINT('',(80.,238.603733341287,30.7213203435596)) ;
#91434 = CARTESIAN_POINT('Origin',(82.8283628290597,247.448254073888,30.7213203435596)) ;
#91435 = CARTESIAN_POINT('',(82.7745180379261,247.36398819427,29.5213203435596)) ;
#91436 = CARTESIAN_POINT('',(82.8283628290597,247.348254073888,29.5213203435596)) ;
#91437 = CARTESIAN_POINT('Origin',(82.8283628290597,247.448254073888,29.5213203435596)) ;
#91438 = CARTESIAN_POINT('',(82.7745180379261,247.36398819427,30.6213203435596)) ;
#91439 = CARTESIAN_POINT('',(82.7745180379261,247.36398819427,30.7213203435596)) ;
#91440 = CARTESIAN_POINT('',(82.9283628290597,247.448254073888,30.6213203435596)) ;
#91441 = CARTESIAN_POINT('Origin',(82.8283628290597,247.448254073888,30.6213203435596)) ;
#91442 = CARTESIAN_POINT('',(82.9283628290597,247.448254073888,29.6213203435596)) ;
#91443 = CARTESIAN_POINT('',(82.9283628290597,247.448254073888,30.7213203435596)) ;
#91444 = CARTESIAN_POINT('Origin',(82.8283628290597,247.448254073888,29.6213203435596)) ;
#91445 = CARTESIAN_POINT('Ctrl Pts',(82.9283628290597,247.448254073888,30.6213203435596)) ;
#91446 = CARTESIAN_POINT('Ctrl Pts',(82.9283628290597,247.448254073888,30.6340619475287)) ;
#91447 = CARTESIAN_POINT('Ctrl Pts',(82.9341320322739,247.440923371758,30.6638411974399)) ;
#91448 = CARTESIAN_POINT('Ctrl Pts',(82.9684492173715,247.395367745016,30.7096337860914)) ;
#91449 = CARTESIAN_POINT('Ctrl Pts',(83.0061199473635,247.33660142623,30.7213203435596)) ;
#91450 = CARTESIAN_POINT('Ctrl Pts',(83.0283628290597,247.297155956632,30.7213203435596)) ;
#91451 = CARTESIAN_POINT('Ctrl Pts',(82.9283628290597,247.427878926694,30.6213203435596)) ;
#91452 = CARTESIAN_POINT('Ctrl Pts',(82.9283628290597,247.427878926694,30.632388067116)) ;
#91453 = CARTESIAN_POINT('Ctrl Pts',(82.9325259207497,247.421320764645,30.658190436137)) ;
#91454 = CARTESIAN_POINT('Ctrl Pts',(82.9597089455937,247.379792518138,30.7026967149053)) ;
#91455 = CARTESIAN_POINT('Ctrl Pts',(82.9956823265646,247.323984315082,30.7191008858943)) ;
#91456 = CARTESIAN_POINT('Ctrl Pts',(83.0184376715155,247.285962574613,30.7213203435596)) ;
#91457 = CARTESIAN_POINT('Ctrl Pts',(82.917054183129,247.392349854163,30.6213203435596)) ;
#91458 = CARTESIAN_POINT('Ctrl Pts',(82.917054183129,247.392349854163,30.6309476358367)) ;
#91459 = CARTESIAN_POINT('Ctrl Pts',(82.9193460938706,247.387147989111,30.6532689555926)) ;
#91460 = CARTESIAN_POINT('Ctrl Pts',(82.9395093507166,247.352576015412,30.6992100994537)) ;
#91461 = CARTESIAN_POINT('Ctrl Pts',(82.9760987671946,247.301944703507,30.7224004125047)) ;
#91462 = CARTESIAN_POINT('Ctrl Pts',(83.0010881693302,247.266396174287,30.7273204280171)) ;
#91463 = CARTESIAN_POINT('Ctrl Pts',(82.8741969828184,247.353879677779,30.6213203435596)) ;
#91464 = CARTESIAN_POINT('Ctrl Pts',(82.8741969828184,247.353879677779,30.6332771649992)) ;
#91465 = CARTESIAN_POINT('Ctrl Pts',(82.8770528905548,247.349680555954,30.6610000049115)) ;
#91466 = CARTESIAN_POINT('Ctrl Pts',(82.9023865039853,247.320424668727,30.7178542537679)) ;
#91467 = CARTESIAN_POINT('Ctrl Pts',(82.9478254184405,247.274206387667,30.7458171439626)) ;
#91468 = CARTESIAN_POINT('Ctrl Pts',(82.9784944719197,247.240915481893,30.7514576611934)) ;
#91469 = CARTESIAN_POINT('Ctrl Pts',(82.8219342251982,247.343491305129,30.6213203435596)) ;
#91470 = CARTESIAN_POINT('Ctrl Pts',(82.8219342251982,247.343491305129,30.6390908352506)) ;
#91471 = CARTESIAN_POINT('Ctrl Pts',(82.8281131661804,247.338693418412,30.6804793222557)) ;
#91472 = CARTESIAN_POINT('Ctrl Pts',(82.8704286563925,247.306698271771,30.7533053642045)) ;
#91473 = CARTESIAN_POINT('Ctrl Pts',(82.9283403572097,247.2592292449,30.7803880252827)) ;
#91474 = CARTESIAN_POINT('Ctrl Pts',(82.9649558842051,247.225646950021,30.7839087790904)) ;
#91475 = CARTESIAN_POINT('Ctrl Pts',(82.7873950106811,247.355759977683,30.6213203435596)) ;
#91476 = CARTESIAN_POINT('Ctrl Pts',(82.7873950106811,247.355759977683,30.6445020491678)) ;
#91477 = CARTESIAN_POINT('Ctrl Pts',(82.7968362794067,247.349589080481,30.6986342225162)) ;
#91478 = CARTESIAN_POINT('Ctrl Pts',(82.8547312920342,247.310456538834,30.784599297317)) ;
#91479 = CARTESIAN_POINT('Ctrl Pts',(82.9217111420117,247.258080750493,30.8090524868466)) ;
#91480 = CARTESIAN_POINT('Ctrl Pts',(82.9620180379262,247.222333709343,30.8101003697968)) ;
#91481 = CARTESIAN_POINT('Ctrl Pts',(82.7745180379261,247.36398819427,30.6213203435596)) ;
#91482 = CARTESIAN_POINT('Ctrl Pts',(82.7745180379261,247.36398819427,30.6468035514977)) ;
#91483 = CARTESIAN_POINT('Ctrl Pts',(82.7853352939526,247.357115661024,30.7063620513201)) ;
#91484 = CARTESIAN_POINT('Ctrl Pts',(82.8496800160108,247.314407260952,30.7979472286232)) ;
#91485 = CARTESIAN_POINT('Ctrl Pts',(82.9203126347458,247.259313837091,30.8213203435596)) ;
#91486 = CARTESIAN_POINT('Ctrl Pts',(82.9620180379262,247.222333709343,30.8213203435596)) ;
#91487 = CARTESIAN_POINT('',(82.7995688863616,247.347612311413,30.7213203451448)) ;
#91488 = CARTESIAN_POINT('',(83.0283628290571,247.297155956642,30.7213203435596)) ;
#91489 = CARTESIAN_POINT('Ctrl Pts',(82.7995655199487,247.347607264512,30.7213203435596)) ;
#91490 = CARTESIAN_POINT('Ctrl Pts',(82.8184849722079,247.334987503492,30.7213203435596)) ;
#91491 = CARTESIAN_POINT('Ctrl Pts',(82.8384029440696,247.32796189855,30.7213203435596)) ;
#91492 = CARTESIAN_POINT('Ctrl Pts',(82.86726782439,247.319640667715,30.7213203435596)) ;
#91493 = CARTESIAN_POINT('Ctrl Pts',(82.8841494442442,247.316356042277,30.7213203435596)) ;
#91494 = CARTESIAN_POINT('Ctrl Pts',(82.9198493149481,247.310901562837,30.7213203435596)) ;
#91495 = CARTESIAN_POINT('Ctrl Pts',(82.9383255275291,247.308684133357,30.7213203435596)) ;
#91496 = CARTESIAN_POINT('Ctrl Pts',(82.9901924598214,247.302694056846,30.7213203435596)) ;
#91497 = CARTESIAN_POINT('Ctrl Pts',(83.0091658974097,247.300554835715,30.7213203435596)) ;
#91498 = CARTESIAN_POINT('Ctrl Pts',(83.0278683017175,247.297244157736,30.7213203435596)) ;
#91499 = CARTESIAN_POINT('Ctrl Pts',(83.0281155851111,247.297200164889,30.7213203435596)) ;
#91500 = CARTESIAN_POINT('Ctrl Pts',(83.0283628290554,247.297155956633,30.7213203435596)) ;
#91501 = CARTESIAN_POINT('Ctrl Pts',(83.0283628290597,247.297155956632,30.7213203435596)) ;
#91502 = CARTESIAN_POINT('Ctrl Pts',(83.0061199473635,247.33660142623,30.7213203435596)) ;
#91503 = CARTESIAN_POINT('Ctrl Pts',(82.9684492173715,247.395367745016,30.7096337860914)) ;
#91504 = CARTESIAN_POINT('Ctrl Pts',(82.9341320322739,247.440923371758,30.6638411974399)) ;
#91505 = CARTESIAN_POINT('Ctrl Pts',(82.9283628290597,247.448254073888,30.6340619475287)) ;
#91506 = CARTESIAN_POINT('Ctrl Pts',(82.9283628290597,247.448254073888,30.6213203435596)) ;
#91507 = CARTESIAN_POINT('Ctrl Pts',(82.7745180379261,247.36398819427,30.6213203435596)) ;
#91508 = CARTESIAN_POINT('Ctrl Pts',(82.7745180379261,247.36398819427,30.6468035514977)) ;
#91509 = CARTESIAN_POINT('Ctrl Pts',(82.7809835635818,247.359880448284,30.6824019516531)) ;
#91510 = CARTESIAN_POINT('Ctrl Pts',(82.7950782219932,247.350599112262,30.7130824661876)) ;
#91511 = CARTESIAN_POINT('Ctrl Pts',(82.799565516924,247.34760726653,30.7213203483033)) ;
#91512 = CARTESIAN_POINT('Origin',(81.9668461709225,246.100000000001,30.7213203435596)) ;
#91513 = CARTESIAN_POINT('',(81.9668461709226,247.600000000001,29.5213203435596)) ;
#91514 = CARTESIAN_POINT('Origin',(81.9668461709225,246.100000000001,29.5213203435596)) ;
#91515 = CARTESIAN_POINT('',(81.9668461709226,247.600000000001,30.7213203435596)) ;
#91516 = CARTESIAN_POINT('',(81.9668461709226,247.600000000001,30.7213203435596)) ;
#91517 = CARTESIAN_POINT('Origin',(81.9668461709225,246.100000000001,30.7213203435596)) ;
#91518 = CARTESIAN_POINT('Origin',(81.3,239.660172336152,29.6213203435596)) ;
#91519 = CARTESIAN_POINT('',(81.2,238.239818409494,29.6213203435596)) ;
#91520 = CARTESIAN_POINT('',(81.2,239.660172336152,29.6213203435596)) ;
#91521 = CARTESIAN_POINT('',(81.3,238.239818409494,29.5213203435596)) ;
#91522 = CARTESIAN_POINT('Origin',(81.3,238.239818409494,29.6213203435596)) ;
#91523 = CARTESIAN_POINT('',(81.3,239.660172336152,29.5213203435596)) ;
#91524 = CARTESIAN_POINT('Ctrl Pts',(81.3,238.239818409494,29.5213203435596)) ;
#91525 = CARTESIAN_POINT('Ctrl Pts',(81.2480070174032,238.055306843022,29.5213203435596)) ;
#91526 = CARTESIAN_POINT('Ctrl Pts',(81.2000505692918,237.833945077818,29.4688545911561)) ;
#91527 = CARTESIAN_POINT('Ctrl Pts',(81.2000038038563,237.610204859837,29.4219256048081)) ;
#91528 = CARTESIAN_POINT('Ctrl Pts',(81.2,237.608784212583,29.4216218542709)) ;
#91529 = CARTESIAN_POINT('Ctrl Pts',(81.2,237.60736287746,29.4213203435596)) ;
#91530 = CARTESIAN_POINT('Ctrl Pts',(81.2700800699658,238.239818409494,29.5213203435596)) ;
#91531 = CARTESIAN_POINT('Ctrl Pts',(81.2280389979125,238.055423609356,29.5373521064363)) ;
#91532 = CARTESIAN_POINT('Ctrl Pts',(81.2001824531038,237.828764886114,29.4782935568788)) ;
#91533 = CARTESIAN_POINT('Ctrl Pts',(81.2000016826941,237.610154623831,29.4220391644932)) ;
#91534 = CARTESIAN_POINT('Ctrl Pts',(81.2,237.608757139533,29.4216792848826)) ;
#91535 = CARTESIAN_POINT('Ctrl Pts',(81.2,237.60736287746,29.4213203435596)) ;
#91536 = CARTESIAN_POINT('Ctrl Pts',(81.2183034919586,238.239818409494,29.5464528346232)) ;
#91537 = CARTESIAN_POINT('Ctrl Pts',(81.2056400608213,238.046097430234,29.5711733353535)) ;
#91538 = CARTESIAN_POINT('Ctrl Pts',(81.2001038970389,237.820640503915,29.494000356449)) ;
#91539 = CARTESIAN_POINT('Ctrl Pts',(81.2000001080443,237.610062474299,29.4222415191829)) ;
#91540 = CARTESIAN_POINT('Ctrl Pts',(81.2,237.608709761695,29.4217797884529)) ;
#91541 = CARTESIAN_POINT('Ctrl Pts',(81.2,237.60736287746,29.4213203435596)) ;
#91542 = CARTESIAN_POINT('Ctrl Pts',(81.2,238.239818409494,29.598880396034)) ;
#91543 = CARTESIAN_POINT('Ctrl Pts',(81.2001340670536,238.026951998836,29.606243609608)) ;
#91544 = CARTESIAN_POINT('Ctrl Pts',(81.2000050990089,237.81354631324,29.5096696755031)) ;
#91545 = CARTESIAN_POINT('Ctrl Pts',(81.1999999804742,237.60996567801,29.4224440728427)) ;
#91546 = CARTESIAN_POINT('Ctrl Pts',(81.2,237.608662383858,29.4218802920233)) ;
#91547 = CARTESIAN_POINT('Ctrl Pts',(81.2,237.60736287746,29.4213203435596)) ;
#91548 = CARTESIAN_POINT('Ctrl Pts',(81.2,238.239818409494,29.6213203435596)) ;
#91549 = CARTESIAN_POINT('Ctrl Pts',(81.2,238.018769899166,29.6213203435596)) ;
#91550 = CARTESIAN_POINT('Ctrl Pts',(81.2000000000001,237.810503044327,29.5163888387536)) ;
#91551 = CARTESIAN_POINT('Ctrl Pts',(81.2,237.609924206993,29.4225308660566)) ;
#91552 = CARTESIAN_POINT('Ctrl Pts',(81.2,237.60864207907,29.4219233649821)) ;
#91553 = CARTESIAN_POINT('Ctrl Pts',(81.2,237.60736287746,29.4213203435596)) ;
#91554 = CARTESIAN_POINT('',(81.2,237.60736287746,29.4213203435596)) ;
#91555 = CARTESIAN_POINT('Ctrl Pts',(81.2,238.239818409494,29.6213203435596)) ;
#91556 = CARTESIAN_POINT('Ctrl Pts',(81.2,238.018769899166,29.6213203435596)) ;
#91557 = CARTESIAN_POINT('Ctrl Pts',(81.2000000000001,237.810503044327,29.5163888387536)) ;
#91558 = CARTESIAN_POINT('Ctrl Pts',(81.2,237.609924206993,29.4225308660566)) ;
#91559 = CARTESIAN_POINT('Ctrl Pts',(81.2,237.60864207907,29.4219233649821)) ;
#91560 = CARTESIAN_POINT('Ctrl Pts',(81.2,237.60736287746,29.4213203435596)) ;
#91561 = CARTESIAN_POINT('',(81.2011028227143,237.670362548256,29.4346494309995)) ;
#91562 = CARTESIAN_POINT('Ctrl Pts',(81.2,237.60736287746,29.4213203435596)) ;
#91563 = CARTESIAN_POINT('Ctrl Pts',(81.2,237.608784212583,29.4216218542709)) ;
#91564 = CARTESIAN_POINT('Ctrl Pts',(81.2000038038563,237.610204859837,29.4219256048081)) ;
#91565 = CARTESIAN_POINT('Ctrl Pts',(81.2000081966347,237.631221262085,29.426333745924)) ;
#91566 = CARTESIAN_POINT('Ctrl Pts',(81.2003844493976,237.650807905606,29.4304888824184)) ;
#91567 = CARTESIAN_POINT('Ctrl Pts',(81.2011028227143,237.670362548256,29.4346494309995)) ;
#91568 = CARTESIAN_POINT('Ctrl Pts',(81.2011028227143,237.670362548256,29.4346494309995)) ;
#91569 = CARTESIAN_POINT('Ctrl Pts',(81.2085352436464,237.872678436069,29.4776952229906)) ;
#91570 = CARTESIAN_POINT('Ctrl Pts',(81.2525894384794,238.07156883933,29.5213203435596)) ;
#91571 = CARTESIAN_POINT('Ctrl Pts',(81.3,238.239818409494,29.5213203435596)) ;
#91572 = CARTESIAN_POINT('Origin',(81.2,238.603733341287,29.5213203435596)) ;
#91573 = CARTESIAN_POINT('',(81.2,226.002365511524,16.1213203435596)) ;
#91574 = CARTESIAN_POINT('',(81.2,226.002365511524,29.5213203435596)) ;
#91575 = CARTESIAN_POINT('',(81.2,237.60736287746,16.1213203435596)) ;
#91576 = CARTESIAN_POINT('',(81.2,234.318247777236,16.1213203435596)) ;
#91577 = CARTESIAN_POINT('',(81.2,237.60736287746,29.5213203435596)) ;
#91578 = CARTESIAN_POINT('Origin',(56.1573593128808,244.208722493294,17.9213203435596)) ;
#91579 = CARTESIAN_POINT('',(56.0573593128807,244.077258377225,18.0720425588636)) ;
#91580 = CARTESIAN_POINT('',(56.0573593128807,244.208722493294,18.1213203435596)) ;
#91581 = CARTESIAN_POINT('Origin',(56.0573593128807,244.208722493294,17.9213203435596)) ;
#91582 = CARTESIAN_POINT('Origin',(56.1573593128807,244.208722493294,18.1213203435596)) ;
#91583 = CARTESIAN_POINT('',(56.1573593128808,244.142990435259,17.9966814512116)) ;
#91584 = CARTESIAN_POINT('Origin',(56.1573593128808,244.208722493294,17.9213203435596)) ;
#91585 = CARTESIAN_POINT('Origin',(56.1573593128808,244.077258377225,18.0720425588636)) ;
#91586 = CARTESIAN_POINT('Origin',(56.1573593128808,237.655597577758,18.1213203435596)) ;
#91587 = CARTESIAN_POINT('',(56.0573593128808,244.4,18.1213203435596)) ;
#91588 = CARTESIAN_POINT('Origin',(56.1573593128807,244.4,18.1213203435596)) ;
#91589 = CARTESIAN_POINT('',(56.0573593128807,237.655597577758,18.1213203435596)) ;
#91590 = CARTESIAN_POINT('Origin',(55.3573593128808,244.4,18.1213203435596)) ;
#91591 = CARTESIAN_POINT('Origin',(55.3573593128808,244.4,18.1213203435596)) ;
#91592 = CARTESIAN_POINT('Origin',(64.0732152677426,244.208722493294,17.9213203435596)) ;
#91593 = CARTESIAN_POINT('',(57.0171572875254,244.142990435259,17.9966814512116)) ;
#91594 = CARTESIAN_POINT('Origin',(57.0171572875254,244.208722493294,17.9213203435596)) ;
#91595 = CARTESIAN_POINT('',(64.0732152677426,244.142990435259,17.9966814512116)) ;
#91596 = CARTESIAN_POINT('Ctrl Pts',(57.1585786437627,244.295771714953,18.0798989873223)) ;
#91597 = CARTESIAN_POINT('Ctrl Pts',(57.1243722498753,244.251856993134,18.0456925934349)) ;
#91598 = CARTESIAN_POINT('Ctrl Pts',(57.073701669366,244.208722493294,18.0213203435596)) ;
#91599 = CARTESIAN_POINT('Ctrl Pts',(57.0171572875254,244.208722493294,18.0213203435596)) ;
#91600 = CARTESIAN_POINT('Ctrl Pts',(57.1662010408867,244.277959825846,18.0875213844463)) ;
#91601 = CARTESIAN_POINT('Ctrl Pts',(57.1322204912758,244.236496138881,18.0497812422628)) ;
#91602 = CARTESIAN_POINT('Ctrl Pts',(57.0781267479544,244.195060440298,18.0213203435596)) ;
#91603 = CARTESIAN_POINT('Ctrl Pts',(57.0171572875254,244.195060440298,18.0213203435596)) ;
#91604 = CARTESIAN_POINT('Ctrl Pts',(57.1878308364965,244.246870893186,18.0924999052801)) ;
#91605 = CARTESIAN_POINT('Ctrl Pts',(57.149399367403,244.209591803697,18.0494141685073)) ;
#91606 = CARTESIAN_POINT('Ctrl Pts',(57.087283042415,244.171163525055,18.0163461021938)) ;
#91607 = CARTESIAN_POINT('Ctrl Pts',(57.0171572875254,244.171163525055,18.0163461021938)) ;
#91608 = CARTESIAN_POINT('Ctrl Pts',(57.2168557429681,244.225940828197,18.0813885694826)) ;
#91609 = CARTESIAN_POINT('Ctrl Pts',(57.1694028080032,244.188418029924,18.0363775851873)) ;
#91610 = CARTESIAN_POINT('Ctrl Pts',(57.0975672104142,244.150712341108,18.0034167126644)) ;
#91611 = CARTESIAN_POINT('Ctrl Pts',(57.0171572875254,244.150712341108,18.0034167126644)) ;
#91612 = CARTESIAN_POINT('Ctrl Pts',(57.2292893218813,244.219798572017,18.0742120091328)) ;
#91613 = CARTESIAN_POINT('Ctrl Pts',(57.1779797310502,244.18105028806,18.0289388407524)) ;
#91614 = CARTESIAN_POINT('Ctrl Pts',(57.1019738602863,244.142990435259,17.9966814512116)) ;
#91615 = CARTESIAN_POINT('Ctrl Pts',(57.0171572875254,244.142990435259,17.9966814512116)) ;
#91616 = CARTESIAN_POINT('',(57.1585786437627,244.295771714953,18.0798989873223)) ;
#91617 = CARTESIAN_POINT('Ctrl Pts',(57.0171572875254,244.208722493294,18.0213203435596)) ;
#91618 = CARTESIAN_POINT('Ctrl Pts',(57.073701669366,244.208722493294,18.0213203435596)) ;
#91619 = CARTESIAN_POINT('Ctrl Pts',(57.1243722498753,244.251856993134,18.0456925934349)) ;
#91620 = CARTESIAN_POINT('Ctrl Pts',(57.1585786437627,244.295771714953,18.0798989873223)) ;
#91621 = CARTESIAN_POINT('',(57.2292893218813,244.219798572017,18.0742120091328)) ;
#91622 = CARTESIAN_POINT('Origin',(57.2292893218813,244.295771714953,18.0091883092036)) ;
#91623 = CARTESIAN_POINT('Ctrl Pts',(57.2292893218813,244.219798572017,18.0742120091328)) ;
#91624 = CARTESIAN_POINT('Ctrl Pts',(57.1779797310502,244.18105028806,18.0289388407524)) ;
#91625 = CARTESIAN_POINT('Ctrl Pts',(57.1019738602863,244.142990435259,17.9966814512116)) ;
#91626 = CARTESIAN_POINT('Ctrl Pts',(57.0171572875254,244.142990435259,17.9966814512116)) ;
#91627 = CARTESIAN_POINT('Ctrl Pts',(57.2287065774412,244.219244545601,18.0735653510966)) ;
#91628 = CARTESIAN_POINT('Ctrl Pts',(57.3814006657422,244.334807512776,18.2082665041401)) ;
#91629 = CARTESIAN_POINT('Ctrl Pts',(57.5818168023902,244.400164102786,18.3850706639092)) ;
#91630 = CARTESIAN_POINT('Ctrl Pts',(57.7829936944083,244.399999844,18.5625564161474)) ;
#91631 = CARTESIAN_POINT('Ctrl Pts',(57.2121022546918,244.227431353028,18.083148048922)) ;
#91632 = CARTESIAN_POINT('Ctrl Pts',(57.3638432729406,244.342814703471,18.2222979585249)) ;
#91633 = CARTESIAN_POINT('Ctrl Pts',(57.5629211478754,244.405277865753,18.4040655266567)) ;
#91634 = CARTESIAN_POINT('Ctrl Pts',(57.7617874567952,244.399924414825,18.5837622386288)) ;
#91635 = CARTESIAN_POINT('Ctrl Pts',(57.1831337441925,244.250669122844,18.0921857128824)) ;
#91636 = CARTESIAN_POINT('Ctrl Pts',(57.3332794540229,244.370076607913,18.239051143939)) ;
#91637 = CARTESIAN_POINT('Ctrl Pts',(57.5299105485602,244.433213916469,18.431067418715)) ;
#91638 = CARTESIAN_POINT('Ctrl Pts',(57.7250965298064,244.425041966314,18.6204797878858)) ;
#91639 = CARTESIAN_POINT('Ctrl Pts',(57.1636274644359,244.281850951555,18.0849477536176)) ;
#91640 = CARTESIAN_POINT('Ctrl Pts',(57.3150551881256,244.409361005203,18.2363879364689)) ;
#91641 = CARTESIAN_POINT('Ctrl Pts',(57.5136740096313,244.480134652266,18.4349332023547)) ;
#91642 = CARTESIAN_POINT('Ctrl Pts',(57.7121552325777,244.477549127776,18.6334758460784)) ;
#91643 = CARTESIAN_POINT('Ctrl Pts',(57.1579051025174,244.295194612823,18.079225446077)) ;
#91644 = CARTESIAN_POINT('Ctrl Pts',(57.3105939795694,244.426164890483,18.231914323129)) ;
#91645 = CARTESIAN_POINT('Ctrl Pts',(57.5110027976195,244.500217797822,18.4323231411791)) ;
#91646 = CARTESIAN_POINT('Ctrl Pts',(57.712167056771,244.499999518812,18.6334874003306)) ;
#91647 = CARTESIAN_POINT('',(57.7112800931608,244.5,18.6326004367204)) ;
#91648 = CARTESIAN_POINT('',(57.7819907712794,244.4,18.5618897586017)) ;
#91649 = CARTESIAN_POINT('Origin',(57.7819907712794,244.5,18.5618897586017)) ;
#91650 = CARTESIAN_POINT('Origin',(57.7819907712794,243.65,18.5618897586017)) ;
#91651 = CARTESIAN_POINT('Origin',(57.7112800931608,243.65,18.6326004367204)) ;
#91652 = CARTESIAN_POINT('Origin',(59.6957106781187,244.5,20.475609665441)) ;
#91653 = CARTESIAN_POINT('',(59.4877499598282,244.5,20.4090703033878)) ;
#91654 = CARTESIAN_POINT('',(59.5584606379469,244.4,20.3383596252692)) ;
#91655 = CARTESIAN_POINT('Origin',(59.5584606379469,244.5,20.3383596252692)) ;
#91656 = CARTESIAN_POINT('',(59.6957106781187,244.4,20.475609665441)) ;
#91657 = CARTESIAN_POINT('',(59.625,244.5,20.5463203435596)) ;
#91658 = CARTESIAN_POINT('Ctrl Pts',(59.5584671942072,244.400000068279,20.338175912058)) ;
#91659 = CARTESIAN_POINT('Ctrl Pts',(59.5733152046798,244.399998916975,20.3678850518884)) ;
#91660 = CARTESIAN_POINT('Ctrl Pts',(59.6079639373555,244.392166720739,20.4372262890232)) ;
#91661 = CARTESIAN_POINT('Ctrl Pts',(59.6346249869036,244.367754219918,20.4905963915537)) ;
#91662 = CARTESIAN_POINT('Ctrl Pts',(59.6446565645846,244.350697787771,20.510678433286)) ;
#91663 = CARTESIAN_POINT('Ctrl Pts',(59.537282725906,244.399957438475,20.3593605952471)) ;
#91664 = CARTESIAN_POINT('Ctrl Pts',(59.5535226580609,244.403204576356,20.3876218149334)) ;
#91665 = CARTESIAN_POINT('Ctrl Pts',(59.5939825862619,244.401172393675,20.4544573327192)) ;
#91666 = CARTESIAN_POINT('Ctrl Pts',(59.6277898217881,244.376233246362,20.5066189259004)) ;
#91667 = CARTESIAN_POINT('Ctrl Pts',(59.6406435698939,244.357497856102,20.5262463389736)) ;
#91668 = CARTESIAN_POINT('Ctrl Pts',(59.5006111373498,244.425081428672,20.396017115008)) ;
#91669 = CARTESIAN_POINT('Ctrl Pts',(59.5229458164964,244.430091479793,20.4219725732252)) ;
#91670 = CARTESIAN_POINT('Ctrl Pts',(59.5781914473742,244.428908376005,20.4846291462517)) ;
#91671 = CARTESIAN_POINT('Ctrl Pts',(59.6235364564538,244.397463327035,20.5345903902754)) ;
#91672 = CARTESIAN_POINT('Ctrl Pts',(59.6406929112882,244.373534147426,20.5534465526952)) ;
#91673 = CARTESIAN_POINT('Ctrl Pts',(59.4876383932168,244.477554105521,20.4089588892195)) ;
#91674 = CARTESIAN_POINT('Ctrl Pts',(59.51569834688,244.479058256544,20.4369804578922)) ;
#91675 = CARTESIAN_POINT('Ctrl Pts',(59.5819260984814,244.46774807284,20.5031955440028)) ;
#91676 = CARTESIAN_POINT('Ctrl Pts',(59.6335489997903,244.424139894224,20.5548732787412)) ;
#91677 = CARTESIAN_POINT('Ctrl Pts',(59.6530089235801,244.39307153877,20.5743292554704)) ;
#91678 = CARTESIAN_POINT('Ctrl Pts',(59.4876318556191,244.499999964608,20.4089521991787)) ;
#91679 = CARTESIAN_POINT('Ctrl Pts',(59.517336511604,244.500017767817,20.4386568551635)) ;
#91680 = CARTESIAN_POINT('Ctrl Pts',(59.5866699888097,244.484389267076,20.5079903323693)) ;
#91681 = CARTESIAN_POINT('Ctrl Pts',(59.6400363483859,244.435560982935,20.5613566919455)) ;
#91682 = CARTESIAN_POINT('Ctrl Pts',(59.6601169821608,244.4014377108,20.5814373257204)) ;
#91683 = CARTESIAN_POINT('',(59.5361382460763,244.470551010537,20.453396295288)) ;
#91684 = CARTESIAN_POINT('',(59.6446141839292,244.350769740148,20.5106667172338)) ;
#91685 = CARTESIAN_POINT('Ctrl Pts',(59.5361418751229,244.470548356227,20.4533975244613)) ;
#91686 = CARTESIAN_POINT('Ctrl Pts',(59.5556542115485,244.456276801076,20.4696116159651)) ;
#91687 = CARTESIAN_POINT('Ctrl Pts',(59.5754367551715,244.439013252497,20.48414635836)) ;
#91688 = CARTESIAN_POINT('Ctrl Pts',(59.6043064288728,244.407760596003,20.500592829049)) ;
#91689 = CARTESIAN_POINT('Ctrl Pts',(59.6145514147285,244.395323576303,20.5053596763027)) ;
#91690 = CARTESIAN_POINT('Ctrl Pts',(59.6312403814749,244.372254380133,20.5102712030638)) ;
#91691 = CARTESIAN_POINT('Ctrl Pts',(59.6380964847321,244.361802761066,20.5112975698589)) ;
#91692 = CARTESIAN_POINT('Ctrl Pts',(59.6444658667391,244.351021269097,20.5106817644182)) ;
#91693 = CARTESIAN_POINT('Ctrl Pts',(59.6445400561483,244.350895531046,20.5106743560996)) ;
#91694 = CARTESIAN_POINT('Ctrl Pts',(59.6446141839293,244.350769740148,20.5106667172364)) ;
#91695 = CARTESIAN_POINT('Origin',(59.5584606379469,244.3,20.3383596252692)) ;
#91696 = CARTESIAN_POINT('',(59.5008788001387,244.499567297188,20.4221991441223)) ;
#91697 = CARTESIAN_POINT('Origin',(59.4877499598282,244.3,20.4090703033878)) ;
#91698 = CARTESIAN_POINT('Ctrl Pts',(59.5008803400812,244.499565874957,20.4222006849129)) ;
#91699 = CARTESIAN_POINT('Ctrl Pts',(59.506343646892,244.494520221898,20.427660931309)) ;
#91700 = CARTESIAN_POINT('Ctrl Pts',(59.5120512929965,244.489533320353,20.4328815347287)) ;
#91701 = CARTESIAN_POINT('Ctrl Pts',(59.5238687470823,244.47979868564,20.4431905436275)) ;
#91702 = CARTESIAN_POINT('Ctrl Pts',(59.5299380750016,244.47508550957,20.4482422082633)) ;
#91703 = CARTESIAN_POINT('Ctrl Pts',(59.5361389131708,244.47055052273,20.4533950632053)) ;
#91704 = CARTESIAN_POINT('Origin',(64.4831104165663,219.797752737776,16.1213203435596)) ;
#91705 = CARTESIAN_POINT('',(63.3432752896628,216.068037482763,16.1213203435596)) ;
#91706 = CARTESIAN_POINT('Origin',(63.3615337515762,216.16706261919,16.1213376927199)) ;
#91707 = CARTESIAN_POINT('',(61.2884174438392,217.560804636007,16.1213203435596)) ;
#91708 = CARTESIAN_POINT('Origin',(64.4831104165663,219.797752737776,16.1213203435596)) ;
#91709 = CARTESIAN_POINT('Origin',(61.3703326482681,217.618162279643,16.1213203435596)) ;
#91710 = CARTESIAN_POINT('Origin',(59.3765805603019,220.465535350009,16.1213203435596)) ;
#91711 = CARTESIAN_POINT('',(56.7626663401537,224.024247053747,16.1213203435596)) ;
#91712 = CARTESIAN_POINT('Origin',(56.8445815445825,224.081604697382,16.1213203435596)) ;
#91713 = CARTESIAN_POINT('',(59.294665355873,220.408177706374,16.1213203435596)) ;
#91714 = CARTESIAN_POINT('Origin',(59.9573593128806,226.261195155516,16.1213203435596)) ;
#91715 = CARTESIAN_POINT('',(56.0573593128808,226.261195155516,16.1213203435596)) ;
#91716 = CARTESIAN_POINT('Origin',(56.1573593128808,226.261195155516,16.1213203435596)) ;
#91717 = CARTESIAN_POINT('Origin',(59.9573593128806,226.261195155516,16.1213203435596)) ;
#91718 = CARTESIAN_POINT('Origin',(56.1573593128808,228.14697868435,16.1213203435596)) ;
#91719 = CARTESIAN_POINT('',(56.0573593128807,238.278291754874,16.1213203435596)) ;
#91720 = CARTESIAN_POINT('Origin',(56.1573593128808,238.278291754874,16.1213203435596)) ;
#91721 = CARTESIAN_POINT('',(56.0573593128808,228.14697868435,16.1213203435596)) ;
#91722 = CARTESIAN_POINT('Origin',(56.1573593128808,238.278291754874,16.7713203435596)) ;
#91723 = CARTESIAN_POINT('',(56.0573593128807,238.483839802785,16.1546761998268)) ;
#91724 = CARTESIAN_POINT('',(56.1573593128808,238.515462579386,16.0598078700217)) ;
#91725 = CARTESIAN_POINT('Origin',(56.1573593128808,238.483839802785,16.1546761998268)) ;
#91726 = CARTESIAN_POINT('Origin',(56.1573593128808,238.278291754874,16.7713203435596)) ;
#91727 = CARTESIAN_POINT('Origin',(56.0573593128807,238.278291754874,16.7713203435596)) ;
#91728 = CARTESIAN_POINT('Origin',(56.1573593128808,236.430915043381,15.4703679466921)) ;
#91729 = CARTESIAN_POINT('',(56.0573593128807,243.855548047911,17.9452456148689)) ;
#91730 = CARTESIAN_POINT('',(56.1573593128807,243.887170824513,17.8503772850638)) ;
#91731 = CARTESIAN_POINT('Origin',(56.1573593128807,243.855548047911,17.9452456148689)) ;
#91732 = CARTESIAN_POINT('',(56.1573593128808,236.462537819982,15.375499616887)) ;
#91733 = CARTESIAN_POINT('',(56.0573593128807,236.430915043381,15.4703679466921)) ;
#91734 = CARTESIAN_POINT('Origin',(56.1573593128808,243.65,18.5618897586017)) ;
#91735 = CARTESIAN_POINT('Origin',(56.1573593128808,243.65,18.5618897586017)) ;
#91736 = CARTESIAN_POINT('Origin',(56.0573593128807,243.65,18.5618897586017)) ;
#91737 = CARTESIAN_POINT('Origin',(55.3573593128808,244.4,29.5213203435596)) ;
#91738 = CARTESIAN_POINT('',(56.0573593128808,244.4,30.7213203435596)) ;
#91739 = CARTESIAN_POINT('',(56.0573593128808,244.4,29.5213203435596)) ;
#91740 = CARTESIAN_POINT('Origin',(55.3573593128808,244.4,30.7213203435596)) ;
#91741 = CARTESIAN_POINT('Origin',(56.0573593128808,226.261195155516,29.5213203435596)) ;
#91742 = CARTESIAN_POINT('',(56.0573593128808,226.261195155516,30.7213203435596)) ;
#91743 = CARTESIAN_POINT('',(56.0573593128808,226.261195155516,29.5213203435596)) ;
#91744 = CARTESIAN_POINT('',(56.0573593128808,226.261195155516,30.7213203435596)) ;
#91745 = CARTESIAN_POINT('Origin',(59.9573593128806,226.261195155516,29.5213203435596)) ;
#91746 = CARTESIAN_POINT('',(56.7626663401537,224.024247053747,30.7213203435596)) ;
#91747 = CARTESIAN_POINT('',(56.7626663401537,224.024247053747,29.5213203435596)) ;
#91748 = CARTESIAN_POINT('Origin',(59.9573593128806,226.261195155516,30.7213203435596)) ;
#91749 = CARTESIAN_POINT('Origin',(60.2642432409823,219.023476982374,29.5213203435596)) ;
#91750 = CARTESIAN_POINT('',(61.2884174438392,217.560804636007,23.2713203435596)) ;
#91751 = CARTESIAN_POINT('',(61.2884174438392,217.560804636007,25.0213203435596)) ;
#91752 = CARTESIAN_POINT('',(60.2642432409823,219.023476982374,23.2713203435596)) ;
#91753 = CARTESIAN_POINT('',(60.8660775466133,218.163968518398,23.2713203435596)) ;
#91754 = CARTESIAN_POINT('',(60.2642432409823,219.023476982374,30.7213203435596)) ;
#91755 = CARTESIAN_POINT('',(60.2642432409823,219.023476982374,29.5213203435596)) ;
#91756 = CARTESIAN_POINT('',(61.2884174438392,217.560804636007,30.7213203435596)) ;
#91757 = CARTESIAN_POINT('Origin',(64.4831104165663,219.797752737776,25.0213203435596)) ;
#91758 = CARTESIAN_POINT('',(63.3432752896628,216.068037482763,23.2713203435596)) ;
#91759 = CARTESIAN_POINT('',(63.3432752896628,216.068037482763,25.0213203435596)) ;
#91760 = CARTESIAN_POINT('Origin',(64.4831104165663,219.797752737776,23.2713203435596)) ;
#91761 = CARTESIAN_POINT('Origin',(69.2808968287545,215.776927458569,16.1213203435596)) ;
#91762 = CARTESIAN_POINT('',(69.4013544815242,215.668771587158,16.1213203435596)) ;
#91763 = CARTESIAN_POINT('Origin',(69.4079308494226,215.768555109772,16.1213203435596)) ;
#91764 = CARTESIAN_POINT('',(69.2743204608562,215.677143935955,16.1213203435596)) ;
#91765 = CARTESIAN_POINT('Ctrl Pts',(68.4157280311031,244.326083322956,17.9953582499056)) ;
#91766 = CARTESIAN_POINT('Ctrl Pts',(68.415503099048,244.326287996807,17.9954135499195)) ;
#91767 = CARTESIAN_POINT('Ctrl Pts',(68.4152781349504,244.326493093575,17.9954686676332)) ;
#91768 = CARTESIAN_POINT('Ctrl Pts',(68.3480453599995,244.387545954585,18.0121657700759)) ;
#91769 = CARTESIAN_POINT('Ctrl Pts',(68.2868811696763,244.449692607864,18.0339989374688)) ;
#91770 = CARTESIAN_POINT('Ctrl Pts',(68.2414978867463,244.482287915021,18.0798261741698)) ;
#91771 = CARTESIAN_POINT('Ctrl Pts',(68.4157280311031,244.326083322956,17.9953582499056)) ;
#91772 = CARTESIAN_POINT('Ctrl Pts',(68.4154763603613,244.326233226319,17.9953987516991)) ;
#91773 = CARTESIAN_POINT('Ctrl Pts',(68.4152333288418,244.326412830281,17.9954758377209)) ;
#91774 = CARTESIAN_POINT('Ctrl Pts',(68.3408356732327,244.374438578966,18.0076269476457)) ;
#91775 = CARTESIAN_POINT('Ctrl Pts',(68.2707325615201,244.423538275651,18.0415477041581)) ;
#91776 = CARTESIAN_POINT('Ctrl Pts',(68.2323584534764,244.441748530438,18.089128043464)) ;
#91777 = CARTESIAN_POINT('Ctrl Pts',(68.4157280311031,244.326083322956,17.9953582499056)) ;
#91778 = CARTESIAN_POINT('Ctrl Pts',(68.4154538754065,244.326202355367,17.9953904107993)) ;
#91779 = CARTESIAN_POINT('Ctrl Pts',(68.415184345804,244.326316512137,17.9954511971732)) ;
#91780 = CARTESIAN_POINT('Ctrl Pts',(68.3337700599932,244.3621377726,18.004245689451)) ;
#91781 = CARTESIAN_POINT('Ctrl Pts',(68.2537549741851,244.397420595634,18.0357515724808)) ;
#91782 = CARTESIAN_POINT('Ctrl Pts',(68.2020344914338,244.402854022253,18.0767019419474)) ;
#91783 = CARTESIAN_POINT('Ctrl Pts',(68.4157280311031,244.326083322956,17.9953582499056)) ;
#91784 = CARTESIAN_POINT('Ctrl Pts',(68.4154317761631,244.326160630694,17.9953791373758)) ;
#91785 = CARTESIAN_POINT('Ctrl Pts',(68.4151352241728,244.326238449581,17.9954000300808)) ;
#91786 = CARTESIAN_POINT('Ctrl Pts',(68.3266140510332,244.349168426876,18.0017543602468)) ;
#91787 = CARTESIAN_POINT('Ctrl Pts',(68.237732147878,244.375710462253,18.0166982540741)) ;
#91788 = CARTESIAN_POINT('Ctrl Pts',(68.1704101577868,244.39111820199,18.0506955811225)) ;
#91789 = CARTESIAN_POINT('',(68.1715529942029,244.390856053509,18.050121315269)) ;
#91790 = CARTESIAN_POINT('',(68.2422637392367,244.481712398084,18.0790566043223)) ;
#91791 = CARTESIAN_POINT('Origin',(68.1715529942029,244.481712107019,18.0083459931195)) ;
#91792 = CARTESIAN_POINT('',(68.4134930867977,244.32811526913,17.9959101696537)) ;
#91793 = CARTESIAN_POINT('Ctrl Pts',(68.2422671027082,244.481712396327,18.0790532408515)) ;
#91794 = CARTESIAN_POINT('Ctrl Pts',(68.2493325411649,244.476606556519,18.0719882407775)) ;
#91795 = CARTESIAN_POINT('Ctrl Pts',(68.2568413561123,244.470680650291,18.0655175608582)) ;
#91796 = CARTESIAN_POINT('Ctrl Pts',(68.2646955001455,244.464145311328,18.0595601342585)) ;
#91797 = CARTESIAN_POINT('Ctrl Pts',(68.2727769201473,244.45742085876,18.0534303171481)) ;
#91798 = CARTESIAN_POINT('Ctrl Pts',(68.2812243384575,244.450051298074,18.0478431272093)) ;
#91799 = CARTESIAN_POINT('Ctrl Pts',(68.2899663542551,244.442222844725,18.0427061835484)) ;
#91800 = CARTESIAN_POINT('Ctrl Pts',(68.2991681976564,244.433982616904,18.0372990380773)) ;
#91801 = CARTESIAN_POINT('Ctrl Pts',(68.3086969039584,244.425234059554,18.0323900053085)) ;
#91802 = CARTESIAN_POINT('Ctrl Pts',(68.3185014235944,244.416145218704,18.0278789496962)) ;
#91803 = CARTESIAN_POINT('Ctrl Pts',(68.3285924324566,244.406790800846,18.0232360805041)) ;
#91804 = CARTESIAN_POINT('Ctrl Pts',(68.3389763842491,244.397075734544,18.0190142970919)) ;
#91805 = CARTESIAN_POINT('Ctrl Pts',(68.3496210593381,244.387133438654,18.0151221223351)) ;
#91806 = CARTESIAN_POINT('Ctrl Pts',(68.3608979552043,244.376600638499,18.0109987790617)) ;
#91807 = CARTESIAN_POINT('Ctrl Pts',(68.3724684244289,244.365812753876,18.0072451144521)) ;
#91808 = CARTESIAN_POINT('Ctrl Pts',(68.3843064678103,244.354874916172,18.0037781849552)) ;
#91809 = CARTESIAN_POINT('Ctrl Pts',(68.3938654112985,244.346042867739,18.0009787203757)) ;
#91810 = CARTESIAN_POINT('Ctrl Pts',(68.403599256299,244.337111839492,17.9983668597683)) ;
#91811 = CARTESIAN_POINT('Ctrl Pts',(68.4134930867977,244.32811526913,17.9959101696537)) ;
#91812 = CARTESIAN_POINT('',(68.4157280311053,244.326083322956,17.9953582499056)) ;
#91813 = CARTESIAN_POINT('Ctrl Pts',(68.4134930867977,244.32811526913,17.9959101696537)) ;
#91814 = CARTESIAN_POINT('Ctrl Pts',(68.4140127841,244.32764270258,17.995781126082)) ;
#91815 = CARTESIAN_POINT('Ctrl Pts',(68.414532921807,244.327169951285,17.995652512562)) ;
#91816 = CARTESIAN_POINT('Ctrl Pts',(68.4150534973794,244.326697018831,17.9955243250024)) ;
#91817 = CARTESIAN_POINT('Ctrl Pts',(68.4152781128779,244.326492960161,17.9954690152373)) ;
#91818 = CARTESIAN_POINT('Ctrl Pts',(68.4155030853425,244.326287968735,17.9954135423348)) ;
#91819 = CARTESIAN_POINT('Ctrl Pts',(68.415728031103,244.326083322956,17.9953582499058)) ;
#91820 = CARTESIAN_POINT('',(68.4126406994004,244.326885339084,17.9955808747352)) ;
#91821 = CARTESIAN_POINT('Ctrl Pts',(68.4157280311031,244.326083322956,17.9953582499056)) ;
#91822 = CARTESIAN_POINT('Ctrl Pts',(68.4154317761631,244.326160630694,17.9953791373758)) ;
#91823 = CARTESIAN_POINT('Ctrl Pts',(68.4151352241728,244.326238449581,17.9954000300808)) ;
#91824 = CARTESIAN_POINT('Ctrl Pts',(68.4141066106842,244.326504895258,17.9954738672148)) ;
#91825 = CARTESIAN_POINT('Ctrl Pts',(68.4133736713245,244.326694994148,17.9955270708784)) ;
#91826 = CARTESIAN_POINT('Ctrl Pts',(68.4126406994004,244.326885339084,17.9955808747352)) ;
#91827 = CARTESIAN_POINT('Ctrl Pts',(68.4126406994004,244.326885339084,17.9955808747352)) ;
#91828 = CARTESIAN_POINT('Ctrl Pts',(68.3256372266032,244.349479206531,18.0019673709072)) ;
#91829 = CARTESIAN_POINT('Ctrl Pts',(68.2381749361321,244.375539775844,18.0168103443043)) ;
#91830 = CARTESIAN_POINT('Ctrl Pts',(68.1715529942029,244.390856053509,18.050121315269)) ;
#91831 = CARTESIAN_POINT('Ctrl Pts',(68.2422636723215,244.481712107019,18.0790566712382)) ;
#91832 = CARTESIAN_POINT('Ctrl Pts',(68.216159455498,244.493714742233,18.1051608880617)) ;
#91833 = CARTESIAN_POINT('Ctrl Pts',(68.1874444287551,244.5,18.1338759148046)) ;
#91834 = CARTESIAN_POINT('Ctrl Pts',(68.1587130280226,244.5,18.1626073155371)) ;
#91835 = CARTESIAN_POINT('Ctrl Pts',(68.2369709753343,244.458690211032,18.0843493682253)) ;
#91836 = CARTESIAN_POINT('Ctrl Pts',(68.2123052970946,244.468092133554,18.1090740358395)) ;
#91837 = CARTESIAN_POINT('Ctrl Pts',(68.1852296346586,244.472056879549,18.1359779514075)) ;
#91838 = CARTESIAN_POINT('Ctrl Pts',(68.1587130280226,244.470080069966,18.1626073155371)) ;
#91839 = CARTESIAN_POINT('Ctrl Pts',(68.2163693612034,244.418594990287,18.0821834080608)) ;
#91840 = CARTESIAN_POINT('Ctrl Pts',(68.1923316647305,244.423578999196,18.1025989413263)) ;
#91841 = CARTESIAN_POINT('Ctrl Pts',(68.1662580373605,244.423426860681,18.1244213984655)) ;
#91842 = CARTESIAN_POINT('Ctrl Pts',(68.1409417831407,244.418303305343,18.1448360706551)) ;
#91843 = CARTESIAN_POINT('Ctrl Pts',(68.1849909585482,244.395956487844,18.0612141162575)) ;
#91844 = CARTESIAN_POINT('Ctrl Pts',(68.1595025691414,244.400924816049,18.0762392209731)) ;
#91845 = CARTESIAN_POINT('Ctrl Pts',(68.131583958965,244.402300999176,18.0923928210252)) ;
#91846 = CARTESIAN_POINT('Ctrl Pts',(68.1038697889688,244.4,18.1077640764833)) ;
#91847 = CARTESIAN_POINT('Ctrl Pts',(68.1715529942029,244.390856053509,18.050121315269)) ;
#91848 = CARTESIAN_POINT('Ctrl Pts',(68.1454487773793,244.396857371116,18.0631734236807)) ;
#91849 = CARTESIAN_POINT('Ctrl Pts',(68.1167337506364,244.4,18.0775309370522)) ;
#91850 = CARTESIAN_POINT('Ctrl Pts',(68.088002349904,244.4,18.0918966374184)) ;
#91851 = CARTESIAN_POINT('',(68.088002349904,244.4,18.0918966374184)) ;
#91852 = CARTESIAN_POINT('',(68.1587130280226,244.5,18.1626073155371)) ;
#91853 = CARTESIAN_POINT('Origin',(68.088002349904,244.5,18.0918966374184)) ;
#91854 = CARTESIAN_POINT('Origin',(68.1587130280226,244.3,18.1626073155371)) ;
#91855 = CARTESIAN_POINT('Origin',(68.088002349904,244.3,18.0918966374184)) ;
#91856 = CARTESIAN_POINT('Origin',(65.9792893218814,244.5,20.200609665441)) ;
#91857 = CARTESIAN_POINT('',(66.1,244.4,20.0798989873224)) ;
#91858 = CARTESIAN_POINT('',(66.1707106781187,244.5,20.150609665441)) ;
#91859 = CARTESIAN_POINT('Origin',(66.1,244.5,20.0798989873224)) ;
#91860 = CARTESIAN_POINT('',(66.05,244.5,20.2713203435597)) ;
#91861 = CARTESIAN_POINT('',(65.9792893218814,244.4,20.200609665441)) ;
#91862 = CARTESIAN_POINT('Ctrl Pts',(66.1708868324018,244.499999967942,20.1504335111579)) ;
#91863 = CARTESIAN_POINT('Ctrl Pts',(66.0635188884297,244.500039048421,20.25780145513)) ;
#91864 = CARTESIAN_POINT('Ctrl Pts',(65.9564406808178,244.46434631255,20.3648796627419)) ;
#91865 = CARTESIAN_POINT('Ctrl Pts',(65.8705697739276,244.399894281784,20.4507505696321)) ;
#91866 = CARTESIAN_POINT('Ctrl Pts',(66.170881676644,244.470075190665,20.1504389438007)) ;
#91867 = CARTESIAN_POINT('Ctrl Pts',(66.0666566269504,244.473068265832,20.2544950124528)) ;
#91868 = CARTESIAN_POINT('Ctrl Pts',(65.9619739267268,244.441148453657,20.3594054251304)) ;
#91869 = CARTESIAN_POINT('Ctrl Pts',(65.8777198541297,244.380841276891,20.4436003927159)) ;
#91870 = CARTESIAN_POINT('Ctrl Pts',(66.1530889222118,244.418272466591,20.1326643833074)) ;
#91871 = CARTESIAN_POINT('Ctrl Pts',(66.0581593621532,244.42596869334,20.2349249147586)) ;
#91872 = CARTESIAN_POINT('Ctrl Pts',(65.9603621384066,244.400754686742,20.3386298810903)) ;
#91873 = CARTESIAN_POINT('Ctrl Pts',(65.8812382246392,244.347587615883,20.4221602225383)) ;
#91874 = CARTESIAN_POINT('Ctrl Pts',(66.1159846943527,244.399981442444,20.0955666391745)) ;
#91875 = CARTESIAN_POINT('Ctrl Pts',(66.0285944646232,244.403450570881,20.2014160256478)) ;
#91876 = CARTESIAN_POINT('Ctrl Pts',(65.9397032095956,244.377094235374,20.3074787984105)) ;
#91877 = CARTESIAN_POINT('Ctrl Pts',(65.8679593077692,244.325965696746,20.3926529481467)) ;
#91878 = CARTESIAN_POINT('Ctrl Pts',(66.1001017858144,244.400000004182,20.0796836953459)) ;
#91879 = CARTESIAN_POINT('Ctrl Pts',(66.0142111292878,244.400022779608,20.1870553905182)) ;
#91880 = CARTESIAN_POINT('Ctrl Pts',(65.9285565399426,244.371463165213,20.2941361064605)) ;
#91881 = CARTESIAN_POINT('Ctrl Pts',(65.8598673418409,244.319900473437,20.3800087345052)) ;
#91882 = CARTESIAN_POINT('',(65.8600000000003,244.32,20.3798989873221)) ;
#91883 = CARTESIAN_POINT('',(65.870710678119,244.4,20.4506096654407)) ;
#91884 = CARTESIAN_POINT('Origin',(65.8000000000003,244.4,20.3798989873221)) ;
#91885 = CARTESIAN_POINT('Origin',(66.1707106781187,244.,20.150609665441)) ;
#91886 = CARTESIAN_POINT('Origin',(66.1,244.,20.0798989873224)) ;
#91887 = CARTESIAN_POINT('Ctrl Pts',(65.870710678119,244.4,20.4506096654407)) ;
#91888 = CARTESIAN_POINT('Ctrl Pts',(65.8360427798554,244.36985400151,20.4852775637043)) ;
#91889 = CARTESIAN_POINT('Ctrl Pts',(65.8021595990186,244.336414539989,20.5191607445411)) ;
#91890 = CARTESIAN_POINT('Ctrl Pts',(65.7707106781184,244.3,20.5506096654413)) ;
#91891 = CARTESIAN_POINT('Ctrl Pts',(65.8778581049433,244.380940195135,20.4434622386164)) ;
#91892 = CARTESIAN_POINT('Ctrl Pts',(65.8430433343115,244.353134492895,20.4771176025337)) ;
#91893 = CARTESIAN_POINT('Ctrl Pts',(65.8097520166116,244.321564032013,20.5105222764137)) ;
#91894 = CARTESIAN_POINT('Ctrl Pts',(65.779668623883,244.286563081353,20.5416517196767)) ;
#91895 = CARTESIAN_POINT('Ctrl Pts',(65.8813668211755,244.347686535338,20.4220307100008)) ;
#91896 = CARTESIAN_POINT('Ctrl Pts',(65.8477072298486,244.32429083244,20.4556827577087)) ;
#91897 = CARTESIAN_POINT('Ctrl Pts',(65.8162031922682,244.295932764198,20.4889255959091)) ;
#91898 = CARTESIAN_POINT('Ctrl Pts',(65.7888149094442,244.263086758199,20.5194962410323)) ;
#91899 = CARTESIAN_POINT('Ctrl Pts',(65.868086390361,244.326064792771,20.3925339722608)) ;
#91900 = CARTESIAN_POINT('Ctrl Pts',(65.83765096067,244.304388217631,20.427955315655)) ;
#91901 = CARTESIAN_POINT('Ctrl Pts',(65.8090916912018,244.277609164501,20.461748760347)) ;
#91902 = CARTESIAN_POINT('Ctrl Pts',(65.7842756013319,244.245700801776,20.4917756576894)) ;
#91903 = CARTESIAN_POINT('Ctrl Pts',(65.8600000000003,244.32,20.3798989873221)) ;
#91904 = CARTESIAN_POINT('Ctrl Pts',(65.8310598414498,244.298294881087,20.4160741855102)) ;
#91905 = CARTESIAN_POINT('Ctrl Pts',(65.8038349716294,244.271779962173,20.4501052727856)) ;
#91906 = CARTESIAN_POINT('Ctrl Pts',(65.7799999999998,244.24,20.4798989873226)) ;
#91907 = CARTESIAN_POINT('',(65.7799999999998,244.24,20.4798989873226)) ;
#91908 = CARTESIAN_POINT('',(65.7707106781184,244.3,20.5506096654413)) ;
#91909 = CARTESIAN_POINT('Origin',(65.6999999999998,244.3,20.4798989873226)) ;
#91910 = CARTESIAN_POINT('Origin',(66.1832249621182,244.169671602392,20.1380953814425)) ;
#91911 = CARTESIAN_POINT('Origin',(66.2266636446466,243.872582870471,19.9189605675217)) ;
#91912 = CARTESIAN_POINT('Ctrl Pts',(65.7714515421241,244.300985201758,20.5498688014357)) ;
#91913 = CARTESIAN_POINT('Ctrl Pts',(65.7063868734546,244.214691234227,20.6149334701051)) ;
#91914 = CARTESIAN_POINT('Ctrl Pts',(65.6704368938516,244.106841295417,20.6508834497081)) ;
#91915 = CARTESIAN_POINT('Ctrl Pts',(65.6707122482682,243.99876732019,20.6506080952915)) ;
#91916 = CARTESIAN_POINT('Ctrl Pts',(65.7871454118088,244.27732415233,20.534176623468)) ;
#91917 = CARTESIAN_POINT('Ctrl Pts',(65.7239411552949,244.198785882952,20.5972314295624)) ;
#91918 = CARTESIAN_POINT('Ctrl Pts',(65.6890022448555,244.098898958229,20.6323192265238)) ;
#91919 = CARTESIAN_POINT('Ctrl Pts',(65.6892698546687,243.998858952482,20.6320504824346)) ;
#91920 = CARTESIAN_POINT('Ctrl Pts',(65.7906574856275,244.253999224632,20.5067481801081)) ;
#91921 = CARTESIAN_POINT('Ctrl Pts',(65.7323922982686,244.182917249722,20.5707044860515)) ;
#91922 = CARTESIAN_POINT('Ctrl Pts',(65.6998049270229,244.091013326971,20.6062210696643)) ;
#91923 = CARTESIAN_POINT('Ctrl Pts',(65.700054515563,243.998949933896,20.6059490395096)) ;
#91924 = CARTESIAN_POINT('Ctrl Pts',(65.7805181325764,244.240689785211,20.4789530628307)) ;
#91925 = CARTESIAN_POINT('Ctrl Pts',(65.7285125559214,244.171669922872,20.5440259656052)) ;
#91926 = CARTESIAN_POINT('Ctrl Pts',(65.6997809923943,244.085431815184,20.5799791663286)) ;
#91927 = CARTESIAN_POINT('Ctrl Pts',(65.7000010583238,243.99901433175,20.5797037872052)) ;
#91928 = CARTESIAN_POINT('',(65.7,244.,20.5798989873224)) ;
#91929 = CARTESIAN_POINT('Origin',(66.1,244.,20.0798989873224)) ;
#91930 = CARTESIAN_POINT('',(65.7000000000001,244.16843697471,20.6213203435596)) ;
#91931 = CARTESIAN_POINT('Ctrl Pts',(65.7,244.,20.5798989873224)) ;
#91932 = CARTESIAN_POINT('Ctrl Pts',(65.7,244.00020850453,20.5800024812788)) ;
#91933 = CARTESIAN_POINT('Ctrl Pts',(65.7,244.000417086861,20.5801058143326)) ;
#91934 = CARTESIAN_POINT('Ctrl Pts',(65.7,244.02719444846,20.5933458356417)) ;
#91935 = CARTESIAN_POINT('Ctrl Pts',(65.7,244.054565273668,20.6036388887893)) ;
#91936 = CARTESIAN_POINT('Ctrl Pts',(65.7,244.105754615284,20.6163080294349)) ;
#91937 = CARTESIAN_POINT('Ctrl Pts',(65.7,244.128852047872,20.619808090116)) ;
#91938 = CARTESIAN_POINT('Ctrl Pts',(65.7,244.157377176375,20.6211837882661)) ;
#91939 = CARTESIAN_POINT('Ctrl Pts',(65.7,244.162669920017,20.621315414962)) ;
#91940 = CARTESIAN_POINT('Ctrl Pts',(65.7,244.167963343701,20.6213203435597)) ;
#91941 = CARTESIAN_POINT('Origin',(66.1707106781187,244.,20.150609665441)) ;
#91942 = CARTESIAN_POINT('Origin',(66.1,244.,24.0213203435596)) ;
#91943 = CARTESIAN_POINT('',(66.1,244.4,18.0918966374184)) ;
#91944 = CARTESIAN_POINT('',(66.1,244.4,24.0213203435596)) ;
#91945 = CARTESIAN_POINT('',(65.8848651777997,244.337219525349,18.0777011469026)) ;
#91946 = CARTESIAN_POINT('Ctrl Pts',(65.8848651777997,244.337219525349,18.0777011469026)) ;
#91947 = CARTESIAN_POINT('Ctrl Pts',(65.9479936757444,244.377493403818,18.0877696165197)) ;
#91948 = CARTESIAN_POINT('Ctrl Pts',(66.0239249506928,244.4,18.0918966374184)) ;
#91949 = CARTESIAN_POINT('Ctrl Pts',(66.1,244.4,18.0918966374184)) ;
#91950 = CARTESIAN_POINT('',(65.7,244.,17.9933962655652)) ;
#91951 = CARTESIAN_POINT('Origin',(66.1,244.,17.9933962655652)) ;
#91952 = CARTESIAN_POINT('',(65.7,244.,24.0213203435596)) ;
#91953 = CARTESIAN_POINT('Origin',(67.55,249.825,18.7713203435596)) ;
#91954 = CARTESIAN_POINT('',(66.8292893218814,245.358578643763,19.4920310216783)) ;
#91955 = CARTESIAN_POINT('',(66.8944035593729,245.423692881254,19.4269167841868)) ;
#91956 = CARTESIAN_POINT('',(66.8292893218813,251.970710678119,19.4920310216783)) ;
#91957 = CARTESIAN_POINT('',(66.8292893218813,250.2125,19.4920310216783)) ;
#91958 = CARTESIAN_POINT('',(68.0684336611227,250.731566338877,18.2528866824369)) ;
#91959 = CARTESIAN_POINT('',(66.7125,252.0875,19.6088203435596)) ;
#91960 = CARTESIAN_POINT('',(68.2414088145807,250.644888384771,18.0799115289789)) ;
#91961 = CARTESIAN_POINT('Ctrl Pts',(68.0684336611227,250.731566338877,18.2528866824369)) ;
#91962 = CARTESIAN_POINT('Ctrl Pts',(68.0965609814737,250.703439018526,18.2247593620858)) ;
#91963 = CARTESIAN_POINT('Ctrl Pts',(68.1259419662347,250.677664283059,18.1953783773249)) ;
#91964 = CARTESIAN_POINT('Ctrl Pts',(68.1716540835089,250.650783089379,18.1496662600507)) ;
#91965 = CARTESIAN_POINT('Ctrl Pts',(68.1899702972436,250.642873774853,18.131350046316)) ;
#91966 = CARTESIAN_POINT('Ctrl Pts',(68.2192212579585,250.639466445032,18.1020990856011)) ;
#91967 = CARTESIAN_POINT('Ctrl Pts',(68.2306528427947,250.640367277029,18.0906675007649)) ;
#91968 = CARTESIAN_POINT('Ctrl Pts',(68.2413962729241,250.644887148136,18.0799240706355)) ;
#91969 = CARTESIAN_POINT('',(68.2414213562374,244.521708245126,18.0798989873223)) ;
#91970 = CARTESIAN_POINT('',(68.2414213562373,249.4375,18.0798989873223)) ;
#91971 = CARTESIAN_POINT('Origin',(69.1914213562374,244.521708245126,17.1298989873223)) ;
#91972 = CARTESIAN_POINT('Origin',(66.8000000000001,244.4,24.0213203435596)) ;
#91973 = CARTESIAN_POINT('',(61.8303059750075,244.4,18.0918966374184)) ;
#91974 = CARTESIAN_POINT('Origin',(61.8303059750075,244.3,18.0918966374184)) ;
#91975 = CARTESIAN_POINT('',(66.1,244.326083322956,17.9953582499056)) ;
#91976 = CARTESIAN_POINT('',(61.8303059750075,244.326083322956,17.9953582499056)) ;
#91977 = CARTESIAN_POINT('Origin',(66.1,244.3,18.0918966374184)) ;
#91978 = CARTESIAN_POINT('Origin',(65.4568347953872,224.289496829998,16.1213203435596)) ;
#91979 = CARTESIAN_POINT('',(65.3568347953872,216.946231446812,16.1213203435596)) ;
#91980 = CARTESIAN_POINT('Origin',(65.4568347953872,216.846231446812,16.1213203435596)) ;
#91981 = CARTESIAN_POINT('',(65.3568347953872,218.546231446812,16.1213203435596)) ;
#91982 = CARTESIAN_POINT('',(65.3568347953872,224.289496829998,16.1213203435596)) ;
#91983 = CARTESIAN_POINT('Ctrl Pts',(65.3568347953872,218.546231446812,16.1213203435596)) ;
#91984 = CARTESIAN_POINT('Ctrl Pts',(65.3568347953872,218.546231446812,16.1153496356238)) ;
#91985 = CARTESIAN_POINT('Ctrl Pts',(65.3573695167032,218.547300046631,16.1095515196401)) ;
#91986 = CARTESIAN_POINT('Ctrl Pts',(65.3595546370681,218.551678573484,16.0971310298406)) ;
#91987 = CARTESIAN_POINT('Ctrl Pts',(65.3613915100209,218.555365057847,16.0908852637126)) ;
#91988 = CARTESIAN_POINT('Ctrl Pts',(65.3670367701187,218.566751467664,16.0762602049506)) ;
#91989 = CARTESIAN_POINT('Ctrl Pts',(65.3714692053955,218.57574568164,16.0686738511528)) ;
#91990 = CARTESIAN_POINT('Ctrl Pts',(65.3839732164585,218.601374810389,16.0514969265816)) ;
#91991 = CARTESIAN_POINT('Ctrl Pts',(65.3941167652591,218.622413030244,16.0422484417149)) ;
#91992 = CARTESIAN_POINT('Ctrl Pts',(65.4209791942954,218.679766384964,16.0263264775169)) ;
#91993 = CARTESIAN_POINT('Ctrl Pts',(65.4380196034223,218.717236626393,16.0215749505388)) ;
#91994 = CARTESIAN_POINT('Ctrl Pts',(65.455898201062,218.758429093735,16.0213236297566)) ;
#91995 = CARTESIAN_POINT('Ctrl Pts',(65.4563667355281,218.759509862814,16.0213203435596)) ;
#91996 = CARTESIAN_POINT('Ctrl Pts',(65.4568347953872,218.760590800757,16.0213203435596)) ;
#91997 = CARTESIAN_POINT('Origin',(64.1568347953872,220.146231446812,16.1213203435596)) ;
#91998 = CARTESIAN_POINT('',(62.9568347953872,218.546231446812,16.1213203435596)) ;
#91999 = CARTESIAN_POINT('Origin',(64.1568347953872,220.146231446812,16.1213203435596)) ;
#92000 = CARTESIAN_POINT('Ctrl Pts',(62.9568347953872,218.546231446812,16.1213203435596)) ;
#92001 = CARTESIAN_POINT('Ctrl Pts',(62.9568347953872,218.546231446812,16.1153496356239)) ;
#92002 = CARTESIAN_POINT('Ctrl Pts',(62.9563000740712,218.547300046631,16.1095515196403)) ;
#92003 = CARTESIAN_POINT('Ctrl Pts',(62.9541149537063,218.551678573484,16.0971310298406)) ;
#92004 = CARTESIAN_POINT('Ctrl Pts',(62.9522780807535,218.555365057847,16.0908852637126)) ;
#92005 = CARTESIAN_POINT('Ctrl Pts',(62.9466328206557,218.566751467664,16.0762602049506)) ;
#92006 = CARTESIAN_POINT('Ctrl Pts',(62.942200385379,218.57574568164,16.0686738511528)) ;
#92007 = CARTESIAN_POINT('Ctrl Pts',(62.929696374316,218.601374810389,16.0514969265817)) ;
#92008 = CARTESIAN_POINT('Ctrl Pts',(62.9195528255154,218.622413030244,16.042248441715)) ;
#92009 = CARTESIAN_POINT('Ctrl Pts',(62.8926903964743,218.679766384974,16.0263264775141)) ;
#92010 = CARTESIAN_POINT('Ctrl Pts',(62.875649987346,218.717236626407,16.0215749505387)) ;
#92011 = CARTESIAN_POINT('Ctrl Pts',(62.8577713897124,218.758429093735,16.0213236297566)) ;
#92012 = CARTESIAN_POINT('Ctrl Pts',(62.8573028552463,218.759509862814,16.0213203435596)) ;
#92013 = CARTESIAN_POINT('Ctrl Pts',(62.8568347953872,218.760590800757,16.0213203435596)) ;
#92014 = CARTESIAN_POINT('Origin',(62.8568347953872,223.489496829998,16.1213203435596)) ;
#92015 = CARTESIAN_POINT('',(62.9568347953872,216.946231446812,16.1213203435596)) ;
#92016 = CARTESIAN_POINT('',(62.9568347953872,223.489496829998,16.1213203435596)) ;
#92017 = CARTESIAN_POINT('Origin',(62.8568347953872,216.846231446812,16.1213203435596)) ;
#92018 = CARTESIAN_POINT('Origin',(67.7248479331787,216.846231446812,16.1213203435596)) ;
#92019 = CARTESIAN_POINT('',(67.7248479331787,216.946231446812,16.1213203435596)) ;
#92020 = CARTESIAN_POINT('Origin',(64.1568347953872,220.146231446812,18.0213203435596)) ;
#92021 = CARTESIAN_POINT('',(65.3568347953872,218.546231446812,23.3713203435596)) ;
#92022 = CARTESIAN_POINT('',(65.3568347953872,218.546231446812,18.0213203435596)) ;
#92023 = CARTESIAN_POINT('',(62.9568347953872,218.546231446812,23.3713203435596)) ;
#92024 = CARTESIAN_POINT('Origin',(64.1568347953872,220.146231446812,23.3713203435596)) ;
#92025 = CARTESIAN_POINT('',(62.9568347953872,218.546231446812,18.0213203435596)) ;
#92026 = CARTESIAN_POINT('Origin',(65.3568347953872,218.546231446812,18.0213203435596)) ;
#92027 = CARTESIAN_POINT('',(65.3568347953872,216.946231446812,23.3713203435596)) ;
#92028 = CARTESIAN_POINT('',(65.3568347953872,216.946231446812,18.0213203435596)) ;
#92029 = CARTESIAN_POINT('',(65.3568347953872,219.383251285823,23.3713203435596)) ;
#92030 = CARTESIAN_POINT('Origin',(70.0928610709702,230.032762213184,16.0213203435596)) ;
#92031 = CARTESIAN_POINT('Ctrl Pts',(70.9999999999998,217.874644018271,23.2713203435596)) ;
#92032 = CARTESIAN_POINT('Ctrl Pts',(70.9999999999998,217.769924263151,23.3236802211194)) ;
#92033 = CARTESIAN_POINT('Ctrl Pts',(70.9523598775596,217.674644018271,23.3713203435597)) ;
#92034 = CARTESIAN_POINT('Ctrl Pts',(70.8999999999997,217.674644018271,23.3713203435596)) ;
#92035 = CARTESIAN_POINT('Ctrl Pts',(70.9999999999998,217.874644018271,23.2713203435596)) ;
#92036 = CARTESIAN_POINT('Ctrl Pts',(70.9999999999998,217.779897573163,23.3336535311308)) ;
#92037 = CARTESIAN_POINT('Ctrl Pts',(70.9364586273346,217.704563948305,23.3713203435597)) ;
#92038 = CARTESIAN_POINT('Ctrl Pts',(70.8999999999997,217.704563948305,23.3713203435596)) ;
#92039 = CARTESIAN_POINT('Ctrl Pts',(70.9999999999998,217.874644018271,23.2713203435596)) ;
#92040 = CARTESIAN_POINT('Ctrl Pts',(70.9999999999998,217.797350865682,23.3511068236508)) ;
#92041 = CARTESIAN_POINT('Ctrl Pts',(70.9227974276425,217.756340925332,23.3964525020675)) ;
#92042 = CARTESIAN_POINT('Ctrl Pts',(70.8999999999997,217.756340925332,23.3964525020674)) ;
#92043 = CARTESIAN_POINT('Ctrl Pts',(70.9999999999998,217.874644018271,23.2713203435596)) ;
#92044 = CARTESIAN_POINT('Ctrl Pts',(70.9999999999998,217.814804158202,23.3685601161707)) ;
#92045 = CARTESIAN_POINT('Ctrl Pts',(70.9405918277816,217.774644018271,23.448880396034)) ;
#92046 = CARTESIAN_POINT('Ctrl Pts',(70.8999999999998,217.774644018271,23.448880396034)) ;
#92047 = CARTESIAN_POINT('Ctrl Pts',(70.9999999999998,217.874644018271,23.2713203435596)) ;
#92048 = CARTESIAN_POINT('Ctrl Pts',(70.9999999999998,217.822284140711,23.3760400986793)) ;
#92049 = CARTESIAN_POINT('Ctrl Pts',(70.9523598775596,217.774644018271,23.4713203435597)) ;
#92050 = CARTESIAN_POINT('Ctrl Pts',(70.8999999999998,217.774644018271,23.4713203435596)) ;
#92051 = CARTESIAN_POINT('',(70.8999999999998,217.774644018271,23.4713203435596)) ;
#92052 = CARTESIAN_POINT('',(70.8999999999998,217.674644018271,23.3713203435596)) ;
#92053 = CARTESIAN_POINT('Origin',(70.8999999999998,217.674644018271,23.4713203435596)) ;
#92054 = CARTESIAN_POINT('',(70.9999999999998,217.874644018271,23.2713203435596)) ;
#92055 = CARTESIAN_POINT('Origin',(70.8999999999998,217.874644018271,23.2713203435596)) ;
#92056 = CARTESIAN_POINT('Origin',(70.8999999999998,217.874644018271,23.2713203435596)) ;
#92057 = CARTESIAN_POINT('Origin',(70.8999999999998,217.874644018271,23.4713203435596)) ;
#92058 = CARTESIAN_POINT('',(70.8292893218811,217.803933340152,23.4713203435596)) ;
#92059 = CARTESIAN_POINT('',(70.7585786437625,217.733222662034,23.3713203435596)) ;
#92060 = CARTESIAN_POINT('Origin',(70.7585786437625,217.733222662034,23.4713203435596)) ;
#92061 = CARTESIAN_POINT('Origin',(70.8999999999998,217.874644018271,23.3713203435596)) ;
#92062 = CARTESIAN_POINT('Origin',(70.8999999999998,217.874644018271,23.4713203435596)) ;
#92063 = CARTESIAN_POINT('Origin',(68.9405576113038,219.551243694493,23.4713203435596)) ;
#92064 = CARTESIAN_POINT('',(70.3022814706893,218.330941191344,23.4713203435596)) ;
#92065 = CARTESIAN_POINT('',(70.2965036217263,218.19529768407,23.3713203435596)) ;
#92066 = CARTESIAN_POINT('Ctrl Pts',(70.3022814706893,218.330941191344,23.4713203435596)) ;
#92067 = CARTESIAN_POINT('Ctrl Pts',(70.3022814706893,218.330941191344,23.4686610045557)) ;
#92068 = CARTESIAN_POINT('Ctrl Pts',(70.3022750583344,218.330797598238,23.4659926797098)) ;
#92069 = CARTESIAN_POINT('Ctrl Pts',(70.3022621053397,218.330507410458,23.4633214758633)) ;
#92070 = CARTESIAN_POINT('Ctrl Pts',(70.3022111056997,218.329364858277,23.4528041832813)) ;
#92071 = CARTESIAN_POINT('Ctrl Pts',(70.3020610895237,218.326006195641,23.4427364614383)) ;
#92072 = CARTESIAN_POINT('Ctrl Pts',(70.3018321156343,218.320842621681,23.4334247968396)) ;
#92073 = CARTESIAN_POINT('Ctrl Pts',(70.3015498927103,218.314478232516,23.4219476576061)) ;
#92074 = CARTESIAN_POINT('Ctrl Pts',(70.301157583221,218.305588184557,23.4119860626266)) ;
#92075 = CARTESIAN_POINT('Ctrl Pts',(70.3007081862357,218.295273815532,23.4036949689328)) ;
#92076 = CARTESIAN_POINT('Ctrl Pts',(70.3001000495539,218.281316120313,23.3924752269849)) ;
#92077 = CARTESIAN_POINT('Ctrl Pts',(70.2993569279694,218.264052061823,23.3837359173529)) ;
#92078 = CARTESIAN_POINT('Ctrl Pts',(70.2985424369338,218.244676672633,23.378163997948)) ;
#92079 = CARTESIAN_POINT('Ctrl Pts',(70.298181690018,218.236095102564,23.3756961343958)) ;
#92080 = CARTESIAN_POINT('Ctrl Pts',(70.2978143471974,218.227276100269,23.3739026646164)) ;
#92081 = CARTESIAN_POINT('Ctrl Pts',(70.2974470041422,218.218368678155,23.372772614714)) ;
#92082 = CARTESIAN_POINT('Ctrl Pts',(70.2972143560673,218.212727372083,23.3720569242152)) ;
#92083 = CARTESIAN_POINT('Ctrl Pts',(70.2969809616316,218.207032740452,23.3716050323275)) ;
#92084 = CARTESIAN_POINT('Ctrl Pts',(70.296748280518,218.201319022744,23.3714185485914)) ;
#92085 = CARTESIAN_POINT('Ctrl Pts',(70.2966666747561,218.199315111556,23.3713531451423)) ;
#92086 = CARTESIAN_POINT('Ctrl Pts',(70.296585101217,218.197307504869,23.3713203435596)) ;
#92087 = CARTESIAN_POINT('Ctrl Pts',(70.2965036217263,218.19529768407,23.3713203435596)) ;
#92088 = CARTESIAN_POINT('',(68.9405576113038,219.551243694493,23.3713203435596)) ;
#92089 = CARTESIAN_POINT('',(69.0112682894225,219.621954372611,23.4713203435596)) ;
#92090 = CARTESIAN_POINT('Origin',(70.9999999999998,217.633222662033,29.5213203435596)) ;
#92091 = CARTESIAN_POINT('',(70.8292893218811,217.803933340152,30.7213203435596)) ;
#92092 = CARTESIAN_POINT('',(70.8292893218811,217.803933340152,29.5213203435596)) ;
#92093 = CARTESIAN_POINT('',(70.4999999999998,218.133222662034,30.7213203435596)) ;
#92094 = CARTESIAN_POINT('',(70.9999999999998,217.633222662033,30.7213203435596)) ;
#92095 = CARTESIAN_POINT('',(70.4999999999998,218.133222662034,29.5213203435596)) ;
#92096 = CARTESIAN_POINT('',(70.4999999999998,218.133222662034,30.7213203435596)) ;
#92097 = CARTESIAN_POINT('',(70.3022814706893,218.330941191344,29.5213203435596)) ;
#92098 = CARTESIAN_POINT('',(70.9999999999998,217.633222662033,29.5213203435596)) ;
#92099 = CARTESIAN_POINT('',(70.3022814706893,218.330941191344,23.3713203435596)) ;
#92100 = CARTESIAN_POINT('Origin',(70.8999999999998,217.874644018271,29.5213203435596)) ;
#92101 = CARTESIAN_POINT('',(70.9999999999998,217.874644018271,30.7213203435596)) ;
#92102 = CARTESIAN_POINT('',(70.9999999999998,217.874644018271,29.5213203435596)) ;
#92103 = CARTESIAN_POINT('Origin',(70.8999999999998,217.874644018271,30.7213203435596)) ;
#92104 = CARTESIAN_POINT('Origin',(70.8999999999999,220.262790180756,23.2713203435596)) ;
#92105 = CARTESIAN_POINT('',(70.8999999999998,217.165524426368,23.3713203435596)) ;
#92106 = CARTESIAN_POINT('',(70.8999999999999,220.262790180756,23.3713203435596)) ;
#92107 = CARTESIAN_POINT('',(70.9999999999998,217.165524426368,23.2713203435596)) ;
#92108 = CARTESIAN_POINT('Origin',(70.8999999999998,217.165524426368,23.2713203435596)) ;
#92109 = CARTESIAN_POINT('',(70.9999999999999,220.262790180756,23.2713203435596)) ;
#92110 = CARTESIAN_POINT('Origin',(82.8283628290598,253.933159539856,29.6213203435596)) ;
#92111 = CARTESIAN_POINT('',(82.8990735071784,254.003870217975,29.6213203435596)) ;
#92112 = CARTESIAN_POINT('',(82.9283628290598,253.933159539856,29.6213203435596)) ;
#92113 = CARTESIAN_POINT('Origin',(82.8283628290598,253.933159539856,29.6213203435596)) ;
#92114 = CARTESIAN_POINT('',(82.8283628290598,253.933159539856,29.5213203435596)) ;
#92115 = CARTESIAN_POINT('Origin',(82.8283628290598,253.933159539856,29.6213203435596)) ;
#92116 = CARTESIAN_POINT('Origin',(82.8283628290598,253.933159539856,29.6213203435596)) ;
#92117 = CARTESIAN_POINT('Origin',(79.2435991885767,257.517923180339,29.6213203435596)) ;
#92118 = CARTESIAN_POINT('',(79.2435991885767,257.517923180339,29.5213203435596)) ;
#92119 = CARTESIAN_POINT('',(79.3143098666953,257.588633858457,29.6213203435596)) ;
#92120 = CARTESIAN_POINT('Origin',(82.8283628290597,243.983954368305,29.6213203435596)) ;
#92121 = CARTESIAN_POINT('',(82.9283628290597,243.983954368305,29.6213203435596)) ;
#92122 = CARTESIAN_POINT('',(82.8283628290597,243.983954368305,29.5213203435596)) ;
#92123 = CARTESIAN_POINT('Origin',(82.8283628290598,253.933159539856,30.6213203435596)) ;
#92124 = CARTESIAN_POINT('',(82.9283628290598,253.933159539856,30.6213203435596)) ;
#92125 = CARTESIAN_POINT('',(82.8990735071784,254.003870217975,30.6213203435596)) ;
#92126 = CARTESIAN_POINT('Origin',(82.8283628290598,253.933159539856,30.6213203435596)) ;
#92127 = CARTESIAN_POINT('',(83.0283628290598,253.933159539856,30.7213203435596)) ;
#92128 = CARTESIAN_POINT('Origin',(83.0283628290598,253.933159539856,30.6213203435596)) ;
#92129 = CARTESIAN_POINT('',(82.9697841852971,254.074580896093,30.7213203435596)) ;
#92130 = CARTESIAN_POINT('Origin',(82.8283628290598,253.933159539856,30.7213203435596)) ;
#92131 = CARTESIAN_POINT('Origin',(82.9697841852971,254.074580896093,30.6213203435596)) ;
#92132 = CARTESIAN_POINT('Origin',(83.0283628290597,249.051115370458,30.6213203435596)) ;
#92133 = CARTESIAN_POINT('',(83.0283628290597,249.051115370458,30.7213203435596)) ;
#92134 = CARTESIAN_POINT('',(82.9283628290597,249.051115370458,30.6213203435596)) ;
#92135 = CARTESIAN_POINT('Origin',(83.6439567661249,253.400408315266,30.6213203435596)) ;
#92136 = CARTESIAN_POINT('',(83.5732460880063,253.329697637147,30.6213203435596)) ;
#92137 = CARTESIAN_POINT('',(83.6439567661249,253.400408315266,30.7213203435596)) ;
#92138 = CARTESIAN_POINT('Origin',(82.8283628290598,253.933159539856,30.7213203435596)) ;
#92139 = CARTESIAN_POINT('',(82.9283628290598,253.933159539856,30.7213203435596)) ;
#92140 = CARTESIAN_POINT('',(82.8990735071784,254.003870217975,30.7213203435596)) ;
#92141 = CARTESIAN_POINT('Origin',(55.2141814145299,240.716611331017,29.5213203435596)) ;
#92142 = CARTESIAN_POINT('',(77.6,262.6,29.5213203435596)) ;
#92143 = CARTESIAN_POINT('',(65.4845247720936,253.51339357907,29.5213203435596)) ;
#92144 = CARTESIAN_POINT('',(77.2,261.8,29.5213203435596)) ;
#92145 = CARTESIAN_POINT('Origin',(78.2,261.8,29.5213203435596)) ;
#92146 = CARTESIAN_POINT('',(77.2,257.723534352175,29.5213203435596)) ;
#92147 = CARTESIAN_POINT('',(77.2,257.,29.5213203435596)) ;
#92148 = CARTESIAN_POINT('',(77.25,256.652146641849,29.5213203435596)) ;
#92149 = CARTESIAN_POINT('Origin',(73.2,257.,29.5213203435596)) ;
#92150 = CARTESIAN_POINT('',(77.25,255.5,29.5213203435596)) ;
#92151 = CARTESIAN_POINT('',(77.25,248.684378986433,29.5213203435596)) ;
#92152 = CARTESIAN_POINT('',(76.7766604535517,253.6,29.5213203435596)) ;
#92153 = CARTESIAN_POINT('Origin',(73.2,255.5,29.5213203435596)) ;
#92154 = CARTESIAN_POINT('',(80.1,253.6,29.5213203435596)) ;
#92155 = CARTESIAN_POINT('',(80.1,253.6,29.5213203435596)) ;
#92156 = CARTESIAN_POINT('',(80.3,253.4,29.5213203435596)) ;
#92157 = CARTESIAN_POINT('Origin',(80.1,253.4,29.5213203435596)) ;
#92158 = CARTESIAN_POINT('',(80.3,252.400000000001,29.5213203435596)) ;
#92159 = CARTESIAN_POINT('',(80.3,252.400000000001,29.5213203435596)) ;
#92160 = CARTESIAN_POINT('',(80.2,252.400000000001,29.5213203435596)) ;
#92161 = CARTESIAN_POINT('',(80.2,252.400000000001,29.5213203435596)) ;
#92162 = CARTESIAN_POINT('',(80.2,249.600000000004,29.5213203435596)) ;
#92163 = CARTESIAN_POINT('',(80.2,249.600000000004,29.5213203435596)) ;
#92164 = CARTESIAN_POINT('',(80.2999999999999,249.600000000004,29.5213203435596)) ;
#92165 = CARTESIAN_POINT('',(80.2999999999999,249.600000000004,29.5213203435596)) ;
#92166 = CARTESIAN_POINT('',(80.2999999999999,248.6,29.5213203435596)) ;
#92167 = CARTESIAN_POINT('',(80.2999999999999,248.6,29.5213203435596)) ;
#92168 = CARTESIAN_POINT('',(80.0999999999999,248.4,29.5213203435596)) ;
#92169 = CARTESIAN_POINT('Origin',(80.0999999999999,248.6,29.5213203435596)) ;
#92170 = CARTESIAN_POINT('',(76.0414213562372,248.4,29.5213203435596)) ;
#92171 = CARTESIAN_POINT('',(76.0414213562372,248.4,29.5213203435596)) ;
#92172 = CARTESIAN_POINT('',(75.8999999999999,248.458578643763,29.5213203435596)) ;
#92173 = CARTESIAN_POINT('Origin',(76.0414213562372,248.6,29.5213203435596)) ;
#92174 = CARTESIAN_POINT('',(75.1585786437627,249.2,29.5213203435596)) ;
#92175 = CARTESIAN_POINT('',(75.1585786437627,249.2,29.5213203435596)) ;
#92176 = CARTESIAN_POINT('',(75.1,249.341421356237,29.5213203435596)) ;
#92177 = CARTESIAN_POINT('Origin',(75.3,249.341421356237,29.5213203435596)) ;
#92178 = CARTESIAN_POINT('',(75.1,251.923339546448,29.5213203435596)) ;
#92179 = CARTESIAN_POINT('',(75.1,252.658578643763,29.5213203435596)) ;
#92180 = CARTESIAN_POINT('',(69.15,255.5,29.5213203435596)) ;
#92181 = CARTESIAN_POINT('Origin',(73.2,255.5,29.5213203435596)) ;
#92182 = CARTESIAN_POINT('',(69.15,256.652146641849,29.5213203435596)) ;
#92183 = CARTESIAN_POINT('',(69.15,248.108305665508,29.5213203435596)) ;
#92184 = CARTESIAN_POINT('',(69.1350889359327,257.,29.5213203435596)) ;
#92185 = CARTESIAN_POINT('Origin',(73.2,257.,29.5213203435596)) ;
#92186 = CARTESIAN_POINT('',(69.1350889359328,261.466666666667,29.5213203435596)) ;
#92187 = CARTESIAN_POINT('',(69.1350889359327,257.,29.5213203435596)) ;
#92188 = CARTESIAN_POINT('',(68.9350889359328,262.066666666667,29.5213203435596)) ;
#92189 = CARTESIAN_POINT('Origin',(68.1350889359328,261.466666666667,29.5213203435596)) ;
#92190 = CARTESIAN_POINT('',(67.6350889359328,263.8,29.5213203435596)) ;
#92191 = CARTESIAN_POINT('',(71.3143388626363,258.894333431062,29.5213203435596)) ;
#92192 = CARTESIAN_POINT('',(57.2649110640674,263.8,29.5213203435596)) ;
#92193 = CARTESIAN_POINT('',(55.2649110640674,263.8,29.5213203435596)) ;
#92194 = CARTESIAN_POINT('',(55.6649110640674,262.6,29.5213203435596)) ;
#92195 = CARTESIAN_POINT('',(50.5686642956594,258.777814923694,29.5213203435596)) ;
#92196 = CARTESIAN_POINT('',(55.2649110640674,261.8,29.5213203435596)) ;
#92197 = CARTESIAN_POINT('Origin',(56.2649110640674,261.8,29.5213203435596)) ;
#92198 = CARTESIAN_POINT('',(55.2649110640674,257.,29.5213203435596)) ;
#92199 = CARTESIAN_POINT('',(55.2649110640674,257.,29.5213203435596)) ;
#92200 = CARTESIAN_POINT('',(55.25,256.652146641849,29.5213203435596)) ;
#92201 = CARTESIAN_POINT('Origin',(51.2,257.,29.5213203435596)) ;
#92202 = CARTESIAN_POINT('',(55.25,255.5,29.5213203435596)) ;
#92203 = CARTESIAN_POINT('',(55.25,248.684378986433,29.5213203435596)) ;
#92204 = CARTESIAN_POINT('',(47.15,255.5,29.5213203435596)) ;
#92205 = CARTESIAN_POINT('Origin',(51.2,255.5,29.5213203435596)) ;
#92206 = CARTESIAN_POINT('',(47.15,256.652146641849,29.5213203435596)) ;
#92207 = CARTESIAN_POINT('',(47.15,248.108305665508,29.5213203435596)) ;
#92208 = CARTESIAN_POINT('',(47.1350889359327,257.,29.5213203435596)) ;
#92209 = CARTESIAN_POINT('Origin',(51.2,257.,29.5213203435596)) ;
#92210 = CARTESIAN_POINT('',(47.1350889359327,261.466666666667,29.5213203435596)) ;
#92211 = CARTESIAN_POINT('',(47.1350889359327,259.8,29.5213203435596)) ;
#92212 = CARTESIAN_POINT('',(46.9350889359326,262.066666666667,29.5213203435596)) ;
#92213 = CARTESIAN_POINT('Origin',(46.1350889359327,261.466666666667,29.5213203435596)) ;
#92214 = CARTESIAN_POINT('',(45.6350889359327,263.8,29.5213203435596)) ;
#92215 = CARTESIAN_POINT('',(53.2743388626362,253.614333431062,29.5213203435596)) ;
#92216 = CARTESIAN_POINT('',(26.7,263.8,29.5213203435596)) ;
#92217 = CARTESIAN_POINT('',(47.1350889359327,263.8,29.5213203435596)) ;
#92218 = CARTESIAN_POINT('',(26.7,245.5,29.5213203435596)) ;
#92219 = CARTESIAN_POINT('',(26.7,252.258305665508,29.5213203435596)) ;
#92220 = CARTESIAN_POINT('',(33.8,245.5,29.5213203435596)) ;
#92221 = CARTESIAN_POINT('',(40.957090707265,245.5,29.5213203435596)) ;
#92222 = CARTESIAN_POINT('',(33.8,248.9,29.5213203435596)) ;
#92223 = CARTESIAN_POINT('',(33.8,243.108305665508,29.5213203435596)) ;
#92224 = CARTESIAN_POINT('',(34.1,248.9,29.5213203435596)) ;
#92225 = CARTESIAN_POINT('',(44.507090707265,248.9,29.5213203435596)) ;
#92226 = CARTESIAN_POINT('',(34.2732050807569,249.,29.5213203435596)) ;
#92227 = CARTESIAN_POINT('Ctrl Pts',(34.1,248.9,29.5213203435596)) ;
#92228 = CARTESIAN_POINT('Ctrl Pts',(34.1277098222081,248.927709822208,29.5213203435596)) ;
#92229 = CARTESIAN_POINT('Ctrl Pts',(34.1615223272204,248.960391271619,29.5213203435596)) ;
#92230 = CARTESIAN_POINT('Ctrl Pts',(34.2184730473151,248.99104280001,29.5213203435596)) ;
#92231 = CARTESIAN_POINT('Ctrl Pts',(34.2477173385693,249.,29.5213203435596)) ;
#92232 = CARTESIAN_POINT('Ctrl Pts',(34.2732050807569,249.,29.5213203435596)) ;
#92233 = CARTESIAN_POINT('',(46.1267949192431,249.,29.5213203435596)) ;
#92234 = CARTESIAN_POINT('',(46.1267949192431,249.,29.5213203435596)) ;
#92235 = CARTESIAN_POINT('',(46.3,248.9,29.5213203435596)) ;
#92236 = CARTESIAN_POINT('Ctrl Pts',(46.1267949192431,249.,29.5213203435596)) ;
#92237 = CARTESIAN_POINT('Ctrl Pts',(46.1522826614306,249.,29.5213203435596)) ;
#92238 = CARTESIAN_POINT('Ctrl Pts',(46.1815269526849,248.99104280001,29.5213203435596)) ;
#92239 = CARTESIAN_POINT('Ctrl Pts',(46.2384776727796,248.960391271619,29.5213203435596)) ;
#92240 = CARTESIAN_POINT('Ctrl Pts',(46.2722901777919,248.927709822208,29.5213203435596)) ;
#92241 = CARTESIAN_POINT('Ctrl Pts',(46.3,248.9,29.5213203435596)) ;
#92242 = CARTESIAN_POINT('',(47.2,248.9,29.5213203435596)) ;
#92243 = CARTESIAN_POINT('',(50.757090707265,248.9,29.5213203435596)) ;
#92244 = CARTESIAN_POINT('',(47.2,246.,29.5213203435596)) ;
#92245 = CARTESIAN_POINT('',(47.2,244.808305665508,29.5213203435596)) ;
#92246 = CARTESIAN_POINT('',(55.3573593128808,246.,29.5213203435596)) ;
#92247 = CARTESIAN_POINT('',(51.207090707265,246.,29.5213203435596)) ;
#92248 = CARTESIAN_POINT('',(56.9573593128808,244.4,29.5213203435596)) ;
#92249 = CARTESIAN_POINT('Origin',(55.3573593128808,244.4,29.5213203435596)) ;
#92250 = CARTESIAN_POINT('',(56.9573593128807,226.261195155516,29.5213203435596)) ;
#92251 = CARTESIAN_POINT('',(56.9573593128808,242.558305665508,29.5213203435596)) ;
#92252 = CARTESIAN_POINT('',(57.4999031800138,224.540465846463,29.5213203435596)) ;
#92253 = CARTESIAN_POINT('Origin',(59.9573593128807,226.261195155516,29.5213203435596)) ;
#92254 = CARTESIAN_POINT('',(60.5916108526749,220.125049696322,29.5213203435596)) ;
#92255 = CARTESIAN_POINT('',(53.3237623239525,230.504613085921,29.5213203435596)) ;
#92256 = CARTESIAN_POINT('',(60.5916108526749,220.645409008718,29.5213203435596)) ;
#92257 = CARTESIAN_POINT('',(60.5916108526749,230.681010169868,29.5213203435596)) ;
#92258 = CARTESIAN_POINT('',(63.1200364144528,223.593701405679,29.5213203435596)) ;
#92259 = CARTESIAN_POINT('Origin',(64.1568347953872,220.146231446812,29.5213203435596)) ;
#92260 = CARTESIAN_POINT('',(63.8582048387328,224.775017823302,29.5213203435596)) ;
#92261 = CARTESIAN_POINT('',(60.2066749117936,218.931348397394,29.5213203435596)) ;
#92262 = CARTESIAN_POINT('',(64.9830939940346,223.650128668,29.5213203435596)) ;
#92263 = CARTESIAN_POINT('',(70.9999999999998,217.633222662033,29.5213203435596)) ;
#92264 = CARTESIAN_POINT('',(67.2791272966079,221.938238572027,29.5213203435596)) ;
#92265 = CARTESIAN_POINT('Origin',(64.1568347953872,220.146231446812,29.5213203435596)) ;
#92266 = CARTESIAN_POINT('',(70.3850625789433,219.622496965577,29.5213203435596)) ;
#92267 = CARTESIAN_POINT('',(60.4556364138638,227.025737280796,29.5213203435596)) ;
#92268 = CARTESIAN_POINT('Ctrl Pts',(70.3850625789433,219.622496965577,29.5213203435596)) ;
#92269 = CARTESIAN_POINT('Ctrl Pts',(70.3511920182576,219.216626210409,29.5213203435596)) ;
#92270 = CARTESIAN_POINT('Ctrl Pts',(70.3247455954692,218.811352574561,29.5213203435596)) ;
#92271 = CARTESIAN_POINT('Ctrl Pts',(70.305749879039,218.406678194919,29.5213203435596)) ;
#92272 = CARTESIAN_POINT('Ctrl Pts',(70.3045647190314,218.381430192685,29.5213203435596)) ;
#92273 = CARTESIAN_POINT('Ctrl Pts',(70.3034085785548,218.356184524476,29.5213203435596)) ;
#92274 = CARTESIAN_POINT('Ctrl Pts',(70.3022814706893,218.330941191344,29.5213203435596)) ;
#92275 = CARTESIAN_POINT('',(70.4999999999999,220.262610236549,29.5213203435596)) ;
#92276 = CARTESIAN_POINT('',(70.5000000000002,229.424916996525,29.5213203435596)) ;
#92277 = CARTESIAN_POINT('',(70.8999999999999,220.262610236549,29.5213203435596)) ;
#92278 = CARTESIAN_POINT('',(63.6796384056928,220.262610236549,29.5213203435596)) ;
#92279 = CARTESIAN_POINT('',(70.8999999999999,220.305309236676,29.5213203435596)) ;
#92280 = CARTESIAN_POINT('',(70.9000000000003,230.510960283846,29.5213203435596)) ;
#92281 = CARTESIAN_POINT('',(72.156281453133,223.25882660182,29.5213203435596)) ;
#92282 = CARTESIAN_POINT('Origin',(74.9999999999998,220.305309236676,29.5213203435596)) ;
#92283 = CARTESIAN_POINT('',(72.2802893291429,223.890441572703,29.5213203435596)) ;
#92284 = CARTESIAN_POINT('Origin',(75.1450953968556,223.000000000001,29.5213203435596)) ;
#92285 = CARTESIAN_POINT('',(71.4146847058821,223.024778714675,29.5213203435596)) ;
#92286 = CARTESIAN_POINT('Origin',(74.9999999999998,220.305309236676,29.5213203435596)) ;
#92287 = CARTESIAN_POINT('',(71.4,223.1,29.5213203435596)) ;
#92288 = CARTESIAN_POINT('Origin',(71.6,223.1,29.5213203435596)) ;
#92289 = CARTESIAN_POINT('',(71.4,225.9,29.5213203435596)) ;
#92290 = CARTESIAN_POINT('',(71.4,225.9,29.5213203435596)) ;
#92291 = CARTESIAN_POINT('',(71.6,226.1,29.5213203435596)) ;
#92292 = CARTESIAN_POINT('Origin',(71.6,225.9,29.5213203435596)) ;
#92293 = CARTESIAN_POINT('',(71.7,226.1,29.5213203435596)) ;
#92294 = CARTESIAN_POINT('',(71.7,226.1,29.5213203435596)) ;
#92295 = CARTESIAN_POINT('',(71.7,231.9,29.5213203435596)) ;
#92296 = CARTESIAN_POINT('',(71.7,231.9,29.5213203435596)) ;
#92297 = CARTESIAN_POINT('',(71.9,232.1,29.5213203435596)) ;
#92298 = CARTESIAN_POINT('Origin',(71.9,231.9,29.5213203435596)) ;
#92299 = CARTESIAN_POINT('',(74.1,232.1,29.5213203435596)) ;
#92300 = CARTESIAN_POINT('',(74.1,232.1,29.5213203435596)) ;
#92301 = CARTESIAN_POINT('',(74.3,231.9,29.5213203435596)) ;
#92302 = CARTESIAN_POINT('Origin',(74.1,231.9,29.5213203435596)) ;
#92303 = CARTESIAN_POINT('',(74.3,226.1,29.5213203435596)) ;
#92304 = CARTESIAN_POINT('',(74.3,226.1,29.5213203435596)) ;
#92305 = CARTESIAN_POINT('',(74.4,226.1,29.5213203435596)) ;
#92306 = CARTESIAN_POINT('',(74.4,226.1,29.5213203435596)) ;
#92307 = CARTESIAN_POINT('',(74.6000000000001,225.9,29.5213203435596)) ;
#92308 = CARTESIAN_POINT('Origin',(74.4,225.9,29.5213203435596)) ;
#92309 = CARTESIAN_POINT('',(74.6,224.787496202879,29.5213203435596)) ;
#92310 = CARTESIAN_POINT('',(74.6,223.1,29.5213203435596)) ;
#92311 = CARTESIAN_POINT('',(75.,224.805309236676,29.5213203435596)) ;
#92312 = CARTESIAN_POINT('Origin',(74.9999999999998,220.305309236676,29.5213203435596)) ;
#92313 = CARTESIAN_POINT('',(80.,224.805309236676,29.5213203435596)) ;
#92314 = CARTESIAN_POINT('',(65.1070907072647,224.805309236677,29.5213203435596)) ;
#92315 = CARTESIAN_POINT('',(80.,225.5,29.5213203435596)) ;
#92316 = CARTESIAN_POINT('',(80.,232.760960283846,29.5213203435596)) ;
#92317 = CARTESIAN_POINT('',(76.0414213562372,225.5,29.5213203435596)) ;
#92318 = CARTESIAN_POINT('',(76.0414213562372,225.5,29.5213203435596)) ;
#92319 = CARTESIAN_POINT('',(75.9707106781185,225.529289321881,29.5213203435596)) ;
#92320 = CARTESIAN_POINT('Origin',(76.0414213562372,225.6,29.5213203435596)) ;
#92321 = CARTESIAN_POINT('',(75.2292893218813,226.270710678119,29.5213203435596)) ;
#92322 = CARTESIAN_POINT('',(75.2292893218813,226.270710678119,29.5213203435596)) ;
#92323 = CARTESIAN_POINT('',(75.1999999999999,226.341421356237,29.5213203435596)) ;
#92324 = CARTESIAN_POINT('Origin',(75.2999999999999,226.341421356237,29.5213203435596)) ;
#92325 = CARTESIAN_POINT('',(75.2,229.658578643763,29.5213203435596)) ;
#92326 = CARTESIAN_POINT('',(75.2,229.658578643763,29.5213203435596)) ;
#92327 = CARTESIAN_POINT('',(75.2292893218813,229.729289321881,29.5213203435596)) ;
#92328 = CARTESIAN_POINT('Origin',(75.3,229.658578643763,29.5213203435596)) ;
#92329 = CARTESIAN_POINT('',(75.9707106781186,230.470710678119,29.5213203435596)) ;
#92330 = CARTESIAN_POINT('',(75.9707106781186,230.470710678119,29.5213203435596)) ;
#92331 = CARTESIAN_POINT('',(76.0414213562372,230.5,29.5213203435596)) ;
#92332 = CARTESIAN_POINT('Origin',(76.0414213562372,230.4,29.5213203435596)) ;
#92333 = CARTESIAN_POINT('',(80.,230.5,29.5213203435596)) ;
#92334 = CARTESIAN_POINT('',(80.1,230.5,29.5213203435596)) ;
#92335 = CARTESIAN_POINT('',(80.,235.608305665508,29.5213203435596)) ;
#92336 = CARTESIAN_POINT('',(82.1145102626716,238.704035802635,29.5213203435596)) ;
#92337 = CARTESIAN_POINT('Origin',(82.2,237.60736287746,29.5213203435596)) ;
#92338 = CARTESIAN_POINT('',(82.183342912681,238.739454580319,29.5213203435596)) ;
#92339 = CARTESIAN_POINT('Origin',(82.106738468369,238.803733341288,29.5213203435596)) ;
#92340 = CARTESIAN_POINT('',(83.9347806063072,240.826736743903,29.5213203435596)) ;
#92341 = CARTESIAN_POINT('',(77.9743376460485,233.723357432561,29.5213203435596)) ;
#92342 = CARTESIAN_POINT('',(84.0283628290596,241.083851787777,29.5213203435596)) ;
#92343 = CARTESIAN_POINT('Origin',(83.6283628290597,241.083851787777,29.5213203435596)) ;
#92344 = CARTESIAN_POINT('',(84.0283628290597,244.265469647218,29.5213203435596)) ;
#92345 = CARTESIAN_POINT('',(84.0283628290597,247.594124250979,29.5213203435596)) ;
#92346 = CARTESIAN_POINT('',(82.27326394817,246.357115043876,29.5213203435596)) ;
#92347 = CARTESIAN_POINT('',(78.9611335727037,250.304358317977,29.5213203435596)) ;
#92348 = CARTESIAN_POINT('',(81.9668461709225,246.500000000001,29.5213203435596)) ;
#92349 = CARTESIAN_POINT('Origin',(81.9668461709225,246.100000000001,29.5213203435596)) ;
#92350 = CARTESIAN_POINT('',(80.6401337790902,246.500000000001,29.5213203435596)) ;
#92351 = CARTESIAN_POINT('',(68.5905137927262,246.500000000001,29.5213203435596)) ;
#92352 = CARTESIAN_POINT('',(80.5401534070282,246.601981212341,29.5213203435596)) ;
#92353 = CARTESIAN_POINT('Origin',(80.6401337790902,246.600000000001,29.5213203435596)) ;
#92354 = CARTESIAN_POINT('',(81.1,247.098386676966,29.5213203435596)) ;
#92355 = CARTESIAN_POINT('Origin',(80.6,247.098386676966,29.5213203435596)) ;
#92356 = CARTESIAN_POINT('',(81.1,247.600000000001,29.5213203435596)) ;
#92357 = CARTESIAN_POINT('',(81.1,243.907499003991,29.5213203435596)) ;
#92358 = CARTESIAN_POINT('',(68.157090707265,247.600000000001,29.5213203435596)) ;
#92359 = CARTESIAN_POINT('',(43.1,251.9,29.5213203435596)) ;
#92360 = CARTESIAN_POINT('',(43.3,252.1,29.5213203435596)) ;
#92361 = CARTESIAN_POINT('Origin',(43.1,252.1,29.5213203435596)) ;
#92362 = CARTESIAN_POINT('',(37.3,251.9,29.5213203435596)) ;
#92363 = CARTESIAN_POINT('',(37.3,251.9,29.5213203435596)) ;
#92364 = CARTESIAN_POINT('',(37.1,252.1,29.5213203435596)) ;
#92365 = CARTESIAN_POINT('Origin',(37.3,252.1,29.5213203435596)) ;
#92366 = CARTESIAN_POINT('',(37.1,259.9,29.5213203435596)) ;
#92367 = CARTESIAN_POINT('',(37.1,259.9,29.5213203435596)) ;
#92368 = CARTESIAN_POINT('',(37.3,260.1,29.5213203435596)) ;
#92369 = CARTESIAN_POINT('Origin',(37.3,259.9,29.5213203435596)) ;
#92370 = CARTESIAN_POINT('',(43.1,260.1,29.5213203435596)) ;
#92371 = CARTESIAN_POINT('',(43.1,260.1,29.5213203435596)) ;
#92372 = CARTESIAN_POINT('',(43.3,259.9,29.5213203435596)) ;
#92373 = CARTESIAN_POINT('Origin',(43.1,259.9,29.5213203435596)) ;
#92374 = CARTESIAN_POINT('',(43.3,252.1,29.5213203435596)) ;
#92375 = CARTESIAN_POINT('',(28.1,254.8,29.5213203435596)) ;
#92376 = CARTESIAN_POINT('Origin',(30.7,254.8,29.5213203435596)) ;
#92377 = CARTESIAN_POINT('',(56.8,257.1,29.5213203435596)) ;
#92378 = CARTESIAN_POINT('',(56.6,256.9,29.5213203435596)) ;
#92379 = CARTESIAN_POINT('Origin',(56.8,256.9,29.5213203435596)) ;
#92380 = CARTESIAN_POINT('',(59.,257.1,29.5213203435596)) ;
#92381 = CARTESIAN_POINT('',(59.,257.1,29.5213203435596)) ;
#92382 = CARTESIAN_POINT('',(59.2,256.9,29.5213203435596)) ;
#92383 = CARTESIAN_POINT('Origin',(59.,256.9,29.5213203435596)) ;
#92384 = CARTESIAN_POINT('',(59.2,251.1,29.5213203435596)) ;
#92385 = CARTESIAN_POINT('',(59.2,251.1,29.5213203435596)) ;
#92386 = CARTESIAN_POINT('',(59.3,251.1,29.5213203435596)) ;
#92387 = CARTESIAN_POINT('',(59.3,251.1,29.5213203435596)) ;
#92388 = CARTESIAN_POINT('',(59.5,250.9,29.5213203435596)) ;
#92389 = CARTESIAN_POINT('Origin',(59.3,250.9,29.5213203435596)) ;
#92390 = CARTESIAN_POINT('',(59.5,248.1,29.5213203435596)) ;
#92391 = CARTESIAN_POINT('',(59.5,248.1,29.5213203435596)) ;
#92392 = CARTESIAN_POINT('',(59.3,247.9,29.5213203435596)) ;
#92393 = CARTESIAN_POINT('Origin',(59.3,248.1,29.5213203435596)) ;
#92394 = CARTESIAN_POINT('',(56.5,247.9,29.5213203435596)) ;
#92395 = CARTESIAN_POINT('',(56.5,247.9,29.5213203435596)) ;
#92396 = CARTESIAN_POINT('',(56.3,248.1,29.5213203435596)) ;
#92397 = CARTESIAN_POINT('Origin',(56.5,248.1,29.5213203435596)) ;
#92398 = CARTESIAN_POINT('',(56.3,250.9,29.5213203435596)) ;
#92399 = CARTESIAN_POINT('',(56.3,250.9,29.5213203435596)) ;
#92400 = CARTESIAN_POINT('',(56.5,251.1,29.5213203435596)) ;
#92401 = CARTESIAN_POINT('Origin',(56.5,250.9,29.5213203435596)) ;
#92402 = CARTESIAN_POINT('',(56.6,251.1,29.5213203435596)) ;
#92403 = CARTESIAN_POINT('',(56.6,251.1,29.5213203435596)) ;
#92404 = CARTESIAN_POINT('',(56.6,256.9,29.5213203435596)) ;
#92405 = CARTESIAN_POINT('',(59.,261.2,29.5213203435596)) ;
#92406 = CARTESIAN_POINT('Origin',(61.5,261.2,29.5213203435596)) ;
#92407 = CARTESIAN_POINT('',(57.9573593128808,242.926794919243,29.5213203435596)) ;
#92408 = CARTESIAN_POINT('',(57.9573593128808,238.073205080757,29.5213203435596)) ;
#92409 = CARTESIAN_POINT('',(57.9573593128808,239.1,29.5213203435596)) ;
#92410 = CARTESIAN_POINT('',(58.0573593128808,243.1,29.5213203435596)) ;
#92411 = CARTESIAN_POINT('Ctrl Pts',(58.0573593128808,243.1,29.5213203435596)) ;
#92412 = CARTESIAN_POINT('Ctrl Pts',(58.0296494906727,243.072290177792,29.5213203435596)) ;
#92413 = CARTESIAN_POINT('Ctrl Pts',(57.9969680412619,243.03847767278,29.5213203435596)) ;
#92414 = CARTESIAN_POINT('Ctrl Pts',(57.9663165128705,242.981526952685,29.5213203435596)) ;
#92415 = CARTESIAN_POINT('Ctrl Pts',(57.9573593128807,242.952282661431,29.5213203435596)) ;
#92416 = CARTESIAN_POINT('Ctrl Pts',(57.9573593128807,242.926794919243,29.5213203435596)) ;
#92417 = CARTESIAN_POINT('',(62.1159379566435,243.1,29.5213203435596)) ;
#92418 = CARTESIAN_POINT('',(62.1159379566435,243.1,29.5213203435596)) ;
#92419 = CARTESIAN_POINT('',(62.2573593128808,243.041421356237,29.5213203435596)) ;
#92420 = CARTESIAN_POINT('Origin',(62.1159379566435,242.9,29.5213203435596)) ;
#92421 = CARTESIAN_POINT('',(62.9987806691181,242.3,29.5213203435596)) ;
#92422 = CARTESIAN_POINT('',(62.9987806691181,242.3,29.5213203435596)) ;
#92423 = CARTESIAN_POINT('',(63.0573593128808,242.158578643763,29.5213203435596)) ;
#92424 = CARTESIAN_POINT('Origin',(62.8573593128808,242.158578643763,29.5213203435596)) ;
#92425 = CARTESIAN_POINT('',(63.0573593128808,238.841421356237,29.5213203435596)) ;
#92426 = CARTESIAN_POINT('',(63.0573593128808,238.841421356237,29.5213203435596)) ;
#92427 = CARTESIAN_POINT('',(62.9987806691181,238.7,29.5213203435596)) ;
#92428 = CARTESIAN_POINT('Origin',(62.8573593128808,238.841421356237,29.5213203435596)) ;
#92429 = CARTESIAN_POINT('',(62.2573593128808,237.958578643763,29.5213203435596)) ;
#92430 = CARTESIAN_POINT('',(62.2573593128808,237.958578643763,29.5213203435596)) ;
#92431 = CARTESIAN_POINT('',(62.1159379566435,237.9,29.5213203435596)) ;
#92432 = CARTESIAN_POINT('Origin',(62.1159379566435,238.1,29.5213203435596)) ;
#92433 = CARTESIAN_POINT('',(58.0573593128808,237.9,29.5213203435596)) ;
#92434 = CARTESIAN_POINT('',(58.0573593128808,237.9,29.5213203435596)) ;
#92435 = CARTESIAN_POINT('Ctrl Pts',(57.9573593128807,238.073205080757,29.5213203435596)) ;
#92436 = CARTESIAN_POINT('Ctrl Pts',(57.9573593128807,238.047717338569,29.5213203435596)) ;
#92437 = CARTESIAN_POINT('Ctrl Pts',(57.9663165128705,238.018473047315,29.5213203435596)) ;
#92438 = CARTESIAN_POINT('Ctrl Pts',(57.9969680412619,237.96152232722,29.5213203435596)) ;
#92439 = CARTESIAN_POINT('Ctrl Pts',(58.0296494906727,237.927709822208,29.5213203435596)) ;
#92440 = CARTESIAN_POINT('Ctrl Pts',(58.0573593128808,237.9,29.5213203435596)) ;
#92441 = CARTESIAN_POINT('',(60.0305643936376,236.,29.5213203435596)) ;
#92442 = CARTESIAN_POINT('',(59.8573593128808,235.9,29.5213203435596)) ;
#92443 = CARTESIAN_POINT('Ctrl Pts',(60.0305643936376,236.,29.5213203435596)) ;
#92444 = CARTESIAN_POINT('Ctrl Pts',(60.0050766514501,236.,29.5213203435596)) ;
#92445 = CARTESIAN_POINT('Ctrl Pts',(59.9758323601959,235.99104280001,29.5213203435596)) ;
#92446 = CARTESIAN_POINT('Ctrl Pts',(59.9188816401012,235.960391271619,29.5213203435596)) ;
#92447 = CARTESIAN_POINT('Ctrl Pts',(59.8850691350889,235.927709822208,29.5213203435596)) ;
#92448 = CARTESIAN_POINT('Ctrl Pts',(59.8573593128808,235.9,29.5213203435596)) ;
#92449 = CARTESIAN_POINT('',(62.2841542321239,236.,29.5213203435596)) ;
#92450 = CARTESIAN_POINT('',(62.4573593128808,230.1,29.5213203435596)) ;
#92451 = CARTESIAN_POINT('',(62.4573593128808,230.1,29.5213203435596)) ;
#92452 = CARTESIAN_POINT('',(62.5573593128808,230.1,29.5213203435596)) ;
#92453 = CARTESIAN_POINT('',(62.5573593128808,230.1,29.5213203435596)) ;
#92454 = CARTESIAN_POINT('',(62.7573593128808,229.9,29.5213203435596)) ;
#92455 = CARTESIAN_POINT('Origin',(62.5573593128808,229.9,29.5213203435596)) ;
#92456 = CARTESIAN_POINT('',(62.7573593128808,227.1,29.5213203435596)) ;
#92457 = CARTESIAN_POINT('',(62.7573593128808,227.1,29.5213203435596)) ;
#92458 = CARTESIAN_POINT('',(62.5573593128808,226.9,29.5213203435596)) ;
#92459 = CARTESIAN_POINT('Origin',(62.5573593128808,227.1,29.5213203435596)) ;
#92460 = CARTESIAN_POINT('',(59.7573593128808,226.9,29.5213203435596)) ;
#92461 = CARTESIAN_POINT('',(59.7573593128808,226.9,29.5213203435596)) ;
#92462 = CARTESIAN_POINT('',(59.5573593128807,227.1,29.5213203435596)) ;
#92463 = CARTESIAN_POINT('Origin',(59.7573593128808,227.1,29.5213203435596)) ;
#92464 = CARTESIAN_POINT('',(59.5573593128808,229.9,29.5213203435596)) ;
#92465 = CARTESIAN_POINT('',(59.5573593128808,229.9,29.5213203435596)) ;
#92466 = CARTESIAN_POINT('',(59.7573593128808,230.1,29.5213203435596)) ;
#92467 = CARTESIAN_POINT('Origin',(59.7573593128808,229.9,29.5213203435596)) ;
#92468 = CARTESIAN_POINT('',(59.8573593128808,230.1,29.5213203435596)) ;
#92469 = CARTESIAN_POINT('',(59.8573593128808,230.1,29.5213203435596)) ;
#92470 = CARTESIAN_POINT('',(59.8573593128808,235.9,29.5213203435596)) ;
#92471 = CARTESIAN_POINT('',(64.8,257.1,29.5213203435596)) ;
#92472 = CARTESIAN_POINT('',(64.6,256.9,29.5213203435596)) ;
#92473 = CARTESIAN_POINT('Origin',(64.8,256.9,29.5213203435596)) ;
#92474 = CARTESIAN_POINT('',(67.,257.1,29.5213203435596)) ;
#92475 = CARTESIAN_POINT('',(67.,257.1,29.5213203435596)) ;
#92476 = CARTESIAN_POINT('',(67.2,256.9,29.5213203435596)) ;
#92477 = CARTESIAN_POINT('Origin',(67.,256.9,29.5213203435596)) ;
#92478 = CARTESIAN_POINT('',(67.2,251.1,29.5213203435596)) ;
#92479 = CARTESIAN_POINT('',(67.2,251.1,29.5213203435596)) ;
#92480 = CARTESIAN_POINT('',(67.3,251.1,29.5213203435596)) ;
#92481 = CARTESIAN_POINT('',(67.3,251.1,29.5213203435596)) ;
#92482 = CARTESIAN_POINT('',(67.5,250.9,29.5213203435596)) ;
#92483 = CARTESIAN_POINT('Origin',(67.3,250.9,29.5213203435596)) ;
#92484 = CARTESIAN_POINT('',(67.5,248.1,29.5213203435596)) ;
#92485 = CARTESIAN_POINT('',(67.5,248.1,29.5213203435596)) ;
#92486 = CARTESIAN_POINT('',(67.3,247.9,29.5213203435596)) ;
#92487 = CARTESIAN_POINT('Origin',(67.3,248.1,29.5213203435596)) ;
#92488 = CARTESIAN_POINT('',(64.5,247.9,29.5213203435596)) ;
#92489 = CARTESIAN_POINT('',(64.5,247.9,29.5213203435596)) ;
#92490 = CARTESIAN_POINT('',(64.3,248.1,29.5213203435596)) ;
#92491 = CARTESIAN_POINT('Origin',(64.5,248.1,29.5213203435596)) ;
#92492 = CARTESIAN_POINT('',(64.3,250.9,29.5213203435596)) ;
#92493 = CARTESIAN_POINT('',(64.3,250.9,29.5213203435596)) ;
#92494 = CARTESIAN_POINT('',(64.5,251.1,29.5213203435596)) ;
#92495 = CARTESIAN_POINT('Origin',(64.5,250.9,29.5213203435596)) ;
#92496 = CARTESIAN_POINT('',(64.6,251.1,29.5213203435596)) ;
#92497 = CARTESIAN_POINT('',(64.6,251.1,29.5213203435596)) ;
#92498 = CARTESIAN_POINT('',(64.6,256.9,29.5213203435596)) ;
#92499 = CARTESIAN_POINT('Origin',(82.9283628290598,253.974580896093,30.7213203435596)) ;
#92500 = CARTESIAN_POINT('Ctrl Pts',(72.2848151277479,223.47832706609,29.6213203435596)) ;
#92501 = CARTESIAN_POINT('Ctrl Pts',(72.2848151277479,223.47832706609,29.6117820586428)) ;
#92502 = CARTESIAN_POINT('Ctrl Pts',(72.2808542722274,223.472044514469,29.5927809266332)) ;
#92503 = CARTESIAN_POINT('Ctrl Pts',(72.2660826403646,223.448322669426,29.568915436412)) ;
#92504 = CARTESIAN_POINT('Ctrl Pts',(72.2400335798865,223.405693978819,29.5444496865641)) ;
#92505 = CARTESIAN_POINT('Ctrl Pts',(72.2020093099499,223.341346933962,29.5259708354515)) ;
#92506 = CARTESIAN_POINT('Ctrl Pts',(72.1712632154036,223.286371940893,29.5213203435596)) ;
#92507 = CARTESIAN_POINT('Ctrl Pts',(72.156281453133,223.25882660182,29.5213203435596)) ;
#92508 = CARTESIAN_POINT('Ctrl Pts',(72.2810000867808,223.455514042998,29.6213203435596)) ;
#92509 = CARTESIAN_POINT('Ctrl Pts',(72.2810000867808,223.455514042998,29.6143550630749)) ;
#92510 = CARTESIAN_POINT('Ctrl Pts',(72.2789291556126,223.45022120786,29.6002951365768)) ;
#92511 = CARTESIAN_POINT('Ctrl Pts',(72.2690858869446,223.429107117665,29.5790237734122)) ;
#92512 = CARTESIAN_POINT('Ctrl Pts',(72.2482378360867,223.389557669006,29.5536298248665)) ;
#92513 = CARTESIAN_POINT('Ctrl Pts',(72.213241144952,223.328135436704,29.5307455300177)) ;
#92514 = CARTESIAN_POINT('Ctrl Pts',(72.1821614688016,223.274848566189,29.5227418738956)) ;
#92515 = CARTESIAN_POINT('Ctrl Pts',(72.1666575336158,223.248049890488,29.5213203435596)) ;
#92516 = CARTESIAN_POINT('Ctrl Pts',(72.2888679854647,223.413391262911,29.6213203435597)) ;
#92517 = CARTESIAN_POINT('Ctrl Pts',(72.2888679854647,223.413391262911,29.6173756251696)) ;
#92518 = CARTESIAN_POINT('Ctrl Pts',(72.2892555769235,223.409994519109,29.609053079611)) ;
#92519 = CARTESIAN_POINT('Ctrl Pts',(72.2851493810959,223.39392773353,29.5895727666044)) ;
#92520 = CARTESIAN_POINT('Ctrl Pts',(72.2693821576178,223.360449550633,29.5609780226199)) ;
#92521 = CARTESIAN_POINT('Ctrl Pts',(72.2355055751497,223.30476013175,29.5309152737761)) ;
#92522 = CARTESIAN_POINT('Ctrl Pts',(72.201962597952,223.25464893562,29.5184715285348)) ;
#92523 = CARTESIAN_POINT('Ctrl Pts',(72.184795277803,223.229211829851,29.5153203301976)) ;
#92524 = CARTESIAN_POINT('Ctrl Pts',(72.3355462445646,223.366840464368,29.6213203435596)) ;
#92525 = CARTESIAN_POINT('Ctrl Pts',(72.3355462445646,223.366840464368,29.6164645616614)) ;
#92526 = CARTESIAN_POINT('Ctrl Pts',(72.3360510372649,223.365000743143,29.6061878672546)) ;
#92527 = CARTESIAN_POINT('Ctrl Pts',(72.3309634543418,223.353337548304,29.5818580530947)) ;
#92528 = CARTESIAN_POINT('Ctrl Pts',(72.3114661600803,223.325571261253,29.5463312063646)) ;
#92529 = CARTESIAN_POINT('Ctrl Pts',(72.2699544689077,223.275650758824,29.5095570918057)) ;
#92530 = CARTESIAN_POINT('Ctrl Pts',(72.2292143217159,223.228761139121,29.4947957329644)) ;
#92531 = CARTESIAN_POINT('Ctrl Pts',(72.2084154512032,223.204679657923,29.4911830637617)) ;
#92532 = CARTESIAN_POINT('Ctrl Pts',(72.3958472601896,223.356104604207,29.6213203435596)) ;
#92533 = CARTESIAN_POINT('Ctrl Pts',(72.3958472601896,223.356104604207,29.6106947817332)) ;
#92534 = CARTESIAN_POINT('Ctrl Pts',(72.3933967836352,223.353510123056,29.5891261889309)) ;
#92535 = CARTESIAN_POINT('Ctrl Pts',(72.3797193135333,223.340262757401,29.554538401925)) ;
#92536 = CARTESIAN_POINT('Ctrl Pts',(72.3487860197444,223.311258504548,29.5122402365605)) ;
#92537 = CARTESIAN_POINT('Ctrl Pts',(72.2951190991269,223.260961486717,29.4740143351241)) ;
#92538 = CARTESIAN_POINT('Ctrl Pts',(72.2468169388032,223.214067870685,29.4609869305912)) ;
#92539 = CARTESIAN_POINT('Ctrl Pts',(72.2225691253102,223.189979496298,29.4587319390131)) ;
#92540 = CARTESIAN_POINT('Ctrl Pts',(72.433908428714,223.373773832992,29.6213203435596)) ;
#92541 = CARTESIAN_POINT('Ctrl Pts',(72.433908428714,223.373773832992,29.6047572686629)) ;
#92542 = CARTESIAN_POINT('Ctrl Pts',(72.4285124008623,223.369273781245,29.5716464499249)) ;
#92543 = CARTESIAN_POINT('Ctrl Pts',(72.4069263743005,223.351045791115,29.5278439559481)) ;
#92544 = CARTESIAN_POINT('Ctrl Pts',(72.3665979735026,223.31640834513,29.4809183052355)) ;
#92545 = CARTESIAN_POINT('Ctrl Pts',(72.304473339827,223.261299627013,29.4436111538445)) ;
#92546 = CARTESIAN_POINT('Ctrl Pts',(72.2517858004854,223.211967617058,29.4332114711027)) ;
#92547 = CARTESIAN_POINT('Ctrl Pts',(72.225640442081,223.186789592914,29.4325403173224)) ;
#92548 = CARTESIAN_POINT('Ctrl Pts',(72.4472638847366,223.384844644141,29.6213203435596)) ;
#92549 = CARTESIAN_POINT('Ctrl Pts',(72.4472638847366,223.384844644141,29.6022437737259)) ;
#92550 = CARTESIAN_POINT('Ctrl Pts',(72.4406894966491,223.379412576914,29.5642415097069)) ;
#92551 = CARTESIAN_POINT('Ctrl Pts',(72.4160080913986,223.358747929883,29.5165105292643)) ;
#92552 = CARTESIAN_POINT('Ctrl Pts',(72.3720483401316,223.321197129049,29.4675790295685)) ;
#92553 = CARTESIAN_POINT('Ctrl Pts',(72.306745659313,223.263425781024,29.4306213273434)) ;
#92554 = CARTESIAN_POINT('Ctrl Pts',(72.2524544719542,223.212606794792,29.4213203435596)) ;
#92555 = CARTESIAN_POINT('Ctrl Pts',(72.225640442081,223.186789592914,29.4213203435596)) ;
#92556 = CARTESIAN_POINT('',(72.2256404420809,223.186789592914,29.4213203435596)) ;
#92557 = CARTESIAN_POINT('',(72.4472638847366,223.384844644141,29.6213203435596)) ;
#92558 = CARTESIAN_POINT('Ctrl Pts',(72.225640442081,223.186789592914,29.4213203435596)) ;
#92559 = CARTESIAN_POINT('Ctrl Pts',(72.2524544719542,223.212606794792,29.4213203435596)) ;
#92560 = CARTESIAN_POINT('Ctrl Pts',(72.306745659313,223.263425781024,29.4306213273434)) ;
#92561 = CARTESIAN_POINT('Ctrl Pts',(72.3720483401316,223.321197129049,29.4675790295685)) ;
#92562 = CARTESIAN_POINT('Ctrl Pts',(72.4160080913986,223.358747929883,29.5165105292643)) ;
#92563 = CARTESIAN_POINT('Ctrl Pts',(72.4406894966491,223.379412576914,29.5642415097069)) ;
#92564 = CARTESIAN_POINT('Ctrl Pts',(72.4472638847366,223.384844644141,29.6022437737259)) ;
#92565 = CARTESIAN_POINT('Ctrl Pts',(72.4472638847366,223.384844644141,29.6213203435596)) ;
#92566 = CARTESIAN_POINT('',(72.2848151277479,223.47832706609,29.6213203435596)) ;
#92567 = CARTESIAN_POINT('Origin',(72.383445481855,223.461833029328,29.6213203435596)) ;
#92568 = CARTESIAN_POINT('Ctrl Pts',(72.2848151277479,223.47832706609,29.6213203435596)) ;
#92569 = CARTESIAN_POINT('Ctrl Pts',(72.2848151277479,223.47832706609,29.6117820586428)) ;
#92570 = CARTESIAN_POINT('Ctrl Pts',(72.2808542722274,223.472044514469,29.5927809266332)) ;
#92571 = CARTESIAN_POINT('Ctrl Pts',(72.2660826403646,223.448322669426,29.568915436412)) ;
#92572 = CARTESIAN_POINT('Ctrl Pts',(72.2400335798865,223.405693978819,29.5444496865641)) ;
#92573 = CARTESIAN_POINT('Ctrl Pts',(72.2020093099499,223.341346933962,29.5259708354515)) ;
#92574 = CARTESIAN_POINT('Ctrl Pts',(72.1712632154036,223.286371940893,29.5213203435596)) ;
#92575 = CARTESIAN_POINT('Ctrl Pts',(72.156281453133,223.25882660182,29.5213203435596)) ;
#92576 = CARTESIAN_POINT('Origin',(72.156281453133,223.25882660182,29.4213203435596)) ;
#92577 = CARTESIAN_POINT('Origin',(72.383445481855,223.461833029328,29.5213203435596)) ;
#92578 = CARTESIAN_POINT('',(72.2848151277479,223.47832706609,29.5213203435596)) ;
#92579 = CARTESIAN_POINT('',(72.4472638847366,223.384844644141,29.5213203435596)) ;
#92580 = CARTESIAN_POINT('Origin',(75.1450953968556,223.000000000001,29.6213203435596)) ;
#92581 = CARTESIAN_POINT('',(72.4201780792821,223.992383802966,29.6213203435596)) ;
#92582 = CARTESIAN_POINT('Ctrl Pts',(72.4201780792825,223.992383802966,29.6213203435596)) ;
#92583 = CARTESIAN_POINT('Ctrl Pts',(72.4201780792825,223.992383802966,29.6145564866725)) ;
#92584 = CARTESIAN_POINT('Ctrl Pts',(72.4191973948714,223.991698158942,29.6078620210061)) ;
#92585 = CARTESIAN_POINT('Ctrl Pts',(72.417299229791,223.990367815798,29.601339025129)) ;
#92586 = CARTESIAN_POINT('Ctrl Pts',(72.4148969906463,223.98868418859,29.5930837915886)) ;
#92587 = CARTESIAN_POINT('Ctrl Pts',(72.4111225700089,223.986035531718,29.5854386000695)) ;
#92588 = CARTESIAN_POINT('Ctrl Pts',(72.4064704600445,223.982754617015,29.5785304102571)) ;
#92589 = CARTESIAN_POINT('Ctrl Pts',(72.3998148180006,223.97806070522,29.5686470586349)) ;
#92590 = CARTESIAN_POINT('Ctrl Pts',(72.3913538115502,223.972063817752,29.5602421869295)) ;
#92591 = CARTESIAN_POINT('Ctrl Pts',(72.3822927902472,223.965583675022,29.5533237804999)) ;
#92592 = CARTESIAN_POINT('Ctrl Pts',(72.3685935368461,223.955786422111,29.5428639217664)) ;
#92593 = CARTESIAN_POINT('Ctrl Pts',(72.3518149123848,223.943668481139,29.5344794129739)) ;
#92594 = CARTESIAN_POINT('Ctrl Pts',(72.3330588183395,223.929867793737,29.528907978084)) ;
#92595 = CARTESIAN_POINT('Ctrl Pts',(72.3174379333076,223.918373985338,29.5242678465264)) ;
#92596 = CARTESIAN_POINT('Ctrl Pts',(72.301017128619,223.906130659284,29.5217464661521)) ;
#92597 = CARTESIAN_POINT('Ctrl Pts',(72.2846076883626,223.893713421533,29.5213699088416)) ;
#92598 = CARTESIAN_POINT('Ctrl Pts',(72.283167988846,223.892623982106,29.5213368711896)) ;
#92599 = CARTESIAN_POINT('Ctrl Pts',(72.2817283570166,223.891533231001,29.5213203435596)) ;
#92600 = CARTESIAN_POINT('Ctrl Pts',(72.2802893291429,223.890441572703,29.5213203435596)) ;
#92601 = CARTESIAN_POINT('Origin',(75.1450953968556,223.000000000001,29.6213203435596)) ;
#92602 = CARTESIAN_POINT('Origin',(74.9999999999998,220.305309236676,29.4213203435596)) ;
#92603 = CARTESIAN_POINT('',(70.9999999999999,220.305309236676,29.4213203435596)) ;
#92604 = CARTESIAN_POINT('Origin',(70.8999999999999,220.305309236676,29.4213203435596)) ;
#92605 = CARTESIAN_POINT('Origin',(74.9999999999998,220.305309236676,29.4213203435596)) ;
#92606 = CARTESIAN_POINT('Origin',(70.9000000000003,230.510960283846,29.4213203435596)) ;
#92607 = CARTESIAN_POINT('',(70.9999999999999,220.262610236549,29.4213203435596)) ;
#92608 = CARTESIAN_POINT('Origin',(70.8999999999999,220.262610236549,29.4213203435596)) ;
#92609 = CARTESIAN_POINT('',(71.0000000000003,230.510960283846,29.4213203435596)) ;
#92610 = CARTESIAN_POINT('Origin',(75.1450953968556,223.000000000001,30.7213203435596)) ;
#92611 = CARTESIAN_POINT('',(72.4201780792821,223.992383802966,30.7213203435596)) ;
#92612 = CARTESIAN_POINT('Origin',(74.9999999999998,220.305309236676,29.5213203435596)) ;
#92613 = CARTESIAN_POINT('',(70.9999999999999,220.305309236676,16.1213203435596)) ;
#92614 = CARTESIAN_POINT('',(70.9999999999999,220.305309236676,29.5213203435596)) ;
#92615 = CARTESIAN_POINT('',(75.,224.305309236676,16.1213203435596)) ;
#92616 = CARTESIAN_POINT('Origin',(74.9999999999998,220.305309236676,16.1213203435596)) ;
#92617 = CARTESIAN_POINT('',(75.,224.305309236676,29.5213203435596)) ;
#92618 = CARTESIAN_POINT('Origin',(70.9999999999999,220.305309236676,29.5213203435596)) ;
#92619 = CARTESIAN_POINT('',(70.9999999999999,220.262610236549,30.7213203435596)) ;
#92620 = CARTESIAN_POINT('',(70.9999999999999,220.262610236549,30.1213203435596)) ;
#92621 = CARTESIAN_POINT('',(70.9999999999999,220.305309236676,30.7213203435596)) ;
#92622 = CARTESIAN_POINT('',(70.9999999999998,217.165524426368,16.1213203435596)) ;
#92623 = CARTESIAN_POINT('',(70.9999999999998,217.165524426368,25.0213203435596)) ;
#92624 = CARTESIAN_POINT('',(71.0000000000001,225.16903572493,16.1213203435596)) ;
#92625 = CARTESIAN_POINT('Origin',(80.1,230.5,29.5213203435596)) ;
#92626 = CARTESIAN_POINT('',(80.,230.5,30.7213203435596)) ;
#92627 = CARTESIAN_POINT('',(76.0414213562372,230.5,25.7213203435596)) ;
#92628 = CARTESIAN_POINT('',(76.0414213562372,230.5,29.5213203435596)) ;
#92629 = CARTESIAN_POINT('',(80.1,230.5,25.7213203435596)) ;
#92630 = CARTESIAN_POINT('',(78.9,230.5,25.7213203435596)) ;
#92631 = CARTESIAN_POINT('',(80.1,230.5,29.5213203435596)) ;
#92632 = CARTESIAN_POINT('Origin',(84.0283628290597,244.57661441259,30.6213203435596)) ;
#92633 = CARTESIAN_POINT('',(84.1283628290597,244.57661441259,30.6213203435596)) ;
#92634 = CARTESIAN_POINT('',(83.9517583847478,244.512335651621,30.6213203435596)) ;
#92635 = CARTESIAN_POINT('Origin',(84.0283628290597,244.57661441259,30.6213203435596)) ;
#92636 = CARTESIAN_POINT('',(84.0283628290597,244.57661441259,30.7213203435596)) ;
#92637 = CARTESIAN_POINT('Origin',(84.0283628290597,244.57661441259,30.6213203435596)) ;
#92638 = CARTESIAN_POINT('Origin',(84.0283628290597,244.57661441259,30.6213203435596)) ;
#92639 = CARTESIAN_POINT('Origin',(79.1,257.325466667661,30.6213203435596)) ;
#92640 = CARTESIAN_POINT('',(79.1,259.648528137424,30.7213203435596)) ;
#92641 = CARTESIAN_POINT('',(79.1,257.325466667661,30.7213203435596)) ;
#92642 = CARTESIAN_POINT('',(79.2,259.648528137424,30.6213203435596)) ;
#92643 = CARTESIAN_POINT('Origin',(79.1,259.648528137424,30.6213203435596)) ;
#92644 = CARTESIAN_POINT('',(79.2,257.325466667661,30.6213203435596)) ;
#92645 = CARTESIAN_POINT('Origin',(79.7999999999999,259.648528137424,30.6213203435596)) ;
#92646 = CARTESIAN_POINT('',(79.3050252531695,259.153553390593,30.7213203435596)) ;
#92647 = CARTESIAN_POINT('',(79.3757359312881,259.224264068712,30.6213203435596)) ;
#92648 = CARTESIAN_POINT('Origin',(79.3050252531695,259.153553390593,30.6213203435596)) ;
#92649 = CARTESIAN_POINT('Origin',(79.7999999999999,259.648528137424,30.6213203435596)) ;
#92650 = CARTESIAN_POINT('Origin',(79.7999999999999,259.648528137424,30.7213203435596)) ;
#92651 = CARTESIAN_POINT('Origin',(82.1504860297137,256.30809261405,30.6213203435596)) ;
#92652 = CARTESIAN_POINT('',(83.7647589321277,254.693819711636,30.7213203435596)) ;
#92653 = CARTESIAN_POINT('',(83.8354696102463,254.764530389755,30.6213203435596)) ;
#92654 = CARTESIAN_POINT('Origin',(83.7647589321277,254.693819711636,30.6213203435596)) ;
#92655 = CARTESIAN_POINT('',(82.2211967078324,256.378803292168,30.6213203435596)) ;
#92656 = CARTESIAN_POINT('',(82.1504860297137,256.30809261405,30.7213203435596)) ;
#92657 = CARTESIAN_POINT('Origin',(83.1283628290598,254.057423608568,30.6213203435596)) ;
#92658 = CARTESIAN_POINT('',(84.0283628290598,254.057423608568,30.7213203435596)) ;
#92659 = CARTESIAN_POINT('',(84.1283628290598,254.057423608568,30.6213203435596)) ;
#92660 = CARTESIAN_POINT('Origin',(84.0283628290598,254.057423608568,30.6213203435596)) ;
#92661 = CARTESIAN_POINT('Origin',(83.1283628290598,254.057423608568,30.6213203435596)) ;
#92662 = CARTESIAN_POINT('Origin',(83.1283628290598,254.057423608568,30.7213203435596)) ;
#92663 = CARTESIAN_POINT('Origin',(84.0283628290598,252.661285253132,30.6213203435596)) ;
#92664 = CARTESIAN_POINT('',(84.1283628290598,252.661285253132,30.6213203435596)) ;
#92665 = CARTESIAN_POINT('',(84.0283628290598,252.661285253132,30.7213203435596)) ;
#92666 = CARTESIAN_POINT('Origin',(82.1755472374987,246.700000000001,30.6213203435596)) ;
#92667 = CARTESIAN_POINT('',(80.9021391328793,246.700000000001,30.7213203435596)) ;
#92668 = CARTESIAN_POINT('',(80.6401337790902,246.600000000001,30.6213203435596)) ;
#92669 = CARTESIAN_POINT('Ctrl Pts',(80.9021391328789,246.700000000001,30.7213203435596)) ;
#92670 = CARTESIAN_POINT('Ctrl Pts',(80.8546339956107,246.663971784673,30.7213203435597)) ;
#92671 = CARTESIAN_POINT('Ctrl Pts',(80.7930243634798,246.633827705385,30.7009621255511)) ;
#92672 = CARTESIAN_POINT('Ctrl Pts',(80.7145517409522,246.610975914622,30.6686175810887)) ;
#92673 = CARTESIAN_POINT('Ctrl Pts',(80.6838650368446,246.60487069038,30.6554832196524)) ;
#92674 = CARTESIAN_POINT('Ctrl Pts',(80.6554491801068,246.601452173645,30.6384990816338)) ;
#92675 = CARTESIAN_POINT('Ctrl Pts',(80.6509273236865,246.60097285483,30.6355928657033)) ;
#92676 = CARTESIAN_POINT('Ctrl Pts',(80.6453291232314,246.600442142126,30.6308486781643)) ;
#92677 = CARTESIAN_POINT('Ctrl Pts',(80.6436891658207,246.600297421838,30.6292287985663)) ;
#92678 = CARTESIAN_POINT('Ctrl Pts',(80.6417701542494,246.600134064326,30.6265722342026)) ;
#92679 = CARTESIAN_POINT('Ctrl Pts',(80.6412262678027,246.600088990182,30.6256529368887)) ;
#92680 = CARTESIAN_POINT('Ctrl Pts',(80.6404087807581,246.600022073172,30.6236520910468)) ;
#92681 = CARTESIAN_POINT('Ctrl Pts',(80.640133779087,246.600000000001,30.6225711229527)) ;
#92682 = CARTESIAN_POINT('Ctrl Pts',(80.640133779087,246.600000000001,30.6213203435596)) ;
#92683 = CARTESIAN_POINT('',(81.9668461709225,246.600000000001,30.6213203435596)) ;
#92684 = CARTESIAN_POINT('',(82.1755472374987,246.600000000001,30.6213203435596)) ;
#92685 = CARTESIAN_POINT('',(81.9668461709225,246.700000000001,30.7213203435596)) ;
#92686 = CARTESIAN_POINT('Origin',(81.9668461709225,246.700000000001,30.6213203435596)) ;
#92687 = CARTESIAN_POINT('',(82.1755472374987,246.700000000001,30.7213203435596)) ;
#92688 = CARTESIAN_POINT('Origin',(81.9668461709225,246.100000000001,30.6213203435596)) ;
#92689 = CARTESIAN_POINT('',(82.349868392482,246.421393804845,30.6213203435596)) ;
#92690 = CARTESIAN_POINT('',(82.4264728367939,246.485672565813,30.7213203435596)) ;
#92691 = CARTESIAN_POINT('Origin',(82.4264728367939,246.485672565813,30.6213203435596)) ;
#92692 = CARTESIAN_POINT('Origin',(81.9668461709225,246.100000000001,30.7213203435596)) ;
#92693 = CARTESIAN_POINT('Origin',(81.9668461709225,246.100000000001,30.6213203435596)) ;
#92694 = CARTESIAN_POINT('Origin',(82.2322613127596,246.717124847304,30.6213203435596)) ;
#92695 = CARTESIAN_POINT('',(82.2322613127596,246.717124847304,30.7213203435596)) ;
#92696 = CARTESIAN_POINT('',(82.1556568684477,246.652846086335,30.6213203435596)) ;
#92697 = CARTESIAN_POINT('Ctrl Pts',(83.9517583847478,244.512335651621,29.6213203435595)) ;
#92698 = CARTESIAN_POINT('Ctrl Pts',(83.9517583847478,244.512335651621,29.613840361051)) ;
#92699 = CARTESIAN_POINT('Ctrl Pts',(83.9530558516882,244.508154425815,29.5988871513645)) ;
#92700 = CARTESIAN_POINT('Ctrl Pts',(83.9606617048516,244.483643751566,29.5704781111071)) ;
#92701 = CARTESIAN_POINT('Ctrl Pts',(83.9826176510995,244.412888369528,29.5344326612966)) ;
#92702 = CARTESIAN_POINT('Ctrl Pts',(84.0111728319539,244.320866249065,29.5213203435597)) ;
#92703 = CARTESIAN_POINT('Ctrl Pts',(84.0283628290598,244.265469647218,29.5213203435596)) ;
#92704 = CARTESIAN_POINT('Ctrl Pts',(83.9667167316546,244.494508987956,29.6213203435595)) ;
#92705 = CARTESIAN_POINT('Ctrl Pts',(83.9667167316546,244.494508987956,29.6159323314173)) ;
#92706 = CARTESIAN_POINT('Ctrl Pts',(83.9682471994807,244.491531314103,29.6051243850722)) ;
#92707 = CARTESIAN_POINT('Ctrl Pts',(83.9770416840541,244.472839452493,29.5814625789605)) ;
#92708 = CARTESIAN_POINT('Ctrl Pts',(84.0006986135097,244.41106523898,29.5432109886374)) ;
#92709 = CARTESIAN_POINT('Ctrl Pts',(84.0277697425286,244.320862018183,29.5239057259475)) ;
#92710 = CARTESIAN_POINT('Ctrl Pts',(84.0433227940768,244.265469647218,29.5213203435596)) ;
#92711 = CARTESIAN_POINT('Ctrl Pts',(84.0041531339772,244.473067607354,29.6213203435595)) ;
#92712 = CARTESIAN_POINT('Ctrl Pts',(84.0041531339772,244.473067607354,29.6184142549133)) ;
#92713 = CARTESIAN_POINT('Ctrl Pts',(84.0057214037908,244.471884181008,29.6125402628528)) ;
#92714 = CARTESIAN_POINT('Ctrl Pts',(84.0144435090324,244.461429167618,29.5934423510192)) ;
#92715 = CARTESIAN_POINT('Ctrl Pts',(84.0362406374818,244.411135552903,29.549141027461)) ;
#92716 = CARTESIAN_POINT('Ctrl Pts',(84.0578024133386,244.321730700198,29.52105144863)) ;
#92717 = CARTESIAN_POINT('Ctrl Pts',(84.0694733069034,244.265469647218,29.515320264092)) ;
#92718 = CARTESIAN_POINT('Ctrl Pts',(84.0702660875844,244.47874053303,29.6213203435596)) ;
#92719 = CARTESIAN_POINT('Ctrl Pts',(84.0702660875844,244.47874053303,29.6177518125551)) ;
#92720 = CARTESIAN_POINT('Ctrl Pts',(84.0711700553681,244.478120540662,29.6105411574913)) ;
#92721 = CARTESIAN_POINT('Ctrl Pts',(84.0761457278699,244.469857764949,29.5866990606539)) ;
#92722 = CARTESIAN_POINT('Ctrl Pts',(84.0879165906551,244.419942996463,29.5315349805942)) ;
#92723 = CARTESIAN_POINT('Ctrl Pts',(84.0982144992168,244.325212271724,29.4977535048477)) ;
#92724 = CARTESIAN_POINT('Ctrl Pts',(84.1035282741147,244.265469647218,29.4911830285845)) ;
#92725 = CARTESIAN_POINT('Ctrl Pts',(84.1175427362197,244.518332038038,29.6213203435597)) ;
#92726 = CARTESIAN_POINT('Ctrl Pts',(84.1175427362197,244.518332038038,29.6131456262106)) ;
#92727 = CARTESIAN_POINT('Ctrl Pts',(84.1177289017234,244.51602318248,29.5967539236182)) ;
#92728 = CARTESIAN_POINT('Ctrl Pts',(84.1187237882151,244.499413268429,29.5589225324798)) ;
#92729 = CARTESIAN_POINT('Ctrl Pts',(84.1210267578767,244.43415692223,29.4947295211468)) ;
#92730 = CARTESIAN_POINT('Ctrl Pts',(84.1229625569563,244.329893500793,29.4628331350402)) ;
#92731 = CARTESIAN_POINT('Ctrl Pts',(84.1239346802222,244.265469647218,29.45873191021)) ;
#92732 = CARTESIAN_POINT('Ctrl Pts',(84.1283628290597,244.55916112007,29.6213203435597)) ;
#92733 = CARTESIAN_POINT('Ctrl Pts',(84.1283628290597,244.55916112007,29.6083780388064)) ;
#92734 = CARTESIAN_POINT('Ctrl Pts',(84.1283572386591,244.554786903413,29.5824972890339)) ;
#92735 = CARTESIAN_POINT('Ctrl Pts',(84.1283610044671,244.528130184705,29.5313432230903)) ;
#92736 = CARTESIAN_POINT('Ctrl Pts',(84.1283711082966,244.446079577053,29.4616562627835)) ;
#92737 = CARTESIAN_POINT('Ctrl Pts',(84.1283567558621,244.333673921744,29.433760966027)) ;
#92738 = CARTESIAN_POINT('Ctrl Pts',(84.1283628290597,244.265469647218,29.4325403173224)) ;
#92739 = CARTESIAN_POINT('Ctrl Pts',(84.1283628290597,244.57661441259,29.6213203435597)) ;
#92740 = CARTESIAN_POINT('Ctrl Pts',(84.1283628290597,244.57661441259,29.6063603785426)) ;
#92741 = CARTESIAN_POINT('Ctrl Pts',(84.1283628290597,244.571344482752,29.5764539591696)) ;
#92742 = CARTESIAN_POINT('Ctrl Pts',(84.1283628290597,244.54045173992,29.5196358786547)) ;
#92743 = CARTESIAN_POINT('Ctrl Pts',(84.1283628290597,244.451273131483,29.4475449790337)) ;
#92744 = CARTESIAN_POINT('Ctrl Pts',(84.1283628290597,244.335290369296,29.4213203435596)) ;
#92745 = CARTESIAN_POINT('Ctrl Pts',(84.1283628290597,244.265469647218,29.4213203435596)) ;
#92746 = CARTESIAN_POINT('',(83.9517583847478,244.512335651621,29.6213203435596)) ;
#92747 = CARTESIAN_POINT('Origin',(84.0283628290597,244.265469647218,29.6213203435596)) ;
#92748 = CARTESIAN_POINT('',(84.1283628290597,244.265469647218,29.4213203435596)) ;
#92749 = CARTESIAN_POINT('Origin',(84.0283628290597,244.265469647218,29.4213203435596)) ;
#92750 = CARTESIAN_POINT('',(84.1283628290597,244.57661441259,29.6213203435596)) ;
#92751 = CARTESIAN_POINT('Origin',(84.1283628290597,244.265469647218,29.6213203435596)) ;
#92752 = CARTESIAN_POINT('Origin',(84.0283628290597,244.57661441259,29.6213203435596)) ;
#92753 = CARTESIAN_POINT('Origin',(82.2,237.60736287746,29.4213203435596)) ;
#92754 = CARTESIAN_POINT('',(82.1222820569742,238.604338263983,29.4213203435596)) ;
#92755 = CARTESIAN_POINT('Origin',(82.2,237.60736287746,29.4213203435596)) ;
#92756 = CARTESIAN_POINT('Origin',(82.1145102626716,238.704035802635,29.4213203435596)) ;
#92757 = CARTESIAN_POINT('Ctrl Pts',(82.1833429126806,238.739454580319,29.5213203435596)) ;
#92758 = CARTESIAN_POINT('Ctrl Pts',(82.1563604922519,238.707298183835,29.5213203435596)) ;
#92759 = CARTESIAN_POINT('Ctrl Pts',(82.1145102626715,238.704035802636,29.5213203435597)) ;
#92760 = CARTESIAN_POINT('Ctrl Pts',(82.2599473569943,238.675175819352,29.5213203435603)) ;
#92761 = CARTESIAN_POINT('Ctrl Pts',(82.2059825161353,238.610863026382,29.5213203435603)) ;
#92762 = CARTESIAN_POINT('Ctrl Pts',(82.1222820569719,238.604338263983,29.5213203435605)) ;
#92763 = CARTESIAN_POINT('Ctrl Pts',(82.2599473569942,238.675175819352,29.4213203435594)) ;
#92764 = CARTESIAN_POINT('Ctrl Pts',(82.2059825161351,238.610863026382,29.4213203435594)) ;
#92765 = CARTESIAN_POINT('Ctrl Pts',(82.1222820569716,238.604338263983,29.4213203435596)) ;
#92766 = CARTESIAN_POINT('',(82.2599473569929,238.67517581935,29.4213203435596)) ;
#92767 = CARTESIAN_POINT('Origin',(82.183342912681,238.739454580319,29.4213203435596)) ;
#92768 = CARTESIAN_POINT('Origin',(82.106738468369,238.803733341288,29.4213203435596)) ;
#92769 = CARTESIAN_POINT('Origin',(77.9743376460485,233.723357432561,29.4213203435596)) ;
#92770 = CARTESIAN_POINT('',(84.0113850506191,240.762457982934,29.4213203435596)) ;
#92771 = CARTESIAN_POINT('Origin',(83.9347806063072,240.826736743903,29.4213203435596)) ;
#92772 = CARTESIAN_POINT('',(78.0509420903604,233.659078671593,29.4213203435596)) ;
#92773 = CARTESIAN_POINT('Origin',(83.6283628290597,241.083851787777,29.4213203435596)) ;
#92774 = CARTESIAN_POINT('',(84.1283628290596,241.083851787777,29.4213203435596)) ;
#92775 = CARTESIAN_POINT('Origin',(84.0283628290596,241.083851787777,29.4213203435596)) ;
#92776 = CARTESIAN_POINT('Origin',(83.6283628290597,241.083851787777,29.4213203435596)) ;
#92777 = CARTESIAN_POINT('Origin',(84.0283628290597,247.594124250979,29.4213203435596)) ;
#92778 = CARTESIAN_POINT('',(84.1283628290597,247.594124250979,29.4213203435596)) ;
#92779 = CARTESIAN_POINT('Origin',(84.0283628290597,244.57661441259,30.1213203435596)) ;
#92780 = CARTESIAN_POINT('',(84.1283628290597,244.57661441259,30.1213203435596)) ;
#92781 = CARTESIAN_POINT('',(83.9517583847478,244.512335651621,30.1213203435596)) ;
#92782 = CARTESIAN_POINT('Origin',(78.9611335727037,250.304358317977,29.6213203435596)) ;
#92783 = CARTESIAN_POINT('',(82.349868392482,246.421393804845,29.6213203435596)) ;
#92784 = CARTESIAN_POINT('Origin',(82.27326394817,246.357115043876,29.6213203435596)) ;
#92785 = CARTESIAN_POINT('',(79.0377380170156,250.368637078946,29.6213203435596)) ;
#92786 = CARTESIAN_POINT('Origin',(81.9668461709225,246.100000000001,29.6213203435596)) ;
#92787 = CARTESIAN_POINT('',(81.9668461709225,246.600000000001,29.6213203435596)) ;
#92788 = CARTESIAN_POINT('Origin',(81.9668461709225,246.500000000001,29.6213203435596)) ;
#92789 = CARTESIAN_POINT('Origin',(81.9668461709225,246.100000000001,29.6213203435596)) ;
#92790 = CARTESIAN_POINT('Origin',(68.5905137927262,246.500000000001,29.6213203435596)) ;
#92791 = CARTESIAN_POINT('',(80.6401337790902,246.600000000001,29.6213203435596)) ;
#92792 = CARTESIAN_POINT('Origin',(80.6401337790902,246.500000000001,29.6213203435596)) ;
#92793 = CARTESIAN_POINT('',(68.5905137927262,246.600000000001,29.6213203435596)) ;
#92794 = CARTESIAN_POINT('Ctrl Pts',(80.6401337790902,246.600000000001,29.6213203435597)) ;
#92795 = CARTESIAN_POINT('Ctrl Pts',(80.6401337790902,246.600000000001,29.6213203435597)) ;
#92796 = CARTESIAN_POINT('Ctrl Pts',(80.6401337790902,246.600000000001,29.6213203435597)) ;
#92797 = CARTESIAN_POINT('Ctrl Pts',(80.6401337790902,246.600000000001,29.6213203435597)) ;
#92798 = CARTESIAN_POINT('Ctrl Pts',(80.6401337790902,246.600000000001,29.6213203435597)) ;
#92799 = CARTESIAN_POINT('Ctrl Pts',(80.6401337790903,246.600000000001,29.5213203435596)) ;
#92800 = CARTESIAN_POINT('Ctrl Pts',(80.6401337790903,246.600000000001,29.5213203435596)) ;
#92801 = CARTESIAN_POINT('Ctrl Pts',(80.6401337790903,246.600000000001,29.5213203435596)) ;
#92802 = CARTESIAN_POINT('Ctrl Pts',(80.6401337790903,246.600000000001,29.5213203435596)) ;
#92803 = CARTESIAN_POINT('Ctrl Pts',(80.6401337790903,246.600000000001,29.5213203435596)) ;
#92804 = CARTESIAN_POINT('Ctrl Pts',(80.5401534070281,246.601981212341,29.5213203435596)) ;
#92805 = CARTESIAN_POINT('Ctrl Pts',(80.5393212408706,246.559986580887,29.5213203435596)) ;
#92806 = CARTESIAN_POINT('Ctrl Pts',(80.5687260721042,246.529993290444,29.5213203435596)) ;
#92807 = CARTESIAN_POINT('Ctrl Pts',(80.5981309033378,246.500000000001,29.5213203435596)) ;
#92808 = CARTESIAN_POINT('Ctrl Pts',(80.6401337790903,246.500000000001,29.5213203435596)) ;
#92809 = CARTESIAN_POINT('',(80.6401238113489,246.599999197424,29.6199061653688)) ;
#92810 = CARTESIAN_POINT('Ctrl Pts',(80.6401238113489,246.599999197424,29.6199061653688)) ;
#92811 = CARTESIAN_POINT('Ctrl Pts',(80.6400214277435,246.599990954774,29.6126436721215)) ;
#92812 = CARTESIAN_POINT('Ctrl Pts',(80.6391298693545,246.599917417426,29.6054249823856)) ;
#92813 = CARTESIAN_POINT('Ctrl Pts',(80.6374776063121,246.599793218341,29.5983912376924)) ;
#92814 = CARTESIAN_POINT('Ctrl Pts',(80.6360675394583,246.599687224918,29.5923885311043)) ;
#92815 = CARTESIAN_POINT('Ctrl Pts',(80.6341044490985,246.599544836505,29.5865185837269)) ;
#92816 = CARTESIAN_POINT('Ctrl Pts',(80.6316004329604,246.599386263502,29.5808495764825)) ;
#92817 = CARTESIAN_POINT('Ctrl Pts',(80.6277164645829,246.599140301617,29.5720564043727)) ;
#92818 = CARTESIAN_POINT('Ctrl Pts',(80.6225913378422,246.598858783748,29.563888015334)) ;
#92819 = CARTESIAN_POINT('Ctrl Pts',(80.6163938828428,246.59865549242,29.5565886095391)) ;
#92820 = CARTESIAN_POINT('Ctrl Pts',(80.6142499206385,246.598585165339,29.5540634358768)) ;
#92821 = CARTESIAN_POINT('Ctrl Pts',(80.611977402984,246.598524419104,29.5516418882813)) ;
#92822 = CARTESIAN_POINT('Ctrl Pts',(80.6095830539163,246.59847852032,29.5493338457366)) ;
#92823 = CARTESIAN_POINT('Ctrl Pts',(80.6024960843674,246.598342665743,29.5425023325488)) ;
#92824 = CARTESIAN_POINT('Ctrl Pts',(80.5944545576649,246.598341217034,29.5367728369097)) ;
#92825 = CARTESIAN_POINT('Ctrl Pts',(80.5857225147289,246.598590611719,29.5323072497772)) ;
#92826 = CARTESIAN_POINT('Ctrl Pts',(80.5830669391223,246.598666457252,29.5309491822156)) ;
#92827 = CARTESIAN_POINT('Ctrl Pts',(80.5803476365109,246.598765322088,29.5297081953568)) ;
#92828 = CARTESIAN_POINT('Ctrl Pts',(80.5775730890624,246.598889896522,29.5285893595314)) ;
#92829 = CARTESIAN_POINT('Ctrl Pts',(80.570390042797,246.599212408188,29.5256927972462)) ;
#92830 = CARTESIAN_POINT('Ctrl Pts',(80.5629312514651,246.599704883803,29.5236511049122)) ;
#92831 = CARTESIAN_POINT('Ctrl Pts',(80.5553357905141,246.600386015029,29.5224824684264)) ;
#92832 = CARTESIAN_POINT('Ctrl Pts',(80.5503172535888,246.600836057789,29.5217103170858)) ;
#92833 = CARTESIAN_POINT('Ctrl Pts',(80.5452392666734,246.601368061613,29.5213203435596)) ;
#92834 = CARTESIAN_POINT('Ctrl Pts',(80.5401534070282,246.601981212341,29.5213203435596)) ;
#92835 = CARTESIAN_POINT('Ctrl Pts',(80.6401337790902,246.600000000001,29.6213203435596)) ;
#92836 = CARTESIAN_POINT('Ctrl Pts',(80.6401337790902,246.600000000001,29.6208503040069)) ;
#92837 = CARTESIAN_POINT('Ctrl Pts',(80.6401304771049,246.599999716412,29.6203788915336)) ;
#92838 = CARTESIAN_POINT('Ctrl Pts',(80.6401238157683,246.599999144307,29.6199061653688)) ;
#92839 = CARTESIAN_POINT('Origin',(82.384248304075,250.850933335322,30.7213203435596)) ;
#92840 = CARTESIAN_POINT('',(81.1,247.600000000001,30.7213203435596)) ;
#92841 = CARTESIAN_POINT('',(81.9668461709226,247.600000000001,30.7213203435596)) ;
#92842 = CARTESIAN_POINT('',(81.1,247.098386676966,30.7213203435596)) ;
#92843 = CARTESIAN_POINT('',(81.1,257.151471862576,30.7213203435596)) ;
#92844 = CARTESIAN_POINT('Origin',(80.6,247.098386676966,30.7213203435596)) ;
#92845 = CARTESIAN_POINT('Origin',(79.2,263.8,29.5213203435596)) ;
#92846 = CARTESIAN_POINT('',(79.2,259.648528137424,20.1213203435596)) ;
#92847 = CARTESIAN_POINT('',(79.2,259.648528137424,29.5213203435596)) ;
#92848 = CARTESIAN_POINT('',(79.2,261.751937515251,20.1213203435596)) ;
#92849 = CARTESIAN_POINT('',(79.2,252.258305665508,20.1213203435596)) ;
#92850 = CARTESIAN_POINT('',(79.2,263.412347523777,22.196832854217)) ;
#92851 = CARTESIAN_POINT('',(79.2,264.929230192226,24.0929361897785)) ;
#92852 = CARTESIAN_POINT('Origin',(79.2,263.1,22.4467108732387)) ;
#92853 = CARTESIAN_POINT('Origin',(79.7999999999999,259.648528137424,29.5213203435596)) ;
#92854 = CARTESIAN_POINT('',(79.3757359312881,259.224264068712,20.1213203435596)) ;
#92855 = CARTESIAN_POINT('',(79.3757359312881,259.224264068712,29.5213203435596)) ;
#92856 = CARTESIAN_POINT('Origin',(79.7999999999999,259.648528137424,20.1213203435596)) ;
#92857 = CARTESIAN_POINT('Origin',(79.3757359312881,259.224264068712,29.5213203435596)) ;
#92858 = CARTESIAN_POINT('',(83.8354696102463,254.764530389755,20.1213203435596)) ;
#92859 = CARTESIAN_POINT('',(83.8354696102463,254.764530389755,29.5213203435596)) ;
#92860 = CARTESIAN_POINT('',(77.9622604865213,260.637739513478,20.1213203435596)) ;
#92861 = CARTESIAN_POINT('Origin',(83.1283628290598,254.057423608568,29.5213203435596)) ;
#92862 = CARTESIAN_POINT('',(84.1283628290598,254.057423608568,20.1213203435596)) ;
#92863 = CARTESIAN_POINT('',(84.1283628290598,254.057423608568,29.5213203435596)) ;
#92864 = CARTESIAN_POINT('Origin',(83.1283628290598,254.057423608568,20.1213203435596)) ;
#92865 = CARTESIAN_POINT('Origin',(84.1283628290598,254.471637170941,29.5213203435596)) ;
#92866 = CARTESIAN_POINT('',(84.1283628290596,241.083851787777,17.0213468614911)) ;
#92867 = CARTESIAN_POINT('',(84.1283628290596,241.083851787777,29.5213203435596)) ;
#92868 = CARTESIAN_POINT('',(84.1283628290597,244.252914644012,18.0777011469026)) ;
#92869 = CARTESIAN_POINT('',(84.1283628290597,249.125613950322,19.7019342490059)) ;
#92870 = CARTESIAN_POINT('',(84.1283628290597,244.521708245126,18.1213203435596)) ;
#92871 = CARTESIAN_POINT('Origin',(84.1283628290597,244.521708245126,17.2713203435596)) ;
#92872 = CARTESIAN_POINT('',(84.1283628290597,250.68933982822,18.1213203435596)) ;
#92873 = CARTESIAN_POINT('',(84.1283628290598,251.76081858547,18.1213203435596)) ;
#92874 = CARTESIAN_POINT('',(84.1283628290597,251.148959235991,18.3117009357884)) ;
#92875 = CARTESIAN_POINT('Origin',(84.1283628290597,250.68933982822,18.7713203435596)) ;
#92876 = CARTESIAN_POINT('',(84.1283628290598,252.782842712475,19.9455844122716)) ;
#92877 = CARTESIAN_POINT('',(84.1283628290598,255.172198614617,22.3349403144135)) ;
#92878 = CARTESIAN_POINT('',(84.1283628290598,253.207106781187,20.1213203435596)) ;
#92879 = CARTESIAN_POINT('Origin',(84.1283628290598,253.207106781187,19.5213203435596)) ;
#92880 = CARTESIAN_POINT('',(84.1283628290597,247.594124250979,20.1213203435596)) ;
#92881 = CARTESIAN_POINT('Origin',(83.6283628290597,241.083851787777,29.5213203435596)) ;
#92882 = CARTESIAN_POINT('',(84.0113850506191,240.762457982934,16.9356418468662)) ;
#92883 = CARTESIAN_POINT('',(84.0113850506191,240.762457982934,29.5213203435596)) ;
#92884 = CARTESIAN_POINT('Origin',(83.6283628290597,241.083851787777,17.0213468614911)) ;
#92885 = CARTESIAN_POINT('Origin',(84.0113850506191,240.762457982934,29.5213203435596)) ;
#92886 = CARTESIAN_POINT('',(82.2599473569929,238.67517581935,16.2398811256715)) ;
#92887 = CARTESIAN_POINT('',(82.2599473569929,238.67517581935,29.5213203435596)) ;
#92888 = CARTESIAN_POINT('',(82.1162867009651,238.503967716415,16.1828117580263)) ;
#92889 = CARTESIAN_POINT('Origin',(82.106738468369,238.803733341288,29.5213203435596)) ;
#92890 = CARTESIAN_POINT('',(82.1222820569742,238.604338263983,16.2280748664436)) ;
#92891 = CARTESIAN_POINT('',(82.1222820569742,238.604338263983,29.5213203435596)) ;
#92892 = CARTESIAN_POINT('Origin',(82.106738468369,238.803733341288,16.2613073793278)) ;
#92893 = CARTESIAN_POINT('Origin',(82.2,237.60736287746,29.5213203435596)) ;
#92894 = CARTESIAN_POINT('',(81.4075488173165,238.217298220807,16.1213203435596)) ;
#92895 = CARTESIAN_POINT('Origin',(82.2,237.60736287746,16.1213203435596)) ;
#92896 = CARTESIAN_POINT('',(81.5957531842379,238.404160082301,16.1546761998268)) ;
#92897 = CARTESIAN_POINT('Ctrl Pts',(81.5957531842379,238.404160082301,16.1546761998268)) ;
#92898 = CARTESIAN_POINT('Ctrl Pts',(81.5259305404763,238.351210461111,16.135261338724)) ;
#92899 = CARTESIAN_POINT('Ctrl Pts',(81.4620702891285,238.288134589433,16.1213203435918)) ;
#92900 = CARTESIAN_POINT('Ctrl Pts',(81.4075488173165,238.217298220807,16.1213203435596)) ;
#92901 = CARTESIAN_POINT('Origin',(82.2,237.60736287746,15.8625172247187)) ;
#92902 = CARTESIAN_POINT('Ctrl Pts',(34.7,253.1,20.1116830603904)) ;
#92903 = CARTESIAN_POINT('Ctrl Pts',(34.7,253.073427194197,20.102041097524)) ;
#92904 = CARTESIAN_POINT('Ctrl Pts',(34.7154525608087,253.037274993038,20.0767697983353)) ;
#92905 = CARTESIAN_POINT('Ctrl Pts',(34.7577940821299,253.006604388018,20.0446943852455)) ;
#92906 = CARTESIAN_POINT('Ctrl Pts',(34.7845676632082,253.,20.0367671642397)) ;
#92907 = CARTESIAN_POINT('Ctrl Pts',(34.8,253.,20.0367671642397)) ;
#92908 = CARTESIAN_POINT('Ctrl Pts',(34.7,253.105341045666,20.0822437084198)) ;
#92909 = CARTESIAN_POINT('Ctrl Pts',(34.6985373524762,253.081350046773,20.0739929287702)) ;
#92910 = CARTESIAN_POINT('Ctrl Pts',(34.7093726656571,253.044545930682,20.0527380915968)) ;
#92911 = CARTESIAN_POINT('Ctrl Pts',(34.752901551485,253.008047944834,20.0242500678859)) ;
#92912 = CARTESIAN_POINT('Ctrl Pts',(34.7827658172387,253.,20.0170821036701)) ;
#92913 = CARTESIAN_POINT('Ctrl Pts',(34.8,253.,20.0170821036701)) ;
#92914 = CARTESIAN_POINT('Ctrl Pts',(34.6748678850179,253.11458383057,20.0312983289888)) ;
#92915 = CARTESIAN_POINT('Ctrl Pts',(34.6726125261121,253.088119687564,20.0253228616253)) ;
#92916 = CARTESIAN_POINT('Ctrl Pts',(34.6847726429031,253.044720925911,20.0108918141144)) ;
#92917 = CARTESIAN_POINT('Ctrl Pts',(34.7400669620698,252.999455928905,19.988446023804)) ;
#92918 = CARTESIAN_POINT('Ctrl Pts',(34.7779762508729,252.989510818984,19.982705579958)) ;
#92919 = CARTESIAN_POINT('Ctrl Pts',(34.8,252.989510818984,19.982705579958)) ;
#92920 = CARTESIAN_POINT('Ctrl Pts',(34.6224399475256,253.117851130198,20.013289274252)) ;
#92921 = CARTESIAN_POINT('Ctrl Pts',(34.6217681694945,253.0793292346,20.0063128558354)) ;
#92922 = CARTESIAN_POINT('Ctrl Pts',(34.64705596785,253.024324397392,19.9886074342206)) ;
#92923 = CARTESIAN_POINT('Ctrl Pts',(34.7229377514464,252.974645254944,19.9645026828736)) ;
#92924 = CARTESIAN_POINT('Ctrl Pts',(34.7717862253283,252.963867715888,19.9584161302793)) ;
#92925 = CARTESIAN_POINT('Ctrl Pts',(34.8,252.963867715888,19.9584161302793)) ;
#92926 = CARTESIAN_POINT('Ctrl Pts',(34.6,253.117851130198,20.013289274252)) ;
#92927 = CARTESIAN_POINT('Ctrl Pts',(34.6,253.073563120525,20.0052543051966)) ;
#92928 = CARTESIAN_POINT('Ctrl Pts',(34.6309051216174,253.013309451927,19.984194889206)) ;
#92929 = CARTESIAN_POINT('Ctrl Pts',(34.7155881642597,252.962191776895,19.9574653782978)) ;
#92930 = CARTESIAN_POINT('Ctrl Pts',(34.7691353264163,252.951184463531,19.950859360793)) ;
#92931 = CARTESIAN_POINT('Ctrl Pts',(34.8,252.951184463531,19.950859360793)) ;
#92932 = CARTESIAN_POINT('',(34.7,253.1,20.1116830603904)) ;
#92933 = CARTESIAN_POINT('',(34.6,253.117851130198,20.013289274252)) ;
#92934 = CARTESIAN_POINT('Origin',(34.6,253.1,20.1116830603904)) ;
#92935 = CARTESIAN_POINT('',(34.8,253.,20.0367671642397)) ;
#92936 = CARTESIAN_POINT('Ctrl Pts',(34.7,253.1,20.1116830603904)) ;
#92937 = CARTESIAN_POINT('Ctrl Pts',(34.7,253.090812284823,20.1083492909262)) ;
#92938 = CARTESIAN_POINT('Ctrl Pts',(34.7012689280364,253.081748379892,20.104053410188)) ;
#92939 = CARTESIAN_POINT('Ctrl Pts',(34.7036906162496,253.073083414005,20.0991758790423)) ;
#92940 = CARTESIAN_POINT('Ctrl Pts',(34.7063605193339,253.06353031835,20.0937984174113)) ;
#92941 = CARTESIAN_POINT('Ctrl Pts',(34.7104314447552,253.054461536474,20.087713960402)) ;
#92942 = CARTESIAN_POINT('Ctrl Pts',(34.715711247738,253.046191020804,20.0814323572824)) ;
#92943 = CARTESIAN_POINT('Ctrl Pts',(34.7194931489978,253.040266884291,20.0769328706863)) ;
#92944 = CARTESIAN_POINT('Ctrl Pts',(34.723894682151,253.034751119387,20.0723322323984)) ;
#92945 = CARTESIAN_POINT('Ctrl Pts',(34.7288341851766,253.029747407162,20.0678178206808)) ;
#92946 = CARTESIAN_POINT('Ctrl Pts',(34.735485753755,253.023009374036,20.0617386829671)) ;
#92947 = CARTESIAN_POINT('Ctrl Pts',(34.7431037307269,253.017203083895,20.0558159042037)) ;
#92948 = CARTESIAN_POINT('Ctrl Pts',(34.7515160670353,253.012539676171,20.0508560690148)) ;
#92949 = CARTESIAN_POINT('Ctrl Pts',(34.7529089921345,253.011767503325,20.0500348133411)) ;
#92950 = CARTESIAN_POINT('Ctrl Pts',(34.7543236613454,253.011026776857,20.0492399588338)) ;
#92951 = CARTESIAN_POINT('Ctrl Pts',(34.7557592220037,253.010318599686,20.0484751671979)) ;
#92952 = CARTESIAN_POINT('Ctrl Pts',(34.7618259802646,253.007325804029,20.0452431157008)) ;
#92953 = CARTESIAN_POINT('Ctrl Pts',(34.7682623077884,253.004920839274,20.0425479732772)) ;
#92954 = CARTESIAN_POINT('Ctrl Pts',(34.7749219946318,253.003195590768,20.0405614926115)) ;
#92955 = CARTESIAN_POINT('Ctrl Pts',(34.7815569385043,253.001476752139,20.038582392388)) ;
#92956 = CARTESIAN_POINT('Ctrl Pts',(34.7884125679264,253.000433128784,20.0373066978724)) ;
#92957 = CARTESIAN_POINT('Ctrl Pts',(34.795320947479,253.000109527644,20.0369042544962)) ;
#92958 = CARTESIAN_POINT('Ctrl Pts',(34.7968786750153,253.000036560836,20.0368135100424)) ;
#92959 = CARTESIAN_POINT('Ctrl Pts',(34.7984390268306,253.,20.0367671642397)) ;
#92960 = CARTESIAN_POINT('Ctrl Pts',(34.8,253.,20.0367671642397)) ;
#92961 = CARTESIAN_POINT('',(34.8,252.951184463531,19.950859360793)) ;
#92962 = CARTESIAN_POINT('Origin',(34.8,252.9,20.0367671642397)) ;
#92963 = CARTESIAN_POINT('Ctrl Pts',(34.8,252.951184463531,19.950859360793)) ;
#92964 = CARTESIAN_POINT('Ctrl Pts',(34.7691353264163,252.951184463531,19.950859360793)) ;
#92965 = CARTESIAN_POINT('Ctrl Pts',(34.7155881642597,252.962191776895,19.9574653782978)) ;
#92966 = CARTESIAN_POINT('Ctrl Pts',(34.6309051216174,253.013309451927,19.984194889206)) ;
#92967 = CARTESIAN_POINT('Ctrl Pts',(34.6,253.073563120525,20.0052543051966)) ;
#92968 = CARTESIAN_POINT('Ctrl Pts',(34.6,253.117851130198,20.013289274252)) ;
#92969 = CARTESIAN_POINT('Origin',(34.8,253.1,20.0213203435596)) ;
#92970 = CARTESIAN_POINT('',(34.8,253.,25.7213203435596)) ;
#92971 = CARTESIAN_POINT('',(34.7,253.1,25.7213203435596)) ;
#92972 = CARTESIAN_POINT('Origin',(34.8,253.1,25.7213203435596)) ;
#92973 = CARTESIAN_POINT('',(34.8,253.,20.0213203435596)) ;
#92974 = CARTESIAN_POINT('',(34.7,253.1,20.0213203435596)) ;
#92975 = CARTESIAN_POINT('Origin',(34.8,258.9,20.1213203435596)) ;
#92976 = CARTESIAN_POINT('',(34.7,258.9,20.1213203435596)) ;
#92977 = CARTESIAN_POINT('',(34.8,259.,20.1213203435596)) ;
#92978 = CARTESIAN_POINT('Origin',(34.8,258.9,20.1213203435596)) ;
#92979 = CARTESIAN_POINT('',(34.6,258.9,20.0213203435596)) ;
#92980 = CARTESIAN_POINT('Origin',(34.6,258.9,20.1213203435596)) ;
#92981 = CARTESIAN_POINT('',(34.8,259.1,20.0213203435596)) ;
#92982 = CARTESIAN_POINT('Origin',(34.8,258.9,20.0213203435596)) ;
#92983 = CARTESIAN_POINT('Origin',(34.8,259.1,20.1213203435596)) ;
#92984 = CARTESIAN_POINT('Origin',(34.6,249.858305665508,20.1213203435596)) ;
#92985 = CARTESIAN_POINT('',(34.7,253.207106781187,20.1213203435596)) ;
#92986 = CARTESIAN_POINT('',(34.6,253.207106781187,20.0213203435596)) ;
#92987 = CARTESIAN_POINT('Origin',(34.6,253.207106781187,20.1213203435596)) ;
#92988 = CARTESIAN_POINT('',(34.6,249.858305665508,20.0213203435596)) ;
#92989 = CARTESIAN_POINT('',(34.7,249.858305665508,20.1213203435596)) ;
#92990 = CARTESIAN_POINT('Origin',(34.6,253.207106781187,19.5213203435596)) ;
#92991 = CARTESIAN_POINT('Origin',(34.7,253.207106781187,19.5213203435596)) ;
#92992 = CARTESIAN_POINT('Origin',(34.6,253.207106781187,19.5213203435596)) ;
#92993 = CARTESIAN_POINT('Origin',(45.6,258.9,20.1213203435596)) ;
#92994 = CARTESIAN_POINT('',(45.6,259.1,20.0213203435596)) ;
#92995 = CARTESIAN_POINT('',(45.8,258.9,20.0213203435596)) ;
#92996 = CARTESIAN_POINT('Origin',(45.6,258.9,20.0213203435596)) ;
#92997 = CARTESIAN_POINT('',(45.7,258.9,20.1213203435596)) ;
#92998 = CARTESIAN_POINT('Origin',(45.8,258.9,20.1213203435596)) ;
#92999 = CARTESIAN_POINT('',(45.6,259.,20.1213203435596)) ;
#93000 = CARTESIAN_POINT('Origin',(45.6,258.9,20.1213203435596)) ;
#93001 = CARTESIAN_POINT('Origin',(45.6,259.1,20.1213203435596)) ;
#93002 = CARTESIAN_POINT('Ctrl Pts',(45.6,253.,20.0367671642397)) ;
#93003 = CARTESIAN_POINT('Ctrl Pts',(45.6154322006349,253.,20.0367671642397)) ;
#93004 = CARTESIAN_POINT('Ctrl Pts',(45.6422059127972,253.006604965661,20.0446949534528)) ;
#93005 = CARTESIAN_POINT('Ctrl Pts',(45.6845468602172,253.037276279324,20.0767704565364)) ;
#93006 = CARTESIAN_POINT('Ctrl Pts',(45.7,253.073427428644,20.1020411825935)) ;
#93007 = CARTESIAN_POINT('Ctrl Pts',(45.7,253.1,20.1116830603905)) ;
#93008 = CARTESIAN_POINT('Ctrl Pts',(45.6,253.,20.0170821036701)) ;
#93009 = CARTESIAN_POINT('Ctrl Pts',(45.617234030707,253.,20.0170821036701)) ;
#93010 = CARTESIAN_POINT('Ctrl Pts',(45.6470983872308,253.008048616484,20.0242505760926)) ;
#93011 = CARTESIAN_POINT('Ctrl Pts',(45.6906265314711,253.044547162949,20.0527386488428)) ;
#93012 = CARTESIAN_POINT('Ctrl Pts',(45.7014626346191,253.081350258442,20.0739930015655)) ;
#93013 = CARTESIAN_POINT('Ctrl Pts',(45.7,253.105341045666,20.0822437084198)) ;
#93014 = CARTESIAN_POINT('Ctrl Pts',(45.6,252.989510790392,19.9827055984603)) ;
#93015 = CARTESIAN_POINT('Ctrl Pts',(45.6220235548152,252.989510790392,19.9827055984603)) ;
#93016 = CARTESIAN_POINT('Ctrl Pts',(45.6599330014319,252.99945672555,19.988446495824)) ;
#93017 = CARTESIAN_POINT('Ctrl Pts',(45.7152263354696,253.044722306011,20.0108922593322)) ;
#93018 = CARTESIAN_POINT('Ctrl Pts',(45.7273875638952,253.088119897512,20.0253230440994)) ;
#93019 = CARTESIAN_POINT('Ctrl Pts',(45.7251322248881,253.114583807029,20.0312984587423)) ;
#93020 = CARTESIAN_POINT('Ctrl Pts',(45.6,252.963867715888,19.9584161302793)) ;
#93021 = CARTESIAN_POINT('Ctrl Pts',(45.6282135257462,252.963867715888,19.9584161302793)) ;
#93022 = CARTESIAN_POINT('Ctrl Pts',(45.6770622165507,252.974646180414,19.9645031139485)) ;
#93023 = CARTESIAN_POINT('Ctrl Pts',(45.7529429049027,253.024326306312,19.9886079012294)) ;
#93024 = CARTESIAN_POINT('Ctrl Pts',(45.7782318245786,253.079329574472,20.0063129173872)) ;
#93025 = CARTESIAN_POINT('Ctrl Pts',(45.7775600524744,253.117851130198,20.013289274252)) ;
#93026 = CARTESIAN_POINT('Ctrl Pts',(45.6,252.951184463531,19.950859360793)) ;
#93027 = CARTESIAN_POINT('Ctrl Pts',(45.6308644012698,252.951184463531,19.950859360793)) ;
#93028 = CARTESIAN_POINT('Ctrl Pts',(45.6844118255944,252.962192739633,19.9574658518039)) ;
#93029 = CARTESIAN_POINT('Ctrl Pts',(45.7690937204345,253.013311595737,19.9841954377069)) ;
#93030 = CARTESIAN_POINT('Ctrl Pts',(45.8,253.073563511271,20.0052543760878)) ;
#93031 = CARTESIAN_POINT('Ctrl Pts',(45.8,253.117851130198,20.013289274252)) ;
#93032 = CARTESIAN_POINT('',(45.7,253.1,20.1116830603904)) ;
#93033 = CARTESIAN_POINT('',(45.6,253.,20.0367671642397)) ;
#93034 = CARTESIAN_POINT('Ctrl Pts',(45.6,253.,20.0367671642397)) ;
#93035 = CARTESIAN_POINT('Ctrl Pts',(45.606919815088,253.,20.0367671642397)) ;
#93036 = CARTESIAN_POINT('Ctrl Pts',(45.6138266569514,253.000722532008,20.0376780151623)) ;
#93037 = CARTESIAN_POINT('Ctrl Pts',(45.6205496933934,253.002134224054,20.0393300400749)) ;
#93038 = CARTESIAN_POINT('Ctrl Pts',(45.6272994466678,253.003551526057,20.0409886300082)) ;
#93039 = CARTESIAN_POINT('Ctrl Pts',(45.6338628594197,253.005663017448,20.0433942963737)) ;
#93040 = CARTESIAN_POINT('Ctrl Pts',(45.6400871492553,253.008386570501,20.0463753313402)) ;
#93041 = CARTESIAN_POINT('Ctrl Pts',(45.641489340038,253.009000124993,20.0470468906447)) ;
#93042 = CARTESIAN_POINT('Ctrl Pts',(45.6428744364713,253.009644566497,20.0477476498085)) ;
#93043 = CARTESIAN_POINT('Ctrl Pts',(45.6442409123064,253.010318665943,20.0484756457334)) ;
#93044 = CARTESIAN_POINT('Ctrl Pts',(45.6529108343034,253.014595645794,20.0530945842625)) ;
#93045 = CARTESIAN_POINT('Ctrl Pts',(45.6608165325297,253.020055382737,20.0588099553703)) ;
#93046 = CARTESIAN_POINT('Ctrl Pts',(45.6677833517525,253.026478457407,20.064815193976)) ;
#93047 = CARTESIAN_POINT('Ctrl Pts',(45.6689369098378,253.027541982882,20.0658095346251)) ;
#93048 = CARTESIAN_POINT('Ctrl Pts',(45.6700647610495,253.028632030776,20.0668118223869)) ;
#93049 = CARTESIAN_POINT('Ctrl Pts',(45.6711661258947,253.029747722278,20.0678183958023)) ;
#93050 = CARTESIAN_POINT('Ctrl Pts',(45.6781502406968,253.036822687096,20.0742014071367)) ;
#93051 = CARTESIAN_POINT('Ctrl Pts',(45.6840571677146,253.044922670849,20.0807567550162)) ;
#93052 = CARTESIAN_POINT('Ctrl Pts',(45.6886617904446,253.053749736053,20.0869548126948)) ;
#93053 = CARTESIAN_POINT('Ctrl Pts',(45.6928454521279,253.061769818617,20.0925862352763)) ;
#93054 = CARTESIAN_POINT('Ctrl Pts',(45.6959545781961,253.070390688776,20.0979227094103)) ;
#93055 = CARTESIAN_POINT('Ctrl Pts',(45.6978463585031,253.079358049325,20.1025669910274)) ;
#93056 = CARTESIAN_POINT('Ctrl Pts',(45.6992655848671,253.086085423777,20.1060511624654)) ;
#93057 = CARTESIAN_POINT('Ctrl Pts',(45.7,253.09300731944,20.1091457609123)) ;
#93058 = CARTESIAN_POINT('Ctrl Pts',(45.7,253.1,20.1116830603905)) ;
#93059 = CARTESIAN_POINT('',(45.8,253.117851130198,20.013289274252)) ;
#93060 = CARTESIAN_POINT('Origin',(45.8,253.1,20.1116830603904)) ;
#93061 = CARTESIAN_POINT('',(45.6,252.951184463531,19.950859360793)) ;
#93062 = CARTESIAN_POINT('Ctrl Pts',(45.8,253.117851130198,20.013289274252)) ;
#93063 = CARTESIAN_POINT('Ctrl Pts',(45.8,253.073563511271,20.0052543760878)) ;
#93064 = CARTESIAN_POINT('Ctrl Pts',(45.7690937204345,253.013311595737,19.9841954377069)) ;
#93065 = CARTESIAN_POINT('Ctrl Pts',(45.6844118255944,252.962192739633,19.9574658518039)) ;
#93066 = CARTESIAN_POINT('Ctrl Pts',(45.6308644012698,252.951184463531,19.950859360793)) ;
#93067 = CARTESIAN_POINT('Ctrl Pts',(45.6,252.951184463531,19.950859360793)) ;
#93068 = CARTESIAN_POINT('Origin',(45.6,252.9,20.0367671642397)) ;
#93069 = CARTESIAN_POINT('Origin',(45.8,253.207106781187,19.5213203435596)) ;
#93070 = CARTESIAN_POINT('',(45.7,253.207106781187,20.1213203435596)) ;
#93071 = CARTESIAN_POINT('',(45.8,253.207106781187,20.0213203435596)) ;
#93072 = CARTESIAN_POINT('Origin',(45.8,253.207106781187,20.1213203435596)) ;
#93073 = CARTESIAN_POINT('Origin',(45.8,253.207106781187,19.5213203435596)) ;
#93074 = CARTESIAN_POINT('Origin',(45.7,253.207106781187,19.5213203435596)) ;
#93075 = CARTESIAN_POINT('Origin',(45.8,246.858305665508,20.1213203435596)) ;
#93076 = CARTESIAN_POINT('',(45.8,246.858305665508,20.0213203435596)) ;
#93077 = CARTESIAN_POINT('',(45.7,246.858305665508,20.1213203435596)) ;
#93078 = CARTESIAN_POINT('Origin',(52.2356360608974,252.9,20.0367671642397)) ;
#93079 = CARTESIAN_POINT('',(43.7,252.951184463531,19.950859360793)) ;
#93080 = CARTESIAN_POINT('',(43.7,253.,20.0367671642397)) ;
#93081 = CARTESIAN_POINT('Origin',(43.7,252.9,20.0367671642397)) ;
#93082 = CARTESIAN_POINT('',(52.2356360608974,253.,20.0367671642397)) ;
#93083 = CARTESIAN_POINT('',(52.2356360608974,252.951184463531,19.950859360793)) ;
#93084 = CARTESIAN_POINT('Ctrl Pts',(43.7,252.951184463531,19.950859360793)) ;
#93085 = CARTESIAN_POINT('Ctrl Pts',(43.6578667992531,252.951184463531,19.950859360793)) ;
#93086 = CARTESIAN_POINT('Ctrl Pts',(43.5592720148238,252.933167716983,19.9409614991614)) ;
#93087 = CARTESIAN_POINT('Ctrl Pts',(43.4889885639036,252.88263705024,19.9039573937935)) ;
#93088 = CARTESIAN_POINT('Ctrl Pts',(43.4621585770309,252.853553390627,19.874873734187)) ;
#93089 = CARTESIAN_POINT('Ctrl Pts',(43.7,252.968095466674,19.9609350534414)) ;
#93090 = CARTESIAN_POINT('Ctrl Pts',(43.6546460334317,252.968095466674,19.9609350534414)) ;
#93091 = CARTESIAN_POINT('Ctrl Pts',(43.5485580847433,252.947930175755,19.9508675198836)) ;
#93092 = CARTESIAN_POINT('Ctrl Pts',(43.4726905198964,252.892278257511,19.9124287196735)) ;
#93093 = CARTESIAN_POINT('Ctrl Pts',(43.4433278943641,252.860791518147,19.8821118617056)) ;
#93094 = CARTESIAN_POINT('Ctrl Pts',(43.7,252.992258727451,19.987541529862)) ;
#93095 = CARTESIAN_POINT('Ctrl Pts',(43.6490293347725,252.992258727451,19.987541529862)) ;
#93096 = CARTESIAN_POINT('Ctrl Pts',(43.5298499627169,252.968039915603,19.9768771591682)) ;
#93097 = CARTESIAN_POINT('Ctrl Pts',(43.4442147468097,252.9018819301,19.9359235128061)) ;
#93098 = CARTESIAN_POINT('Ctrl Pts',(43.4104713759891,252.864580433427,19.9035816876055)) ;
#93099 = CARTESIAN_POINT('Ctrl Pts',(43.7,253.,20.0220033688125)) ;
#93100 = CARTESIAN_POINT('Ctrl Pts',(43.6450557170687,253.,20.0220033688125)) ;
#93101 = CARTESIAN_POINT('Ctrl Pts',(43.5165377588455,252.972371460923,20.0104893451526)) ;
#93102 = CARTESIAN_POINT('Ctrl Pts',(43.4245875894081,252.895637337396,19.9671199842894)) ;
#93103 = CARTESIAN_POINT('Ctrl Pts',(43.3889646181901,252.851707610128,19.9329880225427)) ;
#93104 = CARTESIAN_POINT('Ctrl Pts',(43.7,253.,20.0367671642397)) ;
#93105 = CARTESIAN_POINT('Ctrl Pts',(43.6438223990041,253.,20.0367671642397)) ;
#93106 = CARTESIAN_POINT('Ctrl Pts',(43.5123626864317,252.971173205522,20.0248897302817)) ;
#93107 = CARTESIAN_POINT('Ctrl Pts',(43.4186514185382,252.890324138733,19.9804848038403)) ;
#93108 = CARTESIAN_POINT('Ctrl Pts',(43.3828781027079,252.843790283354,19.9455844123125)) ;
#93109 = CARTESIAN_POINT('',(43.3828781027079,252.843790283354,19.9455844123125)) ;
#93110 = CARTESIAN_POINT('Origin',(43.4621585770309,252.782842712516,19.9455844123125)) ;
#93111 = CARTESIAN_POINT('Ctrl Pts',(43.3828781027079,252.843790283354,19.9455844123125)) ;
#93112 = CARTESIAN_POINT('Ctrl Pts',(43.4186514185382,252.890324138733,19.9804848038403)) ;
#93113 = CARTESIAN_POINT('Ctrl Pts',(43.5123626864317,252.971173205522,20.0248897302817)) ;
#93114 = CARTESIAN_POINT('Ctrl Pts',(43.6438223990041,253.,20.0367671642397)) ;
#93115 = CARTESIAN_POINT('Ctrl Pts',(43.7,253.,20.0367671642397)) ;
#93116 = CARTESIAN_POINT('Ctrl Pts',(43.7,252.951184463531,19.950859360793)) ;
#93117 = CARTESIAN_POINT('Ctrl Pts',(43.6578667992531,252.951184463531,19.950859360793)) ;
#93118 = CARTESIAN_POINT('Ctrl Pts',(43.5592720148238,252.933167716983,19.9409614991614)) ;
#93119 = CARTESIAN_POINT('Ctrl Pts',(43.4889885639036,252.88263705024,19.9039573937935)) ;
#93120 = CARTESIAN_POINT('Ctrl Pts',(43.4621585770309,252.853553390627,19.874873734187)) ;
#93121 = CARTESIAN_POINT('Ctrl Pts',(43.4624808583665,252.853781762386,19.8751022254159)) ;
#93122 = CARTESIAN_POINT('Ctrl Pts',(43.4223598267253,252.801696685177,19.8230175376221)) ;
#93123 = CARTESIAN_POINT('Ctrl Pts',(43.400084060032,252.736117568422,19.7574370653152)) ;
#93124 = CARTESIAN_POINT('Ctrl Pts',(43.4001799908286,252.670367473295,19.6916880667959)) ;
#93125 = CARTESIAN_POINT('Ctrl Pts',(43.4436344606986,252.861063204372,19.8823434902912)) ;
#93126 = CARTESIAN_POINT('Ctrl Pts',(43.3992601718949,252.807355530103,19.8285659598275)) ;
#93127 = CARTESIAN_POINT('Ctrl Pts',(43.3731080437924,252.73934967782,19.7607787624628)) ;
#93128 = CARTESIAN_POINT('Ctrl Pts',(43.3701830998102,252.670391495618,19.6916295804032)) ;
#93129 = CARTESIAN_POINT('Ctrl Pts',(43.4107655857475,252.864902487303,19.9038322711337)) ;
#93130 = CARTESIAN_POINT('Ctrl Pts',(43.359064232039,252.806033227451,19.8493878369772)) ;
#93131 = CARTESIAN_POINT('Ctrl Pts',(43.3260192337239,252.731036352852,19.7803808851145)) ;
#93132 = CARTESIAN_POINT('Ctrl Pts',(43.3182834834246,252.65257254548,19.709389345178)) ;
#93133 = CARTESIAN_POINT('Ctrl Pts',(43.3892456815128,252.852053985775,19.9332636322348)) ;
#93134 = CARTESIAN_POINT('Ctrl Pts',(43.3353433537132,252.785704020096,19.880468688359)) ;
#93135 = CARTESIAN_POINT('Ctrl Pts',(43.3033941446389,252.701582066559,19.8138465043677)) ;
#93136 = CARTESIAN_POINT('Ctrl Pts',(43.2999819361157,252.615417852383,19.7465229726415)) ;
#93137 = CARTESIAN_POINT('Ctrl Pts',(43.383157199699,252.844152887956,19.9458563657641)) ;
#93138 = CARTESIAN_POINT('Ctrl Pts',(43.329628501671,252.77469313003,19.8937615473196)) ;
#93139 = CARTESIAN_POINT('Ctrl Pts',(43.2998965001866,252.687234889187,19.8281678666869)) ;
#93140 = CARTESIAN_POINT('Ctrl Pts',(43.3000002707217,252.59954242249,19.7623985166642)) ;
#93141 = CARTESIAN_POINT('',(43.3,252.6,19.7627416997969)) ;
#93142 = CARTESIAN_POINT('Origin',(43.4,252.6,19.7627416997969)) ;
#93143 = CARTESIAN_POINT('Origin',(43.7,252.6,19.7627416997969)) ;
#93144 = CARTESIAN_POINT('Origin',(43.4,254.579289321881,21.7420310216783)) ;
#93145 = CARTESIAN_POINT('',(43.3,254.579289321881,21.7420310216783)) ;
#93146 = CARTESIAN_POINT('Origin',(45.6,253.1,20.0213203435596)) ;
#93147 = CARTESIAN_POINT('',(45.7,253.1,25.7213203435596)) ;
#93148 = CARTESIAN_POINT('',(45.6,253.,25.7213203435596)) ;
#93149 = CARTESIAN_POINT('Origin',(45.6,253.1,25.7213203435596)) ;
#93150 = CARTESIAN_POINT('',(45.7,253.1,20.0213203435596)) ;
#93151 = CARTESIAN_POINT('',(45.6,253.,20.0213203435596)) ;
#93152 = CARTESIAN_POINT('Origin',(43.1,252.1,19.3213203435596)) ;
#93153 = CARTESIAN_POINT('',(43.1,251.9,19.3213203435596)) ;
#93154 = CARTESIAN_POINT('Origin',(43.1,251.8,19.3213203435596)) ;
#93155 = CARTESIAN_POINT('Origin',(43.1,252.1,19.3213203435596)) ;
#93156 = CARTESIAN_POINT('Origin',(38.75,251.8,19.3213203435596)) ;
#93157 = CARTESIAN_POINT('',(37.3,251.9,19.3213203435596)) ;
#93158 = CARTESIAN_POINT('Origin',(37.3,251.8,19.3213203435596)) ;
#93159 = CARTESIAN_POINT('',(38.75,251.9,19.3213203435596)) ;
#93160 = CARTESIAN_POINT('Origin',(37.3,252.1,19.3213203435596)) ;
#93161 = CARTESIAN_POINT('',(37.1,252.1,19.3213203435596)) ;
#93162 = CARTESIAN_POINT('Origin',(37.,252.1,19.3213203435596)) ;
#93163 = CARTESIAN_POINT('Origin',(37.3,252.1,19.3213203435596)) ;
#93164 = CARTESIAN_POINT('Origin',(37.,254.9,19.3213203435596)) ;
#93165 = CARTESIAN_POINT('',(37.1,254.9,19.3213203435596)) ;
#93166 = CARTESIAN_POINT('Origin',(45.6,258.9,20.0213203435596)) ;
#93167 = CARTESIAN_POINT('',(45.6,259.,25.7213203435596)) ;
#93168 = CARTESIAN_POINT('',(45.7,258.9,25.7213203435596)) ;
#93169 = CARTESIAN_POINT('Origin',(45.6,258.9,25.7213203435596)) ;
#93170 = CARTESIAN_POINT('',(45.6,259.,20.0213203435596)) ;
#93171 = CARTESIAN_POINT('',(45.7,258.9,20.0213203435596)) ;
#93172 = CARTESIAN_POINT('Origin',(50.457090707265,259.1,20.1213203435596)) ;
#93173 = CARTESIAN_POINT('',(43.7,259.,20.1213203435596)) ;
#93174 = CARTESIAN_POINT('',(43.7,259.1,20.0213203435596)) ;
#93175 = CARTESIAN_POINT('Origin',(43.7,259.1,20.1213203435596)) ;
#93176 = CARTESIAN_POINT('',(50.457090707265,259.1,20.0213203435596)) ;
#93177 = CARTESIAN_POINT('',(50.457090707265,259.,20.1213203435596)) ;
#93178 = CARTESIAN_POINT('Origin',(43.7,259.4,20.1213203435596)) ;
#93179 = CARTESIAN_POINT('',(43.3,259.4,20.1213203435596)) ;
#93180 = CARTESIAN_POINT('',(43.4,259.4,20.0213203435596)) ;
#93181 = CARTESIAN_POINT('Origin',(43.4,259.4,20.1213203435596)) ;
#93182 = CARTESIAN_POINT('Origin',(43.7,259.4,20.0213203435596)) ;
#93183 = CARTESIAN_POINT('Origin',(43.7,259.4,20.1213203435596)) ;
#93184 = CARTESIAN_POINT('Origin',(43.4,246.408305665508,20.1213203435596)) ;
#93185 = CARTESIAN_POINT('',(43.3,259.9,20.1213203435596)) ;
#93186 = CARTESIAN_POINT('',(43.4,259.9,20.0213203435596)) ;
#93187 = CARTESIAN_POINT('Origin',(43.4,259.9,20.1213203435596)) ;
#93188 = CARTESIAN_POINT('',(43.4,246.408305665508,20.0213203435596)) ;
#93189 = CARTESIAN_POINT('',(43.3,246.408305665508,20.1213203435596)) ;
#93190 = CARTESIAN_POINT('Origin',(43.1,259.9,20.1213203435596)) ;
#93191 = CARTESIAN_POINT('',(43.1,260.1,20.1213203435596)) ;
#93192 = CARTESIAN_POINT('',(43.1,260.2,20.0213203435596)) ;
#93193 = CARTESIAN_POINT('Origin',(43.1,260.2,20.1213203435596)) ;
#93194 = CARTESIAN_POINT('Origin',(43.1,259.9,20.0213203435596)) ;
#93195 = CARTESIAN_POINT('Origin',(43.1,259.9,20.1213203435596)) ;
#93196 = CARTESIAN_POINT('Origin',(49.1570907072649,260.2,20.1213203435596)) ;
#93197 = CARTESIAN_POINT('',(37.3,260.1,20.1213203435596)) ;
#93198 = CARTESIAN_POINT('',(37.3,260.2,20.0213203435596)) ;
#93199 = CARTESIAN_POINT('Origin',(37.3,260.2,20.1213203435596)) ;
#93200 = CARTESIAN_POINT('',(49.1570907072649,260.2,20.0213203435596)) ;
#93201 = CARTESIAN_POINT('',(49.1570907072649,260.1,20.1213203435596)) ;
#93202 = CARTESIAN_POINT('Origin',(37.3,259.9,20.1213203435596)) ;
#93203 = CARTESIAN_POINT('',(37.1,259.9,20.1213203435596)) ;
#93204 = CARTESIAN_POINT('',(37.,259.9,20.0213203435596)) ;
#93205 = CARTESIAN_POINT('Origin',(37.,259.9,20.1213203435596)) ;
#93206 = CARTESIAN_POINT('Origin',(37.3,259.9,20.0213203435596)) ;
#93207 = CARTESIAN_POINT('Origin',(37.3,259.9,20.1213203435596)) ;
#93208 = CARTESIAN_POINT('Origin',(37.,250.308305665508,20.1213203435596)) ;
#93209 = CARTESIAN_POINT('',(37.1,259.4,20.1213203435596)) ;
#93210 = CARTESIAN_POINT('',(37.,259.4,20.0213203435596)) ;
#93211 = CARTESIAN_POINT('Origin',(37.,259.4,20.1213203435596)) ;
#93212 = CARTESIAN_POINT('',(37.,250.308305665508,20.0213203435596)) ;
#93213 = CARTESIAN_POINT('',(37.1,250.308305665508,20.1213203435596)) ;
#93214 = CARTESIAN_POINT('Origin',(36.7,259.4,20.1213203435596)) ;
#93215 = CARTESIAN_POINT('',(36.7,259.,20.1213203435596)) ;
#93216 = CARTESIAN_POINT('',(36.7,259.1,20.0213203435596)) ;
#93217 = CARTESIAN_POINT('Origin',(36.7,259.1,20.1213203435596)) ;
#93218 = CARTESIAN_POINT('Origin',(36.7,259.4,20.0213203435596)) ;
#93219 = CARTESIAN_POINT('Origin',(36.7,259.4,20.1213203435596)) ;
#93220 = CARTESIAN_POINT('Origin',(46.157090707265,259.1,20.1213203435596)) ;
#93221 = CARTESIAN_POINT('',(46.157090707265,259.1,20.0213203435596)) ;
#93222 = CARTESIAN_POINT('',(46.157090707265,259.,20.1213203435596)) ;
#93223 = CARTESIAN_POINT('Origin',(52.2356360608974,252.9,20.0367671642397)) ;
#93224 = CARTESIAN_POINT('',(36.7,253.,20.0367671642397)) ;
#93225 = CARTESIAN_POINT('',(36.7,252.951184463531,19.950859360793)) ;
#93226 = CARTESIAN_POINT('Origin',(36.7,252.9,20.0367671642397)) ;
#93227 = CARTESIAN_POINT('',(52.2356360608974,252.951184463531,19.950859360793)) ;
#93228 = CARTESIAN_POINT('',(52.2356360608974,253.,20.0367671642397)) ;
#93229 = CARTESIAN_POINT('Ctrl Pts',(36.9378414229691,252.853553390627,19.874873734187)) ;
#93230 = CARTESIAN_POINT('Ctrl Pts',(36.911011436074,252.882637050264,19.9039573938178)) ;
#93231 = CARTESIAN_POINT('Ctrl Pts',(36.840727984334,252.933167717784,19.9409614997224)) ;
#93232 = CARTESIAN_POINT('Ctrl Pts',(36.7421332007821,252.951184463531,19.950859360793)) ;
#93233 = CARTESIAN_POINT('Ctrl Pts',(36.7,252.951184463531,19.950859360793)) ;
#93234 = CARTESIAN_POINT('Ctrl Pts',(36.956672105636,252.860791518147,19.8821118617056)) ;
#93235 = CARTESIAN_POINT('Ctrl Pts',(36.9273094800791,252.892278257538,19.9124287196988)) ;
#93236 = CARTESIAN_POINT('Ctrl Pts',(36.8514419143484,252.947930176663,19.9508675204564)) ;
#93237 = CARTESIAN_POINT('Ctrl Pts',(36.7453539666062,252.968095466674,19.9609350534414)) ;
#93238 = CARTESIAN_POINT('Ctrl Pts',(36.7,252.968095466674,19.9609350534414)) ;
#93239 = CARTESIAN_POINT('Ctrl Pts',(36.9895286392703,252.864580456291,19.9035816764723)) ;
#93240 = CARTESIAN_POINT('Ctrl Pts',(36.9557852684216,252.901881952996,19.9359235017)) ;
#93241 = CARTESIAN_POINT('Ctrl Pts',(36.8701500415939,252.968039937044,19.9768771497705)) ;
#93242 = CARTESIAN_POINT('Ctrl Pts',(36.75097066527,252.99225874652,19.9875415204354)) ;
#93243 = CARTESIAN_POINT('Ctrl Pts',(36.7,252.99225874652,19.9875415204354)) ;
#93244 = CARTESIAN_POINT('Ctrl Pts',(37.0110353818099,252.851707610128,19.9329880225427)) ;
#93245 = CARTESIAN_POINT('Ctrl Pts',(36.9754124105622,252.895637337432,19.9671199843179)) ;
#93246 = CARTESIAN_POINT('Ctrl Pts',(36.8834622400518,252.972371462136,20.0104893458127)) ;
#93247 = CARTESIAN_POINT('Ctrl Pts',(36.7549442829771,253.,20.0220033688125)) ;
#93248 = CARTESIAN_POINT('Ctrl Pts',(36.7,253.,20.0220033688125)) ;
#93249 = CARTESIAN_POINT('Ctrl Pts',(37.0171218972921,252.843790283354,19.9455844123125)) ;
#93250 = CARTESIAN_POINT('Ctrl Pts',(36.981348581432,252.890324138772,19.9804848038695)) ;
#93251 = CARTESIAN_POINT('Ctrl Pts',(36.8876373124453,252.971173206804,20.024889730955)) ;
#93252 = CARTESIAN_POINT('Ctrl Pts',(36.7561776010428,253.,20.0367671642397)) ;
#93253 = CARTESIAN_POINT('Ctrl Pts',(36.7,253.,20.0367671642397)) ;
#93254 = CARTESIAN_POINT('',(37.0171218972921,252.843790283354,19.9455844123125)) ;
#93255 = CARTESIAN_POINT('Ctrl Pts',(36.7,253.,20.0367671642397)) ;
#93256 = CARTESIAN_POINT('Ctrl Pts',(36.7561776010428,253.,20.0367671642397)) ;
#93257 = CARTESIAN_POINT('Ctrl Pts',(36.8876373124453,252.971173206804,20.024889730955)) ;
#93258 = CARTESIAN_POINT('Ctrl Pts',(36.981348581432,252.890324138772,19.9804848038695)) ;
#93259 = CARTESIAN_POINT('Ctrl Pts',(37.0171218972921,252.843790283354,19.9455844123125)) ;
#93260 = CARTESIAN_POINT('Origin',(36.9378414229691,252.782842712516,19.9455844123125)) ;
#93261 = CARTESIAN_POINT('Ctrl Pts',(36.9378414229691,252.853553390627,19.874873734187)) ;
#93262 = CARTESIAN_POINT('Ctrl Pts',(36.911011436074,252.882637050264,19.9039573938178)) ;
#93263 = CARTESIAN_POINT('Ctrl Pts',(36.840727984334,252.933167717784,19.9409614997224)) ;
#93264 = CARTESIAN_POINT('Ctrl Pts',(36.7421332007821,252.951184463531,19.950859360793)) ;
#93265 = CARTESIAN_POINT('Ctrl Pts',(36.7,252.951184463531,19.950859360793)) ;
#93266 = CARTESIAN_POINT('Ctrl Pts',(36.9998200091722,252.670367473296,19.6916880667961)) ;
#93267 = CARTESIAN_POINT('Ctrl Pts',(36.9999159399687,252.736117568423,19.7574370653151)) ;
#93268 = CARTESIAN_POINT('Ctrl Pts',(36.9776401732752,252.801696685177,19.8230175376218)) ;
#93269 = CARTESIAN_POINT('Ctrl Pts',(36.9375191416343,252.853781762386,19.8751022254155)) ;
#93270 = CARTESIAN_POINT('Ctrl Pts',(37.0298169000146,252.670391495515,19.6916295805073)) ;
#93271 = CARTESIAN_POINT('Ctrl Pts',(37.0268919560317,252.739349677716,19.7607787625668)) ;
#93272 = CARTESIAN_POINT('Ctrl Pts',(37.0007398280733,252.807355530054,19.8285659598508)) ;
#93273 = CARTESIAN_POINT('Ctrl Pts',(36.9563655392695,252.861063204323,19.8823434903145)) ;
#93274 = CARTESIAN_POINT('Ctrl Pts',(37.0817165932468,252.652572590665,19.7093892999944)) ;
#93275 = CARTESIAN_POINT('Ctrl Pts',(37.0739808431665,252.731036398121,19.7803808398083)) ;
#93276 = CARTESIAN_POINT('Ctrl Pts',(37.0409357819462,252.806033248649,19.849387826736)) ;
#93277 = CARTESIAN_POINT('Ctrl Pts',(36.9892344284572,252.864902508585,19.9038322607699)) ;
#93278 = CARTESIAN_POINT('Ctrl Pts',(37.1000180638842,252.615417852384,19.7465229726421)) ;
#93279 = CARTESIAN_POINT('Ctrl Pts',(37.096605855361,252.701582066559,19.8138465043679)) ;
#93280 = CARTESIAN_POINT('Ctrl Pts',(37.0646566462868,252.785704020095,19.8804686883588)) ;
#93281 = CARTESIAN_POINT('Ctrl Pts',(37.0107543184878,252.852053985775,19.9332636322344)) ;
#93282 = CARTESIAN_POINT('Ctrl Pts',(37.0999997292783,252.599542422491,19.7623985166648)) ;
#93283 = CARTESIAN_POINT('Ctrl Pts',(37.1001034998132,252.687234889187,19.8281678666871)) ;
#93284 = CARTESIAN_POINT('Ctrl Pts',(37.0703714983291,252.77469313003,19.8937615473193)) ;
#93285 = CARTESIAN_POINT('Ctrl Pts',(37.0168428003015,252.844152887956,19.9458563657635)) ;
#93286 = CARTESIAN_POINT('Origin',(36.7,252.6,19.7627416997969)) ;
#93287 = CARTESIAN_POINT('Origin',(34.8,258.9,20.0213203435596)) ;
#93288 = CARTESIAN_POINT('',(34.7,258.9,25.7213203435596)) ;
#93289 = CARTESIAN_POINT('',(34.8,259.,25.7213203435596)) ;
#93290 = CARTESIAN_POINT('Origin',(34.8,258.9,25.7213203435596)) ;
#93291 = CARTESIAN_POINT('',(34.7,258.9,20.0213203435596)) ;
#93292 = CARTESIAN_POINT('',(34.8,259.,20.0213203435596)) ;
#93293 = CARTESIAN_POINT('Origin',(52.2356360608974,253.207106781187,19.5213203435596)) ;
#93294 = CARTESIAN_POINT('',(26.4,253.207106781187,20.0213203435596)) ;
#93295 = CARTESIAN_POINT('Origin',(26.4,253.207106781187,19.5213203435596)) ;
#93296 = CARTESIAN_POINT('',(52.2356360608974,253.207106781187,20.0213203435596)) ;
#93297 = CARTESIAN_POINT('Origin',(52.2356360608974,253.207106781187,19.5213203435596)) ;
#93298 = CARTESIAN_POINT('',(47.2699693783484,253.207106781187,20.0213203435596)) ;
#93299 = CARTESIAN_POINT('',(52.2356360608974,253.207106781187,20.0213203435596)) ;
#93300 = CARTESIAN_POINT('Ctrl Pts',(47.7791083033805,252.853553390593,19.8748737341529)) ;
#93301 = CARTESIAN_POINT('Ctrl Pts',(47.6146576398327,252.947314708832,19.968635052392)) ;
#93302 = CARTESIAN_POINT('Ctrl Pts',(47.4272201631483,253.072342459309,20.0213203435596)) ;
#93303 = CARTESIAN_POINT('Ctrl Pts',(47.2699693783484,253.207106781187,20.0213203435596)) ;
#93304 = CARTESIAN_POINT('Origin',(43.7,252.6,24.7713203435596)) ;
#93305 = CARTESIAN_POINT('',(43.3,252.6,25.7213203435596)) ;
#93306 = CARTESIAN_POINT('',(43.3,252.6,24.7713203435596)) ;
#93307 = CARTESIAN_POINT('',(43.7,253.,25.7213203435596)) ;
#93308 = CARTESIAN_POINT('Origin',(43.7,252.6,25.7213203435596)) ;
#93309 = CARTESIAN_POINT('',(43.7,253.,24.7713203435596)) ;
#93310 = CARTESIAN_POINT('Origin',(43.1,252.1,29.5213203435596)) ;
#93311 = CARTESIAN_POINT('',(43.1,251.9,29.5213203435596)) ;
#93312 = CARTESIAN_POINT('',(43.3,252.1,29.5213203435596)) ;
#93313 = CARTESIAN_POINT('Origin',(37.3,251.9,29.5213203435596)) ;
#93314 = CARTESIAN_POINT('',(37.3,251.9,29.5213203435596)) ;
#93315 = CARTESIAN_POINT('Origin',(37.3,252.1,29.5213203435596)) ;
#93316 = CARTESIAN_POINT('',(37.1,252.1,29.5213203435596)) ;
#93317 = CARTESIAN_POINT('Origin',(36.7,252.6,24.7713203435596)) ;
#93318 = CARTESIAN_POINT('',(36.7,253.,25.7213203435596)) ;
#93319 = CARTESIAN_POINT('',(36.7,253.,24.7713203435596)) ;
#93320 = CARTESIAN_POINT('',(37.1,252.6,25.7213203435596)) ;
#93321 = CARTESIAN_POINT('Origin',(36.7,252.6,25.7213203435596)) ;
#93322 = CARTESIAN_POINT('',(37.1,252.6,24.7713203435596)) ;
#93323 = CARTESIAN_POINT('Origin',(43.3,252.1,29.5213203435596)) ;
#93324 = CARTESIAN_POINT('',(43.3,259.9,29.5213203435596)) ;
#93325 = CARTESIAN_POINT('',(43.3,259.4,25.7213203435596)) ;
#93326 = CARTESIAN_POINT('',(43.3,259.4,24.7713203435596)) ;
#93327 = CARTESIAN_POINT('',(43.3,254.05,25.7213203435596)) ;
#93328 = CARTESIAN_POINT('Origin',(43.3,253.,20.0213203435596)) ;
#93329 = CARTESIAN_POINT('',(45.7,253.,25.7213203435596)) ;
#93330 = CARTESIAN_POINT('Origin',(37.1,259.9,29.5213203435596)) ;
#93331 = CARTESIAN_POINT('',(37.1,259.4,25.7213203435596)) ;
#93332 = CARTESIAN_POINT('',(37.1,257.95,25.7213203435596)) ;
#93333 = CARTESIAN_POINT('',(37.1,259.4,24.7713203435596)) ;
#93334 = CARTESIAN_POINT('',(37.1,259.9,29.5213203435596)) ;
#93335 = CARTESIAN_POINT('Origin',(34.7,259.,20.0213203435596)) ;
#93336 = CARTESIAN_POINT('',(34.7,253.,25.7213203435596)) ;
#93337 = CARTESIAN_POINT('Origin',(35.9,256.,25.7213203435596)) ;
#93338 = CARTESIAN_POINT('',(36.7,259.,25.7213203435596)) ;
#93339 = CARTESIAN_POINT('',(34.7,259.,25.7213203435596)) ;
#93340 = CARTESIAN_POINT('Origin',(36.7,259.4,25.7213203435596)) ;
#93341 = CARTESIAN_POINT('Origin',(28.4,247.6,22.9713203435596)) ;
#93342 = CARTESIAN_POINT('',(28.4,247.7,21.7213203435596)) ;
#93343 = CARTESIAN_POINT('',(28.3,247.6,21.7213203435596)) ;
#93344 = CARTESIAN_POINT('Origin',(28.4,247.6,21.7213203435596)) ;
#93345 = CARTESIAN_POINT('',(28.3,247.6,26.7213203435596)) ;
#93346 = CARTESIAN_POINT('',(28.3,247.6,22.9713203435596)) ;
#93347 = CARTESIAN_POINT('',(28.4,247.7,26.7213203435596)) ;
#93348 = CARTESIAN_POINT('Origin',(28.4,247.6,26.7213203435596)) ;
#93349 = CARTESIAN_POINT('',(28.4,247.7,22.9713203435596)) ;
#93350 = CARTESIAN_POINT('Origin',(28.3,246.7,24.2213203435596)) ;
#93351 = CARTESIAN_POINT('',(28.3,245.8,21.7213203435596)) ;
#93352 = CARTESIAN_POINT('',(28.3,245.9,21.7213203435596)) ;
#93353 = CARTESIAN_POINT('',(28.3,245.8,26.7213203435596)) ;
#93354 = CARTESIAN_POINT('',(28.3,245.8,25.4713203435596)) ;
#93355 = CARTESIAN_POINT('',(28.3,249.25,26.7213203435596)) ;
#93356 = CARTESIAN_POINT('Origin',(28.4,245.8,25.4713203435596)) ;
#93357 = CARTESIAN_POINT('',(28.4,245.7,26.7213203435596)) ;
#93358 = CARTESIAN_POINT('Origin',(28.4,245.8,26.7213203435596)) ;
#93359 = CARTESIAN_POINT('',(28.4,245.7,21.7213203435596)) ;
#93360 = CARTESIAN_POINT('Origin',(28.4,245.8,21.7213203435596)) ;
#93361 = CARTESIAN_POINT('',(28.4,245.7,25.4713203435596)) ;
#93362 = CARTESIAN_POINT('Origin',(26.4,251.7,26.6213203435596)) ;
#93363 = CARTESIAN_POINT('',(26.3,251.7,26.8213203435596)) ;
#93364 = CARTESIAN_POINT('',(26.3,251.9,26.6213203435596)) ;
#93365 = CARTESIAN_POINT('Origin',(26.3,251.7,26.6213203435596)) ;
#93366 = CARTESIAN_POINT('',(26.4,251.8,26.6213203435596)) ;
#93367 = CARTESIAN_POINT('Origin',(26.4,251.9,26.6213203435596)) ;
#93368 = CARTESIAN_POINT('',(26.4,251.7,26.7213203435596)) ;
#93369 = CARTESIAN_POINT('Origin',(26.4,251.7,26.6213203435596)) ;
#93370 = CARTESIAN_POINT('Origin',(26.4,251.7,26.8213203435596)) ;
#93371 = CARTESIAN_POINT('Origin',(26.4,251.7,21.8213203435596)) ;
#93372 = CARTESIAN_POINT('',(26.4,251.8,21.8213203435596)) ;
#93373 = CARTESIAN_POINT('',(26.4,251.7,21.7213203435596)) ;
#93374 = CARTESIAN_POINT('Origin',(26.4,251.7,21.8213203435596)) ;
#93375 = CARTESIAN_POINT('',(26.3,251.9,21.8213203435596)) ;
#93376 = CARTESIAN_POINT('Origin',(26.4,251.9,21.8213203435596)) ;
#93377 = CARTESIAN_POINT('',(26.3,251.7,21.6213203435596)) ;
#93378 = CARTESIAN_POINT('Origin',(26.3,251.7,21.8213203435596)) ;
#93379 = CARTESIAN_POINT('Origin',(26.4,251.7,21.6213203435596)) ;
#93380 = CARTESIAN_POINT('Origin',(26.4,251.9,25.6213203435596)) ;
#93381 = CARTESIAN_POINT('',(26.3,251.9,25.6213203435596)) ;
#93382 = CARTESIAN_POINT('',(26.4,251.8,25.6213203435596)) ;
#93383 = CARTESIAN_POINT('Origin',(40.8286796564404,245.2,21.6213203435596)) ;
#93384 = CARTESIAN_POINT('',(26.8,245.2,21.7213203435596)) ;
#93385 = CARTESIAN_POINT('',(26.8,245.1,21.6213203435596)) ;
#93386 = CARTESIAN_POINT('Origin',(26.8,245.2,21.6213203435596)) ;
#93387 = CARTESIAN_POINT('',(31.8,245.1,21.6213203435596)) ;
#93388 = CARTESIAN_POINT('',(40.8286796564404,245.1,21.6213203435596)) ;
#93389 = CARTESIAN_POINT('',(31.8,245.2,21.7213203435596)) ;
#93390 = CARTESIAN_POINT('Origin',(31.8,245.2,21.6213203435596)) ;
#93391 = CARTESIAN_POINT('',(40.8286796564404,245.2,21.7213203435596)) ;
#93392 = CARTESIAN_POINT('Origin',(26.8,245.6,21.6213203435596)) ;
#93393 = CARTESIAN_POINT('',(26.4,245.6,21.7213203435596)) ;
#93394 = CARTESIAN_POINT('',(26.3,245.6,21.6213203435596)) ;
#93395 = CARTESIAN_POINT('Origin',(26.4,245.6,21.6213203435596)) ;
#93396 = CARTESIAN_POINT('Origin',(26.8,245.6,21.6213203435596)) ;
#93397 = CARTESIAN_POINT('Origin',(26.8,245.6,21.7213203435596)) ;
#93398 = CARTESIAN_POINT('Origin',(26.4,245.35,21.6213203435596)) ;
#93399 = CARTESIAN_POINT('',(26.3,245.35,21.6213203435596)) ;
#93400 = CARTESIAN_POINT('',(26.4,245.35,21.7213203435596)) ;
#93401 = CARTESIAN_POINT('Origin',(26.3,251.7,21.8213203435596)) ;
#93402 = CARTESIAN_POINT('',(31.8,251.8,21.8213203435596)) ;
#93403 = CARTESIAN_POINT('',(31.8,251.7,21.7213203435596)) ;
#93404 = CARTESIAN_POINT('Origin',(31.8,251.7,21.8213203435596)) ;
#93405 = CARTESIAN_POINT('',(26.3,251.8,21.8213203435596)) ;
#93406 = CARTESIAN_POINT('',(26.3,251.7,21.7213203435596)) ;
#93407 = CARTESIAN_POINT('Origin',(26.3,251.7,26.6213203435596)) ;
#93408 = CARTESIAN_POINT('',(31.8,251.7,26.7213203435596)) ;
#93409 = CARTESIAN_POINT('',(31.8,251.8,26.6213203435596)) ;
#93410 = CARTESIAN_POINT('Origin',(31.8,251.7,26.6213203435596)) ;
#93411 = CARTESIAN_POINT('',(26.3,251.7,26.7213203435596)) ;
#93412 = CARTESIAN_POINT('',(26.3,251.8,26.6213203435596)) ;
#93413 = CARTESIAN_POINT('Origin',(26.4,248.7,26.8213203435596)) ;
#93414 = CARTESIAN_POINT('',(26.4,245.6,26.7213203435596)) ;
#93415 = CARTESIAN_POINT('',(26.3,245.6,26.8213203435596)) ;
#93416 = CARTESIAN_POINT('Origin',(26.4,245.6,26.8213203435596)) ;
#93417 = CARTESIAN_POINT('',(26.3,248.7,26.8213203435596)) ;
#93418 = CARTESIAN_POINT('',(26.4,248.7,26.7213203435596)) ;
#93419 = CARTESIAN_POINT('Origin',(26.8,245.6,26.8213203435596)) ;
#93420 = CARTESIAN_POINT('',(26.8,245.2,26.7213203435596)) ;
#93421 = CARTESIAN_POINT('',(26.8,245.1,26.8213203435596)) ;
#93422 = CARTESIAN_POINT('Origin',(26.8,245.2,26.8213203435596)) ;
#93423 = CARTESIAN_POINT('Origin',(26.8,245.6,26.8213203435596)) ;
#93424 = CARTESIAN_POINT('Origin',(26.8,245.6,26.7213203435596)) ;
#93425 = CARTESIAN_POINT('Origin',(40.8286796564404,245.2,26.8213203435596)) ;
#93426 = CARTESIAN_POINT('',(31.8,245.2,26.7213203435596)) ;
#93427 = CARTESIAN_POINT('',(31.8,245.1,26.8213203435596)) ;
#93428 = CARTESIAN_POINT('Origin',(31.8,245.2,26.8213203435596)) ;
#93429 = CARTESIAN_POINT('',(40.8286796564404,245.1,26.8213203435596)) ;
#93430 = CARTESIAN_POINT('',(40.8286796564404,245.2,26.7213203435596)) ;
#93431 = CARTESIAN_POINT('Origin',(26.8,245.6,29.5213203435596)) ;
#93432 = CARTESIAN_POINT('',(26.3,245.6,18.1213203435596)) ;
#93433 = CARTESIAN_POINT('',(26.3,245.6,29.5213203435596)) ;
#93434 = CARTESIAN_POINT('',(26.8,245.1,18.1213203435596)) ;
#93435 = CARTESIAN_POINT('Origin',(26.8,245.6,18.1213203435596)) ;
#93436 = CARTESIAN_POINT('',(26.8,245.1,29.5213203435596)) ;
#93437 = CARTESIAN_POINT('Origin',(26.3,245.6,29.5213203435596)) ;
#93438 = CARTESIAN_POINT('',(26.3,245.6,30.6213203435596)) ;
#93439 = CARTESIAN_POINT('',(26.3,245.6,29.5213203435596)) ;
#93440 = CARTESIAN_POINT('',(26.3,263.4,30.6213203435596)) ;
#93441 = CARTESIAN_POINT('',(26.3,250.025,30.6213203435596)) ;
#93442 = CARTESIAN_POINT('',(26.3,263.7,30.3213203435596)) ;
#93443 = CARTESIAN_POINT('Origin',(26.3,263.4,30.3213203435596)) ;
#93444 = CARTESIAN_POINT('',(26.3,263.7,22.5563984494954)) ;
#93445 = CARTESIAN_POINT('',(26.3,263.7,29.5213203435596)) ;
#93446 = CARTESIAN_POINT('',(26.3,261.872035100034,20.2714423245379)) ;
#93447 = CARTESIAN_POINT('',(26.3,261.378010680031,19.6539117995346)) ;
#93448 = CARTESIAN_POINT('',(26.3,261.559687576257,20.1213203435596)) ;
#93449 = CARTESIAN_POINT('Origin',(26.3,261.559687576257,20.5213203435596)) ;
#93450 = CARTESIAN_POINT('',(26.3,253.207106781187,20.1213203435596)) ;
#93451 = CARTESIAN_POINT('',(26.3,243.158305665508,20.1213203435596)) ;
#93452 = CARTESIAN_POINT('',(26.3,252.782842712475,19.9455844122715)) ;
#93453 = CARTESIAN_POINT('Origin',(26.3,253.207106781187,19.5213203435596)) ;
#93454 = CARTESIAN_POINT('',(26.3,251.148959235991,18.3117009357884)) ;
#93455 = CARTESIAN_POINT('',(26.3,252.954289321881,20.1170310216783)) ;
#93456 = CARTESIAN_POINT('',(26.3,250.68933982822,18.1213203435596)) ;
#93457 = CARTESIAN_POINT('Origin',(26.3,250.68933982822,18.7713203435596)) ;
#93458 = CARTESIAN_POINT('',(26.3,247.325,18.1213203435596)) ;
#93459 = CARTESIAN_POINT('Origin',(26.8,245.6,29.5213203435596)) ;
#93460 = CARTESIAN_POINT('',(26.8,245.1,30.6213203435596)) ;
#93461 = CARTESIAN_POINT('',(26.8,245.1,29.5213203435596)) ;
#93462 = CARTESIAN_POINT('Origin',(26.8,245.6,30.6213203435596)) ;
#93463 = CARTESIAN_POINT('Origin',(55.3573593128808,245.1,29.5213203435596)) ;
#93464 = CARTESIAN_POINT('',(38.7000000000001,245.1,19.3213203435596)) ;
#93465 = CARTESIAN_POINT('',(47.7786796564403,245.1,19.3213203435596)) ;
#93466 = CARTESIAN_POINT('',(38.7,245.1,20.0213203435596)) ;
#93467 = CARTESIAN_POINT('',(38.7000000000001,245.1,24.3713203435596)) ;
#93468 = CARTESIAN_POINT('',(33.6,245.1,20.0213203435596)) ;
#93469 = CARTESIAN_POINT('',(55.3573593128808,245.1,20.0213203435596)) ;
#93470 = CARTESIAN_POINT('',(33.6,245.1,30.6213203435596)) ;
#93471 = CARTESIAN_POINT('',(33.6,245.1,29.5213203435596)) ;
#93472 = CARTESIAN_POINT('',(42.7786796564403,245.1,30.6213203435596)) ;
#93473 = CARTESIAN_POINT('',(31.8,245.1,26.8713203435596)) ;
#93474 = CARTESIAN_POINT('',(55.2857703637053,245.1,18.1213203435596)) ;
#93475 = CARTESIAN_POINT('Origin',(79.1,252.258305665508,20.1213203435596)) ;
#93476 = CARTESIAN_POINT('',(79.1,259.648528137424,20.0213203435596)) ;
#93477 = CARTESIAN_POINT('Origin',(79.1,259.648528137424,20.1213203435596)) ;
#93478 = CARTESIAN_POINT('',(79.1,261.8,20.0213203435596)) ;
#93479 = CARTESIAN_POINT('',(79.1,252.258305665508,20.0213203435596)) ;
#93480 = CARTESIAN_POINT('Origin',(79.1,261.751937515251,20.1213203435596)) ;
#93481 = CARTESIAN_POINT('Ctrl Pts',(79.199999980455,263.599938801554,22.6718380448513)) ;
#93482 = CARTESIAN_POINT('Ctrl Pts',(79.2000000202887,263.599957412491,22.607806979346)) ;
#93483 = CARTESIAN_POINT('Ctrl Pts',(79.2000000357465,263.570981980112,22.4453050487916)) ;
#93484 = CARTESIAN_POINT('Ctrl Pts',(79.1999999617446,263.478889340347,22.2800545086636)) ;
#93485 = CARTESIAN_POINT('Ctrl Pts',(79.1999999904279,263.412205761232,22.1967251384676)) ;
#93486 = CARTESIAN_POINT('Ctrl Pts',(79.2000134423239,263.621049371538,22.6718434275057)) ;
#93487 = CARTESIAN_POINT('Ctrl Pts',(79.1999992361883,263.620328867382,22.6051015125814)) ;
#93488 = CARTESIAN_POINT('Ctrl Pts',(79.1999926902727,263.588298622545,22.438103534488)) ;
#93489 = CARTESIAN_POINT('Ctrl Pts',(79.200017057909,263.492581805062,22.2711937694893)) ;
#93490 = CARTESIAN_POINT('Ctrl Pts',(79.2000066111913,263.423895611839,22.1873698654484)) ;
#93491 = CARTESIAN_POINT('Ctrl Pts',(79.1878716797392,263.657834283321,22.6718527795981)) ;
#93492 = CARTESIAN_POINT('Ctrl Pts',(79.1887409558727,263.65586150683,22.6004009093503)) ;
#93493 = CARTESIAN_POINT('Ctrl Pts',(79.1909463759846,263.618555604801,22.4255570063445)) ;
#93494 = CARTESIAN_POINT('Ctrl Pts',(79.192991376968,263.516493911492,22.2557189726381)) ;
#93495 = CARTESIAN_POINT('Ctrl Pts',(79.1940100432926,263.444323308611,22.1710217844746)) ;
#93496 = CARTESIAN_POINT('Ctrl Pts',(79.1422513813381,263.696426316946,22.6718625902708)) ;
#93497 = CARTESIAN_POINT('Ctrl Pts',(79.145958048235,263.694409856707,22.595470144496)) ;
#93498 = CARTESIAN_POINT('Ctrl Pts',(79.1555689090378,263.654433984382,22.4112233680768)) ;
#93499 = CARTESIAN_POINT('Ctrl Pts',(79.1650239211106,263.546732261694,22.2362869927029)) ;
#93500 = CARTESIAN_POINT('Ctrl Pts',(79.1698705198354,263.470919230157,22.1497373351169)) ;
#93501 = CARTESIAN_POINT('Ctrl Pts',(79.0875105354057,263.704588703717,22.6718646768523)) ;
#93502 = CARTESIAN_POINT('Ctrl Pts',(79.0937026637392,263.704958374439,22.5944220758485)) ;
#93503 = CARTESIAN_POINT('Ctrl Pts',(79.1102880705233,263.669990271037,22.4059549450491)) ;
#93504 = CARTESIAN_POINT('Ctrl Pts',(79.1280035649932,263.563329571338,22.22586332057)) ;
#93505 = CARTESIAN_POINT('Ctrl Pts',(79.1374152312722,263.486858568468,22.1369812396074)) ;
#93506 = CARTESIAN_POINT('Ctrl Pts',(79.0526048408266,263.689467854776,22.6718608020123)) ;
#93507 = CARTESIAN_POINT('Ctrl Pts',(79.0590423639633,263.692813185744,22.5963703264553)) ;
#93508 = CARTESIAN_POINT('Ctrl Pts',(79.0771746363495,263.666059727285,22.4088436136315)) ;
#93509 = CARTESIAN_POINT('Ctrl Pts',(79.0990228521318,263.564978741887,22.2251604086679)) ;
#93510 = CARTESIAN_POINT('Ctrl Pts',(79.1112130439768,263.490317142384,22.1342133825315)) ;
#93511 = CARTESIAN_POINT('Ctrl Pts',(79.0399427396021,263.679957003543,22.671858403052)) ;
#93512 = CARTESIAN_POINT('Ctrl Pts',(79.0460881739513,263.68459203114,22.5975763648945)) ;
#93513 = CARTESIAN_POINT('Ctrl Pts',(79.0639145191738,263.661746144572,22.4111497893181)) ;
#93514 = CARTESIAN_POINT('Ctrl Pts',(79.0868564475194,263.563832003529,22.2260800781378)) ;
#93515 = CARTESIAN_POINT('Ctrl Pts',(79.0999812750617,263.490315472764,22.1342147151094)) ;
#93516 = CARTESIAN_POINT('',(79.1,263.490434404721,22.1343633494615)) ;
#93517 = CARTESIAN_POINT('Origin',(79.1,263.412347523777,22.196832854217)) ;
#93518 = CARTESIAN_POINT('Origin',(79.1,263.1,22.4467108732388)) ;
#93519 = CARTESIAN_POINT('Origin',(79.1,264.929230192226,24.0929361897785)) ;
#93520 = CARTESIAN_POINT('',(79.1,265.007317073171,24.030466685023)) ;
#93521 = CARTESIAN_POINT('Origin',(79.7999999999999,259.648528137424,20.1213203435596)) ;
#93522 = CARTESIAN_POINT('',(79.3050252531695,259.153553390593,20.0213203435596)) ;
#93523 = CARTESIAN_POINT('Origin',(79.3050252531695,259.153553390593,20.1213203435596)) ;
#93524 = CARTESIAN_POINT('Origin',(79.7999999999999,259.648528137424,20.0213203435596)) ;
#93525 = CARTESIAN_POINT('Origin',(77.8915498084026,260.56702883536,20.1213203435596)) ;
#93526 = CARTESIAN_POINT('',(83.7647589321277,254.693819711636,20.0213203435596)) ;
#93527 = CARTESIAN_POINT('Origin',(83.7647589321277,254.693819711636,20.1213203435596)) ;
#93528 = CARTESIAN_POINT('',(77.8915498084026,260.56702883536,20.0213203435596)) ;
#93529 = CARTESIAN_POINT('Origin',(83.1283628290598,254.057423608568,20.1213203435596)) ;
#93530 = CARTESIAN_POINT('',(84.0283628290598,254.057423608568,20.0213203435596)) ;
#93531 = CARTESIAN_POINT('Origin',(84.0283628290598,254.057423608568,20.1213203435596)) ;
#93532 = CARTESIAN_POINT('Origin',(83.1283628290598,254.057423608568,20.0213203435596)) ;
#93533 = CARTESIAN_POINT('Origin',(84.0283628290597,247.594124250979,20.1213203435596)) ;
#93534 = CARTESIAN_POINT('',(84.0283628290598,253.207106781187,20.0213203435596)) ;
#93535 = CARTESIAN_POINT('Origin',(84.0283628290598,253.207106781187,20.1213203435596)) ;
#93536 = CARTESIAN_POINT('',(84.0283628290597,247.594124250979,20.0213203435596)) ;
#93537 = CARTESIAN_POINT('Origin',(84.0283628290598,253.207106781187,19.5213203435596)) ;
#93538 = CARTESIAN_POINT('',(84.0283628290598,252.853553390593,19.8748737341529)) ;
#93539 = CARTESIAN_POINT('Origin',(84.0283628290598,252.782842712475,19.9455844122716)) ;
#93540 = CARTESIAN_POINT('Origin',(84.0283628290598,253.207106781187,19.5213203435596)) ;
#93541 = CARTESIAN_POINT('Origin',(84.0283628290598,255.172198614617,22.3349403144135)) ;
#93542 = CARTESIAN_POINT('',(84.0283628290598,251.21966991411,18.2409902576697)) ;
#93543 = CARTESIAN_POINT('Origin',(84.0283628290597,251.148959235991,18.3117009357884)) ;
#93544 = CARTESIAN_POINT('',(84.0283628290598,255.242909292735,22.2642296362948)) ;
#93545 = CARTESIAN_POINT('Origin',(84.0283628290598,250.68933982822,18.7713203435596)) ;
#93546 = CARTESIAN_POINT('',(84.0283628290598,250.68933982822,18.0213203435596)) ;
#93547 = CARTESIAN_POINT('Origin',(84.0283628290598,250.68933982822,18.1213203435596)) ;
#93548 = CARTESIAN_POINT('Origin',(84.0283628290598,250.68933982822,18.7713203435596)) ;
#93549 = CARTESIAN_POINT('Origin',(84.0283628290598,251.76081858547,18.1213203435596)) ;
#93550 = CARTESIAN_POINT('',(84.0283628290597,244.521708245126,18.0213203435596)) ;
#93551 = CARTESIAN_POINT('Origin',(84.0283628290597,244.521708245126,18.1213203435596)) ;
#93552 = CARTESIAN_POINT('',(84.0283628290598,251.76081858547,18.0213203435596)) ;
#93553 = CARTESIAN_POINT('Origin',(84.0283628290598,244.521708245126,17.2713203435596)) ;
#93554 = CARTESIAN_POINT('',(84.0283628290598,244.284537420614,17.9828328170975)) ;
#93555 = CARTESIAN_POINT('Origin',(84.0283628290598,244.252914644012,18.0777011469026)) ;
#93556 = CARTESIAN_POINT('Origin',(84.0283628290598,244.521708245126,17.2713203435596)) ;
#93557 = CARTESIAN_POINT('Origin',(84.0283628290597,249.125613950322,19.7019342490059)) ;
#93558 = CARTESIAN_POINT('',(84.0283628290596,241.115474564379,16.926478531686)) ;
#93559 = CARTESIAN_POINT('Origin',(84.0283628290596,241.083851787777,17.0213468614911)) ;
#93560 = CARTESIAN_POINT('',(84.0283628290597,249.157236726923,19.6070659192008)) ;
#93561 = CARTESIAN_POINT('Ctrl Pts',(84.1283622645681,241.084586497772,17.0215693550394)) ;
#93562 = CARTESIAN_POINT('Ctrl Pts',(84.1285407164372,240.967733802477,16.9904098877231)) ;
#93563 = CARTESIAN_POINT('Ctrl Pts',(84.0861524474351,240.851280004504,16.9593566288536)) ;
#93564 = CARTESIAN_POINT('Ctrl Pts',(84.0109024885665,240.761883803078,16.9355183842823)) ;
#93565 = CARTESIAN_POINT('Ctrl Pts',(84.1283591396267,241.089318576984,17.0073731711595)) ;
#93566 = CARTESIAN_POINT('Ctrl Pts',(84.1296466148509,240.972687875819,16.9755449829255)) ;
#93567 = CARTESIAN_POINT('Ctrl Pts',(84.0885132271462,240.855600661952,16.9436904372174)) ;
#93568 = CARTESIAN_POINT('Ctrl Pts',(84.0135991831494,240.765080061658,16.9191205527874)) ;
#93569 = CARTESIAN_POINT('Ctrl Pts',(84.1215046355259,241.098751749129,16.9790430941334)) ;
#93570 = CARTESIAN_POINT('Ctrl Pts',(84.124343019653,240.984169277709,16.9458857218838)) ;
#93571 = CARTESIAN_POINT('Ctrl Pts',(84.0856125763432,240.867917187228,16.912452808833)) ;
#93572 = CARTESIAN_POINT('Ctrl Pts',(84.0122486019915,240.777113726845,16.8864296181804)) ;
#93573 = CARTESIAN_POINT('Ctrl Pts',(84.0879935149337,241.11202068738,16.9390868854387)) ;
#93574 = CARTESIAN_POINT('Ctrl Pts',(84.0909415904953,241.005595606274,16.9049583584226)) ;
#93575 = CARTESIAN_POINT('Ctrl Pts',(84.0552587945595,240.897417390581,16.8703689760042)) ;
#93576 = CARTESIAN_POINT('Ctrl Pts',(83.9870257452385,240.812703535314,16.8433455584424)) ;
#93577 = CARTESIAN_POINT('Ctrl Pts',(84.0506405361305,241.116115853192,16.9266350001795)) ;
#93578 = CARTESIAN_POINT('Ctrl Pts',(84.0518474252873,241.017952351887,16.8938858976742)) ;
#93579 = CARTESIAN_POINT('Ctrl Pts',(84.0172831579462,240.919342924437,16.8610569819731)) ;
#93580 = CARTESIAN_POINT('Ctrl Pts',(83.9540867816564,240.843013317032,16.8355837036259)) ;
#93581 = CARTESIAN_POINT('Ctrl Pts',(84.0281290686331,241.116068437914,16.9266767871987)) ;
#93582 = CARTESIAN_POINT('Ctrl Pts',(84.0282622279932,241.022635623806,16.8955327774992)) ;
#93583 = CARTESIAN_POINT('Ctrl Pts',(83.9943602020726,240.929528751412,16.8644966955634)) ;
#93584 = CARTESIAN_POINT('Ctrl Pts',(83.9341920814085,240.858060634643,16.840674276805)) ;
#93585 = CARTESIAN_POINT('',(83.9347806063072,240.858359520505,16.8407735170612)) ;
#93586 = CARTESIAN_POINT('Origin',(83.9347806063072,240.826736743903,16.9356418468662)) ;
#93587 = CARTESIAN_POINT('Origin',(83.6283628290597,241.115474564379,16.926478531686)) ;
#93588 = CARTESIAN_POINT('Origin',(82.0396822566532,238.568246477383,16.1828117580263)) ;
#93589 = CARTESIAN_POINT('',(82.183342912681,238.77107735692,16.1450127958665)) ;
#93590 = CARTESIAN_POINT('Origin',(82.183342912681,238.739454580319,16.2398811256715)) ;
#93591 = CARTESIAN_POINT('',(82.0396822566532,238.599869253985,16.0879434282213)) ;
#93592 = CARTESIAN_POINT('Ctrl Pts',(82.2600174118103,238.675259362667,16.2399239332136)) ;
#93593 = CARTESIAN_POINT('Ctrl Pts',(82.2259293366007,238.634587417089,16.2331463302158)) ;
#93594 = CARTESIAN_POINT('Ctrl Pts',(82.1750738891123,238.608420964891,16.2287859646011)) ;
#93595 = CARTESIAN_POINT('Ctrl Pts',(82.12216544278,238.604329214334,16.228104116753)) ;
#93596 = CARTESIAN_POINT('Ctrl Pts',(82.2627110753973,238.678465563114,16.2235326723752)) ;
#93597 = CARTESIAN_POINT('Ctrl Pts',(82.2290102704972,238.636513924476,16.2159238942483)) ;
#93598 = CARTESIAN_POINT('Ctrl Pts',(82.1771259429379,238.608697992535,16.2108727836205)) ;
#93599 = CARTESIAN_POINT('Ctrl Pts',(82.1226277921929,238.604359263907,16.2100849868948)) ;
#93600 = CARTESIAN_POINT('Ctrl Pts',(82.2615149316266,238.689015344967,16.1948907345544)) ;
#93601 = CARTESIAN_POINT('Ctrl Pts',(82.2293611646308,238.646803345078,16.1858377152017)) ;
#93602 = CARTESIAN_POINT('Ctrl Pts',(82.1776767840732,238.617677482652,16.1795814374807)) ;
#93603 = CARTESIAN_POINT('Ctrl Pts',(82.1227588786755,238.613157114129,16.1786097279244)) ;
#93604 = CARTESIAN_POINT('Ctrl Pts',(82.2455628907713,238.713040050509,16.1629253456017)) ;
#93605 = CARTESIAN_POINT('Ctrl Pts',(82.217310584656,238.675084611303,16.152902119824)) ;
#93606 = CARTESIAN_POINT('Ctrl Pts',(82.1708850010324,238.648387550594,16.145860959752)) ;
#93607 = CARTESIAN_POINT('Ctrl Pts',(82.1212259488329,238.644250453869,16.1447688539501)) ;
#93608 = CARTESIAN_POINT('Ctrl Pts',(82.2197237261747,238.741281860249,16.1431681067147)) ;
#93609 = CARTESIAN_POINT('Ctrl Pts',(82.1964342697029,238.710695018504,16.1335850929804)) ;
#93610 = CARTESIAN_POINT('Ctrl Pts',(82.1586959941735,238.689424407277,16.1269372215605)) ;
#93611 = CARTESIAN_POINT('Ctrl Pts',(82.1184726934836,238.686124239564,16.1259053349689)) ;
#93612 = CARTESIAN_POINT('Ctrl Pts',(82.1965610315802,238.761185251271,16.1416966134236)) ;
#93613 = CARTESIAN_POINT('Ctrl Pts',(82.1772535578776,238.737197314262,16.1336924132218)) ;
#93614 = CARTESIAN_POINT('Ctrl Pts',(82.1473625086148,238.721189684919,16.1283631541481)) ;
#93615 = CARTESIAN_POINT('Ctrl Pts',(82.1159107239231,238.718695884331,16.1275308599076)) ;
#93616 = CARTESIAN_POINT('Ctrl Pts',(82.1832995175506,238.77118273482,16.1450479792177)) ;
#93617 = CARTESIAN_POINT('Ctrl Pts',(82.1662696739662,238.750868029957,16.138276456763)) ;
#93618 = CARTESIAN_POINT('Ctrl Pts',(82.1408684009841,238.737801298231,16.1339208359832)) ;
#93619 = CARTESIAN_POINT('Ctrl Pts',(82.1144434187989,238.735757954236,16.1332397271054)) ;
#93620 = CARTESIAN_POINT('',(82.1145102626716,238.735658579237,16.1332065366386)) ;
#93621 = CARTESIAN_POINT('Origin',(82.1145102626716,238.704035802635,16.2280748664437)) ;
#93622 = CARTESIAN_POINT('Origin',(82.106738468369,238.835356117889,16.1664390495227)) ;
#93623 = CARTESIAN_POINT('Ctrl Pts',(82.1222820569742,238.604338263983,16.2280748664436)) ;
#93624 = CARTESIAN_POINT('Ctrl Pts',(81.9325164757869,238.58954533045,16.2226507908148)) ;
#93625 = CARTESIAN_POINT('Ctrl Pts',(81.7474165920903,238.519173200702,16.1968476765741)) ;
#93626 = CARTESIAN_POINT('Ctrl Pts',(81.5957531842379,238.404160082301,16.1546761998268)) ;
#93627 = CARTESIAN_POINT('Ctrl Pts',(82.1227471767039,238.604374521797,16.2100662527241)) ;
#93628 = CARTESIAN_POINT('Ctrl Pts',(81.9341196170998,238.589760003749,16.2047187462123)) ;
#93629 = CARTESIAN_POINT('Ctrl Pts',(81.749938274034,238.520260056156,16.1792855328002)) ;
#93630 = CARTESIAN_POINT('Ctrl Pts',(81.5984884580874,238.40623436231,16.1376326562324)) ;
#93631 = CARTESIAN_POINT('Ctrl Pts',(82.12287874392,238.61317412536,16.1786041604694)) ;
#93632 = CARTESIAN_POINT('Ctrl Pts',(81.9345505882512,238.598690936658,16.1733895841157)) ;
#93633 = CARTESIAN_POINT('Ctrl Pts',(81.7504624577361,238.529885387063,16.1486022464915)) ;
#93634 = CARTESIAN_POINT('Ctrl Pts',(81.5983455559221,238.416350288722,16.1078501958846)) ;
#93635 = CARTESIAN_POINT('Ctrl Pts',(82.1213346533239,238.644259546122,16.1447712536724)) ;
#93636 = CARTESIAN_POINT('Ctrl Pts',(81.9292349728752,238.629499343051,16.1396437179694)) ;
#93637 = CARTESIAN_POINT('Ctrl Pts',(81.7413930623854,238.559386993981,16.1152768526036)) ;
#93638 = CARTESIAN_POINT('Ctrl Pts',(81.585998175509,238.443541210205,16.075123488759)) ;
#93639 = CARTESIAN_POINT('Ctrl Pts',(82.1185629971472,238.686097469017,16.1259229298218)) ;
#93640 = CARTESIAN_POINT('Ctrl Pts',(81.9197009618189,238.670732591567,16.1207518832949)) ;
#93641 = CARTESIAN_POINT('Ctrl Pts',(81.7254002682814,238.597712993629,16.0961743956505)) ;
#93642 = CARTESIAN_POINT('Ctrl Pts',(81.565153486231,238.477490209425,16.055737778703)) ;
#93643 = CARTESIAN_POINT('Ctrl Pts',(82.1159855626141,238.718625782101,16.1275289375935)) ;
#93644 = CARTESIAN_POINT('Ctrl Pts',(81.9108414388129,238.70267866242,16.1222138438478)) ;
#93645 = CARTESIAN_POINT('Ctrl Pts',(81.7106181165948,238.626842360931,16.0969302608009)) ;
#93646 = CARTESIAN_POINT('Ctrl Pts',(81.5461840821447,238.502579225023,16.0555134185675)) ;
#93647 = CARTESIAN_POINT('Ctrl Pts',(82.1145102626716,238.735658579237,16.1332065366386)) ;
#93648 = CARTESIAN_POINT('Ctrl Pts',(81.9057681233655,238.71938635235,16.1277824610098)) ;
#93649 = CARTESIAN_POINT('Ctrl Pts',(81.7021582512993,238.641977009628,16.1019793467691)) ;
#93650 = CARTESIAN_POINT('Ctrl Pts',(81.5353285026616,238.515462579386,16.0598078700218)) ;
#93651 = CARTESIAN_POINT('',(81.5353285026616,238.515462579386,16.0598078700217)) ;
#93652 = CARTESIAN_POINT('Origin',(81.5353285026616,238.483839802785,16.1546761998268)) ;
#93653 = CARTESIAN_POINT('Origin',(82.2,237.638985654062,15.7676488949136)) ;
#93654 = CARTESIAN_POINT('Ctrl Pts',(81.5957531842379,238.404160082301,16.1546761998268)) ;
#93655 = CARTESIAN_POINT('Ctrl Pts',(81.5259305404763,238.351210461111,16.135261338724)) ;
#93656 = CARTESIAN_POINT('Ctrl Pts',(81.4620702891285,238.288134589433,16.1213203435918)) ;
#93657 = CARTESIAN_POINT('Ctrl Pts',(81.4075488173165,238.217298220807,16.1213203435596)) ;
#93658 = CARTESIAN_POINT('Ctrl Pts',(81.5984884580875,238.40623436231,16.1376326562324)) ;
#93659 = CARTESIAN_POINT('Ctrl Pts',(81.5278222659162,238.35302801714,16.1189375875305)) ;
#93660 = CARTESIAN_POINT('Ctrl Pts',(81.462938591864,238.289258590766,16.1056627974852)) ;
#93661 = CARTESIAN_POINT('Ctrl Pts',(81.4075488173195,238.217298220811,16.1063603785401)) ;
#93662 = CARTESIAN_POINT('Ctrl Pts',(81.5983274323797,238.417772051001,16.1036566055189)) ;
#93663 = CARTESIAN_POINT('Ctrl Pts',(81.5259047694456,238.362797284882,16.0863863691115)) ;
#93664 = CARTESIAN_POINT('Ctrl Pts',(81.4591047090993,238.296564930755,16.0744149187042)) ;
#93665 = CARTESIAN_POINT('Ctrl Pts',(81.4021235542092,238.22147394772,16.0764991597938)) ;
#93666 = CARTESIAN_POINT('Ctrl Pts',(81.5785656655749,238.458467726493,16.0597468410921)) ;
#93667 = CARTESIAN_POINT('Ctrl Pts',(81.503609725597,238.39738306884,16.0427856245866)) ;
#93668 = CARTESIAN_POINT('Ctrl Pts',(81.4345131100941,238.324304784599,16.0313482653094)) ;
#93669 = CARTESIAN_POINT('Ctrl Pts',(81.375611944421,238.241879454313,16.0344444600661)) ;
#93670 = CARTESIAN_POINT('Ctrl Pts',(81.5516118718862,238.496137547842,16.0533661928403)) ;
#93671 = CARTESIAN_POINT('Ctrl Pts',(81.4754838615336,238.430403938523,16.033529884074)) ;
#93672 = CARTESIAN_POINT('Ctrl Pts',(81.405667898985,238.35229315755,16.0196569420612)) ;
#93673 = CARTESIAN_POINT('Ctrl Pts',(81.346086262007,238.264604838082,16.021320343554)) ;
#93674 = CARTESIAN_POINT('Ctrl Pts',(81.5353285026616,238.515462579386,16.0598078700217)) ;
#93675 = CARTESIAN_POINT('Ctrl Pts',(81.4585235945239,238.448257290954,16.0374061072109)) ;
#93676 = CARTESIAN_POINT('Ctrl Pts',(81.3882773180414,238.368199453823,16.0213203435967)) ;
#93677 = CARTESIAN_POINT('Ctrl Pts',(81.3283036990481,238.278291755183,16.0213203435596)) ;
#93678 = CARTESIAN_POINT('Origin',(81.3283036990481,238.278291755142,16.1213203435596)) ;
#93679 = CARTESIAN_POINT('Ctrl Pts',(81.3283036990481,238.278291755183,16.0213203435596)) ;
#93680 = CARTESIAN_POINT('Ctrl Pts',(81.3882773180414,238.368199453823,16.0213203435967)) ;
#93681 = CARTESIAN_POINT('Ctrl Pts',(81.4585235945239,238.448257290954,16.0374061072109)) ;
#93682 = CARTESIAN_POINT('Ctrl Pts',(81.5353285026616,238.515462579386,16.0598078700217)) ;
#93683 = CARTESIAN_POINT('Origin',(82.2,237.60736287746,16.1213203435596)) ;
#93684 = CARTESIAN_POINT('Origin',(81.1,237.60736287746,16.1213203435596)) ;
#93685 = CARTESIAN_POINT('Origin',(81.1,234.318247777236,16.1213203435596)) ;
#93686 = CARTESIAN_POINT('Origin',(81.1,226.002365511524,16.1213203435596)) ;
#93687 = CARTESIAN_POINT('Origin',(80.5999999999999,226.002365511524,16.1213203435596)) ;
#93688 = CARTESIAN_POINT('',(81.024264068712,225.578101442812,16.1213203435596)) ;
#93689 = CARTESIAN_POINT('Origin',(80.9535533905933,225.648812120931,16.1213203435596)) ;
#93690 = CARTESIAN_POINT('Origin',(80.5999999999999,226.002365511524,16.1213203435596)) ;
#93691 = CARTESIAN_POINT('Origin',(79.3343678337509,224.029626564088,16.1213203435596)) ;
#93692 = CARTESIAN_POINT('',(80.1757359312881,224.729573305388,16.1213203435596)) ;
#93693 = CARTESIAN_POINT('Origin',(80.1050252531694,224.800283983507,16.1213203435596)) ;
#93694 = CARTESIAN_POINT('',(79.4050785118696,223.95891588597,16.1213203435596)) ;
#93695 = CARTESIAN_POINT('Origin',(80.6000000000002,224.305309236676,16.1213203435596)) ;
#93696 = CARTESIAN_POINT('',(80.1316251501201,224.680309236676,16.1213203435596)) ;
#93697 = CARTESIAN_POINT('Origin',(80.0535626751402,224.742809236676,16.1213203435596)) ;
#93698 = CARTESIAN_POINT('Origin',(80.6000000000002,224.305309236676,16.1213203435596)) ;
#93699 = CARTESIAN_POINT('Origin',(79.3510004003203,225.305309236676,16.1213203435596)) ;
#93700 = CARTESIAN_POINT('',(79.3510004003203,224.305309236676,16.1213203435596)) ;
#93701 = CARTESIAN_POINT('Origin',(79.3510004003203,224.405309236676,16.1213203435596)) ;
#93702 = CARTESIAN_POINT('Origin',(79.3510004003203,225.305309236676,16.1213203435596)) ;
#93703 = CARTESIAN_POINT('Origin',(75.046430535485,224.405309236676,16.1213203435596)) ;
#93704 = CARTESIAN_POINT('Origin',(75.,224.405309236676,16.1213203435596)) ;
#93705 = CARTESIAN_POINT('',(75.046430535485,224.305309236676,16.1213203435596)) ;
#93706 = CARTESIAN_POINT('Origin',(74.9999999999998,220.305309236676,16.1213203435596)) ;
#93707 = CARTESIAN_POINT('Origin',(70.8999999999999,220.305309236676,16.1213203435596)) ;
#93708 = CARTESIAN_POINT('Origin',(70.9000000000001,225.16903572493,16.1213203435596)) ;
#93709 = CARTESIAN_POINT('Origin',(70.8999999999998,217.165524426368,16.1213203435596)) ;
#93710 = CARTESIAN_POINT('Origin',(69.4999999999997,217.165524426368,16.1213203435596)) ;
#93711 = CARTESIAN_POINT('Origin',(69.4999999999997,217.165524426368,16.1213203435596)) ;
#93712 = CARTESIAN_POINT('Origin',(69.4013544815242,215.668771587158,25.0213203435596)) ;
#93713 = CARTESIAN_POINT('',(69.4013544815242,215.668771587158,23.2713203435596)) ;
#93714 = CARTESIAN_POINT('',(69.4013544815242,215.668771587158,25.0213203435596)) ;
#93715 = CARTESIAN_POINT('',(67.3755510624416,215.802284899022,23.2713203435596)) ;
#93716 = CARTESIAN_POINT('Origin',(69.4999999999997,217.165524426368,25.0213203435596)) ;
#93717 = CARTESIAN_POINT('Origin',(69.4999999999997,217.165524426368,23.2713203435596)) ;
#93718 = CARTESIAN_POINT('Origin',(80.,224.305309236676,29.5213203435596)) ;
#93719 = CARTESIAN_POINT('',(79.3510004003203,224.305309236676,29.5213203435596)) ;
#93720 = CARTESIAN_POINT('Origin',(79.3510004003203,225.305309236676,29.5213203435596)) ;
#93721 = CARTESIAN_POINT('',(80.1316251501201,224.680309236676,29.5213203435596)) ;
#93722 = CARTESIAN_POINT('Origin',(80.6000000000002,224.305309236676,29.5213203435596)) ;
#93723 = CARTESIAN_POINT('',(80.1757359312881,224.729573305388,29.5213203435596)) ;
#93724 = CARTESIAN_POINT('Origin',(81.024264068712,225.578101442812,29.5213203435596)) ;
#93725 = CARTESIAN_POINT('',(81.024264068712,225.578101442812,29.5213203435596)) ;
#93726 = CARTESIAN_POINT('Origin',(80.5999999999999,226.002365511524,29.5213203435596)) ;
#93727 = CARTESIAN_POINT('Origin',(55.2857703637053,245.2,18.1213203435596)) ;
#93728 = CARTESIAN_POINT('',(26.8,245.2,18.0213203435596)) ;
#93729 = CARTESIAN_POINT('Origin',(26.8,245.2,18.1213203435596)) ;
#93730 = CARTESIAN_POINT('',(55.2857703637053,245.2,18.0213203435596)) ;
#93731 = CARTESIAN_POINT('Origin',(47.7786796564403,245.2,19.3213203435596)) ;
#93732 = CARTESIAN_POINT('Origin',(38.8,245.2,19.3213203435596)) ;
#93733 = CARTESIAN_POINT('Origin',(41.6,246.4,19.3213203435596)) ;
#93734 = CARTESIAN_POINT('',(41.7000000000001,242.9,19.3213203435596)) ;
#93735 = CARTESIAN_POINT('',(41.7,246.4,19.3213203435596)) ;
#93736 = CARTESIAN_POINT('Origin',(41.6000000000001,242.9,19.3213203435596)) ;
#93737 = CARTESIAN_POINT('Origin',(40.2,242.9,19.3213203435596)) ;
#93738 = CARTESIAN_POINT('',(38.7000000000001,242.9,19.3213203435596)) ;
#93739 = CARTESIAN_POINT('Origin',(38.8,242.9,19.3213203435596)) ;
#93740 = CARTESIAN_POINT('Origin',(40.2,242.9,19.3213203435596)) ;
#93741 = CARTESIAN_POINT('Origin',(38.8,247.5,19.3213203435596)) ;
#93742 = CARTESIAN_POINT('',(38.7,247.5,19.3213203435596)) ;
#93743 = CARTESIAN_POINT('Origin',(26.8,245.6,18.1213203435596)) ;
#93744 = CARTESIAN_POINT('',(26.4,245.6,18.0213203435596)) ;
#93745 = CARTESIAN_POINT('Origin',(26.4,245.6,18.1213203435596)) ;
#93746 = CARTESIAN_POINT('Origin',(26.8,245.6,18.0213203435596)) ;
#93747 = CARTESIAN_POINT('Origin',(26.4,247.325,18.1213203435596)) ;
#93748 = CARTESIAN_POINT('',(26.4,250.68933982822,18.0213203435596)) ;
#93749 = CARTESIAN_POINT('Origin',(26.4,250.68933982822,18.1213203435596)) ;
#93750 = CARTESIAN_POINT('',(26.4,247.325,18.0213203435596)) ;
#93751 = CARTESIAN_POINT('Origin',(26.4,250.68933982822,18.7713203435596)) ;
#93752 = CARTESIAN_POINT('Origin',(26.4,251.148959235991,18.3117009357884)) ;
#93753 = CARTESIAN_POINT('Origin',(26.4,250.68933982822,18.7713203435596)) ;
#93754 = CARTESIAN_POINT('Origin',(26.4,252.954289321881,20.1170310216783)) ;
#93755 = CARTESIAN_POINT('Origin',(26.4,252.782842712475,19.9455844122715)) ;
#93756 = CARTESIAN_POINT('Origin',(26.4,253.207106781187,19.5213203435596)) ;
#93757 = CARTESIAN_POINT('Origin',(26.4,253.207106781187,20.1213203435596)) ;
#93758 = CARTESIAN_POINT('Origin',(26.4,243.158305665508,20.1213203435596)) ;
#93759 = CARTESIAN_POINT('',(26.4,261.559687576257,20.0213203435596)) ;
#93760 = CARTESIAN_POINT('Origin',(26.4,261.559687576257,20.1213203435596)) ;
#93761 = CARTESIAN_POINT('',(26.4,243.158305665508,20.0213203435596)) ;
#93762 = CARTESIAN_POINT('Origin',(26.4,261.559687576257,20.5213203435596)) ;
#93763 = CARTESIAN_POINT('',(26.4,261.950121980978,20.2089728197824)) ;
#93764 = CARTESIAN_POINT('Origin',(26.4,261.872035100034,20.2714423245379)) ;
#93765 = CARTESIAN_POINT('Origin',(26.4,261.559687576257,20.5213203435596)) ;
#93766 = CARTESIAN_POINT('Origin',(26.4,261.378010680031,19.6539117995346)) ;
#93767 = CARTESIAN_POINT('',(26.4,263.8,22.5213203435596)) ;
#93768 = CARTESIAN_POINT('',(26.4,261.456097560976,19.5914422947791)) ;
#93769 = CARTESIAN_POINT('Origin',(26.4,263.7,22.5563984494954)) ;
#93770 = CARTESIAN_POINT('Origin',(34.,251.675,30.6213203435596)) ;
#93771 = CARTESIAN_POINT('',(34.1,248.9,30.6213203435596)) ;
#93772 = CARTESIAN_POINT('',(34.,248.9,30.7213203435596)) ;
#93773 = CARTESIAN_POINT('Origin',(34.,248.9,30.6213203435596)) ;
#93774 = CARTESIAN_POINT('',(34.,245.6,30.7213203435596)) ;
#93775 = CARTESIAN_POINT('',(34.,251.675,30.7213203435596)) ;
#93776 = CARTESIAN_POINT('',(34.1,245.6,30.6213203435596)) ;
#93777 = CARTESIAN_POINT('Origin',(34.,245.6,30.6213203435596)) ;
#93778 = CARTESIAN_POINT('',(34.1,251.675,30.6213203435596)) ;
#93779 = CARTESIAN_POINT('Origin',(33.6,245.6,30.6213203435596)) ;
#93780 = CARTESIAN_POINT('',(33.6,245.2,30.7213203435596)) ;
#93781 = CARTESIAN_POINT('Origin',(33.6,245.2,30.6213203435596)) ;
#93782 = CARTESIAN_POINT('Origin',(33.6,245.6,30.6213203435596)) ;
#93783 = CARTESIAN_POINT('Origin',(33.6,245.6,30.7213203435596)) ;
#93784 = CARTESIAN_POINT('Origin',(42.7786796564403,245.2,30.6213203435596)) ;
#93785 = CARTESIAN_POINT('',(26.8,245.2,30.7213203435596)) ;
#93786 = CARTESIAN_POINT('Origin',(26.8,245.2,30.6213203435596)) ;
#93787 = CARTESIAN_POINT('',(42.7786796564403,245.2,30.7213203435596)) ;
#93788 = CARTESIAN_POINT('Origin',(26.8,245.6,30.6213203435596)) ;
#93789 = CARTESIAN_POINT('',(26.4,245.6,30.7213203435596)) ;
#93790 = CARTESIAN_POINT('Origin',(26.4,245.6,30.6213203435596)) ;
#93791 = CARTESIAN_POINT('Origin',(26.8,245.6,30.7213203435596)) ;
#93792 = CARTESIAN_POINT('Origin',(26.4,250.025,30.6213203435596)) ;
#93793 = CARTESIAN_POINT('',(26.4,263.4,30.7213203435596)) ;
#93794 = CARTESIAN_POINT('Origin',(26.4,263.4,30.6213203435596)) ;
#93795 = CARTESIAN_POINT('',(26.4,250.025,30.7213203435596)) ;
#93796 = CARTESIAN_POINT('Origin',(26.4,263.4,30.3213203435596)) ;
#93797 = CARTESIAN_POINT('',(26.4,263.8,30.3213203435596)) ;
#93798 = CARTESIAN_POINT('Origin',(26.4,263.7,30.3213203435596)) ;
#93799 = CARTESIAN_POINT('Origin',(26.4,263.4,30.3213203435596)) ;
#93800 = CARTESIAN_POINT('Origin',(26.4,263.7,29.5213203435596)) ;
#93801 = CARTESIAN_POINT('',(26.4,263.8,29.5213203435596)) ;
#93802 = CARTESIAN_POINT('Origin',(45.7,244.9,18.0213203435596)) ;
#93803 = CARTESIAN_POINT('Origin',(55.2141814145299,249.05,18.0213203435596)) ;
#93804 = CARTESIAN_POINT('',(52.2356360608974,250.68933982822,18.0213203435596)) ;
#93805 = CARTESIAN_POINT('Origin',(52.2356360608974,250.68933982822,18.7713203435596)) ;
#93806 = CARTESIAN_POINT('Origin',(55.2141814145299,240.716611331017,20.0213203435596)) ;
#93807 = CARTESIAN_POINT('',(46.6263598493593,261.559687576257,20.0213203435596)) ;
#93808 = CARTESIAN_POINT('',(47.9856360608974,261.559687576257,20.0213203435596)) ;
#93809 = CARTESIAN_POINT('',(46.6350889359327,261.466666666667,20.0213203435596)) ;
#93810 = CARTESIAN_POINT('Origin',(46.1350889359327,261.466666666667,20.0213203435596)) ;
#93811 = CARTESIAN_POINT('',(46.6350889359327,257.,20.0213203435596)) ;
#93812 = CARTESIAN_POINT('',(46.6350889359327,252.258305665508,20.0213203435596)) ;
#93813 = CARTESIAN_POINT('',(46.65,256.631336165532,20.0213203435596)) ;
#93814 = CARTESIAN_POINT('Origin',(51.2,257.,20.0213203435596)) ;
#93815 = CARTESIAN_POINT('',(46.65,255.5,20.0213203435596)) ;
#93816 = CARTESIAN_POINT('',(46.65,248.108305665508,20.0213203435596)) ;
#93817 = CARTESIAN_POINT('Origin',(51.2,255.5,20.0213203435596)) ;
#93818 = CARTESIAN_POINT('',(30.7743961481358,257.164166814187,20.0213203435596)) ;
#93819 = CARTESIAN_POINT('',(31.705490254513,258.090883136929,20.0213203435593)) ;
#93820 = CARTESIAN_POINT('Ctrl Pts',(30.7743961481358,257.164166814187,20.0213203435596)) ;
#93821 = CARTESIAN_POINT('Ctrl Pts',(30.8077000968365,257.162767488612,20.0213203435596)) ;
#93822 = CARTESIAN_POINT('Ctrl Pts',(30.8410040455373,257.161368163036,20.0213203435596)) ;
#93823 = CARTESIAN_POINT('Ctrl Pts',(30.9447220946478,257.157010261813,20.0213203435596)) ;
#93824 = CARTESIAN_POINT('Ctrl Pts',(31.0509353958286,257.157783514541,20.0213203435571)) ;
#93825 = CARTESIAN_POINT('Ctrl Pts',(31.1897565474607,257.182733549511,20.021320343557)) ;
#93826 = CARTESIAN_POINT('Ctrl Pts',(31.2571806346872,257.213759459052,20.0213203435567)) ;
#93827 = CARTESIAN_POINT('Ctrl Pts',(31.2858437484895,257.241279724063,20.0213203435566)) ;
#93828 = CARTESIAN_POINT('Ctrl Pts',(31.2981495994694,257.253889722425,20.0213203435566)) ;
#93829 = CARTESIAN_POINT('Ctrl Pts',(31.318498748845,257.279979678226,20.0213203435566)) ;
#93830 = CARTESIAN_POINT('Ctrl Pts',(31.352487915175,257.336561723898,20.0213203435566)) ;
#93831 = CARTESIAN_POINT('Ctrl Pts',(31.3833769551383,257.400055955828,20.0213203435566)) ;
#93832 = CARTESIAN_POINT('Ctrl Pts',(31.4095784978925,257.455988292376,20.0213203435565)) ;
#93833 = CARTESIAN_POINT('Ctrl Pts',(31.4215689681375,257.482038502719,20.0213203435565)) ;
#93834 = CARTESIAN_POINT('Ctrl Pts',(31.4271002177055,257.494057204395,20.0213203435565)) ;
#93835 = CARTESIAN_POINT('Ctrl Pts',(31.4298611935316,257.500068246514,20.0213203435565)) ;
#93836 = CARTESIAN_POINT('Ctrl Pts',(31.4326210851137,257.506079046589,20.0213203435565)) ;
#93837 = CARTESIAN_POINT('Ctrl Pts',(31.449163234782,257.542143350465,20.0213203435565)) ;
#93838 = CARTESIAN_POINT('Ctrl Pts',(31.4940316374113,257.640298396679,20.0213203435568)) ;
#93839 = CARTESIAN_POINT('Ctrl Pts',(31.567631288081,257.79951081352,20.0213203435576)) ;
#93840 = CARTESIAN_POINT('Ctrl Pts',(31.6435315049203,257.960632026113,20.0213203435577)) ;
#93841 = CARTESIAN_POINT('Ctrl Pts',(31.6896407086131,258.057612082693,20.0213203435588)) ;
#93842 = CARTESIAN_POINT('Ctrl Pts',(31.7054902513284,258.090883129822,20.0213203435591)) ;
#93843 = CARTESIAN_POINT('',(30.7492082877751,256.564695737578,20.0213203435596)) ;
#93844 = CARTESIAN_POINT('',(30.4489043471128,249.417461949796,20.0213203435596)) ;
#93845 = CARTESIAN_POINT('',(32.2494311094147,257.837238667481,20.0213203435596)) ;
#93846 = CARTESIAN_POINT('Ctrl Pts',(32.2494305846701,257.837237537136,20.0213203435596)) ;
#93847 = CARTESIAN_POINT('Ctrl Pts',(32.2079598075039,257.749584797189,20.0213203435596)) ;
#93848 = CARTESIAN_POINT('Ctrl Pts',(32.1338192164731,257.591081166943,20.0213203435596)) ;
#93849 = CARTESIAN_POINT('Ctrl Pts',(32.0151173093266,257.33883287554,20.0213203435596)) ;
#93850 = CARTESIAN_POINT('Ctrl Pts',(31.9025505811396,257.076333688533,20.0213203435596)) ;
#93851 = CARTESIAN_POINT('Ctrl Pts',(31.735897005124,256.808363024752,20.0213203435596)) ;
#93852 = CARTESIAN_POINT('Ctrl Pts',(31.3799595822748,256.57233432435,20.0213203435596)) ;
#93853 = CARTESIAN_POINT('Ctrl Pts',(31.0569053558616,256.55176728934,20.0213203435596)) ;
#93854 = CARTESIAN_POINT('Ctrl Pts',(30.8158161851762,256.561897086427,20.0213203435597)) ;
#93855 = CARTESIAN_POINT('Ctrl Pts',(30.7825122364757,256.563296412003,20.0213203435596)) ;
#93856 = CARTESIAN_POINT('Ctrl Pts',(30.7492082877751,256.564695737578,20.0213203435596)) ;
#93857 = CARTESIAN_POINT('',(32.7113239146176,257.621855202687,20.0213203435596)) ;
#93858 = CARTESIAN_POINT('',(44.9147880370394,251.931286426383,20.0213203435596)) ;
#93859 = CARTESIAN_POINT('',(32.8217003142836,259.81920153961,20.0213203435596)) ;
#93860 = CARTESIAN_POINT('',(32.319849148055,249.82847140953,20.0213203435596)) ;
#93861 = CARTESIAN_POINT('',(31.2093839453833,258.32222131243,20.0213203435596)) ;
#93862 = CARTESIAN_POINT('',(33.9819120129541,260.896418149051,20.0213203435596)) ;
#93863 = CARTESIAN_POINT('',(44.5070901774322,252.121399060531,20.0213203435596)) ;
#93864 = CARTESIAN_POINT('',(28.594347661489,253.822145724429,20.0213203435596)) ;
#93865 = CARTESIAN_POINT('',(28.704724061155,256.019492061351,20.0213203435596)) ;
#93866 = CARTESIAN_POINT('',(28.3509795345864,248.977232647076,20.0213203435596)) ;
#93867 = CARTESIAN_POINT('',(30.2066640303894,255.319125951608,20.0213203435596)) ;
#93868 = CARTESIAN_POINT('',(32.5650931541241,257.50884617869,20.0213203435596)) ;
#93869 = CARTESIAN_POINT('',(29.7113866401971,255.550077591566,20.0213203435596)) ;
#93870 = CARTESIAN_POINT('',(43.2063774077619,249.25726004992,20.0213203435596)) ;
#93871 = CARTESIAN_POINT('',(30.7304788580035,256.575626202204,20.0213203435596)) ;
#93872 = CARTESIAN_POINT('Ctrl Pts',(30.7304788580035,256.575626202204,20.0213203435596)) ;
#93873 = CARTESIAN_POINT('Ctrl Pts',(30.6975923919765,256.570186398587,20.0213203435596)) ;
#93874 = CARTESIAN_POINT('Ctrl Pts',(30.6647059259495,256.564746594971,20.0213203435597)) ;
#93875 = CARTESIAN_POINT('Ctrl Pts',(30.5574162678237,256.546999638827,20.0213203435596)) ;
#93876 = CARTESIAN_POINT('Ctrl Pts',(30.4098121082759,256.517330456645,20.0213203435596)) ;
#93877 = CARTESIAN_POINT('Ctrl Pts',(30.2468536416027,256.46621770294,20.0213203435596)) ;
#93878 = CARTESIAN_POINT('Ctrl Pts',(30.1477680849333,256.411315348599,20.0213203435596)) ;
#93879 = CARTESIAN_POINT('Ctrl Pts',(30.102845715951,256.376170629923,20.0213203435596)) ;
#93880 = CARTESIAN_POINT('Ctrl Pts',(30.0697165858412,256.329790150052,20.0213203435596)) ;
#93881 = CARTESIAN_POINT('Ctrl Pts',(30.0443195024724,256.279163360013,20.0213203435596)) ;
#93882 = CARTESIAN_POINT('Ctrl Pts',(30.0210609313549,256.227379414746,20.0213203435596)) ;
#93883 = CARTESIAN_POINT('Ctrl Pts',(29.9917240307883,256.158322827055,20.0213203435596)) ;
#93884 = CARTESIAN_POINT('Ctrl Pts',(29.9116103717487,255.966894765232,20.0213203435596)) ;
#93885 = CARTESIAN_POINT('Ctrl Pts',(29.8150167827562,255.758802051448,20.0213203435596)) ;
#93886 = CARTESIAN_POINT('Ctrl Pts',(29.7297455839443,255.586884322961,20.0213203435596)) ;
#93887 = CARTESIAN_POINT('Ctrl Pts',(29.7113866401971,255.550077591566,20.0213203435596)) ;
#93888 = CARTESIAN_POINT('',(30.6325623929048,257.167582590684,20.0213203435596)) ;
#93889 = CARTESIAN_POINT('',(32.3250488694829,246.935614134431,20.0213203435596)) ;
#93890 = CARTESIAN_POINT('',(29.1672125989201,255.803831327378,20.0213203435596)) ;
#93891 = CARTESIAN_POINT('Ctrl Pts',(29.1672135287853,255.803833319767,20.0213203435596)) ;
#93892 = CARTESIAN_POINT('Ctrl Pts',(29.2098526575051,255.890075605729,20.0213203435596)) ;
#93893 = CARTESIAN_POINT('Ctrl Pts',(29.2855162725872,256.046162959787,20.0213203435596)) ;
#93894 = CARTESIAN_POINT('Ctrl Pts',(29.4018690227886,256.296948740307,20.0213203435596)) ;
#93895 = CARTESIAN_POINT('Ctrl Pts',(29.5002329804407,256.562256782507,20.0213203435596)) ;
#93896 = CARTESIAN_POINT('Ctrl Pts',(29.6710833447946,256.82479414277,20.0213203435596)) ;
#93897 = CARTESIAN_POINT('Ctrl Pts',(30.0246139021395,257.050386605117,20.0213203435596)) ;
#93898 = CARTESIAN_POINT('Ctrl Pts',(30.3309225628221,257.117687857779,20.0213203435596)) ;
#93899 = CARTESIAN_POINT('Ctrl Pts',(30.5667894608518,257.156702983451,20.0213203435597)) ;
#93900 = CARTESIAN_POINT('Ctrl Pts',(30.5996759268789,257.162142787068,20.0213203435597)) ;
#93901 = CARTESIAN_POINT('Ctrl Pts',(30.6325623929059,257.167582590684,20.0213203435597)) ;
#93902 = CARTESIAN_POINT('',(42.7981704029692,249.447610102367,20.0213203435596)) ;
#93903 = CARTESIAN_POINT('Origin',(47.9856360608974,261.559687576257,20.5213203435596)) ;
#93904 = CARTESIAN_POINT('',(46.6263598493593,261.950121980978,20.2089728197824)) ;
#93905 = CARTESIAN_POINT('',(47.9856360608974,261.950121980978,20.2089728197824)) ;
#93906 = CARTESIAN_POINT('Origin',(46.6263598493593,261.559687576257,20.5213203435596)) ;
#93907 = CARTESIAN_POINT('Origin',(40.757090707265,262.8,21.2713203435596)) ;
#93908 = CARTESIAN_POINT('',(45.3029147394738,263.8,22.5213203435596)) ;
#93909 = CARTESIAN_POINT('',(40.757090707265,263.8,22.5213203435596)) ;
#93910 = CARTESIAN_POINT('',(46.5350889359327,262.157101071388,20.4676966827949)) ;
#93911 = CARTESIAN_POINT('',(44.3686862542563,265.04563798029,24.0783678189221)) ;
#93912 = CARTESIAN_POINT('Origin',(46.1350889359327,261.857101071388,20.0926966827949)) ;
#93913 = CARTESIAN_POINT('Origin',(26.3,263.8,29.5213203435596)) ;
#93914 = CARTESIAN_POINT('',(26.7,263.8,30.3213203435596)) ;
#93915 = CARTESIAN_POINT('',(28.25,263.8,30.3213203435596)) ;
#93916 = CARTESIAN_POINT('',(26.7,263.8,30.7213203435596)) ;
#93917 = CARTESIAN_POINT('',(45.6350889359327,263.8,22.9467108732387)) ;
#93918 = CARTESIAN_POINT('',(45.6350889359327,263.8,29.5213203435596)) ;
#93919 = CARTESIAN_POINT('Origin',(45.0100889359327,263.8,23.3217108732387)) ;
#93920 = CARTESIAN_POINT('',(42.2,263.8,25.0213203435596)) ;
#93921 = CARTESIAN_POINT('Origin',(40.2,263.8,25.0213203435596)) ;
#93922 = CARTESIAN_POINT('Origin',(28.25,263.4,30.3213203435596)) ;
#93923 = CARTESIAN_POINT('',(26.7,263.4,30.7213203435596)) ;
#93924 = CARTESIAN_POINT('',(28.25,263.4,30.7213203435596)) ;
#93925 = CARTESIAN_POINT('Origin',(26.7,263.4,30.3213203435596)) ;
#93926 = CARTESIAN_POINT('Origin',(30.2,254.45,30.7213203435596)) ;
#93927 = CARTESIAN_POINT('',(33.8,248.9,30.7213203435596)) ;
#93928 = CARTESIAN_POINT('',(34.2,248.9,30.7213203435596)) ;
#93929 = CARTESIAN_POINT('',(33.8,245.5,30.7213203435596)) ;
#93930 = CARTESIAN_POINT('',(33.8,248.9,30.7213203435596)) ;
#93931 = CARTESIAN_POINT('',(26.7,245.5,30.7213203435596)) ;
#93932 = CARTESIAN_POINT('',(26.7,245.5,30.7213203435596)) ;
#93933 = CARTESIAN_POINT('',(26.7,263.8,30.7213203435596)) ;
#93934 = CARTESIAN_POINT('Origin',(33.8,248.9,30.7213203435596)) ;
#93935 = CARTESIAN_POINT('',(34.1,248.9,30.7213203435596)) ;
#93936 = CARTESIAN_POINT('',(33.8,248.9,30.7213203435596)) ;
#93937 = CARTESIAN_POINT('Ctrl Pts',(65.5999303613899,241.999999985716,17.293483289198)) ;
#93938 = CARTESIAN_POINT('Ctrl Pts',(65.6223872883743,241.999983684684,17.293472412949)) ;
#93939 = CARTESIAN_POINT('Ctrl Pts',(65.6596675749485,242.013094396161,17.3022200416641)) ;
#93940 = CARTESIAN_POINT('Ctrl Pts',(65.6931551015551,242.055168995966,17.330288781682)) ;
#93941 = CARTESIAN_POINT('Ctrl Pts',(65.7000053564237,242.085052656273,17.3502211438567)) ;
#93942 = CARTESIAN_POINT('Ctrl Pts',(65.7000000641616,242.100035052592,17.3602131913087)) ;
#93943 = CARTESIAN_POINT('Ctrl Pts',(65.5999249277793,242.000021651293,17.2696626868496)) ;
#93944 = CARTESIAN_POINT('Ctrl Pts',(65.6241340213892,242.000002492859,17.2696523403355)) ;
#93945 = CARTESIAN_POINT('Ctrl Pts',(65.6644103131029,242.015411876757,17.2779740038621)) ;
#93946 = CARTESIAN_POINT('Ctrl Pts',(65.6970732727148,242.062602858122,17.3042522328329)) ;
#93947 = CARTESIAN_POINT('Ctrl Pts',(65.7014293655986,242.09429051932,17.3226735443473)) ;
#93948 = CARTESIAN_POINT('Ctrl Pts',(65.6999581864955,242.109509455678,17.331789222077)) ;
#93949 = CARTESIAN_POINT('Ctrl Pts',(65.5999043794225,241.984498189437,17.2281729676822)) ;
#93950 = CARTESIAN_POINT('Ctrl Pts',(65.6307400247959,241.984473403835,17.2281636615388)) ;
#93951 = CARTESIAN_POINT('Ctrl Pts',(65.6817645791198,242.004408765663,17.2356486243123)) ;
#93952 = CARTESIAN_POINT('Ctrl Pts',(65.7227159874069,242.065586997243,17.2589885526196)) ;
#93953 = CARTESIAN_POINT('Ctrl Pts',(65.7273533452622,242.106413945834,17.2748865541599)) ;
#93954 = CARTESIAN_POINT('Ctrl Pts',(65.7250852524029,242.125921449753,17.2826065722531)) ;
#93955 = CARTESIAN_POINT('Ctrl Pts',(65.599873772515,241.948550664554,17.2041705651312)) ;
#93956 = CARTESIAN_POINT('Ctrl Pts',(65.6405794114654,241.948520314274,17.2041604139615)) ;
#93957 = CARTESIAN_POINT('Ctrl Pts',(65.7080914959693,241.97293082834,17.2123249505645)) ;
#93958 = CARTESIAN_POINT('Ctrl Pts',(65.7672744641676,242.050491491113,17.2381616472598)) ;
#93959 = CARTESIAN_POINT('Ctrl Pts',(65.7782470503292,242.104798334671,17.2562659833551)) ;
#93960 = CARTESIAN_POINT('Ctrl Pts',(65.7775568883756,242.131748070042,17.2652363069337)) ;
#93961 = CARTESIAN_POINT('Ctrl Pts',(65.5998606830298,241.931622827182,17.1985279526202)) ;
#93962 = CARTESIAN_POINT('Ctrl Pts',(65.6447873550492,241.93159020424,17.1985170783063)) ;
#93963 = CARTESIAN_POINT('Ctrl Pts',(65.7193698426426,241.957828422043,17.2072631509073)) ;
#93964 = CARTESIAN_POINT('Ctrl Pts',(65.7863389216959,242.042015023498,17.2353253513923)) ;
#93965 = CARTESIAN_POINT('Ctrl Pts',(65.8000212346729,242.101795553135,17.2552521946044)) ;
#93966 = CARTESIAN_POINT('Ctrl Pts',(65.7999999505254,242.131762093447,17.2652410413751)) ;
#93967 = CARTESIAN_POINT('',(65.8,242.131622776602,17.2651946024269)) ;
#93968 = CARTESIAN_POINT('',(65.6,241.931622776602,17.1985279357602)) ;
#93969 = CARTESIAN_POINT('Origin',(65.6,242.131622776602,17.2651946024269)) ;
#93970 = CARTESIAN_POINT('',(65.6,242.,17.2933962655652)) ;
#93971 = CARTESIAN_POINT('Origin',(65.6,241.9,17.2933962655652)) ;
#93972 = CARTESIAN_POINT('',(65.7,242.1,17.3600629322319)) ;
#93973 = CARTESIAN_POINT('Origin',(65.6,242.1,17.3600629322319)) ;
#93974 = CARTESIAN_POINT('Origin',(65.8,242.1,17.3600629322319)) ;
#93975 = CARTESIAN_POINT('Ctrl Pts',(59.6999999358574,242.100035047439,17.3602131692166)) ;
#93976 = CARTESIAN_POINT('Ctrl Pts',(59.6999946444109,242.08505265448,17.3502211245603)) ;
#93977 = CARTESIAN_POINT('Ctrl Pts',(59.706844874529,242.055168958287,17.3302887398296)) ;
#93978 = CARTESIAN_POINT('Ctrl Pts',(59.7403323865735,242.013094322282,17.3022199784523)) ;
#93979 = CARTESIAN_POINT('Ctrl Pts',(59.777612703929,241.999983687182,17.2934724018186)) ;
#93980 = CARTESIAN_POINT('Ctrl Pts',(59.8000696283755,241.99999998572,17.2934832764019)) ;
#93981 = CARTESIAN_POINT('Ctrl Pts',(59.700041807277,242.109509448604,17.3317892058711)) ;
#93982 = CARTESIAN_POINT('Ctrl Pts',(59.6985706299482,242.094290514752,17.3226735305565)) ;
#93983 = CARTESIAN_POINT('Ctrl Pts',(59.7029267634591,242.06260272335,17.3042521582366)) ;
#93984 = CARTESIAN_POINT('Ctrl Pts',(59.7355897453586,242.015411672362,17.2779738906251)) ;
#93985 = CARTESIAN_POINT('Ctrl Pts',(59.7758659698318,242.000002492707,17.2696523335273)) ;
#93986 = CARTESIAN_POINT('Ctrl Pts',(59.8000750611887,242.000021648067,17.2696626783861)) ;
#93987 = CARTESIAN_POINT('Ctrl Pts',(59.6749147977919,242.125921458688,17.2826065001862)) ;
#93988 = CARTESIAN_POINT('Ctrl Pts',(59.6726467078424,242.106413958098,17.2748864836143)) ;
#93989 = CARTESIAN_POINT('Ctrl Pts',(59.6772839773079,242.06558697052,17.2589884854408)) ;
#93990 = CARTESIAN_POINT('Ctrl Pts',(59.7182353474647,242.004408673025,17.235648539643)) ;
#93991 = CARTESIAN_POINT('Ctrl Pts',(59.7692599649735,241.984473432376,17.2281636368172)) ;
#93992 = CARTESIAN_POINT('Ctrl Pts',(59.8000956065233,241.984498214178,17.2281729415163)) ;
#93993 = CARTESIAN_POINT('Ctrl Pts',(59.6224431111526,242.131748051622,17.2652363008027)) ;
#93994 = CARTESIAN_POINT('Ctrl Pts',(59.6217529522638,242.104798322373,17.2562659792971)) ;
#93995 = CARTESIAN_POINT('Ctrl Pts',(59.6327254809023,242.050491431942,17.2381616006781)) ;
#93996 = CARTESIAN_POINT('Ctrl Pts',(59.69190841539,241.97293070804,17.212324871922)) ;
#93997 = CARTESIAN_POINT('Ctrl Pts',(59.759420576324,241.948520318883,17.2041604155507)) ;
#93998 = CARTESIAN_POINT('Ctrl Pts',(59.8001262089281,241.94855066454,17.2041705651264)) ;
#93999 = CARTESIAN_POINT('Ctrl Pts',(59.60000004946,242.131762072965,17.265241034548)) ;
#94000 = CARTESIAN_POINT('Ctrl Pts',(59.5999787685205,242.101795539627,17.2552521901018)) ;
#94001 = CARTESIAN_POINT('Ctrl Pts',(59.6136610351411,242.042014939473,17.2353253233842)) ;
#94002 = CARTESIAN_POINT('Ctrl Pts',(59.6806300862088,241.957828270871,17.2072631005166)) ;
#94003 = CARTESIAN_POINT('Ctrl Pts',(59.755212631428,241.931590209221,17.1985170799667)) ;
#94004 = CARTESIAN_POINT('Ctrl Pts',(59.8001392964891,241.931622827167,17.1985279526151)) ;
#94005 = CARTESIAN_POINT('',(59.8,241.931622776602,17.1985279357602)) ;
#94006 = CARTESIAN_POINT('',(59.6,242.131622776602,17.2651946024269)) ;
#94007 = CARTESIAN_POINT('Origin',(59.8,242.131622776602,17.2651946024269)) ;
#94008 = CARTESIAN_POINT('',(59.7,242.1,17.3600629322319)) ;
#94009 = CARTESIAN_POINT('Origin',(59.6,242.1,17.3600629322319)) ;
#94010 = CARTESIAN_POINT('',(59.8,242.,17.2933962655652)) ;
#94011 = CARTESIAN_POINT('Origin',(59.8,242.1,17.3600629322319)) ;
#94012 = CARTESIAN_POINT('Origin',(59.8,241.9,17.2933962655652)) ;
#94013 = CARTESIAN_POINT('Origin',(59.5584606379469,244.3,18.0213203435596)) ;
#94014 = CARTESIAN_POINT('',(59.6446141839292,244.350769740148,18.5618897586017)) ;
#94015 = CARTESIAN_POINT('',(59.6446141839292,244.350769740148,18.0213203435596)) ;
#94016 = CARTESIAN_POINT('',(59.5584606379469,244.4,18.5618897586017)) ;
#94017 = CARTESIAN_POINT('Origin',(59.5584606379469,244.3,18.5618897586017)) ;
#94018 = CARTESIAN_POINT('',(59.5584606379469,244.4,18.0213203435596)) ;
#94019 = CARTESIAN_POINT('Ctrl Pts',(59.6449792856958,244.350205175131,18.5813019044811)) ;
#94020 = CARTESIAN_POINT('Ctrl Pts',(59.6430156590439,244.353094663765,18.5096043208207)) ;
#94021 = CARTESIAN_POINT('Ctrl Pts',(59.6643726514291,244.322762794723,18.3446198236948)) ;
#94022 = CARTESIAN_POINT('Ctrl Pts',(59.7030495510182,244.213584940611,18.1990771050326)) ;
#94023 = CARTESIAN_POINT('Ctrl Pts',(59.6996459812343,244.130500642109,18.129314888008)) ;
#94024 = CARTESIAN_POINT('Ctrl Pts',(59.6349464633671,244.367348698933,18.58199169507)) ;
#94025 = CARTESIAN_POINT('Ctrl Pts',(59.6329367571624,244.370044698671,18.5077410022612)) ;
#94026 = CARTESIAN_POINT('Ctrl Pts',(59.6546927064743,244.341795048543,18.3370566394004)) ;
#94027 = CARTESIAN_POINT('Ctrl Pts',(59.6991557712068,244.237488979578,18.1840665355433)) ;
#94028 = CARTESIAN_POINT('Ctrl Pts',(59.700759507625,244.153316861886,18.1088960755437)) ;
#94029 = CARTESIAN_POINT('Ctrl Pts',(59.6082389705581,244.391842293383,18.5831922626804)) ;
#94030 = CARTESIAN_POINT('Ctrl Pts',(59.6063337160284,244.394263327123,18.5045025279965)) ;
#94031 = CARTESIAN_POINT('Ctrl Pts',(59.6269047402143,244.368914661875,18.3237861932478)) ;
#94032 = CARTESIAN_POINT('Ctrl Pts',(59.6716432201894,244.274302161456,18.1578059752604)) ;
#94033 = CARTESIAN_POINT('Ctrl Pts',(59.6762070658786,244.193893615517,18.0736395593349)) ;
#94034 = CARTESIAN_POINT('Ctrl Pts',(59.5735081239853,244.399670610509,18.5840368704358)) ;
#94035 = CARTESIAN_POINT('Ctrl Pts',(59.5719051030305,244.402105264329,18.5022319176753)) ;
#94036 = CARTESIAN_POINT('Ctrl Pts',(59.5892945812339,244.37657507066,18.3141889457068)) ;
#94037 = CARTESIAN_POINT('Ctrl Pts',(59.6230383416314,244.283288012232,18.1450930356084)) ;
#94038 = CARTESIAN_POINT('Ctrl Pts',(59.6226269787515,244.20916290406,18.0620326887834)) ;
#94039 = CARTESIAN_POINT('Ctrl Pts',(59.5586579020403,244.399662026347,18.5842964723602)) ;
#94040 = CARTESIAN_POINT('Ctrl Pts',(59.5571848337607,244.402160845737,18.501538570537)) ;
#94041 = CARTESIAN_POINT('Ctrl Pts',(59.5732055894127,244.375930402281,18.3111050418282)) ;
#94042 = CARTESIAN_POINT('Ctrl Pts',(59.6022571961834,244.281492408201,18.1430838566138)) ;
#94043 = CARTESIAN_POINT('Ctrl Pts',(59.5997425774969,244.209583069344,18.062525619286)) ;
#94044 = CARTESIAN_POINT('',(59.7,244.147690779557,18.1437942097801)) ;
#94045 = CARTESIAN_POINT('',(59.6,244.224258591796,18.0794718176537)) ;
#94046 = CARTESIAN_POINT('Origin',(59.6,244.147690779557,18.1437942097801)) ;
#94047 = CARTESIAN_POINT('Ctrl Pts',(59.6,244.224258591796,18.0794718176537)) ;
#94048 = CARTESIAN_POINT('Ctrl Pts',(59.6,244.288790166617,18.1562886358886)) ;
#94049 = CARTESIAN_POINT('Ctrl Pts',(59.5736962854113,244.373361945941,18.311949011817)) ;
#94050 = CARTESIAN_POINT('Ctrl Pts',(59.5584606379469,244.4,18.4866458512847)) ;
#94051 = CARTESIAN_POINT('Ctrl Pts',(59.5584606379469,244.4,18.5618897586017)) ;
#94052 = CARTESIAN_POINT('Ctrl Pts',(59.6446141839293,244.350769740148,18.5618897586017)) ;
#94053 = CARTESIAN_POINT('Ctrl Pts',(59.6446141839293,244.350769740148,18.5439567476136)) ;
#94054 = CARTESIAN_POINT('Ctrl Pts',(59.6452210304616,244.349749530056,18.5260482379517)) ;
#94055 = CARTESIAN_POINT('Ctrl Pts',(59.6463723337907,244.347756284791,18.5082205111784)) ;
#94056 = CARTESIAN_POINT('Ctrl Pts',(59.6475773410637,244.345670062176,18.4895611884093)) ;
#94057 = CARTESIAN_POINT('Ctrl Pts',(59.6493785330647,244.342517330079,18.4709903607338)) ;
#94058 = CARTESIAN_POINT('Ctrl Pts',(59.6516514055649,244.338324693025,18.4525725587764)) ;
#94059 = CARTESIAN_POINT('Ctrl Pts',(59.6540993463895,244.333809117512,18.4327361230297)) ;
#94060 = CARTESIAN_POINT('Ctrl Pts',(59.6570943867615,244.328086171057,18.4130771945381)) ;
#94061 = CARTESIAN_POINT('Ctrl Pts',(59.6604228321352,244.321170986139,18.3936763934124)) ;
#94062 = CARTESIAN_POINT('Ctrl Pts',(59.6617883780566,244.318333925139,18.3857169162767)) ;
#94063 = CARTESIAN_POINT('Ctrl Pts',(59.663209403941,244.315296090927,18.3778008865419)) ;
#94064 = CARTESIAN_POINT('Ctrl Pts',(59.6646686888534,244.312058499533,18.3699338714232)) ;
#94065 = CARTESIAN_POINT('Ctrl Pts',(59.6682359483491,244.304144124111,18.3507027506552)) ;
#94066 = CARTESIAN_POINT('Ctrl Pts',(59.6720043911007,244.295103438323,18.331764526822)) ;
#94067 = CARTESIAN_POINT('Ctrl Pts',(59.675727045999,244.284910263978,18.3131841990656)) ;
#94068 = CARTESIAN_POINT('Ctrl Pts',(59.6793120602611,244.275093969855,18.2952908563249)) ;
#94069 = CARTESIAN_POINT('Ctrl Pts',(59.6828540129505,244.264207774873,18.2777294333825)) ;
#94070 = CARTESIAN_POINT('Ctrl Pts',(59.6860916942254,244.252252740375,18.2605579828757)) ;
#94071 = CARTESIAN_POINT('Ctrl Pts',(59.6892284705155,244.240670294304,18.2439216946671)) ;
#94072 = CARTESIAN_POINT('Ctrl Pts',(59.6920789697902,244.228083726207,18.2276514500578)) ;
#94073 = CARTESIAN_POINT('Ctrl Pts',(59.6943758946989,244.214531288834,18.2118000413148)) ;
#94074 = CARTESIAN_POINT('Ctrl Pts',(59.6965663032281,244.201607325017,18.1966837174079)) ;
#94075 = CARTESIAN_POINT('Ctrl Pts',(59.6982525026342,244.187804525414,18.1819482843279)) ;
#94076 = CARTESIAN_POINT('Ctrl Pts',(59.6991857824465,244.173199818986,18.1676395251846)) ;
#94077 = CARTESIAN_POINT('Ctrl Pts',(59.6997132846748,244.164945043641,18.1595520232023)) ;
#94078 = CARTESIAN_POINT('Ctrl Pts',(59.7,244.156434931344,18.1516008291015)) ;
#94079 = CARTESIAN_POINT('Ctrl Pts',(59.7,244.147690779557,18.1437942097801)) ;
#94080 = CARTESIAN_POINT('Origin',(59.6,243.65,18.5618897586017)) ;
#94081 = CARTESIAN_POINT('',(59.7,243.855548047911,17.9452456148689)) ;
#94082 = CARTESIAN_POINT('',(59.6,243.887170824513,17.8503772850638)) ;
#94083 = CARTESIAN_POINT('Origin',(59.6,243.855548047911,17.9452456148689)) ;
#94084 = CARTESIAN_POINT('Origin',(59.6,243.65,18.5618897586017)) ;
#94085 = CARTESIAN_POINT('Origin',(59.7,243.65,18.5618897586017)) ;
#94086 = CARTESIAN_POINT('Origin',(59.6,242.688377223398,17.5561886733647)) ;
#94087 = CARTESIAN_POINT('',(59.6,242.72,17.4613203435596)) ;
#94088 = CARTESIAN_POINT('',(59.7,242.688377223398,17.5561886733647)) ;
#94089 = CARTESIAN_POINT('Origin',(59.8,242.1,24.0213203435596)) ;
#94090 = CARTESIAN_POINT('',(59.8,242.,24.0213203435596)) ;
#94091 = CARTESIAN_POINT('',(59.7,242.1,24.0213203435596)) ;
#94092 = CARTESIAN_POINT('Origin',(59.8,242.1,24.0213203435596)) ;
#94093 = CARTESIAN_POINT('',(59.8,242.,24.0213203435596)) ;
#94094 = CARTESIAN_POINT('',(59.7,242.1,24.0213203435596)) ;
#94095 = CARTESIAN_POINT('Origin',(67.0732152677426,241.9,17.2933962655652)) ;
#94096 = CARTESIAN_POINT('',(67.0732152677426,241.931622776602,17.1985279357602)) ;
#94097 = CARTESIAN_POINT('',(67.0732152677426,242.,17.2933962655652)) ;
#94098 = CARTESIAN_POINT('Origin',(65.6,242.1,24.0213203435596)) ;
#94099 = CARTESIAN_POINT('',(65.7,242.1,24.0213203435596)) ;
#94100 = CARTESIAN_POINT('',(65.6,242.,24.0213203435596)) ;
#94101 = CARTESIAN_POINT('Origin',(65.6,242.1,24.0213203435596)) ;
#94102 = CARTESIAN_POINT('',(65.7,242.1,24.0213203435596)) ;
#94103 = CARTESIAN_POINT('',(65.6,242.,24.0213203435596)) ;
#94104 = CARTESIAN_POINT('Origin',(65.8,243.768377223398,17.9161886733647)) ;
#94105 = CARTESIAN_POINT('',(65.8,244.031622776602,17.8985279357602)) ;
#94106 = CARTESIAN_POINT('Origin',(65.8,244.,17.9933962655652)) ;
#94107 = CARTESIAN_POINT('',(65.8,243.8,17.8213203435596)) ;
#94108 = CARTESIAN_POINT('',(65.7,243.768377223398,17.9161886733647)) ;
#94109 = CARTESIAN_POINT('Ctrl Pts',(65.9404964381473,244.284865061027,17.9829450296875)) ;
#94110 = CARTESIAN_POINT('Ctrl Pts',(65.8548709640911,244.23093375671,17.9649691455176)) ;
#94111 = CARTESIAN_POINT('Ctrl Pts',(65.8002174113109,244.131095361456,17.9316866080974)) ;
#94112 = CARTESIAN_POINT('Ctrl Pts',(65.8008983432499,244.029922223798,17.8979656321695)) ;
#94113 = CARTESIAN_POINT('Ctrl Pts',(65.926661685959,244.304690467608,17.9893497096592)) ;
#94114 = CARTESIAN_POINT('Ctrl Pts',(65.8331874853583,244.247141411488,17.9701164230807)) ;
#94115 = CARTESIAN_POINT('Ctrl Pts',(65.7720145633604,244.1402530333,17.9345713375739)) ;
#94116 = CARTESIAN_POINT('Ctrl Pts',(65.7706405073659,244.029858881983,17.8976377622117)) ;
#94117 = CARTESIAN_POINT('Ctrl Pts',(65.9026183136662,244.33370948865,18.0167815320695)) ;
#94118 = CARTESIAN_POINT('Ctrl Pts',(65.7955896720674,244.269304088194,17.9969915494265)) ;
#94119 = CARTESIAN_POINT('Ctrl Pts',(65.7229721832936,244.149101928229,17.9601104641158)) ;
#94120 = CARTESIAN_POINT('Ctrl Pts',(65.7183227383958,244.021629003268,17.9214387220682)) ;
#94121 = CARTESIAN_POINT('Ctrl Pts',(65.889532984467,244.340167226494,18.0597208762946)) ;
#94122 = CARTESIAN_POINT('Ctrl Pts',(65.7760178032742,244.270022860549,18.0411808238425)) ;
#94123 = CARTESIAN_POINT('Ctrl Pts',(65.701573447933,244.139670349221,18.0067716316214)) ;
#94124 = CARTESIAN_POINT('Ctrl Pts',(65.699966159831,244.004831770862,17.9715157748671)) ;
#94125 = CARTESIAN_POINT('Ctrl Pts',(65.8867840653894,244.338435475849,18.0780051345276)) ;
#94126 = CARTESIAN_POINT('Ctrl Pts',(65.7723078698088,244.266384553046,18.0599924038268)) ;
#94127 = CARTESIAN_POINT('Ctrl Pts',(65.6991798482406,244.132988977868,18.0266435100323)) ;
#94128 = CARTESIAN_POINT('Ctrl Pts',(65.700006943225,243.997728300858,17.9928283407797)) ;
#94129 = CARTESIAN_POINT('',(65.9386488833497,244.284537420614,17.9828328170975)) ;
#94130 = CARTESIAN_POINT('Origin',(65.9386488833497,244.252914644012,18.0777011469026)) ;
#94131 = CARTESIAN_POINT('Origin',(66.1,244.031622776602,17.8985279357602)) ;
#94132 = CARTESIAN_POINT('Ctrl Pts',(65.8848651777997,244.337219525349,18.0777011469026)) ;
#94133 = CARTESIAN_POINT('Ctrl Pts',(65.9479936757444,244.377493403818,18.0877696165197)) ;
#94134 = CARTESIAN_POINT('Ctrl Pts',(66.0239249506928,244.4,18.0918966374184)) ;
#94135 = CARTESIAN_POINT('Ctrl Pts',(66.1,244.4,18.0918966374184)) ;
#94136 = CARTESIAN_POINT('Ctrl Pts',(65.8885516400003,244.339571365413,18.0533102596963)) ;
#94137 = CARTESIAN_POINT('Ctrl Pts',(65.9506433947663,244.378209794597,18.0630973328873)) ;
#94138 = CARTESIAN_POINT('Ctrl Pts',(66.0251770337231,244.4,18.0670030923248)) ;
#94139 = CARTESIAN_POINT('Ctrl Pts',(66.1,244.4,18.0670030923248)) ;
#94140 = CARTESIAN_POINT('Ctrl Pts',(65.9040598961178,244.329415666601,18.0108507134782)) ;
#94141 = CARTESIAN_POINT('Ctrl Pts',(65.9615840543736,244.363516408185,18.0201474104081)) ;
#94142 = CARTESIAN_POINT('Ctrl Pts',(66.0306825545291,244.382934786786,18.0236727418492)) ;
#94143 = CARTESIAN_POINT('Ctrl Pts',(66.1,244.382934786786,18.0236727418492)) ;
#94144 = CARTESIAN_POINT('Ctrl Pts',(65.9282779384441,244.299168044213,17.9877096916306)) ;
#94145 = CARTESIAN_POINT('Ctrl Pts',(65.9786741316863,244.32791510767,17.9966840244951)) ;
#94146 = CARTESIAN_POINT('Ctrl Pts',(66.0392695942916,244.344107193227,18.0002280477271)) ;
#94147 = CARTESIAN_POINT('Ctrl Pts',(66.1,244.344107193227,18.0002280477271)) ;
#94148 = CARTESIAN_POINT('Ctrl Pts',(65.9386488833498,244.284537420614,17.9828328170975)) ;
#94149 = CARTESIAN_POINT('Ctrl Pts',(65.9859952568083,244.311189251953,17.9917167608773)) ;
#94150 = CARTESIAN_POINT('Ctrl Pts',(66.0429437130196,244.326083322956,17.9953582499056)) ;
#94151 = CARTESIAN_POINT('Ctrl Pts',(66.1,244.326083322956,17.9953582499056)) ;
#94152 = CARTESIAN_POINT('Ctrl Pts',(66.1,244.326083322956,17.9953582499056)) ;
#94153 = CARTESIAN_POINT('Ctrl Pts',(66.0429437130196,244.326083322956,17.9953582499056)) ;
#94154 = CARTESIAN_POINT('Ctrl Pts',(65.9859952568083,244.311189251953,17.9917167608773)) ;
#94155 = CARTESIAN_POINT('Ctrl Pts',(65.9386488833498,244.284537420614,17.9828328170975)) ;
#94156 = CARTESIAN_POINT('Origin',(59.3,244.147690779557,18.0213203435596)) ;
#94157 = CARTESIAN_POINT('',(59.5361339486826,244.47055415357,24.0213203435596)) ;
#94158 = CARTESIAN_POINT('',(59.5361339486826,244.47055415357,18.0213203435596)) ;
#94159 = CARTESIAN_POINT('',(59.7,244.147690779557,24.0213203435596)) ;
#94160 = CARTESIAN_POINT('Origin',(59.3,244.147690779557,24.0213203435596)) ;
#94161 = CARTESIAN_POINT('',(59.7,244.147690779557,18.0213203435596)) ;
#94162 = CARTESIAN_POINT('Origin',(59.7,244.4,24.0213203435596)) ;
#94163 = CARTESIAN_POINT('',(64.0732152677426,244.4,18.5618897586017)) ;
#94164 = CARTESIAN_POINT('Origin',(64.0732152677426,243.65,18.5618897586017)) ;
#94165 = CARTESIAN_POINT('',(64.0732152677426,243.887170824513,17.8503772850638)) ;
#94166 = CARTESIAN_POINT('Origin',(68.4464305354851,241.4,17.0213203435596)) ;
#94167 = CARTESIAN_POINT('',(70.7915467797171,244.284537420614,17.9828328170975)) ;
#94168 = CARTESIAN_POINT('',(61.8303059750075,244.284537420614,17.9828328170975)) ;
#94169 = CARTESIAN_POINT('',(68.4423055214479,238.515462579386,16.0598078700218)) ;
#94170 = CARTESIAN_POINT('Origin',(74.5283628290597,239.4,16.3546536768929)) ;
#94171 = CARTESIAN_POINT('',(69.2696458032277,238.515462579386,16.0598078700217)) ;
#94172 = CARTESIAN_POINT('Origin',(61.8303059750075,244.521708245126,17.2713203435596)) ;
#94173 = CARTESIAN_POINT('',(68.3954399375726,244.400001501795,18.0113751658507)) ;
#94174 = CARTESIAN_POINT('Origin',(68.7866534367343,244.532775091534,17.7025224033626)) ;
#94175 = CARTESIAN_POINT('',(68.3828427124747,244.521708245126,18.0213203435596)) ;
#94176 = CARTESIAN_POINT('Origin',(69.3328427124747,244.521708245126,17.2713203435596)) ;
#94177 = CARTESIAN_POINT('',(71.1238651198807,244.521708245126,18.0213203435596)) ;
#94178 = CARTESIAN_POINT('',(61.8303059750075,244.521708245126,18.0213203435596)) ;
#94179 = CARTESIAN_POINT('Ctrl Pts',(71.1238651198807,244.521708245126,18.0213203435596)) ;
#94180 = CARTESIAN_POINT('Ctrl Pts',(71.0892631962886,244.498707682821,18.0213203435596)) ;
#94181 = CARTESIAN_POINT('Ctrl Pts',(71.0540815843477,244.474813864772,18.0202605768952)) ;
#94182 = CARTESIAN_POINT('Ctrl Pts',(71.0186887369256,244.450216947004,18.0179052310927)) ;
#94183 = CARTESIAN_POINT('Ctrl Pts',(70.983961512167,244.426082616089,18.0155941815721)) ;
#94184 = CARTESIAN_POINT('Ctrl Pts',(70.9490309224995,244.401271595668,18.0120351354193)) ;
#94185 = CARTESIAN_POINT('Ctrl Pts',(70.9142450211489,244.376005954662,18.0070314570774)) ;
#94186 = CARTESIAN_POINT('Ctrl Pts',(70.88019684882,244.351276139836,18.0021338952536)) ;
#94187 = CARTESIAN_POINT('Ctrl Pts',(70.8462872928706,244.326111176708,17.9958517649843)) ;
#94188 = CARTESIAN_POINT('Ctrl Pts',(70.8128427286074,244.300755833278,17.9880350927442)) ;
#94189 = CARTESIAN_POINT('Ctrl Pts',(70.8057219499922,244.295357353996,17.986370822518)) ;
#94190 = CARTESIAN_POINT('Ctrl Pts',(70.7986222503317,244.289950365561,17.98463713208)) ;
#94191 = CARTESIAN_POINT('Ctrl Pts',(70.7915467797171,244.284537420614,17.9828328170977)) ;
#94192 = CARTESIAN_POINT('Origin',(66.9,250.2125,19.5627416997969)) ;
#94193 = CARTESIAN_POINT('',(66.8,245.395181184141,19.562741699797)) ;
#94194 = CARTESIAN_POINT('',(66.8,252.,19.5627416997969)) ;
#94195 = CARTESIAN_POINT('',(66.8,250.2125,19.5627416997969)) ;
#94196 = CARTESIAN_POINT('Origin',(66.9,251.9,19.5627416997969)) ;
#94197 = CARTESIAN_POINT('Origin',(66.9,245.358578643763,19.5627416997969)) ;
#94198 = CARTESIAN_POINT('Origin',(66.9651142374916,245.423692881254,19.4976274623054)) ;
#94199 = CARTESIAN_POINT('',(65.7,244.229289321881,20.6213203435597)) ;
#94200 = CARTESIAN_POINT('',(66.8944035593729,245.423692881254,19.4269167841868)) ;
#94201 = CARTESIAN_POINT('',(65.7,244.3,20.6920310216783)) ;
#94202 = CARTESIAN_POINT('Origin',(65.7,244.158578643763,20.762741699797)) ;
#94203 = CARTESIAN_POINT('',(66.8,245.4,19.5920310216783)) ;
#94204 = CARTESIAN_POINT('',(66.8944035593729,245.494403559373,19.4976274623054)) ;
#94205 = CARTESIAN_POINT('Origin',(66.8,245.258578643763,19.6627416997969)) ;
#94206 = CARTESIAN_POINT('Origin',(66.8,250.6,24.0213203435596)) ;
#94207 = CARTESIAN_POINT('',(66.8,252.,24.0213203435596)) ;
#94208 = CARTESIAN_POINT('',(66.8,245.4,24.0213203435596)) ;
#94209 = CARTESIAN_POINT('',(66.8,245.4,24.0213203435596)) ;
#94210 = CARTESIAN_POINT('',(66.8,252.,24.0213203435596)) ;
#94211 = CARTESIAN_POINT('',(66.8000000000001,244.4,24.0213203435596)) ;
#94212 = CARTESIAN_POINT('',(66.8,252.,23.0213203435596)) ;
#94213 = CARTESIAN_POINT('',(66.8,252.,24.0213203435596)) ;
#94214 = CARTESIAN_POINT('',(66.8,251.2,23.0213203435596)) ;
#94215 = CARTESIAN_POINT('Origin',(66.3,244.9,24.0213203435596)) ;
#94216 = CARTESIAN_POINT('',(65.7,244.3,24.0213203435596)) ;
#94217 = CARTESIAN_POINT('',(65.7,244.3,24.0213203435596)) ;
#94218 = CARTESIAN_POINT('',(66.0500000000001,244.65,24.0213203435596)) ;
#94219 = CARTESIAN_POINT('Origin',(65.7,244.4,24.0213203435596)) ;
#94220 = CARTESIAN_POINT('',(65.7,253.,24.0213203435596)) ;
#94221 = CARTESIAN_POINT('',(65.7,247.1125,20.6213203435596)) ;
#94222 = CARTESIAN_POINT('Ctrl Pts',(59.6215180227928,252.943103132053,20.0052643657055)) ;
#94223 = CARTESIAN_POINT('Ctrl Pts',(59.4587725290195,252.824132060153,19.9903878946469)) ;
#94224 = CARTESIAN_POINT('Ctrl Pts',(59.2951932514256,252.704225739539,19.9662044395718)) ;
#94225 = CARTESIAN_POINT('Ctrl Pts',(59.1497059100836,252.591093317904,19.9188077169749)) ;
#94226 = CARTESIAN_POINT('Ctrl Pts',(59.6134529174683,252.961577359466,19.9973173267384)) ;
#94227 = CARTESIAN_POINT('Ctrl Pts',(59.4484449972835,252.850355285,19.975257967573)) ;
#94228 = CARTESIAN_POINT('Ctrl Pts',(59.2832533401182,252.736942886568,19.9376027653372)) ;
#94229 = CARTESIAN_POINT('Ctrl Pts',(59.1526056913556,252.627429846356,19.8774372154673)) ;
#94230 = CARTESIAN_POINT('Ctrl Pts',(59.5953124915619,253.000455378881,19.9879673050628)) ;
#94231 = CARTESIAN_POINT('Ctrl Pts',(59.4229785428761,252.907413224572,19.9572312235567)) ;
#94232 = CARTESIAN_POINT('Ctrl Pts',(59.2498021909738,252.812198346872,19.9031169114175)) ;
#94233 = CARTESIAN_POINT('Ctrl Pts',(59.127813604899,252.728969853432,19.818935866661)) ;
#94234 = CARTESIAN_POINT('Ctrl Pts',(59.5750531169448,253.039128908801,19.9926485628779)) ;
#94235 = CARTESIAN_POINT('Ctrl Pts',(59.392366555406,252.963955576352,19.9661862864617)) ;
#94236 = CARTESIAN_POINT('Ctrl Pts',(59.2086840835645,252.888185966827,19.9217979904099)) ;
#94237 = CARTESIAN_POINT('Ctrl Pts',(59.0586509200866,252.823325335416,19.8446456789754)) ;
#94238 = CARTESIAN_POINT('Ctrl Pts',(59.5649218537582,253.057403741307,19.9983832323394)) ;
#94239 = CARTESIAN_POINT('Ctrl Pts',(59.3770535644003,252.989679071533,19.9771311308272)) ;
#94240 = CARTESIAN_POINT('Ctrl Pts',(59.1883855218148,252.921262994303,19.9425833378629)) ;
#94241 = CARTESIAN_POINT('Ctrl Pts',(59.0238256449734,252.853553390593,19.8748737341529)) ;
#94242 = CARTESIAN_POINT('',(59.1497059100836,252.591093317904,19.9188077169749)) ;
#94243 = CARTESIAN_POINT('Ctrl Pts',(59.542455661465,252.885254883942,19.9972444447401)) ;
#94244 = CARTESIAN_POINT('Ctrl Pts',(59.4062589370116,252.785468535468,19.9819452098712)) ;
#94245 = CARTESIAN_POINT('Ctrl Pts',(59.2716294139949,252.685902262273,19.95852783585)) ;
#94246 = CARTESIAN_POINT('Ctrl Pts',(59.1497059100836,252.591093317904,19.9188077169749)) ;
#94247 = CARTESIAN_POINT('Origin',(59.0238256449734,252.712132034356,20.0162950903902)) ;
#94248 = CARTESIAN_POINT('Origin',(57.5854307313793,251.289402981384,18.5935660374187)) ;
#94249 = CARTESIAN_POINT('Origin',(58.508445556536,252.249338399547,19.5535014555817)) ;
#94250 = CARTESIAN_POINT('Origin',(58.7659637180533,252.517157287525,19.8213203435596)) ;
#94251 = CARTESIAN_POINT('Ctrl Pts',(58.7659637180532,252.658578643763,19.6798989873223)) ;
#94252 = CARTESIAN_POINT('Ctrl Pts',(58.8312395983061,252.726465559226,19.7477859027853)) ;
#94253 = CARTESIAN_POINT('Ctrl Pts',(58.9209234411789,252.794277371414,19.815597714974)) ;
#94254 = CARTESIAN_POINT('Ctrl Pts',(59.0238256449735,252.853553390593,19.8748737341529)) ;
#94255 = CARTESIAN_POINT('Ctrl Pts',(58.7987744253355,252.642804265262,19.6641246088212)) ;
#94256 = CARTESIAN_POINT('Ctrl Pts',(58.8593200371507,252.709067270073,19.7304450892964)) ;
#94257 = CARTESIAN_POINT('Ctrl Pts',(58.9447138592872,252.776719345374,19.7980061774175)) ;
#94258 = CARTESIAN_POINT('Ctrl Pts',(59.043725802181,252.836280216206,19.8576005597657)) ;
#94259 = CARTESIAN_POINT('Ctrl Pts',(58.8560072121908,252.600153838287,19.6517435099733)) ;
#94260 = CARTESIAN_POINT('Ctrl Pts',(58.9083980147272,252.665691705911,19.7131626692118)) ;
#94261 = CARTESIAN_POINT('Ctrl Pts',(58.9862562096281,252.734888009256,19.7784583013549)) ;
#94262 = CARTESIAN_POINT('Ctrl Pts',(59.0785034559233,252.796663641143,19.8368436943977)) ;
#94263 = CARTESIAN_POINT('Ctrl Pts',(58.9193709157606,252.511947666345,19.6790230438673)) ;
#94264 = CARTESIAN_POINT('Ctrl Pts',(58.966096968321,252.57969046616,19.7287746196292)) ;
#94265 = CARTESIAN_POINT('Ctrl Pts',(59.0374007547605,252.653426585229,19.7848110624398)) ;
#94266 = CARTESIAN_POINT('Ctrl Pts',(59.1228031445117,252.720566563636,19.8360372340782)) ;
#94267 = CARTESIAN_POINT('Ctrl Pts',(58.939090293356,252.431231488413,19.7407782818034)) ;
#94268 = CARTESIAN_POINT('Ctrl Pts',(58.9902256027549,252.50112873637,19.7794810364602)) ;
#94269 = CARTESIAN_POINT('Ctrl Pts',(59.063052354485,252.577729006518,19.8236599443425)) ;
#94270 = CARTESIAN_POINT('Ctrl Pts',(59.1476646149207,252.648970096141,19.8644745938916)) ;
#94271 = CARTESIAN_POINT('Ctrl Pts',(58.9221907728626,252.391078403777,19.7971809053757)) ;
#94272 = CARTESIAN_POINT('Ctrl Pts',(58.9828221520423,252.460001328931,19.8317384222115)) ;
#94273 = CARTESIAN_POINT('Ctrl Pts',(59.0623707400732,252.535288497676,19.8682866555266)) ;
#94274 = CARTESIAN_POINT('Ctrl Pts',(59.1509486734859,252.606666115812,19.9010775020431)) ;
#94275 = CARTESIAN_POINT('Ctrl Pts',(58.9101303310336,252.378535544275,19.8213203435596)) ;
#94276 = CARTESIAN_POINT('Ctrl Pts',(58.9754062112864,252.446422459738,19.8552638012911)) ;
#94277 = CARTESIAN_POINT('Ctrl Pts',(59.0587301003317,252.520349612145,19.8891697073854)) ;
#94278 = CARTESIAN_POINT('Ctrl Pts',(59.1497059100837,252.591093317904,19.9188077169749)) ;
#94279 = CARTESIAN_POINT('Origin',(59.3208772194954,252.517157287525,19.8213203435596)) ;
#94280 = CARTESIAN_POINT('Ctrl Pts',(58.6541618099201,252.112319238985,19.5569044323066)) ;
#94281 = CARTESIAN_POINT('Ctrl Pts',(58.6412166009376,252.099019648315,19.5315608669829)) ;
#94282 = CARTESIAN_POINT('Ctrl Pts',(58.6089650298832,252.060786697827,19.4580880570343)) ;
#94283 = CARTESIAN_POINT('Ctrl Pts',(58.5547081014922,252.00171431334,19.3867568112521)) ;
#94284 = CARTESIAN_POINT('Ctrl Pts',(58.5216837989603,251.967622766116,19.3539222570156)) ;
#94285 = CARTESIAN_POINT('Ctrl Pts',(58.6704529317958,252.128834613613,19.5244813361219)) ;
#94286 = CARTESIAN_POINT('Ctrl Pts',(58.6563632481609,252.11721748364,19.5005676840661)) ;
#94287 = CARTESIAN_POINT('Ctrl Pts',(58.6192697049124,252.081148152115,19.4296226050024)) ;
#94288 = CARTESIAN_POINT('Ctrl Pts',(58.5632183786603,252.021835092628,19.3587907782628)) ;
#94289 = CARTESIAN_POINT('Ctrl Pts',(58.5301886892986,251.987547381425,19.325699698679)) ;
#94290 = CARTESIAN_POINT('Ctrl Pts',(58.6834103241829,252.172743456881,19.4679237313148)) ;
#94291 = CARTESIAN_POINT('Ctrl Pts',(58.6670478349588,252.162202291369,19.4467076700389)) ;
#94292 = CARTESIAN_POINT('Ctrl Pts',(58.6224726974963,252.126421961247,19.3816931047035)) ;
#94293 = CARTESIAN_POINT('Ctrl Pts',(58.5644098772969,252.066679637707,19.3128450049597)) ;
#94294 = CARTESIAN_POINT('Ctrl Pts',(58.5315660192152,252.032390152714,19.2795140331204)) ;
#94295 = CARTESIAN_POINT('Ctrl Pts',(58.6559664334228,252.262045840093,19.4054163366162)) ;
#94296 = CARTESIAN_POINT('Ctrl Pts',(58.636535671422,252.248751266018,19.3866086493998)) ;
#94297 = CARTESIAN_POINT('Ctrl Pts',(58.5862516151643,252.206525568018,19.329729810431)) ;
#94298 = CARTESIAN_POINT('Ctrl Pts',(58.5288429323904,252.146723044933,19.2656131002727)) ;
#94299 = CARTESIAN_POINT('Ctrl Pts',(58.4967383304864,252.113266200792,19.232617788478)) ;
#94300 = CARTESIAN_POINT('Ctrl Pts',(58.5932444721227,252.342557495049,19.3861425626071)) ;
#94301 = CARTESIAN_POINT('Ctrl Pts',(58.5718821662184,252.324168403092,19.3666955691386)) ;
#94302 = CARTESIAN_POINT('Ctrl Pts',(58.5221767212164,252.27324709964,19.3129859822417)) ;
#94303 = CARTESIAN_POINT('Ctrl Pts',(58.4683968239059,252.214587012998,19.2535098455819)) ;
#94304 = CARTESIAN_POINT('Ctrl Pts',(58.4372786347936,252.182442930322,19.2214525899989)) ;
#94305 = CARTESIAN_POINT('Ctrl Pts',(58.5358524085125,252.381707064668,19.4030284834634)) ;
#94306 = CARTESIAN_POINT('Ctrl Pts',(58.5135668240936,252.35975300744,19.3810656990374)) ;
#94307 = CARTESIAN_POINT('Ctrl Pts',(58.466576100367,252.304160763346,19.3254641250641)) ;
#94308 = CARTESIAN_POINT('Ctrl Pts',(58.4164010358533,252.2473691237,19.2686897384215)) ;
#94309 = CARTESIAN_POINT('Ctrl Pts',(58.3860774651112,252.216264757314,19.2375851065789)) ;
#94310 = CARTESIAN_POINT('Ctrl Pts',(58.5112912559021,252.39369690533,19.4150172488892)) ;
#94311 = CARTESIAN_POINT('Ctrl Pts',(58.488596480636,252.370452373203,19.3917727167619)) ;
#94312 = CARTESIAN_POINT('Ctrl Pts',(58.4427445299486,252.313461846912,19.334782190472)) ;
#94313 = CARTESIAN_POINT('Ctrl Pts',(58.3941384948706,252.257638852692,19.2789591962518)) ;
#94314 = CARTESIAN_POINT('Ctrl Pts',(58.3641533318596,252.226959669971,19.2482800135306)) ;
#94315 = CARTESIAN_POINT('',(58.5249792341639,251.971066018137,19.3570204704755)) ;
#94316 = CARTESIAN_POINT('Origin',(58.3670916964374,252.088555764606,19.3927188206398)) ;
#94317 = CARTESIAN_POINT('Ctrl Pts',(58.6524986843825,252.11059862929,19.5535233690183)) ;
#94318 = CARTESIAN_POINT('Ctrl Pts',(58.6490777400388,252.107038472653,19.5466722663875)) ;
#94319 = CARTESIAN_POINT('Ctrl Pts',(58.6456004439748,252.103274227079,19.5393615524109)) ;
#94320 = CARTESIAN_POINT('Ctrl Pts',(58.6419741682487,252.099258925526,19.5317637793487)) ;
#94321 = CARTESIAN_POINT('Ctrl Pts',(58.6384200614618,252.095323535175,19.5243172146512)) ;
#94322 = CARTESIAN_POINT('Ctrl Pts',(58.6347225086479,252.091146337458,19.5165945586219)) ;
#94323 = CARTESIAN_POINT('Ctrl Pts',(58.630821440443,252.086704458926,19.5087232340329)) ;
#94324 = CARTESIAN_POINT('Ctrl Pts',(58.6269702679149,252.082319393175,19.5009525857324)) ;
#94325 = CARTESIAN_POINT('Ctrl Pts',(58.6229207512004,252.077676015761,19.4930368668497)) ;
#94326 = CARTESIAN_POINT('Ctrl Pts',(58.6186441018831,252.072780693303,19.4850679359159)) ;
#94327 = CARTESIAN_POINT('Ctrl Pts',(58.6156853025889,252.069393865074,19.4795546320481)) ;
#94328 = CARTESIAN_POINT('Ctrl Pts',(58.6126184029932,252.065887060929,19.4740152306126)) ;
#94329 = CARTESIAN_POINT('Ctrl Pts',(58.60944188193,252.062271443542,19.4684719115025)) ;
#94330 = CARTESIAN_POINT('Ctrl Pts',(58.6043334334077,252.056456844825,19.4595572026895)) ;
#94331 = CARTESIAN_POINT('Ctrl Pts',(58.5989562698347,252.050376860908,19.450675029644)) ;
#94332 = CARTESIAN_POINT('Ctrl Pts',(58.5932897765977,252.04404070345,19.4418943388873)) ;
#94333 = CARTESIAN_POINT('Ctrl Pts',(58.5875867409455,252.037663685006,19.4330570226952)) ;
#94334 = CARTESIAN_POINT('Ctrl Pts',(58.5815906397197,252.031027137424,19.4243225888452)) ;
#94335 = CARTESIAN_POINT('Ctrl Pts',(58.5753214413841,252.024174076536,19.4157649379888)) ;
#94336 = CARTESIAN_POINT('Ctrl Pts',(58.5689961570257,252.017259706225,19.4071307279657)) ;
#94337 = CARTESIAN_POINT('Ctrl Pts',(58.5623928420313,252.010125071074,19.3986767325429)) ;
#94338 = CARTESIAN_POINT('Ctrl Pts',(58.5555738544669,252.002847655641,19.3904798460872)) ;
#94339 = CARTESIAN_POINT('Ctrl Pts',(58.5485973256502,251.99540210775,19.3820935843401)) ;
#94340 = CARTESIAN_POINT('Ctrl Pts',(58.5413950213182,251.987807285818,19.3739767810072)) ;
#94341 = CARTESIAN_POINT('Ctrl Pts',(58.5340779798077,251.980178469763,19.366208203947)) ;
#94342 = CARTESIAN_POINT('Ctrl Pts',(58.5311233572343,251.977097952577,19.3630712512438)) ;
#94343 = CARTESIAN_POINT('Ctrl Pts',(58.5281505221452,251.974012237786,19.3599910098373)) ;
#94344 = CARTESIAN_POINT('Ctrl Pts',(58.5251687296973,251.970930243872,19.3569723289424)) ;
#94345 = CARTESIAN_POINT('Ctrl Pts',(58.524967204456,251.971078582415,19.3570195820997)) ;
#94346 = CARTESIAN_POINT('Ctrl Pts',(58.1932634960872,251.627647614635,19.0202451972619)) ;
#94347 = CARTESIAN_POINT('Ctrl Pts',(57.8654129205822,251.287968355625,18.6871483232392)) ;
#94348 = CARTESIAN_POINT('Ctrl Pts',(57.5423066932673,250.95296417531,18.3586344366773)) ;
#94349 = CARTESIAN_POINT('Ctrl Pts',(58.5334325604522,251.991006744364,19.328878031335)) ;
#94350 = CARTESIAN_POINT('Ctrl Pts',(58.202537180283,251.647324552634,18.9915783013781)) ;
#94351 = CARTESIAN_POINT('Ctrl Pts',(57.8754995261934,251.307368901923,18.6579788187517)) ;
#94352 = CARTESIAN_POINT('Ctrl Pts',(57.5532400350036,250.972037111679,18.328983776375)) ;
#94353 = CARTESIAN_POINT('Ctrl Pts',(58.5347701387631,252.035810849651,19.2827761601016)) ;
#94354 = CARTESIAN_POINT('Ctrl Pts',(58.205003850642,251.692198114189,18.9443126242704)) ;
#94355 = CARTESIAN_POINT('Ctrl Pts',(57.8791543584745,251.352251162712,18.6095560812731)) ;
#94356 = CARTESIAN_POINT('Ctrl Pts',(57.5581161076161,251.016886757035,18.279416657513)) ;
#94357 = CARTESIAN_POINT('Ctrl Pts',(58.4998940599975,252.116554687307,19.2358703317831)) ;
#94358 = CARTESIAN_POINT('Ctrl Pts',(58.1707506410098,251.773947691982,18.8957653654841)) ;
#94359 = CARTESIAN_POINT('Ctrl Pts',(57.8455821936292,251.434982083835,18.5593363592066)) ;
#94360 = CARTESIAN_POINT('Ctrl Pts',(57.525280969944,251.100564766762,18.227505789981)) ;
#94361 = CARTESIAN_POINT('Ctrl Pts',(58.4403340595383,252.185604669324,19.2246075759389)) ;
#94362 = CARTESIAN_POINT('Ctrl Pts',(58.1107466473917,251.844202743674,18.8836747590476)) ;
#94363 = CARTESIAN_POINT('Ctrl Pts',(57.7851546063529,251.506441300288,18.5463966965541)) ;
#94364 = CARTESIAN_POINT('Ctrl Pts',(57.4644511534692,251.173238980184,18.2136828428116)) ;
#94365 = CARTESIAN_POINT('Ctrl Pts',(58.3890508349148,252.219324353113,19.2406446966726)) ;
#94366 = CARTESIAN_POINT('Ctrl Pts',(58.0587653814927,251.878470792537,18.899794609743)) ;
#94367 = CARTESIAN_POINT('Ctrl Pts',(57.7324871267912,251.541263118157,18.5625797539281)) ;
#94368 = CARTESIAN_POINT('Ctrl Pts',(57.4110825009508,251.208617131752,18.2299374753112)) ;
#94369 = CARTESIAN_POINT('Ctrl Pts',(58.3670916964373,252.229977120843,19.2512974644025)) ;
#94370 = CARTESIAN_POINT('Ctrl Pts',(58.0365134267979,251.889257498265,18.9105778418249)) ;
#94371 = CARTESIAN_POINT('Ctrl Pts',(57.7099315251708,251.552182999603,18.5735033431626)) ;
#94372 = CARTESIAN_POINT('Ctrl Pts',(57.3882337581722,251.21966991411,18.2409902576697)) ;
#94373 = CARTESIAN_POINT('',(57.5423066932673,250.95296417531,18.3586344366773)) ;
#94374 = CARTESIAN_POINT('Origin',(57.3882337581722,251.078248557873,18.382411613907)) ;
#94375 = CARTESIAN_POINT('Origin',(62.771739895016,256.106054470067,23.4102175261011)) ;
#94376 = CARTESIAN_POINT('Ctrl Pts',(57.08796902046,250.694045291555,18.0213351046284)) ;
#94377 = CARTESIAN_POINT('Ctrl Pts',(57.1258423453833,250.802045427011,18.0220127055346)) ;
#94378 = CARTESIAN_POINT('Ctrl Pts',(57.2314306338671,250.992507784516,18.066477901939)) ;
#94379 = CARTESIAN_POINT('Ctrl Pts',(57.3390787831373,251.150386903953,18.1717072475128)) ;
#94380 = CARTESIAN_POINT('Ctrl Pts',(57.3882337581722,251.21966991411,18.2409902576698)) ;
#94381 = CARTESIAN_POINT('Ctrl Pts',(57.107641411712,250.684638364735,18.0212760848678)) ;
#94382 = CARTESIAN_POINT('Ctrl Pts',(57.1469906807295,250.788268335791,18.0205613562701)) ;
#94383 = CARTESIAN_POINT('Ctrl Pts',(57.255633922619,250.973466511641,18.0590773371353)) ;
#94384 = CARTESIAN_POINT('Ctrl Pts',(57.3675725762443,251.133340840632,18.1585412492811)) ;
#94385 = CARTESIAN_POINT('Ctrl Pts',(57.4186987485437,251.204932870965,18.2262532145251)) ;
#94386 = CARTESIAN_POINT('Ctrl Pts',(57.1420566838705,250.668142088394,18.027486377803)) ;
#94387 = CARTESIAN_POINT('Ctrl Pts',(57.183976115983,250.763206632424,18.0262403194019)) ;
#94388 = CARTESIAN_POINT('Ctrl Pts',(57.2979617793206,250.935859716831,18.0586106436234)) ;
#94389 = CARTESIAN_POINT('Ctrl Pts',(57.4173496108119,251.093267835686,18.1493153206436)) ;
#94390 = CARTESIAN_POINT('Ctrl Pts',(57.4718803430079,251.166163965728,18.2135703095001)) ;
#94391 = CARTESIAN_POINT('Ctrl Pts',(57.1911537271729,250.64450016656,18.0535964453211)) ;
#94392 = CARTESIAN_POINT('Ctrl Pts',(57.235290594596,250.72552619711,18.0564256989547)) ;
#94393 = CARTESIAN_POINT('Ctrl Pts',(57.3527071216605,250.875068403139,18.0913312692755)) ;
#94394 = CARTESIAN_POINT('Ctrl Pts',(57.4769453332363,251.017240971583,18.1755695140533)) ;
#94395 = CARTESIAN_POINT('Ctrl Pts',(57.533955734056,251.085548454793,18.2341294931593)) ;
#94396 = CARTESIAN_POINT('Ctrl Pts',(57.2280967504656,250.626602169704,18.0905610922877)) ;
#94397 = CARTESIAN_POINT('Ctrl Pts',(57.2715143002045,250.695684375206,18.1008339037926)) ;
#94398 = CARTESIAN_POINT('Ctrl Pts',(57.3847356823201,250.825549532579,18.1472995157663)) ;
#94399 = CARTESIAN_POINT('Ctrl Pts',(57.5038966823451,250.949199444535,18.2321302434064)) ;
#94400 = CARTESIAN_POINT('Ctrl Pts',(57.5592426011106,251.009151616513,18.2860619448616)) ;
#94401 = CARTESIAN_POINT('Ctrl Pts',(57.2461791971729,250.61774963895,18.1233215980465)) ;
#94402 = CARTESIAN_POINT('Ctrl Pts',(57.2865158711383,250.680159607724,18.1402603227317)) ;
#94403 = CARTESIAN_POINT('Ctrl Pts',(57.3904321283034,250.800687273232,18.1978577670584)) ;
#94404 = CARTESIAN_POINT('Ctrl Pts',(57.4991294772935,250.913640261489,18.2851184067917)) ;
#94405 = CARTESIAN_POINT('Ctrl Pts',(57.5505066995696,250.967268877587,18.3363964414506)) ;
#94406 = CARTESIAN_POINT('Ctrl Pts',(57.2522759660783,250.614740854374,18.1381958555625)) ;
#94407 = CARTESIAN_POINT('Ctrl Pts',(57.2908028309611,250.674714714559,18.1580345116492)) ;
#94408 = CARTESIAN_POINT('Ctrl Pts',(57.3895885689374,250.792382169794,18.220330010732)) ;
#94409 = CARTESIAN_POINT('Ctrl Pts',(57.492936507439,250.901775998676,18.3084379679755)) ;
#94410 = CARTESIAN_POINT('Ctrl Pts',(57.5423066932674,250.95296417531,18.3586344366773)) ;
#94411 = CARTESIAN_POINT('',(57.2522842181377,250.614754130417,18.1381996970991)) ;
#94412 = CARTESIAN_POINT('Ctrl Pts',(57.2522759660783,250.614740854374,18.1381958555625)) ;
#94413 = CARTESIAN_POINT('Ctrl Pts',(57.2452365621931,250.625532166615,18.1141521490421)) ;
#94414 = CARTESIAN_POINT('Ctrl Pts',(57.2350607949463,250.640021825605,18.0928712338379)) ;
#94415 = CARTESIAN_POINT('Ctrl Pts',(57.2097486588519,250.673406188019,18.058304224436)) ;
#94416 = CARTESIAN_POINT('Ctrl Pts',(57.1947896709115,250.692061496643,18.0451005266235)) ;
#94417 = CARTESIAN_POINT('Ctrl Pts',(57.1694020380105,250.721784873435,18.0321296306987)) ;
#94418 = CARTESIAN_POINT('Ctrl Pts',(57.1602559849713,250.732185523338,18.0289839177341)) ;
#94419 = CARTESIAN_POINT('Ctrl Pts',(57.1411635563705,250.753269492834,18.025401410602)) ;
#94420 = CARTESIAN_POINT('Ctrl Pts',(57.1312497748175,250.76390267473,18.0250400908081)) ;
#94421 = CARTESIAN_POINT('Ctrl Pts',(57.1209450813301,250.774641221836,18.0261880479281)) ;
#94422 = CARTESIAN_POINT('Ctrl Pts',(57.120652398181,250.77494597076,18.0262219055369)) ;
#94423 = CARTESIAN_POINT('Ctrl Pts',(57.1203596587326,250.775250521649,18.0262570222543)) ;
#94424 = CARTESIAN_POINT('Ctrl Pts',(57.5423066932674,250.95296417531,18.3586344366773)) ;
#94425 = CARTESIAN_POINT('Ctrl Pts',(57.492936507439,250.901775998676,18.3084379679755)) ;
#94426 = CARTESIAN_POINT('Ctrl Pts',(57.3896168747837,250.792412131542,18.2203541425176)) ;
#94427 = CARTESIAN_POINT('Ctrl Pts',(57.2908569439244,250.674779169542,18.1580686376687)) ;
#94428 = CARTESIAN_POINT('Ctrl Pts',(57.2523392883266,250.614839410371,18.1382284672602)) ;
#94429 = CARTESIAN_POINT('Origin',(60.4427446298904,253.683899394336,19.8213203435596)) ;
#94430 = CARTESIAN_POINT('',(60.4427446298904,253.683899394336,20.0213203435596)) ;
#94431 = CARTESIAN_POINT('Origin',(52.2356360608974,253.207106781187,19.5213203435596)) ;
#94432 = CARTESIAN_POINT('',(55.1300306216516,253.207106781187,20.0213203435596)) ;
#94433 = CARTESIAN_POINT('Ctrl Pts',(55.1300306216516,253.207106781187,20.0213203435596)) ;
#94434 = CARTESIAN_POINT('Ctrl Pts',(54.9727816340446,253.072343999508,20.0213203435596)) ;
#94435 = CARTESIAN_POINT('Ctrl Pts',(54.7853404806882,252.94731363725,19.9686339808095)) ;
#94436 = CARTESIAN_POINT('Ctrl Pts',(54.6208916966195,252.853553390593,19.8748737341529)) ;
#94437 = CARTESIAN_POINT('',(69.2699693783484,253.207106781187,20.0213203435596)) ;
#94438 = CARTESIAN_POINT('',(52.2356360608974,253.207106781187,20.0213203435596)) ;
#94439 = CARTESIAN_POINT('',(69.7791083033806,252.853553390593,19.8748737341529)) ;
#94440 = CARTESIAN_POINT('Ctrl Pts',(69.7791083033805,252.853553390593,19.8748737341529)) ;
#94441 = CARTESIAN_POINT('Ctrl Pts',(69.6146576393448,252.947314709111,19.9686350526701)) ;
#94442 = CARTESIAN_POINT('Ctrl Pts',(69.4272201636148,253.072342458909,20.0213203435596)) ;
#94443 = CARTESIAN_POINT('Ctrl Pts',(69.2699693783484,253.207106781187,20.0213203435596)) ;
#94444 = CARTESIAN_POINT('',(66.3707106781187,252.853553390593,19.8748737341529)) ;
#94445 = CARTESIAN_POINT('',(52.2356360608974,252.853553390593,19.8748737341529)) ;
#94446 = CARTESIAN_POINT('',(65.8856854219273,253.19999999981,20.021269638343)) ;
#94447 = CARTESIAN_POINT('Origin',(65.8757359312881,253.207106781187,19.5213203435596)) ;
#94448 = CARTESIAN_POINT('',(52.2356360608974,253.2,20.0212698346696)) ;
#94449 = CARTESIAN_POINT('Ctrl Pts',(65.881623518379,253.202901361836,20.0213026576949)) ;
#94450 = CARTESIAN_POINT('Ctrl Pts',(66.0629141248793,253.073408071479,20.0202134719904)) ;
#94451 = CARTESIAN_POINT('Ctrl Pts',(66.2425143263702,252.945122213271,19.9664425568304)) ;
#94452 = CARTESIAN_POINT('Ctrl Pts',(66.3707106781187,252.853553390593,19.8748737341529)) ;
#94453 = CARTESIAN_POINT('Ctrl Pts',(65.8603864536687,253.181665799482,20.0211240424873)) ;
#94454 = CARTESIAN_POINT('Ctrl Pts',(66.0391798872376,253.049783724924,20.0144847987807)) ;
#94455 = CARTESIAN_POINT('Ctrl Pts',(66.2151031676496,252.922902350671,19.9527372340496)) ;
#94456 = CARTESIAN_POINT('Ctrl Pts',(66.3381379840193,252.837267043544,19.8585873871032)) ;
#94457 = CARTESIAN_POINT('Ctrl Pts',(65.8232639540795,253.144444214368,20.0329043207371)) ;
#94458 = CARTESIAN_POINT('Ctrl Pts',(65.9977280232127,253.005226836627,20.0194760945433)) ;
#94459 = CARTESIAN_POINT('Ctrl Pts',(66.167186464512,252.875203335031,19.9457924120113)) ;
#94460 = CARTESIAN_POINT('Ctrl Pts',(66.2813241360136,252.793554120498,19.8454864621427)) ;
#94461 = CARTESIAN_POINT('Ctrl Pts',(65.7749943263166,253.095769049503,20.0811186276069)) ;
#94462 = CARTESIAN_POINT('Ctrl Pts',(65.9461044669602,252.940725734752,20.0657729104122)) ;
#94463 = CARTESIAN_POINT('Ctrl Pts',(66.1107270602757,252.795106259162,19.9834237274542)) ;
#94464 = CARTESIAN_POINT('Ctrl Pts',(66.2187011364029,252.7039244006,19.8724931824299)) ;
#94465 = CARTESIAN_POINT('Ctrl Pts',(65.7461964320231,253.066423830258,20.1461900919877)) ;
#94466 = CARTESIAN_POINT('Ctrl Pts',(65.9191932009661,252.896367685805,20.136008428504)) ;
#94467 = CARTESIAN_POINT('Ctrl Pts',(66.0869160227462,252.732236492732,20.0547507894586)) ;
#94468 = CARTESIAN_POINT('Ctrl Pts',(66.1997216851912,252.622654654284,19.9347834775349)) ;
#94469 = CARTESIAN_POINT('Ctrl Pts',(65.7401074337726,253.059892566227,20.1987710714045)) ;
#94470 = CARTESIAN_POINT('Ctrl Pts',(65.9184828909875,252.881535564304,20.1946701420602)) ;
#94471 = CARTESIAN_POINT('Ctrl Pts',(66.0939250192433,252.706049839441,20.1175725763353)) ;
#94472 = CARTESIAN_POINT('Ctrl Pts',(66.2170745615941,252.582925438406,19.9918655698157)) ;
#94473 = CARTESIAN_POINT('Ctrl Pts',(65.7402021621417,253.059797837858,20.221295583349)) ;
#94474 = CARTESIAN_POINT('Ctrl Pts',(65.921492768642,252.878507231358,20.2197707233628)) ;
#94475 = CARTESIAN_POINT('Ctrl Pts',(66.1010929701329,252.698907029867,20.1444914421387)) ;
#94476 = CARTESIAN_POINT('Ctrl Pts',(66.2292893218814,252.570710678119,20.0162950903902)) ;
#94477 = CARTESIAN_POINT('Origin',(65.8734821123455,253.2,20.0921424382039)) ;
#94478 = CARTESIAN_POINT('',(66.2292893218814,252.570710678119,20.0162950903902)) ;
#94479 = CARTESIAN_POINT('Origin',(66.3707106781187,252.712132034356,20.0162950903902)) ;
#94480 = CARTESIAN_POINT('Origin',(65.7343145750508,253.065685424949,19.5213203435596)) ;
#94481 = CARTESIAN_POINT('Origin',(63.3756911636855,255.707151548789,23.0113146048234)) ;
#94482 = CARTESIAN_POINT('',(68.0045941546019,251.21966991411,18.2409902576697)) ;
#94483 = CARTESIAN_POINT('',(67.8631727983646,250.936827201635,18.382411613907)) ;
#94484 = CARTESIAN_POINT('Origin',(68.0045941546019,251.078248557873,18.382411613907)) ;
#94485 = CARTESIAN_POINT('',(63.2342698074482,255.565730192552,23.0113146048234)) ;
#94486 = CARTESIAN_POINT('',(63.3756911636855,255.848572905027,22.8698932485861)) ;
#94487 = CARTESIAN_POINT('Ctrl Pts',(68.0685234977135,250.731476513624,18.2529125788923)) ;
#94488 = CARTESIAN_POINT('Ctrl Pts',(67.9915773915309,250.808422669384,18.2801593165379)) ;
#94489 = CARTESIAN_POINT('Ctrl Pts',(67.9208460458532,250.879153909218,18.3247963104889)) ;
#94490 = CARTESIAN_POINT('Ctrl Pts',(67.863139102423,250.93686091303,18.3825247079237)) ;
#94491 = CARTESIAN_POINT('Ctrl Pts',(68.0625957834865,250.7373902321,18.2194680319063)) ;
#94492 = CARTESIAN_POINT('Ctrl Pts',(67.9826680670271,250.81728663264,18.2457549454805)) ;
#94493 = CARTESIAN_POINT('Ctrl Pts',(67.908459192823,250.891559782816,18.29032024332)) ;
#94494 = CARTESIAN_POINT('Ctrl Pts',(67.8468303112623,250.953150707556,18.3499362264217)) ;
#94495 = CARTESIAN_POINT('Ctrl Pts',(68.0635796741313,250.759053528145,18.1610618496374)) ;
#94496 = CARTESIAN_POINT('Ctrl Pts',(67.9798052466115,250.845433836891,18.1857150875349)) ;
#94497 = CARTESIAN_POINT('Ctrl Pts',(67.9007979465452,250.927216465425,18.230154819357)) ;
#94498 = CARTESIAN_POINT('Ctrl Pts',(67.8337102502296,250.996881438386,18.2931030142913)) ;
#94499 = CARTESIAN_POINT('Ctrl Pts',(68.0955315081987,250.816176850352,18.0899683881281)) ;
#94500 = CARTESIAN_POINT('Ctrl Pts',(68.0105392122114,250.913117794014,18.1148812713429)) ;
#94501 = CARTESIAN_POINT('Ctrl Pts',(67.9298874864649,251.006131356308,18.1617654797125)) ;
#94502 = CARTESIAN_POINT('Ctrl Pts',(67.8607201289279,251.086540013528,18.2304736893628)) ;
#94503 = CARTESIAN_POINT('Ctrl Pts',(68.1472211618773,250.880004775357,18.055685461842)) ;
#94504 = CARTESIAN_POINT('Ctrl Pts',(68.0651794996633,250.984185012154,18.0846738399297)) ;
#94505 = CARTESIAN_POINT('Ctrl Pts',(67.9881198107097,251.08329094827,18.137196304556)) ;
#94506 = CARTESIAN_POINT('Ctrl Pts',(67.9230204305914,251.167821577733,18.2114983154127)) ;
#94507 = CARTESIAN_POINT('Ctrl Pts',(68.191141483228,250.92296018793,18.0584107582352)) ;
#94508 = CARTESIAN_POINT('Ctrl Pts',(68.1126799325993,251.028292595487,18.0929309831573)) ;
#94509 = CARTESIAN_POINT('Ctrl Pts',(68.0400154676919,251.126346778526,18.1512287876413)) ;
#94510 = CARTESIAN_POINT('Ctrl Pts',(67.9801172777256,251.207550315327,18.2288610080907)) ;
#94511 = CARTESIAN_POINT('Ctrl Pts',(68.2099526347344,250.939674811849,18.0643320877577)) ;
#94512 = CARTESIAN_POINT('Ctrl Pts',(68.1330030864753,251.04460755176,18.1014870418244)) ;
#94513 = CARTESIAN_POINT('Ctrl Pts',(68.0622678793746,251.141065609732,18.1623578912056)) ;
#94514 = CARTESIAN_POINT('Ctrl Pts',(68.0045565913183,251.219763261572,18.2410836242414)) ;
#94515 = CARTESIAN_POINT('',(68.20985501736,250.939768737622,18.0643653511196)) ;
#94516 = CARTESIAN_POINT('Origin',(68.20985501736,250.872987695115,18.2528866824369)) ;
#94517 = CARTESIAN_POINT('Origin',(68.2520815280172,250.547918471983,18.7713203435596)) ;
#94518 = CARTESIAN_POINT('Origin',(68.3935028842545,250.68933982822,18.7713203435596)) ;
#94519 = CARTESIAN_POINT('Ctrl Pts',(68.20985501736,250.939768737622,18.0643653511195)) ;
#94520 = CARTESIAN_POINT('Ctrl Pts',(68.2640374140654,250.865883651205,18.0381925935746)) ;
#94521 = CARTESIAN_POINT('Ctrl Pts',(68.3212444282195,250.78787408645,18.0237007750708)) ;
#94522 = CARTESIAN_POINT('Ctrl Pts',(68.3787050687238,250.70951866758,18.021591849742)) ;
#94523 = CARTESIAN_POINT('Ctrl Pts',(68.1659721653548,250.900778502873,18.0505536062847)) ;
#94524 = CARTESIAN_POINT('Ctrl Pts',(68.2226923077703,250.826137853427,18.0288422946047)) ;
#94525 = CARTESIAN_POINT('Ctrl Pts',(68.2819524792602,250.748870082081,18.0186430165262)) ;
#94526 = CARTESIAN_POINT('Ctrl Pts',(68.3412258152467,250.672066544789,18.0205838310049)) ;
#94527 = CARTESIAN_POINT('Ctrl Pts',(68.0789578599896,250.803901913784,18.0783946040854)) ;
#94528 = CARTESIAN_POINT('Ctrl Pts',(68.1404418139846,250.735363554207,18.0624840627055)) ;
#94529 = CARTESIAN_POINT('Ctrl Pts',(68.2039059525548,250.665266954687,18.0576296401064)) ;
#94530 = CARTESIAN_POINT('Ctrl Pts',(68.2666372217533,250.596333931781,18.0630889529167)) ;
#94531 = CARTESIAN_POINT('Ctrl Pts',(68.0580726283796,250.74192737162,18.1943887730536)) ;
#94532 = CARTESIAN_POINT('Ctrl Pts',(68.1160062559218,250.684163270981,18.1764052639078)) ;
#94533 = CARTESIAN_POINT('Ctrl Pts',(68.1762425132091,250.623639667933,18.1676682325686)) ;
#94534 = CARTESIAN_POINT('Ctrl Pts',(68.2365706774774,250.563429322523,18.1685349672834)) ;
#94535 = CARTESIAN_POINT('Ctrl Pts',(68.0684336611227,250.731566338877,18.2528866824369)) ;
#94536 = CARTESIAN_POINT('Ctrl Pts',(68.1226160578281,250.677383942172,18.233693326904)) ;
#94537 = CARTESIAN_POINT('Ctrl Pts',(68.1798230719822,250.620176928018,18.2230659933345)) ;
#94538 = CARTESIAN_POINT('Ctrl Pts',(68.2372837124865,250.562716287513,18.2215194480934)) ;
#94539 = CARTESIAN_POINT('',(68.357584866715,250.738305523749,18.0229216337057)) ;
#94540 = CARTESIAN_POINT('Origin',(68.3935028842545,250.68933982822,18.7713203435596)) ;
#94541 = CARTESIAN_POINT('Ctrl Pts',(68.2414080333741,250.64489209549,18.0799123114407)) ;
#94542 = CARTESIAN_POINT('Ctrl Pts',(68.2546291643386,250.650461761277,18.0666886890814)) ;
#94543 = CARTESIAN_POINT('Ctrl Pts',(68.2694566046645,250.656926759755,18.0555657574139)) ;
#94544 = CARTESIAN_POINT('Ctrl Pts',(68.3010063111761,250.670467574526,18.0379499729927)) ;
#94545 = CARTESIAN_POINT('Ctrl Pts',(68.317760304708,250.677503134716,18.0313727702642)) ;
#94546 = CARTESIAN_POINT('Ctrl Pts',(68.3507682624113,250.691144831296,18.0232435116254)) ;
#94547 = CARTESIAN_POINT('Ctrl Pts',(68.3633682258265,250.695971216193,18.0222098102947)) ;
#94548 = CARTESIAN_POINT('Ctrl Pts',(68.3691979799543,250.70106845124,18.0217842131582)) ;
#94549 = CARTESIAN_POINT('Ctrl Pts',(68.3698685266312,250.70187026372,18.0217410723846)) ;
#94550 = CARTESIAN_POINT('Ctrl Pts',(68.3706966899262,250.703387313299,18.0216891631644)) ;
#94551 = CARTESIAN_POINT('Ctrl Pts',(68.3709338331895,250.704088059953,18.0216751736344)) ;
#94552 = CARTESIAN_POINT('Ctrl Pts',(68.3712313275294,250.705902215846,18.021657612549)) ;
#94553 = CARTESIAN_POINT('Ctrl Pts',(68.3711853396952,250.707102221528,18.0216601799892)) ;
#94554 = CARTESIAN_POINT('Ctrl Pts',(68.3704253757421,250.711057343193,18.0217055973424)) ;
#94555 = CARTESIAN_POINT('Ctrl Pts',(68.3691918827918,250.714442050838,18.0217732060915)) ;
#94556 = CARTESIAN_POINT('Ctrl Pts',(68.3642229304804,250.725329533552,18.022171205809)) ;
#94557 = CARTESIAN_POINT('Ctrl Pts',(68.360737041717,250.732154691993,18.0225201305636)) ;
#94558 = CARTESIAN_POINT('Ctrl Pts',(68.3575711698691,250.738297080151,18.0229233951598)) ;
#94559 = CARTESIAN_POINT('Origin',(55.2141814145299,249.05,18.0213203435596)) ;
#94560 = CARTESIAN_POINT('',(77.9328605382387,244.521708245126,18.0213203435596)) ;
#94561 = CARTESIAN_POINT('',(61.8303059750075,244.521708245126,18.0213203435596)) ;
#94562 = CARTESIAN_POINT('',(75.4283628290596,245.483789937202,18.0213203435596)) ;
#94563 = CARTESIAN_POINT('Origin',(74.5283628290597,239.4,18.0213203435596)) ;
#94564 = CARTESIAN_POINT('',(75.4283628290596,246.,18.0213203435596)) ;
#94565 = CARTESIAN_POINT('',(75.4283628290596,247.266894968601,18.0213203435596)) ;
#94566 = CARTESIAN_POINT('',(73.6283628290596,246.,18.0213203435596)) ;
#94567 = CARTESIAN_POINT('',(65.3212721217947,246.,18.0213203435596)) ;
#94568 = CARTESIAN_POINT('',(73.6283628290596,245.483789937202,18.0213203435596)) ;
#94569 = CARTESIAN_POINT('',(73.6283628290596,247.525,18.0213203435596)) ;
#94570 = CARTESIAN_POINT('Origin',(74.5283628290597,239.4,18.0213203435596)) ;
#94571 = CARTESIAN_POINT('',(68.3828427124746,250.68933982822,18.0213203435596)) ;
#94572 = CARTESIAN_POINT('',(68.3828427124746,249.4375,18.0213203435596)) ;
#94573 = CARTESIAN_POINT('',(52.2356360608974,250.68933982822,18.0213203435596)) ;
#94574 = CARTESIAN_POINT('',(72.0133921147013,247.214089774802,18.0213203435596)) ;
#94575 = CARTESIAN_POINT('',(72.0133921147013,248.124963207434,18.0213203435596)) ;
#94576 = CARTESIAN_POINT('',(72.0133921147013,248.637481603717,18.0213203435596)) ;
#94577 = CARTESIAN_POINT('',(73.2395171459957,246.537024447301,18.0213203435596)) ;
#94578 = CARTESIAN_POINT('Origin',(72.8133921147013,247.214089774802,18.0213203435596)) ;
#94579 = CARTESIAN_POINT('',(74.19803042292,247.140284551659,18.0213203435596)) ;
#94580 = CARTESIAN_POINT('',(67.3503775087141,242.830572927334,18.0213203435596)) ;
#94581 = CARTESIAN_POINT('',(73.8784366494491,247.648083547285,18.0213203435596)) ;
#94582 = CARTESIAN_POINT('',(71.0478693800126,252.145540430945,18.0213203435596)) ;
#94583 = CARTESIAN_POINT('',(72.9199233725249,247.044823442927,18.0213203435596)) ;
#94584 = CARTESIAN_POINT('',(67.4677237907363,243.613369160683,18.0213203435596)) ;
#94585 = CARTESIAN_POINT('',(72.6133921147013,247.214089774802,18.0213203435596)) ;
#94586 = CARTESIAN_POINT('Origin',(72.8133921147013,247.214089774802,18.0213203435596)) ;
#94587 = CARTESIAN_POINT('',(72.6133921147013,248.124963207434,18.0213203435596)) ;
#94588 = CARTESIAN_POINT('',(72.6133921147013,248.132044887401,18.0213203435596)) ;
#94589 = CARTESIAN_POINT('',(73.1273459706961,248.124963207434,18.0213203435596)) ;
#94590 = CARTESIAN_POINT('',(63.8637867646156,248.124963207434,18.0213203435596)) ;
#94591 = CARTESIAN_POINT('',(72.2987422718658,250.163082385568,18.0213203435596)) ;
#94592 = CARTESIAN_POINT('',(71.6675838322311,251.715544825786,18.0213203435596)) ;
#94593 = CARTESIAN_POINT('',(71.4701385730357,248.124963207434,18.0213203435596)) ;
#94594 = CARTESIAN_POINT('',(70.8466068278818,246.591260172113,18.0213203435596)) ;
#94595 = CARTESIAN_POINT('',(63.416461843198,248.124963207434,18.0213203435596)) ;
#94596 = CARTESIAN_POINT('',(74.9348607567984,249.429895468622,18.0213203435596)) ;
#94597 = CARTESIAN_POINT('',(75.2544545302692,248.922096472997,18.0213203435596)) ;
#94598 = CARTESIAN_POINT('',(72.2495203324155,253.696603031808,18.0213203435596)) ;
#94599 = CARTESIAN_POINT('',(76.1283346412558,249.472090948443,18.0213203435596)) ;
#94600 = CARTESIAN_POINT('',(68.1060880979734,244.423124592531,18.0213203435596)) ;
#94601 = CARTESIAN_POINT('',(76.4348658990794,249.302824616567,18.0213203435596)) ;
#94602 = CARTESIAN_POINT('Origin',(76.2348658990794,249.302824616567,18.0213203435596)) ;
#94603 = CARTESIAN_POINT('',(76.4348658990794,248.391951183936,18.0213203435596)) ;
#94604 = CARTESIAN_POINT('',(76.4348658990794,249.176412308284,18.0213203435596)) ;
#94605 = CARTESIAN_POINT('',(75.9209120430846,248.391951183936,18.0213203435596)) ;
#94606 = CARTESIAN_POINT('',(65.8745236568046,248.391951183936,18.0213203435596)) ;
#94607 = CARTESIAN_POINT('',(76.7495157419148,246.353832005802,18.0213203435596)) ;
#94608 = CARTESIAN_POINT('',(74.3655697550003,252.217631603154,18.0213203435596)) ;
#94609 = CARTESIAN_POINT('',(77.578119440745,248.391951183936,18.0213203435596)) ;
#94610 = CARTESIAN_POINT('',(75.7388649854292,243.867931095515,18.0213203435596)) ;
#94611 = CARTESIAN_POINT('',(77.0348658990794,248.391951183936,18.0213203435596)) ;
#94612 = CARTESIAN_POINT('',(66.3218485782223,248.391951183936,18.0213203435596)) ;
#94613 = CARTESIAN_POINT('',(77.0348658990794,249.302824616567,18.0213203435596)) ;
#94614 = CARTESIAN_POINT('',(77.0348658990794,248.670975591968,18.0213203435596)) ;
#94615 = CARTESIAN_POINT('',(75.8087408677849,249.979889944069,18.0213203435596)) ;
#94616 = CARTESIAN_POINT('Origin',(76.2348658990794,249.302824616567,18.0213203435596)) ;
#94617 = CARTESIAN_POINT('',(68.223434379996,245.20592082588,18.0213203435596)) ;
#94618 = CARTESIAN_POINT('',(74.2283628290596,249.52834685842,18.0213203435596)) ;
#94619 = CARTESIAN_POINT('',(74.8283628290596,249.52834685842,18.0213203435596)) ;
#94620 = CARTESIAN_POINT('',(64.9712721217948,249.52834685842,18.0213203435596)) ;
#94621 = CARTESIAN_POINT('',(74.2283628290596,246.82834685842,18.0213203435596)) ;
#94622 = CARTESIAN_POINT('',(74.2283628290596,249.23917342921,18.0213203435596)) ;
#94623 = CARTESIAN_POINT('',(74.8283628290596,246.82834685842,18.0213203435596)) ;
#94624 = CARTESIAN_POINT('',(64.7712721217948,246.82834685842,18.0213203435596)) ;
#94625 = CARTESIAN_POINT('',(74.8283628290596,247.98917342921,18.0213203435596)) ;
#94626 = CARTESIAN_POINT('Origin',(52.2356360608974,250.68933982822,18.7713203435596)) ;
#94627 = CARTESIAN_POINT('Origin',(68.3985118238593,250.691109216673,18.5008448049847)) ;
#94628 = CARTESIAN_POINT('',(52.2356360608974,251.21966991411,18.2409902576697)) ;
#94629 = CARTESIAN_POINT('Origin',(49.257090707265,252.,19.0213203435596)) ;
#94630 = CARTESIAN_POINT('',(76.6208916966195,252.853553390593,19.8748737341529)) ;
#94631 = CARTESIAN_POINT('Origin',(73.2,255.853553390593,22.8748737341529)) ;
#94632 = CARTESIAN_POINT('',(52.2356360608974,252.853553390593,19.8748737341529)) ;
#94633 = CARTESIAN_POINT('Origin',(68.3828427124746,249.4375,18.2213203435596)) ;
#94634 = CARTESIAN_POINT('Origin',(68.3828427124747,244.521708245126,18.2213203435596)) ;
#94635 = CARTESIAN_POINT('Ctrl Pts',(68.274306674866,244.273916677043,18.0470136686937)) ;
#94636 = CARTESIAN_POINT('Ctrl Pts',(68.2525104982572,244.35458767695,18.0688098453025)) ;
#94637 = CARTESIAN_POINT('Ctrl Pts',(68.2414213562374,244.438144595489,18.0798989873223)) ;
#94638 = CARTESIAN_POINT('Ctrl Pts',(68.2414213562374,244.521708245126,18.0798989873223)) ;
#94639 = CARTESIAN_POINT('Ctrl Pts',(68.310391048944,244.293415664068,18.0109292946157)) ;
#94640 = CARTESIAN_POINT('Ctrl Pts',(68.2892363653393,244.367600584991,18.0321209883094)) ;
#94641 = CARTESIAN_POINT('Ctrl Pts',(68.278445380722,244.444667068531,18.0428749628377)) ;
#94642 = CARTESIAN_POINT('Ctrl Pts',(68.278445380722,244.521708245126,18.0428749628377)) ;
#94643 = CARTESIAN_POINT('Ctrl Pts',(68.362867182144,244.312772739493,17.9917619163006)) ;
#94644 = CARTESIAN_POINT('Ctrl Pts',(68.3414167382309,244.380543003792,18.0113579653632)) ;
#94645 = CARTESIAN_POINT('Ctrl Pts',(68.3304828349148,244.451143558849,18.0213203435596)) ;
#94646 = CARTESIAN_POINT('Ctrl Pts',(68.3304828349148,244.521708245126,18.0213203435596)) ;
#94647 = CARTESIAN_POINT('Ctrl Pts',(68.4157280311033,244.326083322955,17.9953582499055)) ;
#94648 = CARTESIAN_POINT('Ctrl Pts',(68.3939318544945,244.389770954461,18.0125657577545)) ;
#94649 = CARTESIAN_POINT('Ctrl Pts',(68.3828427124747,244.455736942781,18.0213203435596)) ;
#94650 = CARTESIAN_POINT('Ctrl Pts',(68.3828427124747,244.521708245126,18.0213203435596)) ;
#94651 = CARTESIAN_POINT('Ctrl Pts',(58.6558325375659,252.114065839068,19.604968115859)) ;
#94652 = CARTESIAN_POINT('Ctrl Pts',(58.6560546890527,252.114296876615,19.499708534422)) ;
#94653 = CARTESIAN_POINT('Ctrl Pts',(58.6126930842203,252.069200807589,19.3950243599491)) ;
#94654 = CARTESIAN_POINT('Ctrl Pts',(58.5381062355785,251.991630485002,19.3207516809529)) ;
#94655 = CARTESIAN_POINT('Ctrl Pts',(58.6203761977389,252.077191235786,19.6048193809459)) ;
#94656 = CARTESIAN_POINT('Ctrl Pts',(58.6205836533543,252.077409571898,19.519006774521)) ;
#94657 = CARTESIAN_POINT('Ctrl Pts',(58.5800900326603,252.034790418159,19.4335598510852)) ;
#94658 = CARTESIAN_POINT('Ctrl Pts',(58.5108234404051,251.963260236624,19.3777695274782)) ;
#94659 = CARTESIAN_POINT('Ctrl Pts',(58.599917094062,252.026292564171,19.6046716026803)) ;
#94660 = CARTESIAN_POINT('Ctrl Pts',(58.6000890621805,252.026517346894,19.5381801383464)) ;
#94661 = CARTESIAN_POINT('Ctrl Pts',(58.5665185027056,251.982640513062,19.4721422791318)) ;
#94662 = CARTESIAN_POINT('Ctrl Pts',(58.5120777999854,251.908453143741,19.4337397059719)) ;
#94663 = CARTESIAN_POINT('Ctrl Pts',(58.5999998252129,251.97513584248,19.6045649427454)) ;
#94664 = CARTESIAN_POINT('Ctrl Pts',(58.6001105321248,251.975366917946,19.5520192504951)) ;
#94665 = CARTESIAN_POINT('Ctrl Pts',(58.5785017471512,251.930263457254,19.4997602590865)) ;
#94666 = CARTESIAN_POINT('Ctrl Pts',(58.5413122444863,251.852672635479,19.4626317919105)) ;
#94667 = CARTESIAN_POINT('',(58.5414213562373,251.853601400224,19.4627416997969)) ;
#94668 = CARTESIAN_POINT('Origin',(58.4,251.55944497925,19.6041630560343)) ;
#94669 = CARTESIAN_POINT('Origin',(58.6828427124746,251.853601400224,19.3213203435596)) ;
#94670 = CARTESIAN_POINT('Origin',(58.3256944230447,251.482167179217,18.9641720541297)) ;
#94671 = CARTESIAN_POINT('',(57.3360353944838,250.6,18.2573557380434)) ;
#94672 = CARTESIAN_POINT('',(58.1842730668074,251.482167179217,19.105593410367)) ;
#94673 = CARTESIAN_POINT('Ctrl Pts',(57.3360353944838,250.6,18.2573557380434)) ;
#94674 = CARTESIAN_POINT('Ctrl Pts',(57.3181896909239,250.6,18.2395100344835)) ;
#94675 = CARTESIAN_POINT('Ctrl Pts',(57.3005245771568,250.599676577703,18.2194780649264)) ;
#94676 = CARTESIAN_POINT('Ctrl Pts',(57.2777853264116,250.601948658739,18.1885691056682)) ;
#94677 = CARTESIAN_POINT('Ctrl Pts',(57.2699676956912,250.603347306435,18.1767561178791)) ;
#94678 = CARTESIAN_POINT('Ctrl Pts',(57.2610778226503,250.60716749495,18.1601317033773)) ;
#94679 = CARTESIAN_POINT('Ctrl Pts',(57.2586681750948,250.608544938818,18.1551388788019)) ;
#94680 = CARTESIAN_POINT('Ctrl Pts',(57.2549670712099,250.611595514249,18.1461752289758)) ;
#94681 = CARTESIAN_POINT('Ctrl Pts',(57.2535461821065,250.613147135549,18.142207243288)) ;
#94682 = CARTESIAN_POINT('Ctrl Pts',(57.2524006549569,250.6149414558,18.1382539013022)) ;
#94683 = CARTESIAN_POINT('Origin',(58.4,245.5625,19.6041630560343)) ;
#94684 = CARTESIAN_POINT('',(58.5414213562374,245.458578643763,19.4627416997969)) ;
#94685 = CARTESIAN_POINT('Origin',(58.4,245.6,19.6041630560343)) ;
#94686 = CARTESIAN_POINT('',(58.5414213562374,245.5625,19.4627416997969)) ;
#94687 = CARTESIAN_POINT('Origin',(66.25,251.8,20.0213203435596)) ;
#94688 = CARTESIAN_POINT('Ctrl Pts',(57.3360353944838,250.6,18.2573557380434)) ;
#94689 = CARTESIAN_POINT('Ctrl Pts',(57.3340473556883,250.6,18.255367699248)) ;
#94690 = CARTESIAN_POINT('Ctrl Pts',(57.3300486483845,250.6,18.2513689919442)) ;
#94691 = CARTESIAN_POINT('Ctrl Pts',(57.3219725324425,250.6,18.2432928760022)) ;
#94692 = CARTESIAN_POINT('Ctrl Pts',(57.2953493638287,250.6,18.2166697073883)) ;
#94693 = CARTESIAN_POINT('Ctrl Pts',(57.2571236188557,250.6,18.1784439624154)) ;
#94694 = CARTESIAN_POINT('Ctrl Pts',(57.207773891194,250.6,18.1290942347537)) ;
#94695 = CARTESIAN_POINT('Ctrl Pts',(57.1830512714168,250.6,18.1043716149764)) ;
#94696 = CARTESIAN_POINT('Ctrl Pts',(57.1734725423205,250.6,18.0947928858801)) ;
#94697 = CARTESIAN_POINT('Ctrl Pts',(57.3333527411373,250.592253069194,18.194783093941)) ;
#94698 = CARTESIAN_POINT('Ctrl Pts',(57.3316948915604,250.59291821646,18.1930083348525)) ;
#94699 = CARTESIAN_POINT('Ctrl Pts',(57.3283033876591,250.594238062535,18.1894701538716)) ;
#94700 = CARTESIAN_POINT('Ctrl Pts',(57.3212436334276,250.596857460934,18.1824465273365)) ;
#94701 = CARTESIAN_POINT('Ctrl Pts',(57.2969689913209,250.605207915463,18.1598768130777)) ;
#94702 = CARTESIAN_POINT('Ctrl Pts',(57.2569809892506,250.614379141446,18.1302403683433)) ;
#94703 = CARTESIAN_POINT('Ctrl Pts',(57.2003714037071,250.618567551195,18.0947534362098)) ;
#94704 = CARTESIAN_POINT('Ctrl Pts',(57.170211619543,250.615028729546,18.078006465602)) ;
#94705 = CARTESIAN_POINT('Ctrl Pts',(57.1582126167144,250.61077488758,18.0719249151656)) ;
#94706 = CARTESIAN_POINT('Ctrl Pts',(57.3362613117172,250.64045272393,18.0627210228977)) ;
#94707 = CARTESIAN_POINT('Ctrl Pts',(57.3344481626957,250.641874746874,18.0621160423691)) ;
#94708 = CARTESIAN_POINT('Ctrl Pts',(57.3306964101622,250.644659791177,18.0609462582947)) ;
#94709 = CARTESIAN_POINT('Ctrl Pts',(57.3227262302857,250.64994988976,18.0587275800888)) ;
#94710 = CARTESIAN_POINT('Ctrl Pts',(57.294574348591,250.665713573551,18.052155533589)) ;
#94711 = CARTESIAN_POINT('Ctrl Pts',(57.2451381515996,250.678074698665,18.0454508927218)) ;
#94712 = CARTESIAN_POINT('Ctrl Pts',(57.1735021273919,250.671463165854,18.0378317708818)) ;
#94713 = CARTESIAN_POINT('Ctrl Pts',(57.1349950092079,250.654089939879,18.0348746164525)) ;
#94714 = CARTESIAN_POINT('Ctrl Pts',(57.1192875831677,250.63825948163,18.0346271738767)) ;
#94715 = CARTESIAN_POINT('Ctrl Pts',(57.3530175024253,250.774455018098,18.0235461286619)) ;
#94716 = CARTESIAN_POINT('Ctrl Pts',(57.3497024752754,250.775415195087,18.0236910929475)) ;
#94717 = CARTESIAN_POINT('Ctrl Pts',(57.3430153907722,250.777175758591,18.0239599227483)) ;
#94718 = CARTESIAN_POINT('Ctrl Pts',(57.3294481719789,250.780101722395,18.0244426251914)) ;
#94719 = CARTESIAN_POINT('Ctrl Pts',(57.2843980090737,250.78649635771,18.0257611907679)) ;
#94720 = CARTESIAN_POINT('Ctrl Pts',(57.2185876893421,250.779765247521,18.02518066019)) ;
#94721 = CARTESIAN_POINT('Ctrl Pts',(57.1328468261104,250.741672390444,18.0222725008139)) ;
#94722 = CARTESIAN_POINT('Ctrl Pts',(57.0890785776611,250.702463609168,18.0204629952553)) ;
#94723 = CARTESIAN_POINT('Ctrl Pts',(57.0710662135815,250.672308129681,18.0213203435596)) ;
#94724 = CARTESIAN_POINT('Ctrl Pts',(57.3614836315263,250.835788185648,18.0357573764341)) ;
#94725 = CARTESIAN_POINT('Ctrl Pts',(57.3573995943998,250.836527612015,18.0359045939827)) ;
#94726 = CARTESIAN_POINT('Ctrl Pts',(57.3492123791771,250.837811031858,18.0361634130032)) ;
#94727 = CARTESIAN_POINT('Ctrl Pts',(57.3327905714109,250.839665322753,18.0365310164789)) ;
#94728 = CARTESIAN_POINT('Ctrl Pts',(57.2791569903834,250.841940496107,18.0370590762059)) ;
#94729 = CARTESIAN_POINT('Ctrl Pts',(57.2051851586706,250.827317494238,18.0336777240699)) ;
#94730 = CARTESIAN_POINT('Ctrl Pts',(57.112442265655,250.775538088749,18.0255551391046)) ;
#94731 = CARTESIAN_POINT('Ctrl Pts',(57.0661025428336,250.726337647705,18.0213203435596)) ;
#94732 = CARTESIAN_POINT('Ctrl Pts',(57.046945084641,250.68933982822,18.0213203435596)) ;
#94733 = CARTESIAN_POINT('',(57.1734725423205,250.6,18.0947928858801)) ;
#94734 = CARTESIAN_POINT('',(59.35,250.6,20.2713203435596)) ;
#94735 = CARTESIAN_POINT('Origin',(57.046945084641,250.68933982822,18.2213203435596)) ;
#94736 = CARTESIAN_POINT('Ctrl Pts',(57.1734725423205,250.6,18.0947928858801)) ;
#94737 = CARTESIAN_POINT('Ctrl Pts',(57.1731461743363,250.6,18.0944665178959)) ;
#94738 = CARTESIAN_POINT('Ctrl Pts',(57.1725010996802,250.6,18.0938214432399)) ;
#94739 = CARTESIAN_POINT('Ctrl Pts',(57.1712430810202,250.6,18.0925634245799)) ;
#94740 = CARTESIAN_POINT('Ctrl Pts',(57.1691302969587,250.6,18.0904506405183)) ;
#94741 = CARTESIAN_POINT('Ctrl Pts',(57.1669367401687,250.6,18.0882570837283)) ;
#94742 = CARTESIAN_POINT('Ctrl Pts',(57.1649991631621,250.6,18.0863195067217)) ;
#94743 = CARTESIAN_POINT('Ctrl Pts',(57.1604293063194,250.6,18.0817496498791)) ;
#94744 = CARTESIAN_POINT('Ctrl Pts',(57.1584079275307,250.6,18.0797282710903)) ;
#94745 = CARTESIAN_POINT('Ctrl Pts',(57.1585946892593,250.599997334071,18.0799134496435)) ;
#94746 = CARTESIAN_POINT('Ctrl Pts',(57.1429446492179,250.621555453462,18.0490448931659)) ;
#94747 = CARTESIAN_POINT('Ctrl Pts',(57.1424797946325,250.621375921649,18.0489088621478)) ;
#94748 = CARTESIAN_POINT('Ctrl Pts',(57.1415607216988,250.621008706217,18.0486394209038)) ;
#94749 = CARTESIAN_POINT('Ctrl Pts',(57.1397653075042,250.620246901795,18.0481166236226)) ;
#94750 = CARTESIAN_POINT('Ctrl Pts',(57.1367454202683,250.61883616044,18.0472382453025)) ;
#94751 = CARTESIAN_POINT('Ctrl Pts',(57.1335982829151,250.617060962106,18.0463315951316)) ;
#94752 = CARTESIAN_POINT('Ctrl Pts',(57.1308083691544,250.615146586166,18.045539816041)) ;
#94753 = CARTESIAN_POINT('Ctrl Pts',(57.1242109639996,250.609962299049,18.0436867512443)) ;
#94754 = CARTESIAN_POINT('Ctrl Pts',(57.1212989029449,250.60431006208,18.0427897179726)) ;
#94755 = CARTESIAN_POINT('Ctrl Pts',(57.1215631814552,250.5993051408,18.0428708220856)) ;
#94756 = CARTESIAN_POINT('Ctrl Pts',(57.0951621692686,250.655294205737,18.0213057277848)) ;
#94757 = CARTESIAN_POINT('Ctrl Pts',(57.094601304706,250.654745987511,18.0213088809629)) ;
#94758 = CARTESIAN_POINT('Ctrl Pts',(57.0934927123476,250.653637902561,18.0213139894636)) ;
#94759 = CARTESIAN_POINT('Ctrl Pts',(57.0913291481799,250.651379993583,18.0213249675951)) ;
#94760 = CARTESIAN_POINT('Ctrl Pts',(57.0876937748347,250.647315907814,18.0213383959865)) ;
#94761 = CARTESIAN_POINT('Ctrl Pts',(57.0839139948312,250.642433992342,18.0213487187058)) ;
#94762 = CARTESIAN_POINT('Ctrl Pts',(57.0805700602664,250.637351731764,18.0213615345955)) ;
#94763 = CARTESIAN_POINT('Ctrl Pts',(57.0726744213749,250.62385451521,18.0213962624513)) ;
#94764 = CARTESIAN_POINT('Ctrl Pts',(57.0691959132974,250.610399542745,18.0213013549948)) ;
#94765 = CARTESIAN_POINT('Ctrl Pts',(57.069511625002,250.598324499523,18.0213095441839)) ;
#94766 = CARTESIAN_POINT('Ctrl Pts',(57.0469069494654,250.689366755103,18.0213203493371)) ;
#94767 = CARTESIAN_POINT('Ctrl Pts',(57.0462541408344,250.688442020775,18.0213203468729)) ;
#94768 = CARTESIAN_POINT('Ctrl Pts',(57.0449638479257,250.686578176133,18.0213203428908)) ;
#94769 = CARTESIAN_POINT('Ctrl Pts',(57.0424475318287,250.682795217849,18.0213203343216)) ;
#94770 = CARTESIAN_POINT('Ctrl Pts',(57.0382214969108,250.676032304701,18.0213203238896)) ;
#94771 = CARTESIAN_POINT('Ctrl Pts',(57.0338339029805,250.66799976973,18.0213203159184)) ;
#94772 = CARTESIAN_POINT('Ctrl Pts',(57.029958328817,250.659709674647,18.0213203059525)) ;
#94773 = CARTESIAN_POINT('Ctrl Pts',(57.020817631172,250.637802853616,18.0213202788865)) ;
#94774 = CARTESIAN_POINT('Ctrl Pts',(57.0167744273248,250.616535402224,18.0213203540969)) ;
#94775 = CARTESIAN_POINT('Ctrl Pts',(57.0171413288756,250.597336706409,18.0213203476065)) ;
#94776 = CARTESIAN_POINT('',(57.1585786437627,250.6,18.0798989873223)) ;
#94777 = CARTESIAN_POINT('Origin',(57.0171572875254,250.6,18.2213203435596)) ;
#94778 = CARTESIAN_POINT('',(59.35,250.6,20.2713203435596)) ;
#94779 = CARTESIAN_POINT('Origin',(57.0171572875254,247.8875,18.2213203435596)) ;
#94780 = CARTESIAN_POINT('',(57.1585786437627,247.8875,18.0798989873223)) ;
#94781 = CARTESIAN_POINT('Origin',(57.85,246.725,18.7713203435596)) ;
#94782 = CARTESIAN_POINT('',(59.4894251848905,244.51057481511,20.4107455284501)) ;
#94783 = CARTESIAN_POINT('',(59.0458333333334,244.954166666667,19.967153676893)) ;
#94784 = CARTESIAN_POINT('Origin',(59.7722678973651,244.793417527584,20.6935882409247)) ;
#94785 = CARTESIAN_POINT('Origin',(59.7,253.2,24.0213203435596)) ;
#94786 = CARTESIAN_POINT('',(59.7,253.2,24.0213203435596)) ;
#94787 = CARTESIAN_POINT('',(61.2,253.2,24.0213203435596)) ;
#94788 = CARTESIAN_POINT('',(59.7,253.2,24.0213203435596)) ;
#94789 = CARTESIAN_POINT('Origin',(66.95,251.85,24.0213203435596)) ;
#94790 = CARTESIAN_POINT('',(66.7875,252.0125,23.0213203435596)) ;
#94791 = CARTESIAN_POINT('',(66.975,251.825,24.0213203435596)) ;
#94792 = CARTESIAN_POINT('Origin',(69.2696458032277,238.278291754874,16.7713203435596)) ;
#94793 = CARTESIAN_POINT('',(80.6144201366714,238.515462579386,16.0598078700218)) ;
#94794 = CARTESIAN_POINT('Ctrl Pts',(80.5752025501715,238.278291754874,16.0213203435596)) ;
#94795 = CARTESIAN_POINT('Ctrl Pts',(80.5895127461922,238.355434329238,16.0213203435596)) ;
#94796 = CARTESIAN_POINT('Ctrl Pts',(80.6030553487399,238.437267187051,16.0337427392433)) ;
#94797 = CARTESIAN_POINT('Ctrl Pts',(80.6144201366714,238.515462579386,16.0598078700215)) ;
#94798 = CARTESIAN_POINT('',(69.2696458032277,238.515462579386,16.0598078700217)) ;
#94799 = CARTESIAN_POINT('Origin',(74.5283628290597,239.4,16.0213203435596)) ;
#94800 = CARTESIAN_POINT('Ctrl Pts',(68.442305521448,238.515462579386,16.0598078700215)) ;
#94801 = CARTESIAN_POINT('Ctrl Pts',(68.4536700072495,238.437269265856,16.0337434321782)) ;
#94802 = CARTESIAN_POINT('Ctrl Pts',(68.4672116831744,238.355440953127,16.0213203435596)) ;
#94803 = CARTESIAN_POINT('Ctrl Pts',(68.4815231079478,238.278291754874,16.0213203435596)) ;
#94804 = CARTESIAN_POINT('',(73.6283628290596,245.483789937202,18.5213203435596)) ;
#94805 = CARTESIAN_POINT('',(73.6283628290596,245.483789937202,16.0213203435596)) ;
#94806 = CARTESIAN_POINT('',(75.4283628290596,245.483789937202,18.5213203435596)) ;
#94807 = CARTESIAN_POINT('Origin',(74.5283628290597,239.4,18.5213203435596)) ;
#94808 = CARTESIAN_POINT('',(75.4283628290596,245.483789937202,16.0213203435596)) ;
#94809 = CARTESIAN_POINT('',(78.2651788784023,244.284537420614,17.9828328170975)) ;
#94810 = CARTESIAN_POINT('Ctrl Pts',(78.2651788784023,244.284537420614,17.9828328170977)) ;
#94811 = CARTESIAN_POINT('Ctrl Pts',(78.2318038761366,244.310070287572,17.9913437727504)) ;
#94812 = CARTESIAN_POINT('Ctrl Pts',(78.1978897752054,244.335468004199,17.9982799362105)) ;
#94813 = CARTESIAN_POINT('Ctrl Pts',(78.1637671894526,244.360475493408,18.0037846770076)) ;
#94814 = CARTESIAN_POINT('Ctrl Pts',(78.1291333505218,244.385857665779,18.0093718944449)) ;
#94815 = CARTESIAN_POINT('Ctrl Pts',(78.0942847325789,244.410837421656,18.013485084683)) ;
#94816 = CARTESIAN_POINT('Ctrl Pts',(78.059567033835,244.43518585183,18.0163128773869)) ;
#94817 = CARTESIAN_POINT('Ctrl Pts',(78.0239386127422,244.460172995408,18.0192148493742)) ;
#94818 = CARTESIAN_POINT('Ctrl Pts',(77.9884480695404,244.484494937463,18.0207637869309)) ;
#94819 = CARTESIAN_POINT('Ctrl Pts',(77.9534690276318,244.507949572025,18.0211941322164)) ;
#94820 = CARTESIAN_POINT('Ctrl Pts',(77.9465787317034,244.512569749257,18.0212789031594)) ;
#94821 = CARTESIAN_POINT('Ctrl Pts',(77.9397082833141,244.517156417629,18.0213203435596)) ;
#94822 = CARTESIAN_POINT('Ctrl Pts',(77.9328605382387,244.521708245126,18.0213203435596)) ;
#94823 = CARTESIAN_POINT('Origin',(74.5283628290597,239.4,16.3546536768929)) ;
#94824 = CARTESIAN_POINT('Origin',(66.95,251.85,24.0213203435596)) ;
#94825 = CARTESIAN_POINT('Origin',(61.8303059750075,244.521708245126,17.2713203435596)) ;
#94826 = CARTESIAN_POINT('',(61.8303059750075,244.284537420614,17.9828328170975)) ;
#94827 = CARTESIAN_POINT('Origin',(59.7,242.,24.0213203435596)) ;
#94828 = CARTESIAN_POINT('',(59.7,242.,24.0213203435596)) ;
#94829 = CARTESIAN_POINT('Origin',(69.2696458032277,238.278291754874,16.7713203435596)) ;
#94830 = CARTESIAN_POINT('Origin',(60.5916108526749,220.645409008718,23.3713203435596)) ;
#94831 = CARTESIAN_POINT('',(60.5916108526749,219.647053884905,30.7213203435596)) ;
#94832 = CARTESIAN_POINT('',(60.5916108526749,220.125049696322,30.7213203435596)) ;
#94833 = CARTESIAN_POINT('',(60.5916108526749,227.303573749953,30.7213203435596)) ;
#94834 = CARTESIAN_POINT('',(60.5916108526749,219.647053884905,23.3713203435596)) ;
#94835 = CARTESIAN_POINT('',(60.5916108526749,219.647053884905,23.3713203435596)) ;
#94836 = CARTESIAN_POINT('',(60.5916108526749,220.645409008718,23.3713203435596)) ;
#94837 = CARTESIAN_POINT('',(60.5916108526749,220.645409008718,23.3713203435596)) ;
#94838 = CARTESIAN_POINT('',(60.5916108526749,220.645409008718,23.3713203435596)) ;
#94839 = CARTESIAN_POINT('',(60.5916108526749,220.125049696322,27.0463203435596)) ;
#94840 = CARTESIAN_POINT('Origin',(64.1568347953872,220.146231446812,23.3713203435596)) ;
#94841 = CARTESIAN_POINT('',(63.1200364144528,223.593701405679,23.3713203435596)) ;
#94842 = CARTESIAN_POINT('Origin',(64.1568347953872,220.146231446812,23.3713203435596)) ;
#94843 = CARTESIAN_POINT('',(63.1200364144528,223.593701405679,23.3713203435596)) ;
#94844 = CARTESIAN_POINT('Origin',(70.3850625789433,219.622496965577,23.3713203435596)) ;
#94845 = CARTESIAN_POINT('',(67.2791272966079,221.938238572027,23.3713203435596)) ;
#94846 = CARTESIAN_POINT('',(67.2791272966079,221.938238572027,23.3713203435596)) ;
#94847 = CARTESIAN_POINT('',(70.3850625789433,219.622496965577,23.3713203435596)) ;
#94848 = CARTESIAN_POINT('',(64.9830939940346,223.650128668,23.3713203435596)) ;
#94849 = CARTESIAN_POINT('',(70.3850625789433,219.622496965577,23.3713203435596)) ;
#94850 = CARTESIAN_POINT('Ctrl Pts',(84.4412221473412,189.289539758744,23.1313203435596)) ;
#94851 = CARTESIAN_POINT('Ctrl Pts',(84.4412221473412,189.289539758744,30.7993203435596)) ;
#94852 = CARTESIAN_POINT('Ctrl Pts',(83.8416464716194,189.870585945118,23.1313203435596)) ;
#94853 = CARTESIAN_POINT('Ctrl Pts',(83.8416464716194,189.870585945118,30.7993203435596)) ;
#94854 = CARTESIAN_POINT('Ctrl Pts',(82.6693997344123,191.034842241154,23.1313203435596)) ;
#94855 = CARTESIAN_POINT('Ctrl Pts',(82.6693997344123,191.034842241154,30.7993203435596)) ;
#94856 = CARTESIAN_POINT('Ctrl Pts',(80.9917381958488,192.787718030768,23.1313203435596)) ;
#94857 = CARTESIAN_POINT('Ctrl Pts',(80.9917381958488,192.787718030768,30.7993203435596)) ;
#94858 = CARTESIAN_POINT('Ctrl Pts',(78.9189744912756,195.138085698398,23.1313203435596)) ;
#94859 = CARTESIAN_POINT('Ctrl Pts',(78.9189744912756,195.138085698398,30.7993203435596)) ;
#94860 = CARTESIAN_POINT('Ctrl Pts',(76.6209129092212,198.099602509355,23.1313203435596)) ;
#94861 = CARTESIAN_POINT('Ctrl Pts',(76.6209129092212,198.099602509355,30.7993203435596)) ;
#94862 = CARTESIAN_POINT('Ctrl Pts',(74.6447403893034,201.087008680127,23.1313203435596)) ;
#94863 = CARTESIAN_POINT('Ctrl Pts',(74.6447403893034,201.087008680127,30.7993203435596)) ;
#94864 = CARTESIAN_POINT('Ctrl Pts',(73.0215367693529,204.102803944955,23.1313203435596)) ;
#94865 = CARTESIAN_POINT('Ctrl Pts',(73.0215367693529,204.102803944955,30.7993203435596)) ;
#94866 = CARTESIAN_POINT('Ctrl Pts',(71.775922405272,207.148968505506,23.1313203435596)) ;
#94867 = CARTESIAN_POINT('Ctrl Pts',(71.775922405272,207.148968505506,30.7993203435596)) ;
#94868 = CARTESIAN_POINT('Ctrl Pts',(70.9055309357216,210.225312036653,23.1313203435596)) ;
#94869 = CARTESIAN_POINT('Ctrl Pts',(70.9055309357216,210.225312036653,30.7993203435596)) ;
#94870 = CARTESIAN_POINT('Ctrl Pts',(70.3872265023368,213.329973734064,23.1313203435596)) ;
#94871 = CARTESIAN_POINT('Ctrl Pts',(70.3872265023368,213.329973734064,30.7993203435596)) ;
#94872 = CARTESIAN_POINT('Ctrl Pts',(70.2337598673437,215.834709407061,23.1313203435596)) ;
#94873 = CARTESIAN_POINT('Ctrl Pts',(70.2337598673437,215.834709407061,30.7993203435596)) ;
#94874 = CARTESIAN_POINT('Ctrl Pts',(70.2566219573908,217.724357374766,23.1313203435596)) ;
#94875 = CARTESIAN_POINT('Ctrl Pts',(70.2566219573908,217.724357374766,30.7993203435596)) ;
#94876 = CARTESIAN_POINT('Ctrl Pts',(70.3321941673992,218.988975060904,23.1313203435596)) ;
#94877 = CARTESIAN_POINT('Ctrl Pts',(70.3321941673992,218.988975060904,30.7993203435596)) ;
#94878 = CARTESIAN_POINT('Ctrl Pts',(70.3850625789433,219.622496965577,23.1313203435596)) ;
#94879 = CARTESIAN_POINT('Ctrl Pts',(70.3850625789433,219.622496965577,30.7993203435596)) ;
#94880 = CARTESIAN_POINT('Ctrl Pts',(70.3850625789433,219.622496965577,23.3713203435596)) ;
#94881 = CARTESIAN_POINT('Ctrl Pts',(70.3511634134941,219.216283439675,23.3713203435596)) ;
#94882 = CARTESIAN_POINT('Ctrl Pts',(70.3247009237789,218.810668041503,23.3713203435596)) ;
#94883 = CARTESIAN_POINT('Ctrl Pts',(70.3057017675343,218.40565291513,23.3713203435596)) ;
#94884 = CARTESIAN_POINT('Ctrl Pts',(70.3024116855331,218.335516485894,23.3713203435596)) ;
#94885 = CARTESIAN_POINT('Ctrl Pts',(70.2993455385549,218.265398067628,23.3713203435596)) ;
#94886 = CARTESIAN_POINT('Ctrl Pts',(70.2965036217263,218.19529768407,23.3713203435596)) ;
#94887 = CARTESIAN_POINT('Origin',(64.1568347953872,220.146231446812,23.3713203435596)) ;
#94888 = CARTESIAN_POINT('',(60.6037668263229,219.566828299419,30.7213203435596)) ;
#94889 = CARTESIAN_POINT('Origin',(64.1568347953872,220.146231446812,30.7213203435596)) ;
#94890 = CARTESIAN_POINT('',(60.6037668263229,219.566828299419,23.3713203435596)) ;
#94891 = CARTESIAN_POINT('',(60.6037668263229,219.566828299419,23.3713203435596)) ;
#94892 = CARTESIAN_POINT('Origin',(64.1568347953872,220.146231446812,23.3713203435596)) ;
#94893 = CARTESIAN_POINT('Origin',(64.1568347953872,220.146231446812,23.3713203435596)) ;
#94894 = CARTESIAN_POINT('',(64.9830939940346,223.650128668,23.3713203435596)) ;
#94895 = CARTESIAN_POINT('',(64.9830939940346,223.650128668,23.3713203435596)) ;
#94896 = CARTESIAN_POINT('Origin',(64.1568347953872,220.146231446812,23.3713203435596)) ;
#94897 = CARTESIAN_POINT('Origin',(57.4999031800138,224.540465846463,30.7213203435596)) ;
#94898 = CARTESIAN_POINT('',(57.4999031800138,224.540465846463,30.7213203435596)) ;
#94899 = CARTESIAN_POINT('',(57.4999031800138,224.540465846463,30.7213203435596)) ;
#94900 = CARTESIAN_POINT('',(57.4999031800138,224.540465846463,30.7213203435596)) ;
#94901 = CARTESIAN_POINT('Origin',(70.9999999999998,217.633222662033,29.5213203435596)) ;
#94902 = CARTESIAN_POINT('',(63.8582048387328,224.775017823302,23.3713203435596)) ;
#94903 = CARTESIAN_POINT('',(63.8582048387328,224.775017823302,29.5213203435596)) ;
#94904 = CARTESIAN_POINT('',(69.0112682894225,219.621954372611,23.3713203435596)) ;
#94905 = CARTESIAN_POINT('Origin',(63.8582048387328,224.775017823302,29.5213203435596)) ;
#94906 = CARTESIAN_POINT('',(63.0838307469447,223.535760225819,23.3713203435596)) ;
#94907 = CARTESIAN_POINT('Origin',(65.632121620491,220.220271124835,23.3713203435596)) ;
#94908 = CARTESIAN_POINT('',(60.321811570171,219.115605567354,23.3713203435596)) ;
#94909 = CARTESIAN_POINT('',(63.0838307469447,223.535760225819,23.3713203435596)) ;
#94910 = CARTESIAN_POINT('',(61.3703326482681,217.618162279643,23.3713203435596)) ;
#94911 = CARTESIAN_POINT('',(60.9479927510422,218.221326162033,23.3713203435596)) ;
#94912 = CARTESIAN_POINT('',(63.3614933659283,216.167053742856,23.3713203435596)) ;
#94913 = CARTESIAN_POINT('Origin',(64.4831104165663,219.797752737776,23.3713203435596)) ;
#94914 = CARTESIAN_POINT('',(69.4079308494226,215.768555109772,23.3713203435596)) ;
#94915 = CARTESIAN_POINT('',(67.38212743034,215.902068421636,23.3713203435596)) ;
#94916 = CARTESIAN_POINT('Origin',(69.4999999999997,217.165524426368,23.3713203435596)) ;
#94917 = CARTESIAN_POINT('',(62.9568347953872,216.946231446812,23.3713203435596)) ;
#94918 = CARTESIAN_POINT('',(65.4944782079391,216.946231446812,23.3713203435596)) ;
#94919 = CARTESIAN_POINT('',(62.9568347953872,218.583251285823,23.3713203435596)) ;
#94920 = CARTESIAN_POINT('Origin',(64.4831104165663,219.797752737776,23.2713203435596)) ;
#94921 = CARTESIAN_POINT('Origin',(61.3703326482681,217.618162279643,23.2713203435596)) ;
#94922 = CARTESIAN_POINT('Origin',(63.3615337725872,216.167062621809,23.271302987489)) ;
#94923 = CARTESIAN_POINT('Origin',(67.38212743034,215.902068421636,23.2713203435596)) ;
#94924 = CARTESIAN_POINT('Origin',(69.4079308494226,215.768555109772,23.2713203435596)) ;
#94925 = CARTESIAN_POINT('Origin',(69.4999999999997,217.165524426368,23.2713203435596)) ;
#94926 = CARTESIAN_POINT('Origin',(60.9479927510422,218.221326162033,23.2713203435596)) ;
#94927 = CARTESIAN_POINT('Origin',(60.321811570171,219.115605567354,23.2713203435596)) ;
#94928 = CARTESIAN_POINT('Origin',(63.8582048387328,224.775017823302,29.5213203435596)) ;
#94929 = CARTESIAN_POINT('',(60.2066749117936,218.931348397394,30.7213203435596)) ;
#94930 = CARTESIAN_POINT('Origin',(28.3,247.7,21.7213203435596)) ;
#94931 = CARTESIAN_POINT('',(31.,247.7,26.7213203435596)) ;
#94932 = CARTESIAN_POINT('',(27.3,247.7,26.7213203435596)) ;
#94933 = CARTESIAN_POINT('',(31.,247.7,21.7213203435596)) ;
#94934 = CARTESIAN_POINT('',(31.,247.7,21.7213203435596)) ;
#94935 = CARTESIAN_POINT('',(27.3,247.7,21.7213203435596)) ;
#94936 = CARTESIAN_POINT('Origin',(28.3,245.7,26.7213203435596)) ;
#94937 = CARTESIAN_POINT('',(31.,245.7,21.7213203435596)) ;
#94938 = CARTESIAN_POINT('',(27.3,245.7,21.7213203435596)) ;
#94939 = CARTESIAN_POINT('',(31.,245.7,26.7213203435596)) ;
#94940 = CARTESIAN_POINT('',(31.,245.7,26.7213203435596)) ;
#94941 = CARTESIAN_POINT('',(27.3,245.7,26.7213203435596)) ;
#94942 = CARTESIAN_POINT('Origin',(31.,246.7,24.2213203435596)) ;
#94943 = CARTESIAN_POINT('',(31.,249.25,26.7213203435596)) ;
#94944 = CARTESIAN_POINT('',(31.,245.9,21.7213203435596)) ;
#94945 = CARTESIAN_POINT('Origin',(26.3,251.8,26.7213203435596)) ;
#94946 = CARTESIAN_POINT('',(31.8,251.8,26.7213203435596)) ;
#94947 = CARTESIAN_POINT('Origin',(26.3,251.8,21.7213203435596)) ;
#94948 = CARTESIAN_POINT('',(31.8,251.8,21.7213203435596)) ;
#94949 = CARTESIAN_POINT('Origin',(26.3,245.1,21.7213203435596)) ;
#94950 = CARTESIAN_POINT('',(31.8,245.1,21.7213203435596)) ;
#94951 = CARTESIAN_POINT('Origin',(31.8,248.45,24.2213203435596)) ;
#94952 = CARTESIAN_POINT('Origin',(31.6354870749573,258.344201743738,20.2213203435596)) ;
#94953 = CARTESIAN_POINT('',(31.5632689765959,258.377877596062,20.3213203435596)) ;
#94954 = CARTESIAN_POINT('',(31.9729281400346,258.186850390917,20.3213203435596)) ;
#94955 = CARTESIAN_POINT('',(31.6354870749573,258.344201743738,20.3213203435596)) ;
#94956 = CARTESIAN_POINT('',(31.8391836130389,258.138878696195,20.2213203435596)) ;
#94957 = CARTESIAN_POINT('Ctrl Pts',(31.9729281400345,258.186850390917,20.3213203435596)) ;
#94958 = CARTESIAN_POINT('Ctrl Pts',(31.9726024539967,258.186730118955,20.3213203435596)) ;
#94959 = CARTESIAN_POINT('Ctrl Pts',(31.9722767429558,258.186609910221,20.3213194310587)) ;
#94960 = CARTESIAN_POINT('Ctrl Pts',(31.9566232186436,258.18083617139,20.3212317767765)) ;
#94961 = CARTESIAN_POINT('Ctrl Pts',(31.9410876688426,258.175272220085,20.3191272439651)) ;
#94962 = CARTESIAN_POINT('Ctrl Pts',(31.9123178937877,258.165043736205,20.3111145572994)) ;
#94963 = CARTESIAN_POINT('Ctrl Pts',(31.8985908679471,258.160195813954,20.3053444921507)) ;
#94964 = CARTESIAN_POINT('Ctrl Pts',(31.8733668278068,258.151021378108,20.2891795517339)) ;
#94965 = CARTESIAN_POINT('Ctrl Pts',(31.8626456130347,258.147058717567,20.2790419175932)) ;
#94966 = CARTESIAN_POINT('Ctrl Pts',(31.8498697583427,258.142470666398,20.260741297088)) ;
#94967 = CARTESIAN_POINT('Ctrl Pts',(31.8459410167225,258.14109113882,20.2532165079448)) ;
#94968 = CARTESIAN_POINT('Ctrl Pts',(31.8406780156682,258.139281704229,20.2374755979539)) ;
#94969 = CARTESIAN_POINT('Ctrl Pts',(31.8392887152522,258.138829692159,20.2294674434764)) ;
#94970 = CARTESIAN_POINT('Ctrl Pts',(31.8392904312326,258.138828886053,20.2213204095382)) ;
#94971 = CARTESIAN_POINT('',(31.3863264609896,258.350049454246,20.2213203435596)) ;
#94972 = CARTESIAN_POINT('',(31.5932252487832,258.253570965035,20.2213203435596)) ;
#94973 = CARTESIAN_POINT('Origin',(31.5632689765959,258.377877596062,20.2213203435596)) ;
#94974 = CARTESIAN_POINT('Ctrl Pts',(31.8826961677427,258.229957132574,20.2213203435596)) ;
#94975 = CARTESIAN_POINT('Ctrl Pts',(31.8082406667398,258.074105253142,20.2213203435596)) ;
#94976 = CARTESIAN_POINT('Ctrl Pts',(31.6975075374418,257.838597906516,20.2213203435596)) ;
#94977 = CARTESIAN_POINT('Ctrl Pts',(31.5516420000274,257.525488877785,20.2213203435596)) ;
#94978 = CARTESIAN_POINT('Ctrl Pts',(31.4640838198982,257.326016007648,20.2213203435596)) ;
#94979 = CARTESIAN_POINT('Ctrl Pts',(31.3867201416434,257.194870160616,20.2213203435596)) ;
#94980 = CARTESIAN_POINT('Ctrl Pts',(31.318862957822,257.131020174664,20.2213203435596)) ;
#94981 = CARTESIAN_POINT('Ctrl Pts',(31.1611331373571,257.060468743905,20.2213203435597)) ;
#94982 = CARTESIAN_POINT('Ctrl Pts',(30.993693898815,257.054864391304,20.2213203435596)) ;
#94983 = CARTESIAN_POINT('Ctrl Pts',(30.8701100175112,257.060056991359,20.2213203435596)) ;
#94984 = CARTESIAN_POINT('Ctrl Pts',(31.8826961677427,258.229957132574,20.2512402735938)) ;
#94985 = CARTESIAN_POINT('Ctrl Pts',(31.8082407435551,258.074105413933,20.2512402735938)) ;
#94986 = CARTESIAN_POINT('Ctrl Pts',(31.6973456699681,257.838498509911,20.2512402735938)) ;
#94987 = CARTESIAN_POINT('Ctrl Pts',(31.5514897050399,257.525395035868,20.2512402735938)) ;
#94988 = CARTESIAN_POINT('Ctrl Pts',(31.4638702756497,257.325881332878,20.2512402735938)) ;
#94989 = CARTESIAN_POINT('Ctrl Pts',(31.3865371441645,257.194796533992,20.2512402735938)) ;
#94990 = CARTESIAN_POINT('Ctrl Pts',(31.3187416910112,257.131018868321,20.2512402735938)) ;
#94991 = CARTESIAN_POINT('Ctrl Pts',(31.1611435563971,257.060513922087,20.2512402735938)) ;
#94992 = CARTESIAN_POINT('Ctrl Pts',(30.9936750861112,257.054865181754,20.2512402735938)) ;
#94993 = CARTESIAN_POINT('Ctrl Pts',(30.8701100175112,257.060056991359,20.2512402735938)) ;
#94994 = CARTESIAN_POINT('Ctrl Pts',(31.905373394501,258.219123485359,20.3030172712892)) ;
#94995 = CARTESIAN_POINT('Ctrl Pts',(31.8309118350413,258.063258924232,20.3030172712892)) ;
#94996 = CARTESIAN_POINT('Ctrl Pts',(31.7201990688088,257.827925373884,20.3030172712892)) ;
#94997 = CARTESIAN_POINT('Ctrl Pts',(31.5743763641736,257.514858199604,20.3030172712892)) ;
#94998 = CARTESIAN_POINT('Ctrl Pts',(31.4869575684128,257.315781063247,20.3030172712892)) ;
#94999 = CARTESIAN_POINT('Ctrl Pts',(31.4072395052171,257.179852665022,20.3030172712892)) ;
#95000 = CARTESIAN_POINT('Ctrl Pts',(31.3325657749029,257.109128082676,20.3030172712892)) ;
#95001 = CARTESIAN_POINT('Ctrl Pts',(31.1638934400229,257.034573409644,20.3030172712892)) ;
#95002 = CARTESIAN_POINT('Ctrl Pts',(30.9941226236966,257.029692061861,20.3030172712892)) ;
#95003 = CARTESIAN_POINT('Ctrl Pts',(30.8690549760692,257.034947005039,20.3030172712892)) ;
#95004 = CARTESIAN_POINT('Ctrl Pts',(31.952680132801,258.196523521125,20.3213203435596)) ;
#95005 = CARTESIAN_POINT('Ctrl Pts',(31.8782059784266,258.040632596048,20.3213203435596)) ;
#95006 = CARTESIAN_POINT('Ctrl Pts',(31.7674438315788,257.805605128362,20.3213203435597)) ;
#95007 = CARTESIAN_POINT('Ctrl Pts',(31.6217159097903,257.492628417029,20.3213203435597)) ;
#95008 = CARTESIAN_POINT('Ctrl Pts',(31.5345531399074,257.294353655337,20.3213203435597)) ;
#95009 = CARTESIAN_POINT('Ctrl Pts',(31.4499409446598,257.148483052797,20.3213203435597)) ;
#95010 = CARTESIAN_POINT('Ctrl Pts',(31.361082299714,257.063458465252,20.3213203435597)) ;
#95011 = CARTESIAN_POINT('Ctrl Pts',(31.1696575900964,256.980579035594,20.3213203435597)) ;
#95012 = CARTESIAN_POINT('Ctrl Pts',(30.9950063112822,256.977180762913,20.3213203435596)) ;
#95013 = CARTESIAN_POINT('Ctrl Pts',(30.866854064559,256.982565311094,20.3213203435596)) ;
#95014 = CARTESIAN_POINT('Ctrl Pts',(31.9729281400347,258.186850390917,20.3213203435596)) ;
#95015 = CARTESIAN_POINT('Ctrl Pts',(31.8984486030264,258.030948198793,20.3213203435596)) ;
#95016 = CARTESIAN_POINT('Ctrl Pts',(31.7876480706037,257.796041134552,20.3213203435597)) ;
#95017 = CARTESIAN_POINT('Ctrl Pts',(31.6419617369609,257.483103734415,20.3213203435597)) ;
#95018 = CARTESIAN_POINT('Ctrl Pts',(31.5549020259439,257.28516805193,20.3213203435597)) ;
#95019 = CARTESIAN_POINT('Ctrl Pts',(31.4681983211233,257.135048536644,20.3213203435597)) ;
#95020 = CARTESIAN_POINT('Ctrl Pts',(31.373274891254,257.043911031634,20.3213203435597)) ;
#95021 = CARTESIAN_POINT('Ctrl Pts',(31.1721258442632,256.957473430288,20.3213203435597)) ;
#95022 = CARTESIAN_POINT('Ctrl Pts',(30.995382539195,256.954705208349,20.3213203435596)) ;
#95023 = CARTESIAN_POINT('Ctrl Pts',(30.8659120407843,256.960145145257,20.3213203435596)) ;
#95024 = CARTESIAN_POINT('',(30.965916234277,256.957946490344,20.3213203435596)) ;
#95025 = CARTESIAN_POINT('Ctrl Pts',(31.9729281400347,258.186850390917,20.3213203435596)) ;
#95026 = CARTESIAN_POINT('Ctrl Pts',(31.8984486030264,258.030948198793,20.3213203435596)) ;
#95027 = CARTESIAN_POINT('Ctrl Pts',(31.7876480706037,257.796041134552,20.3213203435597)) ;
#95028 = CARTESIAN_POINT('Ctrl Pts',(31.6419617369609,257.483103734415,20.3213203435597)) ;
#95029 = CARTESIAN_POINT('Ctrl Pts',(31.5549020259439,257.28516805193,20.3213203435597)) ;
#95030 = CARTESIAN_POINT('Ctrl Pts',(31.4681983211233,257.135048536644,20.3213203435597)) ;
#95031 = CARTESIAN_POINT('Ctrl Pts',(31.373274891254,257.043911031634,20.3213203435597)) ;
#95032 = CARTESIAN_POINT('Ctrl Pts',(31.2030784552785,256.970774360576,20.3213203435597)) ;
#95033 = CARTESIAN_POINT('Ctrl Pts',(31.06278978041,256.958226134581,20.3213203435597)) ;
#95034 = CARTESIAN_POINT('Ctrl Pts',(30.9659328929364,256.957945874245,20.3213203435597)) ;
#95035 = CARTESIAN_POINT('',(30.8701100175112,257.060056991359,20.2213203435596)) ;
#95036 = CARTESIAN_POINT('Ctrl Pts',(30.9659078630823,256.957945802006,20.3213203435596)) ;
#95037 = CARTESIAN_POINT('Ctrl Pts',(30.965671039864,256.958187990349,20.3213203435596)) ;
#95038 = CARTESIAN_POINT('Ctrl Pts',(30.9654342887815,256.958430251337,20.3213194300433)) ;
#95039 = CARTESIAN_POINT('Ctrl Pts',(30.9538716458124,256.970269071732,20.3212302458049)) ;
#95040 = CARTESIAN_POINT('Ctrl Pts',(30.9426060928688,256.982148587136,20.3190544364554)) ;
#95041 = CARTESIAN_POINT('Ctrl Pts',(30.9218631652494,257.004280924155,20.31084455494)) ;
#95042 = CARTESIAN_POINT('Ctrl Pts',(30.9120149894988,257.01490568464,20.3049218660286)) ;
#95043 = CARTESIAN_POINT('Ctrl Pts',(30.8938674792948,257.034213340876,20.2884844231793)) ;
#95044 = CARTESIAN_POINT('Ctrl Pts',(30.8861826729993,257.042373958168,20.2782727116012)) ;
#95045 = CARTESIAN_POINT('Ctrl Pts',(30.8772600100429,257.052056353529,20.2600246370711)) ;
#95046 = CARTESIAN_POINT('Ctrl Pts',(30.8745807988497,257.055014131683,20.2526227319016)) ;
#95047 = CARTESIAN_POINT('Ctrl Pts',(30.8710246291092,257.05899573171,20.2371678111417)) ;
#95048 = CARTESIAN_POINT('Ctrl Pts',(30.8701100175114,257.060056991359,20.2293097304074)) ;
#95049 = CARTESIAN_POINT('Ctrl Pts',(30.8701100175114,257.060056991359,20.2213203435596)) ;
#95050 = CARTESIAN_POINT('Ctrl Pts',(30.8701100175112,257.060056991359,20.2213203435596)) ;
#95051 = CARTESIAN_POINT('Ctrl Pts',(30.8881460152925,257.059299176326,20.2213203435596)) ;
#95052 = CARTESIAN_POINT('Ctrl Pts',(30.9060122530829,257.058797146371,20.2213203435596)) ;
#95053 = CARTESIAN_POINT('Ctrl Pts',(30.9237874982588,257.058573241475,20.2213203435596)) ;
#95054 = CARTESIAN_POINT('Ctrl Pts',(30.9414214994052,257.058351115751,20.2213203435596)) ;
#95055 = CARTESIAN_POINT('Ctrl Pts',(30.958966057566,257.058402889749,20.2213203435596)) ;
#95056 = CARTESIAN_POINT('Ctrl Pts',(30.9764494613066,257.058765569003,20.2213203435596)) ;
#95057 = CARTESIAN_POINT('Ctrl Pts',(30.9937966530257,257.059125422647,20.2213203435596)) ;
#95058 = CARTESIAN_POINT('Ctrl Pts',(31.0110837583664,257.059791597926,20.2213203435596)) ;
#95059 = CARTESIAN_POINT('Ctrl Pts',(31.0282886130343,257.060812188465,20.2213203435596)) ;
#95060 = CARTESIAN_POINT('Ctrl Pts',(31.0453745456915,257.06182572456,20.2213203435596)) ;
#95061 = CARTESIAN_POINT('Ctrl Pts',(31.0623794450239,257.063189146832,20.2213203435596)) ;
#95062 = CARTESIAN_POINT('Ctrl Pts',(31.0792307306913,257.064957006289,20.2213203435596)) ;
#95063 = CARTESIAN_POINT('Ctrl Pts',(31.0960542072034,257.066721948302,20.2213203435596)) ;
#95064 = CARTESIAN_POINT('Ctrl Pts',(31.1127246102277,257.068890521463,20.2213203435597)) ;
#95065 = CARTESIAN_POINT('Ctrl Pts',(31.1291178321619,257.071517944538,20.2213203435597)) ;
#95066 = CARTESIAN_POINT('Ctrl Pts',(31.1454306602944,257.074132482499,20.2213203435597)) ;
#95067 = CARTESIAN_POINT('Ctrl Pts',(31.1614688636718,257.077202150573,20.2213203435597)) ;
#95068 = CARTESIAN_POINT('Ctrl Pts',(31.1770596212641,257.080772665844,20.2213203435597)) ;
#95069 = CARTESIAN_POINT('Ctrl Pts',(31.1923295505933,257.084269706673,20.2213203435597)) ;
#95070 = CARTESIAN_POINT('Ctrl Pts',(31.2071697772336,257.088248157638,20.2213203435597)) ;
#95071 = CARTESIAN_POINT('Ctrl Pts',(31.2213742220269,257.092729903584,20.2213203435597)) ;
#95072 = CARTESIAN_POINT('Ctrl Pts',(31.2305286847959,257.095618293592,20.2213203435596)) ;
#95073 = CARTESIAN_POINT('Ctrl Pts',(31.2396247906868,257.098783024267,20.2213203435596)) ;
#95074 = CARTESIAN_POINT('Ctrl Pts',(31.2484400659356,257.102196823945,20.2213203435596)) ;
#95075 = CARTESIAN_POINT('Ctrl Pts',(31.2564036162801,257.105280785005,20.2213203435596)) ;
#95076 = CARTESIAN_POINT('Ctrl Pts',(31.2641382578939,257.108567681928,20.2213203435596)) ;
#95077 = CARTESIAN_POINT('Ctrl Pts',(31.2715131924955,257.112021656713,20.2213203435596)) ;
#95078 = CARTESIAN_POINT('Ctrl Pts',(31.2805359440217,257.11624736961,20.2213203435596)) ;
#95079 = CARTESIAN_POINT('Ctrl Pts',(31.289364636101,257.120737569893,20.2213203435596)) ;
#95080 = CARTESIAN_POINT('Ctrl Pts',(31.2978878243988,257.125497027665,20.2213203435596)) ;
#95081 = CARTESIAN_POINT('Ctrl Pts',(31.3034204922576,257.12858654043,20.2213203435596)) ;
#95082 = CARTESIAN_POINT('Ctrl Pts',(31.3088255627919,257.131789527954,20.2213203435596)) ;
#95083 = CARTESIAN_POINT('Ctrl Pts',(31.3140842359417,257.135106517862,20.2213203435596)) ;
#95084 = CARTESIAN_POINT('Ctrl Pts',(31.3251260171775,257.142071293174,20.2213203435596)) ;
#95085 = CARTESIAN_POINT('Ctrl Pts',(31.335568121659,257.149562438639,20.2213203435596)) ;
#95086 = CARTESIAN_POINT('Ctrl Pts',(31.3455081907556,257.157763710087,20.2213203435596)) ;
#95087 = CARTESIAN_POINT('Ctrl Pts',(31.3542057512151,257.164939822604,20.2213203435596)) ;
#95088 = CARTESIAN_POINT('Ctrl Pts',(31.3625183834661,257.172659779784,20.2213203435596)) ;
#95089 = CARTESIAN_POINT('Ctrl Pts',(31.3705318439148,257.181079707773,20.2213203435596)) ;
#95090 = CARTESIAN_POINT('Ctrl Pts',(31.3745857184255,257.185339207359,20.2213203435596)) ;
#95091 = CARTESIAN_POINT('Ctrl Pts',(31.3785634161927,257.189778383009,20.2213203435596)) ;
#95092 = CARTESIAN_POINT('Ctrl Pts',(31.3824791104723,257.194421183466,20.2213203435596)) ;
#95093 = CARTESIAN_POINT('Ctrl Pts',(31.3856937678516,257.198232771319,20.2213203435596)) ;
#95094 = CARTESIAN_POINT('Ctrl Pts',(31.3888701589267,257.202186788496,20.2213203435596)) ;
#95095 = CARTESIAN_POINT('Ctrl Pts',(31.3919927963429,257.206263925275,20.2213203435596)) ;
#95096 = CARTESIAN_POINT('Ctrl Pts',(31.3982423422826,257.214423775492,20.2213203435596)) ;
#95097 = CARTESIAN_POINT('Ctrl Pts',(31.404285482801,257.223091327263,20.2213203435596)) ;
#95098 = CARTESIAN_POINT('Ctrl Pts',(31.4101412935664,257.232211050084,20.2213203435596)) ;
#95099 = CARTESIAN_POINT('Ctrl Pts',(31.4158483968946,257.241099178911,20.2213203435596)) ;
#95100 = CARTESIAN_POINT('Ctrl Pts',(31.421379377071,257.250417334289,20.2213203435596)) ;
#95101 = CARTESIAN_POINT('Ctrl Pts',(31.4267676789623,257.260069003584,20.2213203435596)) ;
#95102 = CARTESIAN_POINT('Ctrl Pts',(31.4313169879582,257.268217846546,20.2213203435596)) ;
#95103 = CARTESIAN_POINT('Ctrl Pts',(31.4357653406137,257.276603779098,20.2213203435596)) ;
#95104 = CARTESIAN_POINT('Ctrl Pts',(31.4401282884918,257.285139319864,20.2213203435596)) ;
#95105 = CARTESIAN_POINT('Ctrl Pts',(31.4425442454129,257.289865825741,20.2213203435596)) ;
#95106 = CARTESIAN_POINT('Ctrl Pts',(31.4449324432114,257.294634794624,20.2213203435596)) ;
#95107 = CARTESIAN_POINT('Ctrl Pts',(31.4472990616257,257.299438290958,20.2213203435596)) ;
#95108 = CARTESIAN_POINT('Ctrl Pts',(31.453697048331,257.312424206006,20.2213203435596)) ;
#95109 = CARTESIAN_POINT('Ctrl Pts',(31.459951086791,257.325681772639,20.2213203435596)) ;
#95110 = CARTESIAN_POINT('Ctrl Pts',(31.4661895021085,257.339150167048,20.2213203435596)) ;
#95111 = CARTESIAN_POINT('Ctrl Pts',(31.4728199784414,257.353464999555,20.2213203435596)) ;
#95112 = CARTESIAN_POINT('Ctrl Pts',(31.479432120829,257.368017614714,20.2213203435596)) ;
#95113 = CARTESIAN_POINT('Ctrl Pts',(31.4861192778588,257.382734893759,20.2213203435596)) ;
#95114 = CARTESIAN_POINT('Ctrl Pts',(31.4934700853774,257.398912753046,20.2213203435596)) ;
#95115 = CARTESIAN_POINT('Ctrl Pts',(31.5009109032352,257.415289051434,20.2213203435596)) ;
#95116 = CARTESIAN_POINT('Ctrl Pts',(31.5085049435486,257.431774039478,20.2213203435596)) ;
#95117 = CARTESIAN_POINT('Ctrl Pts',(31.5089271055015,257.432690460047,20.2213203435596)) ;
#95118 = CARTESIAN_POINT('Ctrl Pts',(31.5093497283266,257.43360721947,20.2213203435596)) ;
#95119 = CARTESIAN_POINT('Ctrl Pts',(31.509772818656,257.434524303432,20.2213203435596)) ;
#95120 = CARTESIAN_POINT('Ctrl Pts',(31.5165025689967,257.449111604719,20.2213203435596)) ;
#95121 = CARTESIAN_POINT('Ctrl Pts',(31.5233210366753,257.463886724714,20.2213203435596)) ;
#95122 = CARTESIAN_POINT('Ctrl Pts',(31.5301544632509,257.478686862547,20.2213203435596)) ;
#95123 = CARTESIAN_POINT('Ctrl Pts',(31.5365608006656,257.492561991765,20.2213203435596)) ;
#95124 = CARTESIAN_POINT('Ctrl Pts',(31.5429807467931,257.506460149131,20.2213203435596)) ;
#95125 = CARTESIAN_POINT('Ctrl Pts',(31.5493714042548,257.520287040577,20.2213203435596)) ;
#95126 = CARTESIAN_POINT('Ctrl Pts',(31.5513920368639,257.52465890183,20.2213203435596)) ;
#95127 = CARTESIAN_POINT('Ctrl Pts',(31.5534094887509,257.529023100625,20.2213203435596)) ;
#95128 = CARTESIAN_POINT('Ctrl Pts',(31.5554299324024,257.533392951736,20.2213203435596)) ;
#95129 = CARTESIAN_POINT('Ctrl Pts',(31.5633310508952,257.550481629959,20.2213203435596)) ;
#95130 = CARTESIAN_POINT('Ctrl Pts',(31.5712513069425,257.567599094905,20.2213203435596)) ;
#95131 = CARTESIAN_POINT('Ctrl Pts',(31.5791650505042,257.584687939887,20.2213203435596)) ;
#95132 = CARTESIAN_POINT('Ctrl Pts',(31.587614982311,257.602934623473,20.2213203435596)) ;
#95133 = CARTESIAN_POINT('Ctrl Pts',(31.5960576753152,257.621149119168,20.2213203435596)) ;
#95134 = CARTESIAN_POINT('Ctrl Pts',(31.6044872091412,257.639316861752,20.2213203435596)) ;
#95135 = CARTESIAN_POINT('Ctrl Pts',(31.6135924929299,257.658941013625,20.2213203435596)) ;
#95136 = CARTESIAN_POINT('Ctrl Pts',(31.6226826149776,257.678511082707,20.2213203435596)) ;
#95137 = CARTESIAN_POINT('Ctrl Pts',(31.6317756665799,257.698063905933,20.2213203435596)) ;
#95138 = CARTESIAN_POINT('Ctrl Pts',(31.6403047005873,257.716403919992,20.2213203435596)) ;
#95139 = CARTESIAN_POINT('Ctrl Pts',(31.6488368372567,257.734729927809,20.2213203435596)) ;
#95140 = CARTESIAN_POINT('Ctrl Pts',(31.6574024333342,257.753105040464,20.2213203435596)) ;
#95141 = CARTESIAN_POINT('Ctrl Pts',(31.6619174230045,257.762790699591,20.2213203435596)) ;
#95142 = CARTESIAN_POINT('Ctrl Pts',(31.6664420477939,257.772490706991,20.2213203435596)) ;
#95143 = CARTESIAN_POINT('Ctrl Pts',(31.6709701075337,257.782191437883,20.2213203435596)) ;
#95144 = CARTESIAN_POINT('Ctrl Pts',(31.6842270030051,257.810592471177,20.2213203435596)) ;
#95145 = CARTESIAN_POINT('Ctrl Pts',(31.6975227286466,257.839019902207,20.2213203435596)) ;
#95146 = CARTESIAN_POINT('Ctrl Pts',(31.7108387516935,257.867425705876,20.2213203435596)) ;
#95147 = CARTESIAN_POINT('Ctrl Pts',(31.7269899500257,257.901879518941,20.2213203435596)) ;
#95148 = CARTESIAN_POINT('Ctrl Pts',(31.7431711953078,257.936302176977,20.2213203435596)) ;
#95149 = CARTESIAN_POINT('Ctrl Pts',(31.7593838316716,257.970678860503,20.2213203435596)) ;
#95150 = CARTESIAN_POINT('Ctrl Pts',(31.7845303488226,258.023998619393,20.2213203435596)) ;
#95151 = CARTESIAN_POINT('Ctrl Pts',(31.8097554620621,258.077217498546,20.2213203435596)) ;
#95152 = CARTESIAN_POINT('Ctrl Pts',(31.8351282490926,258.130384143046,20.2213203435596)) ;
#95153 = CARTESIAN_POINT('Ctrl Pts',(31.836479618475,258.133215829429,20.2213203435596)) ;
#95154 = CARTESIAN_POINT('Ctrl Pts',(31.8378314038708,258.136047348203,20.2213203435596)) ;
#95155 = CARTESIAN_POINT('Ctrl Pts',(31.8391836130389,258.138878696195,20.2213203435596)) ;
#95156 = CARTESIAN_POINT('Origin',(30.9927777216053,257.597448434855,20.2213203435596)) ;
#95157 = CARTESIAN_POINT('',(30.9575197581061,256.75826900652,20.3213203435596)) ;
#95158 = CARTESIAN_POINT('',(30.9927777216053,257.597448434855,20.3213203435596)) ;
#95159 = CARTESIAN_POINT('',(30.8533181106036,256.660409606953,20.2213203435596)) ;
#95160 = CARTESIAN_POINT('Ctrl Pts',(30.9575180778337,256.758268913088,20.3213203435596)) ;
#95161 = CARTESIAN_POINT('Ctrl Pts',(30.9572608740877,256.758025782119,20.3213203435596)) ;
#95162 = CARTESIAN_POINT('Ctrl Pts',(30.9570036902145,256.757782627797,20.321319430125)) ;
#95163 = CARTESIAN_POINT('Ctrl Pts',(30.9447772812169,256.74622121684,20.3212325950421)) ;
#95164 = CARTESIAN_POINT('Ctrl Pts',(30.9327366006538,256.734738416808,20.3191690170698)) ;
#95165 = CARTESIAN_POINT('Ctrl Pts',(30.9104851869289,256.713579232422,20.3112355499301)) ;
#95166 = CARTESIAN_POINT('Ctrl Pts',(30.8998969464719,256.703542376543,20.3055366838106)) ;
#95167 = CARTESIAN_POINT('Ctrl Pts',(30.8801360641889,256.685251674835,20.2894998523043)) ;
#95168 = CARTESIAN_POINT('Ctrl Pts',(30.8716480508847,256.677535742468,20.2794186430539)) ;
#95169 = CARTESIAN_POINT('Ctrl Pts',(30.861575957675,256.66822888513,20.2611063637428)) ;
#95170 = CARTESIAN_POINT('Ctrl Pts',(30.8584846426284,256.665338066437,20.2535176474882)) ;
#95171 = CARTESIAN_POINT('Ctrl Pts',(30.8543790138895,256.661448508963,20.2376314832746)) ;
#95172 = CARTESIAN_POINT('Ctrl Pts',(30.8533181106036,256.660409606953,20.22954590721)) ;
#95173 = CARTESIAN_POINT('Ctrl Pts',(30.8533181106036,256.660409606953,20.2213203435596)) ;
#95174 = CARTESIAN_POINT('',(30.8928658755038,257.601646411582,20.2213203435596)) ;
#95175 = CARTESIAN_POINT('Ctrl Pts',(30.8533181106035,256.660409606953,20.2213203435596)) ;
#95176 = CARTESIAN_POINT('Ctrl Pts',(30.9548849732834,256.656142091714,20.2213203435596)) ;
#95177 = CARTESIAN_POINT('Ctrl Pts',(31.1603957461103,256.65842875267,20.2213203435596)) ;
#95178 = CARTESIAN_POINT('Ctrl Pts',(31.4294296466895,256.727933237041,20.2213203435596)) ;
#95179 = CARTESIAN_POINT('Ctrl Pts',(31.620729986201,256.8593293761,20.2213203435596)) ;
#95180 = CARTESIAN_POINT('Ctrl Pts',(31.7681817196131,257.035881970398,20.2213203435596)) ;
#95181 = CARTESIAN_POINT('Ctrl Pts',(31.8730100005906,257.26858199656,20.2213203435596)) ;
#95182 = CARTESIAN_POINT('Ctrl Pts',(31.9737678628349,257.486117355144,20.2213203435596)) ;
#95183 = CARTESIAN_POINT('Ctrl Pts',(32.0972269406744,257.751397872113,20.2213203435596)) ;
#95184 = CARTESIAN_POINT('Ctrl Pts',(32.1813080297677,257.927086809909,20.2213203435596)) ;
#95185 = CARTESIAN_POINT('Ctrl Pts',(32.2444298429768,258.059216868221,20.2213203435596)) ;
#95186 = CARTESIAN_POINT('Ctrl Pts',(30.8533181106035,256.660409606953,20.2512402735938)) ;
#95187 = CARTESIAN_POINT('Ctrl Pts',(30.9548979600485,256.656141546052,20.2512402735938)) ;
#95188 = CARTESIAN_POINT('Ctrl Pts',(31.1604023801564,256.658404182352,20.2512402735938)) ;
#95189 = CARTESIAN_POINT('Ctrl Pts',(31.4294987777394,256.727910448283,20.2512402735938)) ;
#95190 = CARTESIAN_POINT('Ctrl Pts',(31.6208848030502,256.859363688134,20.2512402735938)) ;
#95191 = CARTESIAN_POINT('Ctrl Pts',(31.7683753766291,257.03598413956,20.2512402735938)) ;
#95192 = CARTESIAN_POINT('Ctrl Pts',(31.8732029711292,257.268708585883,20.2512402735938)) ;
#95193 = CARTESIAN_POINT('Ctrl Pts',(31.9738911236935,257.486192550919,20.2512402735938)) ;
#95194 = CARTESIAN_POINT('Ctrl Pts',(32.0973472479167,257.751471757306,20.2512402735938)) ;
#95195 = CARTESIAN_POINT('Ctrl Pts',(32.1813079612835,257.927086666554,20.2512402735938)) ;
#95196 = CARTESIAN_POINT('Ctrl Pts',(32.2444298429768,258.059216868221,20.2512402735938)) ;
#95197 = CARTESIAN_POINT('Ctrl Pts',(30.8543731520913,256.685519594361,20.3030172699825)) ;
#95198 = CARTESIAN_POINT('Ctrl Pts',(30.9549157428196,256.681295115759,20.3030172699825)) ;
#95199 = CARTESIAN_POINT('Ctrl Pts',(31.1578746686145,256.6836549958,20.3030172699825)) ;
#95200 = CARTESIAN_POINT('Ctrl Pts',(31.4195632325522,256.751572357658,20.3030172699825)) ;
#95201 = CARTESIAN_POINT('Ctrl Pts',(31.6035540679525,256.878134439093,20.3030172699825)) ;
#95202 = CARTESIAN_POINT('Ctrl Pts',(31.7458235525455,257.048058386227,20.3030172699825)) ;
#95203 = CARTESIAN_POINT('Ctrl Pts',(31.8499630479459,257.278384117763,20.3030172699825)) ;
#95204 = CARTESIAN_POINT('Ctrl Pts',(31.9509466435699,257.496794195582,20.3030172699825)) ;
#95205 = CARTESIAN_POINT('Ctrl Pts',(32.0744757842965,257.762079759478,20.3030172699825)) ;
#95206 = CARTESIAN_POINT('Ctrl Pts',(32.1586361363901,257.937931623778,20.3030172699825)) ;
#95207 = CARTESIAN_POINT('Ctrl Pts',(32.221752548216,258.070050375617,20.3030172699825)) ;
#95208 = CARTESIAN_POINT('Ctrl Pts',(30.8565740635558,256.737901287217,20.3213203435596)) ;
#95209 = CARTESIAN_POINT('Ctrl Pts',(30.9549872971979,256.7337662774,20.3213203435596)) ;
#95210 = CARTESIAN_POINT('Ctrl Pts',(31.1526192371051,256.736265271766,20.3213203435596)) ;
#95211 = CARTESIAN_POINT('Ctrl Pts',(31.3990202175279,256.800872763809,20.3213203435596)) ;
#95212 = CARTESIAN_POINT('Ctrl Pts',(31.567811372452,256.917382954853,20.3213203435596)) ;
#95213 = CARTESIAN_POINT('Ctrl Pts',(31.6992922506992,257.073517437575,20.3213203435596)) ;
#95214 = CARTESIAN_POINT('Ctrl Pts',(31.8019944880323,257.298904028522,20.3213203435596)) ;
#95215 = CARTESIAN_POINT('Ctrl Pts',(31.9034094430465,257.519109697895,20.3213203435596)) ;
#95216 = CARTESIAN_POINT('Ctrl Pts',(32.0270830659073,257.784405046748,20.3213203435596)) ;
#95217 = CARTESIAN_POINT('Ctrl Pts',(32.1113404881888,257.960554799894,20.3213203435596)) ;
#95218 = CARTESIAN_POINT('Ctrl Pts',(32.174445671089,258.092650046726,20.3213203435596)) ;
#95219 = CARTESIAN_POINT('Ctrl Pts',(30.8575160873304,256.760321453054,20.3213203435596)) ;
#95220 = CARTESIAN_POINT('Ctrl Pts',(30.9550193069044,256.756224679123,20.3213203435596)) ;
#95221 = CARTESIAN_POINT('Ctrl Pts',(31.1503705386778,256.758780657464,20.3213203435596)) ;
#95222 = CARTESIAN_POINT('Ctrl Pts',(31.3902348566204,256.821971664364,20.3213203435596)) ;
#95223 = CARTESIAN_POINT('Ctrl Pts',(31.5525294429582,256.934185574877,20.3213203435596)) ;
#95224 = CARTESIAN_POINT('Ctrl Pts',(31.6793967698716,257.084425183967,20.3213203435596)) ;
#95225 = CARTESIAN_POINT('Ctrl Pts',(31.781483765643,257.307700348399,20.3213203435596)) ;
#95226 = CARTESIAN_POINT('Ctrl Pts',(31.8830759236654,257.528669084034,20.3213203435596)) ;
#95227 = CARTESIAN_POINT('Ctrl Pts',(32.0068110724735,257.793968481396,20.3213203435596)) ;
#95228 = CARTESIAN_POINT('Ctrl Pts',(32.0910972199716,257.970237850073,20.3213203435596)) ;
#95229 = CARTESIAN_POINT('Ctrl Pts',(32.1541976040146,258.102323051673,20.3213203435596)) ;
#95230 = CARTESIAN_POINT('',(32.2017228806822,257.969823855374,20.2213203435596)) ;
#95231 = CARTESIAN_POINT('Ctrl Pts',(32.2017235795172,257.969823517693,20.2213203435596)) ;
#95232 = CARTESIAN_POINT('Ctrl Pts',(32.1529021533786,257.867592660009,20.2213203435596)) ;
#95233 = CARTESIAN_POINT('Ctrl Pts',(32.0832989624708,257.721470374493,20.2213203435596)) ;
#95234 = CARTESIAN_POINT('Ctrl Pts',(31.9737678628349,257.486117355144,20.2213203435596)) ;
#95235 = CARTESIAN_POINT('Ctrl Pts',(31.8730100005906,257.26858199656,20.2213203435596)) ;
#95236 = CARTESIAN_POINT('Ctrl Pts',(31.7681817196131,257.035881970398,20.2213203435596)) ;
#95237 = CARTESIAN_POINT('Ctrl Pts',(31.620729986201,256.8593293761,20.2213203435596)) ;
#95238 = CARTESIAN_POINT('Ctrl Pts',(31.4294296466895,256.727933237041,20.2213203435596)) ;
#95239 = CARTESIAN_POINT('Ctrl Pts',(31.1603957461103,256.65842875267,20.2213203435596)) ;
#95240 = CARTESIAN_POINT('Ctrl Pts',(30.9548849732834,256.656142091714,20.2213203435596)) ;
#95241 = CARTESIAN_POINT('Ctrl Pts',(30.8533181106035,256.660409606953,20.2213203435596)) ;
#95242 = CARTESIAN_POINT('',(32.1541976040147,258.102323051673,20.3213203435596)) ;
#95243 = CARTESIAN_POINT('Ctrl Pts',(30.957523107636,256.758268931228,20.3213203435596)) ;
#95244 = CARTESIAN_POINT('Ctrl Pts',(31.0216947820032,256.75850044908,20.3213203435596)) ;
#95245 = CARTESIAN_POINT('Ctrl Pts',(31.1831674844922,256.767420842244,20.3213203435596)) ;
#95246 = CARTESIAN_POINT('Ctrl Pts',(31.3902348566204,256.821971664364,20.3213203435596)) ;
#95247 = CARTESIAN_POINT('Ctrl Pts',(31.5525294429582,256.934185574877,20.3213203435596)) ;
#95248 = CARTESIAN_POINT('Ctrl Pts',(31.6793967698716,257.084425183967,20.3213203435596)) ;
#95249 = CARTESIAN_POINT('Ctrl Pts',(31.781483765643,257.307700348399,20.3213203435596)) ;
#95250 = CARTESIAN_POINT('Ctrl Pts',(31.8830759236654,257.528669084034,20.3213203435596)) ;
#95251 = CARTESIAN_POINT('Ctrl Pts',(32.0068110724735,257.793968481396,20.3213203435596)) ;
#95252 = CARTESIAN_POINT('Ctrl Pts',(32.0910972199716,257.970237850073,20.3213203435596)) ;
#95253 = CARTESIAN_POINT('Ctrl Pts',(32.1541976040146,258.102323051673,20.3213203435596)) ;
#95254 = CARTESIAN_POINT('Ctrl Pts',(32.1541976040147,258.102323051673,20.3213203435596)) ;
#95255 = CARTESIAN_POINT('Ctrl Pts',(32.154310750693,258.101997885783,20.3213203435596)) ;
#95256 = CARTESIAN_POINT('Ctrl Pts',(32.1544239638944,258.10167274146,20.321319429295)) ;
#95257 = CARTESIAN_POINT('Ctrl Pts',(32.1598800150608,258.086013269478,20.32123140759)) ;
#95258 = CARTESIAN_POINT('Ctrl Pts',(32.1654271588702,258.070582281274,20.3191133347114)) ;
#95259 = CARTESIAN_POINT('Ctrl Pts',(32.1757628035262,258.042057844251,20.3110552232775)) ;
#95260 = CARTESIAN_POINT('Ctrl Pts',(32.1807182443946,258.028478240893,20.3052525405995)) ;
#95261 = CARTESIAN_POINT('Ctrl Pts',(32.1895979729969,258.003419474963,20.2890377823574)) ;
#95262 = CARTESIAN_POINT('Ctrl Pts',(32.1933219350999,257.992745598067,20.2788893171814)) ;
#95263 = CARTESIAN_POINT('Ctrl Pts',(32.1978571834542,257.980133965385,20.2605941621586)) ;
#95264 = CARTESIAN_POINT('Ctrl Pts',(32.1992720778467,257.976288165441,20.2530925159503)) ;
#95265 = CARTESIAN_POINT('Ctrl Pts',(32.2011977766946,257.971159193015,20.2374109489562)) ;
#95266 = CARTESIAN_POINT('Ctrl Pts',(32.2017254632468,257.969822655041,20.2294326270796)) ;
#95267 = CARTESIAN_POINT('Ctrl Pts',(32.2017235856673,257.969823530571,20.2213203435596)) ;
#95268 = CARTESIAN_POINT('Origin',(32.0431849345645,258.15408910959,20.2213203435596)) ;
#95269 = CARTESIAN_POINT('',(32.6189050513595,257.775288618279,20.2213203435596)) ;
#95270 = CARTESIAN_POINT('',(32.0009231083904,258.063458330887,20.2213203435596)) ;
#95271 = CARTESIAN_POINT('',(32.5264861881013,257.92872203387,20.3213203435596)) ;
#95272 = CARTESIAN_POINT('',(32.0431849345645,258.15408910959,20.3213203435596)) ;
#95273 = CARTESIAN_POINT('Origin',(32.5264861881013,257.92872203387,20.2213203435596)) ;
#95274 = CARTESIAN_POINT('Origin',(32.5262827782143,257.924672599648,20.2213203435596)) ;
#95275 = CARTESIAN_POINT('',(32.7094862928853,259.578557794143,20.2213203435596)) ;
#95276 = CARTESIAN_POINT('',(32.6261568553752,257.91965575689,20.2213203435596)) ;
#95277 = CARTESIAN_POINT('',(32.5972722714868,259.337914048676,20.3213203435596)) ;
#95278 = CARTESIAN_POINT('',(32.5262827782143,257.924672599648,20.3213203435596)) ;
#95279 = CARTESIAN_POINT('Origin',(32.5972722714868,259.337914048676,20.2213203435596)) ;
#95280 = CARTESIAN_POINT('Origin',(32.1602128107536,258.932119389861,20.2213203435596)) ;
#95281 = CARTESIAN_POINT('',(32.092171866909,259.005402607317,20.2213203435596)) ;
#95282 = CARTESIAN_POINT('',(32.1602128107536,258.932119389861,20.3213203435596)) ;
#95283 = CARTESIAN_POINT('Origin',(32.2017221802041,257.969824185949,20.0213203435596)) ;
#95284 = CARTESIAN_POINT('',(32.6189050513595,257.775288618279,20.1213203435596)) ;
#95285 = CARTESIAN_POINT('',(32.6189050513595,257.775288618279,20.0213203435596)) ;
#95286 = CARTESIAN_POINT('',(32.2017221802041,257.969824185949,20.1213203435596)) ;
#95287 = CARTESIAN_POINT('',(44.9570498632135,252.021917205086,20.1213203435596)) ;
#95288 = CARTESIAN_POINT('',(32.2017221802041,257.969824185949,20.0213203435596)) ;
#95289 = CARTESIAN_POINT('Origin',(32.6189050513595,257.775288618279,20.0213203435596)) ;
#95290 = CARTESIAN_POINT('',(32.7094862928853,259.578557794143,20.1213203435596)) ;
#95291 = CARTESIAN_POINT('',(32.7094862928853,259.578557794143,20.0213203435596)) ;
#95292 = CARTESIAN_POINT('',(32.2199750708941,249.833488252288,20.1213203435596)) ;
#95293 = CARTESIAN_POINT('Origin',(32.7094862928853,259.578557794143,20.0213203435596)) ;
#95294 = CARTESIAN_POINT('',(31.3863264609896,258.350049454246,20.1213203435596)) ;
#95295 = CARTESIAN_POINT('',(31.3863264609896,258.350049454246,20.0213203435596)) ;
#95296 = CARTESIAN_POINT('',(34.0499529567987,260.823134931594,20.1213203435596)) ;
#95297 = CARTESIAN_POINT('Origin',(31.3863264609896,258.350049454246,20.0213203435596)) ;
#95298 = CARTESIAN_POINT('',(31.839183613039,258.138878696195,20.1213203435596)) ;
#95299 = CARTESIAN_POINT('',(31.839183613039,258.138878696195,20.0213203435596)) ;
#95300 = CARTESIAN_POINT('',(44.5493520036063,252.212029839235,20.1213203435596)) ;
#95301 = CARTESIAN_POINT('Origin',(31.7767899168982,258.107052294689,20.3213203435596)) ;
#95302 = CARTESIAN_POINT('Ctrl Pts',(30.5502224056744,257.052603781754,20.2213203435596)) ;
#95303 = CARTESIAN_POINT('Ctrl Pts',(30.4504373470295,257.036098173567,20.2213203435596)) ;
#95304 = CARTESIAN_POINT('Ctrl Pts',(30.2507744072825,256.993547832196,20.2213203435598)) ;
#95305 = CARTESIAN_POINT('Ctrl Pts',(29.9535859505325,256.89665014184,20.2213203435598)) ;
#95306 = CARTESIAN_POINT('Ctrl Pts',(29.6697087711132,256.680511270254,20.2213203435599)) ;
#95307 = CARTESIAN_POINT('Ctrl Pts',(29.5798204552179,256.467740611946,20.22132034356)) ;
#95308 = CARTESIAN_POINT('Ctrl Pts',(29.5387593890436,256.371007899967,20.22132034356)) ;
#95309 = CARTESIAN_POINT('Ctrl Pts',(29.5339221017733,256.359561959438,20.22132034356)) ;
#95310 = CARTESIAN_POINT('Ctrl Pts',(29.5255243701777,256.339659474417,20.22132034356)) ;
#95311 = CARTESIAN_POINT('Ctrl Pts',(29.5088379386217,256.300040213624,20.22132034356)) ;
#95312 = CARTESIAN_POINT('Ctrl Pts',(29.4850272312111,256.243996783598,20.22132034356)) ;
#95313 = CARTESIAN_POINT('Ctrl Pts',(29.4607697687769,256.188324327745,20.22132034356)) ;
#95314 = CARTESIAN_POINT('Ctrl Pts',(29.4410231456084,256.143964729335,20.22132034356)) ;
#95315 = CARTESIAN_POINT('Ctrl Pts',(29.3511457605012,255.944690099184,20.22132034356)) ;
#95316 = CARTESIAN_POINT('Ctrl Pts',(29.2580498043477,255.761710546012,20.2213203435596)) ;
#95317 = CARTESIAN_POINT('Ctrl Pts',(29.1697396985386,255.584956164831,20.2213203435596)) ;
#95318 = CARTESIAN_POINT('Ctrl Pts',(30.5502224056744,257.052603781754,20.2512402735938)) ;
#95319 = CARTESIAN_POINT('Ctrl Pts',(30.4504290994671,257.036096809325,20.2512402735938)) ;
#95320 = CARTESIAN_POINT('Ctrl Pts',(30.250787991272,256.993571390254,20.251240273594)) ;
#95321 = CARTESIAN_POINT('Ctrl Pts',(29.953570539349,256.896684290815,20.251240273594)) ;
#95322 = CARTESIAN_POINT('Ctrl Pts',(29.6695953979979,256.680469695693,20.2512402735941)) ;
#95323 = CARTESIAN_POINT('Ctrl Pts',(29.5796974644403,256.467635740865,20.2512402735942)) ;
#95324 = CARTESIAN_POINT('Ctrl Pts',(29.5386402549432,256.370904573759,20.2512402735942)) ;
#95325 = CARTESIAN_POINT('Ctrl Pts',(29.5338026904391,256.359458201952,20.2512402735942)) ;
#95326 = CARTESIAN_POINT('Ctrl Pts',(29.5254052731515,256.339555807343,20.2512402735942)) ;
#95327 = CARTESIAN_POINT('Ctrl Pts',(29.5087194815055,256.299937206453,20.2512402735942)) ;
#95328 = CARTESIAN_POINT('Ctrl Pts',(29.4849117359914,256.243897323674,20.2512402735942)) ;
#95329 = CARTESIAN_POINT('Ctrl Pts',(29.4606563257843,256.188228104397,20.2512402735942)) ;
#95330 = CARTESIAN_POINT('Ctrl Pts',(29.4409117402036,256.143871399368,20.2512402735942)) ;
#95331 = CARTESIAN_POINT('Ctrl Pts',(29.3510404818838,255.944607280785,20.2512402735942)) ;
#95332 = CARTESIAN_POINT('Ctrl Pts',(29.2580505786398,255.761712095772,20.2512402735938)) ;
#95333 = CARTESIAN_POINT('Ctrl Pts',(29.1697396985386,255.584956164831,20.2512402735938)) ;
#95334 = CARTESIAN_POINT('Ctrl Pts',(30.5543238187055,257.027808588799,20.3030173033455)) ;
#95335 = CARTESIAN_POINT('Ctrl Pts',(30.4551892489819,257.011410579038,20.3030173033455)) ;
#95336 = CARTESIAN_POINT('Ctrl Pts',(30.2572087756548,256.969401492031,20.3030173033456)) ;
#95337 = CARTESIAN_POINT('Ctrl Pts',(29.9641223307203,256.873009951542,20.3030173033457)) ;
#95338 = CARTESIAN_POINT('Ctrl Pts',(29.6908334963393,256.664955954783,20.3030173033458)) ;
#95339 = CARTESIAN_POINT('Ctrl Pts',(29.6030899043467,256.458207136188,20.3030173033459)) ;
#95340 = CARTESIAN_POINT('Ctrl Pts',(29.562095221275,256.361626988556,20.3030173033459)) ;
#95341 = CARTESIAN_POINT('Ctrl Pts',(29.5572688117543,256.350206925962,20.3030173033459)) ;
#95342 = CARTESIAN_POINT('Ctrl Pts',(29.5488779342165,256.330320721087,20.3030173033459)) ;
#95343 = CARTESIAN_POINT('Ctrl Pts',(29.5321823528865,256.290679973573,20.3030173033459)) ;
#95344 = CARTESIAN_POINT('Ctrl Pts',(29.5083052653683,256.234480293537,20.3030173033459)) ;
#95345 = CARTESIAN_POINT('Ctrl Pts',(29.4839605385045,256.178607635609,20.3030173033459)) ;
#95346 = CARTESIAN_POINT('Ctrl Pts',(29.4641412177491,256.134084748371,20.3030173033459)) ;
#95347 = CARTESIAN_POINT('Ctrl Pts',(29.3739437406398,255.934101429851,20.3030173033459)) ;
#95348 = CARTESIAN_POINT('Ctrl Pts',(29.2804709943218,255.750355719183,20.3030173033455)) ;
#95349 = CARTESIAN_POINT('Ctrl Pts',(29.1922219572742,255.573723568307,20.3030173033455)) ;
#95350 = CARTESIAN_POINT('Ctrl Pts',(30.5628797492928,256.976083500832,20.3213203435596)) ;
#95351 = CARTESIAN_POINT('Ctrl Pts',(30.4650974797975,256.959909177243,20.3213203435596)) ;
#95352 = CARTESIAN_POINT('Ctrl Pts',(30.2706391777167,256.919043340531,20.3213203435598)) ;
#95353 = CARTESIAN_POINT('Ctrl Pts',(29.9860934580288,256.823713686167,20.3213203435598)) ;
#95354 = CARTESIAN_POINT('Ctrl Pts',(29.7348373077925,256.632482520968,20.3213203435599)) ;
#95355 = CARTESIAN_POINT('Ctrl Pts',(29.6515623522189,256.438259902233,20.32132034356)) ;
#95356 = CARTESIAN_POINT('Ctrl Pts',(29.6107083391225,256.341998894775,20.32132034356)) ;
#95357 = CARTESIAN_POINT('Ctrl Pts',(29.6059044642761,256.330632571226,20.32132034356)) ;
#95358 = CARTESIAN_POINT('Ctrl Pts',(29.5975280633095,256.310780379563,20.32132034356)) ;
#95359 = CARTESIAN_POINT('Ctrl Pts',(29.5808137578388,256.27109518323,20.32132034356)) ;
#95360 = CARTESIAN_POINT('Ctrl Pts',(29.5567998760631,256.214571564109,20.32132034356)) ;
#95361 = CARTESIAN_POINT('Ctrl Pts',(29.5322742720676,256.158283102678,20.32132034356)) ;
#95362 = CARTESIAN_POINT('Ctrl Pts',(29.5123044536673,256.113421221662,20.32132034356)) ;
#95363 = CARTESIAN_POINT('Ctrl Pts',(29.4214427116386,255.911965478229,20.32132034356)) ;
#95364 = CARTESIAN_POINT('Ctrl Pts',(29.3272441297798,255.726669369536,20.3213203435596)) ;
#95365 = CARTESIAN_POINT('Ctrl Pts',(29.2391220484686,255.550291323017,20.3213203435596)) ;
#95366 = CARTESIAN_POINT('Ctrl Pts',(30.566541816524,256.953944383674,20.3213203435596)) ;
#95367 = CARTESIAN_POINT('Ctrl Pts',(30.4693374736902,256.93786565587,20.3213203435596)) ;
#95368 = CARTESIAN_POINT('Ctrl Pts',(30.2763890386465,256.897491801285,20.3213203435598)) ;
#95369 = CARTESIAN_POINT('Ctrl Pts',(29.9954957906156,256.802617777926,20.3213203435598)) ;
#95370 = CARTESIAN_POINT('Ctrl Pts',(29.7536595300643,256.618578974978,20.3213203435599)) ;
#95371 = CARTESIAN_POINT('Ctrl Pts',(29.672296194115,256.429711018626,20.32132034356)) ;
#95372 = CARTESIAN_POINT('Ctrl Pts',(29.6315028005541,256.333586772474,20.32132034356)) ;
#95373 = CARTESIAN_POINT('Ctrl Pts',(29.6267085413676,256.322243404122,20.32132034356)) ;
#95374 = CARTESIAN_POINT('Ctrl Pts',(29.6183383700597,256.302405780253,20.32132034356)) ;
#95375 = CARTESIAN_POINT('Ctrl Pts',(29.6016161185133,256.262701629424,20.32132034356)) ;
#95376 = CARTESIAN_POINT('Ctrl Pts',(29.5775440021221,256.20603973721,20.32132034356)) ;
#95377 = CARTESIAN_POINT('Ctrl Pts',(29.5529411985134,256.14957365025,20.32132034356)) ;
#95378 = CARTESIAN_POINT('Ctrl Pts',(29.532907181819,256.104566982881,20.32132034356)) ;
#95379 = CARTESIAN_POINT('Ctrl Pts',(29.4417617767858,255.902482138686,20.32132034356)) ;
#95380 = CARTESIAN_POINT('Ctrl Pts',(29.3472638190854,255.71653141995,20.3213203435596)) ;
#95381 = CARTESIAN_POINT('Ctrl Pts',(29.2591959942947,255.540261968904,20.3213203435596)) ;
#95382 = CARTESIAN_POINT('',(30.4681271505274,256.936145439019,20.3213203435596)) ;
#95383 = CARTESIAN_POINT('',(29.2591959942946,255.540261968904,20.3213203435596)) ;
#95384 = CARTESIAN_POINT('Ctrl Pts',(30.4681271505274,256.936145439019,20.3213203435596)) ;
#95385 = CARTESIAN_POINT('Ctrl Pts',(30.404199598279,256.923546655539,20.3213203435597)) ;
#95386 = CARTESIAN_POINT('Ctrl Pts',(30.2447009077672,256.88678887236,20.3213203435598)) ;
#95387 = CARTESIAN_POINT('Ctrl Pts',(29.9954957906156,256.802617777926,20.3213203435598)) ;
#95388 = CARTESIAN_POINT('Ctrl Pts',(29.7536595300643,256.618578974978,20.3213203435599)) ;
#95389 = CARTESIAN_POINT('Ctrl Pts',(29.672296194115,256.429711018626,20.32132034356)) ;
#95390 = CARTESIAN_POINT('Ctrl Pts',(29.6315028005541,256.333586772474,20.32132034356)) ;
#95391 = CARTESIAN_POINT('Ctrl Pts',(29.6267085413676,256.322243404122,20.32132034356)) ;
#95392 = CARTESIAN_POINT('Ctrl Pts',(29.6183383700597,256.302405780253,20.32132034356)) ;
#95393 = CARTESIAN_POINT('Ctrl Pts',(29.6016161185133,256.262701629424,20.32132034356)) ;
#95394 = CARTESIAN_POINT('Ctrl Pts',(29.5775440021221,256.20603973721,20.32132034356)) ;
#95395 = CARTESIAN_POINT('Ctrl Pts',(29.5529411985134,256.14957365025,20.32132034356)) ;
#95396 = CARTESIAN_POINT('Ctrl Pts',(29.532907181819,256.104566982881,20.32132034356)) ;
#95397 = CARTESIAN_POINT('Ctrl Pts',(29.4417617767858,255.902482138686,20.32132034356)) ;
#95398 = CARTESIAN_POINT('Ctrl Pts',(29.3472638190854,255.71653141995,20.3213203435596)) ;
#95399 = CARTESIAN_POINT('Ctrl Pts',(29.2591959942947,255.540261968904,20.3213203435596)) ;
#95400 = CARTESIAN_POINT('',(29.213306918992,255.671998198108,20.2213203435596)) ;
#95401 = CARTESIAN_POINT('Ctrl Pts',(29.2591959942946,255.540261968904,20.3213203435596)) ;
#95402 = CARTESIAN_POINT('Ctrl Pts',(29.2590867165055,255.540585371864,20.3213203435596)) ;
#95403 = CARTESIAN_POINT('Ctrl Pts',(29.2589773726705,255.54090875402,20.3213194290187)) ;
#95404 = CARTESIAN_POINT('Ctrl Pts',(29.2536958381592,255.556518479706,20.321231181363)) ;
#95405 = CARTESIAN_POINT('Ctrl Pts',(29.2483227014057,255.57189823562,20.3191028849279)) ;
#95406 = CARTESIAN_POINT('Ctrl Pts',(29.2383131514629,255.600324941419,20.3110059033691)) ;
#95407 = CARTESIAN_POINT('Ctrl Pts',(29.2335189659059,255.613847174906,20.3051753495665)) ;
#95408 = CARTESIAN_POINT('Ctrl Pts',(29.2249637172964,255.638735334461,20.2889211055947)) ;
#95409 = CARTESIAN_POINT('Ctrl Pts',(29.2213832985399,255.649320365818,20.2787669436689)) ;
#95410 = CARTESIAN_POINT('Ctrl Pts',(29.2170223683631,255.661812395744,20.2604759078399)) ;
#95411 = CARTESIAN_POINT('Ctrl Pts',(29.215664386302,255.665610853218,20.2529927710902)) ;
#95412 = CARTESIAN_POINT('Ctrl Pts',(29.213813498395,255.670679065537,20.237359488709)) ;
#95413 = CARTESIAN_POINT('Ctrl Pts',(29.2133053651598,255.671998912603,20.2294043743899)) ;
#95414 = CARTESIAN_POINT('Ctrl Pts',(29.2133063229928,255.671998465958,20.2213203435596)) ;
#95415 = CARTESIAN_POINT('',(30.5502224056744,257.052603781754,20.2213203435596)) ;
#95416 = CARTESIAN_POINT('Ctrl Pts',(29.2133075051976,255.671997914687,20.2213203435597)) ;
#95417 = CARTESIAN_POINT('Ctrl Pts',(29.2307530417186,255.706837709317,20.2213203435597)) ;
#95418 = CARTESIAN_POINT('Ctrl Pts',(29.2480451874319,255.741544522718,20.2213203435597)) ;
#95419 = CARTESIAN_POINT('Ctrl Pts',(29.2651899065699,255.776196982818,20.2213203435597)) ;
#95420 = CARTESIAN_POINT('Ctrl Pts',(29.2836186893254,255.813444758883,20.2213203435598)) ;
#95421 = CARTESIAN_POINT('Ctrl Pts',(29.3018805490242,255.850634869259,20.2213203435598)) ;
#95422 = CARTESIAN_POINT('Ctrl Pts',(29.3199861498403,255.887894741683,20.2213203435598)) ;
#95423 = CARTESIAN_POINT('Ctrl Pts',(29.3342424835541,255.917233131545,20.2213203435599)) ;
#95424 = CARTESIAN_POINT('Ctrl Pts',(29.3484027162989,255.946616480248,20.2213203435599)) ;
#95425 = CARTESIAN_POINT('Ctrl Pts',(29.3624503738921,255.976083989101,20.2213203435599)) ;
#95426 = CARTESIAN_POINT('Ctrl Pts',(29.3744610562137,256.001278572988,20.2213203435599)) ;
#95427 = CARTESIAN_POINT('Ctrl Pts',(29.3863896118145,256.026535087145,20.22132034356)) ;
#95428 = CARTESIAN_POINT('Ctrl Pts',(29.3982031370694,256.051848366021,20.22132034356)) ;
#95429 = CARTESIAN_POINT('Ctrl Pts',(29.4073911676691,256.071535900087,20.22132034356)) ;
#95430 = CARTESIAN_POINT('Ctrl Pts',(29.4165093180901,256.091257405863,20.22132034356)) ;
#95431 = CARTESIAN_POINT('Ctrl Pts',(29.425529160593,256.110992495285,20.22132034356)) ;
#95432 = CARTESIAN_POINT('Ctrl Pts',(29.4305752194442,256.122033089689,20.22132034356)) ;
#95433 = CARTESIAN_POINT('Ctrl Pts',(29.4355961225057,256.13309037525,20.22132034356)) ;
#95434 = CARTESIAN_POINT('Ctrl Pts',(29.4405850973892,256.144158974749,20.22132034356)) ;
#95435 = CARTESIAN_POINT('Ctrl Pts',(29.4455894877222,256.155261775149,20.22132034356)) ;
#95436 = CARTESIAN_POINT('Ctrl Pts',(29.4505617588215,256.166375877005,20.22132034356)) ;
#95437 = CARTESIAN_POINT('Ctrl Pts',(29.4554995354655,256.177507784875,20.22132034356)) ;
#95438 = CARTESIAN_POINT('Ctrl Pts',(29.4589254454287,256.1852312841,20.22132034356)) ;
#95439 = CARTESIAN_POINT('Ctrl Pts',(29.4623367397909,256.192967969647,20.22132034356)) ;
#95440 = CARTESIAN_POINT('Ctrl Pts',(29.4657236710055,256.200700387666,20.22132034356)) ;
#95441 = CARTESIAN_POINT('Ctrl Pts',(29.4710997144517,256.212973980657,20.22132034356)) ;
#95442 = CARTESIAN_POINT('Ctrl Pts',(29.476410769658,256.22531618242,20.22132034356)) ;
#95443 = CARTESIAN_POINT('Ctrl Pts',(29.4816615232414,256.237682350978,20.22132034356)) ;
#95444 = CARTESIAN_POINT('Ctrl Pts',(29.4863645891097,256.248758647807,20.22132034356)) ;
#95445 = CARTESIAN_POINT('Ctrl Pts',(29.491019360315,256.259853814514,20.22132034356)) ;
#95446 = CARTESIAN_POINT('Ctrl Pts',(29.4956515405211,256.270981218767,20.22132034356)) ;
#95447 = CARTESIAN_POINT('Ctrl Pts',(29.5035602780298,256.289979555507,20.22132034356)) ;
#95448 = CARTESIAN_POINT('Ctrl Pts',(29.511399561512,256.309067225097,20.22132034356)) ;
#95449 = CARTESIAN_POINT('Ctrl Pts',(29.5192933563511,256.32825717138,20.22132034356)) ;
#95450 = CARTESIAN_POINT('Ctrl Pts',(29.5225268702631,256.336117897373,20.22132034356)) ;
#95451 = CARTESIAN_POINT('Ctrl Pts',(29.5257686806131,256.343992960907,20.22132034356)) ;
#95452 = CARTESIAN_POINT('Ctrl Pts',(29.529030465216,256.351887406121,20.22132034356)) ;
#95453 = CARTESIAN_POINT('Ctrl Pts',(29.5307511106271,256.356051856747,20.22132034356)) ;
#95454 = CARTESIAN_POINT('Ctrl Pts',(29.5324781961111,256.360223805101,20.22132034356)) ;
#95455 = CARTESIAN_POINT('Ctrl Pts',(29.5342149642331,256.36440733422,20.22132034356)) ;
#95456 = CARTESIAN_POINT('Ctrl Pts',(29.535495630112,256.367492203713,20.22132034356)) ;
#95457 = CARTESIAN_POINT('Ctrl Pts',(29.5367799677669,256.370579502307,20.22132034356)) ;
#95458 = CARTESIAN_POINT('Ctrl Pts',(29.5380635719759,256.373657193282,20.22132034356)) ;
#95459 = CARTESIAN_POINT('Ctrl Pts',(29.5394513950042,256.376984769164,20.22132034356)) ;
#95460 = CARTESIAN_POINT('Ctrl Pts',(29.5408419684465,256.380309842844,20.22132034356)) ;
#95461 = CARTESIAN_POINT('Ctrl Pts',(29.5422463762053,256.383656789344,20.22132034356)) ;
#95462 = CARTESIAN_POINT('Ctrl Pts',(29.5500527870912,256.402260816147,20.22132034356)) ;
#95463 = CARTESIAN_POINT('Ctrl Pts',(29.5582185870785,256.421386647834,20.22132034356)) ;
#95464 = CARTESIAN_POINT('Ctrl Pts',(29.5668254892807,256.440765383713,20.22132034356)) ;
#95465 = CARTESIAN_POINT('Ctrl Pts',(29.5764165175254,256.462359913173,20.22132034356)) ;
#95466 = CARTESIAN_POINT('Ctrl Pts',(29.5865567090972,256.48426749885,20.22132034356)) ;
#95467 = CARTESIAN_POINT('Ctrl Pts',(29.597423005008,256.506146707171,20.22132034356)) ;
#95468 = CARTESIAN_POINT('Ctrl Pts',(29.6089408564768,256.529337817902,20.22132034356)) ;
#95469 = CARTESIAN_POINT('Ctrl Pts',(29.6212791896667,256.55249607905,20.22132034356)) ;
#95470 = CARTESIAN_POINT('Ctrl Pts',(29.6346677671494,256.575263247164,20.2213203435599)) ;
#95471 = CARTESIAN_POINT('Ctrl Pts',(29.6447092002614,256.592338623249,20.2213203435599)) ;
#95472 = CARTESIAN_POINT('Ctrl Pts',(29.6553424455427,256.609195022114,20.2213203435599)) ;
#95473 = CARTESIAN_POINT('Ctrl Pts',(29.6666432561968,256.625702023723,20.2213203435599)) ;
#95474 = CARTESIAN_POINT('Ctrl Pts',(29.6730261077246,256.635025402698,20.2213203435599)) ;
#95475 = CARTESIAN_POINT('Ctrl Pts',(29.6796214358638,256.644237651328,20.2213203435599)) ;
#95476 = CARTESIAN_POINT('Ctrl Pts',(29.6864374605946,256.653317913181,20.2213203435599)) ;
#95477 = CARTESIAN_POINT('Ctrl Pts',(29.6920155866947,256.660749054885,20.2213203435599)) ;
#95478 = CARTESIAN_POINT('Ctrl Pts',(29.6977426583487,256.668093123778,20.2213203435599)) ;
#95479 = CARTESIAN_POINT('Ctrl Pts',(29.7036113206688,256.675328820148,20.2213203435599)) ;
#95480 = CARTESIAN_POINT('Ctrl Pts',(29.7192328828822,256.694589236719,20.2213203435599)) ;
#95481 = CARTESIAN_POINT('Ctrl Pts',(29.7358819982484,256.713110580123,20.2213203435599)) ;
#95482 = CARTESIAN_POINT('Ctrl Pts',(29.7536800879331,256.730900674017,20.2213203435599)) ;
#95483 = CARTESIAN_POINT('Ctrl Pts',(29.7644212276756,256.741636988304,20.2213203435599)) ;
#95484 = CARTESIAN_POINT('Ctrl Pts',(29.7755798595812,256.752107073421,20.2213203435599)) ;
#95485 = CARTESIAN_POINT('Ctrl Pts',(29.7871734949583,256.762313540024,20.2213203435599)) ;
#95486 = CARTESIAN_POINT('Ctrl Pts',(29.8155501675463,256.787294967475,20.2213203435599)) ;
#95487 = CARTESIAN_POINT('Ctrl Pts',(29.8451075130733,256.809701403991,20.2213203435598)) ;
#95488 = CARTESIAN_POINT('Ctrl Pts',(29.8755296737893,256.829949043671,20.2213203435598)) ;
#95489 = CARTESIAN_POINT('Ctrl Pts',(29.8888393691026,256.838807386031,20.2213203435598)) ;
#95490 = CARTESIAN_POINT('Ctrl Pts',(29.9023141156151,256.847252072064,20.2213203435598)) ;
#95491 = CARTESIAN_POINT('Ctrl Pts',(29.9159253289018,256.855315666829,20.2213203435598)) ;
#95492 = CARTESIAN_POINT('Ctrl Pts',(29.9277267736438,256.862307113222,20.2213203435598)) ;
#95493 = CARTESIAN_POINT('Ctrl Pts',(29.939630786004,256.869012052383,20.2213203435598)) ;
#95494 = CARTESIAN_POINT('Ctrl Pts',(29.9516180101726,256.875450759323,20.2213203435598)) ;
#95495 = CARTESIAN_POINT('Ctrl Pts',(29.9566614722954,256.878159758013,20.2213203435598)) ;
#95496 = CARTESIAN_POINT('Ctrl Pts',(29.9617179154655,256.880820619487,20.2213203435598)) ;
#95497 = CARTESIAN_POINT('Ctrl Pts',(29.9667766228262,256.883430336315,20.2213203435598)) ;
#95498 = CARTESIAN_POINT('Ctrl Pts',(29.9906424899446,256.895742405505,20.2213203435598)) ;
#95499 = CARTESIAN_POINT('Ctrl Pts',(30.0146186463981,256.906953970521,20.2213203435598)) ;
#95500 = CARTESIAN_POINT('Ctrl Pts',(30.0386586200925,256.917289953597,20.2213203435598)) ;
#95501 = CARTESIAN_POINT('Ctrl Pts',(30.0634818792387,256.927962710135,20.2213203435598)) ;
#95502 = CARTESIAN_POINT('Ctrl Pts',(30.0883731914004,256.937701390127,20.2213203435598)) ;
#95503 = CARTESIAN_POINT('Ctrl Pts',(30.1133144111727,256.946703407878,20.2213203435598)) ;
#95504 = CARTESIAN_POINT('Ctrl Pts',(30.1392690558496,256.9560712004,20.2213203435598)) ;
#95505 = CARTESIAN_POINT('Ctrl Pts',(30.165277713297,256.96464080163,20.2213203435598)) ;
#95506 = CARTESIAN_POINT('Ctrl Pts',(30.1913553599989,256.97258858843,20.2213203435598)) ;
#95507 = CARTESIAN_POINT('Ctrl Pts',(30.2107444937283,256.978497890863,20.2213203435598)) ;
#95508 = CARTESIAN_POINT('Ctrl Pts',(30.2301725212875,256.984062442463,20.2213203435598)) ;
#95509 = CARTESIAN_POINT('Ctrl Pts',(30.249657583769,256.989341417562,20.2213203435597)) ;
#95510 = CARTESIAN_POINT('Ctrl Pts',(30.262842937433,256.992913649046,20.2213203435597)) ;
#95511 = CARTESIAN_POINT('Ctrl Pts',(30.2760454316719,256.996352315282,20.2213203435597)) ;
#95512 = CARTESIAN_POINT('Ctrl Pts',(30.2892583034633,256.999670387357,20.2213203435597)) ;
#95513 = CARTESIAN_POINT('Ctrl Pts',(30.322651117236,257.008056131547,20.2213203435597)) ;
#95514 = CARTESIAN_POINT('Ctrl Pts',(30.3561115692332,257.015675648504,20.2213203435597)) ;
#95515 = CARTESIAN_POINT('Ctrl Pts',(30.3895792904966,257.02271246259,20.2213203435597)) ;
#95516 = CARTESIAN_POINT('Ctrl Pts',(30.4248514059428,257.030128662721,20.2213203435596)) ;
#95517 = CARTESIAN_POINT('Ctrl Pts',(30.460131466338,257.036897256708,20.2213203435596)) ;
#95518 = CARTESIAN_POINT('Ctrl Pts',(30.4953842467288,257.043186416176,20.2213203435596)) ;
#95519 = CARTESIAN_POINT('Ctrl Pts',(30.5136708291516,257.046448775392,20.2213203435596)) ;
#95520 = CARTESIAN_POINT('Ctrl Pts',(30.5319506504597,257.049581421127,20.2213203435596)) ;
#95521 = CARTESIAN_POINT('Ctrl Pts',(30.5502224056744,257.052603781754,20.2213203435596)) ;
#95522 = CARTESIAN_POINT('Ctrl Pts',(30.4681271505273,256.936145439019,20.3213203435596)) ;
#95523 = CARTESIAN_POINT('Ctrl Pts',(30.4683299268523,256.936432008588,20.3213203435596)) ;
#95524 = CARTESIAN_POINT('Ctrl Pts',(30.4685326646057,256.936718607507,20.3213194297254)) ;
#95525 = CARTESIAN_POINT('Ctrl Pts',(30.4782179507238,256.950414093123,20.3212321344664)) ;
#95526 = CARTESIAN_POINT('Ctrl Pts',(30.4877061821935,256.964022936168,20.3191476657588)) ;
#95527 = CARTESIAN_POINT('Ctrl Pts',(30.5052277006315,256.989161753491,20.3111707686004)) ;
#95528 = CARTESIAN_POINT('Ctrl Pts',(30.5135659702218,257.001123783895,20.3054349322803)) ;
#95529 = CARTESIAN_POINT('Ctrl Pts',(30.5291730023403,257.022992686367,20.2893352101867)) ;
#95530 = CARTESIAN_POINT('Ctrl Pts',(30.5358844390855,257.032244721745,20.2792373192504)) ;
#95531 = CARTESIAN_POINT('Ctrl Pts',(30.5437948938036,257.043343479936,20.2609382270818)) ;
#95532 = CARTESIAN_POINT('Ctrl Pts',(30.5462083785189,257.04677470554,20.253378482991)) ;
#95533 = CARTESIAN_POINT('Ctrl Pts',(30.5494038052607,257.051380924324,20.2375590756384)) ;
#95534 = CARTESIAN_POINT('Ctrl Pts',(30.5502224056744,257.052603781754,20.2295089201093)) ;
#95535 = CARTESIAN_POINT('Ctrl Pts',(30.5502224056744,257.052603781754,20.2213203435596)) ;
#95536 = CARTESIAN_POINT('Origin',(29.3774646884419,255.485112371103,20.2213203435596)) ;
#95537 = CARTESIAN_POINT('',(28.8895617876714,255.712625230168,20.3213203435596)) ;
#95538 = CARTESIAN_POINT('',(29.3774646884419,255.485112371103,20.3213203435596)) ;
#95539 = CARTESIAN_POINT('',(28.7971429244132,255.86605864576,20.2213203435596)) ;
#95540 = CARTESIAN_POINT('Origin',(28.8895617876714,255.712625230168,20.2213203435596)) ;
#95541 = CARTESIAN_POINT('',(29.419726514616,255.575743149807,20.2213203435596)) ;
#95542 = CARTESIAN_POINT('Origin',(28.890502822535,255.731359121804,20.2213203435596)) ;
#95543 = CARTESIAN_POINT('',(28.8187757042858,254.303433215363,20.3213203435596)) ;
#95544 = CARTESIAN_POINT('',(28.890502822535,255.731359121804,20.3213203435596)) ;
#95545 = CARTESIAN_POINT('',(28.7065616828874,254.062789469896,20.2213203435596)) ;
#95546 = CARTESIAN_POINT('Origin',(28.8187757042858,254.303433215363,20.2213203435596)) ;
#95547 = CARTESIAN_POINT('',(28.7906287453741,255.736375964562,20.2213203435596)) ;
#95548 = CARTESIAN_POINT('Origin',(29.2697227541073,254.722122022416,20.2213203435596)) ;
#95549 = CARTESIAN_POINT('',(30.029721514783,255.291297809793,20.2213203435596)) ;
#95550 = CARTESIAN_POINT('',(29.3377636979518,254.64883880496,20.2213203435596)) ;
#95551 = CARTESIAN_POINT('',(29.8527789991768,255.263469667977,20.3213203435596)) ;
#95552 = CARTESIAN_POINT('',(29.2697227541073,254.722122022416,20.3213203435596)) ;
#95553 = CARTESIAN_POINT('Origin',(29.8527789991768,255.263469667977,20.2213203435596)) ;
#95554 = CARTESIAN_POINT('Origin',(29.7856716932347,255.294762318656,20.2213203435596)) ;
#95555 = CARTESIAN_POINT('',(29.5759716504483,255.502885786844,20.2213203435596)) ;
#95556 = CARTESIAN_POINT('',(29.8279335194087,255.385393097359,20.2213203435596)) ;
#95557 = CARTESIAN_POINT('',(29.4405240550635,255.455707305529,20.3213203435596)) ;
#95558 = CARTESIAN_POINT('',(29.7856716932347,255.294762318656,20.3213203435596)) ;
#95559 = CARTESIAN_POINT('Ctrl Pts',(29.4405240550636,255.455707305529,20.3213203435596)) ;
#95560 = CARTESIAN_POINT('Ctrl Pts',(29.4408538386378,255.455825702211,20.3213203435596)) ;
#95561 = CARTESIAN_POINT('Ctrl Pts',(29.4411836478927,255.455944032111,20.3213194308211)) ;
#95562 = CARTESIAN_POINT('Ctrl Pts',(29.4569924888621,255.461612375186,20.3212319872543)) ;
#95563 = CARTESIAN_POINT('Ctrl Pts',(29.4726867912404,255.46706644739,20.3191381135824)) ;
#95564 = CARTESIAN_POINT('Ctrl Pts',(29.5017651669459,255.477084800126,20.3111718218544)) ;
#95565 = CARTESIAN_POINT('Ctrl Pts',(29.51565798919,255.48183265499,20.3054342440869)) ;
#95566 = CARTESIAN_POINT('Ctrl Pts',(29.5412810399391,255.490845015337,20.2893159232801)) ;
#95567 = CARTESIAN_POINT('Ctrl Pts',(29.5521970843937,255.494745565626,20.2791809771031)) ;
#95568 = CARTESIAN_POINT('Ctrl Pts',(29.5652171491802,255.499264264589,20.260871828191)) ;
#95569 = CARTESIAN_POINT('Ctrl Pts',(29.5692328543724,255.500626571788,20.2533267661999)) ;
#95570 = CARTESIAN_POINT('Ctrl Pts',(29.574609399851,255.502411678272,20.2375324969203)) ;
#95571 = CARTESIAN_POINT('Ctrl Pts',(29.5760300223821,255.502857627139,20.2294989756937)) ;
#95572 = CARTESIAN_POINT('Ctrl Pts',(29.5760287878866,255.502858202794,20.2213203435596)) ;
#95573 = CARTESIAN_POINT('Ctrl Pts',(29.5299739324064,255.41100026533,20.2213203435596)) ;
#95574 = CARTESIAN_POINT('Ctrl Pts',(29.6096016195701,255.57031939758,20.2213203435596)) ;
#95575 = CARTESIAN_POINT('Ctrl Pts',(29.7125884839771,255.771554438639,20.2213203435596)) ;
#95576 = CARTESIAN_POINT('Ctrl Pts',(29.8151211010034,255.998133968456,20.2213203435596)) ;
#95577 = CARTESIAN_POINT('Ctrl Pts',(29.8513771953728,256.081187321587,20.2213203435596)) ;
#95578 = CARTESIAN_POINT('Ctrl Pts',(29.8781139616688,256.143488201183,20.2213203435596)) ;
#95579 = CARTESIAN_POINT('Ctrl Pts',(29.8995554831711,256.195063929691,20.2213203435596)) ;
#95580 = CARTESIAN_POINT('Ctrl Pts',(29.9348455746236,256.276402827328,20.2213203435596)) ;
#95581 = CARTESIAN_POINT('Ctrl Pts',(29.9896815685447,256.4130504425,20.2213203435596)) ;
#95582 = CARTESIAN_POINT('Ctrl Pts',(30.1179835005034,256.525685163548,20.2213203435596)) ;
#95583 = CARTESIAN_POINT('Ctrl Pts',(30.3645779003689,256.610912055866,20.2213203435596)) ;
#95584 = CARTESIAN_POINT('Ctrl Pts',(30.5298821415626,256.643803992665,20.2213203435596)) ;
#95585 = CARTESIAN_POINT('Ctrl Pts',(30.6155000490728,256.657966189434,20.2213203435596)) ;
#95586 = CARTESIAN_POINT('Ctrl Pts',(29.5299739324064,255.41100026533,20.2512402735938)) ;
#95587 = CARTESIAN_POINT('Ctrl Pts',(29.6096009693679,255.570318096655,20.2512402735938)) ;
#95588 = CARTESIAN_POINT('Ctrl Pts',(29.712707938933,255.771649641491,20.2512402735938)) ;
#95589 = CARTESIAN_POINT('Ctrl Pts',(29.8152362132554,255.998232225974,20.2512402735938)) ;
#95590 = CARTESIAN_POINT('Ctrl Pts',(29.8515002767356,256.081293849312,20.2512402735938)) ;
#95591 = CARTESIAN_POINT('Ctrl Pts',(29.8782395213483,256.143598800648,20.2512402735938)) ;
#95592 = CARTESIAN_POINT('Ctrl Pts',(29.8996858196018,256.195177190556,20.2512402735938)) ;
#95593 = CARTESIAN_POINT('Ctrl Pts',(29.934976344848,256.276518880556,20.2512402735938)) ;
#95594 = CARTESIAN_POINT('Ctrl Pts',(29.9898180967585,256.413130044856,20.2512402735938)) ;
#95595 = CARTESIAN_POINT('Ctrl Pts',(30.1179763379782,256.525623320505,20.2512402735938)) ;
#95596 = CARTESIAN_POINT('Ctrl Pts',(30.3645571335651,256.610892638431,20.2512402735938)) ;
#95597 = CARTESIAN_POINT('Ctrl Pts',(30.5298900347182,256.643805298284,20.2512402735938)) ;
#95598 = CARTESIAN_POINT('Ctrl Pts',(30.6155000490728,256.657966189434,20.2512402735938)) ;
#95599 = CARTESIAN_POINT('Ctrl Pts',(29.5074932885477,255.422236088995,20.3030173057519)) ;
#95600 = CARTESIAN_POINT('Ctrl Pts',(29.5871722574481,255.58165782578,20.3030173057519)) ;
#95601 = CARTESIAN_POINT('Ctrl Pts',(29.6898117905486,255.782015377311,20.3030173057519)) ;
#95602 = CARTESIAN_POINT('Ctrl Pts',(29.7920157725665,256.007858969755,20.3030173057519)) ;
#95603 = CARTESIAN_POINT('Ctrl Pts',(29.8281359664057,256.090623692282,20.3030173057519)) ;
#95604 = CARTESIAN_POINT('Ctrl Pts',(29.8548106554516,256.152702041668,20.3030173057519)) ;
#95605 = CARTESIAN_POINT('Ctrl Pts',(29.8762058240841,256.204312000057,20.3030173057519)) ;
#95606 = CARTESIAN_POINT('Ctrl Pts',(29.9116403677314,256.285562615183,20.3030173057519)) ;
#95607 = CARTESIAN_POINT('Ctrl Pts',(29.9666803048971,256.425572767907,20.3030173057519)) ;
#95608 = CARTESIAN_POINT('Ctrl Pts',(30.1078757132933,256.55051479079,20.3030173057519)) ;
#95609 = CARTESIAN_POINT('Ctrl Pts',(30.357955853848,256.634175797297,20.3030173057519)) ;
#95610 = CARTESIAN_POINT('Ctrl Pts',(30.5251581921543,256.668496208837,20.3030173057519)) ;
#95611 = CARTESIAN_POINT('Ctrl Pts',(30.611398636369,256.682761380411,20.3030173057519)) ;
#95612 = CARTESIAN_POINT('Ctrl Pts',(29.4605965606009,255.445675069168,20.3213203435596)) ;
#95613 = CARTESIAN_POINT('Ctrl Pts',(29.5403821390099,255.605310110332,20.3213203435596)) ;
#95614 = CARTESIAN_POINT('Ctrl Pts',(29.6423652672512,255.803891903317,20.3213203435596)) ;
#95615 = CARTESIAN_POINT('Ctrl Pts',(29.7438812213478,256.028201995047,20.3213203435596)) ;
#95616 = CARTESIAN_POINT('Ctrl Pts',(29.7797224364993,256.110369300527,20.3213203435596)) ;
#95617 = CARTESIAN_POINT('Ctrl Pts',(29.8062690330564,256.171985741807,20.3213203435596)) ;
#95618 = CARTESIAN_POINT('Ctrl Pts',(29.8275702161123,256.223668617304,20.3213203435596)) ;
#95619 = CARTESIAN_POINT('Ctrl Pts',(29.8633063467445,256.304736651538,20.3213203435596)) ;
#95620 = CARTESIAN_POINT('Ctrl Pts',(29.9187749963249,256.451740686228,20.3213203435596)) ;
#95621 = CARTESIAN_POINT('Ctrl Pts',(30.0867858579854,256.602276621519,20.3213203435596)) ;
#95622 = CARTESIAN_POINT('Ctrl Pts',(30.3441298594353,256.682695120528,20.3213203435596)) ;
#95623 = CARTESIAN_POINT('Ctrl Pts',(30.5153080708237,256.720007224649,20.3213203435596)) ;
#95624 = CARTESIAN_POINT('Ctrl Pts',(30.6028427054544,256.734486470356,20.3213203435596)) ;
#95625 = CARTESIAN_POINT('Ctrl Pts',(29.4405240550634,255.455707305529,20.3213203435596)) ;
#95626 = CARTESIAN_POINT('Ctrl Pts',(29.5203551947139,255.615433505657,20.3213203435596)) ;
#95627 = CARTESIAN_POINT('Ctrl Pts',(29.6220701604893,255.813265522892,20.3213203435596)) ;
#95628 = CARTESIAN_POINT('Ctrl Pts',(29.7232911658707,256.03691957849,20.3213203435596)) ;
#95629 = CARTESIAN_POINT('Ctrl Pts',(29.7590138224883,256.118832061085,20.3213203435596)) ;
#95630 = CARTESIAN_POINT('Ctrl Pts',(29.785505857421,256.180251232298,20.3213203435596)) ;
#95631 = CARTESIAN_POINT('Ctrl Pts',(29.8067673218597,256.231965600798,20.3213203435596)) ;
#95632 = CARTESIAN_POINT('Ctrl Pts',(29.8426325824515,256.31295578499,20.3213203435596)) ;
#95633 = CARTESIAN_POINT('Ctrl Pts',(29.8982853405048,256.462949425189,20.3213203435596)) ;
#95634 = CARTESIAN_POINT('Ctrl Pts',(30.0777583197704,256.624424879292,20.3213203435596)) ;
#95635 = CARTESIAN_POINT('Ctrl Pts',(30.3382099144606,256.703460053722,20.3213203435596)) ;
#95636 = CARTESIAN_POINT('Ctrl Pts',(30.5110929110685,256.742054853877,20.3213203435596)) ;
#95637 = CARTESIAN_POINT('Ctrl Pts',(30.5991806382232,256.756625587514,20.3213203435596)) ;
#95638 = CARTESIAN_POINT('',(30.6155000490728,256.657966189434,20.2213203435596)) ;
#95639 = CARTESIAN_POINT('Ctrl Pts',(30.6155000490728,256.657966189434,20.2213203435596)) ;
#95640 = CARTESIAN_POINT('Ctrl Pts',(30.5934162583261,256.654313273834,20.2213203435596)) ;
#95641 = CARTESIAN_POINT('Ctrl Pts',(30.5716039157812,256.650478363725,20.2213203435596)) ;
#95642 = CARTESIAN_POINT('Ctrl Pts',(30.5499306316617,256.646421331829,20.2213203435596)) ;
#95643 = CARTESIAN_POINT('Ctrl Pts',(30.5289501530439,256.642493986509,20.2213203435596)) ;
#95644 = CARTESIAN_POINT('Ctrl Pts',(30.5080997796798,256.638358378979,20.2213203435596)) ;
#95645 = CARTESIAN_POINT('Ctrl Pts',(30.4873064930217,256.633971075942,20.2213203435596)) ;
#95646 = CARTESIAN_POINT('Ctrl Pts',(30.4672536265848,256.629739998706,20.2213203435596)) ;
#95647 = CARTESIAN_POINT('Ctrl Pts',(30.4472536147319,256.625274726044,20.2213203435596)) ;
#95648 = CARTESIAN_POINT('Ctrl Pts',(30.4272886443642,256.620531223793,20.2213203435596)) ;
#95649 = CARTESIAN_POINT('Ctrl Pts',(30.4142897652556,256.617442803866,20.2213203435596)) ;
#95650 = CARTESIAN_POINT('Ctrl Pts',(30.4013066983077,256.614236338128,20.2213203435596)) ;
#95651 = CARTESIAN_POINT('Ctrl Pts',(30.388346948028,256.6108987856,20.2213203435596)) ;
#95652 = CARTESIAN_POINT('Ctrl Pts',(30.3819900047351,256.609261668241,20.2213203435596)) ;
#95653 = CARTESIAN_POINT('Ctrl Pts',(30.3756388304382,256.607593001585,20.2213203435596)) ;
#95654 = CARTESIAN_POINT('Ctrl Pts',(30.3692952787652,256.605891200963,20.2213203435596)) ;
#95655 = CARTESIAN_POINT('Ctrl Pts',(30.3643550423544,256.604565871268,20.2213203435596)) ;
#95656 = CARTESIAN_POINT('Ctrl Pts',(30.3594204422208,256.603220681278,20.2213203435596)) ;
#95657 = CARTESIAN_POINT('Ctrl Pts',(30.3545032359515,256.601857933052,20.2213203435596)) ;
#95658 = CARTESIAN_POINT('Ctrl Pts',(30.3380407124697,256.597295530452,20.2213203435596)) ;
#95659 = CARTESIAN_POINT('Ctrl Pts',(30.3217321675932,256.592526619223,20.2213203435596)) ;
#95660 = CARTESIAN_POINT('Ctrl Pts',(30.3055753847063,256.587509301036,20.2213203435596)) ;
#95661 = CARTESIAN_POINT('Ctrl Pts',(30.2899301860841,256.582650849936,20.2213203435596)) ;
#95662 = CARTESIAN_POINT('Ctrl Pts',(30.2744270028255,256.577559375667,20.2213203435596)) ;
#95663 = CARTESIAN_POINT('Ctrl Pts',(30.259111696462,256.572195013264,20.2213203435596)) ;
#95664 = CARTESIAN_POINT('Ctrl Pts',(30.2445222032144,256.567084875263,20.2213203435596)) ;
#95665 = CARTESIAN_POINT('Ctrl Pts',(30.2301030378545,256.561727000506,20.2213203435596)) ;
#95666 = CARTESIAN_POINT('Ctrl Pts',(30.2159410139053,256.556086667428,20.2213203435596)) ;
#95667 = CARTESIAN_POINT('Ctrl Pts',(30.2097149645829,256.553607008302,20.2213203435596)) ;
#95668 = CARTESIAN_POINT('Ctrl Pts',(30.203539260331,256.551072762465,20.2213203435596)) ;
#95669 = CARTESIAN_POINT('Ctrl Pts',(30.1974245258637,256.548481045224,20.2213203435596)) ;
#95670 = CARTESIAN_POINT('Ctrl Pts',(30.1828338390648,256.542296813556,20.2213203435596)) ;
#95671 = CARTESIAN_POINT('Ctrl Pts',(30.1687288435062,256.536122143351,20.2213203435596)) ;
#95672 = CARTESIAN_POINT('Ctrl Pts',(30.1551584931796,256.529847245861,20.2213203435596)) ;
#95673 = CARTESIAN_POINT('Ctrl Pts',(30.1514273273943,256.528121963738,20.2213203435596)) ;
#95674 = CARTESIAN_POINT('Ctrl Pts',(30.1477365791022,256.526388810279,20.2213203435596)) ;
#95675 = CARTESIAN_POINT('Ctrl Pts',(30.1440871984713,256.524644752035,20.2213203435596)) ;
#95676 = CARTESIAN_POINT('Ctrl Pts',(30.1411815402234,256.523256122639,20.2213203435596)) ;
#95677 = CARTESIAN_POINT('Ctrl Pts',(30.138302106203,256.521860573952,20.2213203435596)) ;
#95678 = CARTESIAN_POINT('Ctrl Pts',(30.135449332951,256.520456391843,20.2213203435596)) ;
#95679 = CARTESIAN_POINT('Ctrl Pts',(30.1335861372718,256.519539296158,20.2213203435596)) ;
#95680 = CARTESIAN_POINT('Ctrl Pts',(30.1317325967933,256.518617702671,20.2213203435596)) ;
#95681 = CARTESIAN_POINT('Ctrl Pts',(30.1298799116381,256.517686461576,20.2213203435596)) ;
#95682 = CARTESIAN_POINT('Ctrl Pts',(30.1218807340664,256.513665722888,20.2213203435596)) ;
#95683 = CARTESIAN_POINT('Ctrl Pts',(30.1139562040359,256.509493804869,20.2213203435596)) ;
#95684 = CARTESIAN_POINT('Ctrl Pts',(30.1062297261487,256.505164397409,20.2213203435596)) ;
#95685 = CARTESIAN_POINT('Ctrl Pts',(30.0983390998272,256.500743012018,20.2213203435596)) ;
#95686 = CARTESIAN_POINT('Ctrl Pts',(30.0906551333939,256.496157031995,20.2213203435596)) ;
#95687 = CARTESIAN_POINT('Ctrl Pts',(30.0832576762508,256.491379023066,20.2213203435596)) ;
#95688 = CARTESIAN_POINT('Ctrl Pts',(30.0755133796667,256.486376990948,20.2213203435596)) ;
#95689 = CARTESIAN_POINT('Ctrl Pts',(30.0680830047494,256.481163853088,20.2213203435596)) ;
#95690 = CARTESIAN_POINT('Ctrl Pts',(30.0610015763669,256.475693171023,20.2213203435596)) ;
#95691 = CARTESIAN_POINT('Ctrl Pts',(30.0534085353477,256.469827248065,20.2213203435596)) ;
#95692 = CARTESIAN_POINT('Ctrl Pts',(30.0462162092421,256.463663963291,20.2213203435596)) ;
#95693 = CARTESIAN_POINT('Ctrl Pts',(30.0394079239686,256.457144203383,20.2213203435596)) ;
#95694 = CARTESIAN_POINT('Ctrl Pts',(30.0323252760618,256.450361707937,20.2213203435596)) ;
#95695 = CARTESIAN_POINT('Ctrl Pts',(30.0256567171885,256.443191537756,20.2213203435596)) ;
#95696 = CARTESIAN_POINT('Ctrl Pts',(30.0193370543812,256.435590226317,20.2213203435596)) ;
#95697 = CARTESIAN_POINT('Ctrl Pts',(30.0134514152341,256.42851095998,20.2213203435596)) ;
#95698 = CARTESIAN_POINT('Ctrl Pts',(30.0078666198455,256.421056878535,20.2213203435596)) ;
#95699 = CARTESIAN_POINT('Ctrl Pts',(30.0025158682114,256.41323156183,20.2213203435596)) ;
#95700 = CARTESIAN_POINT('Ctrl Pts',(29.9974204876885,256.405779717855,20.2213203435596)) ;
#95701 = CARTESIAN_POINT('Ctrl Pts',(29.9925362825257,256.397990818504,20.2213203435596)) ;
#95702 = CARTESIAN_POINT('Ctrl Pts',(29.9878117975722,256.389913149835,20.2213203435596)) ;
#95703 = CARTESIAN_POINT('Ctrl Pts',(29.9850035581777,256.385111774109,20.2213203435596)) ;
#95704 = CARTESIAN_POINT('Ctrl Pts',(29.9822527683305,256.380210786577,20.2213203435596)) ;
#95705 = CARTESIAN_POINT('Ctrl Pts',(29.9795492395846,256.375224378147,20.2213203435596)) ;
#95706 = CARTESIAN_POINT('Ctrl Pts',(29.973935966022,256.36487121484,20.2213203435596)) ;
#95707 = CARTESIAN_POINT('Ctrl Pts',(29.9685037596898,256.354113134005,20.2213203435596)) ;
#95708 = CARTESIAN_POINT('Ctrl Pts',(29.9631379985744,256.342986062281,20.2213203435596)) ;
#95709 = CARTESIAN_POINT('Ctrl Pts',(29.9575091150603,256.331313349083,20.2213203435596)) ;
#95710 = CARTESIAN_POINT('Ctrl Pts',(29.951953721328,256.319234967557,20.2213203435596)) ;
#95711 = CARTESIAN_POINT('Ctrl Pts',(29.9463917654129,256.306822917892,20.2213203435596)) ;
#95712 = CARTESIAN_POINT('Ctrl Pts',(29.940330026839,256.293295554248,20.2213203435596)) ;
#95713 = CARTESIAN_POINT('Ctrl Pts',(29.9342606912573,256.279372250169,20.2213203435596)) ;
#95714 = CARTESIAN_POINT('Ctrl Pts',(29.9281366213413,256.265175509829,20.2213203435596)) ;
#95715 = CARTESIAN_POINT('Ctrl Pts',(29.9250495282719,256.258019050266,20.2213203435596)) ;
#95716 = CARTESIAN_POINT('Ctrl Pts',(29.9219493584908,256.250793510573,20.2213203435596)) ;
#95717 = CARTESIAN_POINT('Ctrl Pts',(29.9188345104747,256.243516527177,20.2213203435596)) ;
#95718 = CARTESIAN_POINT('Ctrl Pts',(29.917799703434,256.241098985899,20.2213203435596)) ;
#95719 = CARTESIAN_POINT('Ctrl Pts',(29.9167633738339,256.238680704014,20.2213203435596)) ;
#95720 = CARTESIAN_POINT('Ctrl Pts',(29.9157260475512,256.236262805576,20.2213203435596)) ;
#95721 = CARTESIAN_POINT('Ctrl Pts',(29.9114086798316,256.226199475615,20.2213203435596)) ;
#95722 = CARTESIAN_POINT('Ctrl Pts',(29.9070371070764,256.216056684626,20.2213203435596)) ;
#95723 = CARTESIAN_POINT('Ctrl Pts',(29.9026389079555,256.20589382332,20.2213203435596)) ;
#95724 = CARTESIAN_POINT('Ctrl Pts',(29.8967419008071,256.192267685866,20.2213203435596)) ;
#95725 = CARTESIAN_POINT('Ctrl Pts',(29.8907954352119,256.178601428562,20.2213203435596)) ;
#95726 = CARTESIAN_POINT('Ctrl Pts',(29.8848059534797,256.164901729482,20.2213203435596)) ;
#95727 = CARTESIAN_POINT('Ctrl Pts',(29.8803666705202,256.154747789058,20.2213203435596)) ;
#95728 = CARTESIAN_POINT('Ctrl Pts',(29.8759018339445,256.144571176857,20.2213203435596)) ;
#95729 = CARTESIAN_POINT('Ctrl Pts',(29.8714117082223,256.13437046548,20.2213203435596)) ;
#95730 = CARTESIAN_POINT('Ctrl Pts',(29.8630996041311,256.115486946395,20.2213203435596)) ;
#95731 = CARTESIAN_POINT('Ctrl Pts',(29.8547089250513,256.096539146837,20.2213203435596)) ;
#95732 = CARTESIAN_POINT('Ctrl Pts',(29.8462711252824,256.077589395044,20.2213203435596)) ;
#95733 = CARTESIAN_POINT('Ctrl Pts',(29.8377907984774,256.058544135322,20.2213203435596)) ;
#95734 = CARTESIAN_POINT('Ctrl Pts',(29.82926345751,256.039498220475,20.2213203435596)) ;
#95735 = CARTESIAN_POINT('Ctrl Pts',(29.820704336771,256.020480351935,20.2213203435596)) ;
#95736 = CARTESIAN_POINT('Ctrl Pts',(29.8109891323347,255.998893732649,20.2213203435596)) ;
#95737 = CARTESIAN_POINT('Ctrl Pts',(29.8012292399256,255.977334867106,20.2213203435596)) ;
#95738 = CARTESIAN_POINT('Ctrl Pts',(29.791431425698,255.955815501484,20.2213203435596)) ;
#95739 = CARTESIAN_POINT('Ctrl Pts',(29.7810056880256,255.932917000284,20.2213203435596)) ;
#95740 = CARTESIAN_POINT('Ctrl Pts',(29.7705369433913,255.910062911148,20.2213203435596)) ;
#95741 = CARTESIAN_POINT('Ctrl Pts',(29.7600080208177,255.887217116999,20.2213203435596)) ;
#95742 = CARTESIAN_POINT('Ctrl Pts',(29.7465625544269,255.858042967863,20.2213203435596)) ;
#95743 = CARTESIAN_POINT('Ctrl Pts',(29.7330220922707,255.82888937671,20.2213203435596)) ;
#95744 = CARTESIAN_POINT('Ctrl Pts',(29.7194047389056,255.799807444113,20.2213203435596)) ;
#95745 = CARTESIAN_POINT('Ctrl Pts',(29.7026300227241,255.763982482224,20.2213203435596)) ;
#95746 = CARTESIAN_POINT('Ctrl Pts',(29.6857384416576,255.728264855005,20.2213203435596)) ;
#95747 = CARTESIAN_POINT('Ctrl Pts',(29.6687236887841,255.692681924167,20.2213203435596)) ;
#95748 = CARTESIAN_POINT('Ctrl Pts',(29.651375474443,255.656401625791,20.2213203435596)) ;
#95749 = CARTESIAN_POINT('Ctrl Pts',(29.6338974093498,255.620256710442,20.2213203435596)) ;
#95750 = CARTESIAN_POINT('Ctrl Pts',(29.6162632186691,255.584264740826,20.2213203435596)) ;
#95751 = CARTESIAN_POINT('Ctrl Pts',(29.60292557718,255.557042170994,20.2213203435596)) ;
#95752 = CARTESIAN_POINT('Ctrl Pts',(29.5894980112796,255.52990631417,20.2213203435596)) ;
#95753 = CARTESIAN_POINT('Ctrl Pts',(29.5759716504483,255.502885786844,20.2213203435596)) ;
#95754 = CARTESIAN_POINT('',(30.5008469122091,256.738337318211,20.3213203435596)) ;
#95755 = CARTESIAN_POINT('Ctrl Pts',(29.4405240550634,255.455707305529,20.3213203435596)) ;
#95756 = CARTESIAN_POINT('Ctrl Pts',(29.5203551947139,255.615433505657,20.3213203435596)) ;
#95757 = CARTESIAN_POINT('Ctrl Pts',(29.6220701604893,255.813265522892,20.3213203435596)) ;
#95758 = CARTESIAN_POINT('Ctrl Pts',(29.7232911658707,256.03691957849,20.3213203435596)) ;
#95759 = CARTESIAN_POINT('Ctrl Pts',(29.7590138224883,256.118832061085,20.3213203435596)) ;
#95760 = CARTESIAN_POINT('Ctrl Pts',(29.785505857421,256.180251232298,20.3213203435596)) ;
#95761 = CARTESIAN_POINT('Ctrl Pts',(29.8067673218597,256.231965600798,20.3213203435596)) ;
#95762 = CARTESIAN_POINT('Ctrl Pts',(29.8426325824515,256.31295578499,20.3213203435596)) ;
#95763 = CARTESIAN_POINT('Ctrl Pts',(29.8982853405048,256.462949425189,20.3213203435596)) ;
#95764 = CARTESIAN_POINT('Ctrl Pts',(30.0777583197704,256.624424879292,20.3213203435596)) ;
#95765 = CARTESIAN_POINT('Ctrl Pts',(30.3057090045425,256.693597510598,20.3213203435596)) ;
#95766 = CARTESIAN_POINT('Ctrl Pts',(30.446346059137,256.727112644825,20.3213203435596)) ;
#95767 = CARTESIAN_POINT('Ctrl Pts',(30.5008469122103,256.738337318211,20.3213203435596)) ;
#95768 = CARTESIAN_POINT('Ctrl Pts',(30.5008469122093,256.73833731821,20.3213203435596)) ;
#95769 = CARTESIAN_POINT('Ctrl Pts',(30.5011281297113,256.738149508513,20.3213203435596)) ;
#95770 = CARTESIAN_POINT('Ctrl Pts',(30.5014092894833,256.737961609899,20.3213194299206)) ;
#95771 = CARTESIAN_POINT('Ctrl Pts',(30.5150875989089,256.728814269044,20.3212305906335)) ;
#95772 = CARTESIAN_POINT('Ctrl Pts',(30.5284725288954,256.719563247393,20.3190721427316)) ;
#95773 = CARTESIAN_POINT('Ctrl Pts',(30.5531946098367,256.70222613735,20.3109405228244)) ;
#95774 = CARTESIAN_POINT('Ctrl Pts',(30.5649646262603,256.693857183022,20.3050698997908)) ;
#95775 = CARTESIAN_POINT('Ctrl Pts',(30.5866919680773,256.678623368935,20.2887421025002)) ;
#95776 = CARTESIAN_POINT('Ctrl Pts',(30.5959391028663,256.672153993788,20.2785447738736)) ;
#95777 = CARTESIAN_POINT('Ctrl Pts',(30.6067555479079,256.66441843623,20.2602592440806)) ;
#95778 = CARTESIAN_POINT('Ctrl Pts',(30.6100239931557,256.662039953674,20.2528168931027)) ;
#95779 = CARTESIAN_POINT('Ctrl Pts',(30.6143734110351,256.658828819451,20.2372682660181)) ;
#95780 = CARTESIAN_POINT('Ctrl Pts',(30.6155000490728,256.657966189434,20.2293609459321)) ;
#95781 = CARTESIAN_POINT('Ctrl Pts',(30.6155000490728,256.657966189434,20.2213203435596)) ;
#95782 = CARTESIAN_POINT('Origin',(30.5923736638261,256.185010099112,20.2213203435596)) ;
#95783 = CARTESIAN_POINT('',(30.6910330619062,256.201329509961,20.2213203435596)) ;
#95784 = CARTESIAN_POINT('',(30.5923736638261,256.185010099112,20.3213203435596)) ;
#95785 = CARTESIAN_POINT('Origin',(30.029721514783,255.291297809793,20.0213203435596)) ;
#95786 = CARTESIAN_POINT('',(29.5759712687712,255.502885024399,20.1213203435596)) ;
#95787 = CARTESIAN_POINT('',(29.5759712687709,255.502885024398,20.0213203435596)) ;
#95788 = CARTESIAN_POINT('',(30.029721514783,255.291297809793,20.1213203435596)) ;
#95789 = CARTESIAN_POINT('',(43.1641155815879,249.166629271216,20.1213203435596)) ;
#95790 = CARTESIAN_POINT('',(30.029721514783,255.291297809793,20.0213203435596)) ;
#95791 = CARTESIAN_POINT('Ctrl Pts',(29.5759712687716,255.502885024399,20.0213203435596)) ;
#95792 = CARTESIAN_POINT('Ctrl Pts',(29.5759712687716,255.502885024399,20.3813203435596)) ;
#95793 = CARTESIAN_POINT('Ctrl Pts',(29.7060244888525,255.762681865726,20.0213203435596)) ;
#95794 = CARTESIAN_POINT('Ctrl Pts',(29.7060244888525,255.762681865726,20.3813203435596)) ;
#95795 = CARTESIAN_POINT('Ctrl Pts',(29.8400217958637,256.05939235397,20.0213203435596)) ;
#95796 = CARTESIAN_POINT('Ctrl Pts',(29.8400217958637,256.05939235397,20.3813203435596)) ;
#95797 = CARTESIAN_POINT('Ctrl Pts',(29.9188345104747,256.243516527177,20.0213203435596)) ;
#95798 = CARTESIAN_POINT('Ctrl Pts',(29.9188345104747,256.243516527177,20.3813203435596)) ;
#95799 = CARTESIAN_POINT('Ctrl Pts',(30.0015982144022,256.436871097342,20.0213203435596)) ;
#95800 = CARTESIAN_POINT('Ctrl Pts',(30.0015982144022,256.436871097342,20.3813203435596)) ;
#95801 = CARTESIAN_POINT('Ctrl Pts',(30.0230446934974,256.474570522956,20.0213203435596)) ;
#95802 = CARTESIAN_POINT('Ctrl Pts',(30.0230446934974,256.474570522956,20.3813203435596)) ;
#95803 = CARTESIAN_POINT('Ctrl Pts',(30.1974245258637,256.548481045224,20.0213203435596)) ;
#95804 = CARTESIAN_POINT('Ctrl Pts',(30.1974245258637,256.548481045224,20.3813203435596)) ;
#95805 = CARTESIAN_POINT('Ctrl Pts',(30.2961501724434,256.590325701232,20.0213203435596)) ;
#95806 = CARTESIAN_POINT('Ctrl Pts',(30.2961501724434,256.590325701232,20.3813203435596)) ;
#95807 = CARTESIAN_POINT('Ctrl Pts',(30.4375870001386,256.628537303818,20.0213203435596)) ;
#95808 = CARTESIAN_POINT('Ctrl Pts',(30.4375870001386,256.628537303818,20.3813203435596)) ;
#95809 = CARTESIAN_POINT('Ctrl Pts',(30.6155000490728,256.657966189434,20.0213203435596)) ;
#95810 = CARTESIAN_POINT('Ctrl Pts',(30.6155000490728,256.657966189434,20.3813203435596)) ;
#95811 = CARTESIAN_POINT('',(30.6155000490728,256.657966189434,20.1213203435596)) ;
#95812 = CARTESIAN_POINT('',(30.6155000490728,256.657966189434,20.0213203435596)) ;
#95813 = CARTESIAN_POINT('Ctrl Pts',(29.5759712687716,255.502885024399,20.1213203435596)) ;
#95814 = CARTESIAN_POINT('Ctrl Pts',(29.5913953099987,255.533696389076,20.1213203435596)) ;
#95815 = CARTESIAN_POINT('Ctrl Pts',(29.606657599885,255.564590752194,20.1213203435596)) ;
#95816 = CARTESIAN_POINT('Ctrl Pts',(29.6217610079184,255.595501219028,20.1213203435596)) ;
#95817 = CARTESIAN_POINT('Ctrl Pts',(29.6375733914914,255.627862667312,20.1213203435596)) ;
#95818 = CARTESIAN_POINT('Ctrl Pts',(29.6532125375535,255.660243957624,20.1213203435596)) ;
#95819 = CARTESIAN_POINT('Ctrl Pts',(29.6686892717481,255.692609948402,20.1213203435596)) ;
#95820 = CARTESIAN_POINT('Ctrl Pts',(29.672942829729,255.701505275843,20.1213203435596)) ;
#95821 = CARTESIAN_POINT('Ctrl Pts',(29.6771854330678,255.71040235893,20.1213203435596)) ;
#95822 = CARTESIAN_POINT('Ctrl Pts',(29.6814079996186,255.719281115549,20.1213203435596)) ;
#95823 = CARTESIAN_POINT('Ctrl Pts',(29.6963375495941,255.75067335983,20.1213203435596)) ;
#95824 = CARTESIAN_POINT('Ctrl Pts',(29.7110459269022,255.781895244612,20.1213203435596)) ;
#95825 = CARTESIAN_POINT('Ctrl Pts',(29.7256409125464,255.813142245774,20.1213203435596)) ;
#95826 = CARTESIAN_POINT('Ctrl Pts',(29.737497273023,255.838526012405,20.1213203435596)) ;
#95827 = CARTESIAN_POINT('Ctrl Pts',(29.7492789979749,255.863927567679,20.1213203435596)) ;
#95828 = CARTESIAN_POINT('Ctrl Pts',(29.7610245812382,255.889423296196,20.1213203435596)) ;
#95829 = CARTESIAN_POINT('Ctrl Pts',(29.7715454768417,255.912260637863,20.1213203435596)) ;
#95830 = CARTESIAN_POINT('Ctrl Pts',(29.7820375533546,255.93517417614,20.1213203435596)) ;
#95831 = CARTESIAN_POINT('Ctrl Pts',(29.7925088651715,255.958182425098,20.1213203435596)) ;
#95832 = CARTESIAN_POINT('Ctrl Pts',(29.8021506276027,255.979367934068,20.1213203435596)) ;
#95833 = CARTESIAN_POINT('Ctrl Pts',(29.8117749431216,256.000634221753,20.1213203435596)) ;
#95834 = CARTESIAN_POINT('Ctrl Pts',(29.8213682132304,256.021955645211,20.1213203435596)) ;
#95835 = CARTESIAN_POINT('Ctrl Pts',(29.8296255852217,256.040307982096,20.1213203435596)) ;
#95836 = CARTESIAN_POINT('Ctrl Pts',(29.8378598391904,256.058700999499,20.1213203435596)) ;
#95837 = CARTESIAN_POINT('Ctrl Pts',(29.8460471694367,256.077086455705,20.1213203435596)) ;
#95838 = CARTESIAN_POINT('Ctrl Pts',(29.8503425417667,256.086732137202,20.1213203435596)) ;
#95839 = CARTESIAN_POINT('Ctrl Pts',(29.8546247428343,256.096375192364,20.1213203435596)) ;
#95840 = CARTESIAN_POINT('Ctrl Pts',(29.8588884181389,256.106004515113,20.1213203435596)) ;
#95841 = CARTESIAN_POINT('Ctrl Pts',(29.8628290229948,256.114904197494,20.1213203435596)) ;
#95842 = CARTESIAN_POINT('Ctrl Pts',(29.8667535356127,256.123791473506,20.1213203435596)) ;
#95843 = CARTESIAN_POINT('Ctrl Pts',(29.8706737970368,256.132694372067,20.1213203435596)) ;
#95844 = CARTESIAN_POINT('Ctrl Pts',(29.8765711738735,256.146087292099,20.1213203435596)) ;
#95845 = CARTESIAN_POINT('Ctrl Pts',(29.8824574550096,256.159512078262,20.1213203435596)) ;
#95846 = CARTESIAN_POINT('Ctrl Pts',(29.8883430841851,256.172999840968,20.1213203435596)) ;
#95847 = CARTESIAN_POINT('Ctrl Pts',(29.8934307149093,256.184658875864,20.1213203435596)) ;
#95848 = CARTESIAN_POINT('Ctrl Pts',(29.898517743333,256.196364776907,20.1213203435596)) ;
#95849 = CARTESIAN_POINT('Ctrl Pts',(29.9035963493755,256.208106827721,20.1213203435596)) ;
#95850 = CARTESIAN_POINT('Ctrl Pts',(29.905695121645,256.212959318824,20.1213203435596)) ;
#95851 = CARTESIAN_POINT('Ctrl Pts',(29.9077913676636,256.217815491281,20.1213203435596)) ;
#95852 = CARTESIAN_POINT('Ctrl Pts',(29.9098864190254,256.222679100839,20.1213203435596)) ;
#95853 = CARTESIAN_POINT('Ctrl Pts',(29.912860969859,256.229584446516,20.1213203435596)) ;
#95854 = CARTESIAN_POINT('Ctrl Pts',(29.9158371382348,256.236513993535,20.1213203435596)) ;
#95855 = CARTESIAN_POINT('Ctrl Pts',(29.9188345104747,256.243516527177,20.1213203435596)) ;
#95856 = CARTESIAN_POINT('Ctrl Pts',(29.9220123338014,256.250940635019,20.1213203435596)) ;
#95857 = CARTESIAN_POINT('Ctrl Pts',(29.925212850827,256.258400497147,20.1213203435596)) ;
#95858 = CARTESIAN_POINT('Ctrl Pts',(29.928467485032,256.265942362595,20.1213203435596)) ;
#95859 = CARTESIAN_POINT('Ctrl Pts',(29.9334713297245,256.277537620624,20.1213203435596)) ;
#95860 = CARTESIAN_POINT('Ctrl Pts',(29.9385989767258,256.289323440153,20.1213203435596)) ;
#95861 = CARTESIAN_POINT('Ctrl Pts',(29.9439045097073,256.30125136341,20.1213203435596)) ;
#95862 = CARTESIAN_POINT('Ctrl Pts',(29.9465408387867,256.307178370375,20.1213203435596)) ;
#95863 = CARTESIAN_POINT('Ctrl Pts',(29.9492214566145,256.313139672616,20.1213203435596)) ;
#95864 = CARTESIAN_POINT('Ctrl Pts',(29.951956258577,256.319123975837,20.1213203435596)) ;
#95865 = CARTESIAN_POINT('Ctrl Pts',(29.9533078440368,256.322081519868,20.1213203435596)) ;
#95866 = CARTESIAN_POINT('Ctrl Pts',(29.9546721053878,256.325043308408,20.1213203435596)) ;
#95867 = CARTESIAN_POINT('Ctrl Pts',(29.956050766892,256.328008190301,20.1213203435596)) ;
#95868 = CARTESIAN_POINT('Ctrl Pts',(29.9589666164282,256.334278873472,20.1213203435596)) ;
#95869 = CARTESIAN_POINT('Ctrl Pts',(29.9619550897243,256.340585078762,20.1213203435596)) ;
#95870 = CARTESIAN_POINT('Ctrl Pts',(29.9651070813677,256.347046007774,20.1213203435596)) ;
#95871 = CARTESIAN_POINT('Ctrl Pts',(29.9681841792228,256.353353420057,20.1213203435596)) ;
#95872 = CARTESIAN_POINT('Ctrl Pts',(29.9714161991448,256.35980818082,20.1213203435596)) ;
#95873 = CARTESIAN_POINT('Ctrl Pts',(29.9748955028022,256.366473500977,20.1213203435596)) ;
#95874 = CARTESIAN_POINT('Ctrl Pts',(29.9764839882022,256.36951657074,20.1213203435596)) ;
#95875 = CARTESIAN_POINT('Ctrl Pts',(29.9781242063225,256.372602871453,20.1213203435596)) ;
#95876 = CARTESIAN_POINT('Ctrl Pts',(29.9798264965544,256.375735147287,20.1213203435596)) ;
#95877 = CARTESIAN_POINT('Ctrl Pts',(29.9815832708521,256.378967675781,20.1213203435596)) ;
#95878 = CARTESIAN_POINT('Ctrl Pts',(29.9834033211469,256.382244469693,20.1213203435596)) ;
#95879 = CARTESIAN_POINT('Ctrl Pts',(29.9853133457605,256.385589444858,20.1213203435596)) ;
#95880 = CARTESIAN_POINT('Ctrl Pts',(29.9886267348614,256.391392094821,20.1213203435596)) ;
#95881 = CARTESIAN_POINT('Ctrl Pts',(29.9921970041105,256.397371990751,20.1213203435596)) ;
#95882 = CARTESIAN_POINT('Ctrl Pts',(29.9960076069629,256.403360144144,20.1213203435596)) ;
#95883 = CARTESIAN_POINT('Ctrl Pts',(29.9998805570769,256.40944627284,20.1213203435596)) ;
#95884 = CARTESIAN_POINT('Ctrl Pts',(30.0040023918854,256.415540642767,20.1213203435596)) ;
#95885 = CARTESIAN_POINT('Ctrl Pts',(30.0083734751479,256.421518111582,20.1213203435596)) ;
#95886 = CARTESIAN_POINT('Ctrl Pts',(30.0129328358726,256.427753050362,20.1213203435596)) ;
#95887 = CARTESIAN_POINT('Ctrl Pts',(30.0177646044409,256.433860953415,20.1213203435596)) ;
#95888 = CARTESIAN_POINT('Ctrl Pts',(30.0228741686605,256.439757844301,20.1213203435596)) ;
#95889 = CARTESIAN_POINT('Ctrl Pts',(30.0246611862642,256.441820221319,20.1213203435596)) ;
#95890 = CARTESIAN_POINT('Ctrl Pts',(30.0264821328035,256.443857271186,20.1213203435596)) ;
#95891 = CARTESIAN_POINT('Ctrl Pts',(30.0283368868403,256.445866834091,20.1213203435596)) ;
#95892 = CARTESIAN_POINT('Ctrl Pts',(30.0298862112431,256.447545474377,20.1213203435596)) ;
#95893 = CARTESIAN_POINT('Ctrl Pts',(30.0314569037599,256.449202440719,20.1213203435596)) ;
#95894 = CARTESIAN_POINT('Ctrl Pts',(30.033042872478,256.450831503359,20.1213203435596)) ;
#95895 = CARTESIAN_POINT('Ctrl Pts',(30.0386707717201,256.456612323806,20.1213203435596)) ;
#95896 = CARTESIAN_POINT('Ctrl Pts',(30.0445161457859,256.462064166021,20.1213203435596)) ;
#95897 = CARTESIAN_POINT('Ctrl Pts',(30.0505343605665,256.467198645817,20.1213203435596)) ;
#95898 = CARTESIAN_POINT('Ctrl Pts',(30.0562706995585,256.472092641418,20.1213203435596)) ;
#95899 = CARTESIAN_POINT('Ctrl Pts',(30.0621643768898,256.476699356839,20.1213203435596)) ;
#95900 = CARTESIAN_POINT('Ctrl Pts',(30.0681284991347,256.481029630627,20.1213203435596)) ;
#95901 = CARTESIAN_POINT('Ctrl Pts',(30.0737341056397,256.485099602689,20.1213203435596)) ;
#95902 = CARTESIAN_POINT('Ctrl Pts',(30.0794015874553,256.488925833284,20.1213203435596)) ;
#95903 = CARTESIAN_POINT('Ctrl Pts',(30.0850160332146,256.492507744526,20.1213203435596)) ;
#95904 = CARTESIAN_POINT('Ctrl Pts',(30.0872502332293,256.493933122292,20.1213203435596)) ;
#95905 = CARTESIAN_POINT('Ctrl Pts',(30.0894737911333,256.495318583433,20.1213203435596)) ;
#95906 = CARTESIAN_POINT('Ctrl Pts',(30.091683401717,256.49666693007,20.1213203435596)) ;
#95907 = CARTESIAN_POINT('Ctrl Pts',(30.0990683870628,256.501173389365,20.1213203435596)) ;
#95908 = CARTESIAN_POINT('Ctrl Pts',(30.1063559904706,256.505305915035,20.1213203435596)) ;
#95909 = CARTESIAN_POINT('Ctrl Pts',(30.113544973547,256.509186721459,20.1213203435596)) ;
#95910 = CARTESIAN_POINT('Ctrl Pts',(30.1206692308092,256.513032587147,20.1213203435596)) ;
#95911 = CARTESIAN_POINT('Ctrl Pts',(30.1276961540222,256.516629737619,20.1213203435596)) ;
#95912 = CARTESIAN_POINT('Ctrl Pts',(30.1346612641855,256.520067935113,20.1213203435596)) ;
#95913 = CARTESIAN_POINT('Ctrl Pts',(30.1389827717456,256.522201167196,20.1213203435596)) ;
#95914 = CARTESIAN_POINT('Ctrl Pts',(30.1432812579292,256.524272756909,20.1213203435596)) ;
#95915 = CARTESIAN_POINT('Ctrl Pts',(30.1475731986693,256.526301573969,20.1213203435596)) ;
#95916 = CARTESIAN_POINT('Ctrl Pts',(30.1508165612268,256.527834724049,20.1213203435596)) ;
#95917 = CARTESIAN_POINT('Ctrl Pts',(30.1540561636965,256.529343370907,20.1213203435596)) ;
#95918 = CARTESIAN_POINT('Ctrl Pts',(30.1573093625281,256.530838892824,20.1213203435596)) ;
#95919 = CARTESIAN_POINT('Ctrl Pts',(30.1694617945698,256.536425464502,20.1213203435596)) ;
#95920 = CARTESIAN_POINT('Ctrl Pts',(30.1817428975319,256.541804089539,20.1213203435596)) ;
#95921 = CARTESIAN_POINT('Ctrl Pts',(30.1940635106411,256.547052875707,20.1213203435596)) ;
#95922 = CARTESIAN_POINT('Ctrl Pts',(30.1951835168917,256.547530017004,20.1213203435596)) ;
#95923 = CARTESIAN_POINT('Ctrl Pts',(30.1963038727072,256.548006058759,20.1213203435596)) ;
#95924 = CARTESIAN_POINT('Ctrl Pts',(30.1974245258637,256.548481045224,20.1213203435596)) ;
#95925 = CARTESIAN_POINT('Ctrl Pts',(30.208594161561,256.553215271635,20.1213203435596)) ;
#95926 = CARTESIAN_POINT('Ctrl Pts',(30.2197078755529,256.557649623137,20.1213203435596)) ;
#95927 = CARTESIAN_POINT('Ctrl Pts',(30.2307049675344,256.561831588478,20.1213203435596)) ;
#95928 = CARTESIAN_POINT('Ctrl Pts',(30.2422487637936,256.566221454084,20.1213203435596)) ;
#95929 = CARTESIAN_POINT('Ctrl Pts',(30.2536644123742,256.570333309343,20.1213203435596)) ;
#95930 = CARTESIAN_POINT('Ctrl Pts',(30.2649410294572,256.574220554478,20.1213203435596)) ;
#95931 = CARTESIAN_POINT('Ctrl Pts',(30.2767770287943,256.578300628361,20.1213203435596)) ;
#95932 = CARTESIAN_POINT('Ctrl Pts',(30.2884602178804,256.582133338675,20.1213203435596)) ;
#95933 = CARTESIAN_POINT('Ctrl Pts',(30.3000360626451,256.585777382226,20.1213203435596)) ;
#95934 = CARTESIAN_POINT('Ctrl Pts',(30.3121484715133,256.589590334656,20.1213203435596)) ;
#95935 = CARTESIAN_POINT('Ctrl Pts',(30.3241436827804,256.593196802209,20.1213203435596)) ;
#95936 = CARTESIAN_POINT('Ctrl Pts',(30.3361302501676,256.596659505367,20.1213203435596)) ;
#95937 = CARTESIAN_POINT('Ctrl Pts',(30.3476017541364,256.599973415991,20.1213203435596)) ;
#95938 = CARTESIAN_POINT('Ctrl Pts',(30.3590660993346,256.603155652241,20.1213203435596)) ;
#95939 = CARTESIAN_POINT('Ctrl Pts',(30.3706597165934,256.606256700273,20.1213203435596)) ;
#95940 = CARTESIAN_POINT('Ctrl Pts',(30.3745723985987,256.607303260165,20.1213203435596)) ;
#95941 = CARTESIAN_POINT('Ctrl Pts',(30.3785001170307,256.608340533834,20.1213203435596)) ;
#95942 = CARTESIAN_POINT('Ctrl Pts',(30.38244904473,256.609370338222,20.1213203435596)) ;
#95943 = CARTESIAN_POINT('Ctrl Pts',(30.3852902557076,256.610111271395,20.1213203435596)) ;
#95944 = CARTESIAN_POINT('Ctrl Pts',(30.388142904833,256.610848427449,20.1213203435596)) ;
#95945 = CARTESIAN_POINT('Ctrl Pts',(30.3909923573432,256.611578161377,20.1213203435596)) ;
#95946 = CARTESIAN_POINT('Ctrl Pts',(30.4116121950221,256.616858823221,20.1213203435596)) ;
#95947 = CARTESIAN_POINT('Ctrl Pts',(30.4322462282601,256.621799850728,20.1213203435596)) ;
#95948 = CARTESIAN_POINT('Ctrl Pts',(30.4528279178749,256.626445919744,20.1213203435596)) ;
#95949 = CARTESIAN_POINT('Ctrl Pts',(30.4740982133567,256.631247433257,20.1213203435596)) ;
#95950 = CARTESIAN_POINT('Ctrl Pts',(30.4953129743173,256.6357340405,20.1213203435596)) ;
#95951 = CARTESIAN_POINT('Ctrl Pts',(30.5164561522723,256.639951891567,20.1213203435596)) ;
#95952 = CARTESIAN_POINT('Ctrl Pts',(30.5330282715866,256.64325786247,20.1213203435596)) ;
#95953 = CARTESIAN_POINT('Ctrl Pts',(30.5495576412942,256.646398667391,20.1213203435596)) ;
#95954 = CARTESIAN_POINT('Ctrl Pts',(30.5660577288476,256.649394609518,20.1213203435596)) ;
#95955 = CARTESIAN_POINT('Ctrl Pts',(30.5743106576067,256.650893104412,20.1213203435596)) ;
#95956 = CARTESIAN_POINT('Ctrl Pts',(30.5825565323396,256.652355329413,20.1213203435596)) ;
#95957 = CARTESIAN_POINT('Ctrl Pts',(30.5907985781165,256.653783641014,20.1213203435596)) ;
#95958 = CARTESIAN_POINT('Ctrl Pts',(30.5966484079928,256.654797391738,20.1213203435596)) ;
#95959 = CARTESIAN_POINT('Ctrl Pts',(30.6024963300507,256.655794055932,20.1213203435596)) ;
#95960 = CARTESIAN_POINT('Ctrl Pts',(30.6083437875869,256.656774435841,20.1213203435596)) ;
#95961 = CARTESIAN_POINT('Ctrl Pts',(30.6107292733287,256.657174384413,20.1213203435596)) ;
#95962 = CARTESIAN_POINT('Ctrl Pts',(30.6131151734722,256.657571703298,20.1213203435596)) ;
#95963 = CARTESIAN_POINT('Ctrl Pts',(30.6155000490728,256.657966189434,20.1213203435596)) ;
#95964 = CARTESIAN_POINT('Origin',(30.6155000490728,256.657966189434,20.0213203435596)) ;
#95965 = CARTESIAN_POINT('',(30.5502224098271,257.05260375666,20.1213203435596)) ;
#95966 = CARTESIAN_POINT('',(30.5502224056744,257.052603781754,20.0213203435596)) ;
#95967 = CARTESIAN_POINT('',(32.2263894714028,246.919294723581,20.1213203435596)) ;
#95968 = CARTESIAN_POINT('Ctrl Pts',(30.5502224056744,257.052603781754,20.0213203435596)) ;
#95969 = CARTESIAN_POINT('Ctrl Pts',(30.5502224056744,257.052603781754,20.3813203435596)) ;
#95970 = CARTESIAN_POINT('Ctrl Pts',(30.2175036768426,256.997568237865,20.0213203435596)) ;
#95971 = CARTESIAN_POINT('Ctrl Pts',(30.2175036768426,256.997568237865,20.3813203435596)) ;
#95972 = CARTESIAN_POINT('Ctrl Pts',(29.9660260593743,256.919766544724,20.0213203435596)) ;
#95973 = CARTESIAN_POINT('Ctrl Pts',(29.9660260593743,256.919766544724,20.3813203435596)) ;
#95974 = CARTESIAN_POINT('Ctrl Pts',(29.7871734949583,256.762313540024,20.0213203435596)) ;
#95975 = CARTESIAN_POINT('Ctrl Pts',(29.7871734949583,256.762313540024,20.3813203435596)) ;
#95976 = CARTESIAN_POINT('Ctrl Pts',(29.6146430046735,256.610426178574,20.0213203435596)) ;
#95977 = CARTESIAN_POINT('Ctrl Pts',(29.6146430046735,256.610426178574,20.3813203435596)) ;
#95978 = CARTESIAN_POINT('Ctrl Pts',(29.5623693529378,256.421344022006,20.0213203435596)) ;
#95979 = CARTESIAN_POINT('Ctrl Pts',(29.5623693529378,256.421344022006,20.3813203435596)) ;
#95980 = CARTESIAN_POINT('Ctrl Pts',(29.4657236710055,256.200700387666,20.0213203435596)) ;
#95981 = CARTESIAN_POINT('Ctrl Pts',(29.4657236710055,256.200700387666,20.3813203435596)) ;
#95982 = CARTESIAN_POINT('Ctrl Pts',(29.3957391712889,256.040924657844,20.0213203435596)) ;
#95983 = CARTESIAN_POINT('Ctrl Pts',(29.3957391712889,256.040924657844,20.3813203435596)) ;
#95984 = CARTESIAN_POINT('Ctrl Pts',(29.303002575605,255.851124410942,20.0213203435596)) ;
#95985 = CARTESIAN_POINT('Ctrl Pts',(29.303002575605,255.851124410942,20.3813203435596)) ;
#95986 = CARTESIAN_POINT('Ctrl Pts',(29.2133075051976,255.671997914687,20.0213203435596)) ;
#95987 = CARTESIAN_POINT('Ctrl Pts',(29.2133075051976,255.671997914687,20.3813203435596)) ;
#95988 = CARTESIAN_POINT('',(29.2133075051975,255.671997914687,20.1213203435596)) ;
#95989 = CARTESIAN_POINT('',(29.2133075051975,255.671997914687,20.0213203435596)) ;
#95990 = CARTESIAN_POINT('Ctrl Pts',(30.5502224021797,257.052603781176,20.1213203435596)) ;
#95991 = CARTESIAN_POINT('Ctrl Pts',(30.5065121505456,257.045373597616,20.1213203435596)) ;
#95992 = CARTESIAN_POINT('Ctrl Pts',(30.4628107310559,257.037524057822,20.1213203435596)) ;
#95993 = CARTESIAN_POINT('Ctrl Pts',(30.419433748458,257.028837962877,20.1213203435596)) ;
#95994 = CARTESIAN_POINT('Ctrl Pts',(30.3764380403507,257.020228216866,20.1213203435596)) ;
#95995 = CARTESIAN_POINT('Ctrl Pts',(30.3337612777691,257.010796594269,20.1213203435596)) ;
#95996 = CARTESIAN_POINT('Ctrl Pts',(30.2916991266286,257.000281937884,20.1213203435596)) ;
#95997 = CARTESIAN_POINT('Ctrl Pts',(30.2498339205488,256.989816513638,20.1213203435596)) ;
#95998 = CARTESIAN_POINT('Ctrl Pts',(30.2085777501619,256.978278169064,20.1213203435596)) ;
#95999 = CARTESIAN_POINT('Ctrl Pts',(30.1682078765978,256.965359723244,20.1213203435596)) ;
#96000 = CARTESIAN_POINT('Ctrl Pts',(30.132392671999,256.953898781227,20.1213203435596)) ;
#96001 = CARTESIAN_POINT('Ctrl Pts',(30.0972749265278,256.941350869345,20.1213203435596)) ;
#96002 = CARTESIAN_POINT('Ctrl Pts',(30.063037275111,256.927468848656,20.1213203435596)) ;
#96003 = CARTESIAN_POINT('Ctrl Pts',(30.0369143514349,256.91687703082,20.1213203435596)) ;
#96004 = CARTESIAN_POINT('Ctrl Pts',(30.011303572708,256.905507926888,20.1213203435596)) ;
#96005 = CARTESIAN_POINT('Ctrl Pts',(29.9862815616792,256.893239962228,20.1213203435596)) ;
#96006 = CARTESIAN_POINT('Ctrl Pts',(29.9808065317204,256.890555626666,20.1213203435596)) ;
#96007 = CARTESIAN_POINT('Ctrl Pts',(29.9753662544494,256.887831397022,20.1213203435596)) ;
#96008 = CARTESIAN_POINT('Ctrl Pts',(29.9699674807984,256.885069553557,20.1213203435596)) ;
#96009 = CARTESIAN_POINT('Ctrl Pts',(29.9339427287467,256.866640419009,20.1213203435596)) ;
#96010 = CARTESIAN_POINT('Ctrl Pts',(29.8996687771619,256.846493324965,20.1213203435596)) ;
#96011 = CARTESIAN_POINT('Ctrl Pts',(29.8671268712235,256.824286093635,20.1213203435596)) ;
#96012 = CARTESIAN_POINT('Ctrl Pts',(29.8391989590962,256.805227541676,20.1213203435596)) ;
#96013 = CARTESIAN_POINT('Ctrl Pts',(29.812547151782,256.784651260035,20.1213203435596)) ;
#96014 = CARTESIAN_POINT('Ctrl Pts',(29.7871734949583,256.762313540024,20.1213203435596)) ;
#96015 = CARTESIAN_POINT('Ctrl Pts',(29.7798631632135,256.755877883357,20.1213203435596)) ;
#96016 = CARTESIAN_POINT('Ctrl Pts',(29.7727535941871,256.749362117533,20.1213203435596)) ;
#96017 = CARTESIAN_POINT('Ctrl Pts',(29.7658341604035,256.742765184829,20.1213203435596)) ;
#96018 = CARTESIAN_POINT('Ctrl Pts',(29.7629186498988,256.739985560484,20.1213203435596)) ;
#96019 = CARTESIAN_POINT('Ctrl Pts',(29.760038549478,256.737193161988,20.1213203435596)) ;
#96020 = CARTESIAN_POINT('Ctrl Pts',(29.7571877188389,256.734382633857,20.1213203435596)) ;
#96021 = CARTESIAN_POINT('Ctrl Pts',(29.7414155814302,256.718833468903,20.1213203435596)) ;
#96022 = CARTESIAN_POINT('Ctrl Pts',(29.7264026361634,256.70258812366,20.1213203435596)) ;
#96023 = CARTESIAN_POINT('Ctrl Pts',(29.7121305617268,256.685637834918,20.1213203435596)) ;
#96024 = CARTESIAN_POINT('Ctrl Pts',(29.6976717683343,256.668465788628,20.1213203435596)) ;
#96025 = CARTESIAN_POINT('Ctrl Pts',(29.6839733667144,256.650570190372,20.1213203435596)) ;
#96026 = CARTESIAN_POINT('Ctrl Pts',(29.6709626703656,256.631947663274,20.1213203435596)) ;
#96027 = CARTESIAN_POINT('Ctrl Pts',(29.6577459536387,256.613030254183,20.1213203435596)) ;
#96028 = CARTESIAN_POINT('Ctrl Pts',(29.6452388100344,256.593362670542,20.1213203435596)) ;
#96029 = CARTESIAN_POINT('Ctrl Pts',(29.6333105692318,256.572947902923,20.1213203435596)) ;
#96030 = CARTESIAN_POINT('Ctrl Pts',(29.6250306407882,256.558777094514,20.1213203435596)) ;
#96031 = CARTESIAN_POINT('Ctrl Pts',(29.6170284895913,256.544246402727,20.1213203435596)) ;
#96032 = CARTESIAN_POINT('Ctrl Pts',(29.6092459213769,256.529358778693,20.1213203435596)) ;
#96033 = CARTESIAN_POINT('Ctrl Pts',(29.6022331469033,256.515943727656,20.1213203435596)) ;
#96034 = CARTESIAN_POINT('Ctrl Pts',(29.595395074189,256.502230920785,20.1213203435596)) ;
#96035 = CARTESIAN_POINT('Ctrl Pts',(29.5887073572941,256.488280078175,20.1213203435596)) ;
#96036 = CARTESIAN_POINT('Ctrl Pts',(29.5770550838555,256.46397297377,20.1213203435596)) ;
#96037 = CARTESIAN_POINT('Ctrl Pts',(29.5658526158538,256.438926685936,20.1213203435596)) ;
#96038 = CARTESIAN_POINT('Ctrl Pts',(29.5548544878541,256.413358282385,20.1213203435596)) ;
#96039 = CARTESIAN_POINT('Ctrl Pts',(29.5436688986819,256.387354069856,20.1213203435596)) ;
#96040 = CARTESIAN_POINT('Ctrl Pts',(29.5326904502648,256.360809843577,20.1213203435596)) ;
#96041 = CARTESIAN_POINT('Ctrl Pts',(29.5216537891901,256.333994033072,20.1213203435596)) ;
#96042 = CARTESIAN_POINT('Ctrl Pts',(29.5119415174706,256.310396095593,20.1213203435596)) ;
#96043 = CARTESIAN_POINT('Ctrl Pts',(29.502182328794,256.28658856044,20.1213203435596)) ;
#96044 = CARTESIAN_POINT('Ctrl Pts',(29.4922299276695,256.262778202882,20.1213203435596)) ;
#96045 = CARTESIAN_POINT('Ctrl Pts',(29.4888317484153,256.254648319241,20.1213203435596)) ;
#96046 = CARTESIAN_POINT('Ctrl Pts',(29.4854114762981,256.246518287048,20.1213203435596)) ;
#96047 = CARTESIAN_POINT('Ctrl Pts',(29.4819648387099,256.238396879059,20.1213203435596)) ;
#96048 = CARTESIAN_POINT('Ctrl Pts',(29.4793643985126,256.232269389512,20.1213203435596)) ;
#96049 = CARTESIAN_POINT('Ctrl Pts',(29.4767502042541,256.226149754618,20.1213203435596)) ;
#96050 = CARTESIAN_POINT('Ctrl Pts',(29.4741225626305,256.220045764497,20.1213203435596)) ;
#96051 = CARTESIAN_POINT('Ctrl Pts',(29.4713402639055,256.213582507187,20.1213203435596)) ;
#96052 = CARTESIAN_POINT('Ctrl Pts',(29.4685417765459,256.207134167592,20.1213203435596)) ;
#96053 = CARTESIAN_POINT('Ctrl Pts',(29.4657236710055,256.200700387666,20.1213203435596)) ;
#96054 = CARTESIAN_POINT('Ctrl Pts',(29.4555593833296,256.177495156678,20.1213203435596)) ;
#96055 = CARTESIAN_POINT('Ctrl Pts',(29.4451538317021,256.154199155577,20.1213203435596)) ;
#96056 = CARTESIAN_POINT('Ctrl Pts',(29.4346031772323,256.130925997744,20.1213203435596)) ;
#96057 = CARTESIAN_POINT('Ctrl Pts',(29.4257673000282,256.111435380803,20.1213203435596)) ;
#96058 = CARTESIAN_POINT('Ctrl Pts',(29.4168288645707,256.091959615128,20.1213203435596)) ;
#96059 = CARTESIAN_POINT('Ctrl Pts',(29.4078284012213,256.072542223159,20.1213203435596)) ;
#96060 = CARTESIAN_POINT('Ctrl Pts',(29.3998947826689,256.05542641754,20.1213203435596)) ;
#96061 = CARTESIAN_POINT('Ctrl Pts',(29.3919126877309,256.038355551961,20.1213203435596)) ;
#96062 = CARTESIAN_POINT('Ctrl Pts',(29.3839024014031,256.021348711648,20.1213203435596)) ;
#96063 = CARTESIAN_POINT('Ctrl Pts',(29.3795273962477,256.012060028197,20.1213203435596)) ;
#96064 = CARTESIAN_POINT('Ctrl Pts',(29.3751396619238,256.002781349386,20.1213203435596)) ;
#96065 = CARTESIAN_POINT('Ctrl Pts',(29.3707407195716,255.993512741724,20.1213203435596)) ;
#96066 = CARTESIAN_POINT('Ctrl Pts',(29.3568245289963,255.964191213894,20.1213203435596)) ;
#96067 = CARTESIAN_POINT('Ctrl Pts',(29.3428004323725,255.934977549532,20.1213203435596)) ;
#96068 = CARTESIAN_POINT('Ctrl Pts',(29.3287093952518,255.905877638673,20.1213203435596)) ;
#96069 = CARTESIAN_POINT('Ctrl Pts',(29.3106871743266,255.86865929783,20.1213203435596)) ;
#96070 = CARTESIAN_POINT('Ctrl Pts',(29.2925549661882,255.831625614527,20.1213203435596)) ;
#96071 = CARTESIAN_POINT('Ctrl Pts',(29.2743437474354,255.794722208492,20.1213203435596)) ;
#96072 = CARTESIAN_POINT('Ctrl Pts',(29.2540926156927,255.753685101227,20.1213203435596)) ;
#96073 = CARTESIAN_POINT('Ctrl Pts',(29.2337394567466,255.712801761275,20.1213203435596)) ;
#96074 = CARTESIAN_POINT('Ctrl Pts',(29.2133075051976,255.671997914687,20.1213203435596)) ;
#96075 = CARTESIAN_POINT('Origin',(29.6648327135485,255.562453330574,20.3213203435596)) ;
#96076 = CARTESIAN_POINT('Origin',(65.0184058153773,255.92214694455,20.2213203435596)) ;
#96077 = CARTESIAN_POINT('',(65.0184058153773,255.92214694455,20.3213203435596)) ;
#96078 = CARTESIAN_POINT('',(65.0184058153773,255.49075064338,20.3213203435596)) ;
#96079 = CARTESIAN_POINT('',(65.0184058153773,255.92214694455,20.3213203435596)) ;
#96080 = CARTESIAN_POINT('',(64.9184058153773,255.34214694455,20.2213203435596)) ;
#96081 = CARTESIAN_POINT('Origin',(65.0184058153773,255.49075064338,20.2213203435596)) ;
#96082 = CARTESIAN_POINT('',(64.9184058153773,255.82214694455,20.2213203435596)) ;
#96083 = CARTESIAN_POINT('',(64.9184058153773,255.92214694455,20.2213203435596)) ;
#96084 = CARTESIAN_POINT('Origin',(65.0184058153773,255.92214694455,20.2213203435596)) ;
#96085 = CARTESIAN_POINT('Origin',(65.0133528506462,255.488696344833,20.2213203435596)) ;
#96086 = CARTESIAN_POINT('',(66.3254830033414,256.02214694455,20.3213203435596)) ;
#96087 = CARTESIAN_POINT('',(65.0133528506462,255.488696344833,20.3213203435596)) ;
#96088 = CARTESIAN_POINT('',(66.5910039984262,256.02214694455,20.2213203435596)) ;
#96089 = CARTESIAN_POINT('Origin',(66.3254830033414,256.02214694455,20.2213203435596)) ;
#96090 = CARTESIAN_POINT('',(65.0510146558711,255.396059481613,20.2213203435596)) ;
#96091 = CARTESIAN_POINT('Origin',(65.8496519421707,256.215597544267,20.2213203435596)) ;
#96092 = CARTESIAN_POINT('',(65.0184058153773,256.55354324572,20.3213203435596)) ;
#96093 = CARTESIAN_POINT('',(65.8496519421707,256.215597544267,20.3213203435596)) ;
#96094 = CARTESIAN_POINT('',(64.9184058153773,256.70214694455,20.2213203435596)) ;
#96095 = CARTESIAN_POINT('Origin',(65.0184058153773,256.55354324572,20.2213203435596)) ;
#96096 = CARTESIAN_POINT('',(65.8873137473955,256.308234407487,20.2213203435596)) ;
#96097 = CARTESIAN_POINT('Origin',(65.0184058153773,256.36214694455,20.2213203435596)) ;
#96098 = CARTESIAN_POINT('',(64.9184058153773,256.22214694455,20.2213203435596)) ;
#96099 = CARTESIAN_POINT('',(64.9184058153773,256.36214694455,20.2213203435596)) ;
#96100 = CARTESIAN_POINT('',(65.0184058153773,256.12214694455,20.3213203435596)) ;
#96101 = CARTESIAN_POINT('',(65.0184058153773,256.36214694455,20.3213203435596)) ;
#96102 = CARTESIAN_POINT('Origin',(65.0184058153773,256.12214694455,20.2213203435596)) ;
#96103 = CARTESIAN_POINT('Origin',(64.9347049069018,256.12214694455,20.2213203435596)) ;
#96104 = CARTESIAN_POINT('',(63.3110039984262,256.22214694455,20.2213203435596)) ;
#96105 = CARTESIAN_POINT('',(64.9347049069018,256.22214694455,20.2213203435596)) ;
#96106 = CARTESIAN_POINT('',(63.4110039984262,256.12214694455,20.3213203435596)) ;
#96107 = CARTESIAN_POINT('',(64.9347049069018,256.12214694455,20.3213203435596)) ;
#96108 = CARTESIAN_POINT('Origin',(63.4110039984262,256.12214694455,20.2213203435596)) ;
#96109 = CARTESIAN_POINT('Origin',(63.4110039984262,256.12214694455,20.2213203435596)) ;
#96110 = CARTESIAN_POINT('',(63.3110039984262,255.82214694455,20.2213203435596)) ;
#96111 = CARTESIAN_POINT('',(63.3110039984262,256.12214694455,20.2213203435596)) ;
#96112 = CARTESIAN_POINT('',(63.4110039984262,255.92214694455,20.3213203435596)) ;
#96113 = CARTESIAN_POINT('',(63.4110039984262,256.12214694455,20.3213203435596)) ;
#96114 = CARTESIAN_POINT('Origin',(63.4110039984262,255.92214694455,20.2213203435596)) ;
#96115 = CARTESIAN_POINT('Origin',(64.1310039984262,255.92214694455,20.2213203435596)) ;
#96116 = CARTESIAN_POINT('',(64.1310039984262,255.82214694455,20.2213203435596)) ;
#96117 = CARTESIAN_POINT('',(64.1310039984262,255.92214694455,20.3213203435596)) ;
#96118 = CARTESIAN_POINT('Origin',(64.9184058153773,256.22214694455,20.0213203435596)) ;
#96119 = CARTESIAN_POINT('',(63.3110039984262,256.22214694455,20.1213203435596)) ;
#96120 = CARTESIAN_POINT('',(63.3110039984262,256.22214694455,20.0213203435596)) ;
#96121 = CARTESIAN_POINT('',(64.9184058153773,256.22214694455,20.1213203435596)) ;
#96122 = CARTESIAN_POINT('',(60.0662936149535,256.22214694455,20.1213203435596)) ;
#96123 = CARTESIAN_POINT('',(64.9184058153773,256.22214694455,20.0213203435596)) ;
#96124 = CARTESIAN_POINT('Origin',(63.3110039984262,256.22214694455,20.0213203435596)) ;
#96125 = CARTESIAN_POINT('',(63.3110039984262,255.82214694455,20.1213203435596)) ;
#96126 = CARTESIAN_POINT('',(63.3110039984262,255.82214694455,20.0213203435596)) ;
#96127 = CARTESIAN_POINT('',(63.3110039984262,248.469379137783,20.1213203435596)) ;
#96128 = CARTESIAN_POINT('Origin',(63.3110039984262,255.82214694455,20.0213203435596)) ;
#96129 = CARTESIAN_POINT('',(64.9184058153773,255.82214694455,20.1213203435596)) ;
#96130 = CARTESIAN_POINT('',(64.9184058153773,255.82214694455,20.0213203435596)) ;
#96131 = CARTESIAN_POINT('',(59.2625927064781,255.82214694455,20.1213203435596)) ;
#96132 = CARTESIAN_POINT('Origin',(64.9184058153773,255.82214694455,20.0213203435596)) ;
#96133 = CARTESIAN_POINT('',(64.9184058153773,255.34214694455,20.1213203435596)) ;
#96134 = CARTESIAN_POINT('',(64.9184058153773,255.34214694455,20.0213203435596)) ;
#96135 = CARTESIAN_POINT('',(64.9184058153773,248.269379137783,20.1213203435596)) ;
#96136 = CARTESIAN_POINT('Origin',(64.9510039984262,256.02214694455,20.3213203435596)) ;
#96137 = CARTESIAN_POINT('Origin',(62.6000000000001,255.12214694455,20.2213203435596)) ;
#96138 = CARTESIAN_POINT('',(62.6,255.12214694455,20.3213203435596)) ;
#96139 = CARTESIAN_POINT('',(62.8,255.12214694455,20.3213203435596)) ;
#96140 = CARTESIAN_POINT('',(62.6000000000001,255.12214694455,20.3213203435596)) ;
#96141 = CARTESIAN_POINT('',(62.9,255.02214694455,20.2213203435596)) ;
#96142 = CARTESIAN_POINT('Origin',(62.8,255.12214694455,20.2213203435596)) ;
#96143 = CARTESIAN_POINT('',(62.5,255.02214694455,20.2213203435596)) ;
#96144 = CARTESIAN_POINT('',(62.6000000000001,255.02214694455,20.2213203435596)) ;
#96145 = CARTESIAN_POINT('Origin',(62.6,255.12214694455,20.2213203435596)) ;
#96146 = CARTESIAN_POINT('Origin',(62.8,255.52214694455,20.2213203435596)) ;
#96147 = CARTESIAN_POINT('',(62.9,257.02214694455,20.2213203435596)) ;
#96148 = CARTESIAN_POINT('',(62.9,255.52214694455,20.2213203435596)) ;
#96149 = CARTESIAN_POINT('',(62.8,256.92214694455,20.3213203435596)) ;
#96150 = CARTESIAN_POINT('',(62.8,255.52214694455,20.3213203435596)) ;
#96151 = CARTESIAN_POINT('Origin',(62.8,256.92214694455,20.2213203435596)) ;
#96152 = CARTESIAN_POINT('Origin',(62.8,256.92214694455,20.2213203435596)) ;
#96153 = CARTESIAN_POINT('',(62.5,257.02214694455,20.2213203435596)) ;
#96154 = CARTESIAN_POINT('',(62.8,257.02214694455,20.2213203435596)) ;
#96155 = CARTESIAN_POINT('',(62.6,256.92214694455,20.3213203435596)) ;
#96156 = CARTESIAN_POINT('',(62.8,256.92214694455,20.3213203435596)) ;
#96157 = CARTESIAN_POINT('Origin',(62.6,256.92214694455,20.2213203435596)) ;
#96158 = CARTESIAN_POINT('Origin',(62.6,256.52214694455,20.2213203435596)) ;
#96159 = CARTESIAN_POINT('',(62.5,256.52214694455,20.2213203435596)) ;
#96160 = CARTESIAN_POINT('',(62.6,256.52214694455,20.3213203435596)) ;
#96161 = CARTESIAN_POINT('Origin',(62.5,257.02214694455,20.0213203435596)) ;
#96162 = CARTESIAN_POINT('',(62.5,255.02214694455,20.1213203435596)) ;
#96163 = CARTESIAN_POINT('',(62.5,255.02214694455,20.0213203435596)) ;
#96164 = CARTESIAN_POINT('',(62.5,257.02214694455,20.1213203435596)) ;
#96165 = CARTESIAN_POINT('',(62.5,248.869379137783,20.1213203435596)) ;
#96166 = CARTESIAN_POINT('',(62.5,257.02214694455,20.0213203435596)) ;
#96167 = CARTESIAN_POINT('Origin',(62.5,255.02214694455,20.0213203435596)) ;
#96168 = CARTESIAN_POINT('',(62.9,255.02214694455,20.1213203435596)) ;
#96169 = CARTESIAN_POINT('',(62.9,255.02214694455,20.0213203435596)) ;
#96170 = CARTESIAN_POINT('',(58.8570907072643,255.02214694455,20.1213203435596)) ;
#96171 = CARTESIAN_POINT('Origin',(62.7,256.02214694455,20.3213203435596)) ;
#96172 = CARTESIAN_POINT('Origin',(60.3815941846227,255.68214694455,20.2213203435596)) ;
#96173 = CARTESIAN_POINT('',(60.3815941846227,255.49075064338,20.3213203435596)) ;
#96174 = CARTESIAN_POINT('',(60.3815941846227,255.92214694455,20.3213203435596)) ;
#96175 = CARTESIAN_POINT('',(60.3815941846227,255.68214694455,20.3213203435596)) ;
#96176 = CARTESIAN_POINT('',(60.4815941846227,255.82214694455,20.2213203435596)) ;
#96177 = CARTESIAN_POINT('Origin',(60.3815941846227,255.92214694455,20.2213203435596)) ;
#96178 = CARTESIAN_POINT('',(60.4815941846227,255.34214694455,20.2213203435596)) ;
#96179 = CARTESIAN_POINT('',(60.4815941846227,255.68214694455,20.2213203435596)) ;
#96180 = CARTESIAN_POINT('Origin',(60.3815941846227,255.49075064338,20.2213203435596)) ;
#96181 = CARTESIAN_POINT('Origin',(60.4652950930983,255.92214694455,20.2213203435596)) ;
#96182 = CARTESIAN_POINT('',(61.9889960015738,255.92214694455,20.3213203435596)) ;
#96183 = CARTESIAN_POINT('',(60.4652950930983,255.92214694455,20.3213203435596)) ;
#96184 = CARTESIAN_POINT('',(62.0889960015738,255.82214694455,20.2213203435596)) ;
#96185 = CARTESIAN_POINT('Origin',(61.9889960015738,255.92214694455,20.2213203435596)) ;
#96186 = CARTESIAN_POINT('',(60.4652950930983,255.82214694455,20.2213203435596)) ;
#96187 = CARTESIAN_POINT('Origin',(61.9889960015738,255.92214694455,20.2213203435596)) ;
#96188 = CARTESIAN_POINT('',(61.9889960015738,256.12214694455,20.3213203435596)) ;
#96189 = CARTESIAN_POINT('',(61.9889960015738,255.92214694455,20.3213203435596)) ;
#96190 = CARTESIAN_POINT('',(62.0889960015738,256.22214694455,20.2213203435596)) ;
#96191 = CARTESIAN_POINT('Origin',(61.9889960015738,256.12214694455,20.2213203435596)) ;
#96192 = CARTESIAN_POINT('',(62.0889960015738,255.92214694455,20.2213203435596)) ;
#96193 = CARTESIAN_POINT('Origin',(61.2689960015738,256.12214694455,20.2213203435596)) ;
#96194 = CARTESIAN_POINT('',(60.4815941846227,256.22214694455,20.2213203435596)) ;
#96195 = CARTESIAN_POINT('',(61.2689960015738,256.22214694455,20.2213203435596)) ;
#96196 = CARTESIAN_POINT('',(60.3815941846227,256.12214694455,20.3213203435596)) ;
#96197 = CARTESIAN_POINT('',(61.2689960015738,256.12214694455,20.3213203435596)) ;
#96198 = CARTESIAN_POINT('Origin',(60.3815941846227,256.12214694455,20.2213203435596)) ;
#96199 = CARTESIAN_POINT('Origin',(60.3815941846227,256.12214694455,20.2213203435596)) ;
#96200 = CARTESIAN_POINT('',(60.4815941846227,256.70214694455,20.2213203435596)) ;
#96201 = CARTESIAN_POINT('',(60.4815941846227,256.12214694455,20.2213203435596)) ;
#96202 = CARTESIAN_POINT('',(60.3815941846227,256.55354324572,20.3213203435596)) ;
#96203 = CARTESIAN_POINT('',(60.3815941846227,256.12214694455,20.3213203435596)) ;
#96204 = CARTESIAN_POINT('Origin',(60.3815941846227,256.55354324572,20.2213203435596)) ;
#96205 = CARTESIAN_POINT('Origin',(60.3866471493538,256.555597544267,20.2213203435596)) ;
#96206 = CARTESIAN_POINT('',(58.8089960015738,256.02214694455,20.2213203435596)) ;
#96207 = CARTESIAN_POINT('',(60.348985344129,256.648234407487,20.2213203435596)) ;
#96208 = CARTESIAN_POINT('',(59.0745169966587,256.02214694455,20.3213203435596)) ;
#96209 = CARTESIAN_POINT('',(60.3866471493538,256.555597544267,20.3213203435596)) ;
#96210 = CARTESIAN_POINT('Origin',(59.0745169966587,256.02214694455,20.2213203435596)) ;
#96211 = CARTESIAN_POINT('Origin',(59.5503480578294,255.828696344833,20.2213203435596)) ;
#96212 = CARTESIAN_POINT('',(59.5126862526045,255.736059481613,20.2213203435596)) ;
#96213 = CARTESIAN_POINT('',(59.5503480578294,255.828696344833,20.3213203435596)) ;
#96214 = CARTESIAN_POINT('Origin',(60.4815941846227,256.22214694455,20.0213203435596)) ;
#96215 = CARTESIAN_POINT('',(60.4815941846227,256.70214694455,20.1213203435596)) ;
#96216 = CARTESIAN_POINT('',(60.4815941846227,256.70214694455,20.0213203435596)) ;
#96217 = CARTESIAN_POINT('',(60.4815941846227,256.22214694455,20.1213203435596)) ;
#96218 = CARTESIAN_POINT('',(60.4815941846227,248.469379137783,20.1213203435596)) ;
#96219 = CARTESIAN_POINT('',(60.4815941846227,256.22214694455,20.0213203435596)) ;
#96220 = CARTESIAN_POINT('Origin',(60.4815941846227,256.70214694455,20.0213203435596)) ;
#96221 = CARTESIAN_POINT('',(58.8089960015738,256.02214694455,20.1213203435596)) ;
#96222 = CARTESIAN_POINT('',(58.8089960015738,256.02214694455,20.0213203435596)) ;
#96223 = CARTESIAN_POINT('',(55.4328817810691,254.649577194559,20.1213203435596)) ;
#96224 = CARTESIAN_POINT('Origin',(58.8089960015738,256.02214694455,20.0213203435596)) ;
#96225 = CARTESIAN_POINT('',(60.4815941846227,255.34214694455,20.1213203435596)) ;
#96226 = CARTESIAN_POINT('',(60.4815941846227,255.34214694455,20.0213203435596)) ;
#96227 = CARTESIAN_POINT('',(59.9364873877912,255.563761810333,20.1213203435596)) ;
#96228 = CARTESIAN_POINT('Origin',(60.4815941846227,255.34214694455,20.0213203435596)) ;
#96229 = CARTESIAN_POINT('',(60.4815941846227,255.82214694455,20.1213203435596)) ;
#96230 = CARTESIAN_POINT('',(60.4815941846227,255.82214694455,20.0213203435596)) ;
#96231 = CARTESIAN_POINT('',(60.4815941846227,248.029379137783,20.1213203435596)) ;
#96232 = CARTESIAN_POINT('Origin',(60.4489960015738,256.02214694455,20.3213203435596)) ;
#96233 = CARTESIAN_POINT('Origin',(74.4283628290596,248.80334685842,18.2213203435596)) ;
#96234 = CARTESIAN_POINT('',(74.4283628290596,249.32834685842,18.3213203435596)) ;
#96235 = CARTESIAN_POINT('',(74.4283628290596,247.02834685842,18.3213203435596)) ;
#96236 = CARTESIAN_POINT('',(74.4283628290596,248.80334685842,18.3213203435596)) ;
#96237 = CARTESIAN_POINT('',(74.3283628290596,246.92834685842,18.2213203435596)) ;
#96238 = CARTESIAN_POINT('Origin',(74.4283628290596,247.02834685842,18.2213203435596)) ;
#96239 = CARTESIAN_POINT('',(74.3283628290596,249.42834685842,18.2213203435596)) ;
#96240 = CARTESIAN_POINT('',(74.3283628290596,248.80334685842,18.2213203435596)) ;
#96241 = CARTESIAN_POINT('Origin',(74.4283628290596,249.32834685842,18.2213203435596)) ;
#96242 = CARTESIAN_POINT('Origin',(74.4283628290596,247.02834685842,18.2213203435596)) ;
#96243 = CARTESIAN_POINT('',(74.7283628290596,246.92834685842,18.2213203435596)) ;
#96244 = CARTESIAN_POINT('',(74.4283628290596,246.92834685842,18.2213203435596)) ;
#96245 = CARTESIAN_POINT('',(74.6283628290596,247.02834685842,18.3213203435596)) ;
#96246 = CARTESIAN_POINT('',(74.4283628290596,247.02834685842,18.3213203435596)) ;
#96247 = CARTESIAN_POINT('Origin',(74.6283628290596,247.02834685842,18.2213203435596)) ;
#96248 = CARTESIAN_POINT('Origin',(74.6283628290596,247.55334685842,18.2213203435596)) ;
#96249 = CARTESIAN_POINT('',(74.7283628290596,249.42834685842,18.2213203435596)) ;
#96250 = CARTESIAN_POINT('',(74.7283628290596,247.55334685842,18.2213203435596)) ;
#96251 = CARTESIAN_POINT('',(74.6283628290596,249.32834685842,18.3213203435596)) ;
#96252 = CARTESIAN_POINT('',(74.6283628290596,247.55334685842,18.3213203435596)) ;
#96253 = CARTESIAN_POINT('Origin',(74.6283628290596,249.32834685842,18.2213203435596)) ;
#96254 = CARTESIAN_POINT('Origin',(74.6283628290596,249.32834685842,18.2213203435596)) ;
#96255 = CARTESIAN_POINT('',(74.6283628290596,249.42834685842,18.2213203435596)) ;
#96256 = CARTESIAN_POINT('',(74.6283628290596,249.32834685842,18.3213203435596)) ;
#96257 = CARTESIAN_POINT('Origin',(74.7283628290596,249.42834685842,18.0213203435596)) ;
#96258 = CARTESIAN_POINT('',(74.3283628290596,249.42834685842,18.1213203435596)) ;
#96259 = CARTESIAN_POINT('',(74.3283628290596,249.42834685842,18.0213203435596)) ;
#96260 = CARTESIAN_POINT('',(74.7283628290596,249.42834685842,18.1213203435596)) ;
#96261 = CARTESIAN_POINT('',(64.9712721217948,249.42834685842,18.1213203435596)) ;
#96262 = CARTESIAN_POINT('',(74.7283628290596,249.42834685842,18.0213203435596)) ;
#96263 = CARTESIAN_POINT('Origin',(74.3283628290596,249.42834685842,18.0213203435596)) ;
#96264 = CARTESIAN_POINT('',(74.3283628290596,246.92834685842,18.1213203435596)) ;
#96265 = CARTESIAN_POINT('',(74.3283628290596,246.92834685842,18.0213203435596)) ;
#96266 = CARTESIAN_POINT('',(74.3283628290596,249.23917342921,18.1213203435596)) ;
#96267 = CARTESIAN_POINT('Origin',(74.5283628290596,248.17834685842,18.3213203435596)) ;
#96268 = CARTESIAN_POINT('Origin',(76.9136449414663,247.288583115023,18.2213203435596)) ;
#96269 = CARTESIAN_POINT('',(76.7495157419148,246.884873995972,18.3213203435596)) ;
#96270 = CARTESIAN_POINT('',(77.2809120430846,248.191951183936,18.3213203435596)) ;
#96271 = CARTESIAN_POINT('',(76.9136449414663,247.288583115023,18.3213203435596)) ;
#96272 = CARTESIAN_POINT('',(77.4295157419147,248.291951183936,18.2213203435596)) ;
#96273 = CARTESIAN_POINT('Origin',(77.2809120430846,248.191951183936,18.2213203435596)) ;
#96274 = CARTESIAN_POINT('',(76.7495157419148,246.619353000887,18.2213203435596)) ;
#96275 = CARTESIAN_POINT('',(77.0062818046861,247.250921309799,18.2213203435596)) ;
#96276 = CARTESIAN_POINT('Origin',(76.7495157419148,246.884873995972,18.2213203435596)) ;
#96277 = CARTESIAN_POINT('Origin',(76.8191684028636,248.191951183936,18.2213203435596)) ;
#96278 = CARTESIAN_POINT('',(76.8348658990794,248.191951183936,18.3213203435596)) ;
#96279 = CARTESIAN_POINT('',(76.8191684028636,248.191951183936,18.3213203435596)) ;
#96280 = CARTESIAN_POINT('',(76.9348658990794,248.291951183936,18.2213203435596)) ;
#96281 = CARTESIAN_POINT('Origin',(76.8348658990794,248.191951183936,18.2213203435596)) ;
#96282 = CARTESIAN_POINT('',(76.8191684028636,248.291951183936,18.2213203435596)) ;
#96283 = CARTESIAN_POINT('Origin',(76.8348658990794,248.301519996331,18.2213203435596)) ;
#96284 = CARTESIAN_POINT('',(76.8348658990794,249.302824616567,18.3213203435596)) ;
#96285 = CARTESIAN_POINT('',(76.8348658990794,248.301519996331,18.3213203435596)) ;
#96286 = CARTESIAN_POINT('',(76.9348658990794,249.302824616567,18.2213203435596)) ;
#96287 = CARTESIAN_POINT('Origin',(76.8348658990794,249.302824616567,18.2213203435596)) ;
#96288 = CARTESIAN_POINT('',(76.9348658990794,248.301519996331,18.2213203435596)) ;
#96289 = CARTESIAN_POINT('Origin',(76.2348658990794,249.302824616567,18.2213203435596)) ;
#96290 = CARTESIAN_POINT('',(75.9152721256086,249.810623612193,18.3213203435596)) ;
#96291 = CARTESIAN_POINT('',(75.8620064966968,249.895256778131,18.2213203435596)) ;
#96292 = CARTESIAN_POINT('Origin',(75.9152721256086,249.810623612193,18.2213203435596)) ;
#96293 = CARTESIAN_POINT('Origin',(76.2348658990794,249.302824616567,18.2213203435596)) ;
#96294 = CARTESIAN_POINT('Origin',(76.2348658990794,249.302824616567,18.3213203435596)) ;
#96295 = CARTESIAN_POINT('Origin',(75.6824052881838,249.664064064164,18.2213203435596)) ;
#96296 = CARTESIAN_POINT('',(74.9881263857102,249.345262302685,18.2213203435596)) ;
#96297 = CARTESIAN_POINT('',(75.629139659272,249.748697230101,18.2213203435596)) ;
#96298 = CARTESIAN_POINT('',(75.1260251805597,249.313894765659,18.3213203435596)) ;
#96299 = CARTESIAN_POINT('',(75.6824052881838,249.664064064164,18.3213203435596)) ;
#96300 = CARTESIAN_POINT('Origin',(75.1260251805597,249.313894765659,18.2213203435596)) ;
#96301 = CARTESIAN_POINT('Origin',(75.4790336726305,248.753003494924,18.2213203435596)) ;
#96302 = CARTESIAN_POINT('',(75.2011889013574,249.006729638934,18.2213203435596)) ;
#96303 = CARTESIAN_POINT('',(75.3944005066928,248.699737866012,18.2213203435596)) ;
#96304 = CARTESIAN_POINT('',(75.2325564383833,249.144628433784,18.3213203435596)) ;
#96305 = CARTESIAN_POINT('',(75.4790336726305,248.753003494924,18.3213203435596)) ;
#96306 = CARTESIAN_POINT('Origin',(75.2325564383833,249.144628433784,18.2213203435596)) ;
#96307 = CARTESIAN_POINT('Origin',(75.3519964905142,249.219800494565,18.2213203435596)) ;
#96308 = CARTESIAN_POINT('',(76.0218033834322,249.641357280318,18.3213203435596)) ;
#96309 = CARTESIAN_POINT('',(75.3519964905142,249.219800494565,18.3213203435596)) ;
#96310 = CARTESIAN_POINT('',(76.075069012344,249.55672411438,18.2213203435596)) ;
#96311 = CARTESIAN_POINT('Origin',(76.0218033834322,249.641357280318,18.2213203435596)) ;
#96312 = CARTESIAN_POINT('',(75.405262119426,249.135167328628,18.2213203435596)) ;
#96313 = CARTESIAN_POINT('Origin',(76.2348658990794,249.302824616567,18.2213203435596)) ;
#96314 = CARTESIAN_POINT('',(76.6348658990794,249.302824616567,18.3213203435596)) ;
#96315 = CARTESIAN_POINT('',(76.5348658990794,249.302824616567,18.2213203435596)) ;
#96316 = CARTESIAN_POINT('Origin',(76.6348658990794,249.302824616567,18.2213203435596)) ;
#96317 = CARTESIAN_POINT('Origin',(76.2348658990794,249.302824616567,18.2213203435596)) ;
#96318 = CARTESIAN_POINT('Origin',(76.2348658990794,249.302824616567,18.3213203435596)) ;
#96319 = CARTESIAN_POINT('Origin',(76.6348658990794,248.806956712647,18.2213203435596)) ;
#96320 = CARTESIAN_POINT('',(76.5348658990794,248.291951183936,18.2213203435596)) ;
#96321 = CARTESIAN_POINT('',(76.5348658990794,248.806956712647,18.2213203435596)) ;
#96322 = CARTESIAN_POINT('',(76.6348658990794,248.191951183936,18.3213203435596)) ;
#96323 = CARTESIAN_POINT('',(76.6348658990794,248.806956712647,18.3213203435596)) ;
#96324 = CARTESIAN_POINT('Origin',(76.6348658990794,248.191951183936,18.2213203435596)) ;
#96325 = CARTESIAN_POINT('Origin',(76.3718434814459,248.191951183936,18.2213203435596)) ;
#96326 = CARTESIAN_POINT('',(76.0695157419148,248.291951183936,18.2213203435596)) ;
#96327 = CARTESIAN_POINT('',(76.3718434814459,248.291951183936,18.2213203435596)) ;
#96328 = CARTESIAN_POINT('',(76.218119440745,248.191951183936,18.3213203435596)) ;
#96329 = CARTESIAN_POINT('',(76.3718434814459,248.191951183936,18.3213203435596)) ;
#96330 = CARTESIAN_POINT('Origin',(76.218119440745,248.191951183936,18.2213203435596)) ;
#96331 = CARTESIAN_POINT('Origin',(76.1686937834863,248.313523631769,18.2213203435596)) ;
#96332 = CARTESIAN_POINT('',(76.0760569202665,248.275861826544,18.2213203435596)) ;
#96333 = CARTESIAN_POINT('',(76.1686937834863,248.313523631769,18.3213203435596)) ;
#96334 = CARTESIAN_POINT('Origin',(75.2011889013574,249.006729638934,18.0213203435596)) ;
#96335 = CARTESIAN_POINT('',(76.075069012344,249.55672411438,18.1213203435596)) ;
#96336 = CARTESIAN_POINT('',(76.075069012344,249.55672411438,18.0213203435596)) ;
#96337 = CARTESIAN_POINT('',(75.2011889013574,249.006729638934,18.1213203435596)) ;
#96338 = CARTESIAN_POINT('',(68.0528224690616,244.507757758468,18.1213203435596)) ;
#96339 = CARTESIAN_POINT('',(75.2011889013574,249.006729638934,18.0213203435596)) ;
#96340 = CARTESIAN_POINT('Origin',(76.2348658990794,249.302824616567,18.0213203435596)) ;
#96341 = CARTESIAN_POINT('',(76.5348658990794,249.302824616567,18.1213203435596)) ;
#96342 = CARTESIAN_POINT('',(76.5348658990794,249.302824616567,18.0213203435596)) ;
#96343 = CARTESIAN_POINT('Origin',(76.2348658990794,249.302824616567,18.1213203435596)) ;
#96344 = CARTESIAN_POINT('Origin',(76.5348658990794,249.302824616567,18.0213203435596)) ;
#96345 = CARTESIAN_POINT('',(76.5348658990794,248.291951183936,18.1213203435596)) ;
#96346 = CARTESIAN_POINT('',(76.5348658990794,248.291951183936,18.0213203435596)) ;
#96347 = CARTESIAN_POINT('',(76.5348658990794,249.176412308284,18.1213203435596)) ;
#96348 = CARTESIAN_POINT('Origin',(76.5348658990794,248.291951183936,18.0213203435596)) ;
#96349 = CARTESIAN_POINT('',(76.0695157419148,248.291951183936,18.1213203435596)) ;
#96350 = CARTESIAN_POINT('',(76.0695157419148,248.291951183936,18.0213203435596)) ;
#96351 = CARTESIAN_POINT('',(65.8745236568046,248.291951183936,18.1213203435596)) ;
#96352 = CARTESIAN_POINT('Origin',(76.0695157419148,248.291951183936,18.0213203435596)) ;
#96353 = CARTESIAN_POINT('',(76.7495157419148,246.619353000887,18.1213203435596)) ;
#96354 = CARTESIAN_POINT('',(76.7495157419148,246.619353000887,18.0213203435596)) ;
#96355 = CARTESIAN_POINT('',(74.4582066182201,252.255293408379,18.1213203435596)) ;
#96356 = CARTESIAN_POINT('Origin',(76.7495157419148,246.619353000887,18.0213203435596)) ;
#96357 = CARTESIAN_POINT('',(77.4295157419147,248.291951183936,18.1213203435596)) ;
#96358 = CARTESIAN_POINT('',(77.4295157419147,248.291951183936,18.0213203435596)) ;
#96359 = CARTESIAN_POINT('',(75.6462281222094,243.90559290074,18.1213203435596)) ;
#96360 = CARTESIAN_POINT('Origin',(76.2088210638125,248.311088808727,18.3213203435596)) ;
#96361 = CARTESIAN_POINT('Origin',(72.2290896109171,248.324963207434,18.2213203435596)) ;
#96362 = CARTESIAN_POINT('',(71.7673459706961,248.324963207434,18.3213203435596)) ;
#96363 = CARTESIAN_POINT('',(72.2133921147013,248.324963207434,18.3213203435596)) ;
#96364 = CARTESIAN_POINT('',(72.2290896109171,248.324963207434,18.3213203435596)) ;
#96365 = CARTESIAN_POINT('',(72.1133921147013,248.224963207434,18.2213203435596)) ;
#96366 = CARTESIAN_POINT('Origin',(72.2133921147013,248.324963207434,18.2213203435596)) ;
#96367 = CARTESIAN_POINT('',(71.618742271866,248.224963207434,18.2213203435596)) ;
#96368 = CARTESIAN_POINT('',(72.2290896109171,248.224963207434,18.2213203435596)) ;
#96369 = CARTESIAN_POINT('Origin',(71.7673459706961,248.324963207434,18.2213203435596)) ;
#96370 = CARTESIAN_POINT('Origin',(72.2133921147013,248.215394395038,18.2213203435596)) ;
#96371 = CARTESIAN_POINT('',(72.2133921147013,247.214089774802,18.3213203435596)) ;
#96372 = CARTESIAN_POINT('',(72.2133921147013,248.215394395038,18.3213203435596)) ;
#96373 = CARTESIAN_POINT('',(72.1133921147013,247.214089774802,18.2213203435596)) ;
#96374 = CARTESIAN_POINT('Origin',(72.2133921147013,247.214089774802,18.2213203435596)) ;
#96375 = CARTESIAN_POINT('',(72.1133921147013,248.215394395038,18.2213203435596)) ;
#96376 = CARTESIAN_POINT('Origin',(72.8133921147013,247.214089774802,18.2213203435596)) ;
#96377 = CARTESIAN_POINT('',(73.1329858881721,246.706290779176,18.3213203435596)) ;
#96378 = CARTESIAN_POINT('',(73.1862515170839,246.621657613239,18.2213203435596)) ;
#96379 = CARTESIAN_POINT('Origin',(73.1329858881721,246.706290779176,18.2213203435596)) ;
#96380 = CARTESIAN_POINT('Origin',(72.8133921147013,247.214089774802,18.2213203435596)) ;
#96381 = CARTESIAN_POINT('Origin',(72.8133921147013,247.214089774802,18.3213203435596)) ;
#96382 = CARTESIAN_POINT('Origin',(73.3658527255969,246.852850327206,18.2213203435596)) ;
#96383 = CARTESIAN_POINT('',(74.0601316280705,247.171652088685,18.2213203435596)) ;
#96384 = CARTESIAN_POINT('',(73.4191183545087,246.768217161268,18.2213203435596)) ;
#96385 = CARTESIAN_POINT('',(73.922232833221,247.203019625711,18.3213203435596)) ;
#96386 = CARTESIAN_POINT('',(73.3658527255969,246.852850327206,18.3213203435596)) ;
#96387 = CARTESIAN_POINT('Origin',(73.922232833221,247.203019625711,18.2213203435596)) ;
#96388 = CARTESIAN_POINT('Origin',(73.5692243411502,247.763910896445,18.2213203435596)) ;
#96389 = CARTESIAN_POINT('',(73.8157015753974,247.372285957586,18.3213203435596)) ;
#96390 = CARTESIAN_POINT('',(73.5692243411502,247.763910896445,18.3213203435596)) ;
#96391 = CARTESIAN_POINT('',(73.8470691124233,247.510184752435,18.2213203435596)) ;
#96392 = CARTESIAN_POINT('Origin',(73.8157015753974,247.372285957586,18.2213203435596)) ;
#96393 = CARTESIAN_POINT('',(73.6538575070879,247.817176525357,18.2213203435596)) ;
#96394 = CARTESIAN_POINT('Origin',(73.6962615232665,247.297113896804,18.2213203435596)) ;
#96395 = CARTESIAN_POINT('',(73.0264546303485,246.875557111052,18.3213203435596)) ;
#96396 = CARTESIAN_POINT('',(73.6962615232665,247.297113896804,18.3213203435596)) ;
#96397 = CARTESIAN_POINT('',(72.9731890014367,246.960190276989,18.2213203435596)) ;
#96398 = CARTESIAN_POINT('Origin',(73.0264546303485,246.875557111052,18.2213203435596)) ;
#96399 = CARTESIAN_POINT('',(73.6429958943547,247.381747062742,18.2213203435596)) ;
#96400 = CARTESIAN_POINT('Origin',(72.8133921147013,247.214089774802,18.2213203435596)) ;
#96401 = CARTESIAN_POINT('',(72.4133921147013,247.214089774802,18.3213203435596)) ;
#96402 = CARTESIAN_POINT('',(72.5133921147013,247.214089774802,18.2213203435596)) ;
#96403 = CARTESIAN_POINT('Origin',(72.4133921147013,247.214089774802,18.2213203435596)) ;
#96404 = CARTESIAN_POINT('Origin',(72.8133921147013,247.214089774802,18.2213203435596)) ;
#96405 = CARTESIAN_POINT('Origin',(72.8133921147013,247.214089774802,18.3213203435596)) ;
#96406 = CARTESIAN_POINT('Origin',(72.4133921147013,247.709957678722,18.2213203435596)) ;
#96407 = CARTESIAN_POINT('',(72.5133921147013,248.224963207434,18.2213203435596)) ;
#96408 = CARTESIAN_POINT('',(72.5133921147013,247.709957678722,18.2213203435596)) ;
#96409 = CARTESIAN_POINT('',(72.4133921147013,248.324963207434,18.3213203435596)) ;
#96410 = CARTESIAN_POINT('',(72.4133921147013,247.709957678722,18.3213203435596)) ;
#96411 = CARTESIAN_POINT('Origin',(72.4133921147013,248.324963207434,18.2213203435596)) ;
#96412 = CARTESIAN_POINT('Origin',(72.6764145323348,248.324963207434,18.2213203435596)) ;
#96413 = CARTESIAN_POINT('',(72.9787422718659,248.224963207434,18.2213203435596)) ;
#96414 = CARTESIAN_POINT('',(72.6764145323348,248.224963207434,18.2213203435596)) ;
#96415 = CARTESIAN_POINT('',(72.8301385730357,248.324963207434,18.3213203435596)) ;
#96416 = CARTESIAN_POINT('',(72.6764145323348,248.324963207434,18.3213203435596)) ;
#96417 = CARTESIAN_POINT('Origin',(72.8301385730357,248.324963207434,18.2213203435596)) ;
#96418 = CARTESIAN_POINT('Origin',(72.8795642302944,248.2033907596,18.2213203435596)) ;
#96419 = CARTESIAN_POINT('',(72.2987422718658,249.897561390483,18.2213203435596)) ;
#96420 = CARTESIAN_POINT('',(72.9722010935142,248.241052564825,18.2213203435596)) ;
#96421 = CARTESIAN_POINT('',(72.2987422718659,249.632040395398,18.3213203435596)) ;
#96422 = CARTESIAN_POINT('',(72.8795642302944,248.2033907596,18.3213203435596)) ;
#96423 = CARTESIAN_POINT('Origin',(72.2987422718659,249.632040395398,18.2213203435596)) ;
#96424 = CARTESIAN_POINT('Origin',(72.1346130723144,249.228331276346,18.2213203435596)) ;
#96425 = CARTESIAN_POINT('',(72.0419762090946,249.265993081571,18.2213203435596)) ;
#96426 = CARTESIAN_POINT('',(72.1346130723144,249.228331276346,18.3213203435596)) ;
#96427 = CARTESIAN_POINT('Origin',(72.8133921147013,247.214089774802,18.0213203435596)) ;
#96428 = CARTESIAN_POINT('',(72.5133921147013,247.214089774802,18.1213203435596)) ;
#96429 = CARTESIAN_POINT('',(72.5133921147013,247.214089774802,18.0213203435596)) ;
#96430 = CARTESIAN_POINT('',(72.9731890014367,246.960190276989,18.1213203435596)) ;
#96431 = CARTESIAN_POINT('Origin',(72.8133921147013,247.214089774802,18.1213203435596)) ;
#96432 = CARTESIAN_POINT('',(72.9731890014367,246.960190276989,18.0213203435596)) ;
#96433 = CARTESIAN_POINT('Origin',(72.5133921147013,247.214089774802,18.0213203435596)) ;
#96434 = CARTESIAN_POINT('',(72.5133921147013,248.224963207434,18.1213203435596)) ;
#96435 = CARTESIAN_POINT('',(72.5133921147013,248.224963207434,18.0213203435596)) ;
#96436 = CARTESIAN_POINT('',(72.5133921147013,248.132044887401,18.1213203435596)) ;
#96437 = CARTESIAN_POINT('Origin',(72.5133921147013,248.224963207434,18.0213203435596)) ;
#96438 = CARTESIAN_POINT('',(72.9787422718659,248.224963207434,18.1213203435596)) ;
#96439 = CARTESIAN_POINT('',(72.9787422718659,248.224963207434,18.0213203435596)) ;
#96440 = CARTESIAN_POINT('',(63.8637867646156,248.224963207434,18.1213203435596)) ;
#96441 = CARTESIAN_POINT('Origin',(72.9787422718659,248.224963207434,18.0213203435596)) ;
#96442 = CARTESIAN_POINT('',(72.2987422718658,249.897561390483,18.1213203435596)) ;
#96443 = CARTESIAN_POINT('',(72.2987422718658,249.897561390483,18.0213203435596)) ;
#96444 = CARTESIAN_POINT('',(71.5749469690114,251.677883020562,18.1213203435596)) ;
#96445 = CARTESIAN_POINT('Origin',(72.2987422718659,249.897561390483,18.0213203435596)) ;
#96446 = CARTESIAN_POINT('',(71.618742271866,248.224963207434,18.1213203435596)) ;
#96447 = CARTESIAN_POINT('',(71.618742271866,248.224963207434,18.0213203435596)) ;
#96448 = CARTESIAN_POINT('',(70.9392436911016,246.553598366889,18.1213203435596)) ;
#96449 = CARTESIAN_POINT('Origin',(71.618742271866,248.224963207434,18.0213203435596)) ;
#96450 = CARTESIAN_POINT('',(72.1133921147013,248.224963207434,18.1213203435596)) ;
#96451 = CARTESIAN_POINT('',(72.1133921147013,248.224963207434,18.0213203435596)) ;
#96452 = CARTESIAN_POINT('',(63.416461843198,248.224963207434,18.1213203435596)) ;
#96453 = CARTESIAN_POINT('Origin',(72.8394369499682,248.205825582643,18.3213203435596)) ;
#96454 = CARTESIAN_POINT('Ctrl Pts',(31.8391836130391,258.138878696195,20.1213203435596)) ;
#96455 = CARTESIAN_POINT('Ctrl Pts',(31.8088277838837,258.075317586011,20.1213203435596)) ;
#96456 = CARTESIAN_POINT('Ctrl Pts',(31.7480710314216,257.948103917433,20.1213203435577)) ;
#96457 = CARTESIAN_POINT('Ctrl Pts',(31.65807074167,257.757060544542,20.1213203435576)) ;
#96458 = CARTESIAN_POINT('Ctrl Pts',(31.5846672172411,257.598364328898,20.1213203435568)) ;
#96459 = CARTESIAN_POINT('Ctrl Pts',(31.5398429295626,257.500340825891,20.1213203435565)) ;
#96460 = CARTESIAN_POINT('Ctrl Pts',(31.5232414331806,257.464149039576,20.1213203435565)) ;
#96461 = CARTESIAN_POINT('Ctrl Pts',(31.5204692836011,257.458111769045,20.1213203435565)) ;
#96462 = CARTESIAN_POINT('Ctrl Pts',(31.5176945388745,257.45207046735,20.1213203435565)) ;
#96463 = CARTESIAN_POINT('Ctrl Pts',(31.5121271696917,257.43997576795,20.1213203435565)) ;
#96464 = CARTESIAN_POINT('Ctrl Pts',(31.5000486151333,257.413723558212,20.1213203435565)) ;
#96465 = CARTESIAN_POINT('Ctrl Pts',(31.4733366583784,257.356758147137,20.1213203435566)) ;
#96466 = CARTESIAN_POINT('Ctrl Pts',(31.4411791361222,257.290450232183,20.1213203435566)) ;
#96467 = CARTESIAN_POINT('Ctrl Pts',(31.4018882564612,257.224550414268,20.1213203435566)) ;
#96468 = CARTESIAN_POINT('Ctrl Pts',(31.3743956554151,257.188936944183,20.1213203435566)) ;
#96469 = CARTESIAN_POINT('Ctrl Pts',(31.3560237927364,257.170047934177,20.1213203435566)) ;
#96470 = CARTESIAN_POINT('Ctrl Pts',(31.311584729612,257.127602179568,20.1213203435567)) ;
#96471 = CARTESIAN_POINT('Ctrl Pts',(31.2152044538023,257.0849023214,20.121320343557)) ;
#96472 = CARTESIAN_POINT('Ctrl Pts',(31.0594322135369,257.058857932597,20.1213203435571)) ;
#96473 = CARTESIAN_POINT('Ctrl Pts',(30.9440458722358,257.056950442841,20.1213203435596)) ;
#96474 = CARTESIAN_POINT('Ctrl Pts',(30.8368060688104,257.061456316934,20.1213203435596)) ;
#96475 = CARTESIAN_POINT('Ctrl Pts',(30.8035021201096,257.06285564251,20.1213203435596)) ;
#96476 = CARTESIAN_POINT('Ctrl Pts',(30.7701981714089,257.064254968086,20.1213203435596)) ;
#96477 = CARTESIAN_POINT('Ctrl Pts',(31.8391836130391,258.138878696195,20.1063603785425)) ;
#96478 = CARTESIAN_POINT('Ctrl Pts',(31.8088277838837,258.075317586011,20.1063603785425)) ;
#96479 = CARTESIAN_POINT('Ctrl Pts',(31.7480710314216,257.948103917433,20.1063603785406)) ;
#96480 = CARTESIAN_POINT('Ctrl Pts',(31.65807074167,257.757060544542,20.1063603785405)) ;
#96481 = CARTESIAN_POINT('Ctrl Pts',(31.5846672172411,257.598364328898,20.1063603785397)) ;
#96482 = CARTESIAN_POINT('Ctrl Pts',(31.5398429295626,257.500340825891,20.1063603785394)) ;
#96483 = CARTESIAN_POINT('Ctrl Pts',(31.5232414331806,257.464149039576,20.1063603785394)) ;
#96484 = CARTESIAN_POINT('Ctrl Pts',(31.5204692836011,257.458111769045,20.1063603785394)) ;
#96485 = CARTESIAN_POINT('Ctrl Pts',(31.5176945388745,257.45207046735,20.1063603785394)) ;
#96486 = CARTESIAN_POINT('Ctrl Pts',(31.5121271696917,257.43997576795,20.1063603785394)) ;
#96487 = CARTESIAN_POINT('Ctrl Pts',(31.5000486151333,257.413723558212,20.1063603785394)) ;
#96488 = CARTESIAN_POINT('Ctrl Pts',(31.4733366583784,257.356758147137,20.1063603785395)) ;
#96489 = CARTESIAN_POINT('Ctrl Pts',(31.4411791361222,257.290450232183,20.1063603785395)) ;
#96490 = CARTESIAN_POINT('Ctrl Pts',(31.4018882564612,257.224550414268,20.1063603785395)) ;
#96491 = CARTESIAN_POINT('Ctrl Pts',(31.3743956554151,257.188936944183,20.1063603785395)) ;
#96492 = CARTESIAN_POINT('Ctrl Pts',(31.3560237927364,257.170047934177,20.1063603785395)) ;
#96493 = CARTESIAN_POINT('Ctrl Pts',(31.311584729612,257.127602179568,20.1063603785396)) ;
#96494 = CARTESIAN_POINT('Ctrl Pts',(31.2152044538023,257.0849023214,20.1063603785399)) ;
#96495 = CARTESIAN_POINT('Ctrl Pts',(31.0594322135369,257.058857932597,20.10636037854)) ;
#96496 = CARTESIAN_POINT('Ctrl Pts',(30.9440458722358,257.056950442841,20.1063603785425)) ;
#96497 = CARTESIAN_POINT('Ctrl Pts',(30.8368060688104,257.061456316934,20.1063603785425)) ;
#96498 = CARTESIAN_POINT('Ctrl Pts',(30.8035021201096,257.06285564251,20.1063603785425)) ;
#96499 = CARTESIAN_POINT('Ctrl Pts',(30.7701981714089,257.064254968086,20.1063603785425)) ;
#96500 = CARTESIAN_POINT('Ctrl Pts',(31.8330058570152,258.141829099451,20.0764990828381)) ;
#96501 = CARTESIAN_POINT('Ctrl Pts',(31.8026486089796,258.07826500619,20.0764990828381)) ;
#96502 = CARTESIAN_POINT('Ctrl Pts',(31.7419443110348,257.951087199869,20.0764990828362)) ;
#96503 = CARTESIAN_POINT('Ctrl Pts',(31.6519283830522,257.760006830989,20.0764990828361)) ;
#96504 = CARTESIAN_POINT('Ctrl Pts',(31.5785318221264,257.601292622869,20.0764990828353)) ;
#96505 = CARTESIAN_POINT('Ctrl Pts',(31.5337121585615,257.503266786335,20.076499082835)) ;
#96506 = CARTESIAN_POINT('Ctrl Pts',(31.5171153568792,257.467084414751,20.076499082835)) ;
#96507 = CARTESIAN_POINT('Ctrl Pts',(31.5143435056701,257.461047860026,20.076499082835)) ;
#96508 = CARTESIAN_POINT('Ctrl Pts',(31.5115709052337,257.455011047666,20.076499082835)) ;
#96509 = CARTESIAN_POINT('Ctrl Pts',(31.5060037126059,257.442916481506,20.076499082835)) ;
#96510 = CARTESIAN_POINT('Ctrl Pts',(31.4939343137359,257.416686125584,20.076499082835)) ;
#96511 = CARTESIAN_POINT('Ctrl Pts',(31.4672601801766,257.359787112992,20.0764990828351)) ;
#96512 = CARTESIAN_POINT('Ctrl Pts',(31.4351804253194,257.293668828372,20.0764990828351)) ;
#96513 = CARTESIAN_POINT('Ctrl Pts',(31.396265321692,257.228410794591,20.0764990828351)) ;
#96514 = CARTESIAN_POINT('Ctrl Pts',(31.3692366359014,257.193442400304,20.0764990828351)) ;
#96515 = CARTESIAN_POINT('Ctrl Pts',(31.3513485240157,257.175019065014,20.0764990828351)) ;
#96516 = CARTESIAN_POINT('Ctrl Pts',(31.3072749058674,257.133136091133,20.0764990828352)) ;
#96517 = CARTESIAN_POINT('Ctrl Pts',(31.213617844106,257.091685982779,20.0764990828355)) ;
#96518 = CARTESIAN_POINT('Ctrl Pts',(31.0583683718114,257.065331495388,20.0764990828356)) ;
#96519 = CARTESIAN_POINT('Ctrl Pts',(30.9439706532423,257.063749482234,20.0764990828381)) ;
#96520 = CARTESIAN_POINT('Ctrl Pts',(30.8370934679167,257.068296415663,20.0764990828381)) ;
#96521 = CARTESIAN_POINT('Ctrl Pts',(30.8037895192159,257.069695741239,20.0764990828381)) ;
#96522 = CARTESIAN_POINT('Ctrl Pts',(30.7704855705151,257.071095066814,20.0764990828381)) ;
#96523 = CARTESIAN_POINT('Ctrl Pts',(31.8028168586867,258.156246910483,20.0344443101957)) ;
#96524 = CARTESIAN_POINT('Ctrl Pts',(31.7724543635431,258.09267184256,20.0344443101957)) ;
#96525 = CARTESIAN_POINT('Ctrl Pts',(31.7117274582361,257.965437861777,20.0344443101938)) ;
#96526 = CARTESIAN_POINT('Ctrl Pts',(31.6216226089589,257.774168684096,20.0344443101937)) ;
#96527 = CARTESIAN_POINT('Ctrl Pts',(31.5481401064261,257.61526448649,20.0344443101928)) ;
#96528 = CARTESIAN_POINT('Ctrl Pts',(31.5032980635907,257.517187990573,20.0344443101925)) ;
#96529 = CARTESIAN_POINT('Ctrl Pts',(31.4867204866751,257.481047583487,20.0344443101925)) ;
#96530 = CARTESIAN_POINT('Ctrl Pts',(31.4839532755492,257.475020977491,20.0344443101925)) ;
#96531 = CARTESIAN_POINT('Ctrl Pts',(31.481184083603,257.468991878312,20.0344443101925)) ;
#96532 = CARTESIAN_POINT('Ctrl Pts',(31.4756312639653,257.456927791243,20.0344443101925)) ;
#96533 = CARTESIAN_POINT('Ctrl Pts',(31.4635882182489,257.430757014838,20.0344443101926)) ;
#96534 = CARTESIAN_POINT('Ctrl Pts',(31.4370819739745,257.374207932902,20.0344443101926)) ;
#96535 = CARTESIAN_POINT('Ctrl Pts',(31.4054356385254,257.309033959787,20.0344443101926)) ;
#96536 = CARTESIAN_POINT('Ctrl Pts',(31.3682814586617,257.246889338311,20.0344443101927)) ;
#96537 = CARTESIAN_POINT('Ctrl Pts',(31.3436676842271,257.215113947874,20.0344443101927)) ;
#96538 = CARTESIAN_POINT('Ctrl Pts',(31.3277407164849,257.198755573123,20.0344443101927)) ;
#96539 = CARTESIAN_POINT('Ctrl Pts',(31.2896573479193,257.162323560542,20.0344443101927)) ;
#96540 = CARTESIAN_POINT('Ctrl Pts',(31.2049490971881,257.124329856327,20.034444310193)) ;
#96541 = CARTESIAN_POINT('Ctrl Pts',(31.0560063868325,257.098725310413,20.0344443101932)) ;
#96542 = CARTESIAN_POINT('Ctrl Pts',(30.944318021254,257.097275702916,20.0344443101957)) ;
#96543 = CARTESIAN_POINT('Ctrl Pts',(30.838497908478,257.101722101022,20.0344443101957)) ;
#96544 = CARTESIAN_POINT('Ctrl Pts',(30.8051939597772,257.103121426598,20.0344443101956)) ;
#96545 = CARTESIAN_POINT('Ctrl Pts',(30.7718900110764,257.104520752174,20.0344443101956)) ;
#96546 = CARTESIAN_POINT('Ctrl Pts',(31.7691956328132,258.17230390171,20.0213203435596)) ;
#96547 = CARTESIAN_POINT('Ctrl Pts',(31.7388267566149,258.108715463427,20.0213203435596)) ;
#96548 = CARTESIAN_POINT('Ctrl Pts',(31.6781635524218,257.981492660641,20.0213203435577)) ;
#96549 = CARTESIAN_POINT('Ctrl Pts',(31.5879636556681,257.790015763526,20.0213203435576)) ;
#96550 = CARTESIAN_POINT('Ctrl Pts',(31.5144236671445,257.630932497549,20.0213203435568)) ;
#96551 = CARTESIAN_POINT('Ctrl Pts',(31.4695710315332,257.532812090972,20.0213203435565)) ;
#96552 = CARTESIAN_POINT('Ctrl Pts',(31.4530160494117,257.496719707522,20.0213203435565)) ;
#96553 = CARTESIAN_POINT('Ctrl Pts',(31.4502529920088,257.490702125912,20.0213203435565)) ;
#96554 = CARTESIAN_POINT('Ctrl Pts',(31.4474898488209,257.484686149371,20.0213203435565)) ;
#96555 = CARTESIAN_POINT('Ctrl Pts',(31.4419487314663,257.47264650244,20.0213203435565)) ;
#96556 = CARTESIAN_POINT('Ctrl Pts',(31.4299408940992,257.446557123162,20.0213203435565)) ;
#96557 = CARTESIAN_POINT('Ctrl Pts',(31.4036270250294,257.390389643748,20.0213203435566)) ;
#96558 = CARTESIAN_POINT('Ctrl Pts',(31.3724463727691,257.326261721467,20.0213203435566)) ;
#96559 = CARTESIAN_POINT('Ctrl Pts',(31.3372773403256,257.267591748504,20.0213203435566)) ;
#96560 = CARTESIAN_POINT('Ctrl Pts',(31.3153059108559,257.239359411903,20.0213203435566)) ;
#96561 = CARTESIAN_POINT('Ctrl Pts',(31.3016914016871,257.225367890183,20.0213203435566)) ;
#96562 = CARTESIAN_POINT('Ctrl Pts',(31.2689396577891,257.194146001655,20.0213203435567)) ;
#96563 = CARTESIAN_POINT('Ctrl Pts',(31.1955864715343,257.160846289167,20.021320343557)) ;
#96564 = CARTESIAN_POINT('Ctrl Pts',(31.0524719945826,257.135355146069,20.0213203435571)) ;
#96565 = CARTESIAN_POINT('Ctrl Pts',(30.9444770781476,257.134517598386,20.0213203435596)) ;
#96566 = CARTESIAN_POINT('Ctrl Pts',(30.8400620217627,257.138947997199,20.0213203435596)) ;
#96567 = CARTESIAN_POINT('Ctrl Pts',(30.8067580730619,257.140347322774,20.0213203435596)) ;
#96568 = CARTESIAN_POINT('Ctrl Pts',(30.7734541243611,257.14174664835,20.0213203435596)) ;
#96569 = CARTESIAN_POINT('Ctrl Pts',(31.7489464638971,258.181974599884,20.0213203435596)) ;
#96570 = CARTESIAN_POINT('Ctrl Pts',(31.7185740965757,258.118378860957,20.0213203435596)) ;
#96571 = CARTESIAN_POINT('Ctrl Pts',(31.6578910386864,257.991114488338,20.0213203435577)) ;
#96572 = CARTESIAN_POINT('Ctrl Pts',(31.567631288081,257.79951081352,20.0213203435576)) ;
#96573 = CARTESIAN_POINT('Ctrl Pts',(31.4940316374113,257.640298396679,20.0213203435568)) ;
#96574 = CARTESIAN_POINT('Ctrl Pts',(31.449163234782,257.542143350465,20.0213203435565)) ;
#96575 = CARTESIAN_POINT('Ctrl Pts',(31.4326210851137,257.506079046589,20.0213203435565)) ;
#96576 = CARTESIAN_POINT('Ctrl Pts',(31.4298611935316,257.500068246514,20.0213203435565)) ;
#96577 = CARTESIAN_POINT('Ctrl Pts',(31.4271002177055,257.494057204395,20.0213203435565)) ;
#96578 = CARTESIAN_POINT('Ctrl Pts',(31.4215689681375,257.482038502719,20.0213203435565)) ;
#96579 = CARTESIAN_POINT('Ctrl Pts',(31.4095784978925,257.455988292376,20.0213203435565)) ;
#96580 = CARTESIAN_POINT('Ctrl Pts',(31.3833769551383,257.400055955828,20.0213203435566)) ;
#96581 = CARTESIAN_POINT('Ctrl Pts',(31.352487915175,257.336561723898,20.0213203435566)) ;
#96582 = CARTESIAN_POINT('Ctrl Pts',(31.318498748845,257.279979678226,20.0213203435566)) ;
#96583 = CARTESIAN_POINT('Ctrl Pts',(31.2981495994694,257.253889722425,20.0213203435566)) ;
#96584 = CARTESIAN_POINT('Ctrl Pts',(31.2858437484895,257.241279724063,20.0213203435566)) ;
#96585 = CARTESIAN_POINT('Ctrl Pts',(31.2571806346872,257.213759459052,20.0213203435567)) ;
#96586 = CARTESIAN_POINT('Ctrl Pts',(31.1897565474607,257.182733549511,20.021320343557)) ;
#96587 = CARTESIAN_POINT('Ctrl Pts',(31.0509353958286,257.157783514541,20.0213203435571)) ;
#96588 = CARTESIAN_POINT('Ctrl Pts',(30.9447220946478,257.157010261813,20.0213203435596)) ;
#96589 = CARTESIAN_POINT('Ctrl Pts',(30.8410040455373,257.161368163036,20.0213203435596)) ;
#96590 = CARTESIAN_POINT('Ctrl Pts',(30.8077000968365,257.162767488612,20.0213203435596)) ;
#96591 = CARTESIAN_POINT('Ctrl Pts',(30.7743961481358,257.164166814187,20.0213203435596)) ;
#96592 = CARTESIAN_POINT('Ctrl Pts',(31.7054902563519,258.090883140368,20.0213203435591)) ;
#96593 = CARTESIAN_POINT('Ctrl Pts',(31.7058154780415,258.091003801209,20.0213203435591)) ;
#96594 = CARTESIAN_POINT('Ctrl Pts',(31.7061407247937,258.091124403856,20.021321257223)) ;
#96595 = CARTESIAN_POINT('Ctrl Pts',(31.7217810369761,258.09692067528,20.0214090781983)) ;
#96596 = CARTESIAN_POINT('Ctrl Pts',(31.7372849566914,258.102510036199,20.0235188735263)) ;
#96597 = CARTESIAN_POINT('Ctrl Pts',(31.7660644064492,258.112763058849,20.0315488691178)) ;
#96598 = CARTESIAN_POINT('Ctrl Pts',(31.7797833584836,258.117595557464,20.0373252655719)) ;
#96599 = CARTESIAN_POINT('Ctrl Pts',(31.8050910283457,258.126663582567,20.0534375111736)) ;
#96600 = CARTESIAN_POINT('Ctrl Pts',(31.8158319004194,258.130527723509,20.0634821410784)) ;
#96601 = CARTESIAN_POINT('Ctrl Pts',(31.8286405478397,258.135110091431,20.0816547245696)) ;
#96602 = CARTESIAN_POINT('Ctrl Pts',(31.8325699408238,258.1365240484,20.0892046448113)) ;
#96603 = CARTESIAN_POINT('Ctrl Pts',(31.8378194809002,258.138400800961,20.1050586526148)) ;
#96604 = CARTESIAN_POINT('Ctrl Pts',(31.8391836130392,258.138878696195,20.1131223643512)) ;
#96605 = CARTESIAN_POINT('Ctrl Pts',(31.8391836130392,258.138878696195,20.1213203435596)) ;
#96606 = CARTESIAN_POINT('',(30.8701100175112,257.060056991359,20.1213203435596)) ;
#96607 = CARTESIAN_POINT('Ctrl Pts',(31.8391836130389,258.138878696195,20.1213203435596)) ;
#96608 = CARTESIAN_POINT('Ctrl Pts',(31.8161947094271,258.090742958311,20.1213203435596)) ;
#96609 = CARTESIAN_POINT('Ctrl Pts',(31.793311036054,258.042524781297,20.1213203435591)) ;
#96610 = CARTESIAN_POINT('Ctrl Pts',(31.7705219542047,257.994277738389,20.1213203435586)) ;
#96611 = CARTESIAN_POINT('Ctrl Pts',(31.763219062687,257.978816697759,20.1213203435584)) ;
#96612 = CARTESIAN_POINT('Ctrl Pts',(31.7559258446855,257.963352350932,20.1213203435583)) ;
#96613 = CARTESIAN_POINT('Ctrl Pts',(31.7486423864986,257.947886769573,20.1213203435582)) ;
#96614 = CARTESIAN_POINT('Ctrl Pts',(31.7336364378791,257.916023372641,20.1213203435579)) ;
#96615 = CARTESIAN_POINT('Ctrl Pts',(31.7186788666546,257.884169716522,20.1213203435578)) ;
#96616 = CARTESIAN_POINT('Ctrl Pts',(31.7037592987293,257.852317706678,20.1213203435577)) ;
#96617 = CARTESIAN_POINT('Ctrl Pts',(31.6909614196972,257.824995322347,20.1213203435576)) ;
#96618 = CARTESIAN_POINT('Ctrl Pts',(31.6781912970159,257.797673558857,20.1213203435576)) ;
#96619 = CARTESIAN_POINT('Ctrl Pts',(31.6654605313248,257.770384692618,20.1213203435575)) ;
#96620 = CARTESIAN_POINT('Ctrl Pts',(31.6633499687775,257.765860623882,20.1213203435575)) ;
#96621 = CARTESIAN_POINT('Ctrl Pts',(31.6612405375509,257.761337564344,20.1213203435575)) ;
#96622 = CARTESIAN_POINT('Ctrl Pts',(31.6591323537695,257.756815795697,20.1213203435575)) ;
#96623 = CARTESIAN_POINT('Ctrl Pts',(31.6493305524312,257.735792259531,20.1213203435574)) ;
#96624 = CARTESIAN_POINT('Ctrl Pts',(31.6395692606201,257.714825762861,20.1213203435573)) ;
#96625 = CARTESIAN_POINT('Ctrl Pts',(31.6298125740882,257.693842295384,20.1213203435572)) ;
#96626 = CARTESIAN_POINT('Ctrl Pts',(31.6207074593623,257.67426014748,20.1213203435572)) ;
#96627 = CARTESIAN_POINT('Ctrl Pts',(31.6116061277011,257.654662670896,20.1213203435571)) ;
#96628 = CARTESIAN_POINT('Ctrl Pts',(31.6024983920955,257.6350301264,20.121320343557)) ;
#96629 = CARTESIAN_POINT('Ctrl Pts',(31.5941252568093,257.616981079064,20.1213203435569)) ;
#96630 = CARTESIAN_POINT('Ctrl Pts',(31.5857465930023,257.598902102712,20.1213203435568)) ;
#96631 = CARTESIAN_POINT('Ctrl Pts',(31.5773733235883,257.580818658925,20.1213203435568)) ;
#96632 = CARTESIAN_POINT('Ctrl Pts',(31.5750924224581,257.575892680155,20.1213203435568)) ;
#96633 = CARTESIAN_POINT('Ctrl Pts',(31.5728120430202,257.57096663462,20.1213203435567)) ;
#96634 = CARTESIAN_POINT('Ctrl Pts',(31.5705326966186,257.566041672035,20.1213203435567)) ;
#96635 = CARTESIAN_POINT('Ctrl Pts',(31.5639474099359,257.551812904305,20.1213203435567)) ;
#96636 = CARTESIAN_POINT('Ctrl Pts',(31.5573679174951,257.537587063929,20.1213203435566)) ;
#96637 = CARTESIAN_POINT('Ctrl Pts',(31.5507742308301,257.523322084297,20.1213203435566)) ;
#96638 = CARTESIAN_POINT('Ctrl Pts',(31.5446786159545,257.510134648123,20.1213203435565)) ;
#96639 = CARTESIAN_POINT('Ctrl Pts',(31.5385707666793,257.496913509859,20.1213203435565)) ;
#96640 = CARTESIAN_POINT('Ctrl Pts',(31.532453652466,257.483666271913,20.1213203435565)) ;
#96641 = CARTESIAN_POINT('Ctrl Pts',(31.5303660108531,257.479145269978,20.1213203435565)) ;
#96642 = CARTESIAN_POINT('Ctrl Pts',(31.5282774683563,257.474621617872,20.1213203435565)) ;
#96643 = CARTESIAN_POINT('Ctrl Pts',(31.5261887405501,257.470096927279,20.1213203435565)) ;
#96644 = CARTESIAN_POINT('Ctrl Pts',(31.5252619024114,257.468089171268,20.1213203435565)) ;
#96645 = CARTESIAN_POINT('Ctrl Pts',(31.5243348062921,257.466080731128,20.1213203435565)) ;
#96646 = CARTESIAN_POINT('Ctrl Pts',(31.5234072657788,257.464071208821,20.1213203435565)) ;
#96647 = CARTESIAN_POINT('Ctrl Pts',(31.5206246442389,257.458042641898,20.1213203435565)) ;
#96648 = CARTESIAN_POINT('Ctrl Pts',(31.5178386301049,257.452005647303,20.1213203435565)) ;
#96649 = CARTESIAN_POINT('Ctrl Pts',(31.5150484732124,257.445958780731,20.1213203435565)) ;
#96650 = CARTESIAN_POINT('Ctrl Pts',(31.5132912927696,257.442150594995,20.1213203435565)) ;
#96651 = CARTESIAN_POINT('Ctrl Pts',(31.5115322300475,257.438337975969,20.1213203435565)) ;
#96652 = CARTESIAN_POINT('Ctrl Pts',(31.509772818656,257.434524303432,20.1213203435565)) ;
#96653 = CARTESIAN_POINT('Ctrl Pts',(31.5078072976114,257.430263870844,20.1213203435565)) ;
#96654 = CARTESIAN_POINT('Ctrl Pts',(31.5058437201315,257.425992735893,20.1213203435565)) ;
#96655 = CARTESIAN_POINT('Ctrl Pts',(31.5038815376229,257.421712469162,20.1213203435565)) ;
#96656 = CARTESIAN_POINT('Ctrl Pts',(31.4975523389697,257.407906078415,20.1213203435565)) ;
#96657 = CARTESIAN_POINT('Ctrl Pts',(31.4912358139239,257.393993745983,20.1213203435565)) ;
#96658 = CARTESIAN_POINT('Ctrl Pts',(31.4848699785717,257.379985562715,20.1213203435566)) ;
#96659 = CARTESIAN_POINT('Ctrl Pts',(31.4837555525691,257.377533239835,20.1213203435566)) ;
#96660 = CARTESIAN_POINT('Ctrl Pts',(31.4826395531966,257.375078092253,20.1213203435566)) ;
#96661 = CARTESIAN_POINT('Ctrl Pts',(31.4815215526911,257.372620316615,20.1213203435566)) ;
#96662 = CARTESIAN_POINT('Ctrl Pts',(31.4766434373058,257.361896427766,20.1213203435566)) ;
#96663 = CARTESIAN_POINT('Ctrl Pts',(31.4717384967145,257.351142007976,20.1213203435566)) ;
#96664 = CARTESIAN_POINT('Ctrl Pts',(31.4667122855711,257.340279417221,20.1213203435566)) ;
#96665 = CARTESIAN_POINT('Ctrl Pts',(31.4619026837029,257.329884959985,20.1213203435566)) ;
#96666 = CARTESIAN_POINT('Ctrl Pts',(31.456983429614,257.319391751533,20.1213203435566)) ;
#96667 = CARTESIAN_POINT('Ctrl Pts',(31.4518530945931,257.308774346739,20.1213203435566)) ;
#96668 = CARTESIAN_POINT('Ctrl Pts',(31.4472164096362,257.299178567733,20.1213203435566)) ;
#96669 = CARTESIAN_POINT('Ctrl Pts',(31.4424083086682,257.289481950142,20.1213203435566)) ;
#96670 = CARTESIAN_POINT('Ctrl Pts',(31.4373224728242,257.279694483374,20.1213203435566)) ;
#96671 = CARTESIAN_POINT('Ctrl Pts',(31.4358230654828,257.276808940077,20.1213203435566)) ;
#96672 = CARTESIAN_POINT('Ctrl Pts',(31.4342992376485,257.273915674778,20.1213203435566)) ;
#96673 = CARTESIAN_POINT('Ctrl Pts',(31.4327474548286,257.271015368647,20.1213203435566)) ;
#96674 = CARTESIAN_POINT('Ctrl Pts',(31.4286512948732,257.263359582234,20.1213203435566)) ;
#96675 = CARTESIAN_POINT('Ctrl Pts',(31.4243584117938,257.255643973918,20.1213203435566)) ;
#96676 = CARTESIAN_POINT('Ctrl Pts',(31.419744467576,257.247826312544,20.1213203435566)) ;
#96677 = CARTESIAN_POINT('Ctrl Pts',(31.4157201000424,257.241007603619,20.1213203435566)) ;
#96678 = CARTESIAN_POINT('Ctrl Pts',(31.4114518978677,257.234111772635,20.1213203435566)) ;
#96679 = CARTESIAN_POINT('Ctrl Pts',(31.4068277629769,257.22712911912,20.1213203435566)) ;
#96680 = CARTESIAN_POINT('Ctrl Pts',(31.4035112192784,257.22212098764,20.1213203435566)) ;
#96681 = CARTESIAN_POINT('Ctrl Pts',(31.4000098313069,257.217066848291,20.1213203435566)) ;
#96682 = CARTESIAN_POINT('Ctrl Pts',(31.3962725453509,257.211973553155,20.1213203435566)) ;
#96683 = CARTESIAN_POINT('Ctrl Pts',(31.3908345527168,257.204562479516,20.1213203435566)) ;
#96684 = CARTESIAN_POINT('Ctrl Pts',(31.3849071071445,257.197083054429,20.1213203435566)) ;
#96685 = CARTESIAN_POINT('Ctrl Pts',(31.3783637344278,257.189642216166,20.1213203435566)) ;
#96686 = CARTESIAN_POINT('Ctrl Pts',(31.3741084934393,257.184803341577,20.1213203435566)) ;
#96687 = CARTESIAN_POINT('Ctrl Pts',(31.3695918484284,257.179980247687,20.1213203435566)) ;
#96688 = CARTESIAN_POINT('Ctrl Pts',(31.3647692135685,257.175195683227,20.1213203435566)) ;
#96689 = CARTESIAN_POINT('Ctrl Pts',(31.3624414920458,257.17288633699,20.1213203435566)) ;
#96690 = CARTESIAN_POINT('Ctrl Pts',(31.3600437861251,257.170587098048,20.1213203435566)) ;
#96691 = CARTESIAN_POINT('Ctrl Pts',(31.3575620270058,257.168292523018,20.1213203435566)) ;
#96692 = CARTESIAN_POINT('Ctrl Pts',(31.3550802678865,257.165997947987,20.1213203435566)) ;
#96693 = CARTESIAN_POINT('Ctrl Pts',(31.3525136339308,257.163708938113,20.1213203435566)) ;
#96694 = CARTESIAN_POINT('Ctrl Pts',(31.3499252983641,257.161483805886,20.1213203435566)) ;
#96695 = CARTESIAN_POINT('Ctrl Pts',(31.34180172865,257.154500160876,20.1213203435566)) ;
#96696 = CARTESIAN_POINT('Ctrl Pts',(31.3334934711741,257.148157614545,20.1213203435567)) ;
#96697 = CARTESIAN_POINT('Ctrl Pts',(31.3250514390484,257.142337795154,20.1213203435567)) ;
#96698 = CARTESIAN_POINT('Ctrl Pts',(31.3158472909083,257.135992583594,20.1213203435567)) ;
#96699 = CARTESIAN_POINT('Ctrl Pts',(31.3064844393971,257.13026861466,20.1213203435567)) ;
#96700 = CARTESIAN_POINT('Ctrl Pts',(31.2970839532443,257.12504942768,20.1213203435567)) ;
#96701 = CARTESIAN_POINT('Ctrl Pts',(31.2885502552192,257.120311484887,20.1213203435568)) ;
#96702 = CARTESIAN_POINT('Ctrl Pts',(31.2799868778864,257.115990220132,20.1213203435568)) ;
#96703 = CARTESIAN_POINT('Ctrl Pts',(31.2715131924955,257.112021656713,20.1213203435568)) ;
#96704 = CARTESIAN_POINT('Ctrl Pts',(31.2611099851996,257.107149421551,20.1213203435568)) ;
#96705 = CARTESIAN_POINT('Ctrl Pts',(31.2503865049053,257.102794974448,20.1213203435569)) ;
#96706 = CARTESIAN_POINT('Ctrl Pts',(31.2397927939429,257.098958254889,20.1213203435569)) ;
#96707 = CARTESIAN_POINT('Ctrl Pts',(31.2327938866677,257.096423463773,20.1213203435569)) ;
#96708 = CARTESIAN_POINT('Ctrl Pts',(31.225851783864,257.094113215673,20.1213203435569)) ;
#96709 = CARTESIAN_POINT('Ctrl Pts',(31.2190923526486,257.092015936192,20.1213203435569)) ;
#96710 = CARTESIAN_POINT('Ctrl Pts',(31.2102760763554,257.089280470029,20.121320343557)) ;
#96711 = CARTESIAN_POINT('Ctrl Pts',(31.2015479560693,257.086836159472,20.121320343557)) ;
#96712 = CARTESIAN_POINT('Ctrl Pts',(31.192961649612,257.084631260979,20.121320343557)) ;
#96713 = CARTESIAN_POINT('Ctrl Pts',(31.1840312842957,257.082338010776,20.121320343557)) ;
#96714 = CARTESIAN_POINT('Ctrl Pts',(31.1752542408135,257.080303377449,20.121320343557)) ;
#96715 = CARTESIAN_POINT('Ctrl Pts',(31.1666337736506,257.078472857046,20.121320343557)) ;
#96716 = CARTESIAN_POINT('Ctrl Pts',(31.1578040570914,257.076597903402,20.1213203435571)) ;
#96717 = CARTESIAN_POINT('Ctrl Pts',(31.1491383134557,257.074936861673,20.1213203435571)) ;
#96718 = CARTESIAN_POINT('Ctrl Pts',(31.1405845422787,257.073439581227,20.1213203435571)) ;
#96719 = CARTESIAN_POINT('Ctrl Pts',(31.1317559096289,257.071894188119,20.1213203435571)) ;
#96720 = CARTESIAN_POINT('Ctrl Pts',(31.1230463636819,257.070523075047,20.1213203435572)) ;
#96721 = CARTESIAN_POINT('Ctrl Pts',(31.1143441789641,257.069283073925,20.1213203435572)) ;
#96722 = CARTESIAN_POINT('Ctrl Pts',(31.1090904981052,257.068534460747,20.1213203435573)) ;
#96723 = CARTESIAN_POINT('Ctrl Pts',(31.1038384763594,257.067833878059,20.1213203435573)) ;
#96724 = CARTESIAN_POINT('Ctrl Pts',(31.0985547216863,257.06717420603,20.1213203435573)) ;
#96725 = CARTESIAN_POINT('Ctrl Pts',(31.0822151079867,257.065134219923,20.1213203435575)) ;
#96726 = CARTESIAN_POINT('Ctrl Pts',(31.0658113380929,257.063516915152,20.1213203435576)) ;
#96727 = CARTESIAN_POINT('Ctrl Pts',(31.0494699256462,257.062255478661,20.1213203435578)) ;
#96728 = CARTESIAN_POINT('Ctrl Pts',(31.0329217121231,257.060978078653,20.121320343558)) ;
#96729 = CARTESIAN_POINT('Ctrl Pts',(31.0164374106932,257.060065168486,20.1213203435582)) ;
#96730 = CARTESIAN_POINT('Ctrl Pts',(31.0000947450752,257.059451949941,20.1213203435585)) ;
#96731 = CARTESIAN_POINT('Ctrl Pts',(30.9835705235233,257.058831918954,20.1213203435587)) ;
#96732 = CARTESIAN_POINT('Ctrl Pts',(30.9671909481073,257.058517989808,20.1213203435589)) ;
#96733 = CARTESIAN_POINT('Ctrl Pts',(30.9509833440119,257.058453340951,20.1213203435591)) ;
#96734 = CARTESIAN_POINT('Ctrl Pts',(30.9344197759284,257.058387272226,20.1213203435593)) ;
#96735 = CARTESIAN_POINT('Ctrl Pts',(30.9180356893947,257.058581350378,20.1213203435594)) ;
#96736 = CARTESIAN_POINT('Ctrl Pts',(30.9018072392188,257.058989232507,20.1213203435595)) ;
#96737 = CARTESIAN_POINT('Ctrl Pts',(30.891562852584,257.05924671256,20.1213203435596)) ;
#96738 = CARTESIAN_POINT('Ctrl Pts',(30.8813794324915,257.059589694101,20.1213203435596)) ;
#96739 = CARTESIAN_POINT('Ctrl Pts',(30.8712408692026,257.060009804349,20.1213203435596)) ;
#96740 = CARTESIAN_POINT('Ctrl Pts',(30.8708637790654,257.060025429781,20.1213203435596)) ;
#96741 = CARTESIAN_POINT('Ctrl Pts',(30.8704868289408,257.060041158946,20.1213203435596)) ;
#96742 = CARTESIAN_POINT('Ctrl Pts',(30.8701100175113,257.060056991359,20.1213203435596)) ;
#96743 = CARTESIAN_POINT('Ctrl Pts',(30.7743961481367,257.164166814187,20.0213203435596)) ;
#96744 = CARTESIAN_POINT('Ctrl Pts',(30.7746326029829,257.163914930351,20.0213203435596)) ;
#96745 = CARTESIAN_POINT('Ctrl Pts',(30.7748690126325,257.163663002226,20.0213212573643)) ;
#96746 = CARTESIAN_POINT('Ctrl Pts',(30.7862474765949,257.151533217284,20.0214091930669)) ;
#96747 = CARTESIAN_POINT('Ctrl Pts',(30.7973822007925,257.139448779789,20.0235241814884)) ;
#96748 = CARTESIAN_POINT('Ctrl Pts',(30.8179379288125,257.116974935591,20.0315745600298)) ;
#96749 = CARTESIAN_POINT('Ctrl Pts',(30.8276826449037,257.106246996249,20.0373654819654)) ;
#96750 = CARTESIAN_POINT('Ctrl Pts',(30.8457792331966,257.086541872235,20.0535013924982)) ;
#96751 = CARTESIAN_POINT('Ctrl Pts',(30.8534645081883,257.078193034956,20.0635493061725)) ;
#96752 = CARTESIAN_POINT('Ctrl Pts',(30.862600318185,257.068236069426,20.0817133908593)) ;
#96753 = CARTESIAN_POINT('Ctrl Pts',(30.8654074439578,257.065190004858,20.0892538401936)) ;
#96754 = CARTESIAN_POINT('Ctrl Pts',(30.8691476327655,257.061117063952,20.1050848833404)) ;
#96755 = CARTESIAN_POINT('Ctrl Pts',(30.8701100175112,257.060056991359,20.1131368914135)) ;
#96756 = CARTESIAN_POINT('Ctrl Pts',(30.8701100175112,257.060056991359,20.1213203435596)) ;
#96757 = CARTESIAN_POINT('Origin',(30.4489043471128,249.417461949796,20.1213203435596)) ;
#96758 = CARTESIAN_POINT('',(30.853318115509,256.660409724306,20.1213203435596)) ;
#96759 = CARTESIAN_POINT('',(30.5488161932143,249.413263973069,20.1213203435596)) ;
#96760 = CARTESIAN_POINT('Ctrl Pts',(30.8533181205427,256.660409843506,20.1213203435596)) ;
#96761 = CARTESIAN_POINT('Ctrl Pts',(30.8533181205427,256.660409843506,20.1131416452177)) ;
#96762 = CARTESIAN_POINT('Ctrl Pts',(30.852270661312,256.659427382356,20.1050923261438)) ;
#96763 = CARTESIAN_POINT('Ctrl Pts',(30.848206446685,256.6556792969,20.0892708055417)) ;
#96764 = CARTESIAN_POINT('Ctrl Pts',(30.8451552021593,256.652881747536,20.0817291561053)) ;
#96765 = CARTESIAN_POINT('Ctrl Pts',(30.8352215948528,256.643740521483,20.0635661934299)) ;
#96766 = CARTESIAN_POINT('Ctrl Pts',(30.8268708481235,256.636074154367,20.0535155318311)) ;
#96767 = CARTESIAN_POINT('Ctrl Pts',(30.8071303445457,256.617958965926,20.0373366241602)) ;
#96768 = CARTESIAN_POINT('Ctrl Pts',(30.7964637143612,256.608111454119,20.0315189424004)) ;
#96769 = CARTESIAN_POINT('Ctrl Pts',(30.7739733916521,256.587476318765,20.0234653725465)) ;
#96770 = CARTESIAN_POINT('Ctrl Pts',(30.7619107901203,256.576402602838,20.0214062385825)) ;
#96771 = CARTESIAN_POINT('Ctrl Pts',(30.7497119762593,256.565159924822,20.0213212211531)) ;
#96772 = CARTESIAN_POINT('Ctrl Pts',(30.7494601335157,256.564927828289,20.0213203435596)) ;
#96773 = CARTESIAN_POINT('Ctrl Pts',(30.7492082877751,256.564695737578,20.0213203435596)) ;
#96774 = CARTESIAN_POINT('Origin',(44.5070901774322,252.121399060531,20.1213203435596)) ;
#96775 = CARTESIAN_POINT('Origin',(31.2093839453833,258.32222131243,20.1213203435596)) ;
#96776 = CARTESIAN_POINT('Origin',(33.9819120129541,260.896418149051,20.1213203435596)) ;
#96777 = CARTESIAN_POINT('Origin',(32.8217003142836,259.81920153961,20.1213203435596)) ;
#96778 = CARTESIAN_POINT('Origin',(32.319849148055,249.82847140953,20.1213203435596)) ;
#96779 = CARTESIAN_POINT('Origin',(32.7113239146176,257.621855202687,20.1213203435596)) ;
#96780 = CARTESIAN_POINT('Origin',(44.9147880370394,251.931286426383,20.1213203435596)) ;
#96781 = CARTESIAN_POINT('Ctrl Pts',(32.2494313841384,257.837239226894,20.0213203435596)) ;
#96782 = CARTESIAN_POINT('Ctrl Pts',(32.2493153942693,257.837560219903,20.0213203435596)) ;
#96783 = CARTESIAN_POINT('Ctrl Pts',(32.2491993914172,257.83788121024,20.0213212212867)) ;
#96784 = CARTESIAN_POINT('Ctrl Pts',(32.2435730092924,257.853448270305,20.021406349793)) ;
#96785 = CARTESIAN_POINT('Ctrl Pts',(32.2380346526045,257.868835513893,20.0234710123247)) ;
#96786 = CARTESIAN_POINT('Ctrl Pts',(32.2277406393474,257.897506337361,20.0315483482936)) ;
#96787 = CARTESIAN_POINT('Ctrl Pts',(32.2228080732768,257.911121026691,20.0373826504411)) ;
#96788 = CARTESIAN_POINT('Ctrl Pts',(32.2137969550926,257.936231034257,20.0535836290149)) ;
#96789 = CARTESIAN_POINT('Ctrl Pts',(32.2099856311187,257.946839250697,20.0636304094217)) ;
#96790 = CARTESIAN_POINT('Ctrl Pts',(32.205442564853,257.959461423177,20.081776839957)) ;
#96791 = CARTESIAN_POINT('Ctrl Pts',(32.2040624233514,257.963329996811,20.0893091862125)) ;
#96792 = CARTESIAN_POINT('Ctrl Pts',(32.2022100389283,257.968490994962,20.1051145990528)) ;
#96793 = CARTESIAN_POINT('Ctrl Pts',(32.201722180204,257.96982418595,20.1131541545092)) ;
#96794 = CARTESIAN_POINT('Ctrl Pts',(32.201722180204,257.96982418595,20.1213203435596)) ;
#96795 = CARTESIAN_POINT('Ctrl Pts',(30.753406264502,256.66460758368,20.1213203435596)) ;
#96796 = CARTESIAN_POINT('Ctrl Pts',(30.7867102132026,256.663208258104,20.1213203435596)) ;
#96797 = CARTESIAN_POINT('Ctrl Pts',(30.8200141619031,256.661808932529,20.1213203435596)) ;
#96798 = CARTESIAN_POINT('Ctrl Pts',(31.0531097612377,256.652014999784,20.1213203435596)) ;
#96799 = CARTESIAN_POINT('Ctrl Pts',(31.3534533862626,256.674660174757,20.1213203435596)) ;
#96800 = CARTESIAN_POINT('Ctrl Pts',(31.6605197347822,256.879677823259,20.1213203435596)) ;
#96801 = CARTESIAN_POINT('Ctrl Pts',(31.8101800588843,257.116691929027,20.1213203435596)) ;
#96802 = CARTESIAN_POINT('Ctrl Pts',(31.9242228131995,257.380707018173,20.1213203435596)) ;
#96803 = CARTESIAN_POINT('Ctrl Pts',(32.0570123966128,257.663429119505,20.1213203435596)) ;
#96804 = CARTESIAN_POINT('Ctrl Pts',(32.1456747857374,257.852474228961,20.1213203435596)) ;
#96805 = CARTESIAN_POINT('Ctrl Pts',(32.2017221802041,257.96982418595,20.1213203435596)) ;
#96806 = CARTESIAN_POINT('Ctrl Pts',(30.753406264502,256.66460758368,20.1063603785425)) ;
#96807 = CARTESIAN_POINT('Ctrl Pts',(30.7867102132026,256.663208258104,20.1063603785425)) ;
#96808 = CARTESIAN_POINT('Ctrl Pts',(30.8200141619031,256.661808932529,20.1063603785425)) ;
#96809 = CARTESIAN_POINT('Ctrl Pts',(31.0531097612377,256.652014999784,20.1063603785425)) ;
#96810 = CARTESIAN_POINT('Ctrl Pts',(31.3534533862626,256.674660174757,20.1063603785425)) ;
#96811 = CARTESIAN_POINT('Ctrl Pts',(31.6605197347822,256.879677823259,20.1063603785425)) ;
#96812 = CARTESIAN_POINT('Ctrl Pts',(31.8101800588843,257.116691929027,20.1063603785425)) ;
#96813 = CARTESIAN_POINT('Ctrl Pts',(31.9242228131995,257.380707018173,20.1063603785425)) ;
#96814 = CARTESIAN_POINT('Ctrl Pts',(32.0570123966128,257.663429119505,20.1063603785425)) ;
#96815 = CARTESIAN_POINT('Ctrl Pts',(32.1456747857374,257.852474228961,20.1063603785425)) ;
#96816 = CARTESIAN_POINT('Ctrl Pts',(32.2017221802041,257.96982418595,20.1063603785425)) ;
#96817 = CARTESIAN_POINT('Ctrl Pts',(30.7531194015905,256.657780246386,20.0764517751007)) ;
#96818 = CARTESIAN_POINT('Ctrl Pts',(30.786423350291,256.65638092081,20.0764517751007)) ;
#96819 = CARTESIAN_POINT('Ctrl Pts',(30.8197272989916,256.654981595234,20.0764517751007)) ;
#96820 = CARTESIAN_POINT('Ctrl Pts',(31.0536921529186,256.64482049014,20.0764517751007)) ;
#96821 = CARTESIAN_POINT('Ctrl Pts',(31.3553494356536,256.667797230937,20.0764517751007)) ;
#96822 = CARTESIAN_POINT('Ctrl Pts',(31.66580693853,256.874741802429,20.0764517751007)) ;
#96823 = CARTESIAN_POINT('Ctrl Pts',(31.8165721794156,257.113917383899,20.0764517751007)) ;
#96824 = CARTESIAN_POINT('Ctrl Pts',(31.9305266534185,257.377866256042,20.0764517751007)) ;
#96825 = CARTESIAN_POINT('Ctrl Pts',(32.0632111374223,257.660448052357,20.0764517751007)) ;
#96826 = CARTESIAN_POINT('Ctrl Pts',(32.1520275174255,257.849713728641,20.0764517751007)) ;
#96827 = CARTESIAN_POINT('Ctrl Pts',(32.2078883528472,257.96687916646,20.0764517751007)) ;
#96828 = CARTESIAN_POINT('Ctrl Pts',(30.7519150570582,256.629116846515,20.0404585252547)) ;
#96829 = CARTESIAN_POINT('Ctrl Pts',(30.7852190057587,256.62771752094,20.0404585252546)) ;
#96830 = CARTESIAN_POINT('Ctrl Pts',(30.8185229544592,256.626318195364,20.0404585252547)) ;
#96831 = CARTESIAN_POINT('Ctrl Pts',(31.0547005508067,256.616146526555,20.0404585252547)) ;
#96832 = CARTESIAN_POINT('Ctrl Pts',(31.3629325847851,256.638409046288,20.0404585252546)) ;
#96833 = CARTESIAN_POINT('Ctrl Pts',(31.6873976939643,256.854298178497,20.0404585252547)) ;
#96834 = CARTESIAN_POINT('Ctrl Pts',(31.8430521064208,257.10234330074,20.0404585252546)) ;
#96835 = CARTESIAN_POINT('Ctrl Pts',(31.9565799920417,257.365847966563,20.0404585252547)) ;
#96836 = CARTESIAN_POINT('Ctrl Pts',(32.0892804342346,257.64827986717,20.0404585252547)) ;
#96837 = CARTESIAN_POINT('Ctrl Pts',(32.17787741575,257.83732196866,20.0404585252547)) ;
#96838 = CARTESIAN_POINT('Ctrl Pts',(32.2337759667908,257.954515009303,20.0404585252547)) ;
#96839 = CARTESIAN_POINT('Ctrl Pts',(30.7504644798715,256.594593109473,20.0238261114369)) ;
#96840 = CARTESIAN_POINT('Ctrl Pts',(30.7837684285721,256.593193783897,20.0238261114369)) ;
#96841 = CARTESIAN_POINT('Ctrl Pts',(30.8170723772726,256.591794458321,20.023826111437)) ;
#96842 = CARTESIAN_POINT('Ctrl Pts',(31.0559072718364,256.581618428455,20.0238261114369)) ;
#96843 = CARTESIAN_POINT('Ctrl Pts',(31.3720640767969,256.603009197133,20.0238261114369)) ;
#96844 = CARTESIAN_POINT('Ctrl Pts',(31.7133994447527,256.829676306926,20.0238261114369)) ;
#96845 = CARTESIAN_POINT('Ctrl Pts',(31.8749440054121,257.088403260065,20.0238261114369)) ;
#96846 = CARTESIAN_POINT('Ctrl Pts',(31.9879577794308,257.351371992096,20.0238261114369)) ;
#96847 = CARTESIAN_POINT('Ctrl Pts',(32.1206799398744,257.63362574903,20.0238261114369)) ;
#96848 = CARTESIAN_POINT('Ctrl Pts',(32.2090079362795,257.822392285682,20.0238261114369)) ;
#96849 = CARTESIAN_POINT('Ctrl Pts',(32.2649563982988,257.939622954894,20.0238261114369)) ;
#96850 = CARTESIAN_POINT('Ctrl Pts',(30.7495222957,256.572169126191,20.0213203435596)) ;
#96851 = CARTESIAN_POINT('Ctrl Pts',(30.7828262444005,256.570769800615,20.0213203435596)) ;
#96852 = CARTESIAN_POINT('Ctrl Pts',(30.8161301931011,256.569370475039,20.0213203435597)) ;
#96853 = CARTESIAN_POINT('Ctrl Pts',(31.0567131604158,256.559168067985,20.0213203435596)) ;
#96854 = CARTESIAN_POINT('Ctrl Pts',(31.3780009959797,256.580025005874,20.0213203435596)) ;
#96855 = CARTESIAN_POINT('Ctrl Pts',(31.7302975263905,256.81367952226,20.0213203435596)) ;
#96856 = CARTESIAN_POINT('Ctrl Pts',(31.8956640270926,257.079347730437,20.0213203435596)) ;
#96857 = CARTESIAN_POINT('Ctrl Pts',(32.0083447340676,257.341970916896,20.0213203435596)) ;
#96858 = CARTESIAN_POINT('Ctrl Pts',(32.1410739697034,257.624102211558,20.0213203435596)) ;
#96859 = CARTESIAN_POINT('Ctrl Pts',(32.2292405707272,257.812707441946,20.0213203435596)) ;
#96860 = CARTESIAN_POINT('Ctrl Pts',(32.285208825607,257.929950213537,20.0213203435596)) ;
#96861 = CARTESIAN_POINT('Ctrl Pts',(30.7492082877751,256.564695737578,20.0213203435596)) ;
#96862 = CARTESIAN_POINT('Ctrl Pts',(30.7825122364757,256.563296412003,20.0213203435596)) ;
#96863 = CARTESIAN_POINT('Ctrl Pts',(30.8158161851762,256.561897086427,20.0213203435597)) ;
#96864 = CARTESIAN_POINT('Ctrl Pts',(31.0569053558616,256.55176728934,20.0213203435596)) ;
#96865 = CARTESIAN_POINT('Ctrl Pts',(31.3799595822748,256.57233432435,20.0213203435596)) ;
#96866 = CARTESIAN_POINT('Ctrl Pts',(31.735897005124,256.808363024752,20.0213203435596)) ;
#96867 = CARTESIAN_POINT('Ctrl Pts',(31.9025505811396,257.076333688533,20.0213203435596)) ;
#96868 = CARTESIAN_POINT('Ctrl Pts',(32.0151173093266,257.33883287554,20.0213203435596)) ;
#96869 = CARTESIAN_POINT('Ctrl Pts',(32.1478732124172,257.62094670617,20.0213203435596)) ;
#96870 = CARTESIAN_POINT('Ctrl Pts',(32.2359399838344,257.809437053091,20.0213203435596)) ;
#96871 = CARTESIAN_POINT('Ctrl Pts',(32.2919584854562,257.926726515311,20.0213203435596)) ;
#96872 = CARTESIAN_POINT('Ctrl Pts',(30.8533181204414,256.66040984351,20.1213203435596)) ;
#96873 = CARTESIAN_POINT('Ctrl Pts',(31.0538433767003,256.652070516101,20.1213203435596)) ;
#96874 = CARTESIAN_POINT('Ctrl Pts',(31.3537346899415,256.674847991556,20.1213203435596)) ;
#96875 = CARTESIAN_POINT('Ctrl Pts',(31.6605197347822,256.879677823259,20.1213203435596)) ;
#96876 = CARTESIAN_POINT('Ctrl Pts',(31.8101800588843,257.116691929027,20.1213203435596)) ;
#96877 = CARTESIAN_POINT('Ctrl Pts',(31.9242228131995,257.380707018173,20.1213203435596)) ;
#96878 = CARTESIAN_POINT('Ctrl Pts',(32.0570123966128,257.663429119505,20.1213203435596)) ;
#96879 = CARTESIAN_POINT('Ctrl Pts',(32.1456747857374,257.852474228961,20.1213203435596)) ;
#96880 = CARTESIAN_POINT('Ctrl Pts',(32.2017221802041,257.96982418595,20.1213203435596)) ;
#96881 = CARTESIAN_POINT('Ctrl Pts',(30.8533181106036,256.660409606953,20.0213203435596)) ;
#96882 = CARTESIAN_POINT('Ctrl Pts',(30.8533181106036,256.660409606953,20.3813203435596)) ;
#96883 = CARTESIAN_POINT('Ctrl Pts',(31.2255082708192,256.644771364927,20.0213203435596)) ;
#96884 = CARTESIAN_POINT('Ctrl Pts',(31.2255082708192,256.644771364927,20.3813203435596)) ;
#96885 = CARTESIAN_POINT('Ctrl Pts',(31.4869115990368,256.735802916448,20.0213203435596)) ;
#96886 = CARTESIAN_POINT('Ctrl Pts',(31.4869115990368,256.735802916448,20.3813203435596)) ;
#96887 = CARTESIAN_POINT('Ctrl Pts',(31.6392361795028,256.887658160472,20.0213203435596)) ;
#96888 = CARTESIAN_POINT('Ctrl Pts',(31.6392361795028,256.887658160472,20.3813203435596)) ;
#96889 = CARTESIAN_POINT('Ctrl Pts',(31.8202190831926,257.068083426833,20.0213203435596)) ;
#96890 = CARTESIAN_POINT('Ctrl Pts',(31.8202190831926,257.068083426833,20.3813203435596)) ;
#96891 = CARTESIAN_POINT('Ctrl Pts',(31.8533149361085,257.224893291544,20.0213203435596)) ;
#96892 = CARTESIAN_POINT('Ctrl Pts',(31.8533149361085,257.224893291544,20.3813203435596)) ;
#96893 = CARTESIAN_POINT('Ctrl Pts',(31.9557184877316,257.447246089354,20.0213203435596)) ;
#96894 = CARTESIAN_POINT('Ctrl Pts',(31.9557184877316,257.447246089354,20.3813203435596)) ;
#96895 = CARTESIAN_POINT('Ctrl Pts',(32.0253094429367,257.598351625704,20.0213203435596)) ;
#96896 = CARTESIAN_POINT('Ctrl Pts',(32.0253094429367,257.598351625704,20.3813203435596)) ;
#96897 = CARTESIAN_POINT('Ctrl Pts',(32.1145256312286,257.787255283878,20.0213203435596)) ;
#96898 = CARTESIAN_POINT('Ctrl Pts',(32.1145256312286,257.787255283878,20.3813203435596)) ;
#96899 = CARTESIAN_POINT('Ctrl Pts',(32.201722180204,257.969824185949,20.0213203435596)) ;
#96900 = CARTESIAN_POINT('Ctrl Pts',(32.201722180204,257.969824185949,20.3813203435596)) ;
#96901 = CARTESIAN_POINT('',(30.8533181106036,256.660409606953,20.0213203435596)) ;
#96902 = CARTESIAN_POINT('Origin',(30.8701100175113,257.060056991358,20.0213203435596)) ;
#96903 = CARTESIAN_POINT('',(30.8701100175112,257.060056991359,20.0213203435596)) ;
#96904 = CARTESIAN_POINT('Ctrl Pts',(31.8391836130389,258.138878696195,20.0213203435596)) ;
#96905 = CARTESIAN_POINT('Ctrl Pts',(31.8391836130389,258.138878696195,20.3813203435596)) ;
#96906 = CARTESIAN_POINT('Ctrl Pts',(31.7162037244466,257.881374998661,20.0213203435596)) ;
#96907 = CARTESIAN_POINT('Ctrl Pts',(31.7162037244466,257.881374998661,20.3813203435596)) ;
#96908 = CARTESIAN_POINT('Ctrl Pts',(31.5892548552809,257.6068083194,20.0213203435596)) ;
#96909 = CARTESIAN_POINT('Ctrl Pts',(31.5892548552809,257.6068083194,20.3813203435596)) ;
#96910 = CARTESIAN_POINT('Ctrl Pts',(31.509772818656,257.434524303432,20.0213203435596)) ;
#96911 = CARTESIAN_POINT('Ctrl Pts',(31.509772818656,257.434524303432,20.3813203435596)) ;
#96912 = CARTESIAN_POINT('Ctrl Pts',(31.4282577248589,257.257833464625,20.0213203435596)) ;
#96913 = CARTESIAN_POINT('Ctrl Pts',(31.4282577248589,257.257833464625,20.3813203435596)) ;
#96914 = CARTESIAN_POINT('Ctrl Pts',(31.4006948106297,257.172522539205,20.0213203435596)) ;
#96915 = CARTESIAN_POINT('Ctrl Pts',(31.4006948106297,257.172522539205,20.3813203435596)) ;
#96916 = CARTESIAN_POINT('Ctrl Pts',(31.2715131924955,257.112021656713,20.0213203435596)) ;
#96917 = CARTESIAN_POINT('Ctrl Pts',(31.2715131924955,257.112021656713,20.3813203435596)) ;
#96918 = CARTESIAN_POINT('Ctrl Pts',(31.1997685794864,257.078420804952,20.0213203435596)) ;
#96919 = CARTESIAN_POINT('Ctrl Pts',(31.1997685794864,257.078420804952,20.3813203435596)) ;
#96920 = CARTESIAN_POINT('Ctrl Pts',(31.0748905561884,257.051452767045,20.0213203435596)) ;
#96921 = CARTESIAN_POINT('Ctrl Pts',(31.0748905561884,257.051452767045,20.3813203435596)) ;
#96922 = CARTESIAN_POINT('Ctrl Pts',(30.8701100175112,257.060056991359,20.0213203435596)) ;
#96923 = CARTESIAN_POINT('Ctrl Pts',(30.8701100175112,257.060056991359,20.3813203435596)) ;
#96924 = CARTESIAN_POINT('Ctrl Pts',(29.5759712687709,255.502885024398,20.1213203435596)) ;
#96925 = CARTESIAN_POINT('Ctrl Pts',(29.6096896012297,255.570241420972,20.1213203435596)) ;
#96926 = CARTESIAN_POINT('Ctrl Pts',(29.7111240387136,255.772053704706,20.1213203435596)) ;
#96927 = CARTESIAN_POINT('Ctrl Pts',(29.8202483669958,256.007253286122,20.1213203435596)) ;
#96928 = CARTESIAN_POINT('Ctrl Pts',(29.8999342879726,256.197254367133,20.1213203435596)) ;
#96929 = CARTESIAN_POINT('Ctrl Pts',(29.9295469120274,256.267285941343,20.1213203435596)) ;
#96930 = CARTESIAN_POINT('Ctrl Pts',(29.9544466269417,256.322163872416,20.1213203435596)) ;
#96931 = CARTESIAN_POINT('Ctrl Pts',(29.981825823837,256.378579501238,20.1213203435596)) ;
#96932 = CARTESIAN_POINT('Ctrl Pts',(30.030187806939,256.446752104601,20.1213203435596)) ;
#96933 = CARTESIAN_POINT('Ctrl Pts',(30.0935892844406,256.495791347758,20.1213203435596)) ;
#96934 = CARTESIAN_POINT('Ctrl Pts',(30.2113796608321,256.560201882538,20.1213203435596)) ;
#96935 = CARTESIAN_POINT('Ctrl Pts',(30.3858069793213,256.614439322451,20.1213203435596)) ;
#96936 = CARTESIAN_POINT('Ctrl Pts',(30.5388867945401,256.6452934669,20.1213203435596)) ;
#96937 = CARTESIAN_POINT('Ctrl Pts',(30.6483865150998,256.663405993051,20.1213203435596)) ;
#96938 = CARTESIAN_POINT('Ctrl Pts',(30.6812729811269,256.668845796667,20.1213203435596)) ;
#96939 = CARTESIAN_POINT('Ctrl Pts',(30.7141594471539,256.674285600284,20.1213203435596)) ;
#96940 = CARTESIAN_POINT('Ctrl Pts',(29.5759712687709,255.502885024398,20.1063603785425)) ;
#96941 = CARTESIAN_POINT('Ctrl Pts',(29.6096896012297,255.570241420972,20.1063603785425)) ;
#96942 = CARTESIAN_POINT('Ctrl Pts',(29.7111240387136,255.772053704706,20.1063603785425)) ;
#96943 = CARTESIAN_POINT('Ctrl Pts',(29.8202483669958,256.007253286122,20.1063603785425)) ;
#96944 = CARTESIAN_POINT('Ctrl Pts',(29.8999342879726,256.197254367133,20.1063603785425)) ;
#96945 = CARTESIAN_POINT('Ctrl Pts',(29.9295469120274,256.267285941343,20.1063603785425)) ;
#96946 = CARTESIAN_POINT('Ctrl Pts',(29.9544466269417,256.322163872416,20.1063603785425)) ;
#96947 = CARTESIAN_POINT('Ctrl Pts',(29.981825823837,256.378579501238,20.1063603785425)) ;
#96948 = CARTESIAN_POINT('Ctrl Pts',(30.030187806939,256.446752104601,20.1063603785425)) ;
#96949 = CARTESIAN_POINT('Ctrl Pts',(30.0935892844406,256.495791347758,20.1063603785425)) ;
#96950 = CARTESIAN_POINT('Ctrl Pts',(30.2113796608321,256.560201882538,20.1063603785425)) ;
#96951 = CARTESIAN_POINT('Ctrl Pts',(30.3858069793213,256.614439322451,20.1063603785425)) ;
#96952 = CARTESIAN_POINT('Ctrl Pts',(30.5388867945401,256.6452934669,20.1063603785425)) ;
#96953 = CARTESIAN_POINT('Ctrl Pts',(30.6483865150998,256.663405993051,20.1063603785425)) ;
#96954 = CARTESIAN_POINT('Ctrl Pts',(30.6812729811269,256.668845796667,20.1063603785425)) ;
#96955 = CARTESIAN_POINT('Ctrl Pts',(30.7141594471539,256.674285600284,20.1063603785425)) ;
#96956 = CARTESIAN_POINT('Ctrl Pts',(29.5820931728356,255.499820424641,20.0764990745067)) ;
#96957 = CARTESIAN_POINT('Ctrl Pts',(29.6157879144431,255.567133304607,20.0764990745067)) ;
#96958 = CARTESIAN_POINT('Ctrl Pts',(29.7171758868717,255.768968124513,20.0764990745067)) ;
#96959 = CARTESIAN_POINT('Ctrl Pts',(29.8264197782412,256.004440884627,20.0764990745067)) ;
#96960 = CARTESIAN_POINT('Ctrl Pts',(29.9060885809734,256.194470121105,20.0764990745067)) ;
#96961 = CARTESIAN_POINT('Ctrl Pts',(29.9356887118595,256.264457942251,20.0764990745067)) ;
#96962 = CARTESIAN_POINT('Ctrl Pts',(29.9605274326313,256.319158916676,20.0764990745067)) ;
#96963 = CARTESIAN_POINT('Ctrl Pts',(29.9877640220894,256.375182355551,20.0764990745067)) ;
#96964 = CARTESIAN_POINT('Ctrl Pts',(30.0351997933448,256.44195523641,20.0764990745067)) ;
#96965 = CARTESIAN_POINT('Ctrl Pts',(30.09745915079,256.490158379369,20.0764990745067)) ;
#96966 = CARTESIAN_POINT('Ctrl Pts',(30.2138634005463,256.553814059384,20.0764990745067)) ;
#96967 = CARTESIAN_POINT('Ctrl Pts',(30.3874884736995,256.607807329319,20.0764990745067)) ;
#96968 = CARTESIAN_POINT('Ctrl Pts',(30.5401558482827,256.638579125182,20.0764990745067)) ;
#96969 = CARTESIAN_POINT('Ctrl Pts',(30.6495037630039,256.656651643477,20.0764990745067)) ;
#96970 = CARTESIAN_POINT('Ctrl Pts',(30.6823902290309,256.662091447093,20.0764990745067)) ;
#96971 = CARTESIAN_POINT('Ctrl Pts',(30.7152766950579,256.66753125071,20.0764990745067)) ;
#96972 = CARTESIAN_POINT('Ctrl Pts',(29.6120092577916,255.484844556725,20.0344442939593)) ;
#96973 = CARTESIAN_POINT('Ctrl Pts',(29.6457436600241,255.55223306503,20.0344442939593)) ;
#96974 = CARTESIAN_POINT('Ctrl Pts',(29.7471844945767,255.754197572988,20.0344442939593)) ;
#96975 = CARTESIAN_POINT('Ctrl Pts',(29.8570682054636,255.990988132927,20.0344442939593)) ;
#96976 = CARTESIAN_POINT('Ctrl Pts',(29.9369263762561,256.181564104702,20.0344442939593)) ;
#96977 = CARTESIAN_POINT('Ctrl Pts',(29.9664278986104,256.251202813136,20.0344442939593)) ;
#96978 = CARTESIAN_POINT('Ctrl Pts',(29.9906663597142,256.304833928402,20.0344442939593)) ;
#96979 = CARTESIAN_POINT('Ctrl Pts',(30.0172467190228,256.358916591612,20.0344442939593)) ;
#96980 = CARTESIAN_POINT('Ctrl Pts',(30.0594700010607,256.41830695162,20.0344442939593)) ;
#96981 = CARTESIAN_POINT('Ctrl Pts',(30.1154245125015,256.461746853186,20.0344442939593)) ;
#96982 = CARTESIAN_POINT('Ctrl Pts',(30.2256762972524,256.522325166701,20.0344442939593)) ;
#96983 = CARTESIAN_POINT('Ctrl Pts',(30.3954814694958,256.57530322983,20.0344442939593)) ;
#96984 = CARTESIAN_POINT('Ctrl Pts',(30.5463544154014,256.605679815488,20.0344442939593)) ;
#96985 = CARTESIAN_POINT('Ctrl Pts',(30.6549634505227,256.623644968832,20.0344442939593)) ;
#96986 = CARTESIAN_POINT('Ctrl Pts',(30.6878499165497,256.629084772448,20.0344442939593)) ;
#96987 = CARTESIAN_POINT('Ctrl Pts',(30.7207363825767,256.634524576065,20.0344442939593)) ;
#96988 = CARTESIAN_POINT('Ctrl Pts',(29.6453265506804,255.46816605824,20.0213203435596)) ;
#96989 = CARTESIAN_POINT('Ctrl Pts',(29.6790557391669,255.535546911685,20.0213203435596)) ;
#96990 = CARTESIAN_POINT('Ctrl Pts',(29.7804662281711,255.737649617999,20.0213203435596)) ;
#96991 = CARTESIAN_POINT('Ctrl Pts',(29.8910447966664,255.975913266732,20.0213203435596)) ;
#96992 = CARTESIAN_POINT('Ctrl Pts',(29.9710268478646,256.16696772935,20.0213203435596)) ;
#96993 = CARTESIAN_POINT('Ctrl Pts',(30.0004305211738,256.236260757865,20.0213203435596)) ;
#96994 = CARTESIAN_POINT('Ctrl Pts',(30.0240967948258,256.288765755951,20.0213203435596)) ;
#96995 = CARTESIAN_POINT('Ctrl Pts',(30.0499333589383,256.340694722479,20.0213203435596)) ;
#96996 = CARTESIAN_POINT('Ctrl Pts',(30.0865702872101,256.392036123077,20.0213203435596)) ;
#96997 = CARTESIAN_POINT('Ctrl Pts',(30.1357337756256,256.430387158868,20.0213203435596)) ;
#96998 = CARTESIAN_POINT('Ctrl Pts',(30.2389356351689,256.487343368006,20.0213203435596)) ;
#96999 = CARTESIAN_POINT('Ctrl Pts',(30.4044545988853,256.539134076114,20.0213203435596)) ;
#97000 = CARTESIAN_POINT('Ctrl Pts',(30.5532586492272,256.569068223099,20.0213203435596)) ;
#97001 = CARTESIAN_POINT('Ctrl Pts',(30.6610438587183,256.586885712129,20.0213203435597)) ;
#97002 = CARTESIAN_POINT('Ctrl Pts',(30.6939303247453,256.592325515745,20.0213203435596)) ;
#97003 = CARTESIAN_POINT('Ctrl Pts',(30.7268167907724,256.597765319362,20.0213203435596)) ;
#97004 = CARTESIAN_POINT('Ctrl Pts',(29.6653926650914,255.458121044681,20.0213203435596)) ;
#97005 = CARTESIAN_POINT('Ctrl Pts',(29.6991510606097,255.525557472002,20.0213203435596)) ;
#97006 = CARTESIAN_POINT('Ctrl Pts',(29.8006017126181,255.727747494973,20.0213203435596)) ;
#97007 = CARTESIAN_POINT('Ctrl Pts',(29.9116103717487,255.966894765232,20.0213203435596)) ;
#97008 = CARTESIAN_POINT('Ctrl Pts',(29.9917240307883,256.158322827055,20.0213203435596)) ;
#97009 = CARTESIAN_POINT('Ctrl Pts',(30.0210609313549,256.227379414746,20.0213203435596)) ;
#97010 = CARTESIAN_POINT('Ctrl Pts',(30.0443195024724,256.279163360013,20.0213203435596)) ;
#97011 = CARTESIAN_POINT('Ctrl Pts',(30.0697165858412,256.329790150052,20.0213203435596)) ;
#97012 = CARTESIAN_POINT('Ctrl Pts',(30.102845715951,256.376170629923,20.0213203435596)) ;
#97013 = CARTESIAN_POINT('Ctrl Pts',(30.1477680849333,256.411315348599,20.0213203435596)) ;
#97014 = CARTESIAN_POINT('Ctrl Pts',(30.2468536416027,256.46621770294,20.0213203435596)) ;
#97015 = CARTESIAN_POINT('Ctrl Pts',(30.4098121082759,256.517330456645,20.0213203435596)) ;
#97016 = CARTESIAN_POINT('Ctrl Pts',(30.5574162678237,256.546999638827,20.0213203435596)) ;
#97017 = CARTESIAN_POINT('Ctrl Pts',(30.6647059259495,256.564746594971,20.0213203435597)) ;
#97018 = CARTESIAN_POINT('Ctrl Pts',(30.6975923919765,256.570186398587,20.0213203435596)) ;
#97019 = CARTESIAN_POINT('Ctrl Pts',(30.7304788580035,256.575626202204,20.0213203435596)) ;
#97020 = CARTESIAN_POINT('Ctrl Pts',(29.7113866401971,255.550077591566,20.0213203435596)) ;
#97021 = CARTESIAN_POINT('Ctrl Pts',(29.7110571373176,255.549958798757,20.0213203435596)) ;
#97022 = CARTESIAN_POINT('Ctrl Pts',(29.7107276113308,255.549840065814,20.0213212580779)) ;
#97023 = CARTESIAN_POINT('Ctrl Pts',(29.694928578155,255.544150689885,20.0214088991967)) ;
#97024 = CARTESIAN_POINT('Ctrl Pts',(29.6792649744873,255.538667136519,20.0235081059122)) ;
#97025 = CARTESIAN_POINT('Ctrl Pts',(29.650188463837,255.528611542996,20.0314970318247)) ;
#97026 = CARTESIAN_POINT('Ctrl Pts',(29.6363171942346,255.523870388381,20.0372432193757)) ;
#97027 = CARTESIAN_POINT('Ctrl Pts',(29.6106557248686,255.514948318743,20.0533121285624)) ;
#97028 = CARTESIAN_POINT('Ctrl Pts',(29.5997479208537,255.511139096753,20.0633496625201)) ;
#97029 = CARTESIAN_POINT('Ctrl Pts',(29.5867225388609,255.506615978723,20.0815270572468)) ;
#97030 = CARTESIAN_POINT('Ctrl Pts',(29.5827146684804,255.505215912772,20.08909649826)) ;
#97031 = CARTESIAN_POINT('Ctrl Pts',(29.5773629195699,255.50335835714,20.1050033356937)) ;
#97032 = CARTESIAN_POINT('Ctrl Pts',(29.5759712687709,255.502885024398,20.1130919745432)) ;
#97033 = CARTESIAN_POINT('Ctrl Pts',(29.5759712687709,255.502885024398,20.1213203435596)) ;
#97034 = CARTESIAN_POINT('Ctrl Pts',(30.7304788580025,256.575626202204,20.0213203435596)) ;
#97035 = CARTESIAN_POINT('Ctrl Pts',(30.7301957245571,256.575824538007,20.0213203435596)) ;
#97036 = CARTESIAN_POINT('Ctrl Pts',(30.7299126263369,256.576022926472,20.021321258476)) ;
#97037 = CARTESIAN_POINT('Ctrl Pts',(30.7162932839813,256.585570725375,20.0214092548886)) ;
#97038 = CARTESIAN_POINT('Ctrl Pts',(30.7029218650816,256.595123932586,20.0235245925657)) ;
#97039 = CARTESIAN_POINT('Ctrl Pts',(30.6782054645625,256.612919481131,20.0315757241732)) ;
#97040 = CARTESIAN_POINT('Ctrl Pts',(30.6664740137926,256.621427535467,20.0373664729568)) ;
#97041 = CARTESIAN_POINT('Ctrl Pts',(30.6447342707739,256.637012105662,20.0535001884872)) ;
#97042 = CARTESIAN_POINT('Ctrl Pts',(30.6355028892112,256.643611871642,20.0635480166157)) ;
#97043 = CARTESIAN_POINT('Ctrl Pts',(30.6245226322433,256.6514906015,20.0817172500721)) ;
#97044 = CARTESIAN_POINT('Ctrl Pts',(30.6211521485668,256.653899078661,20.0892580265995)) ;
#97045 = CARTESIAN_POINT('Ctrl Pts',(30.6166589348149,256.657123518393,20.1050867998701)) ;
#97046 = CARTESIAN_POINT('Ctrl Pts',(30.6155000490728,256.657966189434,20.1131378012872)) ;
#97047 = CARTESIAN_POINT('Ctrl Pts',(30.6155000490728,256.657966189434,20.1213203435596)) ;
#97048 = CARTESIAN_POINT('Origin',(43.2063774077619,249.25726004992,20.1213203435596)) ;
#97049 = CARTESIAN_POINT('Origin',(30.2066640303894,255.319125951608,20.1213203435596)) ;
#97050 = CARTESIAN_POINT('Origin',(28.3509795345864,248.977232647076,20.1213203435596)) ;
#97051 = CARTESIAN_POINT('',(28.7971429244132,255.86605864576,20.1213203435596)) ;
#97052 = CARTESIAN_POINT('Origin',(28.704724061155,256.019492061351,20.1213203435596)) ;
#97053 = CARTESIAN_POINT('',(28.7065616828874,254.062789469896,20.1213203435596)) ;
#97054 = CARTESIAN_POINT('',(28.4508536117473,248.972215804318,20.1213203435596)) ;
#97055 = CARTESIAN_POINT('Origin',(28.594347661489,253.822145724429,20.1213203435596)) ;
#97056 = CARTESIAN_POINT('Origin',(42.7981704029692,249.447610102367,20.1213203435596)) ;
#97057 = CARTESIAN_POINT('',(42.7559085767951,249.356979323663,20.1213203435596)) ;
#97058 = CARTESIAN_POINT('Ctrl Pts',(29.1672120667081,255.803830362557,20.0213203435596)) ;
#97059 = CARTESIAN_POINT('Ctrl Pts',(29.1673235517997,255.803511486707,20.0213203435596)) ;
#97060 = CARTESIAN_POINT('Ctrl Pts',(29.1674350651738,255.803192616964,20.0213212211779)) ;
#97061 = CARTESIAN_POINT('Ctrl Pts',(29.172875934703,255.78763807154,20.02140682762)) ;
#97062 = CARTESIAN_POINT('Ctrl Pts',(29.178235369087,255.772301108476,20.0234957973127)) ;
#97063 = CARTESIAN_POINT('Ctrl Pts',(29.1881961388463,255.743729511578,20.0316145116046)) ;
#97064 = CARTESIAN_POINT('Ctrl Pts',(29.1929424011081,255.730156724038,20.0375089738243)) ;
#97065 = CARTESIAN_POINT('Ctrl Pts',(29.2020451864744,255.704209432607,20.0544007578192)) ;
#97066 = CARTESIAN_POINT('Ctrl Pts',(29.2055656625208,255.69409678375,20.0647127777204)) ;
#97067 = CARTESIAN_POINT('Ctrl Pts',(29.2097099600077,255.682260454704,20.0818702576819)) ;
#97068 = CARTESIAN_POINT('Ctrl Pts',(29.2110458674259,255.678427653878,20.0893909150032)) ;
#97069 = CARTESIAN_POINT('Ctrl Pts',(29.2128367240668,255.673316457768,20.105158929986)) ;
#97070 = CARTESIAN_POINT('Ctrl Pts',(29.2133075051976,255.671997914687,20.1131782970793)) ;
#97071 = CARTESIAN_POINT('Ctrl Pts',(29.2133075051976,255.671997914687,20.1213203435596)) ;
#97072 = CARTESIAN_POINT('Origin',(32.5650931541241,257.50884617869,20.1213203435596)) ;
#97073 = CARTESIAN_POINT('',(32.4970522102795,257.582129396146,20.1213203435596)) ;
#97074 = CARTESIAN_POINT('Ctrl Pts',(30.6488818037555,257.068923192604,20.1213203435596)) ;
#97075 = CARTESIAN_POINT('Ctrl Pts',(30.6159953377285,257.063483388987,20.1213203435596)) ;
#97076 = CARTESIAN_POINT('Ctrl Pts',(30.5831088717014,257.058043585371,20.1213203435596)) ;
#97077 = CARTESIAN_POINT('Ctrl Pts',(30.35235925836,257.019874918049,20.1213203435596)) ;
#97078 = CARTESIAN_POINT('Ctrl Pts',(30.0562477831581,256.952359843337,20.1213203435596)) ;
#97079 = CARTESIAN_POINT('Ctrl Pts',(29.7424371293616,256.748815981268,20.1213203435596)) ;
#97080 = CARTESIAN_POINT('Ctrl Pts',(29.5940323940009,256.523626711091,20.1213203435596)) ;
#97081 = CARTESIAN_POINT('Ctrl Pts',(29.493524415239,256.258021637289,20.1213203435596)) ;
#97082 = CARTESIAN_POINT('Ctrl Pts',(29.3619731302367,255.972670333182,20.1213203435596)) ;
#97083 = CARTESIAN_POINT('Ctrl Pts',(29.2709280858246,255.787069709302,20.1213203435596)) ;
#97084 = CARTESIAN_POINT('Ctrl Pts',(29.2133075051975,255.671997914687,20.1213203435596)) ;
#97085 = CARTESIAN_POINT('Ctrl Pts',(30.6488818037555,257.068923192604,20.1063603785425)) ;
#97086 = CARTESIAN_POINT('Ctrl Pts',(30.6159953377285,257.063483388987,20.1063603785425)) ;
#97087 = CARTESIAN_POINT('Ctrl Pts',(30.5831088717014,257.058043585371,20.1063603785425)) ;
#97088 = CARTESIAN_POINT('Ctrl Pts',(30.35235925836,257.019874918049,20.1063603785425)) ;
#97089 = CARTESIAN_POINT('Ctrl Pts',(30.0562477831581,256.952359843337,20.1063603785425)) ;
#97090 = CARTESIAN_POINT('Ctrl Pts',(29.7424371293616,256.748815981268,20.1063603785425)) ;
#97091 = CARTESIAN_POINT('Ctrl Pts',(29.5940323940009,256.523626711091,20.1063603785425)) ;
#97092 = CARTESIAN_POINT('Ctrl Pts',(29.493524415239,256.258021637289,20.1063603785425)) ;
#97093 = CARTESIAN_POINT('Ctrl Pts',(29.3619731302367,255.972670333182,20.1063603785425)) ;
#97094 = CARTESIAN_POINT('Ctrl Pts',(29.2709280858246,255.787069709302,20.1063603785425)) ;
#97095 = CARTESIAN_POINT('Ctrl Pts',(29.2133075051975,255.671997914687,20.1063603785425)) ;
#97096 = CARTESIAN_POINT('Ctrl Pts',(30.6479033156902,257.074838666173,20.0802089331821)) ;
#97097 = CARTESIAN_POINT('Ctrl Pts',(30.6150168496632,257.069398862557,20.0802089331821)) ;
#97098 = CARTESIAN_POINT('Ctrl Pts',(30.5821303836361,257.06395905894,20.0802089331821)) ;
#97099 = CARTESIAN_POINT('Ctrl Pts',(30.3513532542168,257.026024900111,20.0802089331821)) ;
#97100 = CARTESIAN_POINT('Ctrl Pts',(30.0541250166344,256.958485975665,20.0802089331821)) ;
#97101 = CARTESIAN_POINT('Ctrl Pts',(29.7381084482561,256.753746292952,20.0802089331821)) ;
#97102 = CARTESIAN_POINT('Ctrl Pts',(29.5884325466772,256.526156268995,20.0802089331821)) ;
#97103 = CARTESIAN_POINT('Ctrl Pts',(29.4880187414454,256.260571687147,20.0802089331821)) ;
#97104 = CARTESIAN_POINT('Ctrl Pts',(29.3567315627788,255.975220870925,20.0802089331821)) ;
#97105 = CARTESIAN_POINT('Ctrl Pts',(29.2652966109379,255.79035111116,20.0802089331821)) ;
#97106 = CARTESIAN_POINT('Ctrl Pts',(29.2079462293641,255.674682498059,20.0802089331821)) ;
#97107 = CARTESIAN_POINT('Ctrl Pts',(30.6439632681149,257.098658320313,20.046158428686)) ;
#97108 = CARTESIAN_POINT('Ctrl Pts',(30.6110768020878,257.093218516696,20.046158428686)) ;
#97109 = CARTESIAN_POINT('Ctrl Pts',(30.5781903360608,257.087778713079,20.046158428686)) ;
#97110 = CARTESIAN_POINT('Ctrl Pts',(30.346034219779,257.049493628584,20.046158428686)) ;
#97111 = CARTESIAN_POINT('Ctrl Pts',(30.0466036859445,256.982025168442,20.046158428686)) ;
#97112 = CARTESIAN_POINT('Ctrl Pts',(29.7209071767827,256.771897391692,20.046158428686)) ;
#97113 = CARTESIAN_POINT('Ctrl Pts',(29.5657738058475,256.535373232231,20.046158428686)) ;
#97114 = CARTESIAN_POINT('Ctrl Pts',(29.4658953017976,256.269858985514,20.046158428686)) ;
#97115 = CARTESIAN_POINT('Ctrl Pts',(29.3348931712675,255.985906642723,20.046158428686)) ;
#97116 = CARTESIAN_POINT('Ctrl Pts',(29.2438344960392,255.800828730593,20.046158428686)) ;
#97117 = CARTESIAN_POINT('Ctrl Pts',(29.1863581460773,255.685492426746,20.046158428686)) ;
#97118 = CARTESIAN_POINT('Ctrl Pts',(30.6397271501173,257.124267875443,20.0298289990098)) ;
#97119 = CARTESIAN_POINT('Ctrl Pts',(30.6068406840902,257.118828071826,20.0298289990098)) ;
#97120 = CARTESIAN_POINT('Ctrl Pts',(30.5739542180632,257.113388268209,20.0298289990098)) ;
#97121 = CARTESIAN_POINT('Ctrl Pts',(30.3405240702817,257.074938910687,20.0298289990098)) ;
#97122 = CARTESIAN_POINT('Ctrl Pts',(30.0383483709799,257.007518825832,20.0298289990098)) ;
#97123 = CARTESIAN_POINT('Ctrl Pts',(29.7023756891282,256.791692300423,20.0298289990098)) ;
#97124 = CARTESIAN_POINT('Ctrl Pts',(29.5414304926382,256.545442119708,20.0298289990098)) ;
#97125 = CARTESIAN_POINT('Ctrl Pts',(29.4421018414893,256.280005496473,20.0298289990098)) ;
#97126 = CARTESIAN_POINT('Ctrl Pts',(29.3115342048088,255.997327031355,20.0298289990098)) ;
#97127 = CARTESIAN_POINT('Ctrl Pts',(29.2205599742109,255.812543583895,20.0298289990098)) ;
#97128 = CARTESIAN_POINT('Ctrl Pts',(29.1631478506694,255.697114655307,20.0298289990098)) ;
#97129 = CARTESIAN_POINT('Ctrl Pts',(30.636200901783,257.145585896132,20.0236265255013)) ;
#97130 = CARTESIAN_POINT('Ctrl Pts',(30.603314435756,257.140146092516,20.0236265255013)) ;
#97131 = CARTESIAN_POINT('Ctrl Pts',(30.5704279697289,257.134706288899,20.0236265255013)) ;
#97132 = CARTESIAN_POINT('Ctrl Pts',(30.3357835140935,257.095963136756,20.0236265255013)) ;
#97133 = CARTESIAN_POINT('Ctrl Pts',(30.0316008933358,257.028603509364,20.0236265255013)) ;
#97134 = CARTESIAN_POINT('Ctrl Pts',(29.6869773794647,256.807963737247,20.0236265255013)) ;
#97135 = CARTESIAN_POINT('Ctrl Pts',(29.5211531836893,256.553706245957,20.0236265255013)) ;
#97136 = CARTESIAN_POINT('Ctrl Pts',(29.4223011707526,256.288332761635,20.0236265255013)) ;
#97137 = CARTESIAN_POINT('Ctrl Pts',(29.2920008308411,256.006884035643,20.0236265255013)) ;
#97138 = CARTESIAN_POINT('Ctrl Pts',(29.2013328910854,255.821963624557,20.0236265255013)) ;
#97139 = CARTESIAN_POINT('Ctrl Pts',(29.1438270325134,255.706789282908,20.0236265255013)) ;
#97140 = CARTESIAN_POINT('Ctrl Pts',(30.6343935863363,257.156512065941,20.0217377892707)) ;
#97141 = CARTESIAN_POINT('Ctrl Pts',(30.6015071203092,257.151072262324,20.0217377892707)) ;
#97142 = CARTESIAN_POINT('Ctrl Pts',(30.5686206542822,257.145632458708,20.0217377892707)) ;
#97143 = CARTESIAN_POINT('Ctrl Pts',(30.3333675899215,257.106752783705,20.0217377892707)) ;
#97144 = CARTESIAN_POINT('Ctrl Pts',(30.0281314560414,257.039422335769,20.0217377892707)) ;
#97145 = CARTESIAN_POINT('Ctrl Pts',(29.6790827674713,256.816321837849,20.0217377892707)) ;
#97146 = CARTESIAN_POINT('Ctrl Pts',(29.510761605924,256.557952389036,20.0217377892707)) ;
#97147 = CARTESIAN_POINT('Ctrl Pts',(29.4121521913412,256.292611397608,20.0217377892707)) ;
#97148 = CARTESIAN_POINT('Ctrl Pts',(29.2819972974163,256.011777796768,20.0217377892707)) ;
#97149 = CARTESIAN_POINT('Ctrl Pts',(29.191465219267,255.826821384756,20.0217377892707)) ;
#97150 = CARTESIAN_POINT('Ctrl Pts',(29.1339244931038,255.711747840063,20.0217377892707)) ;
#97151 = CARTESIAN_POINT('Ctrl Pts',(30.6331727374444,257.163892737824,20.0213203435597)) ;
#97152 = CARTESIAN_POINT('Ctrl Pts',(30.6002862714174,257.158452934208,20.0213203435597)) ;
#97153 = CARTESIAN_POINT('Ctrl Pts',(30.5673998053903,257.153013130591,20.0213203435597)) ;
#97154 = CARTESIAN_POINT('Ctrl Pts',(30.3317495219155,257.114055428562,20.0213203435596)) ;
#97155 = CARTESIAN_POINT('Ctrl Pts',(30.0257765890063,257.04674286674,20.0213203435596)) ;
#97156 = CARTESIAN_POINT('Ctrl Pts',(29.6737474166104,256.821986417431,20.0213203435596)) ;
#97157 = CARTESIAN_POINT('Ctrl Pts',(29.5037432587571,256.560831292509,20.0213203435596)) ;
#97158 = CARTESIAN_POINT('Ctrl Pts',(29.4052960096356,256.295512383638,20.0213203435596)) ;
#97159 = CARTESIAN_POINT('Ctrl Pts',(29.2752478960571,256.015078997478,20.0213203435596)) ;
#97160 = CARTESIAN_POINT('Ctrl Pts',(29.1847862627121,255.830132800747,20.0213203435596)) ;
#97161 = CARTESIAN_POINT('Ctrl Pts',(29.1272352876938,255.715097365469,20.0213203435596)) ;
#97162 = CARTESIAN_POINT('Ctrl Pts',(30.6325623929059,257.167582590684,20.0213203435597)) ;
#97163 = CARTESIAN_POINT('Ctrl Pts',(30.5996759268789,257.162142787068,20.0213203435597)) ;
#97164 = CARTESIAN_POINT('Ctrl Pts',(30.5667894608518,257.156702983451,20.0213203435597)) ;
#97165 = CARTESIAN_POINT('Ctrl Pts',(30.3309225628221,257.117687857779,20.0213203435596)) ;
#97166 = CARTESIAN_POINT('Ctrl Pts',(30.0246139021395,257.050386605117,20.0213203435596)) ;
#97167 = CARTESIAN_POINT('Ctrl Pts',(29.6710833447946,256.82479414277,20.0213203435596)) ;
#97168 = CARTESIAN_POINT('Ctrl Pts',(29.5002329804407,256.562256782507,20.0213203435596)) ;
#97169 = CARTESIAN_POINT('Ctrl Pts',(29.4018690227886,256.296948740307,20.0213203435596)) ;
#97170 = CARTESIAN_POINT('Ctrl Pts',(29.2718632248773,256.016735290733,20.0213203435596)) ;
#97171 = CARTESIAN_POINT('Ctrl Pts',(29.1814644817151,255.831749398905,20.0213203435596)) ;
#97172 = CARTESIAN_POINT('Ctrl Pts',(29.1238911228127,255.716771908939,20.0213203435596)) ;
#97173 = CARTESIAN_POINT('Ctrl Pts',(30.6325623929049,257.167582590684,20.0213203435597)) ;
#97174 = CARTESIAN_POINT('Ctrl Pts',(30.632363372354,257.167303914202,20.0213203435597)) ;
#97175 = CARTESIAN_POINT('Ctrl Pts',(30.6321643395558,257.167025244098,20.0213212207922)) ;
#97176 = CARTESIAN_POINT('Ctrl Pts',(30.6224905315818,257.153481996673,20.0214065029112)) ;
#97177 = CARTESIAN_POINT('Ctrl Pts',(30.6129575908717,257.140181501842,20.0234788659747)) ;
#97178 = CARTESIAN_POINT('Ctrl Pts',(30.5951908320103,257.115407134294,20.0315134132315)) ;
#97179 = CARTESIAN_POINT('Ctrl Pts',(30.5867361809595,257.103625687996,20.0373513069104)) ;
#97180 = CARTESIAN_POINT('Ctrl Pts',(30.5706299595814,257.081105304138,20.0540392142044)) ;
#97181 = CARTESIAN_POINT('Ctrl Pts',(30.5642378623769,257.072204164288,20.0642748433054)) ;
#97182 = CARTESIAN_POINT('Ctrl Pts',(30.5567091101513,257.061696581791,20.081623449277)) ;
#97183 = CARTESIAN_POINT('Ctrl Pts',(30.5542798478843,257.058313743444,20.0891865612042)) ;
#97184 = CARTESIAN_POINT('Ctrl Pts',(30.5510510049725,257.053787395618,20.1050494520494)) ;
#97185 = CARTESIAN_POINT('Ctrl Pts',(30.550222414244,257.052603729947,20.1131190766524)) ;
#97186 = CARTESIAN_POINT('Ctrl Pts',(30.550222414244,257.052603729947,20.1213203435596)) ;
#97187 = CARTESIAN_POINT('Origin',(32.3250488694829,246.935614134431,20.1213203435596)) ;
#97188 = CARTESIAN_POINT('Origin',(28.7065616828874,254.062789469896,20.0213203435596)) ;
#97189 = CARTESIAN_POINT('',(28.7065616828874,254.062789469896,20.0213203435596)) ;
#97190 = CARTESIAN_POINT('Origin',(28.7971429244132,255.86605864576,20.0213203435596)) ;
#97191 = CARTESIAN_POINT('',(28.7971429244132,255.86605864576,20.0213203435596)) ;
#97192 = CARTESIAN_POINT('Origin',(58.2408539117876,252.51941903599,20.1213203435596)) ;
#97193 = CARTESIAN_POINT('',(66.856524993511,256.02214694455,20.0213203435596)) ;
#97194 = CARTESIAN_POINT('',(64.8184058153773,255.19354324572,20.0213203435596)) ;
#97195 = CARTESIAN_POINT('',(58.2408539117876,252.51941903599,20.0213203435596)) ;
#97196 = CARTESIAN_POINT('Origin',(64.8184058153773,255.19354324572,20.1213203435596)) ;
#97197 = CARTESIAN_POINT('',(66.5910039984262,256.02214694455,20.1213203435596)) ;
#97198 = CARTESIAN_POINT('',(58.2031921065628,252.61205589921,20.1213203435596)) ;
#97199 = CARTESIAN_POINT('Origin',(66.856524993511,256.02214694455,20.1213203435596)) ;
#97200 = CARTESIAN_POINT('Origin',(64.4170577015585,257.013919968902,20.1213203435596)) ;
#97201 = CARTESIAN_POINT('',(64.9184058153773,256.70214694455,20.1213203435596)) ;
#97202 = CARTESIAN_POINT('',(64.3793958963336,256.921283105682,20.1213203435596)) ;
#97203 = CARTESIAN_POINT('',(64.8184058153773,256.85075064338,20.0213203435596)) ;
#97204 = CARTESIAN_POINT('Origin',(64.8184058153773,256.85075064338,20.1213203435596)) ;
#97205 = CARTESIAN_POINT('',(64.4170577015585,257.013919968902,20.0213203435596)) ;
#97206 = CARTESIAN_POINT('Origin',(64.8184058153773,248.269379137783,20.1213203435596)) ;
#97207 = CARTESIAN_POINT('',(64.8184058153773,255.72214694455,20.0213203435596)) ;
#97208 = CARTESIAN_POINT('',(64.8184058153773,248.269379137783,20.0213203435596)) ;
#97209 = CARTESIAN_POINT('Origin',(64.8184058153773,255.72214694455,20.1213203435596)) ;
#97210 = CARTESIAN_POINT('Origin',(59.2625927064781,255.72214694455,20.1213203435596)) ;
#97211 = CARTESIAN_POINT('',(63.2110039984262,255.72214694455,20.0213203435596)) ;
#97212 = CARTESIAN_POINT('',(59.2625927064781,255.72214694455,20.0213203435596)) ;
#97213 = CARTESIAN_POINT('Origin',(63.2110039984262,255.72214694455,20.1213203435596)) ;
#97214 = CARTESIAN_POINT('Origin',(63.2110039984262,248.469379137783,20.1213203435596)) ;
#97215 = CARTESIAN_POINT('',(63.2110039984262,256.32214694455,20.0213203435596)) ;
#97216 = CARTESIAN_POINT('',(63.2110039984262,248.469379137783,20.0213203435596)) ;
#97217 = CARTESIAN_POINT('Origin',(63.2110039984262,256.32214694455,20.1213203435596)) ;
#97218 = CARTESIAN_POINT('Origin',(60.0662936149535,256.32214694455,20.1213203435596)) ;
#97219 = CARTESIAN_POINT('',(64.8184058153773,256.32214694455,20.0213203435596)) ;
#97220 = CARTESIAN_POINT('',(60.0662936149535,256.32214694455,20.0213203435596)) ;
#97221 = CARTESIAN_POINT('Origin',(64.8184058153773,256.32214694455,20.1213203435596)) ;
#97222 = CARTESIAN_POINT('Origin',(64.8184058153773,248.709379137783,20.1213203435596)) ;
#97223 = CARTESIAN_POINT('',(64.9184058153773,248.709379137783,20.1213203435596)) ;
#97224 = CARTESIAN_POINT('',(64.8184058153773,248.709379137783,20.0213203435596)) ;
#97225 = CARTESIAN_POINT('Origin',(64.9184058153773,256.70214694455,20.0213203435596)) ;
#97226 = CARTESIAN_POINT('',(64.9184058153773,256.70214694455,20.0213203435596)) ;
#97227 = CARTESIAN_POINT('Origin',(66.5910039984262,256.02214694455,20.0213203435596)) ;
#97228 = CARTESIAN_POINT('',(66.5910039984262,256.02214694455,20.0213203435596)) ;
#97229 = CARTESIAN_POINT('Origin',(64.9184058153773,255.34214694455,20.0213203435596)) ;
#97230 = CARTESIAN_POINT('Origin',(55.2141814145299,240.716611331017,20.0213203435596)) ;
#97231 = CARTESIAN_POINT('',(68.6350889359327,257.,20.0213203435596)) ;
#97232 = CARTESIAN_POINT('',(68.6350889359328,261.466666666667,20.0213203435596)) ;
#97233 = CARTESIAN_POINT('',(68.6350889359325,252.258305665508,20.0213203435596)) ;
#97234 = CARTESIAN_POINT('',(68.65,256.631336165532,20.0213203435596)) ;
#97235 = CARTESIAN_POINT('Origin',(73.2,257.,20.0213203435596)) ;
#97236 = CARTESIAN_POINT('',(68.65,255.5,20.0213203435596)) ;
#97237 = CARTESIAN_POINT('',(68.65,248.108305665508,20.0213203435596)) ;
#97238 = CARTESIAN_POINT('Origin',(73.2,255.5,20.0213203435596)) ;
#97239 = CARTESIAN_POINT('',(55.75,255.5,20.0213203435596)) ;
#97240 = CARTESIAN_POINT('Origin',(51.2,255.5,20.0213203435596)) ;
#97241 = CARTESIAN_POINT('',(55.75,256.631336165532,20.0213203435596)) ;
#97242 = CARTESIAN_POINT('',(55.75,248.684378986433,20.0213203435596)) ;
#97243 = CARTESIAN_POINT('',(55.7649110640674,257.,20.0213203435596)) ;
#97244 = CARTESIAN_POINT('Origin',(51.2,257.,20.0213203435596)) ;
#97245 = CARTESIAN_POINT('',(55.7649110640674,248.858305665508,20.0213203435596)) ;
#97246 = CARTESIAN_POINT('',(56.2695111541429,261.559687576257,20.0213203435596)) ;
#97247 = CARTESIAN_POINT('Ctrl Pts',(56.2695111541429,261.559687576257,20.0213203435596)) ;
#97248 = CARTESIAN_POINT('Ctrl Pts',(56.2620293235127,261.559687576257,20.0213203435596)) ;
#97249 = CARTESIAN_POINT('Ctrl Pts',(56.2545427899591,261.559686365099,20.0213203435619)) ;
#97250 = CARTESIAN_POINT('Ctrl Pts',(56.2469607049508,261.559621906612,20.0213203435607)) ;
#97251 = CARTESIAN_POINT('Ctrl Pts',(56.2429395471374,261.559587721062,20.02132034356)) ;
#97252 = CARTESIAN_POINT('Ctrl Pts',(56.2388941346124,261.559536451947,20.0213203435599)) ;
#97253 = CARTESIAN_POINT('Ctrl Pts',(56.2348134639309,261.559459472082,20.0213203435598)) ;
#97254 = CARTESIAN_POINT('Ctrl Pts',(56.2307620197578,261.559383043561,20.0213203435597)) ;
#97255 = CARTESIAN_POINT('Ctrl Pts',(56.2266758214071,261.559281270923,20.0213203435597)) ;
#97256 = CARTESIAN_POINT('Ctrl Pts',(56.2225540991302,261.559148465343,20.0213203435599)) ;
#97257 = CARTESIAN_POINT('Ctrl Pts',(56.2136298089806,261.55886091673,20.0213203435605)) ;
#97258 = CARTESIAN_POINT('Ctrl Pts',(56.2045275984428,261.558424861714,20.0213203435596)) ;
#97259 = CARTESIAN_POINT('Ctrl Pts',(56.1952509539508,261.557785784382,20.0213203435596)) ;
#97260 = CARTESIAN_POINT('Ctrl Pts',(56.184797181305,261.557065613512,20.0213203435597)) ;
#97261 = CARTESIAN_POINT('Ctrl Pts',(56.1741226379547,261.55608811322,20.0213203435597)) ;
#97262 = CARTESIAN_POINT('Ctrl Pts',(56.1632977864506,261.554797675761,20.0213203435596)) ;
#97263 = CARTESIAN_POINT('Ctrl Pts',(56.1471254853081,261.552869765418,20.0213203435596)) ;
#97264 = CARTESIAN_POINT('Ctrl Pts',(56.1306227005856,261.550241630897,20.0213203435595)) ;
#97265 = CARTESIAN_POINT('Ctrl Pts',(56.1141385164753,261.546788423019,20.0213203435597)) ;
#97266 = CARTESIAN_POINT('Ctrl Pts',(56.1033359290827,261.544525430829,20.0213203435598)) ;
#97267 = CARTESIAN_POINT('Ctrl Pts',(56.0925439545573,261.541909763607,20.0213203435596)) ;
#97268 = CARTESIAN_POINT('Ctrl Pts',(56.0818401088614,261.538912650206,20.0213203435596)) ;
#97269 = CARTESIAN_POINT('Ctrl Pts',(56.0716896860479,261.536070497106,20.0213203435596)) ;
#97270 = CARTESIAN_POINT('Ctrl Pts',(56.0616200212418,261.532885652269,20.02132034356)) ;
#97271 = CARTESIAN_POINT('Ctrl Pts',(56.051650953882,261.52933162481,20.0213203435597)) ;
#97272 = CARTESIAN_POINT('Ctrl Pts',(56.048894385141,261.528348892861,20.0213203435597)) ;
#97273 = CARTESIAN_POINT('Ctrl Pts',(56.0461448965502,261.527337901265,20.0213203435597)) ;
#97274 = CARTESIAN_POINT('Ctrl Pts',(56.0434023233072,261.526297906278,20.0213203435596)) ;
#97275 = CARTESIAN_POINT('Ctrl Pts',(56.0358527224709,261.523435066775,20.0213203435596)) ;
#97276 = CARTESIAN_POINT('Ctrl Pts',(56.0283554905343,261.52035255579,20.0213203435597)) ;
#97277 = CARTESIAN_POINT('Ctrl Pts',(56.0209014644149,261.517041751319,20.0213203435596)) ;
#97278 = CARTESIAN_POINT('Ctrl Pts',(56.0157914271727,261.514772060567,20.0213203435596)) ;
#97279 = CARTESIAN_POINT('Ctrl Pts',(56.0107040385674,261.512396296763,20.0213203435596)) ;
#97280 = CARTESIAN_POINT('Ctrl Pts',(56.0056387442236,261.509913017798,20.0213203435596)) ;
#97281 = CARTESIAN_POINT('Ctrl Pts',(56.0005924317678,261.507439044772,20.0213203435596)) ;
#97282 = CARTESIAN_POINT('Ctrl Pts',(55.995568049491,261.504858361603,20.0213203435597)) ;
#97283 = CARTESIAN_POINT('Ctrl Pts',(55.9905731854363,261.502174888351,20.0213203435597)) ;
#97284 = CARTESIAN_POINT('Ctrl Pts',(55.9832419391146,261.498236201893,20.0213203435597)) ;
#97285 = CARTESIAN_POINT('Ctrl Pts',(55.9759714235957,261.49407441593,20.0213203435596)) ;
#97286 = CARTESIAN_POINT('Ctrl Pts',(55.9687841103927,261.489701274464,20.0213203435596)) ;
#97287 = CARTESIAN_POINT('Ctrl Pts',(55.9642788487677,261.486960035023,20.0213203435596)) ;
#97288 = CARTESIAN_POINT('Ctrl Pts',(55.9598062775265,261.484135753404,20.0213203435596)) ;
#97289 = CARTESIAN_POINT('Ctrl Pts',(55.9553742025499,261.481233192763,20.0213203435596)) ;
#97290 = CARTESIAN_POINT('Ctrl Pts',(55.947918042932,261.47635016268,20.0213203435596)) ;
#97291 = CARTESIAN_POINT('Ctrl Pts',(55.9405757308991,261.471244857424,20.0213203435596)) ;
#97292 = CARTESIAN_POINT('Ctrl Pts',(55.933384073417,261.465939267956,20.0213203435596)) ;
#97293 = CARTESIAN_POINT('Ctrl Pts',(55.9219179108755,261.45748019557,20.0213203435596)) ;
#97294 = CARTESIAN_POINT('Ctrl Pts',(55.9108347324416,261.44851198663,20.0213203435596)) ;
#97295 = CARTESIAN_POINT('Ctrl Pts',(55.9002853073786,261.439128427997,20.0213203435596)) ;
#97296 = CARTESIAN_POINT('',(68.6263598493594,261.559687576257,20.0213203435596)) ;
#97297 = CARTESIAN_POINT('',(55.2268638269143,261.559687576257,20.0213203435596)) ;
#97298 = CARTESIAN_POINT('Origin',(68.1350889359328,261.466666666667,20.0213203435596)) ;
#97299 = CARTESIAN_POINT('',(63.,254.92214694455,20.0213203435596)) ;
#97300 = CARTESIAN_POINT('',(62.4,254.92214694455,20.0213203435596)) ;
#97301 = CARTESIAN_POINT('',(58.8570907072643,254.92214694455,20.0213203435596)) ;
#97302 = CARTESIAN_POINT('',(63.,257.12214694455,20.0213203435596)) ;
#97303 = CARTESIAN_POINT('',(63.,247.869379137783,20.0213203435596)) ;
#97304 = CARTESIAN_POINT('',(62.4,257.12214694455,20.0213203435596)) ;
#97305 = CARTESIAN_POINT('',(59.057090707265,257.12214694455,20.0213203435596)) ;
#97306 = CARTESIAN_POINT('',(62.4,248.869379137783,20.0213203435596)) ;
#97307 = CARTESIAN_POINT('',(62.1889960015738,256.32214694455,20.0213203435596)) ;
#97308 = CARTESIAN_POINT('',(62.1889960015738,255.72214694455,20.0213203435596)) ;
#97309 = CARTESIAN_POINT('',(62.188996001574,248.269379137783,20.0213203435596)) ;
#97310 = CARTESIAN_POINT('',(60.5815941846227,256.32214694455,20.0213203435596)) ;
#97311 = CARTESIAN_POINT('',(58.651588708052,256.32214694455,20.0213203435596)) ;
#97312 = CARTESIAN_POINT('',(60.5815941846227,256.85075064338,20.0213203435596)) ;
#97313 = CARTESIAN_POINT('',(60.5815941846227,248.469379137783,20.0213203435596)) ;
#97314 = CARTESIAN_POINT('',(58.5434750064891,256.02214694455,20.0213203435596)) ;
#97315 = CARTESIAN_POINT('',(55.3952199758442,254.742214057778,20.0213203435596)) ;
#97316 = CARTESIAN_POINT('',(60.5815941846227,255.19354324572,20.0213203435596)) ;
#97317 = CARTESIAN_POINT('',(59.8988255825664,255.471124947113,20.0213203435596)) ;
#97318 = CARTESIAN_POINT('',(60.5815941846227,255.72214694455,20.0213203435596)) ;
#97319 = CARTESIAN_POINT('',(60.5815941846227,248.029379137783,20.0213203435596)) ;
#97320 = CARTESIAN_POINT('',(57.8478877995763,255.72214694455,20.0213203435596)) ;
#97321 = CARTESIAN_POINT('Origin',(58.8570907072643,254.92214694455,20.1213203435596)) ;
#97322 = CARTESIAN_POINT('Origin',(62.4,254.92214694455,20.1213203435596)) ;
#97323 = CARTESIAN_POINT('Origin',(63.,254.92214694455,20.1213203435596)) ;
#97324 = CARTESIAN_POINT('Origin',(62.4,248.869379137783,20.1213203435596)) ;
#97325 = CARTESIAN_POINT('Origin',(62.4,257.12214694455,20.1213203435596)) ;
#97326 = CARTESIAN_POINT('Origin',(59.057090707265,257.12214694455,20.1213203435596)) ;
#97327 = CARTESIAN_POINT('',(62.9,257.02214694455,20.1213203435596)) ;
#97328 = CARTESIAN_POINT('',(59.057090707265,257.02214694455,20.1213203435596)) ;
#97329 = CARTESIAN_POINT('Origin',(63.,257.12214694455,20.1213203435596)) ;
#97330 = CARTESIAN_POINT('Origin',(63.,247.869379137783,20.1213203435596)) ;
#97331 = CARTESIAN_POINT('',(62.9,247.869379137783,20.1213203435596)) ;
#97332 = CARTESIAN_POINT('Origin',(62.9,255.02214694455,20.0213203435596)) ;
#97333 = CARTESIAN_POINT('',(62.9,257.02214694455,20.0213203435596)) ;
#97334 = CARTESIAN_POINT('Origin',(62.188996001574,248.269379137783,20.1213203435596)) ;
#97335 = CARTESIAN_POINT('',(62.0889960015738,255.82214694455,20.1213203435596)) ;
#97336 = CARTESIAN_POINT('Origin',(62.1889960015738,255.72214694455,20.1213203435596)) ;
#97337 = CARTESIAN_POINT('',(62.0889960015738,256.22214694455,20.1213203435596)) ;
#97338 = CARTESIAN_POINT('',(62.088996001574,248.269379137783,20.1213203435596)) ;
#97339 = CARTESIAN_POINT('Origin',(62.1889960015738,256.32214694455,20.1213203435596)) ;
#97340 = CARTESIAN_POINT('Origin',(57.8478877995763,255.72214694455,20.1213203435596)) ;
#97341 = CARTESIAN_POINT('Origin',(60.5815941846227,255.72214694455,20.1213203435596)) ;
#97342 = CARTESIAN_POINT('',(57.8478877995763,255.82214694455,20.1213203435596)) ;
#97343 = CARTESIAN_POINT('Origin',(60.5815941846227,248.029379137783,20.1213203435596)) ;
#97344 = CARTESIAN_POINT('Origin',(60.5815941846227,255.19354324572,20.1213203435596)) ;
#97345 = CARTESIAN_POINT('Origin',(59.8988255825664,255.471124947113,20.1213203435596)) ;
#97346 = CARTESIAN_POINT('Origin',(58.5434750064891,256.02214694455,20.1213203435596)) ;
#97347 = CARTESIAN_POINT('Origin',(55.3952199758442,254.742214057778,20.1213203435596)) ;
#97348 = CARTESIAN_POINT('Origin',(60.5815941846227,256.85075064338,20.1213203435596)) ;
#97349 = CARTESIAN_POINT('Origin',(60.5815941846227,248.469379137783,20.1213203435596)) ;
#97350 = CARTESIAN_POINT('Origin',(60.5815941846227,256.32214694455,20.1213203435596)) ;
#97351 = CARTESIAN_POINT('Origin',(58.651588708052,256.32214694455,20.1213203435596)) ;
#97352 = CARTESIAN_POINT('',(58.651588708052,256.22214694455,20.1213203435596)) ;
#97353 = CARTESIAN_POINT('Origin',(62.0889960015738,256.22214694455,20.0213203435596)) ;
#97354 = CARTESIAN_POINT('',(62.0889960015738,256.22214694455,20.0213203435596)) ;
#97355 = CARTESIAN_POINT('Origin',(62.0889960015738,255.82214694455,20.0213203435596)) ;
#97356 = CARTESIAN_POINT('',(62.0889960015738,255.82214694455,20.0213203435596)) ;
#97357 = CARTESIAN_POINT('Origin',(64.9712721217948,249.52834685842,18.1213203435596)) ;
#97358 = CARTESIAN_POINT('Origin',(74.8283628290596,249.52834685842,18.1213203435596)) ;
#97359 = CARTESIAN_POINT('Origin',(74.2283628290596,249.52834685842,18.1213203435596)) ;
#97360 = CARTESIAN_POINT('Origin',(74.8283628290596,247.98917342921,18.1213203435596)) ;
#97361 = CARTESIAN_POINT('',(74.7283628290596,246.92834685842,18.1213203435596)) ;
#97362 = CARTESIAN_POINT('Origin',(74.8283628290596,246.82834685842,18.1213203435596)) ;
#97363 = CARTESIAN_POINT('',(74.7283628290596,247.98917342921,18.1213203435596)) ;
#97364 = CARTESIAN_POINT('Origin',(74.2283628290596,249.23917342921,18.1213203435596)) ;
#97365 = CARTESIAN_POINT('Origin',(74.2283628290596,246.82834685842,18.1213203435596)) ;
#97366 = CARTESIAN_POINT('Origin',(64.7712721217948,246.82834685842,18.1213203435596)) ;
#97367 = CARTESIAN_POINT('',(64.7712721217948,246.92834685842,18.1213203435596)) ;
#97368 = CARTESIAN_POINT('Origin',(77.0348658990794,248.670975591968,18.1213203435596)) ;
#97369 = CARTESIAN_POINT('',(76.9348658990794,248.291951183936,18.1213203435596)) ;
#97370 = CARTESIAN_POINT('',(76.9348658990794,249.302824616567,18.1213203435596)) ;
#97371 = CARTESIAN_POINT('',(76.9348658990794,248.670975591968,18.1213203435596)) ;
#97372 = CARTESIAN_POINT('Origin',(77.0348658990794,249.302824616567,18.1213203435596)) ;
#97373 = CARTESIAN_POINT('Origin',(77.0348658990794,248.391951183936,18.1213203435596)) ;
#97374 = CARTESIAN_POINT('Origin',(66.3218485782223,248.391951183936,18.1213203435596)) ;
#97375 = CARTESIAN_POINT('Origin',(77.578119440745,248.391951183936,18.1213203435596)) ;
#97376 = CARTESIAN_POINT('',(66.3218485782223,248.291951183936,18.1213203435596)) ;
#97377 = CARTESIAN_POINT('Origin',(75.7388649854292,243.867931095515,18.1213203435596)) ;
#97378 = CARTESIAN_POINT('Origin',(76.7495157419148,246.353832005802,18.1213203435596)) ;
#97379 = CARTESIAN_POINT('Origin',(74.3655697550003,252.217631603154,18.1213203435596)) ;
#97380 = CARTESIAN_POINT('Origin',(75.9209120430846,248.391951183936,18.1213203435596)) ;
#97381 = CARTESIAN_POINT('Origin',(65.8745236568046,248.391951183936,18.1213203435596)) ;
#97382 = CARTESIAN_POINT('Origin',(76.4348658990794,248.391951183936,18.1213203435596)) ;
#97383 = CARTESIAN_POINT('Origin',(68.1060880979734,244.423124592531,18.1213203435596)) ;
#97384 = CARTESIAN_POINT('Origin',(76.1283346412558,249.472090948443,18.1213203435596)) ;
#97385 = CARTESIAN_POINT('Origin',(75.2544545302692,248.922096472997,18.1213203435596)) ;
#97386 = CARTESIAN_POINT('Origin',(76.2348658990794,249.302824616567,18.1213203435596)) ;
#97387 = CARTESIAN_POINT('Origin',(76.4348658990794,249.302824616567,18.1213203435596)) ;
#97388 = CARTESIAN_POINT('Origin',(76.4348658990794,249.176412308284,18.1213203435596)) ;
#97389 = CARTESIAN_POINT('Origin',(76.2348658990794,249.302824616567,18.1213203435596)) ;
#97390 = CARTESIAN_POINT('',(75.8620064966968,249.895256778131,18.1213203435596)) ;
#97391 = CARTESIAN_POINT('Origin',(75.8087408677849,249.979889944069,18.1213203435596)) ;
#97392 = CARTESIAN_POINT('Origin',(76.2348658990794,249.302824616567,18.1213203435596)) ;
#97393 = CARTESIAN_POINT('Origin',(68.223434379996,245.20592082588,18.1213203435596)) ;
#97394 = CARTESIAN_POINT('',(74.9881263857102,249.345262302685,18.1213203435596)) ;
#97395 = CARTESIAN_POINT('Origin',(74.9348607567984,249.429895468622,18.1213203435596)) ;
#97396 = CARTESIAN_POINT('',(68.2767000089078,245.121287659942,18.1213203435596)) ;
#97397 = CARTESIAN_POINT('Origin',(75.8620064966968,249.895256778131,18.0213203435596)) ;
#97398 = CARTESIAN_POINT('',(74.9881263857102,249.345262302685,18.0213203435596)) ;
#97399 = CARTESIAN_POINT('',(75.8620064966968,249.895256778131,18.0213203435596)) ;
#97400 = CARTESIAN_POINT('Origin',(76.2348658990794,249.302824616567,18.0213203435596)) ;
#97401 = CARTESIAN_POINT('',(76.9348658990794,249.302824616567,18.0213203435596)) ;
#97402 = CARTESIAN_POINT('Origin',(76.9348658990794,248.291951183936,18.0213203435596)) ;
#97403 = CARTESIAN_POINT('',(76.9348658990794,248.291951183936,18.0213203435596)) ;
#97404 = CARTESIAN_POINT('Origin',(77.4295157419147,248.291951183936,18.0213203435596)) ;
#97405 = CARTESIAN_POINT('Origin',(71.0478693800126,252.145540430945,18.1213203435596)) ;
#97406 = CARTESIAN_POINT('',(74.0601316280705,247.171652088685,18.1213203435596)) ;
#97407 = CARTESIAN_POINT('Origin',(74.19803042292,247.140284551659,18.1213203435596)) ;
#97408 = CARTESIAN_POINT('',(73.8470691124233,247.510184752435,18.1213203435596)) ;
#97409 = CARTESIAN_POINT('',(70.963236214075,252.092274802033,18.1213203435596)) ;
#97410 = CARTESIAN_POINT('Origin',(73.8784366494491,247.648083547285,18.1213203435596)) ;
#97411 = CARTESIAN_POINT('Origin',(72.0133921147013,248.637481603717,18.1213203435596)) ;
#97412 = CARTESIAN_POINT('',(72.1133921147013,247.214089774802,18.1213203435596)) ;
#97413 = CARTESIAN_POINT('',(72.1133921147013,248.637481603717,18.1213203435596)) ;
#97414 = CARTESIAN_POINT('Origin',(72.0133921147013,247.214089774802,18.1213203435596)) ;
#97415 = CARTESIAN_POINT('Origin',(72.0133921147013,248.124963207434,18.1213203435596)) ;
#97416 = CARTESIAN_POINT('Origin',(63.416461843198,248.124963207434,18.1213203435596)) ;
#97417 = CARTESIAN_POINT('Origin',(71.4701385730357,248.124963207434,18.1213203435596)) ;
#97418 = CARTESIAN_POINT('Origin',(70.8466068278818,246.591260172113,18.1213203435596)) ;
#97419 = CARTESIAN_POINT('Origin',(72.2987422718658,250.163082385568,18.1213203435596)) ;
#97420 = CARTESIAN_POINT('Origin',(71.6675838322311,251.715544825786,18.1213203435596)) ;
#97421 = CARTESIAN_POINT('Origin',(73.1273459706961,248.124963207434,18.1213203435596)) ;
#97422 = CARTESIAN_POINT('Origin',(63.8637867646156,248.124963207434,18.1213203435596)) ;
#97423 = CARTESIAN_POINT('Origin',(72.6133921147013,248.124963207434,18.1213203435596)) ;
#97424 = CARTESIAN_POINT('Origin',(72.8133921147013,247.214089774802,18.1213203435596)) ;
#97425 = CARTESIAN_POINT('',(73.1862515170839,246.621657613239,18.1213203435596)) ;
#97426 = CARTESIAN_POINT('Origin',(73.2395171459957,246.537024447301,18.1213203435596)) ;
#97427 = CARTESIAN_POINT('Origin',(72.8133921147013,247.214089774802,18.1213203435596)) ;
#97428 = CARTESIAN_POINT('Origin',(67.3503775087141,242.830572927334,18.1213203435596)) ;
#97429 = CARTESIAN_POINT('',(67.2971118798023,242.915206093271,18.1213203435596)) ;
#97430 = CARTESIAN_POINT('Origin',(67.4677237907363,243.613369160683,18.1213203435596)) ;
#97431 = CARTESIAN_POINT('',(67.5209894196481,243.528735994745,18.1213203435596)) ;
#97432 = CARTESIAN_POINT('Origin',(72.9199233725249,247.044823442927,18.1213203435596)) ;
#97433 = CARTESIAN_POINT('Origin',(72.8133921147013,247.214089774802,18.1213203435596)) ;
#97434 = CARTESIAN_POINT('Origin',(72.6133921147013,247.214089774802,18.1213203435596)) ;
#97435 = CARTESIAN_POINT('Origin',(72.6133921147013,248.132044887401,18.1213203435596)) ;
#97436 = CARTESIAN_POINT('Origin',(73.8470691124233,247.510184752435,18.0213203435596)) ;
#97437 = CARTESIAN_POINT('',(73.8470691124233,247.510184752435,18.0213203435596)) ;
#97438 = CARTESIAN_POINT('Origin',(74.0601316280705,247.171652088685,18.0213203435596)) ;
#97439 = CARTESIAN_POINT('',(74.0601316280705,247.171652088685,18.0213203435596)) ;
#97440 = CARTESIAN_POINT('Origin',(73.1862515170839,246.621657613239,18.0213203435596)) ;
#97441 = CARTESIAN_POINT('',(73.1862515170839,246.621657613239,18.0213203435596)) ;
#97442 = CARTESIAN_POINT('Origin',(72.8133921147013,247.214089774802,18.0213203435596)) ;
#97443 = CARTESIAN_POINT('',(72.1133921147013,247.214089774802,18.0213203435596)) ;
#97444 = CARTESIAN_POINT('Origin',(72.1133921147013,248.224963207434,18.0213203435596)) ;
#97445 = CARTESIAN_POINT('Origin',(74.9881263857102,249.345262302685,18.0213203435596)) ;
#97446 = CARTESIAN_POINT('Origin',(74.7283628290596,246.92834685842,18.0213203435596)) ;
#97447 = CARTESIAN_POINT('',(74.7283628290596,246.92834685842,18.0213203435596)) ;
#97448 = CARTESIAN_POINT('Origin',(74.3283628290596,246.92834685842,18.0213203435596)) ;
#97449 = CARTESIAN_POINT('Origin',(62.9,257.02214694455,20.0213203435596)) ;
#97450 = CARTESIAN_POINT('Origin',(29.2133075051975,255.671997914687,20.0213203435596)) ;
#97451 = CARTESIAN_POINT('Origin',(60.4815941846227,255.82214694455,20.0213203435596)) ;
#97452 = CARTESIAN_POINT('Origin',(75.8499999999999,228.11847800166,30.7213203435596)) ;
#97453 = CARTESIAN_POINT('',(70.4999999999999,220.262610236549,30.7213203435596)) ;
#97454 = CARTESIAN_POINT('',(73.9975476984278,220.262610236549,30.7213203435596)) ;
#97455 = CARTESIAN_POINT('',(70.4999999999999,220.305309236677,30.7213203435596)) ;
#97456 = CARTESIAN_POINT('Origin',(55.2141814145299,240.716611331017,20.0213203435596)) ;
#97457 = CARTESIAN_POINT('',(77.1300306216516,253.207106781187,20.0213203435596)) ;
#97458 = CARTESIAN_POINT('',(52.2356360608974,253.207106781187,20.0213203435596)) ;
#97459 = CARTESIAN_POINT('',(77.75,255.5,20.0213203435596)) ;
#97460 = CARTESIAN_POINT('Origin',(73.2,255.5,20.0213203435596)) ;
#97461 = CARTESIAN_POINT('',(77.75,256.631336165532,20.0213203435596)) ;
#97462 = CARTESIAN_POINT('',(77.75,248.684378986433,20.0213203435596)) ;
#97463 = CARTESIAN_POINT('',(77.7,257.767080845051,20.0213203435596)) ;
#97464 = CARTESIAN_POINT('Origin',(73.2,257.,20.0213203435596)) ;
#97465 = CARTESIAN_POINT('',(77.7,261.8,20.0213203435596)) ;
#97466 = CARTESIAN_POINT('',(77.7,249.220072841596,20.0213203435596)) ;
#97467 = CARTESIAN_POINT('',(66.207090707265,261.8,20.0213203435596)) ;
#97468 = CARTESIAN_POINT('Origin',(26.7,263.8,30.7213203435596)) ;
#97469 = CARTESIAN_POINT('',(26.7,245.5,30.7213203435596)) ;
#97470 = CARTESIAN_POINT('Origin',(59.9573593128807,226.261195155516,30.7213203435596)) ;
#97471 = CARTESIAN_POINT('',(56.9573593128807,226.261195155516,30.7213203435596)) ;
#97472 = CARTESIAN_POINT('',(56.9573593128807,226.261195155516,30.7213203435596)) ;
#97473 = CARTESIAN_POINT('Origin',(59.9573593128807,226.261195155516,30.7213203435596)) ;
#97474 = CARTESIAN_POINT('Origin',(56.9573593128808,244.4,30.7213203435596)) ;
#97475 = CARTESIAN_POINT('',(56.9573593128808,244.4,30.7213203435596)) ;
#97476 = CARTESIAN_POINT('',(56.9573593128808,244.4,30.7213203435596)) ;
#97477 = CARTESIAN_POINT('',(56.9573593128808,244.4,30.7213203435596)) ;
#97478 = CARTESIAN_POINT('Origin',(55.3573593128808,244.4,30.7213203435596)) ;
#97479 = CARTESIAN_POINT('',(55.3573593128808,246.,30.7213203435596)) ;
#97480 = CARTESIAN_POINT('',(55.3573593128808,246.,30.7213203435596)) ;
#97481 = CARTESIAN_POINT('Origin',(55.3573593128808,244.4,30.7213203435596)) ;
#97482 = CARTESIAN_POINT('Origin',(47.2,246.,30.7213203435596)) ;
#97483 = CARTESIAN_POINT('',(47.2,246.,30.7213203435596)) ;
#97484 = CARTESIAN_POINT('',(47.2,246.,30.7213203435596)) ;
#97485 = CARTESIAN_POINT('',(47.2,246.,30.7213203435596)) ;
#97486 = CARTESIAN_POINT('Origin',(47.2,248.9,30.7213203435596)) ;
#97487 = CARTESIAN_POINT('',(47.2,248.9,30.7213203435596)) ;
#97488 = CARTESIAN_POINT('',(47.2,248.9,30.7213203435596)) ;
#97489 = CARTESIAN_POINT('',(47.2,248.9,30.7213203435596)) ;
#97490 = CARTESIAN_POINT('Origin',(46.3,248.9,30.7213203435596)) ;
#97491 = CARTESIAN_POINT('',(46.3,248.9,30.7213203435596)) ;
#97492 = CARTESIAN_POINT('',(46.3,248.9,30.7213203435596)) ;
#97493 = CARTESIAN_POINT('',(47.2,248.9,30.7213203435596)) ;
#97494 = CARTESIAN_POINT('Origin',(53.5411791018402,233.961738491187,30.7213203435596)) ;
#97495 = CARTESIAN_POINT('',(46.3,245.6,30.7213203435596)) ;
#97496 = CARTESIAN_POINT('',(46.3,245.6,30.7213203435596)) ;
#97497 = CARTESIAN_POINT('Origin',(46.8000000000001,245.6,30.7213203435596)) ;
#97498 = CARTESIAN_POINT('Origin',(46.8000000000001,245.6,29.5213203435596)) ;
#97499 = CARTESIAN_POINT('',(46.3,245.6,20.0213203435596)) ;
#97500 = CARTESIAN_POINT('',(46.3,245.6,29.5213203435596)) ;
#97501 = CARTESIAN_POINT('Origin',(46.8000000000001,245.6,20.0213203435596)) ;
#97502 = CARTESIAN_POINT('Origin',(46.3,245.6,29.5213203435596)) ;
#97503 = CARTESIAN_POINT('',(46.3,248.9,20.0213203435596)) ;
#97504 = CARTESIAN_POINT('',(46.3,248.9,29.5213203435596)) ;
#97505 = CARTESIAN_POINT('',(46.3,245.6,20.0213203435596)) ;
#97506 = CARTESIAN_POINT('Origin',(33.8,245.5,30.7213203435596)) ;
#97507 = CARTESIAN_POINT('',(33.8,245.5,30.7213203435596)) ;
#97508 = CARTESIAN_POINT('Origin',(26.7,245.5,30.7213203435596)) ;
#97509 = CARTESIAN_POINT('Origin',(34.1,248.9,29.5213203435596)) ;
#97510 = CARTESIAN_POINT('',(34.1,245.6,20.0213203435596)) ;
#97511 = CARTESIAN_POINT('',(34.1,245.6,29.5213203435596)) ;
#97512 = CARTESIAN_POINT('',(34.1,248.9,20.0213203435596)) ;
#97513 = CARTESIAN_POINT('',(34.1,248.9,20.0213203435596)) ;
#97514 = CARTESIAN_POINT('',(34.1,248.9,29.5213203435596)) ;
#97515 = CARTESIAN_POINT('Origin',(75.4283628290596,245.483789937202,16.0213203435596)) ;
#97516 = CARTESIAN_POINT('',(75.4283628290596,246.,18.5213203435596)) ;
#97517 = CARTESIAN_POINT('',(75.4283628290596,246.,18.5213203435596)) ;
#97518 = CARTESIAN_POINT('',(75.4283628290596,246.,16.0213203435596)) ;
#97519 = CARTESIAN_POINT('Origin',(75.4283628290596,246.,16.0213203435596)) ;
#97520 = CARTESIAN_POINT('',(73.6283628290596,246.,18.5213203435596)) ;
#97521 = CARTESIAN_POINT('',(73.6283628290596,246.,18.5213203435596)) ;
#97522 = CARTESIAN_POINT('',(73.6283628290596,246.,16.0213203435596)) ;
#97523 = CARTESIAN_POINT('Origin',(73.6283628290596,246.,16.0213203435596)) ;
#97524 = CARTESIAN_POINT('',(73.6283628290596,244.8,18.5213203435596)) ;
#97525 = CARTESIAN_POINT('Origin',(74.5283628290597,239.625,18.5213203435596)) ;
#97526 = CARTESIAN_POINT('Origin',(41.7,245.1,19.2213203435596)) ;
#97527 = CARTESIAN_POINT('',(55.3573593128808,245.1,20.0213203435596)) ;
#97528 = CARTESIAN_POINT('',(38.7,245.1,22.2213203435596)) ;
#97529 = CARTESIAN_POINT('',(38.7,245.1,19.2213203435596)) ;
#97530 = CARTESIAN_POINT('',(41.7,245.1,22.2213203435596)) ;
#97531 = CARTESIAN_POINT('',(55.3573593128808,245.1,22.2213203435596)) ;
#97532 = CARTESIAN_POINT('',(41.7,245.1,19.2213203435596)) ;
#97533 = CARTESIAN_POINT('Origin',(40.2,242.9,19.2213203435596)) ;
#97534 = CARTESIAN_POINT('',(41.7000000000001,242.9,22.2213203435596)) ;
#97535 = CARTESIAN_POINT('',(41.7000000000001,242.9,19.2213203435596)) ;
#97536 = CARTESIAN_POINT('',(38.7000000000001,242.9,22.2213203435596)) ;
#97537 = CARTESIAN_POINT('Origin',(40.2,242.9,22.2213203435596)) ;
#97538 = CARTESIAN_POINT('',(38.7000000000001,242.9,19.2213203435596)) ;
#97539 = CARTESIAN_POINT('Origin',(38.7,245.1,19.2213203435596)) ;
#97540 = CARTESIAN_POINT('',(38.7000000000001,242.9,22.2213203435596)) ;
#97541 = CARTESIAN_POINT('Origin',(41.7000000000001,242.9,19.2213203435596)) ;
#97542 = CARTESIAN_POINT('',(41.7,246.9,22.2213203435596)) ;
#97543 = CARTESIAN_POINT('Origin',(40.2,243.25,22.2213203435596)) ;
#97544 = CARTESIAN_POINT('Origin',(59.7722678973651,244.793417527584,18.0213203435596)) ;
#97545 = CARTESIAN_POINT('',(59.4894251848905,244.51057481511,24.0213203435596)) ;
#97546 = CARTESIAN_POINT('',(59.4894251848905,244.51057481511,18.0213203435596)) ;
#97547 = CARTESIAN_POINT('Origin',(59.7722678973651,244.793417527584,24.0213203435596)) ;
#97548 = CARTESIAN_POINT('Origin',(68.4464305354851,241.4,17.0213203435596)) ;
#97549 = CARTESIAN_POINT('Origin',(66.25,251.8,23.0213203435596)) ;
#97550 = CARTESIAN_POINT('Origin',(66.25,251.8,23.0213203435596)) ;
#97551 = CARTESIAN_POINT('',(58.5931591083782,252.048885472713,23.0213203435596)) ;
#97552 = CARTESIAN_POINT('Origin',(62.7,247.5,24.0213203435596)) ;
#97553 = CARTESIAN_POINT('',(59.35,244.65,24.0213203435596)) ;
#97554 = CARTESIAN_POINT('',(58.3716948501153,251.81856264412,24.0213203435596)) ;
#97555 = CARTESIAN_POINT('',(65.7,242.,24.0213203435596)) ;
#97556 = CARTESIAN_POINT('Origin',(59.1,244.9,24.0213203435596)) ;
#97557 = CARTESIAN_POINT('Origin',(43.7,259.4,24.7713203435596)) ;
#97558 = CARTESIAN_POINT('',(43.7,259.,25.7213203435596)) ;
#97559 = CARTESIAN_POINT('',(43.7,259.,24.7713203435596)) ;
#97560 = CARTESIAN_POINT('Origin',(43.7,259.4,25.7213203435596)) ;
#97561 = CARTESIAN_POINT('Origin',(45.7,259.,20.0213203435596)) ;
#97562 = CARTESIAN_POINT('',(34.7,259.,25.7213203435596)) ;
#97563 = CARTESIAN_POINT('Origin',(36.7,259.4,24.7713203435596)) ;
#97564 = CARTESIAN_POINT('',(36.7,259.,24.7713203435596)) ;
#97565 = CARTESIAN_POINT('Origin',(58.45,251.9,24.0213203435596)) ;
#97566 = CARTESIAN_POINT('Origin',(62.9568347953872,216.946231446812,18.0213203435596)) ;
#97567 = CARTESIAN_POINT('',(62.9568347953872,216.946231446812,18.0213203435596)) ;
#97568 = CARTESIAN_POINT('Origin',(65.3568347953872,216.946231446812,18.0213203435596)) ;
#97569 = CARTESIAN_POINT('Origin',(65.7,242.,24.0213203435596)) ;
#97570 = CARTESIAN_POINT('Origin',(67.55,249.825,18.7713203435596)) ;
#97571 = CARTESIAN_POINT('Origin',(77.7,249.220072841596,20.5213203435596)) ;
#97572 = CARTESIAN_POINT('',(77.2,257.723534352175,20.5213203435596)) ;
#97573 = CARTESIAN_POINT('Ctrl Pts',(77.7,257.767080845051,20.0213203435596)) ;
#97574 = CARTESIAN_POINT('Ctrl Pts',(77.6987927240906,257.766978684289,20.0213203435596)) ;
#97575 = CARTESIAN_POINT('Ctrl Pts',(77.6975854537437,257.766876503587,20.021324716105)) ;
#97576 = CARTESIAN_POINT('Ctrl Pts',(77.6963782127139,257.766774304936,20.0213334610748)) ;
#97577 = CARTESIAN_POINT('Ctrl Pts',(77.6298579761241,257.761143052947,20.0218153180106)) ;
#97578 = CARTESIAN_POINT('Ctrl Pts',(77.5640846778152,257.755510562374,20.0355676249654)) ;
#97579 = CARTESIAN_POINT('Ctrl Pts',(77.5029237754161,257.75021874678,20.0617978068938)) ;
#97580 = CARTESIAN_POINT('Ctrl Pts',(77.4431171654848,257.74504410843,20.0874471710707)) ;
#97581 = CARTESIAN_POINT('Ctrl Pts',(77.3888531038272,257.740294173789,20.1245427545607)) ;
#97582 = CARTESIAN_POINT('Ctrl Pts',(77.3432091028781,257.736270106201,20.171034380765)) ;
#97583 = CARTESIAN_POINT('Ctrl Pts',(77.297752578747,257.73226256695,20.2173350486404)) ;
#97584 = CARTESIAN_POINT('Ctrl Pts',(77.2617111099311,257.729052975728,20.2720740981487)) ;
#97585 = CARTESIAN_POINT('Ctrl Pts',(77.2371396870212,257.726858660253,20.3322163227955)) ;
#97586 = CARTESIAN_POINT('Ctrl Pts',(77.2126212406766,257.724669075773,20.3922288793925)) ;
#97587 = CARTESIAN_POINT('Ctrl Pts',(77.2,257.723534352175,20.4564568635466)) ;
#97588 = CARTESIAN_POINT('Ctrl Pts',(77.2,257.723534352175,20.5213203435596)) ;
#97589 = CARTESIAN_POINT('',(77.2,261.559687576257,20.5213203435596)) ;
#97590 = CARTESIAN_POINT('',(77.2,249.220072841596,20.5213203435596)) ;
#97591 = CARTESIAN_POINT('Origin',(77.7,261.559687576257,20.5213203435596)) ;
#97592 = CARTESIAN_POINT('Origin',(68.6263598493594,261.559687576257,20.5213203435596)) ;
#97593 = CARTESIAN_POINT('',(69.117630762786,261.652708485847,20.5213203435596)) ;
#97594 = CARTESIAN_POINT('Origin',(68.6263598493594,261.559687576257,20.5213203435596)) ;
#97595 = CARTESIAN_POINT('',(68.6263598493594,261.950121980978,20.2089728197824)) ;
#97596 = CARTESIAN_POINT('Origin',(68.6263598493594,261.559687576257,20.5213203435596)) ;
#97597 = CARTESIAN_POINT('Origin',(68.6263598493594,261.559687576257,20.5213203435596)) ;
#97598 = CARTESIAN_POINT('Origin',(73.2,257.,20.5213203435596)) ;
#97599 = CARTESIAN_POINT('',(77.25,256.652146641849,20.5213203435596)) ;
#97600 = CARTESIAN_POINT('Ctrl Pts',(77.75,256.631336165532,20.0213203435596)) ;
#97601 = CARTESIAN_POINT('Ctrl Pts',(77.7485328081134,256.63139550792,20.0213203435596)) ;
#97602 = CARTESIAN_POINT('Ctrl Pts',(77.7470656238674,256.631454864325,20.0213268015157)) ;
#97603 = CARTESIAN_POINT('Ctrl Pts',(77.7455984898958,256.631514233046,20.0213397172261)) ;
#97604 = CARTESIAN_POINT('Ctrl Pts',(77.6796694448428,256.634182103317,20.0219201144309)) ;
#97605 = CARTESIAN_POINT('Ctrl Pts',(77.6144986337877,256.636849380763,20.0355352673941)) ;
#97606 = CARTESIAN_POINT('Ctrl Pts',(77.5538469838264,256.639357070684,20.0614029659297)) ;
#97607 = CARTESIAN_POINT('Ctrl Pts',(77.4939656651802,256.641832910654,20.0869421210828)) ;
#97608 = CARTESIAN_POINT('Ctrl Pts',(77.4396362683022,256.644105318551,20.1239355278407)) ;
#97609 = CARTESIAN_POINT('Ctrl Pts',(77.3939221201998,256.646031042763,20.1703095979733)) ;
#97610 = CARTESIAN_POINT('Ctrl Pts',(77.3482511109358,256.647954949736,20.2166399065224)) ;
#97611 = CARTESIAN_POINT('Ctrl Pts',(77.3120515823072,256.64949525193,20.2714483566738)) ;
#97612 = CARTESIAN_POINT('Ctrl Pts',(77.2873671506917,256.65054853451,20.3316605250927)) ;
#97613 = CARTESIAN_POINT('Ctrl Pts',(77.2626949528298,256.651601295077,20.3918428519969)) ;
#97614 = CARTESIAN_POINT('Ctrl Pts',(77.25,256.652146641849,20.4562688621889)) ;
#97615 = CARTESIAN_POINT('Ctrl Pts',(77.25,256.652146641849,20.5213203435596)) ;
#97616 = CARTESIAN_POINT('Origin',(73.2,257.,20.5213203435596)) ;
#97617 = CARTESIAN_POINT('Ctrl Pts',(55.5095145719656,261.79455482774,20.2277364888237)) ;
#97618 = CARTESIAN_POINT('Ctrl Pts',(55.5340602178732,261.756752943059,20.1881500276994)) ;
#97619 = CARTESIAN_POINT('Ctrl Pts',(55.5890667713761,261.688545713664,20.1225709708889)) ;
#97620 = CARTESIAN_POINT('Ctrl Pts',(55.735413453564,261.557876251656,20.0417117307531)) ;
#97621 = CARTESIAN_POINT('Ctrl Pts',(55.8502255851785,261.475529765423,20.0213203435596)) ;
#97622 = CARTESIAN_POINT('Ctrl Pts',(55.9002853073786,261.439128427997,20.0213203435596)) ;
#97623 = CARTESIAN_POINT('Ctrl Pts',(55.5235850209285,261.795524155342,20.2176307773862)) ;
#97624 = CARTESIAN_POINT('Ctrl Pts',(55.5482267599533,261.758752662429,20.1800147865656)) ;
#97625 = CARTESIAN_POINT('Ctrl Pts',(55.6035725767284,261.691952725752,20.1174091581561)) ;
#97626 = CARTESIAN_POINT('Ctrl Pts',(55.7504527952051,261.564081963617,20.0401902813788)) ;
#97627 = CARTESIAN_POINT('Ctrl Pts',(55.8622446715528,261.484225598423,20.0213203435596)) ;
#97628 = CARTESIAN_POINT('Ctrl Pts',(55.9108349616358,261.448512190495,20.0213203435596)) ;
#97629 = CARTESIAN_POINT('Ctrl Pts',(55.5532287114159,261.797064527402,20.1984257565318)) ;
#97630 = CARTESIAN_POINT('Ctrl Pts',(55.5780804509168,261.762295810682,20.1644899997044)) ;
#97631 = CARTESIAN_POINT('Ctrl Pts',(55.6342304168334,261.698178708499,20.1074661938862)) ;
#97632 = CARTESIAN_POINT('Ctrl Pts',(55.7819183628387,261.575867031561,20.0373124202088)) ;
#97633 = CARTESIAN_POINT('Ctrl Pts',(55.8872841120386,261.500839109789,20.0213203435596)) ;
#97634 = CARTESIAN_POINT('Ctrl Pts',(55.9330008011269,261.466448157126,20.0213203435596)) ;
#97635 = CARTESIAN_POINT('Ctrl Pts',(55.6031763483208,261.79822250744,20.1723029608032)) ;
#97636 = CARTESIAN_POINT('Ctrl Pts',(55.6283903853712,261.766259990504,20.1432509083838)) ;
#97637 = CARTESIAN_POINT('Ctrl Pts',(55.6861581265256,261.705670081893,20.0935677319834)) ;
#97638 = CARTESIAN_POINT('Ctrl Pts',(55.8330482728718,261.591606059386,20.0335654961594)) ;
#97639 = CARTESIAN_POINT('Ctrl Pts',(55.9272521877398,261.523003776658,20.0213203435596)) ;
#97640 = CARTESIAN_POINT('Ctrl Pts',(55.9685491941045,261.490298772052,20.0213203435596)) ;
#97641 = CARTESIAN_POINT('Ctrl Pts',(55.6599047282381,261.79814256388,20.1486416834275)) ;
#97642 = CARTESIAN_POINT('Ctrl Pts',(55.6855379524164,261.768683922706,20.123848253105)) ;
#97643 = CARTESIAN_POINT('Ctrl Pts',(55.7449568036994,261.711182780251,20.0807219288465)) ;
#97644 = CARTESIAN_POINT('Ctrl Pts',(55.887500553162,261.605190989655,20.0304664474941)) ;
#97645 = CARTESIAN_POINT('Ctrl Pts',(55.9689294097052,261.541942710494,20.0213203435596)) ;
#97646 = CARTESIAN_POINT('Ctrl Pts',(56.0055078009848,261.510563832554,20.0213203435596)) ;
#97647 = CARTESIAN_POINT('Ctrl Pts',(55.7252078119995,261.796555096217,20.1272203634637)) ;
#97648 = CARTESIAN_POINT('Ctrl Pts',(55.751115773334,261.769255478328,20.1061252686703)) ;
#97649 = CARTESIAN_POINT('Ctrl Pts',(55.8113298661455,261.714598172442,20.0691496430748)) ;
#97650 = CARTESIAN_POINT('Ctrl Pts',(55.9442663460163,261.616377934868,20.0280919148922)) ;
#97651 = CARTESIAN_POINT('Ctrl Pts',(56.0117059172473,261.557294041147,20.0213203435596)) ;
#97652 = CARTESIAN_POINT('Ctrl Pts',(56.0432529317468,261.526923260636,20.0213203435596)) ;
#97653 = CARTESIAN_POINT('Ctrl Pts',(55.8010086453308,261.793278462298,20.1080994112902)) ;
#97654 = CARTESIAN_POINT('Ctrl Pts',(55.8264732881332,261.767898003963,20.0903515933129)) ;
#97655 = CARTESIAN_POINT('Ctrl Pts',(55.88546498208,261.715868557646,20.0591653394807)) ;
#97656 = CARTESIAN_POINT('Ctrl Pts',(56.0021591954208,261.625132679932,20.0265188148335)) ;
#97657 = CARTESIAN_POINT('Ctrl Pts',(56.0555340297016,261.569069711917,20.0213203435596)) ;
#97658 = CARTESIAN_POINT('Ctrl Pts',(56.081895506616,261.539529506758,20.0213203435596)) ;
#97659 = CARTESIAN_POINT('Ctrl Pts',(55.8886521902875,261.788562905801,20.0918367827122)) ;
#97660 = CARTESIAN_POINT('Ctrl Pts',(55.9122449680893,261.764902435925,20.077124846578)) ;
#97661 = CARTESIAN_POINT('Ctrl Pts',(55.966266526308,261.715404406956,20.0512640137083)) ;
#97662 = CARTESIAN_POINT('Ctrl Pts',(56.060051810839,261.631716223329,20.0257337627999)) ;
#97663 = CARTESIAN_POINT('Ctrl Pts',(56.1003810935014,261.577565074392,20.0213203435596)) ;
#97664 = CARTESIAN_POINT('Ctrl Pts',(56.1213725159607,261.548761013242,20.0213203435596)) ;
#97665 = CARTESIAN_POINT('Ctrl Pts',(55.9864294144668,261.783244910011,20.0795560745166)) ;
#97666 = CARTESIAN_POINT('Ctrl Pts',(56.0059208588127,261.761024223606,20.0673697854514)) ;
#97667 = CARTESIAN_POINT('Ctrl Pts',(56.0496683079691,261.713900171691,20.0459122043803)) ;
#97668 = CARTESIAN_POINT('Ctrl Pts',(56.1161262096349,261.636127836261,20.0255537625844)) ;
#97669 = CARTESIAN_POINT('Ctrl Pts',(56.145213082859,261.582971518512,20.0213203435596)) ;
#97670 = CARTESIAN_POINT('Ctrl Pts',(56.1607380593261,261.554911951281,20.0213203435596)) ;
#97671 = CARTESIAN_POINT('Ctrl Pts',(56.0870864420511,261.778692438248,20.0723692404909)) ;
#97672 = CARTESIAN_POINT('Ctrl Pts',(56.100316035454,261.75738417469,20.0617919516248)) ;
#97673 = CARTESIAN_POINT('Ctrl Pts',(56.1294240269605,261.712066783038,20.0432182833585)) ;
#97674 = CARTESIAN_POINT('Ctrl Pts',(56.1690343411742,261.638107172439,20.0256017416873)) ;
#97675 = CARTESIAN_POINT('Ctrl Pts',(56.1887559131447,261.58555790289,20.0213203435596)) ;
#97676 = CARTESIAN_POINT('Ctrl Pts',(56.1988987568555,261.558363227878,20.0213203435596)) ;
#97677 = CARTESIAN_POINT('Ctrl Pts',(56.1809390611363,261.776355954665,20.0702679342639)) ;
#97678 = CARTESIAN_POINT('Ctrl Pts',(56.1874552820846,261.755032522864,20.0600771865253)) ;
#97679 = CARTESIAN_POINT('Ctrl Pts',(56.2013267910678,261.710037910159,20.0423497842736)) ;
#97680 = CARTESIAN_POINT('Ctrl Pts',(56.2195156636653,261.637327921928,20.0254466687852)) ;
#97681 = CARTESIAN_POINT('Ctrl Pts',(56.2301181856568,261.585806509747,20.0213203435596)) ;
#97682 = CARTESIAN_POINT('Ctrl Pts',(56.2351113333668,261.559674193744,20.0213203435596)) ;
#97683 = CARTESIAN_POINT('Ctrl Pts',(56.2391336395509,261.776281941501,20.0706687254062)) ;
#97684 = CARTESIAN_POINT('Ctrl Pts',(56.2414470866218,261.754222015824,20.0600661769919)) ;
#97685 = CARTESIAN_POINT('Ctrl Pts',(56.2461461230855,261.708290875557,20.0419846645419)) ;
#97686 = CARTESIAN_POINT('Ctrl Pts',(56.2528435308144,261.635323465912,20.0251686372497)) ;
#97687 = CARTESIAN_POINT('Ctrl Pts',(56.2563772874478,261.584992844062,20.0213203435596)) ;
#97688 = CARTESIAN_POINT('Ctrl Pts',(56.2580619020738,261.559687576257,20.0213203435596)) ;
#97689 = CARTESIAN_POINT('Ctrl Pts',(56.2695111541429,261.776281941501,20.0706687254062)) ;
#97690 = CARTESIAN_POINT('Ctrl Pts',(56.2695111541429,261.753848118778,20.0598864727815)) ;
#97691 = CARTESIAN_POINT('Ctrl Pts',(56.2695111541429,261.707367453737,20.0416786272431)) ;
#97692 = CARTESIAN_POINT('Ctrl Pts',(56.2695111541429,261.634358610927,20.0250444537314)) ;
#97693 = CARTESIAN_POINT('Ctrl Pts',(56.2695111541429,261.584578003606,20.0213203435596)) ;
#97694 = CARTESIAN_POINT('Ctrl Pts',(56.2695111541429,261.559687576257,20.0213203435596)) ;
#97695 = CARTESIAN_POINT('Origin',(56.2695111541429,261.559687576257,20.5213203435596)) ;
#97696 = CARTESIAN_POINT('Origin',(55.2268638269143,261.559687576257,20.5213203435596)) ;
#97697 = CARTESIAN_POINT('',(55.2268638269143,261.950121980978,20.2089728197824)) ;
#97698 = CARTESIAN_POINT('Ctrl Pts',(77.1300306216516,253.207106781187,20.0213203435596)) ;
#97699 = CARTESIAN_POINT('Ctrl Pts',(76.9727816340446,253.072343999508,20.0213203435596)) ;
#97700 = CARTESIAN_POINT('Ctrl Pts',(76.7853404806882,252.94731363725,19.9686339808095)) ;
#97701 = CARTESIAN_POINT('Ctrl Pts',(76.6208916966195,252.853553390593,19.8748737341529)) ;
#97702 = CARTESIAN_POINT('Ctrl Pts',(77.0169669281593,253.273071401074,20.0213203435596)) ;
#97703 = CARTESIAN_POINT('Ctrl Pts',(76.8741225322589,253.140600606275,20.0395012945359)) ;
#97704 = CARTESIAN_POINT('Ctrl Pts',(76.6994917884722,252.999180185916,20.0023959135144)) ;
#97705 = CARTESIAN_POINT('Ctrl Pts',(76.543994900258,252.887271264403,19.9085916079623)) ;
#97706 = CARTESIAN_POINT('Ctrl Pts',(76.7919007678944,253.404381490571,20.1298498989989)) ;
#97707 = CARTESIAN_POINT('Ctrl Pts',(76.6768979485241,253.246681150455,20.1631107893611)) ;
#97708 = CARTESIAN_POINT('Ctrl Pts',(76.5281740570552,253.06465267538,20.1270179596422)) ;
#97709 = CARTESIAN_POINT('Ctrl Pts',(76.3903553725496,252.918990684446,20.0116085736344)) ;
#97710 = CARTESIAN_POINT('Ctrl Pts',(76.6981591247668,253.459073068968,20.3904206496601)) ;
#97711 = CARTESIAN_POINT('Ctrl Pts',(76.5739302623505,253.245411894379,20.4018503552973)) ;
#97712 = CARTESIAN_POINT('Ctrl Pts',(76.41949641419,253.033434868643,20.3194987016572)) ;
#97713 = CARTESIAN_POINT('Ctrl Pts',(76.2808206834693,252.870551298285,20.1561059751854)) ;
#97714 = CARTESIAN_POINT('Ctrl Pts',(76.6981591247668,253.459073068968,20.5213203435596)) ;
#97715 = CARTESIAN_POINT('Ctrl Pts',(76.5581902456883,253.219165699387,20.5213203435596)) ;
#97716 = CARTESIAN_POINT('Ctrl Pts',(76.3913470212719,252.996584175367,20.4159476180594)) ;
#97717 = CARTESIAN_POINT('Ctrl Pts',(76.2449695321558,252.82967032967,20.2284271247462)) ;
#97718 = CARTESIAN_POINT('',(76.2449695321558,252.82967032967,20.2284271247462)) ;
#97719 = CARTESIAN_POINT('',(76.6981591247668,253.459073068968,20.5213203435596)) ;
#97720 = CARTESIAN_POINT('Ctrl Pts',(76.2449695321558,252.82967032967,20.2284271247462)) ;
#97721 = CARTESIAN_POINT('Ctrl Pts',(76.3913470212719,252.996584175367,20.4159476180594)) ;
#97722 = CARTESIAN_POINT('Ctrl Pts',(76.5581902456883,253.219165699387,20.5213203435596)) ;
#97723 = CARTESIAN_POINT('Ctrl Pts',(76.6981591247668,253.459073068968,20.5213203435596)) ;
#97724 = CARTESIAN_POINT('Origin',(77.1300306216516,253.207106781187,20.5213203435596)) ;
#97725 = CARTESIAN_POINT('Ctrl Pts',(77.1300306216516,253.207106781187,20.0213203435596)) ;
#97726 = CARTESIAN_POINT('Ctrl Pts',(76.9727816340446,253.072343999508,20.0213203435596)) ;
#97727 = CARTESIAN_POINT('Ctrl Pts',(76.7853404806882,252.94731363725,19.9686339808095)) ;
#97728 = CARTESIAN_POINT('Ctrl Pts',(76.6208916966195,252.853553390593,19.8748737341529)) ;
#97729 = CARTESIAN_POINT('Origin',(76.6208916966195,252.5,20.2284271247462)) ;
#97730 = CARTESIAN_POINT('Origin',(73.2,255.5,20.5213203435596)) ;
#97731 = CARTESIAN_POINT('',(77.25,255.5,20.5213203435596)) ;
#97732 = CARTESIAN_POINT('Origin',(77.75,255.5,20.5213203435596)) ;
#97733 = CARTESIAN_POINT('Origin',(73.2,255.5,20.5213203435596)) ;
#97734 = CARTESIAN_POINT('Origin',(77.75,248.684378986433,20.5213203435596)) ;
#97735 = CARTESIAN_POINT('',(77.25,248.684378986433,20.5213203435596)) ;
#97736 = CARTESIAN_POINT('Origin',(52.2356360608974,253.207106781187,19.5213203435596)) ;
#97737 = CARTESIAN_POINT('Origin',(46.6263598493593,261.559687576257,20.5213203435596)) ;
#97738 = CARTESIAN_POINT('',(47.1176307627859,261.652708485847,20.5213203435596)) ;
#97739 = CARTESIAN_POINT('Origin',(46.6263598493593,261.559687576257,20.5213203435596)) ;
#97740 = CARTESIAN_POINT('Origin',(46.6263598493593,261.559687576257,20.5213203435596)) ;
#97741 = CARTESIAN_POINT('Ctrl Pts',(46.6262992790349,261.950068411826,20.2089058667418)) ;
#97742 = CARTESIAN_POINT('Ctrl Pts',(46.6121566500185,262.024832042591,20.3023601782468)) ;
#97743 = CARTESIAN_POINT('Ctrl Pts',(46.580666198832,262.09625764165,20.3916424900841)) ;
#97744 = CARTESIAN_POINT('Ctrl Pts',(46.5350110422629,262.157126340136,20.4677282733508)) ;
#97745 = CARTESIAN_POINT('Ctrl Pts',(46.7442583096226,261.958793642181,20.2197842338569)) ;
#97746 = CARTESIAN_POINT('Ctrl Pts',(46.7189281932969,262.039807921917,20.3214382905633)) ;
#97747 = CARTESIAN_POINT('Ctrl Pts',(46.675218628264,262.116429910146,20.4166884625079)) ;
#97748 = CARTESIAN_POINT('Ctrl Pts',(46.6167573320855,262.181064672294,20.4976354561752)) ;
#97749 = CARTESIAN_POINT('Ctrl Pts',(46.979430861431,261.907070818778,20.2967667810524)) ;
#97750 = CARTESIAN_POINT('Ctrl Pts',(46.9323308081948,262.013112885638,20.4047147907279)) ;
#97751 = CARTESIAN_POINT('Ctrl Pts',(46.8639746536185,262.109285954832,20.5046230523416)) ;
#97752 = CARTESIAN_POINT('Ctrl Pts',(46.7800765251102,262.189709099368,20.588731540056)) ;
#97753 = CARTESIAN_POINT('Ctrl Pts',(47.1005251724555,261.743097807743,20.4462783497206)) ;
#97754 = CARTESIAN_POINT('Ctrl Pts',(47.0598088706616,261.88150309857,20.5446866530911)) ;
#97755 = CARTESIAN_POINT('Ctrl Pts',(46.9899272559849,262.009912469407,20.6374702762036)) ;
#97756 = CARTESIAN_POINT('Ctrl Pts',(46.8967323918744,262.117798129565,20.7162682354584)) ;
#97757 = CARTESIAN_POINT('Ctrl Pts',(47.1176490922737,261.65261165586,20.5212598248177)) ;
#97758 = CARTESIAN_POINT('Ctrl Pts',(47.0893506066563,261.802146309377,20.6147189832657)) ;
#97759 = CARTESIAN_POINT('Ctrl Pts',(47.0263552568488,261.945003652573,20.7040048227633)) ;
#97760 = CARTESIAN_POINT('Ctrl Pts',(46.9350298022437,262.066745503355,20.780093479502)) ;
#97761 = CARTESIAN_POINT('',(46.9350889359326,262.066666666667,20.7800442065721)) ;
#97762 = CARTESIAN_POINT('Origin',(46.5350889359327,261.766666666667,20.7800442065721)) ;
#97763 = CARTESIAN_POINT('Origin',(46.1350889359327,261.466666666667,20.4050442065721)) ;
#97764 = CARTESIAN_POINT('Origin',(44.3686862542563,264.655203575568,24.3907153426993)) ;
#97765 = CARTESIAN_POINT('',(44.7686862542563,264.955203575568,24.3907153426993)) ;
#97766 = CARTESIAN_POINT('Origin',(51.2,257.,20.5213203435596)) ;
#97767 = CARTESIAN_POINT('',(55.25,256.652146641849,20.5213203435596)) ;
#97768 = CARTESIAN_POINT('',(55.2649110640674,257.,20.5213203435596)) ;
#97769 = CARTESIAN_POINT('Origin',(51.2,257.,20.5213203435596)) ;
#97770 = CARTESIAN_POINT('Origin',(55.7649110640674,257.,20.5213203435596)) ;
#97771 = CARTESIAN_POINT('Ctrl Pts',(55.75,256.631336165532,20.0213203435596)) ;
#97772 = CARTESIAN_POINT('Ctrl Pts',(55.7485328081134,256.63139550792,20.0213203435596)) ;
#97773 = CARTESIAN_POINT('Ctrl Pts',(55.7470656238674,256.631454864325,20.0213268015157)) ;
#97774 = CARTESIAN_POINT('Ctrl Pts',(55.7455984898958,256.631514233046,20.0213397172261)) ;
#97775 = CARTESIAN_POINT('Ctrl Pts',(55.6796694448428,256.634182103317,20.0219201144309)) ;
#97776 = CARTESIAN_POINT('Ctrl Pts',(55.6144986337877,256.636849380763,20.0355352673941)) ;
#97777 = CARTESIAN_POINT('Ctrl Pts',(55.5538469838264,256.639357070684,20.0614029659297)) ;
#97778 = CARTESIAN_POINT('Ctrl Pts',(55.4939656651802,256.641832910654,20.0869421210828)) ;
#97779 = CARTESIAN_POINT('Ctrl Pts',(55.4396362683022,256.644105318551,20.1239355278407)) ;
#97780 = CARTESIAN_POINT('Ctrl Pts',(55.3939221201998,256.646031042763,20.1703095979733)) ;
#97781 = CARTESIAN_POINT('Ctrl Pts',(55.3482511109358,256.647954949736,20.2166399065224)) ;
#97782 = CARTESIAN_POINT('Ctrl Pts',(55.3120515823072,256.64949525193,20.2714483566738)) ;
#97783 = CARTESIAN_POINT('Ctrl Pts',(55.2873671506917,256.65054853451,20.3316605250927)) ;
#97784 = CARTESIAN_POINT('Ctrl Pts',(55.2626949528298,256.651601295077,20.3918428519969)) ;
#97785 = CARTESIAN_POINT('Ctrl Pts',(55.25,256.652146641849,20.4562688621889)) ;
#97786 = CARTESIAN_POINT('Ctrl Pts',(55.25,256.652146641849,20.5213203435596)) ;
#97787 = CARTESIAN_POINT('Ctrl Pts',(69.7791083033805,252.853553390593,19.8748737341529)) ;
#97788 = CARTESIAN_POINT('Ctrl Pts',(69.6146576393448,252.947314709111,19.9686350526701)) ;
#97789 = CARTESIAN_POINT('Ctrl Pts',(69.4272201636148,253.072342458909,20.0213203435596)) ;
#97790 = CARTESIAN_POINT('Ctrl Pts',(69.2699693783484,253.207106781187,20.0213203435596)) ;
#97791 = CARTESIAN_POINT('Ctrl Pts',(69.8560050997421,252.887271264403,19.9085916079623)) ;
#97792 = CARTESIAN_POINT('Ctrl Pts',(69.7005064338981,252.999181465251,20.0023969858787)) ;
#97793 = CARTESIAN_POINT('Ctrl Pts',(69.5258791007283,253.140599091878,20.0395015023792)) ;
#97794 = CARTESIAN_POINT('Ctrl Pts',(69.3830330718407,253.273071401074,20.0213203435596)) ;
#97795 = CARTESIAN_POINT('Ctrl Pts',(70.0096447013339,252.918990818726,20.0116085041473)) ;
#97796 = CARTESIAN_POINT('Ctrl Pts',(69.8718244412945,253.064654474858,20.1270192095074)) ;
#97797 = CARTESIAN_POINT('Ctrl Pts',(69.7231037922912,253.246679596241,20.1631106762666)) ;
#97798 = CARTESIAN_POINT('Ctrl Pts',(69.6080996582165,253.404381739176,20.1298494056682)) ;
#97799 = CARTESIAN_POINT('Ctrl Pts',(70.1191793165307,252.870551298284,20.1561059751854)) ;
#97800 = CARTESIAN_POINT('Ctrl Pts',(69.9805020004785,253.033436730717,20.3195005695518)) ;
#97801 = CARTESIAN_POINT('Ctrl Pts',(69.8260711578255,253.245409451819,20.4018504859609)) ;
#97802 = CARTESIAN_POINT('Ctrl Pts',(69.7018408752332,253.459073068968,20.3904206496601)) ;
#97803 = CARTESIAN_POINT('Ctrl Pts',(70.1550304678442,252.82967032967,20.2284271247462)) ;
#97804 = CARTESIAN_POINT('Ctrl Pts',(70.0086513053506,252.996586083515,20.415949761781)) ;
#97805 = CARTESIAN_POINT('Ctrl Pts',(69.8418113544264,253.219162956782,20.5213203435596)) ;
#97806 = CARTESIAN_POINT('Ctrl Pts',(69.7018408752332,253.459073068968,20.5213203435597)) ;
#97807 = CARTESIAN_POINT('',(69.7018408752332,253.459073068968,20.5213203435596)) ;
#97808 = CARTESIAN_POINT('Origin',(69.2699693783484,253.207106781187,20.5213203435596)) ;
#97809 = CARTESIAN_POINT('',(70.1550304678442,252.82967032967,20.2284271247462)) ;
#97810 = CARTESIAN_POINT('Ctrl Pts',(69.7018408752332,253.459073068968,20.5213203435597)) ;
#97811 = CARTESIAN_POINT('Ctrl Pts',(69.8418113544264,253.219162956782,20.5213203435596)) ;
#97812 = CARTESIAN_POINT('Ctrl Pts',(70.0086513053506,252.996586083515,20.415949761781)) ;
#97813 = CARTESIAN_POINT('Ctrl Pts',(70.1550304678442,252.82967032967,20.2284271247462)) ;
#97814 = CARTESIAN_POINT('Origin',(69.7791083033806,252.5,20.2284271247462)) ;
#97815 = CARTESIAN_POINT('Origin',(68.65,248.108305665508,20.5213203435596)) ;
#97816 = CARTESIAN_POINT('',(69.15,256.652146641849,20.5213203435596)) ;
#97817 = CARTESIAN_POINT('',(69.15,255.5,20.5213203435596)) ;
#97818 = CARTESIAN_POINT('',(69.15,248.108305665508,20.5213203435596)) ;
#97819 = CARTESIAN_POINT('Origin',(68.65,255.5,20.5213203435596)) ;
#97820 = CARTESIAN_POINT('Ctrl Pts',(68.65,256.631336165532,20.0213203435596)) ;
#97821 = CARTESIAN_POINT('Ctrl Pts',(68.6514671918867,256.63139550792,20.0213203435596)) ;
#97822 = CARTESIAN_POINT('Ctrl Pts',(68.6529343761326,256.631454864325,20.0213268015157)) ;
#97823 = CARTESIAN_POINT('Ctrl Pts',(68.6544015101042,256.631514233046,20.0213397172261)) ;
#97824 = CARTESIAN_POINT('Ctrl Pts',(68.7203305551572,256.634182103317,20.0219201144309)) ;
#97825 = CARTESIAN_POINT('Ctrl Pts',(68.7855013662124,256.636849380763,20.0355352673941)) ;
#97826 = CARTESIAN_POINT('Ctrl Pts',(68.8461530161737,256.639357070684,20.0614029659297)) ;
#97827 = CARTESIAN_POINT('Ctrl Pts',(68.9060343348199,256.641832910654,20.0869421210828)) ;
#97828 = CARTESIAN_POINT('Ctrl Pts',(68.9603637316979,256.644105318551,20.1239355278407)) ;
#97829 = CARTESIAN_POINT('Ctrl Pts',(69.0060778798002,256.646031042763,20.1703095979734)) ;
#97830 = CARTESIAN_POINT('Ctrl Pts',(69.0517488890642,256.647954949736,20.2166399065224)) ;
#97831 = CARTESIAN_POINT('Ctrl Pts',(69.0879484176928,256.64949525193,20.2714483566738)) ;
#97832 = CARTESIAN_POINT('Ctrl Pts',(69.1126328493083,256.65054853451,20.3316605250927)) ;
#97833 = CARTESIAN_POINT('Ctrl Pts',(69.1373050471702,256.651601295077,20.3918428519969)) ;
#97834 = CARTESIAN_POINT('Ctrl Pts',(69.15,256.652146641849,20.4562688621889)) ;
#97835 = CARTESIAN_POINT('Ctrl Pts',(69.15,256.652146641849,20.5213203435596)) ;
#97836 = CARTESIAN_POINT('Origin',(73.2,255.5,20.5213203435596)) ;
#97837 = CARTESIAN_POINT('Origin',(73.2,255.5,20.5213203435596)) ;
#97838 = CARTESIAN_POINT('Ctrl Pts',(70.1355962910396,252.851973368904,20.2591799537788)) ;
#97839 = CARTESIAN_POINT('Ctrl Pts',(70.7856774065376,252.099086619409,19.4120576663318)) ;
#97840 = CARTESIAN_POINT('Ctrl Pts',(72.3423540954159,251.274930902987,18.4845162963506)) ;
#97841 = CARTESIAN_POINT('Ctrl Pts',(74.7133620656512,251.567894939807,18.8142426993568)) ;
#97842 = CARTESIAN_POINT('Ctrl Pts',(75.8285852540374,252.347451852855,19.6915099002701)) ;
#97843 = CARTESIAN_POINT('Ctrl Pts',(76.264406030056,252.851970687799,20.2591769318912)) ;
#97844 = CARTESIAN_POINT('Ctrl Pts',(70.0947889951709,252.900719289552,20.1752138941917)) ;
#97845 = CARTESIAN_POINT('Ctrl Pts',(70.7436999646066,252.124445761866,19.333077491043)) ;
#97846 = CARTESIAN_POINT('Ctrl Pts',(72.3252162682866,251.268385211843,18.4095866632333)) ;
#97847 = CARTESIAN_POINT('Ctrl Pts',(74.7427882755993,251.573002122969,18.7379343247678)) ;
#97848 = CARTESIAN_POINT('Ctrl Pts',(75.8701660286286,252.380531879248,19.6108864310171)) ;
#97849 = CARTESIAN_POINT('Ctrl Pts',(76.3052135920791,252.900716378702,20.1752108539644)) ;
#97850 = CARTESIAN_POINT('Ctrl Pts',(69.9783224959303,252.946276054393,20.0291514232781)) ;
#97851 = CARTESIAN_POINT('Ctrl Pts',(70.6482383333472,252.129634870077,19.1954195941612)) ;
#97852 = CARTESIAN_POINT('Ctrl Pts',(72.2905009969719,251.229483751751,18.278969793691)) ;
#97853 = CARTESIAN_POINT('Ctrl Pts',(74.8036092356417,251.549747804448,18.6049119908004)) ;
#97854 = CARTESIAN_POINT('Ctrl Pts',(75.9725494008639,252.399037878032,19.4704581943099)) ;
#97855 = CARTESIAN_POINT('Ctrl Pts',(76.4216801989973,252.946272993645,20.0291483590762)) ;
#97856 = CARTESIAN_POINT('Ctrl Pts',(69.8218648241276,252.909543105076,19.9308614440711)) ;
#97857 = CARTESIAN_POINT('Ctrl Pts',(70.5341758458511,252.069082299954,19.0904632296569)) ;
#97858 = CARTESIAN_POINT('Ctrl Pts',(72.2520280195758,251.147401176394,18.1687895568493)) ;
#97859 = CARTESIAN_POINT('Ctrl Pts',(74.8723377634464,251.475110145404,18.4964972590599)) ;
#97860 = CARTESIAN_POINT('Ctrl Pts',(76.1005933035414,252.346338454721,19.3676988212773)) ;
#97861 = CARTESIAN_POINT('Ctrl Pts',(76.5781378198995,252.909540071613,19.930858408753)) ;
#97862 = CARTESIAN_POINT('Ctrl Pts',(69.7553711163591,252.880849873491,19.9021702170509)) ;
#97863 = CARTESIAN_POINT('Ctrl Pts',(70.4856634311088,252.033932725798,19.0552530693574)) ;
#97864 = CARTESIAN_POINT('Ctrl Pts',(72.2356775436909,251.106558080618,18.1278784241775)) ;
#97865 = CARTESIAN_POINT('Ctrl Pts',(74.9015612406156,251.436227730249,18.4575480738079)) ;
#97866 = CARTESIAN_POINT('Ctrl Pts',(76.155035835944,252.313317347784,19.3346376913431)) ;
#97867 = CARTESIAN_POINT('Ctrl Pts',(76.644631503471,252.880846850851,19.9021671944111)) ;
#97868 = CARTESIAN_POINT('Origin',(73.2,255.5,23.2284271247462)) ;
#97869 = CARTESIAN_POINT('Ctrl Pts',(55.1300306216516,253.207106781187,20.0213203435596)) ;
#97870 = CARTESIAN_POINT('Ctrl Pts',(54.9727816340446,253.072343999508,20.0213203435596)) ;
#97871 = CARTESIAN_POINT('Ctrl Pts',(54.7853404806882,252.94731363725,19.9686339808095)) ;
#97872 = CARTESIAN_POINT('Ctrl Pts',(54.6208916966195,252.853553390593,19.8748737341529)) ;
#97873 = CARTESIAN_POINT('Ctrl Pts',(55.0169669281593,253.273071401074,20.0213203435596)) ;
#97874 = CARTESIAN_POINT('Ctrl Pts',(54.8741225322591,253.140600606275,20.0395012945359)) ;
#97875 = CARTESIAN_POINT('Ctrl Pts',(54.6994917884722,252.999180185916,20.0023959135144)) ;
#97876 = CARTESIAN_POINT('Ctrl Pts',(54.543994900258,252.887271264403,19.9085916079623)) ;
#97877 = CARTESIAN_POINT('Ctrl Pts',(54.7918993697755,253.404382306274,20.1298482803242)) ;
#97878 = CARTESIAN_POINT('Ctrl Pts',(54.6768965504056,253.246681966159,20.1631091706864)) ;
#97879 = CARTESIAN_POINT('Ctrl Pts',(54.5281738146352,253.064653115969,20.1270177316471)) ;
#97880 = CARTESIAN_POINT('Ctrl Pts',(54.3903551301296,252.918991125035,20.0116083456393)) ;
#97881 = CARTESIAN_POINT('Ctrl Pts',(54.6981591247668,253.459073068968,20.3904206496601)) ;
#97882 = CARTESIAN_POINT('Ctrl Pts',(54.573930262351,253.24541189438,20.4018503552973)) ;
#97883 = CARTESIAN_POINT('Ctrl Pts',(54.41949641419,253.033434868643,20.3194987016572)) ;
#97884 = CARTESIAN_POINT('Ctrl Pts',(54.2808206834693,252.870551298285,20.1561059751854)) ;
#97885 = CARTESIAN_POINT('Ctrl Pts',(54.6981591247668,253.459073068968,20.5213203435596)) ;
#97886 = CARTESIAN_POINT('Ctrl Pts',(54.5581902456889,253.219165699388,20.5213203435596)) ;
#97887 = CARTESIAN_POINT('Ctrl Pts',(54.3913470212719,252.996584175367,20.4159476180594)) ;
#97888 = CARTESIAN_POINT('Ctrl Pts',(54.2449695321558,252.82967032967,20.2284271247462)) ;
#97889 = CARTESIAN_POINT('',(54.2449695321558,252.82967032967,20.2284271247462)) ;
#97890 = CARTESIAN_POINT('',(54.6981591247668,253.459073068968,20.5213203435596)) ;
#97891 = CARTESIAN_POINT('Ctrl Pts',(54.2449695321558,252.82967032967,20.2284271247462)) ;
#97892 = CARTESIAN_POINT('Ctrl Pts',(54.3913470212719,252.996584175367,20.4159476180594)) ;
#97893 = CARTESIAN_POINT('Ctrl Pts',(54.5581902456889,253.219165699388,20.5213203435596)) ;
#97894 = CARTESIAN_POINT('Ctrl Pts',(54.6981591247668,253.459073068968,20.5213203435596)) ;
#97895 = CARTESIAN_POINT('Origin',(55.1300306216516,253.207106781187,20.5213203435596)) ;
#97896 = CARTESIAN_POINT('Origin',(54.6208916966195,252.5,20.2284271247462)) ;
#97897 = CARTESIAN_POINT('Origin',(51.2,255.5,20.5213203435596)) ;
#97898 = CARTESIAN_POINT('',(55.25,255.5,20.5213203435596)) ;
#97899 = CARTESIAN_POINT('Origin',(55.75,255.5,20.5213203435596)) ;
#97900 = CARTESIAN_POINT('Origin',(51.2,255.5,20.5213203435596)) ;
#97901 = CARTESIAN_POINT('Origin',(55.75,248.684378986433,20.5213203435596)) ;
#97902 = CARTESIAN_POINT('',(55.25,248.684378986433,20.5213203435596)) ;
#97903 = CARTESIAN_POINT('Ctrl Pts',(47.7791083033805,252.853553390593,19.8748737341529)) ;
#97904 = CARTESIAN_POINT('Ctrl Pts',(47.6146576398327,252.947314708832,19.968635052392)) ;
#97905 = CARTESIAN_POINT('Ctrl Pts',(47.4272201631483,253.072342459309,20.0213203435596)) ;
#97906 = CARTESIAN_POINT('Ctrl Pts',(47.2699693783484,253.207106781187,20.0213203435596)) ;
#97907 = CARTESIAN_POINT('Ctrl Pts',(47.8560050997421,252.887271264403,19.9085916079623)) ;
#97908 = CARTESIAN_POINT('Ctrl Pts',(47.7005064343595,252.999181464919,20.0023969856004)) ;
#97909 = CARTESIAN_POINT('Ctrl Pts',(47.5258791003045,253.140599092271,20.0395015023253)) ;
#97910 = CARTESIAN_POINT('Ctrl Pts',(47.3830330718407,253.273071401074,20.0213203435596)) ;
#97911 = CARTESIAN_POINT('Ctrl Pts',(48.0096449535698,252.918991277155,20.0116082669203)) ;
#97912 = CARTESIAN_POINT('Ctrl Pts',(47.8718246939395,253.064654932855,20.1270189719378)) ;
#97913 = CARTESIAN_POINT('Ctrl Pts',(47.7231052466809,253.246680445441,20.1631089919506)) ;
#97914 = CARTESIAN_POINT('Ctrl Pts',(47.6081011129474,253.404382587908,20.1298477214509)) ;
#97915 = CARTESIAN_POINT('Ctrl Pts',(48.1191793165307,252.870551298284,20.1561059751854)) ;
#97916 = CARTESIAN_POINT('Ctrl Pts',(47.9805020008901,253.033436730234,20.3195005690668)) ;
#97917 = CARTESIAN_POINT('Ctrl Pts',(47.8260711574569,253.245409452453,20.401850485927)) ;
#97918 = CARTESIAN_POINT('Ctrl Pts',(47.7018408752332,253.459073068968,20.3904206496601)) ;
#97919 = CARTESIAN_POINT('Ctrl Pts',(48.1550304678442,252.82967032967,20.2284271247462)) ;
#97920 = CARTESIAN_POINT('Ctrl Pts',(48.0086513057851,252.996586083019,20.4159497612244)) ;
#97921 = CARTESIAN_POINT('Ctrl Pts',(47.8418113540112,253.219162957494,20.5213203435596)) ;
#97922 = CARTESIAN_POINT('Ctrl Pts',(47.7018408752332,253.459073068968,20.5213203435597)) ;
#97923 = CARTESIAN_POINT('',(47.7018408752332,253.459073068968,20.5213203435596)) ;
#97924 = CARTESIAN_POINT('Origin',(47.2699693783484,253.207106781187,20.5213203435596)) ;
#97925 = CARTESIAN_POINT('',(48.1550304678442,252.82967032967,20.2284271247462)) ;
#97926 = CARTESIAN_POINT('Ctrl Pts',(47.7018408752332,253.459073068968,20.5213203435597)) ;
#97927 = CARTESIAN_POINT('Ctrl Pts',(47.8418113540112,253.219162957494,20.5213203435596)) ;
#97928 = CARTESIAN_POINT('Ctrl Pts',(48.0086513057851,252.996586083019,20.4159497612244)) ;
#97929 = CARTESIAN_POINT('Ctrl Pts',(48.1550304678442,252.82967032967,20.2284271247462)) ;
#97930 = CARTESIAN_POINT('Origin',(47.7791083033805,252.5,20.2284271247462)) ;
#97931 = CARTESIAN_POINT('Origin',(46.65,248.108305665508,20.5213203435596)) ;
#97932 = CARTESIAN_POINT('',(47.15,256.652146641849,20.5213203435596)) ;
#97933 = CARTESIAN_POINT('',(47.15,255.5,20.5213203435596)) ;
#97934 = CARTESIAN_POINT('',(47.15,248.108305665508,20.5213203435596)) ;
#97935 = CARTESIAN_POINT('Origin',(46.65,255.5,20.5213203435596)) ;
#97936 = CARTESIAN_POINT('Ctrl Pts',(46.65,256.631336165532,20.0213203435596)) ;
#97937 = CARTESIAN_POINT('Ctrl Pts',(46.6514671918867,256.63139550792,20.0213203435596)) ;
#97938 = CARTESIAN_POINT('Ctrl Pts',(46.6529343761326,256.631454864325,20.0213268015157)) ;
#97939 = CARTESIAN_POINT('Ctrl Pts',(46.6544015101042,256.631514233046,20.0213397172261)) ;
#97940 = CARTESIAN_POINT('Ctrl Pts',(46.7203305551572,256.634182103317,20.0219201144309)) ;
#97941 = CARTESIAN_POINT('Ctrl Pts',(46.7855013662124,256.636849380763,20.0355352673941)) ;
#97942 = CARTESIAN_POINT('Ctrl Pts',(46.8461530161737,256.639357070684,20.0614029659297)) ;
#97943 = CARTESIAN_POINT('Ctrl Pts',(46.9060343348199,256.641832910654,20.0869421210828)) ;
#97944 = CARTESIAN_POINT('Ctrl Pts',(46.9603637316979,256.644105318551,20.1239355278407)) ;
#97945 = CARTESIAN_POINT('Ctrl Pts',(47.0060778798002,256.646031042763,20.1703095979734)) ;
#97946 = CARTESIAN_POINT('Ctrl Pts',(47.0517488890642,256.647954949736,20.2166399065224)) ;
#97947 = CARTESIAN_POINT('Ctrl Pts',(47.0879484176928,256.64949525193,20.2714483566738)) ;
#97948 = CARTESIAN_POINT('Ctrl Pts',(47.1126328493083,256.65054853451,20.3316605250927)) ;
#97949 = CARTESIAN_POINT('Ctrl Pts',(47.1373050471702,256.651601295077,20.3918428519969)) ;
#97950 = CARTESIAN_POINT('Ctrl Pts',(47.15,256.652146641849,20.4562688621889)) ;
#97951 = CARTESIAN_POINT('Ctrl Pts',(47.15,256.652146641849,20.5213203435596)) ;
#97952 = CARTESIAN_POINT('Origin',(51.2,255.5,20.5213203435596)) ;
#97953 = CARTESIAN_POINT('Origin',(51.2,255.5,20.5213203435596)) ;
#97954 = CARTESIAN_POINT('Ctrl Pts',(48.1355790860796,252.851993235277,20.2592073869394)) ;
#97955 = CARTESIAN_POINT('Ctrl Pts',(48.7856610521171,252.099095428559,19.4120715145791)) ;
#97956 = CARTESIAN_POINT('Ctrl Pts',(50.342337689149,251.274913578509,18.4844993376728)) ;
#97957 = CARTESIAN_POINT('Ctrl Pts',(52.7133682967689,251.567886823659,18.8142366178283)) ;
#97958 = CARTESIAN_POINT('Ctrl Pts',(53.8285998534377,252.347462033393,19.6915256689909)) ;
#97959 = CARTESIAN_POINT('Ctrl Pts',(54.2644232365963,252.851990549191,20.2592043594362)) ;
#97960 = CARTESIAN_POINT('Ctrl Pts',(48.0947719613241,252.900740969046,20.1752401619291)) ;
#97961 = CARTESIAN_POINT('Ctrl Pts',(48.7436831353515,252.124455787674,19.3330903436158)) ;
#97962 = CARTESIAN_POINT('Ctrl Pts',(50.3251986179094,251.268368342706,18.4095681618135)) ;
#97963 = CARTESIAN_POINT('Ctrl Pts',(52.7427942699489,251.572994887056,18.7379268805199)) ;
#97964 = CARTESIAN_POINT('Ctrl Pts',(53.8701809022354,252.380543404302,19.6109011660618)) ;
#97965 = CARTESIAN_POINT('Ctrl Pts',(54.3052306275292,252.900738052886,20.1752371160155)) ;
#97966 = CARTESIAN_POINT('Ctrl Pts',(47.9783044652226,252.946300082069,20.029175924824)) ;
#97967 = CARTESIAN_POINT('Ctrl Pts',(48.6482204122624,252.129646231424,19.1954309996876)) ;
#97968 = CARTESIAN_POINT('Ctrl Pts',(50.2904824667079,251.229464286701,18.2789505158584)) ;
#97969 = CARTESIAN_POINT('Ctrl Pts',(52.803616289905,251.549739273436,18.6049035944158)) ;
#97970 = CARTESIAN_POINT('Ctrl Pts',(53.9725652609706,252.39905095601,19.4704714029658)) ;
#97971 = CARTESIAN_POINT('Ctrl Pts',(54.4216982315916,252.946297015605,20.029172854931)) ;
#97972 = CARTESIAN_POINT('Ctrl Pts',(47.8218443356631,252.909567273718,19.9308856107869)) ;
#97973 = CARTESIAN_POINT('Ctrl Pts',(48.5341561059935,252.069093188583,19.0904741258717)) ;
#97974 = CARTESIAN_POINT('Ctrl Pts',(50.2520089559848,251.147381593048,18.168769389023)) ;
#97975 = CARTESIAN_POINT('Ctrl Pts',(52.8723457948022,251.475101351358,18.4964880562147)) ;
#97976 = CARTESIAN_POINT('Ctrl Pts',(54.100611059619,252.346351184295,19.3677115571897)) ;
#97977 = CARTESIAN_POINT('Ctrl Pts',(54.5781583101924,252.90956423463,19.9308825698009)) ;
#97978 = CARTESIAN_POINT('Ctrl Pts',(47.7553501107488,252.880874227796,19.9021945713554)) ;
#97979 = CARTESIAN_POINT('Ctrl Pts',(48.4856433188052,252.033943681986,19.0552640255452)) ;
#97980 = CARTESIAN_POINT('Ctrl Pts',(50.2356583566825,251.106538354053,18.1278586976125)) ;
#97981 = CARTESIAN_POINT('Ctrl Pts',(52.9015694301209,251.436218838326,18.4575391818863)) ;
#97982 = CARTESIAN_POINT('Ctrl Pts',(54.1550539561438,252.313330163616,19.3346505071756)) ;
#97983 = CARTESIAN_POINT('Ctrl Pts',(54.6446525108684,252.880871199536,19.9021915430963)) ;
#97984 = CARTESIAN_POINT('Origin',(51.2,255.5,23.2284271247462)) ;
#97985 = CARTESIAN_POINT('Origin',(46.6350889359327,252.258305665508,20.5213203435596)) ;
#97986 = CARTESIAN_POINT('',(47.1350889359327,261.466666666667,20.5213203435596)) ;
#97987 = CARTESIAN_POINT('Origin',(46.6350889359327,261.466666666667,20.5213203435596)) ;
#97988 = CARTESIAN_POINT('',(47.1350889359327,257.,20.5213203435596)) ;
#97989 = CARTESIAN_POINT('',(47.1350889359327,252.258305665508,20.5213203435596)) ;
#97990 = CARTESIAN_POINT('Origin',(46.6350889359327,257.,20.5213203435596)) ;
#97991 = CARTESIAN_POINT('Origin',(51.2,257.,20.5213203435596)) ;
#97992 = CARTESIAN_POINT('Origin',(51.2,257.,20.5213203435596)) ;
#97993 = CARTESIAN_POINT('Ctrl Pts',(46.6350889359327,261.46666666666,20.0213203435596)) ;
#97994 = CARTESIAN_POINT('Ctrl Pts',(46.6350889359326,261.51358669041,20.0213203435594)) ;
#97995 = CARTESIAN_POINT('Ctrl Pts',(46.6263598493585,261.559687576261,20.0213203435597)) ;
#97996 = CARTESIAN_POINT('Ctrl Pts',(47.135088935933,261.46666666666,20.0213203435596)) ;
#97997 = CARTESIAN_POINT('Ctrl Pts',(47.1350889359328,261.560506714154,20.0213203435591)) ;
#97998 = CARTESIAN_POINT('Ctrl Pts',(47.1176307627857,261.65270848585,20.0213203435596)) ;
#97999 = CARTESIAN_POINT('Ctrl Pts',(47.1350889359328,261.466666666663,20.5213203435598)) ;
#98000 = CARTESIAN_POINT('Ctrl Pts',(47.1350889359326,261.560506714153,20.5213203435594)) ;
#98001 = CARTESIAN_POINT('Ctrl Pts',(47.117630762786,261.652708485847,20.5213203435599)) ;
#98002 = CARTESIAN_POINT('Origin',(46.1350889359327,261.466666666667,20.5213203435596)) ;
#98003 = CARTESIAN_POINT('Origin',(55.7649110640674,248.858305665508,20.5213203435596)) ;
#98004 = CARTESIAN_POINT('',(55.2649110640674,248.858305665508,20.5213203435596)) ;
#98005 = CARTESIAN_POINT('Origin',(68.6350889359325,252.258305665508,20.5213203435596)) ;
#98006 = CARTESIAN_POINT('',(69.1350889359328,261.466666666667,20.5213203435596)) ;
#98007 = CARTESIAN_POINT('Origin',(68.6350889359328,261.466666666667,20.5213203435596)) ;
#98008 = CARTESIAN_POINT('',(69.1350889359327,257.,20.5213203435596)) ;
#98009 = CARTESIAN_POINT('',(69.1350889359325,252.258305665508,20.5213203435596)) ;
#98010 = CARTESIAN_POINT('Origin',(68.6350889359327,257.,20.5213203435596)) ;
#98011 = CARTESIAN_POINT('Origin',(73.2,257.,20.5213203435596)) ;
#98012 = CARTESIAN_POINT('Origin',(73.2,257.,20.5213203435596)) ;
#98013 = CARTESIAN_POINT('Origin',(57.665166384558,263.475191490368,22.9157002361986)) ;
#98014 = CARTESIAN_POINT('',(57.2649110640674,263.8,22.8217108732387)) ;
#98015 = CARTESIAN_POINT('',(57.5776651911054,263.8,22.5213203435596)) ;
#98016 = CARTESIAN_POINT('Origin',(58.0982443974007,263.8,23.3217108732387)) ;
#98017 = CARTESIAN_POINT('',(55.9649110640674,262.590434404722,21.0093633494615)) ;
#98018 = CARTESIAN_POINT('',(57.665166384558,263.865625895089,22.6033527124214)) ;
#98019 = CARTESIAN_POINT('',(55.6649110640674,262.6,21.3217108732387)) ;
#98020 = CARTESIAN_POINT('Origin',(55.9649110640674,262.2,21.3217108732387)) ;
#98021 = CARTESIAN_POINT('',(57.365166384558,263.875191490368,22.9157002361986)) ;
#98022 = CARTESIAN_POINT('Ctrl Pts',(55.9650977189936,262.590464694559,21.0094012321746)) ;
#98023 = CARTESIAN_POINT('Ctrl Pts',(55.8927140481104,262.53619262041,20.9415612709441)) ;
#98024 = CARTESIAN_POINT('Ctrl Pts',(55.8355197652987,262.461874531184,20.848663071755)) ;
#98025 = CARTESIAN_POINT('Ctrl Pts',(55.8015907112375,262.378001899972,20.7438227615689)) ;
#98026 = CARTESIAN_POINT('Ctrl Pts',(55.9077153029172,262.620351120509,21.0467320017693)) ;
#98027 = CARTESIAN_POINT('Ctrl Pts',(55.8195025091066,262.563096995791,20.9750736401434)) ;
#98028 = CARTESIAN_POINT('Ctrl Pts',(55.7469181715793,262.484205180484,20.8768444382602)) ;
#98029 = CARTESIAN_POINT('Ctrl Pts',(55.6986544996547,262.394288534095,20.7641242532738)) ;
#98030 = CARTESIAN_POINT('Ctrl Pts',(55.7930388940241,262.653447436406,21.1426403859049)) ;
#98031 = CARTESIAN_POINT('Ctrl Pts',(55.6732458887353,262.583510286414,21.0686846092405)) ;
#98032 = CARTESIAN_POINT('Ctrl Pts',(55.5698160988869,262.486660039231,20.9668129965483)) ;
#98033 = CARTESIAN_POINT('Ctrl Pts',(55.4933050272729,262.371949383066,20.8484878936816)) ;
#98034 = CARTESIAN_POINT('Ctrl Pts',(55.700947067087,262.62701282797,21.26207073822)) ;
#98035 = CARTESIAN_POINT('Ctrl Pts',(55.5611083984992,262.53238639435,21.1921713125216)) ;
#98036 = CARTESIAN_POINT('Ctrl Pts',(55.445503826815,262.401589921389,21.0962896327055)) ;
#98037 = CARTESIAN_POINT('Ctrl Pts',(55.3681023539349,262.2496543881,20.9868645016167)) ;
#98038 = CARTESIAN_POINT('Ctrl Pts',(55.6651117444407,262.600150470022,21.3218049170024)) ;
#98039 = CARTESIAN_POINT('Ctrl Pts',(55.5202967823214,262.49159734544,21.2539592141385)) ;
#98040 = CARTESIAN_POINT('Ctrl Pts',(55.4058619171326,262.342947400721,21.1610529986893)) ;
#98041 = CARTESIAN_POINT('Ctrl Pts',(55.337960684994,262.175183945868,21.0562008394061)) ;
#98042 = CARTESIAN_POINT('Origin',(56.2649110640674,261.8,20.8217108732387)) ;
#98043 = CARTESIAN_POINT('Origin',(56.2649110640674,262.190434404722,20.5093633494615)) ;
#98044 = CARTESIAN_POINT('Ctrl Pts',(68.6350889359328,261.466666666666,20.0213203435596)) ;
#98045 = CARTESIAN_POINT('Ctrl Pts',(68.6350889359328,261.513586690411,20.0213203435595)) ;
#98046 = CARTESIAN_POINT('Ctrl Pts',(68.6263598493592,261.559687576258,20.0213203435596)) ;
#98047 = CARTESIAN_POINT('Ctrl Pts',(69.1350889359329,261.466666666666,20.0213203435596)) ;
#98048 = CARTESIAN_POINT('Ctrl Pts',(69.1350889359329,261.560506714156,20.0213203435594)) ;
#98049 = CARTESIAN_POINT('Ctrl Pts',(69.1176307627859,261.652708485848,20.0213203435596)) ;
#98050 = CARTESIAN_POINT('Ctrl Pts',(69.1350889359328,261.466666666667,20.5213203435597)) ;
#98051 = CARTESIAN_POINT('Ctrl Pts',(69.1350889359328,261.560506714155,20.5213203435595)) ;
#98052 = CARTESIAN_POINT('Ctrl Pts',(69.117630762786,261.652708485847,20.5213203435597)) ;
#98053 = CARTESIAN_POINT('Origin',(68.1350889359328,261.466666666667,20.5213203435596)) ;
#98054 = CARTESIAN_POINT('Ctrl Pts',(68.6262992790349,261.950068411825,20.2089058667418)) ;
#98055 = CARTESIAN_POINT('Ctrl Pts',(68.6121566500185,262.024832042591,20.3023601782468)) ;
#98056 = CARTESIAN_POINT('Ctrl Pts',(68.580666198832,262.09625764165,20.391642490084)) ;
#98057 = CARTESIAN_POINT('Ctrl Pts',(68.5350110422629,262.157126340135,20.4677282733507)) ;
#98058 = CARTESIAN_POINT('Ctrl Pts',(68.7442583098237,261.958793642379,20.2197842337291)) ;
#98059 = CARTESIAN_POINT('Ctrl Pts',(68.718928193498,262.039807922115,20.3214382904355)) ;
#98060 = CARTESIAN_POINT('Ctrl Pts',(68.675218628314,262.116429910232,20.4166884624688)) ;
#98061 = CARTESIAN_POINT('Ctrl Pts',(68.6167573321357,262.181064672381,20.497635456136)) ;
#98062 = CARTESIAN_POINT('Ctrl Pts',(68.9794298419464,261.907069815511,20.2967674292355)) ;
#98063 = CARTESIAN_POINT('Ctrl Pts',(68.9323297883792,262.013111882128,20.4047154391056)) ;
#98064 = CARTESIAN_POINT('Ctrl Pts',(68.8639744001522,262.109285517,20.5046232503294)) ;
#98065 = CARTESIAN_POINT('Ctrl Pts',(68.780076271313,262.189708661292,20.5887317382383)) ;
#98066 = CARTESIAN_POINT('Ctrl Pts',(69.1005251724556,261.743097807743,20.4462783497206)) ;
#98067 = CARTESIAN_POINT('Ctrl Pts',(69.0598088706616,261.88150309857,20.544686653091)) ;
#98068 = CARTESIAN_POINT('Ctrl Pts',(68.9899272559851,262.009912469407,20.6374702762036)) ;
#98069 = CARTESIAN_POINT('Ctrl Pts',(68.8967323918745,262.117798129565,20.7162682354583)) ;
#98070 = CARTESIAN_POINT('Ctrl Pts',(69.1176490922737,261.65261165586,20.5212598248177)) ;
#98071 = CARTESIAN_POINT('Ctrl Pts',(69.0893506066564,261.802146309377,20.6147189832657)) ;
#98072 = CARTESIAN_POINT('Ctrl Pts',(69.0263552568489,261.945003652573,20.7040048227633)) ;
#98073 = CARTESIAN_POINT('Ctrl Pts',(68.9350298022437,262.066745503355,20.7800934795019)) ;
#98074 = CARTESIAN_POINT('',(68.5350889359328,262.157101071388,20.4676966827948)) ;
#98075 = CARTESIAN_POINT('',(68.9350889359328,262.066666666667,20.780044206572)) ;
#98076 = CARTESIAN_POINT('Origin',(68.5350889359328,261.766666666667,20.780044206572)) ;
#98077 = CARTESIAN_POINT('Origin',(68.1350889359328,261.466666666667,20.405044206572)) ;
#98078 = CARTESIAN_POINT('Origin',(68.1350889359328,261.857101071388,20.0926966827948)) ;
#98079 = CARTESIAN_POINT('Origin',(65.6921072521396,265.557308911724,25.5183470128943)) ;
#98080 = CARTESIAN_POINT('',(67.3029147394739,263.8,22.5213203435596)) ;
#98081 = CARTESIAN_POINT('',(67.6350889359328,263.8,22.9467108732387)) ;
#98082 = CARTESIAN_POINT('Origin',(67.0100889359328,263.8,23.3217108732387)) ;
#98083 = CARTESIAN_POINT('',(66.0921072521396,265.857308911724,25.5183470128943)) ;
#98084 = CARTESIAN_POINT('',(65.6921072521396,265.947743316446,25.205999489117)) ;
#98085 = CARTESIAN_POINT('Origin',(77.3541022134511,261.790576660088,20.8099316983491)) ;
#98086 = CARTESIAN_POINT('',(77.9,262.590434404722,21.0093633494615)) ;
#98087 = CARTESIAN_POINT('',(77.3541022134511,262.18101106481,20.4975841745719)) ;
#98088 = CARTESIAN_POINT('',(77.6,262.6,21.3217108732387)) ;
#98089 = CARTESIAN_POINT('Origin',(77.9,262.2,21.3217108732387)) ;
#98090 = CARTESIAN_POINT('',(77.0541022134511,262.190576660088,20.8099316983491)) ;
#98091 = CARTESIAN_POINT('Ctrl Pts',(77.9013408131542,262.590650840007,21.0096349450888)) ;
#98092 = CARTESIAN_POINT('Ctrl Pts',(77.7773296632107,262.497850078956,20.8936360832999)) ;
#98093 = CARTESIAN_POINT('Ctrl Pts',(77.7008997254075,262.344523367308,20.7019653495671)) ;
#98094 = CARTESIAN_POINT('Ctrl Pts',(77.7014183412461,262.189532131413,20.5082389714827)) ;
#98095 = CARTESIAN_POINT('Ctrl Pts',(77.8439164601299,262.620738304929,21.0470483108589)) ;
#98096 = CARTESIAN_POINT('Ctrl Pts',(77.6926768304702,262.522860915164,20.9244672749778)) ;
#98097 = CARTESIAN_POINT('Ctrl Pts',(77.5898523574372,262.360080698584,20.722059188087)) ;
#98098 = CARTESIAN_POINT('Ctrl Pts',(77.5699237452358,262.189749951308,20.5078746887228)) ;
#98099 = CARTESIAN_POINT('Ctrl Pts',(77.7292852020685,262.654121976102,21.1430750184117)) ;
#98100 = CARTESIAN_POINT('Ctrl Pts',(77.5237875914152,262.53454414738,21.0165447946381)) ;
#98101 = CARTESIAN_POINT('Ctrl Pts',(77.3673899123099,262.334900270471,20.8066567599894)) ;
#98102 = CARTESIAN_POINT('Ctrl Pts',(77.3083819928147,262.104716141742,20.5755253312968)) ;
#98103 = CARTESIAN_POINT('Ctrl Pts',(77.6372360358209,262.62782351523,21.2626696196308)) ;
#98104 = CARTESIAN_POINT('Ctrl Pts',(77.397228569769,262.465950156281,21.1430850537563)) ;
#98105 = CARTESIAN_POINT('Ctrl Pts',(77.2317300815822,262.195301292123,20.9454483332071)) ;
#98106 = CARTESIAN_POINT('Ctrl Pts',(77.19981303009,261.900502715367,20.7387374087547)) ;
#98107 = CARTESIAN_POINT('Ctrl Pts',(77.6014435723759,262.601080513305,21.3223861940545)) ;
#98108 = CARTESIAN_POINT('Ctrl Pts',(77.3528342375612,262.415369091606,21.2063165554919)) ;
#98109 = CARTESIAN_POINT('Ctrl Pts',(77.1994052692525,262.108511154987,21.0145303451059)) ;
#98110 = CARTESIAN_POINT('Ctrl Pts',(77.2000017327813,261.798196834116,20.820583894561)) ;
#98111 = CARTESIAN_POINT('',(77.7,262.190434404721,20.5093633494615)) ;
#98112 = CARTESIAN_POINT('',(77.2,261.8,20.8217108732387)) ;
#98113 = CARTESIAN_POINT('Origin',(77.7,261.8,20.8217108732387)) ;
#98114 = CARTESIAN_POINT('Origin',(78.2,261.8,20.8217108732387)) ;
#98115 = CARTESIAN_POINT('Origin',(78.2,262.190434404721,20.5093633494615)) ;
#98116 = CARTESIAN_POINT('Origin',(77.7,263.431230834727,22.8607494166478)) ;
#98117 = CARTESIAN_POINT('',(77.2,263.431230834727,22.8607494166478)) ;
#98118 = CARTESIAN_POINT('',(77.7,263.821665239449,22.5484018928706)) ;
#98119 = CARTESIAN_POINT('Origin',(47.15,255.5,30.7213203435596)) ;
#98120 = CARTESIAN_POINT('',(47.15,256.652146641849,29.5213203435596)) ;
#98121 = CARTESIAN_POINT('',(47.15,255.5,30.7213203435596)) ;
#98122 = CARTESIAN_POINT('Origin',(51.2,257.,29.5213203435596)) ;
#98123 = CARTESIAN_POINT('',(47.1350889359327,257.,29.5213203435596)) ;
#98124 = CARTESIAN_POINT('Origin',(47.1350889359327,263.8,29.5213203435596)) ;
#98125 = CARTESIAN_POINT('',(47.1350889359327,261.466666666667,29.5213203435596)) ;
#98126 = CARTESIAN_POINT('Origin',(46.1350889359327,261.466666666667,29.5213203435596)) ;
#98127 = CARTESIAN_POINT('',(46.9350889359326,262.066666666667,29.5213203435596)) ;
#98128 = CARTESIAN_POINT('Origin',(46.3850889359327,262.8,29.5213203435596)) ;
#98129 = CARTESIAN_POINT('Origin',(66.207090707265,262.8,21.2713203435596)) ;
#98130 = CARTESIAN_POINT('Origin',(33.6,245.6,29.5213203435596)) ;
#98131 = CARTESIAN_POINT('Origin',(33.6,245.6,20.0213203435596)) ;
#98132 = CARTESIAN_POINT('Origin',(51.2,257.,29.5213203435596)) ;
#98133 = CARTESIAN_POINT('',(55.25,256.652146641849,29.5213203435596)) ;
#98134 = CARTESIAN_POINT('',(55.2649110640674,257.,29.5213203435596)) ;
#98135 = CARTESIAN_POINT('Origin',(73.2,257.,29.5213203435596)) ;
#98136 = CARTESIAN_POINT('',(69.1350889359327,257.,29.5213203435596)) ;
#98137 = CARTESIAN_POINT('',(69.15,256.652146641849,29.5213203435596)) ;
#98138 = CARTESIAN_POINT('Origin',(74.6,224.285258985103,29.5213203435596)) ;
#98139 = CARTESIAN_POINT('',(74.6,224.787496202879,25.7213203435596)) ;
#98140 = CARTESIAN_POINT('',(74.6,224.787496202879,30.7213203435596)) ;
#98141 = CARTESIAN_POINT('',(74.6000000000001,225.9,25.7213203435596)) ;
#98142 = CARTESIAN_POINT('',(74.6000000000001,225.9,29.5213203435596)) ;
#98143 = CARTESIAN_POINT('',(74.6,225.892629492551,25.7213203435596)) ;
#98144 = CARTESIAN_POINT('Origin',(74.4,225.9,29.5213203435596)) ;
#98145 = CARTESIAN_POINT('',(74.4,226.1,25.7213203435596)) ;
#98146 = CARTESIAN_POINT('Origin',(74.4,225.9,25.7213203435596)) ;
#98147 = CARTESIAN_POINT('',(74.4,226.1,29.5213203435596)) ;
#98148 = CARTESIAN_POINT('Origin',(74.4,226.1,29.5213203435596)) ;
#98149 = CARTESIAN_POINT('',(74.3,226.1,25.7213203435596)) ;
#98150 = CARTESIAN_POINT('',(73.7,226.1,25.7213203435596)) ;
#98151 = CARTESIAN_POINT('',(74.3,226.1,29.5213203435596)) ;
#98152 = CARTESIAN_POINT('Origin',(74.3,226.1,29.5213203435596)) ;
#98153 = CARTESIAN_POINT('',(74.3,231.9,25.7213203435596)) ;
#98154 = CARTESIAN_POINT('',(74.3,226.8,25.7213203435596)) ;
#98155 = CARTESIAN_POINT('',(74.3,231.9,29.5213203435596)) ;
#98156 = CARTESIAN_POINT('Origin',(74.1,231.9,29.5213203435596)) ;
#98157 = CARTESIAN_POINT('',(74.1,232.1,25.7213203435596)) ;
#98158 = CARTESIAN_POINT('Origin',(74.1,231.9,25.7213203435596)) ;
#98159 = CARTESIAN_POINT('',(74.1,232.1,29.5213203435596)) ;
#98160 = CARTESIAN_POINT('Origin',(74.1,232.1,29.5213203435596)) ;
#98161 = CARTESIAN_POINT('',(71.9,232.1,25.7213203435596)) ;
#98162 = CARTESIAN_POINT('',(73.55,232.1,25.7213203435596)) ;
#98163 = CARTESIAN_POINT('',(71.9,232.1,29.5213203435596)) ;
#98164 = CARTESIAN_POINT('Origin',(71.9,231.9,29.5213203435596)) ;
#98165 = CARTESIAN_POINT('',(71.7,231.9,25.7213203435596)) ;
#98166 = CARTESIAN_POINT('Origin',(71.9,231.9,25.7213203435596)) ;
#98167 = CARTESIAN_POINT('',(71.7,231.9,29.5213203435596)) ;
#98168 = CARTESIAN_POINT('Origin',(71.7,231.9,29.5213203435596)) ;
#98169 = CARTESIAN_POINT('',(71.7,226.1,25.7213203435596)) ;
#98170 = CARTESIAN_POINT('',(71.7,229.7,25.7213203435596)) ;
#98171 = CARTESIAN_POINT('',(71.7,226.1,29.5213203435596)) ;
#98172 = CARTESIAN_POINT('Origin',(71.7,226.1,29.5213203435596)) ;
#98173 = CARTESIAN_POINT('',(71.6,226.1,25.7213203435596)) ;
#98174 = CARTESIAN_POINT('',(72.3500000000003,226.1,25.7213203435596)) ;
#98175 = CARTESIAN_POINT('',(71.6,226.1,29.5213203435596)) ;
#98176 = CARTESIAN_POINT('Ctrl Pts',(46.3,248.9,29.5213203435596)) ;
#98177 = CARTESIAN_POINT('Ctrl Pts',(46.3,248.9,18.1213203435596)) ;
#98178 = CARTESIAN_POINT('Ctrl Pts',(46.2722901777919,248.927709822208,29.5213203435596)) ;
#98179 = CARTESIAN_POINT('Ctrl Pts',(46.2722901777919,248.927709822208,18.1213203435596)) ;
#98180 = CARTESIAN_POINT('Ctrl Pts',(46.2384776727796,248.960391271619,29.5213203435596)) ;
#98181 = CARTESIAN_POINT('Ctrl Pts',(46.2384776727796,248.960391271619,18.1213203435596)) ;
#98182 = CARTESIAN_POINT('Ctrl Pts',(46.1815269526849,248.99104280001,29.5213203435596)) ;
#98183 = CARTESIAN_POINT('Ctrl Pts',(46.1815269526849,248.99104280001,18.1213203435596)) ;
#98184 = CARTESIAN_POINT('Ctrl Pts',(46.1522826614306,249.,29.5213203435596)) ;
#98185 = CARTESIAN_POINT('Ctrl Pts',(46.1522826614306,249.,18.1213203435596)) ;
#98186 = CARTESIAN_POINT('Ctrl Pts',(46.1267949192431,249.,29.5213203435596)) ;
#98187 = CARTESIAN_POINT('Ctrl Pts',(46.1267949192431,249.,18.1213203435596)) ;
#98188 = CARTESIAN_POINT('',(46.1267949192431,249.,20.0213203435596)) ;
#98189 = CARTESIAN_POINT('',(46.1267949192431,249.,29.5213203435596)) ;
#98190 = CARTESIAN_POINT('Ctrl Pts',(46.3,248.9,20.0213203435596)) ;
#98191 = CARTESIAN_POINT('Ctrl Pts',(46.2722901777919,248.927709822208,20.0213203435596)) ;
#98192 = CARTESIAN_POINT('Ctrl Pts',(46.2384776727796,248.960391271619,20.0213203435596)) ;
#98193 = CARTESIAN_POINT('Ctrl Pts',(46.1815269526849,248.99104280001,20.0213203435596)) ;
#98194 = CARTESIAN_POINT('Ctrl Pts',(46.1522826614306,249.,20.0213203435596)) ;
#98195 = CARTESIAN_POINT('Ctrl Pts',(46.1267949192431,249.,20.0213203435596)) ;
#98196 = CARTESIAN_POINT('Origin',(46.1267949192431,249.,29.5213203435596)) ;
#98197 = CARTESIAN_POINT('',(34.2732050807569,249.,20.0213203435596)) ;
#98198 = CARTESIAN_POINT('',(34.2732050807569,249.,29.5213203435596)) ;
#98199 = CARTESIAN_POINT('',(46.1267949192431,249.,20.0213203435596)) ;
#98200 = CARTESIAN_POINT('Ctrl Pts',(34.2732050807569,249.,29.5213203435596)) ;
#98201 = CARTESIAN_POINT('Ctrl Pts',(34.2732050807569,249.,18.1213203435596)) ;
#98202 = CARTESIAN_POINT('Ctrl Pts',(34.2477173385693,249.,29.5213203435596)) ;
#98203 = CARTESIAN_POINT('Ctrl Pts',(34.2477173385693,249.,18.1213203435596)) ;
#98204 = CARTESIAN_POINT('Ctrl Pts',(34.2184730473151,248.99104280001,29.5213203435596)) ;
#98205 = CARTESIAN_POINT('Ctrl Pts',(34.2184730473151,248.99104280001,18.1213203435596)) ;
#98206 = CARTESIAN_POINT('Ctrl Pts',(34.1615223272204,248.960391271619,29.5213203435596)) ;
#98207 = CARTESIAN_POINT('Ctrl Pts',(34.1615223272204,248.960391271619,18.1213203435596)) ;
#98208 = CARTESIAN_POINT('Ctrl Pts',(34.1277098222081,248.927709822208,29.5213203435596)) ;
#98209 = CARTESIAN_POINT('Ctrl Pts',(34.1277098222081,248.927709822208,18.1213203435596)) ;
#98210 = CARTESIAN_POINT('Ctrl Pts',(34.1,248.9,29.5213203435596)) ;
#98211 = CARTESIAN_POINT('Ctrl Pts',(34.1,248.9,18.1213203435596)) ;
#98212 = CARTESIAN_POINT('Ctrl Pts',(34.2732050807569,249.,20.0213203435596)) ;
#98213 = CARTESIAN_POINT('Ctrl Pts',(34.2477173385693,249.,20.0213203435596)) ;
#98214 = CARTESIAN_POINT('Ctrl Pts',(34.2184730473151,248.99104280001,20.0213203435596)) ;
#98215 = CARTESIAN_POINT('Ctrl Pts',(34.1615223272204,248.960391271619,20.0213203435596)) ;
#98216 = CARTESIAN_POINT('Ctrl Pts',(34.1277098222081,248.927709822208,20.0213203435596)) ;
#98217 = CARTESIAN_POINT('Ctrl Pts',(34.1,248.9,20.0213203435596)) ;
#98218 = CARTESIAN_POINT('Origin',(43.1,259.9,29.5213203435596)) ;
#98219 = CARTESIAN_POINT('',(43.1,260.1,29.5213203435596)) ;
#98220 = CARTESIAN_POINT('Origin',(43.1,260.1,29.5213203435596)) ;
#98221 = CARTESIAN_POINT('',(37.3,260.1,29.5213203435596)) ;
#98222 = CARTESIAN_POINT('',(42.2,260.1,25.0213203435596)) ;
#98223 = CARTESIAN_POINT('Origin',(40.2,260.1,25.0213203435596)) ;
#98224 = CARTESIAN_POINT('Origin',(37.3,259.9,29.5213203435596)) ;
#98225 = CARTESIAN_POINT('Origin',(30.7,254.8,29.5213203435596)) ;
#98226 = CARTESIAN_POINT('',(28.1,254.8,25.7213203435596)) ;
#98227 = CARTESIAN_POINT('',(28.1,254.8,29.5213203435596)) ;
#98228 = CARTESIAN_POINT('Origin',(30.7,254.8,25.7213203435596)) ;
#98229 = CARTESIAN_POINT('Origin',(75.1,252.658578643763,29.5213203435596)) ;
#98230 = CARTESIAN_POINT('',(75.1,251.923339546448,25.7213203435596)) ;
#98231 = CARTESIAN_POINT('',(75.1,251.923339546448,30.7213203435596)) ;
#98232 = CARTESIAN_POINT('',(75.1,249.341421356237,25.7213203435596)) ;
#98233 = CARTESIAN_POINT('',(75.1,249.341421356237,29.5213203435596)) ;
#98234 = CARTESIAN_POINT('',(75.1,251.829289321881,25.7213203435596)) ;
#98235 = CARTESIAN_POINT('Origin',(75.3,249.341421356237,29.5213203435596)) ;
#98236 = CARTESIAN_POINT('',(75.1585786437627,249.2,25.7213203435596)) ;
#98237 = CARTESIAN_POINT('Origin',(75.3,249.341421356237,25.7213203435596)) ;
#98238 = CARTESIAN_POINT('',(75.1585786437627,249.2,29.5213203435596)) ;
#98239 = CARTESIAN_POINT('Origin',(75.1585786437627,249.2,29.5213203435596)) ;
#98240 = CARTESIAN_POINT('',(75.8999999999999,248.458578643763,25.7213203435596)) ;
#98241 = CARTESIAN_POINT('',(75.343933982822,249.014644660941,25.7213203435596)) ;
#98242 = CARTESIAN_POINT('',(75.8999999999999,248.458578643763,29.5213203435596)) ;
#98243 = CARTESIAN_POINT('Origin',(76.0414213562372,248.6,29.5213203435596)) ;
#98244 = CARTESIAN_POINT('',(76.0414213562372,248.4,25.7213203435596)) ;
#98245 = CARTESIAN_POINT('Origin',(76.0414213562372,248.6,25.7213203435596)) ;
#98246 = CARTESIAN_POINT('',(76.0414213562372,248.4,29.5213203435596)) ;
#98247 = CARTESIAN_POINT('Origin',(76.0414213562372,248.4,29.5213203435596)) ;
#98248 = CARTESIAN_POINT('',(80.0999999999999,248.4,25.7213203435596)) ;
#98249 = CARTESIAN_POINT('',(76.8707106781186,248.4,25.7213203435596)) ;
#98250 = CARTESIAN_POINT('',(80.0999999999999,248.4,29.5213203435596)) ;
#98251 = CARTESIAN_POINT('Origin',(59.3,248.1,29.5213203435596)) ;
#98252 = CARTESIAN_POINT('',(59.5,248.1,25.7213203435596)) ;
#98253 = CARTESIAN_POINT('',(59.3,247.9,25.7213203435596)) ;
#98254 = CARTESIAN_POINT('Origin',(59.3,248.1,25.7213203435596)) ;
#98255 = CARTESIAN_POINT('',(59.3,247.9,29.5213203435596)) ;
#98256 = CARTESIAN_POINT('',(59.5,248.1,29.5213203435596)) ;
#98257 = CARTESIAN_POINT('Origin',(59.5,248.1,29.5213203435596)) ;
#98258 = CARTESIAN_POINT('',(59.5,250.9,25.7213203435596)) ;
#98259 = CARTESIAN_POINT('',(59.5,250.3,25.7213203435596)) ;
#98260 = CARTESIAN_POINT('',(59.5,250.9,29.5213203435596)) ;
#98261 = CARTESIAN_POINT('Origin',(59.3,250.9,29.5213203435596)) ;
#98262 = CARTESIAN_POINT('',(59.3,251.1,25.7213203435596)) ;
#98263 = CARTESIAN_POINT('Origin',(59.3,250.9,25.7213203435596)) ;
#98264 = CARTESIAN_POINT('',(59.3,251.1,29.5213203435596)) ;
#98265 = CARTESIAN_POINT('Origin',(59.3,251.1,29.5213203435596)) ;
#98266 = CARTESIAN_POINT('',(59.2,251.1,25.7213203435596)) ;
#98267 = CARTESIAN_POINT('',(58.5999999999998,251.1,25.7213203435596)) ;
#98268 = CARTESIAN_POINT('',(59.2,251.1,29.5213203435596)) ;
#98269 = CARTESIAN_POINT('Origin',(59.2,251.1,29.5213203435596)) ;
#98270 = CARTESIAN_POINT('',(59.2,256.9,25.7213203435596)) ;
#98271 = CARTESIAN_POINT('',(59.2,251.8,25.7213203435596)) ;
#98272 = CARTESIAN_POINT('',(59.2,256.9,29.5213203435596)) ;
#98273 = CARTESIAN_POINT('Origin',(59.,256.9,29.5213203435596)) ;
#98274 = CARTESIAN_POINT('',(59.,257.1,25.7213203435596)) ;
#98275 = CARTESIAN_POINT('Origin',(59.,256.9,25.7213203435596)) ;
#98276 = CARTESIAN_POINT('',(59.,257.1,29.5213203435596)) ;
#98277 = CARTESIAN_POINT('Origin',(59.,257.1,29.5213203435596)) ;
#98278 = CARTESIAN_POINT('',(56.8,257.1,25.7213203435596)) ;
#98279 = CARTESIAN_POINT('',(58.45,257.1,25.7213203435596)) ;
#98280 = CARTESIAN_POINT('',(56.8,257.1,29.5213203435596)) ;
#98281 = CARTESIAN_POINT('Origin',(61.5,261.2,29.5213203435596)) ;
#98282 = CARTESIAN_POINT('',(59.,261.2,25.7213203435596)) ;
#98283 = CARTESIAN_POINT('',(59.,261.2,29.5213203435596)) ;
#98284 = CARTESIAN_POINT('Origin',(61.5,261.2,25.7213203435596)) ;
#98285 = CARTESIAN_POINT('Origin',(63.0573593128808,238.841421356237,29.5213203435596)) ;
#98286 = CARTESIAN_POINT('',(63.0573593128808,242.158578643763,25.7213203435596)) ;
#98287 = CARTESIAN_POINT('',(63.0573593128808,238.841421356237,25.7213203435596)) ;
#98288 = CARTESIAN_POINT('',(63.0573593128808,239.670710678119,25.7213203435596)) ;
#98289 = CARTESIAN_POINT('',(63.0573593128808,238.841421356237,29.5213203435596)) ;
#98290 = CARTESIAN_POINT('',(63.0573593128808,242.158578643763,29.5213203435596)) ;
#98291 = CARTESIAN_POINT('Origin',(62.8573593128808,242.158578643763,29.5213203435596)) ;
#98292 = CARTESIAN_POINT('',(62.9987806691181,242.3,25.7213203435596)) ;
#98293 = CARTESIAN_POINT('Origin',(62.8573593128808,242.158578643763,25.7213203435596)) ;
#98294 = CARTESIAN_POINT('',(62.9987806691181,242.3,29.5213203435596)) ;
#98295 = CARTESIAN_POINT('Origin',(62.9987806691181,242.3,29.5213203435596)) ;
#98296 = CARTESIAN_POINT('',(62.2573593128808,243.041421356237,25.7213203435596)) ;
#98297 = CARTESIAN_POINT('',(62.8257680045734,242.473012664545,25.7213203435596)) ;
#98298 = CARTESIAN_POINT('',(62.2573593128808,243.041421356237,29.5213203435596)) ;
#98299 = CARTESIAN_POINT('Origin',(62.1159379566435,242.9,29.5213203435596)) ;
#98300 = CARTESIAN_POINT('',(62.1159379566435,243.1,25.7213203435596)) ;
#98301 = CARTESIAN_POINT('Origin',(62.1159379566435,242.9,25.7213203435596)) ;
#98302 = CARTESIAN_POINT('',(62.1159379566435,243.1,29.5213203435596)) ;
#98303 = CARTESIAN_POINT('Origin',(62.1159379566435,243.1,29.5213203435596)) ;
#98304 = CARTESIAN_POINT('',(58.0573593128808,243.1,25.7213203435596)) ;
#98305 = CARTESIAN_POINT('',(61.3113339837915,243.1,25.7213203435596)) ;
#98306 = CARTESIAN_POINT('',(58.0573593128808,243.1,29.5213203435596)) ;
#98307 = CARTESIAN_POINT('Ctrl Pts',(58.0573593128808,243.1,29.5213203435596)) ;
#98308 = CARTESIAN_POINT('Ctrl Pts',(58.0573593128808,243.1,18.1213203435596)) ;
#98309 = CARTESIAN_POINT('Ctrl Pts',(58.0296494906727,243.072290177792,29.5213203435596)) ;
#98310 = CARTESIAN_POINT('Ctrl Pts',(58.0296494906727,243.072290177792,18.1213203435596)) ;
#98311 = CARTESIAN_POINT('Ctrl Pts',(57.9969680412619,243.03847767278,29.5213203435596)) ;
#98312 = CARTESIAN_POINT('Ctrl Pts',(57.9969680412619,243.03847767278,18.1213203435596)) ;
#98313 = CARTESIAN_POINT('Ctrl Pts',(57.9663165128705,242.981526952685,29.5213203435596)) ;
#98314 = CARTESIAN_POINT('Ctrl Pts',(57.9663165128705,242.981526952685,18.1213203435596)) ;
#98315 = CARTESIAN_POINT('Ctrl Pts',(57.9573593128807,242.952282661431,29.5213203435596)) ;
#98316 = CARTESIAN_POINT('Ctrl Pts',(57.9573593128807,242.952282661431,18.1213203435596)) ;
#98317 = CARTESIAN_POINT('Ctrl Pts',(57.9573593128807,242.926794919243,29.5213203435596)) ;
#98318 = CARTESIAN_POINT('Ctrl Pts',(57.9573593128807,242.926794919243,18.1213203435596)) ;
#98319 = CARTESIAN_POINT('',(57.9573593128808,242.926794919243,25.7213203435596)) ;
#98320 = CARTESIAN_POINT('Ctrl Pts',(57.9573593128807,242.926794919243,25.7213203435596)) ;
#98321 = CARTESIAN_POINT('Ctrl Pts',(57.9573593128807,242.952282661431,25.7213203435596)) ;
#98322 = CARTESIAN_POINT('Ctrl Pts',(57.9663165128705,242.981526952685,25.7213203435596)) ;
#98323 = CARTESIAN_POINT('Ctrl Pts',(57.9969680412619,243.03847767278,25.7213203435596)) ;
#98324 = CARTESIAN_POINT('Ctrl Pts',(58.0296494906727,243.072290177792,25.7213203435596)) ;
#98325 = CARTESIAN_POINT('Ctrl Pts',(58.0573593128808,243.1,25.7213203435596)) ;
#98326 = CARTESIAN_POINT('',(57.9573593128808,242.926794919243,29.5213203435596)) ;
#98327 = CARTESIAN_POINT('Origin',(62.5573593128808,227.1,29.5213203435596)) ;
#98328 = CARTESIAN_POINT('',(62.7573593128808,227.1,25.7213203435596)) ;
#98329 = CARTESIAN_POINT('',(62.5573593128808,226.9,25.7213203435596)) ;
#98330 = CARTESIAN_POINT('Origin',(62.5573593128808,227.1,25.7213203435596)) ;
#98331 = CARTESIAN_POINT('',(62.5573593128808,226.9,29.5213203435596)) ;
#98332 = CARTESIAN_POINT('',(62.7573593128808,227.1,29.5213203435596)) ;
#98333 = CARTESIAN_POINT('Origin',(62.7573593128808,227.1,29.5213203435596)) ;
#98334 = CARTESIAN_POINT('',(62.7573593128808,229.9,25.7213203435596)) ;
#98335 = CARTESIAN_POINT('',(62.7573593128808,229.275314650971,25.7213203435596)) ;
#98336 = CARTESIAN_POINT('',(62.7573593128808,229.9,29.5213203435596)) ;
#98337 = CARTESIAN_POINT('Origin',(62.5573593128808,229.9,29.5213203435596)) ;
#98338 = CARTESIAN_POINT('',(62.5573593128808,230.1,25.7213203435596)) ;
#98339 = CARTESIAN_POINT('Origin',(62.5573593128808,229.9,25.7213203435596)) ;
#98340 = CARTESIAN_POINT('',(62.5573593128808,230.1,29.5213203435596)) ;
#98341 = CARTESIAN_POINT('Origin',(62.5573593128808,230.1,29.5213203435596)) ;
#98342 = CARTESIAN_POINT('',(62.4573593128808,230.1,25.7213203435596)) ;
#98343 = CARTESIAN_POINT('',(61.8573593128805,230.1,25.7213203435596)) ;
#98344 = CARTESIAN_POINT('',(62.4573593128808,230.1,29.5213203435596)) ;
#98345 = CARTESIAN_POINT('Origin',(62.4573593128808,230.1,29.5213203435596)) ;
#98346 = CARTESIAN_POINT('',(62.4573593128808,230.775314650971,25.7213203435596)) ;
#98347 = CARTESIAN_POINT('Origin',(62.2841542321239,236.,29.5213203435596)) ;
#98348 = CARTESIAN_POINT('',(60.0305643936376,236.,25.7213203435596)) ;
#98349 = CARTESIAN_POINT('',(61.7207567725023,236.,25.7213203435596)) ;
#98350 = CARTESIAN_POINT('',(60.0305643936376,236.,29.5213203435596)) ;
#98351 = CARTESIAN_POINT('Origin',(76.0414213562372,225.6,29.5213203435596)) ;
#98352 = CARTESIAN_POINT('',(76.0414213562372,225.5,25.7213203435596)) ;
#98353 = CARTESIAN_POINT('',(75.9707106781185,225.529289321881,25.7213203435596)) ;
#98354 = CARTESIAN_POINT('Origin',(76.0414213562372,225.6,25.7213203435596)) ;
#98355 = CARTESIAN_POINT('',(75.9707106781185,225.529289321881,29.5213203435596)) ;
#98356 = CARTESIAN_POINT('',(76.0414213562372,225.5,29.5213203435596)) ;
#98357 = CARTESIAN_POINT('Origin',(76.0414213562372,225.5,29.5213203435596)) ;
#98358 = CARTESIAN_POINT('',(80.0999999999999,225.5,25.7213203435596)) ;
#98359 = CARTESIAN_POINT('',(76.8707106781186,225.5,25.7213203435596)) ;
#98360 = CARTESIAN_POINT('',(80.,225.5,30.7213203435596)) ;
#98361 = CARTESIAN_POINT('',(80.0999999999999,225.5,29.5213203435596)) ;
#98362 = CARTESIAN_POINT('Origin',(80.0999999999999,225.6,29.5213203435596)) ;
#98363 = CARTESIAN_POINT('',(80.1999999999999,225.6,25.7213203435596)) ;
#98364 = CARTESIAN_POINT('Origin',(80.0999999999999,225.6,25.7213203435596)) ;
#98365 = CARTESIAN_POINT('',(80.1999999999999,225.6,29.5213203435596)) ;
#98366 = CARTESIAN_POINT('Origin',(80.1999999999999,225.6,29.5213203435596)) ;
#98367 = CARTESIAN_POINT('',(80.2,230.4,25.7213203435596)) ;
#98368 = CARTESIAN_POINT('',(80.1999999999999,226.8,25.7213203435596)) ;
#98369 = CARTESIAN_POINT('',(80.2,230.4,29.5213203435596)) ;
#98370 = CARTESIAN_POINT('Origin',(80.1,230.4,29.5213203435596)) ;
#98371 = CARTESIAN_POINT('Origin',(80.1,230.4,25.7213203435596)) ;
#98372 = CARTESIAN_POINT('Origin',(67.3,248.1,29.5213203435596)) ;
#98373 = CARTESIAN_POINT('',(67.5,248.1,25.7213203435596)) ;
#98374 = CARTESIAN_POINT('',(67.3,247.9,25.7213203435596)) ;
#98375 = CARTESIAN_POINT('Origin',(67.3,248.1,25.7213203435596)) ;
#98376 = CARTESIAN_POINT('',(67.3,247.9,29.5213203435596)) ;
#98377 = CARTESIAN_POINT('',(67.5,248.1,29.5213203435596)) ;
#98378 = CARTESIAN_POINT('Origin',(67.5,248.1,29.5213203435596)) ;
#98379 = CARTESIAN_POINT('',(67.5,250.9,25.7213203435596)) ;
#98380 = CARTESIAN_POINT('',(67.5,250.3,25.7213203435596)) ;
#98381 = CARTESIAN_POINT('',(67.5,250.9,29.5213203435596)) ;
#98382 = CARTESIAN_POINT('Origin',(67.3,250.9,29.5213203435596)) ;
#98383 = CARTESIAN_POINT('',(67.3,251.1,25.7213203435596)) ;
#98384 = CARTESIAN_POINT('Origin',(67.3,250.9,25.7213203435596)) ;
#98385 = CARTESIAN_POINT('',(67.3,251.1,29.5213203435596)) ;
#98386 = CARTESIAN_POINT('Origin',(67.3,251.1,29.5213203435596)) ;
#98387 = CARTESIAN_POINT('',(67.2,251.1,25.7213203435596)) ;
#98388 = CARTESIAN_POINT('',(66.5999999999998,251.1,25.7213203435596)) ;
#98389 = CARTESIAN_POINT('',(67.2,251.1,29.5213203435596)) ;
#98390 = CARTESIAN_POINT('Origin',(67.2,251.1,29.5213203435596)) ;
#98391 = CARTESIAN_POINT('',(67.2,256.9,25.7213203435596)) ;
#98392 = CARTESIAN_POINT('',(67.2,251.8,25.7213203435596)) ;
#98393 = CARTESIAN_POINT('',(67.2,256.9,29.5213203435596)) ;
#98394 = CARTESIAN_POINT('Origin',(67.,256.9,29.5213203435596)) ;
#98395 = CARTESIAN_POINT('',(67.,257.1,25.7213203435596)) ;
#98396 = CARTESIAN_POINT('Origin',(67.,256.9,25.7213203435596)) ;
#98397 = CARTESIAN_POINT('',(67.,257.1,29.5213203435596)) ;
#98398 = CARTESIAN_POINT('Origin',(67.,257.1,29.5213203435596)) ;
#98399 = CARTESIAN_POINT('',(64.8,257.1,25.7213203435596)) ;
#98400 = CARTESIAN_POINT('',(66.45,257.1,25.7213203435596)) ;
#98401 = CARTESIAN_POINT('',(64.8,257.1,29.5213203435596)) ;
#98402 = CARTESIAN_POINT('Origin',(64.8,256.9,29.5213203435596)) ;
#98403 = CARTESIAN_POINT('',(64.6,256.9,25.7213203435596)) ;
#98404 = CARTESIAN_POINT('Origin',(64.8,256.9,25.7213203435596)) ;
#98405 = CARTESIAN_POINT('',(64.6,256.9,29.5213203435596)) ;
#98406 = CARTESIAN_POINT('Origin',(64.6,256.9,29.5213203435596)) ;
#98407 = CARTESIAN_POINT('',(64.6,251.1,25.7213203435596)) ;
#98408 = CARTESIAN_POINT('',(64.6,254.7,25.7213203435596)) ;
#98409 = CARTESIAN_POINT('',(64.6,251.1,29.5213203435596)) ;
#98410 = CARTESIAN_POINT('Origin',(64.6,251.1,29.5213203435596)) ;
#98411 = CARTESIAN_POINT('',(64.5,251.1,25.7213203435596)) ;
#98412 = CARTESIAN_POINT('',(65.2500000000003,251.1,25.7213203435596)) ;
#98413 = CARTESIAN_POINT('',(64.5,251.1,29.5213203435596)) ;
#98414 = CARTESIAN_POINT('Origin',(64.5,250.9,29.5213203435596)) ;
#98415 = CARTESIAN_POINT('',(64.3,250.9,25.7213203435596)) ;
#98416 = CARTESIAN_POINT('Origin',(64.5,250.9,25.7213203435596)) ;
#98417 = CARTESIAN_POINT('',(64.3,250.9,29.5213203435596)) ;
#98418 = CARTESIAN_POINT('Origin',(64.3,250.9,29.5213203435596)) ;
#98419 = CARTESIAN_POINT('',(64.3,248.1,25.7213203435596)) ;
#98420 = CARTESIAN_POINT('',(64.3,251.7,25.7213203435596)) ;
#98421 = CARTESIAN_POINT('',(64.3,248.1,29.5213203435596)) ;
#98422 = CARTESIAN_POINT('Origin',(64.5,248.1,29.5213203435596)) ;
#98423 = CARTESIAN_POINT('',(64.5,247.9,25.7213203435596)) ;
#98424 = CARTESIAN_POINT('Origin',(64.5,248.1,25.7213203435596)) ;
#98425 = CARTESIAN_POINT('',(64.5,247.9,29.5213203435596)) ;
#98426 = CARTESIAN_POINT('Origin',(64.5,247.9,29.5213203435596)) ;
#98427 = CARTESIAN_POINT('',(65.2,247.9,25.7213203435596)) ;
#98428 = CARTESIAN_POINT('Origin',(65.9,252.5,25.7213203435596)) ;
#98429 = CARTESIAN_POINT('Origin',(57.9573593128808,242.926794919243,29.5213203435596)) ;
#98430 = CARTESIAN_POINT('',(57.9573593128808,238.073205080757,25.7213203435596)) ;
#98431 = CARTESIAN_POINT('',(57.9573593128808,241.713397459622,25.7213203435596)) ;
#98432 = CARTESIAN_POINT('',(57.9573593128808,238.073205080757,29.5213203435596)) ;
#98433 = CARTESIAN_POINT('Ctrl Pts',(57.9573593128807,238.073205080757,29.5213203435596)) ;
#98434 = CARTESIAN_POINT('Ctrl Pts',(57.9573593128807,238.073205080757,18.1213203435596)) ;
#98435 = CARTESIAN_POINT('Ctrl Pts',(57.9573593128807,238.047717338569,29.5213203435596)) ;
#98436 = CARTESIAN_POINT('Ctrl Pts',(57.9573593128807,238.047717338569,18.1213203435596)) ;
#98437 = CARTESIAN_POINT('Ctrl Pts',(57.9663165128705,238.018473047315,29.5213203435596)) ;
#98438 = CARTESIAN_POINT('Ctrl Pts',(57.9663165128705,238.018473047315,18.1213203435596)) ;
#98439 = CARTESIAN_POINT('Ctrl Pts',(57.9969680412619,237.96152232722,29.5213203435596)) ;
#98440 = CARTESIAN_POINT('Ctrl Pts',(57.9969680412619,237.96152232722,18.1213203435596)) ;
#98441 = CARTESIAN_POINT('Ctrl Pts',(58.0296494906727,237.927709822208,29.5213203435596)) ;
#98442 = CARTESIAN_POINT('Ctrl Pts',(58.0296494906727,237.927709822208,18.1213203435596)) ;
#98443 = CARTESIAN_POINT('Ctrl Pts',(58.0573593128808,237.9,29.5213203435596)) ;
#98444 = CARTESIAN_POINT('Ctrl Pts',(58.0573593128808,237.9,18.1213203435596)) ;
#98445 = CARTESIAN_POINT('',(58.0573593128808,237.9,25.7213203435596)) ;
#98446 = CARTESIAN_POINT('Ctrl Pts',(58.0573593128808,237.9,25.7213203435596)) ;
#98447 = CARTESIAN_POINT('Ctrl Pts',(58.0296494906727,237.927709822208,25.7213203435596)) ;
#98448 = CARTESIAN_POINT('Ctrl Pts',(57.9969680412619,237.96152232722,25.7213203435596)) ;
#98449 = CARTESIAN_POINT('Ctrl Pts',(57.9663165128705,238.018473047315,25.7213203435596)) ;
#98450 = CARTESIAN_POINT('Ctrl Pts',(57.9573593128807,238.047717338569,25.7213203435596)) ;
#98451 = CARTESIAN_POINT('Ctrl Pts',(57.9573593128807,238.073205080757,25.7213203435596)) ;
#98452 = CARTESIAN_POINT('',(58.0573593128808,237.9,29.5213203435596)) ;
#98453 = CARTESIAN_POINT('Origin',(58.0573593128808,237.9,29.5213203435596)) ;
#98454 = CARTESIAN_POINT('',(62.1159379566435,237.9,25.7213203435596)) ;
#98455 = CARTESIAN_POINT('',(59.2820446619101,237.9,25.7213203435596)) ;
#98456 = CARTESIAN_POINT('',(62.1159379566435,237.9,29.5213203435596)) ;
#98457 = CARTESIAN_POINT('Origin',(62.1159379566435,238.1,29.5213203435596)) ;
#98458 = CARTESIAN_POINT('',(62.2573593128808,237.958578643763,25.7213203435596)) ;
#98459 = CARTESIAN_POINT('Origin',(62.1159379566435,238.1,25.7213203435596)) ;
#98460 = CARTESIAN_POINT('',(62.2573593128808,237.958578643763,29.5213203435596)) ;
#98461 = CARTESIAN_POINT('Origin',(62.2573593128808,237.958578643763,29.5213203435596)) ;
#98462 = CARTESIAN_POINT('',(62.9987806691181,238.7,25.7213203435596)) ;
#98463 = CARTESIAN_POINT('',(62.4550573264548,238.156276657337,25.7213203435596)) ;
#98464 = CARTESIAN_POINT('',(62.9987806691181,238.7,29.5213203435596)) ;
#98465 = CARTESIAN_POINT('Origin',(62.8573593128808,238.841421356237,29.5213203435596)) ;
#98466 = CARTESIAN_POINT('Origin',(62.8573593128808,238.841421356237,25.7213203435596)) ;
#98467 = CARTESIAN_POINT('Origin',(60.5067300109395,240.5,25.7213203435596)) ;
#98468 = CARTESIAN_POINT('Ctrl Pts',(60.0305643936376,236.,29.5213203435596)) ;
#98469 = CARTESIAN_POINT('Ctrl Pts',(60.0305643936376,236.,18.1213203435596)) ;
#98470 = CARTESIAN_POINT('Ctrl Pts',(60.0050766514501,236.,29.5213203435596)) ;
#98471 = CARTESIAN_POINT('Ctrl Pts',(60.0050766514501,236.,18.1213203435596)) ;
#98472 = CARTESIAN_POINT('Ctrl Pts',(59.9758323601959,235.99104280001,29.5213203435596)) ;
#98473 = CARTESIAN_POINT('Ctrl Pts',(59.9758323601959,235.99104280001,18.1213203435596)) ;
#98474 = CARTESIAN_POINT('Ctrl Pts',(59.9188816401012,235.960391271619,29.5213203435596)) ;
#98475 = CARTESIAN_POINT('Ctrl Pts',(59.9188816401012,235.960391271619,18.1213203435596)) ;
#98476 = CARTESIAN_POINT('Ctrl Pts',(59.8850691350889,235.927709822208,29.5213203435596)) ;
#98477 = CARTESIAN_POINT('Ctrl Pts',(59.8850691350889,235.927709822208,18.1213203435596)) ;
#98478 = CARTESIAN_POINT('Ctrl Pts',(59.8573593128808,235.9,29.5213203435596)) ;
#98479 = CARTESIAN_POINT('Ctrl Pts',(59.8573593128808,235.9,18.1213203435596)) ;
#98480 = CARTESIAN_POINT('',(59.8573593128808,235.9,25.7213203435596)) ;
#98481 = CARTESIAN_POINT('Ctrl Pts',(59.8573593128808,235.9,25.7213203435596)) ;
#98482 = CARTESIAN_POINT('Ctrl Pts',(59.8850691350889,235.927709822208,25.7213203435596)) ;
#98483 = CARTESIAN_POINT('Ctrl Pts',(59.9188816401012,235.960391271619,25.7213203435596)) ;
#98484 = CARTESIAN_POINT('Ctrl Pts',(59.9758323601959,235.99104280001,25.7213203435596)) ;
#98485 = CARTESIAN_POINT('Ctrl Pts',(60.0050766514501,236.,25.7213203435596)) ;
#98486 = CARTESIAN_POINT('Ctrl Pts',(60.0305643936376,236.,25.7213203435596)) ;
#98487 = CARTESIAN_POINT('',(59.8573593128808,235.9,29.5213203435596)) ;
#98488 = CARTESIAN_POINT('Origin',(59.8573593128808,235.9,29.5213203435596)) ;
#98489 = CARTESIAN_POINT('',(59.8573593128808,230.1,25.7213203435596)) ;
#98490 = CARTESIAN_POINT('',(59.8573593128808,233.675314650971,25.7213203435596)) ;
#98491 = CARTESIAN_POINT('',(59.8573593128808,230.1,29.5213203435596)) ;
#98492 = CARTESIAN_POINT('Origin',(59.8573593128808,230.1,29.5213203435596)) ;
#98493 = CARTESIAN_POINT('',(59.7573593128808,230.1,25.7213203435596)) ;
#98494 = CARTESIAN_POINT('',(60.5073593128808,230.1,25.7213203435596)) ;
#98495 = CARTESIAN_POINT('',(59.7573593128808,230.1,29.5213203435596)) ;
#98496 = CARTESIAN_POINT('Origin',(59.7573593128808,229.9,29.5213203435596)) ;
#98497 = CARTESIAN_POINT('',(59.5573593128808,229.9,25.7213203435596)) ;
#98498 = CARTESIAN_POINT('Origin',(59.7573593128808,229.9,25.7213203435596)) ;
#98499 = CARTESIAN_POINT('',(59.5573593128808,229.9,29.5213203435596)) ;
#98500 = CARTESIAN_POINT('Origin',(59.5573593128808,229.9,29.5213203435596)) ;
#98501 = CARTESIAN_POINT('',(59.5573593128807,227.1,25.7213203435596)) ;
#98502 = CARTESIAN_POINT('',(59.5573593128808,230.675314650971,25.7213203435596)) ;
#98503 = CARTESIAN_POINT('',(59.5573593128807,227.1,29.5213203435596)) ;
#98504 = CARTESIAN_POINT('Origin',(59.7573593128808,227.1,29.5213203435596)) ;
#98505 = CARTESIAN_POINT('',(59.7573593128808,226.9,25.7213203435596)) ;
#98506 = CARTESIAN_POINT('Origin',(59.7573593128808,227.1,25.7213203435596)) ;
#98507 = CARTESIAN_POINT('',(59.7573593128808,226.9,29.5213203435596)) ;
#98508 = CARTESIAN_POINT('Origin',(59.7573593128808,226.9,29.5213203435596)) ;
#98509 = CARTESIAN_POINT('',(60.4573593128807,226.9,25.7213203435596)) ;
#98510 = CARTESIAN_POINT('Origin',(61.1573593128807,231.450629301941,25.7213203435596)) ;
#98511 = CARTESIAN_POINT('Origin',(80.0999999999999,248.6,29.5213203435596)) ;
#98512 = CARTESIAN_POINT('',(80.2999999999999,248.6,25.7213203435596)) ;
#98513 = CARTESIAN_POINT('Origin',(80.0999999999999,248.6,25.7213203435596)) ;
#98514 = CARTESIAN_POINT('',(80.2999999999999,248.6,29.5213203435596)) ;
#98515 = CARTESIAN_POINT('Origin',(80.2999999999999,248.6,29.5213203435596)) ;
#98516 = CARTESIAN_POINT('',(80.2999999999999,249.600000000004,25.7213203435596)) ;
#98517 = CARTESIAN_POINT('',(80.2999999999999,249.8,25.7213203435596)) ;
#98518 = CARTESIAN_POINT('',(80.2999999999999,249.600000000004,29.5213203435596)) ;
#98519 = CARTESIAN_POINT('Origin',(80.2999999999999,249.600000000004,29.5213203435596)) ;
#98520 = CARTESIAN_POINT('',(80.2,249.600000000004,25.7213203435596)) ;
#98521 = CARTESIAN_POINT('',(79.,249.600000000004,25.7213203435596)) ;
#98522 = CARTESIAN_POINT('',(80.2,249.600000000004,29.5213203435596)) ;
#98523 = CARTESIAN_POINT('Origin',(80.2,249.600000000004,29.5213203435596)) ;
#98524 = CARTESIAN_POINT('',(80.2,252.400000000001,25.7213203435596)) ;
#98525 = CARTESIAN_POINT('',(80.2,250.300000000002,25.7213203435596)) ;
#98526 = CARTESIAN_POINT('',(80.2,252.400000000001,29.5213203435596)) ;
#98527 = CARTESIAN_POINT('Origin',(80.2,252.400000000001,29.5213203435596)) ;
#98528 = CARTESIAN_POINT('',(80.3,252.400000000001,25.7213203435596)) ;
#98529 = CARTESIAN_POINT('',(78.95,252.400000000001,25.7213203435596)) ;
#98530 = CARTESIAN_POINT('',(80.3,252.400000000001,29.5213203435596)) ;
#98531 = CARTESIAN_POINT('Origin',(80.3,252.400000000001,29.5213203435596)) ;
#98532 = CARTESIAN_POINT('',(80.3,253.4,25.7213203435596)) ;
#98533 = CARTESIAN_POINT('',(80.3,251.700000000001,25.7213203435596)) ;
#98534 = CARTESIAN_POINT('',(80.3,253.4,29.5213203435596)) ;
#98535 = CARTESIAN_POINT('Origin',(80.1,253.4,29.5213203435596)) ;
#98536 = CARTESIAN_POINT('',(80.1,253.6,25.7213203435596)) ;
#98537 = CARTESIAN_POINT('Origin',(80.1,253.4,25.7213203435596)) ;
#98538 = CARTESIAN_POINT('',(80.1,253.6,29.5213203435596)) ;
#98539 = CARTESIAN_POINT('Origin',(77.7,251.,25.7213203435596)) ;
#98540 = CARTESIAN_POINT('',(76.7766604535517,253.6,25.7213203435596)) ;
#98541 = CARTESIAN_POINT('Origin',(73.2,255.5,25.7213203435596)) ;
#98542 = CARTESIAN_POINT('',(78.9,253.6,25.7213203435596)) ;
#98543 = CARTESIAN_POINT('Origin',(56.8,256.9,29.5213203435596)) ;
#98544 = CARTESIAN_POINT('',(56.6,256.9,25.7213203435596)) ;
#98545 = CARTESIAN_POINT('Origin',(56.8,256.9,25.7213203435596)) ;
#98546 = CARTESIAN_POINT('',(56.6,256.9,29.5213203435596)) ;
#98547 = CARTESIAN_POINT('Origin',(56.6,256.9,29.5213203435596)) ;
#98548 = CARTESIAN_POINT('',(56.6,251.1,25.7213203435596)) ;
#98549 = CARTESIAN_POINT('',(56.6,254.7,25.7213203435596)) ;
#98550 = CARTESIAN_POINT('',(56.6,251.1,29.5213203435596)) ;
#98551 = CARTESIAN_POINT('Origin',(56.6,251.1,29.5213203435596)) ;
#98552 = CARTESIAN_POINT('',(56.5,251.1,25.7213203435596)) ;
#98553 = CARTESIAN_POINT('',(57.2500000000003,251.1,25.7213203435596)) ;
#98554 = CARTESIAN_POINT('',(56.5,251.1,29.5213203435596)) ;
#98555 = CARTESIAN_POINT('Origin',(56.5,250.9,29.5213203435596)) ;
#98556 = CARTESIAN_POINT('',(56.3,250.9,25.7213203435596)) ;
#98557 = CARTESIAN_POINT('Origin',(56.5,250.9,25.7213203435596)) ;
#98558 = CARTESIAN_POINT('',(56.3,250.9,29.5213203435596)) ;
#98559 = CARTESIAN_POINT('Origin',(56.3,250.9,29.5213203435596)) ;
#98560 = CARTESIAN_POINT('',(56.3,248.1,25.7213203435596)) ;
#98561 = CARTESIAN_POINT('',(56.3,251.7,25.7213203435596)) ;
#98562 = CARTESIAN_POINT('',(56.3,248.1,29.5213203435596)) ;
#98563 = CARTESIAN_POINT('Origin',(56.5,248.1,29.5213203435596)) ;
#98564 = CARTESIAN_POINT('',(56.5,247.9,25.7213203435596)) ;
#98565 = CARTESIAN_POINT('Origin',(56.5,248.1,25.7213203435596)) ;
#98566 = CARTESIAN_POINT('',(56.5,247.9,29.5213203435596)) ;
#98567 = CARTESIAN_POINT('Origin',(56.5,247.9,29.5213203435596)) ;
#98568 = CARTESIAN_POINT('',(57.2,247.9,25.7213203435596)) ;
#98569 = CARTESIAN_POINT('Origin',(57.9,252.5,25.7213203435596)) ;
#98570 = CARTESIAN_POINT('Origin',(76.0414213562372,230.4,29.5213203435596)) ;
#98571 = CARTESIAN_POINT('',(75.9707106781186,230.470710678119,25.7213203435596)) ;
#98572 = CARTESIAN_POINT('Origin',(76.0414213562372,230.4,25.7213203435596)) ;
#98573 = CARTESIAN_POINT('',(75.9707106781186,230.470710678119,29.5213203435596)) ;
#98574 = CARTESIAN_POINT('Origin',(75.9707106781186,230.470710678119,29.5213203435596)) ;
#98575 = CARTESIAN_POINT('',(75.2292893218813,229.729289321881,25.7213203435596)) ;
#98576 = CARTESIAN_POINT('',(75.7853553390592,230.285355339059,25.7213203435596)) ;
#98577 = CARTESIAN_POINT('',(75.2292893218813,229.729289321881,29.5213203435596)) ;
#98578 = CARTESIAN_POINT('Origin',(75.3,229.658578643763,29.5213203435596)) ;
#98579 = CARTESIAN_POINT('',(75.2,229.658578643763,25.7213203435596)) ;
#98580 = CARTESIAN_POINT('Origin',(75.3,229.658578643763,25.7213203435596)) ;
#98581 = CARTESIAN_POINT('',(75.2,229.658578643763,29.5213203435596)) ;
#98582 = CARTESIAN_POINT('Origin',(75.2,229.658578643763,29.5213203435596)) ;
#98583 = CARTESIAN_POINT('',(75.1999999999999,226.341421356237,25.7213203435596)) ;
#98584 = CARTESIAN_POINT('',(75.2,228.829289321881,25.7213203435596)) ;
#98585 = CARTESIAN_POINT('',(75.1999999999999,226.341421356237,29.5213203435596)) ;
#98586 = CARTESIAN_POINT('Origin',(75.2999999999999,226.341421356237,29.5213203435596)) ;
#98587 = CARTESIAN_POINT('',(75.2292893218813,226.270710678119,25.7213203435596)) ;
#98588 = CARTESIAN_POINT('Origin',(75.2999999999999,226.341421356237,25.7213203435596)) ;
#98589 = CARTESIAN_POINT('',(75.2292893218813,226.270710678119,29.5213203435596)) ;
#98590 = CARTESIAN_POINT('Origin',(75.2292893218813,226.270710678119,29.5213203435596)) ;
#98591 = CARTESIAN_POINT('',(75.4146446609407,226.085355339059,25.7213203435596)) ;
#98592 = CARTESIAN_POINT('Origin',(77.7,228.,25.7213203435596)) ;
#98593 = CARTESIAN_POINT('Origin',(30.7,254.8,25.7213203435596)) ;
#98594 = CARTESIAN_POINT('Origin',(71.6,225.9,29.5213203435596)) ;
#98595 = CARTESIAN_POINT('',(71.4,225.9,25.7213203435596)) ;
#98596 = CARTESIAN_POINT('Origin',(71.6,225.9,25.7213203435596)) ;
#98597 = CARTESIAN_POINT('',(71.4,225.9,29.5213203435596)) ;
#98598 = CARTESIAN_POINT('Origin',(71.4,225.9,29.5213203435596)) ;
#98599 = CARTESIAN_POINT('',(71.4,223.1,25.7213203435596)) ;
#98600 = CARTESIAN_POINT('',(71.4,226.7,25.7213203435596)) ;
#98601 = CARTESIAN_POINT('',(71.4,223.1,29.5213203435596)) ;
#98602 = CARTESIAN_POINT('Origin',(61.5,261.2,25.7213203435596)) ;
#98603 = CARTESIAN_POINT('Origin',(56.2649110640674,263.05,29.5213203435596)) ;
#98604 = CARTESIAN_POINT('',(55.6649110640674,262.6,29.5213203435596)) ;
#98605 = CARTESIAN_POINT('',(57.2649110640674,263.8,29.5213203435596)) ;
#98606 = CARTESIAN_POINT('Origin',(55.2649110640674,263.8,29.5213203435596)) ;
#98607 = CARTESIAN_POINT('',(67.6350889359328,263.8,29.5213203435596)) ;
#98608 = CARTESIAN_POINT('',(55.2395462392986,263.8,22.5213203435596)) ;
#98609 = CARTESIAN_POINT('Origin',(68.3850889359328,262.8,29.5213203435596)) ;
#98610 = CARTESIAN_POINT('',(68.9350889359328,262.066666666667,29.5213203435596)) ;
#98611 = CARTESIAN_POINT('Origin',(77.2,257.723534352175,29.5213203435596)) ;
#98612 = CARTESIAN_POINT('',(77.2,257.723534352175,29.5213203435596)) ;
#98613 = CARTESIAN_POINT('',(77.2,261.8,29.5213203435596)) ;
#98614 = CARTESIAN_POINT('Origin',(82.9283628290597,247.251297405594,30.7213203435596)) ;
#98615 = CARTESIAN_POINT('Origin',(81.1,247.600000000001,30.7213203435596)) ;
#98616 = CARTESIAN_POINT('',(81.1,247.600000000001,30.7213203435596)) ;
#98617 = CARTESIAN_POINT('Origin',(84.1283628290597,244.301866670644,30.7213203435596)) ;
#98618 = CARTESIAN_POINT('',(82.349868392482,246.421393804845,30.7213203435596)) ;
#98619 = CARTESIAN_POINT('Origin',(81.9668461709225,246.100000000001,30.7213203435596)) ;
#98620 = CARTESIAN_POINT('',(81.9668461709225,246.600000000001,30.7213203435596)) ;
#98621 = CARTESIAN_POINT('Origin',(81.9668461709225,246.600000000001,30.7213203435596)) ;
#98622 = CARTESIAN_POINT('',(80.6401337790902,246.600000000001,30.7213203435596)) ;
#98623 = CARTESIAN_POINT('Origin',(80.6,247.098386676966,30.7213203435596)) ;
#98624 = CARTESIAN_POINT('',(81.1,247.098386676966,30.7213203435596)) ;
#98625 = CARTESIAN_POINT('Origin',(81.1,247.098386676966,30.7213203435596)) ;
#98626 = CARTESIAN_POINT('Origin',(73.,227.5,25.7213203435596)) ;
#98627 = CARTESIAN_POINT('',(71.4146847058821,223.024778714675,25.7213203435596)) ;
#98628 = CARTESIAN_POINT('Origin',(74.9999999999998,220.305309236676,25.7213203435596)) ;
#98629 = CARTESIAN_POINT('Origin',(71.6,223.1,25.7213203435596)) ;
#98630 = CARTESIAN_POINT('Origin',(71.6,223.1,29.5213203435596)) ;
#98631 = CARTESIAN_POINT('',(71.4146847058821,223.024778714675,30.7213203435596)) ;
#98632 = CARTESIAN_POINT('Origin',(80.,230.5,30.7213203435596)) ;
#98633 = CARTESIAN_POINT('Origin',(74.9999999999998,220.305309236676,30.7213203435596)) ;
#98634 = CARTESIAN_POINT('',(75.,224.805309236676,30.7213203435596)) ;
#98635 = CARTESIAN_POINT('Origin',(75.,224.805309236676,30.7213203435596)) ;
#98636 = CARTESIAN_POINT('',(80.,224.805309236676,30.7213203435596)) ;
#98637 = CARTESIAN_POINT('Origin',(80.,224.805309236676,30.7213203435596)) ;
#98638 = CARTESIAN_POINT('Origin',(72.1450953968557,220.262610236549,30.7213203435596)) ;
#98639 = CARTESIAN_POINT('',(70.4999999999999,220.262610236549,30.7213203435596)) ;
#98640 = CARTESIAN_POINT('Origin',(70.4999999999998,218.133222662034,30.7213203435596)) ;
#98641 = CARTESIAN_POINT('Origin',(69.1350889359328,263.8,29.5213203435596)) ;
#98642 = CARTESIAN_POINT('',(69.1350889359328,261.466666666667,29.5213203435596)) ;
#98643 = CARTESIAN_POINT('Origin',(68.1350889359328,261.466666666667,29.5213203435596)) ;
#98644 = CARTESIAN_POINT('Origin',(78.2,263.05,29.5213203435596)) ;
#98645 = CARTESIAN_POINT('',(77.6,262.6,29.5213203435596)) ;
#98646 = CARTESIAN_POINT('Origin',(78.2,261.8,29.5213203435596)) ;
#98647 = CARTESIAN_POINT('Origin',(55.2395462392986,262.8,21.2713203435596)) ;
#98648 = CARTESIAN_POINT('Origin',(55.2649110640674,257.,29.5213203435596)) ;
#98649 = CARTESIAN_POINT('',(55.2649110640674,261.8,29.5213203435596)) ;
#98650 = CARTESIAN_POINT('Origin',(56.2649110640674,261.8,29.5213203435596)) ;
#98651 = CARTESIAN_POINT('Origin',(40.2,265.,25.0213203435596)) ;
#98652 = CARTESIAN_POINT('',(42.2,265.,25.0213203435596)) ;
#98653 = CARTESIAN_POINT('Origin',(80.1,253.6,29.5213203435596)) ;
#98654 = CARTESIAN_POINT('',(76.7766604535517,253.6,30.7213203435596)) ;
#98655 = CARTESIAN_POINT('Origin',(73.2,257.,29.5213203435596)) ;
#98656 = CARTESIAN_POINT('',(77.25,256.652146641849,29.5213203435596)) ;
#98657 = CARTESIAN_POINT('Origin',(69.15,255.5,30.7213203435596)) ;
#98658 = CARTESIAN_POINT('',(69.15,255.5,30.7213203435596)) ;
#98659 = CARTESIAN_POINT('Origin',(73.2,255.5,30.7213203435596)) ;
#98660 = CARTESIAN_POINT('',(77.25,255.5,30.7213203435596)) ;
#98661 = CARTESIAN_POINT('Origin',(77.25,256.652146641849,30.7213203435596)) ;
#98662 = CARTESIAN_POINT('Origin',(55.25,256.652146641849,30.7213203435596)) ;
#98663 = CARTESIAN_POINT('',(55.25,255.5,30.7213203435596)) ;
#98664 = CARTESIAN_POINT('Origin',(51.2,255.5,30.7213203435596)) ;
#98665 = CARTESIAN_POINT('Origin',(44.5,256.,25.7213203435596)) ;
#98666 = CARTESIAN_POINT('',(45.7,253.,25.7213203435596)) ;
#98667 = CARTESIAN_POINT('',(45.7,259.,25.7213203435596)) ;
#98668 = CARTESIAN_POINT('Origin',(45.7,253.,20.0213203435596)) ;
#98669 = CARTESIAN_POINT('Origin',(37.1,259.,20.0213203435596)) ;
#98670 = CARTESIAN_POINT('Origin',(55.2141814145299,249.05,20.0213203435596)) ;
#98671 = CARTESIAN_POINT('Origin',(43.3,253.,20.0213203435596)) ;
#98672 = CARTESIAN_POINT('',(0.,0.,0.)) ;
#98673 = CARTESIAN_POINT('Origin',(53.3423242584234,235.5,27.7213203435596)) ;
#98674 = CARTESIAN_POINT('',(53.3423242584234,235.5,27.7213203435596)) ;
#98675 = CARTESIAN_POINT('',(55.3573593128808,235.5,27.7213203435596)) ;
#98676 = CARTESIAN_POINT('',(53.3423242584234,235.5,27.7213203435596)) ;
#98677 = CARTESIAN_POINT('',(55.3573593128808,235.5,23.7213203435596)) ;
#98678 = CARTESIAN_POINT('',(55.3573593128808,235.5,28.0213203435596)) ;
#98679 = CARTESIAN_POINT('',(53.3423242584234,235.5,23.7213203435596)) ;
#98680 = CARTESIAN_POINT('',(53.3423242584234,235.5,23.7213203435596)) ;
#98681 = CARTESIAN_POINT('',(53.3423242584234,235.5,27.7213203435596)) ;
#98682 = CARTESIAN_POINT('Origin',(53.3423242584234,234.234064310023,27.7213203435596)) ;
#98683 = CARTESIAN_POINT('',(53.3423242584234,234.234064310023,27.7213203435596)) ;
#98684 = CARTESIAN_POINT('',(53.3423242584234,234.234064310023,27.7213203435596)) ;
#98685 = CARTESIAN_POINT('',(53.3423242584234,234.234064310023,23.7213203435596)) ;
#98686 = CARTESIAN_POINT('',(53.3423242584234,234.234064310023,23.7213203435596)) ;
#98687 = CARTESIAN_POINT('',(53.3423242584234,234.234064310023,27.7213203435596)) ;
#98688 = CARTESIAN_POINT('Origin',(52.3423242584234,234.234064310023,27.7213203435596)) ;
#98689 = CARTESIAN_POINT('',(52.3423242584234,234.234064310023,27.7213203435596)) ;
#98690 = CARTESIAN_POINT('',(52.3423242584234,234.234064310023,27.7213203435596)) ;
#98691 = CARTESIAN_POINT('',(52.3423242584234,234.234064310023,23.7213203435596)) ;
#98692 = CARTESIAN_POINT('',(52.3423242584234,234.234064310023,23.7213203435596)) ;
#98693 = CARTESIAN_POINT('',(52.3423242584234,234.234064310023,27.7213203435596)) ;
#98694 = CARTESIAN_POINT('Origin',(52.3423242584234,233.234064310023,27.7213203435596)) ;
#98695 = CARTESIAN_POINT('',(52.3423242584234,233.234064310023,27.7213203435596)) ;
#98696 = CARTESIAN_POINT('',(52.3423242584234,233.234064310023,27.7213203435596)) ;
#98697 = CARTESIAN_POINT('',(52.3423242584234,233.234064310023,23.7213203435596)) ;
#98698 = CARTESIAN_POINT('',(52.3423242584234,233.234064310023,23.7213203435596)) ;
#98699 = CARTESIAN_POINT('',(52.3423242584234,233.234064310023,27.7213203435596)) ;
#98700 = CARTESIAN_POINT('Origin',(51.3423242584235,233.234064310023,27.7213203435596)) ;
#98701 = CARTESIAN_POINT('',(51.3423242584235,233.234064310023,27.7213203435596)) ;
#98702 = CARTESIAN_POINT('',(51.3423242584235,233.234064310023,27.7213203435596)) ;
#98703 = CARTESIAN_POINT('',(51.3423242584235,233.234064310023,23.7213203435596)) ;
#98704 = CARTESIAN_POINT('',(51.3423242584235,233.234064310023,23.7213203435596)) ;
#98705 = CARTESIAN_POINT('',(51.3423242584235,233.234064310023,27.7213203435596)) ;
#98706 = CARTESIAN_POINT('Origin',(51.3423242584235,232.234064310023,27.7213203435596)) ;
#98707 = CARTESIAN_POINT('',(51.3423242584235,232.234064310023,27.7213203435596)) ;
#98708 = CARTESIAN_POINT('',(51.3423242584235,232.234064310023,27.7213203435596)) ;
#98709 = CARTESIAN_POINT('',(51.3423242584235,232.234064310023,23.7213203435596)) ;
#98710 = CARTESIAN_POINT('',(51.3423242584235,232.234064310023,23.7213203435596)) ;
#98711 = CARTESIAN_POINT('',(51.3423242584235,232.234064310023,27.7213203435596)) ;
#98712 = CARTESIAN_POINT('Origin',(55.3573593128808,226.5,27.7213203435596)) ;
#98713 = CARTESIAN_POINT('',(55.3573593128808,226.5,27.7213203435596)) ;
#98714 = CARTESIAN_POINT('',(55.3573593128808,226.5,27.7213203435596)) ;
#98715 = CARTESIAN_POINT('',(55.3573593128808,226.5,23.7213203435596)) ;
#98716 = CARTESIAN_POINT('',(55.3573593128808,226.5,23.7213203435596)) ;
#98717 = CARTESIAN_POINT('',(55.3573593128808,226.5,28.3213203435596)) ;
#98718 = CARTESIAN_POINT('Origin',(53.3498417856521,231.,23.7213203435596)) ;
#98719 = CARTESIAN_POINT('',(55.3573593128808,228.75,23.7213203435596)) ;
#98720 = CARTESIAN_POINT('Origin',(53.3498417856521,231.,27.7213203435596)) ;
#98721 = CARTESIAN_POINT('',(55.3573593128808,228.75,27.7213203435596)) ;
#98722 = CARTESIAN_POINT('Origin',(55.3573593128808,236.5,28.3213203435596)) ;
#98723 = CARTESIAN_POINT('',(55.3573593128808,236.5,28.3213203435596)) ;
#98724 = CARTESIAN_POINT('',(55.9573593128808,236.5,28.3213203435596)) ;
#98725 = CARTESIAN_POINT('',(55.3573593128808,236.5,28.3213203435596)) ;
#98726 = CARTESIAN_POINT('',(55.9573593128808,236.5,20.3213203435596)) ;
#98727 = CARTESIAN_POINT('',(55.9573593128808,236.5,28.3213203435596)) ;
#98728 = CARTESIAN_POINT('',(55.3573593128808,236.5,20.3213203435596)) ;
#98729 = CARTESIAN_POINT('',(55.3573593128808,236.5,20.3213203435596)) ;
#98730 = CARTESIAN_POINT('',(55.3573593128808,236.5,28.3213203435596)) ;
#98731 = CARTESIAN_POINT('Origin',(55.3573593128808,226.5,28.3213203435596)) ;
#98732 = CARTESIAN_POINT('',(55.3573593128808,226.5,28.3213203435596)) ;
#98733 = CARTESIAN_POINT('',(55.3573593128808,226.5,28.3213203435596)) ;
#98734 = CARTESIAN_POINT('',(55.3573593128808,226.5,28.3213203435596)) ;
#98735 = CARTESIAN_POINT('',(55.3573593128808,226.5,20.3213203435596)) ;
#98736 = CARTESIAN_POINT('',(55.3573593128808,226.5,20.3213203435596)) ;
#98737 = CARTESIAN_POINT('',(55.3573593128808,226.5,28.3213203435596)) ;
#98738 = CARTESIAN_POINT('Origin',(55.9573593128808,226.5,28.3213203435596)) ;
#98739 = CARTESIAN_POINT('',(55.9573593128808,226.5,28.3213203435596)) ;
#98740 = CARTESIAN_POINT('',(55.9573593128808,226.5,28.3213203435596)) ;
#98741 = CARTESIAN_POINT('',(55.9573593128808,226.5,20.3213203435596)) ;
#98742 = CARTESIAN_POINT('',(55.9573593128808,226.5,20.3213203435596)) ;
#98743 = CARTESIAN_POINT('',(55.9573593128808,226.5,28.3213203435596)) ;
#98744 = CARTESIAN_POINT('Origin',(55.9573593128808,236.5,28.3213203435596)) ;
#98745 = CARTESIAN_POINT('',(55.9573593128808,236.5,28.3213203435596)) ;
#98746 = CARTESIAN_POINT('',(55.9573593128808,236.5,20.3213203435596)) ;
#98747 = CARTESIAN_POINT('Origin',(55.6573593128808,231.5,20.3213203435596)) ;
#98748 = CARTESIAN_POINT('Origin',(55.6573593128808,231.5,28.3213203435596)) ;
#98749 = CARTESIAN_POINT('',(0.,0.,0.)) ;
#98750 = CARTESIAN_POINT('Origin',(40.2,265.924309379709,25.0213203435596)) ;
#98751 = CARTESIAN_POINT('',(39.4319120248131,264.737243197272,23.5297151931015)) ;
#98752 = CARTESIAN_POINT('',(39.4319120325861,264.835792165808,23.5297151890988)) ;
#98753 = CARTESIAN_POINT('',(39.4319120248721,265.924309379709,23.5297151930711)) ;
#98754 = CARTESIAN_POINT('',(41.1572720979745,265.,26.3991720020989)) ;
#98755 = CARTESIAN_POINT('Ctrl Pts',(39.4319120248131,264.737243197272,23.5297151931015)) ;
#98756 = CARTESIAN_POINT('Ctrl Pts',(39.4304044404626,264.737322527506,23.5304915094147)) ;
#98757 = CARTESIAN_POINT('Ctrl Pts',(39.4288980211696,264.737401933216,23.5312701174534)) ;
#98758 = CARTESIAN_POINT('Ctrl Pts',(39.4017655580238,264.738834604452,23.545345971115)) ;
#98759 = CARTESIAN_POINT('Ctrl Pts',(39.3764867953982,264.740209382512,23.5592996683641)) ;
#98760 = CARTESIAN_POINT('Ctrl Pts',(39.3158646983467,264.743609119489,23.5948338131558)) ;
#98761 = CARTESIAN_POINT('Ctrl Pts',(39.2809371147819,264.745656348017,23.6170831411784)) ;
#98762 = CARTESIAN_POINT('Ctrl Pts',(39.2049495917101,264.750310835025,23.6695383876079)) ;
#98763 = CARTESIAN_POINT('Ctrl Pts',(39.1643713622691,264.752936389273,23.7003689485121)) ;
#98764 = CARTESIAN_POINT('Ctrl Pts',(39.0570776606221,264.760235887148,23.7898749823946)) ;
#98765 = CARTESIAN_POINT('Ctrl Pts',(38.9935196330723,264.764976767591,23.8520753394917)) ;
#98766 = CARTESIAN_POINT('Ctrl Pts',(38.9062589178821,264.771892128461,23.9522005420064)) ;
#98767 = CARTESIAN_POINT('Ctrl Pts',(38.8786504561284,264.774150951797,23.9865165132885)) ;
#98768 = CARTESIAN_POINT('Ctrl Pts',(38.8405383737826,264.777332483655,24.0379042863935)) ;
#98769 = CARTESIAN_POINT('Ctrl Pts',(38.8289405250687,264.778310004615,24.0541393705838)) ;
#98770 = CARTESIAN_POINT('Ctrl Pts',(38.8082442588673,264.780066197532,24.0842314407711)) ;
#98771 = CARTESIAN_POINT('Ctrl Pts',(38.7990569823385,264.780849756839,24.0980228174524)) ;
#98772 = CARTESIAN_POINT('Ctrl Pts',(38.7755205297153,264.782871876341,24.1345146328457)) ;
#98773 = CARTESIAN_POINT('Ctrl Pts',(38.7615090530597,264.784091369515,24.1574279566855)) ;
#98774 = CARTESIAN_POINT('Ctrl Pts',(38.730302404386,264.786867654561,24.2113270965558)) ;
#98775 = CARTESIAN_POINT('Ctrl Pts',(38.7135265532737,264.788407229425,24.2425411933755)) ;
#98776 = CARTESIAN_POINT('Ctrl Pts',(38.6474731304393,264.794766372148,24.3753674532139)) ;
#98777 = CARTESIAN_POINT('Ctrl Pts',(38.6075300929458,264.799398931744,24.4812875596889)) ;
#98778 = CARTESIAN_POINT('Ctrl Pts',(38.5650438565067,264.806558905916,24.6411622330249)) ;
#98779 = CARTESIAN_POINT('Ctrl Pts',(38.5539491631154,264.808878661246,24.6925074891467)) ;
#98780 = CARTESIAN_POINT('Ctrl Pts',(38.5402808673343,264.812647790166,24.7741479734373)) ;
#98781 = CARTESIAN_POINT('Ctrl Pts',(38.536090856418,264.814048948341,24.804138367956)) ;
#98782 = CARTESIAN_POINT('Ctrl Pts',(38.5294393775916,264.816857677078,24.8634124000482)) ;
#98783 = CARTESIAN_POINT('Ctrl Pts',(38.5269311980604,264.818263301234,24.8926798806991)) ;
#98784 = CARTESIAN_POINT('Ctrl Pts',(38.522465377297,264.821931900017,24.9679834005038)) ;
#98785 = CARTESIAN_POINT('Ctrl Pts',(38.5216335168716,264.824226849211,25.0140596063819)) ;
#98786 = CARTESIAN_POINT('Ctrl Pts',(38.5253565800552,264.832412630974,25.1750513356149)) ;
#98787 = CARTESIAN_POINT('Ctrl Pts',(38.5398229695952,264.838550190996,25.2894098581918)) ;
#98788 = CARTESIAN_POINT('Ctrl Pts',(38.5789038623145,264.847610943719,25.4574467850682)) ;
#98789 = CARTESIAN_POINT('Ctrl Pts',(38.5948222900754,264.850597622558,25.5128122743674)) ;
#98790 = CARTESIAN_POINT('Ctrl Pts',(38.6202728864776,264.85449866004,25.5867700258602)) ;
#98791 = CARTESIAN_POINT('Ctrl Pts',(38.6273491209682,264.855512885922,25.6061625263056)) ;
#98792 = CARTESIAN_POINT('Ctrl Pts',(38.6407241304923,264.857303372889,25.6408170745013)) ;
#98793 = CARTESIAN_POINT('Ctrl Pts',(38.6468928931367,264.858085781612,25.6561240611006)) ;
#98794 = CARTESIAN_POINT('Ctrl Pts',(38.6632446090061,264.86005640523,25.6950328008638)) ;
#98795 = CARTESIAN_POINT('Ctrl Pts',(38.6737456634063,264.861228016883,25.7184956608131)) ;
#98796 = CARTESIAN_POINT('Ctrl Pts',(38.6990171899898,264.863862871164,25.7716501225304)) ;
#98797 = CARTESIAN_POINT('Ctrl Pts',(38.7141371771553,264.865311673756,25.8011639226423)) ;
#98798 = CARTESIAN_POINT('Ctrl Pts',(38.7755726633357,264.870803061255,25.9128015316757)) ;
#98799 = CARTESIAN_POINT('Ctrl Pts',(38.8279036513412,264.874703119596,25.9914154149038)) ;
#98800 = CARTESIAN_POINT('Ctrl Pts',(38.9278985951457,264.881563118496,26.1172295012224)) ;
#98801 = CARTESIAN_POINT('Ctrl Pts',(38.9722858731208,264.884452275983,26.1667355574291)) ;
#98802 = CARTESIAN_POINT('Ctrl Pts',(39.0426653094159,264.88892443338,26.2364274694627)) ;
#98803 = CARTESIAN_POINT('Ctrl Pts',(39.0665050907615,264.890422153507,26.258695810473)) ;
#98804 = CARTESIAN_POINT('Ctrl Pts',(39.1125792981033,264.89329468395,26.2992835698611)) ;
#98805 = CARTESIAN_POINT('Ctrl Pts',(39.1346660304974,264.894662773603,26.3177528355227)) ;
#98806 = CARTESIAN_POINT('Ctrl Pts',(39.1884456830622,264.897977455058,26.3604215819749)) ;
#98807 = CARTESIAN_POINT('Ctrl Pts',(39.2205465973335,264.899943189666,26.38407673626)) ;
#98808 = CARTESIAN_POINT('Ctrl Pts',(39.2930597605727,264.904356110779,26.4336252000818)) ;
#98809 = CARTESIAN_POINT('Ctrl Pts',(39.3338015852083,264.906818185425,26.4589731084199)) ;
#98810 = CARTESIAN_POINT('Ctrl Pts',(39.4559885188033,264.914121405243,26.5279116968206)) ;
#98811 = CARTESIAN_POINT('Ctrl Pts',(39.5400108830261,264.919051974656,26.566566029181)) ;
#98812 = CARTESIAN_POINT('Ctrl Pts',(39.6713920558248,264.926343153125,26.6143273997752)) ;
#98813 = CARTESIAN_POINT('Ctrl Pts',(39.7166702627846,264.928782814097,26.62864443888)) ;
#98814 = CARTESIAN_POINT('Ctrl Pts',(39.7817310051742,264.932132170627,26.6462182009804)) ;
#98815 = CARTESIAN_POINT('Ctrl Pts',(39.8010567606912,264.933107837232,26.6510707398458)) ;
#98816 = CARTESIAN_POINT('Ctrl Pts',(39.8369522698017,264.93487889742,26.6594070004195)) ;
#98817 = CARTESIAN_POINT('Ctrl Pts',(39.8534961786273,264.935678613719,26.6629861608072)) ;
#98818 = CARTESIAN_POINT('Ctrl Pts',(39.8976837332061,264.937775992996,26.6718481000392)) ;
#98819 = CARTESIAN_POINT('Ctrl Pts',(39.9254118456879,264.939052573819,26.6766869163251)) ;
#98820 = CARTESIAN_POINT('Ctrl Pts',(39.9907384050409,264.941993744339,26.6864002567276)) ;
#98821 = CARTESIAN_POINT('Ctrl Pts',(40.028406633528,264.943638655548,26.690702703065)) ;
#98822 = CARTESIAN_POINT('Ctrl Pts',(40.2052785704075,264.951244315129,26.7048543697477)) ;
#98823 = CARTESIAN_POINT('Ctrl Pts',(40.3452067720937,264.95697305041,26.6985890791927)) ;
#98824 = CARTESIAN_POINT('Ctrl Pts',(40.5176897119491,264.964809821159,26.6690991456072)) ;
#98825 = CARTESIAN_POINT('Ctrl Pts',(40.5524325630894,264.966425446333,26.6620192273418)) ;
#98826 = CARTESIAN_POINT('Ctrl Pts',(40.6147723482532,264.969404799588,26.6472441009216)) ;
#98827 = CARTESIAN_POINT('Ctrl Pts',(40.6424463134638,264.970756548302,26.6399324993173)) ;
#98828 = CARTESIAN_POINT('Ctrl Pts',(40.704465240716,264.973856933408,26.6218374269499)) ;
#98829 = CARTESIAN_POINT('Ctrl Pts',(40.7386766867003,264.975617437676,26.6106495448928)) ;
#98830 = CARTESIAN_POINT('Ctrl Pts',(40.8512779527651,264.981583670503,26.5697730560285)) ;
#98831 = CARTESIAN_POINT('Ctrl Pts',(40.9277947283892,264.985928426018,26.5353154878895)) ;
#98832 = CARTESIAN_POINT('Ctrl Pts',(41.0550811114644,264.993557678104,26.4661086949452)) ;
#98833 = CARTESIAN_POINT('Ctrl Pts',(41.1071118799309,264.996802126154,26.4340211651883)) ;
#98834 = CARTESIAN_POINT('Ctrl Pts',(41.1572720979745,265.,26.3991720020989)) ;
#98835 = CARTESIAN_POINT('',(39.225659978706,265.,26.3871558334356)) ;
#98836 = CARTESIAN_POINT('Origin',(40.2,265.,25.0213203435596)) ;
#98837 = CARTESIAN_POINT('Ctrl Pts',(39.225659978706,265.,26.3871558334356)) ;
#98838 = CARTESIAN_POINT('Ctrl Pts',(39.2153375643007,264.999398586693,26.3797921783351)) ;
#98839 = CARTESIAN_POINT('Ctrl Pts',(39.2050987251971,264.998803540393,26.3723115745025)) ;
#98840 = CARTESIAN_POINT('Ctrl Pts',(39.1821482809501,264.997471097196,26.3551413105944)) ;
#98841 = CARTESIAN_POINT('Ctrl Pts',(39.1694882714317,264.996737051312,26.3453845773693)) ;
#98842 = CARTESIAN_POINT('Ctrl Pts',(39.0582891688161,264.990282099836,26.2571252243299)) ;
#98843 = CARTESIAN_POINT('Ctrl Pts',(38.9687388195114,264.985009519897,26.1679316979276)) ;
#98844 = CARTESIAN_POINT('Ctrl Pts',(38.8614953736439,264.977536268327,26.0339081445413)) ;
#98845 = CARTESIAN_POINT('Ctrl Pts',(38.8344434094844,264.975526916063,25.997119319476)) ;
#98846 = CARTESIAN_POINT('Ctrl Pts',(38.7871725793157,264.971727220694,25.9270122319354)) ;
#98847 = CARTESIAN_POINT('Ctrl Pts',(38.7665491542183,264.969949584461,25.8940044557118)) ;
#98848 = CARTESIAN_POINT('Ctrl Pts',(38.7317053771711,264.96670064448,25.8336643349143)) ;
#98849 = CARTESIAN_POINT('Ctrl Pts',(38.7170547799005,264.965243750705,25.806600675999)) ;
#98850 = CARTESIAN_POINT('Ctrl Pts',(38.6857195260224,264.961905303656,25.7447082336931)) ;
#98851 = CARTESIAN_POINT('Ctrl Pts',(38.669476806028,264.960010976513,25.709676263679)) ;
#98852 = CARTESIAN_POINT('Ctrl Pts',(38.6084925735989,264.952175279112,25.5652917050987)) ;
#98853 = CARTESIAN_POINT('Ctrl Pts',(38.5741549049405,264.945929659729,25.4519274112468)) ;
#98854 = CARTESIAN_POINT('Ctrl Pts',(38.5362429748598,264.935175265875,25.2533264290485)) ;
#98855 = CARTESIAN_POINT('Ctrl Pts',(38.5267069951294,264.930709147059,25.1696659586808)) ;
#98856 = CARTESIAN_POINT('Ctrl Pts',(38.5225723652007,264.925266877297,25.0618943820493)) ;
#98857 = CARTESIAN_POINT('Ctrl Pts',(38.5221659172324,264.924086606359,25.0381315005049)) ;
#98858 = CARTESIAN_POINT('Ctrl Pts',(38.5223322482953,264.922134803343,24.9979984297071)) ;
#98859 = CARTESIAN_POINT('Ctrl Pts',(38.5226396085222,264.921350945212,24.9816320007903)) ;
#98860 = CARTESIAN_POINT('Ctrl Pts',(38.5239062545065,264.919564286199,24.9437381579236)) ;
#98861 = CARTESIAN_POINT('Ctrl Pts',(38.5250407417903,264.91856991652,24.9222204106408)) ;
#98862 = CARTESIAN_POINT('Ctrl Pts',(38.5348843182911,264.912353275722,24.7856232519015)) ;
#98863 = CARTESIAN_POINT('Ctrl Pts',(38.5550341356524,264.907581508538,24.6716697907738)) ;
#98864 = CARTESIAN_POINT('Ctrl Pts',(38.608101188325,264.899364401452,24.4858161861708)) ;
#98865 = CARTESIAN_POINT('Ctrl Pts',(38.6346609459615,264.896006783232,24.4125354873651)) ;
#98866 = CARTESIAN_POINT('Ctrl Pts',(38.6793366403557,264.891034860123,24.3117592553561)) ;
#98867 = CARTESIAN_POINT('Ctrl Pts',(38.6933164274786,264.889549493163,24.2825386113984)) ;
#98868 = CARTESIAN_POINT('Ctrl Pts',(38.7208594501208,264.886735836765,24.22900592723)) ;
#98869 = CARTESIAN_POINT('Ctrl Pts',(38.7341990250379,264.885415421392,24.204591322851)) ;
#98870 = CARTESIAN_POINT('Ctrl Pts',(38.7666878401857,264.882288877449,24.1484908820612)) ;
#98871 = CARTESIAN_POINT('Ctrl Pts',(38.7862905747062,264.88046722329,24.1170856303193)) ;
#98872 = CARTESIAN_POINT('Ctrl Pts',(38.8609217532805,264.873750076278,24.005886153229)) ;
#98873 = CARTESIAN_POINT('Ctrl Pts',(38.9217937713385,264.868650688891,23.9302555633882)) ;
#98874 = CARTESIAN_POINT('Ctrl Pts',(39.0363356794035,264.859830231537,23.8107666806675)) ;
#98875 = CARTESIAN_POINT('Ctrl Pts',(39.0868222911744,264.856153642658,23.7641844678424)) ;
#98876 = CARTESIAN_POINT('Ctrl Pts',(39.1622368816876,264.851078579735,23.702717217297)) ;
#98877 = CARTESIAN_POINT('Ctrl Pts',(39.1849142564075,264.849601641214,23.6851812929999)) ;
#98878 = CARTESIAN_POINT('Ctrl Pts',(39.2265980280825,264.84698943238,23.6546222421566)) ;
#98879 = CARTESIAN_POINT('Ctrl Pts',(39.2454445236879,264.845844401979,23.6413931574044)) ;
#98880 = CARTESIAN_POINT('Ctrl Pts',(39.2776898373826,264.843953426749,23.6197357915535)) ;
#98881 = CARTESIAN_POINT('Ctrl Pts',(39.2909448615541,264.843195393758,23.6111026026035)) ;
#98882 = CARTESIAN_POINT('Ctrl Pts',(39.3216635266847,264.841481540571,23.5917082536414)) ;
#98883 = CARTESIAN_POINT('Ctrl Pts',(39.3392055457963,264.84053325582,23.5810777732057)) ;
#98884 = CARTESIAN_POINT('Ctrl Pts',(39.3815807666403,264.838304021937,23.5564492333377)) ;
#98885 = CARTESIAN_POINT('Ctrl Pts',(39.4065800980265,264.837037998039,23.5427596292232)) ;
#98886 = CARTESIAN_POINT('Ctrl Pts',(39.4319120325861,264.835792165808,23.5297151890988)) ;
#98887 = CARTESIAN_POINT('Origin',(40.2,265.924309379709,25.0213203435596)) ;
#98888 = CARTESIAN_POINT('',(39.431912024867,264.240044136826,23.5297151930737)) ;
#98889 = CARTESIAN_POINT('',(39.4319120259791,264.338362624254,23.529715192501)) ;
#98890 = CARTESIAN_POINT('',(39.4319120248721,265.924309379709,23.5297151930711)) ;
#98891 = CARTESIAN_POINT('Ctrl Pts',(39.431912024867,264.240044136826,23.5297151930737)) ;
#98892 = CARTESIAN_POINT('Ctrl Pts',(39.4132822099684,264.241024674624,23.5393084401859)) ;
#98893 = CARTESIAN_POINT('Ctrl Pts',(39.3948328986984,264.241985998715,23.5492503106463)) ;
#98894 = CARTESIAN_POINT('Ctrl Pts',(39.2729335404419,264.24830290277,23.6179164536233)) ;
#98895 = CARTESIAN_POINT('Ctrl Pts',(39.1757869152903,264.253187306839,23.687158681559)) ;
#98896 = CARTESIAN_POINT('Ctrl Pts',(39.0460663182673,264.260530210574,23.8022047100275)) ;
#98897 = CARTESIAN_POINT('Ctrl Pts',(39.007138576516,264.26285881752,23.8402669489468)) ;
#98898 = CARTESIAN_POINT('Ctrl Pts',(38.9407781639254,264.267146306372,23.9117854632675)) ;
#98899 = CARTESIAN_POINT('Ctrl Pts',(38.912659037804,264.269080067746,23.9445380049841)) ;
#98900 = CARTESIAN_POINT('Ctrl Pts',(38.8677636804408,264.272397320149,24.0011064082021)) ;
#98901 = CARTESIAN_POINT('Ctrl Pts',(38.8502881123139,264.273753733266,24.0243410122428)) ;
#98902 = CARTESIAN_POINT('Ctrl Pts',(38.8153418670443,264.276611452506,24.0734075775326)) ;
#98903 = CARTESIAN_POINT('Ctrl Pts',(38.7979701382822,264.278115593169,24.099296009554)) ;
#98904 = CARTESIAN_POINT('Ctrl Pts',(38.7500244828146,264.282521456516,24.1752382698391)) ;
#98905 = CARTESIAN_POINT('Ctrl Pts',(38.7213423528314,264.285485033205,24.2264275700949)) ;
#98906 = CARTESIAN_POINT('Ctrl Pts',(38.6420784451439,264.294733748247,24.3870887329753)) ;
#98907 = CARTESIAN_POINT('Ctrl Pts',(38.6005604560298,264.301221827089,24.5005900581633)) ;
#98908 = CARTESIAN_POINT('Ctrl Pts',(38.5650399790021,264.308842703721,24.6438489225981)) ;
#98909 = CARTESIAN_POINT('Ctrl Pts',(38.5591580175469,264.310225385382,24.6702980604476)) ;
#98910 = CARTESIAN_POINT('Ctrl Pts',(38.5496071397796,264.312701315645,24.7187552541532)) ;
#98911 = CARTESIAN_POINT('Ctrl Pts',(38.5457316795646,264.31380222938,24.7407162895493)) ;
#98912 = CARTESIAN_POINT('Ctrl Pts',(38.5397820767606,264.315670306164,24.7788592795642)) ;
#98913 = CARTESIAN_POINT('Ctrl Pts',(38.5375042501585,264.316446941494,24.7950045600758)) ;
#98914 = CARTESIAN_POINT('Ctrl Pts',(38.5325424462824,264.318304447274,24.8343078218836)) ;
#98915 = CARTESIAN_POINT('Ctrl Pts',(38.530105103436,264.31937333216,24.8574926834839)) ;
#98916 = CARTESIAN_POINT('Ctrl Pts',(38.5204609114229,264.324559288927,24.9721711131197)) ;
#98917 = CARTESIAN_POINT('Ctrl Pts',(38.5202859549722,264.328406459296,25.0641045598926)) ;
#98918 = CARTESIAN_POINT('Ctrl Pts',(38.535639344848,264.336486444213,25.2553265917216)) ;
#98919 = CARTESIAN_POINT('Ctrl Pts',(38.552551418043,264.340713029794,25.3541369107347)) ;
#98920 = CARTESIAN_POINT('Ctrl Pts',(38.5870709941029,264.346753498454,25.4844786072675)) ;
#98921 = CARTESIAN_POINT('Ctrl Pts',(38.5970218535698,264.34833978593,25.5178245528935)) ;
#98922 = CARTESIAN_POINT('Ctrl Pts',(38.6169652688593,264.351278999889,25.5777848005739)) ;
#98923 = CARTESIAN_POINT('Ctrl Pts',(38.6266112524308,264.352620737927,25.6045007513464)) ;
#98924 = CARTESIAN_POINT('Ctrl Pts',(38.6500147219436,264.355712330818,25.6645056491577)) ;
#98925 = CARTESIAN_POINT('Ctrl Pts',(38.6641750930185,264.357474497521,25.6976215509824)) ;
#98926 = CARTESIAN_POINT('Ctrl Pts',(38.7254323492215,264.364697130764,25.8290137118034)) ;
#98927 = CARTESIAN_POINT('Ctrl Pts',(38.7809825392229,264.370421352668,25.9230426007967)) ;
#98928 = CARTESIAN_POINT('Ctrl Pts',(38.8940442842774,264.380544138254,26.0778087351502)) ;
#98929 = CARTESIAN_POINT('Ctrl Pts',(38.947717807763,264.384909042365,26.1409090739036)) ;
#98930 = CARTESIAN_POINT('Ctrl Pts',(39.0211926660056,264.390145964443,26.2153625111654)) ;
#98931 = CARTESIAN_POINT('Ctrl Pts',(39.0368591779498,264.391224519625,26.2306287977629)) ;
#98932 = CARTESIAN_POINT('Ctrl Pts',(39.0647325093007,264.393071082758,26.2567471035433)) ;
#98933 = CARTESIAN_POINT('Ctrl Pts',(39.0768061899353,264.393847731681,26.2677340974336)) ;
#98934 = CARTESIAN_POINT('Ctrl Pts',(39.1068853402126,264.395727852864,26.2943138828354)) ;
#98935 = CARTESIAN_POINT('Ctrl Pts',(39.1250655496236,264.396818345749,26.3097023653233)) ;
#98936 = CARTESIAN_POINT('Ctrl Pts',(39.1964886378161,264.400954621437,26.3675931609585)) ;
#98937 = CARTESIAN_POINT('Ctrl Pts',(39.2519762097907,264.403861845856,26.4072271333079)) ;
#98938 = CARTESIAN_POINT('Ctrl Pts',(39.3795119909923,264.410221069298,26.4870706366956)) ;
#98939 = CARTESIAN_POINT('Ctrl Pts',(39.4524225757243,264.413654975052,26.5255650883706)) ;
#98940 = CARTESIAN_POINT('Ctrl Pts',(39.5640618021591,264.41891785501,26.5743781619071)) ;
#98941 = CARTESIAN_POINT('Ctrl Pts',(39.6008076241019,264.420649696972,26.5889217806131)) ;
#98942 = CARTESIAN_POINT('Ctrl Pts',(39.6710580311562,264.423987279655,26.6138950077881)) ;
#98943 = CARTESIAN_POINT('Ctrl Pts',(39.7044430811037,264.425584314431,26.6245972430872)) ;
#98944 = CARTESIAN_POINT('Ctrl Pts',(39.7654369931549,264.428533855109,26.6420628957595)) ;
#98945 = CARTESIAN_POINT('Ctrl Pts',(39.7929293845093,264.429874692,26.6491854573395)) ;
#98946 = CARTESIAN_POINT('Ctrl Pts',(39.8553889502476,264.432950917972,26.663685905923)) ;
#98947 = CARTESIAN_POINT('Ctrl Pts',(39.8904369731581,264.434698100471,26.6706510933627)) ;
#98948 = CARTESIAN_POINT('Ctrl Pts',(40.0361795808214,264.442052870894,26.6948058301963)) ;
#98949 = CARTESIAN_POINT('Ctrl Pts',(40.1482254517613,264.447943435313,26.7020062253947)) ;
#98950 = CARTESIAN_POINT('Ctrl Pts',(40.3389737752404,264.4580232707,26.6951645407568)) ;
#98951 = CARTESIAN_POINT('Ctrl Pts',(40.4175163670847,264.46218041606,26.686780079503)) ;
#98952 = CARTESIAN_POINT('Ctrl Pts',(40.5173846668642,264.467270170071,26.6689309757283)) ;
#98953 = CARTESIAN_POINT('Ctrl Pts',(40.5395072172764,264.468384663882,26.6645150242635)) ;
#98954 = CARTESIAN_POINT('Ctrl Pts',(40.5774537599682,264.470266194265,26.6561412732288)) ;
#98955 = CARTESIAN_POINT('Ctrl Pts',(40.5933198664014,264.471043199999,26.6523967767594)) ;
#98956 = CARTESIAN_POINT('Ctrl Pts',(40.6314711798773,264.472888883523,26.6428037197553)) ;
#98957 = CARTESIAN_POINT('Ctrl Pts',(40.6536946027953,264.473946118853,26.6367264888121)) ;
#98958 = CARTESIAN_POINT('Ctrl Pts',(40.766709351244,264.479261796876,26.6033050080665)) ;
#98959 = CARTESIAN_POINT('Ctrl Pts',(40.8551963966758,264.483228683936,26.5687554680522)) ;
#98960 = CARTESIAN_POINT('Ctrl Pts',(41.0298470370369,264.491427195233,26.4828802114617)) ;
#98961 = CARTESIAN_POINT('Ctrl Pts',(41.1152876456138,264.495651183807,26.4309480136934)) ;
#98962 = CARTESIAN_POINT('Ctrl Pts',(41.2230008839063,264.501660112862,26.3515357254904)) ;
#98963 = CARTESIAN_POINT('Ctrl Pts',(41.2497771271807,264.50321532966,26.330507716289)) ;
#98964 = CARTESIAN_POINT('Ctrl Pts',(41.2977182226069,264.506126255737,26.2904415791122)) ;
#98965 = CARTESIAN_POINT('Ctrl Pts',(41.3190739450083,264.507472200388,26.2716512592455)) ;
#98966 = CARTESIAN_POINT('Ctrl Pts',(41.366592257236,264.510585991811,26.2276482170967)) ;
#98967 = CARTESIAN_POINT('Ctrl Pts',(41.3924336290613,264.512366659027,26.2021108568985)) ;
#98968 = CARTESIAN_POINT('Ctrl Pts',(41.4806720200064,264.518766764598,26.1090579451391)) ;
#98969 = CARTESIAN_POINT('Ctrl Pts',(41.5383253186715,264.523559098989,26.0372811396274)) ;
#98970 = CARTESIAN_POINT('Ctrl Pts',(41.6272172466736,264.531931248712,25.9058293430199)) ;
#98971 = CARTESIAN_POINT('Ctrl Pts',(41.6612921986356,264.535473596637,25.8483213590859)) ;
#98972 = CARTESIAN_POINT('Ctrl Pts',(41.710035790308,264.540988151677,25.7535887779138)) ;
#98973 = CARTESIAN_POINT('Ctrl Pts',(41.7269617821315,264.543013082286,25.7176056491031)) ;
#98974 = CARTESIAN_POINT('Ctrl Pts',(41.7499024725837,264.545897277305,25.6639654953731)) ;
#98975 = CARTESIAN_POINT('Ctrl Pts',(41.7569264164679,264.546802836909,25.6467567131915)) ;
#98976 = CARTESIAN_POINT('Ctrl Pts',(41.7699110786407,264.548517063275,25.613368819403)) ;
#98977 = CARTESIAN_POINT('Ctrl Pts',(41.7759110196701,264.549327494081,25.5972080622188)) ;
#98978 = CARTESIAN_POINT('Ctrl Pts',(41.7920540946538,264.551568457438,25.551584084156)) ;
#98979 = CARTESIAN_POINT('Ctrl Pts',(41.8016274932276,264.552971018738,25.5219254149515)) ;
#98980 = CARTESIAN_POINT('Ctrl Pts',(41.8228040228152,264.55630328929,25.4494751076159)) ;
#98981 = CARTESIAN_POINT('Ctrl Pts',(41.8335482285678,264.558204348483,25.4064565310586)) ;
#98982 = CARTESIAN_POINT('Ctrl Pts',(41.8695547832027,264.565706673534,25.2333912928301)) ;
#98983 = CARTESIAN_POINT('Ctrl Pts',(41.8810828186049,264.571165169789,25.1009902504229)) ;
#98984 = CARTESIAN_POINT('Ctrl Pts',(41.8758237428878,264.578660469262,24.9336764807616)) ;
#98985 = CARTESIAN_POINT('Ctrl Pts',(41.873634363284,264.580253280481,24.8987867066433)) ;
#98986 = CARTESIAN_POINT('Ctrl Pts',(41.8676951768917,264.583198191272,24.8357302838891)) ;
#98987 = CARTESIAN_POINT('Ctrl Pts',(41.8643165202015,264.584538787246,24.8075417638774)) ;
#98988 = CARTESIAN_POINT('Ctrl Pts',(41.8550632610952,264.58761867794,24.7440254752234)) ;
#98989 = CARTESIAN_POINT('Ctrl Pts',(41.8487695766841,264.589369925801,24.7087735509979)) ;
#98990 = CARTESIAN_POINT('Ctrl Pts',(41.8240241960479,264.595318019672,24.5919164116561)) ;
#98991 = CARTESIAN_POINT('Ctrl Pts',(41.8006007087929,264.599653780808,24.5114993901129)) ;
#98992 = CARTESIAN_POINT('Ctrl Pts',(41.7329485687108,264.609811759641,24.3307620720685)) ;
#98993 = CARTESIAN_POINT('Ctrl Pts',(41.6846948181059,264.615663167122,24.2323431382963)) ;
#98994 = CARTESIAN_POINT('Ctrl Pts',(41.6160022054311,264.622198068891,24.1211886820815)) ;
#98995 = CARTESIAN_POINT('Ctrl Pts',(41.6044536027076,264.623248136182,24.1032738269612)) ;
#98996 = CARTESIAN_POINT('Ctrl Pts',(41.5834555221782,264.62506743693,24.0720244323337)) ;
#98997 = CARTESIAN_POINT('Ctrl Pts',(41.5741477893204,264.625844237799,24.0586003501734)) ;
#98998 = CARTESIAN_POINT('Ctrl Pts',(41.5506661607752,264.62773407751,24.0257685578035)) ;
#98999 = CARTESIAN_POINT('Ctrl Pts',(41.5362690012208,264.628833716756,24.0065259354761)) ;
#99000 = CARTESIAN_POINT('Ctrl Pts',(41.5028997471058,264.631268735791,23.9638682052474)) ;
#99001 = CARTESIAN_POINT('Ctrl Pts',(41.4837000904252,264.632592705322,23.940641396621)) ;
#99002 = CARTESIAN_POINT('Ctrl Pts',(41.4142081997694,264.637169513495,23.8610405469919)) ;
#99003 = CARTESIAN_POINT('Ctrl Pts',(41.3607441122175,264.640320386567,23.8075557090152)) ;
#99004 = CARTESIAN_POINT('Ctrl Pts',(41.2428899909118,264.646926019045,23.7045897054797)) ;
#99005 = CARTESIAN_POINT('Ctrl Pts',(41.1781510925646,264.650379714059,23.6558100322662)) ;
#99006 = CARTESIAN_POINT('Ctrl Pts',(41.0797837925954,264.655605844451,23.5922885177305)) ;
#99007 = CARTESIAN_POINT('Ctrl Pts',(41.0487957146746,264.657248258095,23.5736680687358)) ;
#99008 = CARTESIAN_POINT('Ctrl Pts',(40.9924157507406,264.660243250267,23.5422227349849)) ;
#99009 = CARTESIAN_POINT('Ctrl Pts',(40.9672532232408,264.66158215339,23.5290151346424)) ;
#99010 = CARTESIAN_POINT('Ctrl Pts',(40.9106414927648,264.664604027441,23.5011104865597)) ;
#99011 = CARTESIAN_POINT('Ctrl Pts',(40.8790476778546,264.666296895613,23.4867378648453)) ;
#99012 = CARTESIAN_POINT('Ctrl Pts',(40.8111312142302,264.669951340191,23.4583495278672)) ;
#99013 = CARTESIAN_POINT('Ctrl Pts',(40.7747207640723,264.671919560343,23.4445975041175)) ;
#99014 = CARTESIAN_POINT('Ctrl Pts',(40.6626260181984,264.677995338667,23.4066588082306)) ;
#99015 = CARTESIAN_POINT('Ctrl Pts',(40.5856752245792,264.682193475733,23.3865701767195)) ;
#99016 = CARTESIAN_POINT('Ctrl Pts',(40.436182653323,264.69022147364,23.3586898815297)) ;
#99017 = CARTESIAN_POINT('Ctrl Pts',(40.3639757429192,264.694042185173,23.3500228266856)) ;
#99018 = CARTESIAN_POINT('Ctrl Pts',(40.2676673315645,264.698897927437,23.3447665557978)) ;
#99019 = CARTESIAN_POINT('Ctrl Pts',(40.2438773685744,264.700077716064,23.3439753141406)) ;
#99020 = CARTESIAN_POINT('Ctrl Pts',(40.2037374834939,264.70202636514,23.3434949258404)) ;
#99021 = CARTESIAN_POINT('Ctrl Pts',(40.1873956270982,264.702807550702,23.343538092777)) ;
#99022 = CARTESIAN_POINT('Ctrl Pts',(40.1491056524484,264.704609046989,23.3441987754075)) ;
#99023 = CARTESIAN_POINT('Ctrl Pts',(40.1271647404408,264.705620103466,23.3450082926165)) ;
#99024 = CARTESIAN_POINT('Ctrl Pts',(40.0787947145311,264.707813825624,23.3477444692676)) ;
#99025 = CARTESIAN_POINT('Ctrl Pts',(40.0523824381001,264.708988460367,23.3498670588905)) ;
#99026 = CARTESIAN_POINT('Ctrl Pts',(39.9124685060611,264.715135293397,23.3644536531822)) ;
#99027 = CARTESIAN_POINT('Ctrl Pts',(39.8004078164719,264.719813436412,23.3878546495737)) ;
#99028 = CARTESIAN_POINT('Ctrl Pts',(39.6308878195355,264.727426599087,23.441759169475)) ;
#99029 = CARTESIAN_POINT('Ctrl Pts',(39.5713392483099,264.730206995592,23.4645008237095)) ;
#99030 = CARTESIAN_POINT('Ctrl Pts',(39.4857769654096,264.734451992723,23.5028882824064)) ;
#99031 = CARTESIAN_POINT('Ctrl Pts',(39.458661104631,264.735835640365,23.5159410072526)) ;
#99032 = CARTESIAN_POINT('Ctrl Pts',(39.4319120248131,264.737243197272,23.5297151931015)) ;
#99033 = CARTESIAN_POINT('Ctrl Pts',(39.4319120325861,264.835792165808,23.5297151890988)) ;
#99034 = CARTESIAN_POINT('Ctrl Pts',(39.4603130231985,264.834395396468,23.5150903675857)) ;
#99035 = CARTESIAN_POINT('Ctrl Pts',(39.4891320894357,264.833023970378,23.5012765080419)) ;
#99036 = CARTESIAN_POINT('Ctrl Pts',(39.621570495771,264.826858751005,23.4423873974807)) ;
#99037 = CARTESIAN_POINT('Ctrl Pts',(39.7291763356068,264.822200486286,23.4070294341609)) ;
#99038 = CARTESIAN_POINT('Ctrl Pts',(39.8842993407464,264.815252428622,23.3729027993618)) ;
#99039 = CARTESIAN_POINT('Ctrl Pts',(39.9294613400335,264.813206303652,23.3648917271524)) ;
#99040 = CARTESIAN_POINT('Ctrl Pts',(40.0042188785895,264.809750539146,23.3547698362209)) ;
#99041 = CARTESIAN_POINT('Ctrl Pts',(40.0336436247803,264.80837321832,23.3515759696404)) ;
#99042 = CARTESIAN_POINT('Ctrl Pts',(40.0938902713359,264.805512382131,23.346644876479)) ;
#99043 = CARTESIAN_POINT('Ctrl Pts',(40.1247063534128,264.80402738775,23.3449767284515)) ;
#99044 = CARTESIAN_POINT('Ctrl Pts',(40.2108238312162,264.79981339099,23.3426943365568)) ;
#99045 = CARTESIAN_POINT('Ctrl Pts',(40.2661325005939,264.797032125976,23.3439628524623)) ;
#99046 = CARTESIAN_POINT('Ctrl Pts',(40.4429878790381,264.787926671349,23.356780185482)) ;
#99047 = CARTESIAN_POINT('Ctrl Pts',(40.5633658102133,264.781377829567,23.3788528396579)) ;
#99048 = CARTESIAN_POINT('Ctrl Pts',(40.7063805511062,264.773686075272,23.4215810446935)) ;
#99049 = CARTESIAN_POINT('Ctrl Pts',(40.7322879160633,264.772298066013,23.4300137198069)) ;
#99050 = CARTESIAN_POINT('Ctrl Pts',(40.7791251017808,264.769811925624,23.446530855956)) ;
#99051 = CARTESIAN_POINT('Ctrl Pts',(40.800120174473,264.768706209724,23.4544113881442)) ;
#99052 = CARTESIAN_POINT('Ctrl Pts',(40.8362633101766,264.76682556862,23.4688108536214)) ;
#99053 = CARTESIAN_POINT('Ctrl Pts',(40.851483365359,264.766041334621,23.4751359512571)) ;
#99054 = CARTESIAN_POINT('Ctrl Pts',(40.888518374427,264.764151098008,23.4911708431225)) ;
#99055 = CARTESIAN_POINT('Ctrl Pts',(40.9102232976851,264.763057847776,23.5011236426734)) ;
#99056 = CARTESIAN_POINT('Ctrl Pts',(40.9955037482383,264.758793901546,23.5424543974849)) ;
#99057 = CARTESIAN_POINT('Ctrl Pts',(41.0572788774782,264.755773936296,23.5773865053189)) ;
#99058 = CARTESIAN_POINT('Ctrl Pts',(41.1842684508533,264.749369082032,23.6602265354854)) ;
#99059 = CARTESIAN_POINT('Ctrl Pts',(41.2486038687719,264.745997193338,23.709150240806)) ;
#99060 = CARTESIAN_POINT('Ctrl Pts',(41.3386056518523,264.740810417845,23.7884530375364)) ;
#99061 = CARTESIAN_POINT('Ctrl Pts',(41.367125024726,264.739088619342,23.815416701166)) ;
#99062 = CARTESIAN_POINT('Ctrl Pts',(41.4192001521303,264.735765413338,23.8682303681528)) ;
#99063 = CARTESIAN_POINT('Ctrl Pts',(41.4429442138599,264.734172386311,23.8938652471206)) ;
#99064 = CARTESIAN_POINT('Ctrl Pts',(41.4845884313122,264.731220466203,23.941741214141)) ;
#99065 = CARTESIAN_POINT('Ctrl Pts',(41.5027543924094,264.729872808872,23.9637337448904)) ;
#99066 = CARTESIAN_POINT('Ctrl Pts',(41.542686176494,264.726765690045,24.0146677451005)) ;
#99067 = CARTESIAN_POINT('Ctrl Pts',(41.5640928940294,264.72499379652,24.0438716416054)) ;
#99068 = CARTESIAN_POINT('Ctrl Pts',(41.6451194781059,264.717845173489,24.162262436959)) ;
#99069 = CARTESIAN_POINT('Ctrl Pts',(41.6970671897372,264.712216355083,24.2563784368131)) ;
#99070 = CARTESIAN_POINT('Ctrl Pts',(41.7726258393592,264.702176429026,24.4309190604384)) ;
#99071 = CARTESIAN_POINT('Ctrl Pts',(41.7998905682313,264.697798948963,24.5093853963317)) ;
#99072 = CARTESIAN_POINT('Ctrl Pts',(41.8269843148759,264.692522927052,24.6111187923016)) ;
#99073 = CARTESIAN_POINT('Ctrl Pts',(41.8322978041528,264.69142116348,24.6328010561549)) ;
#99074 = CARTESIAN_POINT('Ctrl Pts',(41.840743339365,264.68955193272,24.6705034265262)) ;
#99075 = CARTESIAN_POINT('Ctrl Pts',(41.8440769041963,264.68877497752,24.6864735370434)) ;
#99076 = CARTESIAN_POINT('Ctrl Pts',(41.8516103411319,264.686916620463,24.7253938146691)) ;
#99077 = CARTESIAN_POINT('Ctrl Pts',(41.8555653851039,264.685847238276,24.7483870612886)) ;
#99078 = CARTESIAN_POINT('Ctrl Pts',(41.8726082846781,264.680692367483,24.8615479673583)) ;
#99079 = CARTESIAN_POINT('Ctrl Pts',(41.8788168598765,264.676873277867,24.9526023552605)) ;
#99080 = CARTESIAN_POINT('Ctrl Pts',(41.8762354274784,264.668732611059,25.1459720532812)) ;
#99081 = CARTESIAN_POINT('Ctrl Pts',(41.8655238894694,264.664416106255,25.247885381978)) ;
#99082 = CARTESIAN_POINT('Ctrl Pts',(41.8389445883439,264.658296193339,25.381699872939)) ;
#99083 = CARTESIAN_POINT('Ctrl Pts',(41.8312650486601,264.656736342656,25.4150041386367)) ;
#99084 = CARTESIAN_POINT('Ctrl Pts',(41.8153805605958,264.653828810208,25.4754025433758)) ;
#99085 = CARTESIAN_POINT('Ctrl Pts',(41.8074966132296,264.652491396902,25.5025682277791)) ;
#99086 = CARTESIAN_POINT('Ctrl Pts',(41.7881107364794,264.649416647595,25.5635612135233)) ;
#99087 = CARTESIAN_POINT('Ctrl Pts',(41.7762076459389,264.647667319931,25.5972457749204)) ;
#99088 = CARTESIAN_POINT('Ctrl Pts',(41.7242087669127,264.640527830177,25.7306769532635)) ;
#99089 = CARTESIAN_POINT('Ctrl Pts',(41.6756475536358,264.634881110729,25.826838112927)) ;
#99090 = CARTESIAN_POINT('Ctrl Pts',(41.5731002289919,264.624736771575,25.9890891145264)) ;
#99091 = CARTESIAN_POINT('Ctrl Pts',(41.5226386536462,264.620273227177,26.0569888497496)) ;
#99092 = CARTESIAN_POINT('Ctrl Pts',(41.4530424827636,264.61495654656,26.1372062136278)) ;
#99093 = CARTESIAN_POINT('Ctrl Pts',(41.4384921327174,264.613885614521,26.1533336187894)) ;
#99094 = CARTESIAN_POINT('Ctrl Pts',(41.4124914762296,264.612048485124,26.1810507607281)) ;
#99095 = CARTESIAN_POINT('Ctrl Pts',(41.4011792400443,264.611273842635,26.1927633327704)) ;
#99096 = CARTESIAN_POINT('Ctrl Pts',(41.3729105993807,264.609396025964,26.221192237276)) ;
#99097 = CARTESIAN_POINT('Ctrl Pts',(41.3557660205301,264.608305895794,26.2377153605269)) ;
#99098 = CARTESIAN_POINT('Ctrl Pts',(41.2874091321541,264.604119692389,26.3008438626757)) ;
#99099 = CARTESIAN_POINT('Ctrl Pts',(41.2336807478188,264.601167399177,26.3446284719447)) ;
#99100 = CARTESIAN_POINT('Ctrl Pts',(41.1110338868682,264.594792418617,26.4325357656551)) ;
#99101 = CARTESIAN_POINT('Ctrl Pts',(41.0412867671059,264.591385591186,26.4751938007185)) ;
#99102 = CARTESIAN_POINT('Ctrl Pts',(40.9203326320714,264.585506290501,26.5375421574317)) ;
#99103 = CARTESIAN_POINT('Ctrl Pts',(40.8707700140226,264.583105984336,26.5601103565535)) ;
#99104 = CARTESIAN_POINT('Ctrl Pts',(40.7917355077343,264.579236596979,26.5915536526393)) ;
#99105 = CARTESIAN_POINT('Ctrl Pts',(40.762966958361,264.577820168485,26.602095983878)) ;
#99106 = CARTESIAN_POINT('Ctrl Pts',(40.7060743851184,264.574996367666,26.6211943892502)) ;
#99107 = CARTESIAN_POINT('Ctrl Pts',(40.6779822082692,264.573591504773,26.6298106691421)) ;
#99108 = CARTESIAN_POINT('Ctrl Pts',(40.605942498399,264.569958271771,26.6498524155158)) ;
#99109 = CARTESIAN_POINT('Ctrl Pts',(40.5617326040619,264.567699651743,26.6602392238709)) ;
#99110 = CARTESIAN_POINT('Ctrl Pts',(40.4077286260042,264.55973973429,26.6898863430483)) ;
#99111 = CARTESIAN_POINT('Ctrl Pts',(40.2964784955942,264.553808444423,26.6999959491021)) ;
#99112 = CARTESIAN_POINT('Ctrl Pts',(40.1248447572972,264.544784897535,26.6984676370998)) ;
#99113 = CARTESIAN_POINT('Ctrl Pts',(40.0646970353294,264.541652596257,26.6946898039301)) ;
#99114 = CARTESIAN_POINT('Ctrl Pts',(39.9838245097663,264.537582747174,26.6852201651987)) ;
#99115 = CARTESIAN_POINT('Ctrl Pts',(39.9628171150925,264.536538795369,26.6823558073586)) ;
#99116 = CARTESIAN_POINT('Ctrl Pts',(39.9257030715583,264.534724539274,26.6765767966)) ;
#99117 = CARTESIAN_POINT('Ctrl Pts',(39.9095760907824,264.53394692403,26.6738235070944)) ;
#99118 = CARTESIAN_POINT('Ctrl Pts',(39.8696445966425,264.532046240274,26.6664035075601)) ;
#99119 = CARTESIAN_POINT('Ctrl Pts',(39.8458968326235,264.530936982642,26.6614558124951)) ;
#99120 = CARTESIAN_POINT('Ctrl Pts',(39.7925136757706,264.528475268262,26.6491201725161)) ;
#99121 = CARTESIAN_POINT('Ctrl Pts',(39.7629557074293,264.527134618253,26.6414344785844)) ;
#99122 = CARTESIAN_POINT('Ctrl Pts',(39.6588766295046,264.522445373623,26.6113157674762)) ;
#99123 = CARTESIAN_POINT('Ctrl Pts',(39.585723532054,264.519203595309,26.5845110293359)) ;
#99124 = CARTESIAN_POINT('Ctrl Pts',(39.4432954874348,264.512611116293,26.5207741953414)) ;
#99125 = CARTESIAN_POINT('Ctrl Pts',(39.3742228625323,264.509266863713,26.4838710657085)) ;
#99126 = CARTESIAN_POINT('Ctrl Pts',(39.2775358603165,264.504168994166,26.4231752013845)) ;
#99127 = CARTESIAN_POINT('Ctrl Pts',(39.2477154412045,264.50253484944,26.4030913255179)) ;
#99128 = CARTESIAN_POINT('Ctrl Pts',(39.195531686536,264.499548785321,26.3654538655108)) ;
#99129 = CARTESIAN_POINT('Ctrl Pts',(39.1729256258476,264.49821018945,26.3482602951387)) ;
#99130 = CARTESIAN_POINT('Ctrl Pts',(39.123576760158,264.495181241812,26.3087100639991)) ;
#99131 = CARTESIAN_POINT('Ctrl Pts',(39.0970728033448,264.493480709015,26.2860775029034)) ;
#99132 = CARTESIAN_POINT('Ctrl Pts',(38.9945795044098,264.48660028113,26.1928822537341)) ;
#99133 = CARTESIAN_POINT('Ctrl Pts',(38.9245044953552,264.481180935281,26.1161732244024)) ;
#99134 = CARTESIAN_POINT('Ctrl Pts',(38.8090997805529,264.471080171141,25.9636153183496)) ;
#99135 = CARTESIAN_POINT('Ctrl Pts',(38.7617893960508,264.466435593155,25.889695244031)) ;
#99136 = CARTESIAN_POINT('Ctrl Pts',(38.7093853084934,264.460844498925,25.7916873838573)) ;
#99137 = CARTESIAN_POINT('Ctrl Pts',(38.698738630309,264.45968010146,25.7707280645133)) ;
#99138 = CARTESIAN_POINT('Ctrl Pts',(38.6814588642479,264.457748574458,25.7348633958412)) ;
#99139 = CARTESIAN_POINT('Ctrl Pts',(38.6745968727737,264.456969632151,25.7200736731255)) ;
#99140 = CARTESIAN_POINT('Ctrl Pts',(38.6589425213988,264.455163891134,25.6850035039807)) ;
#99141 = CARTESIAN_POINT('Ctrl Pts',(38.6503334909669,264.454146701536,25.6646455180901)) ;
#99142 = CARTESIAN_POINT('Ctrl Pts',(38.6128535320748,264.449578247998,25.5708935327125)) ;
#99143 = CARTESIAN_POINT('Ctrl Pts',(38.5887756351206,264.446230653195,25.495685692654)) ;
#99144 = CARTESIAN_POINT('Ctrl Pts',(38.5431902214919,264.438119819372,25.3088775489508)) ;
#99145 = CARTESIAN_POINT('Ctrl Pts',(38.527545539298,264.433382372799,25.1962558630923)) ;
#99146 = CARTESIAN_POINT('Ctrl Pts',(38.5220753660632,264.426723565329,25.0473800794649)) ;
#99147 = CARTESIAN_POINT('Ctrl Pts',(38.52190005134,264.425105200611,25.0118045253802)) ;
#99148 = CARTESIAN_POINT('Ctrl Pts',(38.523617589027,264.42213595683,24.9478897960574)) ;
#99149 = CARTESIAN_POINT('Ctrl Pts',(38.5250990081268,264.420797742369,24.9195530196465)) ;
#99150 = CARTESIAN_POINT('Ctrl Pts',(38.5300218334654,264.417754200358,24.8562366540208)) ;
#99151 = CARTESIAN_POINT('Ctrl Pts',(38.5338452361228,264.416038116422,24.8213008734254)) ;
#99152 = CARTESIAN_POINT('Ctrl Pts',(38.5443140332504,264.412319708539,24.7472354394495)) ;
#99153 = CARTESIAN_POINT('Ctrl Pts',(38.5512565474712,264.410310104689,24.7081697300542)) ;
#99154 = CARTESIAN_POINT('Ctrl Pts',(38.5770222585659,264.403993916823,24.5880707347812)) ;
#99155 = CARTESIAN_POINT('Ctrl Pts',(38.600489603566,264.399587895727,24.5081662162692)) ;
#99156 = CARTESIAN_POINT('Ctrl Pts',(38.6533425799269,264.391672101551,24.3677383347004)) ;
#99157 = CARTESIAN_POINT('Ctrl Pts',(38.6806261169513,264.388164971409,24.3066017974438)) ;
#99158 = CARTESIAN_POINT('Ctrl Pts',(38.7224727803526,264.383598086447,24.226131541578)) ;
#99159 = CARTESIAN_POINT('Ctrl Pts',(38.7339063112038,264.382417670293,24.205243563097)) ;
#99160 = CARTESIAN_POINT('Ctrl Pts',(38.7539170821872,264.380469650882,24.170464653071)) ;
#99161 = CARTESIAN_POINT('Ctrl Pts',(38.7622587906277,264.379689647803,24.1564437760821)) ;
#99162 = CARTESIAN_POINT('Ctrl Pts',(38.7822466189683,264.377894252709,24.1239365818474)) ;
#99163 = CARTESIAN_POINT('Ctrl Pts',(38.7940514362987,264.376887962902,24.1055523714472)) ;
#99164 = CARTESIAN_POINT('Ctrl Pts',(38.8530918967326,264.372084294171,24.0174397741805)) ;
#99165 = CARTESIAN_POINT('Ctrl Pts',(38.9051766140087,264.368523315023,23.951099699316)) ;
#99166 = CARTESIAN_POINT('Ctrl Pts',(39.0343108391942,264.360459630191,23.8099228822857)) ;
#99167 = CARTESIAN_POINT('Ctrl Pts',(39.1139941225095,264.355970492159,23.7380024453812)) ;
#99168 = CARTESIAN_POINT('Ctrl Pts',(39.2290182103572,264.349577494941,23.6526176660407)) ;
#99169 = CARTESIAN_POINT('Ctrl Pts',(39.2587413067597,264.347934487787,23.6320095358068)) ;
#99170 = CARTESIAN_POINT('Ctrl Pts',(39.3129535812011,264.344939764203,23.5969607922664)) ;
#99171 = CARTESIAN_POINT('Ctrl Pts',(39.3371879240245,264.343601780697,23.5821515940277)) ;
#99172 = CARTESIAN_POINT('Ctrl Pts',(39.3848560024173,264.340967349072,23.5546593021696)) ;
#99173 = CARTESIAN_POINT('Ctrl Pts',(39.4082380990316,264.339673930004,23.5419058574188)) ;
#99174 = CARTESIAN_POINT('Ctrl Pts',(39.4319120259791,264.338362624254,23.529715192501)) ;
#99175 = CARTESIAN_POINT('Origin',(40.2,265.924309379709,25.0213203435596)) ;
#99176 = CARTESIAN_POINT('',(39.4328938139748,263.738513013137,23.5316344567886)) ;
#99177 = CARTESIAN_POINT('',(39.4307622574477,263.837133669222,23.5274649509199)) ;
#99178 = CARTESIAN_POINT('',(39.4319120248721,265.924309379709,23.5297151930711)) ;
#99179 = CARTESIAN_POINT('',(41.879903193355,264.075690031382,25.0205900571519)) ;
#99180 = CARTESIAN_POINT('Ctrl Pts',(41.879903193355,264.075690031382,25.0205900571519)) ;
#99181 = CARTESIAN_POINT('Ctrl Pts',(41.8770846065361,264.052182781784,25.5146053170057)) ;
#99182 = CARTESIAN_POINT('Ctrl Pts',(41.3905535149138,264.002901986479,26.5550998150335)) ;
#99183 = CARTESIAN_POINT('Ctrl Pts',(39.6433242486872,263.927847645466,26.9070374174888)) ;
#99184 = CARTESIAN_POINT('Ctrl Pts',(38.3288170683365,263.850527008344,25.6250544739862)) ;
#99185 = CARTESIAN_POINT('Ctrl Pts',(38.5878625678462,263.787415464234,24.1488945231714)) ;
#99186 = CARTESIAN_POINT('Ctrl Pts',(39.2151105892869,263.750077465832,23.6430887984231)) ;
#99187 = CARTESIAN_POINT('Ctrl Pts',(39.4328938139748,263.738513013137,23.5316344567886)) ;
#99188 = CARTESIAN_POINT('Ctrl Pts',(41.8777498633429,264.076929005015,25.0206431782745)) ;
#99189 = CARTESIAN_POINT('Ctrl Pts',(41.8777408662402,264.078070021636,24.9983518880119)) ;
#99190 = CARTESIAN_POINT('Ctrl Pts',(41.8772876117826,264.079198153112,24.9760620559688)) ;
#99191 = CARTESIAN_POINT('Ctrl Pts',(41.8756533446456,264.081220516053,24.9354943906631)) ;
#99192 = CARTESIAN_POINT('Ctrl Pts',(41.8746170375289,264.082120366858,24.9172143808539)) ;
#99193 = CARTESIAN_POINT('Ctrl Pts',(41.8721313117513,264.083767802207,24.8832235652733)) ;
#99194 = CARTESIAN_POINT('Ctrl Pts',(41.8707592432701,264.084518571302,24.8675106546475)) ;
#99195 = CARTESIAN_POINT('Ctrl Pts',(41.8668054817143,264.086353342435,24.8285762481613)) ;
#99196 = CARTESIAN_POINT('Ctrl Pts',(41.8639600573264,264.08742444931,24.8053855863338)) ;
#99197 = CARTESIAN_POINT('Ctrl Pts',(41.8481007558253,264.092439213825,24.6952186002258)) ;
#99198 = CARTESIAN_POINT('Ctrl Pts',(41.8287452869014,264.096136679526,24.6092893517415)) ;
#99199 = CARTESIAN_POINT('Ctrl Pts',(41.7722795253813,264.104180656384,24.4268486715436)) ;
#99200 = CARTESIAN_POINT('Ctrl Pts',(41.7328184553478,264.10852135451,24.3314468380638)) ;
#99201 = CARTESIAN_POINT('Ctrl Pts',(41.6685406991477,264.114702193171,24.2092476071826)) ;
#99202 = CARTESIAN_POINT('Ctrl Pts',(41.6512538387103,264.116299371156,24.1787433330275)) ;
#99203 = CARTESIAN_POINT('Ctrl Pts',(41.6182574671597,264.119249025379,24.1245499417344)) ;
#99204 = CARTESIAN_POINT('Ctrl Pts',(41.6028772742757,264.120589825226,24.1006756578644)) ;
#99205 = CARTESIAN_POINT('Ctrl Pts',(41.5667979621182,264.123665755724,24.0476754475527)) ;
#99206 = CARTESIAN_POINT('Ctrl Pts',(41.5457598571171,264.125412671503,24.0187979080923)) ;
#99207 = CARTESIAN_POINT('Ctrl Pts',(41.4549745219419,264.132769691326,23.9021950659991)) ;
#99208 = CARTESIAN_POINT('Ctrl Pts',(41.3774533465819,264.13866311733,23.8209033826338)) ;
#99209 = CARTESIAN_POINT('Ctrl Pts',(41.2318740816957,264.148792620793,23.6960109892401)) ;
#99210 = CARTESIAN_POINT('Ctrl Pts',(41.1676963262942,264.152996445767,23.6484495257852)) ;
#99211 = CARTESIAN_POINT('Ctrl Pts',(41.0816883045609,264.158103861994,23.5937485473334)) ;
#99212 = CARTESIAN_POINT('Ctrl Pts',(41.0627673445744,264.159196823552,23.5822344906057)) ;
#99213 = CARTESIAN_POINT('Ctrl Pts',(41.029524355229,264.161057195035,23.5628963825955)) ;
#99214 = CARTESIAN_POINT('Ctrl Pts',(41.015307448192,264.161833781896,23.5549012695639)) ;
#99215 = CARTESIAN_POINT('Ctrl Pts',(40.9803399299826,264.163699045892,23.5359025094847)) ;
#99216 = CARTESIAN_POINT('Ctrl Pts',(40.9594712309489,264.164775394716,23.5251251389604)) ;
#99217 = CARTESIAN_POINT('Ctrl Pts',(40.8586337779497,264.169832982762,23.4757026084012)) ;
#99218 = CARTESIAN_POINT('Ctrl Pts',(40.7759013935589,264.17356384224,23.4430071403936)) ;
#99219 = CARTESIAN_POINT('Ctrl Pts',(40.5927346483632,264.181631738491,23.3869527782545)) ;
#99220 = CARTESIAN_POINT('Ctrl Pts',(40.4919549105143,264.185963532902,23.3659779228706)) ;
#99221 = CARTESIAN_POINT('Ctrl Pts',(40.3553579648656,264.192123080523,23.3504171927164)) ;
#99222 = CARTESIAN_POINT('Ctrl Pts',(40.3207072523946,264.193708113994,23.3475572154833)) ;
#99223 = CARTESIAN_POINT('Ctrl Pts',(40.2576288981572,264.196646194499,23.3443198461683)) ;
#99224 = CARTESIAN_POINT('Ctrl Pts',(40.229232546643,264.197988111777,23.3435846362962)) ;
#99225 = CARTESIAN_POINT('Ctrl Pts',(40.164785572145,264.201081811222,23.3435526711184)) ;
#99226 = CARTESIAN_POINT('Ctrl Pts',(40.1287495864773,264.20284597214,23.3446964844213)) ;
#99227 = CARTESIAN_POINT('Ctrl Pts',(39.9844645051002,264.210049869502,23.3539362095259)) ;
#99228 = CARTESIAN_POINT('Ctrl Pts',(39.877088242865,264.215750719623,23.3713661918496)) ;
#99229 = CARTESIAN_POINT('Ctrl Pts',(39.6939907851638,264.22575168644,23.4196539621261)) ;
#99230 = CARTESIAN_POINT('Ctrl Pts',(39.6174091990998,264.230018104946,23.4458934499466)) ;
#99231 = CARTESIAN_POINT('Ctrl Pts',(39.521990308725,264.23522524435,23.4865011317105)) ;
#99232 = CARTESIAN_POINT('Ctrl Pts',(39.5011497412199,264.236355173688,23.4958776010857)) ;
#99233 = CARTESIAN_POINT('Ctrl Pts',(39.4657827943611,264.238251990946,23.5126667075724)) ;
#99234 = CARTESIAN_POINT('Ctrl Pts',(39.4511624035582,264.239029419329,23.5198700474164)) ;
#99235 = CARTESIAN_POINT('Ctrl Pts',(39.4350678387167,264.2398779681,23.5280933016812)) ;
#99236 = CARTESIAN_POINT('Ctrl Pts',(39.4334892848808,264.239961121345,23.5289029979362)) ;
#99237 = CARTESIAN_POINT('Ctrl Pts',(39.431912024867,264.240044136826,23.5297151930737)) ;
#99238 = CARTESIAN_POINT('',(41.8766931555041,264.174309021491,25.0225048790946)) ;
#99239 = CARTESIAN_POINT('Ctrl Pts',(39.4319120259791,264.338362624254,23.529715192501)) ;
#99240 = CARTESIAN_POINT('Ctrl Pts',(39.4390323455915,264.337968227664,23.5260486512172)) ;
#99241 = CARTESIAN_POINT('Ctrl Pts',(39.4461790647084,264.337572220708,23.5224330192047)) ;
#99242 = CARTESIAN_POINT('Ctrl Pts',(39.4881142715112,264.335247709388,23.5015931799167)) ;
#99243 = CARTESIAN_POINT('Ctrl Pts',(39.5234643057111,264.333284461677,23.4855302747096)) ;
#99244 = CARTESIAN_POINT('Ctrl Pts',(39.6323798394147,264.327234989789,23.4405299568904)) ;
#99245 = CARTESIAN_POINT('Ctrl Pts',(39.7074593016282,264.323059053107,23.4155515735615)) ;
#99246 = CARTESIAN_POINT('Ctrl Pts',(39.855014449483,264.315017525861,23.377787200928)) ;
#99247 = CARTESIAN_POINT('Ctrl Pts',(39.9271325458305,264.311161464821,23.3642866306841)) ;
#99248 = CARTESIAN_POINT('Ctrl Pts',(40.0235188989513,264.306274048564,23.3527086080441)) ;
#99249 = CARTESIAN_POINT('Ctrl Pts',(40.047191066422,264.305095036168,23.3503744339759)) ;
#99250 = CARTESIAN_POINT('Ctrl Pts',(40.0871757529087,264.303148234703,23.3472886718005)) ;
#99251 = CARTESIAN_POINT('Ctrl Pts',(40.1034628591235,264.302368107889,23.3462704995395)) ;
#99252 = CARTESIAN_POINT('Ctrl Pts',(40.1416222774926,264.300570885418,23.3444434898145)) ;
#99253 = CARTESIAN_POINT('Ctrl Pts',(40.1634998155945,264.29956295695,23.3438246638934)) ;
#99254 = CARTESIAN_POINT('Ctrl Pts',(40.2715341343524,264.294670555204,23.3428834726316)) ;
#99255 = CARTESIAN_POINT('Ctrl Pts',(40.3576211551497,264.291033812052,23.3487697908435)) ;
#99256 = CARTESIAN_POINT('Ctrl Pts',(40.5463488981929,264.282997093703,23.3763819182621)) ;
#99257 = CARTESIAN_POINT('Ctrl Pts',(40.6481730119896,264.278607696969,23.4011600096864)) ;
#99258 = CARTESIAN_POINT('Ctrl Pts',(40.7810203141091,264.272339445258,23.4469780031944)) ;
#99259 = CARTESIAN_POINT('Ctrl Pts',(40.8146308924844,264.270706451648,23.4597931830893)) ;
#99260 = CARTESIAN_POINT('Ctrl Pts',(40.8740092967406,264.267722593989,23.4846474263884)) ;
#99261 = CARTESIAN_POINT('Ctrl Pts',(40.8999322062344,264.266385048693,23.4962803503998)) ;
#99262 = CARTESIAN_POINT('Ctrl Pts',(40.9564609679694,264.263385806754,23.5233926346267)) ;
#99263 = CARTESIAN_POINT('Ctrl Pts',(40.9869122583999,264.261714946371,23.5391632958224)) ;
#99264 = CARTESIAN_POINT('Ctrl Pts',(41.1030265753594,264.25512278373,23.6038860112563)) ;
#99265 = CARTESIAN_POINT('Ctrl Pts',(41.1847823354294,264.249986467621,23.6594183399636)) ;
#99266 = CARTESIAN_POINT('Ctrl Pts',(41.3350220989899,264.239752654803,23.7821033048645)) ;
#99267 = CARTESIAN_POINT('Ctrl Pts',(41.4035945727203,264.234681606571,23.8485903103051)) ;
#99268 = CARTESIAN_POINT('Ctrl Pts',(41.4812296826987,264.228737573453,23.9378888544084)) ;
#99269 = CARTESIAN_POINT('Ctrl Pts',(41.4959517193035,264.22760058577,23.9555424472142)) ;
#99270 = CARTESIAN_POINT('Ctrl Pts',(41.5204818627628,264.2256970093,23.9862173857321)) ;
#99271 = CARTESIAN_POINT('Ctrl Pts',(41.5304705487348,264.224919610418,23.9990881570199)) ;
#99272 = CARTESIAN_POINT('Ctrl Pts',(41.5538499053762,264.223094235373,24.0301366777674)) ;
#99273 = CARTESIAN_POINT('Ctrl Pts',(41.5670637864611,264.222056804688,24.0484424923686)) ;
#99274 = CARTESIAN_POINT('Ctrl Pts',(41.5955869111078,264.219791557552,24.0896860986495)) ;
#99275 = CARTESIAN_POINT('Ctrl Pts',(41.6107083322645,264.218572743293,24.1127460192723)) ;
#99276 = CARTESIAN_POINT('Ctrl Pts',(41.6583652766146,264.214637365794,24.1894823813251)) ;
#99277 = CARTESIAN_POINT('Ctrl Pts',(41.688459220635,264.211996099433,24.2446135903258)) ;
#99278 = CARTESIAN_POINT('Ctrl Pts',(41.7579401169828,264.205177029998,24.3908474717832)) ;
#99279 = CARTESIAN_POINT('Ctrl Pts',(41.7924640147267,264.200998968375,24.4839839739778)) ;
#99280 = CARTESIAN_POINT('Ctrl Pts',(41.8279961132188,264.194976787318,24.6141867910252)) ;
#99281 = CARTESIAN_POINT('Ctrl Pts',(41.8363196099233,264.193349201256,24.6490475845156)) ;
#99282 = CARTESIAN_POINT('Ctrl Pts',(41.8492284357439,264.190370997022,24.7119704403943)) ;
#99283 = CARTESIAN_POINT('Ctrl Pts',(41.8542288453068,264.189033464771,24.739933402068)) ;
#99284 = CARTESIAN_POINT('Ctrl Pts',(41.8625899506186,264.186383643453,24.7946764261395)) ;
#99285 = CARTESIAN_POINT('Ctrl Pts',(41.8660190550052,264.185073856958,24.8214373290495)) ;
#99286 = CARTESIAN_POINT('Ctrl Pts',(41.8748052654834,264.180879547383,24.9061658870588)) ;
#99287 = CARTESIAN_POINT('Ctrl Pts',(41.8777915094445,264.17792889845,24.9643312464074)) ;
#99288 = CARTESIAN_POINT('Ctrl Pts',(41.8777495642464,264.174918096163,25.0225295461999)) ;
#99289 = CARTESIAN_POINT('Ctrl Pts',(41.8766931555041,264.174309021491,25.0225048790946)) ;
#99290 = CARTESIAN_POINT('Ctrl Pts',(41.8779055444877,264.16603034488,25.1973496541196)) ;
#99291 = CARTESIAN_POINT('Ctrl Pts',(41.7737573850774,264.13197812256,25.9151209251136)) ;
#99292 = CARTESIAN_POINT('Ctrl Pts',(40.7566757434656,264.072152354534,26.9070373909177)) ;
#99293 = CARTESIAN_POINT('Ctrl Pts',(38.9566882099319,263.994831717412,26.5444728956893)) ;
#99294 = CARTESIAN_POINT('Ctrl Pts',(38.2410020294161,263.91751108029,24.8535549132323)) ;
#99295 = CARTESIAN_POINT('Ctrl Pts',(38.9159323185171,263.864945064226,23.8034612485711)) ;
#99296 = CARTESIAN_POINT('Ctrl Pts',(39.4117048817585,263.83815259387,23.5372014183592)) ;
#99297 = CARTESIAN_POINT('Ctrl Pts',(39.4307622574477,263.837133669222,23.5274649509199)) ;
#99298 = CARTESIAN_POINT('Origin',(40.2,265.924309379709,25.0213203435596)) ;
#99299 = CARTESIAN_POINT('',(39.4319120248721,263.238554795302,23.5297151930711)) ;
#99300 = CARTESIAN_POINT('',(39.4319120248721,263.338461000729,23.5297151930711)) ;
#99301 = CARTESIAN_POINT('',(39.4319120248721,265.924309379709,23.5297151930711)) ;
#99302 = CARTESIAN_POINT('',(41.8775578586602,263.575690620291,25.0217527388377)) ;
#99303 = CARTESIAN_POINT('Ctrl Pts',(41.8777499442681,263.575690620291,25.0217527883483)) ;
#99304 = CARTESIAN_POINT('Ctrl Pts',(41.8777329243011,263.572573203823,25.0877849139014)) ;
#99305 = CARTESIAN_POINT('Ctrl Pts',(41.8738133493319,263.569455787356,25.1537158423017)) ;
#99306 = CARTESIAN_POINT('Ctrl Pts',(41.8660523250862,263.566338370888,25.2190947417381)) ;
#99307 = CARTESIAN_POINT('Ctrl Pts',(41.8582740066163,263.563214007747,25.2846193277889)) ;
#99308 = CARTESIAN_POINT('Ctrl Pts',(41.8466372278417,263.560089644607,25.3495890519222)) ;
#99309 = CARTESIAN_POINT('Ctrl Pts',(41.8312540968924,263.556965281466,25.4135640610002)) ;
#99310 = CARTESIAN_POINT('Ctrl Pts',(41.8158157329821,263.553829700334,25.4777687716389)) ;
#99311 = CARTESIAN_POINT('Ctrl Pts',(41.7966042220182,263.550694119202,25.5409712531395)) ;
#99312 = CARTESIAN_POINT('Ctrl Pts',(41.7737816615251,263.54755853807,25.6027464733022)) ;
#99313 = CARTESIAN_POINT('Ctrl Pts',(41.7584624988814,263.545453845332,25.6442117876479)) ;
#99314 = CARTESIAN_POINT('Ctrl Pts',(41.7415173929883,263.543349152593,25.68503446504)) ;
#99315 = CARTESIAN_POINT('Ctrl Pts',(41.7230070307806,263.541244459855,25.7250920726685)) ;
#99316 = CARTESIAN_POINT('Ctrl Pts',(41.6973518096356,263.538327371737,25.7806116119791)) ;
#99317 = CARTESIAN_POINT('Ctrl Pts',(41.6686081706387,263.53541028362,25.8348317573898)) ;
#99318 = CARTESIAN_POINT('Ctrl Pts',(41.6369308169397,263.532493195502,25.8873889839276)) ;
#99319 = CARTESIAN_POINT('Ctrl Pts',(41.6053058407034,263.529580930694,25.9398593088198)) ;
#99320 = CARTESIAN_POINT('Ctrl Pts',(41.5707570426465,263.526668665886,25.9906717442065)) ;
#99321 = CARTESIAN_POINT('Ctrl Pts',(41.533485809679,263.523756401078,26.0394856827284)) ;
#99322 = CARTESIAN_POINT('Ctrl Pts',(41.4962490219902,263.520846827723,26.0882545084494)) ;
#99323 = CARTESIAN_POINT('Ctrl Pts',(41.4562950939316,263.517937254367,26.1350280980593)) ;
#99324 = CARTESIAN_POINT('Ctrl Pts',(41.4138687824863,263.515027681012,26.1794946143)) ;
#99325 = CARTESIAN_POINT('Ctrl Pts',(41.3714662976345,263.512119741672,26.2239361581695)) ;
#99326 = CARTESIAN_POINT('Ctrl Pts',(41.3265945328691,263.509211802332,26.2660728326465)) ;
#99327 = CARTESIAN_POINT('Ctrl Pts',(41.2795372911181,263.506303862991,26.3056272771177)) ;
#99328 = CARTESIAN_POINT('Ctrl Pts',(41.2324894161032,263.503396502476,26.3451738482833)) ;
#99329 = CARTESIAN_POINT('Ctrl Pts',(41.1832573162042,263.50048914196,26.382138884622)) ;
#99330 = CARTESIAN_POINT('Ctrl Pts',(41.1321587541967,263.497581781445,26.4162845436287)) ;
#99331 = CARTESIAN_POINT('Ctrl Pts',(41.0810169293498,263.494671959398,26.4504591122193)) ;
#99332 = CARTESIAN_POINT('Ctrl Pts',(41.0280059065627,263.491762137352,26.4818092506801)) ;
#99333 = CARTESIAN_POINT('Ctrl Pts',(40.9734723809854,263.488852315306,26.5101405269104)) ;
#99334 = CARTESIAN_POINT('Ctrl Pts',(40.918916921347,263.485941322894,26.5384831983319)) ;
#99335 = CARTESIAN_POINT('Ctrl Pts',(40.8628382000286,263.483030330481,26.5638043759017)) ;
#99336 = CARTESIAN_POINT('Ctrl Pts',(40.8056047559154,263.480119338068,26.5859570241065)) ;
#99337 = CARTESIAN_POINT('Ctrl Pts',(40.7482693995172,263.47720316222,26.6081491182511)) ;
#99338 = CARTESIAN_POINT('Ctrl Pts',(40.6897756947109,263.474286986371,26.627161250375)) ;
#99339 = CARTESIAN_POINT('Ctrl Pts',(40.6305084602919,263.471370810523,26.6428959748877)) ;
#99340 = CARTESIAN_POINT('Ctrl Pts',(40.5800585567212,263.46888848126,26.6562898061025)) ;
#99341 = CARTESIAN_POINT('Ctrl Pts',(40.5290485721046,263.466406151996,26.6673096974672)) ;
#99342 = CARTESIAN_POINT('Ctrl Pts',(40.4777199314581,263.463923822733,26.675925040208)) ;
#99343 = CARTESIAN_POINT('Ctrl Pts',(40.4174066934933,263.461006985005,26.6860484179232)) ;
#99344 = CARTESIAN_POINT('Ctrl Pts',(40.3564248957029,263.458090147277,26.6928889412897)) ;
#99345 = CARTESIAN_POINT('Ctrl Pts',(40.2951619462482,263.455173309549,26.6963693776139)) ;
#99346 = CARTESIAN_POINT('Ctrl Pts',(40.2340001096249,263.452261285982,26.6998440695727)) ;
#99347 = CARTESIAN_POINT('Ctrl Pts',(40.1725585453303,263.449349262416,26.6999696590415)) ;
#99348 = CARTESIAN_POINT('Ctrl Pts',(40.1112320620376,263.446437238849,26.6967203900231)) ;
#99349 = CARTESIAN_POINT('Ctrl Pts',(40.0499621389294,263.443527900983,26.6934741177403)) ;
#99350 = CARTESIAN_POINT('Ctrl Pts',(39.9888075904029,263.440618563117,26.6868591846697)) ;
#99351 = CARTESIAN_POINT('Ctrl Pts',(39.9281639212254,263.437709225252,26.6769018754621)) ;
#99352 = CARTESIAN_POINT('Ctrl Pts',(39.867554185143,263.434801515302,26.6669501378552)) ;
#99353 = CARTESIAN_POINT('Ctrl Pts',(39.807455260742,263.431893805353,26.65365981585)) ;
#99354 = CARTESIAN_POINT('Ctrl Pts',(39.7482561967113,263.428986095404,26.6371088812991)) ;
#99355 = CARTESIAN_POINT('Ctrl Pts',(39.689068785836,263.426078957829,26.6205612047491)) ;
#99356 = CARTESIAN_POINT('Ctrl Pts',(39.6307813714153,263.423171820254,26.6007543272832)) ;
#99357 = CARTESIAN_POINT('Ctrl Pts',(39.5737695135502,263.420264682678,26.5778165498964)) ;
#99358 = CARTESIAN_POINT('Ctrl Pts',(39.5167091539581,263.417355071912,26.5548592586425)) ;
#99359 = CARTESIAN_POINT('Ctrl Pts',(39.4609269909413,263.414445461146,26.5287659339765)) ;
#99360 = CARTESIAN_POINT('Ctrl Pts',(39.4067790474548,263.411535850381,26.4997132490294)) ;
#99361 = CARTESIAN_POINT('Ctrl Pts',(39.3526092092718,263.408625063115,26.4706488166421)) ;
#99362 = CARTESIAN_POINT('Ctrl Pts',(39.3000753427169,263.405714275849,26.4386229010154)) ;
#99363 = CARTESIAN_POINT('Ctrl Pts',(39.249506641468,263.402803488583,26.4038569390559)) ;
#99364 = CARTESIAN_POINT('Ctrl Pts',(39.1988476703477,263.399887505289,26.3690289165958)) ;
#99365 = CARTESIAN_POINT('Ctrl Pts',(39.1501612777587,263.396971521996,26.3314513835271)) ;
#99366 = CARTESIAN_POINT('Ctrl Pts',(39.1037448806965,263.394055538702,26.2913871827066)) ;
#99367 = CARTESIAN_POINT('Ctrl Pts',(39.0642028868813,263.391571421005,26.2572566064162)) ;
#99368 = CARTESIAN_POINT('Ctrl Pts',(39.0263078400301,263.389087303308,26.2213221902367)) ;
#99369 = CARTESIAN_POINT('Ctrl Pts',(38.9902214910315,263.386603185611,26.1837664806937)) ;
#99370 = CARTESIAN_POINT('Ctrl Pts',(38.9478786271104,263.383688380968,26.1396995040455)) ;
#99371 = CARTESIAN_POINT('Ctrl Pts',(38.9078655732094,263.380773576325,26.0932316296736)) ;
#99372 = CARTESIAN_POINT('Ctrl Pts',(38.8704644770455,263.377858771682,26.0446386497097)) ;
#99373 = CARTESIAN_POINT('Ctrl Pts',(38.8331252898328,263.374948791831,25.9961261042982)) ;
#99374 = CARTESIAN_POINT('Ctrl Pts',(38.798389782311,263.37203881198,25.9454958379628)) ;
#99375 = CARTESIAN_POINT('Ctrl Pts',(38.7665017994721,263.369128832129,25.8930588201586)) ;
#99376 = CARTESIAN_POINT('Ctrl Pts',(38.7346432991151,263.366221542741,25.8406702837349)) ;
#99377 = CARTESIAN_POINT('Ctrl Pts',(38.7056273667572,263.363314253352,25.7864787394361)) ;
#99378 = CARTESIAN_POINT('Ctrl Pts',(38.679655286762,263.360406963964,25.730825111288)) ;
#99379 = CARTESIAN_POINT('Ctrl Pts',(38.6536977585997,263.357501303493,25.6752026651745)) ;
#99380 = CARTESIAN_POINT('Ctrl Pts',(38.630780914475,263.354595643023,25.6181202193676)) ;
#99381 = CARTESIAN_POINT('Ctrl Pts',(38.611059726689,263.351689982552,25.5599425398626)) ;
#99382 = CARTESIAN_POINT('Ctrl Pts',(38.5913424049923,263.3487848917,25.5017762653558)) ;
#99383 = CARTESIAN_POINT('Ctrl Pts',(38.5748196579882,263.345879800847,25.4425156643958)) ;
#99384 = CARTESIAN_POINT('Ctrl Pts',(38.5615972941645,263.342974709995,25.3825427625912)) ;
#99385 = CARTESIAN_POINT('Ctrl Pts',(38.5483635797371,263.340067125297,25.3225183776586)) ;
#99386 = CARTESIAN_POINT('Ctrl Pts',(38.5384360201161,263.337159540599,25.2617809668352)) ;
#99387 = CARTESIAN_POINT('Ctrl Pts',(38.5318694613474,263.3342519559,25.2007237117402)) ;
#99388 = CARTESIAN_POINT('Ctrl Pts',(38.5253002261765,263.331343186127,25.1396415708903)) ;
#99389 = CARTESIAN_POINT('Ctrl Pts',(38.5220947511226,263.328434416354,25.0782398338323)) ;
#99390 = CARTESIAN_POINT('Ctrl Pts',(38.5222557842831,263.32552564658,25.016914764314)) ;
#99391 = CARTESIAN_POINT('Ctrl Pts',(38.5224171072803,263.322611641435,24.9554793183959)) ;
#99392 = CARTESIAN_POINT('Ctrl Pts',(38.5259570180978,263.31969763629,24.8941213243164)) ;
#99393 = CARTESIAN_POINT('Ctrl Pts',(38.532826150209,263.316783631145,24.8332341477001)) ;
#99394 = CARTESIAN_POINT('Ctrl Pts',(38.5387202061188,263.31428327026,24.7809899314929)) ;
#99395 = CARTESIAN_POINT('Ctrl Pts',(38.5470644947108,263.311782909374,24.7290924455471)) ;
#99396 = CARTESIAN_POINT('Ctrl Pts',(38.5577980721274,263.309282548489,24.6777830230377)) ;
#99397 = CARTESIAN_POINT('Ctrl Pts',(38.5704489428273,263.306335558773,24.6173084166072)) ;
#99398 = CARTESIAN_POINT('Ctrl Pts',(38.5864685731215,263.303388569057,24.5574193685552)) ;
#99399 = CARTESIAN_POINT('Ctrl Pts',(38.6057851883701,263.30044157934,24.4985161767056)) ;
#99400 = CARTESIAN_POINT('Ctrl Pts',(38.6248974385109,263.297525768061,24.4402361663505)) ;
#99401 = CARTESIAN_POINT('Ctrl Pts',(38.6472371113445,263.294609956782,24.382921750514)) ;
#99402 = CARTESIAN_POINT('Ctrl Pts',(38.6726834954224,263.291694145503,24.3269505880656)) ;
#99403 = CARTESIAN_POINT('Ctrl Pts',(38.6981058096377,263.288781092304,24.2710323690211)) ;
#99404 = CARTESIAN_POINT('Ctrl Pts',(38.7266287987076,263.285868039106,24.2164553415877)) ;
#99405 = CARTESIAN_POINT('Ctrl Pts',(38.7580830754285,263.282954985907,24.1635787477778)) ;
#99406 = CARTESIAN_POINT('Ctrl Pts',(38.7895189214046,263.280043639622,24.1107331371952)) ;
#99407 = CARTESIAN_POINT('Ctrl Pts',(38.8238823885485,263.277132293338,24.0595864165176)) ;
#99408 = CARTESIAN_POINT('Ctrl Pts',(38.8609583578683,263.274220947053,24.0104729054478)) ;
#99409 = CARTESIAN_POINT('Ctrl Pts',(38.8988090352623,263.27124876774,23.9603331600198)) ;
#99410 = CARTESIAN_POINT('Ctrl Pts',(38.9394865908686,263.268276588428,23.912313033548)) ;
#99411 = CARTESIAN_POINT('Ctrl Pts',(38.9827169258795,263.265304409115,23.8667351453348)) ;
#99412 = CARTESIAN_POINT('Ctrl Pts',(39.0250778551607,263.262392003332,23.8220738745188)) ;
#99413 = CARTESIAN_POINT('Ctrl Pts',(39.0698894207336,263.25947959755,23.7797578404798)) ;
#99414 = CARTESIAN_POINT('Ctrl Pts',(39.1168561979467,263.256567191767,23.740053561592)) ;
#99415 = CARTESIAN_POINT('Ctrl Pts',(39.1652688777606,263.253565125689,23.6991269608098)) ;
#99416 = CARTESIAN_POINT('Ctrl Pts',(39.2159712282981,263.250563059612,23.6609759589132)) ;
#99417 = CARTESIAN_POINT('Ctrl Pts',(39.2686048925834,263.247560993534,23.6258461530493)) ;
#99418 = CARTESIAN_POINT('Ctrl Pts',(39.3212385568686,263.244558927457,23.5907163471854)) ;
#99419 = CARTESIAN_POINT('Ctrl Pts',(39.375803011097,263.241556861379,23.5586079994299)) ;
#99420 = CARTESIAN_POINT('Ctrl Pts',(39.4319120248721,263.238554795302,23.5297151930711)) ;
#99421 = CARTESIAN_POINT('Ctrl Pts',(39.4328938139748,263.738513013137,23.5316344567886)) ;
#99422 = CARTESIAN_POINT('Ctrl Pts',(39.7004812370594,263.724303920124,23.3946919530109)) ;
#99423 = CARTESIAN_POINT('Ctrl Pts',(40.553309744137,263.684321281405,23.2013871196432)) ;
#99424 = CARTESIAN_POINT('Ctrl Pts',(41.6546450483183,263.630047150456,23.8708672620324)) ;
#99425 = CARTESIAN_POINT('Ctrl Pts',(41.8748774768301,263.58998211252,24.719421150606)) ;
#99426 = CARTESIAN_POINT('Ctrl Pts',(41.8756052318586,263.575690620291,25.0217522355426)) ;
#99427 = CARTESIAN_POINT('',(41.8792166192085,263.674309379709,25.0202225427276)) ;
#99428 = CARTESIAN_POINT('Ctrl Pts',(39.4307622574477,263.837133669222,23.5274649509199)) ;
#99429 = CARTESIAN_POINT('Ctrl Pts',(39.8937583329918,263.812379048163,23.2909189391529)) ;
#99430 = CARTESIAN_POINT('Ctrl Pts',(41.0833957882848,263.761850881396,23.2773060297436)) ;
#99431 = CARTESIAN_POINT('Ctrl Pts',(41.8396641814559,263.707576118226,24.3209713985087)) ;
#99432 = CARTESIAN_POINT('Ctrl Pts',(41.879821877795,263.678055976114,24.9414011775634)) ;
#99433 = CARTESIAN_POINT('Ctrl Pts',(41.8792166192085,263.674309379709,25.0202225427276)) ;
#99434 = CARTESIAN_POINT('Ctrl Pts',(39.4319120248721,263.338461000729,23.5297151930711)) ;
#99435 = CARTESIAN_POINT('Ctrl Pts',(39.4319044575765,263.338461403864,23.5297190897784)) ;
#99436 = CARTESIAN_POINT('Ctrl Pts',(39.43189689031,263.338461806997,23.5297229865437)) ;
#99437 = CARTESIAN_POINT('Ctrl Pts',(39.4058424989406,263.339849808694,23.5431399508344)) ;
#99438 = CARTESIAN_POINT('Ctrl Pts',(39.3801506644007,263.341214537394,23.5572333935033)) ;
#99439 = CARTESIAN_POINT('Ctrl Pts',(39.3160652980963,263.344615811434,23.5946040941535)) ;
#99440 = CARTESIAN_POINT('Ctrl Pts',(39.2782120603637,263.346621717723,23.6187629767869)) ;
#99441 = CARTESIAN_POINT('Ctrl Pts',(39.193782529487,263.351128734748,23.6775443528212)) ;
#99442 = CARTESIAN_POINT('Ctrl Pts',(39.147942008179,263.353599803862,23.7131223859606)) ;
#99443 = CARTESIAN_POINT('Ctrl Pts',(39.0200419202545,263.360736592239,23.8234681553043)) ;
#99444 = CARTESIAN_POINT('Ctrl Pts',(38.9434506885163,263.36531733879,23.9040779328976)) ;
#99445 = CARTESIAN_POINT('Ctrl Pts',(38.8611314484283,263.371363523247,24.0099771130338)) ;
#99446 = CARTESIAN_POINT('Ctrl Pts',(38.8472647856884,263.372428427657,24.0286011092544)) ;
#99447 = CARTESIAN_POINT('Ctrl Pts',(38.8243309000595,263.37428146348,24.0607761469446)) ;
#99448 = CARTESIAN_POINT('Ctrl Pts',(38.8150670371125,263.375057781882,24.0741818732709)) ;
#99449 = CARTESIAN_POINT('Ctrl Pts',(38.7935596389193,263.376928426921,24.1062955711805)) ;
#99450 = CARTESIAN_POINT('Ctrl Pts',(38.781492816229,263.378032348686,24.1251160657035)) ;
#99451 = CARTESIAN_POINT('Ctrl Pts',(38.7555884303837,263.380516773099,24.1673532300005)) ;
#99452 = CARTESIAN_POINT('Ctrl Pts',(38.7419369548427,263.381905025912,24.1908766921485)) ;
#99453 = CARTESIAN_POINT('Ctrl Pts',(38.6703601181564,263.389594067685,24.3214238146592)) ;
#99454 = CARTESIAN_POINT('Ctrl Pts',(38.6236377447206,263.396147514065,24.4341764181685)) ;
#99455 = CARTESIAN_POINT('Ctrl Pts',(38.5733502512279,263.405399704688,24.6063704400849)) ;
#99456 = CARTESIAN_POINT('Ctrl Pts',(38.5600446374816,263.408312746396,24.6625444893242)) ;
#99457 = CARTESIAN_POINT('Ctrl Pts',(38.5440720902454,263.412663317211,24.749822836433)) ;
#99458 = CARTESIAN_POINT('Ctrl Pts',(38.5393333828028,263.414160205158,24.780499508075)) ;
#99459 = CARTESIAN_POINT('Ctrl Pts',(38.5318059400181,263.417011639889,24.8401570440491)) ;
#99460 = CARTESIAN_POINT('Ctrl Pts',(38.5289150858453,263.41836875821,24.8691136058087)) ;
#99461 = CARTESIAN_POINT('Ctrl Pts',(38.5235849726333,263.421701726824,24.9415104177954)) ;
#99462 = CARTESIAN_POINT('Ctrl Pts',(38.5220792577608,263.423649761571,24.9849984063511)) ;
#99463 = CARTESIAN_POINT('Ctrl Pts',(38.5225011724418,263.427980741696,25.0836202657161)) ;
#99464 = CARTESIAN_POINT('Ctrl Pts',(38.5254534333382,263.430337593687,25.1386991011082)) ;
#99465 = CARTESIAN_POINT('Ctrl Pts',(38.5433683106536,263.437724376507,25.3123083204376)) ;
#99466 = CARTESIAN_POINT('Ctrl Pts',(38.5682679108056,263.442628282687,25.4294228230056)) ;
#99467 = CARTESIAN_POINT('Ctrl Pts',(38.6121239160881,263.449015500475,25.5635058129442)) ;
#99468 = CARTESIAN_POINT('Ctrl Pts',(38.6192658359416,263.450014139772,25.5839880680574)) ;
#99469 = CARTESIAN_POINT('Ctrl Pts',(38.6324676319988,263.451800418636,25.6196121796026)) ;
#99470 = CARTESIAN_POINT('Ctrl Pts',(38.6383546152184,263.45257925519,25.6348140193688)) ;
#99471 = CARTESIAN_POINT('Ctrl Pts',(38.6532696752001,263.454510667088,25.6717224767552)) ;
#99472 = CARTESIAN_POINT('Ctrl Pts',(38.662533735973,263.455675059202,25.693328544745)) ;
#99473 = CARTESIAN_POINT('Ctrl Pts',(38.6843174540834,263.458326602395,25.7413232974513)) ;
#99474 = CARTESIAN_POINT('Ctrl Pts',(38.6970784603404,263.459823112037,25.7675941195224)) ;
#99475 = CARTESIAN_POINT('Ctrl Pts',(38.7430329670758,263.464998175439,25.8562352314396)) ;
#99476 = CARTESIAN_POINT('Ctrl Pts',(38.7794761933834,263.468751008503,25.9168356382739)) ;
#99477 = CARTESIAN_POINT('Ctrl Pts',(38.8689869973971,263.47705043823,26.0464006856156)) ;
#99478 = CARTESIAN_POINT('Ctrl Pts',(38.9238197952373,263.481565314494,26.1139098862064)) ;
#99479 = CARTESIAN_POINT('Ctrl Pts',(39.0085115648262,263.487699226595,26.2030583254597)) ;
#99480 = CARTESIAN_POINT('Ctrl Pts',(39.0342257126429,263.489469076468,26.2284325558702)) ;
#99481 = CARTESIAN_POINT('Ctrl Pts',(39.0816018880483,263.492570921132,26.2722553214881)) ;
#99482 = CARTESIAN_POINT('Ctrl Pts',(39.1029512817602,263.493915386886,26.2910198666659)) ;
#99483 = CARTESIAN_POINT('Ctrl Pts',(39.1509963110643,263.496830437889,26.3311309188373)) ;
#99484 = CARTESIAN_POINT('Ctrl Pts',(39.1778884361967,263.498390992979,26.3522225234828)) ;
#99485 = CARTESIAN_POINT('Ctrl Pts',(39.2845272262057,263.504334138981,26.4307197364887)) ;
#99486 = CARTESIAN_POINT('Ctrl Pts',(39.3686136710503,263.508496086443,26.481900875294)) ;
#99487 = CARTESIAN_POINT('Ctrl Pts',(39.5429945408381,263.51669064325,26.568076525783)) ;
#99488 = CARTESIAN_POINT('Ctrl Pts',(39.6327944658652,263.520713540441,26.6032134506906)) ;
#99489 = CARTESIAN_POINT('Ctrl Pts',(39.747057515106,263.526089597176,26.6369354558312)) ;
#99490 = CARTESIAN_POINT('Ctrl Pts',(39.7691422932421,263.527140559994,26.6429647667264)) ;
#99491 = CARTESIAN_POINT('Ctrl Pts',(39.8071463279377,263.528979548858,26.6525090409327)) ;
#99492 = CARTESIAN_POINT('Ctrl Pts',(39.8230053079206,263.529756410549,26.656247112356)) ;
#99493 = CARTESIAN_POINT('Ctrl Pts',(39.8610600518077,263.531643721149,26.6646337367622)) ;
#99494 = CARTESIAN_POINT('Ctrl Pts',(39.883298951415,263.532764376248,26.6690641204087)) ;
#99495 = CARTESIAN_POINT('Ctrl Pts',(39.9329330077061,263.535294655861,26.6779102120752)) ;
#99496 = CARTESIAN_POINT('Ctrl Pts',(39.9603617730635,263.536712456932,26.6820997311774)) ;
#99497 = CARTESIAN_POINT('Ctrl Pts',(40.0509174967801,263.541431817705,26.693641383384)) ;
#99498 = CARTESIAN_POINT('Ctrl Pts',(40.1143584020489,263.544797330329,26.6980875942634)) ;
#99499 = CARTESIAN_POINT('Ctrl Pts',(40.2745680664189,263.553255944834,26.7001984256077)) ;
#99500 = CARTESIAN_POINT('Ctrl Pts',(40.3711770065349,263.558309746368,26.6931139301979)) ;
#99501 = CARTESIAN_POINT('Ctrl Pts',(40.5024958732422,263.564948060427,26.6719747306022)) ;
#99502 = CARTESIAN_POINT('Ctrl Pts',(40.5381514245898,263.566728384874,26.6650409736292)) ;
#99503 = CARTESIAN_POINT('Ctrl Pts',(40.6012675549001,263.569841170859,26.6506261536765)) ;
#99504 = CARTESIAN_POINT('Ctrl Pts',(40.6288150989568,263.571186461844,26.6435936860961)) ;
#99505 = CARTESIAN_POINT('Ctrl Pts',(40.6888966465598,263.574095343964,26.6266183050179)) ;
#99506 = CARTESIAN_POINT('Ctrl Pts',(40.7213340270502,263.575649204437,26.6163791152147)) ;
#99507 = CARTESIAN_POINT('Ctrl Pts',(40.846483191327,263.581602174001,26.5726484172548)) ;
#99508 = CARTESIAN_POINT('Ctrl Pts',(40.9364855233383,263.585778126847,26.5319990247848)) ;
#99509 = CARTESIAN_POINT('Ctrl Pts',(41.1065257039739,263.593996575398,26.4363720968552)) ;
#99510 = CARTESIAN_POINT('Ctrl Pts',(41.1864047889597,263.598029362854,26.381894834373)) ;
#99511 = CARTESIAN_POINT('Ctrl Pts',(41.2788632244251,263.603416216669,26.3063970321614)) ;
#99512 = CARTESIAN_POINT('Ctrl Pts',(41.2962769625047,263.604466104081,26.2915741321219)) ;
#99513 = CARTESIAN_POINT('Ctrl Pts',(41.3255691877186,263.606303890727,26.2655890022676)) ;
#99514 = CARTESIAN_POINT('Ctrl Pts',(41.3375973185249,263.607080669057,26.2546016557788)) ;
#99515 = CARTESIAN_POINT('Ctrl Pts',(41.3659919051207,263.608968672486,26.2278951511075)) ;
#99516 = CARTESIAN_POINT('Ctrl Pts',(41.3822020408915,263.610090138224,26.212016835085)) ;
#99517 = CARTESIAN_POINT('Ctrl Pts',(41.4175251398623,263.612622679174,26.175984281412)) ;
#99518 = CARTESIAN_POINT('Ctrl Pts',(41.4364697245729,263.614041953369,26.1556742472572)) ;
#99519 = CARTESIAN_POINT('Ctrl Pts',(41.4971640145001,263.618769609122,26.0872776849906)) ;
#99520 = CARTESIAN_POINT('Ctrl Pts',(41.5366806976195,263.622142135583,26.0372848562047)) ;
#99521 = CARTESIAN_POINT('Ctrl Pts',(41.6286871494578,263.630596959818,25.9061970663488)) ;
#99522 = CARTESIAN_POINT('Ctrl Pts',(41.6772043377122,263.63563996828,25.8225846347282)) ;
#99523 = CARTESIAN_POINT('Ctrl Pts',(41.7337212149292,263.64226861977,25.7023953005309)) ;
#99524 = CARTESIAN_POINT('Ctrl Pts',(41.7481041164238,263.644049099289,25.6690376768099)) ;
#99525 = CARTESIAN_POINT('Ctrl Pts',(41.7717946615636,263.647161987809,25.6087848524232)) ;
#99526 = CARTESIAN_POINT('Ctrl Pts',(41.7815220283639,263.648507233998,25.5820709071693)) ;
#99527 = CARTESIAN_POINT('Ctrl Pts',(41.8013840827117,263.651415824902,25.5228880041033)) ;
#99528 = CARTESIAN_POINT('Ctrl Pts',(41.8112198767887,263.652969446806,25.4903318399547)) ;
#99529 = CARTESIAN_POINT('Ctrl Pts',(41.8456271061157,263.658912480982,25.3625357860149)) ;
#99530 = CARTESIAN_POINT('Ctrl Pts',(41.8627964239559,263.663079890315,25.2655053044538)) ;
#99531 = CARTESIAN_POINT('Ctrl Pts',(41.8756534546012,263.669295346231,25.1185297823855)) ;
#99532 = CARTESIAN_POINT('Ctrl Pts',(41.8777828183738,263.6713612837,25.0693691759817)) ;
#99533 = CARTESIAN_POINT('Ctrl Pts',(41.877749617714,263.673464688334,25.0201877534197)) ;
#99534 = CARTESIAN_POINT('Origin',(40.2,265.,25.0213203435596)) ;
#99535 = CARTESIAN_POINT('',(41.0856881582581,263.,23.2689252008131)) ;
#99536 = CARTESIAN_POINT('',(39.3481027319431,263.,23.2522518613699)) ;
#99537 = CARTESIAN_POINT('Origin',(40.2,263.,25.0213203435596)) ;
#99538 = CARTESIAN_POINT('',(42.1628844781328,263.339287097289,25.0223486673506)) ;
#99539 = CARTESIAN_POINT('Ctrl Pts',(39.348102731943,263.,23.2522518613699)) ;
#99540 = CARTESIAN_POINT('Ctrl Pts',(38.7751369603565,263.025773545707,23.5281642867049)) ;
#99541 = CARTESIAN_POINT('Ctrl Pts',(37.9268112410175,263.077320637123,24.675932748524)) ;
#99542 = CARTESIAN_POINT('Ctrl Pts',(38.6316894750799,263.154641274244,26.7065505405601)) ;
#99543 = CARTESIAN_POINT('Ctrl Pts',(40.7072375606281,263.231961911367,27.2656011310219)) ;
#99544 = CARTESIAN_POINT('Ctrl Pts',(42.0063554939681,263.293510420748,26.1536188564997)) ;
#99545 = CARTESIAN_POINT('Ctrl Pts',(42.162562288311,263.329285384422,25.2698356603774)) ;
#99546 = CARTESIAN_POINT('Ctrl Pts',(42.1613953394505,263.339286802389,25.0223551866513)) ;
#99547 = CARTESIAN_POINT('',(42.1634995804015,263.839287219101,25.0200366912556)) ;
#99548 = CARTESIAN_POINT('Ctrl Pts',(42.163499732132,263.33928721913,25.0223459738299)) ;
#99549 = CARTESIAN_POINT('Ctrl Pts',(42.1635362473516,263.342109303692,24.9524400574562)) ;
#99550 = CARTESIAN_POINT('Ctrl Pts',(42.1598351621169,263.344931388255,24.8825285938161)) ;
#99551 = CARTESIAN_POINT('Ctrl Pts',(42.1524211029045,263.347753472817,24.813031873084)) ;
#99552 = CARTESIAN_POINT('Ctrl Pts',(42.1450052456119,263.3505762418,24.7435182977953)) ;
#99553 = CARTESIAN_POINT('Ctrl Pts',(42.1338746772063,263.353399010783,24.6744201360336)) ;
#99554 = CARTESIAN_POINT('Ctrl Pts',(42.1191057347347,263.356221779765,24.6061511865783)) ;
#99555 = CARTESIAN_POINT('Ctrl Pts',(42.1043178721143,263.359048164932,24.5377947793598)) ;
#99556 = CARTESIAN_POINT('Ctrl Pts',(42.0858824313739,263.361874550098,24.4702701689134)) ;
#99557 = CARTESIAN_POINT('Ctrl Pts',(42.0639264623263,263.364700935265,24.4039789525613)) ;
#99558 = CARTESIAN_POINT('Ctrl Pts',(42.0419552698865,263.367529280134,24.3376417725266)) ;
#99559 = CARTESIAN_POINT('Ctrl Pts',(42.0164588603084,263.370357625003,24.2725401310562)) ;
#99560 = CARTESIAN_POINT('Ctrl Pts',(41.9876125998093,263.373185969872,24.2090559512568)) ;
#99561 = CARTESIAN_POINT('Ctrl Pts',(41.9587122895671,263.376019614261,24.1454528200388)) ;
#99562 = CARTESIAN_POINT('Ctrl Pts',(41.9264498115641,263.378853258649,24.0834736237973)) ;
#99563 = CARTESIAN_POINT('Ctrl Pts',(41.8910464155505,263.381686903038,24.0234755307486)) ;
#99564 = CARTESIAN_POINT('Ctrl Pts',(41.8705718281761,263.383325663896,23.9887772719162)) ;
#99565 = CARTESIAN_POINT('Ctrl Pts',(41.8490475534782,263.384964424753,23.9547410743326)) ;
#99566 = CARTESIAN_POINT('Ctrl Pts',(41.8265226751408,263.386603185611,23.9214311503893)) ;
#99567 = CARTESIAN_POINT('Ctrl Pts',(41.7879759924163,263.389407586767,23.864428086906)) ;
#99568 = CARTESIAN_POINT('Ctrl Pts',(41.7463588283396,263.392211987923,23.8093498190784)) ;
#99569 = CARTESIAN_POINT('Ctrl Pts',(41.7018899125791,263.395016389079,23.7565441022848)) ;
#99570 = CARTESIAN_POINT('Ctrl Pts',(41.6563626815685,263.397887532148,23.7024816628026)) ;
#99571 = CARTESIAN_POINT('Ctrl Pts',(41.6078464321662,263.400758675217,23.6508018081332)) ;
#99572 = CARTESIAN_POINT('Ctrl Pts',(41.5566234581295,263.403629818285,23.6018468345243)) ;
#99573 = CARTESIAN_POINT('Ctrl Pts',(41.5067181249024,263.406427105134,23.5541511605222)) ;
#99574 = CARTESIAN_POINT('Ctrl Pts',(41.4542440248292,263.409224391982,23.5090422217917)) ;
#99575 = CARTESIAN_POINT('Ctrl Pts',(41.3995018974631,263.41202167883,23.4668019461186)) ;
#99576 = CARTESIAN_POINT('Ctrl Pts',(41.3447906972838,263.414817385319,23.4245855345692)) ;
#99577 = CARTESIAN_POINT('Ctrl Pts',(41.2878143977758,263.417613091809,23.3852348670235)) ;
#99578 = CARTESIAN_POINT('Ctrl Pts',(41.2289072353883,263.420408798298,23.3489919813754)) ;
#99579 = CARTESIAN_POINT('Ctrl Pts',(41.1700136034318,263.423203862639,23.3127574203833)) ;
#99580 = CARTESIAN_POINT('Ctrl Pts',(41.1091904045308,263.42599892698,23.2796294785647)) ;
#99581 = CARTESIAN_POINT('Ctrl Pts',(41.0467998285495,263.428793991322,23.2498062170654)) ;
#99582 = CARTESIAN_POINT('Ctrl Pts',(40.9814533776778,263.431721477273,23.2185700205446)) ;
#99583 = CARTESIAN_POINT('Ctrl Pts',(40.914387846715,263.434648963224,23.1909597090943)) ;
#99584 = CARTESIAN_POINT('Ctrl Pts',(40.8460448913382,263.437576449175,23.1671471455072)) ;
#99585 = CARTESIAN_POINT('Ctrl Pts',(40.7807177996198,263.440374749924,23.1443853916889)) ;
#99586 = CARTESIAN_POINT('Ctrl Pts',(40.7142241584067,263.443173050673,23.1250933492162)) ;
#99587 = CARTESIAN_POINT('Ctrl Pts',(40.6469648055212,263.445971351422,23.1093698440368)) ;
#99588 = CARTESIAN_POINT('Ctrl Pts',(40.5796621742535,263.448771452752,23.0936362214859)) ;
#99589 = CARTESIAN_POINT('Ctrl Pts',(40.5115933301378,263.451571554082,23.0814757916915)) ;
#99590 = CARTESIAN_POINT('Ctrl Pts',(40.4431673895009,263.454371655413,23.0729359177639)) ;
#99591 = CARTESIAN_POINT('Ctrl Pts',(40.3746364793251,263.457176052268,23.0643829431522)) ;
#99592 = CARTESIAN_POINT('Ctrl Pts',(40.3057478649224,263.459980449123,23.0594616363704)) ;
#99593 = CARTESIAN_POINT('Ctrl Pts',(40.2369127523885,263.462784845979,23.0581673442467)) ;
#99594 = CARTESIAN_POINT('Ctrl Pts',(40.227593862907,263.463164504897,23.0579921231305)) ;
#99595 = CARTESIAN_POINT('Ctrl Pts',(40.218275947807,263.463544163815,23.0578832989745)) ;
#99596 = CARTESIAN_POINT('Ctrl Pts',(40.2089600200415,263.463923822733,23.0578407872512)) ;
#99597 = CARTESIAN_POINT('Ctrl Pts',(40.1401422296188,263.466728405221,23.0575267484422)) ;
#99598 = CARTESIAN_POINT('Ctrl Pts',(40.0711826945288,263.469532987708,23.0608344362365)) ;
#99599 = CARTESIAN_POINT('Ctrl Pts',(40.0024920059422,263.472337570195,23.0677792402594)) ;
#99600 = CARTESIAN_POINT('Ctrl Pts',(39.9321716504675,263.475208690598,23.0748888077662)) ;
#99601 = CARTESIAN_POINT('Ctrl Pts',(39.8621335750225,263.478079811,23.0858103715288)) ;
#99602 = CARTESIAN_POINT('Ctrl Pts',(39.7928195976218,263.480950931403,23.1005037542104)) ;
#99603 = CARTESIAN_POINT('Ctrl Pts',(39.7252832136191,263.483748420413,23.1148203173669)) ;
#99604 = CARTESIAN_POINT('Ctrl Pts',(39.6584347405197,263.486545909423,23.1327174457885)) ;
#99605 = CARTESIAN_POINT('Ctrl Pts',(39.5926766314393,263.489343398433,23.1541056863763)) ;
#99606 = CARTESIAN_POINT('Ctrl Pts',(39.5269555016547,263.492139314266,23.1754818992144)) ;
#99607 = CARTESIAN_POINT('Ctrl Pts',(39.4623239815948,263.494935230098,23.2003451777175)) ;
#99608 = CARTESIAN_POINT('Ctrl Pts',(39.399170461448,263.497731145931,23.2285559139195)) ;
#99609 = CARTESIAN_POINT('Ctrl Pts',(39.33603129128,263.500526426465,23.2567602399728)) ;
#99610 = CARTESIAN_POINT('Ctrl Pts',(39.2743698986226,263.503321706999,23.2883103140755)) ;
#99611 = CARTESIAN_POINT('Ctrl Pts',(39.214554111061,263.506116987533,23.3230186477549)) ;
#99612 = CARTESIAN_POINT('Ctrl Pts',(39.1519134864944,263.509044276893,23.3593661036352)) ;
#99613 = CARTESIAN_POINT('Ctrl Pts',(39.0912976294582,263.511971566254,23.3991772600749)) ;
#99614 = CARTESIAN_POINT('Ctrl Pts',(39.0330973689343,263.514898855614,23.4421843457393)) ;
#99615 = CARTESIAN_POINT('Ctrl Pts',(38.9774570625523,263.517697387363,23.483299753152)) ;
#99616 = CARTESIAN_POINT('Ctrl Pts',(38.9240246650862,263.520495919112,23.5273354697586)) ;
#99617 = CARTESIAN_POINT('Ctrl Pts',(38.8731078398971,263.52329445086,23.5740161442092)) ;
#99618 = CARTESIAN_POINT('Ctrl Pts',(38.8221581649257,263.526094788126,23.6207269354234)) ;
#99619 = CARTESIAN_POINT('Ctrl Pts',(38.7737276331946,263.528895125391,23.6700857330352)) ;
#99620 = CARTESIAN_POINT('Ctrl Pts',(38.7280860730949,263.531695462656,23.7217813323011)) ;
#99621 = CARTESIAN_POINT('Ctrl Pts',(38.6823744142712,263.534500100827,23.7735563284048)) ;
#99622 = CARTESIAN_POINT('Ctrl Pts',(38.6394605720532,263.537304738999,23.827674903296)) ;
#99623 = CARTESIAN_POINT('Ctrl Pts',(38.5995725942992,263.54010937717,23.8837947969974)) ;
#99624 = CARTESIAN_POINT('Ctrl Pts',(38.5941914898415,263.540487738065,23.8913656749201)) ;
#99625 = CARTESIAN_POINT('Ctrl Pts',(38.5888653871444,263.54086609896,23.8989729372313)) ;
#99626 = CARTESIAN_POINT('Ctrl Pts',(38.5835947824051,263.541244459855,23.9066157088999)) ;
#99627 = CARTESIAN_POINT('Ctrl Pts',(38.544533355046,263.544048562487,23.9632577044803)) ;
#99628 = CARTESIAN_POINT('Ctrl Pts',(38.5083813890949,263.546852665118,24.0220588127175)) ;
#99629 = CARTESIAN_POINT('Ctrl Pts',(38.4753831864564,263.54965676775,24.082688841615)) ;
#99630 = CARTESIAN_POINT('Ctrl Pts',(38.4415956242334,263.552527948134,24.1447692190344)) ;
#99631 = CARTESIAN_POINT('Ctrl Pts',(38.4111150222394,263.555399128519,24.2087667739603)) ;
#99632 = CARTESIAN_POINT('Ctrl Pts',(38.3841575439488,263.558270308903,24.2742939552694)) ;
#99633 = CARTESIAN_POINT('Ctrl Pts',(38.357896670289,263.561067295495,24.3381278573537)) ;
#99634 = CARTESIAN_POINT('Ctrl Pts',(38.3349792331306,263.563864282087,24.4034128045607)) ;
#99635 = CARTESIAN_POINT('Ctrl Pts',(38.3155583761305,263.566661268679,24.4697661610644)) ;
#99636 = CARTESIAN_POINT('Ctrl Pts',(38.2961484904738,263.569456675181,24.5360820328444)) ;
#99637 = CARTESIAN_POINT('Ctrl Pts',(38.2802314017094,263.572252081683,24.6034646491454)) ;
#99638 = CARTESIAN_POINT('Ctrl Pts',(38.2679109095461,263.575047488185,24.6715146881605)) ;
#99639 = CARTESIAN_POINT('Ctrl Pts',(38.2555932439884,263.577842253356,24.7395491149247)) ;
#99640 = CARTESIAN_POINT('Ctrl Pts',(38.2468706227258,263.580637018527,24.8082501807261)) ;
#99641 = CARTESIAN_POINT('Ctrl Pts',(38.2417957115764,263.583431783699,24.8772085300274)) ;
#99642 = CARTESIAN_POINT('Ctrl Pts',(38.2364792707681,263.586359559805,24.9494488060664)) ;
#99643 = CARTESIAN_POINT('Ctrl Pts',(38.2351665055819,263.589287335912,25.0219708914576)) ;
#99644 = CARTESIAN_POINT('Ctrl Pts',(38.2378567528721,263.592215112018,25.0943006679643)) ;
#99645 = CARTESIAN_POINT('Ctrl Pts',(38.2404277594407,263.595013119335,25.1634245478339)) ;
#99646 = CARTESIAN_POINT('Ctrl Pts',(38.2466543233326,263.597811126652,25.2323723027269)) ;
#99647 = CARTESIAN_POINT('Ctrl Pts',(38.2564826038358,263.600609133968,25.3007346968185)) ;
#99648 = CARTESIAN_POINT('Ctrl Pts',(38.2663172171149,263.603408944159,25.369141139686)) ;
#99649 = CARTESIAN_POINT('Ctrl Pts',(38.2797580709152,263.60620875435,25.4369609933185)) ;
#99650 = CARTESIAN_POINT('Ctrl Pts',(38.2967003789648,263.609008564541,25.5037960450898)) ;
#99651 = CARTESIAN_POINT('Ctrl Pts',(38.3136687125046,263.611812675588,25.5707337638051)) ;
#99652 = CARTESIAN_POINT('Ctrl Pts',(38.3341490833733,263.614616786635,25.6366831992214)) ;
#99653 = CARTESIAN_POINT('Ctrl Pts',(38.3579874974153,263.617420897682,25.7012631281538)) ;
#99654 = CARTESIAN_POINT('Ctrl Pts',(38.361229867408,263.617802297447,25.710046934968)) ;
#99655 = CARTESIAN_POINT('Ctrl Pts',(38.3645342900422,263.618183697212,25.7188054404344)) ;
#99656 = CARTESIAN_POINT('Ctrl Pts',(38.367900311567,263.618565096977,25.727537719191)) ;
#99657 = CARTESIAN_POINT('Ctrl Pts',(38.3926496156565,263.621369410229,25.791743435272)) ;
#99658 = CARTESIAN_POINT('Ctrl Pts',(38.4208232163479,263.62417372348,25.8547637149043)) ;
#99659 = CARTESIAN_POINT('Ctrl Pts',(38.4522861380892,263.626978036731,25.9162105641369)) ;
#99660 = CARTESIAN_POINT('Ctrl Pts',(38.4844989785645,263.629849190788,25.9791219990097)) ;
#99661 = CARTESIAN_POINT('Ctrl Pts',(38.5201598569172,263.632720344845,26.040383521597)) ;
#99662 = CARTESIAN_POINT('Ctrl Pts',(38.5590706117971,263.635591498902,26.0995981338029)) ;
#99663 = CARTESIAN_POINT('Ctrl Pts',(38.5969791725281,263.63838870287,26.1572876011469)) ;
#99664 = CARTESIAN_POINT('Ctrl Pts',(38.6379719273339,263.641185906837,26.2130338976945)) ;
#99665 = CARTESIAN_POINT('Ctrl Pts',(38.6818191935624,263.643983110805,26.2664947445832)) ;
#99666 = CARTESIAN_POINT('Ctrl Pts',(38.7256417206521,263.646778736558,26.3199254282388)) ;
#99667 = CARTESIAN_POINT('Ctrl Pts',(38.7723152545264,263.649574362311,26.3710728450201)) ;
#99668 = CARTESIAN_POINT('Ctrl Pts',(38.8215685088218,263.652369988063,26.4196260591055)) ;
#99669 = CARTESIAN_POINT('Ctrl Pts',(38.870810490521,263.655164973981,26.4681681608129)) ;
#99670 = CARTESIAN_POINT('Ctrl Pts',(38.922630672812,263.657959959898,26.5141168972352)) ;
#99671 = CARTESIAN_POINT('Ctrl Pts',(38.9767206494171,263.660754945816,26.5571979039261)) ;
#99672 = CARTESIAN_POINT('Ctrl Pts',(39.0333763766254,263.663682511506,26.602322452246)) ;
#99673 = CARTESIAN_POINT('Ctrl Pts',(39.0925221659636,263.666610077197,26.6443000437003)) ;
#99674 = CARTESIAN_POINT('Ctrl Pts',(39.1537662292884,263.669537642887,26.6828639472675)) ;
#99675 = CARTESIAN_POINT('Ctrl Pts',(39.21230460047,263.672335872099,26.7197241420141)) ;
#99676 = CARTESIAN_POINT('Ctrl Pts',(39.2727592794513,263.67513410131,26.7534657211203)) ;
#99677 = CARTESIAN_POINT('Ctrl Pts',(39.3347619023668,263.677932330522,26.783902337228)) ;
#99678 = CARTESIAN_POINT('Ctrl Pts',(39.3968044771535,263.680732362794,26.8143585654055)) ;
#99679 = CARTESIAN_POINT('Ctrl Pts',(39.4603965330109,263.683532395067,26.8415054011816)) ;
#99680 = CARTESIAN_POINT('Ctrl Pts',(39.5251500779897,263.686332427339,26.865204784831)) ;
#99681 = CARTESIAN_POINT('Ctrl Pts',(39.5900030547217,263.689136759177,26.8889405598666)) ;
#99682 = CARTESIAN_POINT('Ctrl Pts',(39.6560206129491,263.691941091015,26.9092181821856)) ;
#99683 = CARTESIAN_POINT('Ctrl Pts',(39.7228010388372,263.694745422853,26.9259498092209)) ;
#99684 = CARTESIAN_POINT('Ctrl Pts',(39.7318525675763,263.695125526602,26.9282176414629)) ;
#99685 = CARTESIAN_POINT('Ctrl Pts',(39.740918099865,263.695505630351,26.9304204058221)) ;
#99686 = CARTESIAN_POINT('Ctrl Pts',(39.7499966261111,263.695885734099,26.9325579565969)) ;
#99687 = CARTESIAN_POINT('Ctrl Pts',(39.8169755789748,263.698690038497,26.9483282378862)) ;
#99688 = CARTESIAN_POINT('Ctrl Pts',(39.8849066936081,263.701494342894,26.9606021865827)) ;
#99689 = CARTESIAN_POINT('Ctrl Pts',(39.9533934422283,263.704298647291,26.9692724619814)) ;
#99690 = CARTESIAN_POINT('Ctrl Pts',(40.0235128209001,263.707169802455,26.9781494248409)) ;
#99691 = CARTESIAN_POINT('Ctrl Pts',(40.0942141853674,263.710040957619,26.9832484865268)) ;
#99692 = CARTESIAN_POINT('Ctrl Pts',(40.1650579347143,263.712912112783,26.9845094078307)) ;
#99693 = CARTESIAN_POINT('Ctrl Pts',(40.2340767988411,263.715709309006,26.9857378486875)) ;
#99694 = CARTESIAN_POINT('Ctrl Pts',(40.3032302807727,263.71850650523,26.983323498587)) ;
#99695 = CARTESIAN_POINT('Ctrl Pts',(40.3721061957367,263.721303701453,26.9772630082073)) ;
#99696 = CARTESIAN_POINT('Ctrl Pts',(40.4409432607295,263.724099319898,26.9712059362922)) ;
#99697 = CARTESIAN_POINT('Ctrl Pts',(40.5095025848152,263.726894938342,26.9615068481037)) ;
#99698 = CARTESIAN_POINT('Ctrl Pts',(40.5773744049012,263.729690556786,26.9482144269294)) ;
#99699 = CARTESIAN_POINT('Ctrl Pts',(40.6452307020316,263.732485535845,26.934925045863)) ;
#99700 = CARTESIAN_POINT('Ctrl Pts',(40.7123993293839,263.735280514903,26.9180440580058)) ;
#99701 = CARTESIAN_POINT('Ctrl Pts',(40.7784797918224,263.738075493962,26.8976714249016)) ;
#99702 = CARTESIAN_POINT('Ctrl Pts',(40.8476951170664,263.741003067067,26.8763323123356)) ;
#99703 = CARTESIAN_POINT('Ctrl Pts',(40.9157158954227,263.743930640172,26.8511621496684)) ;
#99704 = CARTESIAN_POINT('Ctrl Pts',(40.9821009073791,263.746858213277,26.8223340638507)) ;
#99705 = CARTESIAN_POINT('Ctrl Pts',(41.0455528173557,263.749656436846,26.7947796949925)) ;
#99706 = CARTESIAN_POINT('Ctrl Pts',(41.1075100309649,263.752454660415,26.7638841087761)) ;
#99707 = CARTESIAN_POINT('Ctrl Pts',(41.1676109269251,263.755252883985,26.7298464171374)) ;
#99708 = CARTESIAN_POINT('Ctrl Pts',(41.2277505586288,263.758052911043,26.6957867878009)) ;
#99709 = CARTESIAN_POINT('Ctrl Pts',(41.2860310811265,263.7608529381,26.6585812847864)) ;
#99710 = CARTESIAN_POINT('Ctrl Pts',(41.3421196810525,263.763652965158,26.6184724603451)) ;
#99711 = CARTESIAN_POINT('Ctrl Pts',(41.3982944203982,263.766457292425,26.5783020378097)) ;
#99712 = CARTESIAN_POINT('Ctrl Pts',(41.4522701434347,263.769261619692,26.5352197043128)) ;
#99713 = CARTESIAN_POINT('Ctrl Pts',(41.5037477688255,263.772065946958,26.489507663108)) ;
#99714 = CARTESIAN_POINT('Ctrl Pts',(41.5107258337244,263.772446088379,26.483311153697)) ;
#99715 = CARTESIAN_POINT('Ctrl Pts',(41.5176580530097,263.7728262298,26.4770663759933)) ;
#99716 = CARTESIAN_POINT('Ctrl Pts',(41.5245437368096,263.773206371221,26.4707740817929)) ;
#99717 = CARTESIAN_POINT('Ctrl Pts',(41.57461281309,263.775970559987,26.4250198230361)) ;
#99718 = CARTESIAN_POINT('Ctrl Pts',(41.6224125805603,263.778734748753,26.3765726870436)) ;
#99719 = CARTESIAN_POINT('Ctrl Pts',(41.6676353975584,263.781498937519,26.3256893825335)) ;
#99720 = CARTESIAN_POINT('Ctrl Pts',(41.712801126539,263.78425963685,26.2748703116817)) ;
#99721 = CARTESIAN_POINT('Ctrl Pts',(41.7553960200713,263.787020336182,26.2216215386591)) ;
#99722 = CARTESIAN_POINT('Ctrl Pts',(41.7951474334239,263.789781035513,26.1662382077058)) ;
#99723 = CARTESIAN_POINT('Ctrl Pts',(41.8348629859507,263.792539244343,26.1109048395543)) ;
#99724 = CARTESIAN_POINT('Ctrl Pts',(41.8717398514875,263.795297453173,26.053441137395)) ;
#99725 = CARTESIAN_POINT('Ctrl Pts',(41.9055453353879,263.798055662003,25.9941756046013)) ;
#99726 = CARTESIAN_POINT('Ctrl Pts',(41.9393324965953,263.800812375874,25.9349421939379)) ;
#99727 = CARTESIAN_POINT('Ctrl Pts',(41.9700513297317,263.803569089744,25.8739093259822)) ;
#99728 = CARTESIAN_POINT('Ctrl Pts',(41.997513287225,263.806325803615,25.8114331407283)) ;
#99729 = CARTESIAN_POINT('Ctrl Pts',(42.0249844738963,263.809083443939,25.7489359590164)) ;
#99730 = CARTESIAN_POINT('Ctrl Pts',(42.0491963823633,263.811841084262,25.6849949460299)) ;
#99731 = CARTESIAN_POINT('Ctrl Pts',(42.0700077617375,263.814598724586,25.6199882156234)) ;
#99732 = CARTESIAN_POINT('Ctrl Pts',(42.0908213077346,263.817356652001,25.554974717522)) ;
#99733 = CARTESIAN_POINT('Ctrl Pts',(42.1082334793487,263.820114579415,25.4888957648959)) ;
#99734 = CARTESIAN_POINT('Ctrl Pts',(42.122153100212,263.82287250683,25.4221441319574)) ;
#99735 = CARTESIAN_POINT('Ctrl Pts',(42.1360919737274,263.825634248818,25.3553001727996)) ;
#99736 = CARTESIAN_POINT('Ctrl Pts',(42.1465285576744,263.828395990807,25.2877821713475)) ;
#99737 = CARTESIAN_POINT('Ctrl Pts',(42.1534231331806,263.831157732795,25.2199917122938)) ;
#99738 = CARTESIAN_POINT('Ctrl Pts',(42.1601881094651,263.833867561564,25.1534755290423)) ;
#99739 = CARTESIAN_POINT('Ctrl Pts',(42.1635431603993,263.836577390332,25.0866975052807)) ;
#99740 = CARTESIAN_POINT('Ctrl Pts',(42.1634995804015,263.839287219101,25.0200366912556)) ;
#99741 = CARTESIAN_POINT('',(42.1634995162458,264.339287219108,25.0226986405015)) ;
#99742 = CARTESIAN_POINT('Ctrl Pts',(42.163499580401,263.83928721913,25.0200366905463)) ;
#99743 = CARTESIAN_POINT('Ctrl Pts',(42.1634393268694,263.843033815535,24.9278717652068)) ;
#99744 = CARTESIAN_POINT('Ctrl Pts',(42.1568885505834,263.846780411939,24.8359264198449)) ;
#99745 = CARTESIAN_POINT('Ctrl Pts',(42.1439469198114,263.850527008343,24.7449100996181)) ;
#99746 = CARTESIAN_POINT('Ctrl Pts',(42.1342602498124,263.853331295038,24.6767853729825)) ;
#99747 = CARTESIAN_POINT('Ctrl Pts',(42.1209705345478,263.856135581733,24.609046166368)) ;
#99748 = CARTESIAN_POINT('Ctrl Pts',(42.1041220948803,263.858939868429,24.5421008763124)) ;
#99749 = CARTESIAN_POINT('Ctrl Pts',(42.0868718893598,263.861811025805,24.4735592169732)) ;
#99750 = CARTESIAN_POINT('Ctrl Pts',(42.0658910379676,263.864682183181,24.405850346248)) ;
#99751 = CARTESIAN_POINT('Ctrl Pts',(42.0412834107829,263.867553340558,24.339405648619)) ;
#99752 = CARTESIAN_POINT('Ctrl Pts',(42.0173098391839,263.870350517889,24.2746730068238)) ;
#99753 = CARTESIAN_POINT('Ctrl Pts',(41.9898943245674,263.87314769522,24.2111406620449)) ;
#99754 = CARTESIAN_POINT('Ctrl Pts',(41.9591837468858,263.875944872551,24.1491937502872)) ;
#99755 = CARTESIAN_POINT('Ctrl Pts',(41.9284904961072,263.878740471716,24.0872817889672)) ;
#99756 = CARTESIAN_POINT('Ctrl Pts',(41.8945060876673,263.88153607088,24.0269539214354)) ;
#99757 = CARTESIAN_POINT('Ctrl Pts',(41.8574249850417,263.884331670045,23.9685740925762)) ;
#99758 = CARTESIAN_POINT('Ctrl Pts',(41.8203523679988,263.887126629468,23.9102076232677)) ;
#99759 = CARTESIAN_POINT('Ctrl Pts',(41.7801847257056,263.889921588892,23.8537887183574)) ;
#99760 = CARTESIAN_POINT('Ctrl Pts',(41.7371609110175,263.892716548316,23.7996540292005)) ;
#99761 = CARTESIAN_POINT('Ctrl Pts',(41.6920954442125,263.895644139745,23.7429504324857)) ;
#99762 = CARTESIAN_POINT('Ctrl Pts',(41.6438963087687,263.898571731175,23.6887537205247)) ;
#99763 = CARTESIAN_POINT('Ctrl Pts',(41.5928853393019,263.901499322604,23.6374118633638)) ;
#99764 = CARTESIAN_POINT('Ctrl Pts',(41.5441288563539,263.904297525875,23.5883391166714)) ;
#99765 = CARTESIAN_POINT('Ctrl Pts',(41.4928042619471,263.907095729145,23.541874496461)) ;
#99766 = CARTESIAN_POINT('Ctrl Pts',(41.4392286140248,263.909893932416,23.4982823623582)) ;
#99767 = CARTESIAN_POINT('Ctrl Pts',(41.3856184397523,263.912693938964,23.4546621356919)) ;
#99768 = CARTESIAN_POINT('Ctrl Pts',(41.3297547183872,263.915493945512,23.413918366189)) ;
#99769 = CARTESIAN_POINT('Ctrl Pts',(41.2719844854997,263.91829395206,23.3762727719533)) ;
#99770 = CARTESIAN_POINT('Ctrl Pts',(41.2141255331622,263.92109825866,23.3385693642685)) ;
#99771 = CARTESIAN_POINT('Ctrl Pts',(41.1543546506205,263.92390256526,23.3039738647254)) ;
#99772 = CARTESIAN_POINT('Ctrl Pts',(41.0930435295117,263.926706871861,23.2726621424244)) ;
#99773 = CARTESIAN_POINT('Ctrl Pts',(41.0847298749895,263.92708712973,23.2684163410593)) ;
#99774 = CARTESIAN_POINT('Ctrl Pts',(41.0763879291037,263.927467387599,23.2642308447549)) ;
#99775 = CARTESIAN_POINT('Ctrl Pts',(41.0680186440471,263.927847645467,23.2601060228176)) ;
#99776 = CARTESIAN_POINT('Ctrl Pts',(41.0062977660224,263.930651929153,23.2296867420853)) ;
#99777 = CARTESIAN_POINT('Ctrl Pts',(40.9428633334637,263.933456212838,23.2024603023848)) ;
#99778 = CARTESIAN_POINT('Ctrl Pts',(40.8780775986114,263.936260496523,23.1786204167507)) ;
#99779 = CARTESIAN_POINT('Ctrl Pts',(40.8117469110722,263.939131654276,23.1542120186896)) ;
#99780 = CARTESIAN_POINT('Ctrl Pts',(40.744000064422,263.942002812029,23.1333540793622)) ;
#99781 = CARTESIAN_POINT('Ctrl Pts',(40.675251878674,263.944873969781,23.1162040999102)) ;
#99782 = CARTESIAN_POINT('Ctrl Pts',(40.6082751827735,263.947671144101,23.0994960377853)) ;
#99783 = CARTESIAN_POINT('Ctrl Pts',(40.5403486362851,263.950468318421,23.0863072672656)) ;
#99784 = CARTESIAN_POINT('Ctrl Pts',(40.4718731205651,263.95326549274,23.0767336891998)) ;
#99785 = CARTESIAN_POINT('Ctrl Pts',(40.4034362385558,263.956061088901,23.0671655125223)) ;
#99786 = CARTESIAN_POINT('Ctrl Pts',(40.3344514837967,263.958856685062,23.0612085479421)) ;
#99787 = CARTESIAN_POINT('Ctrl Pts',(40.2653290723423,263.961652281223,23.0589074506375)) ;
#99788 = CARTESIAN_POINT('Ctrl Pts',(40.1962224784314,263.964447237657,23.0566068799017)) ;
#99789 = CARTESIAN_POINT('Ctrl Pts',(40.1269787773539,263.967242194091,23.0579605307881)) ;
#99790 = CARTESIAN_POINT('Ctrl Pts',(40.058010679081,263.970037150525,23.0629610091307)) ;
#99791 = CARTESIAN_POINT('Ctrl Pts',(39.9857696195808,263.972964744863,23.0681987909823)) ;
#99792 = CARTESIAN_POINT('Ctrl Pts',(39.9138315536871,263.975892339202,23.0774381490376)) ;
#99793 = CARTESIAN_POINT('Ctrl Pts',(39.8426653384802,263.97881993354,23.0906095444816)) ;
#99794 = CARTESIAN_POINT('Ctrl Pts',(39.7746445318474,263.981618133892,23.1031987898134)) ;
#99795 = CARTESIAN_POINT('Ctrl Pts',(39.7073292681962,263.984416334243,23.1193796467941)) ;
#99796 = CARTESIAN_POINT('Ctrl Pts',(39.6411166615528,263.987214534595,23.1390393698455)) ;
#99797 = CARTESIAN_POINT('Ctrl Pts',(39.5748613840908,263.990014538251,23.1587117626364)) ;
#99798 = CARTESIAN_POINT('Ctrl Pts',(39.5097106367583,263.992814541907,23.1818673202465)) ;
#99799 = CARTESIAN_POINT('Ctrl Pts',(39.4460432254316,263.995614545563,23.2083444937253)) ;
#99800 = CARTESIAN_POINT('Ctrl Pts',(39.3822780367358,263.998418849331,23.2348623295824)) ;
#99801 = CARTESIAN_POINT('Ctrl Pts',(39.3200011657801,264.001223153099,23.2647117450625)) ;
#99802 = CARTESIAN_POINT('Ctrl Pts',(39.2595674604394,264.004027456867,23.2976849736117)) ;
#99803 = CARTESIAN_POINT('Ctrl Pts',(39.2513723989487,264.004407732107,23.3021562803764)) ;
#99804 = CARTESIAN_POINT('Ctrl Pts',(39.2432111863563,264.004788007347,23.3066849645074)) ;
#99805 = CARTESIAN_POINT('Ctrl Pts',(39.2350846647403,264.005168282588,23.3112704478604)) ;
#99806 = CARTESIAN_POINT('Ctrl Pts',(39.1751568842898,264.007972563704,23.3450853877112)) ;
#99807 = CARTESIAN_POINT('Ctrl Pts',(39.1168994297693,264.01077684482,23.3821159857374)) ;
#99808 = CARTESIAN_POINT('Ctrl Pts',(39.0606765621799,264.013581125937,23.4221723347644)) ;
#99809 = CARTESIAN_POINT('Ctrl Pts',(39.0031128823909,264.01645228401,23.4631839541955)) ;
#99810 = CARTESIAN_POINT('Ctrl Pts',(38.9476825722119,264.019323442084,23.5073673238714)) ;
#99811 = CARTESIAN_POINT('Ctrl Pts',(38.8947496350886,264.022194600158,23.5544687031752)) ;
#99812 = CARTESIAN_POINT('Ctrl Pts',(38.8431807197224,264.024991771745,23.600356333353)) ;
#99813 = CARTESIAN_POINT('Ctrl Pts',(38.7939824046442,264.027788943331,23.6490130484392)) ;
#99814 = CARTESIAN_POINT('Ctrl Pts',(38.7474599613417,264.030586114918,23.7001618799019)) ;
#99815 = CARTESIAN_POINT('Ctrl Pts',(38.7009637667907,264.033381708293,23.7512818523263)) ;
#99816 = CARTESIAN_POINT('Ctrl Pts',(38.6571407752526,264.036177301668,23.804890790839)) ;
#99817 = CARTESIAN_POINT('Ctrl Pts',(38.6162592032904,264.038972895043,23.8606751183345)) ;
#99818 = CARTESIAN_POINT('Ctrl Pts',(38.5753869871292,264.041767848643,23.9164466795142)) ;
#99819 = CARTESIAN_POINT('Ctrl Pts',(38.5374551413506,264.044562802242,23.974392247734)) ;
#99820 = CARTESIAN_POINT('Ctrl Pts',(38.5026903060573,264.047357755842,24.0341668332846)) ;
#99821 = CARTESIAN_POINT('Ctrl Pts',(38.4662755952239,264.050285352831,24.09677821141)) ;
#99822 = CARTESIAN_POINT('Ctrl Pts',(38.4333363101176,264.05321294982,24.1613960540302)) ;
#99823 = CARTESIAN_POINT('Ctrl Pts',(38.4040794362206,264.056140546809,24.22759395582)) ;
#99824 = CARTESIAN_POINT('Ctrl Pts',(38.3761157138824,264.058938744238,24.2908659154811)) ;
#99825 = CARTESIAN_POINT('Ctrl Pts',(38.3515158675236,264.061736941667,24.3555807041219)) ;
#99826 = CARTESIAN_POINT('Ctrl Pts',(38.3304107415181,264.064535139096,24.4213467986687)) ;
#99827 = CARTESIAN_POINT('Ctrl Pts',(38.3092920144767,264.067335139802,24.4871552756684)) ;
#99828 = CARTESIAN_POINT('Ctrl Pts',(38.2916726140117,264.070135140508,24.5540159359703)) ;
#99829 = CARTESIAN_POINT('Ctrl Pts',(38.2776327573044,264.072935141214,24.6215248530763)) ;
#99830 = CARTESIAN_POINT('Ctrl Pts',(38.2635713389277,264.075739442012,24.6891374468065)) ;
#99831 = CARTESIAN_POINT('Ctrl Pts',(38.2531005018651,264.078543742811,24.7573998023813)) ;
#99832 = CARTESIAN_POINT('Ctrl Pts',(38.2462487852448,264.08134804361,24.8259017138375)) ;
#99833 = CARTESIAN_POINT('Ctrl Pts',(38.2453196219938,264.081728335644,24.8351912776466)) ;
#99834 = CARTESIAN_POINT('Ctrl Pts',(38.2444569364807,264.082108627677,24.8444852468057)) ;
#99835 = CARTESIAN_POINT('Ctrl Pts',(38.2436607261533,264.082488919711,24.8537825997379)) ;
#99836 = CARTESIAN_POINT('Ctrl Pts',(38.2377894554891,264.085293200669,24.9223414637035)) ;
#99837 = CARTESIAN_POINT('Ctrl Pts',(38.2355156869784,264.088097481628,24.991334410235)) ;
#99838 = CARTESIAN_POINT('Ctrl Pts',(38.2368880163663,264.090901762587,25.060353530899)) ;
#99839 = CARTESIAN_POINT('Ctrl Pts',(38.2382930733799,264.093772920681,25.1310186353642)) ;
#99840 = CARTESIAN_POINT('Ctrl Pts',(38.2435205047617,264.096644078774,25.2017106737457)) ;
#99841 = CARTESIAN_POINT('Ctrl Pts',(38.2525660465842,264.099515236868,25.271985951658)) ;
#99842 = CARTESIAN_POINT('Ctrl Pts',(38.2613784947858,264.102312408389,25.3404503132856)) ;
#99843 = CARTESIAN_POINT('Ctrl Pts',(38.2738145764158,264.10510957991,25.4085186194253)) ;
#99844 = CARTESIAN_POINT('Ctrl Pts',(38.2898177240288,264.107906751431,25.4757825780363)) ;
#99845 = CARTESIAN_POINT('Ctrl Pts',(38.3058118425898,264.110702344774,25.5430085860018)) ;
#99846 = CARTESIAN_POINT('Ctrl Pts',(38.3253689206372,264.113497938118,25.6094306737226)) ;
#99847 = CARTESIAN_POINT('Ctrl Pts',(38.3483812619677,264.116293531461,25.6746505043264)) ;
#99848 = CARTESIAN_POINT('Ctrl Pts',(38.3713883371747,264.119088485064,25.7398554100829)) ;
#99849 = CARTESIAN_POINT('Ctrl Pts',(38.397848942836,264.121883438666,25.8038581457887)) ;
#99850 = CARTESIAN_POINT('Ctrl Pts',(38.4276059949864,264.124678392269,25.8662769939221)) ;
#99851 = CARTESIAN_POINT('Ctrl Pts',(38.4587752630291,264.127605989316,25.9316581277304)) ;
#99852 = CARTESIAN_POINT('Ctrl Pts',(38.4935614451515,264.130533586363,25.9953007515779)) ;
#99853 = CARTESIAN_POINT('Ctrl Pts',(38.5317291392618,264.13346118341,26.0567934649934)) ;
#99854 = CARTESIAN_POINT('Ctrl Pts',(38.5682098246742,264.136259380927,26.1155682059243)) ;
#99855 = CARTESIAN_POINT('Ctrl Pts',(38.6077790592181,264.139057578443,26.1723786961002)) ;
#99856 = CARTESIAN_POINT('Ctrl Pts',(38.6501873075505,264.14185577596,26.2268960849888)) ;
#99857 = CARTESIAN_POINT('Ctrl Pts',(38.6926228859955,264.144655776783,26.2814486077589)) ;
#99858 = CARTESIAN_POINT('Ctrl Pts',(38.7379008005125,264.147455777606,26.333704720125)) ;
#99859 = CARTESIAN_POINT('Ctrl Pts',(38.7857327218907,264.150255778429,26.3833703852502)) ;
#99860 = CARTESIAN_POINT('Ctrl Pts',(38.8336381016924,264.153060079386,26.4331123249919)) ;
#99861 = CARTESIAN_POINT('Ctrl Pts',(38.8841049558928,264.155864380342,26.4802555512367)) ;
#99862 = CARTESIAN_POINT('Ctrl Pts',(38.9368106260223,264.158668681298,26.5245451622311)) ;
#99863 = CARTESIAN_POINT('Ctrl Pts',(38.9439580530727,264.159048973143,26.5305512857258)) ;
#99864 = CARTESIAN_POINT('Ctrl Pts',(38.9511466079102,264.159429264988,26.5365049955676)) ;
#99865 = CARTESIAN_POINT('Ctrl Pts',(38.9583754454666,264.159809556832,26.5424057177512)) ;
#99866 = CARTESIAN_POINT('Ctrl Pts',(39.0116811190239,264.162613840753,26.5859178271355)) ;
#99867 = CARTESIAN_POINT('Ctrl Pts',(39.067374064098,264.165418124673,26.6267038710569)) ;
#99868 = CARTESIAN_POINT('Ctrl Pts',(39.1251448299156,264.168222408594,26.6644936799252)) ;
#99869 = CARTESIAN_POINT('Ctrl Pts',(39.1842932560943,264.171093566317,26.70318466296)) ;
#99870 = CARTESIAN_POINT('Ctrl Pts',(39.2456195358669,264.173964724041,26.7387342754357)) ;
#99871 = CARTESIAN_POINT('Ctrl Pts',(39.3087548572949,264.176835881764,26.7708958193836)) ;
#99872 = CARTESIAN_POINT('Ctrl Pts',(39.3702633228545,264.179633056182,26.802228632356)) ;
#99873 = CARTESIAN_POINT('Ctrl Pts',(39.4334882579985,264.182430230599,26.8303456470777)) ;
#99874 = CARTESIAN_POINT('Ctrl Pts',(39.4980605888599,264.185227405017,26.855063322575)) ;
#99875 = CARTESIAN_POINT('Ctrl Pts',(39.5625964869995,264.188023001225,26.8797670519722)) ;
#99876 = CARTESIAN_POINT('Ctrl Pts',(39.6284778178391,264.190818597432,26.9010750743839)) ;
#99877 = CARTESIAN_POINT('Ctrl Pts',(39.6953148947306,264.19361419364,26.91885168573)) ;
#99878 = CARTESIAN_POINT('Ctrl Pts',(39.762136675821,264.19640915007,26.9366242288625)) ;
#99879 = CARTESIAN_POINT('Ctrl Pts',(39.8299132976171,264.1992041065,26.9508668411143)) ;
#99880 = CARTESIAN_POINT('Ctrl Pts',(39.898240945861,264.20199906293,26.9614939758011)) ;
#99881 = CARTESIAN_POINT('Ctrl Pts',(39.9698111600169,264.204926657182,26.9726254331971)) ;
#99882 = CARTESIAN_POINT('Ctrl Pts',(40.0419854358326,264.207854251434,26.9797895834628)) ;
#99883 = CARTESIAN_POINT('Ctrl Pts',(40.1142912819507,264.210781845686,26.982948816449)) ;
#99884 = CARTESIAN_POINT('Ctrl Pts',(40.1834013488205,264.213580045906,26.985968417417)) ;
#99885 = CARTESIAN_POINT('Ctrl Pts',(40.2526310910439,264.216378246127,26.9853297205025)) ;
#99886 = CARTESIAN_POINT('Ctrl Pts',(40.3215682148443,264.219176446347,26.9810533404598)) ;
#99887 = CARTESIAN_POINT('Ctrl Pts',(40.3905497642044,264.221976449828,26.9767742045642)) ;
#99888 = CARTESIAN_POINT('Ctrl Pts',(40.4592378360349,264.224776453309,26.9688527759086)) ;
#99889 = CARTESIAN_POINT('Ctrl Pts',(40.5272270083716,264.22757645679,26.957361338733)) ;
#99890 = CARTESIAN_POINT('Ctrl Pts',(40.5953205937682,264.230380760322,26.9458522538045)) ;
#99891 = CARTESIAN_POINT('Ctrl Pts',(40.6627126646325,264.233185063854,26.93076233205)) ;
#99892 = CARTESIAN_POINT('Ctrl Pts',(40.7290107572647,264.235989367386,26.9122142773111)) ;
#99893 = CARTESIAN_POINT('Ctrl Pts',(40.7380010614685,264.236369642909,26.9096990819583)) ;
#99894 = CARTESIAN_POINT('Ctrl Pts',(40.7469712774647,264.236749918432,26.9071203697556)) ;
#99895 = CARTESIAN_POINT('Ctrl Pts',(40.7559204547825,264.237130193955,26.9044785148119)) ;
#99896 = CARTESIAN_POINT('Ctrl Pts',(40.8219148662837,264.2399344807,26.8849965383031)) ;
#99897 = CARTESIAN_POINT('Ctrl Pts',(40.8870043490843,264.242738767445,26.8620057637231)) ;
#99898 = CARTESIAN_POINT('Ctrl Pts',(40.9507912798502,264.245543054191,26.835609378995)) ;
#99899 = CARTESIAN_POINT('Ctrl Pts',(41.0160992647417,264.248414211561,26.8085835498115)) ;
#99900 = CARTESIAN_POINT('Ctrl Pts',(41.0800412589882,264.251285368931,26.7779876613521)) ;
#99901 = CARTESIAN_POINT('Ctrl Pts',(41.1422055473778,264.254156526302,26.7439871588465)) ;
#99902 = CARTESIAN_POINT('Ctrl Pts',(41.2027680722295,264.256953703654,26.7108627343366)) ;
#99903 = CARTESIAN_POINT('Ctrl Pts',(41.2616429444815,264.259750881006,26.6745072863572)) ;
#99904 = CARTESIAN_POINT('Ctrl Pts',(41.3184704556731,264.262548058358,26.6351220940192)) ;
#99905 = CARTESIAN_POINT('Ctrl Pts',(41.3752659045721,264.265343657532,26.5957591229528)) ;
#99906 = CARTESIAN_POINT('Ctrl Pts',(41.4300158848789,264.268139256706,26.553370076931)) ;
#99907 = CARTESIAN_POINT('Ctrl Pts',(41.4823885679606,264.270934855881,26.508200234729)) ;
#99908 = CARTESIAN_POINT('Ctrl Pts',(41.5347492659552,264.273729815303,26.4630407292992)) ;
#99909 = CARTESIAN_POINT('Ctrl Pts',(41.5847333784703,264.276524774726,26.4151020100271)) ;
#99910 = CARTESIAN_POINT('Ctrl Pts',(41.6320425302669,264.279319734149,26.3646693084629)) ;
#99911 = CARTESIAN_POINT('Ctrl Pts',(41.6815966902733,264.28224732556,26.3118433737766)) ;
#99912 = CARTESIAN_POINT('Ctrl Pts',(41.7282152649853,264.28517491697,26.2562812576092)) ;
#99913 = CARTESIAN_POINT('Ctrl Pts',(41.771600737291,264.288102508381,26.1983519372505)) ;
#99914 = CARTESIAN_POINT('Ctrl Pts',(41.8130687402515,264.290900711624,26.1429828678253)) ;
#99915 = CARTESIAN_POINT('Ctrl Pts',(41.8515831623519,264.293698914866,26.0854518824881)) ;
#99916 = CARTESIAN_POINT('Ctrl Pts',(41.8869285156555,264.296497118109,26.0261110844943)) ;
#99917 = CARTESIAN_POINT('Ctrl Pts',(41.9222966468408,264.299297124619,25.9667320450475)) ;
#99918 = CARTESIAN_POINT('Ctrl Pts',(41.9544914180318,264.30209713113,25.9055413028085)) ;
#99919 = CARTESIAN_POINT('Ctrl Pts',(41.9833438858803,264.30489713764,25.8429144250216)) ;
#99920 = CARTESIAN_POINT('Ctrl Pts',(42.0122406631827,264.307701444191,25.7801913695777)) ;
#99921 = CARTESIAN_POINT('Ctrl Pts',(42.0377847202778,264.310505750741,25.716028231542)) ;
#99922 = CARTESIAN_POINT('Ctrl Pts',(42.0598560586647,264.313310057291,25.6508183110292)) ;
#99923 = CARTESIAN_POINT('Ctrl Pts',(42.0628488846162,264.31369031522,25.6419759862465)) ;
#99924 = CARTESIAN_POINT('Ctrl Pts',(42.0657779348491,264.314070573149,25.6331144322471)) ;
#99925 = CARTESIAN_POINT('Ctrl Pts',(42.0686429823233,264.314450831077,25.6242346447783)) ;
#99926 = CARTESIAN_POINT('Ctrl Pts',(42.0934907007119,264.317748696824,25.5472228464186)) ;
#99927 = CARTESIAN_POINT('Ctrl Pts',(42.1135932196859,264.321046562571,25.4686126575969)) ;
#99928 = CARTESIAN_POINT('Ctrl Pts',(42.1287775563013,264.324344428318,25.3889470405068)) ;
#99929 = CARTESIAN_POINT('Ctrl Pts',(42.1438184949957,264.327611149663,25.3100337700062)) ;
#99930 = CARTESIAN_POINT('Ctrl Pts',(42.1540336338479,264.330877871007,25.2300850204659)) ;
#99931 = CARTESIAN_POINT('Ctrl Pts',(42.1593019886856,264.334144592351,25.1496479210032)) ;
#99932 = CARTESIAN_POINT('Ctrl Pts',(42.1620665528768,264.33585880127,25.1074386295516)) ;
#99933 = CARTESIAN_POINT('Ctrl Pts',(42.1634697555966,264.337573010189,25.0650951796944)) ;
#99934 = CARTESIAN_POINT('Ctrl Pts',(42.1634995162458,264.339287219108,25.0226986405015)) ;
#99935 = CARTESIAN_POINT('',(42.1634993456137,264.839287219109,25.0197172919184)) ;
#99936 = CARTESIAN_POINT('Ctrl Pts',(42.1634995162462,264.33928721913,25.0226986399458)) ;
#99937 = CARTESIAN_POINT('Ctrl Pts',(42.1635479241927,264.342075510692,24.9537374350528)) ;
#99938 = CARTESIAN_POINT('Ctrl Pts',(42.1599589781167,264.344863802254,24.8847297879806)) ;
#99939 = CARTESIAN_POINT('Ctrl Pts',(42.1527445781668,264.347652093816,24.8160866659132)) ;
#99940 = CARTESIAN_POINT('Ctrl Pts',(42.1455318298709,264.350439747031,24.7474592589009)) ;
#99941 = CARTESIAN_POINT('Ctrl Pts',(42.1346953272965,264.353227400245,24.6791966981854)) ;
#99942 = CARTESIAN_POINT('Ctrl Pts',(42.1202988718974,264.35601505346,24.6117052894058)) ;
#99943 = CARTESIAN_POINT('Ctrl Pts',(42.1059008215664,264.358803015509,24.5442064034937)) ;
#99944 = CARTESIAN_POINT('Ctrl Pts',(42.0879421404037,264.361590977558,24.4774793175867)) ;
#99945 = CARTESIAN_POINT('Ctrl Pts',(42.0665374511466,264.364378939607,24.41191883924)) ;
#99946 = CARTESIAN_POINT('Ctrl Pts',(42.0451098024302,264.367169892126,24.3462880383052)) ;
#99947 = CARTESIAN_POINT('Ctrl Pts',(42.0202289238655,264.369960844646,24.2818268077257)) ;
#99948 = CARTESIAN_POINT('Ctrl Pts',(41.9920585786101,264.372751797166,24.2189125290226)) ;
#99949 = CARTESIAN_POINT('Ctrl Pts',(41.9638702000318,264.375544536322,24.1559579755733)) ;
#99950 = CARTESIAN_POINT('Ctrl Pts',(41.9323883879454,264.378337275477,24.0945527802248)) ;
#99951 = CARTESIAN_POINT('Ctrl Pts',(41.8978228576819,264.381130014633,24.0350496941267)) ;
#99952 = CARTESIAN_POINT('Ctrl Pts',(41.8632009898797,264.383927305608,23.9754496253585)) ;
#99953 = CARTESIAN_POINT('Ctrl Pts',(41.825485645075,264.386724596583,23.9177582595413)) ;
#99954 = CARTESIAN_POINT('Ctrl Pts',(41.7849292291823,264.389521887558,23.8622985195703)) ;
#99955 = CARTESIAN_POINT('Ctrl Pts',(41.7740574096359,264.390271747772,23.847431616966)) ;
#99956 = CARTESIAN_POINT('Ctrl Pts',(41.7629816482407,264.391021607986,23.8327248854236)) ;
#99957 = CARTESIAN_POINT('Ctrl Pts',(41.7517072689471,264.3917714682,23.8181841079251)) ;
#99958 = CARTESIAN_POINT('Ctrl Pts',(41.7095436440027,264.394575775559,23.7638048935239)) ;
#99959 = CARTESIAN_POINT('Ctrl Pts',(41.6644411284693,264.397380082918,23.7115455412584)) ;
#99960 = CARTESIAN_POINT('Ctrl Pts',(41.6166405449795,264.400184390277,23.6617388578368)) ;
#99961 = CARTESIAN_POINT('Ctrl Pts',(41.5677005192088,264.40305554507,23.6107449119003)) ;
#99962 = CARTESIAN_POINT('Ctrl Pts',(41.5159323856718,264.405926699864,23.5623225303253)) ;
#99963 = CARTESIAN_POINT('Ctrl Pts',(41.4616400760896,264.408797854657,23.5167949803953)) ;
#99964 = CARTESIAN_POINT('Ctrl Pts',(41.4087462681314,264.411595052114,23.4724401629021)) ;
#99965 = CARTESIAN_POINT('Ctrl Pts',(41.3534571585366,264.41439224957,23.4308331693213)) ;
#99966 = CARTESIAN_POINT('Ctrl Pts',(41.2960911358452,264.417189447027,23.3922357932917)) ;
#99967 = CARTESIAN_POINT('Ctrl Pts',(41.2387574840503,264.419985066061,23.3536601972567)) ;
#99968 = CARTESIAN_POINT('Ctrl Pts',(41.1793496485779,264.422780685096,23.3180911201278)) ;
#99969 = CARTESIAN_POINT('Ctrl Pts',(41.118216854203,264.42557630413,23.2857483748249)) ;
#99970 = CARTESIAN_POINT('Ctrl Pts',(41.0570980555312,264.428371283137,23.2534130340496)) ;
#99971 = CARTESIAN_POINT('Ctrl Pts',(40.9942555130983,264.431166262145,23.2243027856572)) ;
#99972 = CARTESIAN_POINT('Ctrl Pts',(40.9300634902496,264.433961241152,23.1985917432999)) ;
#99973 = CARTESIAN_POINT('Ctrl Pts',(40.8628262161465,264.436888813166,23.1716609764268)) ;
#99974 = CARTESIAN_POINT('Ctrl Pts',(40.7941087586514,264.43981638518,23.1484602139986)) ;
#99975 = CARTESIAN_POINT('Ctrl Pts',(40.7243630542337,264.442743957194,23.1291322880655)) ;
#99976 = CARTESIAN_POINT('Ctrl Pts',(40.6576989524889,264.44554217911,23.1106583357027)) ;
#99977 = CARTESIAN_POINT('Ctrl Pts',(40.5900960628693,264.448340401025,23.09572225469)) ;
#99978 = CARTESIAN_POINT('Ctrl Pts',(40.5219607701516,264.451138622941,23.0843966195882)) ;
#99979 = CARTESIAN_POINT('Ctrl Pts',(40.4537815768329,264.453938647793,23.073063687208)) ;
#99980 = CARTESIAN_POINT('Ctrl Pts',(40.3850697816922,264.456738672645,23.0653458847321)) ;
#99981 = CARTESIAN_POINT('Ctrl Pts',(40.3162366861751,264.459538697498,23.0612638946819)) ;
#99982 = CARTESIAN_POINT('Ctrl Pts',(40.2472978972078,264.462343021797,23.0571756367223)) ;
#99983 = CARTESIAN_POINT('Ctrl Pts',(40.1782379225077,264.465147346097,23.0567343287291)) ;
#99984 = CARTESIAN_POINT('Ctrl Pts',(40.1094667685584,264.467951670397,23.0599086111575)) ;
#99985 = CARTESIAN_POINT('Ctrl Pts',(40.1001443772151,264.468331815372,23.0603389064387)) ;
#99986 = CARTESIAN_POINT('Ctrl Pts',(40.0908272818648,264.468711960347,23.0608355628873)) ;
#99987 = CARTESIAN_POINT('Ctrl Pts',(40.0815164916957,264.469092105321,23.0613984297426)) ;
#99988 = CARTESIAN_POINT('Ctrl Pts',(40.0128312227535,264.471896417238,23.0655506725314)) ;
#99989 = CARTESIAN_POINT('Ctrl Pts',(39.9442392025349,264.474700729154,23.0733254004651)) ;
#99990 = CARTESIAN_POINT('Ctrl Pts',(39.8761510800327,264.477505041071,23.0847114189091)) ;
#99991 = CARTESIAN_POINT('Ctrl Pts',(39.8064400399138,264.480376195295,23.0963688293263)) ;
#99992 = CARTESIAN_POINT('Ctrl Pts',(39.7372577464111,264.483247349518,23.111811956507)) ;
#99993 = CARTESIAN_POINT('Ctrl Pts',(39.669042557486,264.486118503742,23.130972109969)) ;
#99994 = CARTESIAN_POINT('Ctrl Pts',(39.6025843513625,264.488915707154,23.1496387654193)) ;
#99995 = CARTESIAN_POINT('Ctrl Pts',(39.5370445306828,264.491712910567,23.1718331329916)) ;
#99996 = CARTESIAN_POINT('Ctrl Pts',(39.4728188425292,264.494510113979,23.1974399159494)) ;
#99997 = CARTESIAN_POINT('Ctrl Pts',(39.4086293846151,264.497305739465,23.2230322539102)) ;
#99998 = CARTESIAN_POINT('Ctrl Pts',(39.3457530400132,264.500101364952,23.2520330069956)) ;
#99999 = CARTESIAN_POINT('Ctrl Pts',(39.2845682769097,264.502896990439,23.2842777389123)) ;
#100000 = CARTESIAN_POINT('Ctrl Pts',(39.2233975108401,264.505691976379,23.3165150943094)) ;
#100001 = CARTESIAN_POINT('Ctrl Pts',(39.163917988563,264.50848696232,23.3519947271888)) ;
#100002 = CARTESIAN_POINT('Ctrl Pts',(39.1064845590575,264.511281948261,23.3905057524977)) ;
#100003 = CARTESIAN_POINT('Ctrl Pts',(39.046326773118,264.514209514443,23.4308435494357)) ;
#100004 = CARTESIAN_POINT('Ctrl Pts',(38.9884145298127,264.517137080625,23.4745071981758)) ;
#100005 = CARTESIAN_POINT('Ctrl Pts',(38.933120643068,264.520064646807,23.5212040330758)) ;
#100006 = CARTESIAN_POINT('Ctrl Pts',(38.8802695713198,264.522862876764,23.5658378600141)) ;
#100007 = CARTESIAN_POINT('Ctrl Pts',(38.8298107114831,264.52566110672,23.6132421235063)) ;
#100008 = CARTESIAN_POINT('Ctrl Pts',(38.7820331743618,264.528459336677,23.6631221505887)) ;
#100009 = CARTESIAN_POINT('Ctrl Pts',(38.734224847177,264.531259369944,23.7130343226767)) ;
#100010 = CARTESIAN_POINT('Ctrl Pts',(38.689101599458,264.53405940321,23.7654250646338)) ;
#100011 = CARTESIAN_POINT('Ctrl Pts',(38.6469124613425,264.536859436476,23.819966379373)) ;
#100012 = CARTESIAN_POINT('Ctrl Pts',(38.6046585349088,264.539663769651,23.8745914512169)) ;
#100013 = CARTESIAN_POINT('Ctrl Pts',(38.5653479812375,264.542468102826,23.9313732828279)) ;
#100014 = CARTESIAN_POINT('Ctrl Pts',(38.5291861229908,264.545272436001,23.989955597995)) ;
#100015 = CARTESIAN_POINT('Ctrl Pts',(38.5242847082473,264.545652538149,23.9978959040852)) ;
#100016 = CARTESIAN_POINT('Ctrl Pts',(38.5194410689531,264.546032640296,24.0058692530938)) ;
#100017 = CARTESIAN_POINT('Ctrl Pts',(38.5146556495777,264.546412742443,24.0138747269133)) ;
#100018 = CARTESIAN_POINT('Ctrl Pts',(38.4793526268504,264.549216834142,24.0729327533947)) ;
#100019 = CARTESIAN_POINT('Ctrl Pts',(38.4470931245889,264.552020925841,24.1339564703419)) ;
#100020 = CARTESIAN_POINT('Ctrl Pts',(38.4180994832558,264.554825017539,24.196600513298)) ;
#100021 = CARTESIAN_POINT('Ctrl Pts',(38.3884121467348,264.55769619929,24.2607433632047)) ;
#100022 = CARTESIAN_POINT('Ctrl Pts',(38.3621493053107,264.560567381041,24.3265846793667)) ;
#100023 = CARTESIAN_POINT('Ctrl Pts',(38.3395014964272,264.563438562793,24.3937236831134)) ;
#100024 = CARTESIAN_POINT('Ctrl Pts',(38.3174389729793,264.566235544833,24.459127619187)) ;
#100025 = CARTESIAN_POINT('Ctrl Pts',(38.2988070560149,264.569032526874,24.5257624869819)) ;
#100026 = CARTESIAN_POINT('Ctrl Pts',(38.283733713274,264.571829508914,24.5932365102311)) ;
#100027 = CARTESIAN_POINT('Ctrl Pts',(38.2686688730836,264.574624913237,24.6606724728257)) ;
#100028 = CARTESIAN_POINT('Ctrl Pts',(38.2571587297346,264.57742031756,24.7289461766327)) ;
#100029 = CARTESIAN_POINT('Ctrl Pts',(38.2492809271652,264.580215721883,24.7976524002183)) ;
#100030 = CARTESIAN_POINT('Ctrl Pts',(38.2414049252721,264.583010487243,24.8663429192128)) ;
#100031 = CARTESIAN_POINT('Ctrl Pts',(38.2371596703656,264.585805252604,24.9354652774667)) ;
#100032 = CARTESIAN_POINT('Ctrl Pts',(38.2365711286217,264.588600017965,25.0046075628753)) ;
#100033 = CARTESIAN_POINT('Ctrl Pts',(38.2359545756725,264.591527798098,25.0770406237873)) ;
#100034 = CARTESIAN_POINT('Ctrl Pts',(38.2393515526775,264.594455578231,25.1494949762986)) ;
#100035 = CARTESIAN_POINT('Ctrl Pts',(38.2467306029344,264.597383358365,25.2214975462755)) ;
#100036 = CARTESIAN_POINT('Ctrl Pts',(38.2537825947889,264.600181371786,25.2903087779779)) ;
#100037 = CARTESIAN_POINT('Ctrl Pts',(38.2644709950671,264.602979385207,25.3587069333941)) ;
#100038 = CARTESIAN_POINT('Ctrl Pts',(38.2787154960898,264.605777398627,25.4262871385375)) ;
#100039 = CARTESIAN_POINT('Ctrl Pts',(38.2929691857925,264.608577216959,25.4939109375475)) ;
#100040 = CARTESIAN_POINT('Ctrl Pts',(38.3107834159673,264.61137703529,25.5607152655708)) ;
#100041 = CARTESIAN_POINT('Ctrl Pts',(38.3320277571629,264.614176853622,25.6263095583315)) ;
#100042 = CARTESIAN_POINT('Ctrl Pts',(38.35330475354,264.61698097562,25.6920046776376)) ;
#100043 = CARTESIAN_POINT('Ctrl Pts',(38.3780222024389,264.619785097619,25.7564855981368)) ;
#100044 = CARTESIAN_POINT('Ctrl Pts',(38.4060016741804,264.622589219618,25.8193819056941)) ;
#100045 = CARTESIAN_POINT('Ctrl Pts',(38.409807142338,264.622970606267,25.8279363879891)) ;
#100046 = CARTESIAN_POINT('Ctrl Pts',(38.4136728845381,264.623351992916,25.8364615962601)) ;
#100047 = CARTESIAN_POINT('Ctrl Pts',(38.4175983879456,264.623733379566,25.8449566366805)) ;
#100048 = CARTESIAN_POINT('Ctrl Pts',(38.4464655112008,264.62653799703,25.9074269375343)) ;
#100049 = CARTESIAN_POINT('Ctrl Pts',(38.4786733892577,264.629342614494,25.9684916631513)) ;
#100050 = CARTESIAN_POINT('Ctrl Pts',(38.5140620943109,264.632147231958,26.0277723434883)) ;
#100051 = CARTESIAN_POINT('Ctrl Pts',(38.550289879267,264.635018347988,26.0884585917157)) ;
#100052 = CARTESIAN_POINT('Ctrl Pts',(38.589851123995,264.637889464019,26.1472746073566)) ;
#100053 = CARTESIAN_POINT('Ctrl Pts',(38.6325223457163,264.640760580049,26.2038371735969)) ;
#100054 = CARTESIAN_POINT('Ctrl Pts',(38.6740995212223,264.643558083619,26.2589495338428)) ;
#100055 = CARTESIAN_POINT('Ctrl Pts',(38.7186287952341,264.646355587189,26.3119221999099)) ;
#100056 = CARTESIAN_POINT('Ctrl Pts',(38.7658587081481,264.649153090759,26.3624284693292)) ;
#100057 = CARTESIAN_POINT('Ctrl Pts',(38.8130619331503,264.651949013561,26.4129061994865)) ;
#100058 = CARTESIAN_POINT('Ctrl Pts',(38.8629624364252,264.654744936363,26.4609199434834)) ;
#100059 = CARTESIAN_POINT('Ctrl Pts',(38.9152692766348,264.657540859165,26.5061769758449)) ;
#100060 = CARTESIAN_POINT('Ctrl Pts',(38.9675640897254,264.660336139089,26.5514236020776)) ;
#100061 = CARTESIAN_POINT('Ctrl Pts',(39.0222637722745,264.663131419014,26.593914457129)) ;
#100062 = CARTESIAN_POINT('Ctrl Pts',(39.0790427136724,264.665926698938,26.633395717799)) ;
#100063 = CARTESIAN_POINT('Ctrl Pts',(39.1385028264927,264.668853975417,26.6747413321399)) ;
#100064 = CARTESIAN_POINT('Ctrl Pts',(39.20024298406,264.671781251896,26.7127857088493)) ;
#100065 = CARTESIAN_POINT('Ctrl Pts',(39.2638551061375,264.674708528376,26.7472881844231)) ;
#100066 = CARTESIAN_POINT('Ctrl Pts',(39.3246690750271,264.677507040592,26.7802729742342)) ;
#100067 = CARTESIAN_POINT('Ctrl Pts',(39.3871932902662,264.680305552808,26.810020760495)) ;
#100068 = CARTESIAN_POINT('Ctrl Pts',(39.4510480207014,264.683104065025,26.8363694290404)) ;
#100069 = CARTESIAN_POINT('Ctrl Pts',(39.5149437996222,264.685904376241,26.8627350356096)) ;
#100070 = CARTESIAN_POINT('Ctrl Pts',(39.5801713366973,264.688704687458,26.8856970140323)) ;
#100071 = CARTESIAN_POINT('Ctrl Pts',(39.6463344402367,264.691504998675,26.9051427072479)) ;
#100072 = CARTESIAN_POINT('Ctrl Pts',(39.7125989490608,264.694309601806,26.9246182040238)) ;
#100073 = CARTESIAN_POINT('Ctrl Pts',(39.7798014112819,264.697114204936,26.9405665548798)) ;
#100074 = CARTESIAN_POINT('Ctrl Pts',(39.8475351930882,264.699918808067,26.9529261029962)) ;
#100075 = CARTESIAN_POINT('Ctrl Pts',(39.8566739754725,264.700297210941,26.9545936788733)) ;
#100076 = CARTESIAN_POINT('Ctrl Pts',(39.8658224235725,264.700675613815,26.9561960016907)) ;
#100077 = CARTESIAN_POINT('Ctrl Pts',(39.8749795341706,264.701054016688,26.9577329924524)) ;
#100078 = CARTESIAN_POINT('Ctrl Pts',(39.9428436807735,264.703858393443,26.9691237652583)) ;
#100079 = CARTESIAN_POINT('Ctrl Pts',(40.0114309987808,264.706662770198,26.9769634518271)) ;
#100080 = CARTESIAN_POINT('Ctrl Pts',(40.0803387932757,264.709467146952,26.9811707066244)) ;
#100081 = CARTESIAN_POINT('Ctrl Pts',(40.150887212427,264.712338293071,26.9854781318887)) ;
#100082 = CARTESIAN_POINT('Ctrl Pts',(40.2217710722778,264.71520943919,26.9859777612121)) ;
#100083 = CARTESIAN_POINT('Ctrl Pts',(40.2925477963527,264.71808058531,26.9826380524967)) ;
#100084 = CARTESIAN_POINT('Ctrl Pts',(40.3615035625385,264.720877862,26.9793842684834)) ;
#100085 = CARTESIAN_POINT('Ctrl Pts',(40.4303571204035,264.72367513869,26.9724863577426)) ;
#100086 = CARTESIAN_POINT('Ctrl Pts',(40.4986969110173,264.726472415381,26.9619677626826)) ;
#100087 = CARTESIAN_POINT('Ctrl Pts',(40.5669982215106,264.729268117007,26.9514550903333)) ;
#100088 = CARTESIAN_POINT('Ctrl Pts',(40.634785858032,264.732063818633,26.9373258534575)) ;
#100089 = CARTESIAN_POINT('Ctrl Pts',(40.7016540599149,264.73485952026,26.9196552597878)) ;
#100090 = CARTESIAN_POINT('Ctrl Pts',(40.7685070292218,264.737654585025,26.9019886914791)) ;
#100091 = CARTESIAN_POINT('Ctrl Pts',(40.8344405089517,264.740449649791,26.8807824933933)) ;
#100092 = CARTESIAN_POINT('Ctrl Pts',(40.8990613189203,264.743244714556,26.8561624409591)) ;
#100093 = CARTESIAN_POINT('Ctrl Pts',(40.9667438629519,264.746172209494,26.8303758904076)) ;
#100094 = CARTESIAN_POINT('Ctrl Pts',(41.0329856991877,264.749099704432,26.8008441120265)) ;
#100095 = CARTESIAN_POINT('Ctrl Pts',(41.0973578329321,264.75202719937,26.7677685018727)) ;
#100096 = CARTESIAN_POINT('Ctrl Pts',(41.1588894396531,264.754825513744,26.7361524078014)) ;
#100097 = CARTESIAN_POINT('Ctrl Pts',(41.218712467216,264.757623828119,26.7012989621997)) ;
#100098 = CARTESIAN_POINT('Ctrl Pts',(41.2764789663989,264.760422142494,26.663430353547)) ;
#100099 = CARTESIAN_POINT('Ctrl Pts',(41.3342827293884,264.763222261995,26.6255373167477)) ;
#100100 = CARTESIAN_POINT('Ctrl Pts',(41.3900269312364,264.766022381497,26.5846255341491)) ;
#100101 = CARTESIAN_POINT('Ctrl Pts',(41.4433951909114,264.768822500998,26.5409586719846)) ;
#100102 = CARTESIAN_POINT('Ctrl Pts',(41.4968454397676,264.771626922298,26.4972247248094)) ;
#100103 = CARTESIAN_POINT('Ctrl Pts',(41.5479121071341,264.774431343598,26.4507275837462)) ;
#100104 = CARTESIAN_POINT('Ctrl Pts',(41.5963150473167,264.777235764898,26.4017682921028)) ;
#100105 = CARTESIAN_POINT('Ctrl Pts',(41.6028672692048,264.777615394536,26.3951407578843)) ;
#100106 = CARTESIAN_POINT('Ctrl Pts',(41.6093707401449,264.777995024173,26.3884681550574)) ;
#100107 = CARTESIAN_POINT('Ctrl Pts',(41.6158248231222,264.77837465381,26.3817512753716)) ;
#100108 = CARTESIAN_POINT('Ctrl Pts',(41.6628292052529,264.781139455038,26.3328329734866)) ;
#100109 = CARTESIAN_POINT('Ctrl Pts',(41.7073932893235,264.783904256266,26.2813735376347)) ;
#100110 = CARTESIAN_POINT('Ctrl Pts',(41.7492265774585,264.786669057493,26.2276491800284)) ;
#100111 = CARTESIAN_POINT('Ctrl Pts',(41.7910060149023,264.789430299679,26.1739939801174)) ;
#100112 = CARTESIAN_POINT('Ctrl Pts',(41.8300613170704,264.792191541864,26.1180800296299)) ;
#100113 = CARTESIAN_POINT('Ctrl Pts',(41.8661394144824,264.794952784049,26.060219617555)) ;
#100114 = CARTESIAN_POINT('Ctrl Pts',(41.9021840563867,264.797711465712,26.0024128599022)) ;
#100115 = CARTESIAN_POINT('Ctrl Pts',(41.9352567027741,264.800470147375,25.9426636440052)) ;
#100116 = CARTESIAN_POINT('Ctrl Pts',(41.9651463200989,264.803228829038,25.8813149474039)) ;
#100117 = CARTESIAN_POINT('Ctrl Pts',(41.9950189755122,264.805985945191,25.8200010652719)) ;
#100118 = CARTESIAN_POINT('Ctrl Pts',(42.0217119664681,264.808743061343,25.757089954604)) ;
#100119 = CARTESIAN_POINT('Ctrl Pts',(42.0450601063211,264.811500177496,25.6929492992057)) ;
#100120 = CARTESIAN_POINT('Ctrl Pts',(42.0684116860251,264.81425769985,25.6287991940485)) ;
#100121 = CARTESIAN_POINT('Ctrl Pts',(42.0884172473216,264.817015222205,25.5634196508713)) ;
#100122 = CARTESIAN_POINT('Ctrl Pts',(42.1049602730527,264.81977274456,25.4971970167546)) ;
#100123 = CARTESIAN_POINT('Ctrl Pts',(42.1215047963007,264.822530516533,25.4309683879956)) ;
#100124 = CARTESIAN_POINT('Ctrl Pts',(42.1345860514729,264.825288288506,25.3638970075198)) ;
#100125 = CARTESIAN_POINT('Ctrl Pts',(42.1441383952741,264.828046060479,25.2963806097214)) ;
#100126 = CARTESIAN_POINT('Ctrl Pts',(42.1536997060346,264.830806421222,25.2288008330492)) ;
#100127 = CARTESIAN_POINT('Ctrl Pts',(42.1597254422429,264.833566781966,25.1607757055302)) ;
#100128 = CARTESIAN_POINT('Ctrl Pts',(42.1622018410338,264.83632714271,25.0927079128119)) ;
#100129 = CARTESIAN_POINT('Ctrl Pts',(42.1630870308451,264.837313834843,25.0683770510719)) ;
#100130 = CARTESIAN_POINT('Ctrl Pts',(42.1635192039033,264.838300526976,25.0440407370176)) ;
#100131 = CARTESIAN_POINT('Ctrl Pts',(42.1634993456137,264.839287219109,25.0197172919184)) ;
#100132 = CARTESIAN_POINT('',(39.3481011574342,264.999957040867,23.2522526195775)) ;
#100133 = CARTESIAN_POINT('Ctrl Pts',(42.1634993456133,264.83928721913,25.0197172914112)) ;
#100134 = CARTESIAN_POINT('Ctrl Pts',(42.1634231064844,264.843075285805,24.9263357505314)) ;
#100135 = CARTESIAN_POINT('Ctrl Pts',(42.1566814593656,264.846863352479,24.833221909536)) ;
#100136 = CARTESIAN_POINT('Ctrl Pts',(42.1434103250307,264.850651419153,24.7411622478992)) ;
#100137 = CARTESIAN_POINT('Ctrl Pts',(42.1375200820027,264.852332709746,24.7003026072363)) ;
#100138 = CARTESIAN_POINT('Ctrl Pts',(42.1303441968703,264.854014000339,24.6596502838563)) ;
#100139 = CARTESIAN_POINT('Ctrl Pts',(42.1218974742994,264.855695290932,24.6192726495211)) ;
#100140 = CARTESIAN_POINT('Ctrl Pts',(42.1077899698027,264.858503340374,24.5518349358796)) ;
#100141 = CARTESIAN_POINT('Ctrl Pts',(42.0901033726998,264.861311389816,24.4850193578663)) ;
#100142 = CARTESIAN_POINT('Ctrl Pts',(42.0689090738205,264.864119439258,24.4192313768849)) ;
#100143 = CARTESIAN_POINT('Ctrl Pts',(42.0472420055495,264.866990126291,24.3519759001431)) ;
#100144 = CARTESIAN_POINT('Ctrl Pts',(42.0219088766885,264.869860813324,24.2857949364322)) ;
#100145 = CARTESIAN_POINT('Ctrl Pts',(41.9930413906057,264.872731500357,24.2211111074377)) ;
#100146 = CARTESIAN_POINT('Ctrl Pts',(41.9648754428109,264.87553242389,24.1579992262922)) ;
#100147 = CARTESIAN_POINT('Ctrl Pts',(41.9333451893783,264.878333347424,24.0963130074087)) ;
#100148 = CARTESIAN_POINT('Ctrl Pts',(41.8986227463113,264.881134270957,24.0364279556745)) ;
#100149 = CARTESIAN_POINT('Ctrl Pts',(41.8639200754108,264.883933599547,23.9765770045713)) ;
#100150 = CARTESIAN_POINT('Ctrl Pts',(41.8260290658077,264.886732928136,23.9185256046506)) ;
#100151 = CARTESIAN_POINT('Ctrl Pts',(41.7851679310898,264.889532256726,23.862625008174)) ;
#100152 = CARTESIAN_POINT('Ctrl Pts',(41.7443164700062,264.892330922592,23.8067376458361)) ;
#100153 = CARTESIAN_POINT('Ctrl Pts',(41.7004965673578,264.895129588457,23.7530004675247)) ;
#100154 = CARTESIAN_POINT('Ctrl Pts',(41.6539689599815,264.897928254322,23.7017346080311)) ;
#100155 = CARTESIAN_POINT('Ctrl Pts',(41.605358134152,264.900852227133,23.6481733804638)) ;
#100156 = CARTESIAN_POINT('Ctrl Pts',(41.5537917794676,264.903776199944,23.5973104348385)) ;
#100157 = CARTESIAN_POINT('Ctrl Pts',(41.4996115905637,264.906700172755,23.5494704994273)) ;
#100158 = CARTESIAN_POINT('Ctrl Pts',(41.4476950435001,264.90950198233,23.5036293108204)) ;
#100159 = CARTESIAN_POINT('Ctrl Pts',(41.3933791649083,264.912303791906,23.4605638234563)) ;
#100160 = CARTESIAN_POINT('Ctrl Pts',(41.3369979930227,264.915105601481,23.4205181028495)) ;
#100161 = CARTESIAN_POINT('Ctrl Pts',(41.2805812983321,264.917909176329,23.3804471515447)) ;
#100162 = CARTESIAN_POINT('Ctrl Pts',(41.2220971304581,264.920712751176,23.3434000140179)) ;
#100163 = CARTESIAN_POINT('Ctrl Pts',(41.1619067425903,264.923516326024,23.3095763006141)) ;
#100164 = CARTESIAN_POINT('Ctrl Pts',(41.101625711966,264.926324122871,23.2757016509276)) ;
#100165 = CARTESIAN_POINT('Ctrl Pts',(41.039633771008,264.929131919718,23.2450603222638)) ;
#100166 = CARTESIAN_POINT('Ctrl Pts',(40.9763138793755,264.931939716564,23.2178046073685)) ;
#100167 = CARTESIAN_POINT('Ctrl Pts',(40.9682238359863,264.932298453728,23.214322290668)) ;
#100168 = CARTESIAN_POINT('Ctrl Pts',(40.9601121367656,264.932657190891,23.2108951736593)) ;
#100169 = CARTESIAN_POINT('Ctrl Pts',(40.9519795979876,264.933015928055,23.2075235152984)) ;
#100170 = CARTESIAN_POINT('Ctrl Pts',(40.8887483928988,264.935805141089,23.18130857466)) ;
#100171 = CARTESIAN_POINT('Ctrl Pts',(40.8240121001998,264.938594354122,23.1583492976769)) ;
#100172 = CARTESIAN_POINT('Ctrl Pts',(40.7581442156735,264.941383567156,23.1388200687893)) ;
#100173 = CARTESIAN_POINT('Ctrl Pts',(40.6930035405595,264.944141986094,23.1195064508806)) ;
#100174 = CARTESIAN_POINT('Ctrl Pts',(40.6267566189771,264.946900405032,23.1035476997139)) ;
#100175 = CARTESIAN_POINT('Ctrl Pts',(40.5597860729364,264.949658823969,23.0910648600235)) ;
#100176 = CARTESIAN_POINT('Ctrl Pts',(40.4928740653508,264.952414831794,23.0785929314903)) ;
#100177 = CARTESIAN_POINT('Ctrl Pts',(40.4252401800672,264.955170839618,23.0695909839479)) ;
#100178 = CARTESIAN_POINT('Ctrl Pts',(40.3572802186558,264.957926847442,23.0641297082817)) ;
#100179 = CARTESIAN_POINT('Ctrl Pts',(40.2893551072405,264.96068144198,23.0586712331679)) ;
#100180 = CARTESIAN_POINT('Ctrl Pts',(40.2211047526861,264.963436036518,23.0567498687277)) ;
#100181 = CARTESIAN_POINT('Ctrl Pts',(40.1529311591549,264.966190631057,23.0583845895876)) ;
#100182 = CARTESIAN_POINT('Ctrl Pts',(40.0832906166155,264.969004498541,23.0600544861222)) ;
#100183 = CARTESIAN_POINT('Ctrl Pts',(40.0137307198484,264.971818366025,23.0654353438013)) ;
#100184 = CARTESIAN_POINT('Ctrl Pts',(39.9446791624989,264.974632233509,23.0744912498953)) ;
#100185 = CARTESIAN_POINT('Ctrl Pts',(39.8770450615677,264.977388339305,23.0833612608016)) ;
#100186 = CARTESIAN_POINT('Ctrl Pts',(39.8098991283124,264.980144445101,23.0957567194047)) ;
#100187 = CARTESIAN_POINT('Ctrl Pts',(39.743634804907,264.982900550897,23.1115918134518)) ;
#100188 = CARTESIAN_POINT('Ctrl Pts',(39.6752873579909,264.985743299225,23.1279247086535)) ;
#100189 = CARTESIAN_POINT('Ctrl Pts',(39.6078784423246,264.988586047554,23.1479169980995)) ;
#100190 = CARTESIAN_POINT('Ctrl Pts',(39.5418221791217,264.991428795882,23.1714192094165)) ;
#100191 = CARTESIAN_POINT('Ctrl Pts',(39.4757659159188,264.99427154421,23.1949214207335)) ;
#100192 = CARTESIAN_POINT('Ctrl Pts',(39.4110628212892,264.997114292539,23.2219332780187)) ;
#100193 = CARTESIAN_POINT('Ctrl Pts',(39.3481011574342,264.999957040867,23.2522526195775)) ;
#100194 = CARTESIAN_POINT('',(41.0518972680585,265.,23.2522518613707)) ;
#100195 = CARTESIAN_POINT('Origin',(40.2,265.,25.0213203435596)) ;
#100196 = CARTESIAN_POINT('',(42.1634997790836,264.91071278087,25.0203889259126)) ;
#100197 = CARTESIAN_POINT('Ctrl Pts',(41.0518972680585,265.,23.2522518613707)) ;
#100198 = CARTESIAN_POINT('Ctrl Pts',(41.6248630396448,264.974226454293,23.5281642867062)) ;
#100199 = CARTESIAN_POINT('Ctrl Pts',(42.1146717303696,264.944464047916,24.1908662058816)) ;
#100200 = CARTESIAN_POINT('Ctrl Pts',(42.1650160107952,264.914701641539,24.9222347032997)) ;
#100201 = CARTESIAN_POINT('Ctrl Pts',(42.1642443780331,264.91071278087,25.0203885727001)) ;
#100202 = CARTESIAN_POINT('',(42.1634997239514,264.410712780843,25.0223615172765)) ;
#100203 = CARTESIAN_POINT('Ctrl Pts',(42.1634997790836,264.91071278087,25.0203889259126)) ;
#100204 = CARTESIAN_POINT('Ctrl Pts',(42.1635318794642,264.907961693408,25.08805898823)) ;
#100205 = CARTESIAN_POINT('Ctrl Pts',(42.1600614472557,264.905210605947,25.1558539686729)) ;
#100206 = CARTESIAN_POINT('Ctrl Pts',(42.1530760488447,264.902459518485,25.2233752802212)) ;
#100207 = CARTESIAN_POINT('Ctrl Pts',(42.1460976350027,264.899711181784,25.2908290784746)) ;
#100208 = CARTESIAN_POINT('Ctrl Pts',(42.1356112693631,264.896962845084,25.3580092487036)) ;
#100209 = CARTESIAN_POINT('Ctrl Pts',(42.1216565407332,264.894214508383,25.4245180487331)) ;
#100210 = CARTESIAN_POINT('Ctrl Pts',(42.1077106617737,264.891467914595,25.4909846708768)) ;
#100211 = CARTESIAN_POINT('Ctrl Pts',(42.0903008831812,264.888721320807,25.5567802716991)) ;
#100212 = CARTESIAN_POINT('Ctrl Pts',(42.0695182592163,264.885974727019,25.6215150856698)) ;
#100213 = CARTESIAN_POINT('Ctrl Pts',(42.0487412166764,264.883228870862,25.6862325143235)) ;
#100214 = CARTESIAN_POINT('Ctrl Pts',(42.0245932812702,264.880483014705,25.7498892389648)) ;
#100215 = CARTESIAN_POINT('Ctrl Pts',(41.9972154150436,264.877737158547,25.8121104559975)) ;
#100216 = CARTESIAN_POINT('Ctrl Pts',(41.9698165503494,264.874989196354,25.8743793958953)) ;
#100217 = CARTESIAN_POINT('Ctrl Pts',(41.9391830068083,264.872241234161,25.9352101618639)) ;
#100218 = CARTESIAN_POINT('Ctrl Pts',(41.9055035211403,264.869493271968,25.9942489069075)) ;
#100219 = CARTESIAN_POINT('Ctrl Pts',(41.8718123184394,264.866744353764,26.0533081914247)) ;
#100220 = CARTESIAN_POINT('Ctrl Pts',(41.8350733360558,264.86399543556,26.1105737849847)) ;
#100221 = CARTESIAN_POINT('Ctrl Pts',(41.795519279112,264.861246517355,26.1657199590707)) ;
#100222 = CARTESIAN_POINT('Ctrl Pts',(41.7558956597364,264.858492764718,26.2209631169371)) ;
#100223 = CARTESIAN_POINT('Ctrl Pts',(41.7134473926541,264.855739012081,26.2740790117971)) ;
#100224 = CARTESIAN_POINT('Ctrl Pts',(41.6684476868165,264.852985259444,26.3247748464416)) ;
#100225 = CARTESIAN_POINT('Ctrl Pts',(41.6269053725341,264.850443081548,26.3715756478337)) ;
#100226 = CARTESIAN_POINT('Ctrl Pts',(41.5831892778027,264.847900903652,26.4163141561029)) ;
#100227 = CARTESIAN_POINT('Ctrl Pts',(41.537539930606,264.845358725756,26.4587900594265)) ;
#100228 = CARTESIAN_POINT('Ctrl Pts',(41.4871947620435,264.842555041091,26.505635340772)) ;
#100229 = CARTESIAN_POINT('Ctrl Pts',(41.4342916268096,264.839751356426,26.5499200365583)) ;
#100230 = CARTESIAN_POINT('Ctrl Pts',(41.3791209197052,264.836947671762,26.591354135143)) ;
#100231 = CARTESIAN_POINT('Ctrl Pts',(41.3226210085465,264.834076439131,26.6337864875967)) ;
#100232 = CARTESIAN_POINT('Ctrl Pts',(41.2637431565371,264.831205206501,26.6732286841668)) ;
#100233 = CARTESIAN_POINT('Ctrl Pts',(41.2028388445095,264.828333973871,26.7094099448376)) ;
#100234 = CARTESIAN_POINT('Ctrl Pts',(41.1435228607675,264.825537620339,26.7446476316)) ;
#100235 = CARTESIAN_POINT('Ctrl Pts',(41.0822852734038,264.822741266808,26.7767921278507)) ;
#100236 = CARTESIAN_POINT('Ctrl Pts',(41.0194817836898,264.819944913276,26.8056358583161)) ;
#100237 = CARTESIAN_POINT('Ctrl Pts',(40.9567155109527,264.817150216847,26.8344624961572)) ;
#100238 = CARTESIAN_POINT('Ctrl Pts',(40.8923856197779,264.814355520418,26.8599920465211)) ;
#100239 = CARTESIAN_POINT('Ctrl Pts',(40.8268715866425,264.811560823989,26.8820632768688)) ;
#100240 = CARTESIAN_POINT('Ctrl Pts',(40.7613743468544,264.808766843931,26.9041288496526)) ;
#100241 = CARTESIAN_POINT('Ctrl Pts',(40.6946940301555,264.805972863872,26.9227377074936)) ;
#100242 = CARTESIAN_POINT('Ctrl Pts',(40.6272275679252,264.803178883814,26.9377777146495)) ;
#100243 = CARTESIAN_POINT('Ctrl Pts',(40.5565152662079,264.800250484215,26.9535413027891)) ;
#100244 = CARTESIAN_POINT('Ctrl Pts',(40.4849398237965,264.797322084617,26.9653838072331)) ;
#100245 = CARTESIAN_POINT('Ctrl Pts',(40.4129707807618,264.794393685019,26.9732362476246)) ;
#100246 = CARTESIAN_POINT('Ctrl Pts',(40.3442299014721,264.791596638472,26.9807364676402)) ;
#100247 = CARTESIAN_POINT('Ctrl Pts',(40.2751304898507,264.788799591925,26.984596937117)) ;
#100248 = CARTESIAN_POINT('Ctrl Pts',(40.206085015493,264.786002545378,26.9848109146056)) ;
#100249 = CARTESIAN_POINT('Ctrl Pts',(40.1369964994812,264.783203755205,26.9850250254837)) ;
#100250 = CARTESIAN_POINT('Ctrl Pts',(40.0679624746254,264.780404965032,26.9815881443537)) ;
#100251 = CARTESIAN_POINT('Ctrl Pts',(39.9993919948402,264.777606174858,26.9745455426254)) ;
#100252 = CARTESIAN_POINT('Ctrl Pts',(39.9307179913896,264.774803159237,26.9674923083926)) ;
#100253 = CARTESIAN_POINT('Ctrl Pts',(39.8625094096421,264.772000143615,26.9568225715688)) ;
#100254 = CARTESIAN_POINT('Ctrl Pts',(39.7951657177126,264.769197127994,26.9426327736149)) ;
#100255 = CARTESIAN_POINT('Ctrl Pts',(39.7858835730344,264.76881078154,26.9406769592871)) ;
#100256 = CARTESIAN_POINT('Ctrl Pts',(39.776617835104,264.768424435087,26.9386543488758)) ;
#100257 = CARTESIAN_POINT('Ctrl Pts',(39.7673695251547,264.768038088634,26.9365652684283)) ;
#100258 = CARTESIAN_POINT('Ctrl Pts',(39.7001575510037,264.76523032073,26.9213829030218)) ;
#100259 = CARTESIAN_POINT('Ctrl Pts',(39.6336264701506,264.762422552827,26.902631367906)) ;
#100260 = CARTESIAN_POINT('Ctrl Pts',(39.5681805075374,264.759614784923,26.8803890294731)) ;
#100261 = CARTESIAN_POINT('Ctrl Pts',(39.501267149348,264.756744062698,26.8576479848143)) ;
#100262 = CARTESIAN_POINT('Ctrl Pts',(39.4354886779217,264.753873340472,26.8312577286187)) ;
#100263 = CARTESIAN_POINT('Ctrl Pts',(39.3712655380563,264.751002618247,26.8013572649708)) ;
#100264 = CARTESIAN_POINT('Ctrl Pts',(39.3086065396949,264.748201811877,26.7721850210311)) ;
#100265 = CARTESIAN_POINT('Ctrl Pts',(39.2474284393559,264.745401005507,26.7396718313736)) ;
#100266 = CARTESIAN_POINT('Ctrl Pts',(39.1881037596738,264.742600199137,26.7039962626877)) ;
#100267 = CARTESIAN_POINT('Ctrl Pts',(39.1288115674895,264.739800926551,26.668340230727)) ;
#100268 = CARTESIAN_POINT('Ctrl Pts',(39.0713711972851,264.737001653964,26.629525506797)) ;
#100269 = CARTESIAN_POINT('Ctrl Pts',(39.016130114285,264.734202381377,26.5877763256086)) ;
#100270 = CARTESIAN_POINT('Ctrl Pts',(38.9609009043902,264.731403710445,26.5460361176771)) ;
#100271 = CARTESIAN_POINT('Ctrl Pts',(38.9078704301041,264.728605039513,26.5013629984539)) ;
#100272 = CARTESIAN_POINT('Ctrl Pts',(38.8573552983472,264.725806368581,26.4540231931148)) ;
#100273 = CARTESIAN_POINT('Ctrl Pts',(38.8045766368541,264.722882292159,26.4045621410648)) ;
#100274 = CARTESIAN_POINT('Ctrl Pts',(38.7545444947112,264.719958215736,26.352190151185)) ;
#100275 = CARTESIAN_POINT('Ctrl Pts',(38.7075776766873,264.717034139314,26.2972544558389)) ;
#100276 = CARTESIAN_POINT('Ctrl Pts',(38.6625721943867,264.71423217241,26.2446128767711)) ;
#100277 = CARTESIAN_POINT('Ctrl Pts',(38.6203813700412,264.711430205506,26.1896178964985)) ;
#100278 = CARTESIAN_POINT('Ctrl Pts',(38.5812434763964,264.708628238603,26.1326076904194)) ;
#100279 = CARTESIAN_POINT('Ctrl Pts',(38.5420801920694,264.705824453925,26.0755604990074)) ;
#100280 = CARTESIAN_POINT('Ctrl Pts',(38.505974033711,264.703020669247,26.0164958939749)) ;
#100281 = CARTESIAN_POINT('Ctrl Pts',(38.4731183471652,264.700216884569,25.9557784791134)) ;
#100282 = CARTESIAN_POINT('Ctrl Pts',(38.440212338251,264.697408805563,25.8949680683523)) ;
#100283 = CARTESIAN_POINT('Ctrl Pts',(38.4105669385035,264.694600726558,25.832500236649)) ;
#100284 = CARTESIAN_POINT('Ctrl Pts',(38.38432780638,264.691792647552,25.7687604651179)) ;
#100285 = CARTESIAN_POINT('Ctrl Pts',(38.3809788727128,264.691434248872,25.7606252773452)) ;
#100286 = CARTESIAN_POINT('Ctrl Pts',(38.3776853596183,264.691075850192,25.7524693901348)) ;
#100287 = CARTESIAN_POINT('Ctrl Pts',(38.3744475111506,264.690717451512,25.7442936213892)) ;
#100288 = CARTESIAN_POINT('Ctrl Pts',(38.3491290417838,264.687914940494,25.6803629116608)) ;
#100289 = CARTESIAN_POINT('Ctrl Pts',(38.3271260734493,264.685112429476,25.6149825030002)) ;
#100290 = CARTESIAN_POINT('Ctrl Pts',(38.3086026758496,264.682309918458,25.5485284734257)) ;
#100291 = CARTESIAN_POINT('Ctrl Pts',(38.2896240881604,264.679438539122,25.4804414164589)) ;
#100292 = CARTESIAN_POINT('Ctrl Pts',(38.2742986221662,264.676567159786,25.4112277197905)) ;
#100293 = CARTESIAN_POINT('Ctrl Pts',(38.2627503035205,264.673695780449,25.3413138801974)) ;
#100294 = CARTESIAN_POINT('Ctrl Pts',(38.2515077943795,264.670900437731,25.2732514197807)) ;
#100295 = CARTESIAN_POINT('Ctrl Pts',(38.2438449491744,264.668105095013,25.2045259531586)) ;
#100296 = CARTESIAN_POINT('Ctrl Pts',(38.239825227063,264.665309752295,25.1355442882526)) ;
#100297 = CARTESIAN_POINT('Ctrl Pts',(38.2358077982496,264.662516004352,25.066601978187)) ;
#100298 = CARTESIAN_POINT('Ctrl Pts',(38.2354293964421,264.659722256409,24.9974042463009)) ;
#100299 = CARTESIAN_POINT('Ctrl Pts',(38.2387016537863,264.656928508466,24.9283631107076)) ;
#100300 = CARTESIAN_POINT('Ctrl Pts',(38.2419731460447,264.654135413729,24.8593381176099)) ;
#100301 = CARTESIAN_POINT('Ctrl Pts',(38.2488935788787,264.651342318992,24.7904701354936)) ;
#100302 = CARTESIAN_POINT('Ctrl Pts',(38.2594225028232,264.648549224255,24.7221694995843)) ;
#100303 = CARTESIAN_POINT('Ctrl Pts',(38.2704651241443,264.645619856766,24.6505365328817)) ;
#100304 = CARTESIAN_POINT('Ctrl Pts',(38.2854773069324,264.642690489278,24.5795282721564)) ;
#100305 = CARTESIAN_POINT('Ctrl Pts',(38.3043517094858,264.639761121789,24.5096077204295)) ;
#100306 = CARTESIAN_POINT('Ctrl Pts',(38.3223689069501,264.636964795265,24.4428626998276)) ;
#100307 = CARTESIAN_POINT('Ctrl Pts',(38.3439049015649,264.63416846874,24.3771091994739)) ;
#100308 = CARTESIAN_POINT('Ctrl Pts',(38.3688154220767,264.631372142216,24.3127335164339)) ;
#100309 = CARTESIAN_POINT('Ctrl Pts',(38.3937419849194,264.628574014862,24.2483163755689)) ;
#100310 = CARTESIAN_POINT('Ctrl Pts',(38.4220471986119,264.625775887508,24.1852792627708)) ;
#100311 = CARTESIAN_POINT('Ctrl Pts',(38.4535396282047,264.622977760155,24.1239862810453)) ;
#100312 = CARTESIAN_POINT('Ctrl Pts',(38.4850805624662,264.620175323123,24.0625988958135)) ;
#100313 = CARTESIAN_POINT('Ctrl Pts',(38.5198182578509,264.617372886091,24.0029614198518)) ;
#100314 = CARTESIAN_POINT('Ctrl Pts',(38.5575171531634,264.614570449059,23.9454103343824)) ;
#100315 = CARTESIAN_POINT('Ctrl Pts',(38.5627798025449,264.614179237502,23.9373763805533)) ;
#100316 = CARTESIAN_POINT('Ctrl Pts',(38.5681000930982,264.613788025946,23.9293830327128)) ;
#100317 = CARTESIAN_POINT('Ctrl Pts',(38.5734773222752,264.613396814389,23.9214311542105)) ;
#100318 = CARTESIAN_POINT('Ctrl Pts',(38.6120240045259,264.610592413263,23.8644280911393)) ;
#100319 = CARTESIAN_POINT('Ctrl Pts',(38.6536411680877,264.607788012137,23.8093498236701)) ;
#100320 = CARTESIAN_POINT('Ctrl Pts',(38.6981100832999,264.60498361101,23.7565441071784)) ;
#100321 = CARTESIAN_POINT('Ctrl Pts',(38.7436373142871,264.602112467938,23.7024816673664)) ;
#100322 = CARTESIAN_POINT('Ctrl Pts',(38.7921535637017,264.599241324865,23.6508018123646)) ;
#100323 = CARTESIAN_POINT('Ctrl Pts',(38.8433765377836,264.596370181792,23.6018468384303)) ;
#100324 = CARTESIAN_POINT('Ctrl Pts',(38.8932818704625,264.593572894974,23.5541511646772)) ;
#100325 = CARTESIAN_POINT('Ctrl Pts',(38.9457559699578,264.590775608155,23.5090422261409)) ;
#100326 = CARTESIAN_POINT('Ctrl Pts',(39.0004980967225,264.587978321337,23.4668019506051)) ;
#100327 = CARTESIAN_POINT('Ctrl Pts',(39.0552092963014,264.585182614877,23.4245855391925)) ;
#100328 = CARTESIAN_POINT('Ctrl Pts',(39.1121855951858,264.582386908417,23.3852348717268)) ;
#100329 = CARTESIAN_POINT('Ctrl Pts',(39.1710927569323,264.579591201957,23.3489919861002)) ;
#100330 = CARTESIAN_POINT('Ctrl Pts',(39.2299863882496,264.576796137646,23.3127574251286)) ;
#100331 = CARTESIAN_POINT('Ctrl Pts',(39.2908095864941,264.574001073334,23.279629483272)) ;
#100332 = CARTESIAN_POINT('Ctrl Pts',(39.3532001618077,264.571206009022,23.2498062216747)) ;
#100333 = CARTESIAN_POINT('Ctrl Pts',(39.4185466133079,264.568278523042,23.2185700244166)) ;
#100334 = CARTESIAN_POINT('Ctrl Pts',(39.4856121449566,264.565351037063,23.1909597123105)) ;
#100335 = CARTESIAN_POINT('Ctrl Pts',(39.5539551010565,264.562423551083,23.1671471481571)) ;
#100336 = CARTESIAN_POINT('Ctrl Pts',(39.6192821921514,264.559625250363,23.1443853942555)) ;
#100337 = CARTESIAN_POINT('Ctrl Pts',(39.6857758327279,264.556826949643,23.1250933516415)) ;
#100338 = CARTESIAN_POINT('Ctrl Pts',(39.7530351849693,264.554028648923,23.1093698462599)) ;
#100339 = CARTESIAN_POINT('Ctrl Pts',(39.8203378155972,264.551228547621,23.0936362235055)) ;
#100340 = CARTESIAN_POINT('Ctrl Pts',(39.8884066590657,264.54842844632,23.0814757934472)) ;
#100341 = CARTESIAN_POINT('Ctrl Pts',(39.9568325990537,264.545628345018,23.0729359191923)) ;
#100342 = CARTESIAN_POINT('Ctrl Pts',(40.0253635085923,264.542823948191,23.0643829442514)) ;
#100343 = CARTESIAN_POINT('Ctrl Pts',(40.0942521223562,264.540019551364,23.0594616370781)) ;
#100344 = CARTESIAN_POINT('Ctrl Pts',(40.1630872342562,264.537215154537,23.0581673444979)) ;
#100345 = CARTESIAN_POINT('Ctrl Pts',(40.1724061279648,264.536835495447,23.0579921232387)) ;
#100346 = CARTESIAN_POINT('Ctrl Pts',(40.1817240472912,264.536455836357,23.0578832990001)) ;
#100347 = CARTESIAN_POINT('Ctrl Pts',(40.1910399792807,264.536076177267,23.0578407872543)) ;
#100348 = CARTESIAN_POINT('Ctrl Pts',(40.2598577696874,264.533271594782,23.0575267484216)) ;
#100349 = CARTESIAN_POINT('Ctrl Pts',(40.328817304762,264.530467012297,23.0608344361905)) ;
#100350 = CARTESIAN_POINT('Ctrl Pts',(40.3975079933341,264.527662429813,23.0677792401863)) ;
#100351 = CARTESIAN_POINT('Ctrl Pts',(40.467828348868,264.52479130941,23.0748888076727)) ;
#100352 = CARTESIAN_POINT('Ctrl Pts',(40.5378664243726,264.521920189007,23.0858103714212)) ;
#100353 = CARTESIAN_POINT('Ctrl Pts',(40.6071804018321,264.519049068604,23.1005037540946)) ;
#100354 = CARTESIAN_POINT('Ctrl Pts',(40.6747167858233,264.516251579597,23.1148203172286)) ;
#100355 = CARTESIAN_POINT('Ctrl Pts',(40.7415652589116,264.513454090589,23.1327174456261)) ;
#100356 = CARTESIAN_POINT('Ctrl Pts',(40.8073233679819,264.510656601582,23.1541056861881)) ;
#100357 = CARTESIAN_POINT('Ctrl Pts',(40.8730444977572,264.507860685751,23.1754818990006)) ;
#100358 = CARTESIAN_POINT('Ctrl Pts',(40.9376760178087,264.505064769921,23.2003451774765)) ;
#100359 = CARTESIAN_POINT('Ctrl Pts',(41.000829537948,264.502268854091,23.2285559136498)) ;
#100360 = CARTESIAN_POINT('Ctrl Pts',(41.0639687081095,264.499473573559,23.2567602396746)) ;
#100361 = CARTESIAN_POINT('Ctrl Pts',(41.1256301007614,264.496678293028,23.2883103137473)) ;
#100362 = CARTESIAN_POINT('Ctrl Pts',(41.1854458883187,264.493883012496,23.323018647395)) ;
#100363 = CARTESIAN_POINT('Ctrl Pts',(41.2480865129882,264.490955723133,23.3593661033044)) ;
#100364 = CARTESIAN_POINT('Ctrl Pts',(41.3087023701218,264.488028433771,23.3991772597833)) ;
#100365 = CARTESIAN_POINT('Ctrl Pts',(41.3669026307358,264.485101144408,23.4421843454955)) ;
#100366 = CARTESIAN_POINT('Ctrl Pts',(41.4225429371107,264.482302612662,23.483299752885)) ;
#100367 = CARTESIAN_POINT('Ctrl Pts',(41.4759753345706,264.479504080915,23.5273354694665)) ;
#100368 = CARTESIAN_POINT('Ctrl Pts',(41.5268921597548,264.476705549169,23.57401614389)) ;
#100369 = CARTESIAN_POINT('Ctrl Pts',(41.5778418347219,264.473905211906,23.6207269350777)) ;
#100370 = CARTESIAN_POINT('Ctrl Pts',(41.6262723664498,264.471104874643,23.6700857326611)) ;
#100371 = CARTESIAN_POINT('Ctrl Pts',(41.6719139265479,264.46830453738,23.7217813318965)) ;
#100372 = CARTESIAN_POINT('Ctrl Pts',(41.7176255853711,264.465499899211,23.773556327971)) ;
#100373 = CARTESIAN_POINT('Ctrl Pts',(41.76053942759,264.462695261042,23.8276749028311)) ;
#100374 = CARTESIAN_POINT('Ctrl Pts',(41.8004274053468,264.459890622873,23.8837947964993)) ;
#100375 = CARTESIAN_POINT('Ctrl Pts',(41.8058085100117,264.459512261963,23.8913656747085)) ;
#100376 = CARTESIAN_POINT('Ctrl Pts',(41.8111346129118,264.459133901054,23.8989729373091)) ;
#100377 = CARTESIAN_POINT('Ctrl Pts',(41.8164052178499,264.458755540145,23.9066157092696)) ;
#100378 = CARTESIAN_POINT('Ctrl Pts',(41.8558043111795,264.455927197487,23.9637473458282)) ;
#100379 = CARTESIAN_POINT('Ctrl Pts',(41.8922413848146,264.453098854829,24.0230724888577)) ;
#100380 = CARTESIAN_POINT('Ctrl Pts',(41.9254686504755,264.450270512171,24.0842556786478)) ;
#100381 = CARTESIAN_POINT('Ctrl Pts',(41.958646693795,264.447446359375,24.1453482326363)) ;
#100382 = CARTESIAN_POINT('Ctrl Pts',(41.9886241443276,264.444622206579,24.2082929534042)) ;
#100383 = CARTESIAN_POINT('Ctrl Pts',(42.0151963518414,264.441798053783,24.2727253567599)) ;
#100384 = CARTESIAN_POINT('Ctrl Pts',(42.0417338908785,264.438977585629,24.3370736958436)) ;
#100385 = CARTESIAN_POINT('Ctrl Pts',(42.0648748369969,264.436157117475,24.4029054215471)) ;
#100386 = CARTESIAN_POINT('Ctrl Pts',(42.0844611807787,264.433336649321,24.4698329836516)) ;
#100387 = CARTESIAN_POINT('Ctrl Pts',(42.1040323458009,264.430518366936,24.5367086791402)) ;
#100388 = CARTESIAN_POINT('Ctrl Pts',(42.1200542458913,264.42770008455,24.6046780688452)) ;
#100389 = CARTESIAN_POINT('Ctrl Pts',(42.132418041646,264.424881802164,24.6733364900244)) ;
#100390 = CARTESIAN_POINT('Ctrl Pts',(42.1447777802695,264.422064444587,24.7419723812117)) ;
#100391 = CARTESIAN_POINT('Ctrl Pts',(42.1534817087956,264.41924708701,24.8112963876716)) ;
#100392 = CARTESIAN_POINT('Ctrl Pts',(42.1584719621315,264.416429729432,24.8808930543848)) ;
#100393 = CARTESIAN_POINT('Ctrl Pts',(42.161847349748,264.414524079912,24.927967964448)) ;
#100394 = CARTESIAN_POINT('Ctrl Pts',(42.1635247492932,264.412618430391,24.975167391973)) ;
#100395 = CARTESIAN_POINT('Ctrl Pts',(42.1634997239518,264.41071278087,25.0223615166147)) ;
#100396 = CARTESIAN_POINT('',(42.1634998081267,263.910712780839,25.0204523075086)) ;
#100397 = CARTESIAN_POINT('Ctrl Pts',(42.1634997239514,264.410712780843,25.0223615172765)) ;
#100398 = CARTESIAN_POINT('Ctrl Pts',(42.163458777492,264.407594759394,25.0995804871246)) ;
#100399 = CARTESIAN_POINT('Ctrl Pts',(42.1588584816758,264.404476737946,25.176643865133)) ;
#100400 = CARTESIAN_POINT('Ctrl Pts',(42.1497783422879,264.401358716497,25.2530457542185)) ;
#100401 = CARTESIAN_POINT('Ctrl Pts',(42.1406617510449,264.398228177876,25.329754355621)) ;
#100402 = CARTESIAN_POINT('Ctrl Pts',(42.1270294057865,264.395097639255,25.4057958914338)) ;
#100403 = CARTESIAN_POINT('Ctrl Pts',(42.1090116562539,264.391967100634,25.4806750499541)) ;
#100404 = CARTESIAN_POINT('Ctrl Pts',(42.0909101969885,264.388822017658,25.555902094005)) ;
#100405 = CARTESIAN_POINT('Ctrl Pts',(42.0683826202559,264.385676934682,25.6299556886429)) ;
#100406 = CARTESIAN_POINT('Ctrl Pts',(42.0416093908855,264.382531851706,25.7023541910313)) ;
#100407 = CARTESIAN_POINT('Ctrl Pts',(42.0384967163878,264.382166202145,25.7107712918952)) ;
#100408 = CARTESIAN_POINT('Ctrl Pts',(42.0353267074247,264.381800552583,25.7191660468239)) ;
#100409 = CARTESIAN_POINT('Ctrl Pts',(42.0320996884114,264.381434903022,25.727537719247)) ;
#100410 = CARTESIAN_POINT('Ctrl Pts',(42.0073503843503,264.378630589774,25.7917434352487)) ;
#100411 = CARTESIAN_POINT('Ctrl Pts',(41.9791767836945,264.375826276526,25.8547637148073)) ;
#100412 = CARTESIAN_POINT('Ctrl Pts',(41.9477138619951,264.373021963277,25.9162105639722)) ;
#100413 = CARTESIAN_POINT('Ctrl Pts',(41.9155010215255,264.37015080922,25.9791219988485)) ;
#100414 = CARTESIAN_POINT('Ctrl Pts',(41.8798401431771,264.367279655162,26.0403835214419)) ;
#100415 = CARTESIAN_POINT('Ctrl Pts',(41.8409293882998,264.364408501105,26.0995981336555)) ;
#100416 = CARTESIAN_POINT('Ctrl Pts',(41.8030208276166,264.36161129714,26.157287600938)) ;
#100417 = CARTESIAN_POINT('Ctrl Pts',(41.7620280728643,264.358814093176,26.2130338974303)) ;
#100418 = CARTESIAN_POINT('Ctrl Pts',(41.7181808066942,264.356016889211,26.2664947442704)) ;
#100419 = CARTESIAN_POINT('Ctrl Pts',(41.6743582796633,264.353221263461,26.3199254278767)) ;
#100420 = CARTESIAN_POINT('Ctrl Pts',(41.6276847458526,264.350425637712,26.3710728446154)) ;
#100421 = CARTESIAN_POINT('Ctrl Pts',(41.5784314916249,264.347630011962,26.4196260586651)) ;
#100422 = CARTESIAN_POINT('Ctrl Pts',(41.529189509994,264.344835026048,26.4681681603364)) ;
#100423 = CARTESIAN_POINT('Ctrl Pts',(41.4773693277752,264.342040040133,26.5141168967294)) ;
#100424 = CARTESIAN_POINT('Ctrl Pts',(41.4232793512456,264.339245054219,26.5571979033983)) ;
#100425 = CARTESIAN_POINT('Ctrl Pts',(41.3666236239985,264.336317488525,26.6023224517891)) ;
#100426 = CARTESIAN_POINT('Ctrl Pts',(41.3074778346146,264.333389922832,26.6443000433091)) ;
#100427 = CARTESIAN_POINT('Ctrl Pts',(41.246233771239,264.330462357139,26.6828639469354)) ;
#100428 = CARTESIAN_POINT('Ctrl Pts',(41.1876954001309,264.327664127931,26.7197241416617)) ;
#100429 = CARTESIAN_POINT('Ctrl Pts',(41.1272407212263,264.324865898722,26.7534657207546)) ;
#100430 = CARTESIAN_POINT('Ctrl Pts',(41.0652380983901,264.322067669514,26.7839023368564)) ;
#100431 = CARTESIAN_POINT('Ctrl Pts',(41.0031955236829,264.319267637244,26.814358565028)) ;
#100432 = CARTESIAN_POINT('Ctrl Pts',(40.9396034679074,264.316467604975,26.8415054008056)) ;
#100433 = CARTESIAN_POINT('Ctrl Pts',(40.8748499230125,264.313667572706,26.8652047844642)) ;
#100434 = CARTESIAN_POINT('Ctrl Pts',(40.8099969463639,264.310863240871,26.8889405595093)) ;
#100435 = CARTESIAN_POINT('Ctrl Pts',(40.7439793882218,264.308058909036,26.9092181818454)) ;
#100436 = CARTESIAN_POINT('Ctrl Pts',(40.6771989624199,264.305254577201,26.9259498089059)) ;
#100437 = CARTESIAN_POINT('Ctrl Pts',(40.6681474332564,264.304874473434,26.9282176412606)) ;
#100438 = CARTESIAN_POINT('Ctrl Pts',(40.659081900542,264.304494369668,26.9304204057263)) ;
#100439 = CARTESIAN_POINT('Ctrl Pts',(40.650003373869,264.304114265901,26.9325579566016)) ;
#100440 = CARTESIAN_POINT('Ctrl Pts',(40.5830244210172,264.301309961504,26.9483282378873)) ;
#100441 = CARTESIAN_POINT('Ctrl Pts',(40.5150933063956,264.298505657107,26.9606021865817)) ;
#100442 = CARTESIAN_POINT('Ctrl Pts',(40.4466065577867,264.29570135271,26.9692724619795)) ;
#100443 = CARTESIAN_POINT('Ctrl Pts',(40.3764871791172,264.292830197546,26.9781494248393)) ;
#100444 = CARTESIAN_POINT('Ctrl Pts',(40.3057858146515,264.289959042382,26.9832484865257)) ;
#100445 = CARTESIAN_POINT('Ctrl Pts',(40.2349420653057,264.287087887218,26.9845094078303)) ;
#100446 = CARTESIAN_POINT('Ctrl Pts',(40.16592320119,264.284290690995,26.9857378486877)) ;
#100447 = CARTESIAN_POINT('Ctrl Pts',(40.0967697192689,264.281493494772,26.9833234985888)) ;
#100448 = CARTESIAN_POINT('Ctrl Pts',(40.0278938043149,264.278696298549,26.9772630082118)) ;
#100449 = CARTESIAN_POINT('Ctrl Pts',(39.9590567393324,264.275900680105,26.9712059362994)) ;
#100450 = CARTESIAN_POINT('Ctrl Pts',(39.8904974152564,264.273105061661,26.9615068481148)) ;
#100451 = CARTESIAN_POINT('Ctrl Pts',(39.8226255951793,264.270309443217,26.9482144269451)) ;
#100452 = CARTESIAN_POINT('Ctrl Pts',(39.7547692980579,264.267514464159,26.9349250458835)) ;
#100453 = CARTESIAN_POINT('Ctrl Pts',(39.6876006707138,264.264719485101,26.9180440580319)) ;
#100454 = CARTESIAN_POINT('Ctrl Pts',(39.6215202082828,264.261924506042,26.897671424934)) ;
#100455 = CARTESIAN_POINT('Ctrl Pts',(39.5523048830281,264.258996932937,26.876332312369)) ;
#100456 = CARTESIAN_POINT('Ctrl Pts',(39.4842841046609,264.256069359832,26.8511621497015)) ;
#100457 = CARTESIAN_POINT('Ctrl Pts',(39.4178990926936,264.253141786726,26.8223340638823)) ;
#100458 = CARTESIAN_POINT('Ctrl Pts',(39.3544471827243,264.250343563158,26.7947796950303)) ;
#100459 = CARTESIAN_POINT('Ctrl Pts',(39.2924899691217,264.247545339589,26.7638841088208)) ;
#100460 = CARTESIAN_POINT('Ctrl Pts',(39.2323890731672,264.24474711602,26.7298464171897)) ;
#100461 = CARTESIAN_POINT('Ctrl Pts',(39.1722494414693,264.241947088962,26.6957867878608)) ;
#100462 = CARTESIAN_POINT('Ctrl Pts',(39.1139689189766,264.239147061905,26.6585812848545)) ;
#100463 = CARTESIAN_POINT('Ctrl Pts',(39.0578803190547,264.236347034848,26.6184724604218)) ;
#100464 = CARTESIAN_POINT('Ctrl Pts',(39.0017055797137,264.233542707581,26.5783020378954)) ;
#100465 = CARTESIAN_POINT('Ctrl Pts',(38.9477298566808,264.230738380315,26.535219704408)) ;
#100466 = CARTESIAN_POINT('Ctrl Pts',(38.8962522312928,264.227934053049,26.489507663213)) ;
#100467 = CARTESIAN_POINT('Ctrl Pts',(38.8892741663483,264.227553911625,26.4833111537625)) ;
#100468 = CARTESIAN_POINT('Ctrl Pts',(38.882341947018,264.227173770202,26.4770663760187)) ;
#100469 = CARTESIAN_POINT('Ctrl Pts',(38.8754562631737,264.226793628778,26.4707740817777)) ;
#100470 = CARTESIAN_POINT('Ctrl Pts',(38.8246612808289,264.22398936455,26.424356473576)) ;
#100471 = CARTESIAN_POINT('Ctrl Pts',(38.7762165292526,264.221185100322,26.3751808753811)) ;
#100472 = CARTESIAN_POINT('Ctrl Pts',(38.7304342718421,264.218380836093,26.3235141926557)) ;
#100473 = CARTESIAN_POINT('Ctrl Pts',(38.6835598748704,264.215509675908,26.2706149969134)) ;
#100474 = CARTESIAN_POINT('Ctrl Pts',(38.6394770748674,264.212638515723,26.2151046178442)) ;
#100475 = CARTESIAN_POINT('Ctrl Pts',(38.5984835450502,264.209767355539,26.1573121104862)) ;
#100476 = CARTESIAN_POINT('Ctrl Pts',(38.5585466517975,264.206970201492,26.1010092449497)) ;
#100477 = CARTESIAN_POINT('Ctrl Pts',(38.5215419890435,264.204173047445,26.0425409069009)) ;
#100478 = CARTESIAN_POINT('Ctrl Pts',(38.487704774341,264.201375893399,25.9822455800819)) ;
#100479 = CARTESIAN_POINT('Ctrl Pts',(38.4538866535994,264.198580317754,25.9219842772399)) ;
#100480 = CARTESIAN_POINT('Ctrl Pts',(38.4232326720322,264.195784742111,25.8598984558136)) ;
#100481 = CARTESIAN_POINT('Ctrl Pts',(38.3959337131029,264.192989166466,25.796353944432)) ;
#100482 = CARTESIAN_POINT('Ctrl Pts',(38.3686410031823,264.190194230758,25.7328239790339)) ;
#100483 = CARTESIAN_POINT('Ctrl Pts',(38.3447019826041,264.18739929505,25.6678364346535)) ;
#100484 = CARTESIAN_POINT('Ctrl Pts',(38.3242599624995,264.184604359341,25.6017784055398)) ;
#100485 = CARTESIAN_POINT('Ctrl Pts',(38.3028475401916,264.181676745368,25.5325845387411)) ;
#100486 = CARTESIAN_POINT('Ctrl Pts',(38.2852726126217,264.178749131394,25.4622165629685)) ;
#100487 = CARTESIAN_POINT('Ctrl Pts',(38.2716410456622,264.17582151742,25.3911365049494)) ;
#100488 = CARTESIAN_POINT('Ctrl Pts',(38.2586121526955,264.173023338074,25.3231990131888)) ;
#100489 = CARTESIAN_POINT('Ctrl Pts',(38.2491852999413,264.170225158729,25.254611589662)) ;
#100490 = CARTESIAN_POINT('Ctrl Pts',(38.2433999949789,264.167426979383,25.1857851432934)) ;
#100491 = CARTESIAN_POINT('Ctrl Pts',(38.2376109617994,264.164626996811,25.1169143431799)) ;
#100492 = CARTESIAN_POINT('Ctrl Pts',(38.2354681618351,264.161827014238,25.0478047004715)) ;
#100493 = CARTESIAN_POINT('Ctrl Pts',(38.2369589830322,264.159027031665,24.9788678324192)) ;
#100494 = CARTESIAN_POINT('Ctrl Pts',(38.2384520937988,264.156222748942,24.9098250926849)) ;
#100495 = CARTESIAN_POINT('Ctrl Pts',(38.2435899192609,264.153418466219,24.8409561416085)) ;
#100496 = CARTESIAN_POINT('Ctrl Pts',(38.2523080800396,264.150614183497,24.7726671012301)) ;
#100497 = CARTESIAN_POINT('Ctrl Pts',(38.2534906871367,264.150233786216,24.7634037822969)) ;
#100498 = CARTESIAN_POINT('Ctrl Pts',(38.2547390979433,264.149853388936,24.7541511165292)) ;
#100499 = CARTESIAN_POINT('Ctrl Pts',(38.2560530801867,264.149472991656,24.7449100996315)) ;
#100500 = CARTESIAN_POINT('Ctrl Pts',(38.2657397501837,264.146668704961,24.676785373007)) ;
#100501 = CARTESIAN_POINT('Ctrl Pts',(38.2790294654451,264.143864418266,24.6090461664029)) ;
#100502 = CARTESIAN_POINT('Ctrl Pts',(38.2958779051084,264.141060131571,24.5421008763572)) ;
#100503 = CARTESIAN_POINT('Ctrl Pts',(38.3131281106275,264.138188974194,24.4735592170166)) ;
#100504 = CARTESIAN_POINT('Ctrl Pts',(38.3341089620186,264.135317816818,24.4058503462897)) ;
#100505 = CARTESIAN_POINT('Ctrl Pts',(38.3587165892024,264.132446659441,24.3394056486588)) ;
#100506 = CARTESIAN_POINT('Ctrl Pts',(38.3826901607964,264.12964948211,24.2746730068728)) ;
#100507 = CARTESIAN_POINT('Ctrl Pts',(38.4101056754069,264.126852304779,24.2111406621024)) ;
#100508 = CARTESIAN_POINT('Ctrl Pts',(38.4408162530818,264.124055127449,24.1491937503526)) ;
#100509 = CARTESIAN_POINT('Ctrl Pts',(38.4715095038536,264.121259528285,24.0872817890406)) ;
#100510 = CARTESIAN_POINT('Ctrl Pts',(38.5054939122858,264.118463929121,24.026953921516)) ;
#100511 = CARTESIAN_POINT('Ctrl Pts',(38.542575014903,264.115668329957,23.9685740926633)) ;
#100512 = CARTESIAN_POINT('Ctrl Pts',(38.5796476319375,264.112873370534,23.9102076233611)) ;
#100513 = CARTESIAN_POINT('Ctrl Pts',(38.6198152742216,264.110078411111,23.8537887184565)) ;
#100514 = CARTESIAN_POINT('Ctrl Pts',(38.6628390888999,264.107283451688,23.7996540293043)) ;
#100515 = CARTESIAN_POINT('Ctrl Pts',(38.7079045557083,264.104355860258,23.7429504325776)) ;
#100516 = CARTESIAN_POINT('Ctrl Pts',(38.7561036911565,264.101428268829,23.6887537206051)) ;
#100517 = CARTESIAN_POINT('Ctrl Pts',(38.8071146606288,264.098500677399,23.6374118634335)) ;
#100518 = CARTESIAN_POINT('Ctrl Pts',(38.8558711435674,264.095702474129,23.5883391167457)) ;
#100519 = CARTESIAN_POINT('Ctrl Pts',(38.9071957379641,264.092904270859,23.541874496539)) ;
#100520 = CARTESIAN_POINT('Ctrl Pts',(38.9607713858759,264.090106067589,23.498282362439)) ;
#100521 = CARTESIAN_POINT('Ctrl Pts',(39.0143815601378,264.087306061042,23.4546621357755)) ;
#100522 = CARTESIAN_POINT('Ctrl Pts',(39.0702452814918,264.084506054495,23.4139183662745)) ;
#100523 = CARTESIAN_POINT('Ctrl Pts',(39.1280155143677,264.081706047947,23.3762727720397)) ;
#100524 = CARTESIAN_POINT('Ctrl Pts',(39.1858744666936,264.078901741348,23.3385693643558)) ;
#100525 = CARTESIAN_POINT('Ctrl Pts',(39.2456453492233,264.076097434748,23.3039738648127)) ;
#100526 = CARTESIAN_POINT('Ctrl Pts',(39.3069564703197,264.073293128148,23.2726621425105)) ;
#100527 = CARTESIAN_POINT('Ctrl Pts',(39.3152701248978,264.072912870277,23.2684163411158)) ;
#100528 = CARTESIAN_POINT('Ctrl Pts',(39.3236120708399,264.072532612405,23.2642308447827)) ;
#100529 = CARTESIAN_POINT('Ctrl Pts',(39.3319813559531,264.072152354534,23.2601060228175)) ;
#100530 = CARTESIAN_POINT('Ctrl Pts',(39.3937022339776,264.069348070849,23.2296867420853)) ;
#100531 = CARTESIAN_POINT('Ctrl Pts',(39.4571366665362,264.066543787163,23.2024603023848)) ;
#100532 = CARTESIAN_POINT('Ctrl Pts',(39.5219224013884,264.063739503478,23.1786204167508)) ;
#100533 = CARTESIAN_POINT('Ctrl Pts',(39.5882530889276,264.060868345726,23.1542120186896)) ;
#100534 = CARTESIAN_POINT('Ctrl Pts',(39.6559999355778,264.057997187973,23.1333540793622)) ;
#100535 = CARTESIAN_POINT('Ctrl Pts',(39.7247481213259,264.05512603022,23.1162040999102)) ;
#100536 = CARTESIAN_POINT('Ctrl Pts',(39.7917248172262,264.0523288559,23.0994960377853)) ;
#100537 = CARTESIAN_POINT('Ctrl Pts',(39.8596513637146,264.049531681581,23.0863072672656)) ;
#100538 = CARTESIAN_POINT('Ctrl Pts',(39.9281268794345,264.046734507261,23.0767336891999)) ;
#100539 = CARTESIAN_POINT('Ctrl Pts',(39.9965637614437,264.0439389111,23.0671655125224)) ;
#100540 = CARTESIAN_POINT('Ctrl Pts',(40.0655485162028,264.041143314939,23.0612085479421)) ;
#100541 = CARTESIAN_POINT('Ctrl Pts',(40.1346709276571,264.038347718779,23.0589074506375)) ;
#100542 = CARTESIAN_POINT('Ctrl Pts',(40.203777521568,264.035552762344,23.0566068799017)) ;
#100543 = CARTESIAN_POINT('Ctrl Pts',(40.2730212226455,264.03275780591,23.057960530788)) ;
#100544 = CARTESIAN_POINT('Ctrl Pts',(40.3419893209184,264.029962849476,23.0629610091306)) ;
#100545 = CARTESIAN_POINT('Ctrl Pts',(40.414230380419,264.027035255138,23.0681987909823)) ;
#100546 = CARTESIAN_POINT('Ctrl Pts',(40.486168446313,264.024107660799,23.0774381490376)) ;
#100547 = CARTESIAN_POINT('Ctrl Pts',(40.5573346615202,264.02118006646,23.0906095444816)) ;
#100548 = CARTESIAN_POINT('Ctrl Pts',(40.625355468153,264.018381866109,23.1031987898135)) ;
#100549 = CARTESIAN_POINT('Ctrl Pts',(40.6926707318042,264.015583665757,23.1193796467942)) ;
#100550 = CARTESIAN_POINT('Ctrl Pts',(40.7588833384476,264.012785465405,23.1390393698456)) ;
#100551 = CARTESIAN_POINT('Ctrl Pts',(40.8251386159097,264.009985461749,23.1587117626365)) ;
#100552 = CARTESIAN_POINT('Ctrl Pts',(40.8902893632423,264.007185458093,23.1818673202467)) ;
#100553 = CARTESIAN_POINT('Ctrl Pts',(40.953956774569,264.004385454437,23.2083444937256)) ;
#100554 = CARTESIAN_POINT('Ctrl Pts',(41.0177219632648,264.001581150669,23.2348623295827)) ;
#100555 = CARTESIAN_POINT('Ctrl Pts',(41.0799988342206,263.998776846901,23.2647117450629)) ;
#100556 = CARTESIAN_POINT('Ctrl Pts',(41.1404325395613,263.995972543133,23.2976849736121)) ;
#100557 = CARTESIAN_POINT('Ctrl Pts',(41.1486276010531,263.995592267892,23.3021562803774)) ;
#100558 = CARTESIAN_POINT('Ctrl Pts',(41.1567888136466,263.995211992652,23.306684964509)) ;
#100559 = CARTESIAN_POINT('Ctrl Pts',(41.1649153352637,263.994831717412,23.3112704478627)) ;
#100560 = CARTESIAN_POINT('Ctrl Pts',(41.2248431157155,263.992027436295,23.3450853877143)) ;
#100561 = CARTESIAN_POINT('Ctrl Pts',(41.2831005702371,263.989223155179,23.3821159857416)) ;
#100562 = CARTESIAN_POINT('Ctrl Pts',(41.3393234378276,263.986418874063,23.4221723347697)) ;
#100563 = CARTESIAN_POINT('Ctrl Pts',(41.3968871176164,263.983547715989,23.4631839542011)) ;
#100564 = CARTESIAN_POINT('Ctrl Pts',(41.4523174277952,263.980676557915,23.5073673238773)) ;
#100565 = CARTESIAN_POINT('Ctrl Pts',(41.5052503649183,263.977805399841,23.5544687031812)) ;
#100566 = CARTESIAN_POINT('Ctrl Pts',(41.5568192802853,263.975008228254,23.6003563333603)) ;
#100567 = CARTESIAN_POINT('Ctrl Pts',(41.6060175953642,263.972211056668,23.6490130484477)) ;
#100568 = CARTESIAN_POINT('Ctrl Pts',(41.6525400386672,263.969413885081,23.7001618799116)) ;
#100569 = CARTESIAN_POINT('Ctrl Pts',(41.6990362332188,263.966618291706,23.7512818523374)) ;
#100570 = CARTESIAN_POINT('Ctrl Pts',(41.7428592247573,263.963822698331,23.8048907908515)) ;
#100571 = CARTESIAN_POINT('Ctrl Pts',(41.7837407967197,263.961027104956,23.8606751183484)) ;
#100572 = CARTESIAN_POINT('Ctrl Pts',(41.8246130128812,263.958232151356,23.9164466795294)) ;
#100573 = CARTESIAN_POINT('Ctrl Pts',(41.8625448586599,263.955437197757,23.9743922477505)) ;
#100574 = CARTESIAN_POINT('Ctrl Pts',(41.8973096939531,263.952642244157,24.0341668333026)) ;
#100575 = CARTESIAN_POINT('Ctrl Pts',(41.9337244047851,263.949714647168,24.0967782114271)) ;
#100576 = CARTESIAN_POINT('Ctrl Pts',(41.9666636898901,263.946787050179,24.1613960540462)) ;
#100577 = CARTESIAN_POINT('Ctrl Pts',(41.995920563786,263.94385945319,24.2275939558348)) ;
#100578 = CARTESIAN_POINT('Ctrl Pts',(42.0238842861241,263.941061255761,24.2908659154972)) ;
#100579 = CARTESIAN_POINT('Ctrl Pts',(42.0484841324827,263.938263058332,24.3555807041393)) ;
#100580 = CARTESIAN_POINT('Ctrl Pts',(42.069589258488,263.935464860903,24.4213467986874)) ;
#100581 = CARTESIAN_POINT('Ctrl Pts',(42.0907079855291,263.932664860197,24.4871552756885)) ;
#100582 = CARTESIAN_POINT('Ctrl Pts',(42.1083273859935,263.929864859491,24.5540159359917)) ;
#100583 = CARTESIAN_POINT('Ctrl Pts',(42.1223672427004,263.927064858785,24.621524853099)) ;
#100584 = CARTESIAN_POINT('Ctrl Pts',(42.1364286610765,263.924260557987,24.6891374468305)) ;
#100585 = CARTESIAN_POINT('Ctrl Pts',(42.1468994981384,263.921456257188,24.7573998024067)) ;
#100586 = CARTESIAN_POINT('Ctrl Pts',(42.1537512147579,263.918651956389,24.8259017138642)) ;
#100587 = CARTESIAN_POINT('Ctrl Pts',(42.1546803780079,263.918271664356,24.8351912776649)) ;
#100588 = CARTESIAN_POINT('Ctrl Pts',(42.1555430635202,263.917891372322,24.8444852468158)) ;
#100589 = CARTESIAN_POINT('Ctrl Pts',(42.1563392738469,263.917511080289,24.8537825997396)) ;
#100590 = CARTESIAN_POINT('Ctrl Pts',(42.1610837646848,263.915244980483,24.9091840486851)) ;
#100591 = CARTESIAN_POINT('Ctrl Pts',(42.163475200471,263.912978880676,24.9647897749953)) ;
#100592 = CARTESIAN_POINT('Ctrl Pts',(42.1634998081263,263.91071278087,25.0204523067486)) ;
#100593 = CARTESIAN_POINT('',(42.1634999347757,263.410712780838,25.0218264420184)) ;
#100594 = CARTESIAN_POINT('Ctrl Pts',(42.1634998081267,263.910712780839,25.0204523075086)) ;
#100595 = CARTESIAN_POINT('Ctrl Pts',(42.1635299115909,263.907940573848,25.0885464220032)) ;
#100596 = CARTESIAN_POINT('Ctrl Pts',(42.1600135022032,263.905168366856,25.1567718338227)) ;
#100597 = CARTESIAN_POINT('Ctrl Pts',(42.1529358967757,263.902396159865,25.2247254395744)) ;
#100598 = CARTESIAN_POINT('Ctrl Pts',(42.145868575163,263.899627980912,25.2925803082184)) ;
#100599 = CARTESIAN_POINT('Ctrl Pts',(42.135250383065,263.896859801958,25.3601636613063)) ;
#100600 = CARTESIAN_POINT('Ctrl Pts',(42.1211186552297,263.894091623005,25.4270731778424)) ;
#100601 = CARTESIAN_POINT('Ctrl Pts',(42.1069981500108,263.891325642382,25.4939295586369)) ;
#100602 = CARTESIAN_POINT('Ctrl Pts',(42.0893697436254,263.888559661759,25.5601126766334)) ;
#100603 = CARTESIAN_POINT('Ctrl Pts',(42.0683222959035,263.885793681136,25.6252276614734)) ;
#100604 = CARTESIAN_POINT('Ctrl Pts',(42.0472840797745,263.883028913697,25.6903140863168)) ;
#100605 = CARTESIAN_POINT('Ctrl Pts',(42.0228299507088,263.880264146257,25.7543328324265)) ;
#100606 = CARTESIAN_POINT('Ctrl Pts',(41.9950988482286,263.877499378817,25.8169033845355)) ;
#100607 = CARTESIAN_POINT('Ctrl Pts',(41.967370049988,263.874734841108,25.8794687375166)) ;
#100608 = CARTESIAN_POINT('Ctrl Pts',(41.936365023349,263.871970303399,25.9405856794601)) ;
#100609 = CARTESIAN_POINT('Ctrl Pts',(41.9022703963241,263.86920576569,25.999894688103)) ;
#100610 = CARTESIAN_POINT('Ctrl Pts',(41.8681453554388,263.866438761896,26.0592566029093)) ;
#100611 = CARTESIAN_POINT('Ctrl Pts',(41.8309254621913,263.863671758102,26.1168069310684)) ;
#100612 = CARTESIAN_POINT('Ctrl Pts',(41.7908421858289,263.860904754307,26.1722127754519)) ;
#100613 = CARTESIAN_POINT('Ctrl Pts',(41.7507389843784,263.858136375057,26.2276461616541)) ;
#100614 = CARTESIAN_POINT('Ctrl Pts',(41.7077698807821,263.855367995806,26.2809325532818)) ;
#100615 = CARTESIAN_POINT('Ctrl Pts',(41.66220660755,263.852599616555,26.3317722071689)) ;
#100616 = CARTESIAN_POINT('Ctrl Pts',(41.6165695611983,263.849826754923,26.3826941773516)) ;
#100617 = CARTESIAN_POINT('Ctrl Pts',(41.5683303152164,263.847053893291,26.4311611497577)) ;
#100618 = CARTESIAN_POINT('Ctrl Pts',(41.5177966623674,263.844281031659,26.476911016329)) ;
#100619 = CARTESIAN_POINT('Ctrl Pts',(41.4929471980248,263.842917502162,26.4994080972632)) ;
#100620 = CARTESIAN_POINT('Ctrl Pts',(41.4675434202115,263.841553972664,26.5212487856042)) ;
#100621 = CARTESIAN_POINT('Ctrl Pts',(41.4416245545341,263.840190443167,26.5424057177507)) ;
#100622 = CARTESIAN_POINT('Ctrl Pts',(41.3883188809768,263.837386159247,26.585917827135)) ;
#100623 = CARTESIAN_POINT('Ctrl Pts',(41.3326259359026,263.834581875326,26.6267038710564)) ;
#100624 = CARTESIAN_POINT('Ctrl Pts',(41.274855170085,263.831777591406,26.6644936799248)) ;
#100625 = CARTESIAN_POINT('Ctrl Pts',(41.215706743906,263.828906433682,26.7031846629598)) ;
#100626 = CARTESIAN_POINT('Ctrl Pts',(41.1543804641331,263.826035275959,26.7387342754357)) ;
#100627 = CARTESIAN_POINT('Ctrl Pts',(41.0912451427048,263.823164118236,26.7708958193837)) ;
#100628 = CARTESIAN_POINT('Ctrl Pts',(41.0297366771451,263.820366943818,26.8022286323562)) ;
#100629 = CARTESIAN_POINT('Ctrl Pts',(40.966511742001,263.817569769401,26.8303456470779)) ;
#100630 = CARTESIAN_POINT('Ctrl Pts',(40.9019394111395,263.814772594983,26.8550633225752)) ;
#100631 = CARTESIAN_POINT('Ctrl Pts',(40.8374035129998,263.811976998775,26.8797670519724)) ;
#100632 = CARTESIAN_POINT('Ctrl Pts',(40.7715221821602,263.809181402567,26.9010750743841)) ;
#100633 = CARTESIAN_POINT('Ctrl Pts',(40.7046851052687,263.80638580636,26.9188516857302)) ;
#100634 = CARTESIAN_POINT('Ctrl Pts',(40.6378633241782,263.80359084993,26.9366242288627)) ;
#100635 = CARTESIAN_POINT('Ctrl Pts',(40.5700867023821,263.8007958935,26.9508668411144)) ;
#100636 = CARTESIAN_POINT('Ctrl Pts',(40.5017590541382,263.79800093707,26.9614939758012)) ;
#100637 = CARTESIAN_POINT('Ctrl Pts',(40.430188839982,263.795073342818,26.9726254331973)) ;
#100638 = CARTESIAN_POINT('Ctrl Pts',(40.3580145641661,263.792145748566,26.9797895834629)) ;
#100639 = CARTESIAN_POINT('Ctrl Pts',(40.2857087180477,263.789218154314,26.9829488164491)) ;
#100640 = CARTESIAN_POINT('Ctrl Pts',(40.2165986511779,263.786419954093,26.9859684174171)) ;
#100641 = CARTESIAN_POINT('Ctrl Pts',(40.1473689089545,263.783621753873,26.9853297205025)) ;
#100642 = CARTESIAN_POINT('Ctrl Pts',(40.0784317851542,263.780823553653,26.9810533404597)) ;
#100643 = CARTESIAN_POINT('Ctrl Pts',(40.009450235794,263.778023550172,26.976774204564)) ;
#100644 = CARTESIAN_POINT('Ctrl Pts',(39.9407621639637,263.775223546692,26.9688527759084)) ;
#100645 = CARTESIAN_POINT('Ctrl Pts',(39.8727729916271,263.772423543211,26.9573613387328)) ;
#100646 = CARTESIAN_POINT('Ctrl Pts',(39.8046794062305,263.769619239678,26.9458522538042)) ;
#100647 = CARTESIAN_POINT('Ctrl Pts',(39.7372873353663,263.766814936146,26.9307623320496)) ;
#100648 = CARTESIAN_POINT('Ctrl Pts',(39.6709892427341,263.764010632614,26.9122142773108)) ;
#100649 = CARTESIAN_POINT('Ctrl Pts',(39.6619989385297,263.763630357091,26.9096990819577)) ;
#100650 = CARTESIAN_POINT('Ctrl Pts',(39.6530287225328,263.763250081568,26.9071203697549)) ;
#100651 = CARTESIAN_POINT('Ctrl Pts',(39.6440795452144,263.762869806046,26.904478514811)) ;
#100652 = CARTESIAN_POINT('Ctrl Pts',(39.5780851337236,263.760065519301,26.8849965383051)) ;
#100653 = CARTESIAN_POINT('Ctrl Pts',(39.5129956509329,263.757261232556,26.8620057637291)) ;
#100654 = CARTESIAN_POINT('Ctrl Pts',(39.4492087201761,263.754456945811,26.8356093790058)) ;
#100655 = CARTESIAN_POINT('Ctrl Pts',(39.3839007352826,263.75158578844,26.8085835498226)) ;
#100656 = CARTESIAN_POINT('Ctrl Pts',(39.3199587410339,263.74871463107,26.7779876613632)) ;
#100657 = CARTESIAN_POINT('Ctrl Pts',(39.2577944526421,263.7458434737,26.7439871588573)) ;
#100658 = CARTESIAN_POINT('Ctrl Pts',(39.1972319277987,263.743046296348,26.710862734353)) ;
#100659 = CARTESIAN_POINT('Ctrl Pts',(39.1383570555545,263.740249118996,26.6745072863799)) ;
#100660 = CARTESIAN_POINT('Ctrl Pts',(39.08152954437,263.737451941645,26.635122094049)) ;
#100661 = CARTESIAN_POINT('Ctrl Pts',(39.0247340954781,263.734656342471,26.5957591229898)) ;
#100662 = CARTESIAN_POINT('Ctrl Pts',(38.9699841151777,263.731860743297,26.5533700769759)) ;
#100663 = CARTESIAN_POINT('Ctrl Pts',(38.9176114321015,263.729065144123,26.5082002347826)) ;
#100664 = CARTESIAN_POINT('Ctrl Pts',(38.8652507341125,263.726270184701,26.4630407293614)) ;
#100665 = CARTESIAN_POINT('Ctrl Pts',(38.8152666216021,263.723475225279,26.4151020100986)) ;
#100666 = CARTESIAN_POINT('Ctrl Pts',(38.7679574698095,263.720680265856,26.3646693085443)) ;
#100667 = CARTESIAN_POINT('Ctrl Pts',(38.7184033097922,263.717752674445,26.3118433738525)) ;
#100668 = CARTESIAN_POINT('Ctrl Pts',(38.6717847350701,263.714825083034,26.2562812576785)) ;
#100669 = CARTESIAN_POINT('Ctrl Pts',(38.6283992627555,263.711897491623,26.1983519373125)) ;
#100670 = CARTESIAN_POINT('Ctrl Pts',(38.5869312597987,263.709099288381,26.1429828678969)) ;
#100671 = CARTESIAN_POINT('Ctrl Pts',(38.5484168377012,263.706301085138,26.0854518825699)) ;
#100672 = CARTESIAN_POINT('Ctrl Pts',(38.5130714843996,263.703502881896,26.0261110845869)) ;
#100673 = CARTESIAN_POINT('Ctrl Pts',(38.4777033532163,263.700702875386,25.9667320451507)) ;
#100674 = CARTESIAN_POINT('Ctrl Pts',(38.4455085820263,263.697902868876,25.9055413029229)) ;
#100675 = CARTESIAN_POINT('Ctrl Pts',(38.4166561141778,263.695102862366,25.8429144251477)) ;
#100676 = CARTESIAN_POINT('Ctrl Pts',(38.3877593368753,263.692298555816,25.7801913697152)) ;
#100677 = CARTESIAN_POINT('Ctrl Pts',(38.3622152797791,263.689494249266,25.7160282316914)) ;
#100678 = CARTESIAN_POINT('Ctrl Pts',(38.34014394139,263.686689942716,25.6508183111907)) ;
#100679 = CARTESIAN_POINT('Ctrl Pts',(38.3371511154177,263.686309684785,25.641975986349)) ;
#100680 = CARTESIAN_POINT('Ctrl Pts',(38.3342220651648,263.685929426854,25.6331144322903)) ;
#100681 = CARTESIAN_POINT('Ctrl Pts',(38.3313570176715,263.685549168922,25.624234644762)) ;
#100682 = CARTESIAN_POINT('Ctrl Pts',(38.3102283420653,263.682744905993,25.5587494649965)) ;
#100683 = CARTESIAN_POINT('Ctrl Pts',(38.2925075415833,263.679940643063,25.4920328198283)) ;
#100684 = CARTESIAN_POINT('Ctrl Pts',(38.2783336420738,263.677136380134,25.4244712567606)) ;
#100685 = CARTESIAN_POINT('Ctrl Pts',(38.2638216154704,263.674265219786,25.3552979710354)) ;
#100686 = CARTESIAN_POINT('Ctrl Pts',(38.2530281378403,263.671394059439,25.2852393984215)) ;
#100687 = CARTESIAN_POINT('Ctrl Pts',(38.2460487720483,263.668522899092,25.2147288459218)) ;
#100688 = CARTESIAN_POINT('Ctrl Pts',(38.2392493059321,263.665725745586,25.1460357688089)) ;
#100689 = CARTESIAN_POINT('Ctrl Pts',(38.2360697434519,263.66292859208,25.0769142493217)) ;
#100690 = CARTESIAN_POINT('Ctrl Pts',(38.2365467233904,263.660131438574,25.00777484353)) ;
#100691 = CARTESIAN_POINT('Ctrl Pts',(38.2370234342225,263.657335863189,24.9386744453718)) ;
#100692 = CARTESIAN_POINT('Ctrl Pts',(38.2411525901677,263.654540287804,24.8695566674509)) ;
#100693 = CARTESIAN_POINT('Ctrl Pts',(38.24891877186,263.651744712419,24.8008338559926)) ;
#100694 = CARTESIAN_POINT('Ctrl Pts',(38.256683176576,263.648949776688,24.7321267689673)) ;
#100695 = CARTESIAN_POINT('Ctrl Pts',(38.2680828992034,263.646154840957,24.663814953032)) ;
#100696 = CARTESIAN_POINT('Ctrl Pts',(38.2830506609902,263.643359905226,24.5963056594958)) ;
#100697 = CARTESIAN_POINT('Ctrl Pts',(38.2987289591487,263.640432290774,24.5255916243843)) ;
#100698 = CARTESIAN_POINT('Ctrl Pts',(38.3183224084895,263.637504676322,24.4557587781514)) ;
#100699 = CARTESIAN_POINT('Ctrl Pts',(38.3416940811369,263.63457706187,24.3872609126555)) ;
#100700 = CARTESIAN_POINT('Ctrl Pts',(38.3640324558406,263.631778881799,24.3217914441699)) ;
#100701 = CARTESIAN_POINT('Ctrl Pts',(38.3898217722139,263.628980701728,24.2575418544013)) ;
#100702 = CARTESIAN_POINT('Ctrl Pts',(38.4188927833497,263.626182521658,24.1948886568508)) ;
#100703 = CARTESIAN_POINT('Ctrl Pts',(38.447982531191,263.623382538118,24.1321950783688)) ;
#100704 = CARTESIAN_POINT('Ctrl Pts',(38.4803579551235,263.620582554578,24.0711003701115)) ;
#100705 = CARTESIAN_POINT('Ctrl Pts',(38.5158041829826,263.617782571038,24.0119558405473)) ;
#100706 = CARTESIAN_POINT('Ctrl Pts',(38.5513048525648,263.614978287014,23.9527204711311)) ;
#100707 = CARTESIAN_POINT('Ctrl Pts',(38.5898854610192,263.612174002991,23.8954416574321)) ;
#100708 = CARTESIAN_POINT('Ctrl Pts',(38.6312888902081,263.609369718967,23.8404402886788)) ;
#100709 = CARTESIAN_POINT('Ctrl Pts',(38.6369051855656,263.608989323245,23.8329794590316)) ;
#100710 = CARTESIAN_POINT('Ctrl Pts',(38.6425733641873,263.608608927523,23.8255604821681)) ;
#100711 = CARTESIAN_POINT('Ctrl Pts',(38.6482927310412,263.608228531801,23.8181841079402)) ;
#100712 = CARTESIAN_POINT('Ctrl Pts',(38.6904563559798,263.605424224442,23.7638048935454)) ;
#100713 = CARTESIAN_POINT('Ctrl Pts',(38.7355588715066,263.602619917084,23.7115455412858)) ;
#100714 = CARTESIAN_POINT('Ctrl Pts',(38.7833594549891,263.599815609725,23.6617388578696)) ;
#100715 = CARTESIAN_POINT('Ctrl Pts',(38.8322994807614,263.596944454931,23.6107449119291)) ;
#100716 = CARTESIAN_POINT('Ctrl Pts',(38.8840676143003,263.594073300138,23.5623225303503)) ;
#100717 = CARTESIAN_POINT('Ctrl Pts',(38.9383599238844,263.591202145344,23.5167949804171)) ;
#100718 = CARTESIAN_POINT('Ctrl Pts',(38.9912537318354,263.588404947888,23.4724401629284)) ;
#100719 = CARTESIAN_POINT('Ctrl Pts',(39.0465428414221,263.585607750432,23.4308331693517)) ;
#100720 = CARTESIAN_POINT('Ctrl Pts',(39.1039088641049,263.582810552976,23.3922357933253)) ;
#100721 = CARTESIAN_POINT('Ctrl Pts',(39.1612425158913,263.580014933942,23.3536601972934)) ;
#100722 = CARTESIAN_POINT('Ctrl Pts',(39.2206503513546,263.577219314908,23.318091120167)) ;
#100723 = CARTESIAN_POINT('Ctrl Pts',(39.2817831457197,263.574423695874,23.2857483748658)) ;
#100724 = CARTESIAN_POINT('Ctrl Pts',(39.3429019443822,263.571628716867,23.253413034092)) ;
#100725 = CARTESIAN_POINT('Ctrl Pts',(39.4057444868051,263.56883373786,23.2243027857003)) ;
#100726 = CARTESIAN_POINT('Ctrl Pts',(39.4699365096433,263.566038758853,23.1985917433428)) ;
#100727 = CARTESIAN_POINT('Ctrl Pts',(39.5371737837546,263.563111186839,23.1716609764619)) ;
#100728 = CARTESIAN_POINT('Ctrl Pts',(39.605891241258,263.560183614824,23.1484602140269)) ;
#100729 = CARTESIAN_POINT('Ctrl Pts',(39.6756369456841,263.55725604281,23.1291322880882)) ;
#100730 = CARTESIAN_POINT('Ctrl Pts',(39.7423010474188,263.554457820895,23.1106583357251)) ;
#100731 = CARTESIAN_POINT('Ctrl Pts',(39.8099039370277,263.551659598979,23.0957222547113)) ;
#100732 = CARTESIAN_POINT('Ctrl Pts',(39.8780392297342,263.548861377064,23.0843966196071)) ;
#100733 = CARTESIAN_POINT('Ctrl Pts',(39.946218423042,263.546061352212,23.0730636872247)) ;
#100734 = CARTESIAN_POINT('Ctrl Pts',(40.0149302181711,263.54326132736,23.0653458847454)) ;
#100735 = CARTESIAN_POINT('Ctrl Pts',(40.0837633136764,263.540461302508,23.0612638946907)) ;
#100736 = CARTESIAN_POINT('Ctrl Pts',(40.1527021026324,263.537656978209,23.0571756367265)) ;
#100737 = CARTESIAN_POINT('Ctrl Pts',(40.2217620773208,263.534852653909,23.0567343287276)) ;
#100738 = CARTESIAN_POINT('Ctrl Pts',(40.2905332312581,263.53204832961,23.059908611149)) ;
#100739 = CARTESIAN_POINT('Ctrl Pts',(40.299855622657,263.531668184633,23.060338906432)) ;
#100740 = CARTESIAN_POINT('Ctrl Pts',(40.3091727180629,263.531288039656,23.060835562883)) ;
#100741 = CARTESIAN_POINT('Ctrl Pts',(40.3184835082875,263.530907894679,23.0613984297416)) ;
#100742 = CARTESIAN_POINT('Ctrl Pts',(40.3871687771503,263.528103582765,23.065550672525)) ;
#100743 = CARTESIAN_POINT('Ctrl Pts',(40.4557607972916,263.525299270852,23.073325400445)) ;
#100744 = CARTESIAN_POINT('Ctrl Pts',(40.5238489197198,263.522494958938,23.0847114188677)) ;
#100745 = CARTESIAN_POINT('Ctrl Pts',(40.593559959848,263.519623804714,23.0963688292773)) ;
#100746 = CARTESIAN_POINT('Ctrl Pts',(40.6627422533621,263.51675265049,23.1118119564516)) ;
#100747 = CARTESIAN_POINT('Ctrl Pts',(40.7309574422995,263.513881496266,23.1309721099088)) ;
#100748 = CARTESIAN_POINT('Ctrl Pts',(40.7974156483534,263.511084292857,23.1496387653313)) ;
#100749 = CARTESIAN_POINT('Ctrl Pts',(40.8629554689667,263.508287089447,23.1718331328687)) ;
#100750 = CARTESIAN_POINT('Ctrl Pts',(40.927181157058,263.505489886038,23.1974399157849)) ;
#100751 = CARTESIAN_POINT('Ctrl Pts',(40.9913706149098,263.502694260555,23.2230322537039)) ;
#100752 = CARTESIAN_POINT('Ctrl Pts',(41.0542469594534,263.499898635071,23.2520330067409)) ;
#100753 = CARTESIAN_POINT('Ctrl Pts',(41.1154317225032,263.497103009588,23.2842777386029)) ;
#100754 = CARTESIAN_POINT('Ctrl Pts',(41.1766024885195,263.49430802365,23.3165150939454)) ;
#100755 = CARTESIAN_POINT('Ctrl Pts',(41.2360820107478,263.491513037712,23.3519947267641)) ;
#100756 = CARTESIAN_POINT('Ctrl Pts',(41.2935154402097,263.488718051774,23.3905057520064)) ;
#100757 = CARTESIAN_POINT('Ctrl Pts',(41.3536732262298,263.48579048559,23.4308435489592)) ;
#100758 = CARTESIAN_POINT('Ctrl Pts',(41.4115854696119,263.482862919405,23.4745071977217)) ;
#100759 = CARTESIAN_POINT('Ctrl Pts',(41.4668793564282,263.47993535322,23.5212040326503)) ;
#100760 = CARTESIAN_POINT('Ctrl Pts',(41.5197304281352,263.477137123266,23.5658378595235)) ;
#100761 = CARTESIAN_POINT('Ctrl Pts',(41.5701892879359,263.474338893312,23.6132421229446)) ;
#100762 = CARTESIAN_POINT('Ctrl Pts',(41.617966825027,263.471540663358,23.6631221499506)) ;
#100763 = CARTESIAN_POINT('Ctrl Pts',(41.6657751521819,263.468740630095,23.7130343219625)) ;
#100764 = CARTESIAN_POINT('Ctrl Pts',(41.7108983998769,263.465940596832,23.7654250638381)) ;
#100765 = CARTESIAN_POINT('Ctrl Pts',(41.753087537975,263.463140563568,23.8199663784907)) ;
#100766 = CARTESIAN_POINT('Ctrl Pts',(41.7953414643923,263.460336230396,23.8745914502492)) ;
#100767 = CARTESIAN_POINT('Ctrl Pts',(41.8346520180536,263.457531897224,23.9313732817699)) ;
#100768 = CARTESIAN_POINT('Ctrl Pts',(41.8708138762976,263.454727564052,23.9899555968422)) ;
#100769 = CARTESIAN_POINT('Ctrl Pts',(41.8757152912741,263.454347461887,23.9978959032975)) ;
#100770 = CARTESIAN_POINT('Ctrl Pts',(41.8805589307958,263.453967359722,24.0058692526742)) ;
#100771 = CARTESIAN_POINT('Ctrl Pts',(41.8853443503933,263.453587257557,24.0138747268648)) ;
#100772 = CARTESIAN_POINT('Ctrl Pts',(41.9216214507285,263.450705795629,24.0745622767291)) ;
#100773 = CARTESIAN_POINT('Ctrl Pts',(41.9546748140438,263.447824333702,24.1373083768965)) ;
#100774 = CARTESIAN_POINT('Ctrl Pts',(41.9842740327424,263.444942871774,24.2017482441801)) ;
#100775 = CARTESIAN_POINT('Ctrl Pts',(42.0138089006307,263.44206767435,24.2660480146013)) ;
#100776 = CARTESIAN_POINT('Ctrl Pts',(42.0399043812239,263.439192476926,24.3320338182222)) ;
#100777 = CARTESIAN_POINT('Ctrl Pts',(42.0623754778071,263.436317279502,24.3993156573531)) ;
#100778 = CARTESIAN_POINT('Ctrl Pts',(42.084817624012,263.433445786306,24.466510814702)) ;
#100779 = CARTESIAN_POINT('Ctrl Pts',(42.1036445214476,263.430574293109,24.5349982659407)) ;
#100780 = CARTESIAN_POINT('Ctrl Pts',(42.1187190636676,263.427702799912,24.6043678226193)) ;
#100781 = CARTESIAN_POINT('Ctrl Pts',(42.1337749073975,263.424834868521,24.6736513331708)) ;
#100782 = CARTESIAN_POINT('Ctrl Pts',(42.1450875590401,263.42196693713,24.7438143345802)) ;
#100783 = CARTESIAN_POINT('Ctrl Pts',(42.152570042604,263.419099005739,24.8144327443052)) ;
#100784 = CARTESIAN_POINT('Ctrl Pts',(42.159863312118,263.41630359745,24.8832653839454)) ;
#100785 = CARTESIAN_POINT('Ctrl Pts',(42.1635177960648,263.41350818916,24.9525302509306)) ;
#100786 = CARTESIAN_POINT('Ctrl Pts',(42.163499934776,263.41071278087,25.0218264412157)) ;
#100787 = CARTESIAN_POINT('',(41.0528501317078,263.,23.252711030329)) ;
#100788 = CARTESIAN_POINT('Ctrl Pts',(42.1634999347757,263.410712780838,25.0218264420184)) ;
#100789 = CARTESIAN_POINT('Ctrl Pts',(42.1634807839659,263.407715558845,25.096125450968)) ;
#100790 = CARTESIAN_POINT('Ctrl Pts',(42.1592401502437,263.404718336852,25.1703150629735)) ;
#100791 = CARTESIAN_POINT('Ctrl Pts',(42.1508405655625,263.401721114859,25.2439261335915)) ;
#100792 = CARTESIAN_POINT('Ctrl Pts',(42.1424229803534,263.398717469742,25.317694954644)) ;
#100793 = CARTESIAN_POINT('Ctrl Pts',(42.1298287214177,263.395713824625,25.3908823956159)) ;
#100794 = CARTESIAN_POINT('Ctrl Pts',(42.1131713889199,263.392710179507,25.4630300747387)) ;
#100795 = CARTESIAN_POINT('Ctrl Pts',(42.0964543875685,263.389695774921,25.5354361967606)) ;
#100796 = CARTESIAN_POINT('Ctrl Pts',(42.0756452976501,263.386681370334,25.6067947481036)) ;
#100797 = CARTESIAN_POINT('Ctrl Pts',(42.05090791895,263.383666965747,25.6766615719043)) ;
#100798 = CARTESIAN_POINT('Ctrl Pts',(42.0306645464762,263.381200183976,25.7338357840512)) ;
#100799 = CARTESIAN_POINT('Ctrl Pts',(42.0077914895878,263.378733402206,25.790011317915)) ;
#100800 = CARTESIAN_POINT('Ctrl Pts',(41.9824016122412,263.376266620435,25.8449566362763)) ;
#100801 = CARTESIAN_POINT('Ctrl Pts',(41.9535344890115,263.373462002973,25.9074269371122)) ;
#100802 = CARTESIAN_POINT('Ctrl Pts',(41.9213266109815,263.370657385511,25.9684916627149)) ;
#100803 = CARTESIAN_POINT('Ctrl Pts',(41.8859379059561,263.367852768049,26.0277723430411)) ;
#100804 = CARTESIAN_POINT('Ctrl Pts',(41.849710120996,263.364981652018,26.0884585913118)) ;
#100805 = CARTESIAN_POINT('Ctrl Pts',(41.8101488762589,263.362110535988,26.1472746069963)) ;
#100806 = CARTESIAN_POINT('Ctrl Pts',(41.7674776545232,263.359239419957,26.2038371732794)) ;
#100807 = CARTESIAN_POINT('Ctrl Pts',(41.7259004790425,263.35644191639,26.2589495335149)) ;
#100808 = CARTESIAN_POINT('Ctrl Pts',(41.6813712050567,263.353644412822,26.311922199575)) ;
#100809 = CARTESIAN_POINT('Ctrl Pts',(41.6341412921688,263.350846909255,26.3624284689903)) ;
#100810 = CARTESIAN_POINT('Ctrl Pts',(41.5869380671934,263.348050986455,26.4129061991428)) ;
#100811 = CARTESIAN_POINT('Ctrl Pts',(41.5370375639455,263.345255063655,26.4609199431382)) ;
#100812 = CARTESIAN_POINT('Ctrl Pts',(41.4847307237625,263.342459140856,26.5061769755011)) ;
#100813 = CARTESIAN_POINT('Ctrl Pts',(41.4324359106992,263.339663860934,26.5514236017346)) ;
#100814 = CARTESIAN_POINT('Ctrl Pts',(41.3777362281772,263.336868581012,26.59391445679)) ;
#100815 = CARTESIAN_POINT('Ctrl Pts',(41.3209572868056,263.33407330109,26.6333957174666)) ;
#100816 = CARTESIAN_POINT('Ctrl Pts',(41.2614971739138,263.331146024608,26.6747413318834)) ;
#100817 = CARTESIAN_POINT('Ctrl Pts',(41.1997570162666,263.328218748127,26.7127857086607)) ;
#100818 = CARTESIAN_POINT('Ctrl Pts',(41.1361448941024,263.325291471645,26.747288184293)) ;
#100819 = CARTESIAN_POINT('Ctrl Pts',(41.0753309252333,263.322492959431,26.7802729741039)) ;
#100820 = CARTESIAN_POINT('Ctrl Pts',(41.0128067100144,263.319694447218,26.8100207603668)) ;
#100821 = CARTESIAN_POINT('Ctrl Pts',(40.9489519795987,263.316895935004,26.8363694289166)) ;
#100822 = CARTESIAN_POINT('Ctrl Pts',(40.885056200698,263.31409562379,26.8627350354898)) ;
#100823 = CARTESIAN_POINT('Ctrl Pts',(40.8198286636425,263.311295312576,26.8856970139188)) ;
#100824 = CARTESIAN_POINT('Ctrl Pts',(40.7536655601216,263.308495001361,26.9051427071426)) ;
#100825 = CARTESIAN_POINT('Ctrl Pts',(40.6874010513169,263.305690398233,26.9246182039265)) ;
#100826 = CARTESIAN_POINT('Ctrl Pts',(40.6201985891142,263.302885795105,26.9405665547925)) ;
#100827 = CARTESIAN_POINT('Ctrl Pts',(40.5524648073253,263.300081191977,26.9529261029207)) ;
#100828 = CARTESIAN_POINT('Ctrl Pts',(40.54332602458,263.299702789088,26.9545936788657)) ;
#100829 = CARTESIAN_POINT('Ctrl Pts',(40.5341775761182,263.2993243862,26.9561960017459)) ;
#100830 = CARTESIAN_POINT('Ctrl Pts',(40.5250204651575,263.298945983311,26.9577329925652)) ;
#100831 = CARTESIAN_POINT('Ctrl Pts',(40.4571563191861,263.296141606585,26.9691237652409)) ;
#100832 = CARTESIAN_POINT('Ctrl Pts',(40.3885690018021,263.293337229859,26.9769634517495)) ;
#100833 = CARTESIAN_POINT('Ctrl Pts',(40.319661207915,263.290532853132,26.9811707065517)) ;
#100834 = CARTESIAN_POINT('Ctrl Pts',(40.2491127885888,263.28766170701,26.9854781318697)) ;
#100835 = CARTESIAN_POINT('Ctrl Pts',(40.1782289285393,263.284790560887,26.9859777612289)) ;
#100836 = CARTESIAN_POINT('Ctrl Pts',(40.1074522042496,263.281919414764,26.9826380525251)) ;
#100837 = CARTESIAN_POINT('Ctrl Pts',(40.0384964386557,263.279122138103,26.979384268561)) ;
#100838 = CARTESIAN_POINT('Ctrl Pts',(39.9696428813651,263.276324861442,26.9724863579311)) ;
#100839 = CARTESIAN_POINT('Ctrl Pts',(39.9013030913024,263.273527584781,26.9619677630396)) ;
#100840 = CARTESIAN_POINT('Ctrl Pts',(39.8330017813659,263.270731883183,26.9514550908596)) ;
#100841 = CARTESIAN_POINT('Ctrl Pts',(39.7652141453778,263.267936181586,26.9373258542111)) ;
#100842 = CARTESIAN_POINT('Ctrl Pts',(39.6983459439994,263.265140479989,26.9196552608221)) ;
#100843 = CARTESIAN_POINT('Ctrl Pts',(39.6314929752019,263.262345415253,26.9019886927956)) ;
#100844 = CARTESIAN_POINT('Ctrl Pts',(39.5655594959524,263.259550350517,26.8807824950459)) ;
#100845 = CARTESIAN_POINT('Ctrl Pts',(39.5009386864303,263.256755285781,26.8561624429977)) ;
#100846 = CARTESIAN_POINT('Ctrl Pts',(39.4332561415014,263.253827790816,26.8303758923303)) ;
#100847 = CARTESIAN_POINT('Ctrl Pts',(39.3670143043893,263.25090029585,26.8008441137367)) ;
#100848 = CARTESIAN_POINT('Ctrl Pts',(39.3026421698098,263.247972800884,26.7677685032816)) ;
#100849 = CARTESIAN_POINT('Ctrl Pts',(39.2411105635351,263.245174486539,26.7361524095616)) ;
#100850 = CARTESIAN_POINT('Ctrl Pts',(39.181287536387,263.242376172193,26.7012989643614)) ;
#100851 = CARTESIAN_POINT('Ctrl Pts',(39.1235210375826,263.239577857848,26.6634303561571)) ;
#100852 = CARTESIAN_POINT('Ctrl Pts',(39.0657172749725,263.236777738377,26.6255373198069)) ;
#100853 = CARTESIAN_POINT('Ctrl Pts',(39.0099730734674,263.233977618905,26.5846255377044)) ;
#100854 = CARTESIAN_POINT('Ctrl Pts',(38.9566048140936,263.231177499433,26.5409586760798)) ;
#100855 = CARTESIAN_POINT('Ctrl Pts',(38.9031545655358,263.228373078163,26.4972247294426)) ;
#100856 = CARTESIAN_POINT('Ctrl Pts',(38.8520878984263,263.225568656893,26.4507275889612)) ;
#100857 = CARTESIAN_POINT('Ctrl Pts',(38.8036849584539,263.222764235622,26.4017682979397)) ;
#100858 = CARTESIAN_POINT('Ctrl Pts',(38.797132733531,263.222384605811,26.395140760707)) ;
#100859 = CARTESIAN_POINT('Ctrl Pts',(38.7906292596009,263.222004976001,26.3884681548245)) ;
#100860 = CARTESIAN_POINT('Ctrl Pts',(38.7841751736792,263.22162534619,26.3817512720428)) ;
#100861 = CARTESIAN_POINT('Ctrl Pts',(38.7365312003997,263.218822924161,26.3321673359669)) ;
#100862 = CARTESIAN_POINT('Ctrl Pts',(38.6914074066215,263.216020502133,26.2799863446704)) ;
#100863 = CARTESIAN_POINT('Ctrl Pts',(38.6490979521542,263.213218080105,26.2254943708446)) ;
#100864 = CARTESIAN_POINT('Ctrl Pts',(38.6057472495523,263.210346689645,26.1696613334949)) ;
#100865 = CARTESIAN_POINT('Ctrl Pts',(38.5653516687552,263.207475299185,26.11140236663)) ;
#100866 = CARTESIAN_POINT('Ctrl Pts',(38.5281873948101,263.204603908725,26.0510653911942)) ;
#100867 = CARTESIAN_POINT('Ctrl Pts',(38.4920078828847,263.201808603063,25.9923271974779)) ;
#100868 = CARTESIAN_POINT('Ctrl Pts',(38.4588908284484,263.199013297401,25.9316202001215)) ;
#100869 = CARTESIAN_POINT('Ctrl Pts',(38.4290488774882,263.196217991739,25.8692969774795)) ;
#100870 = CARTESIAN_POINT('Ctrl Pts',(38.3992237459258,263.193424261555,25.8070088811964)) ;
#100871 = CARTESIAN_POINT('Ctrl Pts',(38.3726702652924,263.190630531372,25.7431068067474)) ;
#100872 = CARTESIAN_POINT('Ctrl Pts',(38.3495550741375,263.187836801189,25.6779677575877)) ;
#100873 = CARTESIAN_POINT('Ctrl Pts',(38.3264451281523,263.185043704943,25.612843489416)) ;
#100874 = CARTESIAN_POINT('Ctrl Pts',(38.3067720850511,263.182250608697,25.5464832639704)) ;
#100875 = CARTESIAN_POINT('Ctrl Pts',(38.2906537335265,263.179457512451,25.4792822248378)) ;
#100876 = CARTESIAN_POINT('Ctrl Pts',(38.2737488010264,263.176528112169,25.4088017523931)) ;
#100877 = CARTESIAN_POINT('Ctrl Pts',(38.2607545537579,263.173598711887,25.337396860385)) ;
#100878 = CARTESIAN_POINT('Ctrl Pts',(38.2517467833031,263.170669311605,25.265536750933)) ;
#100879 = CARTESIAN_POINT('Ctrl Pts',(38.2431480558051,263.167872935423,25.1969398098517)) ;
#100880 = CARTESIAN_POINT('Ctrl Pts',(38.2381815811983,263.16507655924,25.1279286122452)) ;
#100881 = CARTESIAN_POINT('Ctrl Pts',(38.2368599469755,263.162280183058,25.0589153194325)) ;
#100882 = CARTESIAN_POINT('Ctrl Pts',(38.2355374538086,263.159481989481,24.9898571741492)) ;
#100883 = CARTESIAN_POINT('Ctrl Pts',(38.2378644985265,263.156683795904,24.9207974184139)) ;
#100884 = CARTESIAN_POINT('Ctrl Pts',(38.2438016143948,263.153885602327,24.8521455045452)) ;
#100885 = CARTESIAN_POINT('Ctrl Pts',(38.2497479229573,263.151083076185,24.7833872939384)) ;
#100886 = CARTESIAN_POINT('Ctrl Pts',(38.2593153828646,263.148280550043,24.7150386667268)) ;
#100887 = CARTESIAN_POINT('Ctrl Pts',(38.2724132323186,263.145478023902,24.6475001955476)) ;
#100888 = CARTESIAN_POINT('Ctrl Pts',(38.2742410952635,263.145086918957,24.6380749025441)) ;
#100889 = CARTESIAN_POINT('Ctrl Pts',(38.2761376346203,263.144695814012,24.6286653638711)) ;
#100890 = CARTESIAN_POINT('Ctrl Pts',(38.2781025269689,263.144304709068,24.6192726434584)) ;
#100891 = CARTESIAN_POINT('Ctrl Pts',(38.2922100313937,263.141496659689,24.5518349312221)) ;
#100892 = CARTESIAN_POINT('Ctrl Pts',(38.3098966282719,263.138688610311,24.4850193546318)) ;
#100893 = CARTESIAN_POINT('Ctrl Pts',(38.3310909267631,263.135880560933,24.4192313750733)) ;
#100894 = CARTESIAN_POINT('Ctrl Pts',(38.3527579951909,263.133009873892,24.3519758980682)) ;
#100895 = CARTESIAN_POINT('Ctrl Pts',(38.3780911242255,263.130139186851,24.285794934149)) ;
#100896 = CARTESIAN_POINT('Ctrl Pts',(38.4069586104773,263.12726849981,24.221111105011)) ;
#100897 = CARTESIAN_POINT('Ctrl Pts',(38.4351245577882,263.124467576333,24.1579992251792)) ;
#100898 = CARTESIAN_POINT('Ctrl Pts',(38.4666548105774,263.121666652857,24.0963130076055)) ;
#100899 = CARTESIAN_POINT('Ctrl Pts',(38.5013772528305,263.118865729381,24.0364279571546)) ;
#100900 = CARTESIAN_POINT('Ctrl Pts',(38.5360799229529,263.116066400844,23.9765770072731)) ;
#100901 = CARTESIAN_POINT('Ctrl Pts',(38.5739709316143,263.113267072309,23.9185256085515)) ;
#100902 = CARTESIAN_POINT('Ctrl Pts',(38.6148320652173,263.110467743773,23.8626250132261)) ;
#100903 = CARTESIAN_POINT('Ctrl Pts',(38.65568352523,263.107669077958,23.8067376519794)) ;
#100904 = CARTESIAN_POINT('Ctrl Pts',(38.6995034266407,263.104870412144,23.753000474716)) ;
#100905 = CARTESIAN_POINT('Ctrl Pts',(38.7460310326053,263.102071746329,23.7017346161992)) ;
#100906 = CARTESIAN_POINT('Ctrl Pts',(38.7946418587462,263.099147773464,23.6481733876843)) ;
#100907 = CARTESIAN_POINT('Ctrl Pts',(38.8462082137692,263.096223800599,23.5973104412322)) ;
#100908 = CARTESIAN_POINT('Ctrl Pts',(38.9003884029964,263.093299827733,23.5494705051135)) ;
#100909 = CARTESIAN_POINT('Ctrl Pts',(38.9523049486173,263.090498018201,23.5036293173762)) ;
#100910 = CARTESIAN_POINT('Ctrl Pts',(39.0066208255902,263.087696208668,23.4605638308037)) ;
#100911 = CARTESIAN_POINT('Ctrl Pts',(39.0630019956775,263.084894399136,23.4205181108754)) ;
#100912 = CARTESIAN_POINT('Ctrl Pts',(39.1194186886288,263.082090824328,23.3804471602068)) ;
#100913 = CARTESIAN_POINT('Ctrl Pts',(39.1779028545884,263.079287249519,23.3434000232094)) ;
#100914 = CARTESIAN_POINT('Ctrl Pts',(39.2380932403682,263.076483674711,23.3095763101905)) ;
#100915 = CARTESIAN_POINT('Ctrl Pts',(39.2983742689995,263.0736758779,23.2757016608343)) ;
#100916 = CARTESIAN_POINT('Ctrl Pts',(39.3603662077959,263.070868081088,23.2450603323664)) ;
#100917 = CARTESIAN_POINT('Ctrl Pts',(39.4236860971042,263.068060284276,23.2178046174927)) ;
#100918 = CARTESIAN_POINT('Ctrl Pts',(39.4317761466145,263.067701546833,23.2143222980323)) ;
#100919 = CARTESIAN_POINT('Ctrl Pts',(39.4398878519879,263.067342809389,23.2108951783485)) ;
#100920 = CARTESIAN_POINT('Ctrl Pts',(39.4480203969485,263.066984071946,23.2075235173978)) ;
#100921 = CARTESIAN_POINT('Ctrl Pts',(39.5112921790507,263.064193068948,23.1812917537828)) ;
#100922 = CARTESIAN_POINT('Ctrl Pts',(39.576070983772,263.06140206595,23.1583198387983)) ;
#100923 = CARTESIAN_POINT('Ctrl Pts',(39.6419825877609,263.058611062953,23.1387824773699)) ;
#100924 = CARTESIAN_POINT('Ctrl Pts',(39.7071246471384,263.055852646043,23.1194732225312)) ;
#100925 = CARTESIAN_POINT('Ctrl Pts',(39.7733727088633,263.053094229133,23.1035189237572)) ;
#100926 = CARTESIAN_POINT('Ctrl Pts',(39.8403441402275,263.050335812223,23.0910405937484)) ;
#100927 = CARTESIAN_POINT('Ctrl Pts',(39.9072570590145,263.047579805327,23.078573165989)) ;
#100928 = CARTESIAN_POINT('Ctrl Pts',(39.9748916016868,263.044823798431,23.0695757791274)) ;
#100929 = CARTESIAN_POINT('Ctrl Pts',(40.0428519602401,263.042067791535,23.0641190908521)) ;
#100930 = CARTESIAN_POINT('Ctrl Pts',(40.1107774956255,263.039313196828,23.0586651986064)) ;
#100931 = CARTESIAN_POINT('Ctrl Pts',(40.1790280144218,263.036558602122,23.0567484464848)) ;
#100932 = CARTESIAN_POINT('Ctrl Pts',(40.247201510416,263.033804007415,23.0583877753305)) ;
#100933 = CARTESIAN_POINT('Ctrl Pts',(40.3169194910234,263.030987006797,23.0600642435093)) ;
#100934 = CARTESIAN_POINT('Ctrl Pts',(40.3865563712997,263.028170006179,23.0654599469317)) ;
#100935 = CARTESIAN_POINT('Ctrl Pts',(40.4556830337894,263.025353005561,23.0745387851324)) ;
#100936 = CARTESIAN_POINT('Ctrl Pts',(40.5233155646348,263.022596892734,23.0834213896519)) ;
#100937 = CARTESIAN_POINT('Ctrl Pts',(40.5904592123026,263.019840779907,23.0958293517773)) ;
#100938 = CARTESIAN_POINT('Ctrl Pts',(40.6567205532952,263.01708466708,23.1116767678634)) ;
#100939 = CARTESIAN_POINT('Ctrl Pts',(40.7251776534542,263.014237222567,23.1280493334351)) ;
#100940 = CARTESIAN_POINT('Ctrl Pts',(40.7926923736418,263.011389778053,23.1480931961573)) ;
#100941 = CARTESIAN_POINT('Ctrl Pts',(40.8588485940152,263.00854233354,23.1716580013565)) ;
#100942 = CARTESIAN_POINT('Ctrl Pts',(40.9250048143885,263.005694889027,23.1952228065557)) ;
#100943 = CARTESIAN_POINT('Ctrl Pts',(40.9898020147256,263.002847444513,23.2223082757636)) ;
#100944 = CARTESIAN_POINT('Ctrl Pts',(41.0528501317078,263.,23.252711030329)) ;
#100945 = CARTESIAN_POINT('Ctrl Pts',(41.0528501317078,263.,23.252711030329)) ;
#100946 = CARTESIAN_POINT('Ctrl Pts',(41.0637961405579,263.,23.2581157538237)) ;
#100947 = CARTESIAN_POINT('Ctrl Pts',(41.074742149408,263.,23.2635204773184)) ;
#100948 = CARTESIAN_POINT('Ctrl Pts',(41.0856881582581,263.,23.2689252008131)) ;
#100949 = CARTESIAN_POINT('',(42.1635,255.,25.0213203435596)) ;
#100950 = CARTESIAN_POINT('Origin',(40.2,255.,25.0213203435596)) ;
#100951 = CARTESIAN_POINT('Origin',(40.2,265.924309379709,25.0213203435596)) ;
#100952 = CARTESIAN_POINT('',(39.2427274574787,263.,26.3991716932468)) ;
#100953 = CARTESIAN_POINT('Ctrl Pts',(39.2427274574787,263.,26.3991716932468)) ;
#100954 = CARTESIAN_POINT('Ctrl Pts',(39.2911023455816,263.003084054089,26.4327805089866)) ;
#100955 = CARTESIAN_POINT('Ctrl Pts',(39.3412181789107,263.006211645544,26.4638215959221)) ;
#100956 = CARTESIAN_POINT('Ctrl Pts',(39.4699166383487,263.01394653045,26.5344454303808)) ;
#100957 = CARTESIAN_POINT('Ctrl Pts',(39.5501746528686,263.018506385508,26.5706101629425)) ;
#100958 = CARTESIAN_POINT('Ctrl Pts',(39.6661076125514,263.024630231193,26.6122473389269)) ;
#100959 = CARTESIAN_POINT('Ctrl Pts',(39.6996808889019,263.026353491027,26.6231227004272)) ;
#100960 = CARTESIAN_POINT('Ctrl Pts',(39.7610537645275,263.029415612689,26.6408849987459)) ;
#100961 = CARTESIAN_POINT('Ctrl Pts',(39.7887336180132,263.030765067584,26.6481342687505)) ;
#100962 = CARTESIAN_POINT('Ctrl Pts',(39.8517601410882,263.033771737349,26.6629291376098)) ;
#100963 = CARTESIAN_POINT('Ctrl Pts',(39.8871926527789,263.03541569227,26.6700477922631)) ;
#100964 = CARTESIAN_POINT('Ctrl Pts',(40.025705529455,263.041693627517,26.6932494861919)) ;
#100965 = CARTESIAN_POINT('Ctrl Pts',(40.1299691561863,263.046085821433,26.700850832178)) ;
#100966 = CARTESIAN_POINT('Ctrl Pts',(40.3167787214546,263.053989498904,26.6970349195049)) ;
#100967 = CARTESIAN_POINT('Ctrl Pts',(40.3990509823152,263.057489072505,26.6892631852092)) ;
#100968 = CARTESIAN_POINT('Ctrl Pts',(40.5025796865608,263.062241845599,26.6717130852496)) ;
#100969 = CARTESIAN_POINT('Ctrl Pts',(40.5246704101568,263.063276871209,26.6675097953225)) ;
#100970 = CARTESIAN_POINT('Ctrl Pts',(40.5627942014101,263.065109280979,26.6594586303915)) ;
#100971 = CARTESIAN_POINT('Ctrl Pts',(40.5788664978773,263.065896700378,26.6558162329867)) ;
#100972 = CARTESIAN_POINT('Ctrl Pts',(40.6180174490815,263.067851580907,26.646335132263)) ;
#100973 = CARTESIAN_POINT('Ctrl Pts',(40.6410290389475,263.069031077354,26.6402412613374)) ;
#100974 = CARTESIAN_POINT('Ctrl Pts',(40.7671234650463,263.075634532828,26.6039613959264)) ;
#100975 = CARTESIAN_POINT('Ctrl Pts',(40.8672505236624,263.08138241966,26.5644202025094)) ;
#100976 = CARTESIAN_POINT('Ctrl Pts',(41.0389529161193,263.091519303937,26.476756175076)) ;
#100977 = CARTESIAN_POINT('Ctrl Pts',(41.1119297697296,263.0959336199,26.4321789667875)) ;
#100978 = CARTESIAN_POINT('Ctrl Pts',(41.2090558997039,263.101870477116,26.3621523481488)) ;
#100979 = CARTESIAN_POINT('Ctrl Pts',(41.2362885731461,263.103543880883,26.3412182438542)) ;
#100980 = CARTESIAN_POINT('Ctrl Pts',(41.2849477404721,263.106552212936,26.3013782803977)) ;
#100981 = CARTESIAN_POINT('Ctrl Pts',(41.3065702733717,263.107896150544,26.2827331486183)) ;
#100982 = CARTESIAN_POINT('Ctrl Pts',(41.3545780272055,263.110901574535,26.2391510886397)) ;
#100983 = CARTESIAN_POINT('Ctrl Pts',(41.3806510884628,263.112549377426,26.2138912467673)) ;
#100984 = CARTESIAN_POINT('Ctrl Pts',(41.4751073086673,263.118608432302,26.1162445044194)) ;
#100985 = CARTESIAN_POINT('Ctrl Pts',(41.5378247274081,263.122803876602,26.0386619543441)) ;
#100986 = CARTESIAN_POINT('Ctrl Pts',(41.6276347117263,263.129600955505,25.9047818671928)) ;
#100987 = CARTESIAN_POINT('Ctrl Pts',(41.6591275250957,263.132199923992,25.8517367826009)) ;
#100988 = CARTESIAN_POINT('Ctrl Pts',(41.7002796632013,263.13608235282,25.7728218824172)) ;
#100989 = CARTESIAN_POINT('Ctrl Pts',(41.7123346684026,263.137293244777,25.7482573250673)) ;
#100990 = CARTESIAN_POINT('Ctrl Pts',(41.7331888116543,263.13954664214,25.7029964442953)) ;
#100991 = CARTESIAN_POINT('Ctrl Pts',(41.7421828782459,263.140580413658,25.6823968336961)) ;
#100992 = CARTESIAN_POINT('Ctrl Pts',(41.7569854939115,263.142403288016,25.6465461595278)) ;
#100993 = CARTESIAN_POINT('Ctrl Pts',(41.7629900404973,263.143182096106,25.6313803762269)) ;
#100994 = CARTESIAN_POINT('Ctrl Pts',(41.7769827331857,263.145096227955,25.5944754675309)) ;
#100995 = CARTESIAN_POINT('Ctrl Pts',(41.7847431952058,263.146242664951,25.5726553129982)) ;
#100996 = CARTESIAN_POINT('Ctrl Pts',(41.8214679770377,263.152094654795,25.4622060578001)) ;
#100997 = CARTESIAN_POINT('Ctrl Pts',(41.843458699302,263.157051484054,25.371435403534)) ;
#100998 = CARTESIAN_POINT('Ctrl Pts',(41.8730849494486,263.167223396867,25.1810649885886)) ;
#100999 = CARTESIAN_POINT('Ctrl Pts',(41.8796120584156,263.172409089272,25.0816425807865)) ;
#101000 = CARTESIAN_POINT('Ctrl Pts',(41.8764894512499,263.179060704958,24.9476942236183)) ;
#101001 = CARTESIAN_POINT('Ctrl Pts',(41.87461879154,263.180745460967,24.9132009903328)) ;
#101002 = CARTESIAN_POINT('Ctrl Pts',(41.8692833714942,263.183752319547,24.8506245214068)) ;
#101003 = CARTESIAN_POINT('Ctrl Pts',(41.8661706103987,263.185084292789,24.8225248544848)) ;
#101004 = CARTESIAN_POINT('Ctrl Pts',(41.8574973326201,263.188060815679,24.7589545102575)) ;
#101005 = CARTESIAN_POINT('Ctrl Pts',(41.8515054048496,263.18969189326,24.7235564441324)) ;
#101006 = CARTESIAN_POINT('Ctrl Pts',(41.8288396042035,263.194789620036,24.6116119757236)) ;
#101007 = CARTESIAN_POINT('Ctrl Pts',(41.8079399838252,263.198135712618,24.5360271352042)) ;
#101008 = CARTESIAN_POINT('Ctrl Pts',(41.7478250208186,263.205749223442,24.3659601537163)) ;
#101009 = CARTESIAN_POINT('Ctrl Pts',(41.7051096405367,263.209969965747,24.2730547361341)) ;
#101010 = CARTESIAN_POINT('Ctrl Pts',(41.6404218902882,263.215739775026,24.1606254410539)) ;
#101011 = CARTESIAN_POINT('Ctrl Pts',(41.6260296485181,263.216994073744,24.1369843001121)) ;
#101012 = CARTESIAN_POINT('Ctrl Pts',(41.6020403556091,263.219056457892,24.0996881501309)) ;
#101013 = CARTESIAN_POINT('Ctrl Pts',(41.5928123968713,263.219843806571,24.0858008718972)) ;
#101014 = CARTESIAN_POINT('Ctrl Pts',(41.5722938643976,263.221585631042,24.0558989607961)) ;
#101015 = CARTESIAN_POINT('Ctrl Pts',(41.5609272545832,263.222544244534,24.039940782142)) ;
#101016 = CARTESIAN_POINT('Ctrl Pts',(41.5245861708713,263.225580659118,23.9907654115108)) ;
#101017 = CARTESIAN_POINT('Ctrl Pts',(41.4986562029933,263.22770690375,23.9582758156866)) ;
#101018 = CARTESIAN_POINT('Ctrl Pts',(41.4109059869568,263.234694050313,23.8563343013838)) ;
#101019 = CARTESIAN_POINT('Ctrl Pts',(41.3445135837078,263.239662808617,23.7910460352389)) ;
#101020 = CARTESIAN_POINT('Ctrl Pts',(41.2341691711625,263.247159010316,23.6992394226413)) ;
#101021 = CARTESIAN_POINT('Ctrl Pts',(41.1938387993125,263.24976543816,23.6686604539096)) ;
#101022 = CARTESIAN_POINT('Ctrl Pts',(41.1182555322,263.254391408475,23.6165605199913)) ;
#101023 = CARTESIAN_POINT('Ctrl Pts',(41.0834731061389,263.256428855633,23.5944289685198)) ;
#101024 = CARTESIAN_POINT('Ctrl Pts',(41.0230259574888,263.259817367044,23.5590259489106)) ;
#101025 = CARTESIAN_POINT('Ctrl Pts',(40.9977704581187,263.261190359206,23.5450957540483)) ;
#101026 = CARTESIAN_POINT('Ctrl Pts',(40.9439089115288,263.264033444163,23.5171734933855)) ;
#101027 = CARTESIAN_POINT('Ctrl Pts',(40.9152382740148,263.265498213573,23.5033306941647)) ;
#101028 = CARTESIAN_POINT('Ctrl Pts',(40.8276193800529,263.269843530878,23.4640603732382)) ;
#101029 = CARTESIAN_POINT('Ctrl Pts',(40.7675880952944,263.272644121892,23.4411908274066)) ;
#101030 = CARTESIAN_POINT('Ctrl Pts',(40.5980758009466,263.280250569522,23.3875245171677)) ;
#101031 = CARTESIAN_POINT('Ctrl Pts',(40.4865646037941,263.284906580776,23.3643256552867)) ;
#101032 = CARTESIAN_POINT('Ctrl Pts',(40.3472783566533,263.291026599974,23.3498380828204)) ;
#101033 = CARTESIAN_POINT('Ctrl Pts',(40.320925317618,263.292198756319,23.3477251621585)) ;
#101034 = CARTESIAN_POINT('Ctrl Pts',(40.2726515134719,263.294388350675,23.3450008024137)) ;
#101035 = CARTESIAN_POINT('Ctrl Pts',(40.2507474472316,263.295397806973,23.3441948070596)) ;
#101036 = CARTESIAN_POINT('Ctrl Pts',(40.2125000072133,263.297197425772,23.3435373669686)) ;
#101037 = CARTESIAN_POINT('Ctrl Pts',(40.1961637934343,263.297978396315,23.3434952037403)) ;
#101038 = CARTESIAN_POINT('Ctrl Pts',(40.1560105545898,263.299927803157,23.3439779794298)) ;
#101039 = CARTESIAN_POINT('Ctrl Pts',(40.132201616325,263.301108610646,23.3447715799927)) ;
#101040 = CARTESIAN_POINT('Ctrl Pts',(40.0428126016676,263.30561579772,23.3496582322217)) ;
#101041 = CARTESIAN_POINT('Ctrl Pts',(39.9774771865611,263.309057949274,23.3570953752569)) ;
#101042 = CARTESIAN_POINT('Ctrl Pts',(39.8300932341571,263.316947114412,23.3827073434764)) ;
#101043 = CARTESIAN_POINT('Ctrl Pts',(39.7486255132985,263.321393499707,23.4032517507411)) ;
#101044 = CARTESIAN_POINT('Ctrl Pts',(39.6167153908434,263.328545406163,23.4472599661822)) ;
#101045 = CARTESIAN_POINT('Ctrl Pts',(39.5652860976606,263.3313230774,23.4672849376038)) ;
#101046 = CARTESIAN_POINT('Ctrl Pts',(39.4869005243371,263.335527213952,23.5023479041454)) ;
#101047 = CARTESIAN_POINT('Ctrl Pts',(39.4592163982495,263.337006406119,23.5156550640532)) ;
#101048 = CARTESIAN_POINT('Ctrl Pts',(39.4319120248721,263.338461000729,23.5297151930711)) ;
#101049 = CARTESIAN_POINT('',(41.1743400212928,263.,26.3871558334365)) ;
#101050 = CARTESIAN_POINT('Origin',(40.2,263.,25.0213203435596)) ;
#101051 = CARTESIAN_POINT('',(41.8777498381111,263.075690620251,25.020583310179)) ;
#101052 = CARTESIAN_POINT('Ctrl Pts',(41.8777498381111,263.075690620251,25.020583310179)) ;
#101053 = CARTESIAN_POINT('Ctrl Pts',(41.8777771592572,263.07272122919,25.0827759458533)) ;
#101054 = CARTESIAN_POINT('Ctrl Pts',(41.8743420727466,263.069751838128,25.1450776443993)) ;
#101055 = CARTESIAN_POINT('Ctrl Pts',(41.8674345209409,263.066782447066,25.2070814290289)) ;
#101056 = CARTESIAN_POINT('Ctrl Pts',(41.860540872367,263.063819032671,25.2689604150301)) ;
#101057 = CARTESIAN_POINT('Ctrl Pts',(41.8501887092101,263.060855618275,25.3305422015561)) ;
#101058 = CARTESIAN_POINT('Ctrl Pts',(41.8364199278902,263.05789220388,25.3914215217578)) ;
#101059 = CARTESIAN_POINT('Ctrl Pts',(41.8226673239878,263.054932271303,25.4522293127406)) ;
#101060 = CARTESIAN_POINT('Ctrl Pts',(41.8055061776375,263.051972338726,25.5123358062267)) ;
#101061 = CARTESIAN_POINT('Ctrl Pts',(41.7850297859598,263.049012406148,25.5713436522658)) ;
#101062 = CARTESIAN_POINT('Ctrl Pts',(41.7645710407854,263.046055024434,25.6303006454906)) ;
#101063 = CARTESIAN_POINT('Ctrl Pts',(41.740802882733,263.043097642719,25.688160415573)) ;
#101064 = CARTESIAN_POINT('Ctrl Pts',(41.7138685664242,263.040140261004,25.7445402451752)) ;
#101065 = CARTESIAN_POINT('Ctrl Pts',(41.6869490350041,263.037184502667,25.800889126544)) ;
#101066 = CARTESIAN_POINT('Ctrl Pts',(41.6568670075066,263.034228744329,25.8557592455103)) ;
#101067 = CARTESIAN_POINT('Ctrl Pts',(41.6238133602854,263.031272985992,25.9087889782576)) ;
#101068 = CARTESIAN_POINT('Ctrl Pts',(41.5907565441787,263.028316944283,25.9618237950174)) ;
#101069 = CARTESIAN_POINT('Ctrl Pts',(41.5547277859931,263.025360902574,26.0130174561376)) ;
#101070 = CARTESIAN_POINT('Ctrl Pts',(41.5159626404356,263.022404860865,26.0620351899405)) ;
#101071 = CARTESIAN_POINT('Ctrl Pts',(41.477196741694,263.019448761722,26.1110538761295)) ;
#101072 = CARTESIAN_POINT('Ctrl Pts',(41.4356946569183,263.016492662579,26.1578961760627)) ;
#101073 = CARTESIAN_POINT('Ctrl Pts',(41.3917324065674,263.013536563436,26.2022601953883)) ;
#101074 = CARTESIAN_POINT('Ctrl Pts',(41.3477333703716,263.010577990748,26.2466613367428)) ;
#101075 = CARTESIAN_POINT('Ctrl Pts',(41.3012704057273,263.00761941806,26.2885797186237)) ;
#101076 = CARTESIAN_POINT('Ctrl Pts',(41.2526557659135,263.004660845372,26.3277509391096)) ;
#101077 = CARTESIAN_POINT('Ctrl Pts',(41.2271270912358,263.003107230248,26.3483206553173)) ;
#101078 = CARTESIAN_POINT('Ctrl Pts',(41.2010056420111,263.001553615124,26.3681334975468)) ;
#101079 = CARTESIAN_POINT('Ctrl Pts',(41.1743400212928,263.,26.3871558334365)) ;
#101080 = CARTESIAN_POINT('Ctrl Pts',(39.4319120248721,263.238554795302,23.5297151930711)) ;
#101081 = CARTESIAN_POINT('Ctrl Pts',(39.4729859837156,263.236357167323,23.5085645461534)) ;
#101082 = CARTESIAN_POINT('Ctrl Pts',(39.5148870253905,263.234159539345,23.4891359763675)) ;
#101083 = CARTESIAN_POINT('Ctrl Pts',(39.5574566951772,263.231961911366,23.4714870738407)) ;
#101084 = CARTESIAN_POINT('Ctrl Pts',(39.6139302242998,263.229046506848,23.4480737888466)) ;
#101085 = CARTESIAN_POINT('Ctrl Pts',(39.6717913139331,263.226131102329,23.4277071800005)) ;
#101086 = CARTESIAN_POINT('Ctrl Pts',(39.7306799504516,263.223215697811,23.4105491762016)) ;
#101087 = CARTESIAN_POINT('Ctrl Pts',(39.7894735976778,263.220304995935,23.3934188488227)) ;
#101088 = CARTESIAN_POINT('Ctrl Pts',(39.8492910166438,263.21739429406,23.379486990035)) ;
#101089 = CARTESIAN_POINT('Ctrl Pts',(39.9097534462909,263.214483592184,23.3688670157588)) ;
#101090 = CARTESIAN_POINT('Ctrl Pts',(39.9701615273374,263.211575506686,23.3582565875882)) ;
#101091 = CARTESIAN_POINT('Ctrl Pts',(40.0312129718539,263.208667421188,23.3509522293592)) ;
#101092 = CARTESIAN_POINT('Ctrl Pts',(40.0925167041359,263.205759335691,23.347016785775)) ;
#101093 = CARTESIAN_POINT('Ctrl Pts',(40.1537876337663,263.202852806263,23.3430834479841)) ;
#101094 = CARTESIAN_POINT('Ctrl Pts',(40.215310077744,263.199946276836,23.3425154816823)) ;
#101095 = CARTESIAN_POINT('Ctrl Pts',(40.2766877039282,263.197039747409,23.3453239060436)) ;
#101096 = CARTESIAN_POINT('Ctrl Pts',(40.3380548153899,263.194133715904,23.3481318492882)) ;
#101097 = CARTESIAN_POINT('Ctrl Pts',(40.3992766515522,263.1912276844,23.3543150106123)) ;
#101098 = CARTESIAN_POINT('Ctrl Pts',(40.4599587899172,263.188321652896,23.3638323375563)) ;
#101099 = CARTESIAN_POINT('Ctrl Pts',(40.5206952141623,263.185413021674,23.3733581786444)) ;
#101100 = CARTESIAN_POINT('Ctrl Pts',(40.5808904733218,263.182504390451,23.3862240666862)) ;
#101101 = CARTESIAN_POINT('Ctrl Pts',(40.6401583757575,263.179595759228,23.4023374323618)) ;
#101102 = CARTESIAN_POINT('Ctrl Pts',(40.6994516451042,263.176685883099,23.4184576946255)) ;
#101103 = CARTESIAN_POINT('Ctrl Pts',(40.7578162835293,263.17377600697,23.4378280462673)) ;
#101104 = CARTESIAN_POINT('Ctrl Pts',(40.8148822755349,263.170866130841,23.4603062982246)) ;
#101105 = CARTESIAN_POINT('Ctrl Pts',(40.8720526552897,263.167950931833,23.4828256684391)) ;
#101106 = CARTESIAN_POINT('Ctrl Pts',(40.9279191788123,263.165035732824,23.5084640873553)) ;
#101107 = CARTESIAN_POINT('Ctrl Pts',(40.9821335654524,263.162120533815,23.5370319119222)) ;
#101108 = CARTESIAN_POINT('Ctrl Pts',(41.0284978638453,263.159627447291,23.5614631971352)) ;
#101109 = CARTESIAN_POINT('Ctrl Pts',(41.0736540897011,263.157134360768,23.5880360870147)) ;
#101110 = CARTESIAN_POINT('Ctrl Pts',(41.1174017602243,263.154641274244,23.6166071796584)) ;
#101111 = CARTESIAN_POINT('Ctrl Pts',(41.1683248599349,263.151739275301,23.649864461295)) ;
#101112 = CARTESIAN_POINT('Ctrl Pts',(41.2175404960184,263.148837276357,23.6859619109233)) ;
#101113 = CARTESIAN_POINT('Ctrl Pts',(41.2647134168509,263.145935277414,23.7246976526901)) ;
#101114 = CARTESIAN_POINT('Ctrl Pts',(41.3118076620972,263.143038118461,23.7633687905032)) ;
#101115 = CARTESIAN_POINT('Ctrl Pts',(41.356865561525,263.140140959508,23.80466916243)) ;
#101116 = CARTESIAN_POINT('Ctrl Pts',(41.3995810245911,263.137243800554,23.848353835964)) ;
#101117 = CARTESIAN_POINT('Ctrl Pts',(41.4422568256992,263.134349331657,23.8919979476134)) ;
#101118 = CARTESIAN_POINT('Ctrl Pts',(41.4825941434519,263.13145486276,23.9380216083587)) ;
#101119 = CARTESIAN_POINT('Ctrl Pts',(41.5203214559646,263.128560393863,23.9861409796716)) ;
#101120 = CARTESIAN_POINT('Ctrl Pts',(41.5580278495891,263.12566752988,24.0342336699495)) ;
#101121 = CARTESIAN_POINT('Ctrl Pts',(41.5931267911853,263.122774665896,24.0844193636267)) ;
#101122 = CARTESIAN_POINT('Ctrl Pts',(41.6253864283048,263.119881801913,24.1363804628307)) ;
#101123 = CARTESIAN_POINT('Ctrl Pts',(41.6576402441328,263.11698945995,24.18833218559)) ;
#101124 = CARTESIAN_POINT('Ctrl Pts',(41.6870555025148,263.114097117987,24.2420582416089)) ;
#101125 = CARTESIAN_POINT('Ctrl Pts',(41.713444335914,263.111204776025,24.2972130969519)) ;
#101126 = CARTESIAN_POINT('Ctrl Pts',(41.7398575598809,263.108309760739,24.3524189306087)) ;
#101127 = CARTESIAN_POINT('Ctrl Pts',(41.7632385472967,263.105414745454,24.4090557383128)) ;
#101128 = CARTESIAN_POINT('Ctrl Pts',(41.7834465659634,263.102519730169,24.466755617636)) ;
#101129 = CARTESIAN_POINT('Ctrl Pts',(41.8036634105825,263.099623450472,24.5244806976677)) ;
#101130 = CARTESIAN_POINT('Ctrl Pts',(41.8207043811825,263.096727170774,24.5832692807788)) ;
#101131 = CARTESIAN_POINT('Ctrl Pts',(41.8344788449778,263.093830891077,24.6427388228538)) ;
#101132 = CARTESIAN_POINT('Ctrl Pts',(41.8482796054899,263.090929082115,24.7023218977474)) ;
#101133 = CARTESIAN_POINT('Ctrl Pts',(41.8588013103894,263.088027273154,24.7625880219625)) ;
#101134 = CARTESIAN_POINT('Ctrl Pts',(41.8660047802855,263.085125464192,24.8231458382216)) ;
#101135 = CARTESIAN_POINT('Ctrl Pts',(41.8724630318549,263.082523855169,24.8774387855847)) ;
#101136 = CARTESIAN_POINT('Ctrl Pts',(41.8762548028084,263.079922246146,24.9319658532433)) ;
#101137 = CARTESIAN_POINT('Ctrl Pts',(41.8773874970113,263.077320637123,24.9864456052773)) ;
#101138 = CARTESIAN_POINT('Ctrl Pts',(41.877624057104,263.076777298179,24.9978235527949)) ;
#101139 = CARTESIAN_POINT('Ctrl Pts',(41.8777448388839,263.076233959235,25.0092033057449)) ;
#101140 = CARTESIAN_POINT('Ctrl Pts',(41.8777498381107,263.075690620291,25.0205833093468)) ;
#101141 = CARTESIAN_POINT('Origin',(40.2,263.,25.0213203435596)) ;
#101142 = CARTESIAN_POINT('Ctrl Pts',(41.0856881582581,263.,23.2689252008131)) ;
#101143 = CARTESIAN_POINT('Ctrl Pts',(41.136560203023,263.,23.2988237487254)) ;
#101144 = CARTESIAN_POINT('Ctrl Pts',(41.1859148580529,263.,23.331059625684)) ;
#101145 = CARTESIAN_POINT('Ctrl Pts',(41.2335581419714,263.,23.3656315345143)) ;
#101146 = CARTESIAN_POINT('Ctrl Pts',(41.2443647676521,263.,23.3734732626042)) ;
#101147 = CARTESIAN_POINT('Ctrl Pts',(41.2550832802686,263.,23.3814352538179)) ;
#101148 = CARTESIAN_POINT('Ctrl Pts',(41.2657112952103,263.,23.3895176261393)) ;
#101149 = CARTESIAN_POINT('Ctrl Pts',(41.3262097912653,263.,23.4355254058313)) ;
#101150 = CARTESIAN_POINT('Ctrl Pts',(41.3837800806245,263.,23.4854310739318)) ;
#101151 = CARTESIAN_POINT('Ctrl Pts',(41.4382345422844,263.,23.5388477209115)) ;
#101152 = CARTESIAN_POINT('Ctrl Pts',(41.4520628554996,263.,23.5524124886611)) ;
#101153 = CARTESIAN_POINT('Ctrl Pts',(41.4656930103321,263.,23.5662072310807)) ;
#101154 = CARTESIAN_POINT('Ctrl Pts',(41.4791016494721,263.,23.5802046256661)) ;
#101155 = CARTESIAN_POINT('Ctrl Pts',(41.5290702340151,263.,23.6323672640532)) ;
#101156 = CARTESIAN_POINT('Ctrl Pts',(41.576018175633,263.,23.6873903203988)) ;
#101157 = CARTESIAN_POINT('Ctrl Pts',(41.61980527048,263.,23.7449249724425)) ;
#101158 = CARTESIAN_POINT('Ctrl Pts',(41.6533521475531,263.,23.7890043503116)) ;
#101159 = CARTESIAN_POINT('Ctrl Pts',(41.68504294083,263.,23.8345588425587)) ;
#101160 = CARTESIAN_POINT('Ctrl Pts',(41.7147961550209,263.,23.8814408944727)) ;
#101161 = CARTESIAN_POINT('Ctrl Pts',(41.7260447826157,263.,23.8991653238226)) ;
#101162 = CARTESIAN_POINT('Ctrl Pts',(41.7370162940054,263.,23.9170795619092)) ;
#101163 = CARTESIAN_POINT('Ctrl Pts',(41.7477056363485,263.,23.9351757974312)) ;
#101164 = CARTESIAN_POINT('Ctrl Pts',(41.7567703799348,263.,23.9505217120459)) ;
#101165 = CARTESIAN_POINT('Ctrl Pts',(41.7656346827696,263.,23.9660032706815)) ;
#101166 = CARTESIAN_POINT('Ctrl Pts',(41.7742803042553,263.,23.9815879252681)) ;
#101167 = CARTESIAN_POINT('Ctrl Pts',(41.8089017809343,263.,24.0439968285742)) ;
#101168 = CARTESIAN_POINT('Ctrl Pts',(41.8400645548394,263.,24.1081277587535)) ;
#101169 = CARTESIAN_POINT('Ctrl Pts',(41.8676322251476,263.,24.173652136793)) ;
#101170 = CARTESIAN_POINT('Ctrl Pts',(41.8948232811182,263.,24.2382813568462)) ;
#101171 = CARTESIAN_POINT('Ctrl Pts',(41.9185170247662,263.,24.3042672193153)) ;
#101172 = CARTESIAN_POINT('Ctrl Pts',(41.9385345807979,263.,24.3713076356331)) ;
#101173 = CARTESIAN_POINT('Ctrl Pts',(41.9533071976636,263.,24.4207823259104)) ;
#101174 = CARTESIAN_POINT('Ctrl Pts',(41.9660767335746,263.,24.4708316800822)) ;
#101175 = CARTESIAN_POINT('Ctrl Pts',(41.9767529969391,263.,24.5213342818128)) ;
#101176 = CARTESIAN_POINT('Ctrl Pts',(41.982807227349,263.,24.5499729896388)) ;
#101177 = CARTESIAN_POINT('Ctrl Pts',(41.9881880273261,263.,24.5787574266971)) ;
#101178 = CARTESIAN_POINT('Ctrl Pts',(41.9928765697548,263.,24.6076650255236)) ;
#101179 = CARTESIAN_POINT('Ctrl Pts',(41.9948224733389,263.,24.6196626561349)) ;
#101180 = CARTESIAN_POINT('Ctrl Pts',(41.9966494227026,263.,24.631683708088)) ;
#101181 = CARTESIAN_POINT('Ctrl Pts',(41.9983549861683,263.,24.6437194565562)) ;
#101182 = CARTESIAN_POINT('Ctrl Pts',(42.0079094303121,263.,24.7111428557921)) ;
#101183 = CARTESIAN_POINT('Ctrl Pts',(42.013629467554,263.,24.778810574148)) ;
#101184 = CARTESIAN_POINT('Ctrl Pts',(42.0153609924019,263.,24.8464405106901)) ;
#101185 = CARTESIAN_POINT('Ctrl Pts',(42.0165329099533,263.,24.89221329283)) ;
#101186 = CARTESIAN_POINT('Ctrl Pts',(42.0158767839533,263.,24.9379689419043)) ;
#101187 = CARTESIAN_POINT('Ctrl Pts',(42.0133312280121,263.,24.9836191849968)) ;
#101188 = CARTESIAN_POINT('Ctrl Pts',(42.0095039151958,263.,25.0522555711132)) ;
#101189 = CARTESIAN_POINT('Ctrl Pts',(42.001407309068,263.,25.1206549432494)) ;
#101190 = CARTESIAN_POINT('Ctrl Pts',(41.9892161635851,263.,25.1885066891326)) ;
#101191 = CARTESIAN_POINT('Ctrl Pts',(41.9834556365975,263.,25.2205678120075)) ;
#101192 = CARTESIAN_POINT('Ctrl Pts',(41.9767802052095,263.,25.252506372225)) ;
#101193 = CARTESIAN_POINT('Ctrl Pts',(41.9692048103826,263.,25.2842875802732)) ;
#101194 = CARTESIAN_POINT('Ctrl Pts',(41.9661292099625,263.,25.2971907092924)) ;
#101195 = CARTESIAN_POINT('Ctrl Pts',(41.9629052404632,263.,25.310067883192)) ;
#101196 = CARTESIAN_POINT('Ctrl Pts',(41.9595338081523,263.,25.3229166948442)) ;
#101197 = CARTESIAN_POINT('Ctrl Pts',(41.9566264007368,263.,25.3339970686539)) ;
#101198 = CARTESIAN_POINT('Ctrl Pts',(41.9536092891766,263.,25.3450561348907)) ;
#101199 = CARTESIAN_POINT('Ctrl Pts',(41.9504871902772,263.,25.3560786681579)) ;
#101200 = CARTESIAN_POINT('Ctrl Pts',(41.9320746739268,263.,25.4210838395316)) ;
#101201 = CARTESIAN_POINT('Ctrl Pts',(41.9099834503833,263.,25.484942222437)) ;
#101202 = CARTESIAN_POINT('Ctrl Pts',(41.8844163316153,263.,25.5473739875613)) ;
#101203 = CARTESIAN_POINT('Ctrl Pts',(41.8588447200449,263.,25.6098167235577)) ;
#101204 = CARTESIAN_POINT('Ctrl Pts',(41.8297953520112,263.,25.6708332212835)) ;
#101205 = CARTESIAN_POINT('Ctrl Pts',(41.7974260930702,263.,25.7301185903455)) ;
#101206 = CARTESIAN_POINT('Ctrl Pts',(41.7652951541796,263.,25.7889674683475)) ;
#101207 = CARTESIAN_POINT('Ctrl Pts',(41.7298923901342,263.,25.8461114160743)) ;
#101208 = CARTESIAN_POINT('Ctrl Pts',(41.6913374251241,263.,25.9012152058858)) ;
#101209 = CARTESIAN_POINT('Ctrl Pts',(41.6836283485783,263.,25.9122332247975)) ;
#101210 = CARTESIAN_POINT('Ctrl Pts',(41.6757931522158,263.,25.9231695365843)) ;
#101211 = CARTESIAN_POINT('Ctrl Pts',(41.667832658191,263.,25.9340212385773)) ;
#101212 = CARTESIAN_POINT('Ctrl Pts',(41.660906427956,263.,25.9434630378188)) ;
#101213 = CARTESIAN_POINT('Ctrl Pts',(41.6538848142978,263.,25.9528413248573)) ;
#101214 = CARTESIAN_POINT('Ctrl Pts',(41.646778399557,263.,25.962141416589)) ;
#101215 = CARTESIAN_POINT('Ctrl Pts',(41.6066123392045,263.,26.0147063258163)) ;
#101216 = CARTESIAN_POINT('Ctrl Pts',(41.5636680906624,263.,26.0648760908122)) ;
#101217 = CARTESIAN_POINT('Ctrl Pts',(41.5181015106568,263.,26.112369179746)) ;
#101218 = CARTESIAN_POINT('Ctrl Pts',(41.4738500584133,263.,26.1584915386457)) ;
#101219 = CARTESIAN_POINT('Ctrl Pts',(41.4271247588532,263.,26.2020900403433)) ;
#101220 = CARTESIAN_POINT('Ctrl Pts',(41.3780390291705,263.,26.2428690423025)) ;
#101221 = CARTESIAN_POINT('Ctrl Pts',(41.3294671498362,263.,26.2832211522811)) ;
#101222 = CARTESIAN_POINT('Ctrl Pts',(41.278583472291,263.,26.3208130709105)) ;
#101223 = CARTESIAN_POINT('Ctrl Pts',(41.2254776126781,263.,26.3553123614681)) ;
#101224 = CARTESIAN_POINT('Ctrl Pts',(41.2086540352895,263.,26.3662415035399)) ;
#101225 = CARTESIAN_POINT('Ctrl Pts',(41.1916073222241,263.,26.3768598912907)) ;
#101226 = CARTESIAN_POINT('Ctrl Pts',(41.1743400212929,263.,26.3871558334365)) ;
#101227 = CARTESIAN_POINT('',(39.2243975151537,262.999430917611,26.3874606005124)) ;
#101228 = CARTESIAN_POINT('Ctrl Pts',(39.2427274574787,263.,26.3991716932468)) ;
#101229 = CARTESIAN_POINT('Ctrl Pts',(39.2367806955717,262.99981030587,26.3950401358826)) ;
#101230 = CARTESIAN_POINT('Ctrl Pts',(39.2308606815433,262.999620611741,26.3908700789342)) ;
#101231 = CARTESIAN_POINT('Ctrl Pts',(39.2249679116208,262.999430917611,26.386661871944)) ;
#101232 = CARTESIAN_POINT('Ctrl Pts',(39.2237775472856,263.,26.388236458444)) ;
#101233 = CARTESIAN_POINT('Ctrl Pts',(39.1669376385685,263.,26.3549247848828)) ;
#101234 = CARTESIAN_POINT('Ctrl Pts',(39.1123107922543,263.,26.3182679632608)) ;
#101235 = CARTESIAN_POINT('Ctrl Pts',(39.0602509694005,263.,26.2783516922222)) ;
#101236 = CARTESIAN_POINT('Ctrl Pts',(39.0544382172448,263.,26.2738948312917)) ;
#101237 = CARTESIAN_POINT('Ctrl Pts',(39.0486574820743,263.,26.2693972834884)) ;
#101238 = CARTESIAN_POINT('Ctrl Pts',(39.0429092691825,263.,26.264859129371)) ;
#101239 = CARTESIAN_POINT('Ctrl Pts',(39.0082261335841,263.,26.2374771556025)) ;
#101240 = CARTESIAN_POINT('Ctrl Pts',(38.974726487123,263.,26.2086177375078)) ;
#101241 = CARTESIAN_POINT('Ctrl Pts',(38.9424340004638,263.,26.1783897705185)) ;
#101242 = CARTESIAN_POINT('Ctrl Pts',(38.9236083074801,263.,26.1607676396474)) ;
#101243 = CARTESIAN_POINT('Ctrl Pts',(38.9051929933829,263.,26.1426801918312)) ;
#101244 = CARTESIAN_POINT('Ctrl Pts',(38.8871938087522,263.,26.1241474718767)) ;
#101245 = CARTESIAN_POINT('Ctrl Pts',(38.8774589630145,263.,26.1141240639523)) ;
#101246 = CARTESIAN_POINT('Ctrl Pts',(38.8678456247877,263.,26.1039699594861)) ;
#101247 = CARTESIAN_POINT('Ctrl Pts',(38.8583651879793,263.,26.0936999832725)) ;
#101248 = CARTESIAN_POINT('Ctrl Pts',(38.8138474201968,263.,26.0454747352747)) ;
#101249 = CARTESIAN_POINT('Ctrl Pts',(38.7721995286391,263.,25.9946393686953)) ;
#101250 = CARTESIAN_POINT('Ctrl Pts',(38.7334891808602,263.,25.9415526275785)) ;
#101251 = CARTESIAN_POINT('Ctrl Pts',(38.7023688985965,263.,25.898874778817)) ;
#101252 = CARTESIAN_POINT('Ctrl Pts',(38.673147542335,263.,25.8547406920465)) ;
#101253 = CARTESIAN_POINT('Ctrl Pts',(38.645875368868,263.,25.8093176005942)) ;
#101254 = CARTESIAN_POINT('Ctrl Pts',(38.6367093756936,263.,25.7940512065638)) ;
#101255 = CARTESIAN_POINT('Ctrl Pts',(38.6277636836788,263.,25.7786390871617)) ;
#101256 = CARTESIAN_POINT('Ctrl Pts',(38.6190405938922,263.,25.7630872526879)) ;
#101257 = CARTESIAN_POINT('Ctrl Pts',(38.6116128714022,263.,25.7498448450654)) ;
#101258 = CARTESIAN_POINT('Ctrl Pts',(38.6043456429172,263.,25.7364991203329)) ;
#101259 = CARTESIAN_POINT('Ctrl Pts',(38.5972509227465,263.,25.7230744078097)) ;
#101260 = CARTESIAN_POINT('Ctrl Pts',(38.5653661356432,263.,25.6627416405649)) ;
#101261 = CARTESIAN_POINT('Ctrl Pts',(38.5369123809752,263.,25.6007297614524)) ;
#101262 = CARTESIAN_POINT('Ctrl Pts',(38.5119644979003,263.,25.5374093499191)) ;
#101263 = CARTESIAN_POINT('Ctrl Pts',(38.4870571409114,263.,25.4741917979528)) ;
#101264 = CARTESIAN_POINT('Ctrl Pts',(38.465643799872,263.,25.4096690022917)) ;
#101265 = CARTESIAN_POINT('Ctrl Pts',(38.447837750618,263.,25.3441753824993)) ;
#101266 = CARTESIAN_POINT('Ctrl Pts',(38.4346381616535,263.,25.2956250921608)) ;
#101267 = CARTESIAN_POINT('Ctrl Pts',(38.4234216189492,263.,25.2465405280528)) ;
#101268 = CARTESIAN_POINT('Ctrl Pts',(38.414250442511,263.,25.1970504156763)) ;
#101269 = CARTESIAN_POINT('Ctrl Pts',(38.4090270872937,263.,25.1688637987869)) ;
#101270 = CARTESIAN_POINT('Ctrl Pts',(38.4044674641103,263.,25.140545538497)) ;
#101271 = CARTESIAN_POINT('Ctrl Pts',(38.4005853285551,263.,25.1121189487793)) ;
#101272 = CARTESIAN_POINT('Ctrl Pts',(38.3986277653732,263.,25.0977848678006)) ;
#101273 = CARTESIAN_POINT('Ctrl Pts',(38.3968422492944,263.,25.0834199356196)) ;
#101274 = CARTESIAN_POINT('Ctrl Pts',(38.3952331809663,263.,25.0690525878883)) ;
#101275 = CARTESIAN_POINT('Ctrl Pts',(38.3874502671335,263.,24.9995590633116)) ;
#101276 = CARTESIAN_POINT('Ctrl Pts',(38.3837740175701,263.,24.9298951051885)) ;
#101277 = CARTESIAN_POINT('Ctrl Pts',(38.384311998664,263.,24.8604163963716)) ;
#101278 = CARTESIAN_POINT('Ctrl Pts',(38.3846040717562,263.,24.8226959977267)) ;
#101279 = CARTESIAN_POINT('Ctrl Pts',(38.3861390574197,263.,24.7850297485891)) ;
#101280 = CARTESIAN_POINT('Ctrl Pts',(38.3889402251797,263.,24.7474723441793)) ;
#101281 = CARTESIAN_POINT('Ctrl Pts',(38.3939657642221,263.,24.680091088087)) ;
#101282 = CARTESIAN_POINT('Ctrl Pts',(38.4030636298359,263.,24.6130599957594)) ;
#101283 = CARTESIAN_POINT('Ctrl Pts',(38.4160158840873,263.,24.5466214244428)) ;
#101284 = CARTESIAN_POINT('Ctrl Pts',(38.422527882029,263.,24.51321813948)) ;
#101285 = CARTESIAN_POINT('Ctrl Pts',(38.4300150165224,263.,24.4799646157873)) ;
#101286 = CARTESIAN_POINT('Ctrl Pts',(38.4384544132907,263.,24.4468920772989)) ;
#101287 = CARTESIAN_POINT('Ctrl Pts',(38.4425981998155,263.,24.4306532935215)) ;
#101288 = CARTESIAN_POINT('Ctrl Pts',(38.4469716106731,263.,24.4144581511406)) ;
#101289 = CARTESIAN_POINT('Ctrl Pts',(38.451572204719,263.,24.3983104098412)) ;
#101290 = CARTESIAN_POINT('Ctrl Pts',(38.4544388118984,263.,24.3882488328627)) ;
#101291 = CARTESIAN_POINT('Ctrl Pts',(38.4573929319971,263.,24.3782082726981)) ;
#101292 = CARTESIAN_POINT('Ctrl Pts',(38.4604312466437,263.,24.368197766504)) ;
#101293 = CARTESIAN_POINT('Ctrl Pts',(38.4806470280642,263.,24.3015916941675)) ;
#101294 = CARTESIAN_POINT('Ctrl Pts',(38.5046153480752,263.,24.2362112258845)) ;
#101295 = CARTESIAN_POINT('Ctrl Pts',(38.5320710142609,263.,24.1723085240421)) ;
#101296 = CARTESIAN_POINT('Ctrl Pts',(38.5601590227769,263.,24.1069340537449)) ;
#101297 = CARTESIAN_POINT('Ctrl Pts',(38.5918971212003,263.,24.0431053156208)) ;
#101298 = CARTESIAN_POINT('Ctrl Pts',(38.6270568318401,263.,23.9810964403393)) ;
#101299 = CARTESIAN_POINT('Ctrl Pts',(38.6621511208827,263.,23.9192029448372)) ;
#101300 = CARTESIAN_POINT('Ctrl Pts',(38.700654786082,263.,23.8591216331877)) ;
#101301 = CARTESIAN_POINT('Ctrl Pts',(38.742389300636,263.,23.8011427668039)) ;
#101302 = CARTESIAN_POINT('Ctrl Pts',(38.7526688381686,263.,23.7868621182937)) ;
#101303 = CARTESIAN_POINT('Ctrl Pts',(38.7631445953972,263.,23.7727091410837)) ;
#101304 = CARTESIAN_POINT('Ctrl Pts',(38.7738143068348,263.,23.7586884371728)) ;
#101305 = CARTESIAN_POINT('Ctrl Pts',(38.7824522458874,263.,23.7473376160596)) ;
#101306 = CARTESIAN_POINT('Ctrl Pts',(38.7912188006332,263.,23.7360718015792)) ;
#101307 = CARTESIAN_POINT('Ctrl Pts',(38.8000982758865,263.,23.7249112410076)) ;
#101308 = CARTESIAN_POINT('Ctrl Pts',(38.8456525266383,263.,23.6676543693683)) ;
#101309 = CARTESIAN_POINT('Ctrl Pts',(38.8942517906015,263.,23.6130628129694)) ;
#101310 = CARTESIAN_POINT('Ctrl Pts',(38.9456535024128,263.,23.5614140617915)) ;
#101311 = CARTESIAN_POINT('Ctrl Pts',(38.996702915142,263.,23.5101193028638)) ;
#101312 = CARTESIAN_POINT('Ctrl Pts',(39.0505170528315,263.,23.4617262579711)) ;
#101313 = CARTESIAN_POINT('Ctrl Pts',(39.1069036408252,263.,23.4165290640856)) ;
#101314 = CARTESIAN_POINT('Ctrl Pts',(39.1626773094991,263.,23.3718231613798)) ;
#101315 = CARTESIAN_POINT('Ctrl Pts',(39.2209683536167,263.,23.3302431739907)) ;
#101316 = CARTESIAN_POINT('Ctrl Pts',(39.2816269746244,263.,23.2921084083525)) ;
#101317 = CARTESIAN_POINT('Ctrl Pts',(39.3034799837762,263.,23.2783698932223)) ;
#101318 = CARTESIAN_POINT('Ctrl Pts',(39.3256405828265,263.,23.2650789194409)) ;
#101319 = CARTESIAN_POINT('Ctrl Pts',(39.3481027319428,263.,23.25225186137)) ;
#101320 = CARTESIAN_POINT('Ctrl Pts',(40.9266772327442,265.16663141208,23.5122865229654)) ;
#101321 = CARTESIAN_POINT('Ctrl Pts',(41.4154229970103,265.140857866373,23.7476426923537)) ;
#101322 = CARTESIAN_POINT('Ctrl Pts',(42.139053620203,265.089310774958,24.7267012755206)) ;
#101323 = CARTESIAN_POINT('Ctrl Pts',(41.537785195068,265.011990137836,26.4588392827834)) ;
#101324 = CARTESIAN_POINT('Ctrl Pts',(39.767321066632,264.934669500713,26.9357152639846)) ;
#101325 = CARTESIAN_POINT('Ctrl Pts',(38.3751878547293,264.857348863591,25.744116361454)) ;
#101326 = CARTESIAN_POINT('Ctrl Pts',(38.5739887027783,264.780028226469,23.9217644529074)) ;
#101327 = CARTESIAN_POINT('Ctrl Pts',(40.191063261612,264.702707589347,23.0585544040981)) ;
#101328 = CARTESIAN_POINT('Ctrl Pts',(41.8158285227973,264.625386952225,23.9069987676438)) ;
#101329 = CARTESIAN_POINT('Ctrl Pts',(42.0314636541983,264.548066315103,25.72729466396)) ;
#101330 = CARTESIAN_POINT('Ctrl Pts',(40.6498435869966,264.47074567798,26.9318857254471)) ;
#101331 = CARTESIAN_POINT('Ctrl Pts',(38.8759213080425,264.393425040858,26.4702669479006)) ;
#101332 = CARTESIAN_POINT('Ctrl Pts',(38.2567337248227,264.316104403736,24.7450065743952)) ;
#101333 = CARTESIAN_POINT('Ctrl Pts',(39.3322857677736,264.238783766614,23.2607234419196)) ;
#101334 = CARTESIAN_POINT('Ctrl Pts',(41.1645770980241,264.161463129492,23.3118696438206)) ;
#101335 = CARTESIAN_POINT('Ctrl Pts',(42.1556538103889,264.084142492369,24.8538413017259)) ;
#101336 = CARTESIAN_POINT('Ctrl Pts',(41.4411893612298,264.006821855247,26.5418727571386)) ;
#101337 = CARTESIAN_POINT('Ctrl Pts',(39.6442745448301,263.929501218125,26.9038183269182)) ;
#101338 = CARTESIAN_POINT('Ctrl Pts',(38.3320113478042,263.852180581003,25.6240238449097)) ;
#101339 = CARTESIAN_POINT('Ctrl Pts',(38.648837232223,263.774859943881,23.8186047859197)) ;
#101340 = CARTESIAN_POINT('Ctrl Pts',(40.3184403474066,263.697539306759,23.0620880410149)) ;
#101341 = CARTESIAN_POINT('Ctrl Pts',(41.8847589041631,263.620218669636,24.0142223877692)) ;
#101342 = CARTESIAN_POINT('Ctrl Pts',(41.9817681831547,263.542898032514,25.8446772109839)) ;
#101343 = CARTESIAN_POINT('Ctrl Pts',(40.5249220723503,263.465577395392,26.9570258080617)) ;
#101344 = CARTESIAN_POINT('Ctrl Pts',(38.7846224372234,263.38825675827,26.381335876614)) ;
#101345 = CARTESIAN_POINT('Ctrl Pts',(38.2788622298172,263.310936121148,24.6193214418341)) ;
#101346 = CARTESIAN_POINT('Ctrl Pts',(39.448117170112,263.233615484025,23.2083693842535)) ;
#101347 = CARTESIAN_POINT('Ctrl Pts',(41.2738845567306,263.156294846903,23.377269891905)) ;
#101348 = CARTESIAN_POINT('Ctrl Pts',(42.1610135674441,263.078965437305,24.9821346196071)) ;
#101349 = CARTESIAN_POINT('Ctrl Pts',(41.6141021871797,263.027409573415,26.0701640241726)) ;
#101350 = CARTESIAN_POINT('Ctrl Pts',(41.1722257452137,263.001627255232,26.3851458267893)) ;
#101351 = CARTESIAN_POINT('Ctrl Pts',(40.9687759254743,265.110610308119,23.4248634577175)) ;
#101352 = CARTESIAN_POINT('Ctrl Pts',(41.4858362657664,265.084836762411,23.673854548651)) ;
#101353 = CARTESIAN_POINT('Ctrl Pts',(42.2513890820361,265.033289670997,24.7096330682631)) ;
#101354 = CARTESIAN_POINT('Ctrl Pts',(41.6152872899847,264.955969033874,26.542119266508)) ;
#101355 = CARTESIAN_POINT('Ctrl Pts',(39.7422546180825,264.878648396752,27.0466221699495)) ;
#101356 = CARTESIAN_POINT('Ctrl Pts',(38.2694707600797,264.80132775963,25.7859902032268)) ;
#101357 = CARTESIAN_POINT('Ctrl Pts',(38.4797887651819,264.724007122508,23.8580637292653)) ;
#101358 = CARTESIAN_POINT('Ctrl Pts',(40.1905455283097,264.646686485386,22.9448452131905)) ;
#101359 = CARTESIAN_POINT('Ctrl Pts',(41.9094385403132,264.569365848263,23.8424426215131)) ;
#101360 = CARTESIAN_POINT('Ctrl Pts',(42.1375660916355,264.492045211141,25.768193972003)) ;
#101361 = CARTESIAN_POINT('Ctrl Pts',(40.6759044378011,264.414724574019,27.0425707742258)) ;
#101362 = CARTESIAN_POINT('Ctrl Pts',(38.7992132738682,264.337403936897,26.5542089721305)) ;
#101363 = CARTESIAN_POINT('Ctrl Pts',(38.1441542106657,264.260083299775,24.7289988505517)) ;
#101364 = CARTESIAN_POINT('Ctrl Pts',(39.2820163590266,264.182762662652,23.1587265378696)) ;
#101365 = CARTESIAN_POINT('Ctrl Pts',(41.2204580765855,264.10544202553,23.2128357997664)) ;
#101366 = CARTESIAN_POINT('Ctrl Pts',(42.2689509733383,264.028121388408,24.8441387152086)) ;
#101367 = CARTESIAN_POINT('Ctrl Pts',(41.5130953563313,263.950800751286,26.6299631306286)) ;
#101368 = CARTESIAN_POINT('Ctrl Pts',(39.6120796250978,263.873480114164,27.0128773432121)) ;
#101369 = CARTESIAN_POINT('Ctrl Pts',(38.2237929026015,263.796159477042,25.6589403502952)) ;
#101370 = CARTESIAN_POINT('Ctrl Pts',(38.5589735048453,263.718838839919,23.7489276990081)) ;
#101371 = CARTESIAN_POINT('Ctrl Pts',(40.3253019684505,263.641518202797,22.948583564784)) ;
#101372 = CARTESIAN_POINT('Ctrl Pts',(41.9823622750059,263.564197565675,23.9558780424679)) ;
#101373 = CARTESIAN_POINT('Ctrl Pts',(42.0849916059877,263.486876928553,25.8923768583746)) ;
#101374 = CARTESIAN_POINT('Ctrl Pts',(40.5437458277518,263.409556291431,27.069167300727)) ;
#101375 = CARTESIAN_POINT('Ctrl Pts',(38.702625172926,263.332235654309,26.460125844779)) ;
#101376 = CARTESIAN_POINT('Ctrl Pts',(38.1675646894037,263.254915017186,24.5960323838054)) ;
#101377 = CARTESIAN_POINT('Ctrl Pts',(39.4045582380329,263.177594380064,23.1033394453326)) ;
#101378 = CARTESIAN_POINT('Ctrl Pts',(41.3360980594305,263.100273742942,23.2820248894775)) ;
#101379 = CARTESIAN_POINT('Ctrl Pts',(42.2746212379409,263.022944333345,24.9798644676362)) ;
#101380 = CARTESIAN_POINT('Ctrl Pts',(41.696025564966,262.971388469454,26.1309268303295)) ;
#101381 = CARTESIAN_POINT('Ctrl Pts',(41.2285498339117,262.945606151272,26.4641565173252)) ;
#101382 = CARTESIAN_POINT('Ctrl Pts',(41.0108746182042,265.054589204158,23.3374403924696)) ;
#101383 = CARTESIAN_POINT('Ctrl Pts',(41.5562495345224,265.028815658451,23.6000664049484)) ;
#101384 = CARTESIAN_POINT('Ctrl Pts',(42.3637245438692,264.977268567036,24.6925648610056)) ;
#101385 = CARTESIAN_POINT('Ctrl Pts',(41.6927893849013,264.899947929914,26.6253992502325)) ;
#101386 = CARTESIAN_POINT('Ctrl Pts',(39.7171881695331,264.822627292792,27.1575290759145)) ;
#101387 = CARTESIAN_POINT('Ctrl Pts',(38.1637536654301,264.74530665567,25.8278640449995)) ;
#101388 = CARTESIAN_POINT('Ctrl Pts',(38.3855888275855,264.667986018547,23.7943630056233)) ;
#101389 = CARTESIAN_POINT('Ctrl Pts',(40.1900277950074,264.590665381425,22.8311360222829)) ;
#101390 = CARTESIAN_POINT('Ctrl Pts',(42.0030485578291,264.513344744303,23.7778864753824)) ;
#101391 = CARTESIAN_POINT('Ctrl Pts',(42.2436685290726,264.436024107181,25.8090932800459)) ;
#101392 = CARTESIAN_POINT('Ctrl Pts',(40.7019652886055,264.358703470059,27.1532558230045)) ;
#101393 = CARTESIAN_POINT('Ctrl Pts',(38.7225052396939,264.281382832936,26.6381509963604)) ;
#101394 = CARTESIAN_POINT('Ctrl Pts',(38.0315746965087,264.204062195814,24.7129911267082)) ;
#101395 = CARTESIAN_POINT('Ctrl Pts',(39.2317469502797,264.126741558692,23.0567296338196)) ;
#101396 = CARTESIAN_POINT('Ctrl Pts',(41.276339055147,264.04942092157,23.113801955712)) ;
#101397 = CARTESIAN_POINT('Ctrl Pts',(42.3822481362876,263.972100284448,24.8344361286912)) ;
#101398 = CARTESIAN_POINT('Ctrl Pts',(41.585001351433,263.894779647326,26.7180535041185)) ;
#101399 = CARTESIAN_POINT('Ctrl Pts',(39.5798847053656,263.817459010204,27.121936359506)) ;
#101400 = CARTESIAN_POINT('Ctrl Pts',(38.1155744573986,263.740138373081,25.6938568556807)) ;
#101401 = CARTESIAN_POINT('Ctrl Pts',(38.4691097774677,263.662817735959,23.6792506120963)) ;
#101402 = CARTESIAN_POINT('Ctrl Pts',(40.3321635894945,263.585497098837,22.8350790885532)) ;
#101403 = CARTESIAN_POINT('Ctrl Pts',(42.0799656458485,263.508176461715,23.8975336971666)) ;
#101404 = CARTESIAN_POINT('Ctrl Pts',(42.1882150288208,263.430855824592,25.9400765057655)) ;
#101405 = CARTESIAN_POINT('Ctrl Pts',(40.5625695831534,263.35353518747,27.1813087933923)) ;
#101406 = CARTESIAN_POINT('Ctrl Pts',(38.6206279086286,263.276214550348,26.5389158129438)) ;
#101407 = CARTESIAN_POINT('Ctrl Pts',(38.0562671489902,263.198893913226,24.5727433257766)) ;
#101408 = CARTESIAN_POINT('Ctrl Pts',(39.360999305954,263.121573276104,22.9983095064116)) ;
#101409 = CARTESIAN_POINT('Ctrl Pts',(41.3983115621305,263.044252638982,23.1867798870499)) ;
#101410 = CARTESIAN_POINT('Ctrl Pts',(42.3882289084377,262.966923229383,24.9775943156654)) ;
#101411 = CARTESIAN_POINT('Ctrl Pts',(41.7779489427525,262.915367365494,26.1916896364865)) ;
#101412 = CARTESIAN_POINT('Ctrl Pts',(41.2848739226097,262.889585047311,26.543167207861)) ;
#101413 = CARTESIAN_POINT('Ctrl Pts',(41.0529733109342,264.998568100198,23.2500173272218)) ;
#101414 = CARTESIAN_POINT('Ctrl Pts',(41.6266628032785,264.972794554491,23.5262782612457)) ;
#101415 = CARTESIAN_POINT('Ctrl Pts',(42.4760600057023,264.921247463076,24.6754966537481)) ;
#101416 = CARTESIAN_POINT('Ctrl Pts',(41.770291479818,264.843926825954,26.708679233957)) ;
#101417 = CARTESIAN_POINT('Ctrl Pts',(39.6921217209837,264.766606188831,27.2684359818795)) ;
#101418 = CARTESIAN_POINT('Ctrl Pts',(38.0580365707805,264.689285551709,25.8697378867723)) ;
#101419 = CARTESIAN_POINT('Ctrl Pts',(38.291388889989,264.611964914587,23.7306622819812)) ;
#101420 = CARTESIAN_POINT('Ctrl Pts',(40.1895100617051,264.534644277465,22.7174268313754)) ;
#101421 = CARTESIAN_POINT('Ctrl Pts',(42.096658575345,264.457323640343,23.7133303292517)) ;
#101422 = CARTESIAN_POINT('Ctrl Pts',(42.3497709665098,264.38000300322,25.8499925880888)) ;
#101423 = CARTESIAN_POINT('Ctrl Pts',(40.7280261394099,264.302682366099,27.2639408717831)) ;
#101424 = CARTESIAN_POINT('Ctrl Pts',(38.6457972055196,264.225361728976,26.7220930205903)) ;
#101425 = CARTESIAN_POINT('Ctrl Pts',(37.9189951823518,264.148041091854,24.6969834028647)) ;
#101426 = CARTESIAN_POINT('Ctrl Pts',(39.1814775415326,264.070720454732,22.9547327297695)) ;
#101427 = CARTESIAN_POINT('Ctrl Pts',(41.3322200337085,263.99339981761,23.0147681116578)) ;
#101428 = CARTESIAN_POINT('Ctrl Pts',(42.4955452992371,263.916079180488,24.8247335421739)) ;
#101429 = CARTESIAN_POINT('Ctrl Pts',(41.6569073465345,263.838758543365,26.8061438776086)) ;
#101430 = CARTESIAN_POINT('Ctrl Pts',(39.5476897856333,263.761437906243,27.2309953757999)) ;
#101431 = CARTESIAN_POINT('Ctrl Pts',(38.0073560121957,263.684117269121,25.7287733610662)) ;
#101432 = CARTESIAN_POINT('Ctrl Pts',(38.37924605009,263.606796631999,23.6095735251847)) ;
#101433 = CARTESIAN_POINT('Ctrl Pts',(40.3390252105383,263.529475994877,22.7215746123224)) ;
#101434 = CARTESIAN_POINT('Ctrl Pts',(42.1775690166913,263.452155357755,23.8391893518654)) ;
#101435 = CARTESIAN_POINT('Ctrl Pts',(42.2914384516538,263.374834720632,25.9877761531562)) ;
#101436 = CARTESIAN_POINT('Ctrl Pts',(40.5813933385549,263.29751408351,27.2934502860576)) ;
#101437 = CARTESIAN_POINT('Ctrl Pts',(38.5386306443311,263.220193446388,26.6177057811087)) ;
#101438 = CARTESIAN_POINT('Ctrl Pts',(37.9449696085767,263.142872809266,24.5494542677479)) ;
#101439 = CARTESIAN_POINT('Ctrl Pts',(39.3174403738751,263.065552172143,22.8932795674907)) ;
#101440 = CARTESIAN_POINT('Ctrl Pts',(41.4605250648304,262.988231535021,23.0915348846222)) ;
#101441 = CARTESIAN_POINT('Ctrl Pts',(42.5018365789347,262.910902125423,24.9753241636946)) ;
#101442 = CARTESIAN_POINT('Ctrl Pts',(41.859872320539,262.859346261533,26.2524524426436)) ;
#101443 = CARTESIAN_POINT('Ctrl Pts',(41.3411980113077,262.83356394335,26.6221778983969)) ;
#101444 = CARTESIAN_POINT('',(41.1755994881009,265.000571825747,26.3874569216172)) ;
#101445 = CARTESIAN_POINT('Ctrl Pts',(41.176222444591,265.,26.3882365197604)) ;
#101446 = CARTESIAN_POINT('Ctrl Pts',(41.2333448641361,265.,26.3547592787871)) ;
#101447 = CARTESIAN_POINT('Ctrl Pts',(41.2881836897428,265.,26.3179317509912)) ;
#101448 = CARTESIAN_POINT('Ctrl Pts',(41.3403904534507,265.,26.2778596828438)) ;
#101449 = CARTESIAN_POINT('Ctrl Pts',(41.345987616831,265.,26.2735634978962)) ;
#101450 = CARTESIAN_POINT('Ctrl Pts',(41.3515545184604,265.,26.2692299705254)) ;
#101451 = CARTESIAN_POINT('Ctrl Pts',(41.3570907214659,265.,26.2648591961635)) ;
#101452 = CARTESIAN_POINT('Ctrl Pts',(41.4074661306217,265.,26.2250883375815)) ;
#101453 = CARTESIAN_POINT('Ctrl Pts',(41.455301981662,265.,26.1822376146413)) ;
#101454 = CARTESIAN_POINT('Ctrl Pts',(41.5005335798205,265.,26.136649754872)) ;
#101455 = CARTESIAN_POINT('Ctrl Pts',(41.5445252571308,265.,26.0923115820485)) ;
#101456 = CARTESIAN_POINT('Ctrl Pts',(41.5860537828374,265.,26.0453833811781)) ;
#101457 = CARTESIAN_POINT('Ctrl Pts',(41.6250320641521,265.,25.9961420649553)) ;
#101458 = CARTESIAN_POINT('Ctrl Pts',(41.6367111946857,265.,25.9813878033404)) ;
#101459 = CARTESIAN_POINT('Ctrl Pts',(41.6481611587152,265.,25.9664256536038)) ;
#101460 = CARTESIAN_POINT('Ctrl Pts',(41.6593790545329,265.,25.9512625482557)) ;
#101461 = CARTESIAN_POINT('Ctrl Pts',(41.6666618959751,265.,25.9414184122595)) ;
#101462 = CARTESIAN_POINT('Ctrl Pts',(41.6738419690629,265.,25.9314961857445)) ;
#101463 = CARTESIAN_POINT('Ctrl Pts',(41.6809150430192,265.,25.9215036288907)) ;
#101464 = CARTESIAN_POINT('Ctrl Pts',(41.7192968173398,265.,25.8672793885651)) ;
#101465 = CARTESIAN_POINT('Ctrl Pts',(41.754566870104,265.,25.8109384347298)) ;
#101466 = CARTESIAN_POINT('Ctrl Pts',(41.7866620719983,265.,25.7528431024233)) ;
#101467 = CARTESIAN_POINT('Ctrl Pts',(41.8200023630589,265.,25.6924940416903)) ;
#101468 = CARTESIAN_POINT('Ctrl Pts',(41.8499174491227,265.,25.6302511300383)) ;
#101469 = CARTESIAN_POINT('Ctrl Pts',(41.8762982392818,265.,25.5664770087076)) ;
#101470 = CARTESIAN_POINT('Ctrl Pts',(41.902679029441,265.,25.5027028873769)) ;
#101471 = CARTESIAN_POINT('Ctrl Pts',(41.9255260936111,265.,25.437396500668)) ;
#101472 = CARTESIAN_POINT('Ctrl Pts',(41.9446830446594,265.,25.3708916870739)) ;
#101473 = CARTESIAN_POINT('Ctrl Pts',(41.9479520979212,265.,25.3595429198689)) ;
#101474 = CARTESIAN_POINT('Ctrl Pts',(41.951113571739,265.,25.3481592086006)) ;
#101475 = CARTESIAN_POINT('Ctrl Pts',(41.9541665323496,265.,25.336742163306)) ;
#101476 = CARTESIAN_POINT('Ctrl Pts',(41.9572422469794,265.,25.3252400256368)) ;
#101477 = CARTESIAN_POINT('Ctrl Pts',(41.9602053850662,265.,25.3137130896354)) ;
#101478 = CARTESIAN_POINT('Ctrl Pts',(41.9630546829663,265.,25.302166601324)) ;
#101479 = CARTESIAN_POINT('Ctrl Pts',(41.9797320778241,265.,25.234583164443)) ;
#101480 = CARTESIAN_POINT('Ctrl Pts',(41.9925227683547,265.,25.1662952212329)) ;
#101481 = CARTESIAN_POINT('Ctrl Pts',(42.0013291177796,265.,25.0976636106023)) ;
#101482 = CARTESIAN_POINT('Ctrl Pts',(42.0100463535875,265.,25.0297265001288)) ;
#101483 = CARTESIAN_POINT('Ctrl Pts',(42.0148598907095,265.,24.9614516185098)) ;
#101484 = CARTESIAN_POINT('Ctrl Pts',(42.0156297848673,265.,24.8931674279836)) ;
#101485 = CARTESIAN_POINT('Ctrl Pts',(42.0161777252074,265.,24.8445689781833)) ;
#101486 = CARTESIAN_POINT('Ctrl Pts',(42.0146765242096,265.,24.7959653337813)) ;
#101487 = CARTESIAN_POINT('Ctrl Pts',(42.0110597486091,265.,24.7474724446513)) ;
#101488 = CARTESIAN_POINT('Ctrl Pts',(42.0088703040113,265.,24.7181168788469)) ;
#101489 = CARTESIAN_POINT('Ctrl Pts',(42.0059053067813,265.,24.6888018815549)) ;
#101490 = CARTESIAN_POINT('Ctrl Pts',(42.0021799342865,265.,24.6595474945815)) ;
#101491 = CARTESIAN_POINT('Ctrl Pts',(42.000315561177,265.,24.6449070546031)) ;
#101492 = CARTESIAN_POINT('Ctrl Pts',(41.9982600471454,265.,24.6302782900132)) ;
#101493 = CARTESIAN_POINT('Ctrl Pts',(41.9960195175212,265.,24.6156897113619)) ;
#101494 = CARTESIAN_POINT('Ctrl Pts',(41.9858207846444,265.,24.5492835299357)) ;
#101495 = CARTESIAN_POINT('Ctrl Pts',(41.9717814071419,265.,24.4836067190368)) ;
#101496 = CARTESIAN_POINT('Ctrl Pts',(41.954161865892,265.,24.4188935223847)) ;
#101497 = CARTESIAN_POINT('Ctrl Pts',(41.9358505721337,265.,24.3516396514054)) ;
#101498 = CARTESIAN_POINT('Ctrl Pts',(41.9136724116091,265.,24.2854257589243)) ;
#101499 = CARTESIAN_POINT('Ctrl Pts',(41.8878637011264,265.,24.2205124747507)) ;
#101500 = CARTESIAN_POINT('Ctrl Pts',(41.8679078478126,265.,24.1703201190361)) ;
#101501 = CARTESIAN_POINT('Ctrl Pts',(41.8457801865645,265.,24.1209051901021)) ;
#101502 = CARTESIAN_POINT('Ctrl Pts',(41.8215690313579,265.,24.0723920420978)) ;
#101503 = CARTESIAN_POINT('Ctrl Pts',(41.8084721454918,265.,24.0461491322906)) ;
#101504 = CARTESIAN_POINT('Ctrl Pts',(41.7947652847443,265.,24.0201701869716)) ;
#101505 = CARTESIAN_POINT('Ctrl Pts',(41.7804604108832,265.,23.9944757207669)) ;
#101506 = CARTESIAN_POINT('Ctrl Pts',(41.7739393210212,265.,23.9827625155542)) ;
#101507 = CARTESIAN_POINT('Ctrl Pts',(41.7672931345761,265.,23.971107065469)) ;
#101508 = CARTESIAN_POINT('Ctrl Pts',(41.760525403896,265.,23.9595156589188)) ;
#101509 = CARTESIAN_POINT('Ctrl Pts',(41.7240227911903,265.,23.8969959393823)) ;
#101510 = CARTESIAN_POINT('Ctrl Pts',(41.6841159271636,265.,23.8365546621805)) ;
#101511 = CARTESIAN_POINT('Ctrl Pts',(41.6410467668449,265.,23.778471424062)) ;
#101512 = CARTESIAN_POINT('Ctrl Pts',(41.6017019158626,265.,23.7254108040865)) ;
#101513 = CARTESIAN_POINT('Ctrl Pts',(41.5597171036843,265.,23.6743175785997)) ;
#101514 = CARTESIAN_POINT('Ctrl Pts',(41.5152413929121,265.,23.6254187090586)) ;
#101515 = CARTESIAN_POINT('Ctrl Pts',(41.5020529827085,265.,23.6109186968318)) ;
#101516 = CARTESIAN_POINT('Ctrl Pts',(41.4886453392958,265.,23.5966117579114)) ;
#101517 = CARTESIAN_POINT('Ctrl Pts',(41.4750218437445,265.,23.582504157239)) ;
#101518 = CARTESIAN_POINT('Ctrl Pts',(41.4619489946405,265.,23.5689667700012)) ;
#101519 = CARTESIAN_POINT('Ctrl Pts',(41.44867445627,265.,23.555610276238)) ;
#101520 = CARTESIAN_POINT('Ctrl Pts',(41.4352209361124,265.,23.5424592086853)) ;
#101521 = CARTESIAN_POINT('Ctrl Pts',(41.382909570539,265.,23.4913238705454)) ;
#101522 = CARTESIAN_POINT('Ctrl Pts',(41.3278436810974,265.,23.4432360534943)) ;
#101523 = CARTESIAN_POINT('Ctrl Pts',(41.2702341795315,265.,23.3984890066187)) ;
#101524 = CARTESIAN_POINT('Ctrl Pts',(41.2131253011062,265.,23.3541308089176)) ;
#101525 = CARTESIAN_POINT('Ctrl Pts',(41.1535162684096,265.,23.3130547011252)) ;
#101526 = CARTESIAN_POINT('Ctrl Pts',(41.09157380261,265.,23.275578834956)) ;
#101527 = CARTESIAN_POINT('Ctrl Pts',(41.0784526521616,265.,23.2676403960862)) ;
#101528 = CARTESIAN_POINT('Ctrl Pts',(41.0652266755638,265.,23.2598636479025)) ;
#101529 = CARTESIAN_POINT('Ctrl Pts',(41.0518972680585,265.,23.2522518613707)) ;
#101530 = CARTESIAN_POINT('Ctrl Pts',(41.1750318437943,265.000571825747,26.3866620466095)) ;
#101531 = CARTESIAN_POINT('Ctrl Pts',(41.1691390078094,265.000381217165,26.390870299183)) ;
#101532 = CARTESIAN_POINT('Ctrl Pts',(41.1632189271215,265.000190608582,26.3950404008641)) ;
#101533 = CARTESIAN_POINT('Ctrl Pts',(41.1572720979745,265.,26.3991720020989)) ;
#101534 = CARTESIAN_POINT('Ctrl Pts',(39.0589035087791,265.166342823321,26.6220511683743)) ;
#101535 = CARTESIAN_POINT('Ctrl Pts',(38.5402676181004,265.140560382316,26.2523570027814)) ;
#101536 = CARTESIAN_POINT('Ctrl Pts',(37.8983515099597,265.089004395602,24.975331106744)) ;
#101537 = CARTESIAN_POINT('Ctrl Pts',(38.9395788746228,265.011674863182,23.091694078747)) ;
#101538 = CARTESIAN_POINT('Ctrl Pts',(41.0824868151442,264.934354226059,22.8934551200483)) ;
#101539 = CARTESIAN_POINT('Ctrl Pts',(42.4548443959838,264.857033588937,24.5494931875868)) ;
#101540 = CARTESIAN_POINT('Ctrl Pts',(41.8612323265555,264.779712951815,26.6175741202223)) ;
#101541 = CARTESIAN_POINT('Ctrl Pts',(39.8186381174926,264.702392314693,27.2932628837251)) ;
#101542 = CARTESIAN_POINT('Ctrl Pts',(38.108734046545,264.625071677571,25.9876964426934)) ;
#101543 = CARTESIAN_POINT('Ctrl Pts',(38.2225940897709,264.547751040449,23.8392868516985)) ;
#101544 = CARTESIAN_POINT('Ctrl Pts',(40.060986256048,264.470430403326,22.7217642917497)) ;
#101545 = CARTESIAN_POINT('Ctrl Pts',(42.0206037771449,264.393109766204,23.609689963601)) ;
#101546 = CARTESIAN_POINT('Ctrl Pts',(42.3924631422109,264.315789129082,25.7287150115834)) ;
#101547 = CARTESIAN_POINT('Ctrl Pts',(40.8522564129019,264.23846849196,27.2308131254801)) ;
#101548 = CARTESIAN_POINT('Ctrl Pts',(38.7432128167474,264.161147854838,26.805996668361)) ;
#101549 = CARTESIAN_POINT('Ctrl Pts',(37.9046440334904,264.083827217716,24.8247497563215)) ;
#101550 = CARTESIAN_POINT('Ctrl Pts',(39.0678733499127,264.006506580593,23.0149336087157)) ;
#101551 = CARTESIAN_POINT('Ctrl Pts',(41.2184384524299,263.929185943471,22.9549031784783)) ;
#101552 = CARTESIAN_POINT('Ctrl Pts',(42.4808166842117,263.851865306349,24.6970101535819)) ;
#101553 = CARTESIAN_POINT('Ctrl Pts',(41.7540746063891,263.774544669227,26.7219527438018)) ;
#101554 = CARTESIAN_POINT('Ctrl Pts',(39.6720174113598,263.697224032105,27.2637559039529)) ;
#101555 = CARTESIAN_POINT('Ctrl Pts',(38.0504063428213,263.619903394982,25.849924240912)) ;
#101556 = CARTESIAN_POINT('Ctrl Pts',(38.3034978579432,263.54258275786,23.7134382088736)) ;
#101557 = CARTESIAN_POINT('Ctrl Pts',(40.2104890723333,263.465262120738,22.7176168533932)) ;
#101558 = CARTESIAN_POINT('Ctrl Pts',(42.1084536899185,263.387941483616,23.7307687267153)) ;
#101559 = CARTESIAN_POINT('Ctrl Pts',(42.3417867596045,263.310620846494,25.8696679088864)) ;
#101560 = CARTESIAN_POINT('Ctrl Pts',(40.7078363774025,263.233300209372,27.2682506055213)) ;
#101561 = CARTESIAN_POINT('Ctrl Pts',(38.6298380139055,263.155979572249,26.7085400306708)) ;
#101562 = CARTESIAN_POINT('Ctrl Pts',(37.9241276393564,263.078658935127,24.67552500292)) ;
#101563 = CARTESIAN_POINT('Ctrl Pts',(38.7734548453959,263.027111843712,23.5264015487631)) ;
#101564 = CARTESIAN_POINT('Ctrl Pts',(39.3470970288687,263.001338298005,23.2501633963894)) ;
#101565 = CARTESIAN_POINT('Ctrl Pts',(39.1152036213646,265.110345202765,26.543073337534)) ;
#101566 = CARTESIAN_POINT('Ctrl Pts',(38.622156503643,265.084562761759,26.1916193674943)) ;
#101567 = CARTESIAN_POINT('Ctrl Pts',(38.0119116427954,265.033006775045,24.9776001516761)) ;
#101568 = CARTESIAN_POINT('Ctrl Pts',(39.0017662985697,264.955677242625,23.1868991528075)) ;
#101569 = CARTESIAN_POINT('Ctrl Pts',(41.0389461440178,264.878356605503,22.9984410284024)) ;
#101570 = CARTESIAN_POINT('Ctrl Pts',(42.3435935120022,264.801035968381,24.5727724827267)) ;
#101571 = CARTESIAN_POINT('Ctrl Pts',(41.7792694358313,264.723715331259,26.5388171807061)) ;
#101572 = CARTESIAN_POINT('Ctrl Pts',(39.8374539819582,264.646394694136,27.1811684011086)) ;
#101573 = CARTESIAN_POINT('Ctrl Pts',(38.2119141978569,264.569074057014,25.9400167910603)) ;
#101574 = CARTESIAN_POINT('Ctrl Pts',(38.3201565450318,264.491753419892,23.8976067389154)) ;
#101575 = CARTESIAN_POINT('Ctrl Pts',(40.0678450006814,264.41443278277,22.8352211865956)) ;
#101576 = CARTESIAN_POINT('Ctrl Pts',(41.9307777208776,264.337112145648,23.6793378417008)) ;
#101577 = CARTESIAN_POINT('Ctrl Pts',(42.284290062462,264.259791508526,25.6938131432853)) ;
#101578 = CARTESIAN_POINT('Ctrl Pts',(40.8200749893644,264.182470871404,27.1217998270116)) ;
#101579 = CARTESIAN_POINT('Ctrl Pts',(38.8150886686681,264.105150234281,26.717943222585)) ;
#101580 = CARTESIAN_POINT('Ctrl Pts',(38.0178937019737,264.027829597159,24.8344482754894)) ;
#101581 = CARTESIAN_POINT('Ctrl Pts',(39.1237309030217,263.950508960037,23.1139259375247)) ;
#101582 = CARTESIAN_POINT('Ctrl Pts',(41.1681901167507,263.873188322915,23.0568573251589)) ;
#101583 = CARTESIAN_POINT('Ctrl Pts',(42.3682843636796,263.795867685793,24.7130111669482)) ;
#101584 = CARTESIAN_POINT('Ctrl Pts',(41.6773987284251,263.71854704867,26.6380459082828)) ;
#101585 = CARTESIAN_POINT('Ctrl Pts',(39.6980673373848,263.641226411548,27.1531172546474)) ;
#101586 = CARTESIAN_POINT('Ctrl Pts',(38.1564643018487,263.563905774426,25.8090420779498)) ;
#101587 = CARTESIAN_POINT('Ctrl Pts',(38.3970686338924,263.486585137304,23.7779672929588)) ;
#101588 = CARTESIAN_POINT('Ctrl Pts',(40.2099715561041,263.409264500182,22.8312783770749)) ;
#101589 = CARTESIAN_POINT('Ctrl Pts',(42.0142932412332,263.33194386306,23.7944427471727)) ;
#101590 = CARTESIAN_POINT('Ctrl Pts',(42.236113982037,263.254623225937,25.8278116208275)) ;
#101591 = CARTESIAN_POINT('Ctrl Pts',(40.6827804373985,263.177302588815,27.1573901938967)) ;
#101592 = CARTESIAN_POINT('Ctrl Pts',(38.707307620792,263.099981951693,26.6252949597485)) ;
#101593 = CARTESIAN_POINT('Ctrl Pts',(38.0364160138455,263.022661314571,24.6925860637149)) ;
#101594 = CARTESIAN_POINT('Ctrl Pts',(38.843838597717,262.971114223156,23.600158761322)) ;
#101595 = CARTESIAN_POINT('Ctrl Pts',(39.3891780743093,262.945340677449,23.3375498148907)) ;
#101596 = CARTESIAN_POINT('Ctrl Pts',(39.1715037339501,265.054347582208,26.4640955066937)) ;
#101597 = CARTESIAN_POINT('Ctrl Pts',(38.7040453891857,265.028565141203,26.1308817322073)) ;
#101598 = CARTESIAN_POINT('Ctrl Pts',(38.1254717756312,264.977009154489,24.9798691966081)) ;
#101599 = CARTESIAN_POINT('Ctrl Pts',(39.0639537225165,264.899679622069,23.282104226868)) ;
#101600 = CARTESIAN_POINT('Ctrl Pts',(40.9954054728912,264.822358984947,23.1034269367565)) ;
#101601 = CARTESIAN_POINT('Ctrl Pts',(42.2323426280205,264.745038347824,24.5960517778666)) ;
#101602 = CARTESIAN_POINT('Ctrl Pts',(41.6973065451071,264.667717710702,26.4600602411901)) ;
#101603 = CARTESIAN_POINT('Ctrl Pts',(39.8562698464239,264.59039707358,27.0690739184919)) ;
#101604 = CARTESIAN_POINT('Ctrl Pts',(38.3150943491689,264.513076436458,25.8923371394272)) ;
#101605 = CARTESIAN_POINT('Ctrl Pts',(38.4177190002927,264.435755799336,23.9559266261323)) ;
#101606 = CARTESIAN_POINT('Ctrl Pts',(40.0747037453149,264.358435162214,22.9486780814416)) ;
#101607 = CARTESIAN_POINT('Ctrl Pts',(41.8409516646104,264.281114525091,23.7489857198008)) ;
#101608 = CARTESIAN_POINT('Ctrl Pts',(42.1761169827131,264.203793887969,25.6589112749871)) ;
#101609 = CARTESIAN_POINT('Ctrl Pts',(40.7878935658271,264.126473250847,27.0127865285429)) ;
#101610 = CARTESIAN_POINT('Ctrl Pts',(38.8869645205888,264.049152613725,26.6298897768089)) ;
#101611 = CARTESIAN_POINT('Ctrl Pts',(38.131143370457,263.971831976603,24.8441467946573)) ;
#101612 = CARTESIAN_POINT('Ctrl Pts',(39.1795884561308,263.894511339481,23.2129182663338)) ;
#101613 = CARTESIAN_POINT('Ctrl Pts',(41.1179417810716,263.817190702358,23.1588114718395)) ;
#101614 = CARTESIAN_POINT('Ctrl Pts',(42.2557520431477,263.739870065236,24.7290121803146)) ;
#101615 = CARTESIAN_POINT('Ctrl Pts',(41.6007228504612,263.662549428114,26.5541390727638)) ;
#101616 = CARTESIAN_POINT('Ctrl Pts',(39.7241172634097,263.585228790992,27.042478605342)) ;
#101617 = CARTESIAN_POINT('Ctrl Pts',(38.2625222608762,263.50790815387,25.7681599149875)) ;
#101618 = CARTESIAN_POINT('Ctrl Pts',(38.4906394098416,263.430587516748,23.842496377044)) ;
#101619 = CARTESIAN_POINT('Ctrl Pts',(40.209454039875,263.353266879625,22.9449399007565)) ;
#101620 = CARTESIAN_POINT('Ctrl Pts',(41.9201327925478,263.275946242503,23.8581167676299)) ;
#101621 = CARTESIAN_POINT('Ctrl Pts',(42.1304412044695,263.198625605381,25.7859553327686)) ;
#101622 = CARTESIAN_POINT('Ctrl Pts',(40.6577244973945,263.121304968259,27.046529782272)) ;
#101623 = CARTESIAN_POINT('Ctrl Pts',(38.7847772276786,263.043984331137,26.5420498888262)) ;
#101624 = CARTESIAN_POINT('Ctrl Pts',(38.1487043883347,262.966663694015,24.7096471245099)) ;
#101625 = CARTESIAN_POINT('Ctrl Pts',(38.9142223500379,262.9151166026,23.673915973881)) ;
#101626 = CARTESIAN_POINT('Ctrl Pts',(39.4312591197499,262.889343056892,23.424936233392)) ;
#101627 = CARTESIAN_POINT('Ctrl Pts',(39.2278038465356,264.998349961652,26.3851176758534)) ;
#101628 = CARTESIAN_POINT('Ctrl Pts',(38.7859342747284,264.972567520647,26.0701440969204)) ;
#101629 = CARTESIAN_POINT('Ctrl Pts',(38.239031908467,264.921011533933,24.9821382415402)) ;
#101630 = CARTESIAN_POINT('Ctrl Pts',(39.1261411464635,264.843682001513,23.3773093009285)) ;
#101631 = CARTESIAN_POINT('Ctrl Pts',(40.9518648017648,264.76636136439,23.2084128451104)) ;
#101632 = CARTESIAN_POINT('Ctrl Pts',(42.1210917440389,264.689040727268,24.6193310730064)) ;
#101633 = CARTESIAN_POINT('Ctrl Pts',(41.6153436543828,264.611720090146,26.3813033016739)) ;
#101634 = CARTESIAN_POINT('Ctrl Pts',(39.8750857108895,264.534399453024,26.9569794358752)) ;
#101635 = CARTESIAN_POINT('Ctrl Pts',(38.4182745004808,264.457078815902,25.8446574877941)) ;
#101636 = CARTESIAN_POINT('Ctrl Pts',(38.5152814555536,264.379758178779,24.0142465133491)) ;
#101637 = CARTESIAN_POINT('Ctrl Pts',(40.0815624899484,264.302437541657,23.0621349762875)) ;
#101638 = CARTESIAN_POINT('Ctrl Pts',(41.751125608343,264.225116904535,23.8186335979007)) ;
#101639 = CARTESIAN_POINT('Ctrl Pts',(42.0679439029642,264.147796267413,25.6240094066889)) ;
#101640 = CARTESIAN_POINT('Ctrl Pts',(40.7557121422897,264.070475630291,26.9037732300743)) ;
#101641 = CARTESIAN_POINT('Ctrl Pts',(38.9588403725095,263.993154993169,26.5418363310329)) ;
#101642 = CARTESIAN_POINT('Ctrl Pts',(38.2443930389404,263.915834356047,24.8538453138252)) ;
#101643 = CARTESIAN_POINT('Ctrl Pts',(39.2354460092399,263.838513718924,23.3119105951427)) ;
#101644 = CARTESIAN_POINT('Ctrl Pts',(41.0676934453923,263.761193081802,23.2607656185202)) ;
#101645 = CARTESIAN_POINT('Ctrl Pts',(42.1432197226157,263.68387244468,24.745013193681)) ;
#101646 = CARTESIAN_POINT('Ctrl Pts',(41.5240469724972,263.606551807558,26.4702322372449)) ;
#101647 = CARTESIAN_POINT('Ctrl Pts',(39.7501671894346,263.529231170436,26.9318399560365)) ;
#101648 = CARTESIAN_POINT('Ctrl Pts',(38.3685802199036,263.451910533313,25.7272777520254)) ;
#101649 = CARTESIAN_POINT('Ctrl Pts',(38.5842101857908,263.374589896191,23.9070254611293)) ;
#101650 = CARTESIAN_POINT('Ctrl Pts',(40.2089365236457,263.297269259069,23.0586014244381)) ;
#101651 = CARTESIAN_POINT('Ctrl Pts',(41.8259723438625,263.219948621947,23.9217907880872)) ;
#101652 = CARTESIAN_POINT('Ctrl Pts',(42.024768426902,263.142627984825,25.7440990447097)) ;
#101653 = CARTESIAN_POINT('Ctrl Pts',(40.6326685573906,263.065307347703,26.9356693706473)) ;
#101654 = CARTESIAN_POINT('Ctrl Pts',(38.8622468345652,262.98798671058,26.4588048179041)) ;
#101655 = CARTESIAN_POINT('Ctrl Pts',(38.2609927628238,262.910666073458,24.7267081853047)) ;
#101656 = CARTESIAN_POINT('Ctrl Pts',(38.984606102359,262.859118982043,23.7476731864398)) ;
#101657 = CARTESIAN_POINT('Ctrl Pts',(39.4733401651905,262.833345436336,23.5123226518935)) ;
#101658 = CARTESIAN_POINT('Ctrl Pts',(39.3461468006825,265.,23.2506310193419)) ;
#101659 = CARTESIAN_POINT('Ctrl Pts',(39.2836598899885,265.,23.2857349597673)) ;
#101660 = CARTESIAN_POINT('Ctrl Pts',(39.2234111410066,265.,23.3242492614719)) ;
#101661 = CARTESIAN_POINT('Ctrl Pts',(39.1657274309582,265.,23.3661502764215)) ;
#101662 = CARTESIAN_POINT('Ctrl Pts',(39.1551609910745,265.,23.3738256592144)) ;
#101663 = CARTESIAN_POINT('Ctrl Pts',(39.1446806995909,265.,23.3816147975325)) ;
#101664 = CARTESIAN_POINT('Ctrl Pts',(39.1342886811881,265.,23.3895176998347)) ;
#101665 = CARTESIAN_POINT('Ctrl Pts',(39.0771212535977,265.,23.4329922759572)) ;
#101666 = CARTESIAN_POINT('Ctrl Pts',(39.0226219173678,265.,23.4799068195409)) ;
#101667 = CARTESIAN_POINT('Ctrl Pts',(38.9709292782328,265.,23.5299202960438)) ;
#101668 = CARTESIAN_POINT('Ctrl Pts',(38.9227381202054,265.,23.576546032125)) ;
#101669 = CARTESIAN_POINT('Ctrl Pts',(38.8769864064487,265.,23.6258661246551)) ;
#101670 = CARTESIAN_POINT('Ctrl Pts',(38.833820414566,265.,23.677624408559)) ;
#101671 = CARTESIAN_POINT('Ctrl Pts',(38.821574354322,265.,23.6923080758435)) ;
#101672 = CARTESIAN_POINT('Ctrl Pts',(38.8095366203122,265.,23.7071880609811)) ;
#101673 = CARTESIAN_POINT('Ctrl Pts',(38.7977110827752,265.,23.7222586759874)) ;
#101674 = CARTESIAN_POINT('Ctrl Pts',(38.7880459026511,265.,23.7345761041094)) ;
#101675 = CARTESIAN_POINT('Ctrl Pts',(38.7785200200342,265.,23.7470243724434)) ;
#101676 = CARTESIAN_POINT('Ctrl Pts',(38.7691522808314,265.,23.7595775114929)) ;
#101677 = CARTESIAN_POINT('Ctrl Pts',(38.7262247635429,265.,23.8171020733859)) ;
#101678 = CARTESIAN_POINT('Ctrl Pts',(38.6865461566725,265.,23.8769100637447)) ;
#101679 = CARTESIAN_POINT('Ctrl Pts',(38.6502422519169,265.,23.9386580305023)) ;
#101680 = CARTESIAN_POINT('Ctrl Pts',(38.6140626397624,265.,24.000194592579)) ;
#101681 = CARTESIAN_POINT('Ctrl Pts',(38.5812343178059,265.,24.0636589136051)) ;
#101682 = CARTESIAN_POINT('Ctrl Pts',(38.5519287182427,265.,24.1287322580849)) ;
#101683 = CARTESIAN_POINT('Ctrl Pts',(38.5217417171236,265.,24.1957627625593)) ;
#101684 = CARTESIAN_POINT('Ctrl Pts',(38.4952918231741,265.,24.2645016083237)) ;
#101685 = CARTESIAN_POINT('Ctrl Pts',(38.4728246435875,265.,24.3346069226516)) ;
#101686 = CARTESIAN_POINT('Ctrl Pts',(38.468243329867,265.,24.3489021944358)) ;
#101687 = CARTESIAN_POINT('Ctrl Pts',(38.4638278256027,265.,24.363254272894)) ;
#101688 = CARTESIAN_POINT('Ctrl Pts',(38.4595805403143,265.,24.3776602266839)) ;
#101689 = CARTESIAN_POINT('Ctrl Pts',(38.4560842396259,265.,24.3895189888661)) ;
#101690 = CARTESIAN_POINT('Ctrl Pts',(38.4527017324949,265.,24.4014153269738)) ;
#101691 = CARTESIAN_POINT('Ctrl Pts',(38.4494386829816,265.,24.4133310106522)) ;
#101692 = CARTESIAN_POINT('Ctrl Pts',(38.4310468428157,265.,24.4804925259125)) ;
#101693 = CARTESIAN_POINT('Ctrl Pts',(38.4164092350366,265.,24.54838861124)) ;
#101694 = CARTESIAN_POINT('Ctrl Pts',(38.4056782411265,265.,24.6167188869397)) ;
#101695 = CARTESIAN_POINT('Ctrl Pts',(38.3952678533935,265.,24.6830076827303)) ;
#101696 = CARTESIAN_POINT('Ctrl Pts',(38.3885340905771,265.,24.7497059721214)) ;
#101697 = CARTESIAN_POINT('Ctrl Pts',(38.3856640111701,265.,24.8165403736793)) ;
#101698 = CARTESIAN_POINT('Ctrl Pts',(38.3832741020044,265.,24.872193241152)) ;
#101699 = CARTESIAN_POINT('Ctrl Pts',(38.3835639723321,265.,24.927940723159)) ;
#101700 = CARTESIAN_POINT('Ctrl Pts',(38.3866687294949,265.,24.9836192786205)) ;
#101701 = CARTESIAN_POINT('Ctrl Pts',(38.3882598861759,265.,25.0121539758162)) ;
#101702 = CARTESIAN_POINT('Ctrl Pts',(38.3905908183162,265.,25.0406704514666)) ;
#101703 = CARTESIAN_POINT('Ctrl Pts',(38.3936513495387,265.,25.0691458950175)) ;
#101704 = CARTESIAN_POINT('Ctrl Pts',(38.395335821027,265.,25.0848183614257)) ;
#101705 = CARTESIAN_POINT('Ctrl Pts',(38.3972421531076,265.,25.1004833988623)) ;
#101706 = CARTESIAN_POINT('Ctrl Pts',(38.3993642663105,265.,25.1161068307743)) ;
#101707 = CARTESIAN_POINT('Ctrl Pts',(38.4084656882497,265.,25.1831133626456)) ;
#101708 = CARTESIAN_POINT('Ctrl Pts',(38.421539478526,265.,25.2494500685674)) ;
#101709 = CARTESIAN_POINT('Ctrl Pts',(38.4383668000559,265.,25.3148382144289)) ;
#101710 = CARTESIAN_POINT('Ctrl Pts',(38.4553537568912,265.,25.3808466762818)) ;
#101711 = CARTESIAN_POINT('Ctrl Pts',(38.4761663756549,265.,25.4458894365213)) ;
#101712 = CARTESIAN_POINT('Ctrl Pts',(38.5006298528874,265.,25.5096610392952)) ;
#101713 = CARTESIAN_POINT('Ctrl Pts',(38.5178779680934,265.,25.5546235743043)) ;
#101714 = CARTESIAN_POINT('Ctrl Pts',(38.5369420027397,265.,25.598953840897)) ;
#101715 = CARTESIAN_POINT('Ctrl Pts',(38.5577731540934,265.,25.6425354268357)) ;
#101716 = CARTESIAN_POINT('Ctrl Pts',(38.5703022633925,265.,25.6687480179875)) ;
#101717 = CARTESIAN_POINT('Ctrl Pts',(38.5834708216211,265.,25.6946896051629)) ;
#101718 = CARTESIAN_POINT('Ctrl Pts',(38.597269718404,265.,25.7203330944085)) ;
#101719 = CARTESIAN_POINT('Ctrl Pts',(38.6055041589436,265.,25.7356357516239)) ;
#101720 = CARTESIAN_POINT('Ctrl Pts',(38.6139658244209,265.,25.7508366888722)) ;
#101721 = CARTESIAN_POINT('Ctrl Pts',(38.6226370628273,265.,25.7659031711737)) ;
#101722 = CARTESIAN_POINT('Ctrl Pts',(38.6561962222617,265.,25.8242130062832)) ;
#101723 = CARTESIAN_POINT('Ctrl Pts',(38.6929261030111,265.,25.8805809342695)) ;
#101724 = CARTESIAN_POINT('Ctrl Pts',(38.7326680429986,265.,25.9347034985894)) ;
#101725 = CARTESIAN_POINT('Ctrl Pts',(38.7659314020797,265.,25.9800032069564)) ;
#101726 = CARTESIAN_POINT('Ctrl Pts',(38.8013057749095,265.,26.0237296971601)) ;
#101727 = CARTESIAN_POINT('Ctrl Pts',(38.8387166266962,265.,26.0656831084018)) ;
#101728 = CARTESIAN_POINT('Ctrl Pts',(38.8518657159005,265.,26.0804288070559)) ;
#101729 = CARTESIAN_POINT('Ctrl Pts',(38.8652665170064,265.,26.0949552572956)) ;
#101730 = CARTESIAN_POINT('Ctrl Pts',(38.878916191547,265.,26.1092530611772)) ;
#101731 = CARTESIAN_POINT('Ctrl Pts',(38.8880474805062,265.,26.1188179323643)) ;
#101732 = CARTESIAN_POINT('Ctrl Pts',(38.8972834111552,265.,26.1282734040428)) ;
#101733 = CARTESIAN_POINT('Ctrl Pts',(38.9066223963459,265.,26.137616745478)) ;
#101734 = CARTESIAN_POINT('Ctrl Pts',(38.9528504522405,265.,26.1838663648201)) ;
#101735 = CARTESIAN_POINT('Ctrl Pts',(39.0016043595963,265.,26.2273752673832)) ;
#101736 = CARTESIAN_POINT('Ctrl Pts',(39.0527559256757,265.,26.2678349102572)) ;
#101737 = CARTESIAN_POINT('Ctrl Pts',(39.1039074917551,265.,26.3082945531311)) ;
#101738 = CARTESIAN_POINT('Ctrl Pts',(39.1574572962527,265.,26.3457057053902)) ;
#101739 = CARTESIAN_POINT('Ctrl Pts',(39.2133011547203,265.,26.3797087969272)) ;
#101740 = CARTESIAN_POINT('Ctrl Pts',(39.2174083575791,265.,26.3822096555462)) ;
#101741 = CARTESIAN_POINT('Ctrl Pts',(39.2215279781247,265.,26.3846920529582)) ;
#101742 = CARTESIAN_POINT('Ctrl Pts',(39.225659978706,265.,26.3871558334356)) ;
#101743 = CARTESIAN_POINT('Origin',(40.2,265.,25.0213203435596)) ;
#101744 = CARTESIAN_POINT('Origin',(40.2,255.,25.0213203435596)) ;
#101745 = CARTESIAN_POINT('',(0.,0.,0.)) ;
#101746 = CARTESIAN_POINT('Origin',(40.2,252.25,25.0213203435596)) ;
#101747 = CARTESIAN_POINT('',(37.2,252.5,25.0213203435596)) ;
#101748 = CARTESIAN_POINT('Origin',(40.2,252.5,25.0213203435596)) ;
#101749 = CARTESIAN_POINT('',(36.2317541634482,253.25,25.0213203435596)) ;
#101750 = CARTESIAN_POINT('Origin',(36.2317541634482,252.25,25.0213203435596)) ;
#101751 = CARTESIAN_POINT('Origin',(40.2,253.25,25.0213203435596)) ;
#101752 = CARTESIAN_POINT('Origin',(40.2,253.25,25.0213203435596)) ;
#101753 = CARTESIAN_POINT('',(44.6022755871902,253.25,25.0172786696089)) ;
#101754 = CARTESIAN_POINT('Ctrl Pts',(44.6022755871902,253.25,25.0172786696089)) ;
#101755 = CARTESIAN_POINT('Ctrl Pts',(44.6016731513632,253.25,24.3610929985028)) ;
#101756 = CARTESIAN_POINT('Ctrl Pts',(44.299934454168,253.25,23.0448769970944)) ;
#101757 = CARTESIAN_POINT('Ctrl Pts',(43.0334270863444,253.25,21.4586695119602)) ;
#101758 = CARTESIAN_POINT('Ctrl Pts',(41.2054355147352,253.25,20.58342963668)) ;
#101759 = CARTESIAN_POINT('Ctrl Pts',(39.1790659113798,253.25,20.5860610515089)) ;
#101760 = CARTESIAN_POINT('Ctrl Pts',(37.352045429714,253.25,21.4697629418411)) ;
#101761 = CARTESIAN_POINT('Ctrl Pts',(36.093585354216,253.25,23.0571242602466)) ;
#101762 = CARTESIAN_POINT('Ctrl Pts',(35.6505014385247,253.25,25.0155164250954)) ;
#101763 = CARTESIAN_POINT('Ctrl Pts',(36.2385167868871,253.25,27.6706849907353)) ;
#101764 = CARTESIAN_POINT('Ctrl Pts',(38.5052376987099,253.25,29.4709001024427)) ;
#101765 = CARTESIAN_POINT('Ctrl Pts',(41.2187227037567,253.25,29.4547811745837)) ;
#101766 = CARTESIAN_POINT('Ctrl Pts',(43.0385614834865,253.25,28.5801018538648)) ;
#101767 = CARTESIAN_POINT('Ctrl Pts',(44.3064740862875,253.25,26.9912625003605)) ;
#101768 = CARTESIAN_POINT('Ctrl Pts',(44.6028780230171,253.25,25.6734643407148)) ;
#101769 = CARTESIAN_POINT('Ctrl Pts',(44.6022755871902,253.25,25.0172786696089)) ;
#101770 = CARTESIAN_POINT('Origin',(40.2,259.75,25.0213203435596)) ;
#101771 = CARTESIAN_POINT('',(40.2,258.75,29.0213203435596)) ;
#101772 = CARTESIAN_POINT('Origin',(40.2,258.75,25.0213203435596)) ;
#101773 = CARTESIAN_POINT('',(40.2,259.75,28.0213203435596)) ;
#101774 = CARTESIAN_POINT('Origin',(40.2,259.75,29.0213203435596)) ;
#101775 = CARTESIAN_POINT('Origin',(40.2,259.75,25.0213203435596)) ;
#101776 = CARTESIAN_POINT('Origin',(40.2,258.75,25.0213203435596)) ;
#101777 = CARTESIAN_POINT('',(44.6022762317189,258.75,25.0245853614825)) ;
#101778 = CARTESIAN_POINT('Ctrl Pts',(44.6022762317189,258.75,25.0245853614825)) ;
#101779 = CARTESIAN_POINT('Ctrl Pts',(44.6017895611471,258.75,25.6807711286595)) ;
#101780 = CARTESIAN_POINT('Ctrl Pts',(44.3002814452206,258.75,26.9970327213995)) ;
#101781 = CARTESIAN_POINT('Ctrl Pts',(43.0340508036911,258.75,28.5834625307185)) ;
#101782 = CARTESIAN_POINT('Ctrl Pts',(41.2062107944581,258.75,29.4590205229256)) ;
#101783 = CARTESIAN_POINT('Ctrl Pts',(39.179840924666,258.75,29.4567488348315)) ;
#101784 = CARTESIAN_POINT('Ctrl Pts',(37.352661518855,258.75,28.573366641583)) ;
#101785 = CARTESIAN_POINT('Ctrl Pts',(36.0939258948918,258.75,26.9862351082814)) ;
#101786 = CARTESIAN_POINT('Ctrl Pts',(35.6504972551226,258.75,25.0279233442809)) ;
#101787 = CARTESIAN_POINT('Ctrl Pts',(36.2380473385298,258.75,22.3726556510516)) ;
#101788 = CARTESIAN_POINT('Ctrl Pts',(38.5044538726149,258.75,20.5720464136779)) ;
#101789 = CARTESIAN_POINT('Ctrl Pts',(41.2179394265067,258.75,20.5876861131438)) ;
#101790 = CARTESIAN_POINT('Ctrl Pts',(43.0379329486519,258.75,21.4620443915897)) ;
#101791 = CARTESIAN_POINT('Ctrl Pts',(44.3061264144813,258.75,23.0506570013303)) ;
#101792 = CARTESIAN_POINT('Ctrl Pts',(44.6027629022906,258.75,24.3683995943056)) ;
#101793 = CARTESIAN_POINT('Ctrl Pts',(44.6022762317189,258.75,25.0245853614825)) ;
#101794 = CARTESIAN_POINT('Origin',(40.2,259.75,25.0213203435596)) ;
#101795 = CARTESIAN_POINT('',(42.2,259.75,25.0213203435596)) ;
#101796 = CARTESIAN_POINT('Origin',(40.2,259.75,25.0213203435596)) ;
#101797 = CARTESIAN_POINT('Origin',(40.2,252.5,25.0213203435596)) ;
#101798 = CARTESIAN_POINT('',(42.2,252.5,25.0213203435596)) ;
#101799 = CARTESIAN_POINT('Origin',(40.2,252.5,25.0213203435596)) ;
#101800 = CARTESIAN_POINT('Ctrl Pts',(45.000619097497,253.613636363636,25.0169129554328)) ;
#101801 = CARTESIAN_POINT('Ctrl Pts',(45.0012760452229,253.613636363636,25.7324741241569)) ;
#101802 = CARTESIAN_POINT('Ctrl Pts',(44.6780517556355,253.613636363636,27.1695143290567)) ;
#101803 = CARTESIAN_POINT('Ctrl Pts',(43.2954110430288,253.613636363636,28.9021211121218)) ;
#101804 = CARTESIAN_POINT('Ctrl Pts',(41.310902661555,253.613636363636,29.8559465072077)) ;
#101805 = CARTESIAN_POINT('Ctrl Pts',(38.3518857445079,253.613636363636,29.8735239694493)) ;
#101806 = CARTESIAN_POINT('Ctrl Pts',(35.8800587353911,253.613636363636,27.9104149196633)) ;
#101807 = CARTESIAN_POINT('Ctrl Pts',(35.2388363368697,253.613636363636,25.0149912527819)) ;
#101808 = CARTESIAN_POINT('Ctrl Pts',(35.7220130633906,253.613636363636,22.8793923697138)) ;
#101809 = CARTESIAN_POINT('Ctrl Pts',(37.0943459290232,253.613636363636,21.1483973629633)) ;
#101810 = CARTESIAN_POINT('Ctrl Pts',(39.0866858546119,253.613636363636,20.1847329836666)) ;
#101811 = CARTESIAN_POINT('Ctrl Pts',(41.2964131703577,253.613636363636,20.1818634631127)) ;
#101812 = CARTESIAN_POINT('Ctrl Pts',(43.2898120557582,253.613636363636,21.1363001349984)) ;
#101813 = CARTESIAN_POINT('Ctrl Pts',(44.6709203795502,253.613636363636,22.8660369029294)) ;
#101814 = CARTESIAN_POINT('Ctrl Pts',(44.9999621497711,253.613636363636,24.3013517867086)) ;
#101815 = CARTESIAN_POINT('Ctrl Pts',(45.000619097497,253.613636363636,25.0169129554328)) ;
#101816 = CARTESIAN_POINT('Ctrl Pts',(44.9916508494659,253.515394087275,25.0169211890687)) ;
#101817 = CARTESIAN_POINT('Ctrl Pts',(44.9923066581649,253.515394087275,25.7312417059043)) ;
#101818 = CARTESIAN_POINT('Ctrl Pts',(44.669806273871,253.515394087275,27.1656710082603)) ;
#101819 = CARTESIAN_POINT('Ctrl Pts',(43.2898068204824,253.515394087275,28.8951621017486)) ;
#101820 = CARTESIAN_POINT('Ctrl Pts',(41.3087556470725,253.515394087275,29.8473173528403)) ;
#101821 = CARTESIAN_POINT('Ctrl Pts',(38.3550913443632,253.515394087275,29.8648827277838)) ;
#101822 = CARTESIAN_POINT('Ctrl Pts',(35.8876347144536,253.515394087275,27.9052827379527)) ;
#101823 = CARTESIAN_POINT('Ctrl Pts',(35.2476065093219,253.515394087275,25.0150115927248)) ;
#101824 = CARTESIAN_POINT('Ctrl Pts',(35.7298834843815,253.515394087275,22.8831639909817)) ;
#101825 = CARTESIAN_POINT('Ctrl Pts',(37.0998098286885,253.515394087275,21.1552793273844)) ;
#101826 = CARTESIAN_POINT('Ctrl Pts',(39.0885241435459,253.515394087275,20.1932807299511)) ;
#101827 = CARTESIAN_POINT('Ctrl Pts',(41.2942811943996,253.515394087275,20.1904751850317)) ;
#101828 = CARTESIAN_POINT('Ctrl Pts',(43.2840998769856,253.515394087275,21.1431751573701)) ;
#101829 = CARTESIAN_POINT('Ctrl Pts',(44.6626199958403,253.515394087275,22.8698547975249)) ;
#101830 = CARTESIAN_POINT('Ctrl Pts',(44.990995040767,253.515394087275,24.3026006722331)) ;
#101831 = CARTESIAN_POINT('Ctrl Pts',(44.9916508494659,253.515394087275,25.0169211890687)) ;
#101832 = CARTESIAN_POINT('Ctrl Pts',(44.8975094841571,253.326587333482,25.0170076190744)) ;
#101833 = CARTESIAN_POINT('Ctrl Pts',(44.8981522927289,253.326587333482,25.7171681262213)) ;
#101834 = CARTESIAN_POINT('Ctrl Pts',(44.5818309261722,253.326587333482,27.1233188158886)) ;
#101835 = CARTESIAN_POINT('Ctrl Pts',(43.2288679887831,253.326587333482,28.8186722353256)) ;
#101836 = CARTESIAN_POINT('Ctrl Pts',(41.287065783851,253.326587333482,29.7519743071556)) ;
#101837 = CARTESIAN_POINT('Ctrl Pts',(38.3916613445224,253.326587333482,29.7691674220623)) ;
#101838 = CARTESIAN_POINT('Ctrl Pts',(35.9730064201748,253.326587333482,27.848274780733)) ;
#101839 = CARTESIAN_POINT('Ctrl Pts',(35.345557667694,253.326587333482,25.0151243958764)) ;
#101840 = CARTESIAN_POINT('Ctrl Pts',(35.8183555821575,253.326587333482,22.9254729931295)) ;
#101841 = CARTESIAN_POINT('Ctrl Pts',(37.1611613325258,253.326587333482,21.2316974982721)) ;
#101842 = CARTESIAN_POINT('Ctrl Pts',(39.1106773513727,253.326587333482,20.2887752336348)) ;
#101843 = CARTESIAN_POINT('Ctrl Pts',(41.2728914527978,253.326587333482,20.2859481042472)) ;
#101844 = CARTESIAN_POINT('Ctrl Pts',(43.223428131217,253.326587333482,21.2198697969633)) ;
#101845 = CARTESIAN_POINT('Ctrl Pts',(44.5748751166589,253.326587333482,22.9123973805586)) ;
#101846 = CARTESIAN_POINT('Ctrl Pts',(44.8968666755852,253.326587333482,24.3168471119274)) ;
#101847 = CARTESIAN_POINT('Ctrl Pts',(44.8975094841571,253.326587333482,25.0170076190744)) ;
#101848 = CARTESIAN_POINT('Ctrl Pts',(44.7009263155318,253.25,25.0171880996136)) ;
#101849 = CARTESIAN_POINT('Ctrl Pts',(44.7015422706035,253.25,25.6880992141915)) ;
#101850 = CARTESIAN_POINT('Ctrl Pts',(44.3985223913072,253.25,27.0354440223192)) ;
#101851 = CARTESIAN_POINT('Ctrl Pts',(43.1022098056181,253.25,28.6599141245163)) ;
#101852 = CARTESIAN_POINT('Ctrl Pts',(41.2415356604866,253.25,29.5542185254571)) ;
#101853 = CARTESIAN_POINT('Ctrl Pts',(38.4672058727508,253.25,29.5707031873526)) ;
#101854 = CARTESIAN_POINT('Ctrl Pts',(36.1496360084533,253.25,27.7301124807667)) ;
#101855 = CARTESIAN_POINT('Ctrl Pts',(35.5484429988492,253.25,25.0153882218719)) ;
#101856 = CARTESIAN_POINT('Ctrl Pts',(36.0014566262198,253.25,23.0130584206935)) ;
#101857 = CARTESIAN_POINT('Ctrl Pts',(37.2881518479859,253.25,21.3900989657002)) ;
#101858 = CARTESIAN_POINT('Ctrl Pts',(39.1561351002536,253.25,20.4865648490839)) ;
#101859 = CARTESIAN_POINT('Ctrl Pts',(41.2279480953328,253.25,20.4838872476943)) ;
#101860 = CARTESIAN_POINT('Ctrl Pts',(43.0969345312123,253.25,21.3787505013531)) ;
#101861 = CARTESIAN_POINT('Ctrl Pts',(44.391821336157,253.25,23.000541357777)) ;
#101862 = CARTESIAN_POINT('Ctrl Pts',(44.70031036046,253.25,24.3462769850356)) ;
#101863 = CARTESIAN_POINT('Ctrl Pts',(44.7009263155318,253.25,25.0171880996136)) ;
#101864 = CARTESIAN_POINT('Ctrl Pts',(44.6022755871902,253.25,25.0172786696089)) ;
#101865 = CARTESIAN_POINT('Ctrl Pts',(44.6028780230171,253.25,25.6734643407148)) ;
#101866 = CARTESIAN_POINT('Ctrl Pts',(44.3064740862875,253.25,26.9912625003605)) ;
#101867 = CARTESIAN_POINT('Ctrl Pts',(43.0385614834865,253.25,28.5801018538648)) ;
#101868 = CARTESIAN_POINT('Ctrl Pts',(41.2187227037567,253.25,29.4547811745837)) ;
#101869 = CARTESIAN_POINT('Ctrl Pts',(38.5052376987099,253.25,29.4709001024427)) ;
#101870 = CARTESIAN_POINT('Ctrl Pts',(36.2385167868871,253.25,27.6706849907353)) ;
#101871 = CARTESIAN_POINT('Ctrl Pts',(35.6505014385247,253.25,25.0155164250954)) ;
#101872 = CARTESIAN_POINT('Ctrl Pts',(36.093585354216,253.25,23.0571242602466)) ;
#101873 = CARTESIAN_POINT('Ctrl Pts',(37.352045429714,253.25,21.4697629418411)) ;
#101874 = CARTESIAN_POINT('Ctrl Pts',(39.1790659113798,253.25,20.5860610515089)) ;
#101875 = CARTESIAN_POINT('Ctrl Pts',(41.2054355147352,253.25,20.58342963668)) ;
#101876 = CARTESIAN_POINT('Ctrl Pts',(43.0334270863444,253.25,21.4586695119602)) ;
#101877 = CARTESIAN_POINT('Ctrl Pts',(44.299934454168,253.25,23.0448769970944)) ;
#101878 = CARTESIAN_POINT('Ctrl Pts',(44.6016731513632,253.25,24.3610929985028)) ;
#101879 = CARTESIAN_POINT('Ctrl Pts',(44.6022755871902,253.25,25.0172786696089)) ;
#101880 = CARTESIAN_POINT('',(45.000619097497,253.613636363636,25.0169129554328)) ;
#101881 = CARTESIAN_POINT('Ctrl Pts',(44.6022755871902,253.25,25.0172786696089)) ;
#101882 = CARTESIAN_POINT('Ctrl Pts',(44.7009263155318,253.25,25.0171880996136)) ;
#101883 = CARTESIAN_POINT('Ctrl Pts',(44.8975094841571,253.326587333482,25.0170076190744)) ;
#101884 = CARTESIAN_POINT('Ctrl Pts',(44.9916508494659,253.515394087275,25.0169211890687)) ;
#101885 = CARTESIAN_POINT('Ctrl Pts',(45.000619097497,253.613636363636,25.0169129554328)) ;
#101886 = CARTESIAN_POINT('',(40.199018407139,253.613636363636,29.8223164415809)) ;
#101887 = CARTESIAN_POINT('Ctrl Pts',(45.000619097497,253.613636363636,25.0169129554328)) ;
#101888 = CARTESIAN_POINT('Ctrl Pts',(45.0012760452229,253.613636363636,25.7324741241569)) ;
#101889 = CARTESIAN_POINT('Ctrl Pts',(44.6780517556355,253.613636363636,27.1695143290567)) ;
#101890 = CARTESIAN_POINT('Ctrl Pts',(43.2954110430288,253.613636363636,28.9021211121218)) ;
#101891 = CARTESIAN_POINT('Ctrl Pts',(41.6409075118807,253.613636363636,29.6973344249002)) ;
#101892 = CARTESIAN_POINT('Ctrl Pts',(40.5597413925216,253.613636363636,29.8213340913974)) ;
#101893 = CARTESIAN_POINT('Ctrl Pts',(40.199018407139,253.613636363636,29.8223164415809)) ;
#101894 = CARTESIAN_POINT('Ctrl Pts',(40.199018407139,253.613636363636,29.8223164415809)) ;
#101895 = CARTESIAN_POINT('Ctrl Pts',(39.8399201468488,253.613636363636,29.8232943671808)) ;
#101896 = CARTESIAN_POINT('Ctrl Pts',(38.0422099661677,253.613636363636,29.6275814659016)) ;
#101897 = CARTESIAN_POINT('Ctrl Pts',(35.8800587353911,253.613636363636,27.9104149196633)) ;
#101898 = CARTESIAN_POINT('Ctrl Pts',(35.2388363368697,253.613636363636,25.0149912527819)) ;
#101899 = CARTESIAN_POINT('Ctrl Pts',(35.7220130633906,253.613636363636,22.8793923697138)) ;
#101900 = CARTESIAN_POINT('Ctrl Pts',(37.0943459290232,253.613636363636,21.1483973629633)) ;
#101901 = CARTESIAN_POINT('Ctrl Pts',(39.0866858546119,253.613636363636,20.1847329836666)) ;
#101902 = CARTESIAN_POINT('Ctrl Pts',(41.2964131703577,253.613636363636,20.1818634631127)) ;
#101903 = CARTESIAN_POINT('Ctrl Pts',(43.2898120557582,253.613636363636,21.1363001349984)) ;
#101904 = CARTESIAN_POINT('Ctrl Pts',(44.6709203795502,253.613636363636,22.8660369029294)) ;
#101905 = CARTESIAN_POINT('Ctrl Pts',(44.9999621497711,253.613636363636,24.3013517867086)) ;
#101906 = CARTESIAN_POINT('Ctrl Pts',(45.000619097497,253.613636363636,25.0169129554328)) ;
#101907 = CARTESIAN_POINT('Ctrl Pts',(45.0006198003464,258.386363636364,25.0248807993021)) ;
#101908 = CARTESIAN_POINT('Ctrl Pts',(45.0011505077032,258.386363636364,24.309319525814)) ;
#101909 = CARTESIAN_POINT('Ctrl Pts',(44.6776726244613,258.386363636364,22.8723399155802)) ;
#101910 = CARTESIAN_POINT('Ctrl Pts',(43.2947256347052,258.386363636364,21.1399803933739)) ;
#101911 = CARTESIAN_POINT('Ctrl Pts',(41.3100485088219,258.386363636364,20.1865050903338)) ;
#101912 = CARTESIAN_POINT('Ctrl Pts',(38.351030993267,258.386363636364,20.1694502198588)) ;
#101913 = CARTESIAN_POINT('Ctrl Pts',(35.8795468086148,258.386363636364,22.1329890580946)) ;
#101914 = CARTESIAN_POINT('Ctrl Pts',(35.2388317749291,258.386363636364,25.0285208222065)) ;
#101915 = CARTESIAN_POINT('Ctrl Pts',(35.7223844181683,258.386363636364,27.1640320292898)) ;
#101916 = CARTESIAN_POINT('Ctrl Pts',(37.0950177654945,258.386363636364,28.8947764586432)) ;
#101917 = CARTESIAN_POINT('Ctrl Pts',(39.0875309956096,258.386363636364,29.8580922128038)) ;
#101918 = CARTESIAN_POINT('Ctrl Pts',(41.297258601901,258.386363636364,29.8605694564547)) ;
#101919 = CARTESIAN_POINT('Ctrl Pts',(43.2904922106796,258.386363636364,28.9057858825717)) ;
#101920 = CARTESIAN_POINT('Ctrl Pts',(44.6712987683722,258.386363636364,27.1758066732701)) ;
#101921 = CARTESIAN_POINT('Ctrl Pts',(45.0000890929896,258.386363636364,25.7404420727902)) ;
#101922 = CARTESIAN_POINT('Ctrl Pts',(45.0006198003464,258.386363636364,25.0248807993021)) ;
#101923 = CARTESIAN_POINT('Ctrl Pts',(44.9916515510023,258.484605912725,25.0248741478579)) ;
#101924 = CARTESIAN_POINT('Ctrl Pts',(44.9921813382098,258.484605912725,24.31055352644)) ;
#101925 = CARTESIAN_POINT('Ctrl Pts',(44.6694274518689,258.484605912725,22.876183617039)) ;
#101926 = CARTESIAN_POINT('Ctrl Pts',(43.2891212929352,258.484605912725,21.1469383147985)) ;
#101927 = CARTESIAN_POINT('Ctrl Pts',(41.3079016216169,258.484605912725,20.1951323949763)) ;
#101928 = CARTESIAN_POINT('Ctrl Pts',(38.3542352604705,258.484605912725,20.1780888057549)) ;
#101929 = CARTESIAN_POINT('Ctrl Pts',(35.8871201680428,258.484605912725,22.1381188352666)) ;
#101930 = CARTESIAN_POINT('Ctrl Pts',(35.2475978217452,258.484605912725,25.0284991827555)) ;
#101931 = CARTESIAN_POINT('Ctrl Pts',(35.7302504339899,258.484605912725,27.1602597668809)) ;
#101932 = CARTESIAN_POINT('Ctrl Pts',(37.1004769335098,258.484605912725,28.8878953905237)) ;
#101933 = CARTESIAN_POINT('Ctrl Pts',(39.0893652161804,258.484605912725,29.8495459249166)) ;
#101934 = CARTESIAN_POINT('Ctrl Pts',(41.2951234207584,258.484605912725,29.8519604630792)) ;
#101935 = CARTESIAN_POINT('Ctrl Pts',(43.2847776365318,258.484605912725,28.8989133639222)) ;
#101936 = CARTESIAN_POINT('Ctrl Pts',(44.6629974245713,258.484605912725,27.1719911235959)) ;
#101937 = CARTESIAN_POINT('Ctrl Pts',(44.9911217637948,258.484605912725,25.7391947692758)) ;
#101938 = CARTESIAN_POINT('Ctrl Pts',(44.9916515510023,258.484605912725,25.0248741478579)) ;
#101939 = CARTESIAN_POINT('Ctrl Pts',(44.8975099394367,258.673412411855,25.0248043262399)) ;
#101940 = CARTESIAN_POINT('Ctrl Pts',(44.8980292246472,258.673412411855,24.3246437165838)) ;
#101941 = CARTESIAN_POINT('Ctrl Pts',(44.5814598954824,258.673412411855,22.9185527200586)) ;
#101942 = CARTESIAN_POINT('Ctrl Pts',(43.228197675365,258.673412411855,21.2234416213897)) ;
#101943 = CARTESIAN_POINT('Ctrl Pts',(41.2862303788559,258.673412411855,20.2904821630844)) ;
#101944 = CARTESIAN_POINT('Ctrl Pts',(38.390825913078,258.673412411855,20.2738003530344)) ;
#101945 = CARTESIAN_POINT('Ctrl Pts',(35.9725066923928,258.673412411855,22.1951131679698)) ;
#101946 = CARTESIAN_POINT('Ctrl Pts',(35.3455546200851,258.673412411855,25.0283688520011)) ;
#101947 = CARTESIAN_POINT('Ctrl Pts',(35.8187202161855,258.673412411855,27.1179342822305)) ;
#101948 = CARTESIAN_POINT('Ctrl Pts',(37.1618199075666,258.673412411855,28.8114641917246)) ;
#101949 = CARTESIAN_POINT('Ctrl Pts',(39.1115051232266,258.673412411855,29.7540453502129)) ;
#101950 = CARTESIAN_POINT('Ctrl Pts',(41.2737191756229,258.673412411855,29.7564884307353)) ;
#101951 = CARTESIAN_POINT('Ctrl Pts',(43.2240939182987,258.673412411855,28.822227602684)) ;
#101952 = CARTESIAN_POINT('Ctrl Pts',(44.5752452635221,258.673412411855,27.1294630065087)) ;
#101953 = CARTESIAN_POINT('Ctrl Pts',(44.8969906542263,258.673412411855,25.7249649358961)) ;
#101954 = CARTESIAN_POINT('Ctrl Pts',(44.8975099394367,258.673412411855,25.0248043262399)) ;
#101955 = CARTESIAN_POINT('Ctrl Pts',(44.7009269745037,258.75,25.0246585273691)) ;
#101956 = CARTESIAN_POINT('Ctrl Pts',(44.7014245664355,258.75,24.3537473145643)) ;
#101957 = CARTESIAN_POINT('Ctrl Pts',(44.3981668414899,258.75,23.006459080954)) ;
#101958 = CARTESIAN_POINT('Ctrl Pts',(43.1015668807325,258.75,21.382220583903)) ;
#101959 = CARTESIAN_POINT('Ctrl Pts',(41.24073451057,258.75,20.4882443962037)) ;
#101960 = CARTESIAN_POINT('Ctrl Pts',(38.466403843111,258.75,20.472249738864)) ;
#101961 = CARTESIAN_POINT('Ctrl Pts',(36.1491552604752,258.75,22.3132436329432)) ;
#101962 = CARTESIAN_POINT('Ctrl Pts',(35.5484378202547,258.75,25.0280695257637)) ;
#101963 = CARTESIAN_POINT('Ctrl Pts',(36.0018039888119,258.75,27.0303172322302)) ;
#101964 = CARTESIAN_POINT('Ctrl Pts',(37.2887809850285,258.75,28.6530419860233)) ;
#101965 = CARTESIAN_POINT('Ctrl Pts',(39.1569269380008,258.75,29.5562492220073)) ;
#101966 = CARTESIAN_POINT('Ctrl Pts',(41.2287403938204,258.75,29.5585591526955)) ;
#101967 = CARTESIAN_POINT('Ctrl Pts',(43.0975719802107,258.75,28.663370463087)) ;
#101968 = CARTESIAN_POINT('Ctrl Pts',(44.3921760477315,258.75,27.0413521670251)) ;
#101969 = CARTESIAN_POINT('Ctrl Pts',(44.7004293825719,258.75,25.6955697401738)) ;
#101970 = CARTESIAN_POINT('Ctrl Pts',(44.7009269745037,258.75,25.0246585273691)) ;
#101971 = CARTESIAN_POINT('Ctrl Pts',(44.6022762317189,258.75,25.0245853614825)) ;
#101972 = CARTESIAN_POINT('Ctrl Pts',(44.6027629022906,258.75,24.3683995943056)) ;
#101973 = CARTESIAN_POINT('Ctrl Pts',(44.3061264144813,258.75,23.0506570013303)) ;
#101974 = CARTESIAN_POINT('Ctrl Pts',(43.0379329486519,258.75,21.4620443915897)) ;
#101975 = CARTESIAN_POINT('Ctrl Pts',(41.2179394265067,258.75,20.5876861131438)) ;
#101976 = CARTESIAN_POINT('Ctrl Pts',(38.5044538726149,258.75,20.5720464136779)) ;
#101977 = CARTESIAN_POINT('Ctrl Pts',(36.2380473385298,258.75,22.3726556510516)) ;
#101978 = CARTESIAN_POINT('Ctrl Pts',(35.6504972551226,258.75,25.0279233442809)) ;
#101979 = CARTESIAN_POINT('Ctrl Pts',(36.0939258948918,258.75,26.9862351082814)) ;
#101980 = CARTESIAN_POINT('Ctrl Pts',(37.352661518855,258.75,28.573366641583)) ;
#101981 = CARTESIAN_POINT('Ctrl Pts',(39.179840924666,258.75,29.4567488348315)) ;
#101982 = CARTESIAN_POINT('Ctrl Pts',(41.2062107944581,258.75,29.4590205229256)) ;
#101983 = CARTESIAN_POINT('Ctrl Pts',(43.0340508036911,258.75,28.5834625307185)) ;
#101984 = CARTESIAN_POINT('Ctrl Pts',(44.3002814452206,258.75,26.9970327213995)) ;
#101985 = CARTESIAN_POINT('Ctrl Pts',(44.6017895611471,258.75,25.6807711286595)) ;
#101986 = CARTESIAN_POINT('Ctrl Pts',(44.6022762317189,258.75,25.0245853614825)) ;
#101987 = CARTESIAN_POINT('',(45.0006198003464,258.386363636364,25.0248807993021)) ;
#101988 = CARTESIAN_POINT('Ctrl Pts',(44.6022762317189,258.75,25.0245853614825)) ;
#101989 = CARTESIAN_POINT('Ctrl Pts',(44.7009269745037,258.75,25.0246585273691)) ;
#101990 = CARTESIAN_POINT('Ctrl Pts',(44.8975099394367,258.673412411855,25.0248043262399)) ;
#101991 = CARTESIAN_POINT('Ctrl Pts',(44.9916515510023,258.484605912725,25.0248741478579)) ;
#101992 = CARTESIAN_POINT('Ctrl Pts',(45.0006198003464,258.386363636364,25.0248807993021)) ;
#101993 = CARTESIAN_POINT('',(40.1990240993093,258.386363636364,20.2203337107496)) ;
#101994 = CARTESIAN_POINT('Ctrl Pts',(45.0006198003464,258.386363636364,25.0248807993021)) ;
#101995 = CARTESIAN_POINT('Ctrl Pts',(45.0011505077032,258.386363636364,24.309319525814)) ;
#101996 = CARTESIAN_POINT('Ctrl Pts',(44.6776726244613,258.386363636364,22.8723399155802)) ;
#101997 = CARTESIAN_POINT('Ctrl Pts',(43.2947256347052,258.386363636364,21.1399803933739)) ;
#101998 = CARTESIAN_POINT('Ctrl Pts',(41.6403427347236,258.386363636364,20.3451844961812)) ;
#101999 = CARTESIAN_POINT('Ctrl Pts',(40.5594630598394,258.386363636364,20.2213153661189)) ;
#102000 = CARTESIAN_POINT('Ctrl Pts',(40.1990240993093,258.386363636364,20.2203337107496)) ;
#102001 = CARTESIAN_POINT('Ctrl Pts',(40.1990240993093,258.386363636364,20.2203337107496)) ;
#102002 = CARTESIAN_POINT('Ctrl Pts',(39.8396412077929,258.386363636364,20.2193549315838)) ;
#102003 = CARTESIAN_POINT('Ctrl Pts',(38.0416422229935,258.386363636364,20.4152526693822)) ;
#102004 = CARTESIAN_POINT('Ctrl Pts',(35.8795468086148,258.386363636364,22.1329890580946)) ;
#102005 = CARTESIAN_POINT('Ctrl Pts',(35.2388317749291,258.386363636364,25.0285208222065)) ;
#102006 = CARTESIAN_POINT('Ctrl Pts',(35.7223844181683,258.386363636364,27.1640320292898)) ;
#102007 = CARTESIAN_POINT('Ctrl Pts',(37.0950177654945,258.386363636364,28.8947764586432)) ;
#102008 = CARTESIAN_POINT('Ctrl Pts',(39.0875309956096,258.386363636364,29.8580922128038)) ;
#102009 = CARTESIAN_POINT('Ctrl Pts',(41.297258601901,258.386363636364,29.8605694564547)) ;
#102010 = CARTESIAN_POINT('Ctrl Pts',(43.2904922106796,258.386363636364,28.9057858825717)) ;
#102011 = CARTESIAN_POINT('Ctrl Pts',(44.6712987683722,258.386363636364,27.1758066732701)) ;
#102012 = CARTESIAN_POINT('Ctrl Pts',(45.0000890929896,258.386363636364,25.7404420727902)) ;
#102013 = CARTESIAN_POINT('Ctrl Pts',(45.0006198003464,258.386363636364,25.0248807993021)) ;
#102014 = CARTESIAN_POINT('Origin',(40.2,253.9,25.0213203435596)) ;
#102015 = CARTESIAN_POINT('',(38.3418047738311,253.75,29.6093057948708)) ;
#102016 = CARTESIAN_POINT('',(37.580461549766,253.75,29.2213820464094)) ;
#102017 = CARTESIAN_POINT('Origin',(40.2,253.75,25.0213203435596)) ;
#102018 = CARTESIAN_POINT('',(38.1565530819608,253.9,29.694041680549)) ;
#102019 = CARTESIAN_POINT('Ctrl Pts',(38.3418047738311,253.75,29.6093057948708)) ;
#102020 = CARTESIAN_POINT('Ctrl Pts',(38.3410897979463,253.75,29.6096388244826)) ;
#102021 = CARTESIAN_POINT('Ctrl Pts',(38.3403747898381,253.750003330106,29.6099717982194)) ;
#102022 = CARTESIAN_POINT('Ctrl Pts',(38.3212338170963,253.750181671152,29.6188837045809)) ;
#102023 = CARTESIAN_POINT('Ctrl Pts',(38.3027198224331,253.752566842488,29.6274555764536)) ;
#102024 = CARTESIAN_POINT('Ctrl Pts',(38.2675842178259,253.761740190968,29.6436380121775)) ;
#102025 = CARTESIAN_POINT('Ctrl Pts',(38.2507597781158,253.768377217198,29.6513456347974)) ;
#102026 = CARTESIAN_POINT('Ctrl Pts',(38.2177054917617,253.78721321578,29.6664219076506)) ;
#102027 = CARTESIAN_POINT('Ctrl Pts',(38.2015932119542,253.800023548159,29.6737287158086)) ;
#102028 = CARTESIAN_POINT('Ctrl Pts',(38.1781795794102,253.828041657271,29.6843112161272)) ;
#102029 = CARTESIAN_POINT('Ctrl Pts',(38.1698022074386,253.841958224525,29.6880838741351)) ;
#102030 = CARTESIAN_POINT('Ctrl Pts',(38.1592036720168,253.870954690135,29.6928518010587)) ;
#102031 = CARTESIAN_POINT('Ctrl Pts',(38.1565530819608,253.885320776746,29.694041680549)) ;
#102032 = CARTESIAN_POINT('Ctrl Pts',(38.1565530819608,253.9,29.694041680549)) ;
#102033 = CARTESIAN_POINT('',(37.6207969906631,253.9,29.4210603173112)) ;
#102034 = CARTESIAN_POINT('Origin',(40.2,253.9,25.0213203435596)) ;
#102035 = CARTESIAN_POINT('Ctrl Pts',(37.580461549766,253.75,29.2213820464094)) ;
#102036 = CARTESIAN_POINT('Ctrl Pts',(37.5806123754316,253.75,29.2221562239469)) ;
#102037 = CARTESIAN_POINT('Ctrl Pts',(37.5807632652411,253.750003330105,29.2229303947064)) ;
#102038 = CARTESIAN_POINT('Ctrl Pts',(37.5848041630354,253.750181671152,29.2436540540753)) ;
#102039 = CARTESIAN_POINT('Ctrl Pts',(37.5887516260403,253.752566842488,29.2636706102621)) ;
#102040 = CARTESIAN_POINT('Ctrl Pts',(37.5963119507477,253.761740190968,29.3016077085614)) ;
#102041 = CARTESIAN_POINT('Ctrl Pts',(37.5999655106017,253.768377217198,29.3197493931139)) ;
#102042 = CARTESIAN_POINT('Ctrl Pts',(37.6071973716956,253.78721321578,29.3553524833539)) ;
#102043 = CARTESIAN_POINT('Ctrl Pts',(37.6107566001729,253.800023548159,29.372682425613)) ;
#102044 = CARTESIAN_POINT('Ctrl Pts',(37.6159573654841,253.828041657271,29.3978446898608)) ;
#102045 = CARTESIAN_POINT('Ctrl Pts',(37.6178293167396,253.841958224525,29.406839638893)) ;
#102046 = CARTESIAN_POINT('Ctrl Pts',(37.6202016456472,253.870954690135,29.4182165512944)) ;
#102047 = CARTESIAN_POINT('Ctrl Pts',(37.6207969906631,253.885320776746,29.4210603173112)) ;
#102048 = CARTESIAN_POINT('Ctrl Pts',(37.6207969906631,253.9,29.4210603173112)) ;
#102049 = CARTESIAN_POINT('Origin',(39.0213365437268,253.9,27.5179220536754)) ;
#102050 = CARTESIAN_POINT('',(38.1739035596879,253.75,30.1260525975112)) ;
#102051 = CARTESIAN_POINT('',(39.0213365437268,253.75,27.5179220536754)) ;
#102052 = CARTESIAN_POINT('',(38.0323928885057,253.9,30.0761674639184)) ;
#102053 = CARTESIAN_POINT('Ctrl Pts',(38.1739035596879,253.75,30.1260525975112)) ;
#102054 = CARTESIAN_POINT('Ctrl Pts',(38.172529049521,253.75,30.1255643186931)) ;
#102055 = CARTESIAN_POINT('Ctrl Pts',(38.1711545707753,253.750021261236,30.1250761825186)) ;
#102056 = CARTESIAN_POINT('Ctrl Pts',(38.1697805624966,253.750063777237,30.1245883423369)) ;
#102057 = CARTESIAN_POINT('Ctrl Pts',(38.1521290671495,253.750609968276,30.1183211976405)) ;
#102058 = CARTESIAN_POINT('Ctrl Pts',(38.1347220873535,253.754658837467,30.1121625030257)) ;
#102059 = CARTESIAN_POINT('Ctrl Pts',(38.1184645303643,253.762001431812,30.1064243414529)) ;
#102060 = CARTESIAN_POINT('Ctrl Pts',(38.1015160468841,253.769656077527,30.1004423149597)) ;
#102061 = CARTESIAN_POINT('Ctrl Pts',(38.0861341004722,253.78074710398,30.0950289612179)) ;
#102062 = CARTESIAN_POINT('Ctrl Pts',(38.0731882320494,253.794651469056,30.0904794283364)) ;
#102063 = CARTESIAN_POINT('Ctrl Pts',(38.0602458273977,253.808552113907,30.0859311127188)) ;
#102064 = CARTESIAN_POINT('Ctrl Pts',(38.0499858937768,253.824998688613,30.0823329269323)) ;
#102065 = CARTESIAN_POINT('Ctrl Pts',(38.0429889324131,253.843066458683,30.0798802263626)) ;
#102066 = CARTESIAN_POINT('Ctrl Pts',(38.0359928332805,253.861132002274,30.0774278280375)) ;
#102067 = CARTESIAN_POINT('Ctrl Pts',(38.0323928885057,253.880472526098,30.0761674639184)) ;
#102068 = CARTESIAN_POINT('Ctrl Pts',(38.0323928885057,253.9,30.0761674639184)) ;
#102069 = CARTESIAN_POINT('',(38.8786780662825,253.9,27.4715695045192)) ;
#102070 = CARTESIAN_POINT('Origin',(38.5004065309378,253.9,30.252131183183)) ;
#102071 = CARTESIAN_POINT('',(38.8386601166806,253.75,30.3420450960781)) ;
#102072 = CARTESIAN_POINT('Origin',(38.5004065309378,253.75,30.252131183183)) ;
#102073 = CARTESIAN_POINT('',(38.982466400387,253.9,30.3848650607978)) ;
#102074 = CARTESIAN_POINT('Ctrl Pts',(38.8386601166829,253.75,30.3420450960789)) ;
#102075 = CARTESIAN_POINT('Ctrl Pts',(38.8400591218546,253.75,30.3424579870221)) ;
#102076 = CARTESIAN_POINT('Ctrl Pts',(38.8414580177618,253.750021261236,30.3428709748967)) ;
#102077 = CARTESIAN_POINT('Ctrl Pts',(38.8428563590733,253.750063777237,30.343283925702)) ;
#102078 = CARTESIAN_POINT('Ctrl Pts',(38.8608204540119,253.750609968276,30.3485889877857)) ;
#102079 = CARTESIAN_POINT('Ctrl Pts',(38.8785229863552,253.754658837467,30.3538380651884)) ;
#102080 = CARTESIAN_POINT('Ctrl Pts',(38.8950484329941,253.762001431812,30.3587517471959)) ;
#102081 = CARTESIAN_POINT('Ctrl Pts',(38.9122761911101,253.769656077527,30.3638742547404)) ;
#102082 = CARTESIAN_POINT('Ctrl Pts',(38.927902336659,253.78074710398,30.3685360408181)) ;
#102083 = CARTESIAN_POINT('Ctrl Pts',(38.9410499125525,253.794651469056,30.3724647819375)) ;
#102084 = CARTESIAN_POINT('Ctrl Pts',(38.9541939707066,253.808552113907,30.3763924718906)) ;
#102085 = CARTESIAN_POINT('Ctrl Pts',(38.9646093919075,253.824998688613,30.3795121161123)) ;
#102086 = CARTESIAN_POINT('Ctrl Pts',(38.9717117137828,253.843066458683,30.3816405503697)) ;
#102087 = CARTESIAN_POINT('Ctrl Pts',(38.9788131604437,253.861132002274,30.3837687223415)) ;
#102088 = CARTESIAN_POINT('Ctrl Pts',(38.982466400387,253.880472526098,30.3848650607978)) ;
#102089 = CARTESIAN_POINT('Ctrl Pts',(38.982466400387,253.9,30.3848650607978)) ;
#102090 = CARTESIAN_POINT('Origin',(38.5004065309378,253.9,30.252131183183)) ;
#102091 = CARTESIAN_POINT('Origin',(39.7947637665017,253.9,27.3994606331908)) ;
#102092 = CARTESIAN_POINT('',(39.0065613308239,253.75,29.8252982934377)) ;
#102093 = CARTESIAN_POINT('',(39.7947637665017,253.75,27.3994606331908)) ;
#102094 = CARTESIAN_POINT('',(39.1066265938421,253.9,30.0027392774284)) ;
#102095 = CARTESIAN_POINT('Ctrl Pts',(39.0065613308239,253.75,29.8252982934377)) ;
#102096 = CARTESIAN_POINT('Ctrl Pts',(39.0069440085702,253.75,29.8259879723329)) ;
#102097 = CARTESIAN_POINT('Ctrl Pts',(39.0073267452283,253.750003330105,29.8266776249647)) ;
#102098 = CARTESIAN_POINT('Ctrl Pts',(39.0175738303363,253.750181671152,29.8451382901555)) ;
#102099 = CARTESIAN_POINT('Ctrl Pts',(39.0275135467812,253.752566842487,29.8629553331985)) ;
#102100 = CARTESIAN_POINT('Ctrl Pts',(39.0464270509519,253.761740190968,29.896699388929)) ;
#102101 = CARTESIAN_POINT('Ctrl Pts',(39.0555078816925,253.768377217198,29.9128241441551)) ;
#102102 = CARTESIAN_POINT('Ctrl Pts',(39.0733877502475,253.78721321578,29.9444499271496)) ;
#102103 = CARTESIAN_POINT('Ctrl Pts',(39.0821280243534,253.800023548159,29.9598318195758)) ;
#102104 = CARTESIAN_POINT('Ctrl Pts',(39.0948498133619,253.828041657271,29.9821554300886)) ;
#102105 = CARTESIAN_POINT('Ctrl Pts',(39.0994097369161,253.841958224525,29.9901316702288)) ;
#102106 = CARTESIAN_POINT('Ctrl Pts',(39.1051816150581,253.870954690135,30.0002186669547)) ;
#102107 = CARTESIAN_POINT('Ctrl Pts',(39.1066265938421,253.885320776746,30.0027392774284)) ;
#102108 = CARTESIAN_POINT('Ctrl Pts',(39.1066265938421,253.9,30.0027392774284)) ;
#102109 = CARTESIAN_POINT('',(39.9374222439459,253.9,27.445813182347)) ;
#102110 = CARTESIAN_POINT('Origin',(40.2,253.9,25.0213203435596)) ;
#102111 = CARTESIAN_POINT('',(39.8505167960037,253.75,29.9589677074491)) ;
#102112 = CARTESIAN_POINT('Origin',(40.2,253.75,25.0213203435596)) ;
#102113 = CARTESIAN_POINT('',(39.7005167960037,253.9,30.096802244712)) ;
#102114 = CARTESIAN_POINT('Ctrl Pts',(39.8505167960037,253.75,29.9589677074491)) ;
#102115 = CARTESIAN_POINT('Ctrl Pts',(39.8499397253402,253.75,29.9595053771295)) ;
#102116 = CARTESIAN_POINT('Ctrl Pts',(39.849362606764,253.750003330105,29.9600430036272)) ;
#102117 = CARTESIAN_POINT('Ctrl Pts',(39.8339123904279,253.750181671152,29.9744336161108)) ;
#102118 = CARTESIAN_POINT('Ctrl Pts',(39.8189533892428,253.752566842487,29.9883070896973)) ;
#102119 = CARTESIAN_POINT('Ctrl Pts',(39.7905380911752,253.761740190968,30.0145549995742)) ;
#102120 = CARTESIAN_POINT('Ctrl Pts',(39.7769188845312,253.768377217198,30.0270844220837)) ;
#102121 = CARTESIAN_POINT('Ctrl Pts',(39.7501412146258,253.78721321578,30.0516371458428)) ;
#102122 = CARTESIAN_POINT('Ctrl Pts',(39.7370754538178,253.800023548159,30.0635653016335)) ;
#102123 = CARTESIAN_POINT('Ctrl Pts',(39.7180779384581,253.828041657271,30.0808650678764)) ;
#102124 = CARTESIAN_POINT('Ctrl Pts',(39.7112763996935,253.841958224525,30.087041829166)) ;
#102125 = CARTESIAN_POINT('Ctrl Pts',(39.7026699639647,253.870954690135,30.0948515246968)) ;
#102126 = CARTESIAN_POINT('Ctrl Pts',(39.7005167960037,253.885320776746,30.096802244712)) ;
#102127 = CARTESIAN_POINT('Ctrl Pts',(39.7005167960037,253.9,30.096802244712)) ;
#102128 = CARTESIAN_POINT('Origin',(40.2,253.9,25.0213203435596)) ;
#102129 = CARTESIAN_POINT('Origin',(39.8505167960037,253.9,27.759956707196)) ;
#102130 = CARTESIAN_POINT('',(39.8505167960037,253.75,30.5023074499214)) ;
#102131 = CARTESIAN_POINT('',(39.8505167960037,253.75,27.759956707196)) ;
#102132 = CARTESIAN_POINT('',(39.7005167960037,253.9,30.4985930708324)) ;
#102133 = CARTESIAN_POINT('Ctrl Pts',(39.8505167960037,253.75,30.5023074499214)) ;
#102134 = CARTESIAN_POINT('Ctrl Pts',(39.8490586726999,253.75,30.5022678161701)) ;
#102135 = CARTESIAN_POINT('Ctrl Pts',(39.8476006233589,253.750021261236,30.5022283083714)) ;
#102136 = CARTESIAN_POINT('Ctrl Pts',(39.8461431129253,253.750063777237,30.5021889366963)) ;
#102137 = CARTESIAN_POINT('Ctrl Pts',(39.8274188890355,253.750609968276,30.5016831399336)) ;
#102138 = CARTESIAN_POINT('Ctrl Pts',(39.8089607261724,253.754658837467,30.5012049258669)) ;
#102139 = CARTESIAN_POINT('Ctrl Pts',(39.7917256812164,253.762001431812,30.5007714713078)) ;
#102140 = CARTESIAN_POINT('Ctrl Pts',(39.7737581677139,253.769656077527,30.5003195954547)) ;
#102141 = CARTESIAN_POINT('Ctrl Pts',(39.757456249043,253.78074710398,30.49992447295)) ;
#102142 = CARTESIAN_POINT('Ctrl Pts',(39.7437381135436,253.794651469056,30.4995981034064)) ;
#102143 = CARTESIAN_POINT('Ctrl Pts',(39.7300236484415,253.808552113907,30.4992718211856)) ;
#102144 = CARTESIAN_POINT('Ctrl Pts',(39.7191539711575,253.824998688613,30.4990202369966)) ;
#102145 = CARTESIAN_POINT('Ctrl Pts',(39.7117415393002,253.843066458683,30.4988497601076)) ;
#102146 = CARTESIAN_POINT('Ctrl Pts',(39.704330020872,253.861132002274,30.4986793042264)) ;
#102147 = CARTESIAN_POINT('Ctrl Pts',(39.7005167960037,253.880472526098,30.4985930708322)) ;
#102148 = CARTESIAN_POINT('Ctrl Pts',(39.7005167960037,253.9,30.4985930708322)) ;
#102149 = CARTESIAN_POINT('',(39.7005167960037,253.9,27.759956707196)) ;
#102150 = CARTESIAN_POINT('Origin',(40.2,253.9,30.5213203435596)) ;
#102151 = CARTESIAN_POINT('',(40.5494832039963,253.75,30.5023074499214)) ;
#102152 = CARTESIAN_POINT('Origin',(40.2,253.75,30.5213203435596)) ;
#102153 = CARTESIAN_POINT('',(40.6994832039963,253.9,30.4985930708324)) ;
#102154 = CARTESIAN_POINT('Ctrl Pts',(40.5494832039964,253.75,30.5023074499214)) ;
#102155 = CARTESIAN_POINT('Ctrl Pts',(40.5509413273002,253.75,30.5022678161702)) ;
#102156 = CARTESIAN_POINT('Ctrl Pts',(40.5523993766411,253.750021261236,30.5022283083715)) ;
#102157 = CARTESIAN_POINT('Ctrl Pts',(40.5538568870747,253.750063777237,30.5021889366964)) ;
#102158 = CARTESIAN_POINT('Ctrl Pts',(40.5725811109645,253.750609968276,30.5016831399329)) ;
#102159 = CARTESIAN_POINT('Ctrl Pts',(40.5910392738275,253.754658837467,30.5012049258645)) ;
#102160 = CARTESIAN_POINT('Ctrl Pts',(40.6082743187836,253.762001431812,30.500771471306)) ;
#102161 = CARTESIAN_POINT('Ctrl Pts',(40.6262418322859,253.769656077527,30.5003195954534)) ;
#102162 = CARTESIAN_POINT('Ctrl Pts',(40.642543750957,253.78074710398,30.4999244729504)) ;
#102163 = CARTESIAN_POINT('Ctrl Pts',(40.6562618864565,253.794651469056,30.4995981034069)) ;
#102164 = CARTESIAN_POINT('Ctrl Pts',(40.6699763515586,253.808552113907,30.4992718211861)) ;
#102165 = CARTESIAN_POINT('Ctrl Pts',(40.6808460288425,253.824998688613,30.4990202369969)) ;
#102166 = CARTESIAN_POINT('Ctrl Pts',(40.6882584606999,253.843066458683,30.4988497601079)) ;
#102167 = CARTESIAN_POINT('Ctrl Pts',(40.695669979128,253.861132002274,30.4986793042266)) ;
#102168 = CARTESIAN_POINT('Ctrl Pts',(40.6994832039963,253.880472526098,30.4985930708323)) ;
#102169 = CARTESIAN_POINT('Ctrl Pts',(40.6994832039963,253.9,30.4985930708323)) ;
#102170 = CARTESIAN_POINT('Origin',(40.2,253.9,30.5213203435596)) ;
#102171 = CARTESIAN_POINT('Origin',(40.5494832039963,253.9,27.4082910455649)) ;
#102172 = CARTESIAN_POINT('',(40.5494832039963,253.75,29.9589677074491)) ;
#102173 = CARTESIAN_POINT('',(40.5494832039963,253.75,27.4082910455649)) ;
#102174 = CARTESIAN_POINT('',(40.6994832039963,253.9,30.096802244712)) ;
#102175 = CARTESIAN_POINT('Ctrl Pts',(40.5494832039963,253.75,29.9589677074491)) ;
#102176 = CARTESIAN_POINT('Ctrl Pts',(40.5500602746609,253.75,29.9595053771305)) ;
#102177 = CARTESIAN_POINT('Ctrl Pts',(40.5506373932381,253.750003330106,29.9600430036291)) ;
#102178 = CARTESIAN_POINT('Ctrl Pts',(40.5660876095744,253.750181671152,29.974433616113)) ;
#102179 = CARTESIAN_POINT('Ctrl Pts',(40.5810466107592,253.752566842488,29.9883070896991)) ;
#102180 = CARTESIAN_POINT('Ctrl Pts',(40.6094619088257,253.761740190968,30.014554999575)) ;
#102181 = CARTESIAN_POINT('Ctrl Pts',(40.6230811154693,253.768377217198,30.027084422084)) ;
#102182 = CARTESIAN_POINT('Ctrl Pts',(40.6498587853742,253.78721321578,30.0516371458428)) ;
#102183 = CARTESIAN_POINT('Ctrl Pts',(40.6629245461822,253.800023548159,30.0635653016335)) ;
#102184 = CARTESIAN_POINT('Ctrl Pts',(40.681922061542,253.828041657271,30.0808650678764)) ;
#102185 = CARTESIAN_POINT('Ctrl Pts',(40.6887236003065,253.841958224525,30.087041829166)) ;
#102186 = CARTESIAN_POINT('Ctrl Pts',(40.6973300360353,253.870954690135,30.0948515246968)) ;
#102187 = CARTESIAN_POINT('Ctrl Pts',(40.6994832039963,253.885320776746,30.096802244712)) ;
#102188 = CARTESIAN_POINT('Ctrl Pts',(40.6994832039963,253.9,30.096802244712)) ;
#102189 = CARTESIAN_POINT('',(40.6994832039963,253.9,27.4082910455649)) ;
#102190 = CARTESIAN_POINT('Origin',(40.2,253.9,25.0213203435596)) ;
#102191 = CARTESIAN_POINT('',(41.3934386691762,253.75,29.8252982934377)) ;
#102192 = CARTESIAN_POINT('Origin',(40.2,253.75,25.0213203435596)) ;
#102193 = CARTESIAN_POINT('',(41.293373406158,253.9,30.0027392774284)) ;
#102194 = CARTESIAN_POINT('Ctrl Pts',(41.3934386691762,253.75,29.8252982934377)) ;
#102195 = CARTESIAN_POINT('Ctrl Pts',(41.3930559914298,253.75,29.8259879723329)) ;
#102196 = CARTESIAN_POINT('Ctrl Pts',(41.3926732547717,253.750003330105,29.8266776249647)) ;
#102197 = CARTESIAN_POINT('Ctrl Pts',(41.3824261696638,253.750181671152,29.8451382901554)) ;
#102198 = CARTESIAN_POINT('Ctrl Pts',(41.3724864532188,253.752566842487,29.8629553331985)) ;
#102199 = CARTESIAN_POINT('Ctrl Pts',(41.3535729490481,253.761740190968,29.896699388929)) ;
#102200 = CARTESIAN_POINT('Ctrl Pts',(41.3444921183076,253.768377217198,29.912824144155)) ;
#102201 = CARTESIAN_POINT('Ctrl Pts',(41.3266122497526,253.78721321578,29.9444499271496)) ;
#102202 = CARTESIAN_POINT('Ctrl Pts',(41.3178719756467,253.800023548159,29.9598318195758)) ;
#102203 = CARTESIAN_POINT('Ctrl Pts',(41.3051501866382,253.828041657271,29.9821554300886)) ;
#102204 = CARTESIAN_POINT('Ctrl Pts',(41.300590263084,253.841958224525,29.9901316702288)) ;
#102205 = CARTESIAN_POINT('Ctrl Pts',(41.294818384942,253.870954690135,30.0002186669547)) ;
#102206 = CARTESIAN_POINT('Ctrl Pts',(41.293373406158,253.885320776746,30.0027392774284)) ;
#102207 = CARTESIAN_POINT('Ctrl Pts',(41.293373406158,253.9,30.0027392774284)) ;
#102208 = CARTESIAN_POINT('Origin',(40.2,253.9,25.0213203435596)) ;
#102209 = CARTESIAN_POINT('Origin',(40.7139068992805,253.9,27.7339145522423)) ;
#102210 = CARTESIAN_POINT('',(41.5613398833194,253.75,30.342045096078)) ;
#102211 = CARTESIAN_POINT('',(40.7139068992805,253.75,27.7339145522423)) ;
#102212 = CARTESIAN_POINT('',(41.4175335996131,253.9,30.3848650607978)) ;
#102213 = CARTESIAN_POINT('Ctrl Pts',(41.5613398833194,253.75,30.342045096078)) ;
#102214 = CARTESIAN_POINT('Ctrl Pts',(41.559940878147,253.75,30.3424579870215)) ;
#102215 = CARTESIAN_POINT('Ctrl Pts',(41.558541982239,253.750021261236,30.3428709748967)) ;
#102216 = CARTESIAN_POINT('Ctrl Pts',(41.5571436409268,253.750063777237,30.3432839257022)) ;
#102217 = CARTESIAN_POINT('Ctrl Pts',(41.5391795459883,253.750609968276,30.3485889877849)) ;
#102218 = CARTESIAN_POINT('Ctrl Pts',(41.521477013645,253.754658837467,30.3538380651887)) ;
#102219 = CARTESIAN_POINT('Ctrl Pts',(41.504951567006,253.762001431812,30.3587517471961)) ;
#102220 = CARTESIAN_POINT('Ctrl Pts',(41.4877238088899,253.769656077527,30.3638742547405)) ;
#102221 = CARTESIAN_POINT('Ctrl Pts',(41.472097663341,253.78074710398,30.368536040818)) ;
#102222 = CARTESIAN_POINT('Ctrl Pts',(41.4589500874475,253.794651469056,30.3724647819372)) ;
#102223 = CARTESIAN_POINT('Ctrl Pts',(41.4458060292934,253.808552113907,30.3763924718902)) ;
#102224 = CARTESIAN_POINT('Ctrl Pts',(41.4353906080926,253.824998688613,30.3795121161121)) ;
#102225 = CARTESIAN_POINT('Ctrl Pts',(41.4282882862172,253.843066458683,30.3816405503694)) ;
#102226 = CARTESIAN_POINT('Ctrl Pts',(41.4211868395563,253.861132002274,30.3837687223411)) ;
#102227 = CARTESIAN_POINT('Ctrl Pts',(41.4175335996131,253.880472526098,30.3848650607977)) ;
#102228 = CARTESIAN_POINT('Ctrl Pts',(41.4175335996131,253.9,30.3848650607977)) ;
#102229 = CARTESIAN_POINT('',(40.5712484218362,253.9,27.7802671013986)) ;
#102230 = CARTESIAN_POINT('Origin',(41.8995934690622,253.9,30.252131183183)) ;
#102231 = CARTESIAN_POINT('',(42.2260964403122,253.75,30.1260525975114)) ;
#102232 = CARTESIAN_POINT('Origin',(41.8995934690622,253.75,30.252131183183)) ;
#102233 = CARTESIAN_POINT('',(42.3676071114944,253.9,30.0761674639184)) ;
#102234 = CARTESIAN_POINT('Ctrl Pts',(42.2260964403122,253.75,30.1260525975113)) ;
#102235 = CARTESIAN_POINT('Ctrl Pts',(42.2274709504791,253.75,30.1255643186932)) ;
#102236 = CARTESIAN_POINT('Ctrl Pts',(42.2288454292249,253.750021261236,30.1250761825188)) ;
#102237 = CARTESIAN_POINT('Ctrl Pts',(42.2302194375035,253.750063777237,30.1245883423371)) ;
#102238 = CARTESIAN_POINT('Ctrl Pts',(42.24787093285,253.750609968276,30.1183211976397)) ;
#102239 = CARTESIAN_POINT('Ctrl Pts',(42.2652779126467,253.754658837467,30.112162503026)) ;
#102240 = CARTESIAN_POINT('Ctrl Pts',(42.2815354696359,253.762001431812,30.1064243414531)) ;
#102241 = CARTESIAN_POINT('Ctrl Pts',(42.298483953116,253.769656077527,30.1004423149599)) ;
#102242 = CARTESIAN_POINT('Ctrl Pts',(42.3138658995278,253.78074710398,30.095028961218)) ;
#102243 = CARTESIAN_POINT('Ctrl Pts',(42.3268117679506,253.794651469056,30.0904794283365)) ;
#102244 = CARTESIAN_POINT('Ctrl Pts',(42.3397541726023,253.808552113907,30.085931112719)) ;
#102245 = CARTESIAN_POINT('Ctrl Pts',(42.3500141062232,253.824998688613,30.0823329269323)) ;
#102246 = CARTESIAN_POINT('Ctrl Pts',(42.3570110675869,253.843066458683,30.0798802263626)) ;
#102247 = CARTESIAN_POINT('Ctrl Pts',(42.3640071667196,253.861132002274,30.0774278280376)) ;
#102248 = CARTESIAN_POINT('Ctrl Pts',(42.3676071114944,253.880472526098,30.0761674639185)) ;
#102249 = CARTESIAN_POINT('Ctrl Pts',(42.3676071114944,253.9,30.0761674639186)) ;
#102250 = CARTESIAN_POINT('Origin',(41.8995934690622,253.9,30.252131183183)) ;
#102251 = CARTESIAN_POINT('Origin',(41.2699927904911,253.9,27.1834681346239)) ;
#102252 = CARTESIAN_POINT('',(42.0581952261689,253.75,29.6093057948708)) ;
#102253 = CARTESIAN_POINT('',(41.2699927904911,253.75,27.1834681346239)) ;
#102254 = CARTESIAN_POINT('',(42.2434469180392,253.9,29.694041680549)) ;
#102255 = CARTESIAN_POINT('Ctrl Pts',(42.0581952261689,253.75,29.6093057948708)) ;
#102256 = CARTESIAN_POINT('Ctrl Pts',(42.0589102020537,253.75,29.6096388244826)) ;
#102257 = CARTESIAN_POINT('Ctrl Pts',(42.059625210162,253.750003330106,29.6099717982194)) ;
#102258 = CARTESIAN_POINT('Ctrl Pts',(42.0787661829038,253.750181671152,29.6188837045809)) ;
#102259 = CARTESIAN_POINT('Ctrl Pts',(42.0972801775669,253.752566842488,29.6274555764536)) ;
#102260 = CARTESIAN_POINT('Ctrl Pts',(42.1324157821739,253.761740190968,29.6436380121774)) ;
#102261 = CARTESIAN_POINT('Ctrl Pts',(42.1492402218841,253.768377217198,29.6513456347973)) ;
#102262 = CARTESIAN_POINT('Ctrl Pts',(42.1822945082382,253.78721321578,29.6664219076506)) ;
#102263 = CARTESIAN_POINT('Ctrl Pts',(42.1984067880458,253.800023548159,29.6737287158085)) ;
#102264 = CARTESIAN_POINT('Ctrl Pts',(42.2218204205898,253.828041657271,29.6843112161272)) ;
#102265 = CARTESIAN_POINT('Ctrl Pts',(42.2301977925614,253.841958224525,29.6880838741351)) ;
#102266 = CARTESIAN_POINT('Ctrl Pts',(42.2407963279832,253.870954690135,29.6928518010587)) ;
#102267 = CARTESIAN_POINT('Ctrl Pts',(42.2434469180392,253.885320776746,29.694041680549)) ;
#102268 = CARTESIAN_POINT('Ctrl Pts',(42.2434469180392,253.9,29.694041680549)) ;
#102269 = CARTESIAN_POINT('',(41.4126512679354,253.9,27.1371155854676)) ;
#102270 = CARTESIAN_POINT('Origin',(40.2,253.9,25.0213203435596)) ;
#102271 = CARTESIAN_POINT('',(42.8195384502335,253.75,29.2213820464098)) ;
#102272 = CARTESIAN_POINT('Origin',(40.2,253.75,25.0213203435596)) ;
#102273 = CARTESIAN_POINT('',(42.7792030093369,253.9,29.4210603173112)) ;
#102274 = CARTESIAN_POINT('Ctrl Pts',(42.8195384502335,253.75,29.2213820464098)) ;
#102275 = CARTESIAN_POINT('Ctrl Pts',(42.8193876245675,253.75,29.222156223949)) ;
#102276 = CARTESIAN_POINT('Ctrl Pts',(42.8192367347585,253.750003330105,29.2229303947088)) ;
#102277 = CARTESIAN_POINT('Ctrl Pts',(42.8151958369642,253.750181671152,29.2436540540784)) ;
#102278 = CARTESIAN_POINT('Ctrl Pts',(42.8112483739592,253.752566842488,29.2636706102647)) ;
#102279 = CARTESIAN_POINT('Ctrl Pts',(42.8036880492521,253.761740190969,29.3016077085626)) ;
#102280 = CARTESIAN_POINT('Ctrl Pts',(42.8000344893982,253.768377217198,29.3197493931144)) ;
#102281 = CARTESIAN_POINT('Ctrl Pts',(42.7928026283045,253.78721321578,29.3553524833538)) ;
#102282 = CARTESIAN_POINT('Ctrl Pts',(42.7892433998272,253.800023548159,29.3726824256129)) ;
#102283 = CARTESIAN_POINT('Ctrl Pts',(42.784042634516,253.828041657271,29.3978446898607)) ;
#102284 = CARTESIAN_POINT('Ctrl Pts',(42.7821706832604,253.841958224525,29.4068396388929)) ;
#102285 = CARTESIAN_POINT('Ctrl Pts',(42.7797983543528,253.870954690135,29.4182165512944)) ;
#102286 = CARTESIAN_POINT('Ctrl Pts',(42.7792030093369,253.885320776746,29.4210603173112)) ;
#102287 = CARTESIAN_POINT('Ctrl Pts',(42.7792030093369,253.9,29.4210603173112)) ;
#102288 = CARTESIAN_POINT('Origin',(40.2,253.9,25.0213203435596)) ;
#102289 = CARTESIAN_POINT('Origin',(41.5269922146558,253.9,27.4423447763876)) ;
#102290 = CARTESIAN_POINT('',(43.1389055378431,253.75,29.6609531317893)) ;
#102291 = CARTESIAN_POINT('',(41.5269922146558,253.75,27.4423447763876)) ;
#102292 = CARTESIAN_POINT('',(43.0153697314369,253.9,29.7461159238265)) ;
#102293 = CARTESIAN_POINT('Ctrl Pts',(43.1389055378431,253.75,29.6609531317893)) ;
#102294 = CARTESIAN_POINT('Ctrl Pts',(43.1377025951759,253.75,29.661778130785)) ;
#102295 = CARTESIAN_POINT('Ctrl Pts',(43.1364997863788,253.750021261236,29.6626031882036)) ;
#102296 = CARTESIAN_POINT('Ctrl Pts',(43.1352974935786,253.750063777237,29.6634280389876)) ;
#102297 = CARTESIAN_POINT('Ctrl Pts',(43.1198519783685,253.750609968276,29.6740246634766)) ;
#102298 = CARTESIAN_POINT('Ctrl Pts',(43.1046379237495,253.754658837467,29.6844872160813)) ;
#102299 = CARTESIAN_POINT('Ctrl Pts',(43.0904397012843,253.762001431812,29.6942670492247)) ;
#102300 = CARTESIAN_POINT('Ctrl Pts',(43.0756380715522,253.769656077527,29.7044625134375)) ;
#102301 = CARTESIAN_POINT('Ctrl Pts',(43.0622172951262,253.78074710398,29.7137248799966)) ;
#102302 = CARTESIAN_POINT('Ctrl Pts',(43.0509272551715,253.794651469056,29.7215241592249)) ;
#102303 = CARTESIAN_POINT('Ctrl Pts',(43.0396402359576,253.808552113907,29.7293213516934)) ;
#102304 = CARTESIAN_POINT('Ctrl Pts',(43.0306986048354,253.824998688613,29.7355068518135)) ;
#102305 = CARTESIAN_POINT('Ctrl Pts',(43.0246016176919,253.843066458683,29.7397258512424)) ;
#102306 = CARTESIAN_POINT('Ctrl Pts',(43.0185053818762,253.861132002274,29.7439443307668)) ;
#102307 = CARTESIAN_POINT('Ctrl Pts',(43.0153697314371,253.880472526098,29.7461159238268)) ;
#102308 = CARTESIAN_POINT('Ctrl Pts',(43.015369731437,253.9,29.7461159238267)) ;
#102309 = CARTESIAN_POINT('',(41.4056396654995,253.9,27.5305125642315)) ;
#102310 = CARTESIAN_POINT('Origin',(43.4328188876086,253.9,29.4709138126218)) ;
#102311 = CARTESIAN_POINT('',(43.7043812404062,253.75,29.2501109853232)) ;
#102312 = CARTESIAN_POINT('Origin',(43.4328188876086,253.75,29.4709138126218)) ;
#102313 = CARTESIAN_POINT('',(43.8235505323126,253.9,29.1589382016729)) ;
#102314 = CARTESIAN_POINT('Ctrl Pts',(43.7043812404062,253.75,29.2501109853232)) ;
#102315 = CARTESIAN_POINT('Ctrl Pts',(43.7055375908048,253.75,29.2492218575706)) ;
#102316 = CARTESIAN_POINT('Ctrl Pts',(43.7066939553966,253.750021261236,29.2483328751888)) ;
#102317 = CARTESIAN_POINT('Ctrl Pts',(43.7078499640179,253.750063777237,29.2474443196972)) ;
#102318 = CARTESIAN_POINT('Ctrl Pts',(43.7227008794821,253.750609968276,29.2360292988668)) ;
#102319 = CARTESIAN_POINT('Ctrl Pts',(43.7373527597389,253.754658837467,29.2247929796351)) ;
#102320 = CARTESIAN_POINT('Ctrl Pts',(43.7510414258099,253.762001431812,29.2143118022833)) ;
#102321 = CARTESIAN_POINT('Ctrl Pts',(43.7653118436181,253.769656077527,29.2033851875821)) ;
#102322 = CARTESIAN_POINT('Ctrl Pts',(43.7782681256832,253.78074710398,29.1934834993827)) ;
#102323 = CARTESIAN_POINT('Ctrl Pts',(43.7891744952288,253.794651469056,29.18515614314)) ;
#102324 = CARTESIAN_POINT('Ctrl Pts',(43.8000779466878,253.808552113907,29.1768310149483)) ;
#102325 = CARTESIAN_POINT('Ctrl Pts',(43.808723822858,253.824998688613,29.1702384430595)) ;
#102326 = CARTESIAN_POINT('Ctrl Pts',(43.8146204023989,253.843066458683,29.1657436062296)) ;
#102327 = CARTESIAN_POINT('Ctrl Pts',(43.8205162553081,253.861132002274,29.1612493232955)) ;
#102328 = CARTESIAN_POINT('Ctrl Pts',(43.8235505323127,253.880472526098,29.1589382016731)) ;
#102329 = CARTESIAN_POINT('Ctrl Pts',(43.8235505323126,253.9,29.1589382016729)) ;
#102330 = CARTESIAN_POINT('Origin',(43.4328188876086,253.9,29.4709138126218)) ;
#102331 = CARTESIAN_POINT('Origin',(41.8857640275745,253.9,26.746999133324)) ;
#102332 = CARTESIAN_POINT('',(43.3850141527966,253.75,28.8105398999439)) ;
#102333 = CARTESIAN_POINT('',(41.8857640275745,253.75,26.746999133324)) ;
#102334 = CARTESIAN_POINT('',(43.5873838102126,253.9,28.8338825951576)) ;
#102335 = CARTESIAN_POINT('Ctrl Pts',(43.3850141527966,253.75,28.8105398999439)) ;
#102336 = CARTESIAN_POINT('Ctrl Pts',(43.3857970470792,253.75,28.8106356902272)) ;
#102337 = CARTESIAN_POINT('Ctrl Pts',(43.3865799547416,253.750003330105,28.8107314174126)) ;
#102338 = CARTESIAN_POINT('Ctrl Pts',(43.4075380321148,253.750181671152,28.8132922581638)) ;
#102339 = CARTESIAN_POINT('Ctrl Pts',(43.4277947414637,253.752566842487,28.815723453781)) ;
#102340 = CARTESIAN_POINT('Ctrl Pts',(43.4662113348296,253.761740190968,28.8202563657946)) ;
#102341 = CARTESIAN_POINT('Ctrl Pts',(43.4845941142253,253.768377217198,28.8223877127212)) ;
#102342 = CARTESIAN_POINT('Ctrl Pts',(43.5206894331777,253.78721321578,28.8265117640394)) ;
#102343 = CARTESIAN_POINT('Ctrl Pts',(43.5382710497767,253.800023548159,28.8284819832727)) ;
#102344 = CARTESIAN_POINT('Ctrl Pts',(43.5638089100193,253.828041657271,28.8313113288033)) ;
#102345 = CARTESIAN_POINT('Ctrl Pts',(43.5729420796607,253.841958224525,28.832310589478)) ;
#102346 = CARTESIAN_POINT('Ctrl Pts',(43.584495256284,253.870954690135,28.8335700298871)) ;
#102347 = CARTESIAN_POINT('Ctrl Pts',(43.5873838102126,253.885320776746,28.8338825951576)) ;
#102348 = CARTESIAN_POINT('Ctrl Pts',(43.5873838102126,253.9,28.8338825951576)) ;
#102349 = CARTESIAN_POINT('',(42.0071165767308,253.9,26.6588313454802)) ;
#102350 = CARTESIAN_POINT('Origin',(40.2,253.9,25.0213203435596)) ;
#102351 = CARTESIAN_POINT('',(43.9892195563843,253.75,28.2063344963563)) ;
#102352 = CARTESIAN_POINT('Origin',(40.2,253.75,25.0213203435596)) ;
#102353 = CARTESIAN_POINT('',(44.012562251598,253.9,28.4087041537722)) ;
#102354 = CARTESIAN_POINT('Ctrl Pts',(43.9892195563843,253.75,28.2063344963563)) ;
#102355 = CARTESIAN_POINT('Ctrl Pts',(43.9893153466677,253.75,28.2071173906402)) ;
#102356 = CARTESIAN_POINT('Ctrl Pts',(43.9894110738533,253.750003330106,28.2079002983041)) ;
#102357 = CARTESIAN_POINT('Ctrl Pts',(43.9919719146048,253.750181671152,28.2288583756769)) ;
#102358 = CARTESIAN_POINT('Ctrl Pts',(43.9944031102216,253.752566842488,28.2491150850258)) ;
#102359 = CARTESIAN_POINT('Ctrl Pts',(43.9989360222351,253.761740190968,28.2875316783904)) ;
#102360 = CARTESIAN_POINT('Ctrl Pts',(44.0010673691616,253.768377217198,28.3059144577855)) ;
#102361 = CARTESIAN_POINT('Ctrl Pts',(44.0051914204798,253.78721321578,28.3420097767375)) ;
#102362 = CARTESIAN_POINT('Ctrl Pts',(44.0071616397131,253.800023548159,28.3595913933363)) ;
#102363 = CARTESIAN_POINT('Ctrl Pts',(44.0099909852436,253.828041657271,28.3851292535788)) ;
#102364 = CARTESIAN_POINT('Ctrl Pts',(44.0109902459184,253.841958224525,28.3942624232203)) ;
#102365 = CARTESIAN_POINT('Ctrl Pts',(44.0122496863275,253.870954690135,28.4058155998437)) ;
#102366 = CARTESIAN_POINT('Ctrl Pts',(44.012562251598,253.885320776746,28.4087041537722)) ;
#102367 = CARTESIAN_POINT('Ctrl Pts',(44.012562251598,253.9,28.4087041537722)) ;
#102368 = CARTESIAN_POINT('Origin',(40.2,253.9,25.0213203435596)) ;
#102369 = CARTESIAN_POINT('Origin',(42.2101822863621,253.9,26.9137882607786)) ;
#102370 = CARTESIAN_POINT('',(44.4287906417639,253.75,28.5257015839661)) ;
#102371 = CARTESIAN_POINT('',(42.2101822863621,253.75,26.9137882607786)) ;
#102372 = CARTESIAN_POINT('',(44.3376178581133,253.9,28.6448708758722)) ;
#102373 = CARTESIAN_POINT('Ctrl Pts',(44.4287906417639,253.75,28.5257015839661)) ;
#102374 = CARTESIAN_POINT('Ctrl Pts',(44.4279015140116,253.75,28.5268579343644)) ;
#102375 = CARTESIAN_POINT('Ctrl Pts',(44.4270125316306,253.750021261236,28.5280142989575)) ;
#102376 = CARTESIAN_POINT('Ctrl Pts',(44.4261239761386,253.750063777237,28.5291703075782)) ;
#102377 = CARTESIAN_POINT('Ctrl Pts',(44.4147089553012,253.750609968276,28.5440212230371)) ;
#102378 = CARTESIAN_POINT('Ctrl Pts',(44.403472636075,253.754658837467,28.5586731032981)) ;
#102379 = CARTESIAN_POINT('Ctrl Pts',(44.3929914587233,253.762001431812,28.5723617693692)) ;
#102380 = CARTESIAN_POINT('Ctrl Pts',(44.3820648440222,253.769656077527,28.5866321871774)) ;
#102381 = CARTESIAN_POINT('Ctrl Pts',(44.3721631558234,253.78074710398,28.5995884692429)) ;
#102382 = CARTESIAN_POINT('Ctrl Pts',(44.3638357995806,253.794651469056,28.6104948387886)) ;
#102383 = CARTESIAN_POINT('Ctrl Pts',(44.3555106713888,253.808552113907,28.6213982902475)) ;
#102384 = CARTESIAN_POINT('Ctrl Pts',(44.3489180994998,253.824998688613,28.6300441664176)) ;
#102385 = CARTESIAN_POINT('Ctrl Pts',(44.3444232626699,253.843066458683,28.6359407459585)) ;
#102386 = CARTESIAN_POINT('Ctrl Pts',(44.3399289797359,253.861132002274,28.6418365988678)) ;
#102387 = CARTESIAN_POINT('Ctrl Pts',(44.3376178581134,253.880472526098,28.6448708758723)) ;
#102388 = CARTESIAN_POINT('Ctrl Pts',(44.3376178581134,253.9,28.6448708758723)) ;
#102389 = CARTESIAN_POINT('',(42.1220144985182,253.9,27.0351408099348)) ;
#102390 = CARTESIAN_POINT('Origin',(44.6495934690622,253.9,28.2541392311682)) ;
#102391 = CARTESIAN_POINT('',(44.8396327882296,253.75,27.9602258814027)) ;
#102392 = CARTESIAN_POINT('Origin',(44.6495934690622,253.75,28.2541392311682)) ;
#102393 = CARTESIAN_POINT('',(44.9247955802669,253.9,27.8366900749965)) ;
#102394 = CARTESIAN_POINT('Ctrl Pts',(44.8396327882335,253.75,27.9602258813973)) ;
#102395 = CARTESIAN_POINT('Ctrl Pts',(44.8404577872282,253.75,27.9590229387317)) ;
#102396 = CARTESIAN_POINT('Ctrl Pts',(44.841282844644,253.750021261236,27.957820129936)) ;
#102397 = CARTESIAN_POINT('Ctrl Pts',(44.8421076954273,253.750063777237,27.9566178371377)) ;
#102398 = CARTESIAN_POINT('Ctrl Pts',(44.8527043199225,253.750609968276,27.9411723219304)) ;
#102399 = CARTESIAN_POINT('Ctrl Pts',(44.8631668725218,253.754658837467,27.9259582673091)) ;
#102400 = CARTESIAN_POINT('Ctrl Pts',(44.8729467056653,253.762001431812,27.911760044844)) ;
#102401 = CARTESIAN_POINT('Ctrl Pts',(44.8831421698783,253.769656077527,27.8969584151118)) ;
#102402 = CARTESIAN_POINT('Ctrl Pts',(44.8924045364365,253.78074710398,27.8835376386854)) ;
#102403 = CARTESIAN_POINT('Ctrl Pts',(44.9002038156648,253.794651469056,27.8722475987308)) ;
#102404 = CARTESIAN_POINT('Ctrl Pts',(44.9080010081334,253.808552113907,27.8609605795169)) ;
#102405 = CARTESIAN_POINT('Ctrl Pts',(44.9141865082541,253.824998688613,27.8520189483951)) ;
#102406 = CARTESIAN_POINT('Ctrl Pts',(44.918405507683,253.843066458683,27.8459219612516)) ;
#102407 = CARTESIAN_POINT('Ctrl Pts',(44.9226239872073,253.861132002274,27.8398257254358)) ;
#102408 = CARTESIAN_POINT('Ctrl Pts',(44.9247955802671,253.880472526098,27.8366900749966)) ;
#102409 = CARTESIAN_POINT('Ctrl Pts',(44.924795580267,253.9,27.8366900749965)) ;
#102410 = CARTESIAN_POINT('Origin',(44.6495934690622,253.9,28.2541392311682)) ;
#102411 = CARTESIAN_POINT('Origin',(42.3365209362303,253.9,26.1416086685709)) ;
#102412 = CARTESIAN_POINT('',(44.4000617028502,253.75,27.6408587937931)) ;
#102413 = CARTESIAN_POINT('',(42.3365209362303,253.75,26.1416086685709)) ;
#102414 = CARTESIAN_POINT('',(44.5997399737516,253.9,27.6005233528965)) ;
#102415 = CARTESIAN_POINT('Ctrl Pts',(44.4000617028502,253.75,27.6408587937931)) ;
#102416 = CARTESIAN_POINT('Ctrl Pts',(44.4008358803894,253.75,27.6407079681271)) ;
#102417 = CARTESIAN_POINT('Ctrl Pts',(44.4016100511492,253.750003330105,27.6405570783181)) ;
#102418 = CARTESIAN_POINT('Ctrl Pts',(44.4223337105192,253.750181671152,27.6365161805235)) ;
#102419 = CARTESIAN_POINT('Ctrl Pts',(44.4423502667051,253.752566842488,27.6325687175188)) ;
#102420 = CARTESIAN_POINT('Ctrl Pts',(44.480287365003,253.761740190969,27.6250083928117)) ;
#102421 = CARTESIAN_POINT('Ctrl Pts',(44.4984290495548,253.768377217198,27.6213548329578)) ;
#102422 = CARTESIAN_POINT('Ctrl Pts',(44.5340321397943,253.78721321578,27.6141229718641)) ;
#102423 = CARTESIAN_POINT('Ctrl Pts',(44.5513620820533,253.800023548159,27.6105637433868)) ;
#102424 = CARTESIAN_POINT('Ctrl Pts',(44.5765243463011,253.828041657271,27.6053629780756)) ;
#102425 = CARTESIAN_POINT('Ctrl Pts',(44.5855192953333,253.841958224525,27.6034910268201)) ;
#102426 = CARTESIAN_POINT('Ctrl Pts',(44.5968962077348,253.870954690135,27.6011186979124)) ;
#102427 = CARTESIAN_POINT('Ctrl Pts',(44.5997399737516,253.885320776746,27.6005233528965)) ;
#102428 = CARTESIAN_POINT('Ctrl Pts',(44.5997399737516,253.9,27.6005233528965)) ;
#102429 = CARTESIAN_POINT('',(42.4246887240742,253.9,26.0202561194147)) ;
#102430 = CARTESIAN_POINT('Origin',(40.2,253.9,25.0213203435596)) ;
#102431 = CARTESIAN_POINT('',(44.7879854513112,253.75,26.8795155697285)) ;
#102432 = CARTESIAN_POINT('Origin',(40.2,253.75,25.0213203435596)) ;
#102433 = CARTESIAN_POINT('',(44.8727213369894,253.9,27.0647672615988)) ;
#102434 = CARTESIAN_POINT('Ctrl Pts',(44.7879854513112,253.75,26.8795155697285)) ;
#102435 = CARTESIAN_POINT('Ctrl Pts',(44.788318480923,253.75,26.8802305456133)) ;
#102436 = CARTESIAN_POINT('Ctrl Pts',(44.7886514546598,253.750003330106,26.8809455537216)) ;
#102437 = CARTESIAN_POINT('Ctrl Pts',(44.7975633610213,253.750181671152,26.9000865264628)) ;
#102438 = CARTESIAN_POINT('Ctrl Pts',(44.806135232894,253.752566842488,26.9186005211264)) ;
#102439 = CARTESIAN_POINT('Ctrl Pts',(44.8223176686178,253.761740190968,26.9537361257334)) ;
#102440 = CARTESIAN_POINT('Ctrl Pts',(44.8300252912377,253.768377217198,26.9705605654437)) ;
#102441 = CARTESIAN_POINT('Ctrl Pts',(44.845101564091,253.78721321578,27.0036148517979)) ;
#102442 = CARTESIAN_POINT('Ctrl Pts',(44.8524083722489,253.800023548159,27.0197271316054)) ;
#102443 = CARTESIAN_POINT('Ctrl Pts',(44.8629908725676,253.828041657271,27.0431407641494)) ;
#102444 = CARTESIAN_POINT('Ctrl Pts',(44.8667635305755,253.841958224525,27.051518136121)) ;
#102445 = CARTESIAN_POINT('Ctrl Pts',(44.8715314574991,253.870954690135,27.0621166715429)) ;
#102446 = CARTESIAN_POINT('Ctrl Pts',(44.8727213369894,253.885320776746,27.0647672615988)) ;
#102447 = CARTESIAN_POINT('Ctrl Pts',(44.8727213369894,253.9,27.0647672615988)) ;
#102448 = CARTESIAN_POINT('Origin',(40.2,253.9,25.0213203435596)) ;
#102449 = CARTESIAN_POINT('Origin',(42.6966017101158,253.9,26.1999837998328)) ;
#102450 = CARTESIAN_POINT('',(45.3047322539518,253.75,27.0474167838718)) ;
#102451 = CARTESIAN_POINT('',(42.6966017101158,253.75,26.1999837998328)) ;
#102452 = CARTESIAN_POINT('',(45.2548471203588,253.9,27.188927455054)) ;
#102453 = CARTESIAN_POINT('Ctrl Pts',(45.3047322539518,253.75,27.0474167838718)) ;
#102454 = CARTESIAN_POINT('Ctrl Pts',(45.3042439751337,253.75,27.0487912940387)) ;
#102455 = CARTESIAN_POINT('Ctrl Pts',(45.3037558389592,253.750021261236,27.0501657727844)) ;
#102456 = CARTESIAN_POINT('Ctrl Pts',(45.3032679987773,253.750063777237,27.0515397810629)) ;
#102457 = CARTESIAN_POINT('Ctrl Pts',(45.2970008540777,253.750609968276,27.0691912764083)) ;
#102458 = CARTESIAN_POINT('Ctrl Pts',(45.2908421594672,253.754658837467,27.0865982562064)) ;
#102459 = CARTESIAN_POINT('Ctrl Pts',(45.2851039978939,253.762001431812,27.1028558131956)) ;
#102460 = CARTESIAN_POINT('Ctrl Pts',(45.2791219714003,253.769656077527,27.1198042966757)) ;
#102461 = CARTESIAN_POINT('Ctrl Pts',(45.2737086176584,253.78074710398,27.1351862430874)) ;
#102462 = CARTESIAN_POINT('Ctrl Pts',(45.2691590847767,253.794651469056,27.1481321115101)) ;
#102463 = CARTESIAN_POINT('Ctrl Pts',(45.2646107691591,253.808552113907,27.1610745161618)) ;
#102464 = CARTESIAN_POINT('Ctrl Pts',(45.2610125833728,253.824998688613,27.1713344497829)) ;
#102465 = CARTESIAN_POINT('Ctrl Pts',(45.2585598828031,253.843066458683,27.1783314111466)) ;
#102466 = CARTESIAN_POINT('Ctrl Pts',(45.2561074844782,253.861132002274,27.1853275102792)) ;
#102467 = CARTESIAN_POINT('Ctrl Pts',(45.2548471203586,253.880472526098,27.1889274550539)) ;
#102468 = CARTESIAN_POINT('Ctrl Pts',(45.2548471203588,253.9,27.1889274550539)) ;
#102469 = CARTESIAN_POINT('',(42.6502491609595,253.9,26.3426422772771)) ;
#102470 = CARTESIAN_POINT('Origin',(45.4308108396234,253.9,26.7209138126218)) ;
#102471 = CARTESIAN_POINT('',(45.5207247525186,253.75,26.382660226879)) ;
#102472 = CARTESIAN_POINT('Origin',(45.4308108396234,253.75,26.7209138126218)) ;
#102473 = CARTESIAN_POINT('',(45.5635447172382,253.9,26.2388539431727)) ;
#102474 = CARTESIAN_POINT('Ctrl Pts',(45.5207247525205,253.75,26.3826602268732)) ;
#102475 = CARTESIAN_POINT('Ctrl Pts',(45.5211376434635,253.75,26.3812612217023)) ;
#102476 = CARTESIAN_POINT('Ctrl Pts',(45.5215506313349,253.750021261236,26.3798623257963)) ;
#102477 = CARTESIAN_POINT('Ctrl Pts',(45.521963582141,253.750063777237,26.3784639844859)) ;
#102478 = CARTESIAN_POINT('Ctrl Pts',(45.5272686442386,253.750609968276,26.3604998895502)) ;
#102479 = CARTESIAN_POINT('Ctrl Pts',(45.5325177216272,253.754658837467,26.3427973572037)) ;
#102480 = CARTESIAN_POINT('Ctrl Pts',(45.5374314036352,253.762001431812,26.3262719105652)) ;
#102481 = CARTESIAN_POINT('Ctrl Pts',(45.5425539111803,253.769656077527,26.3090441524495)) ;
#102482 = CARTESIAN_POINT('Ctrl Pts',(45.5472156972587,253.78074710398,26.2934180069008)) ;
#102483 = CARTESIAN_POINT('Ctrl Pts',(45.551144438378,253.794651469056,26.2802704310072)) ;
#102484 = CARTESIAN_POINT('Ctrl Pts',(45.5550721283311,253.808552113907,26.2671263728531)) ;
#102485 = CARTESIAN_POINT('Ctrl Pts',(45.5581917725533,253.824998688613,26.2567109516524)) ;
#102486 = CARTESIAN_POINT('Ctrl Pts',(45.5603202068105,253.843066458683,26.249608629777)) ;
#102487 = CARTESIAN_POINT('Ctrl Pts',(45.5624483787821,253.861132002274,26.2425071831161)) ;
#102488 = CARTESIAN_POINT('Ctrl Pts',(45.5635447172386,253.880472526098,26.2388539431728)) ;
#102489 = CARTESIAN_POINT('Ctrl Pts',(45.5635447172384,253.9,26.2388539431728)) ;
#102490 = CARTESIAN_POINT('Origin',(45.4308108396234,253.9,26.7209138126218)) ;
#102491 = CARTESIAN_POINT('Origin',(42.5781402896312,253.9,25.426556577058)) ;
#102492 = CARTESIAN_POINT('',(45.0039779498781,253.75,26.2147590127358)) ;
#102493 = CARTESIAN_POINT('',(42.5781402896312,253.75,25.426556577058)) ;
#102494 = CARTESIAN_POINT('',(45.1814189338688,253.9,26.1146937497175)) ;
#102495 = CARTESIAN_POINT('Ctrl Pts',(45.0039779498781,253.75,26.2147590127358)) ;
#102496 = CARTESIAN_POINT('Ctrl Pts',(45.0046676287764,253.75,26.2143763349877)) ;
#102497 = CARTESIAN_POINT('Ctrl Pts',(45.0053572814057,253.750003330105,26.213993598331)) ;
#102498 = CARTESIAN_POINT('Ctrl Pts',(45.0238179465998,253.750181671152,26.2037465132207)) ;
#102499 = CARTESIAN_POINT('Ctrl Pts',(45.0416349896415,253.752566842488,26.1938067967769)) ;
#102500 = CARTESIAN_POINT('Ctrl Pts',(45.0753790453708,253.761740190968,26.1748932926068)) ;
#102501 = CARTESIAN_POINT('Ctrl Pts',(45.0915038005961,253.768377217198,26.1658124618668)) ;
#102502 = CARTESIAN_POINT('Ctrl Pts',(45.1231295835901,253.78721321578,26.1479325933121)) ;
#102503 = CARTESIAN_POINT('Ctrl Pts',(45.1385114760162,253.800023548159,26.1391923192062)) ;
#102504 = CARTESIAN_POINT('Ctrl Pts',(45.1608350865289,253.828041657271,26.1264705301978)) ;
#102505 = CARTESIAN_POINT('Ctrl Pts',(45.1688113266691,253.841958224525,26.1219106066435)) ;
#102506 = CARTESIAN_POINT('Ctrl Pts',(45.1788983233951,253.870954690135,26.1161387285016)) ;
#102507 = CARTESIAN_POINT('Ctrl Pts',(45.1814189338688,253.885320776746,26.1146937497175)) ;
#102508 = CARTESIAN_POINT('Ctrl Pts',(45.1814189338688,253.9,26.1146937497175)) ;
#102509 = CARTESIAN_POINT('',(42.6244928387874,253.9,25.2838980996137)) ;
#102510 = CARTESIAN_POINT('Origin',(40.2,253.9,25.0213203435596)) ;
#102511 = CARTESIAN_POINT('',(45.1376473638895,253.75,25.3708035475559)) ;
#102512 = CARTESIAN_POINT('Origin',(40.2,253.75,25.0213203435596)) ;
#102513 = CARTESIAN_POINT('',(45.2754819011524,253.9,25.5208035475559)) ;
#102514 = CARTESIAN_POINT('Ctrl Pts',(45.1376473638895,253.75,25.3708035475559)) ;
#102515 = CARTESIAN_POINT('Ctrl Pts',(45.1381850335709,253.75,25.3713806182205)) ;
#102516 = CARTESIAN_POINT('Ctrl Pts',(45.1387226600695,253.750003330106,25.3719577367977)) ;
#102517 = CARTESIAN_POINT('Ctrl Pts',(45.1531132725536,253.750181671152,25.3874079531344)) ;
#102518 = CARTESIAN_POINT('Ctrl Pts',(45.1669867461395,253.752566842488,25.4023669543188)) ;
#102519 = CARTESIAN_POINT('Ctrl Pts',(45.1932346560153,253.761740190968,25.4307822523852)) ;
#102520 = CARTESIAN_POINT('Ctrl Pts',(45.2057640785244,253.768377217198,25.4444014590288)) ;
#102521 = CARTESIAN_POINT('Ctrl Pts',(45.2303168022832,253.78721321578,25.4711791289338)) ;
#102522 = CARTESIAN_POINT('Ctrl Pts',(45.2422449580739,253.800023548158,25.4842448897418)) ;
#102523 = CARTESIAN_POINT('Ctrl Pts',(45.2595447243168,253.828041657271,25.5032424051016)) ;
#102524 = CARTESIAN_POINT('Ctrl Pts',(45.2657214856064,253.841958224525,25.5100439438662)) ;
#102525 = CARTESIAN_POINT('Ctrl Pts',(45.2735311811371,253.870954690135,25.5186503795949)) ;
#102526 = CARTESIAN_POINT('Ctrl Pts',(45.2754819011524,253.885320776746,25.5208035475559)) ;
#102527 = CARTESIAN_POINT('Ctrl Pts',(45.2754819011524,253.9,25.5208035475559)) ;
#102528 = CARTESIAN_POINT('Origin',(40.2,253.9,25.0213203435596)) ;
#102529 = CARTESIAN_POINT('Origin',(42.9386363636364,253.9,25.3708035475559)) ;
#102530 = CARTESIAN_POINT('',(45.6809871063618,253.75,25.3708035475559)) ;
#102531 = CARTESIAN_POINT('',(42.9386363636364,253.75,25.3708035475559)) ;
#102532 = CARTESIAN_POINT('',(45.6772727272728,253.9,25.5208035475559)) ;
#102533 = CARTESIAN_POINT('Ctrl Pts',(45.6809871063618,253.75,25.3708035475559)) ;
#102534 = CARTESIAN_POINT('Ctrl Pts',(45.6809474726106,253.75,25.3722616708597)) ;
#102535 = CARTESIAN_POINT('Ctrl Pts',(45.6809079648117,253.750021261236,25.3737197202007)) ;
#102536 = CARTESIAN_POINT('Ctrl Pts',(45.6808685931366,253.750063777237,25.3751772306343)) ;
#102537 = CARTESIAN_POINT('Ctrl Pts',(45.6803627963739,253.750609968276,25.3939014545242)) ;
#102538 = CARTESIAN_POINT('Ctrl Pts',(45.6798845823057,253.754658837467,25.4123596173872)) ;
#102539 = CARTESIAN_POINT('Ctrl Pts',(45.679451127747,253.762001431812,25.4295946623432)) ;
#102540 = CARTESIAN_POINT('Ctrl Pts',(45.6789992518942,253.769656077527,25.4475621758455)) ;
#102541 = CARTESIAN_POINT('Ctrl Pts',(45.6786041293909,253.78074710398,25.4638640945166)) ;
#102542 = CARTESIAN_POINT('Ctrl Pts',(45.6782777598473,253.794651469056,25.4775822300161)) ;
#102543 = CARTESIAN_POINT('Ctrl Pts',(45.6779514776265,253.808552113907,25.4912966951182)) ;
#102544 = CARTESIAN_POINT('Ctrl Pts',(45.6776998934371,253.824998688613,25.5021663724021)) ;
#102545 = CARTESIAN_POINT('Ctrl Pts',(45.6775294165481,253.843066458683,25.5095788042595)) ;
#102546 = CARTESIAN_POINT('Ctrl Pts',(45.6773589606669,253.861132002274,25.5169903226876)) ;
#102547 = CARTESIAN_POINT('Ctrl Pts',(45.6772727272728,253.880472526098,25.5208035475559)) ;
#102548 = CARTESIAN_POINT('Ctrl Pts',(45.6772727272728,253.9,25.5208035475559)) ;
#102549 = CARTESIAN_POINT('',(42.9386363636364,253.9,25.5208035475559)) ;
#102550 = CARTESIAN_POINT('Origin',(45.7,253.9,25.0213203435596)) ;
#102551 = CARTESIAN_POINT('',(45.6809871063617,253.75,24.6718371395634)) ;
#102552 = CARTESIAN_POINT('Origin',(45.7,253.75,25.0213203435596)) ;
#102553 = CARTESIAN_POINT('',(45.6772727272728,253.9,24.5218371395634)) ;
#102554 = CARTESIAN_POINT('Ctrl Pts',(45.6809871063617,253.75,24.6718371395631)) ;
#102555 = CARTESIAN_POINT('Ctrl Pts',(45.6809474726104,253.75,24.6703790162594)) ;
#102556 = CARTESIAN_POINT('Ctrl Pts',(45.6809079648117,253.750021261236,24.6689209669185)) ;
#102557 = CARTESIAN_POINT('Ctrl Pts',(45.6808685931366,253.750063777237,24.667463456485)) ;
#102558 = CARTESIAN_POINT('Ctrl Pts',(45.6803627963739,253.750609968276,24.6487392325951)) ;
#102559 = CARTESIAN_POINT('Ctrl Pts',(45.679884582305,253.754658837467,24.6302810697321)) ;
#102560 = CARTESIAN_POINT('Ctrl Pts',(45.6794511277464,253.762001431812,24.6130460247761)) ;
#102561 = CARTESIAN_POINT('Ctrl Pts',(45.6789992518938,253.769656077527,24.5950785112738)) ;
#102562 = CARTESIAN_POINT('Ctrl Pts',(45.6786041293905,253.78074710398,24.5787765926027)) ;
#102563 = CARTESIAN_POINT('Ctrl Pts',(45.678277759847,253.794651469056,24.5650584571032)) ;
#102564 = CARTESIAN_POINT('Ctrl Pts',(45.6779514776263,253.808552113907,24.5513439920011)) ;
#102565 = CARTESIAN_POINT('Ctrl Pts',(45.6776998934372,253.824998688613,24.5404743147172)) ;
#102566 = CARTESIAN_POINT('Ctrl Pts',(45.6775294165482,253.843066458683,24.5330618828599)) ;
#102567 = CARTESIAN_POINT('Ctrl Pts',(45.6773589606669,253.861132002274,24.5256503644317)) ;
#102568 = CARTESIAN_POINT('Ctrl Pts',(45.6772727272727,253.880472526098,24.5218371395634)) ;
#102569 = CARTESIAN_POINT('Ctrl Pts',(45.6772727272727,253.9,24.5218371395634)) ;
#102570 = CARTESIAN_POINT('Origin',(45.7,253.9,25.0213203435596)) ;
#102571 = CARTESIAN_POINT('Origin',(42.5869707020053,253.9,24.6718371395634)) ;
#102572 = CARTESIAN_POINT('',(45.1376473638895,253.75,24.6718371395634)) ;
#102573 = CARTESIAN_POINT('',(42.5869707020053,253.75,24.6718371395634)) ;
#102574 = CARTESIAN_POINT('',(45.2754819011524,253.9,24.5218371395634)) ;
#102575 = CARTESIAN_POINT('Ctrl Pts',(45.1376473638895,253.75,24.6718371395634)) ;
#102576 = CARTESIAN_POINT('Ctrl Pts',(45.1381850335709,253.75,24.6712600688988)) ;
#102577 = CARTESIAN_POINT('Ctrl Pts',(45.1387226600695,253.750003330106,24.6706829503216)) ;
#102578 = CARTESIAN_POINT('Ctrl Pts',(45.1531132725535,253.750181671152,24.655232733985)) ;
#102579 = CARTESIAN_POINT('Ctrl Pts',(45.1669867461395,253.752566842488,24.6402737328004)) ;
#102580 = CARTESIAN_POINT('Ctrl Pts',(45.1932346560154,253.761740190968,24.611858434734)) ;
#102581 = CARTESIAN_POINT('Ctrl Pts',(45.2057640785244,253.768377217198,24.5982392280904)) ;
#102582 = CARTESIAN_POINT('Ctrl Pts',(45.2303168022832,253.78721321578,24.5714615581854)) ;
#102583 = CARTESIAN_POINT('Ctrl Pts',(45.2422449580739,253.800023548159,24.5583957973774)) ;
#102584 = CARTESIAN_POINT('Ctrl Pts',(45.2595447243168,253.828041657271,24.5393982820176)) ;
#102585 = CARTESIAN_POINT('Ctrl Pts',(45.2657214856064,253.841958224525,24.5325967432531)) ;
#102586 = CARTESIAN_POINT('Ctrl Pts',(45.2735311811371,253.870954690135,24.5239903075244)) ;
#102587 = CARTESIAN_POINT('Ctrl Pts',(45.2754819011524,253.885320776746,24.5218371395634)) ;
#102588 = CARTESIAN_POINT('Ctrl Pts',(45.2754819011524,253.9,24.5218371395634)) ;
#102589 = CARTESIAN_POINT('',(42.5869707020053,253.9,24.5218371395634)) ;
#102590 = CARTESIAN_POINT('Origin',(40.2,253.9,25.0213203435596)) ;
#102591 = CARTESIAN_POINT('',(45.0039779498781,253.75,23.8278816743835)) ;
#102592 = CARTESIAN_POINT('Origin',(40.2,253.75,25.0213203435596)) ;
#102593 = CARTESIAN_POINT('',(45.1814189338688,253.9,23.9279469374017)) ;
#102594 = CARTESIAN_POINT('Ctrl Pts',(45.0039779498781,253.75,23.8278816743835)) ;
#102595 = CARTESIAN_POINT('Ctrl Pts',(45.0046676287764,253.75,23.8282643521316)) ;
#102596 = CARTESIAN_POINT('Ctrl Pts',(45.0053572814057,253.750003330105,23.8286470887883)) ;
#102597 = CARTESIAN_POINT('Ctrl Pts',(45.0238179465996,253.750181671152,23.8388941738984)) ;
#102598 = CARTESIAN_POINT('Ctrl Pts',(45.0416349896414,253.752566842488,23.8488338903424)) ;
#102599 = CARTESIAN_POINT('Ctrl Pts',(45.0753790453708,253.761740190968,23.8677473945125)) ;
#102600 = CARTESIAN_POINT('Ctrl Pts',(45.0915038005961,253.768377217198,23.8768282252525)) ;
#102601 = CARTESIAN_POINT('Ctrl Pts',(45.12312958359,253.78721321578,23.8947080938071)) ;
#102602 = CARTESIAN_POINT('Ctrl Pts',(45.1385114760162,253.800023548159,23.903448367913)) ;
#102603 = CARTESIAN_POINT('Ctrl Pts',(45.1608350865289,253.828041657271,23.9161701569215)) ;
#102604 = CARTESIAN_POINT('Ctrl Pts',(45.1688113266691,253.841958224525,23.9207300804757)) ;
#102605 = CARTESIAN_POINT('Ctrl Pts',(45.1788983233951,253.870954690135,23.9265019586177)) ;
#102606 = CARTESIAN_POINT('Ctrl Pts',(45.1814189338688,253.885320776746,23.9279469374017)) ;
#102607 = CARTESIAN_POINT('Ctrl Pts',(45.1814189338688,253.9,23.9279469374017)) ;
#102608 = CARTESIAN_POINT('Origin',(40.2,253.9,25.0213203435596)) ;
#102609 = CARTESIAN_POINT('Origin',(42.9125942086827,253.9,24.5074134442792)) ;
#102610 = CARTESIAN_POINT('',(45.5207247525188,253.75,23.6599804602402)) ;
#102611 = CARTESIAN_POINT('',(42.9125942086827,253.75,24.5074134442792)) ;
#102612 = CARTESIAN_POINT('',(45.5635447172382,253.9,23.8037867439466)) ;
#102613 = CARTESIAN_POINT('Ctrl Pts',(45.5207247525188,253.75,23.6599804602402)) ;
#102614 = CARTESIAN_POINT('Ctrl Pts',(45.5211376434623,253.75,23.661379465413)) ;
#102615 = CARTESIAN_POINT('Ctrl Pts',(45.5215506313346,253.750021261236,23.662778361321)) ;
#102616 = CARTESIAN_POINT('Ctrl Pts',(45.5219635821411,253.750063777237,23.6641767026334)) ;
#102617 = CARTESIAN_POINT('Ctrl Pts',(45.5272686442365,253.750609968276,23.6821407975692)) ;
#102618 = CARTESIAN_POINT('Ctrl Pts',(45.5325177216276,253.754658837467,23.6998433299153)) ;
#102619 = CARTESIAN_POINT('Ctrl Pts',(45.5374314036355,253.762001431812,23.716368776554)) ;
#102620 = CARTESIAN_POINT('Ctrl Pts',(45.5425539111805,253.769656077527,23.7335965346699)) ;
#102621 = CARTESIAN_POINT('Ctrl Pts',(45.5472156972587,253.78074710398,23.7492226802186)) ;
#102622 = CARTESIAN_POINT('Ctrl Pts',(45.551144438378,253.794651469056,23.7623702561121)) ;
#102623 = CARTESIAN_POINT('Ctrl Pts',(45.555072128331,253.808552113907,23.7755143142662)) ;
#102624 = CARTESIAN_POINT('Ctrl Pts',(45.5581917725533,253.824998688613,23.7859297354669)) ;
#102625 = CARTESIAN_POINT('Ctrl Pts',(45.5603202068105,253.843066458683,23.7930320573423)) ;
#102626 = CARTESIAN_POINT('Ctrl Pts',(45.5624483787821,253.861132002274,23.8001335040032)) ;
#102627 = CARTESIAN_POINT('Ctrl Pts',(45.5635447172385,253.880472526098,23.8037867439465)) ;
#102628 = CARTESIAN_POINT('Ctrl Pts',(45.5635447172382,253.9,23.8037867439466)) ;
#102629 = CARTESIAN_POINT('',(42.9589467578389,253.9,24.6500719217234)) ;
#102630 = CARTESIAN_POINT('Origin',(45.4308108396234,253.9,23.3217268744974)) ;
#102631 = CARTESIAN_POINT('',(45.3047322539519,253.75,22.9952239032474)) ;
#102632 = CARTESIAN_POINT('Origin',(45.4308108396234,253.75,23.3217268744974)) ;
#102633 = CARTESIAN_POINT('',(45.2548471203588,253.9,22.8537132320653)) ;
#102634 = CARTESIAN_POINT('Ctrl Pts',(45.3047322539504,253.75,22.9952239032429)) ;
#102635 = CARTESIAN_POINT('Ctrl Pts',(45.3042439751329,253.75,22.9938493930776)) ;
#102636 = CARTESIAN_POINT('Ctrl Pts',(45.303755838959,253.750021261236,22.9924749143332)) ;
#102637 = CARTESIAN_POINT('Ctrl Pts',(45.3032679987774,253.750063777237,22.9911009060563)) ;
#102638 = CARTESIAN_POINT('Ctrl Pts',(45.2970008540754,253.750609968276,22.9734494107125)) ;
#102639 = CARTESIAN_POINT('Ctrl Pts',(45.290842159469,253.754658837467,22.9560424309124)) ;
#102640 = CARTESIAN_POINT('Ctrl Pts',(45.2851039978953,253.762001431812,22.9397848739232)) ;
#102641 = CARTESIAN_POINT('Ctrl Pts',(45.2791219714013,253.769656077527,22.9228363904432)) ;
#102642 = CARTESIAN_POINT('Ctrl Pts',(45.2737086176589,253.78074710398,22.9074544440317)) ;
#102643 = CARTESIAN_POINT('Ctrl Pts',(45.2691590847773,253.794651469056,22.8945085756089)) ;
#102644 = CARTESIAN_POINT('Ctrl Pts',(45.2646107691597,253.808552113907,22.8815661709572)) ;
#102645 = CARTESIAN_POINT('Ctrl Pts',(45.2610125833727,253.824998688613,22.8713062373364)) ;
#102646 = CARTESIAN_POINT('Ctrl Pts',(45.2585598828031,253.843066458683,22.8643092759728)) ;
#102647 = CARTESIAN_POINT('Ctrl Pts',(45.2561074844782,253.861132002274,22.85731317684)) ;
#102648 = CARTESIAN_POINT('Ctrl Pts',(45.2548471203588,253.880472526098,22.8537132320654)) ;
#102649 = CARTESIAN_POINT('Ctrl Pts',(45.254847120359,253.9,22.8537132320653)) ;
#102650 = CARTESIAN_POINT('Origin',(45.4308108396234,253.9,23.3217268744974)) ;
#102651 = CARTESIAN_POINT('Origin',(42.3621477910643,253.9,23.9513275530686)) ;
#102652 = CARTESIAN_POINT('',(44.7879854513112,253.75,23.1631251173908)) ;
#102653 = CARTESIAN_POINT('',(42.3621477910643,253.75,23.9513275530686)) ;
#102654 = CARTESIAN_POINT('',(44.8727213369894,253.9,22.9778734255204)) ;
#102655 = CARTESIAN_POINT('Ctrl Pts',(44.7879854513112,253.75,23.1631251173908)) ;
#102656 = CARTESIAN_POINT('Ctrl Pts',(44.788318480923,253.75,23.162410141506)) ;
#102657 = CARTESIAN_POINT('Ctrl Pts',(44.7886514546598,253.750003330106,23.1616951333976)) ;
#102658 = CARTESIAN_POINT('Ctrl Pts',(44.7975633610212,253.750181671152,23.1425541606572)) ;
#102659 = CARTESIAN_POINT('Ctrl Pts',(44.8061352328939,253.752566842488,23.1240401659929)) ;
#102660 = CARTESIAN_POINT('Ctrl Pts',(44.8223176686178,253.761740190968,23.0889045613858)) ;
#102661 = CARTESIAN_POINT('Ctrl Pts',(44.8300252912377,253.768377217198,23.0720801216756)) ;
#102662 = CARTESIAN_POINT('Ctrl Pts',(44.845101564091,253.78721321578,23.0390258353215)) ;
#102663 = CARTESIAN_POINT('Ctrl Pts',(44.8524083722489,253.800023548159,23.0229135555138)) ;
#102664 = CARTESIAN_POINT('Ctrl Pts',(44.8629908725676,253.828041657271,22.9994999229698)) ;
#102665 = CARTESIAN_POINT('Ctrl Pts',(44.8667635305755,253.841958224525,22.9911225509982)) ;
#102666 = CARTESIAN_POINT('Ctrl Pts',(44.8715314574991,253.870954690135,22.9805240155764)) ;
#102667 = CARTESIAN_POINT('Ctrl Pts',(44.8727213369894,253.885320776746,22.9778734255204)) ;
#102668 = CARTESIAN_POINT('Ctrl Pts',(44.8727213369894,253.9,22.9778734255204)) ;
#102669 = CARTESIAN_POINT('',(42.315795241908,253.9,23.8086690756243)) ;
#102670 = CARTESIAN_POINT('Origin',(40.2,253.9,25.0213203435596)) ;
#102671 = CARTESIAN_POINT('',(44.4000617028502,253.75,22.4017818933262)) ;
#102672 = CARTESIAN_POINT('Origin',(40.2,253.75,25.0213203435596)) ;
#102673 = CARTESIAN_POINT('',(44.5997399737516,253.9,22.4421173342227)) ;
#102674 = CARTESIAN_POINT('Ctrl Pts',(44.4000617028502,253.75,22.4017818933262)) ;
#102675 = CARTESIAN_POINT('Ctrl Pts',(44.400835880386,253.75,22.4019327189915)) ;
#102676 = CARTESIAN_POINT('Ctrl Pts',(44.4016100511485,253.750003330106,22.4020836088011)) ;
#102677 = CARTESIAN_POINT('Ctrl Pts',(44.4223337105147,253.750181671152,22.4061245065945)) ;
#102678 = CARTESIAN_POINT('Ctrl Pts',(44.4423502667022,253.752566842488,22.4100719695998)) ;
#102679 = CARTESIAN_POINT('Ctrl Pts',(44.4802873650014,253.761740190968,22.4176322943072)) ;
#102680 = CARTESIAN_POINT('Ctrl Pts',(44.4984290495541,253.768377217198,22.4212858541613)) ;
#102681 = CARTESIAN_POINT('Ctrl Pts',(44.5340321397943,253.78721321578,22.4285177152552)) ;
#102682 = CARTESIAN_POINT('Ctrl Pts',(44.5513620820533,253.800023548159,22.4320769437325)) ;
#102683 = CARTESIAN_POINT('Ctrl Pts',(44.5765243463011,253.828041657271,22.4372777090437)) ;
#102684 = CARTESIAN_POINT('Ctrl Pts',(44.5855192953333,253.841958224525,22.4391496602992)) ;
#102685 = CARTESIAN_POINT('Ctrl Pts',(44.5968962077347,253.870954690135,22.4415219892068)) ;
#102686 = CARTESIAN_POINT('Ctrl Pts',(44.5997399737516,253.885320776746,22.4421173342227)) ;
#102687 = CARTESIAN_POINT('Ctrl Pts',(44.5997399737516,253.9,22.4421173342227)) ;
#102688 = CARTESIAN_POINT('Origin',(40.2,253.9,25.0213203435596)) ;
#102689 = CARTESIAN_POINT('Origin',(42.621024432828,253.9,23.6943281289039)) ;
#102690 = CARTESIAN_POINT('',(44.8396327882296,253.75,22.0824148057166)) ;
#102691 = CARTESIAN_POINT('',(42.621024432828,253.75,23.6943281289039)) ;
#102692 = CARTESIAN_POINT('',(44.9247955802669,253.9,22.2059506121228)) ;
#102693 = CARTESIAN_POINT('Ctrl Pts',(44.8396327882296,253.75,22.0824148057166)) ;
#102694 = CARTESIAN_POINT('Ctrl Pts',(44.8404577872253,253.75,22.0836177483836)) ;
#102695 = CARTESIAN_POINT('Ctrl Pts',(44.8412828446445,253.750021261236,22.0848205571807)) ;
#102696 = CARTESIAN_POINT('Ctrl Pts',(44.8421076954281,253.750063777237,22.086022849981)) ;
#102697 = CARTESIAN_POINT('Ctrl Pts',(44.8527043199125,253.750609968276,22.101468365193)) ;
#102698 = CARTESIAN_POINT('Ctrl Pts',(44.8631668725215,253.754658837467,22.11668241981)) ;
#102699 = CARTESIAN_POINT('Ctrl Pts',(44.8729467056649,253.762001431812,22.1308806422755)) ;
#102700 = CARTESIAN_POINT('Ctrl Pts',(44.8831421698776,253.769656077527,22.1456822720076)) ;
#102701 = CARTESIAN_POINT('Ctrl Pts',(44.8924045364365,253.78074710398,22.1591030484338)) ;
#102702 = CARTESIAN_POINT('Ctrl Pts',(44.9002038156649,253.794651469056,22.1703930883885)) ;
#102703 = CARTESIAN_POINT('Ctrl Pts',(44.9080010081335,253.808552113907,22.1816801076023)) ;
#102704 = CARTESIAN_POINT('Ctrl Pts',(44.9141865082534,253.824998688613,22.1906217387246)) ;
#102705 = CARTESIAN_POINT('Ctrl Pts',(44.9184055076825,253.843066458683,22.1967187258681)) ;
#102706 = CARTESIAN_POINT('Ctrl Pts',(44.9226239872069,253.861132002274,22.2028149616837)) ;
#102707 = CARTESIAN_POINT('Ctrl Pts',(44.9247955802668,253.880472526098,22.2059506121229)) ;
#102708 = CARTESIAN_POINT('Ctrl Pts',(44.9247955802668,253.9,22.2059506121229)) ;
#102709 = CARTESIAN_POINT('',(42.7091922206719,253.9,23.8156806780601)) ;
#102710 = CARTESIAN_POINT('Origin',(44.6495934690622,253.9,21.788501455951)) ;
#102711 = CARTESIAN_POINT('',(44.4287906417638,253.75,21.5169391031533)) ;
#102712 = CARTESIAN_POINT('Origin',(44.6495934690622,253.75,21.788501455951)) ;
#102713 = CARTESIAN_POINT('',(44.3376178581133,253.9,21.3977698112471)) ;
#102714 = CARTESIAN_POINT('Ctrl Pts',(44.4287906417615,253.75,21.5169391031502)) ;
#102715 = CARTESIAN_POINT('Ctrl Pts',(44.4279015140102,253.75,21.5157827527532)) ;
#102716 = CARTESIAN_POINT('Ctrl Pts',(44.4270125316307,253.750021261236,21.5146263881596)) ;
#102717 = CARTESIAN_POINT('Ctrl Pts',(44.4261239761389,253.750063777237,21.5134703795409)) ;
#102718 = CARTESIAN_POINT('Ctrl Pts',(44.4147089552932,253.750609968276,21.4986194640919)) ;
#102719 = CARTESIAN_POINT('Ctrl Pts',(44.4034726360771,253.754658837467,21.4839675838201)) ;
#102720 = CARTESIAN_POINT('Ctrl Pts',(44.3929914587243,253.762001431812,21.4702789177492)) ;
#102721 = CARTESIAN_POINT('Ctrl Pts',(44.3820648440225,253.769656077527,21.4560084999418)) ;
#102722 = CARTESIAN_POINT('Ctrl Pts',(44.3721631558231,253.78074710398,21.4430522178766)) ;
#102723 = CARTESIAN_POINT('Ctrl Pts',(44.3638357995804,253.794651469056,21.4321458483308)) ;
#102724 = CARTESIAN_POINT('Ctrl Pts',(44.3555106713887,253.808552113907,21.4212423968718)) ;
#102725 = CARTESIAN_POINT('Ctrl Pts',(44.3489180994998,253.824998688613,21.4125965207017)) ;
#102726 = CARTESIAN_POINT('Ctrl Pts',(44.3444232626702,253.843066458683,21.4066999411606)) ;
#102727 = CARTESIAN_POINT('Ctrl Pts',(44.3399289797363,253.861132002274,21.4008040882512)) ;
#102728 = CARTESIAN_POINT('Ctrl Pts',(44.3376178581132,253.880472526098,21.3977698112471)) ;
#102729 = CARTESIAN_POINT('Ctrl Pts',(44.3376178581134,253.9,21.397769811247)) ;
#102730 = CARTESIAN_POINT('Origin',(44.6495934690622,253.9,21.788501455951)) ;
#102731 = CARTESIAN_POINT('Origin',(41.9256787897644,253.9,23.3355563159851)) ;
#102732 = CARTESIAN_POINT('',(43.9892195563843,253.75,21.836306190763)) ;
#102733 = CARTESIAN_POINT('',(41.9256787897644,253.75,23.3355563159851)) ;
#102734 = CARTESIAN_POINT('',(44.012562251598,253.9,21.6339365333471)) ;
#102735 = CARTESIAN_POINT('Ctrl Pts',(43.9892195563843,253.75,21.836306190763)) ;
#102736 = CARTESIAN_POINT('Ctrl Pts',(43.9893153466677,253.75,21.8355232964791)) ;
#102737 = CARTESIAN_POINT('Ctrl Pts',(43.9894110738533,253.750003330106,21.8347403888152)) ;
#102738 = CARTESIAN_POINT('Ctrl Pts',(43.9919719146053,253.750181671152,21.8137823114442)) ;
#102739 = CARTESIAN_POINT('Ctrl Pts',(43.9944031102216,253.752566842488,21.7935256020938)) ;
#102740 = CARTESIAN_POINT('Ctrl Pts',(43.9989360222351,253.761740190968,21.7551090087292)) ;
#102741 = CARTESIAN_POINT('Ctrl Pts',(44.0010673691616,253.768377217198,21.7367262293339)) ;
#102742 = CARTESIAN_POINT('Ctrl Pts',(44.0051914204798,253.78721321578,21.7006309103819)) ;
#102743 = CARTESIAN_POINT('Ctrl Pts',(44.007161639713,253.800023548159,21.683049293783)) ;
#102744 = CARTESIAN_POINT('Ctrl Pts',(44.0099909852437,253.828041657271,21.6575114335403)) ;
#102745 = CARTESIAN_POINT('Ctrl Pts',(44.0109902459184,253.841958224525,21.648378263899)) ;
#102746 = CARTESIAN_POINT('Ctrl Pts',(44.0122496863275,253.870954690135,21.6368250872756)) ;
#102747 = CARTESIAN_POINT('Ctrl Pts',(44.012562251598,253.885320776746,21.6339365333471)) ;
#102748 = CARTESIAN_POINT('Ctrl Pts',(44.012562251598,253.9,21.633936533347)) ;
#102749 = CARTESIAN_POINT('',(41.8375110019206,253.9,23.2142037668289)) ;
#102750 = CARTESIAN_POINT('Origin',(40.2,253.9,25.0213203435596)) ;
#102751 = CARTESIAN_POINT('',(43.3850141527966,253.75,21.2321007871753)) ;
#102752 = CARTESIAN_POINT('Origin',(40.2,253.75,25.0213203435596)) ;
#102753 = CARTESIAN_POINT('',(43.5873838102126,253.9,21.2087580919617)) ;
#102754 = CARTESIAN_POINT('Ctrl Pts',(43.3850141527966,253.75,21.2321007871753)) ;
#102755 = CARTESIAN_POINT('Ctrl Pts',(43.3857970470791,253.75,21.2320049968921)) ;
#102756 = CARTESIAN_POINT('Ctrl Pts',(43.3865799547417,253.750003330105,21.2319092697067)) ;
#102757 = CARTESIAN_POINT('Ctrl Pts',(43.4075380321123,253.750181671152,21.2293484289549)) ;
#102758 = CARTESIAN_POINT('Ctrl Pts',(43.4277947414631,253.752566842487,21.2269172333384)) ;
#102759 = CARTESIAN_POINT('Ctrl Pts',(43.4662113348294,253.761740190968,21.2223843213247)) ;
#102760 = CARTESIAN_POINT('Ctrl Pts',(43.4845941142251,253.768377217197,21.2202529743981)) ;
#102761 = CARTESIAN_POINT('Ctrl Pts',(43.5206894331778,253.78721321578,21.2161289230798)) ;
#102762 = CARTESIAN_POINT('Ctrl Pts',(43.5382710497766,253.800023548159,21.2141587038466)) ;
#102763 = CARTESIAN_POINT('Ctrl Pts',(43.5638089100192,253.828041657271,21.211329358316)) ;
#102764 = CARTESIAN_POINT('Ctrl Pts',(43.5729420796606,253.841958224525,21.2103300976412)) ;
#102765 = CARTESIAN_POINT('Ctrl Pts',(43.5844952562841,253.870954690135,21.2090706572321)) ;
#102766 = CARTESIAN_POINT('Ctrl Pts',(43.5873838102126,253.885320776746,21.2087580919617)) ;
#102767 = CARTESIAN_POINT('Ctrl Pts',(43.5873838102126,253.9,21.2087580919617)) ;
#102768 = CARTESIAN_POINT('Origin',(40.2,253.9,25.0213203435596)) ;
#102769 = CARTESIAN_POINT('Origin',(42.0924679172189,253.9,23.0111380571975)) ;
#102770 = CARTESIAN_POINT('',(43.7043812404062,253.75,20.792529701796)) ;
#102771 = CARTESIAN_POINT('',(42.0924679172189,253.75,23.0111380571975)) ;
#102772 = CARTESIAN_POINT('',(43.8235505323125,253.9,20.8837024854464)) ;
#102773 = CARTESIAN_POINT('Ctrl Pts',(43.7043812404062,253.75,20.792529701796)) ;
#102774 = CARTESIAN_POINT('Ctrl Pts',(43.7055375908043,253.75,20.7934188295481)) ;
#102775 = CARTESIAN_POINT('Ctrl Pts',(43.7066939553987,253.750021261236,20.7943078119284)) ;
#102776 = CARTESIAN_POINT('Ctrl Pts',(43.7078499640185,253.750063777237,20.7951963674209)) ;
#102777 = CARTESIAN_POINT('Ctrl Pts',(43.7227008794692,253.750609968276,20.8066113882653)) ;
#102778 = CARTESIAN_POINT('Ctrl Pts',(43.7373527597391,253.754658837467,20.8178477074831)) ;
#102779 = CARTESIAN_POINT('Ctrl Pts',(43.7510414258101,253.762001431812,20.8283288848357)) ;
#102780 = CARTESIAN_POINT('Ctrl Pts',(43.7653118436178,253.769656077527,20.8392554995374)) ;
#102781 = CARTESIAN_POINT('Ctrl Pts',(43.778268125683,253.78074710398,20.8491571877367)) ;
#102782 = CARTESIAN_POINT('Ctrl Pts',(43.7891744952286,253.794651469056,20.8574845439794)) ;
#102783 = CARTESIAN_POINT('Ctrl Pts',(43.8000779466876,253.808552113907,20.8658096721711)) ;
#102784 = CARTESIAN_POINT('Ctrl Pts',(43.8087238228576,253.824998688613,20.8724022440603)) ;
#102785 = CARTESIAN_POINT('Ctrl Pts',(43.8146204023986,253.843066458683,20.87689708089)) ;
#102786 = CARTESIAN_POINT('Ctrl Pts',(43.820516255308,253.861132002274,20.8813913638238)) ;
#102787 = CARTESIAN_POINT('Ctrl Pts',(43.8235505323122,253.880472526098,20.8837024854468)) ;
#102788 = CARTESIAN_POINT('Ctrl Pts',(43.8235505323123,253.9,20.8837024854466)) ;
#102789 = CARTESIAN_POINT('',(42.2138204663752,253.9,23.0993058450414)) ;
#102790 = CARTESIAN_POINT('Origin',(43.4328188876086,253.9,20.5717268744974)) ;
#102791 = CARTESIAN_POINT('',(43.1389055378431,253.75,20.38168755533)) ;
#102792 = CARTESIAN_POINT('Origin',(43.4328188876086,253.75,20.5717268744974)) ;
#102793 = CARTESIAN_POINT('',(43.0153697314369,253.9,20.2965247632928)) ;
#102794 = CARTESIAN_POINT('Ctrl Pts',(43.1389055378404,253.75,20.381687555328)) ;
#102795 = CARTESIAN_POINT('Ctrl Pts',(43.137702595174,253.75,20.3808625563329)) ;
#102796 = CARTESIAN_POINT('Ctrl Pts',(43.1364997863777,253.750021261236,20.3800374989153)) ;
#102797 = CARTESIAN_POINT('Ctrl Pts',(43.1352974935784,253.750063777237,20.3792126481319)) ;
#102798 = CARTESIAN_POINT('Ctrl Pts',(43.1198519783686,253.750609968276,20.3686160236418)) ;
#102799 = CARTESIAN_POINT('Ctrl Pts',(43.1046379237494,253.754658837467,20.3581534710382)) ;
#102800 = CARTESIAN_POINT('Ctrl Pts',(43.0904397012842,253.762001431812,20.3483736378948)) ;
#102801 = CARTESIAN_POINT('Ctrl Pts',(43.075638071552,253.769656077527,20.3381781736819)) ;
#102802 = CARTESIAN_POINT('Ctrl Pts',(43.0622172951261,253.78074710398,20.3289158071227)) ;
#102803 = CARTESIAN_POINT('Ctrl Pts',(43.0509272551714,253.794651469056,20.3211165278944)) ;
#102804 = CARTESIAN_POINT('Ctrl Pts',(43.0396402359575,253.808552113907,20.3133193354259)) ;
#102805 = CARTESIAN_POINT('Ctrl Pts',(43.0306986048352,253.824998688613,20.3071338353061)) ;
#102806 = CARTESIAN_POINT('Ctrl Pts',(43.0246016176917,253.843066458683,20.3029148358772)) ;
#102807 = CARTESIAN_POINT('Ctrl Pts',(43.0185053818759,253.861132002274,20.2986963563528)) ;
#102808 = CARTESIAN_POINT('Ctrl Pts',(43.0153697314369,253.880472526098,20.2965247632927)) ;
#102809 = CARTESIAN_POINT('Ctrl Pts',(43.0153697314369,253.9,20.2965247632927)) ;
#102810 = CARTESIAN_POINT('Origin',(43.4328188876086,253.9,20.5717268744974)) ;
#102811 = CARTESIAN_POINT('Origin',(41.3202883250113,253.9,22.8847994073294)) ;
#102812 = CARTESIAN_POINT('',(42.8195384502335,253.75,20.8212586407095)) ;
#102813 = CARTESIAN_POINT('',(41.3202883250113,253.75,22.8847994073294)) ;
#102814 = CARTESIAN_POINT('',(42.7792030093369,253.9,20.6215803698081)) ;
#102815 = CARTESIAN_POINT('Ctrl Pts',(42.8195384502335,253.75,20.8212586407095)) ;
#102816 = CARTESIAN_POINT('Ctrl Pts',(42.8193876245682,253.75,20.8204844631737)) ;
#102817 = CARTESIAN_POINT('Ctrl Pts',(42.8192367347586,253.750003330106,20.8197102924112)) ;
#102818 = CARTESIAN_POINT('Ctrl Pts',(42.8151958369649,253.750181671152,20.7989866330446)) ;
#102819 = CARTESIAN_POINT('Ctrl Pts',(42.8112483739597,253.752566842488,20.7789700768574)) ;
#102820 = CARTESIAN_POINT('Ctrl Pts',(42.8036880492523,253.761740190968,20.7410329785579)) ;
#102821 = CARTESIAN_POINT('Ctrl Pts',(42.8000344893984,253.768377217198,20.7228912940054)) ;
#102822 = CARTESIAN_POINT('Ctrl Pts',(42.7928026283045,253.78721321578,20.6872882037656)) ;
#102823 = CARTESIAN_POINT('Ctrl Pts',(42.7892433998272,253.800023548159,20.6699582615064)) ;
#102824 = CARTESIAN_POINT('Ctrl Pts',(42.7840426345159,253.828041657271,20.6447959972585)) ;
#102825 = CARTESIAN_POINT('Ctrl Pts',(42.7821706832604,253.841958224525,20.6358010482263)) ;
#102826 = CARTESIAN_POINT('Ctrl Pts',(42.7797983543528,253.870954690135,20.6244241358249)) ;
#102827 = CARTESIAN_POINT('Ctrl Pts',(42.7792030093369,253.885320776746,20.6215803698081)) ;
#102828 = CARTESIAN_POINT('Ctrl Pts',(42.7792030093369,253.9,20.6215803698081)) ;
#102829 = CARTESIAN_POINT('',(41.1989357758551,253.9,22.7966316194855)) ;
#102830 = CARTESIAN_POINT('Origin',(40.2,253.9,25.0213203435596)) ;
#102831 = CARTESIAN_POINT('',(42.0581952261689,253.75,20.4333348922484)) ;
#102832 = CARTESIAN_POINT('Origin',(40.2,253.75,25.0213203435596)) ;
#102833 = CARTESIAN_POINT('',(42.2434469180392,253.9,20.3485990065702)) ;
#102834 = CARTESIAN_POINT('Ctrl Pts',(42.0581952261685,253.75,20.4333348922483)) ;
#102835 = CARTESIAN_POINT('Ctrl Pts',(42.0589102020531,253.75,20.4330018626366)) ;
#102836 = CARTESIAN_POINT('Ctrl Pts',(42.0596252101622,253.750003330106,20.4326688888998)) ;
#102837 = CARTESIAN_POINT('Ctrl Pts',(42.0787661829037,253.750181671152,20.4237569825383)) ;
#102838 = CARTESIAN_POINT('Ctrl Pts',(42.0972801775669,253.752566842488,20.4151851106656)) ;
#102839 = CARTESIAN_POINT('Ctrl Pts',(42.132415782174,253.761740190968,20.3990026749418)) ;
#102840 = CARTESIAN_POINT('Ctrl Pts',(42.1492402218842,253.768377217198,20.3912950523219)) ;
#102841 = CARTESIAN_POINT('Ctrl Pts',(42.1822945082381,253.78721321578,20.3762187794687)) ;
#102842 = CARTESIAN_POINT('Ctrl Pts',(42.1984067880458,253.800023548159,20.3689119713107)) ;
#102843 = CARTESIAN_POINT('Ctrl Pts',(42.2218204205899,253.828041657271,20.3583294709921)) ;
#102844 = CARTESIAN_POINT('Ctrl Pts',(42.2301977925614,253.841958224525,20.3545568129842)) ;
#102845 = CARTESIAN_POINT('Ctrl Pts',(42.2407963279832,253.870954690135,20.3497888860605)) ;
#102846 = CARTESIAN_POINT('Ctrl Pts',(42.2434469180392,253.885320776746,20.3485990065702)) ;
#102847 = CARTESIAN_POINT('Ctrl Pts',(42.2434469180392,253.9,20.3485990065702)) ;
#102848 = CARTESIAN_POINT('Origin',(40.2,253.9,25.0213203435596)) ;
#102849 = CARTESIAN_POINT('Origin',(41.3786634562732,253.9,22.5247186334439)) ;
#102850 = CARTESIAN_POINT('',(42.3676071114944,253.9,19.9664732232009)) ;
#102851 = CARTESIAN_POINT('',(41.5213219337175,253.9,22.5710711826001)) ;
#102852 = CARTESIAN_POINT('',(42.2260964403123,253.75,19.9165880896075)) ;
#102853 = CARTESIAN_POINT('',(41.3786634562732,253.75,22.5247186334439)) ;
#102854 = CARTESIAN_POINT('Ctrl Pts',(42.2260964403123,253.75,19.9165880896075)) ;
#102855 = CARTESIAN_POINT('Ctrl Pts',(42.2274709504793,253.75,19.9170763684256)) ;
#102856 = CARTESIAN_POINT('Ctrl Pts',(42.2288454292246,253.750021261236,19.9175645046006)) ;
#102857 = CARTESIAN_POINT('Ctrl Pts',(42.2302194375034,253.750063777237,19.9180523447822)) ;
#102858 = CARTESIAN_POINT('Ctrl Pts',(42.2478709328509,253.750609968276,19.9243194894782)) ;
#102859 = CARTESIAN_POINT('Ctrl Pts',(42.2652779126467,253.754658837467,19.9304781840933)) ;
#102860 = CARTESIAN_POINT('Ctrl Pts',(42.2815354696358,253.762001431812,19.9362163456661)) ;
#102861 = CARTESIAN_POINT('Ctrl Pts',(42.298483953116,253.769656077527,19.9421983721592)) ;
#102862 = CARTESIAN_POINT('Ctrl Pts',(42.3138658995279,253.78074710398,19.947611725901)) ;
#102863 = CARTESIAN_POINT('Ctrl Pts',(42.3268117679507,253.794651469056,19.9521612587826)) ;
#102864 = CARTESIAN_POINT('Ctrl Pts',(42.3397541726024,253.808552113907,19.9567095744001)) ;
#102865 = CARTESIAN_POINT('Ctrl Pts',(42.3500141062233,253.824998688613,19.9603077601869)) ;
#102866 = CARTESIAN_POINT('Ctrl Pts',(42.3570110675869,253.843066458683,19.9627604607566)) ;
#102867 = CARTESIAN_POINT('Ctrl Pts',(42.3640071667196,253.861132002274,19.9652128590817)) ;
#102868 = CARTESIAN_POINT('Ctrl Pts',(42.3676071114944,253.880472526098,19.9664732232006)) ;
#102869 = CARTESIAN_POINT('Ctrl Pts',(42.3676071114945,253.9,19.9664732232005)) ;
#102870 = CARTESIAN_POINT('Origin',(41.8995934690622,253.9,19.7905095039363)) ;
#102871 = CARTESIAN_POINT('',(41.4175335996131,253.9,19.6577756263215)) ;
#102872 = CARTESIAN_POINT('Origin',(41.8995934690622,253.9,19.7905095039363)) ;
#102873 = CARTESIAN_POINT('',(41.5613398833193,253.75,19.7005955910415)) ;
#102874 = CARTESIAN_POINT('Origin',(41.8995934690622,253.75,19.7905095039363)) ;
#102875 = CARTESIAN_POINT('Ctrl Pts',(41.5613398833094,253.75,19.7005955910383)) ;
#102876 = CARTESIAN_POINT('Ctrl Pts',(41.5599408781403,253.75,19.7001827000958)) ;
#102877 = CARTESIAN_POINT('Ctrl Pts',(41.5585419822356,253.750021261236,19.699769712222)) ;
#102878 = CARTESIAN_POINT('Ctrl Pts',(41.5571436409267,253.750063777237,19.6993567614174)) ;
#102879 = CARTESIAN_POINT('Ctrl Pts',(41.5391795459882,253.750609968276,19.694051699333)) ;
#102880 = CARTESIAN_POINT('Ctrl Pts',(41.521477013645,253.754658837467,19.6888026219303)) ;
#102881 = CARTESIAN_POINT('Ctrl Pts',(41.5049515670061,253.762001431812,19.683888939923)) ;
#102882 = CARTESIAN_POINT('Ctrl Pts',(41.4877238088899,253.769656077527,19.6787664323788)) ;
#102883 = CARTESIAN_POINT('Ctrl Pts',(41.4720976633411,253.78074710398,19.6741046463012)) ;
#102884 = CARTESIAN_POINT('Ctrl Pts',(41.4589500874475,253.794651469056,19.6701759051819)) ;
#102885 = CARTESIAN_POINT('Ctrl Pts',(41.4458060292935,253.808552113907,19.6662482152289)) ;
#102886 = CARTESIAN_POINT('Ctrl Pts',(41.4353906080927,253.824998688613,19.6631285710069)) ;
#102887 = CARTESIAN_POINT('Ctrl Pts',(41.4282882862173,253.843066458683,19.6610001367495)) ;
#102888 = CARTESIAN_POINT('Ctrl Pts',(41.4211868395564,253.861132002274,19.6588719647777)) ;
#102889 = CARTESIAN_POINT('Ctrl Pts',(41.4175335996131,253.880472526098,19.6577756263216)) ;
#102890 = CARTESIAN_POINT('Ctrl Pts',(41.4175335996131,253.9,19.6577756263216)) ;
#102891 = CARTESIAN_POINT('Origin',(40.6052362334984,253.9,22.6431800539285)) ;
#102892 = CARTESIAN_POINT('',(41.2933734061579,253.9,20.0399014096908)) ;
#102893 = CARTESIAN_POINT('',(40.4625777560541,253.9,22.5968275047722)) ;
#102894 = CARTESIAN_POINT('',(41.3934386691762,253.75,20.2173423936815)) ;
#102895 = CARTESIAN_POINT('',(40.6052362334984,253.75,22.6431800539285)) ;
#102896 = CARTESIAN_POINT('Ctrl Pts',(41.3934386691762,253.75,20.2173423936815)) ;
#102897 = CARTESIAN_POINT('Ctrl Pts',(41.3930559914292,253.75,20.2166527147851)) ;
#102898 = CARTESIAN_POINT('Ctrl Pts',(41.3926732547703,253.750003330106,20.2159630621521)) ;
#102899 = CARTESIAN_POINT('Ctrl Pts',(41.3824261696622,253.750181671152,20.197502396961)) ;
#102900 = CARTESIAN_POINT('Ctrl Pts',(41.3724864532176,253.752566842488,20.1796853539185)) ;
#102901 = CARTESIAN_POINT('Ctrl Pts',(41.3535729490475,253.761740190968,20.1459412981892)) ;
#102902 = CARTESIAN_POINT('Ctrl Pts',(41.3444921183073,253.768377217198,20.1298165429637)) ;
#102903 = CARTESIAN_POINT('Ctrl Pts',(41.3266122497526,253.78721321578,20.0981907599697)) ;
#102904 = CARTESIAN_POINT('Ctrl Pts',(41.3178719756466,253.800023548159,20.0828088675435)) ;
#102905 = CARTESIAN_POINT('Ctrl Pts',(41.3051501866381,253.828041657271,20.0604852570307)) ;
#102906 = CARTESIAN_POINT('Ctrl Pts',(41.3005902630839,253.841958224525,20.0525090168905)) ;
#102907 = CARTESIAN_POINT('Ctrl Pts',(41.294818384942,253.870954690135,20.0424220201646)) ;
#102908 = CARTESIAN_POINT('Ctrl Pts',(41.2933734061579,253.885320776746,20.0399014096908)) ;
#102909 = CARTESIAN_POINT('Ctrl Pts',(41.2933734061579,253.9,20.0399014096908)) ;
#102910 = CARTESIAN_POINT('Origin',(40.2,253.9,25.0213203435596)) ;
#102911 = CARTESIAN_POINT('',(40.6994832039963,253.9,19.9458384424072)) ;
#102912 = CARTESIAN_POINT('Origin',(40.2,253.9,25.0213203435596)) ;
#102913 = CARTESIAN_POINT('',(40.5494832039963,253.75,20.0836729796702)) ;
#102914 = CARTESIAN_POINT('Origin',(40.2,253.75,25.0213203435596)) ;
#102915 = CARTESIAN_POINT('Ctrl Pts',(40.5494832039963,253.75,20.0836729796702)) ;
#102916 = CARTESIAN_POINT('Ctrl Pts',(40.5500602746619,253.75,20.0831353099878)) ;
#102917 = CARTESIAN_POINT('Ctrl Pts',(40.5506373932401,253.750003330106,20.0825976834882)) ;
#102918 = CARTESIAN_POINT('Ctrl Pts',(40.5660876095772,253.750181671152,20.0682070710039)) ;
#102919 = CARTESIAN_POINT('Ctrl Pts',(40.5810466107612,253.752566842488,20.0543335974184)) ;
#102920 = CARTESIAN_POINT('Ctrl Pts',(40.6094619088267,253.761740190969,20.0280856875433)) ;
#102921 = CARTESIAN_POINT('Ctrl Pts',(40.6230811154698,253.768377217198,20.0155562650348)) ;
#102922 = CARTESIAN_POINT('Ctrl Pts',(40.6498587853742,253.78721321578,19.9910035412764)) ;
#102923 = CARTESIAN_POINT('Ctrl Pts',(40.6629245461823,253.800023548159,19.9790753854858)) ;
#102924 = CARTESIAN_POINT('Ctrl Pts',(40.681922061542,253.828041657271,19.9617756192428)) ;
#102925 = CARTESIAN_POINT('Ctrl Pts',(40.6887236003065,253.841958224525,19.9555988579533)) ;
#102926 = CARTESIAN_POINT('Ctrl Pts',(40.6973300360353,253.870954690135,19.9477891624225)) ;
#102927 = CARTESIAN_POINT('Ctrl Pts',(40.6994832039963,253.885320776746,19.9458384424072)) ;
#102928 = CARTESIAN_POINT('Ctrl Pts',(40.6994832039963,253.9,19.9458384424072)) ;
#102929 = CARTESIAN_POINT('Origin',(40.5494832039963,253.9,22.2826839799233)) ;
#102930 = CARTESIAN_POINT('',(40.6994832039963,253.9,19.5440476162869)) ;
#102931 = CARTESIAN_POINT('',(40.6994832039963,253.9,22.2826839799233)) ;
#102932 = CARTESIAN_POINT('',(40.5494832039963,253.75,19.5403332371978)) ;
#102933 = CARTESIAN_POINT('',(40.5494832039963,253.75,22.2826839799233)) ;
#102934 = CARTESIAN_POINT('Ctrl Pts',(40.5494832039963,253.75,19.5403332371978)) ;
#102935 = CARTESIAN_POINT('Ctrl Pts',(40.5509413273001,253.75,19.5403728709491)) ;
#102936 = CARTESIAN_POINT('Ctrl Pts',(40.5523993766411,253.750021261236,19.5404123787478)) ;
#102937 = CARTESIAN_POINT('Ctrl Pts',(40.5538568870747,253.750063777237,19.5404517504229)) ;
#102938 = CARTESIAN_POINT('Ctrl Pts',(40.5725811109644,253.750609968276,19.5409575471863)) ;
#102939 = CARTESIAN_POINT('Ctrl Pts',(40.5910392738275,253.754658837467,19.5414357612545)) ;
#102940 = CARTESIAN_POINT('Ctrl Pts',(40.6082743187835,253.762001431812,19.5418692158132)) ;
#102941 = CARTESIAN_POINT('Ctrl Pts',(40.626241832286,253.769656077527,19.5423210916659)) ;
#102942 = CARTESIAN_POINT('Ctrl Pts',(40.642543750957,253.78074710398,19.5427162141691)) ;
#102943 = CARTESIAN_POINT('Ctrl Pts',(40.6562618864565,253.794651469056,19.5430425837128)) ;
#102944 = CARTESIAN_POINT('Ctrl Pts',(40.6699763515586,253.808552113907,19.5433688659336)) ;
#102945 = CARTESIAN_POINT('Ctrl Pts',(40.6808460288425,253.824998688613,19.5436204501224)) ;
#102946 = CARTESIAN_POINT('Ctrl Pts',(40.6882584606999,253.843066458683,19.5437909270114)) ;
#102947 = CARTESIAN_POINT('Ctrl Pts',(40.695669979128,253.861132002274,19.5439613828926)) ;
#102948 = CARTESIAN_POINT('Ctrl Pts',(40.6994832039963,253.880472526098,19.5440476162869)) ;
#102949 = CARTESIAN_POINT('Ctrl Pts',(40.6994832039963,253.9,19.5440476162869)) ;
#102950 = CARTESIAN_POINT('Origin',(40.2,253.9,19.5213203435596)) ;
#102951 = CARTESIAN_POINT('',(39.7005167960037,253.9,19.5440476162869)) ;
#102952 = CARTESIAN_POINT('Origin',(40.2,253.9,19.5213203435596)) ;
#102953 = CARTESIAN_POINT('',(39.8505167960037,253.75,19.5403332371979)) ;
#102954 = CARTESIAN_POINT('Origin',(40.2,253.75,19.5213203435596)) ;
#102955 = CARTESIAN_POINT('Ctrl Pts',(39.8505167960037,253.75,19.5403332371979)) ;
#102956 = CARTESIAN_POINT('Ctrl Pts',(39.8490586726999,253.75,19.5403728709491)) ;
#102957 = CARTESIAN_POINT('Ctrl Pts',(39.8476006233589,253.750021261236,19.5404123787479)) ;
#102958 = CARTESIAN_POINT('Ctrl Pts',(39.8461431129253,253.750063777237,19.540451750423)) ;
#102959 = CARTESIAN_POINT('Ctrl Pts',(39.8274188890355,253.750609968276,19.5409575471857)) ;
#102960 = CARTESIAN_POINT('Ctrl Pts',(39.8089607261725,253.754658837467,19.5414357612546)) ;
#102961 = CARTESIAN_POINT('Ctrl Pts',(39.7917256812165,253.762001431812,19.5418692158132)) ;
#102962 = CARTESIAN_POINT('Ctrl Pts',(39.773758167714,253.769656077527,19.5423210916658)) ;
#102963 = CARTESIAN_POINT('Ctrl Pts',(39.757456249043,253.78074710398,19.5427162141691)) ;
#102964 = CARTESIAN_POINT('Ctrl Pts',(39.7437381135436,253.794651469056,19.5430425837128)) ;
#102965 = CARTESIAN_POINT('Ctrl Pts',(39.7300236484415,253.808552113907,19.5433688659337)) ;
#102966 = CARTESIAN_POINT('Ctrl Pts',(39.7191539711575,253.824998688613,19.5436204501225)) ;
#102967 = CARTESIAN_POINT('Ctrl Pts',(39.7117415393002,253.843066458683,19.5437909270115)) ;
#102968 = CARTESIAN_POINT('Ctrl Pts',(39.704330020872,253.861132002274,19.5439613828928)) ;
#102969 = CARTESIAN_POINT('Ctrl Pts',(39.7005167960037,253.880472526098,19.5440476162869)) ;
#102970 = CARTESIAN_POINT('Ctrl Pts',(39.7005167960037,253.9,19.5440476162869)) ;
#102971 = CARTESIAN_POINT('Origin',(39.8505167960037,253.9,22.6343496415544)) ;
#102972 = CARTESIAN_POINT('',(39.7005167960037,253.9,19.9458384424072)) ;
#102973 = CARTESIAN_POINT('',(39.7005167960037,253.9,22.6343496415544)) ;
#102974 = CARTESIAN_POINT('',(39.8505167960037,253.75,20.0836729796702)) ;
#102975 = CARTESIAN_POINT('',(39.8505167960037,253.75,22.6343496415544)) ;
#102976 = CARTESIAN_POINT('Ctrl Pts',(39.8505167960037,253.75,20.0836729796702)) ;
#102977 = CARTESIAN_POINT('Ctrl Pts',(39.8499397253381,253.75,20.0831353099878)) ;
#102978 = CARTESIAN_POINT('Ctrl Pts',(39.8493626067599,253.750003330106,20.0825976834882)) ;
#102979 = CARTESIAN_POINT('Ctrl Pts',(39.833912390423,253.750181671152,20.0682070710039)) ;
#102980 = CARTESIAN_POINT('Ctrl Pts',(39.8189533892388,253.752566842488,20.0543335974184)) ;
#102981 = CARTESIAN_POINT('Ctrl Pts',(39.7905380911733,253.761740190969,20.0280856875433)) ;
#102982 = CARTESIAN_POINT('Ctrl Pts',(39.7769188845303,253.768377217198,20.0155562650348)) ;
#102983 = CARTESIAN_POINT('Ctrl Pts',(39.7501412146258,253.78721321578,19.9910035412764)) ;
#102984 = CARTESIAN_POINT('Ctrl Pts',(39.7370754538178,253.800023548159,19.9790753854858)) ;
#102985 = CARTESIAN_POINT('Ctrl Pts',(39.718077938458,253.828041657271,19.9617756192428)) ;
#102986 = CARTESIAN_POINT('Ctrl Pts',(39.7112763996935,253.841958224525,19.9555988579533)) ;
#102987 = CARTESIAN_POINT('Ctrl Pts',(39.7026699639648,253.870954690135,19.9477891624225)) ;
#102988 = CARTESIAN_POINT('Ctrl Pts',(39.7005167960037,253.885320776746,19.9458384424072)) ;
#102989 = CARTESIAN_POINT('Ctrl Pts',(39.7005167960037,253.9,19.9458384424072)) ;
#102990 = CARTESIAN_POINT('Origin',(40.2,253.9,25.0213203435596)) ;
#102991 = CARTESIAN_POINT('',(39.1066265938421,253.9,20.0399014096908)) ;
#102992 = CARTESIAN_POINT('Origin',(40.2,253.9,25.0213203435596)) ;
#102993 = CARTESIAN_POINT('',(39.0065613308239,253.75,20.2173423936815)) ;
#102994 = CARTESIAN_POINT('Origin',(40.2,253.75,25.0213203435596)) ;
#102995 = CARTESIAN_POINT('Ctrl Pts',(39.0065613308239,253.75,20.2173423936815)) ;
#102996 = CARTESIAN_POINT('Ctrl Pts',(39.0069440085716,253.75,20.2166527147839)) ;
#102997 = CARTESIAN_POINT('Ctrl Pts',(39.0073267452311,253.750003330106,20.2159630621497)) ;
#102998 = CARTESIAN_POINT('Ctrl Pts',(39.0175738303395,253.750181671152,20.197502396958)) ;
#102999 = CARTESIAN_POINT('Ctrl Pts',(39.0275135467838,253.752566842488,20.1796853539161)) ;
#103000 = CARTESIAN_POINT('Ctrl Pts',(39.0464270509533,253.761740190969,20.1459412981879)) ;
#103001 = CARTESIAN_POINT('Ctrl Pts',(39.0555078816931,253.768377217198,20.1298165429631)) ;
#103002 = CARTESIAN_POINT('Ctrl Pts',(39.0733877502474,253.78721321578,20.0981907599697)) ;
#103003 = CARTESIAN_POINT('Ctrl Pts',(39.0821280243534,253.800023548159,20.0828088675435)) ;
#103004 = CARTESIAN_POINT('Ctrl Pts',(39.0948498133619,253.828041657271,20.0604852570307)) ;
#103005 = CARTESIAN_POINT('Ctrl Pts',(39.0994097369161,253.841958224525,20.0525090168905)) ;
#103006 = CARTESIAN_POINT('Ctrl Pts',(39.1051816150581,253.870954690135,20.0424220201645)) ;
#103007 = CARTESIAN_POINT('Ctrl Pts',(39.1066265938421,253.885320776746,20.0399014096908)) ;
#103008 = CARTESIAN_POINT('Ctrl Pts',(39.1066265938421,253.9,20.0399014096908)) ;
#103009 = CARTESIAN_POINT('Origin',(39.6860931007195,253.9,22.3087261348769)) ;
#103010 = CARTESIAN_POINT('',(38.982466400387,253.9,19.6577756263215)) ;
#103011 = CARTESIAN_POINT('',(39.8287515781638,253.9,22.2623735857207)) ;
#103012 = CARTESIAN_POINT('',(38.8386601166806,253.75,19.7005955910409)) ;
#103013 = CARTESIAN_POINT('',(39.6860931007195,253.75,22.3087261348769)) ;
#103014 = CARTESIAN_POINT('Ctrl Pts',(38.8386601166806,253.75,19.7005955910409)) ;
#103015 = CARTESIAN_POINT('Ctrl Pts',(38.840059121853,253.75,19.7001827000975)) ;
#103016 = CARTESIAN_POINT('Ctrl Pts',(38.841458017761,253.750021261236,19.6997697122226)) ;
#103017 = CARTESIAN_POINT('Ctrl Pts',(38.8428563590732,253.750063777237,19.6993567614171)) ;
#103018 = CARTESIAN_POINT('Ctrl Pts',(38.8608204540116,253.750609968276,19.6940516993336)) ;
#103019 = CARTESIAN_POINT('Ctrl Pts',(38.8785229863551,253.754658837467,19.6888026219308)) ;
#103020 = CARTESIAN_POINT('Ctrl Pts',(38.8950484329941,253.762001431812,19.6838889399233)) ;
#103021 = CARTESIAN_POINT('Ctrl Pts',(38.9122761911102,253.769656077527,19.6787664323789)) ;
#103022 = CARTESIAN_POINT('Ctrl Pts',(38.9279023366589,253.78074710398,19.6741046463011)) ;
#103023 = CARTESIAN_POINT('Ctrl Pts',(38.9410499125525,253.794651469056,19.6701759051817)) ;
#103024 = CARTESIAN_POINT('Ctrl Pts',(38.9541939707065,253.808552113907,19.6662482152286)) ;
#103025 = CARTESIAN_POINT('Ctrl Pts',(38.9646093919074,253.824998688613,19.6631285710068)) ;
#103026 = CARTESIAN_POINT('Ctrl Pts',(38.9717117137827,253.843066458683,19.6610001367494)) ;
#103027 = CARTESIAN_POINT('Ctrl Pts',(38.9788131604436,253.861132002274,19.6588719647776)) ;
#103028 = CARTESIAN_POINT('Ctrl Pts',(38.9824664003869,253.880472526098,19.6577756263214)) ;
#103029 = CARTESIAN_POINT('Ctrl Pts',(38.9824664003869,253.9,19.6577756263214)) ;
#103030 = CARTESIAN_POINT('Origin',(38.5004065309378,253.9,19.7905095039363)) ;
#103031 = CARTESIAN_POINT('',(38.0323928885057,253.9,19.9664732232009)) ;
#103032 = CARTESIAN_POINT('Origin',(38.5004065309378,253.9,19.7905095039363)) ;
#103033 = CARTESIAN_POINT('',(38.173903559688,253.75,19.9165880896082)) ;
#103034 = CARTESIAN_POINT('Origin',(38.5004065309378,253.75,19.7905095039363)) ;
#103035 = CARTESIAN_POINT('Ctrl Pts',(38.1739035596861,253.75,19.9165880896088)) ;
#103036 = CARTESIAN_POINT('Ctrl Pts',(38.1725290495197,253.75,19.9170763684267)) ;
#103037 = CARTESIAN_POINT('Ctrl Pts',(38.1711545707748,253.750021261236,19.917564504601)) ;
#103038 = CARTESIAN_POINT('Ctrl Pts',(38.1697805624967,253.750063777237,19.9180523447824)) ;
#103039 = CARTESIAN_POINT('Ctrl Pts',(38.1521290671492,253.750609968276,19.9243194894788)) ;
#103040 = CARTESIAN_POINT('Ctrl Pts',(38.1347220873535,253.754658837467,19.9304781840937)) ;
#103041 = CARTESIAN_POINT('Ctrl Pts',(38.1184645303644,253.762001431812,19.9362163456665)) ;
#103042 = CARTESIAN_POINT('Ctrl Pts',(38.1015160468842,253.769656077527,19.9421983721597)) ;
#103043 = CARTESIAN_POINT('Ctrl Pts',(38.0861341004723,253.78074710398,19.9476117259015)) ;
#103044 = CARTESIAN_POINT('Ctrl Pts',(38.0731882320495,253.794651469056,19.952161258783)) ;
#103045 = CARTESIAN_POINT('Ctrl Pts',(38.0602458273978,253.808552113907,19.9567095744005)) ;
#103046 = CARTESIAN_POINT('Ctrl Pts',(38.0499858937768,253.824998688613,19.960307760187)) ;
#103047 = CARTESIAN_POINT('Ctrl Pts',(38.0429889324131,253.843066458683,19.9627604607567)) ;
#103048 = CARTESIAN_POINT('Ctrl Pts',(38.0359928332805,253.861132002274,19.9652128590818)) ;
#103049 = CARTESIAN_POINT('Ctrl Pts',(38.0323928885057,253.880472526098,19.966473223201)) ;
#103050 = CARTESIAN_POINT('Ctrl Pts',(38.0323928885057,253.9,19.9664732232009)) ;
#103051 = CARTESIAN_POINT('Origin',(39.1300072095089,253.9,22.8591725524954)) ;
#103052 = CARTESIAN_POINT('',(38.1565530819608,253.9,20.3485990065702)) ;
#103053 = CARTESIAN_POINT('',(38.9873487320647,253.9,22.9055251016516)) ;
#103054 = CARTESIAN_POINT('',(38.3418047738312,253.75,20.4333348922484)) ;
#103055 = CARTESIAN_POINT('',(39.1300072095089,253.75,22.8591725524954)) ;
#103056 = CARTESIAN_POINT('Ctrl Pts',(38.3418047738312,253.75,20.4333348922484)) ;
#103057 = CARTESIAN_POINT('Ctrl Pts',(38.3410897979451,253.75,20.4330018626361)) ;
#103058 = CARTESIAN_POINT('Ctrl Pts',(38.3403747898355,253.750003330106,20.4326688888987)) ;
#103059 = CARTESIAN_POINT('Ctrl Pts',(38.3212338170932,253.750181671152,20.4237569825369)) ;
#103060 = CARTESIAN_POINT('Ctrl Pts',(38.3027198224307,253.752566842488,20.4151851106646)) ;
#103061 = CARTESIAN_POINT('Ctrl Pts',(38.2675842178248,253.761740190969,20.3990026749412)) ;
#103062 = CARTESIAN_POINT('Ctrl Pts',(38.2507597781153,253.768377217198,20.3912950523217)) ;
#103063 = CARTESIAN_POINT('Ctrl Pts',(38.2177054917619,253.78721321578,20.3762187794687)) ;
#103064 = CARTESIAN_POINT('Ctrl Pts',(38.2015932119542,253.800023548159,20.3689119713107)) ;
#103065 = CARTESIAN_POINT('Ctrl Pts',(38.1781795794102,253.828041657271,20.3583294709921)) ;
#103066 = CARTESIAN_POINT('Ctrl Pts',(38.1698022074386,253.841958224525,20.3545568129842)) ;
#103067 = CARTESIAN_POINT('Ctrl Pts',(38.1592036720168,253.870954690135,20.3497888860605)) ;
#103068 = CARTESIAN_POINT('Ctrl Pts',(38.1565530819608,253.885320776746,20.3485990065702)) ;
#103069 = CARTESIAN_POINT('Ctrl Pts',(38.1565530819608,253.9,20.3485990065702)) ;
#103070 = CARTESIAN_POINT('Origin',(40.2,253.9,25.0213203435596)) ;
#103071 = CARTESIAN_POINT('',(37.6207969906631,253.9,20.6215803698081)) ;
#103072 = CARTESIAN_POINT('Origin',(40.2,253.9,25.0213203435596)) ;
#103073 = CARTESIAN_POINT('',(37.5804615497666,253.75,20.8212586407095)) ;
#103074 = CARTESIAN_POINT('Origin',(40.2,253.75,25.0213203435596)) ;
#103075 = CARTESIAN_POINT('Ctrl Pts',(37.5804615497666,253.75,20.8212586407095)) ;
#103076 = CARTESIAN_POINT('Ctrl Pts',(37.5806123754316,253.75,20.8204844631751)) ;
#103077 = CARTESIAN_POINT('Ctrl Pts',(37.5807632652409,253.750003330105,20.8197102924139)) ;
#103078 = CARTESIAN_POINT('Ctrl Pts',(37.5848041630341,253.750181671152,20.7989866330484)) ;
#103079 = CARTESIAN_POINT('Ctrl Pts',(37.5887516260398,253.752566842487,20.7789700768601)) ;
#103080 = CARTESIAN_POINT('Ctrl Pts',(37.5963119507474,253.761740190968,20.7410329785595)) ;
#103081 = CARTESIAN_POINT('Ctrl Pts',(37.5999655106015,253.768377217197,20.7228912940061)) ;
#103082 = CARTESIAN_POINT('Ctrl Pts',(37.6071973716955,253.78721321578,20.6872882037654)) ;
#103083 = CARTESIAN_POINT('Ctrl Pts',(37.6107566001728,253.800023548159,20.6699582615064)) ;
#103084 = CARTESIAN_POINT('Ctrl Pts',(37.615957365484,253.828041657271,20.6447959972585)) ;
#103085 = CARTESIAN_POINT('Ctrl Pts',(37.6178293167396,253.841958224525,20.6358010482263)) ;
#103086 = CARTESIAN_POINT('Ctrl Pts',(37.6202016456472,253.870954690135,20.6244241358249)) ;
#103087 = CARTESIAN_POINT('Ctrl Pts',(37.6207969906631,253.885320776746,20.6215803698081)) ;
#103088 = CARTESIAN_POINT('Ctrl Pts',(37.6207969906631,253.9,20.6215803698081)) ;
#103089 = CARTESIAN_POINT('Origin',(38.8730077853443,253.9,22.6002959107317)) ;
#103090 = CARTESIAN_POINT('',(37.3846302685632,253.9,20.2965247632928)) ;
#103091 = CARTESIAN_POINT('',(38.9943603345005,253.9,22.5121281228878)) ;
#103092 = CARTESIAN_POINT('',(37.2610944621568,253.75,20.3816875553298)) ;
#103093 = CARTESIAN_POINT('',(38.8730077853443,253.75,22.6002959107317)) ;
#103094 = CARTESIAN_POINT('Ctrl Pts',(37.2610944621568,253.75,20.3816875553298)) ;
#103095 = CARTESIAN_POINT('Ctrl Pts',(37.2622974048239,253.75,20.3808625563341)) ;
#103096 = CARTESIAN_POINT('Ctrl Pts',(37.263500213621,253.750021261236,20.3800374989151)) ;
#103097 = CARTESIAN_POINT('Ctrl Pts',(37.2647025064213,253.750063777237,20.3792126481315)) ;
#103098 = CARTESIAN_POINT('Ctrl Pts',(37.280148021633,253.750609968276,20.3686160236467)) ;
#103099 = CARTESIAN_POINT('Ctrl Pts',(37.2953620762501,253.754658837467,20.3581534710378)) ;
#103100 = CARTESIAN_POINT('Ctrl Pts',(37.3095602987156,253.762001431812,20.3483736378944)) ;
#103101 = CARTESIAN_POINT('Ctrl Pts',(37.3243619284479,253.769656077527,20.3381781736817)) ;
#103102 = CARTESIAN_POINT('Ctrl Pts',(37.3377827048739,253.78074710398,20.3289158071227)) ;
#103103 = CARTESIAN_POINT('Ctrl Pts',(37.3490727448286,253.794651469056,20.3211165278944)) ;
#103104 = CARTESIAN_POINT('Ctrl Pts',(37.3603597640425,253.808552113907,20.3133193354259)) ;
#103105 = CARTESIAN_POINT('Ctrl Pts',(37.3693013951648,253.824998688613,20.307133835306)) ;
#103106 = CARTESIAN_POINT('Ctrl Pts',(37.3753983823083,253.843066458683,20.302914835877)) ;
#103107 = CARTESIAN_POINT('Ctrl Pts',(37.3814946181239,253.861132002274,20.2986963563525)) ;
#103108 = CARTESIAN_POINT('Ctrl Pts',(37.3846302685631,253.880472526098,20.2965247632926)) ;
#103109 = CARTESIAN_POINT('Ctrl Pts',(37.384630268563,253.9,20.2965247632926)) ;
#103110 = CARTESIAN_POINT('Origin',(36.9671811123914,253.9,20.5717268744974)) ;
#103111 = CARTESIAN_POINT('',(36.5764494676875,253.9,20.8837024854464)) ;
#103112 = CARTESIAN_POINT('Origin',(36.9671811123914,253.9,20.5717268744974)) ;
#103113 = CARTESIAN_POINT('',(36.6956187595939,253.75,20.7925297017961)) ;
#103114 = CARTESIAN_POINT('Origin',(36.9671811123914,253.75,20.5717268744974)) ;
#103115 = CARTESIAN_POINT('Ctrl Pts',(36.69561875959,253.75,20.7925297017989)) ;
#103116 = CARTESIAN_POINT('Ctrl Pts',(36.6944624091931,253.75,20.7934188295502)) ;
#103117 = CARTESIAN_POINT('Ctrl Pts',(36.6933060446003,253.750021261236,20.7943078119297)) ;
#103118 = CARTESIAN_POINT('Ctrl Pts',(36.6921500359814,253.750063777237,20.7951963674211)) ;
#103119 = CARTESIAN_POINT('Ctrl Pts',(36.677299120528,253.750609968276,20.8066113882631)) ;
#103120 = CARTESIAN_POINT('Ctrl Pts',(36.662647240261,253.754658837467,20.8178477074835)) ;
#103121 = CARTESIAN_POINT('Ctrl Pts',(36.64895857419,253.762001431812,20.8283288848358)) ;
#103122 = CARTESIAN_POINT('Ctrl Pts',(36.6346881563821,253.769656077527,20.8392554995373)) ;
#103123 = CARTESIAN_POINT('Ctrl Pts',(36.6217318743169,253.78074710398,20.8491571877365)) ;
#103124 = CARTESIAN_POINT('Ctrl Pts',(36.6108255047712,253.794651469056,20.8574845439793)) ;
#103125 = CARTESIAN_POINT('Ctrl Pts',(36.5999220533123,253.808552113907,20.865809672171)) ;
#103126 = CARTESIAN_POINT('Ctrl Pts',(36.5912761771423,253.824998688613,20.8724022440601)) ;
#103127 = CARTESIAN_POINT('Ctrl Pts',(36.5853795976012,253.843066458683,20.8768970808898)) ;
#103128 = CARTESIAN_POINT('Ctrl Pts',(36.5794837446919,253.861132002274,20.8813913638237)) ;
#103129 = CARTESIAN_POINT('Ctrl Pts',(36.5764494676877,253.880472526098,20.8837024854467)) ;
#103130 = CARTESIAN_POINT('Ctrl Pts',(36.5764494676876,253.9,20.8837024854466)) ;
#103131 = CARTESIAN_POINT('Origin',(38.5142359724255,253.9,23.2956415537952)) ;
#103132 = CARTESIAN_POINT('',(36.8126161897874,253.9,21.2087580919617)) ;
#103133 = CARTESIAN_POINT('',(38.3928834232693,253.9,23.3838093416391)) ;
#103134 = CARTESIAN_POINT('',(37.0149858472034,253.75,21.2321007871753)) ;
#103135 = CARTESIAN_POINT('',(38.5142359724255,253.75,23.2956415537952)) ;
#103136 = CARTESIAN_POINT('Ctrl Pts',(37.0149858472034,253.75,21.2321007871753)) ;
#103137 = CARTESIAN_POINT('Ctrl Pts',(37.0142029529195,253.75,21.2320049968919)) ;
#103138 = CARTESIAN_POINT('Ctrl Pts',(37.0134200452556,253.750003330106,21.2319092697064)) ;
#103139 = CARTESIAN_POINT('Ctrl Pts',(36.9924619678835,253.750181671152,21.2293484289546)) ;
#103140 = CARTESIAN_POINT('Ctrl Pts',(36.972205258534,253.752566842488,21.226917233338)) ;
#103141 = CARTESIAN_POINT('Ctrl Pts',(36.9337886651694,253.761740190968,21.2223843213245)) ;
#103142 = CARTESIAN_POINT('Ctrl Pts',(36.9154058857743,253.768377217198,21.220252974398)) ;
#103143 = CARTESIAN_POINT('Ctrl Pts',(36.8793105668223,253.78721321578,21.2161289230799)) ;
#103144 = CARTESIAN_POINT('Ctrl Pts',(36.8617289502234,253.800023548159,21.2141587038466)) ;
#103145 = CARTESIAN_POINT('Ctrl Pts',(36.8361910899809,253.828041657271,21.211329358316)) ;
#103146 = CARTESIAN_POINT('Ctrl Pts',(36.8270579203394,253.841958224525,21.2103300976413)) ;
#103147 = CARTESIAN_POINT('Ctrl Pts',(36.815504743716,253.870954690135,21.2090706572321)) ;
#103148 = CARTESIAN_POINT('Ctrl Pts',(36.8126161897874,253.885320776746,21.2087580919617)) ;
#103149 = CARTESIAN_POINT('Ctrl Pts',(36.8126161897874,253.9,21.2087580919617)) ;
#103150 = CARTESIAN_POINT('Origin',(40.2,253.9,25.0213203435596)) ;
#103151 = CARTESIAN_POINT('',(36.3874377484021,253.9,21.633936533347)) ;
#103152 = CARTESIAN_POINT('Origin',(40.2,253.9,25.0213203435596)) ;
#103153 = CARTESIAN_POINT('',(36.4107804436157,253.75,21.836306190763)) ;
#103154 = CARTESIAN_POINT('Origin',(40.2,253.75,25.0213203435596)) ;
#103155 = CARTESIAN_POINT('Ctrl Pts',(36.4107804436157,253.75,21.836306190763)) ;
#103156 = CARTESIAN_POINT('Ctrl Pts',(36.410684653332,253.75,21.835523296477)) ;
#103157 = CARTESIAN_POINT('Ctrl Pts',(36.410588926147,253.750003330105,21.8347403888173)) ;
#103158 = CARTESIAN_POINT('Ctrl Pts',(36.4080280853953,253.750181671152,21.8137823114414)) ;
#103159 = CARTESIAN_POINT('Ctrl Pts',(36.4055968897783,253.752566842488,21.7935256020932)) ;
#103160 = CARTESIAN_POINT('Ctrl Pts',(36.4010639777649,253.761740190968,21.7551090087289)) ;
#103161 = CARTESIAN_POINT('Ctrl Pts',(36.3989326308384,253.768377217198,21.7367262293338)) ;
#103162 = CARTESIAN_POINT('Ctrl Pts',(36.3948085795202,253.78721321578,21.7006309103819)) ;
#103163 = CARTESIAN_POINT('Ctrl Pts',(36.392838360287,253.800023548159,21.683049293783)) ;
#103164 = CARTESIAN_POINT('Ctrl Pts',(36.3900090147564,253.828041657271,21.6575114335404)) ;
#103165 = CARTESIAN_POINT('Ctrl Pts',(36.3890097540816,253.841958224525,21.648378263899)) ;
#103166 = CARTESIAN_POINT('Ctrl Pts',(36.3877503136725,253.870954690135,21.6368250872756)) ;
#103167 = CARTESIAN_POINT('Ctrl Pts',(36.3874377484021,253.885320776746,21.633936533347)) ;
#103168 = CARTESIAN_POINT('Ctrl Pts',(36.3874377484021,253.9,21.633936533347)) ;
#103169 = CARTESIAN_POINT('Origin',(38.1898177136379,253.9,23.1288524263407)) ;
#103170 = CARTESIAN_POINT('',(36.0623821418868,253.9,21.3977698112471)) ;
#103171 = CARTESIAN_POINT('',(38.2779855014818,253.9,23.0074998771845)) ;
#103172 = CARTESIAN_POINT('',(35.9712093582363,253.75,21.5169391031534)) ;
#103173 = CARTESIAN_POINT('',(38.1898177136379,253.75,23.1288524263407)) ;
#103174 = CARTESIAN_POINT('Ctrl Pts',(35.9712093582363,253.75,21.5169391031534)) ;
#103175 = CARTESIAN_POINT('Ctrl Pts',(35.9720984859888,253.75,21.5157827527548)) ;
#103176 = CARTESIAN_POINT('Ctrl Pts',(35.9729874683704,253.750021261236,21.5146263881627)) ;
#103177 = CARTESIAN_POINT('Ctrl Pts',(35.9738760238622,253.750063777237,21.5134703795415)) ;
#103178 = CARTESIAN_POINT('Ctrl Pts',(35.9852910446951,253.750609968276,21.4986194640776)) ;
#103179 = CARTESIAN_POINT('Ctrl Pts',(35.9965273639257,253.754658837467,21.4839675838214)) ;
#103180 = CARTESIAN_POINT('Ctrl Pts',(36.0070085412772,253.762001431812,21.4702789177503)) ;
#103181 = CARTESIAN_POINT('Ctrl Pts',(36.017935155978,253.769656077527,21.4560084999421)) ;
#103182 = CARTESIAN_POINT('Ctrl Pts',(36.0278368441765,253.78074710398,21.4430522178762)) ;
#103183 = CARTESIAN_POINT('Ctrl Pts',(36.0361642004193,253.794651469056,21.4321458483306)) ;
#103184 = CARTESIAN_POINT('Ctrl Pts',(36.0444893286111,253.808552113907,21.4212423968717)) ;
#103185 = CARTESIAN_POINT('Ctrl Pts',(36.0510819005004,253.824998688613,21.4125965207018)) ;
#103186 = CARTESIAN_POINT('Ctrl Pts',(36.0555767373303,253.843066458683,21.4066999411609)) ;
#103187 = CARTESIAN_POINT('Ctrl Pts',(36.0600710202644,253.861132002274,21.4008040882518)) ;
#103188 = CARTESIAN_POINT('Ctrl Pts',(36.0623821418865,253.880472526098,21.3977698112469)) ;
#103189 = CARTESIAN_POINT('Ctrl Pts',(36.0623821418867,253.9,21.3977698112471)) ;
#103190 = CARTESIAN_POINT('Origin',(35.7504065309378,253.9,21.788501455951)) ;
#103191 = CARTESIAN_POINT('',(35.4752044197332,253.9,22.2059506121228)) ;
#103192 = CARTESIAN_POINT('Origin',(35.7504065309378,253.9,21.788501455951)) ;
#103193 = CARTESIAN_POINT('',(35.5603672117704,253.75,22.0824148057165)) ;
#103194 = CARTESIAN_POINT('Origin',(35.7504065309378,253.75,21.788501455951)) ;
#103195 = CARTESIAN_POINT('Ctrl Pts',(35.5603672117688,253.75,22.0824148057187)) ;
#103196 = CARTESIAN_POINT('Ctrl Pts',(35.5595422127734,253.75,22.0836177483853)) ;
#103197 = CARTESIAN_POINT('Ctrl Pts',(35.5587171553563,253.750021261236,22.084820557182)) ;
#103198 = CARTESIAN_POINT('Ctrl Pts',(35.5578923045725,253.750063777237,22.0860228499814)) ;
#103199 = CARTESIAN_POINT('Ctrl Pts',(35.5472956800797,253.750609968276,22.1014683651895)) ;
#103200 = CARTESIAN_POINT('Ctrl Pts',(35.5368331274791,253.754658837467,22.1166824198107)) ;
#103201 = CARTESIAN_POINT('Ctrl Pts',(35.5270532943355,253.762001431812,22.1308806422758)) ;
#103202 = CARTESIAN_POINT('Ctrl Pts',(35.5168578301224,253.769656077527,22.1456822720078)) ;
#103203 = CARTESIAN_POINT('Ctrl Pts',(35.5075954635634,253.78074710398,22.1591030484337)) ;
#103204 = CARTESIAN_POINT('Ctrl Pts',(35.4997961843351,253.794651469056,22.1703930883885)) ;
#103205 = CARTESIAN_POINT('Ctrl Pts',(35.4919989918666,253.808552113907,22.1816801076023)) ;
#103206 = CARTESIAN_POINT('Ctrl Pts',(35.4858134917463,253.824998688613,22.1906217387244)) ;
#103207 = CARTESIAN_POINT('Ctrl Pts',(35.4815944923174,253.843066458683,22.1967187258679)) ;
#103208 = CARTESIAN_POINT('Ctrl Pts',(35.4773760127931,253.861132002274,22.2028149616837)) ;
#103209 = CARTESIAN_POINT('Ctrl Pts',(35.4752044197329,253.880472526098,22.2059506121226)) ;
#103210 = CARTESIAN_POINT('Ctrl Pts',(35.475204419733,253.9,22.2059506121227)) ;
#103211 = CARTESIAN_POINT('Origin',(38.0634790637697,253.9,23.9010320185483)) ;
#103212 = CARTESIAN_POINT('',(35.8002600262485,253.9,22.4421173342227)) ;
#103213 = CARTESIAN_POINT('',(37.9753112759259,253.9,24.0223845677046)) ;
#103214 = CARTESIAN_POINT('',(35.9999382971499,253.75,22.4017818933262)) ;
#103215 = CARTESIAN_POINT('',(38.0634790637697,253.75,23.9010320185483)) ;
#103216 = CARTESIAN_POINT('Ctrl Pts',(35.9999382971499,253.75,22.4017818933262)) ;
#103217 = CARTESIAN_POINT('Ctrl Pts',(35.999164119612,253.75,22.4019327189919)) ;
#103218 = CARTESIAN_POINT('Ctrl Pts',(35.9983899488536,253.750003330105,22.4020836088006)) ;
#103219 = CARTESIAN_POINT('Ctrl Pts',(35.9776662894844,253.750181671152,22.4061245065949)) ;
#103220 = CARTESIAN_POINT('Ctrl Pts',(35.9576497332976,253.752566842488,22.4100719696)) ;
#103221 = CARTESIAN_POINT('Ctrl Pts',(35.9197126349982,253.761740190968,22.4176322943074)) ;
#103222 = CARTESIAN_POINT('Ctrl Pts',(35.9015709504457,253.768377217198,22.4212858541613)) ;
#103223 = CARTESIAN_POINT('Ctrl Pts',(35.8659678602058,253.78721321578,22.4285177152552)) ;
#103224 = CARTESIAN_POINT('Ctrl Pts',(35.8486379179467,253.800023548159,22.4320769437325)) ;
#103225 = CARTESIAN_POINT('Ctrl Pts',(35.823475653699,253.828041657271,22.4372777090437)) ;
#103226 = CARTESIAN_POINT('Ctrl Pts',(35.8144807046667,253.841958224525,22.4391496602992)) ;
#103227 = CARTESIAN_POINT('Ctrl Pts',(35.8031037922653,253.870954690135,22.4415219892068)) ;
#103228 = CARTESIAN_POINT('Ctrl Pts',(35.8002600262485,253.885320776746,22.4421173342227)) ;
#103229 = CARTESIAN_POINT('Ctrl Pts',(35.8002600262485,253.9,22.4421173342227)) ;
#103230 = CARTESIAN_POINT('Origin',(40.2,253.9,25.0213203435596)) ;
#103231 = CARTESIAN_POINT('',(35.5272786630106,253.9,22.9778734255204)) ;
#103232 = CARTESIAN_POINT('Origin',(40.2,253.9,25.0213203435596)) ;
#103233 = CARTESIAN_POINT('',(35.6120145486888,253.75,23.1631251173908)) ;
#103234 = CARTESIAN_POINT('Origin',(40.2,253.75,25.0213203435596)) ;
#103235 = CARTESIAN_POINT('Ctrl Pts',(35.6120145486888,253.75,23.1631251173908)) ;
#103236 = CARTESIAN_POINT('Ctrl Pts',(35.611681519077,253.75,23.162410141506)) ;
#103237 = CARTESIAN_POINT('Ctrl Pts',(35.6113485453403,253.750003330106,23.1616951333977)) ;
#103238 = CARTESIAN_POINT('Ctrl Pts',(35.6024366389787,253.750181671152,23.1425541606558)) ;
#103239 = CARTESIAN_POINT('Ctrl Pts',(35.593864767106,253.752566842488,23.1240401659928)) ;
#103240 = CARTESIAN_POINT('Ctrl Pts',(35.5776823313821,253.761740190968,23.0889045613856)) ;
#103241 = CARTESIAN_POINT('Ctrl Pts',(35.5699747087623,253.768377217198,23.0720801216755)) ;
#103242 = CARTESIAN_POINT('Ctrl Pts',(35.5548984359091,253.78721321578,23.0390258353216)) ;
#103243 = CARTESIAN_POINT('Ctrl Pts',(35.5475916277511,253.800023548159,23.0229135555139)) ;
#103244 = CARTESIAN_POINT('Ctrl Pts',(35.5370091274324,253.828041657271,22.9994999229698)) ;
#103245 = CARTESIAN_POINT('Ctrl Pts',(35.5332364694246,253.841958224525,22.9911225509982)) ;
#103246 = CARTESIAN_POINT('Ctrl Pts',(35.5284685425009,253.870954690135,22.9805240155764)) ;
#103247 = CARTESIAN_POINT('Ctrl Pts',(35.5272786630106,253.885320776746,22.9778734255204)) ;
#103248 = CARTESIAN_POINT('Ctrl Pts',(35.5272786630106,253.9,22.9778734255204)) ;
#103249 = CARTESIAN_POINT('Origin',(37.7033982898842,253.9,23.8426568872864)) ;
#103250 = CARTESIAN_POINT('',(35.1451528796413,253.9,22.8537132320653)) ;
#103251 = CARTESIAN_POINT('',(37.7497508390405,253.9,23.6999984098422)) ;
#103252 = CARTESIAN_POINT('',(35.0952677460482,253.75,22.9952239032475)) ;
#103253 = CARTESIAN_POINT('',(37.7033982898842,253.75,23.8426568872864)) ;
#103254 = CARTESIAN_POINT('Ctrl Pts',(35.0952677460482,253.75,22.9952239032474)) ;
#103255 = CARTESIAN_POINT('Ctrl Pts',(35.0957560248663,253.75,22.9938493930805)) ;
#103256 = CARTESIAN_POINT('Ctrl Pts',(35.0962441610409,253.750021261236,22.9924749143349)) ;
#103257 = CARTESIAN_POINT('Ctrl Pts',(35.0967320012226,253.750063777237,22.9911009060562)) ;
#103258 = CARTESIAN_POINT('Ctrl Pts',(35.1029991459191,253.750609968276,22.9734494107094)) ;
#103259 = CARTESIAN_POINT('Ctrl Pts',(35.1091578405339,253.754658837467,22.9560424309131)) ;
#103260 = CARTESIAN_POINT('Ctrl Pts',(35.1148960021067,253.762001431812,22.9397848739239)) ;
#103261 = CARTESIAN_POINT('Ctrl Pts',(35.1208780285998,253.769656077527,22.9228363904437)) ;
#103262 = CARTESIAN_POINT('Ctrl Pts',(35.1262913823416,253.78074710398,22.9074544440318)) ;
#103263 = CARTESIAN_POINT('Ctrl Pts',(35.1308409152232,253.794651469056,22.894508575609)) ;
#103264 = CARTESIAN_POINT('Ctrl Pts',(35.1353892308407,253.808552113907,22.8815661709573)) ;
#103265 = CARTESIAN_POINT('Ctrl Pts',(35.1389874166273,253.824998688613,22.8713062373364)) ;
#103266 = CARTESIAN_POINT('Ctrl Pts',(35.141440117197,253.843066458683,22.8643092759727)) ;
#103267 = CARTESIAN_POINT('Ctrl Pts',(35.1438925155221,253.861132002274,22.8573131768401)) ;
#103268 = CARTESIAN_POINT('Ctrl Pts',(35.1451528796412,253.880472526098,22.8537132320653)) ;
#103269 = CARTESIAN_POINT('Ctrl Pts',(35.1451528796412,253.9,22.8537132320653)) ;
#103270 = CARTESIAN_POINT('Origin',(34.9691891603767,253.9,23.3217268744974)) ;
#103271 = CARTESIAN_POINT('',(34.8364552827619,253.9,23.8037867439466)) ;
#103272 = CARTESIAN_POINT('Origin',(34.9691891603767,253.9,23.3217268744974)) ;
#103273 = CARTESIAN_POINT('',(34.8792752474816,253.75,23.6599804602403)) ;
#103274 = CARTESIAN_POINT('Origin',(34.9691891603767,253.75,23.3217268744974)) ;
#103275 = CARTESIAN_POINT('Ctrl Pts',(34.8792752474796,253.75,23.6599804602464)) ;
#103276 = CARTESIAN_POINT('Ctrl Pts',(34.8788623565368,253.75,23.6613794654168)) ;
#103277 = CARTESIAN_POINT('Ctrl Pts',(34.8784493686624,253.750021261236,23.6627783613227)) ;
#103278 = CARTESIAN_POINT('Ctrl Pts',(34.8780364178575,253.750063777237,23.6641767026329)) ;
#103279 = CARTESIAN_POINT('Ctrl Pts',(34.8727313557742,253.750609968276,23.6821407975714)) ;
#103280 = CARTESIAN_POINT('Ctrl Pts',(34.8674822783712,253.754658837467,23.6998433299148)) ;
#103281 = CARTESIAN_POINT('Ctrl Pts',(34.8625685963638,253.762001431812,23.7163687765538)) ;
#103282 = CARTESIAN_POINT('Ctrl Pts',(34.8574460888193,253.769656077527,23.7335965346698)) ;
#103283 = CARTESIAN_POINT('Ctrl Pts',(34.8527843027414,253.78074710398,23.7492226802185)) ;
#103284 = CARTESIAN_POINT('Ctrl Pts',(34.8488555616221,253.794651469056,23.7623702561121)) ;
#103285 = CARTESIAN_POINT('Ctrl Pts',(34.844927871669,253.808552113907,23.7755143142662)) ;
#103286 = CARTESIAN_POINT('Ctrl Pts',(34.8418082274473,253.824998688613,23.785929735467)) ;
#103287 = CARTESIAN_POINT('Ctrl Pts',(34.8396797931899,253.843066458683,23.7930320573424)) ;
#103288 = CARTESIAN_POINT('Ctrl Pts',(34.837551621218,253.861132002274,23.8001335040032)) ;
#103289 = CARTESIAN_POINT('Ctrl Pts',(34.8364552827618,253.880472526098,23.8037867439466)) ;
#103290 = CARTESIAN_POINT('Ctrl Pts',(34.8364552827619,253.9,23.8037867439466)) ;
#103291 = CARTESIAN_POINT('Origin',(37.8218597103689,253.9,24.6160841100613)) ;
#103292 = CARTESIAN_POINT('',(35.2185810661312,253.9,23.9279469374017)) ;
#103293 = CARTESIAN_POINT('',(37.7755071612126,253.9,24.7587425875056)) ;
#103294 = CARTESIAN_POINT('',(35.3960220501219,253.75,23.8278816743835)) ;
#103295 = CARTESIAN_POINT('',(37.8218597103689,253.75,24.6160841100613)) ;
#103296 = CARTESIAN_POINT('Ctrl Pts',(35.3960220501219,253.75,23.8278816743835)) ;
#103297 = CARTESIAN_POINT('Ctrl Pts',(35.3953323712255,253.75,23.8282643521305)) ;
#103298 = CARTESIAN_POINT('Ctrl Pts',(35.3946427185925,253.750003330106,23.8286470887893)) ;
#103299 = CARTESIAN_POINT('Ctrl Pts',(35.3761820534012,253.750181671152,23.8388941738976)) ;
#103300 = CARTESIAN_POINT('Ctrl Pts',(35.3583650103588,253.752566842488,23.8488338903421)) ;
#103301 = CARTESIAN_POINT('Ctrl Pts',(35.3246209546295,253.761740190968,23.8677473945122)) ;
#103302 = CARTESIAN_POINT('Ctrl Pts',(35.3084961994041,253.768377217198,23.8768282252524)) ;
#103303 = CARTESIAN_POINT('Ctrl Pts',(35.27687041641,253.78721321578,23.8947080938071)) ;
#103304 = CARTESIAN_POINT('Ctrl Pts',(35.2614885239839,253.800023548159,23.903448367913)) ;
#103305 = CARTESIAN_POINT('Ctrl Pts',(35.2391649134711,253.828041657271,23.9161701569215)) ;
#103306 = CARTESIAN_POINT('Ctrl Pts',(35.2311886733309,253.841958224525,23.9207300804757)) ;
#103307 = CARTESIAN_POINT('Ctrl Pts',(35.2211016766049,253.870954690135,23.9265019586177)) ;
#103308 = CARTESIAN_POINT('Ctrl Pts',(35.2185810661312,253.885320776746,23.9279469374017)) ;
#103309 = CARTESIAN_POINT('Ctrl Pts',(35.2185810661312,253.9,23.9279469374017)) ;
#103310 = CARTESIAN_POINT('Origin',(40.2,253.9,25.0213203435596)) ;
#103311 = CARTESIAN_POINT('',(35.1245180988476,253.9,24.5218371395634)) ;
#103312 = CARTESIAN_POINT('Origin',(40.2,253.9,25.0213203435596)) ;
#103313 = CARTESIAN_POINT('',(35.2623526361106,253.75,24.6718371395634)) ;
#103314 = CARTESIAN_POINT('Origin',(40.2,253.75,25.0213203435596)) ;
#103315 = CARTESIAN_POINT('Ctrl Pts',(35.2623526361106,253.75,24.6718371395634)) ;
#103316 = CARTESIAN_POINT('Ctrl Pts',(35.2618149664292,253.75,24.6712600688988)) ;
#103317 = CARTESIAN_POINT('Ctrl Pts',(35.2612773399305,253.750003330106,24.6706829503216)) ;
#103318 = CARTESIAN_POINT('Ctrl Pts',(35.2468867274465,253.750181671152,24.655232733985)) ;
#103319 = CARTESIAN_POINT('Ctrl Pts',(35.2330132538605,253.752566842488,24.6402737328005)) ;
#103320 = CARTESIAN_POINT('Ctrl Pts',(35.2067653439847,253.761740190968,24.6118584347341)) ;
#103321 = CARTESIAN_POINT('Ctrl Pts',(35.1942359214757,253.768377217198,24.5982392280904)) ;
#103322 = CARTESIAN_POINT('Ctrl Pts',(35.1696831977168,253.78721321578,24.5714615581854)) ;
#103323 = CARTESIAN_POINT('Ctrl Pts',(35.1577550419262,253.800023548159,24.5583957973774)) ;
#103324 = CARTESIAN_POINT('Ctrl Pts',(35.1404552756832,253.828041657271,24.5393982820177)) ;
#103325 = CARTESIAN_POINT('Ctrl Pts',(35.1342785143937,253.841958224525,24.5325967432531)) ;
#103326 = CARTESIAN_POINT('Ctrl Pts',(35.1264688188629,253.870954690135,24.5239903075244)) ;
#103327 = CARTESIAN_POINT('Ctrl Pts',(35.1245180988476,253.885320776746,24.5218371395634)) ;
#103328 = CARTESIAN_POINT('Ctrl Pts',(35.1245180988476,253.9,24.5218371395634)) ;
#103329 = CARTESIAN_POINT('Origin',(37.4613636363637,253.9,24.6718371395634)) ;
#103330 = CARTESIAN_POINT('',(34.7227272727273,253.9,24.5218371395634)) ;
#103331 = CARTESIAN_POINT('',(37.4613636363637,253.9,24.5218371395634)) ;
#103332 = CARTESIAN_POINT('',(34.7190128936382,253.75,24.6718371395634)) ;
#103333 = CARTESIAN_POINT('',(37.4613636363637,253.75,24.6718371395634)) ;
#103334 = CARTESIAN_POINT('Ctrl Pts',(34.7190128936382,253.75,24.6718371395634)) ;
#103335 = CARTESIAN_POINT('Ctrl Pts',(34.7190525273894,253.75,24.6703790162596)) ;
#103336 = CARTESIAN_POINT('Ctrl Pts',(34.7190920351881,253.750021261236,24.6689209669185)) ;
#103337 = CARTESIAN_POINT('Ctrl Pts',(34.7191314068632,253.750063777237,24.6674634564849)) ;
#103338 = CARTESIAN_POINT('Ctrl Pts',(34.7196372036259,253.750609968276,24.6487392325953)) ;
#103339 = CARTESIAN_POINT('Ctrl Pts',(34.720115417695,253.754658837467,24.6302810697322)) ;
#103340 = CARTESIAN_POINT('Ctrl Pts',(34.7205488722535,253.762001431812,24.6130460247761)) ;
#103341 = CARTESIAN_POINT('Ctrl Pts',(34.7210007481061,253.769656077527,24.5950785112738)) ;
#103342 = CARTESIAN_POINT('Ctrl Pts',(34.7213958706093,253.78074710398,24.5787765926027)) ;
#103343 = CARTESIAN_POINT('Ctrl Pts',(34.7217222401528,253.794651469056,24.5650584571033)) ;
#103344 = CARTESIAN_POINT('Ctrl Pts',(34.7220485223735,253.808552113907,24.5513439920011)) ;
#103345 = CARTESIAN_POINT('Ctrl Pts',(34.7223001065627,253.824998688613,24.5404743147171)) ;
#103346 = CARTESIAN_POINT('Ctrl Pts',(34.7224705834518,253.843066458683,24.5330618828598)) ;
#103347 = CARTESIAN_POINT('Ctrl Pts',(34.7226410393332,253.861132002274,24.5256503644317)) ;
#103348 = CARTESIAN_POINT('Ctrl Pts',(34.7227272727271,253.880472526098,24.5218371395634)) ;
#103349 = CARTESIAN_POINT('Ctrl Pts',(34.7227272727271,253.9,24.5218371395634)) ;
#103350 = CARTESIAN_POINT('Origin',(34.7,253.9,25.0213203435596)) ;
#103351 = CARTESIAN_POINT('',(34.7227272727273,253.9,25.5208035475559)) ;
#103352 = CARTESIAN_POINT('Origin',(34.7,253.9,25.0213203435596)) ;
#103353 = CARTESIAN_POINT('',(34.7190128936384,253.75,25.3708035475559)) ;
#103354 = CARTESIAN_POINT('Origin',(34.7,253.75,25.0213203435596)) ;
#103355 = CARTESIAN_POINT('Ctrl Pts',(34.7190128936384,253.75,25.3708035475559)) ;
#103356 = CARTESIAN_POINT('Ctrl Pts',(34.7190525273896,253.75,25.3722616708596)) ;
#103357 = CARTESIAN_POINT('Ctrl Pts',(34.7190920351885,253.750021261236,25.3737197202007)) ;
#103358 = CARTESIAN_POINT('Ctrl Pts',(34.7191314068636,253.750063777237,25.3751772306343)) ;
#103359 = CARTESIAN_POINT('Ctrl Pts',(34.7196372036263,253.750609968276,25.3939014545242)) ;
#103360 = CARTESIAN_POINT('Ctrl Pts',(34.7201154176943,253.754658837467,25.4123596173871)) ;
#103361 = CARTESIAN_POINT('Ctrl Pts',(34.720548872253,253.762001431812,25.4295946623432)) ;
#103362 = CARTESIAN_POINT('Ctrl Pts',(34.7210007481058,253.769656077527,25.4475621758457)) ;
#103363 = CARTESIAN_POINT('Ctrl Pts',(34.7213958706092,253.78074710398,25.4638640945166)) ;
#103364 = CARTESIAN_POINT('Ctrl Pts',(34.7217222401529,253.794651469056,25.4775822300161)) ;
#103365 = CARTESIAN_POINT('Ctrl Pts',(34.7220485223737,253.808552113907,25.4912966951182)) ;
#103366 = CARTESIAN_POINT('Ctrl Pts',(34.7223001065631,253.824998688613,25.5021663724021)) ;
#103367 = CARTESIAN_POINT('Ctrl Pts',(34.7224705834521,253.843066458683,25.5095788042595)) ;
#103368 = CARTESIAN_POINT('Ctrl Pts',(34.7226410393334,253.861132002274,25.5169903226876)) ;
#103369 = CARTESIAN_POINT('Ctrl Pts',(34.7227272727275,253.880472526098,25.5208035475559)) ;
#103370 = CARTESIAN_POINT('Ctrl Pts',(34.7227272727275,253.9,25.5208035475559)) ;
#103371 = CARTESIAN_POINT('Origin',(37.8130292979948,253.9,25.3708035475559)) ;
#103372 = CARTESIAN_POINT('',(35.1245180988476,253.9,25.5208035475559)) ;
#103373 = CARTESIAN_POINT('',(37.8130292979948,253.9,25.5208035475559)) ;
#103374 = CARTESIAN_POINT('',(35.2623526361106,253.75,25.3708035475559)) ;
#103375 = CARTESIAN_POINT('',(37.8130292979948,253.75,25.3708035475559)) ;
#103376 = CARTESIAN_POINT('Ctrl Pts',(35.2623526361106,253.75,25.3708035475559)) ;
#103377 = CARTESIAN_POINT('Ctrl Pts',(35.2618149664292,253.75,25.3713806182205)) ;
#103378 = CARTESIAN_POINT('Ctrl Pts',(35.2612773399305,253.750003330106,25.3719577367977)) ;
#103379 = CARTESIAN_POINT('Ctrl Pts',(35.2468867274466,253.750181671152,25.3874079531342)) ;
#103380 = CARTESIAN_POINT('Ctrl Pts',(35.2330132538606,253.752566842488,25.4023669543188)) ;
#103381 = CARTESIAN_POINT('Ctrl Pts',(35.2067653439847,253.761740190968,25.4307822523853)) ;
#103382 = CARTESIAN_POINT('Ctrl Pts',(35.1942359214756,253.768377217198,25.4444014590289)) ;
#103383 = CARTESIAN_POINT('Ctrl Pts',(35.1696831977168,253.78721321578,25.4711791289339)) ;
#103384 = CARTESIAN_POINT('Ctrl Pts',(35.1577550419262,253.800023548159,25.4842448897419)) ;
#103385 = CARTESIAN_POINT('Ctrl Pts',(35.1404552756832,253.828041657271,25.5032424051016)) ;
#103386 = CARTESIAN_POINT('Ctrl Pts',(35.1342785143937,253.841958224525,25.5100439438662)) ;
#103387 = CARTESIAN_POINT('Ctrl Pts',(35.1264688188629,253.870954690135,25.5186503795949)) ;
#103388 = CARTESIAN_POINT('Ctrl Pts',(35.1245180988476,253.885320776746,25.5208035475559)) ;
#103389 = CARTESIAN_POINT('Ctrl Pts',(35.1245180988476,253.9,25.5208035475559)) ;
#103390 = CARTESIAN_POINT('Origin',(40.2,253.9,25.0213203435596)) ;
#103391 = CARTESIAN_POINT('',(35.2185810661312,253.9,26.1146937497175)) ;
#103392 = CARTESIAN_POINT('Origin',(40.2,253.9,25.0213203435596)) ;
#103393 = CARTESIAN_POINT('',(35.3960220501219,253.75,26.2147590127358)) ;
#103394 = CARTESIAN_POINT('Origin',(40.2,253.75,25.0213203435596)) ;
#103395 = CARTESIAN_POINT('Ctrl Pts',(35.3960220501219,253.75,26.2147590127358)) ;
#103396 = CARTESIAN_POINT('Ctrl Pts',(35.3953323712267,253.75,26.2143763349894)) ;
#103397 = CARTESIAN_POINT('Ctrl Pts',(35.3946427185949,253.750003330105,26.2139935983313)) ;
#103398 = CARTESIAN_POINT('Ctrl Pts',(35.3761820534042,253.750181671152,26.2037465132234)) ;
#103399 = CARTESIAN_POINT('Ctrl Pts',(35.3583650103612,253.752566842487,26.1938067967784)) ;
#103400 = CARTESIAN_POINT('Ctrl Pts',(35.3246209546306,253.761740190968,26.1748932926076)) ;
#103401 = CARTESIAN_POINT('Ctrl Pts',(35.3084961994046,253.768377217198,26.1658124618672)) ;
#103402 = CARTESIAN_POINT('Ctrl Pts',(35.2768704164101,253.78721321578,26.1479325933122)) ;
#103403 = CARTESIAN_POINT('Ctrl Pts',(35.2614885239839,253.800023548159,26.1391923192062)) ;
#103404 = CARTESIAN_POINT('Ctrl Pts',(35.2391649134711,253.828041657271,26.1264705301977)) ;
#103405 = CARTESIAN_POINT('Ctrl Pts',(35.2311886733309,253.841958224525,26.1219106066435)) ;
#103406 = CARTESIAN_POINT('Ctrl Pts',(35.2211016766049,253.870954690135,26.1161387285016)) ;
#103407 = CARTESIAN_POINT('Ctrl Pts',(35.2185810661312,253.885320776746,26.1146937497175)) ;
#103408 = CARTESIAN_POINT('Ctrl Pts',(35.2185810661312,253.9,26.1146937497175)) ;
#103409 = CARTESIAN_POINT('Origin',(37.4874057913173,253.9,25.5352272428401)) ;
#103410 = CARTESIAN_POINT('',(34.8364552827619,253.9,26.2388539431727)) ;
#103411 = CARTESIAN_POINT('',(37.4410532421611,253.9,25.3925687653958)) ;
#103412 = CARTESIAN_POINT('',(34.8792752474813,253.75,26.3826602268791)) ;
#103413 = CARTESIAN_POINT('',(37.4874057913173,253.75,25.5352272428401)) ;
#103414 = CARTESIAN_POINT('Ctrl Pts',(34.8792752474813,253.75,26.3826602268791)) ;
#103415 = CARTESIAN_POINT('Ctrl Pts',(34.8788623565379,253.75,26.3812612217066)) ;
#103416 = CARTESIAN_POINT('Ctrl Pts',(34.8784493686629,253.750021261236,26.3798623257986)) ;
#103417 = CARTESIAN_POINT('Ctrl Pts',(34.8780364178574,253.750063777237,26.3784639844864)) ;
#103418 = CARTESIAN_POINT('Ctrl Pts',(34.872731355774,253.750609968276,26.3604998895479)) ;
#103419 = CARTESIAN_POINT('Ctrl Pts',(34.8674822783721,253.754658837467,26.3427973572042)) ;
#103420 = CARTESIAN_POINT('Ctrl Pts',(34.8625685963644,253.762001431812,26.3262719105654)) ;
#103421 = CARTESIAN_POINT('Ctrl Pts',(34.8574460888198,253.769656077527,26.3090441524495)) ;
#103422 = CARTESIAN_POINT('Ctrl Pts',(34.8527843027409,253.78074710398,26.2934180069009)) ;
#103423 = CARTESIAN_POINT('Ctrl Pts',(34.8488555616216,253.794651469056,26.2802704310073)) ;
#103424 = CARTESIAN_POINT('Ctrl Pts',(34.8449278716686,253.808552113907,26.2671263728532)) ;
#103425 = CARTESIAN_POINT('Ctrl Pts',(34.8418082274471,253.824998688613,26.2567109516523)) ;
#103426 = CARTESIAN_POINT('Ctrl Pts',(34.8396797931898,253.843066458683,26.2496086297769)) ;
#103427 = CARTESIAN_POINT('Ctrl Pts',(34.8375516212181,253.861132002274,26.242507183116)) ;
#103428 = CARTESIAN_POINT('Ctrl Pts',(34.8364552827617,253.880472526098,26.2388539431727)) ;
#103429 = CARTESIAN_POINT('Ctrl Pts',(34.8364552827617,253.9,26.2388539431727)) ;
#103430 = CARTESIAN_POINT('Origin',(34.9691891603767,253.9,26.7209138126218)) ;
#103431 = CARTESIAN_POINT('',(35.1451528796413,253.9,27.188927455054)) ;
#103432 = CARTESIAN_POINT('Origin',(34.9691891603767,253.9,26.7209138126218)) ;
#103433 = CARTESIAN_POINT('',(35.0952677460484,253.75,27.0474167838717)) ;
#103434 = CARTESIAN_POINT('Origin',(34.9691891603767,253.75,26.7209138126218)) ;
#103435 = CARTESIAN_POINT('Ctrl Pts',(35.0952677460487,253.75,27.0474167838725)) ;
#103436 = CARTESIAN_POINT('Ctrl Pts',(35.0957560248667,253.75,27.0487912940392)) ;
#103437 = CARTESIAN_POINT('Ctrl Pts',(35.0962441610412,253.750021261236,27.0501657727845)) ;
#103438 = CARTESIAN_POINT('Ctrl Pts',(35.0967320012228,253.750063777237,27.051539781063)) ;
#103439 = CARTESIAN_POINT('Ctrl Pts',(35.1029991459191,253.750609968276,27.0691912764102)) ;
#103440 = CARTESIAN_POINT('Ctrl Pts',(35.1091578405316,253.754658837467,27.086598256207)) ;
#103441 = CARTESIAN_POINT('Ctrl Pts',(35.114896002105,253.762001431812,27.1028558131961)) ;
#103442 = CARTESIAN_POINT('Ctrl Pts',(35.1208780285987,253.769656077527,27.1198042966762)) ;
#103443 = CARTESIAN_POINT('Ctrl Pts',(35.1262913823415,253.78074710398,27.1351862430875)) ;
#103444 = CARTESIAN_POINT('Ctrl Pts',(35.1308409152232,253.794651469056,27.1481321115102)) ;
#103445 = CARTESIAN_POINT('Ctrl Pts',(35.1353892308407,253.808552113907,27.1610745161619)) ;
#103446 = CARTESIAN_POINT('Ctrl Pts',(35.1389874166275,253.824998688613,27.1713344497828)) ;
#103447 = CARTESIAN_POINT('Ctrl Pts',(35.1414401171972,253.843066458683,27.1783314111465)) ;
#103448 = CARTESIAN_POINT('Ctrl Pts',(35.1438925155223,253.861132002274,27.1853275102791)) ;
#103449 = CARTESIAN_POINT('Ctrl Pts',(35.1451528796413,253.880472526098,27.1889274550539)) ;
#103450 = CARTESIAN_POINT('Ctrl Pts',(35.1451528796413,253.9,27.1889274550539)) ;
#103451 = CARTESIAN_POINT('Origin',(38.0378522089358,253.9,26.0913131340507)) ;
#103452 = CARTESIAN_POINT('',(35.5272786630106,253.9,27.0647672615988)) ;
#103453 = CARTESIAN_POINT('',(38.084204758092,253.9,26.233971611495)) ;
#103454 = CARTESIAN_POINT('',(35.6120145486888,253.75,26.8795155697285)) ;
#103455 = CARTESIAN_POINT('',(38.0378522089358,253.75,26.0913131340507)) ;
#103456 = CARTESIAN_POINT('Ctrl Pts',(35.6120145486888,253.75,26.8795155697285)) ;
#103457 = CARTESIAN_POINT('Ctrl Pts',(35.611681519077,253.75,26.8802305456133)) ;
#103458 = CARTESIAN_POINT('Ctrl Pts',(35.6113485453403,253.750003330106,26.8809455537216)) ;
#103459 = CARTESIAN_POINT('Ctrl Pts',(35.6024366389788,253.750181671152,26.9000865264633)) ;
#103460 = CARTESIAN_POINT('Ctrl Pts',(35.5938647671061,253.752566842488,26.9186005211265)) ;
#103461 = CARTESIAN_POINT('Ctrl Pts',(35.5776823313821,253.761740190968,26.9537361257337)) ;
#103462 = CARTESIAN_POINT('Ctrl Pts',(35.5699747087622,253.768377217198,26.9705605654438)) ;
#103463 = CARTESIAN_POINT('Ctrl Pts',(35.554898435909,253.78721321578,27.0036148517979)) ;
#103464 = CARTESIAN_POINT('Ctrl Pts',(35.5475916277511,253.800023548159,27.0197271316055)) ;
#103465 = CARTESIAN_POINT('Ctrl Pts',(35.5370091274324,253.828041657271,27.0431407641495)) ;
#103466 = CARTESIAN_POINT('Ctrl Pts',(35.5332364694245,253.841958224525,27.0515181361211)) ;
#103467 = CARTESIAN_POINT('Ctrl Pts',(35.5284685425009,253.870954690135,27.0621166715429)) ;
#103468 = CARTESIAN_POINT('Ctrl Pts',(35.5272786630106,253.885320776746,27.0647672615988)) ;
#103469 = CARTESIAN_POINT('Ctrl Pts',(35.5272786630106,253.9,27.0647672615988)) ;
#103470 = CARTESIAN_POINT('Origin',(40.2,253.9,25.0213203435596)) ;
#103471 = CARTESIAN_POINT('',(35.8002600262484,253.9,27.6005233528965)) ;
#103472 = CARTESIAN_POINT('Origin',(40.2,253.9,25.0213203435596)) ;
#103473 = CARTESIAN_POINT('',(35.9999382971499,253.75,27.6408587937931)) ;
#103474 = CARTESIAN_POINT('Origin',(40.2,253.75,25.0213203435596)) ;
#103475 = CARTESIAN_POINT('Ctrl Pts',(35.9999382971499,253.75,27.6408587937931)) ;
#103476 = CARTESIAN_POINT('Ctrl Pts',(35.999164119612,253.75,27.6407079681274)) ;
#103477 = CARTESIAN_POINT('Ctrl Pts',(35.9983899488536,253.750003330105,27.6405570783186)) ;
#103478 = CARTESIAN_POINT('Ctrl Pts',(35.9776662894844,253.750181671152,27.6365161805243)) ;
#103479 = CARTESIAN_POINT('Ctrl Pts',(35.9576497332976,253.752566842488,27.6325687175194)) ;
#103480 = CARTESIAN_POINT('Ctrl Pts',(35.9197126349983,253.761740190968,27.6250083928119)) ;
#103481 = CARTESIAN_POINT('Ctrl Pts',(35.9015709504458,253.768377217198,27.621354832958)) ;
#103482 = CARTESIAN_POINT('Ctrl Pts',(35.8659678602057,253.78721321578,27.6141229718641)) ;
#103483 = CARTESIAN_POINT('Ctrl Pts',(35.8486379179467,253.800023548159,27.6105637433868)) ;
#103484 = CARTESIAN_POINT('Ctrl Pts',(35.823475653699,253.828041657271,27.6053629780756)) ;
#103485 = CARTESIAN_POINT('Ctrl Pts',(35.8144807046667,253.841958224525,27.6034910268201)) ;
#103486 = CARTESIAN_POINT('Ctrl Pts',(35.8031037922653,253.870954690135,27.6011186979124)) ;
#103487 = CARTESIAN_POINT('Ctrl Pts',(35.8002600262485,253.885320776746,27.6005233528965)) ;
#103488 = CARTESIAN_POINT('Ctrl Pts',(35.8002600262485,253.9,27.6005233528965)) ;
#103489 = CARTESIAN_POINT('Origin',(37.7789755671721,253.9,26.3483125582154)) ;
#103490 = CARTESIAN_POINT('',(35.4752044197332,253.9,27.8366900749965)) ;
#103491 = CARTESIAN_POINT('',(37.6908077793282,253.9,26.2269600090591)) ;
#103492 = CARTESIAN_POINT('',(35.5603672117706,253.75,27.9602258814026)) ;
#103493 = CARTESIAN_POINT('',(37.7789755671721,253.75,26.3483125582154)) ;
#103494 = CARTESIAN_POINT('Ctrl Pts',(35.5603672117706,253.75,27.9602258814026)) ;
#103495 = CARTESIAN_POINT('Ctrl Pts',(35.5595422127747,253.75,27.9590229387353)) ;
#103496 = CARTESIAN_POINT('Ctrl Pts',(35.5587171553567,253.750021261236,27.957820129938)) ;
#103497 = CARTESIAN_POINT('Ctrl Pts',(35.5578923045725,253.750063777237,27.9566178371378)) ;
#103498 = CARTESIAN_POINT('Ctrl Pts',(35.5472956800808,253.750609968276,27.9411723219294)) ;
#103499 = CARTESIAN_POINT('Ctrl Pts',(35.5368331274772,253.754658837467,27.92595826731)) ;
#103500 = CARTESIAN_POINT('Ctrl Pts',(35.527053294334,253.762001431812,27.9117600448446)) ;
#103501 = CARTESIAN_POINT('Ctrl Pts',(35.5168578301213,253.769656077527,27.8969584151122)) ;
#103502 = CARTESIAN_POINT('Ctrl Pts',(35.5075954635632,253.78074710398,27.8835376386856)) ;
#103503 = CARTESIAN_POINT('Ctrl Pts',(35.499796184335,253.794651469056,27.8722475987309)) ;
#103504 = CARTESIAN_POINT('Ctrl Pts',(35.4919989918665,253.808552113907,27.860960579517)) ;
#103505 = CARTESIAN_POINT('Ctrl Pts',(35.4858134917465,253.824998688613,27.8520189483947)) ;
#103506 = CARTESIAN_POINT('Ctrl Pts',(35.4815944923177,253.843066458683,27.8459219612512)) ;
#103507 = CARTESIAN_POINT('Ctrl Pts',(35.4773760127934,253.861132002274,27.8398257254355)) ;
#103508 = CARTESIAN_POINT('Ctrl Pts',(35.4752044197331,253.880472526098,27.8366900749965)) ;
#103509 = CARTESIAN_POINT('Ctrl Pts',(35.4752044197332,253.9,27.8366900749965)) ;
#103510 = CARTESIAN_POINT('Origin',(35.7504065309378,253.9,28.2541392311682)) ;
#103511 = CARTESIAN_POINT('',(36.0623821418868,253.9,28.6448708758722)) ;
#103512 = CARTESIAN_POINT('Origin',(35.7504065309378,253.9,28.2541392311682)) ;
#103513 = CARTESIAN_POINT('',(35.9712093582363,253.75,28.5257015839659)) ;
#103514 = CARTESIAN_POINT('Origin',(35.7504065309378,253.75,28.2541392311682)) ;
#103515 = CARTESIAN_POINT('Ctrl Pts',(35.9712093582364,253.75,28.5257015839658)) ;
#103516 = CARTESIAN_POINT('Ctrl Pts',(35.9720984859886,253.75,28.5268579343639)) ;
#103517 = CARTESIAN_POINT('Ctrl Pts',(35.9729874683689,253.750021261236,28.5280142989583)) ;
#103518 = CARTESIAN_POINT('Ctrl Pts',(35.9738760238612,253.750063777237,28.5291703075783)) ;
#103519 = CARTESIAN_POINT('Ctrl Pts',(35.9852910447033,253.750609968276,28.5440212230314)) ;
#103520 = CARTESIAN_POINT('Ctrl Pts',(35.9965273639227,253.754658837467,28.5586731032995)) ;
#103521 = CARTESIAN_POINT('Ctrl Pts',(36.0070085412753,253.762001431812,28.5723617693703)) ;
#103522 = CARTESIAN_POINT('Ctrl Pts',(36.017935155977,253.769656077527,28.5866321871779)) ;
#103523 = CARTESIAN_POINT('Ctrl Pts',(36.0278368441769,253.78074710398,28.5995884692427)) ;
#103524 = CARTESIAN_POINT('Ctrl Pts',(36.0361642004197,253.794651469056,28.6104948387884)) ;
#103525 = CARTESIAN_POINT('Ctrl Pts',(36.0444893286114,253.808552113907,28.6213982902473)) ;
#103526 = CARTESIAN_POINT('Ctrl Pts',(36.0510819005004,253.824998688613,28.6300441664174)) ;
#103527 = CARTESIAN_POINT('Ctrl Pts',(36.0555767373301,253.843066458683,28.6359407459584)) ;
#103528 = CARTESIAN_POINT('Ctrl Pts',(36.0600710202639,253.861132002274,28.6418365988678)) ;
#103529 = CARTESIAN_POINT('Ctrl Pts',(36.0623821418869,253.880472526098,28.6448708758721)) ;
#103530 = CARTESIAN_POINT('Ctrl Pts',(36.0623821418868,253.9,28.6448708758721)) ;
#103531 = CARTESIAN_POINT('Origin',(38.4743212102356,253.9,26.7070843711341)) ;
#103532 = CARTESIAN_POINT('',(36.387437748402,253.9,28.4087041537722)) ;
#103533 = CARTESIAN_POINT('',(38.5624889980795,253.9,26.8284369202904)) ;
#103534 = CARTESIAN_POINT('',(36.4107804436157,253.75,28.2063344963562)) ;
#103535 = CARTESIAN_POINT('',(38.4743212102356,253.75,26.7070843711341)) ;
#103536 = CARTESIAN_POINT('Ctrl Pts',(36.4107804436157,253.75,28.2063344963562)) ;
#103537 = CARTESIAN_POINT('Ctrl Pts',(36.4106846533323,253.75,28.2071173906402)) ;
#103538 = CARTESIAN_POINT('Ctrl Pts',(36.4105889261468,253.750003330106,28.2079002983041)) ;
#103539 = CARTESIAN_POINT('Ctrl Pts',(36.408028085395,253.750181671152,28.228858375676)) ;
#103540 = CARTESIAN_POINT('Ctrl Pts',(36.4055968897784,253.752566842488,28.2491150850256)) ;
#103541 = CARTESIAN_POINT('Ctrl Pts',(36.4010639777649,253.761740190968,28.2875316783901)) ;
#103542 = CARTESIAN_POINT('Ctrl Pts',(36.3989326308384,253.768377217198,28.3059144577853)) ;
#103543 = CARTESIAN_POINT('Ctrl Pts',(36.3948085795202,253.78721321578,28.3420097767375)) ;
#103544 = CARTESIAN_POINT('Ctrl Pts',(36.3928383602869,253.800023548159,28.3595913933363)) ;
#103545 = CARTESIAN_POINT('Ctrl Pts',(36.3900090147564,253.828041657271,28.3851292535788)) ;
#103546 = CARTESIAN_POINT('Ctrl Pts',(36.3890097540816,253.841958224525,28.3942624232202)) ;
#103547 = CARTESIAN_POINT('Ctrl Pts',(36.3877503136725,253.870954690135,28.4058155998437)) ;
#103548 = CARTESIAN_POINT('Ctrl Pts',(36.387437748402,253.885320776746,28.4087041537722)) ;
#103549 = CARTESIAN_POINT('Ctrl Pts',(36.387437748402,253.9,28.4087041537722)) ;
#103550 = CARTESIAN_POINT('Origin',(40.2,253.9,25.0213203435596)) ;
#103551 = CARTESIAN_POINT('',(36.8126161897874,253.9,28.8338825951576)) ;
#103552 = CARTESIAN_POINT('Origin',(40.2,253.9,25.0213203435596)) ;
#103553 = CARTESIAN_POINT('',(37.0149858472034,253.75,28.8105398999439)) ;
#103554 = CARTESIAN_POINT('Origin',(40.2,253.75,25.0213203435596)) ;
#103555 = CARTESIAN_POINT('Ctrl Pts',(37.0149858472034,253.75,28.8105398999439)) ;
#103556 = CARTESIAN_POINT('Ctrl Pts',(37.0142029529195,253.75,28.8106356902274)) ;
#103557 = CARTESIAN_POINT('Ctrl Pts',(37.0134200452556,253.750003330106,28.8107314174129)) ;
#103558 = CARTESIAN_POINT('Ctrl Pts',(36.9924619678827,253.750181671152,28.8132922581644)) ;
#103559 = CARTESIAN_POINT('Ctrl Pts',(36.9722052585338,253.752566842488,28.8157234537813)) ;
#103560 = CARTESIAN_POINT('Ctrl Pts',(36.9337886651694,253.761740190968,28.8202563657947)) ;
#103561 = CARTESIAN_POINT('Ctrl Pts',(36.9154058857743,253.768377217198,28.8223877127213)) ;
#103562 = CARTESIAN_POINT('Ctrl Pts',(36.8793105668222,253.78721321578,28.8265117640394)) ;
#103563 = CARTESIAN_POINT('Ctrl Pts',(36.8617289502234,253.800023548159,28.8284819832727)) ;
#103564 = CARTESIAN_POINT('Ctrl Pts',(36.8361910899809,253.828041657271,28.8313113288033)) ;
#103565 = CARTESIAN_POINT('Ctrl Pts',(36.8270579203394,253.841958224525,28.832310589478)) ;
#103566 = CARTESIAN_POINT('Ctrl Pts',(36.815504743716,253.870954690135,28.8335700298872)) ;
#103567 = CARTESIAN_POINT('Ctrl Pts',(36.8126161897874,253.885320776746,28.8338825951576)) ;
#103568 = CARTESIAN_POINT('Ctrl Pts',(36.8126161897874,253.9,28.8338825951576)) ;
#103569 = CARTESIAN_POINT('Origin',(38.3075320827811,253.9,27.0315026299217)) ;
#103570 = CARTESIAN_POINT('',(36.5764494676875,253.9,29.1589382016729)) ;
#103571 = CARTESIAN_POINT('',(38.1861795336248,253.9,26.9433348420779)) ;
#103572 = CARTESIAN_POINT('',(36.6956187595936,253.75,29.2501109853235)) ;
#103573 = CARTESIAN_POINT('',(38.3075320827811,253.75,27.0315026299217)) ;
#103574 = CARTESIAN_POINT('Ctrl Pts',(36.6956187595936,253.75,29.2501109853235)) ;
#103575 = CARTESIAN_POINT('Ctrl Pts',(36.6944624091953,253.75,29.2492218575712)) ;
#103576 = CARTESIAN_POINT('Ctrl Pts',(36.693306044602,253.750021261236,29.2483328751903)) ;
#103577 = CARTESIAN_POINT('Ctrl Pts',(36.6921500359814,253.750063777237,29.2474443196982)) ;
#103578 = CARTESIAN_POINT('Ctrl Pts',(36.6772991205231,253.750609968276,29.2360292988605)) ;
#103579 = CARTESIAN_POINT('Ctrl Pts',(36.6626472402606,253.754658837467,29.2247929796359)) ;
#103580 = CARTESIAN_POINT('Ctrl Pts',(36.6489585741898,253.762001431812,29.2143118022838)) ;
#103581 = CARTESIAN_POINT('Ctrl Pts',(36.6346881563818,253.769656077527,29.2033851875823)) ;
#103582 = CARTESIAN_POINT('Ctrl Pts',(36.6217318743171,253.78074710398,29.1934834993824)) ;
#103583 = CARTESIAN_POINT('Ctrl Pts',(36.6108255047715,253.794651469056,29.1851561431397)) ;
#103584 = CARTESIAN_POINT('Ctrl Pts',(36.5999220533126,253.808552113907,29.176831014948)) ;
#103585 = CARTESIAN_POINT('Ctrl Pts',(36.5912761771423,253.824998688613,29.1702384430592)) ;
#103586 = CARTESIAN_POINT('Ctrl Pts',(36.5853795976013,253.843066458683,29.1657436062294)) ;
#103587 = CARTESIAN_POINT('Ctrl Pts',(36.579483744692,253.861132002274,29.1612493232954)) ;
#103588 = CARTESIAN_POINT('Ctrl Pts',(36.5764494676874,253.880472526098,29.1589382016731)) ;
#103589 = CARTESIAN_POINT('Ctrl Pts',(36.5764494676874,253.9,29.158938201673)) ;
#103590 = CARTESIAN_POINT('Origin',(36.9671811123914,253.9,29.4709138126218)) ;
#103591 = CARTESIAN_POINT('',(37.3846302685632,253.9,29.7461159238265)) ;
#103592 = CARTESIAN_POINT('Origin',(36.9671811123914,253.9,29.4709138126218)) ;
#103593 = CARTESIAN_POINT('',(37.2610944621571,253.75,29.6609531317891)) ;
#103594 = CARTESIAN_POINT('Origin',(36.9671811123914,253.75,29.4709138126218)) ;
#103595 = CARTESIAN_POINT('Ctrl Pts',(37.2610944621618,253.75,29.6609531317925)) ;
#103596 = CARTESIAN_POINT('Ctrl Pts',(37.2622974048275,253.75,29.6617781307873)) ;
#103597 = CARTESIAN_POINT('Ctrl Pts',(37.2635002136233,253.750021261236,29.6626031882038)) ;
#103598 = CARTESIAN_POINT('Ctrl Pts',(37.2647025064218,253.750063777237,29.663428038987)) ;
#103599 = CARTESIAN_POINT('Ctrl Pts',(37.2801480216301,253.750609968276,29.6740246634796)) ;
#103600 = CARTESIAN_POINT('Ctrl Pts',(37.2953620762498,253.754658837467,29.6844872160823)) ;
#103601 = CARTESIAN_POINT('Ctrl Pts',(37.3095602987151,253.762001431812,29.6942670492256)) ;
#103602 = CARTESIAN_POINT('Ctrl Pts',(37.3243619284475,253.769656077527,29.7044625134383)) ;
#103603 = CARTESIAN_POINT('Ctrl Pts',(37.337782704874,253.78074710398,29.7137248799965)) ;
#103604 = CARTESIAN_POINT('Ctrl Pts',(37.3490727448287,253.794651469056,29.7215241592247)) ;
#103605 = CARTESIAN_POINT('Ctrl Pts',(37.3603597640426,253.808552113907,29.7293213516932)) ;
#103606 = CARTESIAN_POINT('Ctrl Pts',(37.3693013951648,253.824998688613,29.7355068518133)) ;
#103607 = CARTESIAN_POINT('Ctrl Pts',(37.3753983823083,253.843066458683,29.7397258512422)) ;
#103608 = CARTESIAN_POINT('Ctrl Pts',(37.3814946181241,253.861132002274,29.7439443307665)) ;
#103609 = CARTESIAN_POINT('Ctrl Pts',(37.3846302685631,253.880472526098,29.7461159238265)) ;
#103610 = CARTESIAN_POINT('Ctrl Pts',(37.3846302685632,253.9,29.7461159238264)) ;
#103611 = CARTESIAN_POINT('Origin',(39.0797116749887,253.9,27.1578412797899)) ;
#103612 = CARTESIAN_POINT('',(39.201064224145,253.9,27.2460090676338)) ;
#103613 = CARTESIAN_POINT('',(39.0797116749887,253.75,27.1578412797899)) ;
#103614 = CARTESIAN_POINT('Origin',(42.3676071114944,258.25,19.9664732232009)) ;
#103615 = CARTESIAN_POINT('',(42.3676071114944,258.1,19.9664732232009)) ;
#103616 = CARTESIAN_POINT('',(42.3676071114944,258.25,19.9664732232009)) ;
#103617 = CARTESIAN_POINT('',(42.2434469180392,258.1,20.3485990065702)) ;
#103618 = CARTESIAN_POINT('',(41.5213219337175,258.1,22.5710711826001)) ;
#103619 = CARTESIAN_POINT('',(42.2434469180392,258.25,20.3485990065702)) ;
#103620 = CARTESIAN_POINT('Origin',(41.8995934690622,258.25,19.7905095039363)) ;
#103621 = CARTESIAN_POINT('',(41.4175335996131,258.1,19.6577756263215)) ;
#103622 = CARTESIAN_POINT('',(41.4175335996131,258.25,19.6577756263215)) ;
#103623 = CARTESIAN_POINT('Origin',(41.8995934690622,258.1,19.7905095039363)) ;
#103624 = CARTESIAN_POINT('Origin',(41.2001922680488,258.25,20.3266834644245)) ;
#103625 = CARTESIAN_POINT('',(41.2933734061579,258.1,20.0399014096908)) ;
#103626 = CARTESIAN_POINT('',(41.2933734061579,258.25,20.0399014096908)) ;
#103627 = CARTESIAN_POINT('',(40.4625777560541,258.1,22.5968275047722)) ;
#103628 = CARTESIAN_POINT('Origin',(40.2,258.25,25.0213203435596)) ;
#103629 = CARTESIAN_POINT('',(40.6994832039963,258.1,19.9458384424072)) ;
#103630 = CARTESIAN_POINT('',(40.6994832039963,258.25,19.9458384424072)) ;
#103631 = CARTESIAN_POINT('Origin',(40.2,258.1,25.0213203435596)) ;
#103632 = CARTESIAN_POINT('Origin',(40.6994832039963,258.25,19.5440476162869)) ;
#103633 = CARTESIAN_POINT('',(40.6994832039963,258.1,19.5440476162869)) ;
#103634 = CARTESIAN_POINT('',(40.6994832039963,258.25,19.5440476162869)) ;
#103635 = CARTESIAN_POINT('',(40.6994832039963,258.1,22.2826839799233)) ;
#103636 = CARTESIAN_POINT('Origin',(40.2,258.25,19.5213203435596)) ;
#103637 = CARTESIAN_POINT('',(39.7005167960037,258.1,19.5440476162869)) ;
#103638 = CARTESIAN_POINT('',(39.7005167960037,258.25,19.5440476162869)) ;
#103639 = CARTESIAN_POINT('Origin',(40.2,258.1,19.5213203435596)) ;
#103640 = CARTESIAN_POINT('Origin',(39.7005167960037,258.25,20.2473789395491)) ;
#103641 = CARTESIAN_POINT('',(39.7005167960037,258.1,19.9458384424072)) ;
#103642 = CARTESIAN_POINT('',(39.7005167960037,258.25,19.9458384424072)) ;
#103643 = CARTESIAN_POINT('',(39.7005167960037,258.1,22.6343496415544)) ;
#103644 = CARTESIAN_POINT('Origin',(40.2,258.25,25.0213203435596)) ;
#103645 = CARTESIAN_POINT('',(39.1066265938421,258.1,20.0399014096908)) ;
#103646 = CARTESIAN_POINT('',(39.1066265938421,258.25,20.0399014096908)) ;
#103647 = CARTESIAN_POINT('Origin',(40.2,258.1,25.0213203435596)) ;
#103648 = CARTESIAN_POINT('Origin',(38.982466400387,258.25,19.6577756263215)) ;
#103649 = CARTESIAN_POINT('',(38.982466400387,258.1,19.6577756263215)) ;
#103650 = CARTESIAN_POINT('',(38.982466400387,258.25,19.6577756263215)) ;
#103651 = CARTESIAN_POINT('',(39.8287515781638,258.1,22.2623735857207)) ;
#103652 = CARTESIAN_POINT('Origin',(38.5004065309378,258.25,19.7905095039363)) ;
#103653 = CARTESIAN_POINT('',(38.0323928885057,258.1,19.9664732232009)) ;
#103654 = CARTESIAN_POINT('',(38.0323928885057,258.25,19.9664732232009)) ;
#103655 = CARTESIAN_POINT('Origin',(38.5004065309378,258.1,19.7905095039363)) ;
#103656 = CARTESIAN_POINT('Origin',(38.2497342200699,258.25,20.6353810613039)) ;
#103657 = CARTESIAN_POINT('',(38.1565530819608,258.1,20.3485990065702)) ;
#103658 = CARTESIAN_POINT('',(38.1565530819608,258.25,20.3485990065702)) ;
#103659 = CARTESIAN_POINT('',(38.9873487320647,258.1,22.9055251016516)) ;
#103660 = CARTESIAN_POINT('Origin',(40.2,258.25,25.0213203435596)) ;
#103661 = CARTESIAN_POINT('',(37.6207969906631,258.1,20.6215803698081)) ;
#103662 = CARTESIAN_POINT('',(37.6207969906631,258.25,20.6215803698081)) ;
#103663 = CARTESIAN_POINT('Origin',(40.2,258.1,25.0213203435596)) ;
#103664 = CARTESIAN_POINT('Origin',(37.3846302685632,258.25,20.2965247632928)) ;
#103665 = CARTESIAN_POINT('',(37.3846302685632,258.1,20.2965247632928)) ;
#103666 = CARTESIAN_POINT('',(37.3846302685632,258.25,20.2965247632928)) ;
#103667 = CARTESIAN_POINT('',(38.9943603345005,258.1,22.5121281228878)) ;
#103668 = CARTESIAN_POINT('Origin',(36.9671811123914,258.25,20.5717268744974)) ;
#103669 = CARTESIAN_POINT('',(36.5764494676875,258.1,20.8837024854464)) ;
#103670 = CARTESIAN_POINT('',(36.5764494676875,258.25,20.8837024854464)) ;
#103671 = CARTESIAN_POINT('Origin',(36.9671811123914,258.1,20.5717268744974)) ;
#103672 = CARTESIAN_POINT('Origin',(36.9898572469764,258.25,21.4527094786418)) ;
#103673 = CARTESIAN_POINT('',(36.8126161897874,258.1,21.2087580919617)) ;
#103674 = CARTESIAN_POINT('',(36.8126161897874,258.25,21.2087580919617)) ;
#103675 = CARTESIAN_POINT('',(38.3928834232693,258.1,23.3838093416391)) ;
#103676 = CARTESIAN_POINT('Origin',(40.2,258.25,25.0213203435596)) ;
#103677 = CARTESIAN_POINT('',(36.3874377484021,258.1,21.633936533347)) ;
#103678 = CARTESIAN_POINT('',(36.3874377484021,258.25,21.633936533347)) ;
#103679 = CARTESIAN_POINT('Origin',(40.2,258.1,25.0213203435596)) ;
#103680 = CARTESIAN_POINT('Origin',(36.0623821418868,258.25,21.3977698112471)) ;
#103681 = CARTESIAN_POINT('',(36.0623821418868,258.1,21.3977698112471)) ;
#103682 = CARTESIAN_POINT('',(36.0623821418868,258.25,21.3977698112471)) ;
#103683 = CARTESIAN_POINT('',(38.2779855014818,258.1,23.0074998771845)) ;
#103684 = CARTESIAN_POINT('Origin',(35.7504065309378,258.25,21.788501455951)) ;
#103685 = CARTESIAN_POINT('',(35.4752044197332,258.1,22.2059506121228)) ;
#103686 = CARTESIAN_POINT('',(35.4752044197332,258.25,22.2059506121228)) ;
#103687 = CARTESIAN_POINT('Origin',(35.7504065309378,258.1,21.788501455951)) ;
#103688 = CARTESIAN_POINT('Origin',(36.0442114129285,258.25,22.6193583914117)) ;
#103689 = CARTESIAN_POINT('',(35.8002600262485,258.1,22.4421173342227)) ;
#103690 = CARTESIAN_POINT('',(35.8002600262485,258.25,22.4421173342227)) ;
#103691 = CARTESIAN_POINT('',(37.9753112759259,258.1,24.0223845677046)) ;
#103692 = CARTESIAN_POINT('Origin',(40.2,258.25,25.0213203435596)) ;
#103693 = CARTESIAN_POINT('',(35.5272786630106,258.1,22.9778734255204)) ;
#103694 = CARTESIAN_POINT('',(35.5272786630106,258.25,22.9778734255204)) ;
#103695 = CARTESIAN_POINT('Origin',(40.2,258.1,25.0213203435596)) ;
#103696 = CARTESIAN_POINT('Origin',(35.1451528796413,258.25,22.8537132320653)) ;
#103697 = CARTESIAN_POINT('',(35.1451528796413,258.1,22.8537132320653)) ;
#103698 = CARTESIAN_POINT('',(35.1451528796413,258.25,22.8537132320653)) ;
#103699 = CARTESIAN_POINT('',(37.7497508390405,258.1,23.6999984098422)) ;
#103700 = CARTESIAN_POINT('Origin',(34.9691891603767,258.25,23.3217268744974)) ;
#103701 = CARTESIAN_POINT('',(34.8364552827619,258.1,23.8037867439466)) ;
#103702 = CARTESIAN_POINT('',(34.8364552827619,258.25,23.8037867439466)) ;
#103703 = CARTESIAN_POINT('Origin',(34.9691891603767,258.1,23.3217268744974)) ;
#103704 = CARTESIAN_POINT('Origin',(35.5053631208649,258.25,24.0211280755108)) ;
#103705 = CARTESIAN_POINT('',(35.2185810661312,258.1,23.9279469374017)) ;
#103706 = CARTESIAN_POINT('',(35.2185810661312,258.25,23.9279469374017)) ;
#103707 = CARTESIAN_POINT('',(37.7755071612126,258.1,24.7587425875056)) ;
#103708 = CARTESIAN_POINT('Origin',(40.2,258.25,25.0213203435596)) ;
#103709 = CARTESIAN_POINT('',(35.1245180988476,258.1,24.5218371395634)) ;
#103710 = CARTESIAN_POINT('',(35.1245180988476,258.25,24.5218371395634)) ;
#103711 = CARTESIAN_POINT('Origin',(40.2,258.1,25.0213203435596)) ;
#103712 = CARTESIAN_POINT('Origin',(34.7227272727273,258.25,24.5218371395634)) ;
#103713 = CARTESIAN_POINT('',(34.7227272727273,258.1,24.5218371395634)) ;
#103714 = CARTESIAN_POINT('',(34.7227272727273,258.25,24.5218371395634)) ;
#103715 = CARTESIAN_POINT('',(37.4613636363637,258.1,24.5218371395634)) ;
#103716 = CARTESIAN_POINT('Origin',(34.7,258.25,25.0213203435596)) ;
#103717 = CARTESIAN_POINT('',(34.7227272727273,258.1,25.5208035475559)) ;
#103718 = CARTESIAN_POINT('',(34.7227272727273,258.25,25.5208035475559)) ;
#103719 = CARTESIAN_POINT('Origin',(34.7,258.1,25.0213203435596)) ;
#103720 = CARTESIAN_POINT('Origin',(35.4260585959895,258.25,25.5208035475559)) ;
#103721 = CARTESIAN_POINT('',(35.1245180988476,258.1,25.5208035475559)) ;
#103722 = CARTESIAN_POINT('',(35.1245180988476,258.25,25.5208035475559)) ;
#103723 = CARTESIAN_POINT('',(37.8130292979948,258.1,25.5208035475559)) ;
#103724 = CARTESIAN_POINT('Origin',(40.2,258.25,25.0213203435596)) ;
#103725 = CARTESIAN_POINT('',(35.2185810661312,258.1,26.1146937497175)) ;
#103726 = CARTESIAN_POINT('',(35.2185810661312,258.25,26.1146937497175)) ;
#103727 = CARTESIAN_POINT('Origin',(40.2,258.1,25.0213203435596)) ;
#103728 = CARTESIAN_POINT('Origin',(34.8364552827619,258.25,26.2388539431727)) ;
#103729 = CARTESIAN_POINT('',(34.8364552827619,258.1,26.2388539431727)) ;
#103730 = CARTESIAN_POINT('',(34.8364552827619,258.25,26.2388539431727)) ;
#103731 = CARTESIAN_POINT('',(37.4410532421611,258.1,25.3925687653958)) ;
#103732 = CARTESIAN_POINT('Origin',(34.9691891603767,258.25,26.7209138126218)) ;
#103733 = CARTESIAN_POINT('',(35.1451528796413,258.1,27.188927455054)) ;
#103734 = CARTESIAN_POINT('',(35.1451528796413,258.25,27.188927455054)) ;
#103735 = CARTESIAN_POINT('Origin',(34.9691891603767,258.1,26.7209138126218)) ;
#103736 = CARTESIAN_POINT('Origin',(35.8140607177443,258.25,26.9715861234897)) ;
#103737 = CARTESIAN_POINT('',(35.5272786630106,258.1,27.0647672615988)) ;
#103738 = CARTESIAN_POINT('',(35.5272786630106,258.25,27.0647672615988)) ;
#103739 = CARTESIAN_POINT('',(38.084204758092,258.1,26.233971611495)) ;
#103740 = CARTESIAN_POINT('Origin',(40.2,258.25,25.0213203435596)) ;
#103741 = CARTESIAN_POINT('',(35.8002600262484,258.1,27.6005233528965)) ;
#103742 = CARTESIAN_POINT('',(35.8002600262484,258.25,27.6005233528965)) ;
#103743 = CARTESIAN_POINT('Origin',(40.2,258.1,25.0213203435596)) ;
#103744 = CARTESIAN_POINT('Origin',(35.4752044197332,258.25,27.8366900749965)) ;
#103745 = CARTESIAN_POINT('',(35.4752044197332,258.1,27.8366900749965)) ;
#103746 = CARTESIAN_POINT('',(35.4752044197332,258.25,27.8366900749965)) ;
#103747 = CARTESIAN_POINT('',(37.6908077793282,258.1,26.2269600090591)) ;
#103748 = CARTESIAN_POINT('Origin',(35.7504065309378,258.25,28.2541392311682)) ;
#103749 = CARTESIAN_POINT('',(36.0623821418868,258.1,28.6448708758722)) ;
#103750 = CARTESIAN_POINT('',(36.0623821418868,258.25,28.6448708758722)) ;
#103751 = CARTESIAN_POINT('Origin',(35.7504065309378,258.1,28.2541392311682)) ;
#103752 = CARTESIAN_POINT('Origin',(36.6313891350821,258.25,28.2314630965833)) ;
#103753 = CARTESIAN_POINT('',(36.387437748402,258.1,28.4087041537722)) ;
#103754 = CARTESIAN_POINT('',(36.387437748402,258.25,28.4087041537722)) ;
#103755 = CARTESIAN_POINT('',(38.5624889980795,258.1,26.8284369202904)) ;
#103756 = CARTESIAN_POINT('Origin',(40.2,258.25,25.0213203435596)) ;
#103757 = CARTESIAN_POINT('',(36.8126161897874,258.1,28.8338825951576)) ;
#103758 = CARTESIAN_POINT('',(36.8126161897874,258.25,28.8338825951576)) ;
#103759 = CARTESIAN_POINT('Origin',(40.2,258.1,25.0213203435596)) ;
#103760 = CARTESIAN_POINT('Origin',(36.5764494676875,258.25,29.1589382016729)) ;
#103761 = CARTESIAN_POINT('',(36.5764494676875,258.1,29.1589382016729)) ;
#103762 = CARTESIAN_POINT('',(36.5764494676875,258.25,29.1589382016729)) ;
#103763 = CARTESIAN_POINT('',(38.1861795336248,258.1,26.9433348420779)) ;
#103764 = CARTESIAN_POINT('Origin',(36.9671811123914,258.25,29.4709138126218)) ;
#103765 = CARTESIAN_POINT('',(37.3846302685632,258.1,29.7461159238265)) ;
#103766 = CARTESIAN_POINT('',(37.3846302685632,258.25,29.7461159238265)) ;
#103767 = CARTESIAN_POINT('Origin',(36.9671811123914,258.1,29.4709138126218)) ;
#103768 = CARTESIAN_POINT('Origin',(37.7980380478521,258.25,29.1771089306311)) ;
#103769 = CARTESIAN_POINT('',(37.6207969906631,258.1,29.4210603173112)) ;
#103770 = CARTESIAN_POINT('',(37.6207969906631,258.25,29.4210603173112)) ;
#103771 = CARTESIAN_POINT('',(39.201064224145,258.1,27.2460090676338)) ;
#103772 = CARTESIAN_POINT('Origin',(40.2,258.25,25.0213203435596)) ;
#103773 = CARTESIAN_POINT('',(38.1565530819608,258.1,29.694041680549)) ;
#103774 = CARTESIAN_POINT('',(38.1565530819608,258.25,29.694041680549)) ;
#103775 = CARTESIAN_POINT('Origin',(40.2,258.1,25.0213203435596)) ;
#103776 = CARTESIAN_POINT('Origin',(40.2,253.75,25.0213203435596)) ;
#103777 = CARTESIAN_POINT('Origin',(40.2,253.75,25.0213203435596)) ;
#103778 = CARTESIAN_POINT('Origin',(40.2,253.75,25.0213203435596)) ;
#103779 = CARTESIAN_POINT('Origin',(40.2,253.75,25.0213203435596)) ;
#103780 = CARTESIAN_POINT('Origin',(40.2,253.75,25.0213203435596)) ;
#103781 = CARTESIAN_POINT('Origin',(40.2,253.75,25.0213203435596)) ;
#103782 = CARTESIAN_POINT('Origin',(40.2,253.75,25.0213203435596)) ;
#103783 = CARTESIAN_POINT('Origin',(40.2,253.75,25.0213203435596)) ;
#103784 = CARTESIAN_POINT('Origin',(40.2,253.75,25.0213203435596)) ;
#103785 = CARTESIAN_POINT('Origin',(40.2,253.75,25.0213203435596)) ;
#103786 = CARTESIAN_POINT('Origin',(40.2,253.75,25.0213203435596)) ;
#103787 = CARTESIAN_POINT('Origin',(40.2,253.75,25.0213203435596)) ;
#103788 = CARTESIAN_POINT('Origin',(40.2,253.75,25.0213203435596)) ;
#103789 = CARTESIAN_POINT('Origin',(40.2,253.75,25.0213203435596)) ;
#103790 = CARTESIAN_POINT('Origin',(40.2,253.75,25.0213203435596)) ;
#103791 = CARTESIAN_POINT('Origin',(40.2,253.75,25.0213203435596)) ;
#103792 = CARTESIAN_POINT('Origin',(40.2,253.75,25.0213203435596)) ;
#103793 = CARTESIAN_POINT('Origin',(40.2,253.75,25.0213203435596)) ;
#103794 = CARTESIAN_POINT('Origin',(40.2,253.75,25.0213203435596)) ;
#103795 = CARTESIAN_POINT('Origin',(40.2,253.75,25.0213203435596)) ;
#103796 = CARTESIAN_POINT('Origin',(40.2,253.75,25.0213203435596)) ;
#103797 = CARTESIAN_POINT('Origin',(40.2,253.75,25.0213203435596)) ;
#103798 = CARTESIAN_POINT('Origin',(40.2,253.75,25.0213203435596)) ;
#103799 = CARTESIAN_POINT('Origin',(40.2,253.75,25.0213203435596)) ;
#103800 = CARTESIAN_POINT('Origin',(40.2,253.75,25.0213203435596)) ;
#103801 = CARTESIAN_POINT('Origin',(40.2,253.75,25.0213203435596)) ;
#103802 = CARTESIAN_POINT('Origin',(40.2,253.75,25.0213203435596)) ;
#103803 = CARTESIAN_POINT('Origin',(40.2,253.75,25.0213203435596)) ;
#103804 = CARTESIAN_POINT('Origin',(40.2,253.75,25.0213203435596)) ;
#103805 = CARTESIAN_POINT('Origin',(40.2,253.75,25.0213203435596)) ;
#103806 = CARTESIAN_POINT('Origin',(40.2,253.75,25.0213203435596)) ;
#103807 = CARTESIAN_POINT('Origin',(40.2,253.75,25.0213203435596)) ;
#103808 = CARTESIAN_POINT('Origin',(40.2,253.75,25.0213203435596)) ;
#103809 = CARTESIAN_POINT('Origin',(40.2,253.75,25.0213203435596)) ;
#103810 = CARTESIAN_POINT('Origin',(40.2,253.75,25.0213203435596)) ;
#103811 = CARTESIAN_POINT('Origin',(40.2,253.75,25.0213203435596)) ;
#103812 = CARTESIAN_POINT('Origin',(40.2,253.75,25.0213203435596)) ;
#103813 = CARTESIAN_POINT('',(40.2,253.75,29.9713203435596)) ;
#103814 = CARTESIAN_POINT('Origin',(40.2,253.75,25.0213203435596)) ;
#103815 = CARTESIAN_POINT('Origin',(40.2,253.75,25.0213203435596)) ;
#103816 = CARTESIAN_POINT('Origin',(40.2,253.6,25.0213203435596)) ;
#103817 = CARTESIAN_POINT('Origin',(40.2,253.6,29.9713203435596)) ;
#103818 = CARTESIAN_POINT('Origin',(40.2,253.75,25.0213203435596)) ;
#103819 = CARTESIAN_POINT('Origin',(40.2,253.75,25.0213203435596)) ;
#103820 = CARTESIAN_POINT('Origin',(40.2,258.4,25.0213203435596)) ;
#103821 = CARTESIAN_POINT('',(40.2,258.25,20.0713203435596)) ;
#103822 = CARTESIAN_POINT('Origin',(40.2,258.4,20.0713203435596)) ;
#103823 = CARTESIAN_POINT('',(39.8505167960037,258.25,20.0836729796702)) ;
#103824 = CARTESIAN_POINT('Origin',(40.2,258.25,25.0213203435596)) ;
#103825 = CARTESIAN_POINT('',(39.0065613308239,258.25,20.2173423936815)) ;
#103826 = CARTESIAN_POINT('Origin',(40.2,258.25,25.0213203435596)) ;
#103827 = CARTESIAN_POINT('',(38.3418047738312,258.25,20.4333348922484)) ;
#103828 = CARTESIAN_POINT('Origin',(40.2,258.25,25.0213203435596)) ;
#103829 = CARTESIAN_POINT('',(37.5804615497666,258.25,20.8212586407095)) ;
#103830 = CARTESIAN_POINT('Origin',(40.2,258.25,25.0213203435596)) ;
#103831 = CARTESIAN_POINT('',(37.0149858472034,258.25,21.2321007871753)) ;
#103832 = CARTESIAN_POINT('Origin',(40.2,258.25,25.0213203435596)) ;
#103833 = CARTESIAN_POINT('',(36.4107804436157,258.25,21.836306190763)) ;
#103834 = CARTESIAN_POINT('Origin',(40.2,258.25,25.0213203435596)) ;
#103835 = CARTESIAN_POINT('',(35.9999382971499,258.25,22.4017818933262)) ;
#103836 = CARTESIAN_POINT('Origin',(40.2,258.25,25.0213203435596)) ;
#103837 = CARTESIAN_POINT('',(35.6120145486888,258.25,23.1631251173908)) ;
#103838 = CARTESIAN_POINT('Origin',(40.2,258.25,25.0213203435596)) ;
#103839 = CARTESIAN_POINT('',(35.3960220501219,258.25,23.8278816743835)) ;
#103840 = CARTESIAN_POINT('Origin',(40.2,258.25,25.0213203435596)) ;
#103841 = CARTESIAN_POINT('',(35.2623526361106,258.25,24.6718371395634)) ;
#103842 = CARTESIAN_POINT('Origin',(40.2,258.25,25.0213203435596)) ;
#103843 = CARTESIAN_POINT('',(35.2623526361106,258.25,25.3708035475559)) ;
#103844 = CARTESIAN_POINT('Origin',(40.2,258.25,25.0213203435596)) ;
#103845 = CARTESIAN_POINT('',(35.3960220501219,258.25,26.2147590127358)) ;
#103846 = CARTESIAN_POINT('Origin',(40.2,258.25,25.0213203435596)) ;
#103847 = CARTESIAN_POINT('',(35.6120145486888,258.25,26.8795155697285)) ;
#103848 = CARTESIAN_POINT('Origin',(40.2,258.25,25.0213203435596)) ;
#103849 = CARTESIAN_POINT('',(35.9999382971499,258.25,27.6408587937931)) ;
#103850 = CARTESIAN_POINT('Origin',(40.2,258.25,25.0213203435596)) ;
#103851 = CARTESIAN_POINT('',(36.4107804436157,258.25,28.2063344963562)) ;
#103852 = CARTESIAN_POINT('Origin',(40.2,258.25,25.0213203435596)) ;
#103853 = CARTESIAN_POINT('',(37.0149858472034,258.25,28.8105398999439)) ;
#103854 = CARTESIAN_POINT('Origin',(40.2,258.25,25.0213203435596)) ;
#103855 = CARTESIAN_POINT('',(37.5804615497666,258.25,29.2213820464098)) ;
#103856 = CARTESIAN_POINT('Origin',(40.2,258.25,25.0213203435596)) ;
#103857 = CARTESIAN_POINT('',(38.3418047738312,258.25,29.6093057948708)) ;
#103858 = CARTESIAN_POINT('Origin',(40.2,258.25,25.0213203435596)) ;
#103859 = CARTESIAN_POINT('',(39.0065613308239,258.25,29.8252982934377)) ;
#103860 = CARTESIAN_POINT('Origin',(40.2,258.25,25.0213203435596)) ;
#103861 = CARTESIAN_POINT('',(39.8505167960038,258.25,29.9589677074491)) ;
#103862 = CARTESIAN_POINT('Origin',(40.2,258.25,25.0213203435596)) ;
#103863 = CARTESIAN_POINT('',(40.5494832039963,258.25,29.9589677074491)) ;
#103864 = CARTESIAN_POINT('Origin',(40.2,258.25,25.0213203435596)) ;
#103865 = CARTESIAN_POINT('',(41.3934386691762,258.25,29.8252982934377)) ;
#103866 = CARTESIAN_POINT('Origin',(40.2,258.25,25.0213203435596)) ;
#103867 = CARTESIAN_POINT('',(42.0581952261689,258.25,29.6093057948708)) ;
#103868 = CARTESIAN_POINT('Origin',(40.2,258.25,25.0213203435596)) ;
#103869 = CARTESIAN_POINT('',(42.8195384502335,258.25,29.2213820464098)) ;
#103870 = CARTESIAN_POINT('Origin',(40.2,258.25,25.0213203435596)) ;
#103871 = CARTESIAN_POINT('',(43.3850141527966,258.25,28.8105398999439)) ;
#103872 = CARTESIAN_POINT('Origin',(40.2,258.25,25.0213203435596)) ;
#103873 = CARTESIAN_POINT('',(43.9892195563843,258.25,28.2063344963563)) ;
#103874 = CARTESIAN_POINT('Origin',(40.2,258.25,25.0213203435596)) ;
#103875 = CARTESIAN_POINT('',(44.4000617028502,258.25,27.6408587937931)) ;
#103876 = CARTESIAN_POINT('Origin',(40.2,258.25,25.0213203435596)) ;
#103877 = CARTESIAN_POINT('',(44.7879854513112,258.25,26.8795155697285)) ;
#103878 = CARTESIAN_POINT('Origin',(40.2,258.25,25.0213203435596)) ;
#103879 = CARTESIAN_POINT('',(45.0039779498781,258.25,26.2147590127358)) ;
#103880 = CARTESIAN_POINT('Origin',(40.2,258.25,25.0213203435596)) ;
#103881 = CARTESIAN_POINT('',(45.1376473638895,258.25,25.3708035475559)) ;
#103882 = CARTESIAN_POINT('Origin',(40.2,258.25,25.0213203435596)) ;
#103883 = CARTESIAN_POINT('',(45.1376473638895,258.25,24.6718371395634)) ;
#103884 = CARTESIAN_POINT('Origin',(40.2,258.25,25.0213203435596)) ;
#103885 = CARTESIAN_POINT('',(45.0039779498781,258.25,23.8278816743835)) ;
#103886 = CARTESIAN_POINT('Origin',(40.2,258.25,25.0213203435596)) ;
#103887 = CARTESIAN_POINT('',(44.7879854513112,258.25,23.1631251173908)) ;
#103888 = CARTESIAN_POINT('Origin',(40.2,258.25,25.0213203435596)) ;
#103889 = CARTESIAN_POINT('',(44.4000617028502,258.25,22.4017818933262)) ;
#103890 = CARTESIAN_POINT('Origin',(40.2,258.25,25.0213203435596)) ;
#103891 = CARTESIAN_POINT('',(43.9892195563843,258.25,21.836306190763)) ;
#103892 = CARTESIAN_POINT('Origin',(40.2,258.25,25.0213203435596)) ;
#103893 = CARTESIAN_POINT('',(43.3850141527966,258.25,21.2321007871753)) ;
#103894 = CARTESIAN_POINT('Origin',(40.2,258.25,25.0213203435596)) ;
#103895 = CARTESIAN_POINT('',(42.8195384502335,258.25,20.8212586407095)) ;
#103896 = CARTESIAN_POINT('Origin',(40.2,258.25,25.0213203435596)) ;
#103897 = CARTESIAN_POINT('',(42.0581952261685,258.25,20.4333348922483)) ;
#103898 = CARTESIAN_POINT('Origin',(40.2,258.25,25.0213203435596)) ;
#103899 = CARTESIAN_POINT('',(41.3934386691762,258.25,20.2173423936815)) ;
#103900 = CARTESIAN_POINT('Origin',(40.2,258.25,25.0213203435596)) ;
#103901 = CARTESIAN_POINT('',(40.5494832039963,258.25,20.0836729796702)) ;
#103902 = CARTESIAN_POINT('Origin',(40.2,258.25,25.0213203435596)) ;
#103903 = CARTESIAN_POINT('Origin',(40.2,258.25,25.0213203435596)) ;
#103904 = CARTESIAN_POINT('Origin',(40.2,258.25,25.0213203435596)) ;
#103905 = CARTESIAN_POINT('',(42.2260964403124,258.25,19.9165880896072)) ;
#103906 = CARTESIAN_POINT('',(41.3786634562732,258.25,22.5247186334439)) ;
#103907 = CARTESIAN_POINT('',(41.5613398833194,258.25,19.700595591041)) ;
#103908 = CARTESIAN_POINT('Origin',(41.8995934690622,258.25,19.7905095039363)) ;
#103909 = CARTESIAN_POINT('',(40.6052362334984,258.25,22.6431800539285)) ;
#103910 = CARTESIAN_POINT('Origin',(40.2,258.25,25.0213203435596)) ;
#103911 = CARTESIAN_POINT('',(43.7043812404059,258.25,20.7925297017964)) ;
#103912 = CARTESIAN_POINT('',(42.0924679172189,258.25,23.0111380571975)) ;
#103913 = CARTESIAN_POINT('',(43.1389055378432,258.25,20.3816875553299)) ;
#103914 = CARTESIAN_POINT('Origin',(43.4328188876086,258.25,20.5717268744974)) ;
#103915 = CARTESIAN_POINT('',(41.3202883250113,258.25,22.8847994073294)) ;
#103916 = CARTESIAN_POINT('Origin',(40.2,258.25,25.0213203435596)) ;
#103917 = CARTESIAN_POINT('',(44.8396327882295,258.25,22.0824148057166)) ;
#103918 = CARTESIAN_POINT('',(42.621024432828,258.25,23.6943281289039)) ;
#103919 = CARTESIAN_POINT('',(44.428790641764,258.25,21.5169391031532)) ;
#103920 = CARTESIAN_POINT('Origin',(44.6495934690622,258.25,21.788501455951)) ;
#103921 = CARTESIAN_POINT('',(41.9256787897644,258.25,23.3355563159851)) ;
#103922 = CARTESIAN_POINT('Origin',(40.2,258.25,25.0213203435596)) ;
#103923 = CARTESIAN_POINT('',(45.5207247525196,258.25,23.6599804602399)) ;
#103924 = CARTESIAN_POINT('',(42.9125942086827,258.25,24.5074134442792)) ;
#103925 = CARTESIAN_POINT('',(45.3047322539521,258.25,22.9952239032473)) ;
#103926 = CARTESIAN_POINT('Origin',(45.4308108396234,258.25,23.3217268744974)) ;
#103927 = CARTESIAN_POINT('',(42.3621477910643,258.25,23.9513275530686)) ;
#103928 = CARTESIAN_POINT('Origin',(40.2,258.25,25.0213203435596)) ;
#103929 = CARTESIAN_POINT('',(45.6809871063617,258.25,25.3708035475559)) ;
#103930 = CARTESIAN_POINT('',(42.9386363636364,258.25,25.3708035475559)) ;
#103931 = CARTESIAN_POINT('',(45.6809871063617,258.25,24.6718371395634)) ;
#103932 = CARTESIAN_POINT('Origin',(45.7,258.25,25.0213203435596)) ;
#103933 = CARTESIAN_POINT('',(42.5869707020053,258.25,24.6718371395634)) ;
#103934 = CARTESIAN_POINT('Origin',(40.2,258.25,25.0213203435596)) ;
#103935 = CARTESIAN_POINT('',(45.3047322539528,258.25,27.0474167838721)) ;
#103936 = CARTESIAN_POINT('',(42.6966017101158,258.25,26.1999837998328)) ;
#103937 = CARTESIAN_POINT('',(45.5207247525189,258.25,26.3826602268791)) ;
#103938 = CARTESIAN_POINT('Origin',(45.4308108396234,258.25,26.7209138126218)) ;
#103939 = CARTESIAN_POINT('',(42.5781402896312,258.25,25.426556577058)) ;
#103940 = CARTESIAN_POINT('Origin',(40.2,258.25,25.0213203435596)) ;
#103941 = CARTESIAN_POINT('',(44.4287906417642,258.25,28.5257015839662)) ;
#103942 = CARTESIAN_POINT('',(42.2101822863621,258.25,26.9137882607786)) ;
#103943 = CARTESIAN_POINT('',(44.8396327882299,258.25,27.9602258814029)) ;
#103944 = CARTESIAN_POINT('Origin',(44.6495934690622,258.25,28.2541392311682)) ;
#103945 = CARTESIAN_POINT('',(42.3365209362303,258.25,26.1416086685709)) ;
#103946 = CARTESIAN_POINT('Origin',(40.2,258.25,25.0213203435596)) ;
#103947 = CARTESIAN_POINT('',(43.1389055378432,258.25,29.6609531317894)) ;
#103948 = CARTESIAN_POINT('',(41.5269922146558,258.25,27.4423447763876)) ;
#103949 = CARTESIAN_POINT('',(43.7043812404062,258.25,29.2501109853232)) ;
#103950 = CARTESIAN_POINT('Origin',(43.4328188876086,258.25,29.4709138126218)) ;
#103951 = CARTESIAN_POINT('',(41.8857640275745,258.25,26.746999133324)) ;
#103952 = CARTESIAN_POINT('Origin',(40.2,258.25,25.0213203435596)) ;
#103953 = CARTESIAN_POINT('',(41.5613398833195,258.25,30.3420450960785)) ;
#103954 = CARTESIAN_POINT('',(40.7139068992805,258.25,27.7339145522423)) ;
#103955 = CARTESIAN_POINT('',(42.2260964403121,258.25,30.1260525975113)) ;
#103956 = CARTESIAN_POINT('Origin',(41.8995934690622,258.25,30.252131183183)) ;
#103957 = CARTESIAN_POINT('',(41.2699927904911,258.25,27.1834681346239)) ;
#103958 = CARTESIAN_POINT('Origin',(40.2,258.25,25.0213203435596)) ;
#103959 = CARTESIAN_POINT('',(39.8505167960037,258.25,30.5023074499212)) ;
#103960 = CARTESIAN_POINT('',(39.8505167960037,258.25,27.759956707196)) ;
#103961 = CARTESIAN_POINT('',(40.5494832039963,258.25,30.5023074499214)) ;
#103962 = CARTESIAN_POINT('Origin',(40.2,258.25,30.5213203435596)) ;
#103963 = CARTESIAN_POINT('',(40.5494832039963,258.25,27.4082910455649)) ;
#103964 = CARTESIAN_POINT('Origin',(40.2,258.25,25.0213203435596)) ;
#103965 = CARTESIAN_POINT('',(38.1739035596877,258.25,30.1260525975118)) ;
#103966 = CARTESIAN_POINT('',(39.0213365437268,258.25,27.5179220536754)) ;
#103967 = CARTESIAN_POINT('',(38.8386601166806,258.25,30.3420450960783)) ;
#103968 = CARTESIAN_POINT('Origin',(38.5004065309378,258.25,30.252131183183)) ;
#103969 = CARTESIAN_POINT('',(39.7947637665017,258.25,27.3994606331908)) ;
#103970 = CARTESIAN_POINT('Origin',(40.2,258.25,25.0213203435596)) ;
#103971 = CARTESIAN_POINT('',(36.6956187595938,258.25,29.2501109853234)) ;
#103972 = CARTESIAN_POINT('',(38.3075320827811,258.25,27.0315026299217)) ;
#103973 = CARTESIAN_POINT('',(37.2610944621569,258.25,29.6609531317893)) ;
#103974 = CARTESIAN_POINT('Origin',(36.9671811123914,258.25,29.4709138126218)) ;
#103975 = CARTESIAN_POINT('',(39.0797116749887,258.25,27.1578412797899)) ;
#103976 = CARTESIAN_POINT('Origin',(40.2,258.25,25.0213203435596)) ;
#103977 = CARTESIAN_POINT('',(35.5603672117705,258.25,27.9602258814026)) ;
#103978 = CARTESIAN_POINT('',(37.7789755671721,258.25,26.3483125582154)) ;
#103979 = CARTESIAN_POINT('',(35.9712093582364,258.25,28.5257015839658)) ;
#103980 = CARTESIAN_POINT('Origin',(35.7504065309378,258.25,28.2541392311682)) ;
#103981 = CARTESIAN_POINT('',(38.4743212102356,258.25,26.7070843711341)) ;
#103982 = CARTESIAN_POINT('Origin',(40.2,258.25,25.0213203435596)) ;
#103983 = CARTESIAN_POINT('',(34.8792752474809,258.25,26.3826602268792)) ;
#103984 = CARTESIAN_POINT('',(37.4874057913173,258.25,25.5352272428401)) ;
#103985 = CARTESIAN_POINT('',(35.0952677460484,258.25,27.0474167838717)) ;
#103986 = CARTESIAN_POINT('Origin',(34.9691891603767,258.25,26.7209138126218)) ;
#103987 = CARTESIAN_POINT('',(38.0378522089358,258.25,26.0913131340507)) ;
#103988 = CARTESIAN_POINT('Origin',(40.2,258.25,25.0213203435596)) ;
#103989 = CARTESIAN_POINT('',(34.7190128936382,258.25,24.6718371395634)) ;
#103990 = CARTESIAN_POINT('',(37.4613636363637,258.25,24.6718371395634)) ;
#103991 = CARTESIAN_POINT('',(34.7190128936385,258.25,25.3708035475559)) ;
#103992 = CARTESIAN_POINT('Origin',(34.7,258.25,25.0213203435596)) ;
#103993 = CARTESIAN_POINT('',(37.8130292979948,258.25,25.3708035475559)) ;
#103994 = CARTESIAN_POINT('Origin',(40.2,258.25,25.0213203435596)) ;
#103995 = CARTESIAN_POINT('',(35.0952677460478,258.25,22.9952239032473)) ;
#103996 = CARTESIAN_POINT('',(37.7033982898842,258.25,23.8426568872864)) ;
#103997 = CARTESIAN_POINT('',(34.8792752474813,258.25,23.6599804602402)) ;
#103998 = CARTESIAN_POINT('Origin',(34.9691891603767,258.25,23.3217268744974)) ;
#103999 = CARTESIAN_POINT('',(37.8218597103689,258.25,24.6160841100613)) ;
#104000 = CARTESIAN_POINT('Origin',(40.2,258.25,25.0213203435596)) ;
#104001 = CARTESIAN_POINT('',(35.9712093582363,258.25,21.5169391031534)) ;
#104002 = CARTESIAN_POINT('',(38.1898177136379,258.25,23.1288524263407)) ;
#104003 = CARTESIAN_POINT('',(35.5603672117703,258.25,22.0824148057165)) ;
#104004 = CARTESIAN_POINT('Origin',(35.7504065309378,258.25,21.788501455951)) ;
#104005 = CARTESIAN_POINT('',(38.0634790637697,258.25,23.9010320185483)) ;
#104006 = CARTESIAN_POINT('Origin',(40.2,258.25,25.0213203435596)) ;
#104007 = CARTESIAN_POINT('',(37.261094462157,258.25,20.3816875553301)) ;
#104008 = CARTESIAN_POINT('',(38.8730077853443,258.25,22.6002959107317)) ;
#104009 = CARTESIAN_POINT('',(36.6956187595937,258.25,20.7925297017959)) ;
#104010 = CARTESIAN_POINT('Origin',(36.9671811123914,258.25,20.5717268744974)) ;
#104011 = CARTESIAN_POINT('',(38.5142359724255,258.25,23.2956415537952)) ;
#104012 = CARTESIAN_POINT('Origin',(40.2,258.25,25.0213203435596)) ;
#104013 = CARTESIAN_POINT('',(38.8386601166805,258.25,19.7005955910407)) ;
#104014 = CARTESIAN_POINT('',(39.6860931007195,258.25,22.3087261348769)) ;
#104015 = CARTESIAN_POINT('',(38.1739035596879,258.25,19.9165880896081)) ;
#104016 = CARTESIAN_POINT('Origin',(38.5004065309378,258.25,19.7905095039363)) ;
#104017 = CARTESIAN_POINT('',(39.1300072095089,258.25,22.8591725524954)) ;
#104018 = CARTESIAN_POINT('Origin',(40.2,258.25,25.0213203435596)) ;
#104019 = CARTESIAN_POINT('',(40.5494832039963,258.25,19.5403332371977)) ;
#104020 = CARTESIAN_POINT('',(40.5494832039963,258.25,22.2826839799233)) ;
#104021 = CARTESIAN_POINT('',(39.8505167960037,258.25,19.5403332371979)) ;
#104022 = CARTESIAN_POINT('Origin',(40.2,258.25,19.5213203435596)) ;
#104023 = CARTESIAN_POINT('',(39.8505167960037,258.25,22.6343496415544)) ;
#104024 = CARTESIAN_POINT('Origin',(40.2,258.1,25.0213203435596)) ;
#104025 = CARTESIAN_POINT('',(39.1066265938421,258.1,30.0027392774284)) ;
#104026 = CARTESIAN_POINT('Ctrl Pts',(39.0065613308239,258.25,29.8252982934377)) ;
#104027 = CARTESIAN_POINT('Ctrl Pts',(39.0069440085726,258.25,29.8259879723372)) ;
#104028 = CARTESIAN_POINT('Ctrl Pts',(39.00732674523,258.249996669895,29.8266776249678)) ;
#104029 = CARTESIAN_POINT('Ctrl Pts',(39.0175738303397,258.249818328848,29.8451382901616)) ;
#104030 = CARTESIAN_POINT('Ctrl Pts',(39.0275135467839,258.247433157512,29.8629553332033)) ;
#104031 = CARTESIAN_POINT('Ctrl Pts',(39.0464270509533,258.238259809031,29.8966993889314)) ;
#104032 = CARTESIAN_POINT('Ctrl Pts',(39.0555078816931,258.231622782802,29.9128241441561)) ;
#104033 = CARTESIAN_POINT('Ctrl Pts',(39.0733877502474,258.21278678422,29.9444499271496)) ;
#104034 = CARTESIAN_POINT('Ctrl Pts',(39.0821280243534,258.199976451841,29.9598318195758)) ;
#104035 = CARTESIAN_POINT('Ctrl Pts',(39.0948498133619,258.171958342729,29.9821554300886)) ;
#104036 = CARTESIAN_POINT('Ctrl Pts',(39.0994097369161,258.158041775475,29.9901316702287)) ;
#104037 = CARTESIAN_POINT('Ctrl Pts',(39.1051816150581,258.129045309865,30.0002186669547)) ;
#104038 = CARTESIAN_POINT('Ctrl Pts',(39.1066265938421,258.114679223254,30.0027392774284)) ;
#104039 = CARTESIAN_POINT('Ctrl Pts',(39.1066265938421,258.1,30.0027392774284)) ;
#104040 = CARTESIAN_POINT('',(39.7005167960037,258.1,30.096802244712)) ;
#104041 = CARTESIAN_POINT('Origin',(40.2,258.1,25.0213203435596)) ;
#104042 = CARTESIAN_POINT('Ctrl Pts',(39.8505167960038,258.25,29.9589677074491)) ;
#104043 = CARTESIAN_POINT('Ctrl Pts',(39.8499397253402,258.25,29.9595053771295)) ;
#104044 = CARTESIAN_POINT('Ctrl Pts',(39.849362606764,258.249996669894,29.9600430036272)) ;
#104045 = CARTESIAN_POINT('Ctrl Pts',(39.833912390428,258.249818328848,29.9744336161106)) ;
#104046 = CARTESIAN_POINT('Ctrl Pts',(39.8189533892428,258.247433157513,29.9883070896971)) ;
#104047 = CARTESIAN_POINT('Ctrl Pts',(39.7905380911752,258.238259809032,30.0145549995742)) ;
#104048 = CARTESIAN_POINT('Ctrl Pts',(39.7769188845312,258.231622782802,30.0270844220836)) ;
#104049 = CARTESIAN_POINT('Ctrl Pts',(39.7501412146258,258.21278678422,30.0516371458428)) ;
#104050 = CARTESIAN_POINT('Ctrl Pts',(39.7370754538178,258.199976451841,30.0635653016335)) ;
#104051 = CARTESIAN_POINT('Ctrl Pts',(39.7180779384581,258.171958342729,30.0808650678764)) ;
#104052 = CARTESIAN_POINT('Ctrl Pts',(39.7112763996935,258.158041775475,30.087041829166)) ;
#104053 = CARTESIAN_POINT('Ctrl Pts',(39.7026699639648,258.129045309865,30.0948515246967)) ;
#104054 = CARTESIAN_POINT('Ctrl Pts',(39.7005167960037,258.114679223254,30.096802244712)) ;
#104055 = CARTESIAN_POINT('Ctrl Pts',(39.7005167960037,258.1,30.096802244712)) ;
#104056 = CARTESIAN_POINT('Origin',(39.7947637665017,258.1,27.3994606331908)) ;
#104057 = CARTESIAN_POINT('',(38.982466400387,258.1,30.3848650607978)) ;
#104058 = CARTESIAN_POINT('Ctrl Pts',(38.8386601166806,258.25,30.3420450960783)) ;
#104059 = CARTESIAN_POINT('Ctrl Pts',(38.840059121853,258.25,30.3424579870217)) ;
#104060 = CARTESIAN_POINT('Ctrl Pts',(38.8414580177611,258.249978738764,30.3428709748965)) ;
#104061 = CARTESIAN_POINT('Ctrl Pts',(38.8428563590733,258.249936222763,30.343283925702)) ;
#104062 = CARTESIAN_POINT('Ctrl Pts',(38.860820454012,258.249390031724,30.3485889877858)) ;
#104063 = CARTESIAN_POINT('Ctrl Pts',(38.8785229863556,258.245341162533,30.3538380651872)) ;
#104064 = CARTESIAN_POINT('Ctrl Pts',(38.8950484329944,258.237998568189,30.3587517471949)) ;
#104065 = CARTESIAN_POINT('Ctrl Pts',(38.9122761911102,258.230343922473,30.3638742547396)) ;
#104066 = CARTESIAN_POINT('Ctrl Pts',(38.9279023366588,258.21925289602,30.3685360408185)) ;
#104067 = CARTESIAN_POINT('Ctrl Pts',(38.9410499125524,258.205348530944,30.3724647819377)) ;
#104068 = CARTESIAN_POINT('Ctrl Pts',(38.9541939707065,258.191447886093,30.3763924718908)) ;
#104069 = CARTESIAN_POINT('Ctrl Pts',(38.9646093919075,258.175001311387,30.3795121161122)) ;
#104070 = CARTESIAN_POINT('Ctrl Pts',(38.9717117137828,258.156933541317,30.3816405503696)) ;
#104071 = CARTESIAN_POINT('Ctrl Pts',(38.9788131604437,258.138867997726,30.3837687223414)) ;
#104072 = CARTESIAN_POINT('Ctrl Pts',(38.982466400387,258.119527473902,30.3848650607978)) ;
#104073 = CARTESIAN_POINT('Ctrl Pts',(38.982466400387,258.1,30.3848650607978)) ;
#104074 = CARTESIAN_POINT('',(39.9374222439459,258.1,27.445813182347)) ;
#104075 = CARTESIAN_POINT('Origin',(39.8505167960037,258.1,27.759956707196)) ;
#104076 = CARTESIAN_POINT('',(39.7005167960037,258.1,30.4985930708324)) ;
#104077 = CARTESIAN_POINT('',(39.7005167960037,258.1,27.759956707196)) ;
#104078 = CARTESIAN_POINT('Ctrl Pts',(39.7005167960037,258.1,30.4985930708323)) ;
#104079 = CARTESIAN_POINT('Ctrl Pts',(39.7005167960037,258.119527473902,30.4985930708323)) ;
#104080 = CARTESIAN_POINT('Ctrl Pts',(39.704330020872,258.138867997726,30.4986793042264)) ;
#104081 = CARTESIAN_POINT('Ctrl Pts',(39.7117415393001,258.156933541317,30.4988497601077)) ;
#104082 = CARTESIAN_POINT('Ctrl Pts',(39.7191539711575,258.175001311387,30.4990202369967)) ;
#104083 = CARTESIAN_POINT('Ctrl Pts',(39.7300236484414,258.191447886093,30.4992718211856)) ;
#104084 = CARTESIAN_POINT('Ctrl Pts',(39.7437381135435,258.205348530944,30.4995981034065)) ;
#104085 = CARTESIAN_POINT('Ctrl Pts',(39.757456249043,258.21925289602,30.4999244729501)) ;
#104086 = CARTESIAN_POINT('Ctrl Pts',(39.773758167714,258.230343922473,30.5003195954534)) ;
#104087 = CARTESIAN_POINT('Ctrl Pts',(39.7917256812165,258.237998568189,30.5007714713061)) ;
#104088 = CARTESIAN_POINT('Ctrl Pts',(39.8089607261725,258.245341162533,30.5012049258647)) ;
#104089 = CARTESIAN_POINT('Ctrl Pts',(39.8274188890354,258.249390031724,30.5016831399335)) ;
#104090 = CARTESIAN_POINT('Ctrl Pts',(39.8461431129254,258.249936222763,30.5021889366962)) ;
#104091 = CARTESIAN_POINT('Ctrl Pts',(39.847600623359,258.249978738764,30.5022283083713)) ;
#104092 = CARTESIAN_POINT('Ctrl Pts',(39.8490586727,258.25,30.50226781617)) ;
#104093 = CARTESIAN_POINT('Ctrl Pts',(39.8505167960037,258.25,30.5023074499212)) ;
#104094 = CARTESIAN_POINT('Origin',(39.0213365437268,258.1,27.5179220536754)) ;
#104095 = CARTESIAN_POINT('Ctrl Pts',(38.3418047738311,258.25,29.6093057948708)) ;
#104096 = CARTESIAN_POINT('Ctrl Pts',(38.3410897979463,258.25,29.6096388244826)) ;
#104097 = CARTESIAN_POINT('Ctrl Pts',(38.3403747898381,258.249996669894,29.6099717982194)) ;
#104098 = CARTESIAN_POINT('Ctrl Pts',(38.3212338170961,258.249818328848,29.6188837045809)) ;
#104099 = CARTESIAN_POINT('Ctrl Pts',(38.3027198224331,258.247433157512,29.6274555764537)) ;
#104100 = CARTESIAN_POINT('Ctrl Pts',(38.267584217826,258.238259809032,29.6436380121775)) ;
#104101 = CARTESIAN_POINT('Ctrl Pts',(38.2507597781159,258.231622782802,29.6513456347974)) ;
#104102 = CARTESIAN_POINT('Ctrl Pts',(38.2177054917619,258.21278678422,29.6664219076506)) ;
#104103 = CARTESIAN_POINT('Ctrl Pts',(38.2015932119542,258.199976451841,29.6737287158086)) ;
#104104 = CARTESIAN_POINT('Ctrl Pts',(38.1781795794102,258.171958342729,29.6843112161272)) ;
#104105 = CARTESIAN_POINT('Ctrl Pts',(38.1698022074386,258.158041775475,29.6880838741351)) ;
#104106 = CARTESIAN_POINT('Ctrl Pts',(38.1592036720168,258.129045309865,29.6928518010587)) ;
#104107 = CARTESIAN_POINT('Ctrl Pts',(38.1565530819608,258.114679223254,29.694041680549)) ;
#104108 = CARTESIAN_POINT('Ctrl Pts',(38.1565530819608,258.1,29.694041680549)) ;
#104109 = CARTESIAN_POINT('',(38.0323928885057,258.1,30.0761674639184)) ;
#104110 = CARTESIAN_POINT('',(38.8786780662825,258.1,27.4715695045192)) ;
#104111 = CARTESIAN_POINT('Ctrl Pts',(38.0323928885057,258.1,30.0761674639184)) ;
#104112 = CARTESIAN_POINT('Ctrl Pts',(38.0323928885057,258.119527473902,30.0761674639184)) ;
#104113 = CARTESIAN_POINT('Ctrl Pts',(38.0359928332805,258.138867997726,30.0774278280375)) ;
#104114 = CARTESIAN_POINT('Ctrl Pts',(38.0429889324131,258.156933541317,30.0798802263626)) ;
#104115 = CARTESIAN_POINT('Ctrl Pts',(38.0499858937768,258.175001311387,30.0823329269323)) ;
#104116 = CARTESIAN_POINT('Ctrl Pts',(38.0602458273977,258.191447886093,30.0859311127189)) ;
#104117 = CARTESIAN_POINT('Ctrl Pts',(38.0731882320494,258.205348530944,30.0904794283364)) ;
#104118 = CARTESIAN_POINT('Ctrl Pts',(38.0861341004722,258.21925289602,30.095028961218)) ;
#104119 = CARTESIAN_POINT('Ctrl Pts',(38.1015160468841,258.230343922473,30.1004423149597)) ;
#104120 = CARTESIAN_POINT('Ctrl Pts',(38.1184645303642,258.237998568189,30.1064243414529)) ;
#104121 = CARTESIAN_POINT('Ctrl Pts',(38.1347220873534,258.245341162533,30.1121625030258)) ;
#104122 = CARTESIAN_POINT('Ctrl Pts',(38.1521290671494,258.249390031724,30.1183211976404)) ;
#104123 = CARTESIAN_POINT('Ctrl Pts',(38.1697805624966,258.249936222763,30.1245883423369)) ;
#104124 = CARTESIAN_POINT('Ctrl Pts',(38.1711545707754,258.249978738764,30.1250761825186)) ;
#104125 = CARTESIAN_POINT('Ctrl Pts',(38.1725290495207,258.25,30.1255643186937)) ;
#104126 = CARTESIAN_POINT('Ctrl Pts',(38.1739035596877,258.25,30.1260525975118)) ;
#104127 = CARTESIAN_POINT('Origin',(40.2,258.1,25.0213203435596)) ;
#104128 = CARTESIAN_POINT('Ctrl Pts',(37.580461549766,258.25,29.2213820464094)) ;
#104129 = CARTESIAN_POINT('Ctrl Pts',(37.5806123754309,258.25,29.2221562239435)) ;
#104130 = CARTESIAN_POINT('Ctrl Pts',(37.5807632652409,258.249996669894,29.2229303947057)) ;
#104131 = CARTESIAN_POINT('Ctrl Pts',(37.5848041630347,258.249818328848,29.2436540540717)) ;
#104132 = CARTESIAN_POINT('Ctrl Pts',(37.5887516260397,258.247433157513,29.2636706102593)) ;
#104133 = CARTESIAN_POINT('Ctrl Pts',(37.5963119507474,258.238259809032,29.3016077085599)) ;
#104134 = CARTESIAN_POINT('Ctrl Pts',(37.5999655106015,258.231622782802,29.3197493931132)) ;
#104135 = CARTESIAN_POINT('Ctrl Pts',(37.6071973716956,258.21278678422,29.3553524833539)) ;
#104136 = CARTESIAN_POINT('Ctrl Pts',(37.6107566001729,258.199976451841,29.3726824256129)) ;
#104137 = CARTESIAN_POINT('Ctrl Pts',(37.6159573654841,258.171958342729,29.3978446898607)) ;
#104138 = CARTESIAN_POINT('Ctrl Pts',(37.6178293167396,258.158041775475,29.4068396388929)) ;
#104139 = CARTESIAN_POINT('Ctrl Pts',(37.6202016456472,258.129045309865,29.4182165512943)) ;
#104140 = CARTESIAN_POINT('Ctrl Pts',(37.6207969906631,258.114679223254,29.4210603173112)) ;
#104141 = CARTESIAN_POINT('Ctrl Pts',(37.6207969906631,258.1,29.4210603173112)) ;
#104142 = CARTESIAN_POINT('Origin',(39.0797116749887,258.1,27.1578412797899)) ;
#104143 = CARTESIAN_POINT('Ctrl Pts',(37.2610944621569,258.25,29.6609531317893)) ;
#104144 = CARTESIAN_POINT('Ctrl Pts',(37.2622974048242,258.25,29.6617781307852)) ;
#104145 = CARTESIAN_POINT('Ctrl Pts',(37.2635002136217,258.249978738764,29.6626031882028)) ;
#104146 = CARTESIAN_POINT('Ctrl Pts',(37.2647025064219,258.249936222763,29.6634280389871)) ;
#104147 = CARTESIAN_POINT('Ctrl Pts',(37.2801480216302,258.249390031724,29.6740246634793)) ;
#104148 = CARTESIAN_POINT('Ctrl Pts',(37.2953620762498,258.245341162533,29.6844872160823)) ;
#104149 = CARTESIAN_POINT('Ctrl Pts',(37.3095602987151,258.237998568188,29.6942670492256)) ;
#104150 = CARTESIAN_POINT('Ctrl Pts',(37.3243619284475,258.230343922473,29.7044625134383)) ;
#104151 = CARTESIAN_POINT('Ctrl Pts',(37.337782704874,258.21925289602,29.7137248799965)) ;
#104152 = CARTESIAN_POINT('Ctrl Pts',(37.3490727448287,258.205348530944,29.7215241592247)) ;
#104153 = CARTESIAN_POINT('Ctrl Pts',(37.3603597640426,258.191447886093,29.7293213516932)) ;
#104154 = CARTESIAN_POINT('Ctrl Pts',(37.3693013951648,258.175001311387,29.7355068518133)) ;
#104155 = CARTESIAN_POINT('Ctrl Pts',(37.3753983823083,258.156933541317,29.7397258512422)) ;
#104156 = CARTESIAN_POINT('Ctrl Pts',(37.3814946181241,258.138867997726,29.7439443307665)) ;
#104157 = CARTESIAN_POINT('Ctrl Pts',(37.3846302685632,258.119527473902,29.7461159238265)) ;
#104158 = CARTESIAN_POINT('Ctrl Pts',(37.3846302685632,258.1,29.7461159238264)) ;
#104159 = CARTESIAN_POINT('Origin',(40.7139068992805,258.1,27.7339145522423)) ;
#104160 = CARTESIAN_POINT('',(41.293373406158,258.1,30.0027392774284)) ;
#104161 = CARTESIAN_POINT('',(41.4175335996131,258.1,30.3848650607978)) ;
#104162 = CARTESIAN_POINT('',(40.5712484218362,258.1,27.7802671013986)) ;
#104163 = CARTESIAN_POINT('Ctrl Pts',(41.4175335996131,258.1,30.3848650607978)) ;
#104164 = CARTESIAN_POINT('Ctrl Pts',(41.4175335996131,258.119527473902,30.3848650607978)) ;
#104165 = CARTESIAN_POINT('Ctrl Pts',(41.4211868395563,258.138867997726,30.3837687223413)) ;
#104166 = CARTESIAN_POINT('Ctrl Pts',(41.4282882862172,258.156933541317,30.3816405503694)) ;
#104167 = CARTESIAN_POINT('Ctrl Pts',(41.4353906080925,258.175001311387,30.379512116112)) ;
#104168 = CARTESIAN_POINT('Ctrl Pts',(41.4458060292935,258.191447886093,30.3763924718905)) ;
#104169 = CARTESIAN_POINT('Ctrl Pts',(41.4589500874475,258.205348530944,30.3724647819374)) ;
#104170 = CARTESIAN_POINT('Ctrl Pts',(41.4720976633411,258.21925289602,30.3685360408181)) ;
#104171 = CARTESIAN_POINT('Ctrl Pts',(41.4877238088896,258.230343922473,30.3638742547393)) ;
#104172 = CARTESIAN_POINT('Ctrl Pts',(41.5049515670055,258.237998568189,30.3587517471944)) ;
#104173 = CARTESIAN_POINT('Ctrl Pts',(41.5214770136443,258.245341162533,30.3538380651865)) ;
#104174 = CARTESIAN_POINT('Ctrl Pts',(41.5391795459882,258.249390031724,30.3485889877863)) ;
#104175 = CARTESIAN_POINT('Ctrl Pts',(41.5571436409267,258.249936222763,30.3432839257019)) ;
#104176 = CARTESIAN_POINT('Ctrl Pts',(41.558541982239,258.249978738764,30.3428709748963)) ;
#104177 = CARTESIAN_POINT('Ctrl Pts',(41.5599408781471,258.25,30.342457987022)) ;
#104178 = CARTESIAN_POINT('Ctrl Pts',(41.5613398833195,258.25,30.3420450960785)) ;
#104179 = CARTESIAN_POINT('Ctrl Pts',(41.3934386691762,258.25,29.8252982934377)) ;
#104180 = CARTESIAN_POINT('Ctrl Pts',(41.3930559914292,258.25,29.8259879723341)) ;
#104181 = CARTESIAN_POINT('Ctrl Pts',(41.3926732547703,258.249996669894,29.8266776249672)) ;
#104182 = CARTESIAN_POINT('Ctrl Pts',(41.3824261696622,258.249818328848,29.8451382901584)) ;
#104183 = CARTESIAN_POINT('Ctrl Pts',(41.3724864532176,258.247433157512,29.8629553332008)) ;
#104184 = CARTESIAN_POINT('Ctrl Pts',(41.3535729490475,258.238259809032,29.8966993889301)) ;
#104185 = CARTESIAN_POINT('Ctrl Pts',(41.3444921183073,258.231622782802,29.9128241441556)) ;
#104186 = CARTESIAN_POINT('Ctrl Pts',(41.3266122497526,258.21278678422,29.9444499271496)) ;
#104187 = CARTESIAN_POINT('Ctrl Pts',(41.3178719756467,258.199976451841,29.9598318195758)) ;
#104188 = CARTESIAN_POINT('Ctrl Pts',(41.3051501866381,258.171958342729,29.9821554300886)) ;
#104189 = CARTESIAN_POINT('Ctrl Pts',(41.3005902630839,258.158041775475,29.9901316702288)) ;
#104190 = CARTESIAN_POINT('Ctrl Pts',(41.294818384942,258.129045309865,30.0002186669547)) ;
#104191 = CARTESIAN_POINT('Ctrl Pts',(41.293373406158,258.114679223254,30.0027392774284)) ;
#104192 = CARTESIAN_POINT('Ctrl Pts',(41.293373406158,258.1,30.0027392774284)) ;
#104193 = CARTESIAN_POINT('Origin',(38.3075320827811,258.1,27.0315026299217)) ;
#104194 = CARTESIAN_POINT('Ctrl Pts',(37.0149858472034,258.25,28.8105398999439)) ;
#104195 = CARTESIAN_POINT('Ctrl Pts',(37.0142029529195,258.25,28.8106356902274)) ;
#104196 = CARTESIAN_POINT('Ctrl Pts',(37.0134200452556,258.249996669894,28.8107314174129)) ;
#104197 = CARTESIAN_POINT('Ctrl Pts',(36.9924619678827,258.249818328848,28.8132922581644)) ;
#104198 = CARTESIAN_POINT('Ctrl Pts',(36.9722052585338,258.247433157512,28.8157234537812)) ;
#104199 = CARTESIAN_POINT('Ctrl Pts',(36.9337886651692,258.238259809032,28.8202563657947)) ;
#104200 = CARTESIAN_POINT('Ctrl Pts',(36.9154058857742,258.231622782802,28.8223877127213)) ;
#104201 = CARTESIAN_POINT('Ctrl Pts',(36.8793105668223,258.21278678422,28.8265117640394)) ;
#104202 = CARTESIAN_POINT('Ctrl Pts',(36.8617289502234,258.199976451841,28.8284819832727)) ;
#104203 = CARTESIAN_POINT('Ctrl Pts',(36.8361910899808,258.171958342729,28.8313113288033)) ;
#104204 = CARTESIAN_POINT('Ctrl Pts',(36.8270579203394,258.158041775475,28.832310589478)) ;
#104205 = CARTESIAN_POINT('Ctrl Pts',(36.815504743716,258.129045309865,28.8335700298872)) ;
#104206 = CARTESIAN_POINT('Ctrl Pts',(36.8126161897874,258.114679223254,28.8338825951576)) ;
#104207 = CARTESIAN_POINT('Ctrl Pts',(36.8126161897874,258.1,28.8338825951576)) ;
#104208 = CARTESIAN_POINT('Ctrl Pts',(36.5764494676875,258.1,29.1589382016729)) ;
#104209 = CARTESIAN_POINT('Ctrl Pts',(36.5764494676875,258.119527473902,29.1589382016729)) ;
#104210 = CARTESIAN_POINT('Ctrl Pts',(36.5794837446919,258.138867997726,29.1612493232956)) ;
#104211 = CARTESIAN_POINT('Ctrl Pts',(36.5853795976012,258.156933541317,29.1657436062296)) ;
#104212 = CARTESIAN_POINT('Ctrl Pts',(36.5912761771422,258.175001311387,29.1702384430593)) ;
#104213 = CARTESIAN_POINT('Ctrl Pts',(36.5999220533124,258.191447886093,29.1768310149482)) ;
#104214 = CARTESIAN_POINT('Ctrl Pts',(36.6108255047713,258.205348530944,29.1851561431399)) ;
#104215 = CARTESIAN_POINT('Ctrl Pts',(36.6217318743169,258.21925289602,29.1934834993827)) ;
#104216 = CARTESIAN_POINT('Ctrl Pts',(36.6346881563825,258.230343922473,29.2033851875816)) ;
#104217 = CARTESIAN_POINT('Ctrl Pts',(36.6489585741907,258.237998568189,29.2143118022826)) ;
#104218 = CARTESIAN_POINT('Ctrl Pts',(36.6626472402618,258.245341162533,29.2247929796343)) ;
#104219 = CARTESIAN_POINT('Ctrl Pts',(36.6772991205231,258.249390031724,29.2360292988605)) ;
#104220 = CARTESIAN_POINT('Ctrl Pts',(36.6921500359814,258.249936222763,29.2474443196982)) ;
#104221 = CARTESIAN_POINT('Ctrl Pts',(36.693306044602,258.249978738764,29.2483328751903)) ;
#104222 = CARTESIAN_POINT('Ctrl Pts',(36.6944624091955,258.25,29.249221857571)) ;
#104223 = CARTESIAN_POINT('Ctrl Pts',(36.6956187595938,258.25,29.2501109853234)) ;
#104224 = CARTESIAN_POINT('Origin',(40.2,258.1,25.0213203435596)) ;
#104225 = CARTESIAN_POINT('Ctrl Pts',(36.4107804436157,258.25,28.2063344963562)) ;
#104226 = CARTESIAN_POINT('Ctrl Pts',(36.4106846533323,258.25,28.2071173906402)) ;
#104227 = CARTESIAN_POINT('Ctrl Pts',(36.4105889261468,258.249996669894,28.2079002983041)) ;
#104228 = CARTESIAN_POINT('Ctrl Pts',(36.408028085395,258.249818328848,28.228858375676)) ;
#104229 = CARTESIAN_POINT('Ctrl Pts',(36.4055968897784,258.247433157512,28.2491150850256)) ;
#104230 = CARTESIAN_POINT('Ctrl Pts',(36.4010639777649,258.238259809032,28.2875316783901)) ;
#104231 = CARTESIAN_POINT('Ctrl Pts',(36.3989326308384,258.231622782802,28.3059144577853)) ;
#104232 = CARTESIAN_POINT('Ctrl Pts',(36.3948085795202,258.21278678422,28.3420097767375)) ;
#104233 = CARTESIAN_POINT('Ctrl Pts',(36.392838360287,258.199976451841,28.3595913933363)) ;
#104234 = CARTESIAN_POINT('Ctrl Pts',(36.3900090147564,258.171958342729,28.3851292535788)) ;
#104235 = CARTESIAN_POINT('Ctrl Pts',(36.3890097540816,258.158041775475,28.3942624232202)) ;
#104236 = CARTESIAN_POINT('Ctrl Pts',(36.3877503136725,258.129045309865,28.4058155998437)) ;
#104237 = CARTESIAN_POINT('Ctrl Pts',(36.387437748402,258.114679223254,28.4087041537722)) ;
#104238 = CARTESIAN_POINT('Ctrl Pts',(36.387437748402,258.1,28.4087041537722)) ;
#104239 = CARTESIAN_POINT('Origin',(38.4743212102356,258.1,26.7070843711341)) ;
#104240 = CARTESIAN_POINT('Ctrl Pts',(35.9712093582364,258.25,28.5257015839658)) ;
#104241 = CARTESIAN_POINT('Ctrl Pts',(35.9720984859886,258.25,28.5268579343639)) ;
#104242 = CARTESIAN_POINT('Ctrl Pts',(35.9729874683689,258.249978738764,28.5280142989582)) ;
#104243 = CARTESIAN_POINT('Ctrl Pts',(35.9738760238612,258.249936222763,28.5291703075783)) ;
#104244 = CARTESIAN_POINT('Ctrl Pts',(35.9852910447034,258.249390031724,28.5440212230315)) ;
#104245 = CARTESIAN_POINT('Ctrl Pts',(35.9965273639239,258.245341162533,28.5586731032987)) ;
#104246 = CARTESIAN_POINT('Ctrl Pts',(36.0070085412762,258.237998568188,28.5723617693696)) ;
#104247 = CARTESIAN_POINT('Ctrl Pts',(36.0179351559777,258.230343922473,28.5866321871773)) ;
#104248 = CARTESIAN_POINT('Ctrl Pts',(36.0278368441767,258.21925289602,28.5995884692428)) ;
#104249 = CARTESIAN_POINT('Ctrl Pts',(36.0361642004195,258.205348530944,28.6104948387885)) ;
#104250 = CARTESIAN_POINT('Ctrl Pts',(36.0444893286112,258.191447886093,28.6213982902474)) ;
#104251 = CARTESIAN_POINT('Ctrl Pts',(36.0510819005005,258.175001311387,28.6300441664173)) ;
#104252 = CARTESIAN_POINT('Ctrl Pts',(36.0555767373301,258.156933541317,28.6359407459584)) ;
#104253 = CARTESIAN_POINT('Ctrl Pts',(36.0600710202639,258.138867997726,28.6418365988678)) ;
#104254 = CARTESIAN_POINT('Ctrl Pts',(36.0623821418869,258.119527473902,28.6448708758721)) ;
#104255 = CARTESIAN_POINT('Ctrl Pts',(36.0623821418868,258.1,28.6448708758721)) ;
#104256 = CARTESIAN_POINT('Origin',(41.5269922146558,258.1,27.4423447763876)) ;
#104257 = CARTESIAN_POINT('',(42.7792030093369,258.1,29.4210603173112)) ;
#104258 = CARTESIAN_POINT('',(43.0153697314369,258.1,29.7461159238265)) ;
#104259 = CARTESIAN_POINT('',(41.4056396654995,258.1,27.5305125642315)) ;
#104260 = CARTESIAN_POINT('Ctrl Pts',(43.0153697314369,258.1,29.7461159238265)) ;
#104261 = CARTESIAN_POINT('Ctrl Pts',(43.0153697314369,258.119527473902,29.7461159238265)) ;
#104262 = CARTESIAN_POINT('Ctrl Pts',(43.0185053818762,258.138867997726,29.7439443307668)) ;
#104263 = CARTESIAN_POINT('Ctrl Pts',(43.0246016176919,258.156933541317,29.7397258512424)) ;
#104264 = CARTESIAN_POINT('Ctrl Pts',(43.0306986048354,258.175001311387,29.7355068518134)) ;
#104265 = CARTESIAN_POINT('Ctrl Pts',(43.0396402359576,258.191447886093,29.7293213516934)) ;
#104266 = CARTESIAN_POINT('Ctrl Pts',(43.0509272551715,258.205348530944,29.721524159225)) ;
#104267 = CARTESIAN_POINT('Ctrl Pts',(43.0622172951262,258.21925289602,29.7137248799967)) ;
#104268 = CARTESIAN_POINT('Ctrl Pts',(43.0756380715528,258.230343922473,29.7044625134387)) ;
#104269 = CARTESIAN_POINT('Ctrl Pts',(43.0904397012854,258.237998568188,29.6942670492262)) ;
#104270 = CARTESIAN_POINT('Ctrl Pts',(43.1046379237509,258.245341162533,29.6844872160833)) ;
#104271 = CARTESIAN_POINT('Ctrl Pts',(43.1198519783685,258.249390031724,29.674024663477)) ;
#104272 = CARTESIAN_POINT('Ctrl Pts',(43.1352974935786,258.249936222763,29.6634280389875)) ;
#104273 = CARTESIAN_POINT('Ctrl Pts',(43.1364997863788,258.249978738764,29.6626031882035)) ;
#104274 = CARTESIAN_POINT('Ctrl Pts',(43.137702595176,258.25,29.6617781307852)) ;
#104275 = CARTESIAN_POINT('Ctrl Pts',(43.1389055378432,258.25,29.6609531317894)) ;
#104276 = CARTESIAN_POINT('Ctrl Pts',(42.8195384502335,258.25,29.2213820464098)) ;
#104277 = CARTESIAN_POINT('Ctrl Pts',(42.8193876245684,258.25,29.2221562239442)) ;
#104278 = CARTESIAN_POINT('Ctrl Pts',(42.8192367347592,258.249996669894,29.2229303947053)) ;
#104279 = CARTESIAN_POINT('Ctrl Pts',(42.8151958369656,258.249818328848,29.2436540540713)) ;
#104280 = CARTESIAN_POINT('Ctrl Pts',(42.8112483739603,258.247433157513,29.2636706102592)) ;
#104281 = CARTESIAN_POINT('Ctrl Pts',(42.8036880492526,258.238259809032,29.3016077085601)) ;
#104282 = CARTESIAN_POINT('Ctrl Pts',(42.8000344893985,258.231622782802,29.3197493931132)) ;
#104283 = CARTESIAN_POINT('Ctrl Pts',(42.7928026283045,258.21278678422,29.3553524833537)) ;
#104284 = CARTESIAN_POINT('Ctrl Pts',(42.7892433998272,258.199976451841,29.3726824256128)) ;
#104285 = CARTESIAN_POINT('Ctrl Pts',(42.784042634516,258.171958342729,29.3978446898607)) ;
#104286 = CARTESIAN_POINT('Ctrl Pts',(42.7821706832605,258.158041775475,29.4068396388929)) ;
#104287 = CARTESIAN_POINT('Ctrl Pts',(42.7797983543528,258.129045309865,29.4182165512944)) ;
#104288 = CARTESIAN_POINT('Ctrl Pts',(42.7792030093369,258.114679223254,29.4210603173112)) ;
#104289 = CARTESIAN_POINT('Ctrl Pts',(42.7792030093369,258.1,29.4210603173112)) ;
#104290 = CARTESIAN_POINT('Origin',(37.7789755671721,258.1,26.3483125582154)) ;
#104291 = CARTESIAN_POINT('Ctrl Pts',(35.9999382971499,258.25,27.6408587937931)) ;
#104292 = CARTESIAN_POINT('Ctrl Pts',(35.9991641196141,258.25,27.6407079681278)) ;
#104293 = CARTESIAN_POINT('Ctrl Pts',(35.9983899488515,258.249996669894,27.6405570783182)) ;
#104294 = CARTESIAN_POINT('Ctrl Pts',(35.9776662894848,258.249818328848,27.6365161805244)) ;
#104295 = CARTESIAN_POINT('Ctrl Pts',(35.9576497332977,258.247433157512,27.6325687175194)) ;
#104296 = CARTESIAN_POINT('Ctrl Pts',(35.9197126349983,258.238259809032,27.6250083928119)) ;
#104297 = CARTESIAN_POINT('Ctrl Pts',(35.9015709504458,258.231622782802,27.621354832958)) ;
#104298 = CARTESIAN_POINT('Ctrl Pts',(35.8659678602057,258.21278678422,27.6141229718641)) ;
#104299 = CARTESIAN_POINT('Ctrl Pts',(35.8486379179467,258.199976451841,27.6105637433868)) ;
#104300 = CARTESIAN_POINT('Ctrl Pts',(35.8234756536989,258.171958342729,27.6053629780756)) ;
#104301 = CARTESIAN_POINT('Ctrl Pts',(35.8144807046667,258.158041775475,27.6034910268201)) ;
#104302 = CARTESIAN_POINT('Ctrl Pts',(35.8031037922653,258.129045309865,27.6011186979124)) ;
#104303 = CARTESIAN_POINT('Ctrl Pts',(35.8002600262485,258.114679223254,27.6005233528965)) ;
#104304 = CARTESIAN_POINT('Ctrl Pts',(35.8002600262485,258.1,27.6005233528965)) ;
#104305 = CARTESIAN_POINT('Ctrl Pts',(35.4752044197332,258.1,27.8366900749965)) ;
#104306 = CARTESIAN_POINT('Ctrl Pts',(35.4752044197331,258.119527473902,27.8366900749965)) ;
#104307 = CARTESIAN_POINT('Ctrl Pts',(35.4773760127932,258.138867997726,27.8398257254356)) ;
#104308 = CARTESIAN_POINT('Ctrl Pts',(35.4815944923175,258.156933541317,27.8459219612513)) ;
#104309 = CARTESIAN_POINT('Ctrl Pts',(35.4858134917465,258.175001311387,27.8520189483948)) ;
#104310 = CARTESIAN_POINT('Ctrl Pts',(35.4919989918669,258.191447886093,27.8609605795168)) ;
#104311 = CARTESIAN_POINT('Ctrl Pts',(35.4997961843353,258.205348530944,27.8722475987306)) ;
#104312 = CARTESIAN_POINT('Ctrl Pts',(35.5075954635636,258.21925289602,27.8835376386854)) ;
#104313 = CARTESIAN_POINT('Ctrl Pts',(35.5168578301215,258.230343922473,27.896958415112)) ;
#104314 = CARTESIAN_POINT('Ctrl Pts',(35.5270532943343,258.237998568188,27.9117600448444)) ;
#104315 = CARTESIAN_POINT('Ctrl Pts',(35.5368331274775,258.245341162533,27.9259582673097)) ;
#104316 = CARTESIAN_POINT('Ctrl Pts',(35.547295680081,258.249390031724,27.9411723219293)) ;
#104317 = CARTESIAN_POINT('Ctrl Pts',(35.5578923045725,258.249936222763,27.9566178371378)) ;
#104318 = CARTESIAN_POINT('Ctrl Pts',(35.5587171553567,258.249978738764,27.957820129938)) ;
#104319 = CARTESIAN_POINT('Ctrl Pts',(35.5595422127747,258.25,27.9590229387353)) ;
#104320 = CARTESIAN_POINT('Ctrl Pts',(35.5603672117705,258.25,27.9602258814026)) ;
#104321 = CARTESIAN_POINT('Origin',(40.2,258.1,25.0213203435596)) ;
#104322 = CARTESIAN_POINT('Ctrl Pts',(35.6120145486888,258.25,26.8795155697285)) ;
#104323 = CARTESIAN_POINT('Ctrl Pts',(35.611681519077,258.25,26.8802305456133)) ;
#104324 = CARTESIAN_POINT('Ctrl Pts',(35.6113485453403,258.249996669894,26.8809455537216)) ;
#104325 = CARTESIAN_POINT('Ctrl Pts',(35.6024366389787,258.249818328848,26.9000865264635)) ;
#104326 = CARTESIAN_POINT('Ctrl Pts',(35.593864767106,258.247433157512,26.9186005211265)) ;
#104327 = CARTESIAN_POINT('Ctrl Pts',(35.5776823313821,258.238259809032,26.9537361257336)) ;
#104328 = CARTESIAN_POINT('Ctrl Pts',(35.5699747087623,258.231622782802,26.9705605654438)) ;
#104329 = CARTESIAN_POINT('Ctrl Pts',(35.5548984359091,258.21278678422,27.0036148517977)) ;
#104330 = CARTESIAN_POINT('Ctrl Pts',(35.5475916277511,258.199976451841,27.0197271316054)) ;
#104331 = CARTESIAN_POINT('Ctrl Pts',(35.5370091274324,258.171958342729,27.0431407641495)) ;
#104332 = CARTESIAN_POINT('Ctrl Pts',(35.5332364694246,258.158041775475,27.051518136121)) ;
#104333 = CARTESIAN_POINT('Ctrl Pts',(35.5284685425009,258.129045309865,27.0621166715428)) ;
#104334 = CARTESIAN_POINT('Ctrl Pts',(35.5272786630106,258.114679223254,27.0647672615988)) ;
#104335 = CARTESIAN_POINT('Ctrl Pts',(35.5272786630106,258.1,27.0647672615988)) ;
#104336 = CARTESIAN_POINT('Origin',(38.0378522089358,258.1,26.0913131340507)) ;
#104337 = CARTESIAN_POINT('Ctrl Pts',(35.0952677460484,258.25,27.0474167838717)) ;
#104338 = CARTESIAN_POINT('Ctrl Pts',(35.0957560248665,258.25,27.0487912940387)) ;
#104339 = CARTESIAN_POINT('Ctrl Pts',(35.096244161041,258.249978738764,27.0501657727844)) ;
#104340 = CARTESIAN_POINT('Ctrl Pts',(35.0967320012227,258.249936222763,27.0515397810631)) ;
#104341 = CARTESIAN_POINT('Ctrl Pts',(35.1029991459195,258.249390031724,27.0691912764099)) ;
#104342 = CARTESIAN_POINT('Ctrl Pts',(35.109157840533,258.245341162533,27.0865982562064)) ;
#104343 = CARTESIAN_POINT('Ctrl Pts',(35.114896002106,258.237998568189,27.1028558131956)) ;
#104344 = CARTESIAN_POINT('Ctrl Pts',(35.1208780285994,258.230343922473,27.1198042966759)) ;
#104345 = CARTESIAN_POINT('Ctrl Pts',(35.1262913823413,258.21925289602,27.1351862430876)) ;
#104346 = CARTESIAN_POINT('Ctrl Pts',(35.1308409152229,258.205348530944,27.1481321115103)) ;
#104347 = CARTESIAN_POINT('Ctrl Pts',(35.1353892308406,258.191447886093,27.161074516162)) ;
#104348 = CARTESIAN_POINT('Ctrl Pts',(35.1389874166276,258.175001311387,27.1713344497828)) ;
#104349 = CARTESIAN_POINT('Ctrl Pts',(35.1414401171973,258.156933541317,27.1783314111464)) ;
#104350 = CARTESIAN_POINT('Ctrl Pts',(35.1438925155223,258.138867997726,27.1853275102791)) ;
#104351 = CARTESIAN_POINT('Ctrl Pts',(35.1451528796413,258.119527473902,27.1889274550539)) ;
#104352 = CARTESIAN_POINT('Ctrl Pts',(35.1451528796413,258.1,27.1889274550539)) ;
#104353 = CARTESIAN_POINT('Origin',(42.2101822863621,258.1,26.9137882607786)) ;
#104354 = CARTESIAN_POINT('',(44.012562251598,258.1,28.4087041537722)) ;
#104355 = CARTESIAN_POINT('',(44.3376178581133,258.1,28.6448708758722)) ;
#104356 = CARTESIAN_POINT('',(42.1220144985182,258.1,27.0351408099348)) ;
#104357 = CARTESIAN_POINT('Ctrl Pts',(44.3376178581132,258.1,28.6448708758722)) ;
#104358 = CARTESIAN_POINT('Ctrl Pts',(44.3376178581133,258.119527473902,28.6448708758722)) ;
#104359 = CARTESIAN_POINT('Ctrl Pts',(44.339928979736,258.138867997726,28.6418365988678)) ;
#104360 = CARTESIAN_POINT('Ctrl Pts',(44.3444232626699,258.156933541317,28.6359407459585)) ;
#104361 = CARTESIAN_POINT('Ctrl Pts',(44.3489180994996,258.175001311387,28.6300441664175)) ;
#104362 = CARTESIAN_POINT('Ctrl Pts',(44.3555106713886,258.191447886093,28.6213982902472)) ;
#104363 = CARTESIAN_POINT('Ctrl Pts',(44.3638357995803,258.205348530944,28.6104948387884)) ;
#104364 = CARTESIAN_POINT('Ctrl Pts',(44.3721631558231,258.21925289602,28.5995884692428)) ;
#104365 = CARTESIAN_POINT('Ctrl Pts',(44.382064844023,258.230343922473,28.5866321871781)) ;
#104366 = CARTESIAN_POINT('Ctrl Pts',(44.3929914587245,258.237998568189,28.5723617693702)) ;
#104367 = CARTESIAN_POINT('Ctrl Pts',(44.4034726360766,258.245341162533,28.5586731032994)) ;
#104368 = CARTESIAN_POINT('Ctrl Pts',(44.414708955301,258.249390031724,28.5440212230371)) ;
#104369 = CARTESIAN_POINT('Ctrl Pts',(44.4261239761384,258.249936222763,28.5291703075781)) ;
#104370 = CARTESIAN_POINT('Ctrl Pts',(44.4270125316305,258.249978738764,28.5280142989574)) ;
#104371 = CARTESIAN_POINT('Ctrl Pts',(44.4279015140117,258.25,28.5268579343646)) ;
#104372 = CARTESIAN_POINT('Ctrl Pts',(44.4287906417641,258.25,28.5257015839662)) ;
#104373 = CARTESIAN_POINT('Ctrl Pts',(43.9892195563843,258.25,28.2063344963563)) ;
#104374 = CARTESIAN_POINT('Ctrl Pts',(43.9893153466677,258.25,28.2071173906402)) ;
#104375 = CARTESIAN_POINT('Ctrl Pts',(43.9894110738533,258.249996669894,28.2079002983041)) ;
#104376 = CARTESIAN_POINT('Ctrl Pts',(43.9919719146048,258.249818328848,28.2288583756768)) ;
#104377 = CARTESIAN_POINT('Ctrl Pts',(43.9944031102216,258.247433157512,28.2491150850258)) ;
#104378 = CARTESIAN_POINT('Ctrl Pts',(43.9989360222351,258.238259809032,28.2875316783904)) ;
#104379 = CARTESIAN_POINT('Ctrl Pts',(44.0010673691616,258.231622782802,28.3059144577855)) ;
#104380 = CARTESIAN_POINT('Ctrl Pts',(44.0051914204798,258.21278678422,28.3420097767374)) ;
#104381 = CARTESIAN_POINT('Ctrl Pts',(44.0071616397131,258.199976451841,28.3595913933363)) ;
#104382 = CARTESIAN_POINT('Ctrl Pts',(44.0099909852437,258.171958342729,28.3851292535789)) ;
#104383 = CARTESIAN_POINT('Ctrl Pts',(44.0109902459184,258.158041775475,28.3942624232203)) ;
#104384 = CARTESIAN_POINT('Ctrl Pts',(44.0122496863275,258.129045309865,28.4058155998437)) ;
#104385 = CARTESIAN_POINT('Ctrl Pts',(44.012562251598,258.114679223254,28.4087041537722)) ;
#104386 = CARTESIAN_POINT('Ctrl Pts',(44.012562251598,258.1,28.4087041537722)) ;
#104387 = CARTESIAN_POINT('Origin',(37.4874057913173,258.1,25.5352272428401)) ;
#104388 = CARTESIAN_POINT('Ctrl Pts',(35.3960220501219,258.25,26.2147590127358)) ;
#104389 = CARTESIAN_POINT('Ctrl Pts',(35.3953323712255,258.25,26.2143763349887)) ;
#104390 = CARTESIAN_POINT('Ctrl Pts',(35.3946427185925,258.249996669894,26.2139935983299)) ;
#104391 = CARTESIAN_POINT('Ctrl Pts',(35.3761820534011,258.249818328848,26.2037465132217)) ;
#104392 = CARTESIAN_POINT('Ctrl Pts',(35.3583650103588,258.247433157512,26.1938067967771)) ;
#104393 = CARTESIAN_POINT('Ctrl Pts',(35.3246209546296,258.238259809032,26.1748932926071)) ;
#104394 = CARTESIAN_POINT('Ctrl Pts',(35.3084961994042,258.231622782802,26.1658124618669)) ;
#104395 = CARTESIAN_POINT('Ctrl Pts',(35.2768704164101,258.21278678422,26.1479325933122)) ;
#104396 = CARTESIAN_POINT('Ctrl Pts',(35.2614885239839,258.199976451842,26.1391923192063)) ;
#104397 = CARTESIAN_POINT('Ctrl Pts',(35.2391649134711,258.171958342729,26.1264705301978)) ;
#104398 = CARTESIAN_POINT('Ctrl Pts',(35.2311886733309,258.158041775475,26.1219106066435)) ;
#104399 = CARTESIAN_POINT('Ctrl Pts',(35.2211016766049,258.129045309865,26.1161387285016)) ;
#104400 = CARTESIAN_POINT('Ctrl Pts',(35.2185810661312,258.114679223254,26.1146937497175)) ;
#104401 = CARTESIAN_POINT('Ctrl Pts',(35.2185810661312,258.1,26.1146937497175)) ;
#104402 = CARTESIAN_POINT('Ctrl Pts',(34.8364552827617,258.1,26.2388539431727)) ;
#104403 = CARTESIAN_POINT('Ctrl Pts',(34.8364552827616,258.119527473902,26.2388539431727)) ;
#104404 = CARTESIAN_POINT('Ctrl Pts',(34.837551621218,258.138867997726,26.242507183116)) ;
#104405 = CARTESIAN_POINT('Ctrl Pts',(34.8396797931898,258.156933541317,26.2496086297769)) ;
#104406 = CARTESIAN_POINT('Ctrl Pts',(34.8418082274472,258.175001311387,26.2567109516523)) ;
#104407 = CARTESIAN_POINT('Ctrl Pts',(34.8449278716689,258.191447886093,26.2671263728531)) ;
#104408 = CARTESIAN_POINT('Ctrl Pts',(34.848855561622,258.205348530944,26.2802704310072)) ;
#104409 = CARTESIAN_POINT('Ctrl Pts',(34.8527843027412,258.21925289602,26.2934180069008)) ;
#104410 = CARTESIAN_POINT('Ctrl Pts',(34.85744608882,258.230343922473,26.3090441524493)) ;
#104411 = CARTESIAN_POINT('Ctrl Pts',(34.8625685963648,258.237998568189,26.3262719105653)) ;
#104412 = CARTESIAN_POINT('Ctrl Pts',(34.8674822783726,258.245341162533,26.3427973572041)) ;
#104413 = CARTESIAN_POINT('Ctrl Pts',(34.8727313557738,258.249390031724,26.3604998895481)) ;
#104414 = CARTESIAN_POINT('Ctrl Pts',(34.8780364178575,258.249936222763,26.3784639844864)) ;
#104415 = CARTESIAN_POINT('Ctrl Pts',(34.878449368663,258.249978738764,26.3798623257986)) ;
#104416 = CARTESIAN_POINT('Ctrl Pts',(34.8788623565375,258.25,26.3812612217067)) ;
#104417 = CARTESIAN_POINT('Ctrl Pts',(34.8792752474809,258.25,26.3826602268792)) ;
#104418 = CARTESIAN_POINT('Origin',(40.2,258.1,25.0213203435596)) ;
#104419 = CARTESIAN_POINT('Ctrl Pts',(35.2623526361106,258.25,25.3708035475559)) ;
#104420 = CARTESIAN_POINT('Ctrl Pts',(35.2618149664292,258.25,25.3713806182205)) ;
#104421 = CARTESIAN_POINT('Ctrl Pts',(35.2612773399305,258.249996669894,25.3719577367977)) ;
#104422 = CARTESIAN_POINT('Ctrl Pts',(35.2468867274466,258.249818328848,25.3874079531342)) ;
#104423 = CARTESIAN_POINT('Ctrl Pts',(35.2330132538606,258.247433157512,25.4023669543188)) ;
#104424 = CARTESIAN_POINT('Ctrl Pts',(35.2067653439847,258.238259809032,25.4307822523853)) ;
#104425 = CARTESIAN_POINT('Ctrl Pts',(35.1942359214756,258.231622782802,25.4444014590289)) ;
#104426 = CARTESIAN_POINT('Ctrl Pts',(35.1696831977168,258.21278678422,25.4711791289339)) ;
#104427 = CARTESIAN_POINT('Ctrl Pts',(35.1577550419262,258.199976451841,25.4842448897419)) ;
#104428 = CARTESIAN_POINT('Ctrl Pts',(35.1404552756832,258.171958342729,25.5032424051016)) ;
#104429 = CARTESIAN_POINT('Ctrl Pts',(35.1342785143937,258.158041775475,25.5100439438662)) ;
#104430 = CARTESIAN_POINT('Ctrl Pts',(35.1264688188629,258.129045309865,25.5186503795949)) ;
#104431 = CARTESIAN_POINT('Ctrl Pts',(35.1245180988476,258.114679223254,25.5208035475559)) ;
#104432 = CARTESIAN_POINT('Ctrl Pts',(35.1245180988476,258.1,25.5208035475559)) ;
#104433 = CARTESIAN_POINT('Origin',(37.8130292979948,258.1,25.3708035475559)) ;
#104434 = CARTESIAN_POINT('Ctrl Pts',(34.7190128936385,258.25,25.3708035475559)) ;
#104435 = CARTESIAN_POINT('Ctrl Pts',(34.7190525273897,258.25,25.3722616708597)) ;
#104436 = CARTESIAN_POINT('Ctrl Pts',(34.7190920351885,258.249978738764,25.3737197202007)) ;
#104437 = CARTESIAN_POINT('Ctrl Pts',(34.7191314068636,258.249936222763,25.3751772306343)) ;
#104438 = CARTESIAN_POINT('Ctrl Pts',(34.7196372036263,258.249390031724,25.3939014545243)) ;
#104439 = CARTESIAN_POINT('Ctrl Pts',(34.7201154176929,258.245341162533,25.4123596173872)) ;
#104440 = CARTESIAN_POINT('Ctrl Pts',(34.720548872252,258.237998568188,25.4295946623432)) ;
#104441 = CARTESIAN_POINT('Ctrl Pts',(34.7210007481052,258.230343922473,25.4475621758456)) ;
#104442 = CARTESIAN_POINT('Ctrl Pts',(34.7213958706096,258.21925289602,25.4638640945166)) ;
#104443 = CARTESIAN_POINT('Ctrl Pts',(34.7217222401531,258.205348530944,25.4775822300161)) ;
#104444 = CARTESIAN_POINT('Ctrl Pts',(34.7220485223739,258.191447886093,25.4912966951182)) ;
#104445 = CARTESIAN_POINT('Ctrl Pts',(34.7223001065631,258.175001311387,25.5021663724021)) ;
#104446 = CARTESIAN_POINT('Ctrl Pts',(34.7224705834521,258.156933541317,25.5095788042595)) ;
#104447 = CARTESIAN_POINT('Ctrl Pts',(34.7226410393334,258.138867997726,25.5169903226876)) ;
#104448 = CARTESIAN_POINT('Ctrl Pts',(34.7227272727275,258.119527473902,25.5208035475559)) ;
#104449 = CARTESIAN_POINT('Ctrl Pts',(34.7227272727275,258.1,25.5208035475559)) ;
#104450 = CARTESIAN_POINT('Origin',(42.6966017101158,258.1,26.1999837998328)) ;
#104451 = CARTESIAN_POINT('',(44.8727213369894,258.1,27.0647672615988)) ;
#104452 = CARTESIAN_POINT('',(45.2548471203588,258.1,27.188927455054)) ;
#104453 = CARTESIAN_POINT('',(42.6502491609595,258.1,26.3426422772771)) ;
#104454 = CARTESIAN_POINT('Ctrl Pts',(45.2548471203589,258.1,27.188927455054)) ;
#104455 = CARTESIAN_POINT('Ctrl Pts',(45.2548471203587,258.119527473902,27.1889274550539)) ;
#104456 = CARTESIAN_POINT('Ctrl Pts',(45.2561074844781,258.138867997726,27.1853275102792)) ;
#104457 = CARTESIAN_POINT('Ctrl Pts',(45.2585598828031,258.156933541317,27.1783314111465)) ;
#104458 = CARTESIAN_POINT('Ctrl Pts',(45.2610125833727,258.175001311387,27.1713344497829)) ;
#104459 = CARTESIAN_POINT('Ctrl Pts',(45.2646107691594,258.191447886093,27.1610745161619)) ;
#104460 = CARTESIAN_POINT('Ctrl Pts',(45.2691590847769,258.205348530944,27.1481321115102)) ;
#104461 = CARTESIAN_POINT('Ctrl Pts',(45.2737086176586,258.21925289602,27.1351862430874)) ;
#104462 = CARTESIAN_POINT('Ctrl Pts',(45.2791219714006,258.230343922473,27.1198042966759)) ;
#104463 = CARTESIAN_POINT('Ctrl Pts',(45.2851039978943,258.237998568188,27.1028558131957)) ;
#104464 = CARTESIAN_POINT('Ctrl Pts',(45.2908421594676,258.245341162533,27.0865982562065)) ;
#104465 = CARTESIAN_POINT('Ctrl Pts',(45.2970008540775,258.249390031724,27.0691912764082)) ;
#104466 = CARTESIAN_POINT('Ctrl Pts',(45.3032679987774,258.249936222763,27.051539781063)) ;
#104467 = CARTESIAN_POINT('Ctrl Pts',(45.3037558389593,258.249978738764,27.0501657727844)) ;
#104468 = CARTESIAN_POINT('Ctrl Pts',(45.3042439751347,258.25,27.0487912940391)) ;
#104469 = CARTESIAN_POINT('Ctrl Pts',(45.3047322539528,258.25,27.0474167838722)) ;
#104470 = CARTESIAN_POINT('Ctrl Pts',(44.7879854513112,258.25,26.8795155697285)) ;
#104471 = CARTESIAN_POINT('Ctrl Pts',(44.7883184809236,258.25,26.8802305456146)) ;
#104472 = CARTESIAN_POINT('Ctrl Pts',(44.7886514546609,258.249996669894,26.8809455537241)) ;
#104473 = CARTESIAN_POINT('Ctrl Pts',(44.7975633610227,258.249818328848,26.9000865264659)) ;
#104474 = CARTESIAN_POINT('Ctrl Pts',(44.8061352328951,258.247433157512,26.9186005211289)) ;
#104475 = CARTESIAN_POINT('Ctrl Pts',(44.8223176686183,258.238259809031,26.9537361257345)) ;
#104476 = CARTESIAN_POINT('Ctrl Pts',(44.8300252912379,258.231622782802,26.9705605654442)) ;
#104477 = CARTESIAN_POINT('Ctrl Pts',(44.845101564091,258.21278678422,27.0036148517979)) ;
#104478 = CARTESIAN_POINT('Ctrl Pts',(44.8524083722489,258.199976451841,27.0197271316054)) ;
#104479 = CARTESIAN_POINT('Ctrl Pts',(44.8629908725676,258.171958342729,27.0431407641494)) ;
#104480 = CARTESIAN_POINT('Ctrl Pts',(44.8667635305755,258.158041775475,27.051518136121)) ;
#104481 = CARTESIAN_POINT('Ctrl Pts',(44.8715314574991,258.129045309865,27.0621166715428)) ;
#104482 = CARTESIAN_POINT('Ctrl Pts',(44.8727213369894,258.114679223254,27.0647672615988)) ;
#104483 = CARTESIAN_POINT('Ctrl Pts',(44.8727213369894,258.1,27.0647672615988)) ;
#104484 = CARTESIAN_POINT('Origin',(37.4613636363637,258.1,24.6718371395634)) ;
#104485 = CARTESIAN_POINT('Ctrl Pts',(35.2623526361106,258.25,24.6718371395634)) ;
#104486 = CARTESIAN_POINT('Ctrl Pts',(35.2618149664301,258.25,24.6712600688998)) ;
#104487 = CARTESIAN_POINT('Ctrl Pts',(35.2612773399324,258.249996669894,24.6706829503236)) ;
#104488 = CARTESIAN_POINT('Ctrl Pts',(35.2468867274488,258.249818328848,24.6552327339874)) ;
#104489 = CARTESIAN_POINT('Ctrl Pts',(35.2330132538624,258.247433157513,24.6402737328024)) ;
#104490 = CARTESIAN_POINT('Ctrl Pts',(35.2067653439856,258.238259809032,24.611858434735)) ;
#104491 = CARTESIAN_POINT('Ctrl Pts',(35.1942359214761,258.231622782802,24.5982392280908)) ;
#104492 = CARTESIAN_POINT('Ctrl Pts',(35.1696831977168,258.21278678422,24.5714615581854)) ;
#104493 = CARTESIAN_POINT('Ctrl Pts',(35.1577550419262,258.199976451841,24.5583957973774)) ;
#104494 = CARTESIAN_POINT('Ctrl Pts',(35.1404552756832,258.171958342729,24.5393982820177)) ;
#104495 = CARTESIAN_POINT('Ctrl Pts',(35.1342785143937,258.158041775475,24.5325967432531)) ;
#104496 = CARTESIAN_POINT('Ctrl Pts',(35.1264688188629,258.129045309865,24.5239903075244)) ;
#104497 = CARTESIAN_POINT('Ctrl Pts',(35.1245180988476,258.114679223254,24.5218371395634)) ;
#104498 = CARTESIAN_POINT('Ctrl Pts',(35.1245180988476,258.1,24.5218371395634)) ;
#104499 = CARTESIAN_POINT('Ctrl Pts',(34.7227272727271,258.1,24.5218371395634)) ;
#104500 = CARTESIAN_POINT('Ctrl Pts',(34.7227272727271,258.119527473902,24.5218371395634)) ;
#104501 = CARTESIAN_POINT('Ctrl Pts',(34.722641039333,258.138867997726,24.5256503644317)) ;
#104502 = CARTESIAN_POINT('Ctrl Pts',(34.7224705834517,258.156933541317,24.5330618828598)) ;
#104503 = CARTESIAN_POINT('Ctrl Pts',(34.7223001065627,258.175001311387,24.5404743147172)) ;
#104504 = CARTESIAN_POINT('Ctrl Pts',(34.7220485223736,258.191447886093,24.5513439920011)) ;
#104505 = CARTESIAN_POINT('Ctrl Pts',(34.7217222401528,258.205348530944,24.5650584571032)) ;
#104506 = CARTESIAN_POINT('Ctrl Pts',(34.7213958706093,258.21925289602,24.5787765926027)) ;
#104507 = CARTESIAN_POINT('Ctrl Pts',(34.7210007481061,258.230343922473,24.5950785112738)) ;
#104508 = CARTESIAN_POINT('Ctrl Pts',(34.7205488722535,258.237998568189,24.6130460247761)) ;
#104509 = CARTESIAN_POINT('Ctrl Pts',(34.720115417695,258.245341162533,24.6302810697322)) ;
#104510 = CARTESIAN_POINT('Ctrl Pts',(34.7196372036259,258.249390031724,24.6487392325953)) ;
#104511 = CARTESIAN_POINT('Ctrl Pts',(34.7191314068632,258.249936222763,24.6674634564849)) ;
#104512 = CARTESIAN_POINT('Ctrl Pts',(34.7190920351881,258.249978738764,24.6689209669185)) ;
#104513 = CARTESIAN_POINT('Ctrl Pts',(34.7190525273894,258.25,24.6703790162596)) ;
#104514 = CARTESIAN_POINT('Ctrl Pts',(34.7190128936382,258.25,24.6718371395634)) ;
#104515 = CARTESIAN_POINT('Origin',(40.2,258.1,25.0213203435596)) ;
#104516 = CARTESIAN_POINT('Ctrl Pts',(35.3960220501219,258.25,23.8278816743835)) ;
#104517 = CARTESIAN_POINT('Ctrl Pts',(35.3953323712255,258.25,23.8282643521305)) ;
#104518 = CARTESIAN_POINT('Ctrl Pts',(35.3946427185925,258.249996669894,23.8286470887893)) ;
#104519 = CARTESIAN_POINT('Ctrl Pts',(35.3761820534012,258.249818328848,23.8388941738976)) ;
#104520 = CARTESIAN_POINT('Ctrl Pts',(35.3583650103588,258.247433157512,23.8488338903421)) ;
#104521 = CARTESIAN_POINT('Ctrl Pts',(35.3246209546295,258.238259809032,23.8677473945122)) ;
#104522 = CARTESIAN_POINT('Ctrl Pts',(35.3084961994041,258.231622782802,23.8768282252524)) ;
#104523 = CARTESIAN_POINT('Ctrl Pts',(35.27687041641,258.21278678422,23.8947080938071)) ;
#104524 = CARTESIAN_POINT('Ctrl Pts',(35.2614885239839,258.199976451841,23.903448367913)) ;
#104525 = CARTESIAN_POINT('Ctrl Pts',(35.2391649134711,258.171958342729,23.9161701569215)) ;
#104526 = CARTESIAN_POINT('Ctrl Pts',(35.2311886733309,258.158041775475,23.9207300804757)) ;
#104527 = CARTESIAN_POINT('Ctrl Pts',(35.2211016766049,258.129045309865,23.9265019586177)) ;
#104528 = CARTESIAN_POINT('Ctrl Pts',(35.2185810661312,258.114679223254,23.9279469374017)) ;
#104529 = CARTESIAN_POINT('Ctrl Pts',(35.2185810661312,258.1,23.9279469374017)) ;
#104530 = CARTESIAN_POINT('Origin',(37.8218597103689,258.1,24.6160841100613)) ;
#104531 = CARTESIAN_POINT('Ctrl Pts',(34.8792752474813,258.25,23.6599804602402)) ;
#104532 = CARTESIAN_POINT('Ctrl Pts',(34.8788623565378,258.25,23.6613794654126)) ;
#104533 = CARTESIAN_POINT('Ctrl Pts',(34.8784493686632,258.249978738764,23.6627783613207)) ;
#104534 = CARTESIAN_POINT('Ctrl Pts',(34.8780364178576,258.249936222763,23.6641767026329)) ;
#104535 = CARTESIAN_POINT('Ctrl Pts',(34.8727313557735,258.249390031724,23.6821407975715)) ;
#104536 = CARTESIAN_POINT('Ctrl Pts',(34.8674822783725,258.245341162533,23.6998433299152)) ;
#104537 = CARTESIAN_POINT('Ctrl Pts',(34.8625685963647,258.237998568189,23.716368776554)) ;
#104538 = CARTESIAN_POINT('Ctrl Pts',(34.85744608882,258.230343922473,23.7335965346698)) ;
#104539 = CARTESIAN_POINT('Ctrl Pts',(34.852784302741,258.21925289602,23.7492226802184)) ;
#104540 = CARTESIAN_POINT('Ctrl Pts',(34.8488555616218,258.205348530944,23.762370256112)) ;
#104541 = CARTESIAN_POINT('Ctrl Pts',(34.8449278716688,258.191447886093,23.7755143142661)) ;
#104542 = CARTESIAN_POINT('Ctrl Pts',(34.841808227447,258.175001311387,23.7859297354669)) ;
#104543 = CARTESIAN_POINT('Ctrl Pts',(34.8396797931897,258.156933541317,23.7930320573423)) ;
#104544 = CARTESIAN_POINT('Ctrl Pts',(34.8375516212179,258.138867997726,23.8001335040032)) ;
#104545 = CARTESIAN_POINT('Ctrl Pts',(34.8364552827619,258.119527473902,23.8037867439466)) ;
#104546 = CARTESIAN_POINT('Ctrl Pts',(34.8364552827619,258.1,23.8037867439466)) ;
#104547 = CARTESIAN_POINT('Origin',(42.9386363636364,258.1,25.3708035475559)) ;
#104548 = CARTESIAN_POINT('',(45.2754819011524,258.1,25.5208035475559)) ;
#104549 = CARTESIAN_POINT('',(45.6772727272728,258.1,25.5208035475559)) ;
#104550 = CARTESIAN_POINT('',(42.9386363636364,258.1,25.5208035475559)) ;
#104551 = CARTESIAN_POINT('Ctrl Pts',(45.6772727272728,258.1,25.5208035475559)) ;
#104552 = CARTESIAN_POINT('Ctrl Pts',(45.6772727272728,258.119527473902,25.5208035475559)) ;
#104553 = CARTESIAN_POINT('Ctrl Pts',(45.6773589606669,258.138867997726,25.5169903226876)) ;
#104554 = CARTESIAN_POINT('Ctrl Pts',(45.6775294165481,258.156933541317,25.5095788042595)) ;
#104555 = CARTESIAN_POINT('Ctrl Pts',(45.6776998934371,258.175001311387,25.5021663724021)) ;
#104556 = CARTESIAN_POINT('Ctrl Pts',(45.6779514776262,258.191447886093,25.4912966951182)) ;
#104557 = CARTESIAN_POINT('Ctrl Pts',(45.6782777598469,258.205348530944,25.4775822300161)) ;
#104558 = CARTESIAN_POINT('Ctrl Pts',(45.6786041293904,258.21925289602,25.4638640945166)) ;
#104559 = CARTESIAN_POINT('Ctrl Pts',(45.6789992518937,258.230343922473,25.4475621758455)) ;
#104560 = CARTESIAN_POINT('Ctrl Pts',(45.6794511277462,258.237998568189,25.4295946623431)) ;
#104561 = CARTESIAN_POINT('Ctrl Pts',(45.6798845823047,258.245341162533,25.4123596173871)) ;
#104562 = CARTESIAN_POINT('Ctrl Pts',(45.6803627963736,258.249390031724,25.3939014545241)) ;
#104563 = CARTESIAN_POINT('Ctrl Pts',(45.6808685931367,258.249936222763,25.3751772306343)) ;
#104564 = CARTESIAN_POINT('Ctrl Pts',(45.6809079648118,258.249978738764,25.3737197202007)) ;
#104565 = CARTESIAN_POINT('Ctrl Pts',(45.6809474726105,258.25,25.3722616708597)) ;
#104566 = CARTESIAN_POINT('Ctrl Pts',(45.6809871063617,258.25,25.3708035475559)) ;
#104567 = CARTESIAN_POINT('Ctrl Pts',(45.1376473638895,258.25,25.3708035475559)) ;
#104568 = CARTESIAN_POINT('Ctrl Pts',(45.1381850335699,258.25,25.3713806182195)) ;
#104569 = CARTESIAN_POINT('Ctrl Pts',(45.1387226600676,258.249996669894,25.3719577367957)) ;
#104570 = CARTESIAN_POINT('Ctrl Pts',(45.1531132725512,258.249818328848,25.3874079531319)) ;
#104571 = CARTESIAN_POINT('Ctrl Pts',(45.1669867461377,258.247433157513,25.4023669543169)) ;
#104572 = CARTESIAN_POINT('Ctrl Pts',(45.1932346560144,258.238259809032,25.4307822523842)) ;
#104573 = CARTESIAN_POINT('Ctrl Pts',(45.205764078524,258.231622782802,25.4444014590284)) ;
#104574 = CARTESIAN_POINT('Ctrl Pts',(45.2303168022832,258.21278678422,25.4711791289339)) ;
#104575 = CARTESIAN_POINT('Ctrl Pts',(45.2422449580739,258.199976451841,25.4842448897419)) ;
#104576 = CARTESIAN_POINT('Ctrl Pts',(45.2595447243168,258.171958342729,25.5032424051016)) ;
#104577 = CARTESIAN_POINT('Ctrl Pts',(45.2657214856064,258.158041775475,25.5100439438662)) ;
#104578 = CARTESIAN_POINT('Ctrl Pts',(45.2735311811371,258.129045309865,25.5186503795949)) ;
#104579 = CARTESIAN_POINT('Ctrl Pts',(45.2754819011524,258.114679223254,25.5208035475559)) ;
#104580 = CARTESIAN_POINT('Ctrl Pts',(45.2754819011524,258.1,25.5208035475559)) ;
#104581 = CARTESIAN_POINT('Origin',(37.7033982898842,258.1,23.8426568872864)) ;
#104582 = CARTESIAN_POINT('Ctrl Pts',(35.6120145486888,258.25,23.1631251173908)) ;
#104583 = CARTESIAN_POINT('Ctrl Pts',(35.611681519077,258.25,23.162410141506)) ;
#104584 = CARTESIAN_POINT('Ctrl Pts',(35.6113485453403,258.249996669894,23.1616951333977)) ;
#104585 = CARTESIAN_POINT('Ctrl Pts',(35.6024366389787,258.249818328848,23.1425541606558)) ;
#104586 = CARTESIAN_POINT('Ctrl Pts',(35.593864767106,258.247433157512,23.1240401659927)) ;
#104587 = CARTESIAN_POINT('Ctrl Pts',(35.5776823313822,258.238259809032,23.0889045613858)) ;
#104588 = CARTESIAN_POINT('Ctrl Pts',(35.5699747087623,258.231622782802,23.0720801216756)) ;
#104589 = CARTESIAN_POINT('Ctrl Pts',(35.5548984359091,258.21278678422,23.0390258353215)) ;
#104590 = CARTESIAN_POINT('Ctrl Pts',(35.5475916277511,258.199976451841,23.0229135555139)) ;
#104591 = CARTESIAN_POINT('Ctrl Pts',(35.5370091274324,258.171958342729,22.9994999229698)) ;
#104592 = CARTESIAN_POINT('Ctrl Pts',(35.5332364694246,258.158041775475,22.9911225509982)) ;
#104593 = CARTESIAN_POINT('Ctrl Pts',(35.5284685425009,258.129045309865,22.9805240155765)) ;
#104594 = CARTESIAN_POINT('Ctrl Pts',(35.5272786630106,258.114679223254,22.9778734255204)) ;
#104595 = CARTESIAN_POINT('Ctrl Pts',(35.5272786630106,258.1,22.9778734255204)) ;
#104596 = CARTESIAN_POINT('Ctrl Pts',(35.1451528796411,258.1,22.8537132320652)) ;
#104597 = CARTESIAN_POINT('Ctrl Pts',(35.1451528796411,258.119527473902,22.8537132320652)) ;
#104598 = CARTESIAN_POINT('Ctrl Pts',(35.1438925155222,258.138867997726,22.8573131768401)) ;
#104599 = CARTESIAN_POINT('Ctrl Pts',(35.1414401171971,258.156933541317,22.8643092759728)) ;
#104600 = CARTESIAN_POINT('Ctrl Pts',(35.1389874166274,258.175001311387,22.8713062373364)) ;
#104601 = CARTESIAN_POINT('Ctrl Pts',(35.1353892308407,258.191447886093,22.8815661709573)) ;
#104602 = CARTESIAN_POINT('Ctrl Pts',(35.1308409152232,258.205348530944,22.894508575609)) ;
#104603 = CARTESIAN_POINT('Ctrl Pts',(35.1262913823417,258.21925289602,22.9074544440319)) ;
#104604 = CARTESIAN_POINT('Ctrl Pts',(35.1208780285999,258.230343922473,22.9228363904437)) ;
#104605 = CARTESIAN_POINT('Ctrl Pts',(35.1148960021068,258.237998568189,22.9397848739239)) ;
#104606 = CARTESIAN_POINT('Ctrl Pts',(35.109157840534,258.245341162533,22.9560424309131)) ;
#104607 = CARTESIAN_POINT('Ctrl Pts',(35.1029991459193,258.249390031724,22.9734494107092)) ;
#104608 = CARTESIAN_POINT('Ctrl Pts',(35.0967320012226,258.249936222763,22.9911009060562)) ;
#104609 = CARTESIAN_POINT('Ctrl Pts',(35.0962441610409,258.249978738764,22.992474914335)) ;
#104610 = CARTESIAN_POINT('Ctrl Pts',(35.0957560248659,258.25,22.9938493930803)) ;
#104611 = CARTESIAN_POINT('Ctrl Pts',(35.0952677460478,258.25,22.9952239032473)) ;
#104612 = CARTESIAN_POINT('Origin',(40.2,258.1,25.0213203435596)) ;
#104613 = CARTESIAN_POINT('Ctrl Pts',(35.9999382971499,258.25,22.4017818933262)) ;
#104614 = CARTESIAN_POINT('Ctrl Pts',(35.9991641196141,258.25,22.4019327189915)) ;
#104615 = CARTESIAN_POINT('Ctrl Pts',(35.9983899488515,258.249996669894,22.402083608801)) ;
#104616 = CARTESIAN_POINT('Ctrl Pts',(35.9776662894848,258.249818328848,22.4061245065949)) ;
#104617 = CARTESIAN_POINT('Ctrl Pts',(35.9576497332977,258.247433157512,22.4100719696)) ;
#104618 = CARTESIAN_POINT('Ctrl Pts',(35.9197126349982,258.238259809032,22.4176322943074)) ;
#104619 = CARTESIAN_POINT('Ctrl Pts',(35.9015709504457,258.231622782802,22.4212858541613)) ;
#104620 = CARTESIAN_POINT('Ctrl Pts',(35.8659678602058,258.21278678422,22.4285177152552)) ;
#104621 = CARTESIAN_POINT('Ctrl Pts',(35.8486379179467,258.199976451841,22.4320769437325)) ;
#104622 = CARTESIAN_POINT('Ctrl Pts',(35.823475653699,258.171958342729,22.4372777090437)) ;
#104623 = CARTESIAN_POINT('Ctrl Pts',(35.8144807046667,258.158041775475,22.4391496602992)) ;
#104624 = CARTESIAN_POINT('Ctrl Pts',(35.8031037922653,258.129045309865,22.4415219892068)) ;
#104625 = CARTESIAN_POINT('Ctrl Pts',(35.8002600262485,258.114679223254,22.4421173342227)) ;
#104626 = CARTESIAN_POINT('Ctrl Pts',(35.8002600262485,258.1,22.4421173342227)) ;
#104627 = CARTESIAN_POINT('Origin',(38.0634790637697,258.1,23.9010320185483)) ;
#104628 = CARTESIAN_POINT('Ctrl Pts',(35.5603672117703,258.25,22.0824148057165)) ;
#104629 = CARTESIAN_POINT('Ctrl Pts',(35.5595422127744,258.25,22.0836177483838)) ;
#104630 = CARTESIAN_POINT('Ctrl Pts',(35.5587171553568,258.249978738764,22.0848205571812)) ;
#104631 = CARTESIAN_POINT('Ctrl Pts',(35.5578923045725,258.249936222763,22.0860228499814)) ;
#104632 = CARTESIAN_POINT('Ctrl Pts',(35.54729568008,258.249390031724,22.1014683651895)) ;
#104633 = CARTESIAN_POINT('Ctrl Pts',(35.5368331274791,258.245341162533,22.1166824198106)) ;
#104634 = CARTESIAN_POINT('Ctrl Pts',(35.5270532943355,258.237998568189,22.1308806422756)) ;
#104635 = CARTESIAN_POINT('Ctrl Pts',(35.5168578301224,258.230343922473,22.1456822720076)) ;
#104636 = CARTESIAN_POINT('Ctrl Pts',(35.5075954635632,258.21925289602,22.1591030484335)) ;
#104637 = CARTESIAN_POINT('Ctrl Pts',(35.4997961843348,258.205348530944,22.1703930883883)) ;
#104638 = CARTESIAN_POINT('Ctrl Pts',(35.4919989918663,258.191447886093,22.1816801076021)) ;
#104639 = CARTESIAN_POINT('Ctrl Pts',(35.4858134917463,258.175001311387,22.1906217387244)) ;
#104640 = CARTESIAN_POINT('Ctrl Pts',(35.4815944923173,258.156933541317,22.1967187258679)) ;
#104641 = CARTESIAN_POINT('Ctrl Pts',(35.477376012793,258.138867997726,22.2028149616836)) ;
#104642 = CARTESIAN_POINT('Ctrl Pts',(35.4752044197329,258.119527473902,22.2059506121226)) ;
#104643 = CARTESIAN_POINT('Ctrl Pts',(35.475204419733,258.1,22.2059506121227)) ;
#104644 = CARTESIAN_POINT('Origin',(42.9125942086827,258.1,24.5074134442792)) ;
#104645 = CARTESIAN_POINT('',(45.1814189338688,258.1,23.9279469374017)) ;
#104646 = CARTESIAN_POINT('',(45.5635447172382,258.1,23.8037867439466)) ;
#104647 = CARTESIAN_POINT('',(42.9589467578389,258.1,24.6500719217234)) ;
#104648 = CARTESIAN_POINT('Ctrl Pts',(45.5635447172382,258.1,23.8037867439466)) ;
#104649 = CARTESIAN_POINT('Ctrl Pts',(45.5635447172384,258.119527473902,23.8037867439465)) ;
#104650 = CARTESIAN_POINT('Ctrl Pts',(45.5624483787821,258.138867997726,23.8001335040032)) ;
#104651 = CARTESIAN_POINT('Ctrl Pts',(45.5603202068104,258.156933541317,23.7930320573423)) ;
#104652 = CARTESIAN_POINT('Ctrl Pts',(45.5581917725532,258.175001311387,23.7859297354669)) ;
#104653 = CARTESIAN_POINT('Ctrl Pts',(45.5550721283311,258.191447886093,23.7755143142662)) ;
#104654 = CARTESIAN_POINT('Ctrl Pts',(45.551144438378,258.205348530944,23.7623702561121)) ;
#104655 = CARTESIAN_POINT('Ctrl Pts',(45.5472156972587,258.21925289602,23.7492226802186)) ;
#104656 = CARTESIAN_POINT('Ctrl Pts',(45.5425539111806,258.230343922473,23.7335965346699)) ;
#104657 = CARTESIAN_POINT('Ctrl Pts',(45.5374314036356,258.237998568189,23.716368776554)) ;
#104658 = CARTESIAN_POINT('Ctrl Pts',(45.5325177216277,258.245341162533,23.6998433299152)) ;
#104659 = CARTESIAN_POINT('Ctrl Pts',(45.5272686442365,258.249390031724,23.6821407975691)) ;
#104660 = CARTESIAN_POINT('Ctrl Pts',(45.5219635821412,258.249936222763,23.6641767026333)) ;
#104661 = CARTESIAN_POINT('Ctrl Pts',(45.5215506313346,258.249978738764,23.6627783613209)) ;
#104662 = CARTESIAN_POINT('Ctrl Pts',(45.5211376434632,258.25,23.6613794654128)) ;
#104663 = CARTESIAN_POINT('Ctrl Pts',(45.5207247525196,258.25,23.65998046024)) ;
#104664 = CARTESIAN_POINT('Ctrl Pts',(45.0039779498781,258.25,23.8278816743835)) ;
#104665 = CARTESIAN_POINT('Ctrl Pts',(45.0046676287764,258.25,23.8282643521315)) ;
#104666 = CARTESIAN_POINT('Ctrl Pts',(45.0053572814057,258.249996669895,23.8286470887883)) ;
#104667 = CARTESIAN_POINT('Ctrl Pts',(45.0238179465998,258.249818328848,23.8388941738985)) ;
#104668 = CARTESIAN_POINT('Ctrl Pts',(45.0416349896415,258.247433157512,23.8488338903423)) ;
#104669 = CARTESIAN_POINT('Ctrl Pts',(45.0753790453705,258.238259809032,23.8677473945122)) ;
#104670 = CARTESIAN_POINT('Ctrl Pts',(45.091503800596,258.231622782802,23.8768282252524)) ;
#104671 = CARTESIAN_POINT('Ctrl Pts',(45.1231295835901,258.21278678422,23.8947080938071)) ;
#104672 = CARTESIAN_POINT('Ctrl Pts',(45.1385114760162,258.199976451841,23.903448367913)) ;
#104673 = CARTESIAN_POINT('Ctrl Pts',(45.1608350865288,258.171958342729,23.9161701569214)) ;
#104674 = CARTESIAN_POINT('Ctrl Pts',(45.1688113266691,258.158041775475,23.9207300804757)) ;
#104675 = CARTESIAN_POINT('Ctrl Pts',(45.1788983233951,258.129045309865,23.9265019586177)) ;
#104676 = CARTESIAN_POINT('Ctrl Pts',(45.1814189338688,258.114679223254,23.9279469374017)) ;
#104677 = CARTESIAN_POINT('Ctrl Pts',(45.1814189338688,258.1,23.9279469374017)) ;
#104678 = CARTESIAN_POINT('Origin',(38.1898177136379,258.1,23.1288524263407)) ;
#104679 = CARTESIAN_POINT('Ctrl Pts',(36.4107804436157,258.25,21.836306190763)) ;
#104680 = CARTESIAN_POINT('Ctrl Pts',(36.410684653332,258.25,21.835523296477)) ;
#104681 = CARTESIAN_POINT('Ctrl Pts',(36.410588926147,258.249996669895,21.8347403888173)) ;
#104682 = CARTESIAN_POINT('Ctrl Pts',(36.4080280853953,258.249818328848,21.8137823114415)) ;
#104683 = CARTESIAN_POINT('Ctrl Pts',(36.4055968897784,258.247433157512,21.7935256020932)) ;
#104684 = CARTESIAN_POINT('Ctrl Pts',(36.4010639777649,258.238259809032,21.7551090087287)) ;
#104685 = CARTESIAN_POINT('Ctrl Pts',(36.3989326308384,258.231622782802,21.7367262293337)) ;
#104686 = CARTESIAN_POINT('Ctrl Pts',(36.3948085795202,258.21278678422,21.7006309103817)) ;
#104687 = CARTESIAN_POINT('Ctrl Pts',(36.392838360287,258.199976451841,21.6830492937829)) ;
#104688 = CARTESIAN_POINT('Ctrl Pts',(36.3900090147564,258.171958342729,21.6575114335404)) ;
#104689 = CARTESIAN_POINT('Ctrl Pts',(36.3890097540817,258.158041775475,21.648378263899)) ;
#104690 = CARTESIAN_POINT('Ctrl Pts',(36.3877503136725,258.129045309865,21.6368250872756)) ;
#104691 = CARTESIAN_POINT('Ctrl Pts',(36.3874377484021,258.114679223254,21.633936533347)) ;
#104692 = CARTESIAN_POINT('Ctrl Pts',(36.3874377484021,258.1,21.633936533347)) ;
#104693 = CARTESIAN_POINT('Ctrl Pts',(36.0623821418867,258.1,21.3977698112471)) ;
#104694 = CARTESIAN_POINT('Ctrl Pts',(36.0623821418865,258.119527473902,21.3977698112469)) ;
#104695 = CARTESIAN_POINT('Ctrl Pts',(36.060071020264,258.138867997726,21.4008040882515)) ;
#104696 = CARTESIAN_POINT('Ctrl Pts',(36.05557673733,258.156933541317,21.4066999411607)) ;
#104697 = CARTESIAN_POINT('Ctrl Pts',(36.0510819005001,258.175001311387,21.4125965207016)) ;
#104698 = CARTESIAN_POINT('Ctrl Pts',(36.0444893286114,258.191447886093,21.421242396872)) ;
#104699 = CARTESIAN_POINT('Ctrl Pts',(36.0361642004197,258.205348530944,21.4321458483309)) ;
#104700 = CARTESIAN_POINT('Ctrl Pts',(36.0278368441769,258.21925289602,21.4430522178765)) ;
#104701 = CARTESIAN_POINT('Ctrl Pts',(36.0179351559774,258.230343922473,21.4560084999414)) ;
#104702 = CARTESIAN_POINT('Ctrl Pts',(36.0070085412762,258.237998568188,21.4702789177496)) ;
#104703 = CARTESIAN_POINT('Ctrl Pts',(35.9965273639244,258.245341162533,21.4839675838205)) ;
#104704 = CARTESIAN_POINT('Ctrl Pts',(35.9852910446948,258.249390031724,21.4986194640775)) ;
#104705 = CARTESIAN_POINT('Ctrl Pts',(35.9738760238622,258.249936222763,21.5134703795415)) ;
#104706 = CARTESIAN_POINT('Ctrl Pts',(35.9729874683704,258.249978738764,21.5146263881627)) ;
#104707 = CARTESIAN_POINT('Ctrl Pts',(35.9720984859888,258.25,21.5157827527548)) ;
#104708 = CARTESIAN_POINT('Ctrl Pts',(35.9712093582363,258.25,21.5169391031534)) ;
#104709 = CARTESIAN_POINT('Origin',(40.2,258.1,25.0213203435596)) ;
#104710 = CARTESIAN_POINT('Ctrl Pts',(37.0149858472034,258.25,21.2321007871753)) ;
#104711 = CARTESIAN_POINT('Ctrl Pts',(37.0142029529195,258.25,21.2320049968919)) ;
#104712 = CARTESIAN_POINT('Ctrl Pts',(37.0134200452556,258.249996669894,21.2319092697064)) ;
#104713 = CARTESIAN_POINT('Ctrl Pts',(36.9924619678836,258.249818328848,21.2293484289546)) ;
#104714 = CARTESIAN_POINT('Ctrl Pts',(36.972205258534,258.247433157512,21.226917233338)) ;
#104715 = CARTESIAN_POINT('Ctrl Pts',(36.9337886651695,258.238259809032,21.2223843213245)) ;
#104716 = CARTESIAN_POINT('Ctrl Pts',(36.9154058857743,258.231622782802,21.220252974398)) ;
#104717 = CARTESIAN_POINT('Ctrl Pts',(36.8793105668222,258.21278678422,21.2161289230798)) ;
#104718 = CARTESIAN_POINT('Ctrl Pts',(36.8617289502234,258.199976451841,21.2141587038466)) ;
#104719 = CARTESIAN_POINT('Ctrl Pts',(36.8361910899808,258.171958342729,21.211329358316)) ;
#104720 = CARTESIAN_POINT('Ctrl Pts',(36.8270579203394,258.158041775475,21.2103300976413)) ;
#104721 = CARTESIAN_POINT('Ctrl Pts',(36.815504743716,258.129045309865,21.2090706572321)) ;
#104722 = CARTESIAN_POINT('Ctrl Pts',(36.8126161897874,258.114679223254,21.2087580919617)) ;
#104723 = CARTESIAN_POINT('Ctrl Pts',(36.8126161897874,258.1,21.2087580919617)) ;
#104724 = CARTESIAN_POINT('Origin',(38.5142359724255,258.1,23.2956415537952)) ;
#104725 = CARTESIAN_POINT('Ctrl Pts',(36.6956187595937,258.25,20.7925297017959)) ;
#104726 = CARTESIAN_POINT('Ctrl Pts',(36.6944624091956,258.25,20.7934188295481)) ;
#104727 = CARTESIAN_POINT('Ctrl Pts',(36.6933060446015,258.249978738764,20.7943078119286)) ;
#104728 = CARTESIAN_POINT('Ctrl Pts',(36.6921500359814,258.249936222763,20.795196367421)) ;
#104729 = CARTESIAN_POINT('Ctrl Pts',(36.6772991205284,258.249390031724,20.8066113882632)) ;
#104730 = CARTESIAN_POINT('Ctrl Pts',(36.6626472402613,258.245341162533,20.8178477074839)) ;
#104731 = CARTESIAN_POINT('Ctrl Pts',(36.6489585741903,258.237998568189,20.8283288848361)) ;
#104732 = CARTESIAN_POINT('Ctrl Pts',(36.6346881563824,258.230343922473,20.8392554995376)) ;
#104733 = CARTESIAN_POINT('Ctrl Pts',(36.6217318743171,258.21925289602,20.8491571877367)) ;
#104734 = CARTESIAN_POINT('Ctrl Pts',(36.6108255047715,258.205348530944,20.8574845439796)) ;
#104735 = CARTESIAN_POINT('Ctrl Pts',(36.5999220533126,258.191447886093,20.8658096721713)) ;
#104736 = CARTESIAN_POINT('Ctrl Pts',(36.5912761771423,258.175001311387,20.8724022440602)) ;
#104737 = CARTESIAN_POINT('Ctrl Pts',(36.5853795976013,258.156933541317,20.8768970808899)) ;
#104738 = CARTESIAN_POINT('Ctrl Pts',(36.5794837446919,258.138867997726,20.8813913638238)) ;
#104739 = CARTESIAN_POINT('Ctrl Pts',(36.5764494676877,258.119527473902,20.8837024854467)) ;
#104740 = CARTESIAN_POINT('Ctrl Pts',(36.5764494676876,258.1,20.8837024854466)) ;
#104741 = CARTESIAN_POINT('Origin',(42.621024432828,258.1,23.6943281289039)) ;
#104742 = CARTESIAN_POINT('',(44.5997399737516,258.1,22.4421173342227)) ;
#104743 = CARTESIAN_POINT('',(44.9247955802669,258.1,22.2059506121228)) ;
#104744 = CARTESIAN_POINT('',(42.7091922206719,258.1,23.8156806780601)) ;
#104745 = CARTESIAN_POINT('Ctrl Pts',(44.9247955802669,258.1,22.2059506121228)) ;
#104746 = CARTESIAN_POINT('Ctrl Pts',(44.9247955802668,258.119527473902,22.2059506121229)) ;
#104747 = CARTESIAN_POINT('Ctrl Pts',(44.922623987207,258.138867997726,22.2028149616837)) ;
#104748 = CARTESIAN_POINT('Ctrl Pts',(44.9184055076825,258.156933541317,22.196718725868)) ;
#104749 = CARTESIAN_POINT('Ctrl Pts',(44.9141865082535,258.175001311387,22.1906217387246)) ;
#104750 = CARTESIAN_POINT('Ctrl Pts',(44.9080010081334,258.191447886093,22.1816801076024)) ;
#104751 = CARTESIAN_POINT('Ctrl Pts',(44.9002038156649,258.205348530944,22.1703930883885)) ;
#104752 = CARTESIAN_POINT('Ctrl Pts',(44.8924045364365,258.21925289602,22.1591030484337)) ;
#104753 = CARTESIAN_POINT('Ctrl Pts',(44.8831421698776,258.230343922473,22.1456822720076)) ;
#104754 = CARTESIAN_POINT('Ctrl Pts',(44.872946705665,258.237998568189,22.1308806422754)) ;
#104755 = CARTESIAN_POINT('Ctrl Pts',(44.8631668725217,258.245341162533,22.1166824198098)) ;
#104756 = CARTESIAN_POINT('Ctrl Pts',(44.8527043199125,258.249390031724,22.101468365193)) ;
#104757 = CARTESIAN_POINT('Ctrl Pts',(44.8421076954281,258.249936222763,22.086022849981)) ;
#104758 = CARTESIAN_POINT('Ctrl Pts',(44.8412828446445,258.249978738764,22.0848205571807)) ;
#104759 = CARTESIAN_POINT('Ctrl Pts',(44.8404577872252,258.25,22.0836177483837)) ;
#104760 = CARTESIAN_POINT('Ctrl Pts',(44.8396327882295,258.25,22.0824148057166)) ;
#104761 = CARTESIAN_POINT('Ctrl Pts',(44.4000617028502,258.25,22.4017818933262)) ;
#104762 = CARTESIAN_POINT('Ctrl Pts',(44.400835880386,258.25,22.4019327189915)) ;
#104763 = CARTESIAN_POINT('Ctrl Pts',(44.4016100511485,258.249996669894,22.4020836088011)) ;
#104764 = CARTESIAN_POINT('Ctrl Pts',(44.4223337105146,258.249818328848,22.4061245065945)) ;
#104765 = CARTESIAN_POINT('Ctrl Pts',(44.4423502667022,258.247433157512,22.4100719695999)) ;
#104766 = CARTESIAN_POINT('Ctrl Pts',(44.4802873650017,258.238259809032,22.4176322943074)) ;
#104767 = CARTESIAN_POINT('Ctrl Pts',(44.4984290495542,258.231622782802,22.4212858541613)) ;
#104768 = CARTESIAN_POINT('Ctrl Pts',(44.5340321397943,258.21278678422,22.4285177152552)) ;
#104769 = CARTESIAN_POINT('Ctrl Pts',(44.5513620820533,258.199976451841,22.4320769437325)) ;
#104770 = CARTESIAN_POINT('Ctrl Pts',(44.5765243463011,258.171958342729,22.4372777090437)) ;
#104771 = CARTESIAN_POINT('Ctrl Pts',(44.5855192953333,258.158041775475,22.4391496602992)) ;
#104772 = CARTESIAN_POINT('Ctrl Pts',(44.5968962077348,258.129045309865,22.4415219892068)) ;
#104773 = CARTESIAN_POINT('Ctrl Pts',(44.5997399737516,258.114679223254,22.4421173342227)) ;
#104774 = CARTESIAN_POINT('Ctrl Pts',(44.5997399737516,258.1,22.4421173342227)) ;
#104775 = CARTESIAN_POINT('Origin',(38.8730077853443,258.1,22.6002959107317)) ;
#104776 = CARTESIAN_POINT('Ctrl Pts',(37.5804615497666,258.25,20.8212586407095)) ;
#104777 = CARTESIAN_POINT('Ctrl Pts',(37.5806123754319,258.25,20.8204844631737)) ;
#104778 = CARTESIAN_POINT('Ctrl Pts',(37.5807632652414,258.249996669894,20.8197102924111)) ;
#104779 = CARTESIAN_POINT('Ctrl Pts',(37.5848041630348,258.249818328848,20.7989866330451)) ;
#104780 = CARTESIAN_POINT('Ctrl Pts',(37.5887516260403,258.247433157512,20.7789700768575)) ;
#104781 = CARTESIAN_POINT('Ctrl Pts',(37.5963119507477,258.238259809032,20.7410329785581)) ;
#104782 = CARTESIAN_POINT('Ctrl Pts',(37.5999655106017,258.231622782802,20.7228912940055)) ;
#104783 = CARTESIAN_POINT('Ctrl Pts',(37.6071973716956,258.21278678422,20.6872882037655)) ;
#104784 = CARTESIAN_POINT('Ctrl Pts',(37.6107566001728,258.199976451841,20.6699582615064)) ;
#104785 = CARTESIAN_POINT('Ctrl Pts',(37.615957365484,258.171958342729,20.6447959972586)) ;
#104786 = CARTESIAN_POINT('Ctrl Pts',(37.6178293167396,258.158041775475,20.6358010482264)) ;
#104787 = CARTESIAN_POINT('Ctrl Pts',(37.6202016456472,258.129045309865,20.6244241358249)) ;
#104788 = CARTESIAN_POINT('Ctrl Pts',(37.6207969906631,258.114679223254,20.6215803698081)) ;
#104789 = CARTESIAN_POINT('Ctrl Pts',(37.6207969906631,258.1,20.6215803698081)) ;
#104790 = CARTESIAN_POINT('Ctrl Pts',(37.384630268563,258.1,20.2965247632925)) ;
#104791 = CARTESIAN_POINT('Ctrl Pts',(37.384630268563,258.119527473902,20.2965247632926)) ;
#104792 = CARTESIAN_POINT('Ctrl Pts',(37.3814946181239,258.138867997726,20.2986963563525)) ;
#104793 = CARTESIAN_POINT('Ctrl Pts',(37.3753983823082,258.156933541317,20.302914835877)) ;
#104794 = CARTESIAN_POINT('Ctrl Pts',(37.3693013951648,258.175001311387,20.307133835306)) ;
#104795 = CARTESIAN_POINT('Ctrl Pts',(37.3603597640427,258.191447886093,20.3133193354261)) ;
#104796 = CARTESIAN_POINT('Ctrl Pts',(37.3490727448288,258.205348530944,20.3211165278946)) ;
#104797 = CARTESIAN_POINT('Ctrl Pts',(37.337782704874,258.21925289602,20.328915807123)) ;
#104798 = CARTESIAN_POINT('Ctrl Pts',(37.324361928448,258.230343922473,20.338178173682)) ;
#104799 = CARTESIAN_POINT('Ctrl Pts',(37.3095602987158,258.237998568189,20.3483736378947)) ;
#104800 = CARTESIAN_POINT('Ctrl Pts',(37.2953620762502,258.245341162533,20.358153471038)) ;
#104801 = CARTESIAN_POINT('Ctrl Pts',(37.280148021633,258.249390031724,20.3686160236467)) ;
#104802 = CARTESIAN_POINT('Ctrl Pts',(37.2647025064213,258.249936222763,20.3792126481315)) ;
#104803 = CARTESIAN_POINT('Ctrl Pts',(37.263500213621,258.249978738764,20.3800374989151)) ;
#104804 = CARTESIAN_POINT('Ctrl Pts',(37.262297404824,258.25,20.3808625563344)) ;
#104805 = CARTESIAN_POINT('Ctrl Pts',(37.261094462157,258.25,20.3816875553301)) ;
#104806 = CARTESIAN_POINT('Origin',(40.2,258.1,25.0213203435596)) ;
#104807 = CARTESIAN_POINT('Ctrl Pts',(38.3418047738312,258.25,20.4333348922484)) ;
#104808 = CARTESIAN_POINT('Ctrl Pts',(38.3410897979463,258.25,20.4330018626367)) ;
#104809 = CARTESIAN_POINT('Ctrl Pts',(38.3403747898381,258.249996669894,20.4326688888999)) ;
#104810 = CARTESIAN_POINT('Ctrl Pts',(38.3212338170963,258.249818328848,20.4237569825383)) ;
#104811 = CARTESIAN_POINT('Ctrl Pts',(38.3027198224331,258.247433157512,20.4151851106656)) ;
#104812 = CARTESIAN_POINT('Ctrl Pts',(38.267584217826,258.238259809032,20.3990026749417)) ;
#104813 = CARTESIAN_POINT('Ctrl Pts',(38.2507597781159,258.231622782802,20.3912950523219)) ;
#104814 = CARTESIAN_POINT('Ctrl Pts',(38.2177054917619,258.21278678422,20.3762187794687)) ;
#104815 = CARTESIAN_POINT('Ctrl Pts',(38.2015932119542,258.199976451841,20.3689119713107)) ;
#104816 = CARTESIAN_POINT('Ctrl Pts',(38.1781795794102,258.171958342729,20.3583294709921)) ;
#104817 = CARTESIAN_POINT('Ctrl Pts',(38.1698022074386,258.158041775475,20.3545568129842)) ;
#104818 = CARTESIAN_POINT('Ctrl Pts',(38.1592036720168,258.129045309865,20.3497888860605)) ;
#104819 = CARTESIAN_POINT('Ctrl Pts',(38.1565530819608,258.114679223254,20.3485990065702)) ;
#104820 = CARTESIAN_POINT('Ctrl Pts',(38.1565530819608,258.1,20.3485990065702)) ;
#104821 = CARTESIAN_POINT('Origin',(39.1300072095089,258.1,22.8591725524954)) ;
#104822 = CARTESIAN_POINT('Ctrl Pts',(38.1739035596879,258.25,19.9165880896081)) ;
#104823 = CARTESIAN_POINT('Ctrl Pts',(38.172529049521,258.25,19.9170763684262)) ;
#104824 = CARTESIAN_POINT('Ctrl Pts',(38.1711545707754,258.249978738764,19.9175645046008)) ;
#104825 = CARTESIAN_POINT('Ctrl Pts',(38.1697805624967,258.249936222763,19.9180523447825)) ;
#104826 = CARTESIAN_POINT('Ctrl Pts',(38.1521290671494,258.249390031724,19.9243194894788)) ;
#104827 = CARTESIAN_POINT('Ctrl Pts',(38.1347220873532,258.245341162533,19.9304781840928)) ;
#104828 = CARTESIAN_POINT('Ctrl Pts',(38.1184645303641,258.237998568189,19.9362163456658)) ;
#104829 = CARTESIAN_POINT('Ctrl Pts',(38.1015160468838,258.230343922473,19.9421983721592)) ;
#104830 = CARTESIAN_POINT('Ctrl Pts',(38.0861341004721,258.21925289602,19.9476117259011)) ;
#104831 = CARTESIAN_POINT('Ctrl Pts',(38.0731882320494,258.205348530944,19.9521612587827)) ;
#104832 = CARTESIAN_POINT('Ctrl Pts',(38.0602458273977,258.191447886093,19.9567095744004)) ;
#104833 = CARTESIAN_POINT('Ctrl Pts',(38.0499858937768,258.175001311387,19.9603077601871)) ;
#104834 = CARTESIAN_POINT('Ctrl Pts',(38.0429889324132,258.156933541317,19.9627604607569)) ;
#104835 = CARTESIAN_POINT('Ctrl Pts',(38.0359928332805,258.138867997726,19.9652128590819)) ;
#104836 = CARTESIAN_POINT('Ctrl Pts',(38.0323928885057,258.119527473902,19.9664732232009)) ;
#104837 = CARTESIAN_POINT('Ctrl Pts',(38.0323928885057,258.1,19.9664732232009)) ;
#104838 = CARTESIAN_POINT('Origin',(42.0924679172189,258.1,23.0111380571975)) ;
#104839 = CARTESIAN_POINT('',(43.5873838102126,258.1,21.2087580919617)) ;
#104840 = CARTESIAN_POINT('',(43.8235505323125,258.1,20.8837024854464)) ;
#104841 = CARTESIAN_POINT('',(42.2138204663752,258.1,23.0993058450414)) ;
#104842 = CARTESIAN_POINT('Ctrl Pts',(43.8235505323125,258.1,20.8837024854464)) ;
#104843 = CARTESIAN_POINT('Ctrl Pts',(43.8235505323124,258.119527473902,20.8837024854464)) ;
#104844 = CARTESIAN_POINT('Ctrl Pts',(43.8205162553077,258.138867997726,20.8813913638241)) ;
#104845 = CARTESIAN_POINT('Ctrl Pts',(43.8146204023984,258.156933541317,20.8768970808903)) ;
#104846 = CARTESIAN_POINT('Ctrl Pts',(43.8087238228574,258.175001311387,20.8724022440606)) ;
#104847 = CARTESIAN_POINT('Ctrl Pts',(43.8000779466875,258.191447886093,20.8658096721712)) ;
#104848 = CARTESIAN_POINT('Ctrl Pts',(43.7891744952286,258.205348530944,20.8574845439795)) ;
#104849 = CARTESIAN_POINT('Ctrl Pts',(43.7782681256829,258.21925289602,20.8491571877368)) ;
#104850 = CARTESIAN_POINT('Ctrl Pts',(43.7653118436174,258.230343922473,20.8392554995377)) ;
#104851 = CARTESIAN_POINT('Ctrl Pts',(43.7510414258095,258.237998568189,20.8283288848364)) ;
#104852 = CARTESIAN_POINT('Ctrl Pts',(43.7373527597384,258.245341162533,20.8178477074844)) ;
#104853 = CARTESIAN_POINT('Ctrl Pts',(43.7227008794732,258.249390031724,20.8066113882618)) ;
#104854 = CARTESIAN_POINT('Ctrl Pts',(43.7078499640187,258.249936222763,20.7951963674209)) ;
#104855 = CARTESIAN_POINT('Ctrl Pts',(43.7066939553985,258.249978738764,20.7943078119287)) ;
#104856 = CARTESIAN_POINT('Ctrl Pts',(43.7055375908041,258.25,20.7934188295486)) ;
#104857 = CARTESIAN_POINT('Ctrl Pts',(43.7043812404059,258.25,20.7925297017964)) ;
#104858 = CARTESIAN_POINT('Ctrl Pts',(43.3850141527966,258.25,21.2321007871753)) ;
#104859 = CARTESIAN_POINT('Ctrl Pts',(43.3857970470805,258.25,21.2320049968919)) ;
#104860 = CARTESIAN_POINT('Ctrl Pts',(43.3865799547445,258.249996669894,21.2319092697064)) ;
#104861 = CARTESIAN_POINT('Ctrl Pts',(43.4075380321166,258.249818328848,21.2293484289546)) ;
#104862 = CARTESIAN_POINT('Ctrl Pts',(43.4277947414661,258.247433157512,21.226917233338)) ;
#104863 = CARTESIAN_POINT('Ctrl Pts',(43.4662113348306,258.238259809032,21.2223843213245)) ;
#104864 = CARTESIAN_POINT('Ctrl Pts',(43.4845941142257,258.231622782802,21.220252974398)) ;
#104865 = CARTESIAN_POINT('Ctrl Pts',(43.5206894331777,258.21278678422,21.2161289230799)) ;
#104866 = CARTESIAN_POINT('Ctrl Pts',(43.5382710497766,258.199976451841,21.2141587038466)) ;
#104867 = CARTESIAN_POINT('Ctrl Pts',(43.5638089100192,258.171958342729,21.211329358316)) ;
#104868 = CARTESIAN_POINT('Ctrl Pts',(43.5729420796606,258.158041775475,21.2103300976413)) ;
#104869 = CARTESIAN_POINT('Ctrl Pts',(43.584495256284,258.129045309865,21.2090706572321)) ;
#104870 = CARTESIAN_POINT('Ctrl Pts',(43.5873838102126,258.114679223254,21.2087580919617)) ;
#104871 = CARTESIAN_POINT('Ctrl Pts',(43.5873838102126,258.1,21.2087580919617)) ;
#104872 = CARTESIAN_POINT('Origin',(39.6860931007195,258.1,22.3087261348769)) ;
#104873 = CARTESIAN_POINT('Ctrl Pts',(39.0065613308239,258.25,20.2173423936815)) ;
#104874 = CARTESIAN_POINT('Ctrl Pts',(39.0069440085709,258.25,20.2166527147851)) ;
#104875 = CARTESIAN_POINT('Ctrl Pts',(39.0073267452297,258.249996669894,20.2159630621521)) ;
#104876 = CARTESIAN_POINT('Ctrl Pts',(39.0175738303378,258.249818328848,20.197502396961)) ;
#104877 = CARTESIAN_POINT('Ctrl Pts',(39.0275135467826,258.247433157512,20.1796853539185)) ;
#104878 = CARTESIAN_POINT('Ctrl Pts',(39.0464270509528,258.238259809032,20.1459412981889)) ;
#104879 = CARTESIAN_POINT('Ctrl Pts',(39.0555078816928,258.231622782802,20.1298165429636)) ;
#104880 = CARTESIAN_POINT('Ctrl Pts',(39.0733877502474,258.21278678422,20.0981907599697)) ;
#104881 = CARTESIAN_POINT('Ctrl Pts',(39.0821280243534,258.199976451841,20.0828088675435)) ;
#104882 = CARTESIAN_POINT('Ctrl Pts',(39.0948498133619,258.171958342729,20.0604852570307)) ;
#104883 = CARTESIAN_POINT('Ctrl Pts',(39.0994097369161,258.158041775475,20.0525090168905)) ;
#104884 = CARTESIAN_POINT('Ctrl Pts',(39.1051816150581,258.129045309865,20.0424220201645)) ;
#104885 = CARTESIAN_POINT('Ctrl Pts',(39.1066265938421,258.114679223254,20.0399014096908)) ;
#104886 = CARTESIAN_POINT('Ctrl Pts',(39.1066265938421,258.1,20.0399014096908)) ;
#104887 = CARTESIAN_POINT('Ctrl Pts',(38.982466400387,258.1,19.6577756263215)) ;
#104888 = CARTESIAN_POINT('Ctrl Pts',(38.9824664003869,258.119527473902,19.6577756263214)) ;
#104889 = CARTESIAN_POINT('Ctrl Pts',(38.9788131604436,258.138867997726,19.6588719647777)) ;
#104890 = CARTESIAN_POINT('Ctrl Pts',(38.9717117137828,258.156933541317,19.6610001367495)) ;
#104891 = CARTESIAN_POINT('Ctrl Pts',(38.9646093919074,258.175001311387,19.6631285710069)) ;
#104892 = CARTESIAN_POINT('Ctrl Pts',(38.9541939707066,258.191447886093,19.6662482152287)) ;
#104893 = CARTESIAN_POINT('Ctrl Pts',(38.9410499125525,258.205348530944,19.6701759051818)) ;
#104894 = CARTESIAN_POINT('Ctrl Pts',(38.9279023366589,258.21925289602,19.674104646301)) ;
#104895 = CARTESIAN_POINT('Ctrl Pts',(38.9122761911104,258.230343922473,19.6787664323798)) ;
#104896 = CARTESIAN_POINT('Ctrl Pts',(38.8950484329945,258.237998568189,19.6838889399248)) ;
#104897 = CARTESIAN_POINT('Ctrl Pts',(38.8785229863557,258.245341162533,19.6888026219327)) ;
#104898 = CARTESIAN_POINT('Ctrl Pts',(38.8608204540116,258.249390031724,19.6940516993334)) ;
#104899 = CARTESIAN_POINT('Ctrl Pts',(38.8428563590732,258.249936222763,19.6993567614171)) ;
#104900 = CARTESIAN_POINT('Ctrl Pts',(38.841458017761,258.249978738764,19.6997697122226)) ;
#104901 = CARTESIAN_POINT('Ctrl Pts',(38.8400591218529,258.25,19.7001827000972)) ;
#104902 = CARTESIAN_POINT('Ctrl Pts',(38.8386601166805,258.25,19.7005955910407)) ;
#104903 = CARTESIAN_POINT('Origin',(40.2,258.1,25.0213203435596)) ;
#104904 = CARTESIAN_POINT('Ctrl Pts',(39.8505167960037,258.25,20.0836729796702)) ;
#104905 = CARTESIAN_POINT('Ctrl Pts',(39.8499397253391,258.25,20.0831353099888)) ;
#104906 = CARTESIAN_POINT('Ctrl Pts',(39.8493626067619,258.249996669894,20.0825976834901)) ;
#104907 = CARTESIAN_POINT('Ctrl Pts',(39.8339123904255,258.249818328848,20.0682070710063)) ;
#104908 = CARTESIAN_POINT('Ctrl Pts',(39.8189533892408,258.247433157512,20.0543335974202)) ;
#104909 = CARTESIAN_POINT('Ctrl Pts',(39.7905380911743,258.238259809032,20.0280856875442)) ;
#104910 = CARTESIAN_POINT('Ctrl Pts',(39.7769188845308,258.231622782802,20.0155562650352)) ;
#104911 = CARTESIAN_POINT('Ctrl Pts',(39.7501412146257,258.21278678422,19.9910035412763)) ;
#104912 = CARTESIAN_POINT('Ctrl Pts',(39.7370754538178,258.199976451841,19.9790753854857)) ;
#104913 = CARTESIAN_POINT('Ctrl Pts',(39.7180779384581,258.171958342729,19.9617756192428)) ;
#104914 = CARTESIAN_POINT('Ctrl Pts',(39.7112763996935,258.158041775475,19.9555988579533)) ;
#104915 = CARTESIAN_POINT('Ctrl Pts',(39.7026699639648,258.129045309865,19.9477891624225)) ;
#104916 = CARTESIAN_POINT('Ctrl Pts',(39.7005167960037,258.114679223254,19.9458384424072)) ;
#104917 = CARTESIAN_POINT('Ctrl Pts',(39.7005167960037,258.1,19.9458384424072)) ;
#104918 = CARTESIAN_POINT('Origin',(39.8505167960037,258.1,22.6343496415544)) ;
#104919 = CARTESIAN_POINT('Ctrl Pts',(39.8505167960037,258.25,19.5403332371979)) ;
#104920 = CARTESIAN_POINT('Ctrl Pts',(39.8490586726999,258.25,19.5403728709491)) ;
#104921 = CARTESIAN_POINT('Ctrl Pts',(39.8476006233589,258.249978738764,19.5404123787479)) ;
#104922 = CARTESIAN_POINT('Ctrl Pts',(39.8461431129253,258.249936222763,19.540451750423)) ;
#104923 = CARTESIAN_POINT('Ctrl Pts',(39.8274188890355,258.249390031724,19.5409575471857)) ;
#104924 = CARTESIAN_POINT('Ctrl Pts',(39.8089607261725,258.245341162533,19.5414357612546)) ;
#104925 = CARTESIAN_POINT('Ctrl Pts',(39.7917256812165,258.237998568189,19.5418692158132)) ;
#104926 = CARTESIAN_POINT('Ctrl Pts',(39.773758167714,258.230343922473,19.5423210916658)) ;
#104927 = CARTESIAN_POINT('Ctrl Pts',(39.757456249043,258.21925289602,19.5427162141691)) ;
#104928 = CARTESIAN_POINT('Ctrl Pts',(39.7437381135436,258.205348530944,19.5430425837128)) ;
#104929 = CARTESIAN_POINT('Ctrl Pts',(39.7300236484415,258.191447886093,19.5433688659337)) ;
#104930 = CARTESIAN_POINT('Ctrl Pts',(39.7191539711575,258.175001311387,19.5436204501225)) ;
#104931 = CARTESIAN_POINT('Ctrl Pts',(39.7117415393001,258.156933541317,19.5437909270115)) ;
#104932 = CARTESIAN_POINT('Ctrl Pts',(39.704330020872,258.138867997726,19.5439613828928)) ;
#104933 = CARTESIAN_POINT('Ctrl Pts',(39.7005167960037,258.119527473902,19.5440476162869)) ;
#104934 = CARTESIAN_POINT('Ctrl Pts',(39.7005167960037,258.1,19.5440476162869)) ;
#104935 = CARTESIAN_POINT('Origin',(41.3786634562732,258.1,22.5247186334439)) ;
#104936 = CARTESIAN_POINT('Ctrl Pts',(42.3676071114945,258.1,19.9664732232005)) ;
#104937 = CARTESIAN_POINT('Ctrl Pts',(42.3676071114945,258.119527473902,19.9664732232005)) ;
#104938 = CARTESIAN_POINT('Ctrl Pts',(42.3640071667196,258.138867997726,19.9652128590816)) ;
#104939 = CARTESIAN_POINT('Ctrl Pts',(42.357011067587,258.156933541317,19.9627604607565)) ;
#104940 = CARTESIAN_POINT('Ctrl Pts',(42.3500141062233,258.175001311387,19.9603077601868)) ;
#104941 = CARTESIAN_POINT('Ctrl Pts',(42.3397541726022,258.191447886093,19.9567095744005)) ;
#104942 = CARTESIAN_POINT('Ctrl Pts',(42.3268117679506,258.205348530944,19.9521612587828)) ;
#104943 = CARTESIAN_POINT('Ctrl Pts',(42.3138658995279,258.21925289602,19.9476117259012)) ;
#104944 = CARTESIAN_POINT('Ctrl Pts',(42.2984839531161,258.230343922473,19.9421983721593)) ;
#104945 = CARTESIAN_POINT('Ctrl Pts',(42.2815354696358,258.237998568189,19.9362163456661)) ;
#104946 = CARTESIAN_POINT('Ctrl Pts',(42.2652779126467,258.245341162533,19.9304781840933)) ;
#104947 = CARTESIAN_POINT('Ctrl Pts',(42.2478709328508,258.249390031724,19.9243194894782)) ;
#104948 = CARTESIAN_POINT('Ctrl Pts',(42.2302194375034,258.249936222763,19.9180523447823)) ;
#104949 = CARTESIAN_POINT('Ctrl Pts',(42.2288454292246,258.249978738764,19.9175645046006)) ;
#104950 = CARTESIAN_POINT('Ctrl Pts',(42.2274709504794,258.25,19.9170763684254)) ;
#104951 = CARTESIAN_POINT('Ctrl Pts',(42.2260964403124,258.25,19.9165880896073)) ;
#104952 = CARTESIAN_POINT('Ctrl Pts',(42.0581952261685,258.25,20.4333348922483)) ;
#104953 = CARTESIAN_POINT('Ctrl Pts',(42.0589102020544,258.25,20.433001862636)) ;
#104954 = CARTESIAN_POINT('Ctrl Pts',(42.0596252101647,258.249996669894,20.4326688888986)) ;
#104955 = CARTESIAN_POINT('Ctrl Pts',(42.0787661829066,258.249818328848,20.423756982537)) ;
#104956 = CARTESIAN_POINT('Ctrl Pts',(42.0972801775694,258.247433157512,20.4151851106646)) ;
#104957 = CARTESIAN_POINT('Ctrl Pts',(42.1324157821755,258.238259809031,20.3990026749411)) ;
#104958 = CARTESIAN_POINT('Ctrl Pts',(42.1492402218848,258.231622782802,20.3912950523216)) ;
#104959 = CARTESIAN_POINT('Ctrl Pts',(42.1822945082381,258.21278678422,20.3762187794687)) ;
#104960 = CARTESIAN_POINT('Ctrl Pts',(42.1984067880458,258.199976451841,20.3689119713107)) ;
#104961 = CARTESIAN_POINT('Ctrl Pts',(42.2218204205898,258.171958342729,20.3583294709921)) ;
#104962 = CARTESIAN_POINT('Ctrl Pts',(42.2301977925614,258.158041775475,20.3545568129842)) ;
#104963 = CARTESIAN_POINT('Ctrl Pts',(42.2407963279832,258.129045309865,20.3497888860605)) ;
#104964 = CARTESIAN_POINT('Ctrl Pts',(42.2434469180392,258.114679223254,20.3485990065702)) ;
#104965 = CARTESIAN_POINT('Ctrl Pts',(42.2434469180392,258.1,20.3485990065702)) ;
#104966 = CARTESIAN_POINT('Origin',(40.5494832039963,258.1,22.2826839799233)) ;
#104967 = CARTESIAN_POINT('Ctrl Pts',(40.5494832039963,258.25,20.0836729796702)) ;
#104968 = CARTESIAN_POINT('Ctrl Pts',(40.5500602746609,258.25,20.0831353099888)) ;
#104969 = CARTESIAN_POINT('Ctrl Pts',(40.5506373932381,258.249996669894,20.0825976834901)) ;
#104970 = CARTESIAN_POINT('Ctrl Pts',(40.5660876095746,258.249818328848,20.0682070710062)) ;
#104971 = CARTESIAN_POINT('Ctrl Pts',(40.5810466107592,258.247433157512,20.0543335974202)) ;
#104972 = CARTESIAN_POINT('Ctrl Pts',(40.6094619088255,258.238259809032,20.0280856875444)) ;
#104973 = CARTESIAN_POINT('Ctrl Pts',(40.6230811154692,258.231622782802,20.0155562650353)) ;
#104974 = CARTESIAN_POINT('Ctrl Pts',(40.6498587853742,258.21278678422,19.9910035412764)) ;
#104975 = CARTESIAN_POINT('Ctrl Pts',(40.6629245461822,258.199976451841,19.9790753854858)) ;
#104976 = CARTESIAN_POINT('Ctrl Pts',(40.681922061542,258.171958342729,19.9617756192429)) ;
#104977 = CARTESIAN_POINT('Ctrl Pts',(40.6887236003065,258.158041775475,19.9555988579533)) ;
#104978 = CARTESIAN_POINT('Ctrl Pts',(40.6973300360353,258.129045309865,19.9477891624225)) ;
#104979 = CARTESIAN_POINT('Ctrl Pts',(40.6994832039963,258.114679223254,19.9458384424072)) ;
#104980 = CARTESIAN_POINT('Ctrl Pts',(40.6994832039963,258.1,19.9458384424072)) ;
#104981 = CARTESIAN_POINT('Ctrl Pts',(40.6994832039963,258.1,19.5440476162867)) ;
#104982 = CARTESIAN_POINT('Ctrl Pts',(40.6994832039963,258.119527473902,19.5440476162867)) ;
#104983 = CARTESIAN_POINT('Ctrl Pts',(40.695669979128,258.138867997726,19.5439613828925)) ;
#104984 = CARTESIAN_POINT('Ctrl Pts',(40.6882584606999,258.156933541317,19.5437909270112)) ;
#104985 = CARTESIAN_POINT('Ctrl Pts',(40.6808460288425,258.175001311387,19.5436204501222)) ;
#104986 = CARTESIAN_POINT('Ctrl Pts',(40.6699763515586,258.191447886093,19.5433688659334)) ;
#104987 = CARTESIAN_POINT('Ctrl Pts',(40.6562618864565,258.205348530944,19.5430425837125)) ;
#104988 = CARTESIAN_POINT('Ctrl Pts',(40.642543750957,258.21925289602,19.5427162141689)) ;
#104989 = CARTESIAN_POINT('Ctrl Pts',(40.626241832286,258.230343922473,19.5423210916655)) ;
#104990 = CARTESIAN_POINT('Ctrl Pts',(40.6082743187836,258.237998568189,19.5418692158129)) ;
#104991 = CARTESIAN_POINT('Ctrl Pts',(40.5910392738275,258.245341162533,19.5414357612543)) ;
#104992 = CARTESIAN_POINT('Ctrl Pts',(40.5725811109643,258.249390031724,19.5409575471862)) ;
#104993 = CARTESIAN_POINT('Ctrl Pts',(40.5538568870747,258.249936222763,19.5404517504227)) ;
#104994 = CARTESIAN_POINT('Ctrl Pts',(40.5523993766411,258.249978738764,19.5404123787476)) ;
#104995 = CARTESIAN_POINT('Ctrl Pts',(40.5509413273001,258.25,19.5403728709489)) ;
#104996 = CARTESIAN_POINT('Ctrl Pts',(40.5494832039963,258.25,19.5403332371977)) ;
#104997 = CARTESIAN_POINT('Origin',(40.2,258.1,25.0213203435596)) ;
#104998 = CARTESIAN_POINT('Ctrl Pts',(41.3934386691762,258.25,20.2173423936815)) ;
#104999 = CARTESIAN_POINT('Ctrl Pts',(41.3930559914298,258.25,20.2166527147863)) ;
#105000 = CARTESIAN_POINT('Ctrl Pts',(41.3926732547717,258.249996669894,20.2159630621546)) ;
#105001 = CARTESIAN_POINT('Ctrl Pts',(41.3824261696639,258.249818328848,20.1975023969641)) ;
#105002 = CARTESIAN_POINT('Ctrl Pts',(41.3724864532189,258.247433157513,20.1796853539209)) ;
#105003 = CARTESIAN_POINT('Ctrl Pts',(41.353572949048,258.238259809032,20.1459412981901)) ;
#105004 = CARTESIAN_POINT('Ctrl Pts',(41.3444921183075,258.231622782802,20.1298165429642)) ;
#105005 = CARTESIAN_POINT('Ctrl Pts',(41.3266122497526,258.21278678422,20.0981907599697)) ;
#105006 = CARTESIAN_POINT('Ctrl Pts',(41.3178719756467,258.199976451841,20.0828088675435)) ;
#105007 = CARTESIAN_POINT('Ctrl Pts',(41.3051501866382,258.171958342729,20.0604852570307)) ;
#105008 = CARTESIAN_POINT('Ctrl Pts',(41.3005902630839,258.158041775475,20.0525090168905)) ;
#105009 = CARTESIAN_POINT('Ctrl Pts',(41.294818384942,258.129045309865,20.0424220201645)) ;
#105010 = CARTESIAN_POINT('Ctrl Pts',(41.2933734061579,258.114679223254,20.0399014096908)) ;
#105011 = CARTESIAN_POINT('Ctrl Pts',(41.2933734061579,258.1,20.0399014096908)) ;
#105012 = CARTESIAN_POINT('Origin',(40.6052362334984,258.1,22.6431800539285)) ;
#105013 = CARTESIAN_POINT('Ctrl Pts',(41.5613398833194,258.25,19.700595591041)) ;
#105014 = CARTESIAN_POINT('Ctrl Pts',(41.559940878147,258.25,19.7001827000975)) ;
#105015 = CARTESIAN_POINT('Ctrl Pts',(41.5585419822389,258.249978738764,19.699769712223)) ;
#105016 = CARTESIAN_POINT('Ctrl Pts',(41.5571436409267,258.249936222763,19.6993567614174)) ;
#105017 = CARTESIAN_POINT('Ctrl Pts',(41.5391795459882,258.249390031724,19.6940516993328)) ;
#105018 = CARTESIAN_POINT('Ctrl Pts',(41.5214770136451,258.245341162533,19.6888026219299)) ;
#105019 = CARTESIAN_POINT('Ctrl Pts',(41.5049515670062,258.237998568188,19.6838889399227)) ;
#105020 = CARTESIAN_POINT('Ctrl Pts',(41.4877238088901,258.230343922473,19.6787664323785)) ;
#105021 = CARTESIAN_POINT('Ctrl Pts',(41.4720976633413,258.21925289602,19.6741046463007)) ;
#105022 = CARTESIAN_POINT('Ctrl Pts',(41.4589500874477,258.205348530944,19.6701759051814)) ;
#105023 = CARTESIAN_POINT('Ctrl Pts',(41.4458060292936,258.191447886093,19.6662482152285)) ;
#105024 = CARTESIAN_POINT('Ctrl Pts',(41.4353906080926,258.175001311387,19.6631285710071)) ;
#105025 = CARTESIAN_POINT('Ctrl Pts',(41.4282882862172,258.156933541317,19.6610001367497)) ;
#105026 = CARTESIAN_POINT('Ctrl Pts',(41.4211868395564,258.138867997726,19.6588719647779)) ;
#105027 = CARTESIAN_POINT('Ctrl Pts',(41.4175335996131,258.119527473902,19.6577756263216)) ;
#105028 = CARTESIAN_POINT('Ctrl Pts',(41.4175335996131,258.1,19.6577756263216)) ;
#105029 = CARTESIAN_POINT('Origin',(41.8995934690622,258.1,19.7905095039363)) ;
#105030 = CARTESIAN_POINT('Origin',(40.2,258.1,19.5213203435596)) ;
#105031 = CARTESIAN_POINT('Origin',(40.2,258.1,25.0213203435596)) ;
#105032 = CARTESIAN_POINT('',(42.7792030093369,258.1,20.6215803698081)) ;
#105033 = CARTESIAN_POINT('Origin',(40.2,258.1,25.0213203435596)) ;
#105034 = CARTESIAN_POINT('Ctrl Pts',(42.8195384502335,258.25,20.8212586407095)) ;
#105035 = CARTESIAN_POINT('Ctrl Pts',(42.8193876245682,258.25,20.8204844631737)) ;
#105036 = CARTESIAN_POINT('Ctrl Pts',(42.8192367347586,258.249996669894,20.8197102924112)) ;
#105037 = CARTESIAN_POINT('Ctrl Pts',(42.8151958369648,258.249818328848,20.7989866330445)) ;
#105038 = CARTESIAN_POINT('Ctrl Pts',(42.8112483739597,258.247433157512,20.7789700768574)) ;
#105039 = CARTESIAN_POINT('Ctrl Pts',(42.8036880492523,258.238259809032,20.7410329785579)) ;
#105040 = CARTESIAN_POINT('Ctrl Pts',(42.8000344893984,258.231622782802,20.7228912940054)) ;
#105041 = CARTESIAN_POINT('Ctrl Pts',(42.7928026283045,258.21278678422,20.6872882037655)) ;
#105042 = CARTESIAN_POINT('Ctrl Pts',(42.7892433998272,258.199976451841,20.6699582615064)) ;
#105043 = CARTESIAN_POINT('Ctrl Pts',(42.784042634516,258.171958342729,20.6447959972585)) ;
#105044 = CARTESIAN_POINT('Ctrl Pts',(42.7821706832604,258.158041775475,20.6358010482263)) ;
#105045 = CARTESIAN_POINT('Ctrl Pts',(42.7797983543528,258.129045309865,20.6244241358249)) ;
#105046 = CARTESIAN_POINT('Ctrl Pts',(42.7792030093369,258.114679223254,20.6215803698081)) ;
#105047 = CARTESIAN_POINT('Ctrl Pts',(42.7792030093369,258.1,20.6215803698081)) ;
#105048 = CARTESIAN_POINT('Origin',(41.3202883250113,258.1,22.8847994073294)) ;
#105049 = CARTESIAN_POINT('',(43.0153697314369,258.1,20.2965247632928)) ;
#105050 = CARTESIAN_POINT('',(41.1989357758551,258.1,22.7966316194855)) ;
#105051 = CARTESIAN_POINT('Ctrl Pts',(43.1389055378432,258.25,20.3816875553299)) ;
#105052 = CARTESIAN_POINT('Ctrl Pts',(43.137702595176,258.25,20.3808625563341)) ;
#105053 = CARTESIAN_POINT('Ctrl Pts',(43.1364997863787,258.249978738764,20.3800374989159)) ;
#105054 = CARTESIAN_POINT('Ctrl Pts',(43.1352974935785,258.249936222763,20.3792126481319)) ;
#105055 = CARTESIAN_POINT('Ctrl Pts',(43.1198519783687,258.249390031724,20.368616023642)) ;
#105056 = CARTESIAN_POINT('Ctrl Pts',(43.1046379237506,258.245341162533,20.3581534710365)) ;
#105057 = CARTESIAN_POINT('Ctrl Pts',(43.0904397012851,258.237998568188,20.3483736378934)) ;
#105058 = CARTESIAN_POINT('Ctrl Pts',(43.0756380715526,258.230343922473,20.3381781736809)) ;
#105059 = CARTESIAN_POINT('Ctrl Pts',(43.0622172951261,258.21925289602,20.3289158071227)) ;
#105060 = CARTESIAN_POINT('Ctrl Pts',(43.0509272551714,258.205348530944,20.3211165278944)) ;
#105061 = CARTESIAN_POINT('Ctrl Pts',(43.0396402359575,258.191447886093,20.3133193354259)) ;
#105062 = CARTESIAN_POINT('Ctrl Pts',(43.0306986048352,258.175001311387,20.3071338353061)) ;
#105063 = CARTESIAN_POINT('Ctrl Pts',(43.0246016176917,258.156933541317,20.3029148358772)) ;
#105064 = CARTESIAN_POINT('Ctrl Pts',(43.0185053818759,258.138867997726,20.2986963563528)) ;
#105065 = CARTESIAN_POINT('Ctrl Pts',(43.0153697314369,258.119527473902,20.2965247632927)) ;
#105066 = CARTESIAN_POINT('Ctrl Pts',(43.0153697314369,258.1,20.2965247632927)) ;
#105067 = CARTESIAN_POINT('Origin',(43.4328188876086,258.1,20.5717268744974)) ;
#105068 = CARTESIAN_POINT('Origin',(43.4328188876086,258.1,20.5717268744974)) ;
#105069 = CARTESIAN_POINT('Origin',(38.5004065309378,258.1,19.7905095039363)) ;
#105070 = CARTESIAN_POINT('Origin',(40.2,258.1,25.0213203435596)) ;
#105071 = CARTESIAN_POINT('',(44.012562251598,258.1,21.6339365333471)) ;
#105072 = CARTESIAN_POINT('Origin',(40.2,258.1,25.0213203435596)) ;
#105073 = CARTESIAN_POINT('Ctrl Pts',(43.9892195563843,258.25,21.836306190763)) ;
#105074 = CARTESIAN_POINT('Ctrl Pts',(43.9893153466675,258.25,21.8355232964805)) ;
#105075 = CARTESIAN_POINT('Ctrl Pts',(43.9894110738529,258.249996669894,21.8347403888179)) ;
#105076 = CARTESIAN_POINT('Ctrl Pts',(43.9919719146049,258.249818328848,21.8137823114479)) ;
#105077 = CARTESIAN_POINT('Ctrl Pts',(43.9944031102213,258.247433157513,21.7935256020966)) ;
#105078 = CARTESIAN_POINT('Ctrl Pts',(43.998936022235,258.238259809032,21.7551090087302)) ;
#105079 = CARTESIAN_POINT('Ctrl Pts',(44.0010673691616,258.231622782802,21.7367262293345)) ;
#105080 = CARTESIAN_POINT('Ctrl Pts',(44.0051914204798,258.21278678422,21.7006309103821)) ;
#105081 = CARTESIAN_POINT('Ctrl Pts',(44.007161639713,258.199976451842,21.6830492937831)) ;
#105082 = CARTESIAN_POINT('Ctrl Pts',(44.0099909852436,258.171958342729,21.6575114335403)) ;
#105083 = CARTESIAN_POINT('Ctrl Pts',(44.0109902459184,258.158041775475,21.648378263899)) ;
#105084 = CARTESIAN_POINT('Ctrl Pts',(44.0122496863275,258.129045309865,21.6368250872756)) ;
#105085 = CARTESIAN_POINT('Ctrl Pts',(44.012562251598,258.114679223254,21.6339365333471)) ;
#105086 = CARTESIAN_POINT('Ctrl Pts',(44.012562251598,258.1,21.6339365333471)) ;
#105087 = CARTESIAN_POINT('Origin',(41.9256787897644,258.1,23.3355563159851)) ;
#105088 = CARTESIAN_POINT('',(44.3376178581133,258.1,21.3977698112471)) ;
#105089 = CARTESIAN_POINT('',(41.8375110019206,258.1,23.2142037668289)) ;
#105090 = CARTESIAN_POINT('Ctrl Pts',(44.428790641764,258.25,21.5169391031532)) ;
#105091 = CARTESIAN_POINT('Ctrl Pts',(44.4279015140119,258.25,21.5157827527552)) ;
#105092 = CARTESIAN_POINT('Ctrl Pts',(44.4270125316316,258.249978738765,21.5146263881606)) ;
#105093 = CARTESIAN_POINT('Ctrl Pts',(44.426123976139,258.249936222763,21.5134703795409)) ;
#105094 = CARTESIAN_POINT('Ctrl Pts',(44.4147089552931,258.249390031725,21.4986194640922)) ;
#105095 = CARTESIAN_POINT('Ctrl Pts',(44.4034726360758,258.245341162534,21.4839675838213)) ;
#105096 = CARTESIAN_POINT('Ctrl Pts',(44.3929914587233,258.237998568189,21.4702789177501)) ;
#105097 = CARTESIAN_POINT('Ctrl Pts',(44.3820648440218,258.230343922473,21.4560084999423)) ;
#105098 = CARTESIAN_POINT('Ctrl Pts',(44.3721631558235,258.21925289602,21.4430522178764)) ;
#105099 = CARTESIAN_POINT('Ctrl Pts',(44.3638357995807,258.205348530944,21.4321458483306)) ;
#105100 = CARTESIAN_POINT('Ctrl Pts',(44.355510671389,258.191447886093,21.4212423968717)) ;
#105101 = CARTESIAN_POINT('Ctrl Pts',(44.3489180994998,258.175001311387,21.4125965207017)) ;
#105102 = CARTESIAN_POINT('Ctrl Pts',(44.3444232626702,258.156933541317,21.4066999411606)) ;
#105103 = CARTESIAN_POINT('Ctrl Pts',(44.3399289797364,258.138867997726,21.4008040882511)) ;
#105104 = CARTESIAN_POINT('Ctrl Pts',(44.3376178581132,258.119527473902,21.3977698112471)) ;
#105105 = CARTESIAN_POINT('Ctrl Pts',(44.3376178581134,258.1,21.397769811247)) ;
#105106 = CARTESIAN_POINT('Origin',(44.6495934690622,258.1,21.788501455951)) ;
#105107 = CARTESIAN_POINT('Origin',(44.6495934690622,258.1,21.788501455951)) ;
#105108 = CARTESIAN_POINT('Origin',(36.9671811123914,258.1,20.5717268744974)) ;
#105109 = CARTESIAN_POINT('Origin',(40.2,258.1,25.0213203435596)) ;
#105110 = CARTESIAN_POINT('',(44.8727213369894,258.1,22.9778734255204)) ;
#105111 = CARTESIAN_POINT('Origin',(40.2,258.1,25.0213203435596)) ;
#105112 = CARTESIAN_POINT('Ctrl Pts',(44.7879854513112,258.25,23.1631251173908)) ;
#105113 = CARTESIAN_POINT('Ctrl Pts',(44.788318480923,258.25,23.162410141506)) ;
#105114 = CARTESIAN_POINT('Ctrl Pts',(44.7886514546598,258.249996669894,23.1616951333976)) ;
#105115 = CARTESIAN_POINT('Ctrl Pts',(44.7975633610212,258.249818328848,23.1425541606572)) ;
#105116 = CARTESIAN_POINT('Ctrl Pts',(44.8061352328939,258.247433157512,23.1240401659929)) ;
#105117 = CARTESIAN_POINT('Ctrl Pts',(44.8223176686178,258.238259809032,23.0889045613858)) ;
#105118 = CARTESIAN_POINT('Ctrl Pts',(44.8300252912377,258.231622782802,23.0720801216756)) ;
#105119 = CARTESIAN_POINT('Ctrl Pts',(44.845101564091,258.21278678422,23.0390258353215)) ;
#105120 = CARTESIAN_POINT('Ctrl Pts',(44.8524083722489,258.199976451841,23.0229135555138)) ;
#105121 = CARTESIAN_POINT('Ctrl Pts',(44.8629908725676,258.171958342729,22.9994999229698)) ;
#105122 = CARTESIAN_POINT('Ctrl Pts',(44.8667635305755,258.158041775475,22.9911225509982)) ;
#105123 = CARTESIAN_POINT('Ctrl Pts',(44.8715314574991,258.129045309865,22.9805240155764)) ;
#105124 = CARTESIAN_POINT('Ctrl Pts',(44.8727213369894,258.114679223254,22.9778734255204)) ;
#105125 = CARTESIAN_POINT('Ctrl Pts',(44.8727213369894,258.1,22.9778734255204)) ;
#105126 = CARTESIAN_POINT('Origin',(42.3621477910643,258.1,23.9513275530686)) ;
#105127 = CARTESIAN_POINT('',(45.2548471203588,258.1,22.8537132320653)) ;
#105128 = CARTESIAN_POINT('',(42.315795241908,258.1,23.8086690756243)) ;
#105129 = CARTESIAN_POINT('Ctrl Pts',(45.3047322539521,258.25,22.9952239032473)) ;
#105130 = CARTESIAN_POINT('Ctrl Pts',(45.3042439751341,258.25,22.9938493930806)) ;
#105131 = CARTESIAN_POINT('Ctrl Pts',(45.3037558389596,258.249978738764,22.9924749143347)) ;
#105132 = CARTESIAN_POINT('Ctrl Pts',(45.3032679987775,258.249936222763,22.9911009060563)) ;
#105133 = CARTESIAN_POINT('Ctrl Pts',(45.2970008540754,258.249390031724,22.9734494107125)) ;
#105134 = CARTESIAN_POINT('Ctrl Pts',(45.2908421594689,258.245341162533,22.9560424309124)) ;
#105135 = CARTESIAN_POINT('Ctrl Pts',(45.2851039978952,258.237998568188,22.9397848739232)) ;
#105136 = CARTESIAN_POINT('Ctrl Pts',(45.2791219714012,258.230343922473,22.9228363904432)) ;
#105137 = CARTESIAN_POINT('Ctrl Pts',(45.2737086176589,258.21925289602,22.9074544440317)) ;
#105138 = CARTESIAN_POINT('Ctrl Pts',(45.2691590847773,258.205348530944,22.8945085756089)) ;
#105139 = CARTESIAN_POINT('Ctrl Pts',(45.2646107691597,258.191447886093,22.8815661709572)) ;
#105140 = CARTESIAN_POINT('Ctrl Pts',(45.2610125833727,258.175001311387,22.8713062373364)) ;
#105141 = CARTESIAN_POINT('Ctrl Pts',(45.2585598828031,258.156933541317,22.8643092759727)) ;
#105142 = CARTESIAN_POINT('Ctrl Pts',(45.2561074844783,258.138867997726,22.85731317684)) ;
#105143 = CARTESIAN_POINT('Ctrl Pts',(45.2548471203588,258.119527473902,22.8537132320654)) ;
#105144 = CARTESIAN_POINT('Ctrl Pts',(45.254847120359,258.1,22.8537132320653)) ;
#105145 = CARTESIAN_POINT('Origin',(45.4308108396234,258.1,23.3217268744974)) ;
#105146 = CARTESIAN_POINT('Origin',(45.4308108396234,258.1,23.3217268744974)) ;
#105147 = CARTESIAN_POINT('Origin',(35.7504065309378,258.1,21.788501455951)) ;
#105148 = CARTESIAN_POINT('Origin',(40.2,258.1,25.0213203435596)) ;
#105149 = CARTESIAN_POINT('',(45.2754819011524,258.1,24.5218371395634)) ;
#105150 = CARTESIAN_POINT('Origin',(40.2,258.1,25.0213203435596)) ;
#105151 = CARTESIAN_POINT('Ctrl Pts',(45.1376473638895,258.25,24.6718371395634)) ;
#105152 = CARTESIAN_POINT('Ctrl Pts',(45.1381850335709,258.25,24.6712600688988)) ;
#105153 = CARTESIAN_POINT('Ctrl Pts',(45.1387226600695,258.249996669894,24.6706829503216)) ;
#105154 = CARTESIAN_POINT('Ctrl Pts',(45.1531132725535,258.249818328848,24.655232733985)) ;
#105155 = CARTESIAN_POINT('Ctrl Pts',(45.1669867461395,258.247433157512,24.6402737328004)) ;
#105156 = CARTESIAN_POINT('Ctrl Pts',(45.1932346560154,258.238259809032,24.611858434734)) ;
#105157 = CARTESIAN_POINT('Ctrl Pts',(45.2057640785244,258.231622782802,24.5982392280904)) ;
#105158 = CARTESIAN_POINT('Ctrl Pts',(45.2303168022832,258.21278678422,24.5714615581854)) ;
#105159 = CARTESIAN_POINT('Ctrl Pts',(45.2422449580739,258.199976451841,24.5583957973774)) ;
#105160 = CARTESIAN_POINT('Ctrl Pts',(45.2595447243168,258.171958342729,24.5393982820176)) ;
#105161 = CARTESIAN_POINT('Ctrl Pts',(45.2657214856064,258.158041775475,24.5325967432531)) ;
#105162 = CARTESIAN_POINT('Ctrl Pts',(45.2735311811371,258.129045309865,24.5239903075244)) ;
#105163 = CARTESIAN_POINT('Ctrl Pts',(45.2754819011524,258.114679223254,24.5218371395634)) ;
#105164 = CARTESIAN_POINT('Ctrl Pts',(45.2754819011524,258.1,24.5218371395634)) ;
#105165 = CARTESIAN_POINT('Origin',(42.5869707020053,258.1,24.6718371395634)) ;
#105166 = CARTESIAN_POINT('',(45.6772727272728,258.1,24.5218371395634)) ;
#105167 = CARTESIAN_POINT('',(42.5869707020053,258.1,24.5218371395634)) ;
#105168 = CARTESIAN_POINT('Ctrl Pts',(45.6809871063617,258.25,24.6718371395634)) ;
#105169 = CARTESIAN_POINT('Ctrl Pts',(45.6809474726105,258.25,24.6703790162596)) ;
#105170 = CARTESIAN_POINT('Ctrl Pts',(45.6809079648117,258.249978738764,24.6689209669186)) ;
#105171 = CARTESIAN_POINT('Ctrl Pts',(45.6808685931366,258.249936222763,24.667463456485)) ;
#105172 = CARTESIAN_POINT('Ctrl Pts',(45.6803627963739,258.249390031724,24.6487392325953)) ;
#105173 = CARTESIAN_POINT('Ctrl Pts',(45.6798845823058,258.245341162533,24.6302810697322)) ;
#105174 = CARTESIAN_POINT('Ctrl Pts',(45.6794511277471,258.237998568189,24.6130460247761)) ;
#105175 = CARTESIAN_POINT('Ctrl Pts',(45.6789992518944,258.230343922473,24.5950785112736)) ;
#105176 = CARTESIAN_POINT('Ctrl Pts',(45.678604129391,258.21925289602,24.5787765926027)) ;
#105177 = CARTESIAN_POINT('Ctrl Pts',(45.6782777598474,258.205348530944,24.5650584571032)) ;
#105178 = CARTESIAN_POINT('Ctrl Pts',(45.6779514776265,258.191447886093,24.5513439920011)) ;
#105179 = CARTESIAN_POINT('Ctrl Pts',(45.6776998934372,258.175001311387,24.5404743147172)) ;
#105180 = CARTESIAN_POINT('Ctrl Pts',(45.6775294165482,258.156933541317,24.5330618828598)) ;
#105181 = CARTESIAN_POINT('Ctrl Pts',(45.6773589606669,258.138867997726,24.5256503644317)) ;
#105182 = CARTESIAN_POINT('Ctrl Pts',(45.6772727272727,258.119527473902,24.5218371395634)) ;
#105183 = CARTESIAN_POINT('Ctrl Pts',(45.6772727272727,258.1,24.5218371395634)) ;
#105184 = CARTESIAN_POINT('Origin',(45.7,258.1,25.0213203435596)) ;
#105185 = CARTESIAN_POINT('Origin',(45.7,258.1,25.0213203435596)) ;
#105186 = CARTESIAN_POINT('Origin',(34.9691891603767,258.1,23.3217268744974)) ;
#105187 = CARTESIAN_POINT('Origin',(40.2,258.1,25.0213203435596)) ;
#105188 = CARTESIAN_POINT('',(45.1814189338688,258.1,26.1146937497175)) ;
#105189 = CARTESIAN_POINT('Origin',(40.2,258.1,25.0213203435596)) ;
#105190 = CARTESIAN_POINT('Ctrl Pts',(45.0039779498781,258.25,26.2147590127358)) ;
#105191 = CARTESIAN_POINT('Ctrl Pts',(45.0046676287764,258.25,26.2143763349877)) ;
#105192 = CARTESIAN_POINT('Ctrl Pts',(45.0053572814057,258.249996669895,26.213993598331)) ;
#105193 = CARTESIAN_POINT('Ctrl Pts',(45.0238179465998,258.249818328848,26.2037465132206)) ;
#105194 = CARTESIAN_POINT('Ctrl Pts',(45.0416349896415,258.247433157512,26.1938067967769)) ;
#105195 = CARTESIAN_POINT('Ctrl Pts',(45.0753790453709,258.238259809032,26.1748932926068)) ;
#105196 = CARTESIAN_POINT('Ctrl Pts',(45.0915038005962,258.231622782802,26.1658124618668)) ;
#105197 = CARTESIAN_POINT('Ctrl Pts',(45.1231295835901,258.21278678422,26.1479325933121)) ;
#105198 = CARTESIAN_POINT('Ctrl Pts',(45.1385114760162,258.199976451841,26.1391923192062)) ;
#105199 = CARTESIAN_POINT('Ctrl Pts',(45.1608350865289,258.171958342729,26.1264705301978)) ;
#105200 = CARTESIAN_POINT('Ctrl Pts',(45.1688113266691,258.158041775475,26.1219106066435)) ;
#105201 = CARTESIAN_POINT('Ctrl Pts',(45.1788983233951,258.129045309865,26.1161387285016)) ;
#105202 = CARTESIAN_POINT('Ctrl Pts',(45.1814189338688,258.114679223254,26.1146937497175)) ;
#105203 = CARTESIAN_POINT('Ctrl Pts',(45.1814189338688,258.1,26.1146937497175)) ;
#105204 = CARTESIAN_POINT('Origin',(42.5781402896312,258.1,25.426556577058)) ;
#105205 = CARTESIAN_POINT('',(45.5635447172382,258.1,26.2388539431727)) ;
#105206 = CARTESIAN_POINT('',(42.6244928387874,258.1,25.2838980996137)) ;
#105207 = CARTESIAN_POINT('Ctrl Pts',(45.5207247525189,258.25,26.3826602268791)) ;
#105208 = CARTESIAN_POINT('Ctrl Pts',(45.5211376434625,258.25,26.3812612217063)) ;
#105209 = CARTESIAN_POINT('Ctrl Pts',(45.5215506313345,258.249978738764,26.3798623257983)) ;
#105210 = CARTESIAN_POINT('Ctrl Pts',(45.5219635821412,258.249936222763,26.3784639844859)) ;
#105211 = CARTESIAN_POINT('Ctrl Pts',(45.527268644238,258.249390031724,26.3604998895502)) ;
#105212 = CARTESIAN_POINT('Ctrl Pts',(45.5325177216272,258.245341162533,26.3427973572038)) ;
#105213 = CARTESIAN_POINT('Ctrl Pts',(45.5374314036352,258.237998568189,26.3262719105652)) ;
#105214 = CARTESIAN_POINT('Ctrl Pts',(45.5425539111803,258.230343922473,26.3090441524495)) ;
#105215 = CARTESIAN_POINT('Ctrl Pts',(45.5472156972587,258.21925289602,26.2934180069008)) ;
#105216 = CARTESIAN_POINT('Ctrl Pts',(45.551144438378,258.205348530944,26.2802704310072)) ;
#105217 = CARTESIAN_POINT('Ctrl Pts',(45.5550721283311,258.191447886093,26.2671263728531)) ;
#105218 = CARTESIAN_POINT('Ctrl Pts',(45.5581917725533,258.175001311387,26.2567109516524)) ;
#105219 = CARTESIAN_POINT('Ctrl Pts',(45.5603202068105,258.156933541317,26.249608629777)) ;
#105220 = CARTESIAN_POINT('Ctrl Pts',(45.5624483787821,258.138867997726,26.2425071831161)) ;
#105221 = CARTESIAN_POINT('Ctrl Pts',(45.5635447172386,258.119527473902,26.2388539431728)) ;
#105222 = CARTESIAN_POINT('Ctrl Pts',(45.5635447172384,258.1,26.2388539431728)) ;
#105223 = CARTESIAN_POINT('Origin',(45.4308108396234,258.1,26.7209138126218)) ;
#105224 = CARTESIAN_POINT('Origin',(45.4308108396234,258.1,26.7209138126218)) ;
#105225 = CARTESIAN_POINT('Origin',(34.7,258.1,25.0213203435596)) ;
#105226 = CARTESIAN_POINT('Origin',(40.2,258.1,25.0213203435596)) ;
#105227 = CARTESIAN_POINT('',(44.5997399737516,258.1,27.6005233528965)) ;
#105228 = CARTESIAN_POINT('Origin',(40.2,258.1,25.0213203435596)) ;
#105229 = CARTESIAN_POINT('Ctrl Pts',(44.4000617028502,258.25,27.6408587937931)) ;
#105230 = CARTESIAN_POINT('Ctrl Pts',(44.400835880388,258.25,27.6407079681274)) ;
#105231 = CARTESIAN_POINT('Ctrl Pts',(44.4016100511464,258.249996669895,27.6405570783186)) ;
#105232 = CARTESIAN_POINT('Ctrl Pts',(44.4223337105158,258.249818328848,27.6365161805241)) ;
#105233 = CARTESIAN_POINT('Ctrl Pts',(44.4423502667025,258.247433157512,27.6325687175193)) ;
#105234 = CARTESIAN_POINT('Ctrl Pts',(44.4802873650018,258.238259809032,27.6250083928119)) ;
#105235 = CARTESIAN_POINT('Ctrl Pts',(44.4984290495543,258.231622782802,27.621354832958)) ;
#105236 = CARTESIAN_POINT('Ctrl Pts',(44.5340321397943,258.21278678422,27.6141229718641)) ;
#105237 = CARTESIAN_POINT('Ctrl Pts',(44.5513620820533,258.199976451841,27.6105637433868)) ;
#105238 = CARTESIAN_POINT('Ctrl Pts',(44.5765243463011,258.171958342729,27.6053629780756)) ;
#105239 = CARTESIAN_POINT('Ctrl Pts',(44.5855192953333,258.158041775475,27.6034910268201)) ;
#105240 = CARTESIAN_POINT('Ctrl Pts',(44.5968962077348,258.129045309865,27.6011186979124)) ;
#105241 = CARTESIAN_POINT('Ctrl Pts',(44.5997399737516,258.114679223254,27.6005233528965)) ;
#105242 = CARTESIAN_POINT('Ctrl Pts',(44.5997399737516,258.1,27.6005233528965)) ;
#105243 = CARTESIAN_POINT('Origin',(42.3365209362303,258.1,26.1416086685709)) ;
#105244 = CARTESIAN_POINT('',(44.9247955802669,258.1,27.8366900749965)) ;
#105245 = CARTESIAN_POINT('',(42.4246887240742,258.1,26.0202561194147)) ;
#105246 = CARTESIAN_POINT('Ctrl Pts',(44.8396327882299,258.25,27.9602258814029)) ;
#105247 = CARTESIAN_POINT('Ctrl Pts',(44.8404577872258,258.25,27.9590229387355)) ;
#105248 = CARTESIAN_POINT('Ctrl Pts',(44.8412828446427,258.249978738764,27.9578201299378)) ;
#105249 = CARTESIAN_POINT('Ctrl Pts',(44.8421076954273,258.249936222763,27.9566178371377)) ;
#105250 = CARTESIAN_POINT('Ctrl Pts',(44.8527043199227,258.249390031724,27.9411723219305)) ;
#105251 = CARTESIAN_POINT('Ctrl Pts',(44.8631668725218,258.245341162533,27.9259582673091)) ;
#105252 = CARTESIAN_POINT('Ctrl Pts',(44.8729467056653,258.237998568189,27.911760044844)) ;
#105253 = CARTESIAN_POINT('Ctrl Pts',(44.8831421698783,258.230343922473,27.8969584151118)) ;
#105254 = CARTESIAN_POINT('Ctrl Pts',(44.8924045364365,258.21925289602,27.8835376386854)) ;
#105255 = CARTESIAN_POINT('Ctrl Pts',(44.9002038156649,258.205348530944,27.8722475987307)) ;
#105256 = CARTESIAN_POINT('Ctrl Pts',(44.9080010081334,258.191447886093,27.8609605795169)) ;
#105257 = CARTESIAN_POINT('Ctrl Pts',(44.9141865082541,258.175001311387,27.8520189483951)) ;
#105258 = CARTESIAN_POINT('Ctrl Pts',(44.918405507683,258.156933541317,27.8459219612516)) ;
#105259 = CARTESIAN_POINT('Ctrl Pts',(44.9226239872073,258.138867997726,27.8398257254358)) ;
#105260 = CARTESIAN_POINT('Ctrl Pts',(44.9247955802671,258.119527473902,27.8366900749966)) ;
#105261 = CARTESIAN_POINT('Ctrl Pts',(44.924795580267,258.1,27.8366900749965)) ;
#105262 = CARTESIAN_POINT('Origin',(44.6495934690622,258.1,28.2541392311682)) ;
#105263 = CARTESIAN_POINT('Origin',(44.6495934690622,258.1,28.2541392311682)) ;
#105264 = CARTESIAN_POINT('Origin',(34.9691891603767,258.1,26.7209138126218)) ;
#105265 = CARTESIAN_POINT('Origin',(40.2,258.1,25.0213203435596)) ;
#105266 = CARTESIAN_POINT('',(43.5873838102126,258.1,28.8338825951576)) ;
#105267 = CARTESIAN_POINT('Origin',(40.2,258.1,25.0213203435596)) ;
#105268 = CARTESIAN_POINT('Ctrl Pts',(43.3850141527966,258.25,28.8105398999439)) ;
#105269 = CARTESIAN_POINT('Ctrl Pts',(43.3857970470841,258.25,28.8106356902278)) ;
#105270 = CARTESIAN_POINT('Ctrl Pts',(43.3865799547451,258.249996669895,28.810731417413)) ;
#105271 = CARTESIAN_POINT('Ctrl Pts',(43.4075380321218,258.249818328848,28.8132922581646)) ;
#105272 = CARTESIAN_POINT('Ctrl Pts',(43.4277947414691,258.247433157512,28.8157234537816)) ;
#105273 = CARTESIAN_POINT('Ctrl Pts',(43.4662113348325,258.238259809031,28.8202563657949)) ;
#105274 = CARTESIAN_POINT('Ctrl Pts',(43.4845941142266,258.231622782802,28.8223877127214)) ;
#105275 = CARTESIAN_POINT('Ctrl Pts',(43.5206894331777,258.21278678422,28.8265117640394)) ;
#105276 = CARTESIAN_POINT('Ctrl Pts',(43.5382710497767,258.199976451841,28.8284819832727)) ;
#105277 = CARTESIAN_POINT('Ctrl Pts',(43.5638089100193,258.171958342729,28.8313113288033)) ;
#105278 = CARTESIAN_POINT('Ctrl Pts',(43.5729420796607,258.158041775475,28.832310589478)) ;
#105279 = CARTESIAN_POINT('Ctrl Pts',(43.584495256284,258.129045309865,28.8335700298871)) ;
#105280 = CARTESIAN_POINT('Ctrl Pts',(43.5873838102126,258.114679223254,28.8338825951576)) ;
#105281 = CARTESIAN_POINT('Ctrl Pts',(43.5873838102126,258.1,28.8338825951576)) ;
#105282 = CARTESIAN_POINT('Origin',(41.8857640275745,258.1,26.746999133324)) ;
#105283 = CARTESIAN_POINT('',(43.8235505323126,258.1,29.1589382016729)) ;
#105284 = CARTESIAN_POINT('',(42.0071165767308,258.1,26.6588313454802)) ;
#105285 = CARTESIAN_POINT('Ctrl Pts',(43.7043812404062,258.25,29.2501109853232)) ;
#105286 = CARTESIAN_POINT('Ctrl Pts',(43.7055375908047,258.25,29.2492218575707)) ;
#105287 = CARTESIAN_POINT('Ctrl Pts',(43.7066939553966,258.249978738764,29.2483328751888)) ;
#105288 = CARTESIAN_POINT('Ctrl Pts',(43.7078499640179,258.249936222763,29.2474443196972)) ;
#105289 = CARTESIAN_POINT('Ctrl Pts',(43.7227008794821,258.249390031724,29.2360292988668)) ;
#105290 = CARTESIAN_POINT('Ctrl Pts',(43.737352759739,258.245341162533,29.2247929796352)) ;
#105291 = CARTESIAN_POINT('Ctrl Pts',(43.75104142581,258.237998568188,29.2143118022834)) ;
#105292 = CARTESIAN_POINT('Ctrl Pts',(43.7653118436182,258.230343922473,29.2033851875822)) ;
#105293 = CARTESIAN_POINT('Ctrl Pts',(43.7782681256832,258.21925289602,29.1934834993828)) ;
#105294 = CARTESIAN_POINT('Ctrl Pts',(43.7891744952288,258.205348530944,29.18515614314)) ;
#105295 = CARTESIAN_POINT('Ctrl Pts',(43.8000779466878,258.191447886093,29.1768310149483)) ;
#105296 = CARTESIAN_POINT('Ctrl Pts',(43.808723822858,258.175001311387,29.1702384430595)) ;
#105297 = CARTESIAN_POINT('Ctrl Pts',(43.8146204023989,258.156933541317,29.1657436062296)) ;
#105298 = CARTESIAN_POINT('Ctrl Pts',(43.8205162553081,258.138867997726,29.1612493232955)) ;
#105299 = CARTESIAN_POINT('Ctrl Pts',(43.8235505323127,258.119527473902,29.1589382016731)) ;
#105300 = CARTESIAN_POINT('Ctrl Pts',(43.8235505323126,258.1,29.1589382016729)) ;
#105301 = CARTESIAN_POINT('Origin',(43.4328188876086,258.1,29.4709138126218)) ;
#105302 = CARTESIAN_POINT('Origin',(43.4328188876086,258.1,29.4709138126218)) ;
#105303 = CARTESIAN_POINT('Origin',(35.7504065309378,258.1,28.2541392311682)) ;
#105304 = CARTESIAN_POINT('Origin',(40.2,258.1,25.0213203435596)) ;
#105305 = CARTESIAN_POINT('',(42.2434469180392,258.1,29.694041680549)) ;
#105306 = CARTESIAN_POINT('Origin',(40.2,258.1,25.0213203435596)) ;
#105307 = CARTESIAN_POINT('Ctrl Pts',(42.0581952261689,258.25,29.6093057948708)) ;
#105308 = CARTESIAN_POINT('Ctrl Pts',(42.0589102020537,258.25,29.6096388244826)) ;
#105309 = CARTESIAN_POINT('Ctrl Pts',(42.059625210162,258.249996669894,29.6099717982194)) ;
#105310 = CARTESIAN_POINT('Ctrl Pts',(42.0787661829036,258.249818328848,29.6188837045809)) ;
#105311 = CARTESIAN_POINT('Ctrl Pts',(42.0972801775669,258.247433157512,29.6274555764535)) ;
#105312 = CARTESIAN_POINT('Ctrl Pts',(42.1324157821741,258.238259809032,29.6436380121775)) ;
#105313 = CARTESIAN_POINT('Ctrl Pts',(42.1492402218842,258.231622782802,29.6513456347974)) ;
#105314 = CARTESIAN_POINT('Ctrl Pts',(42.1822945082383,258.21278678422,29.6664219076506)) ;
#105315 = CARTESIAN_POINT('Ctrl Pts',(42.1984067880459,258.199976451841,29.6737287158086)) ;
#105316 = CARTESIAN_POINT('Ctrl Pts',(42.2218204205899,258.171958342729,29.6843112161272)) ;
#105317 = CARTESIAN_POINT('Ctrl Pts',(42.2301977925615,258.158041775475,29.6880838741351)) ;
#105318 = CARTESIAN_POINT('Ctrl Pts',(42.2407963279833,258.129045309865,29.6928518010587)) ;
#105319 = CARTESIAN_POINT('Ctrl Pts',(42.2434469180392,258.114679223254,29.694041680549)) ;
#105320 = CARTESIAN_POINT('Ctrl Pts',(42.2434469180392,258.1,29.694041680549)) ;
#105321 = CARTESIAN_POINT('Origin',(41.2699927904911,258.1,27.1834681346239)) ;
#105322 = CARTESIAN_POINT('',(42.3676071114944,258.1,30.0761674639184)) ;
#105323 = CARTESIAN_POINT('',(41.4126512679354,258.1,27.1371155854676)) ;
#105324 = CARTESIAN_POINT('Ctrl Pts',(42.2260964403121,258.25,30.1260525975113)) ;
#105325 = CARTESIAN_POINT('Ctrl Pts',(42.2274709504791,258.25,30.1255643186932)) ;
#105326 = CARTESIAN_POINT('Ctrl Pts',(42.2288454292248,258.249978738764,30.1250761825189)) ;
#105327 = CARTESIAN_POINT('Ctrl Pts',(42.2302194375035,258.249936222763,30.1245883423371)) ;
#105328 = CARTESIAN_POINT('Ctrl Pts',(42.24787093285,258.249390031724,30.1183211976397)) ;
#105329 = CARTESIAN_POINT('Ctrl Pts',(42.2652779126467,258.245341162533,30.112162503026)) ;
#105330 = CARTESIAN_POINT('Ctrl Pts',(42.2815354696359,258.237998568188,30.1064243414531)) ;
#105331 = CARTESIAN_POINT('Ctrl Pts',(42.298483953116,258.230343922473,30.1004423149599)) ;
#105332 = CARTESIAN_POINT('Ctrl Pts',(42.3138658995278,258.21925289602,30.095028961218)) ;
#105333 = CARTESIAN_POINT('Ctrl Pts',(42.3268117679506,258.205348530944,30.0904794283365)) ;
#105334 = CARTESIAN_POINT('Ctrl Pts',(42.3397541726023,258.191447886093,30.085931112719)) ;
#105335 = CARTESIAN_POINT('Ctrl Pts',(42.3500141062232,258.175001311387,30.0823329269323)) ;
#105336 = CARTESIAN_POINT('Ctrl Pts',(42.3570110675869,258.156933541317,30.0798802263626)) ;
#105337 = CARTESIAN_POINT('Ctrl Pts',(42.3640071667196,258.138867997726,30.0774278280376)) ;
#105338 = CARTESIAN_POINT('Ctrl Pts',(42.3676071114944,258.119527473902,30.0761674639185)) ;
#105339 = CARTESIAN_POINT('Ctrl Pts',(42.3676071114944,258.1,30.0761674639186)) ;
#105340 = CARTESIAN_POINT('Origin',(41.8995934690622,258.1,30.252131183183)) ;
#105341 = CARTESIAN_POINT('Origin',(41.8995934690622,258.1,30.252131183183)) ;
#105342 = CARTESIAN_POINT('Origin',(36.9671811123914,258.1,29.4709138126218)) ;
#105343 = CARTESIAN_POINT('Origin',(40.2,258.1,25.0213203435596)) ;
#105344 = CARTESIAN_POINT('',(40.6994832039963,258.1,30.096802244712)) ;
#105345 = CARTESIAN_POINT('Origin',(40.2,258.1,25.0213203435596)) ;
#105346 = CARTESIAN_POINT('Ctrl Pts',(40.5494832039963,258.25,29.9589677074491)) ;
#105347 = CARTESIAN_POINT('Ctrl Pts',(40.5500602746609,258.25,29.9595053771305)) ;
#105348 = CARTESIAN_POINT('Ctrl Pts',(40.5506373932381,258.249996669894,29.9600430036291)) ;
#105349 = CARTESIAN_POINT('Ctrl Pts',(40.5660876095745,258.249818328848,29.974433616113)) ;
#105350 = CARTESIAN_POINT('Ctrl Pts',(40.5810466107592,258.247433157512,29.9883070896991)) ;
#105351 = CARTESIAN_POINT('Ctrl Pts',(40.6094619088257,258.238259809032,30.014554999575)) ;
#105352 = CARTESIAN_POINT('Ctrl Pts',(40.6230811154693,258.231622782802,30.027084422084)) ;
#105353 = CARTESIAN_POINT('Ctrl Pts',(40.6498587853742,258.21278678422,30.0516371458428)) ;
#105354 = CARTESIAN_POINT('Ctrl Pts',(40.6629245461822,258.199976451841,30.0635653016335)) ;
#105355 = CARTESIAN_POINT('Ctrl Pts',(40.681922061542,258.171958342729,30.0808650678764)) ;
#105356 = CARTESIAN_POINT('Ctrl Pts',(40.6887236003065,258.158041775475,30.087041829166)) ;
#105357 = CARTESIAN_POINT('Ctrl Pts',(40.6973300360353,258.129045309865,30.0948515246968)) ;
#105358 = CARTESIAN_POINT('Ctrl Pts',(40.6994832039963,258.114679223254,30.096802244712)) ;
#105359 = CARTESIAN_POINT('Ctrl Pts',(40.6994832039963,258.1,30.096802244712)) ;
#105360 = CARTESIAN_POINT('Origin',(40.5494832039963,258.1,27.4082910455649)) ;
#105361 = CARTESIAN_POINT('',(40.6994832039963,258.1,30.4985930708324)) ;
#105362 = CARTESIAN_POINT('',(40.6994832039963,258.1,27.4082910455649)) ;
#105363 = CARTESIAN_POINT('Ctrl Pts',(40.5494832039963,258.25,30.5023074499214)) ;
#105364 = CARTESIAN_POINT('Ctrl Pts',(40.5509413273001,258.25,30.5022678161702)) ;
#105365 = CARTESIAN_POINT('Ctrl Pts',(40.5523993766411,258.249978738764,30.5022283083715)) ;
#105366 = CARTESIAN_POINT('Ctrl Pts',(40.5538568870747,258.249936222763,30.5021889366964)) ;
#105367 = CARTESIAN_POINT('Ctrl Pts',(40.5725811109644,258.249390031724,30.501683139933)) ;
#105368 = CARTESIAN_POINT('Ctrl Pts',(40.5910392738276,258.245341162533,30.5012049258673)) ;
#105369 = CARTESIAN_POINT('Ctrl Pts',(40.6082743187837,258.237998568188,30.5007714713081)) ;
#105370 = CARTESIAN_POINT('Ctrl Pts',(40.6262418322861,258.230343922473,30.5003195954549)) ;
#105371 = CARTESIAN_POINT('Ctrl Pts',(40.642543750957,258.21925289602,30.4999244729506)) ;
#105372 = CARTESIAN_POINT('Ctrl Pts',(40.6562618864565,258.205348530944,30.499598103407)) ;
#105373 = CARTESIAN_POINT('Ctrl Pts',(40.6699763515586,258.191447886093,30.4992718211862)) ;
#105374 = CARTESIAN_POINT('Ctrl Pts',(40.6808460288425,258.175001311387,30.4990202369969)) ;
#105375 = CARTESIAN_POINT('Ctrl Pts',(40.6882584606999,258.156933541317,30.4988497601079)) ;
#105376 = CARTESIAN_POINT('Ctrl Pts',(40.695669979128,258.138867997726,30.4986793042266)) ;
#105377 = CARTESIAN_POINT('Ctrl Pts',(40.6994832039963,258.119527473902,30.4985930708323)) ;
#105378 = CARTESIAN_POINT('Ctrl Pts',(40.6994832039963,258.1,30.4985930708323)) ;
#105379 = CARTESIAN_POINT('Origin',(40.2,258.1,30.5213203435596)) ;
#105380 = CARTESIAN_POINT('Origin',(40.2,258.1,30.5213203435596)) ;
#105381 = CARTESIAN_POINT('Origin',(38.5004065309378,258.1,30.252131183183)) ;
#105382 = CARTESIAN_POINT('Origin',(38.5004065309378,258.1,30.252131183183)) ;
#105383 = CARTESIAN_POINT('Origin',(40.2,258.25,25.0213203435596)) ;
#105384 = CARTESIAN_POINT('',(39.7005167960037,258.25,30.096802244712)) ;
#105385 = CARTESIAN_POINT('',(39.1066265938421,258.25,30.0027392774284)) ;
#105386 = CARTESIAN_POINT('Origin',(39.1998077319512,258.25,29.7159572226947)) ;
#105387 = CARTESIAN_POINT('',(38.982466400387,258.25,30.3848650607978)) ;
#105388 = CARTESIAN_POINT('Origin',(38.5004065309378,258.25,30.252131183183)) ;
#105389 = CARTESIAN_POINT('',(38.0323928885057,258.25,30.0761674639184)) ;
#105390 = CARTESIAN_POINT('Origin',(38.0323928885057,258.25,30.0761674639184)) ;
#105391 = CARTESIAN_POINT('Origin',(42.601961952148,258.25,20.8655317564881)) ;
#105392 = CARTESIAN_POINT('',(42.7792030093369,258.25,20.6215803698081)) ;
#105393 = CARTESIAN_POINT('',(43.0153697314369,258.25,20.2965247632928)) ;
#105394 = CARTESIAN_POINT('Origin',(43.8235505323125,258.25,20.8837024854464)) ;
#105395 = CARTESIAN_POINT('',(43.8235505323125,258.25,20.8837024854464)) ;
#105396 = CARTESIAN_POINT('',(43.5873838102126,258.25,21.2087580919617)) ;
#105397 = CARTESIAN_POINT('Origin',(43.4328188876086,258.25,20.5717268744974)) ;
#105398 = CARTESIAN_POINT('Origin',(43.7686108649179,258.25,21.811177590536)) ;
#105399 = CARTESIAN_POINT('',(44.012562251598,258.25,21.6339365333471)) ;
#105400 = CARTESIAN_POINT('',(44.3376178581133,258.25,21.3977698112471)) ;
#105401 = CARTESIAN_POINT('Origin',(44.9247955802669,258.25,22.2059506121228)) ;
#105402 = CARTESIAN_POINT('',(44.9247955802669,258.25,22.2059506121228)) ;
#105403 = CARTESIAN_POINT('',(44.5997399737516,258.25,22.4421173342227)) ;
#105404 = CARTESIAN_POINT('Origin',(44.6495934690622,258.25,21.788501455951)) ;
#105405 = CARTESIAN_POINT('Origin',(44.5859392822557,258.25,23.0710545636296)) ;
#105406 = CARTESIAN_POINT('',(44.8727213369894,258.25,22.9778734255204)) ;
#105407 = CARTESIAN_POINT('',(45.2548471203588,258.25,22.8537132320653)) ;
#105408 = CARTESIAN_POINT('Origin',(45.5635447172382,258.25,23.8037867439466)) ;
#105409 = CARTESIAN_POINT('',(45.5635447172382,258.25,23.8037867439466)) ;
#105410 = CARTESIAN_POINT('',(45.1814189338688,258.25,23.9279469374017)) ;
#105411 = CARTESIAN_POINT('Origin',(45.4308108396234,258.25,23.3217268744974)) ;
#105412 = CARTESIAN_POINT('Origin',(44.9739414040105,258.25,24.5218371395634)) ;
#105413 = CARTESIAN_POINT('',(45.2754819011524,258.25,24.5218371395634)) ;
#105414 = CARTESIAN_POINT('',(45.6772727272728,258.25,24.5218371395634)) ;
#105415 = CARTESIAN_POINT('Origin',(45.6772727272728,258.25,25.5208035475559)) ;
#105416 = CARTESIAN_POINT('',(45.6772727272728,258.25,25.5208035475559)) ;
#105417 = CARTESIAN_POINT('',(45.2754819011524,258.25,25.5208035475559)) ;
#105418 = CARTESIAN_POINT('Origin',(45.7,258.25,25.0213203435596)) ;
#105419 = CARTESIAN_POINT('Origin',(44.8946368791351,258.25,26.0215126116084)) ;
#105420 = CARTESIAN_POINT('',(45.1814189338688,258.25,26.1146937497175)) ;
#105421 = CARTESIAN_POINT('',(45.5635447172382,258.25,26.2388539431727)) ;
#105422 = CARTESIAN_POINT('Origin',(45.2548471203588,258.25,27.188927455054)) ;
#105423 = CARTESIAN_POINT('',(45.2548471203588,258.25,27.188927455054)) ;
#105424 = CARTESIAN_POINT('',(44.8727213369894,258.25,27.0647672615988)) ;
#105425 = CARTESIAN_POINT('Origin',(45.4308108396234,258.25,26.7209138126218)) ;
#105426 = CARTESIAN_POINT('Origin',(44.3557885870715,258.25,27.4232822957076)) ;
#105427 = CARTESIAN_POINT('',(44.5997399737516,258.25,27.6005233528965)) ;
#105428 = CARTESIAN_POINT('',(44.9247955802669,258.25,27.8366900749965)) ;
#105429 = CARTESIAN_POINT('Origin',(44.3376178581133,258.25,28.6448708758722)) ;
#105430 = CARTESIAN_POINT('',(44.3376178581133,258.25,28.6448708758722)) ;
#105431 = CARTESIAN_POINT('',(44.012562251598,258.25,28.4087041537722)) ;
#105432 = CARTESIAN_POINT('Origin',(44.6495934690622,258.25,28.2541392311682)) ;
#105433 = CARTESIAN_POINT('Origin',(43.4101427530237,258.25,28.5899312084775)) ;
#105434 = CARTESIAN_POINT('',(43.5873838102126,258.25,28.8338825951576)) ;
#105435 = CARTESIAN_POINT('',(43.8235505323126,258.25,29.1589382016729)) ;
#105436 = CARTESIAN_POINT('Origin',(43.0153697314369,258.25,29.7461159238265)) ;
#105437 = CARTESIAN_POINT('',(43.0153697314369,258.25,29.7461159238265)) ;
#105438 = CARTESIAN_POINT('',(42.7792030093369,258.25,29.4210603173112)) ;
#105439 = CARTESIAN_POINT('Origin',(43.4328188876086,258.25,29.4709138126218)) ;
#105440 = CARTESIAN_POINT('Origin',(42.1502657799301,258.25,29.4072596258153)) ;
#105441 = CARTESIAN_POINT('',(42.2434469180392,258.25,29.694041680549)) ;
#105442 = CARTESIAN_POINT('',(42.3676071114944,258.25,30.0761674639184)) ;
#105443 = CARTESIAN_POINT('Origin',(41.4175335996131,258.25,30.3848650607978)) ;
#105444 = CARTESIAN_POINT('',(41.4175335996131,258.25,30.3848650607978)) ;
#105445 = CARTESIAN_POINT('',(41.293373406158,258.25,30.0027392774284)) ;
#105446 = CARTESIAN_POINT('Origin',(41.8995934690622,258.25,30.252131183183)) ;
#105447 = CARTESIAN_POINT('Origin',(40.6994832039963,258.25,29.7952617475701)) ;
#105448 = CARTESIAN_POINT('',(40.6994832039963,258.25,30.096802244712)) ;
#105449 = CARTESIAN_POINT('',(40.6994832039963,258.25,30.4985930708324)) ;
#105450 = CARTESIAN_POINT('Origin',(39.7005167960037,258.25,30.4985930708324)) ;
#105451 = CARTESIAN_POINT('',(39.7005167960037,258.25,30.4985930708324)) ;
#105452 = CARTESIAN_POINT('Origin',(40.2,258.25,30.5213203435596)) ;
#105453 = CARTESIAN_POINT('Origin',(40.2,258.25,25.0213203435596)) ;
#105454 = CARTESIAN_POINT('Origin',(40.2,258.25,25.0213203435596)) ;
#105455 = CARTESIAN_POINT('Origin',(40.2,258.25,25.0213203435596)) ;
#105456 = CARTESIAN_POINT('Origin',(40.2,258.25,25.0213203435596)) ;
#105457 = CARTESIAN_POINT('Origin',(40.2,258.25,25.0213203435596)) ;
#105458 = CARTESIAN_POINT('Origin',(40.2,258.25,25.0213203435596)) ;
#105459 = CARTESIAN_POINT('Origin',(40.2,258.25,25.0213203435596)) ;
#105460 = CARTESIAN_POINT('Origin',(40.2,258.25,25.0213203435596)) ;
#105461 = CARTESIAN_POINT('Origin',(40.2,258.25,25.0213203435596)) ;
#105462 = CARTESIAN_POINT('Origin',(40.2,258.75,25.0213203435596)) ;
#105463 = CARTESIAN_POINT('',(42.2,258.75,25.0213203435596)) ;
#105464 = CARTESIAN_POINT('',(0.,0.,0.)) ;
#105465 = CARTESIAN_POINT('Origin',(66.4402651077866,248.040265107786,23.0213203435596)) ;
#105466 = CARTESIAN_POINT('',(66.1902651077865,245.040265107786,23.0213203435596)) ;
#105467 = CARTESIAN_POINT('Origin',(66.1902651077865,248.040265107786,23.0213203435596)) ;
#105468 = CARTESIAN_POINT('',(65.4402651077865,244.072019271234,23.0213203435596)) ;
#105469 = CARTESIAN_POINT('Origin',(66.4402651077866,244.072019271234,23.0213203435596)) ;
#105470 = CARTESIAN_POINT('Origin',(65.4402651077865,248.040265107786,23.0213203435596)) ;
#105471 = CARTESIAN_POINT('Origin',(65.4402651077865,248.040265107786,23.0213203435596)) ;
#105472 = CARTESIAN_POINT('',(65.4402651077865,252.442540694976,23.0172786696089)) ;
#105473 = CARTESIAN_POINT('Ctrl Pts',(65.4402651077866,252.442540694976,23.0172786696089)) ;
#105474 = CARTESIAN_POINT('Ctrl Pts',(65.4402651077866,252.44193825915,22.3610929985028)) ;
#105475 = CARTESIAN_POINT('Ctrl Pts',(65.4402651077866,252.140233304353,21.0448319450019)) ;
#105476 = CARTESIAN_POINT('Ctrl Pts',(65.4402651077865,250.873971934894,19.4582865154112)) ;
#105477 = CARTESIAN_POINT('Ctrl Pts',(65.4402651077866,249.045854854551,18.5832034982517)) ;
#105478 = CARTESIAN_POINT('Ctrl Pts',(65.4402651077866,247.020059922002,18.5850672640655)) ;
#105479 = CARTESIAN_POINT('Ctrl Pts',(65.4402651077866,245.192236164937,19.4697890066313)) ;
#105480 = CARTESIAN_POINT('Ctrl Pts',(65.4402651077866,243.935614231154,21.0547463401441)) ;
#105481 = CARTESIAN_POINT('Ctrl Pts',(65.4402651077866,243.488804604471,23.0179171559172)) ;
#105482 = CARTESIAN_POINT('Ctrl Pts',(65.4402651077866,243.938490009196,24.9980925373954)) ;
#105483 = CARTESIAN_POINT('Ctrl Pts',(65.4402651077866,245.203459264903,26.5808573752723)) ;
#105484 = CARTESIAN_POINT('Ctrl Pts',(65.4402651077866,247.029377891764,27.4604808473129)) ;
#105485 = CARTESIAN_POINT('Ctrl Pts',(65.4402651077865,249.055861093547,27.4588462212786)) ;
#105486 = CARTESIAN_POINT('Ctrl Pts',(65.4402651077866,250.87986399868,26.5790375520551)) ;
#105487 = CARTESIAN_POINT('Ctrl Pts',(65.4402651077865,252.145441264101,24.9929395133859)) ;
#105488 = CARTESIAN_POINT('Ctrl Pts',(65.4402651077865,252.443143130803,23.6734643407148)) ;
#105489 = CARTESIAN_POINT('Ctrl Pts',(65.4402651077865,252.442540694976,23.0172786696089)) ;
#105490 = CARTESIAN_POINT('Origin',(58.9402651077865,248.040265107786,23.0213203435596)) ;
#105491 = CARTESIAN_POINT('',(59.9402651077865,248.040265107786,27.0213203435596)) ;
#105492 = CARTESIAN_POINT('Origin',(59.9402651077865,248.040265107786,23.0213203435596)) ;
#105493 = CARTESIAN_POINT('',(58.9402651077865,248.040265107786,26.0213203435596)) ;
#105494 = CARTESIAN_POINT('Origin',(58.9402651077865,248.040265107786,27.0213203435596)) ;
#105495 = CARTESIAN_POINT('Origin',(58.9402651077865,248.040265107786,23.0213203435596)) ;
#105496 = CARTESIAN_POINT('Origin',(59.9402651077865,248.040265107786,23.0213203435596)) ;
#105497 = CARTESIAN_POINT('',(59.9402651077865,252.442541339505,23.0245853614825)) ;
#105498 = CARTESIAN_POINT('Ctrl Pts',(59.9402651077865,252.442541339505,23.0245853614825)) ;
#105499 = CARTESIAN_POINT('Ctrl Pts',(59.9402651077865,252.442054668933,23.6807711286595)) ;
#105500 = CARTESIAN_POINT('Ctrl Pts',(59.9402651077865,252.140582866504,24.9970918038166)) ;
#105501 = CARTESIAN_POINT('Ctrl Pts',(59.9402651077865,250.874603529792,26.5838602800608)) ;
#105502 = CARTESIAN_POINT('Ctrl Pts',(59.9402651077865,249.046642816666,27.4592688287601)) ;
#105503 = CARTESIAN_POINT('Ctrl Pts',(59.9402651077865,247.02084725416,27.457759936616)) ;
#105504 = CARTESIAN_POINT('Ctrl Pts',(59.9402651077865,245.192869526073,26.5733619136289)) ;
#105505 = CARTESIAN_POINT('Ctrl Pts',(59.9402651077865,243.935964506927,24.9886198977872)) ;
#105506 = CARTESIAN_POINT('Ctrl Pts',(59.9402651077865,243.488807364186,23.0255250811106)) ;
#105507 = CARTESIAN_POINT('Ctrl Pts',(59.9402651077865,243.938143019334,21.0452698397019)) ;
#105508 = CARTESIAN_POINT('Ctrl Pts',(59.9402651077865,245.202832783418,19.462280744107)) ;
#105509 = CARTESIAN_POINT('Ctrl Pts',(59.9402651077865,247.028596667264,18.582335498899)) ;
#105510 = CARTESIAN_POINT('Ctrl Pts',(59.9402651077865,249.055081848073,18.5836132230762)) ;
#105511 = CARTESIAN_POINT('Ctrl Pts',(59.9402651077865,250.87923966532,19.4631003199451)) ;
#105512 = CARTESIAN_POINT('Ctrl Pts',(59.9402651077865,252.145094800052,21.0489759066127)) ;
#105513 = CARTESIAN_POINT('Ctrl Pts',(59.9402651077865,252.443028010077,22.3683995943057)) ;
#105514 = CARTESIAN_POINT('Ctrl Pts',(59.9402651077865,252.442541339505,23.0245853614825)) ;
#105515 = CARTESIAN_POINT('Origin',(58.9402651077865,248.040265107786,23.0213203435596)) ;
#105516 = CARTESIAN_POINT('',(58.9402651077865,250.040265107786,23.0213203435596)) ;
#105517 = CARTESIAN_POINT('Origin',(58.9402651077865,248.040265107786,23.0213203435596)) ;
#105518 = CARTESIAN_POINT('Origin',(66.1902651077865,248.040265107786,23.0213203435596)) ;
#105519 = CARTESIAN_POINT('',(66.1902651077865,250.040265107786,23.0213203435596)) ;
#105520 = CARTESIAN_POINT('Origin',(66.1902651077865,248.040265107786,23.0213203435596)) ;
#105521 = CARTESIAN_POINT('Ctrl Pts',(65.0766287441502,252.840884205283,23.0169129554328)) ;
#105522 = CARTESIAN_POINT('Ctrl Pts',(65.0766287441502,252.841541153009,23.7324741241568)) ;
#105523 = CARTESIAN_POINT('Ctrl Pts',(65.0766287441502,252.516901489192,25.1713430879785)) ;
#105524 = CARTESIAN_POINT('Ctrl Pts',(65.0766287441502,251.136807428881,26.9009605060916)) ;
#105525 = CARTESIAN_POINT('Ctrl Pts',(65.0766287441502,249.147758127707,27.8603793829806)) ;
#105526 = CARTESIAN_POINT('Ctrl Pts',(65.0766287441502,246.937906934488,27.8621619194897)) ;
#105527 = CARTESIAN_POINT('Ctrl Pts',(65.0766287441502,244.946768565938,26.9029449975024)) ;
#105528 = CARTESIAN_POINT('Ctrl Pts',(65.0766287441502,243.567337531596,25.176962387584)) ;
#105529 = CARTESIAN_POINT('Ctrl Pts',(65.0766287441502,243.076961974903,23.0176092156974)) ;
#105530 = CARTESIAN_POINT('Ctrl Pts',(65.0766287441502,243.564201536425,20.8767992815642)) ;
#105531 = CARTESIAN_POINT('Ctrl Pts',(65.0766287441502,244.934529934584,19.1484257862475)) ;
#105532 = CARTESIAN_POINT('Ctrl Pts',(65.0766287441502,246.927745820604,18.1836492725528)) ;
#105533 = CARTESIAN_POINT('Ctrl Pts',(65.0766287441502,249.136846465985,18.1816168623636)) ;
#105534 = CARTESIAN_POINT('Ctrl Pts',(65.0766287441502,251.13038221688,19.1358824826931)) ;
#105535 = CARTESIAN_POINT('Ctrl Pts',(65.0766287441502,252.511222282944,20.8659877742614)) ;
#105536 = CARTESIAN_POINT('Ctrl Pts',(65.0766287441502,252.840227257557,22.3013517867086)) ;
#105537 = CARTESIAN_POINT('Ctrl Pts',(65.0766287441502,252.840884205283,23.0169129554328)) ;
#105538 = CARTESIAN_POINT('Ctrl Pts',(65.1748710205118,252.831915957252,23.0169211890687)) ;
#105539 = CARTESIAN_POINT('Ctrl Pts',(65.1748710205118,252.832571765951,23.7312417059042)) ;
#105540 = CARTESIAN_POINT('Ctrl Pts',(65.1748710205118,252.508661681794,25.1674922263976)) ;
#105541 = CARTESIAN_POINT('Ctrl Pts',(65.1748710205118,251.131222805096,26.8940046369024)) ;
#105542 = CARTESIAN_POINT('Ctrl Pts',(65.1748710205118,249.145626752009,27.851731242655)) ;
#105543 = CARTESIAN_POINT('Ctrl Pts',(65.1748710205118,246.939810869674,27.8535478771211)) ;
#105544 = CARTESIAN_POINT('Ctrl Pts',(65.1748710205118,244.952192187541,26.8960024422975)) ;
#105545 = CARTESIAN_POINT('Ctrl Pts',(65.1748710205118,243.575204883934,25.173113845116)) ;
#105546 = CARTESIAN_POINT('Ctrl Pts',(65.1748710205118,243.085737340501,23.0176042703897)) ;
#105547 = CARTESIAN_POINT('Ctrl Pts',(65.1748710205118,243.572070300257,20.8805601134562)) ;
#105548 = CARTESIAN_POINT('Ctrl Pts',(65.1748710205118,244.939993984156,19.1552952558752)) ;
#105549 = CARTESIAN_POINT('Ctrl Pts',(65.1748710205118,246.929583107595,18.1921893326471)) ;
#105550 = CARTESIAN_POINT('Ctrl Pts',(65.1748710205118,249.13471409468,18.1902224427852)) ;
#105551 = CARTESIAN_POINT('Ctrl Pts',(65.1748710205118,251.124669629215,19.1427533342878)) ;
#105552 = CARTESIAN_POINT('Ctrl Pts',(65.1748710205118,252.502921872703,20.869804047502)) ;
#105553 = CARTESIAN_POINT('Ctrl Pts',(65.1748710205118,252.831260148553,22.3026006722331)) ;
#105554 = CARTESIAN_POINT('Ctrl Pts',(65.1748710205118,252.831915957252,23.0169211890687)) ;
#105555 = CARTESIAN_POINT('Ctrl Pts',(65.3636768956757,252.737773789869,23.0170076198108)) ;
#105556 = CARTESIAN_POINT('Ctrl Pts',(65.3636768956757,252.738416598441,23.7171681269576)) ;
#105557 = CARTESIAN_POINT('Ctrl Pts',(65.3636768956757,252.420709470249,25.1251094967809)) ;
#105558 = CARTESIAN_POINT('Ctrl Pts',(65.3636768956758,251.070232680745,26.8175359526613)) ;
#105559 = CARTESIAN_POINT('Ctrl Pts',(65.3636768956757,249.12399117821,27.7563151648642)) ;
#105560 = CARTESIAN_POINT('Ctrl Pts',(65.3636768956758,246.961634836841,27.7580471751047)) ;
#105561 = CARTESIAN_POINT('Ctrl Pts',(65.3636768956758,245.013328686296,26.8194722536279)) ;
#105562 = CARTESIAN_POINT('Ctrl Pts',(65.3636768956758,243.663569427515,25.1306039104643)) ;
#105563 = CARTESIAN_POINT('Ctrl Pts',(65.3636768956758,243.183729076732,23.0176928098972)) ;
#105564 = CARTESIAN_POINT('Ctrl Pts',(65.3636768956758,243.660502243309,20.9229407854373)) ;
#105565 = CARTESIAN_POINT('Ctrl Pts',(65.3636768956758,245.001347179161,19.2317295875749)) ;
#105566 = CARTESIAN_POINT('Ctrl Pts',(65.3636768956758,246.951719972586,18.2877181762278)) ;
#105567 = CARTESIAN_POINT('Ctrl Pts',(65.3636768956758,249.113320875214,18.2857092340863)) ;
#105568 = CARTESIAN_POINT('Ctrl Pts',(65.3636768956758,251.063991246017,19.2194629073674)) ;
#105569 = CARTESIAN_POINT('Ctrl Pts',(65.3636768956758,252.415175533547,20.9123499681276)) ;
#105570 = CARTESIAN_POINT('Ctrl Pts',(65.3636768956758,252.737130981298,22.3168471126638)) ;
#105571 = CARTESIAN_POINT('Ctrl Pts',(65.3636768956758,252.737773789869,23.0170076198108)) ;
#105572 = CARTESIAN_POINT('Ctrl Pts',(65.4402651077865,252.541191423318,23.0171880996136)) ;
#105573 = CARTESIAN_POINT('Ctrl Pts',(65.4402651077865,252.54180737839,23.6880992141914)) ;
#105574 = CARTESIAN_POINT('Ctrl Pts',(65.4402651077865,252.237461144507,25.0371577162623)) ;
#105575 = CARTESIAN_POINT('Ctrl Pts',(65.4402651077866,250.943540302405,26.6588261848968)) ;
#105576 = CARTESIAN_POINT('Ctrl Pts',(65.4402651077865,249.078606004666,27.558372331764)) ;
#105577 = CARTESIAN_POINT('Ctrl Pts',(65.4402651077866,247.006690998239,27.5600517492951)) ;
#105578 = CARTESIAN_POINT('Ctrl Pts',(65.4402651077866,245.139811685101,26.6606905000547)) ;
#105579 = CARTESIAN_POINT('Ctrl Pts',(65.4402651077866,243.846466640749,25.042429009221)) ;
#105580 = CARTESIAN_POINT('Ctrl Pts',(65.4402651077866,243.386702460434,23.0178383037529)) ;
#105581 = CARTESIAN_POINT('Ctrl Pts',(65.4402651077866,243.843525449649,21.0106238048176)) ;
#105582 = CARTESIAN_POINT('Ctrl Pts',(65.4402651077866,245.128340916242,19.3901229016862)) ;
#105583 = CARTESIAN_POINT('Ctrl Pts',(65.4402651077866,246.997145550192,18.485546674421)) ;
#105584 = CARTESIAN_POINT('Ctrl Pts',(65.4402651077866,249.068370873645,18.4836546021279)) ;
#105585 = CARTESIAN_POINT('Ctrl Pts',(65.4402651077865,250.937485683585,19.3783578426627)) ;
#105586 = CARTESIAN_POINT('Ctrl Pts',(65.4402651077866,252.23212095168,21.0004949225647)) ;
#105587 = CARTESIAN_POINT('Ctrl Pts',(65.4402651077866,252.540575468246,22.3462769850356)) ;
#105588 = CARTESIAN_POINT('Ctrl Pts',(65.4402651077866,252.541191423318,23.0171880996136)) ;
#105589 = CARTESIAN_POINT('Ctrl Pts',(65.4402651077865,252.442540694976,23.0172786696089)) ;
#105590 = CARTESIAN_POINT('Ctrl Pts',(65.4402651077865,252.443143130803,23.6734643407148)) ;
#105591 = CARTESIAN_POINT('Ctrl Pts',(65.4402651077865,252.145441264101,24.9929395133859)) ;
#105592 = CARTESIAN_POINT('Ctrl Pts',(65.4402651077866,250.87986399868,26.5790375520551)) ;
#105593 = CARTESIAN_POINT('Ctrl Pts',(65.4402651077865,249.055861093547,27.4588462212786)) ;
#105594 = CARTESIAN_POINT('Ctrl Pts',(65.4402651077866,247.029377891764,27.4604808473129)) ;
#105595 = CARTESIAN_POINT('Ctrl Pts',(65.4402651077866,245.203459264903,26.5808573752723)) ;
#105596 = CARTESIAN_POINT('Ctrl Pts',(65.4402651077866,243.938490009196,24.9980925373954)) ;
#105597 = CARTESIAN_POINT('Ctrl Pts',(65.4402651077866,243.488804604471,23.0179171559172)) ;
#105598 = CARTESIAN_POINT('Ctrl Pts',(65.4402651077866,243.935614231154,21.0547463401441)) ;
#105599 = CARTESIAN_POINT('Ctrl Pts',(65.4402651077866,245.192236164937,19.4697890066313)) ;
#105600 = CARTESIAN_POINT('Ctrl Pts',(65.4402651077866,247.020059922002,18.5850672640655)) ;
#105601 = CARTESIAN_POINT('Ctrl Pts',(65.4402651077866,249.045854854551,18.5832034982517)) ;
#105602 = CARTESIAN_POINT('Ctrl Pts',(65.4402651077865,250.873971934894,19.4582865154112)) ;
#105603 = CARTESIAN_POINT('Ctrl Pts',(65.4402651077866,252.140233304353,21.0448319450019)) ;
#105604 = CARTESIAN_POINT('Ctrl Pts',(65.4402651077866,252.44193825915,22.3610929985028)) ;
#105605 = CARTESIAN_POINT('Ctrl Pts',(65.4402651077866,252.442540694976,23.0172786696089)) ;
#105606 = CARTESIAN_POINT('',(65.0766287441502,252.840884205283,23.0169129554328)) ;
#105607 = CARTESIAN_POINT('Ctrl Pts',(65.4402651077865,252.442540694976,23.0172786696089)) ;
#105608 = CARTESIAN_POINT('Ctrl Pts',(65.4402651077865,252.541191423318,23.0171880996136)) ;
#105609 = CARTESIAN_POINT('Ctrl Pts',(65.3636768956757,252.737773789869,23.0170076198108)) ;
#105610 = CARTESIAN_POINT('Ctrl Pts',(65.1748710205118,252.831915957252,23.0169211890687)) ;
#105611 = CARTESIAN_POINT('Ctrl Pts',(65.0766287441502,252.840884205283,23.0169129554328)) ;
#105612 = CARTESIAN_POINT('',(65.0766287441502,248.040357057742,27.8212999984394)) ;
#105613 = CARTESIAN_POINT('Ctrl Pts',(65.0766287441502,252.840884205283,23.0169129554328)) ;
#105614 = CARTESIAN_POINT('Ctrl Pts',(65.0766287441502,252.841541153009,23.7324741241568)) ;
#105615 = CARTESIAN_POINT('Ctrl Pts',(65.0766287441502,252.516901489192,25.1713430879785)) ;
#105616 = CARTESIAN_POINT('Ctrl Pts',(65.0766287441502,251.136807428881,26.9009605060916)) ;
#105617 = CARTESIAN_POINT('Ctrl Pts',(65.0766287441502,249.478518089747,27.700837157902)) ;
#105618 = CARTESIAN_POINT('Ctrl Pts',(65.0766287441502,248.400319833693,27.8212533107379)) ;
#105619 = CARTESIAN_POINT('Ctrl Pts',(65.0766287441502,248.040357057742,27.8212999984394)) ;
#105620 = CARTESIAN_POINT('Ctrl Pts',(65.0766287441502,248.040357057742,27.8212999984394)) ;
#105621 = CARTESIAN_POINT('Ctrl Pts',(65.0766287441502,247.682015582841,27.8213464758557)) ;
#105622 = CARTESIAN_POINT('Ctrl Pts',(65.0766287441502,246.605301499027,27.7019315873951)) ;
#105623 = CARTESIAN_POINT('Ctrl Pts',(65.0766287441502,244.946768565938,26.9029449975024)) ;
#105624 = CARTESIAN_POINT('Ctrl Pts',(65.0766287441502,243.567337531596,25.176962387584)) ;
#105625 = CARTESIAN_POINT('Ctrl Pts',(65.0766287441502,243.076961974903,23.0176092156974)) ;
#105626 = CARTESIAN_POINT('Ctrl Pts',(65.0766287441502,243.564201536425,20.8767992815642)) ;
#105627 = CARTESIAN_POINT('Ctrl Pts',(65.0766287441502,244.934529934584,19.1484257862475)) ;
#105628 = CARTESIAN_POINT('Ctrl Pts',(65.0766287441502,246.927745820604,18.1836492725528)) ;
#105629 = CARTESIAN_POINT('Ctrl Pts',(65.0766287441502,249.136846465985,18.1816168623636)) ;
#105630 = CARTESIAN_POINT('Ctrl Pts',(65.0766287441502,251.13038221688,19.1358824826931)) ;
#105631 = CARTESIAN_POINT('Ctrl Pts',(65.0766287441502,252.511222282944,20.8659877742614)) ;
#105632 = CARTESIAN_POINT('Ctrl Pts',(65.0766287441502,252.840227257557,22.3013517867086)) ;
#105633 = CARTESIAN_POINT('Ctrl Pts',(65.0766287441502,252.840884205283,23.0169129554328)) ;
#105634 = CARTESIAN_POINT('Ctrl Pts',(60.3039014714229,252.840884908133,23.0248807993021)) ;
#105635 = CARTESIAN_POINT('Ctrl Pts',(60.3039014714229,252.841415615489,22.3093195258141)) ;
#105636 = CARTESIAN_POINT('Ctrl Pts',(60.3039014714229,252.516523675061,20.8705067056309)) ;
#105637 = CARTESIAN_POINT('Ctrl Pts',(60.3039014714229,251.136126602205,19.141131868271)) ;
#105638 = CARTESIAN_POINT('Ctrl Pts',(60.3039014714229,249.146908371569,18.1820636614743)) ;
#105639 = CARTESIAN_POINT('Ctrl Pts',(60.3039014714228,246.937055020249,18.180670321379)) ;
#105640 = CARTESIAN_POINT('Ctrl Pts',(60.3039014714228,244.946085396763,19.1402381324422)) ;
#105641 = CARTESIAN_POINT('Ctrl Pts',(60.3039014714229,243.566959144073,20.8664652922218)) ;
#105642 = CARTESIAN_POINT('Ctrl Pts',(60.3039014714228,243.076964984333,23.02590555023)) ;
#105643 = CARTESIAN_POINT('Ctrl Pts',(60.3039014714229,243.564583507187,25.1666326084264)) ;
#105644 = CARTESIAN_POINT('Ctrl Pts',(60.3039014714229,244.935220605921,26.8947713028763)) ;
#105645 = CARTESIAN_POINT('Ctrl Pts',(60.3039014714229,246.928604395157,27.859194804961)) ;
#105646 = CARTESIAN_POINT('Ctrl Pts',(60.3039014714229,249.137705727497,27.8608402304461)) ;
#105647 = CARTESIAN_POINT('Ctrl Pts',(60.3039014714229,251.131070962159,26.9062196225889)) ;
#105648 = CARTESIAN_POINT('Ctrl Pts',(60.3039014714229,252.511603475512,25.175871101808)) ;
#105649 = CARTESIAN_POINT('Ctrl Pts',(60.3039014714229,252.840354200776,23.7404420727902)) ;
#105650 = CARTESIAN_POINT('Ctrl Pts',(60.3039014714229,252.840884908133,23.0248807993021)) ;
#105651 = CARTESIAN_POINT('Ctrl Pts',(60.2056591950613,252.831916658789,23.0248741478579)) ;
#105652 = CARTESIAN_POINT('Ctrl Pts',(60.2056591950613,252.832446445996,22.31055352644)) ;
#105653 = CARTESIAN_POINT('Ctrl Pts',(60.2056591950613,252.508284848399,20.8743600638376)) ;
#105654 = CARTESIAN_POINT('Ctrl Pts',(60.2056591950612,251.130544493213,19.1480906302711)) ;
#105655 = CARTESIAN_POINT('Ctrl Pts',(60.2056591950613,249.144779759817,18.1907143485154)) ;
#105656 = CARTESIAN_POINT('Ctrl Pts',(60.2056591950612,246.938963013392,18.1892858361865)) ;
#105657 = CARTESIAN_POINT('Ctrl Pts',(60.2056591950612,244.951513228265,19.1471814493788)) ;
#105658 = CARTESIAN_POINT('Ctrl Pts',(60.2056591950613,243.574830611665,20.8703131984953)) ;
#105659 = CARTESIAN_POINT('Ctrl Pts',(60.2056591950613,243.085744226675,23.0259087382533)) ;
#105660 = CARTESIAN_POINT('Ctrl Pts',(60.2056591950613,243.572455132768,25.1628696592994)) ;
#105661 = CARTESIAN_POINT('Ctrl Pts',(60.2056591950613,244.940686770073,26.8878990509792)) ;
#105662 = CARTESIAN_POINT('Ctrl Pts',(60.2056591950613,246.9304425947,27.8506526804878)) ;
#105663 = CARTESIAN_POINT('Ctrl Pts',(60.2056591950613,249.135573431834,27.8522327343816)) ;
#105664 = CARTESIAN_POINT('Ctrl Pts',(60.2056591950613,251.125358278647,26.8993483215869)) ;
#105665 = CARTESIAN_POINT('Ctrl Pts',(60.2056591950613,252.503302661219,25.1720554371834)) ;
#105666 = CARTESIAN_POINT('Ctrl Pts',(60.2056591950613,252.831386871581,23.7391947692758)) ;
#105667 = CARTESIAN_POINT('Ctrl Pts',(60.2056591950613,252.831916658789,23.0248741478579)) ;
#105668 = CARTESIAN_POINT('Ctrl Pts',(60.0168530828095,252.737774694053,23.024804325978)) ;
#105669 = CARTESIAN_POINT('Ctrl Pts',(60.0168530828095,252.738293979264,22.3246437163219)) ;
#105670 = CARTESIAN_POINT('Ctrl Pts',(60.0168530828095,252.420339841483,20.9167569091084)) ;
#105671 = CARTESIAN_POINT('Ctrl Pts',(60.0168530828094,251.069566142761,19.2245675100239)) ;
#105672 = CARTESIAN_POINT('Ctrl Pts',(60.0168530828095,249.123159359322,18.2861313252103)) ;
#105673 = CARTESIAN_POINT('Ctrl Pts',(60.0168530828094,246.960800415503,18.2847802781622)) ;
#105674 = CARTESIAN_POINT('Ctrl Pts',(60.0168530828094,245.012659210062,19.2236985730182)) ;
#105675 = CARTESIAN_POINT('Ctrl Pts',(60.0168530828094,243.663198013795,20.9128065556026)) ;
#105676 = CARTESIAN_POINT('Ctrl Pts',(60.0168530828094,243.18373069356,23.0258032190076)) ;
#105677 = CARTESIAN_POINT('Ctrl Pts',(60.0168530828094,243.660874803201,25.1204743342267)) ;
#105678 = CARTESIAN_POINT('Ctrl Pts',(60.0168530828094,245.002021874673,26.8114561732744)) ;
#105679 = CARTESIAN_POINT('Ctrl Pts',(60.0168530828095,246.952559313171,27.7551221353331)) ;
#105680 = CARTESIAN_POINT('Ctrl Pts',(60.0168530828094,249.114161208371,27.7567526134108)) ;
#105681 = CARTESIAN_POINT('Ctrl Pts',(60.0168530828094,251.064664927345,26.8226512873956)) ;
#105682 = CARTESIAN_POINT('Ctrl Pts',(60.0168530828095,252.415548621932,25.1295260055957)) ;
#105683 = CARTESIAN_POINT('Ctrl Pts',(60.0168530828095,252.737255408843,23.7249649356341)) ;
#105684 = CARTESIAN_POINT('Ctrl Pts',(60.0168530828095,252.737774694053,23.024804325978)) ;
#105685 = CARTESIAN_POINT('Ctrl Pts',(59.9402651077865,252.54119208229,23.0246585273691)) ;
#105686 = CARTESIAN_POINT('Ctrl Pts',(59.9402651077865,252.541689674222,22.3537473145644)) ;
#105687 = CARTESIAN_POINT('Ctrl Pts',(59.9402651077865,252.237106976482,21.0047416734212)) ;
#105688 = CARTESIAN_POINT('Ctrl Pts',(59.9402651077865,250.942902249354,19.3833008269238)) ;
#105689 = CARTESIAN_POINT('Ctrl Pts',(59.9402651077865,249.077809553585,18.4840835259144)) ;
#105690 = CARTESIAN_POINT('Ctrl Pts',(59.9402651077865,247.005892805063,18.4827689323583)) ;
#105691 = CARTESIAN_POINT('Ctrl Pts',(59.9402651077865,245.139171804449,19.3824591533555)) ;
#105692 = CARTESIAN_POINT('Ctrl Pts',(59.9402651077865,243.84611261837,21.000949722106)) ;
#105693 = CARTESIAN_POINT('Ctrl Pts',(59.9402651077865,243.386706128535,23.0256218681107)) ;
#105694 = CARTESIAN_POINT('Ctrl Pts',(59.9402651077865,243.843884354356,25.0327585526377)) ;
#105695 = CARTESIAN_POINT('Ctrl Pts',(59.9402651077865,245.12898921281,26.6530390723829)) ;
#105696 = CARTESIAN_POINT('Ctrl Pts',(59.9402651077865,246.997951074417,27.5572843385644)) ;
#105697 = CARTESIAN_POINT('Ctrl Pts',(59.9402651077865,249.069176859737,27.558813459608)) ;
#105698 = CARTESIAN_POINT('Ctrl Pts',(59.9402651077865,250.938131691571,26.6637775677947)) ;
#105699 = CARTESIAN_POINT('Ctrl Pts',(59.9402651077865,252.232478414354,25.0414125746018)) ;
#105700 = CARTESIAN_POINT('Ctrl Pts',(59.9402651077865,252.540694490358,23.6955697401738)) ;
#105701 = CARTESIAN_POINT('Ctrl Pts',(59.9402651077865,252.54119208229,23.0246585273691)) ;
#105702 = CARTESIAN_POINT('Ctrl Pts',(59.9402651077865,252.442541339505,23.0245853614825)) ;
#105703 = CARTESIAN_POINT('Ctrl Pts',(59.9402651077865,252.443028010077,22.3683995943057)) ;
#105704 = CARTESIAN_POINT('Ctrl Pts',(59.9402651077865,252.145094800052,21.0489759066127)) ;
#105705 = CARTESIAN_POINT('Ctrl Pts',(59.9402651077865,250.87923966532,19.4631003199451)) ;
#105706 = CARTESIAN_POINT('Ctrl Pts',(59.9402651077865,249.055081848073,18.5836132230762)) ;
#105707 = CARTESIAN_POINT('Ctrl Pts',(59.9402651077865,247.028596667264,18.582335498899)) ;
#105708 = CARTESIAN_POINT('Ctrl Pts',(59.9402651077865,245.202832783418,19.462280744107)) ;
#105709 = CARTESIAN_POINT('Ctrl Pts',(59.9402651077865,243.938143019334,21.0452698397019)) ;
#105710 = CARTESIAN_POINT('Ctrl Pts',(59.9402651077865,243.488807364186,23.0255250811106)) ;
#105711 = CARTESIAN_POINT('Ctrl Pts',(59.9402651077865,243.935964506927,24.9886198977872)) ;
#105712 = CARTESIAN_POINT('Ctrl Pts',(59.9402651077865,245.192869526073,26.5733619136289)) ;
#105713 = CARTESIAN_POINT('Ctrl Pts',(59.9402651077865,247.02084725416,27.457759936616)) ;
#105714 = CARTESIAN_POINT('Ctrl Pts',(59.9402651077865,249.046642816666,27.4592688287601)) ;
#105715 = CARTESIAN_POINT('Ctrl Pts',(59.9402651077865,250.874603529792,26.5838602800608)) ;
#105716 = CARTESIAN_POINT('Ctrl Pts',(59.9402651077865,252.140582866504,24.9970918038166)) ;
#105717 = CARTESIAN_POINT('Ctrl Pts',(59.9402651077865,252.442054668933,23.6807711286595)) ;
#105718 = CARTESIAN_POINT('Ctrl Pts',(59.9402651077865,252.442541339505,23.0245853614825)) ;
#105719 = CARTESIAN_POINT('',(60.3039014714229,252.840884908133,23.0248807993021)) ;
#105720 = CARTESIAN_POINT('Ctrl Pts',(59.9402651077865,252.442541339505,23.0245853614825)) ;
#105721 = CARTESIAN_POINT('Ctrl Pts',(59.9402651077865,252.54119208229,23.0246585273691)) ;
#105722 = CARTESIAN_POINT('Ctrl Pts',(60.0168530828095,252.737774694053,23.024804325978)) ;
#105723 = CARTESIAN_POINT('Ctrl Pts',(60.2056591950613,252.831916658789,23.0248741478579)) ;
#105724 = CARTESIAN_POINT('Ctrl Pts',(60.3039014714229,252.840884908133,23.0248807993021)) ;
#105725 = CARTESIAN_POINT('',(60.3039014714229,248.040364444053,18.2213381124782)) ;
#105726 = CARTESIAN_POINT('Ctrl Pts',(60.3039014714229,252.840884908133,23.0248807993021)) ;
#105727 = CARTESIAN_POINT('Ctrl Pts',(60.3039014714229,252.841415615489,22.3093195258141)) ;
#105728 = CARTESIAN_POINT('Ctrl Pts',(60.3039014714229,252.516523675061,20.8705067056309)) ;
#105729 = CARTESIAN_POINT('Ctrl Pts',(60.3039014714229,251.136126602205,19.141131868271)) ;
#105730 = CARTESIAN_POINT('Ctrl Pts',(60.3039014714229,249.477958337868,18.3416738503658)) ;
#105731 = CARTESIAN_POINT('Ctrl Pts',(60.3039014714229,248.400043702177,18.2213846529397)) ;
#105732 = CARTESIAN_POINT('Ctrl Pts',(60.3039014714229,248.040364444053,18.2213381124782)) ;
#105733 = CARTESIAN_POINT('Ctrl Pts',(60.3039014714229,248.040364444053,18.2213381124782)) ;
#105734 = CARTESIAN_POINT('Ctrl Pts',(60.3039014714229,247.681739029051,18.2212917083782)) ;
#105735 = CARTESIAN_POINT('Ctrl Pts',(60.3039014714228,246.604739915942,18.3408329242945)) ;
#105736 = CARTESIAN_POINT('Ctrl Pts',(60.3039014714228,244.946085396763,19.1402381324422)) ;
#105737 = CARTESIAN_POINT('Ctrl Pts',(60.3039014714229,243.566959144073,20.8664652922218)) ;
#105738 = CARTESIAN_POINT('Ctrl Pts',(60.3039014714228,243.076964984333,23.02590555023)) ;
#105739 = CARTESIAN_POINT('Ctrl Pts',(60.3039014714229,243.564583507187,25.1666326084264)) ;
#105740 = CARTESIAN_POINT('Ctrl Pts',(60.3039014714229,244.935220605921,26.8947713028763)) ;
#105741 = CARTESIAN_POINT('Ctrl Pts',(60.3039014714229,246.928604395157,27.859194804961)) ;
#105742 = CARTESIAN_POINT('Ctrl Pts',(60.3039014714229,249.137705727497,27.8608402304461)) ;
#105743 = CARTESIAN_POINT('Ctrl Pts',(60.3039014714229,251.131070962159,26.9062196225889)) ;
#105744 = CARTESIAN_POINT('Ctrl Pts',(60.3039014714229,252.511603475512,25.175871101808)) ;
#105745 = CARTESIAN_POINT('Ctrl Pts',(60.3039014714229,252.840354200776,23.7404420727902)) ;
#105746 = CARTESIAN_POINT('Ctrl Pts',(60.3039014714229,252.840884908133,23.0248807993021)) ;
#105747 = CARTESIAN_POINT('Origin',(64.7902651077865,248.040265107786,23.0213203435596)) ;
#105748 = CARTESIAN_POINT('',(64.9402651077865,246.182069881617,27.6093057948708)) ;
#105749 = CARTESIAN_POINT('',(64.9402651077865,245.420726657552,27.2213820464094)) ;
#105750 = CARTESIAN_POINT('Origin',(64.9402651077865,248.040265107786,23.0213203435596)) ;
#105751 = CARTESIAN_POINT('',(64.7902651077865,245.996818189747,27.694041680549)) ;
#105752 = CARTESIAN_POINT('Ctrl Pts',(64.9402651077865,246.182069881617,27.6093057948708)) ;
#105753 = CARTESIAN_POINT('Ctrl Pts',(64.9402651077865,246.181354905733,27.6096388244826)) ;
#105754 = CARTESIAN_POINT('Ctrl Pts',(64.940261777681,246.180639897624,27.6099717982194)) ;
#105755 = CARTESIAN_POINT('Ctrl Pts',(64.9400834366345,246.161498924883,27.6188837045809)) ;
#105756 = CARTESIAN_POINT('Ctrl Pts',(64.9376982652988,246.142984930219,27.6274555764536)) ;
#105757 = CARTESIAN_POINT('Ctrl Pts',(64.9285249168183,246.107849325612,27.6436380121775)) ;
#105758 = CARTESIAN_POINT('Ctrl Pts',(64.9218878905886,246.091024885902,27.6513456347974)) ;
#105759 = CARTESIAN_POINT('Ctrl Pts',(64.9030518920066,246.057970599548,27.6664219076507)) ;
#105760 = CARTESIAN_POINT('Ctrl Pts',(64.8902415596279,246.04185831974,27.6737287158086)) ;
#105761 = CARTESIAN_POINT('Ctrl Pts',(64.8622234505159,246.018444687196,27.6843112161272)) ;
#105762 = CARTESIAN_POINT('Ctrl Pts',(64.8483068832618,246.010067315225,27.6880838741351)) ;
#105763 = CARTESIAN_POINT('Ctrl Pts',(64.8193104176513,245.999468779803,27.6928518010587)) ;
#105764 = CARTESIAN_POINT('Ctrl Pts',(64.8049443310403,245.996818189747,27.694041680549)) ;
#105765 = CARTESIAN_POINT('Ctrl Pts',(64.7902651077865,245.996818189747,27.694041680549)) ;
#105766 = CARTESIAN_POINT('',(64.7902651077865,245.461062098449,27.4210603173112)) ;
#105767 = CARTESIAN_POINT('Origin',(64.7902651077865,248.040265107786,23.0213203435596)) ;
#105768 = CARTESIAN_POINT('Ctrl Pts',(64.9402651077865,245.420726657552,27.2213820464094)) ;
#105769 = CARTESIAN_POINT('Ctrl Pts',(64.9402651077865,245.420877483218,27.2221562239469)) ;
#105770 = CARTESIAN_POINT('Ctrl Pts',(64.9402617776811,245.421028373027,27.2229303947064)) ;
#105771 = CARTESIAN_POINT('Ctrl Pts',(64.9400834366345,245.425069270822,27.2436540540753)) ;
#105772 = CARTESIAN_POINT('Ctrl Pts',(64.9376982652987,245.429016733827,27.2636706102621)) ;
#105773 = CARTESIAN_POINT('Ctrl Pts',(64.9285249168183,245.436577058534,27.3016077085614)) ;
#105774 = CARTESIAN_POINT('Ctrl Pts',(64.9218878905886,245.440230618388,27.3197493931139)) ;
#105775 = CARTESIAN_POINT('Ctrl Pts',(64.9030518920066,245.447462479482,27.3553524833539)) ;
#105776 = CARTESIAN_POINT('Ctrl Pts',(64.8902415596279,245.451021707959,27.372682425613)) ;
#105777 = CARTESIAN_POINT('Ctrl Pts',(64.8622234505159,245.45622247327,27.3978446898608)) ;
#105778 = CARTESIAN_POINT('Ctrl Pts',(64.8483068832618,245.458094424526,27.406839638893)) ;
#105779 = CARTESIAN_POINT('Ctrl Pts',(64.8193104176514,245.460466753434,27.4182165512944)) ;
#105780 = CARTESIAN_POINT('Ctrl Pts',(64.8049443310403,245.461062098449,27.4210603173112)) ;
#105781 = CARTESIAN_POINT('Ctrl Pts',(64.7902651077865,245.461062098449,27.4210603173112)) ;
#105782 = CARTESIAN_POINT('Origin',(64.7902651077865,246.861601651513,25.5179220536754)) ;
#105783 = CARTESIAN_POINT('',(64.9402651077865,246.014168667474,28.1260525975113)) ;
#105784 = CARTESIAN_POINT('',(64.9402651077865,246.861601651513,25.5179220536754)) ;
#105785 = CARTESIAN_POINT('',(64.7902651077865,245.872657996292,28.0761674639184)) ;
#105786 = CARTESIAN_POINT('Ctrl Pts',(64.9402651077865,246.014168667474,28.1260525975113)) ;
#105787 = CARTESIAN_POINT('Ctrl Pts',(64.9402651077865,246.012794157307,28.1255643186931)) ;
#105788 = CARTESIAN_POINT('Ctrl Pts',(64.940243846551,246.011419678562,28.1250761825186)) ;
#105789 = CARTESIAN_POINT('Ctrl Pts',(64.9402013305492,246.010045670283,28.1245883423369)) ;
#105790 = CARTESIAN_POINT('Ctrl Pts',(64.939655139511,245.992394174936,28.1183211976405)) ;
#105791 = CARTESIAN_POINT('Ctrl Pts',(64.9356062703199,245.97498719514,28.1121625030257)) ;
#105792 = CARTESIAN_POINT('Ctrl Pts',(64.928263675975,245.958729638151,28.1064243414529)) ;
#105793 = CARTESIAN_POINT('Ctrl Pts',(64.9206090302591,245.94178115467,28.1004423149597)) ;
#105794 = CARTESIAN_POINT('Ctrl Pts',(64.9095180038061,245.926399208258,28.095028961218)) ;
#105795 = CARTESIAN_POINT('Ctrl Pts',(64.8956136387304,245.913453339836,28.0904794283363)) ;
#105796 = CARTESIAN_POINT('Ctrl Pts',(64.8817129938792,245.900510935184,28.0859311127188)) ;
#105797 = CARTESIAN_POINT('Ctrl Pts',(64.8652664191736,245.890251001563,28.0823329269323)) ;
#105798 = CARTESIAN_POINT('Ctrl Pts',(64.8471986491033,245.883254040199,28.0798802263625)) ;
#105799 = CARTESIAN_POINT('Ctrl Pts',(64.8291331055125,245.876257941067,28.0774278280374)) ;
#105800 = CARTESIAN_POINT('Ctrl Pts',(64.8097925816883,245.872657996292,28.0761674639184)) ;
#105801 = CARTESIAN_POINT('Ctrl Pts',(64.7902651077865,245.872657996292,28.0761674639184)) ;
#105802 = CARTESIAN_POINT('',(64.7902651077865,246.718943174069,25.4715695045192)) ;
#105803 = CARTESIAN_POINT('Origin',(64.7902651077865,246.340671638724,28.252131183183)) ;
#105804 = CARTESIAN_POINT('',(64.9402651077865,246.678925224467,28.3420450960781)) ;
#105805 = CARTESIAN_POINT('Origin',(64.9402651077865,246.340671638724,28.252131183183)) ;
#105806 = CARTESIAN_POINT('',(64.7902651077865,246.822731508173,28.3848650607978)) ;
#105807 = CARTESIAN_POINT('Ctrl Pts',(64.9402651077865,246.678925224469,28.3420450960789)) ;
#105808 = CARTESIAN_POINT('Ctrl Pts',(64.9402651077865,246.680324229641,28.3424579870221)) ;
#105809 = CARTESIAN_POINT('Ctrl Pts',(64.9402438465509,246.681723125548,28.3428709748967)) ;
#105810 = CARTESIAN_POINT('Ctrl Pts',(64.9402013305491,246.683121466859,28.343283925702)) ;
#105811 = CARTESIAN_POINT('Ctrl Pts',(64.9396551395109,246.701085561798,28.3485889877857)) ;
#105812 = CARTESIAN_POINT('Ctrl Pts',(64.9356062703199,246.718788094141,28.3538380651884)) ;
#105813 = CARTESIAN_POINT('Ctrl Pts',(64.9282636759749,246.73531354078,28.3587517471959)) ;
#105814 = CARTESIAN_POINT('Ctrl Pts',(64.920609030259,246.752541298897,28.3638742547404)) ;
#105815 = CARTESIAN_POINT('Ctrl Pts',(64.9095180038064,246.768167444445,28.3685360408182)) ;
#105816 = CARTESIAN_POINT('Ctrl Pts',(64.8956136387306,246.781315020339,28.3724647819376)) ;
#105817 = CARTESIAN_POINT('Ctrl Pts',(64.8817129938792,246.794459078493,28.3763924718907)) ;
#105818 = CARTESIAN_POINT('Ctrl Pts',(64.8652664191735,246.804874499694,28.3795121161122)) ;
#105819 = CARTESIAN_POINT('Ctrl Pts',(64.8471986491031,246.811976821569,28.3816405503697)) ;
#105820 = CARTESIAN_POINT('Ctrl Pts',(64.8291331055123,246.81907826823,28.3837687223415)) ;
#105821 = CARTESIAN_POINT('Ctrl Pts',(64.8097925816884,246.822731508174,28.3848650607972)) ;
#105822 = CARTESIAN_POINT('Ctrl Pts',(64.7902651077865,246.822731508174,28.3848650607972)) ;
#105823 = CARTESIAN_POINT('Origin',(64.7902651077865,246.340671638724,28.252131183183)) ;
#105824 = CARTESIAN_POINT('Origin',(64.7902651077865,247.635028874288,25.3994606331908)) ;
#105825 = CARTESIAN_POINT('',(64.9402651077865,246.84682643861,27.8252982934377)) ;
#105826 = CARTESIAN_POINT('',(64.9402651077865,247.635028874288,25.3994606331908)) ;
#105827 = CARTESIAN_POINT('',(64.7902651077865,246.946891701628,28.0027392774284)) ;
#105828 = CARTESIAN_POINT('Ctrl Pts',(64.9402651077865,246.84682643861,27.8252982934377)) ;
#105829 = CARTESIAN_POINT('Ctrl Pts',(64.9402651077865,246.847209116357,27.8259879723329)) ;
#105830 = CARTESIAN_POINT('Ctrl Pts',(64.940261777681,246.847591853015,27.8266776249647)) ;
#105831 = CARTESIAN_POINT('Ctrl Pts',(64.9400834366348,246.857838938123,27.8451382901555)) ;
#105832 = CARTESIAN_POINT('Ctrl Pts',(64.9376982652992,246.867778654567,27.8629553331985)) ;
#105833 = CARTESIAN_POINT('Ctrl Pts',(64.9285249168188,246.886692158738,27.896699388929)) ;
#105834 = CARTESIAN_POINT('Ctrl Pts',(64.921887890589,246.895772989479,27.9128241441551)) ;
#105835 = CARTESIAN_POINT('Ctrl Pts',(64.9030518920066,246.913652858034,27.9444499271496)) ;
#105836 = CARTESIAN_POINT('Ctrl Pts',(64.890241559628,246.92239313214,27.9598318195758)) ;
#105837 = CARTESIAN_POINT('Ctrl Pts',(64.8622234505159,246.935114921148,27.9821554300886)) ;
#105838 = CARTESIAN_POINT('Ctrl Pts',(64.8483068832618,246.939674844702,27.9901316702288)) ;
#105839 = CARTESIAN_POINT('Ctrl Pts',(64.8193104176513,246.945446722844,28.0002186669547)) ;
#105840 = CARTESIAN_POINT('Ctrl Pts',(64.8049443310403,246.946891701628,28.0027392774284)) ;
#105841 = CARTESIAN_POINT('Ctrl Pts',(64.7902651077865,246.946891701628,28.0027392774284)) ;
#105842 = CARTESIAN_POINT('',(64.7902651077865,247.777687351732,25.445813182347)) ;
#105843 = CARTESIAN_POINT('Origin',(64.7902651077865,248.040265107786,23.0213203435596)) ;
#105844 = CARTESIAN_POINT('',(64.9402651077865,247.69078190379,27.9589677074491)) ;
#105845 = CARTESIAN_POINT('Origin',(64.9402651077865,248.040265107786,23.0213203435596)) ;
#105846 = CARTESIAN_POINT('',(64.7902651077865,247.54078190379,28.096802244712)) ;
#105847 = CARTESIAN_POINT('Ctrl Pts',(64.9402651077865,247.69078190379,27.9589677074491)) ;
#105848 = CARTESIAN_POINT('Ctrl Pts',(64.9402651077865,247.690204833126,27.9595053771295)) ;
#105849 = CARTESIAN_POINT('Ctrl Pts',(64.940261777681,247.68962771455,27.9600430036272)) ;
#105850 = CARTESIAN_POINT('Ctrl Pts',(64.9400834366348,247.674177498214,27.9744336161108)) ;
#105851 = CARTESIAN_POINT('Ctrl Pts',(64.9376982652992,247.659218497029,27.9883070896973)) ;
#105852 = CARTESIAN_POINT('Ctrl Pts',(64.9285249168187,247.630803198961,28.0145549995742)) ;
#105853 = CARTESIAN_POINT('Ctrl Pts',(64.9218878905889,247.617183992317,28.0270844220837)) ;
#105854 = CARTESIAN_POINT('Ctrl Pts',(64.9030518920067,247.590406322412,28.0516371458428)) ;
#105855 = CARTESIAN_POINT('Ctrl Pts',(64.890241559628,247.577340561604,28.0635653016335)) ;
#105856 = CARTESIAN_POINT('Ctrl Pts',(64.8622234505159,247.558343046244,28.0808650678764)) ;
#105857 = CARTESIAN_POINT('Ctrl Pts',(64.8483068832618,247.55154150748,28.087041829166)) ;
#105858 = CARTESIAN_POINT('Ctrl Pts',(64.8193104176513,247.542935071751,28.0948515246968)) ;
#105859 = CARTESIAN_POINT('Ctrl Pts',(64.8049443310403,247.54078190379,28.096802244712)) ;
#105860 = CARTESIAN_POINT('Ctrl Pts',(64.7902651077865,247.54078190379,28.096802244712)) ;
#105861 = CARTESIAN_POINT('Origin',(64.7902651077865,248.040265107786,23.0213203435596)) ;
#105862 = CARTESIAN_POINT('Origin',(64.7902651077865,247.69078190379,25.759956707196)) ;
#105863 = CARTESIAN_POINT('',(64.9402651077865,247.69078190379,28.5023074499214)) ;
#105864 = CARTESIAN_POINT('',(64.9402651077865,247.69078190379,25.759956707196)) ;
#105865 = CARTESIAN_POINT('',(64.7902651077865,247.54078190379,28.4985930708324)) ;
#105866 = CARTESIAN_POINT('Ctrl Pts',(64.9402651077865,247.69078190379,28.5023074499214)) ;
#105867 = CARTESIAN_POINT('Ctrl Pts',(64.9402651077865,247.689323780486,28.5022678161701)) ;
#105868 = CARTESIAN_POINT('Ctrl Pts',(64.940243846551,247.687865731145,28.5022283083713)) ;
#105869 = CARTESIAN_POINT('Ctrl Pts',(64.9402013305491,247.686408220711,28.5021889366962)) ;
#105870 = CARTESIAN_POINT('Ctrl Pts',(64.9396551395109,247.667683996822,28.5016831399336)) ;
#105871 = CARTESIAN_POINT('Ctrl Pts',(64.9356062703199,247.649225833959,28.5012049258669)) ;
#105872 = CARTESIAN_POINT('Ctrl Pts',(64.928263675975,247.631990789003,28.5007714713078)) ;
#105873 = CARTESIAN_POINT('Ctrl Pts',(64.9206090302591,247.6140232755,28.5003195954547)) ;
#105874 = CARTESIAN_POINT('Ctrl Pts',(64.9095180038061,247.597721356829,28.49992447295)) ;
#105875 = CARTESIAN_POINT('Ctrl Pts',(64.8956136387305,247.58400322133,28.4995981034064)) ;
#105876 = CARTESIAN_POINT('Ctrl Pts',(64.8817129938794,247.570288756228,28.4992718211856)) ;
#105877 = CARTESIAN_POINT('Ctrl Pts',(64.8652664191737,247.559419078944,28.4990202369966)) ;
#105878 = CARTESIAN_POINT('Ctrl Pts',(64.8471986491032,247.552006647086,28.4988497601076)) ;
#105879 = CARTESIAN_POINT('Ctrl Pts',(64.8291331055122,247.544595128658,28.4986793042264)) ;
#105880 = CARTESIAN_POINT('Ctrl Pts',(64.8097925816883,247.54078190379,28.4985930708322)) ;
#105881 = CARTESIAN_POINT('Ctrl Pts',(64.7902651077865,247.54078190379,28.4985930708322)) ;
#105882 = CARTESIAN_POINT('',(64.7902651077865,247.54078190379,25.759956707196)) ;
#105883 = CARTESIAN_POINT('Origin',(64.7902651077865,248.040265107786,28.5213203435596)) ;
#105884 = CARTESIAN_POINT('',(64.9402651077865,248.389748311783,28.5023074499214)) ;
#105885 = CARTESIAN_POINT('Origin',(64.9402651077865,248.040265107786,28.5213203435596)) ;
#105886 = CARTESIAN_POINT('',(64.7902651077865,248.539748311783,28.4985930708324)) ;
#105887 = CARTESIAN_POINT('Ctrl Pts',(64.9402651077865,248.389748311783,28.5023074499214)) ;
#105888 = CARTESIAN_POINT('Ctrl Pts',(64.9402651077865,248.391206435086,28.5022678161702)) ;
#105889 = CARTESIAN_POINT('Ctrl Pts',(64.940243846551,248.392664484427,28.5022283083715)) ;
#105890 = CARTESIAN_POINT('Ctrl Pts',(64.9402013305492,248.394121994861,28.5021889366964)) ;
#105891 = CARTESIAN_POINT('Ctrl Pts',(64.939655139511,248.412846218751,28.5016831399329)) ;
#105892 = CARTESIAN_POINT('Ctrl Pts',(64.9356062703199,248.431304381614,28.5012049258645)) ;
#105893 = CARTESIAN_POINT('Ctrl Pts',(64.9282636759751,248.44853942657,28.500771471306)) ;
#105894 = CARTESIAN_POINT('Ctrl Pts',(64.9206090302595,248.466506940072,28.5003195954534)) ;
#105895 = CARTESIAN_POINT('Ctrl Pts',(64.9095180038067,248.482808858743,28.4999244729504)) ;
#105896 = CARTESIAN_POINT('Ctrl Pts',(64.8956136387307,248.496526994243,28.4995981034069)) ;
#105897 = CARTESIAN_POINT('Ctrl Pts',(64.8817129938793,248.510241459345,28.4992718211861)) ;
#105898 = CARTESIAN_POINT('Ctrl Pts',(64.8652664191737,248.521111136629,28.4990202369969)) ;
#105899 = CARTESIAN_POINT('Ctrl Pts',(64.8471986491033,248.528523568487,28.4988497601079)) ;
#105900 = CARTESIAN_POINT('Ctrl Pts',(64.8291331055125,248.535935086915,28.4986793042266)) ;
#105901 = CARTESIAN_POINT('Ctrl Pts',(64.8097925816883,248.539748311783,28.4985930708331)) ;
#105902 = CARTESIAN_POINT('Ctrl Pts',(64.7902651077865,248.539748311783,28.4985930708331)) ;
#105903 = CARTESIAN_POINT('Origin',(64.7902651077865,248.040265107786,28.5213203435596)) ;
#105904 = CARTESIAN_POINT('Origin',(64.7902651077865,248.389748311783,25.4082910455649)) ;
#105905 = CARTESIAN_POINT('',(64.9402651077865,248.389748311783,27.9589677074491)) ;
#105906 = CARTESIAN_POINT('',(64.9402651077865,248.389748311783,25.4082910455649)) ;
#105907 = CARTESIAN_POINT('',(64.7902651077865,248.539748311783,28.096802244712)) ;
#105908 = CARTESIAN_POINT('Ctrl Pts',(64.9402651077865,248.389748311783,27.9589677074491)) ;
#105909 = CARTESIAN_POINT('Ctrl Pts',(64.9402651077865,248.390325382447,27.9595053771305)) ;
#105910 = CARTESIAN_POINT('Ctrl Pts',(64.940261777681,248.390902501024,27.9600430036291)) ;
#105911 = CARTESIAN_POINT('Ctrl Pts',(64.9400834366345,248.406352717361,27.974433616113)) ;
#105912 = CARTESIAN_POINT('Ctrl Pts',(64.9376982652987,248.421311718545,27.9883070896991)) ;
#105913 = CARTESIAN_POINT('Ctrl Pts',(64.9285249168183,248.449727016612,28.014554999575)) ;
#105914 = CARTESIAN_POINT('Ctrl Pts',(64.9218878905887,248.463346223256,28.027084422084)) ;
#105915 = CARTESIAN_POINT('Ctrl Pts',(64.9030518920067,248.490123893161,28.0516371458428)) ;
#105916 = CARTESIAN_POINT('Ctrl Pts',(64.890241559628,248.503189653969,28.0635653016335)) ;
#105917 = CARTESIAN_POINT('Ctrl Pts',(64.8622234505159,248.522187169328,28.0808650678765)) ;
#105918 = CARTESIAN_POINT('Ctrl Pts',(64.8483068832618,248.528988708093,28.087041829166)) ;
#105919 = CARTESIAN_POINT('Ctrl Pts',(64.8193104176513,248.537595143822,28.0948515246968)) ;
#105920 = CARTESIAN_POINT('Ctrl Pts',(64.8049443310403,248.539748311783,28.096802244712)) ;
#105921 = CARTESIAN_POINT('Ctrl Pts',(64.7902651077865,248.539748311783,28.096802244712)) ;
#105922 = CARTESIAN_POINT('',(64.7902651077865,248.539748311783,25.4082910455649)) ;
#105923 = CARTESIAN_POINT('Origin',(64.7902651077865,248.040265107786,23.0213203435596)) ;
#105924 = CARTESIAN_POINT('',(64.9402651077865,249.233703776962,27.8252982934377)) ;
#105925 = CARTESIAN_POINT('Origin',(64.9402651077865,248.040265107786,23.0213203435596)) ;
#105926 = CARTESIAN_POINT('',(64.7902651077865,249.133638513944,28.0027392774284)) ;
#105927 = CARTESIAN_POINT('Ctrl Pts',(64.9402651077865,249.233703776962,27.8252982934377)) ;
#105928 = CARTESIAN_POINT('Ctrl Pts',(64.9402651077865,249.233321099216,27.8259879723329)) ;
#105929 = CARTESIAN_POINT('Ctrl Pts',(64.940261777681,249.232938362558,27.8266776249647)) ;
#105930 = CARTESIAN_POINT('Ctrl Pts',(64.9400834366348,249.22269127745,27.8451382901554)) ;
#105931 = CARTESIAN_POINT('Ctrl Pts',(64.9376982652992,249.212751561005,27.8629553331984)) ;
#105932 = CARTESIAN_POINT('Ctrl Pts',(64.9285249168188,249.193838056834,27.896699388929)) ;
#105933 = CARTESIAN_POINT('Ctrl Pts',(64.921887890589,249.184757226094,27.9128241441551)) ;
#105934 = CARTESIAN_POINT('Ctrl Pts',(64.9030518920067,249.166877357539,27.9444499271496)) ;
#105935 = CARTESIAN_POINT('Ctrl Pts',(64.890241559628,249.158137083433,27.9598318195758)) ;
#105936 = CARTESIAN_POINT('Ctrl Pts',(64.8622234505159,249.145415294424,27.9821554300886)) ;
#105937 = CARTESIAN_POINT('Ctrl Pts',(64.8483068832618,249.14085537087,27.9901316702287)) ;
#105938 = CARTESIAN_POINT('Ctrl Pts',(64.8193104176513,249.135083492728,28.0002186669547)) ;
#105939 = CARTESIAN_POINT('Ctrl Pts',(64.8049443310403,249.133638513944,28.0027392774284)) ;
#105940 = CARTESIAN_POINT('Ctrl Pts',(64.7902651077865,249.133638513944,28.0027392774284)) ;
#105941 = CARTESIAN_POINT('Origin',(64.7902651077865,248.040265107786,23.0213203435596)) ;
#105942 = CARTESIAN_POINT('Origin',(64.7902651077865,248.554172007067,25.7339145522423)) ;
#105943 = CARTESIAN_POINT('',(64.9402651077865,249.401604991106,28.342045096078)) ;
#105944 = CARTESIAN_POINT('',(64.9402651077865,248.554172007067,25.7339145522423)) ;
#105945 = CARTESIAN_POINT('',(64.7902651077865,249.257798707399,28.3848650607978)) ;
#105946 = CARTESIAN_POINT('Ctrl Pts',(64.9402651077865,249.401604991106,28.342045096078)) ;
#105947 = CARTESIAN_POINT('Ctrl Pts',(64.9402651077865,249.400205985933,28.3424579870215)) ;
#105948 = CARTESIAN_POINT('Ctrl Pts',(64.940243846551,249.398807090025,28.3428709748967)) ;
#105949 = CARTESIAN_POINT('Ctrl Pts',(64.9402013305491,249.397408748713,28.3432839257022)) ;
#105950 = CARTESIAN_POINT('Ctrl Pts',(64.9396551395108,249.379444653775,28.3485889877849)) ;
#105951 = CARTESIAN_POINT('Ctrl Pts',(64.9356062703196,249.361742121431,28.3538380651888)) ;
#105952 = CARTESIAN_POINT('Ctrl Pts',(64.9282636759748,249.345216674792,28.3587517471961)) ;
#105953 = CARTESIAN_POINT('Ctrl Pts',(64.920609030259,249.327988916676,28.3638742547405)) ;
#105954 = CARTESIAN_POINT('Ctrl Pts',(64.909518003806,249.312362771127,28.368536040818)) ;
#105955 = CARTESIAN_POINT('Ctrl Pts',(64.8956136387302,249.299215195234,28.3724647819372)) ;
#105956 = CARTESIAN_POINT('Ctrl Pts',(64.8817129938788,249.286071137079,28.3763924718902)) ;
#105957 = CARTESIAN_POINT('Ctrl Pts',(64.8652664191736,249.275655715879,28.3795121161121)) ;
#105958 = CARTESIAN_POINT('Ctrl Pts',(64.8471986491032,249.268553394004,28.3816405503694)) ;
#105959 = CARTESIAN_POINT('Ctrl Pts',(64.8291331055125,249.261451947343,28.3837687223412)) ;
#105960 = CARTESIAN_POINT('Ctrl Pts',(64.8097925816883,249.257798707399,28.3848650607976)) ;
#105961 = CARTESIAN_POINT('Ctrl Pts',(64.7902651077865,249.257798707399,28.3848650607976)) ;
#105962 = CARTESIAN_POINT('',(64.7902651077865,248.411513529623,25.7802671013986)) ;
#105963 = CARTESIAN_POINT('Origin',(64.7902651077865,249.739858576849,28.252131183183)) ;
#105964 = CARTESIAN_POINT('',(64.9402651077865,250.066361548098,28.1260525975114)) ;
#105965 = CARTESIAN_POINT('Origin',(64.9402651077865,249.739858576849,28.252131183183)) ;
#105966 = CARTESIAN_POINT('',(64.7902651077865,250.207872219281,28.0761674639184)) ;
#105967 = CARTESIAN_POINT('Ctrl Pts',(64.9402651077865,250.066361548098,28.1260525975114)) ;
#105968 = CARTESIAN_POINT('Ctrl Pts',(64.9402651077865,250.067736058265,28.1255643186932)) ;
#105969 = CARTESIAN_POINT('Ctrl Pts',(64.940243846551,250.069110537011,28.1250761825189)) ;
#105970 = CARTESIAN_POINT('Ctrl Pts',(64.9402013305491,250.070484545289,28.1245883423371)) ;
#105971 = CARTESIAN_POINT('Ctrl Pts',(64.9396551395109,250.088136040636,28.1183211976397)) ;
#105972 = CARTESIAN_POINT('Ctrl Pts',(64.9356062703197,250.105543020433,28.112162503026)) ;
#105973 = CARTESIAN_POINT('Ctrl Pts',(64.9282636759749,250.121800577422,28.1064243414531)) ;
#105974 = CARTESIAN_POINT('Ctrl Pts',(64.9206090302592,250.138749060902,28.1004423149599)) ;
#105975 = CARTESIAN_POINT('Ctrl Pts',(64.9095180038062,250.154131007314,28.095028961218)) ;
#105976 = CARTESIAN_POINT('Ctrl Pts',(64.8956136387303,250.167076875737,28.0904794283365)) ;
#105977 = CARTESIAN_POINT('Ctrl Pts',(64.8817129938789,250.180019280389,28.085931112719)) ;
#105978 = CARTESIAN_POINT('Ctrl Pts',(64.8652664191733,250.190279214009,28.0823329269325)) ;
#105979 = CARTESIAN_POINT('Ctrl Pts',(64.847198649103,250.197276175373,28.0798802263628)) ;
#105980 = CARTESIAN_POINT('Ctrl Pts',(64.8291331055122,250.204272274506,28.0774278280377)) ;
#105981 = CARTESIAN_POINT('Ctrl Pts',(64.8097925816882,250.20787221928,28.0761674639187)) ;
#105982 = CARTESIAN_POINT('Ctrl Pts',(64.7902651077865,250.20787221928,28.0761674639188)) ;
#105983 = CARTESIAN_POINT('Origin',(64.7902651077865,249.739858576849,28.252131183183)) ;
#105984 = CARTESIAN_POINT('Origin',(64.7902651077865,249.110257898277,25.1834681346239)) ;
#105985 = CARTESIAN_POINT('',(64.9402651077865,249.898460333955,27.6093057948708)) ;
#105986 = CARTESIAN_POINT('',(64.9402651077865,249.110257898277,25.1834681346239)) ;
#105987 = CARTESIAN_POINT('',(64.7902651077865,250.083712025826,27.694041680549)) ;
#105988 = CARTESIAN_POINT('Ctrl Pts',(64.9402651077865,249.898460333955,27.6093057948708)) ;
#105989 = CARTESIAN_POINT('Ctrl Pts',(64.9402651077865,249.89917530984,27.6096388244826)) ;
#105990 = CARTESIAN_POINT('Ctrl Pts',(64.940261777681,249.899890317948,27.6099717982194)) ;
#105991 = CARTESIAN_POINT('Ctrl Pts',(64.9400834366345,249.91903129069,27.6188837045809)) ;
#105992 = CARTESIAN_POINT('Ctrl Pts',(64.9376982652987,249.937545285353,27.6274555764536)) ;
#105993 = CARTESIAN_POINT('Ctrl Pts',(64.9285249168183,249.97268088996,27.6436380121774)) ;
#105994 = CARTESIAN_POINT('Ctrl Pts',(64.9218878905887,249.98950532967,27.6513456347973)) ;
#105995 = CARTESIAN_POINT('Ctrl Pts',(64.9030518920066,250.022559616025,27.6664219076506)) ;
#105996 = CARTESIAN_POINT('Ctrl Pts',(64.890241559628,250.038671895832,27.6737287158085)) ;
#105997 = CARTESIAN_POINT('Ctrl Pts',(64.862223450516,250.062085528376,27.6843112161272)) ;
#105998 = CARTESIAN_POINT('Ctrl Pts',(64.8483068832619,250.070462900348,27.6880838741351)) ;
#105999 = CARTESIAN_POINT('Ctrl Pts',(64.8193104176514,250.08106143577,27.6928518010587)) ;
#106000 = CARTESIAN_POINT('Ctrl Pts',(64.8049443310404,250.083712025825,27.6940416805491)) ;
#106001 = CARTESIAN_POINT('Ctrl Pts',(64.7902651077866,250.083712025825,27.6940416805491)) ;
#106002 = CARTESIAN_POINT('',(64.7902651077865,249.252916375722,25.1371155854676)) ;
#106003 = CARTESIAN_POINT('Origin',(64.7902651077865,248.040265107786,23.0213203435596)) ;
#106004 = CARTESIAN_POINT('',(64.9402651077865,250.65980355802,27.2213820464098)) ;
#106005 = CARTESIAN_POINT('Origin',(64.9402651077865,248.040265107786,23.0213203435596)) ;
#106006 = CARTESIAN_POINT('',(64.7902651077865,250.619468117123,27.4210603173112)) ;
#106007 = CARTESIAN_POINT('Ctrl Pts',(64.9402651077865,250.65980355802,27.2213820464098)) ;
#106008 = CARTESIAN_POINT('Ctrl Pts',(64.9402651077865,250.659652732354,27.222156223949)) ;
#106009 = CARTESIAN_POINT('Ctrl Pts',(64.9402617776811,250.659501842545,27.2229303947088)) ;
#106010 = CARTESIAN_POINT('Ctrl Pts',(64.9400834366342,250.655460944751,27.2436540540784)) ;
#106011 = CARTESIAN_POINT('Ctrl Pts',(64.9376982652983,250.651513481746,27.2636706102647)) ;
#106012 = CARTESIAN_POINT('Ctrl Pts',(64.9285249168178,250.643953157038,27.3016077085626)) ;
#106013 = CARTESIAN_POINT('Ctrl Pts',(64.9218878905883,250.640299597185,27.3197493931144)) ;
#106014 = CARTESIAN_POINT('Ctrl Pts',(64.9030518920067,250.633067736091,27.3553524833538)) ;
#106015 = CARTESIAN_POINT('Ctrl Pts',(64.890241559628,250.629508507613,27.3726824256129)) ;
#106016 = CARTESIAN_POINT('Ctrl Pts',(64.8622234505159,250.624307742302,27.3978446898607)) ;
#106017 = CARTESIAN_POINT('Ctrl Pts',(64.8483068832619,250.622435791047,27.4068396388929)) ;
#106018 = CARTESIAN_POINT('Ctrl Pts',(64.8193104176513,250.620063462139,27.4182165512944)) ;
#106019 = CARTESIAN_POINT('Ctrl Pts',(64.8049443310403,250.619468117123,27.4210603173112)) ;
#106020 = CARTESIAN_POINT('Ctrl Pts',(64.7902651077865,250.619468117123,27.4210603173112)) ;
#106021 = CARTESIAN_POINT('Origin',(64.7902651077865,248.040265107786,23.0213203435596)) ;
#106022 = CARTESIAN_POINT('Origin',(64.7902651077865,249.367257322442,25.4423447763876)) ;
#106023 = CARTESIAN_POINT('',(64.9402651077865,250.979170645629,27.6609531317893)) ;
#106024 = CARTESIAN_POINT('',(64.9402651077865,249.367257322442,25.4423447763876)) ;
#106025 = CARTESIAN_POINT('',(64.7902651077865,250.855634839223,27.7461159238265)) ;
#106026 = CARTESIAN_POINT('Ctrl Pts',(64.9402651077865,250.979170645629,27.6609531317893)) ;
#106027 = CARTESIAN_POINT('Ctrl Pts',(64.9402651077865,250.977967702962,27.661778130785)) ;
#106028 = CARTESIAN_POINT('Ctrl Pts',(64.940243846551,250.976764894165,27.6626031882036)) ;
#106029 = CARTESIAN_POINT('Ctrl Pts',(64.9402013305491,250.975562601365,27.6634280389876)) ;
#106030 = CARTESIAN_POINT('Ctrl Pts',(64.9396551395109,250.960117086155,27.6740246634766)) ;
#106031 = CARTESIAN_POINT('Ctrl Pts',(64.9356062703198,250.944903031536,27.6844872160811)) ;
#106032 = CARTESIAN_POINT('Ctrl Pts',(64.928263675975,250.93070480907,27.6942670492246)) ;
#106033 = CARTESIAN_POINT('Ctrl Pts',(64.9206090302591,250.915903179338,27.7044625134376)) ;
#106034 = CARTESIAN_POINT('Ctrl Pts',(64.9095180038061,250.902482402912,27.7137248799966)) ;
#106035 = CARTESIAN_POINT('Ctrl Pts',(64.8956136387304,250.891192362958,27.721524159225)) ;
#106036 = CARTESIAN_POINT('Ctrl Pts',(64.8817129938793,250.879905343744,27.7293213516936)) ;
#106037 = CARTESIAN_POINT('Ctrl Pts',(64.8652664191737,250.870963712622,27.7355068518136)) ;
#106038 = CARTESIAN_POINT('Ctrl Pts',(64.8471986491032,250.864866725478,27.7397258512424)) ;
#106039 = CARTESIAN_POINT('Ctrl Pts',(64.8291331055123,250.858770489662,27.7439443307667)) ;
#106040 = CARTESIAN_POINT('Ctrl Pts',(64.8097925816884,250.855634839223,27.7461159238267)) ;
#106041 = CARTESIAN_POINT('Ctrl Pts',(64.7902651077866,250.855634839223,27.7461159238267)) ;
#106042 = CARTESIAN_POINT('',(64.7902651077865,249.245904773286,25.5305125642315)) ;
#106043 = CARTESIAN_POINT('Origin',(64.7902651077865,251.273083995395,27.4709138126218)) ;
#106044 = CARTESIAN_POINT('',(64.9402651077865,251.544646348192,27.2501109853232)) ;
#106045 = CARTESIAN_POINT('Origin',(64.9402651077865,251.273083995395,27.4709138126218)) ;
#106046 = CARTESIAN_POINT('',(64.7902651077865,251.663815640099,27.1589382016729)) ;
#106047 = CARTESIAN_POINT('Ctrl Pts',(64.9402651077865,251.544646348192,27.2501109853233)) ;
#106048 = CARTESIAN_POINT('Ctrl Pts',(64.9402651077865,251.545802698591,27.2492218575708)) ;
#106049 = CARTESIAN_POINT('Ctrl Pts',(64.940243846551,251.546959063183,27.2483328751889)) ;
#106050 = CARTESIAN_POINT('Ctrl Pts',(64.9402013305491,251.548115071804,27.2474443196972)) ;
#106051 = CARTESIAN_POINT('Ctrl Pts',(64.9396551395109,251.562965987268,27.2360292988668)) ;
#106052 = CARTESIAN_POINT('Ctrl Pts',(64.9356062703198,251.577617867525,27.2247929796351)) ;
#106053 = CARTESIAN_POINT('Ctrl Pts',(64.928263675975,251.591306533596,27.2143118022833)) ;
#106054 = CARTESIAN_POINT('Ctrl Pts',(64.9206090302591,251.605576951405,27.203385187582)) ;
#106055 = CARTESIAN_POINT('Ctrl Pts',(64.9095180038061,251.61853323347,27.1934834993828)) ;
#106056 = CARTESIAN_POINT('Ctrl Pts',(64.8956136387304,251.629439603015,27.1851561431399)) ;
#106057 = CARTESIAN_POINT('Ctrl Pts',(64.8817129938793,251.640343054474,27.1768310149481)) ;
#106058 = CARTESIAN_POINT('Ctrl Pts',(64.8652664191738,251.648988930644,27.1702384430593)) ;
#106059 = CARTESIAN_POINT('Ctrl Pts',(64.8471986491033,251.654885510185,27.1657436062294)) ;
#106060 = CARTESIAN_POINT('Ctrl Pts',(64.8291331055125,251.660781363094,27.1612493232952)) ;
#106061 = CARTESIAN_POINT('Ctrl Pts',(64.8097925816883,251.663815640098,27.1589382016717)) ;
#106062 = CARTESIAN_POINT('Ctrl Pts',(64.7902651077865,251.663815640098,27.1589382016716)) ;
#106063 = CARTESIAN_POINT('Origin',(64.7902651077865,251.273083995395,27.4709138126218)) ;
#106064 = CARTESIAN_POINT('Origin',(64.7902651077865,249.726029135361,24.746999133324)) ;
#106065 = CARTESIAN_POINT('',(64.9402651077865,251.225279260583,26.8105398999439)) ;
#106066 = CARTESIAN_POINT('',(64.9402651077865,249.726029135361,24.746999133324)) ;
#106067 = CARTESIAN_POINT('',(64.7902651077865,251.427648917999,26.8338825951576)) ;
#106068 = CARTESIAN_POINT('Ctrl Pts',(64.9402651077865,251.225279260583,26.8105398999439)) ;
#106069 = CARTESIAN_POINT('Ctrl Pts',(64.9402651077865,251.226062154865,26.8106356902272)) ;
#106070 = CARTESIAN_POINT('Ctrl Pts',(64.940261777681,251.226845062528,26.8107314174126)) ;
#106071 = CARTESIAN_POINT('Ctrl Pts',(64.9400834366348,251.247803139901,26.8132922581638)) ;
#106072 = CARTESIAN_POINT('Ctrl Pts',(64.9376982652992,251.26805984925,26.815723453781)) ;
#106073 = CARTESIAN_POINT('Ctrl Pts',(64.9285249168187,251.306476442616,26.8202563657946)) ;
#106074 = CARTESIAN_POINT('Ctrl Pts',(64.9218878905889,251.324859222012,26.8223877127212)) ;
#106075 = CARTESIAN_POINT('Ctrl Pts',(64.9030518920067,251.360954540964,26.8265117640394)) ;
#106076 = CARTESIAN_POINT('Ctrl Pts',(64.890241559628,251.378536157563,26.8284819832727)) ;
#106077 = CARTESIAN_POINT('Ctrl Pts',(64.8622234505159,251.404074017806,26.8313113288033)) ;
#106078 = CARTESIAN_POINT('Ctrl Pts',(64.8483068832618,251.413207187447,26.832310589478)) ;
#106079 = CARTESIAN_POINT('Ctrl Pts',(64.8193104176513,251.42476036407,26.8335700298871)) ;
#106080 = CARTESIAN_POINT('Ctrl Pts',(64.8049443310403,251.427648917999,26.8338825951576)) ;
#106081 = CARTESIAN_POINT('Ctrl Pts',(64.7902651077865,251.427648917999,26.8338825951576)) ;
#106082 = CARTESIAN_POINT('',(64.7902651077865,249.847381684517,24.6588313454802)) ;
#106083 = CARTESIAN_POINT('Origin',(64.7902651077865,248.040265107786,23.0213203435596)) ;
#106084 = CARTESIAN_POINT('',(64.9402651077865,251.829484664171,26.2063344963563)) ;
#106085 = CARTESIAN_POINT('Origin',(64.9402651077865,248.040265107786,23.0213203435596)) ;
#106086 = CARTESIAN_POINT('',(64.7902651077865,251.852827359384,26.4087041537722)) ;
#106087 = CARTESIAN_POINT('Ctrl Pts',(64.9402651077865,251.829484664171,26.2063344963563)) ;
#106088 = CARTESIAN_POINT('Ctrl Pts',(64.9402651077865,251.829580454454,26.2071173906402)) ;
#106089 = CARTESIAN_POINT('Ctrl Pts',(64.940261777681,251.82967618164,26.2079002983041)) ;
#106090 = CARTESIAN_POINT('Ctrl Pts',(64.9400834366345,251.832237022391,26.2288583756769)) ;
#106091 = CARTESIAN_POINT('Ctrl Pts',(64.9376982652987,251.834668218008,26.2491150850258)) ;
#106092 = CARTESIAN_POINT('Ctrl Pts',(64.9285249168183,251.839201130021,26.2875316783904)) ;
#106093 = CARTESIAN_POINT('Ctrl Pts',(64.9218878905886,251.841332476948,26.3059144577855)) ;
#106094 = CARTESIAN_POINT('Ctrl Pts',(64.9030518920066,251.845456528266,26.3420097767375)) ;
#106095 = CARTESIAN_POINT('Ctrl Pts',(64.8902415596279,251.847426747499,26.3595913933363)) ;
#106096 = CARTESIAN_POINT('Ctrl Pts',(64.862223450516,251.85025609303,26.3851292535788)) ;
#106097 = CARTESIAN_POINT('Ctrl Pts',(64.8483068832619,251.851255353705,26.3942624232203)) ;
#106098 = CARTESIAN_POINT('Ctrl Pts',(64.8193104176513,251.852514794114,26.4058155998437)) ;
#106099 = CARTESIAN_POINT('Ctrl Pts',(64.8049443310403,251.852827359384,26.4087041537722)) ;
#106100 = CARTESIAN_POINT('Ctrl Pts',(64.7902651077865,251.852827359384,26.4087041537722)) ;
#106101 = CARTESIAN_POINT('Origin',(64.7902651077865,248.040265107786,23.0213203435596)) ;
#106102 = CARTESIAN_POINT('Origin',(64.7902651077865,250.050447394148,24.9137882607786)) ;
#106103 = CARTESIAN_POINT('',(64.9402651077865,252.26905574955,26.5257015839661)) ;
#106104 = CARTESIAN_POINT('',(64.9402651077865,250.050447394148,24.9137882607786)) ;
#106105 = CARTESIAN_POINT('',(64.7902651077865,252.1778829659,26.6448708758722)) ;
#106106 = CARTESIAN_POINT('Ctrl Pts',(64.9402651077865,252.26905574955,26.5257015839661)) ;
#106107 = CARTESIAN_POINT('Ctrl Pts',(64.9402651077865,252.268166621798,26.5268579343644)) ;
#106108 = CARTESIAN_POINT('Ctrl Pts',(64.940243846551,252.267277639417,26.5280142989575)) ;
#106109 = CARTESIAN_POINT('Ctrl Pts',(64.9402013305492,252.266389083925,26.5291703075781)) ;
#106110 = CARTESIAN_POINT('Ctrl Pts',(64.9396551395109,252.254974063088,26.544021223037)) ;
#106111 = CARTESIAN_POINT('Ctrl Pts',(64.9356062703198,252.243737743861,26.558673103298)) ;
#106112 = CARTESIAN_POINT('Ctrl Pts',(64.928263675975,252.233256566509,26.5723617693692)) ;
#106113 = CARTESIAN_POINT('Ctrl Pts',(64.9206090302592,252.222329951808,26.5866321871775)) ;
#106114 = CARTESIAN_POINT('Ctrl Pts',(64.9095180038065,252.21242826361,26.5995884692432)) ;
#106115 = CARTESIAN_POINT('Ctrl Pts',(64.8956136387306,252.204100907367,26.6104948387888)) ;
#106116 = CARTESIAN_POINT('Ctrl Pts',(64.8817129938792,252.195775779175,26.6213982902478)) ;
#106117 = CARTESIAN_POINT('Ctrl Pts',(64.8652664191737,252.189183207286,26.6300441664177)) ;
#106118 = CARTESIAN_POINT('Ctrl Pts',(64.8471986491032,252.184688370456,26.6359407459586)) ;
#106119 = CARTESIAN_POINT('Ctrl Pts',(64.8291331055124,252.180194087522,26.6418365988679)) ;
#106120 = CARTESIAN_POINT('Ctrl Pts',(64.8097925816884,252.1778829659,26.6448708758726)) ;
#106121 = CARTESIAN_POINT('Ctrl Pts',(64.7902651077865,252.1778829659,26.6448708758726)) ;
#106122 = CARTESIAN_POINT('',(64.7902651077865,249.962279606305,25.0351408099348)) ;
#106123 = CARTESIAN_POINT('Origin',(64.7902651077865,252.489858576849,26.2541392311682)) ;
#106124 = CARTESIAN_POINT('',(64.9402651077865,252.679897896016,25.9602258814027)) ;
#106125 = CARTESIAN_POINT('Origin',(64.9402651077865,252.489858576849,26.2541392311682)) ;
#106126 = CARTESIAN_POINT('',(64.7902651077865,252.765060688053,25.8366900749965)) ;
#106127 = CARTESIAN_POINT('Ctrl Pts',(64.9402651077865,252.67989789602,25.9602258813973)) ;
#106128 = CARTESIAN_POINT('Ctrl Pts',(64.9402651077864,252.680722895014,25.9590229387317)) ;
#106129 = CARTESIAN_POINT('Ctrl Pts',(64.9402438465509,252.68154795243,25.957820129936)) ;
#106130 = CARTESIAN_POINT('Ctrl Pts',(64.9402013305492,252.682372803213,25.9566178371377)) ;
#106131 = CARTESIAN_POINT('Ctrl Pts',(64.9396551395109,252.692969427709,25.9411723219305)) ;
#106132 = CARTESIAN_POINT('Ctrl Pts',(64.9356062703198,252.703431980308,25.9259582673091)) ;
#106133 = CARTESIAN_POINT('Ctrl Pts',(64.928263675975,252.713211813452,25.9117600448439)) ;
#106134 = CARTESIAN_POINT('Ctrl Pts',(64.9206090302592,252.723407277665,25.8969584151117)) ;
#106135 = CARTESIAN_POINT('Ctrl Pts',(64.9095180038063,252.732669644223,25.8835376386852)) ;
#106136 = CARTESIAN_POINT('Ctrl Pts',(64.8956136387305,252.740468923451,25.8722475987305)) ;
#106137 = CARTESIAN_POINT('Ctrl Pts',(64.8817129938792,252.74826611592,25.8609605795167)) ;
#106138 = CARTESIAN_POINT('Ctrl Pts',(64.8652664191738,252.75445161604,25.8520189483948)) ;
#106139 = CARTESIAN_POINT('Ctrl Pts',(64.8471986491033,252.758670615469,25.8459219612514)) ;
#106140 = CARTESIAN_POINT('Ctrl Pts',(64.8291331055124,252.762889094994,25.8398257254358)) ;
#106141 = CARTESIAN_POINT('Ctrl Pts',(64.8097925816883,252.765060688054,25.8366900749968)) ;
#106142 = CARTESIAN_POINT('Ctrl Pts',(64.7902651077865,252.765060688054,25.8366900749968)) ;
#106143 = CARTESIAN_POINT('Origin',(64.7902651077865,252.489858576849,26.2541392311682)) ;
#106144 = CARTESIAN_POINT('Origin',(64.7902651077865,250.176786044017,24.1416086685709)) ;
#106145 = CARTESIAN_POINT('',(64.9402651077865,252.240326810636,25.6408587937931)) ;
#106146 = CARTESIAN_POINT('',(64.9402651077865,250.176786044017,24.1416086685709)) ;
#106147 = CARTESIAN_POINT('',(64.7902651077865,252.440005081538,25.6005233528965)) ;
#106148 = CARTESIAN_POINT('Ctrl Pts',(64.9402651077865,252.240326810636,25.6408587937931)) ;
#106149 = CARTESIAN_POINT('Ctrl Pts',(64.9402651077865,252.241100988176,25.6407079681271)) ;
#106150 = CARTESIAN_POINT('Ctrl Pts',(64.9402617776811,252.241875158935,25.6405570783181)) ;
#106151 = CARTESIAN_POINT('Ctrl Pts',(64.9400834366342,252.262598818305,25.6365161805235)) ;
#106152 = CARTESIAN_POINT('Ctrl Pts',(64.9376982652982,252.282615374491,25.6325687175188)) ;
#106153 = CARTESIAN_POINT('Ctrl Pts',(64.9285249168178,252.320552472789,25.6250083928117)) ;
#106154 = CARTESIAN_POINT('Ctrl Pts',(64.9218878905884,252.338694157341,25.6213548329578)) ;
#106155 = CARTESIAN_POINT('Ctrl Pts',(64.9030518920066,252.374297247581,25.6141229718641)) ;
#106156 = CARTESIAN_POINT('Ctrl Pts',(64.8902415596279,252.39162718984,25.6105637433868)) ;
#106157 = CARTESIAN_POINT('Ctrl Pts',(64.8622234505159,252.416789454087,25.6053629780756)) ;
#106158 = CARTESIAN_POINT('Ctrl Pts',(64.8483068832619,252.42578440312,25.6034910268201)) ;
#106159 = CARTESIAN_POINT('Ctrl Pts',(64.8193104176513,252.437161315521,25.6011186979124)) ;
#106160 = CARTESIAN_POINT('Ctrl Pts',(64.8049443310403,252.440005081538,25.6005233528966)) ;
#106161 = CARTESIAN_POINT('Ctrl Pts',(64.7902651077865,252.440005081538,25.6005233528966)) ;
#106162 = CARTESIAN_POINT('',(64.7902651077865,250.26495383186,24.0202561194147)) ;
#106163 = CARTESIAN_POINT('Origin',(64.7902651077865,248.040265107786,23.0213203435596)) ;
#106164 = CARTESIAN_POINT('',(64.9402651077865,252.628250559098,24.8795155697285)) ;
#106165 = CARTESIAN_POINT('Origin',(64.9402651077865,248.040265107786,23.0213203435596)) ;
#106166 = CARTESIAN_POINT('',(64.7902651077865,252.712986444776,25.0647672615988)) ;
#106167 = CARTESIAN_POINT('Ctrl Pts',(64.9402651077865,252.628250559098,24.8795155697285)) ;
#106168 = CARTESIAN_POINT('Ctrl Pts',(64.9402651077865,252.628583588709,24.8802305456133)) ;
#106169 = CARTESIAN_POINT('Ctrl Pts',(64.940261777681,252.628916562446,24.8809455537216)) ;
#106170 = CARTESIAN_POINT('Ctrl Pts',(64.9400834366345,252.637828468808,24.9000865264628)) ;
#106171 = CARTESIAN_POINT('Ctrl Pts',(64.9376982652988,252.64640034068,24.9186005211264)) ;
#106172 = CARTESIAN_POINT('Ctrl Pts',(64.9285249168184,252.662582776404,24.9537361257334)) ;
#106173 = CARTESIAN_POINT('Ctrl Pts',(64.9218878905887,252.670290399024,24.9705605654437)) ;
#106174 = CARTESIAN_POINT('Ctrl Pts',(64.9030518920066,252.685366671877,25.0036148517979)) ;
#106175 = CARTESIAN_POINT('Ctrl Pts',(64.8902415596279,252.692673480035,25.0197271316054)) ;
#106176 = CARTESIAN_POINT('Ctrl Pts',(64.8622234505159,252.703255980354,25.0431407641494)) ;
#106177 = CARTESIAN_POINT('Ctrl Pts',(64.8483068832618,252.707028638362,25.051518136121)) ;
#106178 = CARTESIAN_POINT('Ctrl Pts',(64.8193104176513,252.711796565285,25.0621166715429)) ;
#106179 = CARTESIAN_POINT('Ctrl Pts',(64.8049443310403,252.712986444776,25.0647672615988)) ;
#106180 = CARTESIAN_POINT('Ctrl Pts',(64.7902651077865,252.712986444776,25.0647672615988)) ;
#106181 = CARTESIAN_POINT('Origin',(64.7902651077865,248.040265107786,23.0213203435596)) ;
#106182 = CARTESIAN_POINT('Origin',(64.7902651077865,250.536866817902,24.1999837998328)) ;
#106183 = CARTESIAN_POINT('',(64.9402651077865,253.144997361738,25.0474167838718)) ;
#106184 = CARTESIAN_POINT('',(64.9402651077865,250.536866817902,24.1999837998328)) ;
#106185 = CARTESIAN_POINT('',(64.7902651077865,253.095112228145,25.188927455054)) ;
#106186 = CARTESIAN_POINT('Ctrl Pts',(64.9402651077865,253.144997361738,25.0474167838718)) ;
#106187 = CARTESIAN_POINT('Ctrl Pts',(64.9402651077865,253.14450908292,25.0487912940387)) ;
#106188 = CARTESIAN_POINT('Ctrl Pts',(64.940243846551,253.144020946746,25.0501657727844)) ;
#106189 = CARTESIAN_POINT('Ctrl Pts',(64.9402013305491,253.143533106564,25.0515397810629)) ;
#106190 = CARTESIAN_POINT('Ctrl Pts',(64.9396551395109,253.137265961864,25.0691912764082)) ;
#106191 = CARTESIAN_POINT('Ctrl Pts',(64.9356062703198,253.131107267253,25.0865982562063)) ;
#106192 = CARTESIAN_POINT('Ctrl Pts',(64.928263675975,253.12536910568,25.1028558131956)) ;
#106193 = CARTESIAN_POINT('Ctrl Pts',(64.9206090302592,253.119387079187,25.1198042966758)) ;
#106194 = CARTESIAN_POINT('Ctrl Pts',(64.9095180038063,253.113973725445,25.1351862430875)) ;
#106195 = CARTESIAN_POINT('Ctrl Pts',(64.8956136387304,253.109424192563,25.1481321115103)) ;
#106196 = CARTESIAN_POINT('Ctrl Pts',(64.8817129938791,253.104875876945,25.161074516162)) ;
#106197 = CARTESIAN_POINT('Ctrl Pts',(64.8652664191736,253.101277691159,25.1713344497829)) ;
#106198 = CARTESIAN_POINT('Ctrl Pts',(64.8471986491031,253.098824990589,25.1783314111465)) ;
#106199 = CARTESIAN_POINT('Ctrl Pts',(64.8291331055122,253.096372592264,25.1853275102792)) ;
#106200 = CARTESIAN_POINT('Ctrl Pts',(64.8097925816883,253.095112228145,25.1889274550539)) ;
#106201 = CARTESIAN_POINT('Ctrl Pts',(64.7902651077865,253.095112228145,25.1889274550539)) ;
#106202 = CARTESIAN_POINT('',(64.7902651077865,250.490514268746,24.3426422772771)) ;
#106203 = CARTESIAN_POINT('Origin',(64.7902651077865,253.27107594741,24.7209138126218)) ;
#106204 = CARTESIAN_POINT('',(64.9402651077865,253.360989860305,24.382660226879)) ;
#106205 = CARTESIAN_POINT('Origin',(64.9402651077865,253.27107594741,24.7209138126218)) ;
#106206 = CARTESIAN_POINT('',(64.7902651077865,253.403809825024,24.2388539431727)) ;
#106207 = CARTESIAN_POINT('Ctrl Pts',(64.9402651077865,253.360989860307,24.3826602268732)) ;
#106208 = CARTESIAN_POINT('Ctrl Pts',(64.9402651077864,253.36140275125,24.3812612217023)) ;
#106209 = CARTESIAN_POINT('Ctrl Pts',(64.9402438465509,253.361815739121,24.3798623257963)) ;
#106210 = CARTESIAN_POINT('Ctrl Pts',(64.9402013305491,253.362228689927,24.3784639844859)) ;
#106211 = CARTESIAN_POINT('Ctrl Pts',(64.9396551395108,253.367533752025,24.3604998895503)) ;
#106212 = CARTESIAN_POINT('Ctrl Pts',(64.9356062703196,253.372782829414,24.3427973572038)) ;
#106213 = CARTESIAN_POINT('Ctrl Pts',(64.9282636759748,253.377696511422,24.3262719105652)) ;
#106214 = CARTESIAN_POINT('Ctrl Pts',(64.9206090302591,253.382819018967,24.3090441524495)) ;
#106215 = CARTESIAN_POINT('Ctrl Pts',(64.9095180038062,253.387480805045,24.2934180069007)) ;
#106216 = CARTESIAN_POINT('Ctrl Pts',(64.8956136387303,253.391409546165,24.2802704310071)) ;
#106217 = CARTESIAN_POINT('Ctrl Pts',(64.8817129938789,253.395337236118,24.2671263728531)) ;
#106218 = CARTESIAN_POINT('Ctrl Pts',(64.8652664191735,253.39845688034,24.2567109516527)) ;
#106219 = CARTESIAN_POINT('Ctrl Pts',(64.8471986491031,253.400585314597,24.2496086297771)) ;
#106220 = CARTESIAN_POINT('Ctrl Pts',(64.8291331055124,253.402713486568,24.2425071831161)) ;
#106221 = CARTESIAN_POINT('Ctrl Pts',(64.8097925816883,253.403809825025,24.238853943173)) ;
#106222 = CARTESIAN_POINT('Ctrl Pts',(64.7902651077865,253.403809825025,24.238853943173)) ;
#106223 = CARTESIAN_POINT('Origin',(64.7902651077865,253.27107594741,24.7209138126218)) ;
#106224 = CARTESIAN_POINT('Origin',(64.7902651077865,250.418405397417,23.426556577058)) ;
#106225 = CARTESIAN_POINT('',(64.9402651077865,252.844243057664,24.2147590127358)) ;
#106226 = CARTESIAN_POINT('',(64.9402651077865,250.418405397417,23.426556577058)) ;
#106227 = CARTESIAN_POINT('',(64.7902651077865,253.021684041655,24.1146937497175)) ;
#106228 = CARTESIAN_POINT('Ctrl Pts',(64.9402651077865,252.844243057664,24.2147590127358)) ;
#106229 = CARTESIAN_POINT('Ctrl Pts',(64.9402651077865,252.844932736563,24.2143763349877)) ;
#106230 = CARTESIAN_POINT('Ctrl Pts',(64.9402617776811,252.845622389192,24.213993598331)) ;
#106231 = CARTESIAN_POINT('Ctrl Pts',(64.9400834366345,252.864083054386,24.2037465132207)) ;
#106232 = CARTESIAN_POINT('Ctrl Pts',(64.9376982652987,252.881900097428,24.1938067967769)) ;
#106233 = CARTESIAN_POINT('Ctrl Pts',(64.9285249168183,252.915644153157,24.1748932926068)) ;
#106234 = CARTESIAN_POINT('Ctrl Pts',(64.9218878905886,252.931768908382,24.1658124618668)) ;
#106235 = CARTESIAN_POINT('Ctrl Pts',(64.9030518920066,252.963394691376,24.1479325933121)) ;
#106236 = CARTESIAN_POINT('Ctrl Pts',(64.8902415596279,252.978776583803,24.1391923192062)) ;
#106237 = CARTESIAN_POINT('Ctrl Pts',(64.8622234505159,253.001100194315,24.1264705301978)) ;
#106238 = CARTESIAN_POINT('Ctrl Pts',(64.8483068832618,253.009076434455,24.1219106066435)) ;
#106239 = CARTESIAN_POINT('Ctrl Pts',(64.8193104176514,253.019163431181,24.1161387285016)) ;
#106240 = CARTESIAN_POINT('Ctrl Pts',(64.8049443310404,253.021684041655,24.1146937497175)) ;
#106241 = CARTESIAN_POINT('Ctrl Pts',(64.7902651077865,253.021684041655,24.1146937497175)) ;
#106242 = CARTESIAN_POINT('',(64.7902651077865,250.464757946574,23.2838980996137)) ;
#106243 = CARTESIAN_POINT('Origin',(64.7902651077865,248.040265107786,23.0213203435596)) ;
#106244 = CARTESIAN_POINT('',(64.9402651077865,252.977912471676,23.3708035475559)) ;
#106245 = CARTESIAN_POINT('Origin',(64.9402651077865,248.040265107786,23.0213203435596)) ;
#106246 = CARTESIAN_POINT('',(64.7902651077865,253.115747008939,23.5208035475559)) ;
#106247 = CARTESIAN_POINT('Ctrl Pts',(64.9402651077865,252.977912471676,23.3708035475559)) ;
#106248 = CARTESIAN_POINT('Ctrl Pts',(64.9402651077865,252.978450141357,23.3713806182205)) ;
#106249 = CARTESIAN_POINT('Ctrl Pts',(64.940261777681,252.978987767856,23.3719577367977)) ;
#106250 = CARTESIAN_POINT('Ctrl Pts',(64.9400834366345,252.99337838034,23.3874079531344)) ;
#106251 = CARTESIAN_POINT('Ctrl Pts',(64.9376982652987,253.007251853926,23.4023669543188)) ;
#106252 = CARTESIAN_POINT('Ctrl Pts',(64.9285249168183,253.033499763802,23.4307822523852)) ;
#106253 = CARTESIAN_POINT('Ctrl Pts',(64.9218878905887,253.046029186311,23.4444014590288)) ;
#106254 = CARTESIAN_POINT('Ctrl Pts',(64.9030518920067,253.070581910069,23.4711791289338)) ;
#106255 = CARTESIAN_POINT('Ctrl Pts',(64.890241559628,253.08251006586,23.4842448897418)) ;
#106256 = CARTESIAN_POINT('Ctrl Pts',(64.8622234505159,253.099809832103,23.5032424051016)) ;
#106257 = CARTESIAN_POINT('Ctrl Pts',(64.8483068832618,253.105986593393,23.5100439438662)) ;
#106258 = CARTESIAN_POINT('Ctrl Pts',(64.8193104176514,253.113796288923,23.5186503795949)) ;
#106259 = CARTESIAN_POINT('Ctrl Pts',(64.8049443310404,253.115747008939,23.5208035475559)) ;
#106260 = CARTESIAN_POINT('Ctrl Pts',(64.7902651077866,253.115747008939,23.5208035475559)) ;
#106261 = CARTESIAN_POINT('Origin',(64.7902651077865,248.040265107786,23.0213203435596)) ;
#106262 = CARTESIAN_POINT('Origin',(64.7902651077865,250.778901471423,23.3708035475559)) ;
#106263 = CARTESIAN_POINT('',(64.9402651077865,253.521252214148,23.3708035475559)) ;
#106264 = CARTESIAN_POINT('',(64.9402651077865,250.778901471423,23.3708035475559)) ;
#106265 = CARTESIAN_POINT('',(64.7902651077865,253.517537835059,23.5208035475559)) ;
#106266 = CARTESIAN_POINT('Ctrl Pts',(64.9402651077865,253.521252214148,23.3708035475559)) ;
#106267 = CARTESIAN_POINT('Ctrl Pts',(64.9402651077865,253.521212580397,23.3722616708597)) ;
#106268 = CARTESIAN_POINT('Ctrl Pts',(64.940243846551,253.521173072598,23.3737197202007)) ;
#106269 = CARTESIAN_POINT('Ctrl Pts',(64.9402013305491,253.521133700923,23.3751772306343)) ;
#106270 = CARTESIAN_POINT('Ctrl Pts',(64.9396551395109,253.52062790416,23.3939014545241)) ;
#106271 = CARTESIAN_POINT('Ctrl Pts',(64.9356062703198,253.520149690092,23.4123596173871)) ;
#106272 = CARTESIAN_POINT('Ctrl Pts',(64.928263675975,253.519716235533,23.4295946623432)) ;
#106273 = CARTESIAN_POINT('Ctrl Pts',(64.9206090302592,253.51926435968,23.4475621758456)) ;
#106274 = CARTESIAN_POINT('Ctrl Pts',(64.9095180038063,253.518869237177,23.4638640945167)) ;
#106275 = CARTESIAN_POINT('Ctrl Pts',(64.8956136387304,253.518542867634,23.4775822300162)) ;
#106276 = CARTESIAN_POINT('Ctrl Pts',(64.8817129938792,253.518216585413,23.4912966951183)) ;
#106277 = CARTESIAN_POINT('Ctrl Pts',(64.8652664191737,253.517965001223,23.5021663724021)) ;
#106278 = CARTESIAN_POINT('Ctrl Pts',(64.8471986491033,253.517794524334,23.5095788042594)) ;
#106279 = CARTESIAN_POINT('Ctrl Pts',(64.8291331055124,253.517624068453,23.5169903226877)) ;
#106280 = CARTESIAN_POINT('Ctrl Pts',(64.8097925816883,253.517537835059,23.5208035475559)) ;
#106281 = CARTESIAN_POINT('Ctrl Pts',(64.7902651077866,253.517537835059,23.5208035475559)) ;
#106282 = CARTESIAN_POINT('',(64.7902651077865,250.778901471423,23.5208035475559)) ;
#106283 = CARTESIAN_POINT('Origin',(64.7902651077865,253.540265107786,23.0213203435596)) ;
#106284 = CARTESIAN_POINT('',(64.9402651077865,253.521252214148,22.6718371395634)) ;
#106285 = CARTESIAN_POINT('Origin',(64.9402651077865,253.540265107786,23.0213203435596)) ;
#106286 = CARTESIAN_POINT('',(64.7902651077865,253.517537835059,22.5218371395634)) ;
#106287 = CARTESIAN_POINT('Ctrl Pts',(64.9402651077865,253.521252214148,22.6718371395631)) ;
#106288 = CARTESIAN_POINT('Ctrl Pts',(64.9402651077865,253.521212580397,22.6703790162594)) ;
#106289 = CARTESIAN_POINT('Ctrl Pts',(64.940243846551,253.521173072598,22.6689209669185)) ;
#106290 = CARTESIAN_POINT('Ctrl Pts',(64.9402013305491,253.521133700923,22.667463456485)) ;
#106291 = CARTESIAN_POINT('Ctrl Pts',(64.9396551395109,253.52062790416,22.6487392325952)) ;
#106292 = CARTESIAN_POINT('Ctrl Pts',(64.9356062703198,253.520149690091,22.6302810697322)) ;
#106293 = CARTESIAN_POINT('Ctrl Pts',(64.928263675975,253.519716235533,22.6130460247761)) ;
#106294 = CARTESIAN_POINT('Ctrl Pts',(64.9206090302592,253.51926435968,22.5950785112737)) ;
#106295 = CARTESIAN_POINT('Ctrl Pts',(64.9095180038063,253.518869237177,22.5787765926026)) ;
#106296 = CARTESIAN_POINT('Ctrl Pts',(64.8956136387304,253.518542867634,22.5650584571031)) ;
#106297 = CARTESIAN_POINT('Ctrl Pts',(64.8817129938791,253.518216585413,22.5513439920009)) ;
#106298 = CARTESIAN_POINT('Ctrl Pts',(64.8652664191736,253.517965001224,22.5404743147172)) ;
#106299 = CARTESIAN_POINT('Ctrl Pts',(64.8471986491032,253.517794524335,22.5330618828598)) ;
#106300 = CARTESIAN_POINT('Ctrl Pts',(64.8291331055124,253.517624068453,22.5256503644316)) ;
#106301 = CARTESIAN_POINT('Ctrl Pts',(64.8097925816883,253.517537835059,22.5218371395634)) ;
#106302 = CARTESIAN_POINT('Ctrl Pts',(64.7902651077865,253.517537835059,22.5218371395634)) ;
#106303 = CARTESIAN_POINT('Origin',(64.7902651077865,253.540265107786,23.0213203435596)) ;
#106304 = CARTESIAN_POINT('Origin',(64.7902651077865,250.427235809792,22.6718371395634)) ;
#106305 = CARTESIAN_POINT('',(64.9402651077865,252.977912471676,22.6718371395634)) ;
#106306 = CARTESIAN_POINT('',(64.9402651077865,250.427235809792,22.6718371395634)) ;
#106307 = CARTESIAN_POINT('',(64.7902651077865,253.115747008939,22.5218371395634)) ;
#106308 = CARTESIAN_POINT('Ctrl Pts',(64.9402651077865,252.977912471676,22.6718371395634)) ;
#106309 = CARTESIAN_POINT('Ctrl Pts',(64.9402651077865,252.978450141357,22.6712600688988)) ;
#106310 = CARTESIAN_POINT('Ctrl Pts',(64.940261777681,252.978987767856,22.6706829503216)) ;
#106311 = CARTESIAN_POINT('Ctrl Pts',(64.9400834366345,252.99337838034,22.655232733985)) ;
#106312 = CARTESIAN_POINT('Ctrl Pts',(64.9376982652987,253.007251853926,22.6402737328004)) ;
#106313 = CARTESIAN_POINT('Ctrl Pts',(64.9285249168183,253.033499763802,22.611858434734)) ;
#106314 = CARTESIAN_POINT('Ctrl Pts',(64.9218878905887,253.046029186311,22.5982392280904)) ;
#106315 = CARTESIAN_POINT('Ctrl Pts',(64.9030518920067,253.07058191007,22.5714615581854)) ;
#106316 = CARTESIAN_POINT('Ctrl Pts',(64.890241559628,253.08251006586,22.5583957973774)) ;
#106317 = CARTESIAN_POINT('Ctrl Pts',(64.8622234505159,253.099809832103,22.5393982820177)) ;
#106318 = CARTESIAN_POINT('Ctrl Pts',(64.8483068832618,253.105986593393,22.5325967432531)) ;
#106319 = CARTESIAN_POINT('Ctrl Pts',(64.8193104176513,253.113796288923,22.5239903075244)) ;
#106320 = CARTESIAN_POINT('Ctrl Pts',(64.8049443310403,253.115747008939,22.5218371395634)) ;
#106321 = CARTESIAN_POINT('Ctrl Pts',(64.7902651077865,253.115747008939,22.5218371395634)) ;
#106322 = CARTESIAN_POINT('',(64.7902651077865,250.427235809792,22.5218371395634)) ;
#106323 = CARTESIAN_POINT('Origin',(64.7902651077865,248.040265107786,23.0213203435596)) ;
#106324 = CARTESIAN_POINT('',(64.9402651077865,252.844243057664,21.8278816743835)) ;
#106325 = CARTESIAN_POINT('Origin',(64.9402651077865,248.040265107786,23.0213203435596)) ;
#106326 = CARTESIAN_POINT('',(64.7902651077865,253.021684041655,21.9279469374017)) ;
#106327 = CARTESIAN_POINT('Ctrl Pts',(64.9402651077865,252.844243057664,21.8278816743835)) ;
#106328 = CARTESIAN_POINT('Ctrl Pts',(64.9402651077865,252.844932736563,21.8282643521316)) ;
#106329 = CARTESIAN_POINT('Ctrl Pts',(64.9402617776811,252.845622389192,21.8286470887883)) ;
#106330 = CARTESIAN_POINT('Ctrl Pts',(64.9400834366345,252.864083054386,21.8388941738985)) ;
#106331 = CARTESIAN_POINT('Ctrl Pts',(64.9376982652987,252.881900097428,21.8488338903424)) ;
#106332 = CARTESIAN_POINT('Ctrl Pts',(64.9285249168182,252.915644153157,21.8677473945125)) ;
#106333 = CARTESIAN_POINT('Ctrl Pts',(64.9218878905886,252.931768908382,21.8768282252525)) ;
#106334 = CARTESIAN_POINT('Ctrl Pts',(64.9030518920066,252.963394691376,21.8947080938071)) ;
#106335 = CARTESIAN_POINT('Ctrl Pts',(64.8902415596279,252.978776583803,21.903448367913)) ;
#106336 = CARTESIAN_POINT('Ctrl Pts',(64.8622234505159,253.001100194315,21.9161701569215)) ;
#106337 = CARTESIAN_POINT('Ctrl Pts',(64.8483068832618,253.009076434455,21.9207300804757)) ;
#106338 = CARTESIAN_POINT('Ctrl Pts',(64.8193104176514,253.019163431181,21.9265019586177)) ;
#106339 = CARTESIAN_POINT('Ctrl Pts',(64.8049443310404,253.021684041655,21.9279469374017)) ;
#106340 = CARTESIAN_POINT('Ctrl Pts',(64.7902651077865,253.021684041655,21.9279469374017)) ;
#106341 = CARTESIAN_POINT('Origin',(64.7902651077865,248.040265107786,23.0213203435596)) ;
#106342 = CARTESIAN_POINT('Origin',(64.7902651077865,250.752859316469,22.5074134442792)) ;
#106343 = CARTESIAN_POINT('',(64.9402651077865,253.360989860305,21.6599804602402)) ;
#106344 = CARTESIAN_POINT('',(64.9402651077865,250.752859316469,22.5074134442792)) ;
#106345 = CARTESIAN_POINT('',(64.7902651077865,253.403809825024,21.8037867439466)) ;
#106346 = CARTESIAN_POINT('Ctrl Pts',(64.9402651077865,253.360989860305,21.6599804602402)) ;
#106347 = CARTESIAN_POINT('Ctrl Pts',(64.9402651077865,253.361402751249,21.661379465413)) ;
#106348 = CARTESIAN_POINT('Ctrl Pts',(64.940243846551,253.361815739121,21.662778361321)) ;
#106349 = CARTESIAN_POINT('Ctrl Pts',(64.9402013305491,253.362228689928,21.6641767026333)) ;
#106350 = CARTESIAN_POINT('Ctrl Pts',(64.9396551395108,253.367533752023,21.6821407975691)) ;
#106351 = CARTESIAN_POINT('Ctrl Pts',(64.9356062703197,253.372782829414,21.6998433299152)) ;
#106352 = CARTESIAN_POINT('Ctrl Pts',(64.928263675975,253.377696511422,21.716368776554)) ;
#106353 = CARTESIAN_POINT('Ctrl Pts',(64.9206090302591,253.382819018967,21.73359653467)) ;
#106354 = CARTESIAN_POINT('Ctrl Pts',(64.9095180038062,253.387480805045,21.7492226802187)) ;
#106355 = CARTESIAN_POINT('Ctrl Pts',(64.8956136387304,253.391409546164,21.7623702561123)) ;
#106356 = CARTESIAN_POINT('Ctrl Pts',(64.8817129938792,253.395337236117,21.7755143142665)) ;
#106357 = CARTESIAN_POINT('Ctrl Pts',(64.8652664191735,253.39845688034,21.7859297354668)) ;
#106358 = CARTESIAN_POINT('Ctrl Pts',(64.8471986491032,253.400585314597,21.7930320573423)) ;
#106359 = CARTESIAN_POINT('Ctrl Pts',(64.8291331055125,253.402713486568,21.8001335040033)) ;
#106360 = CARTESIAN_POINT('Ctrl Pts',(64.8097925816883,253.403809825025,21.8037867439465)) ;
#106361 = CARTESIAN_POINT('Ctrl Pts',(64.7902651077865,253.403809825024,21.8037867439468)) ;
#106362 = CARTESIAN_POINT('',(64.7902651077865,250.799211865625,22.6500719217234)) ;
#106363 = CARTESIAN_POINT('Origin',(64.7902651077865,253.27107594741,21.3217268744974)) ;
#106364 = CARTESIAN_POINT('',(64.9402651077865,253.144997361738,20.9952239032474)) ;
#106365 = CARTESIAN_POINT('Origin',(64.9402651077865,253.27107594741,21.3217268744974)) ;
#106366 = CARTESIAN_POINT('',(64.7902651077865,253.095112228145,20.8537132320653)) ;
#106367 = CARTESIAN_POINT('Ctrl Pts',(64.9402651077865,253.144997361737,20.995223903243)) ;
#106368 = CARTESIAN_POINT('Ctrl Pts',(64.9402651077865,253.144509082919,20.9938493930776)) ;
#106369 = CARTESIAN_POINT('Ctrl Pts',(64.9402438465509,253.144020946745,20.9924749143332)) ;
#106370 = CARTESIAN_POINT('Ctrl Pts',(64.9402013305491,253.143533106564,20.9911009060563)) ;
#106371 = CARTESIAN_POINT('Ctrl Pts',(64.9396551395109,253.137265961862,20.9734494107126)) ;
#106372 = CARTESIAN_POINT('Ctrl Pts',(64.9356062703199,253.131107267255,20.9560424309125)) ;
#106373 = CARTESIAN_POINT('Ctrl Pts',(64.9282636759749,253.125369105682,20.9397848739233)) ;
#106374 = CARTESIAN_POINT('Ctrl Pts',(64.9206090302591,253.119387079188,20.9228363904431)) ;
#106375 = CARTESIAN_POINT('Ctrl Pts',(64.9095180038061,253.113973725445,20.9074544440316)) ;
#106376 = CARTESIAN_POINT('Ctrl Pts',(64.8956136387303,253.109424192564,20.8945085756089)) ;
#106377 = CARTESIAN_POINT('Ctrl Pts',(64.881712993879,253.104875876946,20.8815661709571)) ;
#106378 = CARTESIAN_POINT('Ctrl Pts',(64.8652664191735,253.101277691159,20.8713062373366)) ;
#106379 = CARTESIAN_POINT('Ctrl Pts',(64.8471986491031,253.098824990589,20.8643092759729)) ;
#106380 = CARTESIAN_POINT('Ctrl Pts',(64.8291331055122,253.096372592264,20.8573131768402)) ;
#106381 = CARTESIAN_POINT('Ctrl Pts',(64.8097925816883,253.095112228145,20.8537132320655)) ;
#106382 = CARTESIAN_POINT('Ctrl Pts',(64.7902651077865,253.095112228145,20.8537132320655)) ;
#106383 = CARTESIAN_POINT('Origin',(64.7902651077865,253.27107594741,21.3217268744974)) ;
#106384 = CARTESIAN_POINT('Origin',(64.7902651077865,250.202412898851,21.9513275530686)) ;
#106385 = CARTESIAN_POINT('',(64.9402651077865,252.628250559098,21.1631251173908)) ;
#106386 = CARTESIAN_POINT('',(64.9402651077865,250.202412898851,21.9513275530686)) ;
#106387 = CARTESIAN_POINT('',(64.7902651077865,252.712986444776,20.9778734255204)) ;
#106388 = CARTESIAN_POINT('Ctrl Pts',(64.9402651077865,252.628250559098,21.1631251173908)) ;
#106389 = CARTESIAN_POINT('Ctrl Pts',(64.9402651077865,252.628583588709,21.162410141506)) ;
#106390 = CARTESIAN_POINT('Ctrl Pts',(64.940261777681,252.628916562446,21.1616951333976)) ;
#106391 = CARTESIAN_POINT('Ctrl Pts',(64.9400834366345,252.637828468808,21.1425541606572)) ;
#106392 = CARTESIAN_POINT('Ctrl Pts',(64.9376982652988,252.64640034068,21.1240401659929)) ;
#106393 = CARTESIAN_POINT('Ctrl Pts',(64.9285249168183,252.662582776404,21.0889045613858)) ;
#106394 = CARTESIAN_POINT('Ctrl Pts',(64.9218878905887,252.670290399024,21.0720801216756)) ;
#106395 = CARTESIAN_POINT('Ctrl Pts',(64.9030518920067,252.685366671877,21.0390258353215)) ;
#106396 = CARTESIAN_POINT('Ctrl Pts',(64.890241559628,252.692673480035,21.0229135555138)) ;
#106397 = CARTESIAN_POINT('Ctrl Pts',(64.8622234505159,252.703255980354,20.9994999229698)) ;
#106398 = CARTESIAN_POINT('Ctrl Pts',(64.8483068832618,252.707028638362,20.9911225509982)) ;
#106399 = CARTESIAN_POINT('Ctrl Pts',(64.8193104176512,252.711796565285,20.9805240155764)) ;
#106400 = CARTESIAN_POINT('Ctrl Pts',(64.8049443310403,252.712986444776,20.9778734255205)) ;
#106401 = CARTESIAN_POINT('Ctrl Pts',(64.7902651077865,252.712986444776,20.9778734255204)) ;
#106402 = CARTESIAN_POINT('',(64.7902651077865,250.156060349694,21.8086690756243)) ;
#106403 = CARTESIAN_POINT('Origin',(64.7902651077865,248.040265107786,23.0213203435596)) ;
#106404 = CARTESIAN_POINT('',(64.9402651077865,252.240326810636,20.4017818933262)) ;
#106405 = CARTESIAN_POINT('Origin',(64.9402651077865,248.040265107786,23.0213203435596)) ;
#106406 = CARTESIAN_POINT('',(64.7902651077865,252.440005081538,20.4421173342227)) ;
#106407 = CARTESIAN_POINT('Ctrl Pts',(64.9402651077865,252.240326810636,20.4017818933262)) ;
#106408 = CARTESIAN_POINT('Ctrl Pts',(64.9402651077865,252.241100988172,20.4019327189915)) ;
#106409 = CARTESIAN_POINT('Ctrl Pts',(64.940261777681,252.241875158935,20.402083608801)) ;
#106410 = CARTESIAN_POINT('Ctrl Pts',(64.9400834366345,252.262598818301,20.4061245065945)) ;
#106411 = CARTESIAN_POINT('Ctrl Pts',(64.9376982652987,252.282615374489,20.4100719695998)) ;
#106412 = CARTESIAN_POINT('Ctrl Pts',(64.9285249168184,252.320552472788,20.4176322943072)) ;
#106413 = CARTESIAN_POINT('Ctrl Pts',(64.9218878905887,252.33869415734,20.4212858541613)) ;
#106414 = CARTESIAN_POINT('Ctrl Pts',(64.9030518920066,252.374297247581,20.4285177152552)) ;
#106415 = CARTESIAN_POINT('Ctrl Pts',(64.8902415596279,252.39162718984,20.4320769437325)) ;
#106416 = CARTESIAN_POINT('Ctrl Pts',(64.8622234505159,252.416789454087,20.4372777090437)) ;
#106417 = CARTESIAN_POINT('Ctrl Pts',(64.8483068832618,252.42578440312,20.4391496602992)) ;
#106418 = CARTESIAN_POINT('Ctrl Pts',(64.8193104176514,252.437161315521,20.4415219892068)) ;
#106419 = CARTESIAN_POINT('Ctrl Pts',(64.8049443310403,252.440005081538,20.4421173342227)) ;
#106420 = CARTESIAN_POINT('Ctrl Pts',(64.7902651077865,252.440005081538,20.4421173342227)) ;
#106421 = CARTESIAN_POINT('Origin',(64.7902651077865,248.040265107786,23.0213203435596)) ;
#106422 = CARTESIAN_POINT('Origin',(64.7902651077865,250.461289540614,21.6943281289039)) ;
#106423 = CARTESIAN_POINT('',(64.9402651077865,252.679897896016,20.0824148057166)) ;
#106424 = CARTESIAN_POINT('',(64.9402651077865,250.461289540614,21.6943281289039)) ;
#106425 = CARTESIAN_POINT('',(64.7902651077865,252.765060688053,20.2059506121228)) ;
#106426 = CARTESIAN_POINT('Ctrl Pts',(64.9402651077865,252.679897896016,20.0824148057166)) ;
#106427 = CARTESIAN_POINT('Ctrl Pts',(64.9402651077865,252.680722895012,20.0836177483836)) ;
#106428 = CARTESIAN_POINT('Ctrl Pts',(64.940243846551,252.681547952431,20.0848205571807)) ;
#106429 = CARTESIAN_POINT('Ctrl Pts',(64.9402013305491,252.682372803215,20.086022849981)) ;
#106430 = CARTESIAN_POINT('Ctrl Pts',(64.9396551395108,252.692969427699,20.1014683651929)) ;
#106431 = CARTESIAN_POINT('Ctrl Pts',(64.9356062703198,252.703431980308,20.1166824198099)) ;
#106432 = CARTESIAN_POINT('Ctrl Pts',(64.9282636759749,252.713211813451,20.1308806422754)) ;
#106433 = CARTESIAN_POINT('Ctrl Pts',(64.9206090302592,252.723407277664,20.1456822720077)) ;
#106434 = CARTESIAN_POINT('Ctrl Pts',(64.9095180038062,252.732669644223,20.1591030484337)) ;
#106435 = CARTESIAN_POINT('Ctrl Pts',(64.8956136387303,252.740468923451,20.1703930883885)) ;
#106436 = CARTESIAN_POINT('Ctrl Pts',(64.881712993879,252.74826611592,20.1816801076024)) ;
#106437 = CARTESIAN_POINT('Ctrl Pts',(64.8652664191735,252.75445161604,20.1906217387244)) ;
#106438 = CARTESIAN_POINT('Ctrl Pts',(64.8471986491032,252.758670615469,20.1967187258679)) ;
#106439 = CARTESIAN_POINT('Ctrl Pts',(64.8291331055124,252.762889094993,20.2028149616837)) ;
#106440 = CARTESIAN_POINT('Ctrl Pts',(64.8097925816883,252.765060688053,20.2059506121227)) ;
#106441 = CARTESIAN_POINT('Ctrl Pts',(64.7902651077865,252.765060688053,20.2059506121227)) ;
#106442 = CARTESIAN_POINT('',(64.7902651077865,250.549457328458,21.8156806780601)) ;
#106443 = CARTESIAN_POINT('Origin',(64.7902651077865,252.489858576849,19.788501455951)) ;
#106444 = CARTESIAN_POINT('',(64.9402651077865,252.26905574955,19.5169391031533)) ;
#106445 = CARTESIAN_POINT('Origin',(64.9402651077865,252.489858576849,19.788501455951)) ;
#106446 = CARTESIAN_POINT('',(64.7902651077865,252.1778829659,19.3977698112471)) ;
#106447 = CARTESIAN_POINT('Ctrl Pts',(64.9402651077865,252.269055749548,19.5169391031502)) ;
#106448 = CARTESIAN_POINT('Ctrl Pts',(64.9402651077865,252.268166621797,19.5157827527532)) ;
#106449 = CARTESIAN_POINT('Ctrl Pts',(64.9402438465509,252.267277639417,19.5146263881596)) ;
#106450 = CARTESIAN_POINT('Ctrl Pts',(64.9402013305491,252.266389083925,19.5134703795409)) ;
#106451 = CARTESIAN_POINT('Ctrl Pts',(64.9396551395109,252.25497406308,19.498619464092)) ;
#106452 = CARTESIAN_POINT('Ctrl Pts',(64.9356062703198,252.243737743863,19.4839675838203)) ;
#106453 = CARTESIAN_POINT('Ctrl Pts',(64.9282636759749,252.233256566511,19.4702789177493)) ;
#106454 = CARTESIAN_POINT('Ctrl Pts',(64.9206090302592,252.222329951809,19.4560084999417)) ;
#106455 = CARTESIAN_POINT('Ctrl Pts',(64.9095180038061,252.212428263609,19.4430522178766)) ;
#106456 = CARTESIAN_POINT('Ctrl Pts',(64.8956136387303,252.204100907367,19.4321458483308)) ;
#106457 = CARTESIAN_POINT('Ctrl Pts',(64.881712993879,252.195775779175,19.4212423968718)) ;
#106458 = CARTESIAN_POINT('Ctrl Pts',(64.8652664191735,252.189183207286,19.4125965207019)) ;
#106459 = CARTESIAN_POINT('Ctrl Pts',(64.8471986491031,252.184688370457,19.4066999411606)) ;
#106460 = CARTESIAN_POINT('Ctrl Pts',(64.8291331055122,252.180194087523,19.4008040882511)) ;
#106461 = CARTESIAN_POINT('Ctrl Pts',(64.8097925816882,252.177882965899,19.3977698112477)) ;
#106462 = CARTESIAN_POINT('Ctrl Pts',(64.7902651077865,252.177882965899,19.3977698112476)) ;
#106463 = CARTESIAN_POINT('Origin',(64.7902651077865,252.489858576849,19.788501455951)) ;
#106464 = CARTESIAN_POINT('Origin',(64.7902651077865,249.765943897551,21.3355563159851)) ;
#106465 = CARTESIAN_POINT('',(64.9402651077865,251.829484664171,19.836306190763)) ;
#106466 = CARTESIAN_POINT('',(64.9402651077865,249.765943897551,21.3355563159851)) ;
#106467 = CARTESIAN_POINT('',(64.7902651077865,251.852827359384,19.6339365333471)) ;
#106468 = CARTESIAN_POINT('Ctrl Pts',(64.9402651077865,251.829484664171,19.836306190763)) ;
#106469 = CARTESIAN_POINT('Ctrl Pts',(64.9402651077865,251.829580454454,19.8355232964791)) ;
#106470 = CARTESIAN_POINT('Ctrl Pts',(64.940261777681,251.82967618164,19.8347403888152)) ;
#106471 = CARTESIAN_POINT('Ctrl Pts',(64.9400834366345,251.832237022392,19.8137823114442)) ;
#106472 = CARTESIAN_POINT('Ctrl Pts',(64.9376982652988,251.834668218008,19.7935256020938)) ;
#106473 = CARTESIAN_POINT('Ctrl Pts',(64.9285249168184,251.839201130021,19.7551090087292)) ;
#106474 = CARTESIAN_POINT('Ctrl Pts',(64.9218878905887,251.841332476948,19.7367262293339)) ;
#106475 = CARTESIAN_POINT('Ctrl Pts',(64.9030518920067,251.845456528266,19.7006309103819)) ;
#106476 = CARTESIAN_POINT('Ctrl Pts',(64.890241559628,251.847426747499,19.683049293783)) ;
#106477 = CARTESIAN_POINT('Ctrl Pts',(64.8622234505158,251.85025609303,19.6575114335403)) ;
#106478 = CARTESIAN_POINT('Ctrl Pts',(64.8483068832618,251.851255353705,19.648378263899)) ;
#106479 = CARTESIAN_POINT('Ctrl Pts',(64.8193104176512,251.852514794114,19.6368250872756)) ;
#106480 = CARTESIAN_POINT('Ctrl Pts',(64.8049443310403,251.852827359384,19.6339365333471)) ;
#106481 = CARTESIAN_POINT('Ctrl Pts',(64.7902651077865,251.852827359384,19.6339365333471)) ;
#106482 = CARTESIAN_POINT('',(64.7902651077865,249.677776109707,21.2142037668289)) ;
#106483 = CARTESIAN_POINT('Origin',(64.7902651077865,248.040265107786,23.0213203435596)) ;
#106484 = CARTESIAN_POINT('',(64.9402651077865,251.225279260583,19.2321007871753)) ;
#106485 = CARTESIAN_POINT('Origin',(64.9402651077865,248.040265107786,23.0213203435596)) ;
#106486 = CARTESIAN_POINT('',(64.7902651077865,251.427648917999,19.2087580919617)) ;
#106487 = CARTESIAN_POINT('Ctrl Pts',(64.9402651077865,251.225279260583,19.2321007871753)) ;
#106488 = CARTESIAN_POINT('Ctrl Pts',(64.9402651077865,251.226062154865,19.2320049968921)) ;
#106489 = CARTESIAN_POINT('Ctrl Pts',(64.940261777681,251.226845062528,19.2319092697067)) ;
#106490 = CARTESIAN_POINT('Ctrl Pts',(64.9400834366348,251.247803139899,19.2293484289549)) ;
#106491 = CARTESIAN_POINT('Ctrl Pts',(64.9376982652993,251.268059849249,19.2269172333384)) ;
#106492 = CARTESIAN_POINT('Ctrl Pts',(64.9285249168188,251.306476442616,19.2223843213247)) ;
#106493 = CARTESIAN_POINT('Ctrl Pts',(64.921887890589,251.324859222011,19.2202529743981)) ;
#106494 = CARTESIAN_POINT('Ctrl Pts',(64.9030518920067,251.360954540964,19.2161289230798)) ;
#106495 = CARTESIAN_POINT('Ctrl Pts',(64.890241559628,251.378536157563,19.2141587038466)) ;
#106496 = CARTESIAN_POINT('Ctrl Pts',(64.8622234505159,251.404074017806,19.211329358316)) ;
#106497 = CARTESIAN_POINT('Ctrl Pts',(64.8483068832618,251.413207187447,19.2103300976412)) ;
#106498 = CARTESIAN_POINT('Ctrl Pts',(64.8193104176513,251.42476036407,19.2090706572321)) ;
#106499 = CARTESIAN_POINT('Ctrl Pts',(64.8049443310403,251.427648917999,19.2087580919617)) ;
#106500 = CARTESIAN_POINT('Ctrl Pts',(64.7902651077865,251.427648917999,19.2087580919617)) ;
#106501 = CARTESIAN_POINT('Origin',(64.7902651077865,248.040265107786,23.0213203435596)) ;
#106502 = CARTESIAN_POINT('Origin',(64.7902651077865,249.932733025005,21.0111380571975)) ;
#106503 = CARTESIAN_POINT('',(64.9402651077865,251.544646348193,18.792529701796)) ;
#106504 = CARTESIAN_POINT('',(64.9402651077865,249.932733025005,21.0111380571975)) ;
#106505 = CARTESIAN_POINT('',(64.7902651077865,251.663815640099,18.8837024854464)) ;
#106506 = CARTESIAN_POINT('Ctrl Pts',(64.9402651077865,251.544646348193,18.792529701796)) ;
#106507 = CARTESIAN_POINT('Ctrl Pts',(64.9402651077865,251.545802698591,18.7934188295481)) ;
#106508 = CARTESIAN_POINT('Ctrl Pts',(64.940243846551,251.546959063185,18.7943078119284)) ;
#106509 = CARTESIAN_POINT('Ctrl Pts',(64.9402013305491,251.548115071805,18.7951963674209)) ;
#106510 = CARTESIAN_POINT('Ctrl Pts',(64.9396551395109,251.562965987255,18.8066113882653)) ;
#106511 = CARTESIAN_POINT('Ctrl Pts',(64.93560627032,251.577617867525,18.817847707483)) ;
#106512 = CARTESIAN_POINT('Ctrl Pts',(64.928263675975,251.591306533596,18.8283288848357)) ;
#106513 = CARTESIAN_POINT('Ctrl Pts',(64.9206090302591,251.605576951404,18.8392554995375)) ;
#106514 = CARTESIAN_POINT('Ctrl Pts',(64.9095180038063,251.618533233469,18.8491571877368)) ;
#106515 = CARTESIAN_POINT('Ctrl Pts',(64.8956136387304,251.629439603015,18.8574845439795)) ;
#106516 = CARTESIAN_POINT('Ctrl Pts',(64.881712993879,251.640343054474,18.8658096721712)) ;
#106517 = CARTESIAN_POINT('Ctrl Pts',(64.8652664191734,251.648988930644,18.8724022440602)) ;
#106518 = CARTESIAN_POINT('Ctrl Pts',(64.8471986491031,251.654885510185,18.8768970808899)) ;
#106519 = CARTESIAN_POINT('Ctrl Pts',(64.8291331055123,251.660781363094,18.8813913638239)) ;
#106520 = CARTESIAN_POINT('Ctrl Pts',(64.8097925816882,251.663815640099,18.8837024854465)) ;
#106521 = CARTESIAN_POINT('Ctrl Pts',(64.7902651077865,251.663815640099,18.8837024854463)) ;
#106522 = CARTESIAN_POINT('',(64.7902651077865,250.054085574161,21.0993058450414)) ;
#106523 = CARTESIAN_POINT('Origin',(64.7902651077865,251.273083995395,18.5717268744974)) ;
#106524 = CARTESIAN_POINT('',(64.9402651077865,250.979170645629,18.38168755533)) ;
#106525 = CARTESIAN_POINT('Origin',(64.9402651077865,251.273083995395,18.5717268744974)) ;
#106526 = CARTESIAN_POINT('',(64.7902651077865,250.855634839223,18.2965247632928)) ;
#106527 = CARTESIAN_POINT('Ctrl Pts',(64.9402651077865,250.979170645627,18.381687555328)) ;
#106528 = CARTESIAN_POINT('Ctrl Pts',(64.9402651077865,250.97796770296,18.3808625563329)) ;
#106529 = CARTESIAN_POINT('Ctrl Pts',(64.9402438465509,250.976764894164,18.3800374989153)) ;
#106530 = CARTESIAN_POINT('Ctrl Pts',(64.9402013305491,250.975562601365,18.3792126481319)) ;
#106531 = CARTESIAN_POINT('Ctrl Pts',(64.9396551395108,250.960117086155,18.3686160236418)) ;
#106532 = CARTESIAN_POINT('Ctrl Pts',(64.9356062703197,250.944903031536,18.3581534710383)) ;
#106533 = CARTESIAN_POINT('Ctrl Pts',(64.9282636759749,250.930704809071,18.3483736378949)) ;
#106534 = CARTESIAN_POINT('Ctrl Pts',(64.920609030259,250.915903179338,18.3381781736819)) ;
#106535 = CARTESIAN_POINT('Ctrl Pts',(64.9095180038059,250.902482402912,18.3289158071228)) ;
#106536 = CARTESIAN_POINT('Ctrl Pts',(64.8956136387303,250.891192362958,18.3211165278944)) ;
#106537 = CARTESIAN_POINT('Ctrl Pts',(64.8817129938791,250.879905343744,18.3133193354259)) ;
#106538 = CARTESIAN_POINT('Ctrl Pts',(64.8652664191733,250.870963712621,18.3071338353064)) ;
#106539 = CARTESIAN_POINT('Ctrl Pts',(64.847198649103,250.864866725478,18.3029148358775)) ;
#106540 = CARTESIAN_POINT('Ctrl Pts',(64.8291331055123,250.858770489662,18.2986963563531)) ;
#106541 = CARTESIAN_POINT('Ctrl Pts',(64.8097925816882,250.855634839223,18.2965247632931)) ;
#106542 = CARTESIAN_POINT('Ctrl Pts',(64.7902651077865,250.855634839223,18.2965247632931)) ;
#106543 = CARTESIAN_POINT('Origin',(64.7902651077865,251.273083995395,18.5717268744974)) ;
#106544 = CARTESIAN_POINT('Origin',(64.7902651077865,249.160553432798,20.8847994073294)) ;
#106545 = CARTESIAN_POINT('',(64.9402651077865,250.65980355802,18.8212586407095)) ;
#106546 = CARTESIAN_POINT('',(64.9402651077865,249.160553432798,20.8847994073294)) ;
#106547 = CARTESIAN_POINT('',(64.7902651077865,250.619468117123,18.6215803698081)) ;
#106548 = CARTESIAN_POINT('Ctrl Pts',(64.9402651077865,250.65980355802,18.8212586407095)) ;
#106549 = CARTESIAN_POINT('Ctrl Pts',(64.9402651077865,250.659652732354,18.8204844631737)) ;
#106550 = CARTESIAN_POINT('Ctrl Pts',(64.940261777681,250.659501842545,18.8197102924112)) ;
#106551 = CARTESIAN_POINT('Ctrl Pts',(64.9400834366345,250.655460944751,18.7989866330446)) ;
#106552 = CARTESIAN_POINT('Ctrl Pts',(64.9376982652987,250.651513481746,18.7789700768574)) ;
#106553 = CARTESIAN_POINT('Ctrl Pts',(64.9285249168183,250.643953157039,18.7410329785579)) ;
#106554 = CARTESIAN_POINT('Ctrl Pts',(64.9218878905886,250.640299597185,18.7228912940054)) ;
#106555 = CARTESIAN_POINT('Ctrl Pts',(64.9030518920067,250.633067736091,18.6872882037656)) ;
#106556 = CARTESIAN_POINT('Ctrl Pts',(64.890241559628,250.629508507613,18.6699582615064)) ;
#106557 = CARTESIAN_POINT('Ctrl Pts',(64.8622234505159,250.624307742302,18.6447959972585)) ;
#106558 = CARTESIAN_POINT('Ctrl Pts',(64.8483068832618,250.622435791047,18.6358010482263)) ;
#106559 = CARTESIAN_POINT('Ctrl Pts',(64.8193104176513,250.620063462139,18.6244241358249)) ;
#106560 = CARTESIAN_POINT('Ctrl Pts',(64.8049443310403,250.619468117123,18.6215803698081)) ;
#106561 = CARTESIAN_POINT('Ctrl Pts',(64.7902651077865,250.619468117123,18.6215803698081)) ;
#106562 = CARTESIAN_POINT('',(64.7902651077865,249.039200883641,20.7966316194855)) ;
#106563 = CARTESIAN_POINT('Origin',(64.7902651077865,248.040265107786,23.0213203435596)) ;
#106564 = CARTESIAN_POINT('',(64.9402651077865,249.898460333955,18.4333348922484)) ;
#106565 = CARTESIAN_POINT('Origin',(64.9402651077865,248.040265107786,23.0213203435596)) ;
#106566 = CARTESIAN_POINT('',(64.7902651077865,250.083712025826,18.3485990065702)) ;
#106567 = CARTESIAN_POINT('Ctrl Pts',(64.9402651077865,249.898460333955,18.4333348922483)) ;
#106568 = CARTESIAN_POINT('Ctrl Pts',(64.9402651077865,249.899175309839,18.4330018626366)) ;
#106569 = CARTESIAN_POINT('Ctrl Pts',(64.940261777681,249.899890317948,18.4326688888998)) ;
#106570 = CARTESIAN_POINT('Ctrl Pts',(64.9400834366345,249.91903129069,18.4237569825383)) ;
#106571 = CARTESIAN_POINT('Ctrl Pts',(64.9376982652987,249.937545285353,18.4151851106656)) ;
#106572 = CARTESIAN_POINT('Ctrl Pts',(64.9285249168183,249.97268088996,18.3990026749418)) ;
#106573 = CARTESIAN_POINT('Ctrl Pts',(64.9218878905886,249.98950532967,18.3912950523219)) ;
#106574 = CARTESIAN_POINT('Ctrl Pts',(64.9030518920067,250.022559616024,18.3762187794687)) ;
#106575 = CARTESIAN_POINT('Ctrl Pts',(64.890241559628,250.038671895832,18.3689119713107)) ;
#106576 = CARTESIAN_POINT('Ctrl Pts',(64.8622234505159,250.062085528376,18.3583294709921)) ;
#106577 = CARTESIAN_POINT('Ctrl Pts',(64.8483068832618,250.070462900348,18.3545568129842)) ;
#106578 = CARTESIAN_POINT('Ctrl Pts',(64.8193104176513,250.08106143577,18.3497888860605)) ;
#106579 = CARTESIAN_POINT('Ctrl Pts',(64.8049443310403,250.083712025826,18.3485990065702)) ;
#106580 = CARTESIAN_POINT('Ctrl Pts',(64.7902651077865,250.083712025826,18.3485990065702)) ;
#106581 = CARTESIAN_POINT('Origin',(64.7902651077865,248.040265107786,23.0213203435596)) ;
#106582 = CARTESIAN_POINT('Origin',(64.7902651077865,249.21892856406,20.5247186334439)) ;
#106583 = CARTESIAN_POINT('',(64.7902651077865,250.207872219281,17.9664732232009)) ;
#106584 = CARTESIAN_POINT('',(64.7902651077865,249.361587041504,20.5710711826001)) ;
#106585 = CARTESIAN_POINT('',(64.9402651077865,250.066361548099,17.9165880896075)) ;
#106586 = CARTESIAN_POINT('',(64.9402651077865,249.21892856406,20.5247186334439)) ;
#106587 = CARTESIAN_POINT('Ctrl Pts',(64.9402651077865,250.066361548099,17.9165880896075)) ;
#106588 = CARTESIAN_POINT('Ctrl Pts',(64.9402651077865,250.067736058266,17.9170763684256)) ;
#106589 = CARTESIAN_POINT('Ctrl Pts',(64.940243846551,250.069110537011,17.9175645046006)) ;
#106590 = CARTESIAN_POINT('Ctrl Pts',(64.9402013305492,250.07048454529,17.9180523447822)) ;
#106591 = CARTESIAN_POINT('Ctrl Pts',(64.939655139511,250.088136040637,17.9243194894782)) ;
#106592 = CARTESIAN_POINT('Ctrl Pts',(64.9356062703199,250.105543020433,17.9304781840933)) ;
#106593 = CARTESIAN_POINT('Ctrl Pts',(64.9282636759752,250.121800577422,17.9362163456661)) ;
#106594 = CARTESIAN_POINT('Ctrl Pts',(64.9206090302596,250.138749060902,17.9421983721593)) ;
#106595 = CARTESIAN_POINT('Ctrl Pts',(64.9095180038067,250.154131007314,17.9476117259011)) ;
#106596 = CARTESIAN_POINT('Ctrl Pts',(64.8956136387307,250.167076875737,17.9521612587827)) ;
#106597 = CARTESIAN_POINT('Ctrl Pts',(64.8817129938793,250.180019280389,17.9567095744003)) ;
#106598 = CARTESIAN_POINT('Ctrl Pts',(64.8652664191736,250.19027921401,17.9603077601869)) ;
#106599 = CARTESIAN_POINT('Ctrl Pts',(64.8471986491033,250.197276175374,17.9627604607567)) ;
#106600 = CARTESIAN_POINT('Ctrl Pts',(64.8291331055124,250.204272274506,17.9652128590818)) ;
#106601 = CARTESIAN_POINT('Ctrl Pts',(64.8097925816883,250.207872219281,17.9664732232008)) ;
#106602 = CARTESIAN_POINT('Ctrl Pts',(64.7902651077865,250.207872219281,17.9664732232008)) ;
#106603 = CARTESIAN_POINT('Origin',(64.7902651077865,249.739858576849,17.7905095039363)) ;
#106604 = CARTESIAN_POINT('',(64.7902651077865,249.257798707399,17.6577756263215)) ;
#106605 = CARTESIAN_POINT('Origin',(64.7902651077865,249.739858576849,17.7905095039363)) ;
#106606 = CARTESIAN_POINT('',(64.9402651077865,249.401604991106,17.7005955910415)) ;
#106607 = CARTESIAN_POINT('Origin',(64.9402651077865,249.739858576849,17.7905095039363)) ;
#106608 = CARTESIAN_POINT('Ctrl Pts',(64.9402651077865,249.401604991096,17.7005955910383)) ;
#106609 = CARTESIAN_POINT('Ctrl Pts',(64.9402651077864,249.400205985927,17.7001827000958)) ;
#106610 = CARTESIAN_POINT('Ctrl Pts',(64.9402438465509,249.398807090022,17.699769712222)) ;
#106611 = CARTESIAN_POINT('Ctrl Pts',(64.9402013305491,249.397408748713,17.6993567614174)) ;
#106612 = CARTESIAN_POINT('Ctrl Pts',(64.9396551395108,249.379444653775,17.694051699333)) ;
#106613 = CARTESIAN_POINT('Ctrl Pts',(64.9356062703196,249.361742121431,17.6888026219303)) ;
#106614 = CARTESIAN_POINT('Ctrl Pts',(64.9282636759748,249.345216674792,17.683888939923)) ;
#106615 = CARTESIAN_POINT('Ctrl Pts',(64.9206090302589,249.327988916676,17.6787664323787)) ;
#106616 = CARTESIAN_POINT('Ctrl Pts',(64.9095180038059,249.312362771127,17.6741046463012)) ;
#106617 = CARTESIAN_POINT('Ctrl Pts',(64.8956136387303,249.299215195234,17.6701759051819)) ;
#106618 = CARTESIAN_POINT('Ctrl Pts',(64.8817129938792,249.28607113708,17.6662482152289)) ;
#106619 = CARTESIAN_POINT('Ctrl Pts',(64.8652664191736,249.275655715879,17.663128571007)) ;
#106620 = CARTESIAN_POINT('Ctrl Pts',(64.8471986491032,249.268553394004,17.6610001367496)) ;
#106621 = CARTESIAN_POINT('Ctrl Pts',(64.8291331055123,249.261451947343,17.6588719647777)) ;
#106622 = CARTESIAN_POINT('Ctrl Pts',(64.8097925816883,249.257798707399,17.6577756263226)) ;
#106623 = CARTESIAN_POINT('Ctrl Pts',(64.7902651077865,249.257798707399,17.6577756263226)) ;
#106624 = CARTESIAN_POINT('Origin',(64.7902651077865,248.445501341285,20.6431800539285)) ;
#106625 = CARTESIAN_POINT('',(64.7902651077865,249.133638513944,18.0399014096908)) ;
#106626 = CARTESIAN_POINT('',(64.7902651077865,248.30284286384,20.5968275047722)) ;
#106627 = CARTESIAN_POINT('',(64.9402651077865,249.233703776962,18.2173423936815)) ;
#106628 = CARTESIAN_POINT('',(64.9402651077865,248.445501341285,20.6431800539285)) ;
#106629 = CARTESIAN_POINT('Ctrl Pts',(64.9402651077865,249.233703776962,18.2173423936815)) ;
#106630 = CARTESIAN_POINT('Ctrl Pts',(64.9402651077865,249.233321099215,18.2166527147851)) ;
#106631 = CARTESIAN_POINT('Ctrl Pts',(64.940261777681,249.232938362557,18.2159630621521)) ;
#106632 = CARTESIAN_POINT('Ctrl Pts',(64.9400834366345,249.222691277449,18.197502396961)) ;
#106633 = CARTESIAN_POINT('Ctrl Pts',(64.9376982652987,249.212751561004,18.1796853539185)) ;
#106634 = CARTESIAN_POINT('Ctrl Pts',(64.9285249168183,249.193838056834,18.1459412981892)) ;
#106635 = CARTESIAN_POINT('Ctrl Pts',(64.9218878905887,249.184757226094,18.1298165429637)) ;
#106636 = CARTESIAN_POINT('Ctrl Pts',(64.9030518920067,249.166877357539,18.0981907599697)) ;
#106637 = CARTESIAN_POINT('Ctrl Pts',(64.890241559628,249.158137083433,18.0828088675435)) ;
#106638 = CARTESIAN_POINT('Ctrl Pts',(64.8622234505158,249.145415294424,18.0604852570307)) ;
#106639 = CARTESIAN_POINT('Ctrl Pts',(64.8483068832618,249.14085537087,18.0525090168905)) ;
#106640 = CARTESIAN_POINT('Ctrl Pts',(64.8193104176514,249.135083492728,18.0424220201646)) ;
#106641 = CARTESIAN_POINT('Ctrl Pts',(64.8049443310403,249.133638513944,18.0399014096908)) ;
#106642 = CARTESIAN_POINT('Ctrl Pts',(64.7902651077865,249.133638513944,18.0399014096908)) ;
#106643 = CARTESIAN_POINT('Origin',(64.7902651077865,248.040265107786,23.0213203435596)) ;
#106644 = CARTESIAN_POINT('',(64.7902651077865,248.539748311783,17.9458384424072)) ;
#106645 = CARTESIAN_POINT('Origin',(64.7902651077865,248.040265107786,23.0213203435596)) ;
#106646 = CARTESIAN_POINT('',(64.9402651077865,248.389748311783,18.0836729796702)) ;
#106647 = CARTESIAN_POINT('Origin',(64.9402651077865,248.040265107786,23.0213203435596)) ;
#106648 = CARTESIAN_POINT('Ctrl Pts',(64.9402651077865,248.389748311783,18.0836729796702)) ;
#106649 = CARTESIAN_POINT('Ctrl Pts',(64.9402651077865,248.390325382448,18.0831353099878)) ;
#106650 = CARTESIAN_POINT('Ctrl Pts',(64.940261777681,248.390902501026,18.0825976834882)) ;
#106651 = CARTESIAN_POINT('Ctrl Pts',(64.9400834366341,248.406352717363,18.0682070710039)) ;
#106652 = CARTESIAN_POINT('Ctrl Pts',(64.9376982652983,248.421311718547,18.0543335974184)) ;
#106653 = CARTESIAN_POINT('Ctrl Pts',(64.9285249168178,248.449727016613,18.0280856875433)) ;
#106654 = CARTESIAN_POINT('Ctrl Pts',(64.9218878905883,248.463346223256,18.0155562650348)) ;
#106655 = CARTESIAN_POINT('Ctrl Pts',(64.9030518920067,248.490123893161,17.9910035412764)) ;
#106656 = CARTESIAN_POINT('Ctrl Pts',(64.890241559628,248.503189653969,17.9790753854858)) ;
#106657 = CARTESIAN_POINT('Ctrl Pts',(64.8622234505158,248.522187169328,17.9617756192428)) ;
#106658 = CARTESIAN_POINT('Ctrl Pts',(64.8483068832618,248.528988708093,17.9555988579533)) ;
#106659 = CARTESIAN_POINT('Ctrl Pts',(64.8193104176513,248.537595143822,17.9477891624225)) ;
#106660 = CARTESIAN_POINT('Ctrl Pts',(64.8049443310403,248.539748311783,17.9458384424072)) ;
#106661 = CARTESIAN_POINT('Ctrl Pts',(64.7902651077865,248.539748311783,17.9458384424072)) ;
#106662 = CARTESIAN_POINT('Origin',(64.7902651077865,248.389748311783,20.2826839799233)) ;
#106663 = CARTESIAN_POINT('',(64.7902651077865,248.539748311783,17.5440476162869)) ;
#106664 = CARTESIAN_POINT('',(64.7902651077865,248.539748311783,20.2826839799233)) ;
#106665 = CARTESIAN_POINT('',(64.9402651077865,248.389748311783,17.5403332371978)) ;
#106666 = CARTESIAN_POINT('',(64.9402651077865,248.389748311783,20.2826839799233)) ;
#106667 = CARTESIAN_POINT('Ctrl Pts',(64.9402651077865,248.389748311783,17.5403332371978)) ;
#106668 = CARTESIAN_POINT('Ctrl Pts',(64.9402651077865,248.391206435086,17.5403728709491)) ;
#106669 = CARTESIAN_POINT('Ctrl Pts',(64.940243846551,248.392664484427,17.5404123787478)) ;
#106670 = CARTESIAN_POINT('Ctrl Pts',(64.9402013305492,248.394121994861,17.5404517504229)) ;
#106671 = CARTESIAN_POINT('Ctrl Pts',(64.939655139511,248.412846218751,17.5409575471863)) ;
#106672 = CARTESIAN_POINT('Ctrl Pts',(64.9356062703198,248.431304381614,17.5414357612545)) ;
#106673 = CARTESIAN_POINT('Ctrl Pts',(64.9282636759751,248.44853942657,17.5418692158132)) ;
#106674 = CARTESIAN_POINT('Ctrl Pts',(64.9206090302595,248.466506940072,17.5423210916659)) ;
#106675 = CARTESIAN_POINT('Ctrl Pts',(64.9095180038066,248.482808858743,17.5427162141691)) ;
#106676 = CARTESIAN_POINT('Ctrl Pts',(64.8956136387307,248.496526994243,17.5430425837127)) ;
#106677 = CARTESIAN_POINT('Ctrl Pts',(64.8817129938794,248.510241459345,17.5433688659336)) ;
#106678 = CARTESIAN_POINT('Ctrl Pts',(64.8652664191738,248.521111136629,17.5436204501224)) ;
#106679 = CARTESIAN_POINT('Ctrl Pts',(64.8471986491034,248.528523568487,17.5437909270114)) ;
#106680 = CARTESIAN_POINT('Ctrl Pts',(64.8291331055125,248.535935086915,17.5439613828926)) ;
#106681 = CARTESIAN_POINT('Ctrl Pts',(64.8097925816883,248.539748311783,17.5440476162861)) ;
#106682 = CARTESIAN_POINT('Ctrl Pts',(64.7902651077865,248.539748311783,17.5440476162861)) ;
#106683 = CARTESIAN_POINT('Origin',(64.7902651077865,248.040265107786,17.5213203435596)) ;
#106684 = CARTESIAN_POINT('',(64.7902651077865,247.54078190379,17.5440476162869)) ;
#106685 = CARTESIAN_POINT('Origin',(64.7902651077865,248.040265107786,17.5213203435596)) ;
#106686 = CARTESIAN_POINT('',(64.9402651077865,247.69078190379,17.5403332371979)) ;
#106687 = CARTESIAN_POINT('Origin',(64.9402651077865,248.040265107786,17.5213203435596)) ;
#106688 = CARTESIAN_POINT('Ctrl Pts',(64.9402651077865,247.69078190379,17.5403332371979)) ;
#106689 = CARTESIAN_POINT('Ctrl Pts',(64.9402651077865,247.689323780486,17.5403728709491)) ;
#106690 = CARTESIAN_POINT('Ctrl Pts',(64.940243846551,247.687865731145,17.5404123787479)) ;
#106691 = CARTESIAN_POINT('Ctrl Pts',(64.9402013305491,247.686408220711,17.540451750423)) ;
#106692 = CARTESIAN_POINT('Ctrl Pts',(64.9396551395109,247.667683996822,17.5409575471857)) ;
#106693 = CARTESIAN_POINT('Ctrl Pts',(64.9356062703199,247.649225833959,17.5414357612546)) ;
#106694 = CARTESIAN_POINT('Ctrl Pts',(64.928263675975,247.631990789003,17.5418692158132)) ;
#106695 = CARTESIAN_POINT('Ctrl Pts',(64.9206090302591,247.6140232755,17.5423210916658)) ;
#106696 = CARTESIAN_POINT('Ctrl Pts',(64.9095180038062,247.597721356829,17.5427162141691)) ;
#106697 = CARTESIAN_POINT('Ctrl Pts',(64.8956136387305,247.58400322133,17.5430425837128)) ;
#106698 = CARTESIAN_POINT('Ctrl Pts',(64.8817129938794,247.570288756228,17.5433688659337)) ;
#106699 = CARTESIAN_POINT('Ctrl Pts',(64.8652664191737,247.559419078944,17.5436204501225)) ;
#106700 = CARTESIAN_POINT('Ctrl Pts',(64.8471986491032,247.552006647086,17.5437909270115)) ;
#106701 = CARTESIAN_POINT('Ctrl Pts',(64.8291331055122,247.544595128658,17.5439613828928)) ;
#106702 = CARTESIAN_POINT('Ctrl Pts',(64.8097925816883,247.54078190379,17.5440476162862)) ;
#106703 = CARTESIAN_POINT('Ctrl Pts',(64.7902651077865,247.54078190379,17.5440476162862)) ;
#106704 = CARTESIAN_POINT('Origin',(64.7902651077865,247.69078190379,20.6343496415544)) ;
#106705 = CARTESIAN_POINT('',(64.7902651077865,247.54078190379,17.9458384424072)) ;
#106706 = CARTESIAN_POINT('',(64.7902651077865,247.54078190379,20.6343496415544)) ;
#106707 = CARTESIAN_POINT('',(64.9402651077865,247.69078190379,18.0836729796702)) ;
#106708 = CARTESIAN_POINT('',(64.9402651077865,247.69078190379,20.6343496415544)) ;
#106709 = CARTESIAN_POINT('Ctrl Pts',(64.9402651077865,247.69078190379,18.0836729796702)) ;
#106710 = CARTESIAN_POINT('Ctrl Pts',(64.9402651077865,247.690204833124,18.0831353099878)) ;
#106711 = CARTESIAN_POINT('Ctrl Pts',(64.940261777681,247.689627714546,18.0825976834882)) ;
#106712 = CARTESIAN_POINT('Ctrl Pts',(64.9400834366341,247.674177498209,18.0682070710039)) ;
#106713 = CARTESIAN_POINT('Ctrl Pts',(64.9376982652983,247.659218497025,18.0543335974184)) ;
#106714 = CARTESIAN_POINT('Ctrl Pts',(64.9285249168178,247.63080319896,18.0280856875433)) ;
#106715 = CARTESIAN_POINT('Ctrl Pts',(64.9218878905883,247.617183992317,18.0155562650348)) ;
#106716 = CARTESIAN_POINT('Ctrl Pts',(64.9030518920067,247.590406322412,17.9910035412764)) ;
#106717 = CARTESIAN_POINT('Ctrl Pts',(64.890241559628,247.577340561604,17.9790753854858)) ;
#106718 = CARTESIAN_POINT('Ctrl Pts',(64.8622234505159,247.558343046244,17.9617756192428)) ;
#106719 = CARTESIAN_POINT('Ctrl Pts',(64.8483068832618,247.55154150748,17.9555988579533)) ;
#106720 = CARTESIAN_POINT('Ctrl Pts',(64.8193104176513,247.542935071751,17.9477891624225)) ;
#106721 = CARTESIAN_POINT('Ctrl Pts',(64.8049443310403,247.54078190379,17.9458384424072)) ;
#106722 = CARTESIAN_POINT('Ctrl Pts',(64.7902651077865,247.54078190379,17.9458384424072)) ;
#106723 = CARTESIAN_POINT('Origin',(64.7902651077865,248.040265107786,23.0213203435596)) ;
#106724 = CARTESIAN_POINT('',(64.7902651077865,246.946891701628,18.0399014096908)) ;
#106725 = CARTESIAN_POINT('Origin',(64.7902651077865,248.040265107786,23.0213203435596)) ;
#106726 = CARTESIAN_POINT('',(64.9402651077865,246.84682643861,18.2173423936815)) ;
#106727 = CARTESIAN_POINT('Origin',(64.9402651077865,248.040265107786,23.0213203435596)) ;
#106728 = CARTESIAN_POINT('Ctrl Pts',(64.9402651077865,246.84682643861,18.2173423936815)) ;
#106729 = CARTESIAN_POINT('Ctrl Pts',(64.9402651077865,246.847209116358,18.2166527147839)) ;
#106730 = CARTESIAN_POINT('Ctrl Pts',(64.940261777681,246.847591853017,18.2159630621497)) ;
#106731 = CARTESIAN_POINT('Ctrl Pts',(64.9400834366341,246.857838938126,18.197502396958)) ;
#106732 = CARTESIAN_POINT('Ctrl Pts',(64.9376982652983,246.86777865457,18.1796853539161)) ;
#106733 = CARTESIAN_POINT('Ctrl Pts',(64.9285249168178,246.88669215874,18.1459412981879)) ;
#106734 = CARTESIAN_POINT('Ctrl Pts',(64.9218878905883,246.895772989479,18.1298165429631)) ;
#106735 = CARTESIAN_POINT('Ctrl Pts',(64.9030518920067,246.913652858034,18.0981907599697)) ;
#106736 = CARTESIAN_POINT('Ctrl Pts',(64.890241559628,246.92239313214,18.0828088675435)) ;
#106737 = CARTESIAN_POINT('Ctrl Pts',(64.8622234505159,246.935114921148,18.0604852570307)) ;
#106738 = CARTESIAN_POINT('Ctrl Pts',(64.8483068832618,246.939674844702,18.0525090168905)) ;
#106739 = CARTESIAN_POINT('Ctrl Pts',(64.8193104176513,246.945446722844,18.0424220201645)) ;
#106740 = CARTESIAN_POINT('Ctrl Pts',(64.8049443310403,246.946891701628,18.0399014096908)) ;
#106741 = CARTESIAN_POINT('Ctrl Pts',(64.7902651077865,246.946891701628,18.0399014096908)) ;
#106742 = CARTESIAN_POINT('Origin',(64.7902651077865,247.526358208506,20.3087261348769)) ;
#106743 = CARTESIAN_POINT('',(64.7902651077865,246.822731508173,17.6577756263215)) ;
#106744 = CARTESIAN_POINT('',(64.7902651077865,247.66901668595,20.2623735857207)) ;
#106745 = CARTESIAN_POINT('',(64.9402651077865,246.678925224467,17.7005955910409)) ;
#106746 = CARTESIAN_POINT('',(64.9402651077865,247.526358208506,20.3087261348769)) ;
#106747 = CARTESIAN_POINT('Ctrl Pts',(64.9402651077865,246.678925224467,17.7005955910409)) ;
#106748 = CARTESIAN_POINT('Ctrl Pts',(64.9402651077865,246.680324229639,17.7001827000975)) ;
#106749 = CARTESIAN_POINT('Ctrl Pts',(64.940243846551,246.681723125547,17.6997697122226)) ;
#106750 = CARTESIAN_POINT('Ctrl Pts',(64.9402013305492,246.683121466859,17.6993567614171)) ;
#106751 = CARTESIAN_POINT('Ctrl Pts',(64.9396551395109,246.701085561798,17.6940516993336)) ;
#106752 = CARTESIAN_POINT('Ctrl Pts',(64.93560627032,246.718788094141,17.6888026219308)) ;
#106753 = CARTESIAN_POINT('Ctrl Pts',(64.928263675975,246.73531354078,17.6838889399233)) ;
#106754 = CARTESIAN_POINT('Ctrl Pts',(64.9206090302591,246.752541298897,17.6787664323789)) ;
#106755 = CARTESIAN_POINT('Ctrl Pts',(64.9095180038064,246.768167444445,17.6741046463009)) ;
#106756 = CARTESIAN_POINT('Ctrl Pts',(64.8956136387306,246.781315020339,17.6701759051816)) ;
#106757 = CARTESIAN_POINT('Ctrl Pts',(64.8817129938792,246.794459078493,17.6662482152284)) ;
#106758 = CARTESIAN_POINT('Ctrl Pts',(64.8652664191735,246.804874499694,17.6631285710069)) ;
#106759 = CARTESIAN_POINT('Ctrl Pts',(64.8471986491032,246.811976821569,17.6610001367494)) ;
#106760 = CARTESIAN_POINT('Ctrl Pts',(64.8291331055123,246.81907826823,17.6588719647776)) ;
#106761 = CARTESIAN_POINT('Ctrl Pts',(64.8097925816884,246.822731508174,17.6577756263219)) ;
#106762 = CARTESIAN_POINT('Ctrl Pts',(64.7902651077865,246.822731508174,17.6577756263219)) ;
#106763 = CARTESIAN_POINT('Origin',(64.7902651077865,246.340671638724,17.7905095039363)) ;
#106764 = CARTESIAN_POINT('',(64.7902651077865,245.872657996292,17.9664732232009)) ;
#106765 = CARTESIAN_POINT('Origin',(64.7902651077865,246.340671638724,17.7905095039363)) ;
#106766 = CARTESIAN_POINT('',(64.9402651077865,246.014168667474,17.9165880896082)) ;
#106767 = CARTESIAN_POINT('Origin',(64.9402651077865,246.340671638724,17.7905095039363)) ;
#106768 = CARTESIAN_POINT('Ctrl Pts',(64.9402651077865,246.014168667472,17.9165880896088)) ;
#106769 = CARTESIAN_POINT('Ctrl Pts',(64.9402651077865,246.012794157306,17.9170763684267)) ;
#106770 = CARTESIAN_POINT('Ctrl Pts',(64.9402438465509,246.011419678561,17.917564504601)) ;
#106771 = CARTESIAN_POINT('Ctrl Pts',(64.9402013305491,246.010045670283,17.9180523447824)) ;
#106772 = CARTESIAN_POINT('Ctrl Pts',(64.9396551395109,245.992394174936,17.9243194894788)) ;
#106773 = CARTESIAN_POINT('Ctrl Pts',(64.9356062703199,245.97498719514,17.9304781840937)) ;
#106774 = CARTESIAN_POINT('Ctrl Pts',(64.928263675975,245.958729638151,17.9362163456665)) ;
#106775 = CARTESIAN_POINT('Ctrl Pts',(64.9206090302592,245.94178115467,17.9421983721597)) ;
#106776 = CARTESIAN_POINT('Ctrl Pts',(64.9095180038062,245.926399208258,17.9476117259015)) ;
#106777 = CARTESIAN_POINT('Ctrl Pts',(64.8956136387304,245.913453339835,17.9521612587831)) ;
#106778 = CARTESIAN_POINT('Ctrl Pts',(64.8817129938793,245.900510935184,17.9567095744006)) ;
#106779 = CARTESIAN_POINT('Ctrl Pts',(64.8652664191737,245.890251001563,17.960307760187)) ;
#106780 = CARTESIAN_POINT('Ctrl Pts',(64.8471986491033,245.883254040199,17.9627604607568)) ;
#106781 = CARTESIAN_POINT('Ctrl Pts',(64.8291331055124,245.876257941067,17.9652128590819)) ;
#106782 = CARTESIAN_POINT('Ctrl Pts',(64.8097925816883,245.872657996292,17.9664732232011)) ;
#106783 = CARTESIAN_POINT('Ctrl Pts',(64.7902651077865,245.872657996292,17.9664732232011)) ;
#106784 = CARTESIAN_POINT('Origin',(64.7902651077865,246.970272317295,20.8591725524954)) ;
#106785 = CARTESIAN_POINT('',(64.7902651077865,245.996818189747,18.3485990065702)) ;
#106786 = CARTESIAN_POINT('',(64.7902651077865,246.827613839851,20.9055251016516)) ;
#106787 = CARTESIAN_POINT('',(64.9402651077865,246.182069881617,18.4333348922484)) ;
#106788 = CARTESIAN_POINT('',(64.9402651077865,246.970272317295,20.8591725524954)) ;
#106789 = CARTESIAN_POINT('Ctrl Pts',(64.9402651077865,246.182069881617,18.4333348922484)) ;
#106790 = CARTESIAN_POINT('Ctrl Pts',(64.9402651077865,246.181354905731,18.4330018626361)) ;
#106791 = CARTESIAN_POINT('Ctrl Pts',(64.940261777681,246.180639897622,18.4326688888987)) ;
#106792 = CARTESIAN_POINT('Ctrl Pts',(64.9400834366341,246.16149892488,18.4237569825369)) ;
#106793 = CARTESIAN_POINT('Ctrl Pts',(64.9376982652983,246.142984930217,18.4151851106646)) ;
#106794 = CARTESIAN_POINT('Ctrl Pts',(64.9285249168178,246.107849325611,18.3990026749412)) ;
#106795 = CARTESIAN_POINT('Ctrl Pts',(64.9218878905884,246.091024885902,18.3912950523217)) ;
#106796 = CARTESIAN_POINT('Ctrl Pts',(64.9030518920067,246.057970599548,18.3762187794687)) ;
#106797 = CARTESIAN_POINT('Ctrl Pts',(64.890241559628,246.041858319741,18.3689119713107)) ;
#106798 = CARTESIAN_POINT('Ctrl Pts',(64.862223450516,246.018444687197,18.3583294709921)) ;
#106799 = CARTESIAN_POINT('Ctrl Pts',(64.8483068832619,246.010067315225,18.3545568129842)) ;
#106800 = CARTESIAN_POINT('Ctrl Pts',(64.8193104176514,245.999468779803,18.3497888860605)) ;
#106801 = CARTESIAN_POINT('Ctrl Pts',(64.8049443310404,245.996818189747,18.3485990065702)) ;
#106802 = CARTESIAN_POINT('Ctrl Pts',(64.7902651077866,245.996818189747,18.3485990065702)) ;
#106803 = CARTESIAN_POINT('Origin',(64.7902651077865,248.040265107786,23.0213203435596)) ;
#106804 = CARTESIAN_POINT('',(64.7902651077865,245.461062098449,18.6215803698081)) ;
#106805 = CARTESIAN_POINT('Origin',(64.7902651077865,248.040265107786,23.0213203435596)) ;
#106806 = CARTESIAN_POINT('',(64.9402651077865,245.420726657553,18.8212586407095)) ;
#106807 = CARTESIAN_POINT('Origin',(64.9402651077865,248.040265107786,23.0213203435596)) ;
#106808 = CARTESIAN_POINT('Ctrl Pts',(64.9402651077865,245.420726657553,18.8212586407095)) ;
#106809 = CARTESIAN_POINT('Ctrl Pts',(64.9402651077865,245.420877483218,18.8204844631751)) ;
#106810 = CARTESIAN_POINT('Ctrl Pts',(64.940261777681,245.421028373027,18.8197102924139)) ;
#106811 = CARTESIAN_POINT('Ctrl Pts',(64.9400834366348,245.42506927082,18.7989866330484)) ;
#106812 = CARTESIAN_POINT('Ctrl Pts',(64.9376982652992,245.429016733826,18.7789700768601)) ;
#106813 = CARTESIAN_POINT('Ctrl Pts',(64.9285249168188,245.436577058534,18.7410329785595)) ;
#106814 = CARTESIAN_POINT('Ctrl Pts',(64.921887890589,245.440230618388,18.7228912940061)) ;
#106815 = CARTESIAN_POINT('Ctrl Pts',(64.9030518920066,245.447462479482,18.6872882037654)) ;
#106816 = CARTESIAN_POINT('Ctrl Pts',(64.8902415596279,245.451021707959,18.6699582615064)) ;
#106817 = CARTESIAN_POINT('Ctrl Pts',(64.8622234505159,245.45622247327,18.6447959972585)) ;
#106818 = CARTESIAN_POINT('Ctrl Pts',(64.8483068832618,245.458094424526,18.6358010482263)) ;
#106819 = CARTESIAN_POINT('Ctrl Pts',(64.8193104176514,245.460466753434,18.6244241358249)) ;
#106820 = CARTESIAN_POINT('Ctrl Pts',(64.8049443310403,245.461062098449,18.6215803698081)) ;
#106821 = CARTESIAN_POINT('Ctrl Pts',(64.7902651077865,245.461062098449,18.6215803698081)) ;
#106822 = CARTESIAN_POINT('Origin',(64.7902651077865,246.713272893131,20.6002959107317)) ;
#106823 = CARTESIAN_POINT('',(64.7902651077865,245.224895376349,18.2965247632928)) ;
#106824 = CARTESIAN_POINT('',(64.7902651077865,246.834625442287,20.5121281228878)) ;
#106825 = CARTESIAN_POINT('',(64.9402651077865,245.101359569943,18.3816875553298)) ;
#106826 = CARTESIAN_POINT('',(64.9402651077865,246.713272893131,20.6002959107317)) ;
#106827 = CARTESIAN_POINT('Ctrl Pts',(64.9402651077865,245.101359569943,18.3816875553298)) ;
#106828 = CARTESIAN_POINT('Ctrl Pts',(64.9402651077865,245.10256251261,18.3808625563341)) ;
#106829 = CARTESIAN_POINT('Ctrl Pts',(64.940243846551,245.103765321407,18.3800374989151)) ;
#106830 = CARTESIAN_POINT('Ctrl Pts',(64.9402013305492,245.104967614207,18.3792126481315)) ;
#106831 = CARTESIAN_POINT('Ctrl Pts',(64.939655139511,245.120413129419,18.3686160236467)) ;
#106832 = CARTESIAN_POINT('Ctrl Pts',(64.93560627032,245.135627184036,18.3581534710379)) ;
#106833 = CARTESIAN_POINT('Ctrl Pts',(64.9282636759752,245.149825406502,18.3483736378944)) ;
#106834 = CARTESIAN_POINT('Ctrl Pts',(64.9206090302594,245.164627036234,18.3381781736815)) ;
#106835 = CARTESIAN_POINT('Ctrl Pts',(64.9095180038065,245.17804781266,18.3289158071225)) ;
#106836 = CARTESIAN_POINT('Ctrl Pts',(64.8956136387306,245.189337852615,18.3211165278942)) ;
#106837 = CARTESIAN_POINT('Ctrl Pts',(64.8817129938792,245.200624871829,18.3133193354257)) ;
#106838 = CARTESIAN_POINT('Ctrl Pts',(64.8652664191738,245.209566502951,18.3071338353058)) ;
#106839 = CARTESIAN_POINT('Ctrl Pts',(64.8471986491033,245.215663490095,18.3029148358767)) ;
#106840 = CARTESIAN_POINT('Ctrl Pts',(64.8291331055125,245.22175972591,18.2986963563522)) ;
#106841 = CARTESIAN_POINT('Ctrl Pts',(64.8097925816884,245.22489537635,18.2965247632923)) ;
#106842 = CARTESIAN_POINT('Ctrl Pts',(64.7902651077865,245.224895376349,18.2965247632922)) ;
#106843 = CARTESIAN_POINT('Origin',(64.7902651077865,244.807446220178,18.5717268744974)) ;
#106844 = CARTESIAN_POINT('',(64.7902651077865,244.416714575474,18.8837024854464)) ;
#106845 = CARTESIAN_POINT('Origin',(64.7902651077865,244.807446220178,18.5717268744974)) ;
#106846 = CARTESIAN_POINT('',(64.9402651077865,244.53588386738,18.7925297017961)) ;
#106847 = CARTESIAN_POINT('Origin',(64.9402651077865,244.807446220178,18.5717268744974)) ;
#106848 = CARTESIAN_POINT('Ctrl Pts',(64.9402651077865,244.535883867376,18.7925297017989)) ;
#106849 = CARTESIAN_POINT('Ctrl Pts',(64.9402651077864,244.534727516979,18.7934188295502)) ;
#106850 = CARTESIAN_POINT('Ctrl Pts',(64.9402438465509,244.533571152387,18.7943078119297)) ;
#106851 = CARTESIAN_POINT('Ctrl Pts',(64.9402013305491,244.532415143768,18.795196367421)) ;
#106852 = CARTESIAN_POINT('Ctrl Pts',(64.9396551395109,244.517564228314,18.8066113882631)) ;
#106853 = CARTESIAN_POINT('Ctrl Pts',(64.9356062703197,244.502912348047,18.8178477074834)) ;
#106854 = CARTESIAN_POINT('Ctrl Pts',(64.9282636759748,244.489223681976,18.8283288848357)) ;
#106855 = CARTESIAN_POINT('Ctrl Pts',(64.920609030259,244.474953264168,18.8392554995373)) ;
#106856 = CARTESIAN_POINT('Ctrl Pts',(64.9095180038061,244.461996982103,18.8491571877365)) ;
#106857 = CARTESIAN_POINT('Ctrl Pts',(64.8956136387302,244.451090612557,18.8574845439792)) ;
#106858 = CARTESIAN_POINT('Ctrl Pts',(64.8817129938788,244.440187161098,18.8658096721709)) ;
#106859 = CARTESIAN_POINT('Ctrl Pts',(64.8652664191737,244.431541284929,18.8724022440602)) ;
#106860 = CARTESIAN_POINT('Ctrl Pts',(64.8471986491032,244.425644705388,18.8768970808898)) ;
#106861 = CARTESIAN_POINT('Ctrl Pts',(64.8291331055122,244.419748852478,18.8813913638236)) ;
#106862 = CARTESIAN_POINT('Ctrl Pts',(64.8097925816883,244.416714575474,18.8837024854465)) ;
#106863 = CARTESIAN_POINT('Ctrl Pts',(64.7902651077865,244.416714575474,18.8837024854465)) ;
#106864 = CARTESIAN_POINT('Origin',(64.7902651077865,246.354501080212,21.2956415537952)) ;
#106865 = CARTESIAN_POINT('',(64.7902651077865,244.652881297574,19.2087580919617)) ;
#106866 = CARTESIAN_POINT('',(64.7902651077865,246.233148531056,21.3838093416391)) ;
#106867 = CARTESIAN_POINT('',(64.9402651077865,244.85525095499,19.2321007871753)) ;
#106868 = CARTESIAN_POINT('',(64.9402651077865,246.354501080212,21.2956415537952)) ;
#106869 = CARTESIAN_POINT('Ctrl Pts',(64.9402651077865,244.85525095499,19.2321007871753)) ;
#106870 = CARTESIAN_POINT('Ctrl Pts',(64.9402651077865,244.854468060706,19.2320049968919)) ;
#106871 = CARTESIAN_POINT('Ctrl Pts',(64.940261777681,244.853685153042,19.2319092697064)) ;
#106872 = CARTESIAN_POINT('Ctrl Pts',(64.9400834366345,244.83272707567,19.2293484289546)) ;
#106873 = CARTESIAN_POINT('Ctrl Pts',(64.9376982652987,244.81247036632,19.226917233338)) ;
#106874 = CARTESIAN_POINT('Ctrl Pts',(64.9285249168183,244.774053772956,19.2223843213245)) ;
#106875 = CARTESIAN_POINT('Ctrl Pts',(64.9218878905887,244.755670993561,19.220252974398)) ;
#106876 = CARTESIAN_POINT('Ctrl Pts',(64.9030518920067,244.719575674609,19.2161289230799)) ;
#106877 = CARTESIAN_POINT('Ctrl Pts',(64.890241559628,244.70199405801,19.2141587038466)) ;
#106878 = CARTESIAN_POINT('Ctrl Pts',(64.862223450516,244.676456197767,19.211329358316)) ;
#106879 = CARTESIAN_POINT('Ctrl Pts',(64.8483068832619,244.667323028126,19.2103300976413)) ;
#106880 = CARTESIAN_POINT('Ctrl Pts',(64.8193104176513,244.655769851502,19.2090706572321)) ;
#106881 = CARTESIAN_POINT('Ctrl Pts',(64.8049443310403,244.652881297574,19.2087580919617)) ;
#106882 = CARTESIAN_POINT('Ctrl Pts',(64.7902651077866,244.652881297574,19.2087580919617)) ;
#106883 = CARTESIAN_POINT('Origin',(64.7902651077865,248.040265107786,23.0213203435596)) ;
#106884 = CARTESIAN_POINT('',(64.7902651077865,244.227702856188,19.633936533347)) ;
#106885 = CARTESIAN_POINT('Origin',(64.7902651077865,248.040265107786,23.0213203435596)) ;
#106886 = CARTESIAN_POINT('',(64.9402651077865,244.251045551402,19.836306190763)) ;
#106887 = CARTESIAN_POINT('Origin',(64.9402651077865,248.040265107786,23.0213203435596)) ;
#106888 = CARTESIAN_POINT('Ctrl Pts',(64.9402651077865,244.251045551402,19.836306190763)) ;
#106889 = CARTESIAN_POINT('Ctrl Pts',(64.9402651077865,244.250949761118,19.835523296477)) ;
#106890 = CARTESIAN_POINT('Ctrl Pts',(64.9402617776811,244.250854033933,19.8347403888173)) ;
#106891 = CARTESIAN_POINT('Ctrl Pts',(64.9400834366345,244.248293193182,19.8137823114414)) ;
#106892 = CARTESIAN_POINT('Ctrl Pts',(64.9376982652987,244.245861997565,19.7935256020932)) ;
#106893 = CARTESIAN_POINT('Ctrl Pts',(64.9285249168183,244.241329085551,19.7551090087289)) ;
#106894 = CARTESIAN_POINT('Ctrl Pts',(64.9218878905886,244.239197738625,19.7367262293338)) ;
#106895 = CARTESIAN_POINT('Ctrl Pts',(64.9030518920067,244.235073687307,19.7006309103819)) ;
#106896 = CARTESIAN_POINT('Ctrl Pts',(64.890241559628,244.233103468073,19.683049293783)) ;
#106897 = CARTESIAN_POINT('Ctrl Pts',(64.8622234505159,244.230274122543,19.6575114335404)) ;
#106898 = CARTESIAN_POINT('Ctrl Pts',(64.8483068832618,244.229274861868,19.648378263899)) ;
#106899 = CARTESIAN_POINT('Ctrl Pts',(64.8193104176514,244.228015421459,19.6368250872756)) ;
#106900 = CARTESIAN_POINT('Ctrl Pts',(64.8049443310404,244.227702856188,19.6339365333471)) ;
#106901 = CARTESIAN_POINT('Ctrl Pts',(64.7902651077866,244.227702856188,19.6339365333471)) ;
#106902 = CARTESIAN_POINT('Origin',(64.7902651077865,246.030082821424,21.1288524263407)) ;
#106903 = CARTESIAN_POINT('',(64.7902651077865,243.902647249673,19.3977698112471)) ;
#106904 = CARTESIAN_POINT('',(64.7902651077865,246.118250609268,21.0074998771845)) ;
#106905 = CARTESIAN_POINT('',(64.9402651077865,243.811474466023,19.5169391031534)) ;
#106906 = CARTESIAN_POINT('',(64.9402651077865,246.030082821424,21.1288524263407)) ;
#106907 = CARTESIAN_POINT('Ctrl Pts',(64.9402651077865,243.811474466023,19.5169391031534)) ;
#106908 = CARTESIAN_POINT('Ctrl Pts',(64.9402651077865,243.812363593775,19.5157827527548)) ;
#106909 = CARTESIAN_POINT('Ctrl Pts',(64.940243846551,243.813252576157,19.5146263881627)) ;
#106910 = CARTESIAN_POINT('Ctrl Pts',(64.9402013305491,243.814141131649,19.5134703795416)) ;
#106911 = CARTESIAN_POINT('Ctrl Pts',(64.9396551395108,243.825556152481,19.4986194640777)) ;
#106912 = CARTESIAN_POINT('Ctrl Pts',(64.9356062703196,243.836792471712,19.4839675838214)) ;
#106913 = CARTESIAN_POINT('Ctrl Pts',(64.928263675975,243.847273649063,19.4702789177503)) ;
#106914 = CARTESIAN_POINT('Ctrl Pts',(64.9206090302592,243.858200263764,19.456008499942)) ;
#106915 = CARTESIAN_POINT('Ctrl Pts',(64.9095180038061,243.868101951963,19.4430522178762)) ;
#106916 = CARTESIAN_POINT('Ctrl Pts',(64.8956136387302,243.876429308206,19.4321458483306)) ;
#106917 = CARTESIAN_POINT('Ctrl Pts',(64.8817129938788,243.884754436398,19.4212423968717)) ;
#106918 = CARTESIAN_POINT('Ctrl Pts',(64.8652664191734,243.891347008287,19.412596520702)) ;
#106919 = CARTESIAN_POINT('Ctrl Pts',(64.847198649103,243.895841845117,19.4066999411611)) ;
#106920 = CARTESIAN_POINT('Ctrl Pts',(64.8291331055123,243.900336128051,19.4008040882519)) ;
#106921 = CARTESIAN_POINT('Ctrl Pts',(64.8097925816883,243.902647249673,19.3977698112471)) ;
#106922 = CARTESIAN_POINT('Ctrl Pts',(64.7902651077865,243.902647249673,19.3977698112472)) ;
#106923 = CARTESIAN_POINT('Origin',(64.7902651077865,243.590671638724,19.788501455951)) ;
#106924 = CARTESIAN_POINT('',(64.7902651077865,243.315469527519,20.2059506121228)) ;
#106925 = CARTESIAN_POINT('Origin',(64.7902651077865,243.590671638724,19.788501455951)) ;
#106926 = CARTESIAN_POINT('',(64.9402651077865,243.400632319557,20.0824148057165)) ;
#106927 = CARTESIAN_POINT('Origin',(64.9402651077865,243.590671638724,19.788501455951)) ;
#106928 = CARTESIAN_POINT('Ctrl Pts',(64.9402651077865,243.400632319555,20.0824148057187)) ;
#106929 = CARTESIAN_POINT('Ctrl Pts',(64.9402651077865,243.39980732056,20.0836177483853)) ;
#106930 = CARTESIAN_POINT('Ctrl Pts',(64.9402438465509,243.398982263143,20.084820557182)) ;
#106931 = CARTESIAN_POINT('Ctrl Pts',(64.9402013305491,243.398157412359,20.0860228499814)) ;
#106932 = CARTESIAN_POINT('Ctrl Pts',(64.9396551395109,243.387560787866,20.1014683651894)) ;
#106933 = CARTESIAN_POINT('Ctrl Pts',(64.9356062703196,243.377098235265,20.1166824198106)) ;
#106934 = CARTESIAN_POINT('Ctrl Pts',(64.9282636759749,243.367318402122,20.1308806422758)) ;
#106935 = CARTESIAN_POINT('Ctrl Pts',(64.9206090302592,243.357122937909,20.1456822720079)) ;
#106936 = CARTESIAN_POINT('Ctrl Pts',(64.9095180038063,243.34786057135,20.1591030484339)) ;
#106937 = CARTESIAN_POINT('Ctrl Pts',(64.8956136387305,243.340061292122,20.1703930883887)) ;
#106938 = CARTESIAN_POINT('Ctrl Pts',(64.8817129938791,243.332264099653,20.1816801076026)) ;
#106939 = CARTESIAN_POINT('Ctrl Pts',(64.8652664191737,243.326078599533,20.1906217387245)) ;
#106940 = CARTESIAN_POINT('Ctrl Pts',(64.8471986491031,243.321859600104,20.1967187258679)) ;
#106941 = CARTESIAN_POINT('Ctrl Pts',(64.8291331055123,243.317641120579,20.2028149616835)) ;
#106942 = CARTESIAN_POINT('Ctrl Pts',(64.8097925816883,243.315469527519,20.2059506121225)) ;
#106943 = CARTESIAN_POINT('Ctrl Pts',(64.7902651077865,243.315469527519,20.2059506121226)) ;
#106944 = CARTESIAN_POINT('Origin',(64.7902651077865,245.903744171556,21.9010320185483)) ;
#106945 = CARTESIAN_POINT('',(64.7902651077865,243.640525134035,20.4421173342227)) ;
#106946 = CARTESIAN_POINT('',(64.7902651077865,245.815576383712,22.0223845677046)) ;
#106947 = CARTESIAN_POINT('',(64.9402651077865,243.840203404936,20.4017818933262)) ;
#106948 = CARTESIAN_POINT('',(64.9402651077865,245.903744171556,21.9010320185483)) ;
#106949 = CARTESIAN_POINT('Ctrl Pts',(64.9402651077865,243.840203404936,20.4017818933262)) ;
#106950 = CARTESIAN_POINT('Ctrl Pts',(64.9402651077865,243.839429227398,20.4019327189919)) ;
#106951 = CARTESIAN_POINT('Ctrl Pts',(64.9402617776811,243.83865505664,20.4020836088006)) ;
#106952 = CARTESIAN_POINT('Ctrl Pts',(64.9400834366345,243.817931397271,20.4061245065949)) ;
#106953 = CARTESIAN_POINT('Ctrl Pts',(64.9376982652987,243.797914841084,20.4100719696)) ;
#106954 = CARTESIAN_POINT('Ctrl Pts',(64.9285249168183,243.759977742784,20.4176322943074)) ;
#106955 = CARTESIAN_POINT('Ctrl Pts',(64.9218878905886,243.741836058232,20.4212858541613)) ;
#106956 = CARTESIAN_POINT('Ctrl Pts',(64.9030518920066,243.706232967992,20.4285177152552)) ;
#106957 = CARTESIAN_POINT('Ctrl Pts',(64.8902415596279,243.688903025733,20.4320769437325)) ;
#106958 = CARTESIAN_POINT('Ctrl Pts',(64.862223450516,243.663740761485,20.4372777090437)) ;
#106959 = CARTESIAN_POINT('Ctrl Pts',(64.8483068832619,243.654745812453,20.4391496602992)) ;
#106960 = CARTESIAN_POINT('Ctrl Pts',(64.8193104176513,243.643368900052,20.4415219892068)) ;
#106961 = CARTESIAN_POINT('Ctrl Pts',(64.8049443310403,243.640525134035,20.4421173342227)) ;
#106962 = CARTESIAN_POINT('Ctrl Pts',(64.7902651077865,243.640525134035,20.4421173342227)) ;
#106963 = CARTESIAN_POINT('Origin',(64.7902651077865,248.040265107786,23.0213203435596)) ;
#106964 = CARTESIAN_POINT('',(64.7902651077865,243.367543770797,20.9778734255204)) ;
#106965 = CARTESIAN_POINT('Origin',(64.7902651077865,248.040265107786,23.0213203435596)) ;
#106966 = CARTESIAN_POINT('',(64.9402651077865,243.452279656475,21.1631251173908)) ;
#106967 = CARTESIAN_POINT('Origin',(64.9402651077865,248.040265107786,23.0213203435596)) ;
#106968 = CARTESIAN_POINT('Ctrl Pts',(64.9402651077865,243.452279656475,21.1631251173908)) ;
#106969 = CARTESIAN_POINT('Ctrl Pts',(64.9402651077865,243.451946626863,21.162410141506)) ;
#106970 = CARTESIAN_POINT('Ctrl Pts',(64.940261777681,243.451613653127,21.1616951333977)) ;
#106971 = CARTESIAN_POINT('Ctrl Pts',(64.9400834366345,243.442701746765,21.1425541606558)) ;
#106972 = CARTESIAN_POINT('Ctrl Pts',(64.9376982652987,243.434129874892,21.1240401659928)) ;
#106973 = CARTESIAN_POINT('Ctrl Pts',(64.9285249168183,243.417947439168,21.0889045613856)) ;
#106974 = CARTESIAN_POINT('Ctrl Pts',(64.9218878905886,243.410239816549,21.0720801216755)) ;
#106975 = CARTESIAN_POINT('Ctrl Pts',(64.9030518920067,243.395163543695,21.0390258353216)) ;
#106976 = CARTESIAN_POINT('Ctrl Pts',(64.890241559628,243.387856735537,21.0229135555139)) ;
#106977 = CARTESIAN_POINT('Ctrl Pts',(64.8622234505159,243.377274235219,20.9994999229698)) ;
#106978 = CARTESIAN_POINT('Ctrl Pts',(64.8483068832618,243.373501577211,20.9911225509982)) ;
#106979 = CARTESIAN_POINT('Ctrl Pts',(64.8193104176513,243.368733650287,20.9805240155764)) ;
#106980 = CARTESIAN_POINT('Ctrl Pts',(64.8049443310403,243.367543770797,20.9778734255204)) ;
#106981 = CARTESIAN_POINT('Ctrl Pts',(64.7902651077865,243.367543770797,20.9778734255204)) ;
#106982 = CARTESIAN_POINT('Origin',(64.7902651077865,245.543663397671,21.8426568872864)) ;
#106983 = CARTESIAN_POINT('',(64.7902651077865,242.985417987428,20.8537132320653)) ;
#106984 = CARTESIAN_POINT('',(64.7902651077865,245.590015946827,21.6999984098422)) ;
#106985 = CARTESIAN_POINT('',(64.9402651077865,242.935532853835,20.9952239032475)) ;
#106986 = CARTESIAN_POINT('',(64.9402651077865,245.543663397671,21.8426568872864)) ;
#106987 = CARTESIAN_POINT('Ctrl Pts',(64.9402651077865,242.935532853835,20.9952239032475)) ;
#106988 = CARTESIAN_POINT('Ctrl Pts',(64.9402651077865,242.936021132653,20.9938493930805)) ;
#106989 = CARTESIAN_POINT('Ctrl Pts',(64.940243846551,242.936509268827,20.9924749143349)) ;
#106990 = CARTESIAN_POINT('Ctrl Pts',(64.9402013305491,242.936997109009,20.9911009060562)) ;
#106991 = CARTESIAN_POINT('Ctrl Pts',(64.9396551395109,242.943264253705,20.9734494107095)) ;
#106992 = CARTESIAN_POINT('Ctrl Pts',(64.9356062703199,242.94942294832,20.9560424309132)) ;
#106993 = CARTESIAN_POINT('Ctrl Pts',(64.928263675975,242.955161109893,20.9397848739239)) ;
#106994 = CARTESIAN_POINT('Ctrl Pts',(64.9206090302593,242.961143136386,20.9228363904435)) ;
#106995 = CARTESIAN_POINT('Ctrl Pts',(64.9095180038063,242.966556490128,20.9074544440317)) ;
#106996 = CARTESIAN_POINT('Ctrl Pts',(64.8956136387305,242.97110602301,20.8945085756088)) ;
#106997 = CARTESIAN_POINT('Ctrl Pts',(64.8817129938792,242.975654338627,20.881566170957)) ;
#106998 = CARTESIAN_POINT('Ctrl Pts',(64.8652664191736,242.979252524414,20.8713062373364)) ;
#106999 = CARTESIAN_POINT('Ctrl Pts',(64.8471986491032,242.981705224983,20.8643092759726)) ;
#107000 = CARTESIAN_POINT('Ctrl Pts',(64.8291331055124,242.984157623308,20.8573131768398)) ;
#107001 = CARTESIAN_POINT('Ctrl Pts',(64.8097925816883,242.985417987427,20.853713232065)) ;
#107002 = CARTESIAN_POINT('Ctrl Pts',(64.7902651077865,242.985417987427,20.853713232065)) ;
#107003 = CARTESIAN_POINT('Origin',(64.7902651077865,242.809454268163,21.3217268744974)) ;
#107004 = CARTESIAN_POINT('',(64.7902651077865,242.676720390548,21.8037867439466)) ;
#107005 = CARTESIAN_POINT('Origin',(64.7902651077865,242.809454268163,21.3217268744974)) ;
#107006 = CARTESIAN_POINT('',(64.9402651077865,242.719540355268,21.6599804602403)) ;
#107007 = CARTESIAN_POINT('Origin',(64.9402651077865,242.809454268163,21.3217268744974)) ;
#107008 = CARTESIAN_POINT('Ctrl Pts',(64.9402651077865,242.719540355266,21.6599804602464)) ;
#107009 = CARTESIAN_POINT('Ctrl Pts',(64.9402651077864,242.719127464323,21.6613794654168)) ;
#107010 = CARTESIAN_POINT('Ctrl Pts',(64.9402438465509,242.718714476449,21.6627783613227)) ;
#107011 = CARTESIAN_POINT('Ctrl Pts',(64.9402013305491,242.718301525644,21.6641767026329)) ;
#107012 = CARTESIAN_POINT('Ctrl Pts',(64.9396551395109,242.71299646356,21.6821407975713)) ;
#107013 = CARTESIAN_POINT('Ctrl Pts',(64.9356062703198,242.707747386158,21.6998433299147)) ;
#107014 = CARTESIAN_POINT('Ctrl Pts',(64.928263675975,242.70283370415,21.7163687765538)) ;
#107015 = CARTESIAN_POINT('Ctrl Pts',(64.9206090302592,242.697711196606,21.7335965346699)) ;
#107016 = CARTESIAN_POINT('Ctrl Pts',(64.9095180038063,242.693049410528,21.7492226802188)) ;
#107017 = CARTESIAN_POINT('Ctrl Pts',(64.8956136387304,242.689120669408,21.7623702561123)) ;
#107018 = CARTESIAN_POINT('Ctrl Pts',(64.8817129938791,242.685192979455,21.7755143142664)) ;
#107019 = CARTESIAN_POINT('Ctrl Pts',(64.8652664191737,242.682073335234,21.7859297354671)) ;
#107020 = CARTESIAN_POINT('Ctrl Pts',(64.8471986491032,242.679944900976,21.7930320573425)) ;
#107021 = CARTESIAN_POINT('Ctrl Pts',(64.8291331055123,242.677816729004,21.8001335040033)) ;
#107022 = CARTESIAN_POINT('Ctrl Pts',(64.8097925816883,242.676720390548,21.8037867439466)) ;
#107023 = CARTESIAN_POINT('Ctrl Pts',(64.7902651077865,242.676720390548,21.8037867439466)) ;
#107024 = CARTESIAN_POINT('Origin',(64.7902651077865,245.662124818155,22.6160841100613)) ;
#107025 = CARTESIAN_POINT('',(64.7902651077865,243.058846173918,21.9279469374017)) ;
#107026 = CARTESIAN_POINT('',(64.7902651077865,245.615772268999,22.7587425875056)) ;
#107027 = CARTESIAN_POINT('',(64.9402651077865,243.236287157908,21.8278816743835)) ;
#107028 = CARTESIAN_POINT('',(64.9402651077865,245.662124818155,22.6160841100613)) ;
#107029 = CARTESIAN_POINT('Ctrl Pts',(64.9402651077865,243.236287157908,21.8278816743835)) ;
#107030 = CARTESIAN_POINT('Ctrl Pts',(64.9402651077865,243.235597479012,21.8282643521305)) ;
#107031 = CARTESIAN_POINT('Ctrl Pts',(64.940261777681,243.234907826379,21.8286470887893)) ;
#107032 = CARTESIAN_POINT('Ctrl Pts',(64.9400834366345,243.216447161187,21.8388941738976)) ;
#107033 = CARTESIAN_POINT('Ctrl Pts',(64.9376982652987,243.198630118145,21.8488338903421)) ;
#107034 = CARTESIAN_POINT('Ctrl Pts',(64.9285249168183,243.164886062416,21.8677473945122)) ;
#107035 = CARTESIAN_POINT('Ctrl Pts',(64.9218878905887,243.14876130719,21.8768282252524)) ;
#107036 = CARTESIAN_POINT('Ctrl Pts',(64.9030518920067,243.117135524196,21.8947080938071)) ;
#107037 = CARTESIAN_POINT('Ctrl Pts',(64.890241559628,243.10175363177,21.903448367913)) ;
#107038 = CARTESIAN_POINT('Ctrl Pts',(64.8622234505159,243.079430021257,21.9161701569215)) ;
#107039 = CARTESIAN_POINT('Ctrl Pts',(64.8483068832618,243.071453781117,21.9207300804757)) ;
#107040 = CARTESIAN_POINT('Ctrl Pts',(64.8193104176513,243.061366784391,21.9265019586177)) ;
#107041 = CARTESIAN_POINT('Ctrl Pts',(64.8049443310403,243.058846173917,21.9279469374017)) ;
#107042 = CARTESIAN_POINT('Ctrl Pts',(64.7902651077865,243.058846173917,21.9279469374017)) ;
#107043 = CARTESIAN_POINT('Origin',(64.7902651077865,248.040265107786,23.0213203435596)) ;
#107044 = CARTESIAN_POINT('',(64.7902651077865,242.964783206634,22.5218371395634)) ;
#107045 = CARTESIAN_POINT('Origin',(64.7902651077865,248.040265107786,23.0213203435596)) ;
#107046 = CARTESIAN_POINT('',(64.9402651077865,243.102617743897,22.6718371395634)) ;
#107047 = CARTESIAN_POINT('Origin',(64.9402651077865,248.040265107786,23.0213203435596)) ;
#107048 = CARTESIAN_POINT('Ctrl Pts',(64.9402651077865,243.102617743897,22.6718371395634)) ;
#107049 = CARTESIAN_POINT('Ctrl Pts',(64.9402651077865,243.102080074215,22.6712600688988)) ;
#107050 = CARTESIAN_POINT('Ctrl Pts',(64.940261777681,243.101542447717,22.6706829503216)) ;
#107051 = CARTESIAN_POINT('Ctrl Pts',(64.9400834366345,243.087151835233,22.655232733985)) ;
#107052 = CARTESIAN_POINT('Ctrl Pts',(64.9376982652987,243.073278361647,22.6402737328005)) ;
#107053 = CARTESIAN_POINT('Ctrl Pts',(64.9285249168183,243.047030451771,22.6118584347341)) ;
#107054 = CARTESIAN_POINT('Ctrl Pts',(64.9218878905887,243.034501029262,22.5982392280904)) ;
#107055 = CARTESIAN_POINT('Ctrl Pts',(64.9030518920067,243.009948305503,22.5714615581854)) ;
#107056 = CARTESIAN_POINT('Ctrl Pts',(64.890241559628,242.998020149712,22.5583957973774)) ;
#107057 = CARTESIAN_POINT('Ctrl Pts',(64.8622234505159,242.98072038347,22.5393982820177)) ;
#107058 = CARTESIAN_POINT('Ctrl Pts',(64.8483068832618,242.97454362218,22.5325967432531)) ;
#107059 = CARTESIAN_POINT('Ctrl Pts',(64.8193104176514,242.966733926649,22.5239903075244)) ;
#107060 = CARTESIAN_POINT('Ctrl Pts',(64.8049443310404,242.964783206634,22.5218371395634)) ;
#107061 = CARTESIAN_POINT('Ctrl Pts',(64.7902651077866,242.964783206634,22.5218371395634)) ;
#107062 = CARTESIAN_POINT('Origin',(64.7902651077865,245.30162874415,22.6718371395634)) ;
#107063 = CARTESIAN_POINT('',(64.7902651077865,242.562992380514,22.5218371395634)) ;
#107064 = CARTESIAN_POINT('',(64.7902651077865,245.30162874415,22.5218371395634)) ;
#107065 = CARTESIAN_POINT('',(64.9402651077865,242.559278001424,22.6718371395634)) ;
#107066 = CARTESIAN_POINT('',(64.9402651077865,245.30162874415,22.6718371395634)) ;
#107067 = CARTESIAN_POINT('Ctrl Pts',(64.9402651077865,242.559278001424,22.6718371395634)) ;
#107068 = CARTESIAN_POINT('Ctrl Pts',(64.9402651077865,242.559317635176,22.6703790162596)) ;
#107069 = CARTESIAN_POINT('Ctrl Pts',(64.940243846551,242.559357142974,22.6689209669185)) ;
#107070 = CARTESIAN_POINT('Ctrl Pts',(64.9402013305491,242.559396514649,22.6674634564849)) ;
#107071 = CARTESIAN_POINT('Ctrl Pts',(64.9396551395109,242.559902311412,22.6487392325954)) ;
#107072 = CARTESIAN_POINT('Ctrl Pts',(64.9356062703199,242.560380525481,22.6302810697323)) ;
#107073 = CARTESIAN_POINT('Ctrl Pts',(64.928263675975,242.56081398004,22.6130460247761)) ;
#107074 = CARTESIAN_POINT('Ctrl Pts',(64.9206090302592,242.561265855892,22.5950785112737)) ;
#107075 = CARTESIAN_POINT('Ctrl Pts',(64.9095180038063,242.561660978396,22.5787765926026)) ;
#107076 = CARTESIAN_POINT('Ctrl Pts',(64.8956136387304,242.561987347939,22.5650584571031)) ;
#107077 = CARTESIAN_POINT('Ctrl Pts',(64.881712993879,242.56231363016,22.5513439920008)) ;
#107078 = CARTESIAN_POINT('Ctrl Pts',(64.8652664191735,242.562565214349,22.5404743147171)) ;
#107079 = CARTESIAN_POINT('Ctrl Pts',(64.8471986491031,242.562735691238,22.5330618828598)) ;
#107080 = CARTESIAN_POINT('Ctrl Pts',(64.8291331055124,242.562906147119,22.5256503644317)) ;
#107081 = CARTESIAN_POINT('Ctrl Pts',(64.8097925816883,242.562992380514,22.5218371395634)) ;
#107082 = CARTESIAN_POINT('Ctrl Pts',(64.7902651077865,242.562992380514,22.5218371395634)) ;
#107083 = CARTESIAN_POINT('Origin',(64.7902651077865,242.540265107786,23.0213203435596)) ;
#107084 = CARTESIAN_POINT('',(64.7902651077865,242.562992380514,23.5208035475559)) ;
#107085 = CARTESIAN_POINT('Origin',(64.7902651077865,242.540265107786,23.0213203435596)) ;
#107086 = CARTESIAN_POINT('',(64.9402651077865,242.559278001425,23.3708035475559)) ;
#107087 = CARTESIAN_POINT('Origin',(64.9402651077865,242.540265107786,23.0213203435596)) ;
#107088 = CARTESIAN_POINT('Ctrl Pts',(64.9402651077865,242.559278001425,23.3708035475559)) ;
#107089 = CARTESIAN_POINT('Ctrl Pts',(64.9402651077865,242.559317635176,23.3722616708596)) ;
#107090 = CARTESIAN_POINT('Ctrl Pts',(64.940243846551,242.559357142975,23.3737197202007)) ;
#107091 = CARTESIAN_POINT('Ctrl Pts',(64.9402013305491,242.55939651465,23.3751772306343)) ;
#107092 = CARTESIAN_POINT('Ctrl Pts',(64.9396551395109,242.559902311413,23.3939014545241)) ;
#107093 = CARTESIAN_POINT('Ctrl Pts',(64.9356062703199,242.560380525481,23.412359617387)) ;
#107094 = CARTESIAN_POINT('Ctrl Pts',(64.928263675975,242.56081398004,23.4295946623431)) ;
#107095 = CARTESIAN_POINT('Ctrl Pts',(64.9206090302592,242.561265855892,23.4475621758458)) ;
#107096 = CARTESIAN_POINT('Ctrl Pts',(64.9095180038062,242.561660978395,23.4638640945167)) ;
#107097 = CARTESIAN_POINT('Ctrl Pts',(64.8956136387304,242.561987347939,23.4775822300162)) ;
#107098 = CARTESIAN_POINT('Ctrl Pts',(64.8817129938791,242.56231363016,23.4912966951184)) ;
#107099 = CARTESIAN_POINT('Ctrl Pts',(64.8652664191737,242.562565214349,23.5021663724021)) ;
#107100 = CARTESIAN_POINT('Ctrl Pts',(64.8471986491032,242.562735691238,23.5095788042594)) ;
#107101 = CARTESIAN_POINT('Ctrl Pts',(64.8291331055124,242.56290614712,23.5169903226877)) ;
#107102 = CARTESIAN_POINT('Ctrl Pts',(64.8097925816884,242.562992380514,23.5208035475559)) ;
#107103 = CARTESIAN_POINT('Ctrl Pts',(64.7902651077866,242.562992380514,23.5208035475559)) ;
#107104 = CARTESIAN_POINT('Origin',(64.7902651077865,245.653294405781,23.3708035475559)) ;
#107105 = CARTESIAN_POINT('',(64.7902651077865,242.964783206634,23.5208035475559)) ;
#107106 = CARTESIAN_POINT('',(64.7902651077865,245.653294405781,23.5208035475559)) ;
#107107 = CARTESIAN_POINT('',(64.9402651077865,243.102617743897,23.3708035475559)) ;
#107108 = CARTESIAN_POINT('',(64.9402651077865,245.653294405781,23.3708035475559)) ;
#107109 = CARTESIAN_POINT('Ctrl Pts',(64.9402651077865,243.102617743897,23.3708035475559)) ;
#107110 = CARTESIAN_POINT('Ctrl Pts',(64.9402651077865,243.102080074215,23.3713806182205)) ;
#107111 = CARTESIAN_POINT('Ctrl Pts',(64.940261777681,243.101542447717,23.3719577367977)) ;
#107112 = CARTESIAN_POINT('Ctrl Pts',(64.9400834366345,243.087151835233,23.3874079531342)) ;
#107113 = CARTESIAN_POINT('Ctrl Pts',(64.9376982652987,243.073278361647,23.4023669543188)) ;
#107114 = CARTESIAN_POINT('Ctrl Pts',(64.9285249168183,243.047030451771,23.4307822523853)) ;
#107115 = CARTESIAN_POINT('Ctrl Pts',(64.9218878905887,243.034501029262,23.4444014590289)) ;
#107116 = CARTESIAN_POINT('Ctrl Pts',(64.9030518920067,243.009948305503,23.4711791289339)) ;
#107117 = CARTESIAN_POINT('Ctrl Pts',(64.890241559628,242.998020149712,23.4842448897419)) ;
#107118 = CARTESIAN_POINT('Ctrl Pts',(64.8622234505159,242.98072038347,23.5032424051016)) ;
#107119 = CARTESIAN_POINT('Ctrl Pts',(64.8483068832618,242.97454362218,23.5100439438662)) ;
#107120 = CARTESIAN_POINT('Ctrl Pts',(64.8193104176513,242.966733926649,23.5186503795949)) ;
#107121 = CARTESIAN_POINT('Ctrl Pts',(64.8049443310403,242.964783206634,23.5208035475559)) ;
#107122 = CARTESIAN_POINT('Ctrl Pts',(64.7902651077865,242.964783206634,23.5208035475559)) ;
#107123 = CARTESIAN_POINT('Origin',(64.7902651077865,248.040265107786,23.0213203435596)) ;
#107124 = CARTESIAN_POINT('',(64.7902651077865,243.058846173918,24.1146937497175)) ;
#107125 = CARTESIAN_POINT('Origin',(64.7902651077865,248.040265107786,23.0213203435596)) ;
#107126 = CARTESIAN_POINT('',(64.9402651077865,243.236287157908,24.2147590127358)) ;
#107127 = CARTESIAN_POINT('Origin',(64.9402651077865,248.040265107786,23.0213203435596)) ;
#107128 = CARTESIAN_POINT('Ctrl Pts',(64.9402651077865,243.236287157908,24.2147590127358)) ;
#107129 = CARTESIAN_POINT('Ctrl Pts',(64.9402651077865,243.235597479013,24.2143763349894)) ;
#107130 = CARTESIAN_POINT('Ctrl Pts',(64.940261777681,243.234907826381,24.2139935983313)) ;
#107131 = CARTESIAN_POINT('Ctrl Pts',(64.9400834366348,243.216447161191,24.2037465132234)) ;
#107132 = CARTESIAN_POINT('Ctrl Pts',(64.9376982652992,243.198630118147,24.1938067967784)) ;
#107133 = CARTESIAN_POINT('Ctrl Pts',(64.9285249168188,243.164886062417,24.1748932926076)) ;
#107134 = CARTESIAN_POINT('Ctrl Pts',(64.921887890589,243.148761307191,24.1658124618672)) ;
#107135 = CARTESIAN_POINT('Ctrl Pts',(64.9030518920067,243.117135524196,24.1479325933122)) ;
#107136 = CARTESIAN_POINT('Ctrl Pts',(64.890241559628,243.10175363177,24.1391923192062)) ;
#107137 = CARTESIAN_POINT('Ctrl Pts',(64.8622234505159,243.079430021257,24.1264705301977)) ;
#107138 = CARTESIAN_POINT('Ctrl Pts',(64.8483068832618,243.071453781117,24.1219106066435)) ;
#107139 = CARTESIAN_POINT('Ctrl Pts',(64.8193104176513,243.061366784391,24.1161387285016)) ;
#107140 = CARTESIAN_POINT('Ctrl Pts',(64.8049443310403,243.058846173917,24.1146937497176)) ;
#107141 = CARTESIAN_POINT('Ctrl Pts',(64.7902651077865,243.058846173917,24.1146937497176)) ;
#107142 = CARTESIAN_POINT('Origin',(64.7902651077865,245.327670899104,23.5352272428401)) ;
#107143 = CARTESIAN_POINT('',(64.7902651077865,242.676720390548,24.2388539431727)) ;
#107144 = CARTESIAN_POINT('',(64.7902651077865,245.281318349947,23.3925687653958)) ;
#107145 = CARTESIAN_POINT('',(64.9402651077865,242.719540355268,24.3826602268791)) ;
#107146 = CARTESIAN_POINT('',(64.9402651077865,245.327670899104,23.5352272428401)) ;
#107147 = CARTESIAN_POINT('Ctrl Pts',(64.9402651077865,242.719540355268,24.3826602268791)) ;
#107148 = CARTESIAN_POINT('Ctrl Pts',(64.9402651077865,242.719127464324,24.3812612217067)) ;
#107149 = CARTESIAN_POINT('Ctrl Pts',(64.940243846551,242.718714476449,24.3798623257986)) ;
#107150 = CARTESIAN_POINT('Ctrl Pts',(64.9402013305491,242.718301525644,24.3784639844864)) ;
#107151 = CARTESIAN_POINT('Ctrl Pts',(64.9396551395108,242.71299646356,24.360499889548)) ;
#107152 = CARTESIAN_POINT('Ctrl Pts',(64.9356062703197,242.707747386158,24.3427973572043)) ;
#107153 = CARTESIAN_POINT('Ctrl Pts',(64.9282636759749,242.702833704151,24.3262719105654)) ;
#107154 = CARTESIAN_POINT('Ctrl Pts',(64.9206090302591,242.697711196606,24.3090441524494)) ;
#107155 = CARTESIAN_POINT('Ctrl Pts',(64.9095180038062,242.693049410527,24.2934180069009)) ;
#107156 = CARTESIAN_POINT('Ctrl Pts',(64.8956136387304,242.689120669408,24.2802704310072)) ;
#107157 = CARTESIAN_POINT('Ctrl Pts',(64.8817129938791,242.685192979455,24.2671263728531)) ;
#107158 = CARTESIAN_POINT('Ctrl Pts',(64.8652664191735,242.682073335233,24.2567109516525)) ;
#107159 = CARTESIAN_POINT('Ctrl Pts',(64.8471986491031,242.679944900976,24.2496086297771)) ;
#107160 = CARTESIAN_POINT('Ctrl Pts',(64.8291331055123,242.677816729004,24.2425071831162)) ;
#107161 = CARTESIAN_POINT('Ctrl Pts',(64.8097925816884,242.676720390548,24.2388539431728)) ;
#107162 = CARTESIAN_POINT('Ctrl Pts',(64.7902651077866,242.676720390548,24.2388539431728)) ;
#107163 = CARTESIAN_POINT('Origin',(64.7902651077865,242.809454268163,24.7209138126218)) ;
#107164 = CARTESIAN_POINT('',(64.7902651077865,242.985417987428,25.188927455054)) ;
#107165 = CARTESIAN_POINT('Origin',(64.7902651077865,242.809454268163,24.7209138126218)) ;
#107166 = CARTESIAN_POINT('',(64.9402651077865,242.935532853835,25.0474167838717)) ;
#107167 = CARTESIAN_POINT('Origin',(64.9402651077865,242.809454268163,24.7209138126218)) ;
#107168 = CARTESIAN_POINT('Ctrl Pts',(64.9402651077865,242.935532853835,25.0474167838725)) ;
#107169 = CARTESIAN_POINT('Ctrl Pts',(64.9402651077865,242.936021132653,25.0487912940392)) ;
#107170 = CARTESIAN_POINT('Ctrl Pts',(64.940243846551,242.936509268827,25.0501657727845)) ;
#107171 = CARTESIAN_POINT('Ctrl Pts',(64.9402013305491,242.936997109009,25.051539781063)) ;
#107172 = CARTESIAN_POINT('Ctrl Pts',(64.9396551395109,242.943264253705,25.0691912764101)) ;
#107173 = CARTESIAN_POINT('Ctrl Pts',(64.9356062703198,242.949422948318,25.0865982562069)) ;
#107174 = CARTESIAN_POINT('Ctrl Pts',(64.9282636759749,242.955161109891,25.102855813196)) ;
#107175 = CARTESIAN_POINT('Ctrl Pts',(64.9206090302591,242.961143136385,25.1198042966763)) ;
#107176 = CARTESIAN_POINT('Ctrl Pts',(64.9095180038061,242.966556490128,25.1351862430876)) ;
#107177 = CARTESIAN_POINT('Ctrl Pts',(64.8956136387304,242.97110602301,25.1481321115104)) ;
#107178 = CARTESIAN_POINT('Ctrl Pts',(64.8817129938791,242.975654338627,25.1610745161621)) ;
#107179 = CARTESIAN_POINT('Ctrl Pts',(64.8652664191736,242.979252524414,25.1713344497827)) ;
#107180 = CARTESIAN_POINT('Ctrl Pts',(64.8471986491031,242.981705224984,25.1783314111464)) ;
#107181 = CARTESIAN_POINT('Ctrl Pts',(64.8291331055122,242.984157623309,25.1853275102791)) ;
#107182 = CARTESIAN_POINT('Ctrl Pts',(64.8097925816883,242.985417987428,25.1889274550538)) ;
#107183 = CARTESIAN_POINT('Ctrl Pts',(64.7902651077865,242.985417987428,25.1889274550538)) ;
#107184 = CARTESIAN_POINT('Origin',(64.7902651077865,245.878117316722,24.0913131340507)) ;
#107185 = CARTESIAN_POINT('',(64.7902651077865,243.367543770797,25.0647672615988)) ;
#107186 = CARTESIAN_POINT('',(64.7902651077865,245.924469865878,24.233971611495)) ;
#107187 = CARTESIAN_POINT('',(64.9402651077865,243.452279656475,24.8795155697285)) ;
#107188 = CARTESIAN_POINT('',(64.9402651077865,245.878117316722,24.0913131340507)) ;
#107189 = CARTESIAN_POINT('Ctrl Pts',(64.9402651077865,243.452279656475,24.8795155697285)) ;
#107190 = CARTESIAN_POINT('Ctrl Pts',(64.9402651077865,243.451946626863,24.8802305456133)) ;
#107191 = CARTESIAN_POINT('Ctrl Pts',(64.940261777681,243.451613653127,24.8809455537216)) ;
#107192 = CARTESIAN_POINT('Ctrl Pts',(64.9400834366345,243.442701746765,24.9000865264632)) ;
#107193 = CARTESIAN_POINT('Ctrl Pts',(64.9376982652988,243.434129874892,24.9186005211265)) ;
#107194 = CARTESIAN_POINT('Ctrl Pts',(64.9285249168183,243.417947439168,24.9537361257337)) ;
#107195 = CARTESIAN_POINT('Ctrl Pts',(64.9218878905886,243.410239816549,24.9705605654438)) ;
#107196 = CARTESIAN_POINT('Ctrl Pts',(64.9030518920066,243.395163543695,25.0036148517979)) ;
#107197 = CARTESIAN_POINT('Ctrl Pts',(64.8902415596279,243.387856735537,25.0197271316055)) ;
#107198 = CARTESIAN_POINT('Ctrl Pts',(64.8622234505159,243.377274235219,25.0431407641495)) ;
#107199 = CARTESIAN_POINT('Ctrl Pts',(64.8483068832618,243.373501577211,25.0515181361211)) ;
#107200 = CARTESIAN_POINT('Ctrl Pts',(64.8193104176513,243.368733650287,25.0621166715429)) ;
#107201 = CARTESIAN_POINT('Ctrl Pts',(64.8049443310403,243.367543770797,25.0647672615988)) ;
#107202 = CARTESIAN_POINT('Ctrl Pts',(64.7902651077865,243.367543770797,25.0647672615988)) ;
#107203 = CARTESIAN_POINT('Origin',(64.7902651077865,248.040265107786,23.0213203435596)) ;
#107204 = CARTESIAN_POINT('',(64.7902651077865,243.640525134035,25.6005233528965)) ;
#107205 = CARTESIAN_POINT('Origin',(64.7902651077865,248.040265107786,23.0213203435596)) ;
#107206 = CARTESIAN_POINT('',(64.9402651077865,243.840203404936,25.6408587937931)) ;
#107207 = CARTESIAN_POINT('Origin',(64.9402651077865,248.040265107786,23.0213203435596)) ;
#107208 = CARTESIAN_POINT('Ctrl Pts',(64.9402651077865,243.840203404936,25.6408587937931)) ;
#107209 = CARTESIAN_POINT('Ctrl Pts',(64.9402651077865,243.839429227398,25.6407079681274)) ;
#107210 = CARTESIAN_POINT('Ctrl Pts',(64.9402617776811,243.83865505664,25.6405570783186)) ;
#107211 = CARTESIAN_POINT('Ctrl Pts',(64.9400834366345,243.817931397271,25.6365161805243)) ;
#107212 = CARTESIAN_POINT('Ctrl Pts',(64.9376982652987,243.797914841084,25.6325687175194)) ;
#107213 = CARTESIAN_POINT('Ctrl Pts',(64.9285249168183,243.759977742785,25.6250083928119)) ;
#107214 = CARTESIAN_POINT('Ctrl Pts',(64.9218878905886,243.741836058232,25.621354832958)) ;
#107215 = CARTESIAN_POINT('Ctrl Pts',(64.9030518920066,243.706232967992,25.6141229718641)) ;
#107216 = CARTESIAN_POINT('Ctrl Pts',(64.8902415596279,243.688903025733,25.6105637433868)) ;
#107217 = CARTESIAN_POINT('Ctrl Pts',(64.862223450516,243.663740761485,25.6053629780756)) ;
#107218 = CARTESIAN_POINT('Ctrl Pts',(64.8483068832619,243.654745812453,25.6034910268201)) ;
#107219 = CARTESIAN_POINT('Ctrl Pts',(64.8193104176514,243.643368900052,25.6011186979124)) ;
#107220 = CARTESIAN_POINT('Ctrl Pts',(64.8049443310403,243.640525134035,25.6005233528966)) ;
#107221 = CARTESIAN_POINT('Ctrl Pts',(64.7902651077865,243.640525134035,25.6005233528966)) ;
#107222 = CARTESIAN_POINT('Origin',(64.7902651077865,245.619240674958,24.3483125582154)) ;
#107223 = CARTESIAN_POINT('',(64.7902651077865,243.315469527519,25.8366900749965)) ;
#107224 = CARTESIAN_POINT('',(64.7902651077865,245.531072887114,24.2269600090591)) ;
#107225 = CARTESIAN_POINT('',(64.9402651077865,243.400632319557,25.9602258814026)) ;
#107226 = CARTESIAN_POINT('',(64.9402651077865,245.619240674958,24.3483125582154)) ;
#107227 = CARTESIAN_POINT('Ctrl Pts',(64.9402651077865,243.400632319557,25.9602258814026)) ;
#107228 = CARTESIAN_POINT('Ctrl Pts',(64.9402651077865,243.399807320561,25.9590229387353)) ;
#107229 = CARTESIAN_POINT('Ctrl Pts',(64.940243846551,243.398982263143,25.957820129938)) ;
#107230 = CARTESIAN_POINT('Ctrl Pts',(64.9402013305491,243.398157412359,25.9566178371379)) ;
#107231 = CARTESIAN_POINT('Ctrl Pts',(64.9396551395109,243.387560787867,25.9411723219294)) ;
#107232 = CARTESIAN_POINT('Ctrl Pts',(64.9356062703199,243.377098235264,25.9259582673101)) ;
#107233 = CARTESIAN_POINT('Ctrl Pts',(64.928263675975,243.36731840212,25.9117600448446)) ;
#107234 = CARTESIAN_POINT('Ctrl Pts',(64.9206090302591,243.357122937907,25.8969584151121)) ;
#107235 = CARTESIAN_POINT('Ctrl Pts',(64.9095180038062,243.347860571349,25.8835376386856)) ;
#107236 = CARTESIAN_POINT('Ctrl Pts',(64.8956136387305,243.340061292121,25.8722475987307)) ;
#107237 = CARTESIAN_POINT('Ctrl Pts',(64.8817129938793,243.332264099653,25.8609605795167)) ;
#107238 = CARTESIAN_POINT('Ctrl Pts',(64.8652664191737,243.326078599533,25.8520189483946)) ;
#107239 = CARTESIAN_POINT('Ctrl Pts',(64.8471986491033,243.321859600104,25.845921961251)) ;
#107240 = CARTESIAN_POINT('Ctrl Pts',(64.8291331055125,243.31764112058,25.8398257254351)) ;
#107241 = CARTESIAN_POINT('Ctrl Pts',(64.8097925816885,243.315469527519,25.8366900749965)) ;
#107242 = CARTESIAN_POINT('Ctrl Pts',(64.7902651077865,243.31546952752,25.836690074996)) ;
#107243 = CARTESIAN_POINT('Origin',(64.7902651077865,243.590671638724,26.2541392311682)) ;
#107244 = CARTESIAN_POINT('',(64.7902651077865,243.902647249673,26.6448708758722)) ;
#107245 = CARTESIAN_POINT('Origin',(64.7902651077865,243.590671638724,26.2541392311682)) ;
#107246 = CARTESIAN_POINT('',(64.9402651077865,243.811474466023,26.5257015839659)) ;
#107247 = CARTESIAN_POINT('Origin',(64.9402651077865,243.590671638724,26.2541392311682)) ;
#107248 = CARTESIAN_POINT('Ctrl Pts',(64.9402651077865,243.811474466023,26.5257015839661)) ;
#107249 = CARTESIAN_POINT('Ctrl Pts',(64.9402651077865,243.812363593775,26.5268579343641)) ;
#107250 = CARTESIAN_POINT('Ctrl Pts',(64.940243846551,243.813252576156,26.5280142989584)) ;
#107251 = CARTESIAN_POINT('Ctrl Pts',(64.9402013305491,243.814141131648,26.5291703075783)) ;
#107252 = CARTESIAN_POINT('Ctrl Pts',(64.9396551395109,243.82555615249,26.5440212230313)) ;
#107253 = CARTESIAN_POINT('Ctrl Pts',(64.9356062703199,243.836792471709,26.5586731032994)) ;
#107254 = CARTESIAN_POINT('Ctrl Pts',(64.928263675975,243.847273649061,26.5723617693703)) ;
#107255 = CARTESIAN_POINT('Ctrl Pts',(64.9206090302593,243.858200263763,26.586632187178)) ;
#107256 = CARTESIAN_POINT('Ctrl Pts',(64.9095180038064,243.868101951963,26.5995884692429)) ;
#107257 = CARTESIAN_POINT('Ctrl Pts',(64.8956136387305,243.876429308206,26.6104948387885)) ;
#107258 = CARTESIAN_POINT('Ctrl Pts',(64.8817129938791,243.884754436398,26.6213982902475)) ;
#107259 = CARTESIAN_POINT('Ctrl Pts',(64.8652664191736,243.891347008287,26.6300441664173)) ;
#107260 = CARTESIAN_POINT('Ctrl Pts',(64.8471986491033,243.895841845116,26.6359407459585)) ;
#107261 = CARTESIAN_POINT('Ctrl Pts',(64.8291331055124,243.90033612805,26.6418365988681)) ;
#107262 = CARTESIAN_POINT('Ctrl Pts',(64.8097925816883,243.902647249673,26.6448708758722)) ;
#107263 = CARTESIAN_POINT('Ctrl Pts',(64.7902651077866,243.902647249673,26.6448708758723)) ;
#107264 = CARTESIAN_POINT('Origin',(64.7902651077865,246.314586318022,24.7070843711341)) ;
#107265 = CARTESIAN_POINT('',(64.7902651077865,244.227702856188,26.4087041537722)) ;
#107266 = CARTESIAN_POINT('',(64.7902651077865,246.402754105866,24.8284369202904)) ;
#107267 = CARTESIAN_POINT('',(64.9402651077865,244.251045551402,26.2063344963562)) ;
#107268 = CARTESIAN_POINT('',(64.9402651077865,246.314586318022,24.7070843711341)) ;
#107269 = CARTESIAN_POINT('Ctrl Pts',(64.9402651077865,244.251045551402,26.2063344963562)) ;
#107270 = CARTESIAN_POINT('Ctrl Pts',(64.9402651077865,244.250949761119,26.2071173906402)) ;
#107271 = CARTESIAN_POINT('Ctrl Pts',(64.940261777681,244.250854033933,26.2079002983041)) ;
#107272 = CARTESIAN_POINT('Ctrl Pts',(64.9400834366345,244.248293193181,26.228858375676)) ;
#107273 = CARTESIAN_POINT('Ctrl Pts',(64.9376982652988,244.245861997565,26.2491150850256)) ;
#107274 = CARTESIAN_POINT('Ctrl Pts',(64.9285249168183,244.241329085551,26.2875316783901)) ;
#107275 = CARTESIAN_POINT('Ctrl Pts',(64.9218878905887,244.239197738625,26.3059144577853)) ;
#107276 = CARTESIAN_POINT('Ctrl Pts',(64.9030518920066,244.235073687307,26.3420097767375)) ;
#107277 = CARTESIAN_POINT('Ctrl Pts',(64.8902415596279,244.233103468073,26.3595913933363)) ;
#107278 = CARTESIAN_POINT('Ctrl Pts',(64.862223450516,244.230274122543,26.3851292535788)) ;
#107279 = CARTESIAN_POINT('Ctrl Pts',(64.8483068832619,244.229274861868,26.3942624232202)) ;
#107280 = CARTESIAN_POINT('Ctrl Pts',(64.8193104176513,244.228015421459,26.4058155998437)) ;
#107281 = CARTESIAN_POINT('Ctrl Pts',(64.8049443310403,244.227702856188,26.4087041537722)) ;
#107282 = CARTESIAN_POINT('Ctrl Pts',(64.7902651077865,244.227702856188,26.4087041537722)) ;
#107283 = CARTESIAN_POINT('Origin',(64.7902651077865,248.040265107786,23.0213203435596)) ;
#107284 = CARTESIAN_POINT('',(64.7902651077865,244.652881297574,26.8338825951576)) ;
#107285 = CARTESIAN_POINT('Origin',(64.7902651077865,248.040265107786,23.0213203435596)) ;
#107286 = CARTESIAN_POINT('',(64.9402651077865,244.85525095499,26.8105398999439)) ;
#107287 = CARTESIAN_POINT('Origin',(64.9402651077865,248.040265107786,23.0213203435596)) ;
#107288 = CARTESIAN_POINT('Ctrl Pts',(64.9402651077865,244.85525095499,26.8105398999439)) ;
#107289 = CARTESIAN_POINT('Ctrl Pts',(64.9402651077865,244.854468060706,26.8106356902274)) ;
#107290 = CARTESIAN_POINT('Ctrl Pts',(64.940261777681,244.853685153042,26.8107314174129)) ;
#107291 = CARTESIAN_POINT('Ctrl Pts',(64.9400834366345,244.832727075669,26.8132922581644)) ;
#107292 = CARTESIAN_POINT('Ctrl Pts',(64.9376982652987,244.81247036632,26.8157234537813)) ;
#107293 = CARTESIAN_POINT('Ctrl Pts',(64.9285249168183,244.774053772956,26.8202563657947)) ;
#107294 = CARTESIAN_POINT('Ctrl Pts',(64.9218878905887,244.755670993561,26.8223877127213)) ;
#107295 = CARTESIAN_POINT('Ctrl Pts',(64.9030518920066,244.719575674608,26.8265117640394)) ;
#107296 = CARTESIAN_POINT('Ctrl Pts',(64.890241559628,244.70199405801,26.8284819832727)) ;
#107297 = CARTESIAN_POINT('Ctrl Pts',(64.862223450516,244.676456197767,26.8313113288033)) ;
#107298 = CARTESIAN_POINT('Ctrl Pts',(64.8483068832619,244.667323028126,26.832310589478)) ;
#107299 = CARTESIAN_POINT('Ctrl Pts',(64.8193104176514,244.655769851502,26.8335700298872)) ;
#107300 = CARTESIAN_POINT('Ctrl Pts',(64.8049443310404,244.652881297574,26.8338825951576)) ;
#107301 = CARTESIAN_POINT('Ctrl Pts',(64.7902651077866,244.652881297574,26.8338825951576)) ;
#107302 = CARTESIAN_POINT('Origin',(64.7902651077865,246.147797190567,25.0315026299217)) ;
#107303 = CARTESIAN_POINT('',(64.7902651077865,244.416714575474,27.1589382016729)) ;
#107304 = CARTESIAN_POINT('',(64.7902651077865,246.026444641411,24.9433348420779)) ;
#107305 = CARTESIAN_POINT('',(64.9402651077865,244.53588386738,27.2501109853235)) ;
#107306 = CARTESIAN_POINT('',(64.9402651077865,246.147797190567,25.0315026299217)) ;
#107307 = CARTESIAN_POINT('Ctrl Pts',(64.9402651077865,244.53588386738,27.2501109853235)) ;
#107308 = CARTESIAN_POINT('Ctrl Pts',(64.9402651077865,244.534727516982,27.2492218575712)) ;
#107309 = CARTESIAN_POINT('Ctrl Pts',(64.940243846551,244.533571152388,27.2483328751903)) ;
#107310 = CARTESIAN_POINT('Ctrl Pts',(64.9402013305491,244.532415143768,27.2474443196982)) ;
#107311 = CARTESIAN_POINT('Ctrl Pts',(64.9396551395109,244.51756422831,27.2360292988605)) ;
#107312 = CARTESIAN_POINT('Ctrl Pts',(64.9356062703199,244.502912348047,27.2247929796359)) ;
#107313 = CARTESIAN_POINT('Ctrl Pts',(64.9282636759751,244.489223681976,27.2143118022837)) ;
#107314 = CARTESIAN_POINT('Ctrl Pts',(64.9206090302593,244.474953264168,27.2033851875822)) ;
#107315 = CARTESIAN_POINT('Ctrl Pts',(64.9095180038062,244.461996982103,27.1934834993823)) ;
#107316 = CARTESIAN_POINT('Ctrl Pts',(64.8956136387306,244.451090612558,27.1851561431395)) ;
#107317 = CARTESIAN_POINT('Ctrl Pts',(64.8817129938794,244.440187161099,27.1768310149477)) ;
#107318 = CARTESIAN_POINT('Ctrl Pts',(64.8652664191739,244.431541284929,27.1702384430589)) ;
#107319 = CARTESIAN_POINT('Ctrl Pts',(64.8471986491033,244.425644705387,27.1657436062292)) ;
#107320 = CARTESIAN_POINT('Ctrl Pts',(64.8291331055124,244.419748852478,27.1612493232953)) ;
#107321 = CARTESIAN_POINT('Ctrl Pts',(64.8097925816884,244.416714575474,27.1589382016726)) ;
#107322 = CARTESIAN_POINT('Ctrl Pts',(64.7902651077865,244.416714575474,27.1589382016725)) ;
#107323 = CARTESIAN_POINT('Origin',(64.7902651077865,244.807446220178,27.4709138126218)) ;
#107324 = CARTESIAN_POINT('',(64.7902651077865,245.224895376349,27.7461159238265)) ;
#107325 = CARTESIAN_POINT('Origin',(64.7902651077865,244.807446220178,27.4709138126218)) ;
#107326 = CARTESIAN_POINT('',(64.9402651077865,245.101359569943,27.6609531317891)) ;
#107327 = CARTESIAN_POINT('Origin',(64.9402651077865,244.807446220178,27.4709138126218)) ;
#107328 = CARTESIAN_POINT('Ctrl Pts',(64.9402651077865,245.101359569948,27.6609531317925)) ;
#107329 = CARTESIAN_POINT('Ctrl Pts',(64.9402651077864,245.102562512614,27.6617781307873)) ;
#107330 = CARTESIAN_POINT('Ctrl Pts',(64.9402438465509,245.10376532141,27.6626031882038)) ;
#107331 = CARTESIAN_POINT('Ctrl Pts',(64.9402013305491,245.104967614209,27.663428038987)) ;
#107332 = CARTESIAN_POINT('Ctrl Pts',(64.9396551395108,245.120413129416,27.6740246634796)) ;
#107333 = CARTESIAN_POINT('Ctrl Pts',(64.9356062703197,245.135627184036,27.6844872160823)) ;
#107334 = CARTESIAN_POINT('Ctrl Pts',(64.9282636759749,245.149825406501,27.6942670492256)) ;
#107335 = CARTESIAN_POINT('Ctrl Pts',(64.9206090302591,245.164627036234,27.7044625134384)) ;
#107336 = CARTESIAN_POINT('Ctrl Pts',(64.9095180038063,245.17804781266,27.7137248799967)) ;
#107337 = CARTESIAN_POINT('Ctrl Pts',(64.8956136387305,245.189337852615,27.7215241592249)) ;
#107338 = CARTESIAN_POINT('Ctrl Pts',(64.8817129938791,245.200624871829,27.7293213516933)) ;
#107339 = CARTESIAN_POINT('Ctrl Pts',(64.8652664191736,245.209566502951,27.7355068518133)) ;
#107340 = CARTESIAN_POINT('Ctrl Pts',(64.8471986491032,245.215663490095,27.7397258512423)) ;
#107341 = CARTESIAN_POINT('Ctrl Pts',(64.8291331055125,245.22175972591,27.7439443307667)) ;
#107342 = CARTESIAN_POINT('Ctrl Pts',(64.8097925816882,245.224895376349,27.7461159238267)) ;
#107343 = CARTESIAN_POINT('Ctrl Pts',(64.7902651077865,245.22489537635,27.7461159238262)) ;
#107344 = CARTESIAN_POINT('Origin',(64.7902651077865,246.919976782775,25.1578412797899)) ;
#107345 = CARTESIAN_POINT('',(64.7902651077865,247.041329331931,25.2460090676338)) ;
#107346 = CARTESIAN_POINT('',(64.9402651077865,246.919976782775,25.1578412797899)) ;
#107347 = CARTESIAN_POINT('Origin',(60.4402651077865,250.207872219281,17.9664732232009)) ;
#107348 = CARTESIAN_POINT('',(60.5902651077865,250.207872219281,17.9664732232009)) ;
#107349 = CARTESIAN_POINT('',(60.4402651077865,250.207872219281,17.9664732232009)) ;
#107350 = CARTESIAN_POINT('',(60.5902651077865,250.083712025826,18.3485990065702)) ;
#107351 = CARTESIAN_POINT('',(60.5902651077865,249.361587041504,20.5710711826001)) ;
#107352 = CARTESIAN_POINT('',(60.4402651077865,250.083712025826,18.3485990065702)) ;
#107353 = CARTESIAN_POINT('Origin',(60.4402651077865,249.739858576849,17.7905095039363)) ;
#107354 = CARTESIAN_POINT('',(60.5902651077865,249.257798707399,17.6577756263215)) ;
#107355 = CARTESIAN_POINT('',(60.4402651077865,249.257798707399,17.6577756263215)) ;
#107356 = CARTESIAN_POINT('Origin',(60.5902651077865,249.739858576849,17.7905095039363)) ;
#107357 = CARTESIAN_POINT('Origin',(60.4402651077865,249.040457375835,18.3266834644245)) ;
#107358 = CARTESIAN_POINT('',(60.5902651077865,249.133638513944,18.0399014096908)) ;
#107359 = CARTESIAN_POINT('',(60.4402651077865,249.133638513944,18.0399014096908)) ;
#107360 = CARTESIAN_POINT('',(60.5902651077865,248.30284286384,20.5968275047722)) ;
#107361 = CARTESIAN_POINT('Origin',(60.4402651077865,248.040265107786,23.0213203435596)) ;
#107362 = CARTESIAN_POINT('',(60.5902651077865,248.539748311783,17.9458384424072)) ;
#107363 = CARTESIAN_POINT('',(60.4402651077865,248.539748311783,17.9458384424072)) ;
#107364 = CARTESIAN_POINT('Origin',(60.5902651077865,248.040265107786,23.0213203435596)) ;
#107365 = CARTESIAN_POINT('Origin',(60.4402651077865,248.539748311783,17.5440476162869)) ;
#107366 = CARTESIAN_POINT('',(60.5902651077865,248.539748311783,17.5440476162869)) ;
#107367 = CARTESIAN_POINT('',(60.4402651077865,248.539748311783,17.5440476162869)) ;
#107368 = CARTESIAN_POINT('',(60.5902651077865,248.539748311783,20.2826839799233)) ;
#107369 = CARTESIAN_POINT('Origin',(60.4402651077865,248.040265107786,17.5213203435596)) ;
#107370 = CARTESIAN_POINT('',(60.5902651077865,247.54078190379,17.5440476162869)) ;
#107371 = CARTESIAN_POINT('',(60.4402651077865,247.54078190379,17.5440476162869)) ;
#107372 = CARTESIAN_POINT('Origin',(60.5902651077865,248.040265107786,17.5213203435596)) ;
#107373 = CARTESIAN_POINT('Origin',(60.4402651077865,247.54078190379,18.2473789395491)) ;
#107374 = CARTESIAN_POINT('',(60.5902651077865,247.54078190379,17.9458384424072)) ;
#107375 = CARTESIAN_POINT('',(60.4402651077865,247.54078190379,17.9458384424072)) ;
#107376 = CARTESIAN_POINT('',(60.5902651077865,247.54078190379,20.6343496415544)) ;
#107377 = CARTESIAN_POINT('Origin',(60.4402651077865,248.040265107786,23.0213203435596)) ;
#107378 = CARTESIAN_POINT('',(60.5902651077865,246.946891701628,18.0399014096908)) ;
#107379 = CARTESIAN_POINT('',(60.4402651077865,246.946891701628,18.0399014096908)) ;
#107380 = CARTESIAN_POINT('Origin',(60.5902651077865,248.040265107786,23.0213203435596)) ;
#107381 = CARTESIAN_POINT('Origin',(60.4402651077865,246.822731508173,17.6577756263215)) ;
#107382 = CARTESIAN_POINT('',(60.5902651077865,246.822731508173,17.6577756263215)) ;
#107383 = CARTESIAN_POINT('',(60.4402651077865,246.822731508173,17.6577756263215)) ;
#107384 = CARTESIAN_POINT('',(60.5902651077865,247.66901668595,20.2623735857207)) ;
#107385 = CARTESIAN_POINT('Origin',(60.4402651077865,246.340671638724,17.7905095039363)) ;
#107386 = CARTESIAN_POINT('',(60.5902651077865,245.872657996292,17.9664732232009)) ;
#107387 = CARTESIAN_POINT('',(60.4402651077865,245.872657996292,17.9664732232009)) ;
#107388 = CARTESIAN_POINT('Origin',(60.5902651077865,246.340671638724,17.7905095039363)) ;
#107389 = CARTESIAN_POINT('Origin',(60.4402651077865,246.089999327856,18.6353810613039)) ;
#107390 = CARTESIAN_POINT('',(60.5902651077865,245.996818189747,18.3485990065702)) ;
#107391 = CARTESIAN_POINT('',(60.4402651077865,245.996818189747,18.3485990065702)) ;
#107392 = CARTESIAN_POINT('',(60.5902651077865,246.827613839851,20.9055251016516)) ;
#107393 = CARTESIAN_POINT('Origin',(60.4402651077865,248.040265107786,23.0213203435596)) ;
#107394 = CARTESIAN_POINT('',(60.5902651077865,245.461062098449,18.6215803698081)) ;
#107395 = CARTESIAN_POINT('',(60.4402651077865,245.461062098449,18.6215803698081)) ;
#107396 = CARTESIAN_POINT('Origin',(60.5902651077865,248.040265107786,23.0213203435596)) ;
#107397 = CARTESIAN_POINT('Origin',(60.4402651077865,245.224895376349,18.2965247632928)) ;
#107398 = CARTESIAN_POINT('',(60.5902651077865,245.224895376349,18.2965247632928)) ;
#107399 = CARTESIAN_POINT('',(60.4402651077865,245.224895376349,18.2965247632928)) ;
#107400 = CARTESIAN_POINT('',(60.5902651077865,246.834625442287,20.5121281228878)) ;
#107401 = CARTESIAN_POINT('Origin',(60.4402651077865,244.807446220178,18.5717268744974)) ;
#107402 = CARTESIAN_POINT('',(60.5902651077865,244.416714575474,18.8837024854464)) ;
#107403 = CARTESIAN_POINT('',(60.4402651077865,244.416714575474,18.8837024854464)) ;
#107404 = CARTESIAN_POINT('Origin',(60.5902651077865,244.807446220178,18.5717268744974)) ;
#107405 = CARTESIAN_POINT('Origin',(60.4402651077865,244.830122354763,19.4527094786418)) ;
#107406 = CARTESIAN_POINT('',(60.5902651077865,244.652881297574,19.2087580919617)) ;
#107407 = CARTESIAN_POINT('',(60.4402651077865,244.652881297574,19.2087580919617)) ;
#107408 = CARTESIAN_POINT('',(60.5902651077865,246.233148531056,21.3838093416391)) ;
#107409 = CARTESIAN_POINT('Origin',(60.4402651077865,248.040265107786,23.0213203435596)) ;
#107410 = CARTESIAN_POINT('',(60.5902651077865,244.227702856188,19.633936533347)) ;
#107411 = CARTESIAN_POINT('',(60.4402651077865,244.227702856188,19.633936533347)) ;
#107412 = CARTESIAN_POINT('Origin',(60.5902651077865,248.040265107786,23.0213203435596)) ;
#107413 = CARTESIAN_POINT('Origin',(60.4402651077865,243.902647249673,19.3977698112471)) ;
#107414 = CARTESIAN_POINT('',(60.5902651077865,243.902647249673,19.3977698112471)) ;
#107415 = CARTESIAN_POINT('',(60.4402651077865,243.902647249673,19.3977698112471)) ;
#107416 = CARTESIAN_POINT('',(60.5902651077865,246.118250609268,21.0074998771845)) ;
#107417 = CARTESIAN_POINT('Origin',(60.4402651077865,243.590671638724,19.788501455951)) ;
#107418 = CARTESIAN_POINT('',(60.5902651077865,243.315469527519,20.2059506121228)) ;
#107419 = CARTESIAN_POINT('',(60.4402651077865,243.315469527519,20.2059506121228)) ;
#107420 = CARTESIAN_POINT('Origin',(60.5902651077865,243.590671638724,19.788501455951)) ;
#107421 = CARTESIAN_POINT('Origin',(60.4402651077865,243.884476520715,20.6193583914117)) ;
#107422 = CARTESIAN_POINT('',(60.5902651077865,243.640525134035,20.4421173342227)) ;
#107423 = CARTESIAN_POINT('',(60.4402651077865,243.640525134035,20.4421173342227)) ;
#107424 = CARTESIAN_POINT('',(60.5902651077865,245.815576383712,22.0223845677046)) ;
#107425 = CARTESIAN_POINT('Origin',(60.4402651077865,248.040265107786,23.0213203435596)) ;
#107426 = CARTESIAN_POINT('',(60.5902651077865,243.367543770797,20.9778734255204)) ;
#107427 = CARTESIAN_POINT('',(60.4402651077865,243.367543770797,20.9778734255204)) ;
#107428 = CARTESIAN_POINT('Origin',(60.5902651077865,248.040265107786,23.0213203435596)) ;
#107429 = CARTESIAN_POINT('Origin',(60.4402651077865,242.985417987428,20.8537132320653)) ;
#107430 = CARTESIAN_POINT('',(60.5902651077865,242.985417987428,20.8537132320653)) ;
#107431 = CARTESIAN_POINT('',(60.4402651077865,242.985417987428,20.8537132320653)) ;
#107432 = CARTESIAN_POINT('',(60.5902651077865,245.590015946827,21.6999984098422)) ;
#107433 = CARTESIAN_POINT('Origin',(60.4402651077865,242.809454268163,21.3217268744974)) ;
#107434 = CARTESIAN_POINT('',(60.5902651077865,242.676720390548,21.8037867439466)) ;
#107435 = CARTESIAN_POINT('',(60.4402651077865,242.676720390548,21.8037867439466)) ;
#107436 = CARTESIAN_POINT('Origin',(60.5902651077865,242.809454268163,21.3217268744974)) ;
#107437 = CARTESIAN_POINT('Origin',(60.4402651077865,243.345628228651,22.0211280755108)) ;
#107438 = CARTESIAN_POINT('',(60.5902651077865,243.058846173918,21.9279469374017)) ;
#107439 = CARTESIAN_POINT('',(60.4402651077865,243.058846173918,21.9279469374017)) ;
#107440 = CARTESIAN_POINT('',(60.5902651077865,245.615772268999,22.7587425875056)) ;
#107441 = CARTESIAN_POINT('Origin',(60.4402651077865,248.040265107786,23.0213203435596)) ;
#107442 = CARTESIAN_POINT('',(60.5902651077865,242.964783206634,22.5218371395634)) ;
#107443 = CARTESIAN_POINT('',(60.4402651077865,242.964783206634,22.5218371395634)) ;
#107444 = CARTESIAN_POINT('Origin',(60.5902651077865,248.040265107786,23.0213203435596)) ;
#107445 = CARTESIAN_POINT('Origin',(60.4402651077865,242.562992380514,22.5218371395634)) ;
#107446 = CARTESIAN_POINT('',(60.5902651077865,242.562992380514,22.5218371395634)) ;
#107447 = CARTESIAN_POINT('',(60.4402651077865,242.562992380514,22.5218371395634)) ;
#107448 = CARTESIAN_POINT('',(60.5902651077865,245.30162874415,22.5218371395634)) ;
#107449 = CARTESIAN_POINT('Origin',(60.4402651077865,242.540265107786,23.0213203435596)) ;
#107450 = CARTESIAN_POINT('',(60.5902651077865,242.562992380514,23.5208035475559)) ;
#107451 = CARTESIAN_POINT('',(60.4402651077865,242.562992380514,23.5208035475559)) ;
#107452 = CARTESIAN_POINT('Origin',(60.5902651077865,242.540265107786,23.0213203435596)) ;
#107453 = CARTESIAN_POINT('Origin',(60.4402651077865,243.266323703776,23.5208035475559)) ;
#107454 = CARTESIAN_POINT('',(60.5902651077865,242.964783206634,23.5208035475559)) ;
#107455 = CARTESIAN_POINT('',(60.4402651077865,242.964783206634,23.5208035475559)) ;
#107456 = CARTESIAN_POINT('',(60.5902651077865,245.653294405781,23.5208035475559)) ;
#107457 = CARTESIAN_POINT('Origin',(60.4402651077865,248.040265107786,23.0213203435596)) ;
#107458 = CARTESIAN_POINT('',(60.5902651077865,243.058846173918,24.1146937497175)) ;
#107459 = CARTESIAN_POINT('',(60.4402651077865,243.058846173918,24.1146937497175)) ;
#107460 = CARTESIAN_POINT('Origin',(60.5902651077865,248.040265107786,23.0213203435596)) ;
#107461 = CARTESIAN_POINT('Origin',(60.4402651077865,242.676720390548,24.2388539431727)) ;
#107462 = CARTESIAN_POINT('',(60.5902651077865,242.676720390548,24.2388539431727)) ;
#107463 = CARTESIAN_POINT('',(60.4402651077865,242.676720390548,24.2388539431727)) ;
#107464 = CARTESIAN_POINT('',(60.5902651077865,245.281318349947,23.3925687653958)) ;
#107465 = CARTESIAN_POINT('Origin',(60.4402651077865,242.809454268163,24.7209138126218)) ;
#107466 = CARTESIAN_POINT('',(60.5902651077865,242.985417987428,25.188927455054)) ;
#107467 = CARTESIAN_POINT('',(60.4402651077865,242.985417987428,25.188927455054)) ;
#107468 = CARTESIAN_POINT('Origin',(60.5902651077865,242.809454268163,24.7209138126218)) ;
#107469 = CARTESIAN_POINT('Origin',(60.4402651077865,243.654325825531,24.9715861234897)) ;
#107470 = CARTESIAN_POINT('',(60.5902651077865,243.367543770797,25.0647672615988)) ;
#107471 = CARTESIAN_POINT('',(60.4402651077865,243.367543770797,25.0647672615988)) ;
#107472 = CARTESIAN_POINT('',(60.5902651077865,245.924469865878,24.233971611495)) ;
#107473 = CARTESIAN_POINT('Origin',(60.4402651077865,248.040265107786,23.0213203435596)) ;
#107474 = CARTESIAN_POINT('',(60.5902651077865,243.640525134035,25.6005233528965)) ;
#107475 = CARTESIAN_POINT('',(60.4402651077865,243.640525134035,25.6005233528965)) ;
#107476 = CARTESIAN_POINT('Origin',(60.5902651077865,248.040265107786,23.0213203435596)) ;
#107477 = CARTESIAN_POINT('Origin',(60.4402651077865,243.315469527519,25.8366900749965)) ;
#107478 = CARTESIAN_POINT('',(60.5902651077865,243.315469527519,25.8366900749965)) ;
#107479 = CARTESIAN_POINT('',(60.4402651077865,243.315469527519,25.8366900749965)) ;
#107480 = CARTESIAN_POINT('',(60.5902651077865,245.531072887114,24.2269600090591)) ;
#107481 = CARTESIAN_POINT('Origin',(60.4402651077865,243.590671638724,26.2541392311682)) ;
#107482 = CARTESIAN_POINT('',(60.5902651077865,243.902647249673,26.6448708758722)) ;
#107483 = CARTESIAN_POINT('',(60.4402651077865,243.902647249673,26.6448708758722)) ;
#107484 = CARTESIAN_POINT('Origin',(60.5902651077865,243.590671638724,26.2541392311682)) ;
#107485 = CARTESIAN_POINT('Origin',(60.4402651077865,244.471654242868,26.2314630965833)) ;
#107486 = CARTESIAN_POINT('',(60.5902651077865,244.227702856188,26.4087041537722)) ;
#107487 = CARTESIAN_POINT('',(60.4402651077865,244.227702856188,26.4087041537722)) ;
#107488 = CARTESIAN_POINT('',(60.5902651077865,246.402754105866,24.8284369202904)) ;
#107489 = CARTESIAN_POINT('Origin',(60.4402651077865,248.040265107786,23.0213203435596)) ;
#107490 = CARTESIAN_POINT('',(60.5902651077865,244.652881297574,26.8338825951576)) ;
#107491 = CARTESIAN_POINT('',(60.4402651077865,244.652881297574,26.8338825951576)) ;
#107492 = CARTESIAN_POINT('Origin',(60.5902651077865,248.040265107786,23.0213203435596)) ;
#107493 = CARTESIAN_POINT('Origin',(60.4402651077865,244.416714575474,27.1589382016729)) ;
#107494 = CARTESIAN_POINT('',(60.5902651077865,244.416714575474,27.1589382016729)) ;
#107495 = CARTESIAN_POINT('',(60.4402651077865,244.416714575474,27.1589382016729)) ;
#107496 = CARTESIAN_POINT('',(60.5902651077865,246.026444641411,24.9433348420779)) ;
#107497 = CARTESIAN_POINT('Origin',(60.4402651077865,244.807446220178,27.4709138126218)) ;
#107498 = CARTESIAN_POINT('',(60.5902651077865,245.224895376349,27.7461159238265)) ;
#107499 = CARTESIAN_POINT('',(60.4402651077865,245.224895376349,27.7461159238265)) ;
#107500 = CARTESIAN_POINT('Origin',(60.5902651077865,244.807446220178,27.4709138126218)) ;
#107501 = CARTESIAN_POINT('Origin',(60.4402651077865,245.638303155638,27.1771089306311)) ;
#107502 = CARTESIAN_POINT('',(60.5902651077865,245.461062098449,27.4210603173112)) ;
#107503 = CARTESIAN_POINT('',(60.4402651077865,245.461062098449,27.4210603173112)) ;
#107504 = CARTESIAN_POINT('',(60.5902651077865,247.041329331931,25.2460090676338)) ;
#107505 = CARTESIAN_POINT('Origin',(60.4402651077865,248.040265107786,23.0213203435596)) ;
#107506 = CARTESIAN_POINT('',(60.5902651077865,245.996818189747,27.694041680549)) ;
#107507 = CARTESIAN_POINT('',(60.4402651077865,245.996818189747,27.694041680549)) ;
#107508 = CARTESIAN_POINT('Origin',(60.5902651077865,248.040265107786,23.0213203435596)) ;
#107509 = CARTESIAN_POINT('Origin',(64.9402651077865,248.040265107786,23.0213203435596)) ;
#107510 = CARTESIAN_POINT('Origin',(64.9402651077865,248.040265107786,23.0213203435596)) ;
#107511 = CARTESIAN_POINT('Origin',(64.9402651077865,248.040265107786,23.0213203435596)) ;
#107512 = CARTESIAN_POINT('Origin',(64.9402651077865,248.040265107786,23.0213203435596)) ;
#107513 = CARTESIAN_POINT('Origin',(64.9402651077865,248.040265107786,23.0213203435596)) ;
#107514 = CARTESIAN_POINT('Origin',(64.9402651077865,248.040265107786,23.0213203435596)) ;
#107515 = CARTESIAN_POINT('Origin',(64.9402651077865,248.040265107786,23.0213203435596)) ;
#107516 = CARTESIAN_POINT('Origin',(64.9402651077865,248.040265107786,23.0213203435596)) ;
#107517 = CARTESIAN_POINT('Origin',(64.9402651077865,248.040265107786,23.0213203435596)) ;
#107518 = CARTESIAN_POINT('Origin',(64.9402651077865,248.040265107786,23.0213203435596)) ;
#107519 = CARTESIAN_POINT('Origin',(64.9402651077865,248.040265107786,23.0213203435596)) ;
#107520 = CARTESIAN_POINT('Origin',(64.9402651077865,248.040265107786,23.0213203435596)) ;
#107521 = CARTESIAN_POINT('Origin',(64.9402651077865,248.040265107786,23.0213203435596)) ;
#107522 = CARTESIAN_POINT('Origin',(64.9402651077865,248.040265107786,23.0213203435596)) ;
#107523 = CARTESIAN_POINT('Origin',(64.9402651077865,248.040265107786,23.0213203435596)) ;
#107524 = CARTESIAN_POINT('Origin',(64.9402651077865,248.040265107786,23.0213203435596)) ;
#107525 = CARTESIAN_POINT('Origin',(64.9402651077865,248.040265107786,23.0213203435596)) ;
#107526 = CARTESIAN_POINT('Origin',(64.9402651077865,248.040265107786,23.0213203435596)) ;
#107527 = CARTESIAN_POINT('Origin',(64.9402651077865,248.040265107786,23.0213203435596)) ;
#107528 = CARTESIAN_POINT('Origin',(64.9402651077865,248.040265107786,23.0213203435596)) ;
#107529 = CARTESIAN_POINT('Origin',(64.9402651077865,248.040265107786,23.0213203435596)) ;
#107530 = CARTESIAN_POINT('Origin',(64.9402651077865,248.040265107786,23.0213203435596)) ;
#107531 = CARTESIAN_POINT('Origin',(64.9402651077865,248.040265107786,23.0213203435596)) ;
#107532 = CARTESIAN_POINT('Origin',(64.9402651077865,248.040265107786,23.0213203435596)) ;
#107533 = CARTESIAN_POINT('Origin',(64.9402651077865,248.040265107786,23.0213203435596)) ;
#107534 = CARTESIAN_POINT('Origin',(64.9402651077865,248.040265107786,23.0213203435596)) ;
#107535 = CARTESIAN_POINT('Origin',(64.9402651077865,248.040265107786,23.0213203435596)) ;
#107536 = CARTESIAN_POINT('Origin',(64.9402651077865,248.040265107786,23.0213203435596)) ;
#107537 = CARTESIAN_POINT('Origin',(64.9402651077865,248.040265107786,23.0213203435596)) ;
#107538 = CARTESIAN_POINT('Origin',(64.9402651077865,248.040265107786,23.0213203435596)) ;
#107539 = CARTESIAN_POINT('Origin',(64.9402651077865,248.040265107786,23.0213203435596)) ;
#107540 = CARTESIAN_POINT('Origin',(64.9402651077865,248.040265107786,23.0213203435596)) ;
#107541 = CARTESIAN_POINT('Origin',(64.9402651077865,248.040265107786,23.0213203435596)) ;
#107542 = CARTESIAN_POINT('Origin',(64.9402651077865,248.040265107786,23.0213203435596)) ;
#107543 = CARTESIAN_POINT('Origin',(64.9402651077865,248.040265107786,23.0213203435596)) ;
#107544 = CARTESIAN_POINT('Origin',(64.9402651077865,248.040265107786,23.0213203435596)) ;
#107545 = CARTESIAN_POINT('Origin',(64.9402651077865,248.040265107786,23.0213203435596)) ;
#107546 = CARTESIAN_POINT('',(64.9402651077865,248.040265107786,27.9713203435596)) ;
#107547 = CARTESIAN_POINT('Origin',(64.9402651077865,248.040265107786,23.0213203435596)) ;
#107548 = CARTESIAN_POINT('Origin',(64.9402651077865,248.040265107786,23.0213203435596)) ;
#107549 = CARTESIAN_POINT('Origin',(65.0902651077865,248.040265107786,23.0213203435596)) ;
#107550 = CARTESIAN_POINT('Origin',(65.0902651077865,248.040265107786,27.9713203435596)) ;
#107551 = CARTESIAN_POINT('Origin',(64.9402651077865,248.040265107786,23.0213203435596)) ;
#107552 = CARTESIAN_POINT('Origin',(64.9402651077865,248.040265107786,23.0213203435596)) ;
#107553 = CARTESIAN_POINT('Origin',(60.2902651077865,248.040265107786,23.0213203435596)) ;
#107554 = CARTESIAN_POINT('',(60.4402651077865,248.040265107786,18.0713203435596)) ;
#107555 = CARTESIAN_POINT('Origin',(60.2902651077865,248.040265107786,18.0713203435596)) ;
#107556 = CARTESIAN_POINT('',(60.4402651077865,247.69078190379,18.0836729796702)) ;
#107557 = CARTESIAN_POINT('Origin',(60.4402651077865,248.040265107786,23.0213203435596)) ;
#107558 = CARTESIAN_POINT('',(60.4402651077865,246.84682643861,18.2173423936815)) ;
#107559 = CARTESIAN_POINT('Origin',(60.4402651077865,248.040265107786,23.0213203435596)) ;
#107560 = CARTESIAN_POINT('',(60.4402651077865,246.182069881617,18.4333348922484)) ;
#107561 = CARTESIAN_POINT('Origin',(60.4402651077865,248.040265107786,23.0213203435596)) ;
#107562 = CARTESIAN_POINT('',(60.4402651077865,245.420726657553,18.8212586407095)) ;
#107563 = CARTESIAN_POINT('Origin',(60.4402651077865,248.040265107786,23.0213203435596)) ;
#107564 = CARTESIAN_POINT('',(60.4402651077865,244.85525095499,19.2321007871753)) ;
#107565 = CARTESIAN_POINT('Origin',(60.4402651077865,248.040265107786,23.0213203435596)) ;
#107566 = CARTESIAN_POINT('',(60.4402651077865,244.251045551402,19.836306190763)) ;
#107567 = CARTESIAN_POINT('Origin',(60.4402651077865,248.040265107786,23.0213203435596)) ;
#107568 = CARTESIAN_POINT('',(60.4402651077865,243.840203404936,20.4017818933262)) ;
#107569 = CARTESIAN_POINT('Origin',(60.4402651077865,248.040265107786,23.0213203435596)) ;
#107570 = CARTESIAN_POINT('',(60.4402651077865,243.452279656475,21.1631251173908)) ;
#107571 = CARTESIAN_POINT('Origin',(60.4402651077865,248.040265107786,23.0213203435596)) ;
#107572 = CARTESIAN_POINT('',(60.4402651077865,243.236287157908,21.8278816743835)) ;
#107573 = CARTESIAN_POINT('Origin',(60.4402651077865,248.040265107786,23.0213203435596)) ;
#107574 = CARTESIAN_POINT('',(60.4402651077865,243.102617743897,22.6718371395634)) ;
#107575 = CARTESIAN_POINT('Origin',(60.4402651077865,248.040265107786,23.0213203435596)) ;
#107576 = CARTESIAN_POINT('',(60.4402651077865,243.102617743897,23.3708035475559)) ;
#107577 = CARTESIAN_POINT('Origin',(60.4402651077865,248.040265107786,23.0213203435596)) ;
#107578 = CARTESIAN_POINT('',(60.4402651077865,243.236287157908,24.2147590127358)) ;
#107579 = CARTESIAN_POINT('Origin',(60.4402651077865,248.040265107786,23.0213203435596)) ;
#107580 = CARTESIAN_POINT('',(60.4402651077865,243.452279656475,24.8795155697285)) ;
#107581 = CARTESIAN_POINT('Origin',(60.4402651077865,248.040265107786,23.0213203435596)) ;
#107582 = CARTESIAN_POINT('',(60.4402651077865,243.840203404936,25.6408587937931)) ;
#107583 = CARTESIAN_POINT('Origin',(60.4402651077865,248.040265107786,23.0213203435596)) ;
#107584 = CARTESIAN_POINT('',(60.4402651077865,244.251045551402,26.2063344963562)) ;
#107585 = CARTESIAN_POINT('Origin',(60.4402651077865,248.040265107786,23.0213203435596)) ;
#107586 = CARTESIAN_POINT('',(60.4402651077865,244.85525095499,26.8105398999439)) ;
#107587 = CARTESIAN_POINT('Origin',(60.4402651077865,248.040265107786,23.0213203435596)) ;
#107588 = CARTESIAN_POINT('',(60.4402651077865,245.420726657553,27.2213820464098)) ;
#107589 = CARTESIAN_POINT('Origin',(60.4402651077865,248.040265107786,23.0213203435596)) ;
#107590 = CARTESIAN_POINT('',(60.4402651077865,246.182069881617,27.6093057948708)) ;
#107591 = CARTESIAN_POINT('Origin',(60.4402651077865,248.040265107786,23.0213203435596)) ;
#107592 = CARTESIAN_POINT('',(60.4402651077865,246.84682643861,27.8252982934377)) ;
#107593 = CARTESIAN_POINT('Origin',(60.4402651077865,248.040265107786,23.0213203435596)) ;
#107594 = CARTESIAN_POINT('',(60.4402651077865,247.69078190379,27.9589677074491)) ;
#107595 = CARTESIAN_POINT('Origin',(60.4402651077865,248.040265107786,23.0213203435596)) ;
#107596 = CARTESIAN_POINT('',(60.4402651077865,248.389748311783,27.9589677074491)) ;
#107597 = CARTESIAN_POINT('Origin',(60.4402651077865,248.040265107786,23.0213203435596)) ;
#107598 = CARTESIAN_POINT('',(60.4402651077865,249.233703776962,27.8252982934377)) ;
#107599 = CARTESIAN_POINT('Origin',(60.4402651077865,248.040265107786,23.0213203435596)) ;
#107600 = CARTESIAN_POINT('',(60.4402651077865,249.898460333955,27.6093057948708)) ;
#107601 = CARTESIAN_POINT('Origin',(60.4402651077865,248.040265107786,23.0213203435596)) ;
#107602 = CARTESIAN_POINT('',(60.4402651077865,250.65980355802,27.2213820464098)) ;
#107603 = CARTESIAN_POINT('Origin',(60.4402651077865,248.040265107786,23.0213203435596)) ;
#107604 = CARTESIAN_POINT('',(60.4402651077865,251.225279260583,26.8105398999439)) ;
#107605 = CARTESIAN_POINT('Origin',(60.4402651077865,248.040265107786,23.0213203435596)) ;
#107606 = CARTESIAN_POINT('',(60.4402651077865,251.829484664171,26.2063344963563)) ;
#107607 = CARTESIAN_POINT('Origin',(60.4402651077865,248.040265107786,23.0213203435596)) ;
#107608 = CARTESIAN_POINT('',(60.4402651077865,252.240326810636,25.6408587937931)) ;
#107609 = CARTESIAN_POINT('Origin',(60.4402651077865,248.040265107786,23.0213203435596)) ;
#107610 = CARTESIAN_POINT('',(60.4402651077865,252.628250559098,24.8795155697285)) ;
#107611 = CARTESIAN_POINT('Origin',(60.4402651077865,248.040265107786,23.0213203435596)) ;
#107612 = CARTESIAN_POINT('',(60.4402651077865,252.844243057664,24.2147590127358)) ;
#107613 = CARTESIAN_POINT('Origin',(60.4402651077865,248.040265107786,23.0213203435596)) ;
#107614 = CARTESIAN_POINT('',(60.4402651077865,252.977912471676,23.3708035475559)) ;
#107615 = CARTESIAN_POINT('Origin',(60.4402651077865,248.040265107786,23.0213203435596)) ;
#107616 = CARTESIAN_POINT('',(60.4402651077865,252.977912471676,22.6718371395634)) ;
#107617 = CARTESIAN_POINT('Origin',(60.4402651077865,248.040265107786,23.0213203435596)) ;
#107618 = CARTESIAN_POINT('',(60.4402651077865,252.844243057664,21.8278816743835)) ;
#107619 = CARTESIAN_POINT('Origin',(60.4402651077865,248.040265107786,23.0213203435596)) ;
#107620 = CARTESIAN_POINT('',(60.4402651077865,252.628250559098,21.1631251173908)) ;
#107621 = CARTESIAN_POINT('Origin',(60.4402651077865,248.040265107786,23.0213203435596)) ;
#107622 = CARTESIAN_POINT('',(60.4402651077865,252.240326810636,20.4017818933262)) ;
#107623 = CARTESIAN_POINT('Origin',(60.4402651077865,248.040265107786,23.0213203435596)) ;
#107624 = CARTESIAN_POINT('',(60.4402651077865,251.829484664171,19.836306190763)) ;
#107625 = CARTESIAN_POINT('Origin',(60.4402651077865,248.040265107786,23.0213203435596)) ;
#107626 = CARTESIAN_POINT('',(60.4402651077865,251.225279260583,19.2321007871753)) ;
#107627 = CARTESIAN_POINT('Origin',(60.4402651077865,248.040265107786,23.0213203435596)) ;
#107628 = CARTESIAN_POINT('',(60.4402651077865,250.65980355802,18.8212586407095)) ;
#107629 = CARTESIAN_POINT('Origin',(60.4402651077865,248.040265107786,23.0213203435596)) ;
#107630 = CARTESIAN_POINT('',(60.4402651077865,249.898460333955,18.4333348922483)) ;
#107631 = CARTESIAN_POINT('Origin',(60.4402651077865,248.040265107786,23.0213203435596)) ;
#107632 = CARTESIAN_POINT('',(60.4402651077865,249.233703776962,18.2173423936815)) ;
#107633 = CARTESIAN_POINT('Origin',(60.4402651077865,248.040265107786,23.0213203435596)) ;
#107634 = CARTESIAN_POINT('',(60.4402651077865,248.389748311783,18.0836729796702)) ;
#107635 = CARTESIAN_POINT('Origin',(60.4402651077865,248.040265107786,23.0213203435596)) ;
#107636 = CARTESIAN_POINT('Origin',(60.4402651077865,248.040265107786,23.0213203435596)) ;
#107637 = CARTESIAN_POINT('Origin',(60.4402651077865,248.040265107786,23.0213203435596)) ;
#107638 = CARTESIAN_POINT('',(60.4402651077865,250.066361548099,17.9165880896072)) ;
#107639 = CARTESIAN_POINT('',(60.4402651077865,249.21892856406,20.5247186334439)) ;
#107640 = CARTESIAN_POINT('',(60.4402651077865,249.401604991106,17.700595591041)) ;
#107641 = CARTESIAN_POINT('Origin',(60.4402651077865,249.739858576849,17.7905095039363)) ;
#107642 = CARTESIAN_POINT('',(60.4402651077865,248.445501341285,20.6431800539285)) ;
#107643 = CARTESIAN_POINT('Origin',(60.4402651077865,248.040265107786,23.0213203435596)) ;
#107644 = CARTESIAN_POINT('',(60.4402651077865,251.544646348192,18.7925297017964)) ;
#107645 = CARTESIAN_POINT('',(60.4402651077865,249.932733025005,21.0111380571975)) ;
#107646 = CARTESIAN_POINT('',(60.4402651077865,250.979170645629,18.3816875553299)) ;
#107647 = CARTESIAN_POINT('Origin',(60.4402651077865,251.273083995395,18.5717268744974)) ;
#107648 = CARTESIAN_POINT('',(60.4402651077865,249.160553432798,20.8847994073294)) ;
#107649 = CARTESIAN_POINT('Origin',(60.4402651077865,248.040265107786,23.0213203435596)) ;
#107650 = CARTESIAN_POINT('',(60.4402651077865,252.679897896016,20.0824148057166)) ;
#107651 = CARTESIAN_POINT('',(60.4402651077865,250.461289540614,21.6943281289039)) ;
#107652 = CARTESIAN_POINT('',(60.4402651077865,252.26905574955,19.5169391031532)) ;
#107653 = CARTESIAN_POINT('Origin',(60.4402651077865,252.489858576849,19.788501455951)) ;
#107654 = CARTESIAN_POINT('',(60.4402651077865,249.765943897551,21.3355563159851)) ;
#107655 = CARTESIAN_POINT('Origin',(60.4402651077865,248.040265107786,23.0213203435596)) ;
#107656 = CARTESIAN_POINT('',(60.4402651077865,253.360989860306,21.6599804602399)) ;
#107657 = CARTESIAN_POINT('',(60.4402651077865,250.752859316469,22.5074134442792)) ;
#107658 = CARTESIAN_POINT('',(60.4402651077865,253.144997361738,20.9952239032473)) ;
#107659 = CARTESIAN_POINT('Origin',(60.4402651077865,253.27107594741,21.3217268744974)) ;
#107660 = CARTESIAN_POINT('',(60.4402651077865,250.202412898851,21.9513275530686)) ;
#107661 = CARTESIAN_POINT('Origin',(60.4402651077865,248.040265107786,23.0213203435596)) ;
#107662 = CARTESIAN_POINT('',(60.4402651077865,253.521252214148,23.3708035475559)) ;
#107663 = CARTESIAN_POINT('',(60.4402651077865,250.778901471423,23.3708035475559)) ;
#107664 = CARTESIAN_POINT('',(60.4402651077865,253.521252214148,22.6718371395634)) ;
#107665 = CARTESIAN_POINT('Origin',(60.4402651077865,253.540265107786,23.0213203435596)) ;
#107666 = CARTESIAN_POINT('',(60.4402651077865,250.427235809792,22.6718371395634)) ;
#107667 = CARTESIAN_POINT('Origin',(60.4402651077865,248.040265107786,23.0213203435596)) ;
#107668 = CARTESIAN_POINT('',(60.4402651077865,253.144997361739,25.0474167838721)) ;
#107669 = CARTESIAN_POINT('',(60.4402651077865,250.536866817902,24.1999837998328)) ;
#107670 = CARTESIAN_POINT('',(60.4402651077865,253.360989860305,24.3826602268791)) ;
#107671 = CARTESIAN_POINT('Origin',(60.4402651077865,253.27107594741,24.7209138126218)) ;
#107672 = CARTESIAN_POINT('',(60.4402651077865,250.418405397417,23.426556577058)) ;
#107673 = CARTESIAN_POINT('Origin',(60.4402651077865,248.040265107786,23.0213203435596)) ;
#107674 = CARTESIAN_POINT('',(60.4402651077865,252.26905574955,26.5257015839662)) ;
#107675 = CARTESIAN_POINT('',(60.4402651077865,250.050447394148,24.9137882607786)) ;
#107676 = CARTESIAN_POINT('',(60.4402651077865,252.679897896016,25.9602258814029)) ;
#107677 = CARTESIAN_POINT('Origin',(60.4402651077865,252.489858576849,26.2541392311682)) ;
#107678 = CARTESIAN_POINT('',(60.4402651077865,250.176786044017,24.1416086685709)) ;
#107679 = CARTESIAN_POINT('Origin',(60.4402651077865,248.040265107786,23.0213203435596)) ;
#107680 = CARTESIAN_POINT('',(60.4402651077865,250.979170645629,27.6609531317894)) ;
#107681 = CARTESIAN_POINT('',(60.4402651077865,249.367257322442,25.4423447763876)) ;
#107682 = CARTESIAN_POINT('',(60.4402651077865,251.544646348192,27.2501109853232)) ;
#107683 = CARTESIAN_POINT('Origin',(60.4402651077865,251.273083995395,27.4709138126218)) ;
#107684 = CARTESIAN_POINT('',(60.4402651077865,249.726029135361,24.746999133324)) ;
#107685 = CARTESIAN_POINT('Origin',(60.4402651077865,248.040265107786,23.0213203435596)) ;
#107686 = CARTESIAN_POINT('',(60.4402651077865,249.401604991106,28.3420450960785)) ;
#107687 = CARTESIAN_POINT('',(60.4402651077865,248.554172007067,25.7339145522423)) ;
#107688 = CARTESIAN_POINT('',(60.4402651077865,250.066361548098,28.1260525975113)) ;
#107689 = CARTESIAN_POINT('Origin',(60.4402651077865,249.739858576849,28.252131183183)) ;
#107690 = CARTESIAN_POINT('',(60.4402651077865,249.110257898277,25.1834681346239)) ;
#107691 = CARTESIAN_POINT('Origin',(60.4402651077865,248.040265107786,23.0213203435596)) ;
#107692 = CARTESIAN_POINT('',(60.4402651077865,247.69078190379,28.5023074499212)) ;
#107693 = CARTESIAN_POINT('',(60.4402651077865,247.69078190379,25.759956707196)) ;
#107694 = CARTESIAN_POINT('',(60.4402651077865,248.389748311783,28.5023074499214)) ;
#107695 = CARTESIAN_POINT('Origin',(60.4402651077865,248.040265107786,28.5213203435596)) ;
#107696 = CARTESIAN_POINT('',(60.4402651077865,248.389748311783,25.4082910455649)) ;
#107697 = CARTESIAN_POINT('Origin',(60.4402651077865,248.040265107786,23.0213203435596)) ;
#107698 = CARTESIAN_POINT('',(60.4402651077865,246.014168667474,28.1260525975118)) ;
#107699 = CARTESIAN_POINT('',(60.4402651077865,246.861601651513,25.5179220536754)) ;
#107700 = CARTESIAN_POINT('',(60.4402651077865,246.678925224467,28.3420450960783)) ;
#107701 = CARTESIAN_POINT('Origin',(60.4402651077865,246.340671638724,28.252131183183)) ;
#107702 = CARTESIAN_POINT('',(60.4402651077865,247.635028874288,25.3994606331908)) ;
#107703 = CARTESIAN_POINT('Origin',(60.4402651077865,248.040265107786,23.0213203435596)) ;
#107704 = CARTESIAN_POINT('',(60.4402651077865,244.53588386738,27.2501109853234)) ;
#107705 = CARTESIAN_POINT('',(60.4402651077865,246.147797190567,25.0315026299217)) ;
#107706 = CARTESIAN_POINT('',(60.4402651077865,245.101359569943,27.6609531317894)) ;
#107707 = CARTESIAN_POINT('Origin',(60.4402651077865,244.807446220178,27.4709138126218)) ;
#107708 = CARTESIAN_POINT('',(60.4402651077865,246.919976782775,25.1578412797899)) ;
#107709 = CARTESIAN_POINT('Origin',(60.4402651077865,248.040265107786,23.0213203435596)) ;
#107710 = CARTESIAN_POINT('',(60.4402651077865,243.400632319557,25.9602258814026)) ;
#107711 = CARTESIAN_POINT('',(60.4402651077865,245.619240674958,24.3483125582154)) ;
#107712 = CARTESIAN_POINT('',(60.4402651077865,243.811474466023,26.5257015839658)) ;
#107713 = CARTESIAN_POINT('Origin',(60.4402651077865,243.590671638724,26.2541392311682)) ;
#107714 = CARTESIAN_POINT('',(60.4402651077865,246.314586318022,24.7070843711341)) ;
#107715 = CARTESIAN_POINT('Origin',(60.4402651077865,248.040265107786,23.0213203435596)) ;
#107716 = CARTESIAN_POINT('',(60.4402651077865,242.719540355267,24.3826602268792)) ;
#107717 = CARTESIAN_POINT('',(60.4402651077865,245.327670899104,23.5352272428401)) ;
#107718 = CARTESIAN_POINT('',(60.4402651077865,242.935532853835,25.0474167838717)) ;
#107719 = CARTESIAN_POINT('Origin',(60.4402651077865,242.809454268163,24.7209138126218)) ;
#107720 = CARTESIAN_POINT('',(60.4402651077865,245.878117316722,24.0913131340507)) ;
#107721 = CARTESIAN_POINT('Origin',(60.4402651077865,248.040265107786,23.0213203435596)) ;
#107722 = CARTESIAN_POINT('',(60.4402651077865,242.559278001424,22.6718371395634)) ;
#107723 = CARTESIAN_POINT('',(60.4402651077865,245.30162874415,22.6718371395634)) ;
#107724 = CARTESIAN_POINT('',(60.4402651077865,242.559278001425,23.3708035475559)) ;
#107725 = CARTESIAN_POINT('Origin',(60.4402651077865,242.540265107786,23.0213203435596)) ;
#107726 = CARTESIAN_POINT('',(60.4402651077865,245.653294405781,23.3708035475559)) ;
#107727 = CARTESIAN_POINT('Origin',(60.4402651077865,248.040265107786,23.0213203435596)) ;
#107728 = CARTESIAN_POINT('',(60.4402651077865,242.935532853834,20.9952239032473)) ;
#107729 = CARTESIAN_POINT('',(60.4402651077865,245.543663397671,21.8426568872864)) ;
#107730 = CARTESIAN_POINT('',(60.4402651077865,242.719540355268,21.6599804602402)) ;
#107731 = CARTESIAN_POINT('Origin',(60.4402651077865,242.809454268163,21.3217268744974)) ;
#107732 = CARTESIAN_POINT('',(60.4402651077865,245.662124818155,22.6160841100613)) ;
#107733 = CARTESIAN_POINT('Origin',(60.4402651077865,248.040265107786,23.0213203435596)) ;
#107734 = CARTESIAN_POINT('',(60.4402651077865,243.811474466023,19.5169391031534)) ;
#107735 = CARTESIAN_POINT('',(60.4402651077865,246.030082821424,21.1288524263407)) ;
#107736 = CARTESIAN_POINT('',(60.4402651077865,243.400632319557,20.0824148057165)) ;
#107737 = CARTESIAN_POINT('Origin',(60.4402651077865,243.590671638724,19.788501455951)) ;
#107738 = CARTESIAN_POINT('',(60.4402651077865,245.903744171556,21.9010320185483)) ;
#107739 = CARTESIAN_POINT('Origin',(60.4402651077865,248.040265107786,23.0213203435596)) ;
#107740 = CARTESIAN_POINT('',(60.4402651077865,245.101359569943,18.3816875553301)) ;
#107741 = CARTESIAN_POINT('',(60.4402651077865,246.713272893131,20.6002959107317)) ;
#107742 = CARTESIAN_POINT('',(60.4402651077865,244.53588386738,18.7925297017959)) ;
#107743 = CARTESIAN_POINT('Origin',(60.4402651077865,244.807446220178,18.5717268744974)) ;
#107744 = CARTESIAN_POINT('',(60.4402651077865,246.354501080212,21.2956415537952)) ;
#107745 = CARTESIAN_POINT('Origin',(60.4402651077865,248.040265107786,23.0213203435596)) ;
#107746 = CARTESIAN_POINT('',(60.4402651077865,246.678925224467,17.7005955910407)) ;
#107747 = CARTESIAN_POINT('',(60.4402651077865,247.526358208506,20.3087261348769)) ;
#107748 = CARTESIAN_POINT('',(60.4402651077865,246.014168667474,17.9165880896081)) ;
#107749 = CARTESIAN_POINT('Origin',(60.4402651077865,246.340671638724,17.7905095039363)) ;
#107750 = CARTESIAN_POINT('',(60.4402651077865,246.970272317295,20.8591725524954)) ;
#107751 = CARTESIAN_POINT('Origin',(60.4402651077865,248.040265107786,23.0213203435596)) ;
#107752 = CARTESIAN_POINT('',(60.4402651077865,248.389748311783,17.5403332371977)) ;
#107753 = CARTESIAN_POINT('',(60.4402651077865,248.389748311783,20.2826839799233)) ;
#107754 = CARTESIAN_POINT('',(60.4402651077865,247.69078190379,17.5403332371979)) ;
#107755 = CARTESIAN_POINT('Origin',(60.4402651077865,248.040265107786,17.5213203435596)) ;
#107756 = CARTESIAN_POINT('',(60.4402651077865,247.69078190379,20.6343496415544)) ;
#107757 = CARTESIAN_POINT('Origin',(60.5902651077865,248.040265107786,23.0213203435596)) ;
#107758 = CARTESIAN_POINT('',(60.5902651077865,246.946891701628,28.0027392774284)) ;
#107759 = CARTESIAN_POINT('Ctrl Pts',(60.4402651077865,246.84682643861,27.8252982934377)) ;
#107760 = CARTESIAN_POINT('Ctrl Pts',(60.4402651077865,246.847209116359,27.8259879723372)) ;
#107761 = CARTESIAN_POINT('Ctrl Pts',(60.440268437892,246.847591853016,27.8266776249678)) ;
#107762 = CARTESIAN_POINT('Ctrl Pts',(60.4404467789389,246.857838938126,27.8451382901616)) ;
#107763 = CARTESIAN_POINT('Ctrl Pts',(60.4428319502748,246.86777865457,27.8629553332033)) ;
#107764 = CARTESIAN_POINT('Ctrl Pts',(60.4520052987552,246.88669215874,27.8966993889314)) ;
#107765 = CARTESIAN_POINT('Ctrl Pts',(60.4586423249847,246.895772989479,27.9128241441561)) ;
#107766 = CARTESIAN_POINT('Ctrl Pts',(60.4774783235664,246.913652858034,27.9444499271496)) ;
#107767 = CARTESIAN_POINT('Ctrl Pts',(60.4902886559451,246.92239313214,27.9598318195758)) ;
#107768 = CARTESIAN_POINT('Ctrl Pts',(60.5183067650572,246.935114921148,27.9821554300886)) ;
#107769 = CARTESIAN_POINT('Ctrl Pts',(60.5322233323112,246.939674844702,27.9901316702287)) ;
#107770 = CARTESIAN_POINT('Ctrl Pts',(60.5612197979218,246.945446722844,28.0002186669547)) ;
#107771 = CARTESIAN_POINT('Ctrl Pts',(60.5755858845328,246.946891701628,28.0027392774284)) ;
#107772 = CARTESIAN_POINT('Ctrl Pts',(60.5902651077866,246.946891701628,28.0027392774284)) ;
#107773 = CARTESIAN_POINT('',(60.5902651077865,247.54078190379,28.096802244712)) ;
#107774 = CARTESIAN_POINT('Origin',(60.5902651077865,248.040265107786,23.0213203435596)) ;
#107775 = CARTESIAN_POINT('Ctrl Pts',(60.4402651077865,247.69078190379,27.9589677074491)) ;
#107776 = CARTESIAN_POINT('Ctrl Pts',(60.4402651077865,247.690204833126,27.9595053771295)) ;
#107777 = CARTESIAN_POINT('Ctrl Pts',(60.440268437892,247.68962771455,27.9600430036272)) ;
#107778 = CARTESIAN_POINT('Ctrl Pts',(60.4404467789383,247.674177498214,27.9744336161106)) ;
#107779 = CARTESIAN_POINT('Ctrl Pts',(60.4428319502738,247.659218497029,27.9883070896971)) ;
#107780 = CARTESIAN_POINT('Ctrl Pts',(60.4520052987543,247.630803198961,28.0145549995742)) ;
#107781 = CARTESIAN_POINT('Ctrl Pts',(60.4586423249841,247.617183992317,28.0270844220836)) ;
#107782 = CARTESIAN_POINT('Ctrl Pts',(60.4774783235664,247.590406322412,28.0516371458428)) ;
#107783 = CARTESIAN_POINT('Ctrl Pts',(60.4902886559451,247.577340561604,28.0635653016335)) ;
#107784 = CARTESIAN_POINT('Ctrl Pts',(60.5183067650572,247.558343046244,28.0808650678764)) ;
#107785 = CARTESIAN_POINT('Ctrl Pts',(60.5322233323112,247.55154150748,28.087041829166)) ;
#107786 = CARTESIAN_POINT('Ctrl Pts',(60.5612197979217,247.542935071751,28.0948515246967)) ;
#107787 = CARTESIAN_POINT('Ctrl Pts',(60.5755858845327,247.54078190379,28.096802244712)) ;
#107788 = CARTESIAN_POINT('Ctrl Pts',(60.5902651077865,247.54078190379,28.096802244712)) ;
#107789 = CARTESIAN_POINT('Origin',(60.5902651077865,247.635028874288,25.3994606331908)) ;
#107790 = CARTESIAN_POINT('',(60.5902651077865,246.822731508173,28.3848650607978)) ;
#107791 = CARTESIAN_POINT('Ctrl Pts',(60.4402651077865,246.678925224467,28.3420450960783)) ;
#107792 = CARTESIAN_POINT('Ctrl Pts',(60.4402651077865,246.680324229639,28.3424579870217)) ;
#107793 = CARTESIAN_POINT('Ctrl Pts',(60.440286369022,246.681723125547,28.3428709748965)) ;
#107794 = CARTESIAN_POINT('Ctrl Pts',(60.4403288850239,246.683121466859,28.343283925702)) ;
#107795 = CARTESIAN_POINT('Ctrl Pts',(60.4408750760621,246.701085561798,28.3485889877858)) ;
#107796 = CARTESIAN_POINT('Ctrl Pts',(60.4449239452533,246.718788094142,28.3538380651872)) ;
#107797 = CARTESIAN_POINT('Ctrl Pts',(60.4522665395981,246.735313540781,28.3587517471949)) ;
#107798 = CARTESIAN_POINT('Ctrl Pts',(60.4599211853139,246.752541298897,28.3638742547396)) ;
#107799 = CARTESIAN_POINT('Ctrl Pts',(60.4710122117666,246.768167444445,28.3685360408185)) ;
#107800 = CARTESIAN_POINT('Ctrl Pts',(60.4849165768426,246.781315020339,28.3724647819378)) ;
#107801 = CARTESIAN_POINT('Ctrl Pts',(60.4988172216939,246.794459078493,28.3763924718908)) ;
#107802 = CARTESIAN_POINT('Ctrl Pts',(60.5152637963995,246.804874499694,28.3795121161121)) ;
#107803 = CARTESIAN_POINT('Ctrl Pts',(60.5333315664699,246.811976821569,28.3816405503696)) ;
#107804 = CARTESIAN_POINT('Ctrl Pts',(60.5513971100607,246.81907826823,28.3837687223414)) ;
#107805 = CARTESIAN_POINT('Ctrl Pts',(60.5707376338846,246.822731508174,28.3848650607972)) ;
#107806 = CARTESIAN_POINT('Ctrl Pts',(60.5902651077865,246.822731508174,28.3848650607972)) ;
#107807 = CARTESIAN_POINT('',(60.5902651077865,247.777687351732,25.445813182347)) ;
#107808 = CARTESIAN_POINT('Origin',(60.5902651077865,247.69078190379,25.759956707196)) ;
#107809 = CARTESIAN_POINT('',(60.5902651077865,247.54078190379,28.4985930708324)) ;
#107810 = CARTESIAN_POINT('',(60.5902651077865,247.54078190379,25.759956707196)) ;
#107811 = CARTESIAN_POINT('Ctrl Pts',(60.5902651077865,247.54078190379,28.4985930708324)) ;
#107812 = CARTESIAN_POINT('Ctrl Pts',(60.5707376338847,247.54078190379,28.4985930708324)) ;
#107813 = CARTESIAN_POINT('Ctrl Pts',(60.5513971100608,247.544595128658,28.4986793042264)) ;
#107814 = CARTESIAN_POINT('Ctrl Pts',(60.5333315664699,247.552006647086,28.4988497601077)) ;
#107815 = CARTESIAN_POINT('Ctrl Pts',(60.5152637963994,247.559419078944,28.4990202369967)) ;
#107816 = CARTESIAN_POINT('Ctrl Pts',(60.4988172216937,247.570288756228,28.4992718211856)) ;
#107817 = CARTESIAN_POINT('Ctrl Pts',(60.4849165768426,247.58400322133,28.4995981034065)) ;
#107818 = CARTESIAN_POINT('Ctrl Pts',(60.4710122117669,247.597721356829,28.4999244729501)) ;
#107819 = CARTESIAN_POINT('Ctrl Pts',(60.4599211853139,247.6140232755,28.5003195954534)) ;
#107820 = CARTESIAN_POINT('Ctrl Pts',(60.452266539598,247.631990789003,28.5007714713061)) ;
#107821 = CARTESIAN_POINT('Ctrl Pts',(60.4449239452531,247.649225833959,28.5012049258647)) ;
#107822 = CARTESIAN_POINT('Ctrl Pts',(60.4408750760621,247.667683996822,28.5016831399335)) ;
#107823 = CARTESIAN_POINT('Ctrl Pts',(60.4403288850239,247.686408220711,28.5021889366962)) ;
#107824 = CARTESIAN_POINT('Ctrl Pts',(60.440286369022,247.687865731145,28.5022283083713)) ;
#107825 = CARTESIAN_POINT('Ctrl Pts',(60.4402651077865,247.689323780486,28.50226781617)) ;
#107826 = CARTESIAN_POINT('Ctrl Pts',(60.4402651077865,247.69078190379,28.5023074499212)) ;
#107827 = CARTESIAN_POINT('Origin',(60.5902651077865,246.861601651513,25.5179220536754)) ;
#107828 = CARTESIAN_POINT('Ctrl Pts',(60.4402651077865,246.182069881617,27.6093057948708)) ;
#107829 = CARTESIAN_POINT('Ctrl Pts',(60.4402651077865,246.181354905733,27.6096388244826)) ;
#107830 = CARTESIAN_POINT('Ctrl Pts',(60.4402684378921,246.180639897624,27.6099717982194)) ;
#107831 = CARTESIAN_POINT('Ctrl Pts',(60.4404467789386,246.161498924882,27.6188837045809)) ;
#107832 = CARTESIAN_POINT('Ctrl Pts',(60.4428319502743,246.142984930219,27.6274555764537)) ;
#107833 = CARTESIAN_POINT('Ctrl Pts',(60.4520052987548,246.107849325612,27.6436380121775)) ;
#107834 = CARTESIAN_POINT('Ctrl Pts',(60.4586423249844,246.091024885902,27.6513456347974)) ;
#107835 = CARTESIAN_POINT('Ctrl Pts',(60.4774783235664,246.057970599548,27.6664219076506)) ;
#107836 = CARTESIAN_POINT('Ctrl Pts',(60.4902886559451,246.04185831974,27.6737287158086)) ;
#107837 = CARTESIAN_POINT('Ctrl Pts',(60.5183067650571,246.018444687196,27.6843112161272)) ;
#107838 = CARTESIAN_POINT('Ctrl Pts',(60.5322233323112,246.010067315225,27.6880838741351)) ;
#107839 = CARTESIAN_POINT('Ctrl Pts',(60.5612197979218,245.999468779803,27.6928518010587)) ;
#107840 = CARTESIAN_POINT('Ctrl Pts',(60.5755858845328,245.996818189747,27.694041680549)) ;
#107841 = CARTESIAN_POINT('Ctrl Pts',(60.5902651077865,245.996818189747,27.694041680549)) ;
#107842 = CARTESIAN_POINT('',(60.5902651077865,245.872657996292,28.0761674639184)) ;
#107843 = CARTESIAN_POINT('',(60.5902651077865,246.718943174069,25.4715695045192)) ;
#107844 = CARTESIAN_POINT('Ctrl Pts',(60.5902651077865,245.872657996292,28.0761674639184)) ;
#107845 = CARTESIAN_POINT('Ctrl Pts',(60.5707376338847,245.872657996292,28.0761674639184)) ;
#107846 = CARTESIAN_POINT('Ctrl Pts',(60.5513971100606,245.876257941067,28.0774278280374)) ;
#107847 = CARTESIAN_POINT('Ctrl Pts',(60.5333315664698,245.883254040199,28.0798802263625)) ;
#107848 = CARTESIAN_POINT('Ctrl Pts',(60.5152637963995,245.890251001563,28.0823329269323)) ;
#107849 = CARTESIAN_POINT('Ctrl Pts',(60.4988172216939,245.900510935184,28.0859311127188)) ;
#107850 = CARTESIAN_POINT('Ctrl Pts',(60.4849165768426,245.913453339835,28.0904794283364)) ;
#107851 = CARTESIAN_POINT('Ctrl Pts',(60.4710122117669,245.926399208258,28.0950289612181)) ;
#107852 = CARTESIAN_POINT('Ctrl Pts',(60.4599211853139,245.94178115467,28.1004423149597)) ;
#107853 = CARTESIAN_POINT('Ctrl Pts',(60.452266539598,245.958729638151,28.1064243414529)) ;
#107854 = CARTESIAN_POINT('Ctrl Pts',(60.4449239452531,245.97498719514,28.1121625030258)) ;
#107855 = CARTESIAN_POINT('Ctrl Pts',(60.4408750760621,245.992394174936,28.1183211976404)) ;
#107856 = CARTESIAN_POINT('Ctrl Pts',(60.4403288850239,246.010045670283,28.1245883423369)) ;
#107857 = CARTESIAN_POINT('Ctrl Pts',(60.440286369022,246.011419678562,28.1250761825186)) ;
#107858 = CARTESIAN_POINT('Ctrl Pts',(60.4402651077865,246.012794157307,28.1255643186937)) ;
#107859 = CARTESIAN_POINT('Ctrl Pts',(60.4402651077865,246.014168667474,28.1260525975118)) ;
#107860 = CARTESIAN_POINT('Origin',(60.5902651077865,248.040265107786,23.0213203435596)) ;
#107861 = CARTESIAN_POINT('Ctrl Pts',(60.4402651077865,245.420726657552,27.2213820464094)) ;
#107862 = CARTESIAN_POINT('Ctrl Pts',(60.4402651077865,245.420877483217,27.2221562239435)) ;
#107863 = CARTESIAN_POINT('Ctrl Pts',(60.440268437892,245.421028373027,27.2229303947057)) ;
#107864 = CARTESIAN_POINT('Ctrl Pts',(60.4404467789383,245.425069270821,27.2436540540717)) ;
#107865 = CARTESIAN_POINT('Ctrl Pts',(60.4428319502739,245.429016733826,27.2636706102593)) ;
#107866 = CARTESIAN_POINT('Ctrl Pts',(60.4520052987543,245.436577058534,27.3016077085599)) ;
#107867 = CARTESIAN_POINT('Ctrl Pts',(60.4586423249841,245.440230618388,27.3197493931132)) ;
#107868 = CARTESIAN_POINT('Ctrl Pts',(60.4774783235665,245.447462479482,27.3553524833539)) ;
#107869 = CARTESIAN_POINT('Ctrl Pts',(60.4902886559452,245.451021707959,27.3726824256129)) ;
#107870 = CARTESIAN_POINT('Ctrl Pts',(60.5183067650571,245.45622247327,27.3978446898607)) ;
#107871 = CARTESIAN_POINT('Ctrl Pts',(60.5322233323112,245.458094424526,27.4068396388929)) ;
#107872 = CARTESIAN_POINT('Ctrl Pts',(60.5612197979217,245.460466753434,27.4182165512943)) ;
#107873 = CARTESIAN_POINT('Ctrl Pts',(60.5755858845327,245.461062098449,27.4210603173112)) ;
#107874 = CARTESIAN_POINT('Ctrl Pts',(60.5902651077865,245.461062098449,27.4210603173112)) ;
#107875 = CARTESIAN_POINT('Origin',(60.5902651077865,246.919976782775,25.1578412797899)) ;
#107876 = CARTESIAN_POINT('Ctrl Pts',(60.4402651077865,245.101359569943,27.6609531317894)) ;
#107877 = CARTESIAN_POINT('Ctrl Pts',(60.4402651077865,245.102562512611,27.6617781307852)) ;
#107878 = CARTESIAN_POINT('Ctrl Pts',(60.440286369022,245.103765321408,27.6626031882028)) ;
#107879 = CARTESIAN_POINT('Ctrl Pts',(60.4403288850239,245.104967614208,27.6634280389871)) ;
#107880 = CARTESIAN_POINT('Ctrl Pts',(60.4408750760621,245.120413129416,27.6740246634793)) ;
#107881 = CARTESIAN_POINT('Ctrl Pts',(60.4449239452533,245.135627184036,27.6844872160823)) ;
#107882 = CARTESIAN_POINT('Ctrl Pts',(60.4522665395981,245.149825406502,27.6942670492256)) ;
#107883 = CARTESIAN_POINT('Ctrl Pts',(60.4599211853139,245.164627036234,27.7044625134384)) ;
#107884 = CARTESIAN_POINT('Ctrl Pts',(60.4710122117667,245.17804781266,27.7137248799967)) ;
#107885 = CARTESIAN_POINT('Ctrl Pts',(60.4849165768426,245.189337852615,27.7215241592249)) ;
#107886 = CARTESIAN_POINT('Ctrl Pts',(60.4988172216939,245.200624871829,27.7293213516934)) ;
#107887 = CARTESIAN_POINT('Ctrl Pts',(60.5152637963994,245.209566502951,27.7355068518133)) ;
#107888 = CARTESIAN_POINT('Ctrl Pts',(60.5333315664698,245.215663490095,27.7397258512423)) ;
#107889 = CARTESIAN_POINT('Ctrl Pts',(60.5513971100606,245.22175972591,27.7439443307667)) ;
#107890 = CARTESIAN_POINT('Ctrl Pts',(60.5707376338847,245.224895376349,27.7461159238267)) ;
#107891 = CARTESIAN_POINT('Ctrl Pts',(60.5902651077865,245.22489537635,27.7461159238262)) ;
#107892 = CARTESIAN_POINT('Origin',(60.5902651077865,248.554172007067,25.7339145522423)) ;
#107893 = CARTESIAN_POINT('',(60.5902651077865,249.133638513944,28.0027392774284)) ;
#107894 = CARTESIAN_POINT('',(60.5902651077865,249.257798707399,28.3848650607978)) ;
#107895 = CARTESIAN_POINT('',(60.5902651077865,248.411513529623,25.7802671013986)) ;
#107896 = CARTESIAN_POINT('Ctrl Pts',(60.5902651077865,249.257798707399,28.3848650607969)) ;
#107897 = CARTESIAN_POINT('Ctrl Pts',(60.5707376338847,249.257798707399,28.3848650607969)) ;
#107898 = CARTESIAN_POINT('Ctrl Pts',(60.5513971100606,249.261451947343,28.3837687223414)) ;
#107899 = CARTESIAN_POINT('Ctrl Pts',(60.5333315664698,249.268553394004,28.3816405503695)) ;
#107900 = CARTESIAN_POINT('Ctrl Pts',(60.5152637963994,249.275655715879,28.379512116112)) ;
#107901 = CARTESIAN_POINT('Ctrl Pts',(60.4988172216938,249.28607113708,28.3763924718905)) ;
#107902 = CARTESIAN_POINT('Ctrl Pts',(60.4849165768427,249.299215195234,28.3724647819375)) ;
#107903 = CARTESIAN_POINT('Ctrl Pts',(60.471012211767,249.312362771127,28.3685360408181)) ;
#107904 = CARTESIAN_POINT('Ctrl Pts',(60.4599211853138,249.327988916676,28.3638742547393)) ;
#107905 = CARTESIAN_POINT('Ctrl Pts',(60.452266539598,249.345216674792,28.3587517471944)) ;
#107906 = CARTESIAN_POINT('Ctrl Pts',(60.4449239452532,249.361742121431,28.3538380651865)) ;
#107907 = CARTESIAN_POINT('Ctrl Pts',(60.4408750760622,249.379444653775,28.3485889877863)) ;
#107908 = CARTESIAN_POINT('Ctrl Pts',(60.4403288850239,249.397408748713,28.3432839257019)) ;
#107909 = CARTESIAN_POINT('Ctrl Pts',(60.440286369022,249.398807090025,28.3428709748963)) ;
#107910 = CARTESIAN_POINT('Ctrl Pts',(60.4402651077865,249.400205985933,28.342457987022)) ;
#107911 = CARTESIAN_POINT('Ctrl Pts',(60.4402651077865,249.401604991106,28.3420450960785)) ;
#107912 = CARTESIAN_POINT('Ctrl Pts',(60.4402651077865,249.233703776962,27.8252982934377)) ;
#107913 = CARTESIAN_POINT('Ctrl Pts',(60.4402651077865,249.233321099215,27.8259879723341)) ;
#107914 = CARTESIAN_POINT('Ctrl Pts',(60.4402684378921,249.232938362557,27.8266776249672)) ;
#107915 = CARTESIAN_POINT('Ctrl Pts',(60.4404467789386,249.222691277448,27.8451382901584)) ;
#107916 = CARTESIAN_POINT('Ctrl Pts',(60.4428319502743,249.212751561004,27.8629553332008)) ;
#107917 = CARTESIAN_POINT('Ctrl Pts',(60.4520052987547,249.193838056834,27.8966993889301)) ;
#107918 = CARTESIAN_POINT('Ctrl Pts',(60.4586423249844,249.184757226094,27.9128241441556)) ;
#107919 = CARTESIAN_POINT('Ctrl Pts',(60.4774783235664,249.166877357539,27.9444499271496)) ;
#107920 = CARTESIAN_POINT('Ctrl Pts',(60.4902886559451,249.158137083433,27.9598318195758)) ;
#107921 = CARTESIAN_POINT('Ctrl Pts',(60.5183067650572,249.145415294424,27.9821554300886)) ;
#107922 = CARTESIAN_POINT('Ctrl Pts',(60.5322233323113,249.14085537087,27.9901316702288)) ;
#107923 = CARTESIAN_POINT('Ctrl Pts',(60.5612197979218,249.135083492728,28.0002186669547)) ;
#107924 = CARTESIAN_POINT('Ctrl Pts',(60.5755858845327,249.133638513944,28.0027392774284)) ;
#107925 = CARTESIAN_POINT('Ctrl Pts',(60.5902651077865,249.133638513944,28.0027392774284)) ;
#107926 = CARTESIAN_POINT('Origin',(60.5902651077865,246.147797190567,25.0315026299217)) ;
#107927 = CARTESIAN_POINT('Ctrl Pts',(60.4402651077865,244.85525095499,26.8105398999439)) ;
#107928 = CARTESIAN_POINT('Ctrl Pts',(60.4402651077865,244.854468060706,26.8106356902274)) ;
#107929 = CARTESIAN_POINT('Ctrl Pts',(60.4402684378921,244.853685153042,26.8107314174129)) ;
#107930 = CARTESIAN_POINT('Ctrl Pts',(60.4404467789386,244.832727075669,26.8132922581644)) ;
#107931 = CARTESIAN_POINT('Ctrl Pts',(60.4428319502743,244.81247036632,26.8157234537812)) ;
#107932 = CARTESIAN_POINT('Ctrl Pts',(60.4520052987548,244.774053772956,26.8202563657947)) ;
#107933 = CARTESIAN_POINT('Ctrl Pts',(60.4586423249844,244.75567099356,26.8223877127213)) ;
#107934 = CARTESIAN_POINT('Ctrl Pts',(60.4774783235664,244.719575674609,26.8265117640394)) ;
#107935 = CARTESIAN_POINT('Ctrl Pts',(60.4902886559451,244.70199405801,26.8284819832727)) ;
#107936 = CARTESIAN_POINT('Ctrl Pts',(60.5183067650572,244.676456197767,26.8313113288033)) ;
#107937 = CARTESIAN_POINT('Ctrl Pts',(60.5322233323112,244.667323028126,26.832310589478)) ;
#107938 = CARTESIAN_POINT('Ctrl Pts',(60.5612197979217,244.655769851502,26.8335700298872)) ;
#107939 = CARTESIAN_POINT('Ctrl Pts',(60.5755858845327,244.652881297574,26.8338825951576)) ;
#107940 = CARTESIAN_POINT('Ctrl Pts',(60.5902651077865,244.652881297574,26.8338825951576)) ;
#107941 = CARTESIAN_POINT('Ctrl Pts',(60.5902651077865,244.416714575474,27.1589382016726)) ;
#107942 = CARTESIAN_POINT('Ctrl Pts',(60.5707376338846,244.416714575474,27.1589382016726)) ;
#107943 = CARTESIAN_POINT('Ctrl Pts',(60.5513971100607,244.419748852478,27.1612493232954)) ;
#107944 = CARTESIAN_POINT('Ctrl Pts',(60.5333315664697,244.425644705387,27.1657436062293)) ;
#107945 = CARTESIAN_POINT('Ctrl Pts',(60.5152637963991,244.431541284929,27.1702384430589)) ;
#107946 = CARTESIAN_POINT('Ctrl Pts',(60.4988172216935,244.440187161099,27.1768310149478)) ;
#107947 = CARTESIAN_POINT('Ctrl Pts',(60.4849165768424,244.451090612557,27.1851561431397)) ;
#107948 = CARTESIAN_POINT('Ctrl Pts',(60.4710122117667,244.461996982103,27.1934834993826)) ;
#107949 = CARTESIAN_POINT('Ctrl Pts',(60.4599211853136,244.474953264169,27.2033851875814)) ;
#107950 = CARTESIAN_POINT('Ctrl Pts',(60.4522665395979,244.489223681977,27.2143118022826)) ;
#107951 = CARTESIAN_POINT('Ctrl Pts',(60.4449239452532,244.502912348048,27.2247929796344)) ;
#107952 = CARTESIAN_POINT('Ctrl Pts',(60.4408750760621,244.51756422831,27.2360292988605)) ;
#107953 = CARTESIAN_POINT('Ctrl Pts',(60.4403288850239,244.532415143768,27.2474443196983)) ;
#107954 = CARTESIAN_POINT('Ctrl Pts',(60.440286369022,244.533571152388,27.2483328751903)) ;
#107955 = CARTESIAN_POINT('Ctrl Pts',(60.4402651077865,244.534727516982,27.249221857571)) ;
#107956 = CARTESIAN_POINT('Ctrl Pts',(60.4402651077865,244.53588386738,27.2501109853234)) ;
#107957 = CARTESIAN_POINT('Origin',(60.5902651077865,248.040265107786,23.0213203435596)) ;
#107958 = CARTESIAN_POINT('Ctrl Pts',(60.4402651077865,244.251045551402,26.2063344963562)) ;
#107959 = CARTESIAN_POINT('Ctrl Pts',(60.4402651077865,244.250949761119,26.2071173906402)) ;
#107960 = CARTESIAN_POINT('Ctrl Pts',(60.4402684378921,244.250854033933,26.2079002983041)) ;
#107961 = CARTESIAN_POINT('Ctrl Pts',(60.4404467789386,244.248293193181,26.228858375676)) ;
#107962 = CARTESIAN_POINT('Ctrl Pts',(60.4428319502743,244.245861997565,26.2491150850256)) ;
#107963 = CARTESIAN_POINT('Ctrl Pts',(60.4520052987547,244.241329085551,26.2875316783901)) ;
#107964 = CARTESIAN_POINT('Ctrl Pts',(60.4586423249843,244.239197738625,26.3059144577853)) ;
#107965 = CARTESIAN_POINT('Ctrl Pts',(60.4774783235665,244.235073687307,26.3420097767375)) ;
#107966 = CARTESIAN_POINT('Ctrl Pts',(60.4902886559452,244.233103468073,26.3595913933363)) ;
#107967 = CARTESIAN_POINT('Ctrl Pts',(60.5183067650571,244.230274122543,26.3851292535788)) ;
#107968 = CARTESIAN_POINT('Ctrl Pts',(60.5322233323112,244.229274861868,26.3942624232202)) ;
#107969 = CARTESIAN_POINT('Ctrl Pts',(60.5612197979218,244.228015421459,26.4058155998437)) ;
#107970 = CARTESIAN_POINT('Ctrl Pts',(60.5755858845328,244.227702856188,26.4087041537722)) ;
#107971 = CARTESIAN_POINT('Ctrl Pts',(60.5902651077865,244.227702856188,26.4087041537722)) ;
#107972 = CARTESIAN_POINT('Origin',(60.5902651077865,246.314586318022,24.7070843711341)) ;
#107973 = CARTESIAN_POINT('Ctrl Pts',(60.4402651077865,243.811474466023,26.5257015839658)) ;
#107974 = CARTESIAN_POINT('Ctrl Pts',(60.4402651077865,243.812363593775,26.5268579343639)) ;
#107975 = CARTESIAN_POINT('Ctrl Pts',(60.440286369022,243.813252576155,26.5280142989582)) ;
#107976 = CARTESIAN_POINT('Ctrl Pts',(60.4403288850239,243.814141131647,26.5291703075783)) ;
#107977 = CARTESIAN_POINT('Ctrl Pts',(60.4408750760621,243.82555615249,26.5440212230314)) ;
#107978 = CARTESIAN_POINT('Ctrl Pts',(60.4449239452531,243.83679247171,26.5586731032986)) ;
#107979 = CARTESIAN_POINT('Ctrl Pts',(60.452266539598,243.847273649062,26.5723617693696)) ;
#107980 = CARTESIAN_POINT('Ctrl Pts',(60.4599211853137,243.858200263764,26.5866321871774)) ;
#107981 = CARTESIAN_POINT('Ctrl Pts',(60.4710122117667,243.868101951963,26.599588469243)) ;
#107982 = CARTESIAN_POINT('Ctrl Pts',(60.4849165768426,243.876429308206,26.6104948387886)) ;
#107983 = CARTESIAN_POINT('Ctrl Pts',(60.498817221694,243.884754436398,26.6213982902475)) ;
#107984 = CARTESIAN_POINT('Ctrl Pts',(60.5152637963994,243.891347008287,26.6300441664173)) ;
#107985 = CARTESIAN_POINT('Ctrl Pts',(60.5333315664698,243.895841845116,26.6359407459585)) ;
#107986 = CARTESIAN_POINT('Ctrl Pts',(60.5513971100606,243.90033612805,26.6418365988681)) ;
#107987 = CARTESIAN_POINT('Ctrl Pts',(60.5707376338848,243.902647249673,26.6448708758722)) ;
#107988 = CARTESIAN_POINT('Ctrl Pts',(60.5902651077865,243.902647249673,26.6448708758723)) ;
#107989 = CARTESIAN_POINT('Origin',(60.5902651077865,249.367257322442,25.4423447763876)) ;
#107990 = CARTESIAN_POINT('',(60.5902651077865,250.619468117123,27.4210603173112)) ;
#107991 = CARTESIAN_POINT('',(60.5902651077865,250.855634839223,27.7461159238265)) ;
#107992 = CARTESIAN_POINT('',(60.5902651077865,249.245904773286,25.5305125642315)) ;
#107993 = CARTESIAN_POINT('Ctrl Pts',(60.5902651077865,250.855634839223,27.7461159238265)) ;
#107994 = CARTESIAN_POINT('Ctrl Pts',(60.5707376338848,250.855634839223,27.7461159238265)) ;
#107995 = CARTESIAN_POINT('Ctrl Pts',(60.5513971100609,250.858770489662,27.7439443307668)) ;
#107996 = CARTESIAN_POINT('Ctrl Pts',(60.5333315664698,250.864866725478,27.7397258512425)) ;
#107997 = CARTESIAN_POINT('Ctrl Pts',(60.5152637963993,250.870963712622,27.7355068518136)) ;
#107998 = CARTESIAN_POINT('Ctrl Pts',(60.4988172216938,250.879905343744,27.7293213516936)) ;
#107999 = CARTESIAN_POINT('Ctrl Pts',(60.4849165768427,250.891192362958,27.7215241592251)) ;
#108000 = CARTESIAN_POINT('Ctrl Pts',(60.471012211767,250.902482402912,27.7137248799968)) ;
#108001 = CARTESIAN_POINT('Ctrl Pts',(60.4599211853139,250.915903179339,27.7044625134388)) ;
#108002 = CARTESIAN_POINT('Ctrl Pts',(60.4522665395981,250.930704809072,27.6942670492262)) ;
#108003 = CARTESIAN_POINT('Ctrl Pts',(60.4449239452533,250.944903031537,27.6844872160832)) ;
#108004 = CARTESIAN_POINT('Ctrl Pts',(60.4408750760621,250.960117086155,27.674024663477)) ;
#108005 = CARTESIAN_POINT('Ctrl Pts',(60.4403288850239,250.975562601365,27.6634280389875)) ;
#108006 = CARTESIAN_POINT('Ctrl Pts',(60.440286369022,250.976764894165,27.6626031882035)) ;
#108007 = CARTESIAN_POINT('Ctrl Pts',(60.4402651077865,250.977967702962,27.6617781307852)) ;
#108008 = CARTESIAN_POINT('Ctrl Pts',(60.4402651077865,250.979170645629,27.6609531317894)) ;
#108009 = CARTESIAN_POINT('Ctrl Pts',(60.4402651077865,250.65980355802,27.2213820464098)) ;
#108010 = CARTESIAN_POINT('Ctrl Pts',(60.4402651077865,250.659652732355,27.2221562239442)) ;
#108011 = CARTESIAN_POINT('Ctrl Pts',(60.440268437892,250.659501842545,27.2229303947054)) ;
#108012 = CARTESIAN_POINT('Ctrl Pts',(60.4404467789383,250.655460944752,27.2436540540713)) ;
#108013 = CARTESIAN_POINT('Ctrl Pts',(60.4428319502738,250.651513481747,27.2636706102592)) ;
#108014 = CARTESIAN_POINT('Ctrl Pts',(60.4520052987543,250.643953157039,27.3016077085601)) ;
#108015 = CARTESIAN_POINT('Ctrl Pts',(60.4586423249841,250.640299597185,27.3197493931132)) ;
#108016 = CARTESIAN_POINT('Ctrl Pts',(60.4774783235664,250.633067736091,27.3553524833537)) ;
#108017 = CARTESIAN_POINT('Ctrl Pts',(60.4902886559451,250.629508507613,27.3726824256129)) ;
#108018 = CARTESIAN_POINT('Ctrl Pts',(60.5183067650571,250.624307742302,27.3978446898607)) ;
#108019 = CARTESIAN_POINT('Ctrl Pts',(60.5322233323112,250.622435791047,27.4068396388929)) ;
#108020 = CARTESIAN_POINT('Ctrl Pts',(60.5612197979217,250.620063462139,27.4182165512944)) ;
#108021 = CARTESIAN_POINT('Ctrl Pts',(60.5755858845327,250.619468117123,27.4210603173112)) ;
#108022 = CARTESIAN_POINT('Ctrl Pts',(60.5902651077865,250.619468117123,27.4210603173112)) ;
#108023 = CARTESIAN_POINT('Origin',(60.5902651077865,245.619240674958,24.3483125582154)) ;
#108024 = CARTESIAN_POINT('Ctrl Pts',(60.4402651077865,243.840203404936,25.6408587937931)) ;
#108025 = CARTESIAN_POINT('Ctrl Pts',(60.4402651077865,243.8394292274,25.6407079681278)) ;
#108026 = CARTESIAN_POINT('Ctrl Pts',(60.4402684378921,243.838655056638,25.6405570783182)) ;
#108027 = CARTESIAN_POINT('Ctrl Pts',(60.4404467789386,243.817931397271,25.6365161805244)) ;
#108028 = CARTESIAN_POINT('Ctrl Pts',(60.4428319502743,243.797914841084,25.6325687175194)) ;
#108029 = CARTESIAN_POINT('Ctrl Pts',(60.4520052987548,243.759977742785,25.6250083928119)) ;
#108030 = CARTESIAN_POINT('Ctrl Pts',(60.4586423249844,243.741836058232,25.621354832958)) ;
#108031 = CARTESIAN_POINT('Ctrl Pts',(60.4774783235665,243.706232967992,25.6141229718641)) ;
#108032 = CARTESIAN_POINT('Ctrl Pts',(60.4902886559452,243.688903025733,25.6105637433868)) ;
#108033 = CARTESIAN_POINT('Ctrl Pts',(60.5183067650571,243.663740761485,25.6053629780756)) ;
#108034 = CARTESIAN_POINT('Ctrl Pts',(60.5322233323112,243.654745812453,25.6034910268201)) ;
#108035 = CARTESIAN_POINT('Ctrl Pts',(60.5612197979217,243.643368900052,25.6011186979124)) ;
#108036 = CARTESIAN_POINT('Ctrl Pts',(60.5755858845327,243.640525134035,25.6005233528966)) ;
#108037 = CARTESIAN_POINT('Ctrl Pts',(60.5902651077865,243.640525134035,25.6005233528966)) ;
#108038 = CARTESIAN_POINT('Ctrl Pts',(60.5902651077865,243.31546952752,25.836690074996)) ;
#108039 = CARTESIAN_POINT('Ctrl Pts',(60.5707376338846,243.315469527519,25.8366900749965)) ;
#108040 = CARTESIAN_POINT('Ctrl Pts',(60.5513971100607,243.317641120579,25.8398257254355)) ;
#108041 = CARTESIAN_POINT('Ctrl Pts',(60.5333315664698,243.321859600104,25.8459219612512)) ;
#108042 = CARTESIAN_POINT('Ctrl Pts',(60.5152637963993,243.326078599533,25.8520189483946)) ;
#108043 = CARTESIAN_POINT('Ctrl Pts',(60.4988172216938,243.332264099653,25.8609605795165)) ;
#108044 = CARTESIAN_POINT('Ctrl Pts',(60.4849165768425,243.340061292122,25.8722475987304)) ;
#108045 = CARTESIAN_POINT('Ctrl Pts',(60.4710122117667,243.34786057135,25.8835376386851)) ;
#108046 = CARTESIAN_POINT('Ctrl Pts',(60.4599211853137,243.357122937908,25.8969584151118)) ;
#108047 = CARTESIAN_POINT('Ctrl Pts',(60.452266539598,243.367318402121,25.9117600448443)) ;
#108048 = CARTESIAN_POINT('Ctrl Pts',(60.4449239452532,243.377098235264,25.9259582673098)) ;
#108049 = CARTESIAN_POINT('Ctrl Pts',(60.4408750760621,243.387560787867,25.9411723219294)) ;
#108050 = CARTESIAN_POINT('Ctrl Pts',(60.4403288850239,243.398157412359,25.9566178371378)) ;
#108051 = CARTESIAN_POINT('Ctrl Pts',(60.440286369022,243.398982263143,25.957820129938)) ;
#108052 = CARTESIAN_POINT('Ctrl Pts',(60.4402651077865,243.399807320561,25.9590229387353)) ;
#108053 = CARTESIAN_POINT('Ctrl Pts',(60.4402651077865,243.400632319557,25.9602258814026)) ;
#108054 = CARTESIAN_POINT('Origin',(60.5902651077865,248.040265107786,23.0213203435596)) ;
#108055 = CARTESIAN_POINT('Ctrl Pts',(60.4402651077865,243.452279656475,24.8795155697285)) ;
#108056 = CARTESIAN_POINT('Ctrl Pts',(60.4402651077865,243.451946626863,24.8802305456133)) ;
#108057 = CARTESIAN_POINT('Ctrl Pts',(60.4402684378921,243.451613653127,24.8809455537216)) ;
#108058 = CARTESIAN_POINT('Ctrl Pts',(60.4404467789386,243.442701746765,24.9000865264635)) ;
#108059 = CARTESIAN_POINT('Ctrl Pts',(60.4428319502743,243.434129874892,24.9186005211265)) ;
#108060 = CARTESIAN_POINT('Ctrl Pts',(60.4520052987548,243.417947439168,24.9537361257336)) ;
#108061 = CARTESIAN_POINT('Ctrl Pts',(60.4586423249844,243.410239816549,24.9705605654438)) ;
#108062 = CARTESIAN_POINT('Ctrl Pts',(60.4774783235664,243.395163543695,25.0036148517977)) ;
#108063 = CARTESIAN_POINT('Ctrl Pts',(60.4902886559451,243.387856735537,25.0197271316054)) ;
#108064 = CARTESIAN_POINT('Ctrl Pts',(60.5183067650571,243.377274235219,25.0431407641495)) ;
#108065 = CARTESIAN_POINT('Ctrl Pts',(60.5322233323112,243.373501577211,25.051518136121)) ;
#108066 = CARTESIAN_POINT('Ctrl Pts',(60.5612197979217,243.368733650287,25.0621166715428)) ;
#108067 = CARTESIAN_POINT('Ctrl Pts',(60.5755858845327,243.367543770797,25.0647672615988)) ;
#108068 = CARTESIAN_POINT('Ctrl Pts',(60.5902651077865,243.367543770797,25.0647672615988)) ;
#108069 = CARTESIAN_POINT('Origin',(60.5902651077865,245.878117316722,24.0913131340507)) ;
#108070 = CARTESIAN_POINT('Ctrl Pts',(60.4402651077865,242.935532853835,25.0474167838717)) ;
#108071 = CARTESIAN_POINT('Ctrl Pts',(60.4402651077865,242.936021132653,25.0487912940387)) ;
#108072 = CARTESIAN_POINT('Ctrl Pts',(60.440286369022,242.936509268827,25.0501657727844)) ;
#108073 = CARTESIAN_POINT('Ctrl Pts',(60.4403288850239,242.936997109009,25.0515397810631)) ;
#108074 = CARTESIAN_POINT('Ctrl Pts',(60.4408750760621,242.943264253706,25.0691912764098)) ;
#108075 = CARTESIAN_POINT('Ctrl Pts',(60.4449239452531,242.949422948319,25.0865982562063)) ;
#108076 = CARTESIAN_POINT('Ctrl Pts',(60.452266539598,242.955161109892,25.1028558131956)) ;
#108077 = CARTESIAN_POINT('Ctrl Pts',(60.4599211853139,242.961143136386,25.119804296676)) ;
#108078 = CARTESIAN_POINT('Ctrl Pts',(60.4710122117669,242.966556490128,25.1351862430876)) ;
#108079 = CARTESIAN_POINT('Ctrl Pts',(60.4849165768426,242.97110602301,25.1481321115104)) ;
#108080 = CARTESIAN_POINT('Ctrl Pts',(60.4988172216939,242.975654338627,25.1610745161621)) ;
#108081 = CARTESIAN_POINT('Ctrl Pts',(60.5152637963994,242.979252524414,25.1713344497827)) ;
#108082 = CARTESIAN_POINT('Ctrl Pts',(60.5333315664698,242.981705224984,25.1783314111464)) ;
#108083 = CARTESIAN_POINT('Ctrl Pts',(60.5513971100607,242.984157623309,25.185327510279)) ;
#108084 = CARTESIAN_POINT('Ctrl Pts',(60.5707376338847,242.985417987428,25.1889274550538)) ;
#108085 = CARTESIAN_POINT('Ctrl Pts',(60.5902651077865,242.985417987428,25.1889274550538)) ;
#108086 = CARTESIAN_POINT('Origin',(60.5902651077865,250.050447394148,24.9137882607786)) ;
#108087 = CARTESIAN_POINT('',(60.5902651077865,251.852827359384,26.4087041537722)) ;
#108088 = CARTESIAN_POINT('',(60.5902651077865,252.1778829659,26.6448708758722)) ;
#108089 = CARTESIAN_POINT('',(60.5902651077865,249.962279606305,25.0351408099348)) ;
#108090 = CARTESIAN_POINT('Ctrl Pts',(60.5902651077865,252.177882965899,26.6448708758719)) ;
#108091 = CARTESIAN_POINT('Ctrl Pts',(60.5707376338846,252.177882965899,26.6448708758719)) ;
#108092 = CARTESIAN_POINT('Ctrl Pts',(60.5513971100607,252.180194087522,26.6418365988679)) ;
#108093 = CARTESIAN_POINT('Ctrl Pts',(60.5333315664698,252.184688370456,26.6359407459586)) ;
#108094 = CARTESIAN_POINT('Ctrl Pts',(60.5152637963993,252.189183207286,26.6300441664176)) ;
#108095 = CARTESIAN_POINT('Ctrl Pts',(60.4988172216936,252.195775779175,26.6213982902475)) ;
#108096 = CARTESIAN_POINT('Ctrl Pts',(60.4849165768425,252.204100907366,26.6104948387886)) ;
#108097 = CARTESIAN_POINT('Ctrl Pts',(60.4710122117668,252.212428263609,26.599588469243)) ;
#108098 = CARTESIAN_POINT('Ctrl Pts',(60.4599211853138,252.222329951809,26.5866321871782)) ;
#108099 = CARTESIAN_POINT('Ctrl Pts',(60.452266539598,252.233256566511,26.5723617693702)) ;
#108100 = CARTESIAN_POINT('Ctrl Pts',(60.4449239452532,252.243737743863,26.5586731032993)) ;
#108101 = CARTESIAN_POINT('Ctrl Pts',(60.4408750760621,252.254974063087,26.544021223037)) ;
#108102 = CARTESIAN_POINT('Ctrl Pts',(60.4403288850239,252.266389083925,26.5291703075782)) ;
#108103 = CARTESIAN_POINT('Ctrl Pts',(60.440286369022,252.267277639417,26.5280142989575)) ;
#108104 = CARTESIAN_POINT('Ctrl Pts',(60.4402651077865,252.268166621798,26.5268579343646)) ;
#108105 = CARTESIAN_POINT('Ctrl Pts',(60.4402651077865,252.26905574955,26.5257015839662)) ;
#108106 = CARTESIAN_POINT('Ctrl Pts',(60.4402651077865,251.829484664171,26.2063344963563)) ;
#108107 = CARTESIAN_POINT('Ctrl Pts',(60.4402651077865,251.829580454454,26.2071173906402)) ;
#108108 = CARTESIAN_POINT('Ctrl Pts',(60.4402684378921,251.82967618164,26.2079002983041)) ;
#108109 = CARTESIAN_POINT('Ctrl Pts',(60.4404467789386,251.832237022391,26.2288583756768)) ;
#108110 = CARTESIAN_POINT('Ctrl Pts',(60.4428319502743,251.834668218008,26.2491150850258)) ;
#108111 = CARTESIAN_POINT('Ctrl Pts',(60.4520052987548,251.839201130021,26.2875316783904)) ;
#108112 = CARTESIAN_POINT('Ctrl Pts',(60.4586423249844,251.841332476948,26.3059144577855)) ;
#108113 = CARTESIAN_POINT('Ctrl Pts',(60.4774783235664,251.845456528266,26.3420097767374)) ;
#108114 = CARTESIAN_POINT('Ctrl Pts',(60.4902886559451,251.847426747499,26.3595913933363)) ;
#108115 = CARTESIAN_POINT('Ctrl Pts',(60.5183067650572,251.85025609303,26.3851292535789)) ;
#108116 = CARTESIAN_POINT('Ctrl Pts',(60.5322233323112,251.851255353705,26.3942624232203)) ;
#108117 = CARTESIAN_POINT('Ctrl Pts',(60.5612197979217,251.852514794114,26.4058155998437)) ;
#108118 = CARTESIAN_POINT('Ctrl Pts',(60.5755858845327,251.852827359384,26.4087041537722)) ;
#108119 = CARTESIAN_POINT('Ctrl Pts',(60.5902651077865,251.852827359384,26.4087041537722)) ;
#108120 = CARTESIAN_POINT('Origin',(60.5902651077865,245.327670899104,23.5352272428401)) ;
#108121 = CARTESIAN_POINT('Ctrl Pts',(60.4402651077865,243.236287157908,24.2147590127358)) ;
#108122 = CARTESIAN_POINT('Ctrl Pts',(60.4402651077865,243.235597479012,24.2143763349887)) ;
#108123 = CARTESIAN_POINT('Ctrl Pts',(60.4402684378921,243.234907826379,24.2139935983299)) ;
#108124 = CARTESIAN_POINT('Ctrl Pts',(60.4404467789386,243.216447161187,24.2037465132216)) ;
#108125 = CARTESIAN_POINT('Ctrl Pts',(60.4428319502744,243.198630118145,24.1938067967771)) ;
#108126 = CARTESIAN_POINT('Ctrl Pts',(60.4520052987547,243.164886062416,24.1748932926071)) ;
#108127 = CARTESIAN_POINT('Ctrl Pts',(60.4586423249843,243.14876130719,24.1658124618669)) ;
#108128 = CARTESIAN_POINT('Ctrl Pts',(60.4774783235664,243.117135524196,24.1479325933122)) ;
#108129 = CARTESIAN_POINT('Ctrl Pts',(60.490288655945,243.10175363177,24.1391923192063)) ;
#108130 = CARTESIAN_POINT('Ctrl Pts',(60.5183067650571,243.079430021257,24.1264705301978)) ;
#108131 = CARTESIAN_POINT('Ctrl Pts',(60.5322233323112,243.071453781117,24.1219106066435)) ;
#108132 = CARTESIAN_POINT('Ctrl Pts',(60.5612197979217,243.061366784391,24.1161387285016)) ;
#108133 = CARTESIAN_POINT('Ctrl Pts',(60.5755858845327,243.058846173917,24.1146937497176)) ;
#108134 = CARTESIAN_POINT('Ctrl Pts',(60.5902651077865,243.058846173917,24.1146937497176)) ;
#108135 = CARTESIAN_POINT('Ctrl Pts',(60.5902651077865,242.676720390548,24.2388539431728)) ;
#108136 = CARTESIAN_POINT('Ctrl Pts',(60.5707376338847,242.676720390548,24.2388539431728)) ;
#108137 = CARTESIAN_POINT('Ctrl Pts',(60.5513971100608,242.677816729004,24.2425071831162)) ;
#108138 = CARTESIAN_POINT('Ctrl Pts',(60.5333315664699,242.679944900976,24.249608629777)) ;
#108139 = CARTESIAN_POINT('Ctrl Pts',(60.5152637963994,242.682073335234,24.2567109516523)) ;
#108140 = CARTESIAN_POINT('Ctrl Pts',(60.4988172216939,242.685192979455,24.2671263728531)) ;
#108141 = CARTESIAN_POINT('Ctrl Pts',(60.4849165768427,242.689120669408,24.2802704310071)) ;
#108142 = CARTESIAN_POINT('Ctrl Pts',(60.4710122117669,242.693049410527,24.2934180069008)) ;
#108143 = CARTESIAN_POINT('Ctrl Pts',(60.4599211853139,242.697711196606,24.3090441524492)) ;
#108144 = CARTESIAN_POINT('Ctrl Pts',(60.4522665395981,242.702833704151,24.3262719105652)) ;
#108145 = CARTESIAN_POINT('Ctrl Pts',(60.4449239452532,242.707747386159,24.3427973572042)) ;
#108146 = CARTESIAN_POINT('Ctrl Pts',(60.4408750760622,242.71299646356,24.3604998895482)) ;
#108147 = CARTESIAN_POINT('Ctrl Pts',(60.4403288850239,242.718301525644,24.3784639844864)) ;
#108148 = CARTESIAN_POINT('Ctrl Pts',(60.440286369022,242.718714476449,24.3798623257986)) ;
#108149 = CARTESIAN_POINT('Ctrl Pts',(60.4402651077865,242.719127464324,24.3812612217067)) ;
#108150 = CARTESIAN_POINT('Ctrl Pts',(60.4402651077865,242.719540355267,24.3826602268792)) ;
#108151 = CARTESIAN_POINT('Origin',(60.5902651077865,248.040265107786,23.0213203435596)) ;
#108152 = CARTESIAN_POINT('Ctrl Pts',(60.4402651077865,243.102617743897,23.3708035475559)) ;
#108153 = CARTESIAN_POINT('Ctrl Pts',(60.4402651077865,243.102080074215,23.3713806182205)) ;
#108154 = CARTESIAN_POINT('Ctrl Pts',(60.4402684378921,243.101542447717,23.3719577367977)) ;
#108155 = CARTESIAN_POINT('Ctrl Pts',(60.4404467789386,243.087151835233,23.3874079531342)) ;
#108156 = CARTESIAN_POINT('Ctrl Pts',(60.4428319502743,243.073278361647,23.4023669543188)) ;
#108157 = CARTESIAN_POINT('Ctrl Pts',(60.4520052987548,243.047030451771,23.4307822523853)) ;
#108158 = CARTESIAN_POINT('Ctrl Pts',(60.4586423249844,243.034501029262,23.4444014590289)) ;
#108159 = CARTESIAN_POINT('Ctrl Pts',(60.4774783235664,243.009948305503,23.4711791289339)) ;
#108160 = CARTESIAN_POINT('Ctrl Pts',(60.4902886559451,242.998020149712,23.4842448897419)) ;
#108161 = CARTESIAN_POINT('Ctrl Pts',(60.5183067650572,242.98072038347,23.5032424051016)) ;
#108162 = CARTESIAN_POINT('Ctrl Pts',(60.5322233323113,242.97454362218,23.5100439438662)) ;
#108163 = CARTESIAN_POINT('Ctrl Pts',(60.5612197979217,242.966733926649,23.5186503795949)) ;
#108164 = CARTESIAN_POINT('Ctrl Pts',(60.5755858845327,242.964783206634,23.5208035475559)) ;
#108165 = CARTESIAN_POINT('Ctrl Pts',(60.5902651077865,242.964783206634,23.5208035475559)) ;
#108166 = CARTESIAN_POINT('Origin',(60.5902651077865,245.653294405781,23.3708035475559)) ;
#108167 = CARTESIAN_POINT('Ctrl Pts',(60.4402651077865,242.559278001425,23.3708035475559)) ;
#108168 = CARTESIAN_POINT('Ctrl Pts',(60.4402651077865,242.559317635176,23.3722616708597)) ;
#108169 = CARTESIAN_POINT('Ctrl Pts',(60.440286369022,242.559357142975,23.3737197202007)) ;
#108170 = CARTESIAN_POINT('Ctrl Pts',(60.4403288850239,242.55939651465,23.3751772306343)) ;
#108171 = CARTESIAN_POINT('Ctrl Pts',(60.4408750760621,242.559902311413,23.3939014545242)) ;
#108172 = CARTESIAN_POINT('Ctrl Pts',(60.4449239452532,242.560380525479,23.4123596173871)) ;
#108173 = CARTESIAN_POINT('Ctrl Pts',(60.4522665395981,242.560813980038,23.4295946623433)) ;
#108174 = CARTESIAN_POINT('Ctrl Pts',(60.4599211853139,242.561265855891,23.4475621758458)) ;
#108175 = CARTESIAN_POINT('Ctrl Pts',(60.4710122117669,242.561660978396,23.4638640945168)) ;
#108176 = CARTESIAN_POINT('Ctrl Pts',(60.4849165768427,242.561987347939,23.4775822300163)) ;
#108177 = CARTESIAN_POINT('Ctrl Pts',(60.498817221694,242.56231363016,23.4912966951184)) ;
#108178 = CARTESIAN_POINT('Ctrl Pts',(60.5152637963995,242.562565214349,23.5021663724021)) ;
#108179 = CARTESIAN_POINT('Ctrl Pts',(60.5333315664699,242.562735691238,23.5095788042595)) ;
#108180 = CARTESIAN_POINT('Ctrl Pts',(60.5513971100607,242.56290614712,23.5169903226877)) ;
#108181 = CARTESIAN_POINT('Ctrl Pts',(60.5707376338847,242.562992380514,23.5208035475559)) ;
#108182 = CARTESIAN_POINT('Ctrl Pts',(60.5902651077865,242.562992380514,23.5208035475559)) ;
#108183 = CARTESIAN_POINT('Origin',(60.5902651077865,250.536866817902,24.1999837998328)) ;
#108184 = CARTESIAN_POINT('',(60.5902651077865,252.712986444776,25.0647672615988)) ;
#108185 = CARTESIAN_POINT('',(60.5902651077865,253.095112228145,25.188927455054)) ;
#108186 = CARTESIAN_POINT('',(60.5902651077865,250.490514268746,24.3426422772771)) ;
#108187 = CARTESIAN_POINT('Ctrl Pts',(60.5902651077865,253.095112228145,25.1889274550539)) ;
#108188 = CARTESIAN_POINT('Ctrl Pts',(60.5707376338848,253.095112228145,25.1889274550539)) ;
#108189 = CARTESIAN_POINT('Ctrl Pts',(60.5513971100608,253.096372592264,25.1853275102792)) ;
#108190 = CARTESIAN_POINT('Ctrl Pts',(60.5333315664699,253.098824990589,25.1783314111465)) ;
#108191 = CARTESIAN_POINT('Ctrl Pts',(60.5152637963995,253.101277691159,25.1713344497829)) ;
#108192 = CARTESIAN_POINT('Ctrl Pts',(60.4988172216938,253.104875876946,25.1610745161622)) ;
#108193 = CARTESIAN_POINT('Ctrl Pts',(60.4849165768426,253.109424192563,25.1481321115104)) ;
#108194 = CARTESIAN_POINT('Ctrl Pts',(60.4710122117668,253.113973725445,25.1351862430876)) ;
#108195 = CARTESIAN_POINT('Ctrl Pts',(60.4599211853139,253.119387079187,25.119804296676)) ;
#108196 = CARTESIAN_POINT('Ctrl Pts',(60.452266539598,253.125369105681,25.1028558131957)) ;
#108197 = CARTESIAN_POINT('Ctrl Pts',(60.4449239452531,253.131107267254,25.0865982562064)) ;
#108198 = CARTESIAN_POINT('Ctrl Pts',(60.4408750760621,253.137265961864,25.0691912764081)) ;
#108199 = CARTESIAN_POINT('Ctrl Pts',(60.4403288850239,253.143533106564,25.051539781063)) ;
#108200 = CARTESIAN_POINT('Ctrl Pts',(60.440286369022,253.144020946746,25.0501657727844)) ;
#108201 = CARTESIAN_POINT('Ctrl Pts',(60.4402651077865,253.144509082921,25.0487912940391)) ;
#108202 = CARTESIAN_POINT('Ctrl Pts',(60.4402651077865,253.144997361739,25.0474167838722)) ;
#108203 = CARTESIAN_POINT('Ctrl Pts',(60.4402651077865,252.628250559098,24.8795155697285)) ;
#108204 = CARTESIAN_POINT('Ctrl Pts',(60.4402651077865,252.62858358871,24.8802305456146)) ;
#108205 = CARTESIAN_POINT('Ctrl Pts',(60.4402684378921,252.628916562447,24.8809455537241)) ;
#108206 = CARTESIAN_POINT('Ctrl Pts',(60.4404467789389,252.637828468809,24.9000865264659)) ;
#108207 = CARTESIAN_POINT('Ctrl Pts',(60.4428319502748,252.646400340681,24.9186005211289)) ;
#108208 = CARTESIAN_POINT('Ctrl Pts',(60.4520052987552,252.662582776405,24.9537361257345)) ;
#108209 = CARTESIAN_POINT('Ctrl Pts',(60.4586423249846,252.670290399024,24.9705605654442)) ;
#108210 = CARTESIAN_POINT('Ctrl Pts',(60.4774783235664,252.685366671877,25.0036148517979)) ;
#108211 = CARTESIAN_POINT('Ctrl Pts',(60.4902886559451,252.692673480035,25.0197271316054)) ;
#108212 = CARTESIAN_POINT('Ctrl Pts',(60.5183067650571,252.703255980354,25.0431407641494)) ;
#108213 = CARTESIAN_POINT('Ctrl Pts',(60.5322233323112,252.707028638362,25.051518136121)) ;
#108214 = CARTESIAN_POINT('Ctrl Pts',(60.5612197979217,252.711796565285,25.0621166715428)) ;
#108215 = CARTESIAN_POINT('Ctrl Pts',(60.5755858845327,252.712986444776,25.0647672615988)) ;
#108216 = CARTESIAN_POINT('Ctrl Pts',(60.5902651077865,252.712986444776,25.0647672615988)) ;
#108217 = CARTESIAN_POINT('Origin',(60.5902651077865,245.30162874415,22.6718371395634)) ;
#108218 = CARTESIAN_POINT('Ctrl Pts',(60.4402651077865,243.102617743897,22.6718371395634)) ;
#108219 = CARTESIAN_POINT('Ctrl Pts',(60.4402651077865,243.102080074216,22.6712600688998)) ;
#108220 = CARTESIAN_POINT('Ctrl Pts',(60.440268437892,243.101542447719,22.6706829503236)) ;
#108221 = CARTESIAN_POINT('Ctrl Pts',(60.4404467789383,243.087151835235,22.6552327339874)) ;
#108222 = CARTESIAN_POINT('Ctrl Pts',(60.4428319502739,243.073278361649,22.6402737328024)) ;
#108223 = CARTESIAN_POINT('Ctrl Pts',(60.4520052987543,243.047030451772,22.611858434735)) ;
#108224 = CARTESIAN_POINT('Ctrl Pts',(60.4586423249841,243.034501029262,22.5982392280909)) ;
#108225 = CARTESIAN_POINT('Ctrl Pts',(60.4774783235664,243.009948305503,22.5714615581854)) ;
#108226 = CARTESIAN_POINT('Ctrl Pts',(60.4902886559451,242.998020149712,22.5583957973774)) ;
#108227 = CARTESIAN_POINT('Ctrl Pts',(60.5183067650572,242.98072038347,22.5393982820177)) ;
#108228 = CARTESIAN_POINT('Ctrl Pts',(60.5322233323112,242.97454362218,22.5325967432531)) ;
#108229 = CARTESIAN_POINT('Ctrl Pts',(60.5612197979217,242.966733926649,22.5239903075244)) ;
#108230 = CARTESIAN_POINT('Ctrl Pts',(60.5755858845327,242.964783206634,22.5218371395634)) ;
#108231 = CARTESIAN_POINT('Ctrl Pts',(60.5902651077865,242.964783206634,22.5218371395634)) ;
#108232 = CARTESIAN_POINT('Ctrl Pts',(60.5902651077865,242.562992380513,22.5218371395634)) ;
#108233 = CARTESIAN_POINT('Ctrl Pts',(60.5707376338847,242.562992380513,22.5218371395634)) ;
#108234 = CARTESIAN_POINT('Ctrl Pts',(60.5513971100607,242.562906147119,22.5256503644316)) ;
#108235 = CARTESIAN_POINT('Ctrl Pts',(60.5333315664699,242.562735691238,22.5330618828598)) ;
#108236 = CARTESIAN_POINT('Ctrl Pts',(60.5152637963995,242.562565214349,22.5404743147172)) ;
#108237 = CARTESIAN_POINT('Ctrl Pts',(60.498817221694,242.56231363016,22.5513439920009)) ;
#108238 = CARTESIAN_POINT('Ctrl Pts',(60.4849165768426,242.561987347939,22.5650584571031)) ;
#108239 = CARTESIAN_POINT('Ctrl Pts',(60.4710122117667,242.561660978396,22.5787765926026)) ;
#108240 = CARTESIAN_POINT('Ctrl Pts',(60.4599211853138,242.561265855892,22.5950785112737)) ;
#108241 = CARTESIAN_POINT('Ctrl Pts',(60.452266539598,242.56081398004,22.6130460247761)) ;
#108242 = CARTESIAN_POINT('Ctrl Pts',(60.4449239452532,242.560380525481,22.6302810697323)) ;
#108243 = CARTESIAN_POINT('Ctrl Pts',(60.4408750760621,242.559902311412,22.6487392325954)) ;
#108244 = CARTESIAN_POINT('Ctrl Pts',(60.4403288850239,242.559396514649,22.6674634564849)) ;
#108245 = CARTESIAN_POINT('Ctrl Pts',(60.440286369022,242.559357142974,22.6689209669185)) ;
#108246 = CARTESIAN_POINT('Ctrl Pts',(60.4402651077865,242.559317635176,22.6703790162596)) ;
#108247 = CARTESIAN_POINT('Ctrl Pts',(60.4402651077865,242.559278001424,22.6718371395634)) ;
#108248 = CARTESIAN_POINT('Origin',(60.5902651077865,248.040265107786,23.0213203435596)) ;
#108249 = CARTESIAN_POINT('Ctrl Pts',(60.4402651077865,243.236287157908,21.8278816743835)) ;
#108250 = CARTESIAN_POINT('Ctrl Pts',(60.4402651077865,243.235597479012,21.8282643521305)) ;
#108251 = CARTESIAN_POINT('Ctrl Pts',(60.4402684378921,243.234907826379,21.8286470887893)) ;
#108252 = CARTESIAN_POINT('Ctrl Pts',(60.4404467789386,243.216447161187,21.8388941738976)) ;
#108253 = CARTESIAN_POINT('Ctrl Pts',(60.4428319502744,243.198630118145,21.8488338903421)) ;
#108254 = CARTESIAN_POINT('Ctrl Pts',(60.4520052987547,243.164886062416,21.8677473945122)) ;
#108255 = CARTESIAN_POINT('Ctrl Pts',(60.4586423249844,243.14876130719,21.8768282252524)) ;
#108256 = CARTESIAN_POINT('Ctrl Pts',(60.4774783235664,243.117135524196,21.8947080938071)) ;
#108257 = CARTESIAN_POINT('Ctrl Pts',(60.4902886559451,243.10175363177,21.903448367913)) ;
#108258 = CARTESIAN_POINT('Ctrl Pts',(60.5183067650572,243.079430021257,21.9161701569215)) ;
#108259 = CARTESIAN_POINT('Ctrl Pts',(60.5322233323112,243.071453781117,21.9207300804757)) ;
#108260 = CARTESIAN_POINT('Ctrl Pts',(60.5612197979217,243.061366784391,21.9265019586177)) ;
#108261 = CARTESIAN_POINT('Ctrl Pts',(60.5755858845327,243.058846173917,21.9279469374017)) ;
#108262 = CARTESIAN_POINT('Ctrl Pts',(60.5902651077865,243.058846173917,21.9279469374017)) ;
#108263 = CARTESIAN_POINT('Origin',(60.5902651077865,245.662124818155,22.6160841100613)) ;
#108264 = CARTESIAN_POINT('Ctrl Pts',(60.4402651077865,242.719540355268,21.6599804602402)) ;
#108265 = CARTESIAN_POINT('Ctrl Pts',(60.4402651077865,242.719127464324,21.6613794654127)) ;
#108266 = CARTESIAN_POINT('Ctrl Pts',(60.440286369022,242.71871447645,21.6627783613207)) ;
#108267 = CARTESIAN_POINT('Ctrl Pts',(60.4403288850239,242.718301525644,21.6641767026329)) ;
#108268 = CARTESIAN_POINT('Ctrl Pts',(60.4408750760621,242.71299646356,21.6821407975714)) ;
#108269 = CARTESIAN_POINT('Ctrl Pts',(60.4449239452532,242.707747386159,21.6998433299151)) ;
#108270 = CARTESIAN_POINT('Ctrl Pts',(60.452266539598,242.702833704151,21.716368776554)) ;
#108271 = CARTESIAN_POINT('Ctrl Pts',(60.4599211853138,242.697711196606,21.7335965346699)) ;
#108272 = CARTESIAN_POINT('Ctrl Pts',(60.4710122117667,242.693049410527,21.7492226802185)) ;
#108273 = CARTESIAN_POINT('Ctrl Pts',(60.4849165768426,242.689120669408,21.7623702561122)) ;
#108274 = CARTESIAN_POINT('Ctrl Pts',(60.4988172216939,242.685192979455,21.7755143142664)) ;
#108275 = CARTESIAN_POINT('Ctrl Pts',(60.5152637963995,242.682073335233,21.7859297354669)) ;
#108276 = CARTESIAN_POINT('Ctrl Pts',(60.5333315664699,242.679944900976,21.7930320573423)) ;
#108277 = CARTESIAN_POINT('Ctrl Pts',(60.5513971100607,242.677816729004,21.8001335040032)) ;
#108278 = CARTESIAN_POINT('Ctrl Pts',(60.5707376338847,242.676720390548,21.8037867439466)) ;
#108279 = CARTESIAN_POINT('Ctrl Pts',(60.5902651077865,242.676720390548,21.8037867439466)) ;
#108280 = CARTESIAN_POINT('Origin',(60.5902651077865,250.778901471423,23.3708035475559)) ;
#108281 = CARTESIAN_POINT('',(60.5902651077865,253.115747008939,23.5208035475559)) ;
#108282 = CARTESIAN_POINT('',(60.5902651077865,253.517537835059,23.5208035475559)) ;
#108283 = CARTESIAN_POINT('',(60.5902651077865,250.778901471423,23.5208035475559)) ;
#108284 = CARTESIAN_POINT('Ctrl Pts',(60.5902651077865,253.517537835059,23.5208035475559)) ;
#108285 = CARTESIAN_POINT('Ctrl Pts',(60.5707376338847,253.517537835059,23.5208035475559)) ;
#108286 = CARTESIAN_POINT('Ctrl Pts',(60.5513971100607,253.517624068453,23.5169903226877)) ;
#108287 = CARTESIAN_POINT('Ctrl Pts',(60.5333315664699,253.517794524334,23.5095788042595)) ;
#108288 = CARTESIAN_POINT('Ctrl Pts',(60.5152637963995,253.517965001223,23.5021663724021)) ;
#108289 = CARTESIAN_POINT('Ctrl Pts',(60.498817221694,253.518216585412,23.4912966951184)) ;
#108290 = CARTESIAN_POINT('Ctrl Pts',(60.4849165768426,253.518542867633,23.4775822300162)) ;
#108291 = CARTESIAN_POINT('Ctrl Pts',(60.4710122117667,253.518869237177,23.4638640945167)) ;
#108292 = CARTESIAN_POINT('Ctrl Pts',(60.4599211853138,253.51926435968,23.4475621758456)) ;
#108293 = CARTESIAN_POINT('Ctrl Pts',(60.452266539598,253.519716235533,23.4295946623432)) ;
#108294 = CARTESIAN_POINT('Ctrl Pts',(60.4449239452532,253.520149690091,23.412359617387)) ;
#108295 = CARTESIAN_POINT('Ctrl Pts',(60.4408750760621,253.52062790416,23.393901454524)) ;
#108296 = CARTESIAN_POINT('Ctrl Pts',(60.4403288850239,253.521133700923,23.3751772306343)) ;
#108297 = CARTESIAN_POINT('Ctrl Pts',(60.440286369022,253.521173072598,23.3737197202007)) ;
#108298 = CARTESIAN_POINT('Ctrl Pts',(60.4402651077865,253.521212580397,23.3722616708597)) ;
#108299 = CARTESIAN_POINT('Ctrl Pts',(60.4402651077865,253.521252214148,23.3708035475559)) ;
#108300 = CARTESIAN_POINT('Ctrl Pts',(60.4402651077865,252.977912471676,23.3708035475559)) ;
#108301 = CARTESIAN_POINT('Ctrl Pts',(60.4402651077865,252.978450141356,23.3713806182195)) ;
#108302 = CARTESIAN_POINT('Ctrl Pts',(60.440268437892,252.978987767854,23.3719577367957)) ;
#108303 = CARTESIAN_POINT('Ctrl Pts',(60.4404467789383,252.993378380338,23.3874079531319)) ;
#108304 = CARTESIAN_POINT('Ctrl Pts',(60.4428319502739,253.007251853924,23.4023669543169)) ;
#108305 = CARTESIAN_POINT('Ctrl Pts',(60.4520052987543,253.033499763801,23.4307822523842)) ;
#108306 = CARTESIAN_POINT('Ctrl Pts',(60.4586423249841,253.04602918631,23.4444014590284)) ;
#108307 = CARTESIAN_POINT('Ctrl Pts',(60.4774783235664,253.07058191007,23.4711791289339)) ;
#108308 = CARTESIAN_POINT('Ctrl Pts',(60.4902886559451,253.08251006586,23.4842448897419)) ;
#108309 = CARTESIAN_POINT('Ctrl Pts',(60.5183067650572,253.099809832103,23.5032424051016)) ;
#108310 = CARTESIAN_POINT('Ctrl Pts',(60.5322233323112,253.105986593393,23.5100439438662)) ;
#108311 = CARTESIAN_POINT('Ctrl Pts',(60.5612197979217,253.113796288923,23.5186503795949)) ;
#108312 = CARTESIAN_POINT('Ctrl Pts',(60.5755858845327,253.115747008939,23.5208035475559)) ;
#108313 = CARTESIAN_POINT('Ctrl Pts',(60.5902651077865,253.115747008939,23.5208035475559)) ;
#108314 = CARTESIAN_POINT('Origin',(60.5902651077865,245.543663397671,21.8426568872864)) ;
#108315 = CARTESIAN_POINT('Ctrl Pts',(60.4402651077865,243.452279656475,21.1631251173908)) ;
#108316 = CARTESIAN_POINT('Ctrl Pts',(60.4402651077865,243.451946626863,21.162410141506)) ;
#108317 = CARTESIAN_POINT('Ctrl Pts',(60.4402684378921,243.451613653127,21.1616951333977)) ;
#108318 = CARTESIAN_POINT('Ctrl Pts',(60.4404467789386,243.442701746765,21.1425541606558)) ;
#108319 = CARTESIAN_POINT('Ctrl Pts',(60.4428319502743,243.434129874892,21.1240401659927)) ;
#108320 = CARTESIAN_POINT('Ctrl Pts',(60.4520052987547,243.417947439169,21.0889045613858)) ;
#108321 = CARTESIAN_POINT('Ctrl Pts',(60.4586423249843,243.410239816549,21.0720801216756)) ;
#108322 = CARTESIAN_POINT('Ctrl Pts',(60.4774783235664,243.395163543695,21.0390258353215)) ;
#108323 = CARTESIAN_POINT('Ctrl Pts',(60.4902886559451,243.387856735537,21.0229135555139)) ;
#108324 = CARTESIAN_POINT('Ctrl Pts',(60.5183067650571,243.377274235219,20.9994999229698)) ;
#108325 = CARTESIAN_POINT('Ctrl Pts',(60.5322233323112,243.373501577211,20.9911225509982)) ;
#108326 = CARTESIAN_POINT('Ctrl Pts',(60.5612197979217,243.368733650287,20.9805240155765)) ;
#108327 = CARTESIAN_POINT('Ctrl Pts',(60.5755858845327,243.367543770797,20.9778734255204)) ;
#108328 = CARTESIAN_POINT('Ctrl Pts',(60.5902651077865,243.367543770797,20.9778734255204)) ;
#108329 = CARTESIAN_POINT('Ctrl Pts',(60.5902651077865,242.985417987427,20.853713232065)) ;
#108330 = CARTESIAN_POINT('Ctrl Pts',(60.5707376338848,242.985417987427,20.853713232065)) ;
#108331 = CARTESIAN_POINT('Ctrl Pts',(60.5513971100606,242.984157623308,20.8573131768398)) ;
#108332 = CARTESIAN_POINT('Ctrl Pts',(60.5333315664698,242.981705224983,20.8643092759726)) ;
#108333 = CARTESIAN_POINT('Ctrl Pts',(60.5152637963994,242.979252524414,20.8713062373364)) ;
#108334 = CARTESIAN_POINT('Ctrl Pts',(60.4988172216939,242.975654338627,20.881566170957)) ;
#108335 = CARTESIAN_POINT('Ctrl Pts',(60.4849165768425,242.97110602301,20.8945085756088)) ;
#108336 = CARTESIAN_POINT('Ctrl Pts',(60.4710122117666,242.966556490128,20.9074544440317)) ;
#108337 = CARTESIAN_POINT('Ctrl Pts',(60.4599211853137,242.961143136386,20.9228363904435)) ;
#108338 = CARTESIAN_POINT('Ctrl Pts',(60.452266539598,242.955161109893,20.9397848739239)) ;
#108339 = CARTESIAN_POINT('Ctrl Pts',(60.4449239452531,242.94942294832,20.9560424309132)) ;
#108340 = CARTESIAN_POINT('Ctrl Pts',(60.4408750760621,242.943264253706,20.9734494107093)) ;
#108341 = CARTESIAN_POINT('Ctrl Pts',(60.4403288850239,242.936997109009,20.9911009060562)) ;
#108342 = CARTESIAN_POINT('Ctrl Pts',(60.440286369022,242.936509268827,20.992474914335)) ;
#108343 = CARTESIAN_POINT('Ctrl Pts',(60.4402651077865,242.936021132652,20.9938493930803)) ;
#108344 = CARTESIAN_POINT('Ctrl Pts',(60.4402651077865,242.935532853834,20.9952239032473)) ;
#108345 = CARTESIAN_POINT('Origin',(60.5902651077865,248.040265107786,23.0213203435596)) ;
#108346 = CARTESIAN_POINT('Ctrl Pts',(60.4402651077865,243.840203404936,20.4017818933262)) ;
#108347 = CARTESIAN_POINT('Ctrl Pts',(60.4402651077865,243.8394292274,20.4019327189915)) ;
#108348 = CARTESIAN_POINT('Ctrl Pts',(60.4402684378921,243.838655056638,20.402083608801)) ;
#108349 = CARTESIAN_POINT('Ctrl Pts',(60.4404467789386,243.817931397271,20.4061245065949)) ;
#108350 = CARTESIAN_POINT('Ctrl Pts',(60.4428319502743,243.797914841084,20.4100719696)) ;
#108351 = CARTESIAN_POINT('Ctrl Pts',(60.4520052987548,243.759977742784,20.4176322943074)) ;
#108352 = CARTESIAN_POINT('Ctrl Pts',(60.4586423249845,243.741836058232,20.4212858541613)) ;
#108353 = CARTESIAN_POINT('Ctrl Pts',(60.4774783235665,243.706232967992,20.4285177152552)) ;
#108354 = CARTESIAN_POINT('Ctrl Pts',(60.4902886559452,243.688903025733,20.4320769437325)) ;
#108355 = CARTESIAN_POINT('Ctrl Pts',(60.5183067650571,243.663740761485,20.4372777090437)) ;
#108356 = CARTESIAN_POINT('Ctrl Pts',(60.5322233323112,243.654745812453,20.4391496602992)) ;
#108357 = CARTESIAN_POINT('Ctrl Pts',(60.5612197979217,243.643368900052,20.4415219892068)) ;
#108358 = CARTESIAN_POINT('Ctrl Pts',(60.5755858845327,243.640525134035,20.4421173342227)) ;
#108359 = CARTESIAN_POINT('Ctrl Pts',(60.5902651077865,243.640525134035,20.4421173342227)) ;
#108360 = CARTESIAN_POINT('Origin',(60.5902651077865,245.903744171556,21.9010320185483)) ;
#108361 = CARTESIAN_POINT('Ctrl Pts',(60.4402651077865,243.400632319557,20.0824148057165)) ;
#108362 = CARTESIAN_POINT('Ctrl Pts',(60.4402651077865,243.399807320561,20.0836177483838)) ;
#108363 = CARTESIAN_POINT('Ctrl Pts',(60.440286369022,243.398982263143,20.0848205571812)) ;
#108364 = CARTESIAN_POINT('Ctrl Pts',(60.4403288850239,243.398157412359,20.0860228499813)) ;
#108365 = CARTESIAN_POINT('Ctrl Pts',(60.4408750760622,243.387560787866,20.1014683651894)) ;
#108366 = CARTESIAN_POINT('Ctrl Pts',(60.4449239452533,243.377098235265,20.1166824198105)) ;
#108367 = CARTESIAN_POINT('Ctrl Pts',(60.452266539598,243.367318402122,20.1308806422757)) ;
#108368 = CARTESIAN_POINT('Ctrl Pts',(60.4599211853137,243.357122937909,20.1456822720077)) ;
#108369 = CARTESIAN_POINT('Ctrl Pts',(60.4710122117668,243.347860571349,20.1591030484335)) ;
#108370 = CARTESIAN_POINT('Ctrl Pts',(60.4849165768427,243.340061292121,20.1703930883883)) ;
#108371 = CARTESIAN_POINT('Ctrl Pts',(60.4988172216941,243.332264099652,20.1816801076022)) ;
#108372 = CARTESIAN_POINT('Ctrl Pts',(60.5152637963994,243.326078599533,20.1906217387245)) ;
#108373 = CARTESIAN_POINT('Ctrl Pts',(60.5333315664698,243.321859600104,20.1967187258679)) ;
#108374 = CARTESIAN_POINT('Ctrl Pts',(60.5513971100607,243.317641120579,20.2028149616835)) ;
#108375 = CARTESIAN_POINT('Ctrl Pts',(60.5707376338847,243.315469527519,20.2059506121225)) ;
#108376 = CARTESIAN_POINT('Ctrl Pts',(60.5902651077865,243.315469527519,20.2059506121226)) ;
#108377 = CARTESIAN_POINT('Origin',(60.5902651077865,250.752859316469,22.5074134442792)) ;
#108378 = CARTESIAN_POINT('',(60.5902651077865,253.021684041655,21.9279469374017)) ;
#108379 = CARTESIAN_POINT('',(60.5902651077865,253.403809825024,21.8037867439466)) ;
#108380 = CARTESIAN_POINT('',(60.5902651077865,250.799211865625,22.6500719217234)) ;
#108381 = CARTESIAN_POINT('Ctrl Pts',(60.5902651077865,253.403809825024,21.8037867439468)) ;
#108382 = CARTESIAN_POINT('Ctrl Pts',(60.5707376338847,253.403809825025,21.8037867439465)) ;
#108383 = CARTESIAN_POINT('Ctrl Pts',(60.5513971100607,253.402713486568,21.8001335040034)) ;
#108384 = CARTESIAN_POINT('Ctrl Pts',(60.5333315664699,253.400585314596,21.7930320573425)) ;
#108385 = CARTESIAN_POINT('Ctrl Pts',(60.5152637963994,253.398456880339,21.785929735467)) ;
#108386 = CARTESIAN_POINT('Ctrl Pts',(60.4988172216939,253.395337236117,21.7755143142665)) ;
#108387 = CARTESIAN_POINT('Ctrl Pts',(60.4849165768426,253.391409546164,21.7623702561124)) ;
#108388 = CARTESIAN_POINT('Ctrl Pts',(60.4710122117668,253.387480805045,21.7492226802187)) ;
#108389 = CARTESIAN_POINT('Ctrl Pts',(60.4599211853139,253.382819018967,21.73359653467)) ;
#108390 = CARTESIAN_POINT('Ctrl Pts',(60.452266539598,253.377696511422,21.716368776554)) ;
#108391 = CARTESIAN_POINT('Ctrl Pts',(60.4449239452532,253.372782829414,21.6998433299151)) ;
#108392 = CARTESIAN_POINT('Ctrl Pts',(60.4408750760622,253.367533752023,21.682140797569)) ;
#108393 = CARTESIAN_POINT('Ctrl Pts',(60.4403288850239,253.362228689928,21.6641767026334)) ;
#108394 = CARTESIAN_POINT('Ctrl Pts',(60.440286369022,253.361815739121,21.662778361321)) ;
#108395 = CARTESIAN_POINT('Ctrl Pts',(60.4402651077865,253.361402751249,21.6613794654128)) ;
#108396 = CARTESIAN_POINT('Ctrl Pts',(60.4402651077865,253.360989860306,21.65998046024)) ;
#108397 = CARTESIAN_POINT('Ctrl Pts',(60.4402651077865,252.844243057664,21.8278816743835)) ;
#108398 = CARTESIAN_POINT('Ctrl Pts',(60.4402651077865,252.844932736563,21.8282643521315)) ;
#108399 = CARTESIAN_POINT('Ctrl Pts',(60.440268437892,252.845622389192,21.8286470887883)) ;
#108400 = CARTESIAN_POINT('Ctrl Pts',(60.4404467789386,252.864083054386,21.8388941738985)) ;
#108401 = CARTESIAN_POINT('Ctrl Pts',(60.4428319502744,252.881900097428,21.8488338903423)) ;
#108402 = CARTESIAN_POINT('Ctrl Pts',(60.4520052987548,252.915644153157,21.8677473945122)) ;
#108403 = CARTESIAN_POINT('Ctrl Pts',(60.4586423249844,252.931768908382,21.8768282252524)) ;
#108404 = CARTESIAN_POINT('Ctrl Pts',(60.4774783235665,252.963394691376,21.8947080938071)) ;
#108405 = CARTESIAN_POINT('Ctrl Pts',(60.4902886559452,252.978776583802,21.903448367913)) ;
#108406 = CARTESIAN_POINT('Ctrl Pts',(60.5183067650571,253.001100194315,21.9161701569214)) ;
#108407 = CARTESIAN_POINT('Ctrl Pts',(60.5322233323112,253.009076434455,21.9207300804757)) ;
#108408 = CARTESIAN_POINT('Ctrl Pts',(60.5612197979217,253.019163431181,21.9265019586177)) ;
#108409 = CARTESIAN_POINT('Ctrl Pts',(60.5755858845327,253.021684041655,21.9279469374017)) ;
#108410 = CARTESIAN_POINT('Ctrl Pts',(60.5902651077865,253.021684041655,21.9279469374017)) ;
#108411 = CARTESIAN_POINT('Origin',(60.5902651077865,246.030082821424,21.1288524263407)) ;
#108412 = CARTESIAN_POINT('Ctrl Pts',(60.4402651077865,244.251045551402,19.836306190763)) ;
#108413 = CARTESIAN_POINT('Ctrl Pts',(60.4402651077865,244.250949761118,19.835523296477)) ;
#108414 = CARTESIAN_POINT('Ctrl Pts',(60.440268437892,244.250854033933,19.8347403888173)) ;
#108415 = CARTESIAN_POINT('Ctrl Pts',(60.4404467789386,244.248293193182,19.8137823114415)) ;
#108416 = CARTESIAN_POINT('Ctrl Pts',(60.4428319502744,244.245861997565,19.7935256020932)) ;
#108417 = CARTESIAN_POINT('Ctrl Pts',(60.4520052987548,244.241329085551,19.7551090087287)) ;
#108418 = CARTESIAN_POINT('Ctrl Pts',(60.4586423249845,244.239197738625,19.7367262293337)) ;
#108419 = CARTESIAN_POINT('Ctrl Pts',(60.4774783235665,244.235073687307,19.7006309103817)) ;
#108420 = CARTESIAN_POINT('Ctrl Pts',(60.4902886559452,244.233103468073,19.6830492937829)) ;
#108421 = CARTESIAN_POINT('Ctrl Pts',(60.5183067650571,244.230274122543,19.6575114335404)) ;
#108422 = CARTESIAN_POINT('Ctrl Pts',(60.5322233323112,244.229274861868,19.648378263899)) ;
#108423 = CARTESIAN_POINT('Ctrl Pts',(60.5612197979218,244.228015421459,19.6368250872756)) ;
#108424 = CARTESIAN_POINT('Ctrl Pts',(60.5755858845328,244.227702856188,19.633936533347)) ;
#108425 = CARTESIAN_POINT('Ctrl Pts',(60.5902651077866,244.227702856188,19.6339365333471)) ;
#108426 = CARTESIAN_POINT('Ctrl Pts',(60.5902651077865,243.902647249673,19.3977698112473)) ;
#108427 = CARTESIAN_POINT('Ctrl Pts',(60.5707376338847,243.902647249673,19.3977698112472)) ;
#108428 = CARTESIAN_POINT('Ctrl Pts',(60.5513971100607,243.90033612805,19.4008040882514)) ;
#108429 = CARTESIAN_POINT('Ctrl Pts',(60.5333315664699,243.895841845116,19.4066999411606)) ;
#108430 = CARTESIAN_POINT('Ctrl Pts',(60.5152637963995,243.891347008286,19.4125965207015)) ;
#108431 = CARTESIAN_POINT('Ctrl Pts',(60.4988172216941,243.884754436398,19.4212423968719)) ;
#108432 = CARTESIAN_POINT('Ctrl Pts',(60.4849165768427,243.876429308206,19.4321458483307)) ;
#108433 = CARTESIAN_POINT('Ctrl Pts',(60.4710122117668,243.868101951963,19.4430522178763)) ;
#108434 = CARTESIAN_POINT('Ctrl Pts',(60.459921185314,243.858200263764,19.4560084999413)) ;
#108435 = CARTESIAN_POINT('Ctrl Pts',(60.4522665395982,243.847273649063,19.4702789177496)) ;
#108436 = CARTESIAN_POINT('Ctrl Pts',(60.4449239452534,243.836792471711,19.4839675838205)) ;
#108437 = CARTESIAN_POINT('Ctrl Pts',(60.4408750760622,243.825556152481,19.4986194640776)) ;
#108438 = CARTESIAN_POINT('Ctrl Pts',(60.4403288850239,243.814141131649,19.5134703795415)) ;
#108439 = CARTESIAN_POINT('Ctrl Pts',(60.440286369022,243.813252576157,19.5146263881627)) ;
#108440 = CARTESIAN_POINT('Ctrl Pts',(60.4402651077865,243.812363593775,19.5157827527548)) ;
#108441 = CARTESIAN_POINT('Ctrl Pts',(60.4402651077865,243.811474466023,19.5169391031534)) ;
#108442 = CARTESIAN_POINT('Origin',(60.5902651077865,248.040265107786,23.0213203435596)) ;
#108443 = CARTESIAN_POINT('Ctrl Pts',(60.4402651077865,244.85525095499,19.2321007871753)) ;
#108444 = CARTESIAN_POINT('Ctrl Pts',(60.4402651077865,244.854468060706,19.2320049968919)) ;
#108445 = CARTESIAN_POINT('Ctrl Pts',(60.4402684378921,244.853685153042,19.2319092697064)) ;
#108446 = CARTESIAN_POINT('Ctrl Pts',(60.4404467789386,244.83272707567,19.2293484289546)) ;
#108447 = CARTESIAN_POINT('Ctrl Pts',(60.4428319502743,244.81247036632,19.226917233338)) ;
#108448 = CARTESIAN_POINT('Ctrl Pts',(60.4520052987547,244.774053772956,19.2223843213245)) ;
#108449 = CARTESIAN_POINT('Ctrl Pts',(60.4586423249843,244.755670993561,19.220252974398)) ;
#108450 = CARTESIAN_POINT('Ctrl Pts',(60.4774783235665,244.719575674608,19.2161289230798)) ;
#108451 = CARTESIAN_POINT('Ctrl Pts',(60.4902886559452,244.70199405801,19.2141587038466)) ;
#108452 = CARTESIAN_POINT('Ctrl Pts',(60.5183067650571,244.676456197767,19.211329358316)) ;
#108453 = CARTESIAN_POINT('Ctrl Pts',(60.5322233323112,244.667323028126,19.2103300976413)) ;
#108454 = CARTESIAN_POINT('Ctrl Pts',(60.5612197979218,244.655769851502,19.2090706572321)) ;
#108455 = CARTESIAN_POINT('Ctrl Pts',(60.5755858845328,244.652881297574,19.2087580919617)) ;
#108456 = CARTESIAN_POINT('Ctrl Pts',(60.5902651077865,244.652881297574,19.2087580919617)) ;
#108457 = CARTESIAN_POINT('Origin',(60.5902651077865,246.354501080212,21.2956415537952)) ;
#108458 = CARTESIAN_POINT('Ctrl Pts',(60.4402651077865,244.53588386738,18.7925297017959)) ;
#108459 = CARTESIAN_POINT('Ctrl Pts',(60.4402651077865,244.534727516982,18.7934188295481)) ;
#108460 = CARTESIAN_POINT('Ctrl Pts',(60.440286369022,244.533571152388,18.7943078119286)) ;
#108461 = CARTESIAN_POINT('Ctrl Pts',(60.4403288850239,244.532415143768,18.7951963674209)) ;
#108462 = CARTESIAN_POINT('Ctrl Pts',(60.4408750760621,244.517564228315,18.8066113882632)) ;
#108463 = CARTESIAN_POINT('Ctrl Pts',(60.4449239452531,244.502912348048,18.8178477074838)) ;
#108464 = CARTESIAN_POINT('Ctrl Pts',(60.452266539598,244.489223681977,18.8283288848361)) ;
#108465 = CARTESIAN_POINT('Ctrl Pts',(60.4599211853138,244.474953264169,18.8392554995377)) ;
#108466 = CARTESIAN_POINT('Ctrl Pts',(60.471012211767,244.461996982103,18.8491571877367)) ;
#108467 = CARTESIAN_POINT('Ctrl Pts',(60.4849165768427,244.451090612558,18.8574845439796)) ;
#108468 = CARTESIAN_POINT('Ctrl Pts',(60.4988172216939,244.440187161099,18.8658096721714)) ;
#108469 = CARTESIAN_POINT('Ctrl Pts',(60.5152637963994,244.431541284929,18.8724022440603)) ;
#108470 = CARTESIAN_POINT('Ctrl Pts',(60.5333315664699,244.425644705388,18.8768970808899)) ;
#108471 = CARTESIAN_POINT('Ctrl Pts',(60.5513971100608,244.419748852478,18.8813913638236)) ;
#108472 = CARTESIAN_POINT('Ctrl Pts',(60.5707376338847,244.416714575474,18.8837024854465)) ;
#108473 = CARTESIAN_POINT('Ctrl Pts',(60.5902651077865,244.416714575474,18.8837024854465)) ;
#108474 = CARTESIAN_POINT('Origin',(60.5902651077865,250.461289540614,21.6943281289039)) ;
#108475 = CARTESIAN_POINT('',(60.5902651077865,252.440005081538,20.4421173342227)) ;
#108476 = CARTESIAN_POINT('',(60.5902651077865,252.765060688053,20.2059506121228)) ;
#108477 = CARTESIAN_POINT('',(60.5902651077865,250.549457328458,21.8156806780601)) ;
#108478 = CARTESIAN_POINT('Ctrl Pts',(60.5902651077865,252.765060688053,20.2059506121228)) ;
#108479 = CARTESIAN_POINT('Ctrl Pts',(60.5707376338847,252.765060688053,20.2059506121228)) ;
#108480 = CARTESIAN_POINT('Ctrl Pts',(60.5513971100607,252.762889094993,20.2028149616837)) ;
#108481 = CARTESIAN_POINT('Ctrl Pts',(60.5333315664699,252.758670615469,20.1967187258679)) ;
#108482 = CARTESIAN_POINT('Ctrl Pts',(60.5152637963996,252.75445161604,20.1906217387244)) ;
#108483 = CARTESIAN_POINT('Ctrl Pts',(60.498817221694,252.74826611592,20.1816801076024)) ;
#108484 = CARTESIAN_POINT('Ctrl Pts',(60.4849165768427,252.740468923451,20.1703930883885)) ;
#108485 = CARTESIAN_POINT('Ctrl Pts',(60.4710122117669,252.732669644223,20.1591030484338)) ;
#108486 = CARTESIAN_POINT('Ctrl Pts',(60.4599211853138,252.723407277664,20.1456822720077)) ;
#108487 = CARTESIAN_POINT('Ctrl Pts',(60.4522665395981,252.713211813451,20.1308806422753)) ;
#108488 = CARTESIAN_POINT('Ctrl Pts',(60.4449239452532,252.703431980308,20.1166824198097)) ;
#108489 = CARTESIAN_POINT('Ctrl Pts',(60.4408750760621,252.692969427699,20.1014683651929)) ;
#108490 = CARTESIAN_POINT('Ctrl Pts',(60.4403288850239,252.682372803215,20.086022849981)) ;
#108491 = CARTESIAN_POINT('Ctrl Pts',(60.440286369022,252.681547952431,20.0848205571807)) ;
#108492 = CARTESIAN_POINT('Ctrl Pts',(60.4402651077865,252.680722895011,20.0836177483837)) ;
#108493 = CARTESIAN_POINT('Ctrl Pts',(60.4402651077865,252.679897896016,20.0824148057166)) ;
#108494 = CARTESIAN_POINT('Ctrl Pts',(60.4402651077865,252.240326810636,20.4017818933262)) ;
#108495 = CARTESIAN_POINT('Ctrl Pts',(60.4402651077865,252.241100988172,20.4019327189915)) ;
#108496 = CARTESIAN_POINT('Ctrl Pts',(60.4402684378921,252.241875158935,20.402083608801)) ;
#108497 = CARTESIAN_POINT('Ctrl Pts',(60.4404467789386,252.262598818301,20.4061245065945)) ;
#108498 = CARTESIAN_POINT('Ctrl Pts',(60.4428319502743,252.282615374488,20.4100719695999)) ;
#108499 = CARTESIAN_POINT('Ctrl Pts',(60.4520052987548,252.320552472788,20.4176322943074)) ;
#108500 = CARTESIAN_POINT('Ctrl Pts',(60.4586423249844,252.338694157341,20.4212858541613)) ;
#108501 = CARTESIAN_POINT('Ctrl Pts',(60.4774783235665,252.374297247581,20.4285177152552)) ;
#108502 = CARTESIAN_POINT('Ctrl Pts',(60.4902886559452,252.39162718984,20.4320769437325)) ;
#108503 = CARTESIAN_POINT('Ctrl Pts',(60.5183067650572,252.416789454087,20.4372777090437)) ;
#108504 = CARTESIAN_POINT('Ctrl Pts',(60.5322233323113,252.42578440312,20.4391496602992)) ;
#108505 = CARTESIAN_POINT('Ctrl Pts',(60.5612197979218,252.437161315521,20.4415219892068)) ;
#108506 = CARTESIAN_POINT('Ctrl Pts',(60.5755858845328,252.440005081538,20.4421173342227)) ;
#108507 = CARTESIAN_POINT('Ctrl Pts',(60.5902651077866,252.440005081538,20.4421173342227)) ;
#108508 = CARTESIAN_POINT('Origin',(60.5902651077865,246.713272893131,20.6002959107317)) ;
#108509 = CARTESIAN_POINT('Ctrl Pts',(60.4402651077865,245.420726657553,18.8212586407095)) ;
#108510 = CARTESIAN_POINT('Ctrl Pts',(60.4402651077865,245.420877483218,18.8204844631737)) ;
#108511 = CARTESIAN_POINT('Ctrl Pts',(60.4402684378921,245.421028373028,18.8197102924111)) ;
#108512 = CARTESIAN_POINT('Ctrl Pts',(60.4404467789386,245.425069270821,18.7989866330451)) ;
#108513 = CARTESIAN_POINT('Ctrl Pts',(60.4428319502743,245.429016733827,18.7789700768575)) ;
#108514 = CARTESIAN_POINT('Ctrl Pts',(60.4520052987547,245.436577058534,18.7410329785581)) ;
#108515 = CARTESIAN_POINT('Ctrl Pts',(60.4586423249843,245.440230618388,18.7228912940055)) ;
#108516 = CARTESIAN_POINT('Ctrl Pts',(60.4774783235664,245.447462479482,18.6872882037655)) ;
#108517 = CARTESIAN_POINT('Ctrl Pts',(60.4902886559451,245.451021707959,18.6699582615064)) ;
#108518 = CARTESIAN_POINT('Ctrl Pts',(60.5183067650571,245.45622247327,18.6447959972586)) ;
#108519 = CARTESIAN_POINT('Ctrl Pts',(60.5322233323112,245.458094424526,18.6358010482264)) ;
#108520 = CARTESIAN_POINT('Ctrl Pts',(60.5612197979217,245.460466753434,18.6244241358249)) ;
#108521 = CARTESIAN_POINT('Ctrl Pts',(60.5755858845327,245.461062098449,18.6215803698081)) ;
#108522 = CARTESIAN_POINT('Ctrl Pts',(60.5902651077865,245.461062098449,18.6215803698081)) ;
#108523 = CARTESIAN_POINT('Ctrl Pts',(60.5902651077865,245.22489537635,18.2965247632932)) ;
#108524 = CARTESIAN_POINT('Ctrl Pts',(60.5707376338848,245.22489537635,18.2965247632932)) ;
#108525 = CARTESIAN_POINT('Ctrl Pts',(60.5513971100606,245.22175972591,18.2986963563521)) ;
#108526 = CARTESIAN_POINT('Ctrl Pts',(60.5333315664697,245.215663490095,18.3029148358767)) ;
#108527 = CARTESIAN_POINT('Ctrl Pts',(60.5152637963993,245.209566502951,18.3071338353058)) ;
#108528 = CARTESIAN_POINT('Ctrl Pts',(60.4988172216938,245.200624871829,18.3133193354258)) ;
#108529 = CARTESIAN_POINT('Ctrl Pts',(60.4849165768424,245.189337852615,18.3211165278944)) ;
#108530 = CARTESIAN_POINT('Ctrl Pts',(60.4710122117664,245.17804781266,18.3289158071227)) ;
#108531 = CARTESIAN_POINT('Ctrl Pts',(60.4599211853135,245.164627036234,18.3381781736818)) ;
#108532 = CARTESIAN_POINT('Ctrl Pts',(60.4522665395978,245.149825406502,18.3483736378946)) ;
#108533 = CARTESIAN_POINT('Ctrl Pts',(60.444923945253,245.135627184036,18.3581534710381)) ;
#108534 = CARTESIAN_POINT('Ctrl Pts',(60.440875076062,245.120413129419,18.3686160236467)) ;
#108535 = CARTESIAN_POINT('Ctrl Pts',(60.4403288850238,245.104967614207,18.3792126481315)) ;
#108536 = CARTESIAN_POINT('Ctrl Pts',(60.440286369022,245.103765321407,18.3800374989151)) ;
#108537 = CARTESIAN_POINT('Ctrl Pts',(60.4402651077865,245.10256251261,18.3808625563344)) ;
#108538 = CARTESIAN_POINT('Ctrl Pts',(60.4402651077865,245.101359569943,18.3816875553301)) ;
#108539 = CARTESIAN_POINT('Origin',(60.5902651077865,248.040265107786,23.0213203435596)) ;
#108540 = CARTESIAN_POINT('Ctrl Pts',(60.4402651077865,246.182069881617,18.4333348922484)) ;
#108541 = CARTESIAN_POINT('Ctrl Pts',(60.4402651077865,246.181354905733,18.4330018626367)) ;
#108542 = CARTESIAN_POINT('Ctrl Pts',(60.4402684378921,246.180639897624,18.4326688888999)) ;
#108543 = CARTESIAN_POINT('Ctrl Pts',(60.4404467789386,246.161498924883,18.4237569825383)) ;
#108544 = CARTESIAN_POINT('Ctrl Pts',(60.4428319502743,246.142984930219,18.4151851106656)) ;
#108545 = CARTESIAN_POINT('Ctrl Pts',(60.4520052987548,246.107849325612,18.3990026749417)) ;
#108546 = CARTESIAN_POINT('Ctrl Pts',(60.4586423249844,246.091024885902,18.3912950523219)) ;
#108547 = CARTESIAN_POINT('Ctrl Pts',(60.4774783235664,246.057970599548,18.3762187794687)) ;
#108548 = CARTESIAN_POINT('Ctrl Pts',(60.4902886559451,246.04185831974,18.3689119713107)) ;
#108549 = CARTESIAN_POINT('Ctrl Pts',(60.5183067650572,246.018444687196,18.3583294709921)) ;
#108550 = CARTESIAN_POINT('Ctrl Pts',(60.5322233323112,246.010067315225,18.3545568129842)) ;
#108551 = CARTESIAN_POINT('Ctrl Pts',(60.5612197979218,245.999468779803,18.3497888860605)) ;
#108552 = CARTESIAN_POINT('Ctrl Pts',(60.5755858845328,245.996818189747,18.3485990065702)) ;
#108553 = CARTESIAN_POINT('Ctrl Pts',(60.5902651077866,245.996818189747,18.3485990065702)) ;
#108554 = CARTESIAN_POINT('Origin',(60.5902651077865,246.970272317295,20.8591725524954)) ;
#108555 = CARTESIAN_POINT('Ctrl Pts',(60.4402651077865,246.014168667474,17.9165880896081)) ;
#108556 = CARTESIAN_POINT('Ctrl Pts',(60.4402651077865,246.012794157307,17.9170763684262)) ;
#108557 = CARTESIAN_POINT('Ctrl Pts',(60.440286369022,246.011419678562,17.9175645046008)) ;
#108558 = CARTESIAN_POINT('Ctrl Pts',(60.4403288850238,246.010045670283,17.9180523447825)) ;
#108559 = CARTESIAN_POINT('Ctrl Pts',(60.440875076062,245.992394174936,17.9243194894788)) ;
#108560 = CARTESIAN_POINT('Ctrl Pts',(60.444923945253,245.97498719514,17.9304781840928)) ;
#108561 = CARTESIAN_POINT('Ctrl Pts',(60.4522665395979,245.958729638151,17.9362163456658)) ;
#108562 = CARTESIAN_POINT('Ctrl Pts',(60.4599211853138,245.94178115467,17.9421983721592)) ;
#108563 = CARTESIAN_POINT('Ctrl Pts',(60.4710122117668,245.926399208258,17.9476117259011)) ;
#108564 = CARTESIAN_POINT('Ctrl Pts',(60.4849165768426,245.913453339835,17.9521612587828)) ;
#108565 = CARTESIAN_POINT('Ctrl Pts',(60.4988172216937,245.900510935184,17.9567095744005)) ;
#108566 = CARTESIAN_POINT('Ctrl Pts',(60.5152637963994,245.890251001563,17.9603077601871)) ;
#108567 = CARTESIAN_POINT('Ctrl Pts',(60.5333315664698,245.883254040199,17.9627604607569)) ;
#108568 = CARTESIAN_POINT('Ctrl Pts',(60.5513971100606,245.876257941067,17.965212859082)) ;
#108569 = CARTESIAN_POINT('Ctrl Pts',(60.5707376338847,245.872657996292,17.966473223201)) ;
#108570 = CARTESIAN_POINT('Ctrl Pts',(60.5902651077865,245.872657996292,17.966473223201)) ;
#108571 = CARTESIAN_POINT('Origin',(60.5902651077865,249.932733025005,21.0111380571975)) ;
#108572 = CARTESIAN_POINT('',(60.5902651077865,251.427648917999,19.2087580919617)) ;
#108573 = CARTESIAN_POINT('',(60.5902651077865,251.663815640099,18.8837024854464)) ;
#108574 = CARTESIAN_POINT('',(60.5902651077865,250.054085574161,21.0993058450414)) ;
#108575 = CARTESIAN_POINT('Ctrl Pts',(60.5902651077865,251.663815640098,18.8837024854471)) ;
#108576 = CARTESIAN_POINT('Ctrl Pts',(60.5707376338847,251.663815640098,18.8837024854471)) ;
#108577 = CARTESIAN_POINT('Ctrl Pts',(60.5513971100607,251.660781363094,18.8813913638241)) ;
#108578 = CARTESIAN_POINT('Ctrl Pts',(60.53333156647,251.654885510185,18.8768970808902)) ;
#108579 = CARTESIAN_POINT('Ctrl Pts',(60.5152637963997,251.648988930644,18.8724022440604)) ;
#108580 = CARTESIAN_POINT('Ctrl Pts',(60.498817221694,251.640343054474,18.8658096721712)) ;
#108581 = CARTESIAN_POINT('Ctrl Pts',(60.4849165768427,251.629439603015,18.8574845439796)) ;
#108582 = CARTESIAN_POINT('Ctrl Pts',(60.4710122117668,251.618533233469,18.8491571877369)) ;
#108583 = CARTESIAN_POINT('Ctrl Pts',(60.459921185314,251.605576951404,18.8392554995377)) ;
#108584 = CARTESIAN_POINT('Ctrl Pts',(60.4522665395982,251.591306533596,18.8283288848364)) ;
#108585 = CARTESIAN_POINT('Ctrl Pts',(60.4449239452533,251.577617867525,18.8178477074843)) ;
#108586 = CARTESIAN_POINT('Ctrl Pts',(60.4408750760622,251.562965987259,18.8066113882618)) ;
#108587 = CARTESIAN_POINT('Ctrl Pts',(60.4403288850239,251.548115071805,18.7951963674209)) ;
#108588 = CARTESIAN_POINT('Ctrl Pts',(60.4402863690221,251.546959063185,18.7943078119287)) ;
#108589 = CARTESIAN_POINT('Ctrl Pts',(60.4402651077865,251.54580269859,18.7934188295486)) ;
#108590 = CARTESIAN_POINT('Ctrl Pts',(60.4402651077865,251.544646348192,18.7925297017964)) ;
#108591 = CARTESIAN_POINT('Ctrl Pts',(60.4402651077865,251.225279260583,19.2321007871753)) ;
#108592 = CARTESIAN_POINT('Ctrl Pts',(60.4402651077865,251.226062154867,19.2320049968919)) ;
#108593 = CARTESIAN_POINT('Ctrl Pts',(60.4402684378921,251.226845062531,19.2319092697064)) ;
#108594 = CARTESIAN_POINT('Ctrl Pts',(60.4404467789386,251.247803139903,19.2293484289546)) ;
#108595 = CARTESIAN_POINT('Ctrl Pts',(60.4428319502743,251.268059849252,19.226917233338)) ;
#108596 = CARTESIAN_POINT('Ctrl Pts',(60.4520052987547,251.306476442617,19.2223843213245)) ;
#108597 = CARTESIAN_POINT('Ctrl Pts',(60.4586423249844,251.324859222012,19.220252974398)) ;
#108598 = CARTESIAN_POINT('Ctrl Pts',(60.4774783235664,251.360954540964,19.2161289230799)) ;
#108599 = CARTESIAN_POINT('Ctrl Pts',(60.4902886559451,251.378536157563,19.2141587038466)) ;
#108600 = CARTESIAN_POINT('Ctrl Pts',(60.5183067650571,251.404074017805,19.211329358316)) ;
#108601 = CARTESIAN_POINT('Ctrl Pts',(60.5322233323112,251.413207187447,19.2103300976413)) ;
#108602 = CARTESIAN_POINT('Ctrl Pts',(60.5612197979217,251.42476036407,19.2090706572321)) ;
#108603 = CARTESIAN_POINT('Ctrl Pts',(60.5755858845327,251.427648917999,19.2087580919617)) ;
#108604 = CARTESIAN_POINT('Ctrl Pts',(60.5902651077865,251.427648917999,19.2087580919617)) ;
#108605 = CARTESIAN_POINT('Origin',(60.5902651077865,247.526358208506,20.3087261348769)) ;
#108606 = CARTESIAN_POINT('Ctrl Pts',(60.4402651077865,246.84682643861,18.2173423936815)) ;
#108607 = CARTESIAN_POINT('Ctrl Pts',(60.4402651077865,246.847209116357,18.2166527147851)) ;
#108608 = CARTESIAN_POINT('Ctrl Pts',(60.4402684378921,246.847591853016,18.2159630621521)) ;
#108609 = CARTESIAN_POINT('Ctrl Pts',(60.4404467789386,246.857838938124,18.197502396961)) ;
#108610 = CARTESIAN_POINT('Ctrl Pts',(60.4428319502743,246.867778654569,18.1796853539185)) ;
#108611 = CARTESIAN_POINT('Ctrl Pts',(60.4520052987548,246.886692158739,18.1459412981889)) ;
#108612 = CARTESIAN_POINT('Ctrl Pts',(60.4586423249845,246.895772989479,18.1298165429636)) ;
#108613 = CARTESIAN_POINT('Ctrl Pts',(60.4774783235664,246.913652858034,18.0981907599697)) ;
#108614 = CARTESIAN_POINT('Ctrl Pts',(60.4902886559451,246.92239313214,18.0828088675435)) ;
#108615 = CARTESIAN_POINT('Ctrl Pts',(60.5183067650572,246.935114921148,18.0604852570307)) ;
#108616 = CARTESIAN_POINT('Ctrl Pts',(60.5322233323113,246.939674844702,18.0525090168905)) ;
#108617 = CARTESIAN_POINT('Ctrl Pts',(60.5612197979218,246.945446722844,18.0424220201645)) ;
#108618 = CARTESIAN_POINT('Ctrl Pts',(60.5755858845328,246.946891701628,18.0399014096908)) ;
#108619 = CARTESIAN_POINT('Ctrl Pts',(60.5902651077866,246.946891701628,18.0399014096908)) ;
#108620 = CARTESIAN_POINT('Ctrl Pts',(60.5902651077865,246.822731508173,17.6577756263214)) ;
#108621 = CARTESIAN_POINT('Ctrl Pts',(60.5707376338846,246.822731508173,17.6577756263213)) ;
#108622 = CARTESIAN_POINT('Ctrl Pts',(60.5513971100607,246.81907826823,17.6588719647777)) ;
#108623 = CARTESIAN_POINT('Ctrl Pts',(60.5333315664699,246.811976821569,17.6610001367495)) ;
#108624 = CARTESIAN_POINT('Ctrl Pts',(60.5152637963995,246.804874499694,17.6631285710069)) ;
#108625 = CARTESIAN_POINT('Ctrl Pts',(60.4988172216938,246.794459078493,17.6662482152286)) ;
#108626 = CARTESIAN_POINT('Ctrl Pts',(60.4849165768425,246.781315020339,17.6701759051817)) ;
#108627 = CARTESIAN_POINT('Ctrl Pts',(60.4710122117665,246.768167444445,17.6741046463009)) ;
#108628 = CARTESIAN_POINT('Ctrl Pts',(60.4599211853139,246.752541298897,17.6787664323798)) ;
#108629 = CARTESIAN_POINT('Ctrl Pts',(60.452266539598,246.735313540781,17.6838889399248)) ;
#108630 = CARTESIAN_POINT('Ctrl Pts',(60.4449239452532,246.718788094142,17.6888026219327)) ;
#108631 = CARTESIAN_POINT('Ctrl Pts',(60.4408750760621,246.701085561798,17.6940516993334)) ;
#108632 = CARTESIAN_POINT('Ctrl Pts',(60.4403288850239,246.683121466859,17.6993567614171)) ;
#108633 = CARTESIAN_POINT('Ctrl Pts',(60.440286369022,246.681723125547,17.6997697122226)) ;
#108634 = CARTESIAN_POINT('Ctrl Pts',(60.4402651077865,246.680324229639,17.7001827000972)) ;
#108635 = CARTESIAN_POINT('Ctrl Pts',(60.4402651077865,246.678925224467,17.7005955910407)) ;
#108636 = CARTESIAN_POINT('Origin',(60.5902651077865,248.040265107786,23.0213203435596)) ;
#108637 = CARTESIAN_POINT('Ctrl Pts',(60.4402651077865,247.69078190379,18.0836729796702)) ;
#108638 = CARTESIAN_POINT('Ctrl Pts',(60.4402651077865,247.690204833125,18.0831353099888)) ;
#108639 = CARTESIAN_POINT('Ctrl Pts',(60.4402684378921,247.689627714548,18.0825976834901)) ;
#108640 = CARTESIAN_POINT('Ctrl Pts',(60.4404467789386,247.674177498212,18.0682070710063)) ;
#108641 = CARTESIAN_POINT('Ctrl Pts',(60.4428319502743,247.659218497027,18.0543335974202)) ;
#108642 = CARTESIAN_POINT('Ctrl Pts',(60.4520052987548,247.630803198961,18.0280856875442)) ;
#108643 = CARTESIAN_POINT('Ctrl Pts',(60.4586423249844,247.617183992317,18.0155562650352)) ;
#108644 = CARTESIAN_POINT('Ctrl Pts',(60.4774783235665,247.590406322412,17.9910035412763)) ;
#108645 = CARTESIAN_POINT('Ctrl Pts',(60.4902886559452,247.577340561604,17.9790753854857)) ;
#108646 = CARTESIAN_POINT('Ctrl Pts',(60.5183067650572,247.558343046244,17.9617756192428)) ;
#108647 = CARTESIAN_POINT('Ctrl Pts',(60.5322233323113,247.55154150748,17.9555988579533)) ;
#108648 = CARTESIAN_POINT('Ctrl Pts',(60.5612197979218,247.542935071751,17.9477891624225)) ;
#108649 = CARTESIAN_POINT('Ctrl Pts',(60.5755858845328,247.54078190379,17.9458384424072)) ;
#108650 = CARTESIAN_POINT('Ctrl Pts',(60.5902651077866,247.54078190379,17.9458384424072)) ;
#108651 = CARTESIAN_POINT('Origin',(60.5902651077865,247.69078190379,20.6343496415544)) ;
#108652 = CARTESIAN_POINT('Ctrl Pts',(60.4402651077865,247.69078190379,17.5403332371979)) ;
#108653 = CARTESIAN_POINT('Ctrl Pts',(60.4402651077865,247.689323780486,17.5403728709491)) ;
#108654 = CARTESIAN_POINT('Ctrl Pts',(60.440286369022,247.687865731145,17.5404123787479)) ;
#108655 = CARTESIAN_POINT('Ctrl Pts',(60.4403288850239,247.686408220711,17.540451750423)) ;
#108656 = CARTESIAN_POINT('Ctrl Pts',(60.4408750760621,247.667683996822,17.5409575471857)) ;
#108657 = CARTESIAN_POINT('Ctrl Pts',(60.4449239452531,247.649225833959,17.5414357612546)) ;
#108658 = CARTESIAN_POINT('Ctrl Pts',(60.452266539598,247.631990789003,17.5418692158132)) ;
#108659 = CARTESIAN_POINT('Ctrl Pts',(60.4599211853139,247.6140232755,17.5423210916658)) ;
#108660 = CARTESIAN_POINT('Ctrl Pts',(60.4710122117669,247.597721356829,17.5427162141691)) ;
#108661 = CARTESIAN_POINT('Ctrl Pts',(60.4849165768426,247.58400322133,17.5430425837128)) ;
#108662 = CARTESIAN_POINT('Ctrl Pts',(60.4988172216937,247.570288756228,17.5433688659337)) ;
#108663 = CARTESIAN_POINT('Ctrl Pts',(60.5152637963994,247.559419078944,17.5436204501225)) ;
#108664 = CARTESIAN_POINT('Ctrl Pts',(60.5333315664699,247.552006647086,17.5437909270115)) ;
#108665 = CARTESIAN_POINT('Ctrl Pts',(60.5513971100608,247.544595128658,17.5439613828928)) ;
#108666 = CARTESIAN_POINT('Ctrl Pts',(60.5707376338847,247.54078190379,17.5440476162862)) ;
#108667 = CARTESIAN_POINT('Ctrl Pts',(60.5902651077865,247.54078190379,17.5440476162862)) ;
#108668 = CARTESIAN_POINT('Origin',(60.5902651077865,249.21892856406,20.5247186334439)) ;
#108669 = CARTESIAN_POINT('Ctrl Pts',(60.5902651077865,250.207872219281,17.9664732232009)) ;
#108670 = CARTESIAN_POINT('Ctrl Pts',(60.5707376338848,250.207872219281,17.9664732232009)) ;
#108671 = CARTESIAN_POINT('Ctrl Pts',(60.5513971100606,250.204272274506,17.9652128590817)) ;
#108672 = CARTESIAN_POINT('Ctrl Pts',(60.5333315664697,250.197276175374,17.9627604607566)) ;
#108673 = CARTESIAN_POINT('Ctrl Pts',(60.5152637963994,250.19027921401,17.9603077601868)) ;
#108674 = CARTESIAN_POINT('Ctrl Pts',(60.4988172216938,250.180019280389,17.9567095744006)) ;
#108675 = CARTESIAN_POINT('Ctrl Pts',(60.4849165768424,250.167076875737,17.952161258783)) ;
#108676 = CARTESIAN_POINT('Ctrl Pts',(60.4710122117664,250.154131007314,17.9476117259013)) ;
#108677 = CARTESIAN_POINT('Ctrl Pts',(60.4599211853138,250.138749060903,17.9421983721593)) ;
#108678 = CARTESIAN_POINT('Ctrl Pts',(60.452266539598,250.121800577423,17.9362163456661)) ;
#108679 = CARTESIAN_POINT('Ctrl Pts',(60.4449239452531,250.105543020433,17.9304781840933)) ;
#108680 = CARTESIAN_POINT('Ctrl Pts',(60.440875076062,250.088136040637,17.9243194894782)) ;
#108681 = CARTESIAN_POINT('Ctrl Pts',(60.4403288850239,250.07048454529,17.9180523447823)) ;
#108682 = CARTESIAN_POINT('Ctrl Pts',(60.440286369022,250.069110537011,17.9175645046006)) ;
#108683 = CARTESIAN_POINT('Ctrl Pts',(60.4402651077865,250.067736058266,17.9170763684254)) ;
#108684 = CARTESIAN_POINT('Ctrl Pts',(60.4402651077865,250.066361548099,17.9165880896073)) ;
#108685 = CARTESIAN_POINT('Ctrl Pts',(60.4402651077865,249.898460333955,18.4333348922483)) ;
#108686 = CARTESIAN_POINT('Ctrl Pts',(60.4402651077865,249.899175309841,18.433001862636)) ;
#108687 = CARTESIAN_POINT('Ctrl Pts',(60.4402684378921,249.899890317951,18.4326688888986)) ;
#108688 = CARTESIAN_POINT('Ctrl Pts',(60.4404467789389,249.919031290693,18.423756982537)) ;
#108689 = CARTESIAN_POINT('Ctrl Pts',(60.4428319502748,249.937545285356,18.4151851106646)) ;
#108690 = CARTESIAN_POINT('Ctrl Pts',(60.4520052987553,249.972680889962,18.3990026749411)) ;
#108691 = CARTESIAN_POINT('Ctrl Pts',(60.4586423249848,249.989505329671,18.3912950523216)) ;
#108692 = CARTESIAN_POINT('Ctrl Pts',(60.4774783235664,250.022559616024,18.3762187794687)) ;
#108693 = CARTESIAN_POINT('Ctrl Pts',(60.4902886559451,250.038671895832,18.3689119713107)) ;
#108694 = CARTESIAN_POINT('Ctrl Pts',(60.5183067650571,250.062085528376,18.3583294709921)) ;
#108695 = CARTESIAN_POINT('Ctrl Pts',(60.5322233323112,250.070462900348,18.3545568129842)) ;
#108696 = CARTESIAN_POINT('Ctrl Pts',(60.5612197979218,250.08106143577,18.3497888860605)) ;
#108697 = CARTESIAN_POINT('Ctrl Pts',(60.5755858845328,250.083712025826,18.3485990065702)) ;
#108698 = CARTESIAN_POINT('Ctrl Pts',(60.5902651077866,250.083712025826,18.3485990065702)) ;
#108699 = CARTESIAN_POINT('Origin',(60.5902651077865,248.389748311783,20.2826839799233)) ;
#108700 = CARTESIAN_POINT('Ctrl Pts',(60.4402651077865,248.389748311783,18.0836729796702)) ;
#108701 = CARTESIAN_POINT('Ctrl Pts',(60.4402651077865,248.390325382447,18.0831353099888)) ;
#108702 = CARTESIAN_POINT('Ctrl Pts',(60.4402684378921,248.390902501024,18.0825976834901)) ;
#108703 = CARTESIAN_POINT('Ctrl Pts',(60.4404467789386,248.406352717361,18.0682070710062)) ;
#108704 = CARTESIAN_POINT('Ctrl Pts',(60.4428319502743,248.421311718545,18.0543335974202)) ;
#108705 = CARTESIAN_POINT('Ctrl Pts',(60.4520052987547,248.449727016612,18.0280856875444)) ;
#108706 = CARTESIAN_POINT('Ctrl Pts',(60.4586423249843,248.463346223255,18.0155562650353)) ;
#108707 = CARTESIAN_POINT('Ctrl Pts',(60.4774783235664,248.490123893161,17.9910035412764)) ;
#108708 = CARTESIAN_POINT('Ctrl Pts',(60.4902886559451,248.503189653969,17.9790753854858)) ;
#108709 = CARTESIAN_POINT('Ctrl Pts',(60.5183067650571,248.522187169328,17.9617756192429)) ;
#108710 = CARTESIAN_POINT('Ctrl Pts',(60.5322233323112,248.528988708093,17.9555988579533)) ;
#108711 = CARTESIAN_POINT('Ctrl Pts',(60.5612197979217,248.537595143822,17.9477891624225)) ;
#108712 = CARTESIAN_POINT('Ctrl Pts',(60.5755858845327,248.539748311783,17.9458384424072)) ;
#108713 = CARTESIAN_POINT('Ctrl Pts',(60.5902651077865,248.539748311783,17.9458384424072)) ;
#108714 = CARTESIAN_POINT('Ctrl Pts',(60.5902651077865,248.539748311783,17.5440476162869)) ;
#108715 = CARTESIAN_POINT('Ctrl Pts',(60.5707376338848,248.539748311783,17.5440476162869)) ;
#108716 = CARTESIAN_POINT('Ctrl Pts',(60.5513971100606,248.535935086915,17.5439613828925)) ;
#108717 = CARTESIAN_POINT('Ctrl Pts',(60.5333315664697,248.528523568487,17.5437909270112)) ;
#108718 = CARTESIAN_POINT('Ctrl Pts',(60.5152637963993,248.521111136629,17.5436204501222)) ;
#108719 = CARTESIAN_POINT('Ctrl Pts',(60.4988172216937,248.510241459345,17.5433688659334)) ;
#108720 = CARTESIAN_POINT('Ctrl Pts',(60.4849165768423,248.496526994243,17.5430425837125)) ;
#108721 = CARTESIAN_POINT('Ctrl Pts',(60.4710122117664,248.482808858743,17.5427162141689)) ;
#108722 = CARTESIAN_POINT('Ctrl Pts',(60.4599211853135,248.466506940072,17.5423210916655)) ;
#108723 = CARTESIAN_POINT('Ctrl Pts',(60.4522665395979,248.44853942657,17.5418692158129)) ;
#108724 = CARTESIAN_POINT('Ctrl Pts',(60.4449239452532,248.431304381614,17.5414357612543)) ;
#108725 = CARTESIAN_POINT('Ctrl Pts',(60.440875076062,248.41284621875,17.5409575471862)) ;
#108726 = CARTESIAN_POINT('Ctrl Pts',(60.4403288850238,248.394121994861,17.5404517504227)) ;
#108727 = CARTESIAN_POINT('Ctrl Pts',(60.440286369022,248.392664484427,17.5404123787476)) ;
#108728 = CARTESIAN_POINT('Ctrl Pts',(60.4402651077865,248.391206435086,17.5403728709489)) ;
#108729 = CARTESIAN_POINT('Ctrl Pts',(60.4402651077865,248.389748311783,17.5403332371977)) ;
#108730 = CARTESIAN_POINT('Origin',(60.5902651077865,248.040265107786,23.0213203435596)) ;
#108731 = CARTESIAN_POINT('Ctrl Pts',(60.4402651077865,249.233703776962,18.2173423936815)) ;
#108732 = CARTESIAN_POINT('Ctrl Pts',(60.4402651077865,249.233321099216,18.2166527147863)) ;
#108733 = CARTESIAN_POINT('Ctrl Pts',(60.440268437892,249.232938362558,18.2159630621546)) ;
#108734 = CARTESIAN_POINT('Ctrl Pts',(60.4404467789383,249.22269127745,18.1975023969641)) ;
#108735 = CARTESIAN_POINT('Ctrl Pts',(60.4428319502738,249.212751561005,18.1796853539209)) ;
#108736 = CARTESIAN_POINT('Ctrl Pts',(60.4520052987543,249.193838056834,18.1459412981901)) ;
#108737 = CARTESIAN_POINT('Ctrl Pts',(60.4586423249841,249.184757226094,18.1298165429642)) ;
#108738 = CARTESIAN_POINT('Ctrl Pts',(60.4774783235664,249.166877357539,18.0981907599697)) ;
#108739 = CARTESIAN_POINT('Ctrl Pts',(60.4902886559451,249.158137083433,18.0828088675435)) ;
#108740 = CARTESIAN_POINT('Ctrl Pts',(60.5183067650571,249.145415294424,18.0604852570307)) ;
#108741 = CARTESIAN_POINT('Ctrl Pts',(60.5322233323112,249.14085537087,18.0525090168905)) ;
#108742 = CARTESIAN_POINT('Ctrl Pts',(60.5612197979217,249.135083492728,18.0424220201645)) ;
#108743 = CARTESIAN_POINT('Ctrl Pts',(60.5755858845327,249.133638513944,18.0399014096908)) ;
#108744 = CARTESIAN_POINT('Ctrl Pts',(60.5902651077865,249.133638513944,18.0399014096908)) ;
#108745 = CARTESIAN_POINT('Origin',(60.5902651077865,248.445501341285,20.6431800539285)) ;
#108746 = CARTESIAN_POINT('Ctrl Pts',(60.4402651077865,249.401604991106,17.700595591041)) ;
#108747 = CARTESIAN_POINT('Ctrl Pts',(60.4402651077865,249.400205985933,17.7001827000975)) ;
#108748 = CARTESIAN_POINT('Ctrl Pts',(60.440286369022,249.398807090025,17.699769712223)) ;
#108749 = CARTESIAN_POINT('Ctrl Pts',(60.4403288850239,249.397408748713,17.6993567614174)) ;
#108750 = CARTESIAN_POINT('Ctrl Pts',(60.4408750760622,249.379444653775,17.6940516993328)) ;
#108751 = CARTESIAN_POINT('Ctrl Pts',(60.4449239452535,249.361742121431,17.6888026219299)) ;
#108752 = CARTESIAN_POINT('Ctrl Pts',(60.4522665395983,249.345216674792,17.6838889399227)) ;
#108753 = CARTESIAN_POINT('Ctrl Pts',(60.4599211853141,249.327988916676,17.6787664323785)) ;
#108754 = CARTESIAN_POINT('Ctrl Pts',(60.4710122117672,249.312362771127,17.6741046463007)) ;
#108755 = CARTESIAN_POINT('Ctrl Pts',(60.4849165768428,249.299215195234,17.6701759051814)) ;
#108756 = CARTESIAN_POINT('Ctrl Pts',(60.4988172216939,249.28607113708,17.6662482152284)) ;
#108757 = CARTESIAN_POINT('Ctrl Pts',(60.5152637963996,249.275655715879,17.6631285710071)) ;
#108758 = CARTESIAN_POINT('Ctrl Pts',(60.5333315664699,249.268553394004,17.6610001367497)) ;
#108759 = CARTESIAN_POINT('Ctrl Pts',(60.5513971100607,249.261451947343,17.6588719647779)) ;
#108760 = CARTESIAN_POINT('Ctrl Pts',(60.5707376338848,249.2577987074,17.6577756263218)) ;
#108761 = CARTESIAN_POINT('Ctrl Pts',(60.5902651077865,249.2577987074,17.6577756263218)) ;
#108762 = CARTESIAN_POINT('Origin',(60.5902651077865,249.739858576849,17.7905095039363)) ;
#108763 = CARTESIAN_POINT('Origin',(60.5902651077865,248.040265107786,17.5213203435596)) ;
#108764 = CARTESIAN_POINT('Origin',(60.5902651077865,248.040265107786,23.0213203435596)) ;
#108765 = CARTESIAN_POINT('',(60.5902651077865,250.619468117123,18.6215803698081)) ;
#108766 = CARTESIAN_POINT('Origin',(60.5902651077865,248.040265107786,23.0213203435596)) ;
#108767 = CARTESIAN_POINT('Ctrl Pts',(60.4402651077865,250.65980355802,18.8212586407095)) ;
#108768 = CARTESIAN_POINT('Ctrl Pts',(60.4402651077865,250.659652732354,18.8204844631737)) ;
#108769 = CARTESIAN_POINT('Ctrl Pts',(60.4402684378921,250.659501842545,18.8197102924112)) ;
#108770 = CARTESIAN_POINT('Ctrl Pts',(60.4404467789386,250.655460944751,18.7989866330445)) ;
#108771 = CARTESIAN_POINT('Ctrl Pts',(60.4428319502743,250.651513481746,18.7789700768574)) ;
#108772 = CARTESIAN_POINT('Ctrl Pts',(60.4520052987548,250.643953157039,18.7410329785579)) ;
#108773 = CARTESIAN_POINT('Ctrl Pts',(60.4586423249844,250.640299597185,18.7228912940054)) ;
#108774 = CARTESIAN_POINT('Ctrl Pts',(60.4774783235664,250.633067736091,18.6872882037655)) ;
#108775 = CARTESIAN_POINT('Ctrl Pts',(60.4902886559451,250.629508507613,18.6699582615064)) ;
#108776 = CARTESIAN_POINT('Ctrl Pts',(60.5183067650571,250.624307742302,18.6447959972585)) ;
#108777 = CARTESIAN_POINT('Ctrl Pts',(60.5322233323112,250.622435791047,18.6358010482263)) ;
#108778 = CARTESIAN_POINT('Ctrl Pts',(60.5612197979218,250.620063462139,18.6244241358249)) ;
#108779 = CARTESIAN_POINT('Ctrl Pts',(60.5755858845328,250.619468117123,18.6215803698081)) ;
#108780 = CARTESIAN_POINT('Ctrl Pts',(60.5902651077865,250.619468117123,18.6215803698081)) ;
#108781 = CARTESIAN_POINT('Origin',(60.5902651077865,249.160553432798,20.8847994073294)) ;
#108782 = CARTESIAN_POINT('',(60.5902651077865,250.855634839223,18.2965247632928)) ;
#108783 = CARTESIAN_POINT('',(60.5902651077865,249.039200883641,20.7966316194855)) ;
#108784 = CARTESIAN_POINT('Ctrl Pts',(60.4402651077865,250.979170645629,18.3816875553299)) ;
#108785 = CARTESIAN_POINT('Ctrl Pts',(60.4402651077865,250.977967702962,18.3808625563341)) ;
#108786 = CARTESIAN_POINT('Ctrl Pts',(60.440286369022,250.976764894165,18.3800374989159)) ;
#108787 = CARTESIAN_POINT('Ctrl Pts',(60.4403288850239,250.975562601365,18.3792126481319)) ;
#108788 = CARTESIAN_POINT('Ctrl Pts',(60.4408750760622,250.960117086155,18.368616023642)) ;
#108789 = CARTESIAN_POINT('Ctrl Pts',(60.4449239452534,250.944903031537,18.3581534710365)) ;
#108790 = CARTESIAN_POINT('Ctrl Pts',(60.4522665395982,250.930704809071,18.3483736378934)) ;
#108791 = CARTESIAN_POINT('Ctrl Pts',(60.459921185314,250.915903179339,18.3381781736808)) ;
#108792 = CARTESIAN_POINT('Ctrl Pts',(60.4710122117671,250.902482402912,18.3289158071227)) ;
#108793 = CARTESIAN_POINT('Ctrl Pts',(60.4849165768428,250.891192362958,18.3211165278944)) ;
#108794 = CARTESIAN_POINT('Ctrl Pts',(60.498817221694,250.879905343744,18.3133193354258)) ;
#108795 = CARTESIAN_POINT('Ctrl Pts',(60.5152637963998,250.870963712621,18.3071338353064)) ;
#108796 = CARTESIAN_POINT('Ctrl Pts',(60.5333315664701,250.864866725478,18.3029148358775)) ;
#108797 = CARTESIAN_POINT('Ctrl Pts',(60.5513971100608,250.858770489662,18.2986963563531)) ;
#108798 = CARTESIAN_POINT('Ctrl Pts',(60.5707376338847,250.855634839223,18.2965247632931)) ;
#108799 = CARTESIAN_POINT('Ctrl Pts',(60.5902651077865,250.855634839223,18.2965247632931)) ;
#108800 = CARTESIAN_POINT('Origin',(60.5902651077865,251.273083995395,18.5717268744974)) ;
#108801 = CARTESIAN_POINT('Origin',(60.5902651077865,251.273083995395,18.5717268744974)) ;
#108802 = CARTESIAN_POINT('Origin',(60.5902651077865,246.340671638724,17.7905095039363)) ;
#108803 = CARTESIAN_POINT('Origin',(60.5902651077865,248.040265107786,23.0213203435596)) ;
#108804 = CARTESIAN_POINT('',(60.5902651077865,251.852827359384,19.6339365333471)) ;
#108805 = CARTESIAN_POINT('Origin',(60.5902651077865,248.040265107786,23.0213203435596)) ;
#108806 = CARTESIAN_POINT('Ctrl Pts',(60.4402651077865,251.829484664171,19.836306190763)) ;
#108807 = CARTESIAN_POINT('Ctrl Pts',(60.4402651077865,251.829580454454,19.8355232964805)) ;
#108808 = CARTESIAN_POINT('Ctrl Pts',(60.440268437892,251.829676181639,19.8347403888179)) ;
#108809 = CARTESIAN_POINT('Ctrl Pts',(60.4404467789383,251.832237022391,19.8137823114479)) ;
#108810 = CARTESIAN_POINT('Ctrl Pts',(60.4428319502738,251.834668218008,19.7935256020966)) ;
#108811 = CARTESIAN_POINT('Ctrl Pts',(60.4520052987543,251.839201130021,19.7551090087302)) ;
#108812 = CARTESIAN_POINT('Ctrl Pts',(60.4586423249841,251.841332476948,19.7367262293345)) ;
#108813 = CARTESIAN_POINT('Ctrl Pts',(60.4774783235663,251.845456528266,19.7006309103821)) ;
#108814 = CARTESIAN_POINT('Ctrl Pts',(60.490288655945,251.847426747499,19.6830492937831)) ;
#108815 = CARTESIAN_POINT('Ctrl Pts',(60.5183067650572,251.85025609303,19.6575114335403)) ;
#108816 = CARTESIAN_POINT('Ctrl Pts',(60.5322233323113,251.851255353705,19.648378263899)) ;
#108817 = CARTESIAN_POINT('Ctrl Pts',(60.5612197979218,251.852514794114,19.6368250872756)) ;
#108818 = CARTESIAN_POINT('Ctrl Pts',(60.5755858845328,251.852827359384,19.6339365333471)) ;
#108819 = CARTESIAN_POINT('Ctrl Pts',(60.5902651077865,251.852827359384,19.633936533347)) ;
#108820 = CARTESIAN_POINT('Origin',(60.5902651077865,249.765943897551,21.3355563159851)) ;
#108821 = CARTESIAN_POINT('',(60.5902651077865,252.1778829659,19.3977698112471)) ;
#108822 = CARTESIAN_POINT('',(60.5902651077865,249.677776109707,21.2142037668289)) ;
#108823 = CARTESIAN_POINT('Ctrl Pts',(60.4402651077865,252.26905574955,19.5169391031532)) ;
#108824 = CARTESIAN_POINT('Ctrl Pts',(60.4402651077865,252.268166621798,19.5157827527552)) ;
#108825 = CARTESIAN_POINT('Ctrl Pts',(60.440286369022,252.267277639418,19.5146263881606)) ;
#108826 = CARTESIAN_POINT('Ctrl Pts',(60.4403288850239,252.266389083925,19.5134703795409)) ;
#108827 = CARTESIAN_POINT('Ctrl Pts',(60.4408750760621,252.254974063079,19.4986194640923)) ;
#108828 = CARTESIAN_POINT('Ctrl Pts',(60.4449239452531,252.243737743862,19.4839675838214)) ;
#108829 = CARTESIAN_POINT('Ctrl Pts',(60.4522665395981,252.23325656651,19.4702789177502)) ;
#108830 = CARTESIAN_POINT('Ctrl Pts',(60.4599211853138,252.222329951808,19.4560084999423)) ;
#108831 = CARTESIAN_POINT('Ctrl Pts',(60.4710122117667,252.21242826361,19.4430522178763)) ;
#108832 = CARTESIAN_POINT('Ctrl Pts',(60.4849165768426,252.204100907367,19.4321458483306)) ;
#108833 = CARTESIAN_POINT('Ctrl Pts',(60.498817221694,252.195775779175,19.4212423968717)) ;
#108834 = CARTESIAN_POINT('Ctrl Pts',(60.5152637963995,252.189183207286,19.4125965207019)) ;
#108835 = CARTESIAN_POINT('Ctrl Pts',(60.5333315664699,252.184688370457,19.4066999411606)) ;
#108836 = CARTESIAN_POINT('Ctrl Pts',(60.5513971100608,252.180194087523,19.4008040882511)) ;
#108837 = CARTESIAN_POINT('Ctrl Pts',(60.5707376338848,252.177882965899,19.3977698112477)) ;
#108838 = CARTESIAN_POINT('Ctrl Pts',(60.5902651077865,252.177882965899,19.3977698112476)) ;
#108839 = CARTESIAN_POINT('Origin',(60.5902651077865,252.489858576849,19.788501455951)) ;
#108840 = CARTESIAN_POINT('Origin',(60.5902651077865,252.489858576849,19.788501455951)) ;
#108841 = CARTESIAN_POINT('Origin',(60.5902651077865,244.807446220178,18.5717268744974)) ;
#108842 = CARTESIAN_POINT('Origin',(60.5902651077865,248.040265107786,23.0213203435596)) ;
#108843 = CARTESIAN_POINT('',(60.5902651077865,252.712986444776,20.9778734255204)) ;
#108844 = CARTESIAN_POINT('Origin',(60.5902651077865,248.040265107786,23.0213203435596)) ;
#108845 = CARTESIAN_POINT('Ctrl Pts',(60.4402651077865,252.628250559098,21.1631251173908)) ;
#108846 = CARTESIAN_POINT('Ctrl Pts',(60.4402651077865,252.628583588709,21.162410141506)) ;
#108847 = CARTESIAN_POINT('Ctrl Pts',(60.4402684378921,252.628916562446,21.1616951333976)) ;
#108848 = CARTESIAN_POINT('Ctrl Pts',(60.4404467789386,252.637828468808,21.1425541606572)) ;
#108849 = CARTESIAN_POINT('Ctrl Pts',(60.4428319502743,252.64640034068,21.1240401659929)) ;
#108850 = CARTESIAN_POINT('Ctrl Pts',(60.4520052987547,252.662582776404,21.0889045613858)) ;
#108851 = CARTESIAN_POINT('Ctrl Pts',(60.4586423249843,252.670290399024,21.0720801216756)) ;
#108852 = CARTESIAN_POINT('Ctrl Pts',(60.4774783235664,252.685366671877,21.0390258353215)) ;
#108853 = CARTESIAN_POINT('Ctrl Pts',(60.4902886559451,252.692673480035,21.0229135555138)) ;
#108854 = CARTESIAN_POINT('Ctrl Pts',(60.5183067650571,252.703255980354,20.9994999229698)) ;
#108855 = CARTESIAN_POINT('Ctrl Pts',(60.5322233323112,252.707028638362,20.9911225509982)) ;
#108856 = CARTESIAN_POINT('Ctrl Pts',(60.5612197979218,252.711796565285,20.9805240155764)) ;
#108857 = CARTESIAN_POINT('Ctrl Pts',(60.5755858845328,252.712986444776,20.9778734255204)) ;
#108858 = CARTESIAN_POINT('Ctrl Pts',(60.5902651077866,252.712986444776,20.9778734255204)) ;
#108859 = CARTESIAN_POINT('Origin',(60.5902651077865,250.202412898851,21.9513275530686)) ;
#108860 = CARTESIAN_POINT('',(60.5902651077865,253.095112228145,20.8537132320653)) ;
#108861 = CARTESIAN_POINT('',(60.5902651077865,250.156060349694,21.8086690756243)) ;
#108862 = CARTESIAN_POINT('Ctrl Pts',(60.4402651077865,253.144997361738,20.9952239032473)) ;
#108863 = CARTESIAN_POINT('Ctrl Pts',(60.4402651077865,253.14450908292,20.9938493930806)) ;
#108864 = CARTESIAN_POINT('Ctrl Pts',(60.440286369022,253.144020946746,20.9924749143347)) ;
#108865 = CARTESIAN_POINT('Ctrl Pts',(60.4403288850239,253.143533106564,20.9911009060563)) ;
#108866 = CARTESIAN_POINT('Ctrl Pts',(60.4408750760621,253.137265961862,20.9734494107126)) ;
#108867 = CARTESIAN_POINT('Ctrl Pts',(60.4449239452531,253.131107267255,20.9560424309125)) ;
#108868 = CARTESIAN_POINT('Ctrl Pts',(60.4522665395981,253.125369105682,20.9397848739233)) ;
#108869 = CARTESIAN_POINT('Ctrl Pts',(60.4599211853139,253.119387079188,20.9228363904431)) ;
#108870 = CARTESIAN_POINT('Ctrl Pts',(60.4710122117669,253.113973725445,20.9074544440316)) ;
#108871 = CARTESIAN_POINT('Ctrl Pts',(60.4849165768427,253.109424192564,20.8945085756088)) ;
#108872 = CARTESIAN_POINT('Ctrl Pts',(60.4988172216941,253.104875876946,20.8815661709571)) ;
#108873 = CARTESIAN_POINT('Ctrl Pts',(60.5152637963996,253.101277691159,20.8713062373365)) ;
#108874 = CARTESIAN_POINT('Ctrl Pts',(60.53333156647,253.098824990589,20.8643092759729)) ;
#108875 = CARTESIAN_POINT('Ctrl Pts',(60.5513971100609,253.096372592264,20.8573131768402)) ;
#108876 = CARTESIAN_POINT('Ctrl Pts',(60.5707376338848,253.095112228145,20.8537132320655)) ;
#108877 = CARTESIAN_POINT('Ctrl Pts',(60.5902651077865,253.095112228145,20.8537132320655)) ;
#108878 = CARTESIAN_POINT('Origin',(60.5902651077865,253.27107594741,21.3217268744974)) ;
#108879 = CARTESIAN_POINT('Origin',(60.5902651077865,253.27107594741,21.3217268744974)) ;
#108880 = CARTESIAN_POINT('Origin',(60.5902651077865,243.590671638724,19.788501455951)) ;
#108881 = CARTESIAN_POINT('Origin',(60.5902651077865,248.040265107786,23.0213203435596)) ;
#108882 = CARTESIAN_POINT('',(60.5902651077865,253.115747008939,22.5218371395634)) ;
#108883 = CARTESIAN_POINT('Origin',(60.5902651077865,248.040265107786,23.0213203435596)) ;
#108884 = CARTESIAN_POINT('Ctrl Pts',(60.4402651077865,252.977912471676,22.6718371395634)) ;
#108885 = CARTESIAN_POINT('Ctrl Pts',(60.4402651077865,252.978450141357,22.6712600688988)) ;
#108886 = CARTESIAN_POINT('Ctrl Pts',(60.4402684378921,252.978987767856,22.6706829503216)) ;
#108887 = CARTESIAN_POINT('Ctrl Pts',(60.4404467789386,252.99337838034,22.655232733985)) ;
#108888 = CARTESIAN_POINT('Ctrl Pts',(60.4428319502743,253.007251853926,22.6402737328004)) ;
#108889 = CARTESIAN_POINT('Ctrl Pts',(60.4520052987548,253.033499763802,22.611858434734)) ;
#108890 = CARTESIAN_POINT('Ctrl Pts',(60.4586423249844,253.046029186311,22.5982392280904)) ;
#108891 = CARTESIAN_POINT('Ctrl Pts',(60.4774783235664,253.07058191007,22.5714615581854)) ;
#108892 = CARTESIAN_POINT('Ctrl Pts',(60.4902886559451,253.08251006586,22.5583957973774)) ;
#108893 = CARTESIAN_POINT('Ctrl Pts',(60.5183067650572,253.099809832103,22.5393982820177)) ;
#108894 = CARTESIAN_POINT('Ctrl Pts',(60.5322233323113,253.105986593393,22.5325967432531)) ;
#108895 = CARTESIAN_POINT('Ctrl Pts',(60.5612197979217,253.113796288923,22.5239903075244)) ;
#108896 = CARTESIAN_POINT('Ctrl Pts',(60.5755858845327,253.115747008939,22.5218371395634)) ;
#108897 = CARTESIAN_POINT('Ctrl Pts',(60.5902651077865,253.115747008939,22.5218371395634)) ;
#108898 = CARTESIAN_POINT('Origin',(60.5902651077865,250.427235809792,22.6718371395634)) ;
#108899 = CARTESIAN_POINT('',(60.5902651077865,253.517537835059,22.5218371395634)) ;
#108900 = CARTESIAN_POINT('',(60.5902651077865,250.427235809792,22.5218371395634)) ;
#108901 = CARTESIAN_POINT('Ctrl Pts',(60.4402651077865,253.521252214148,22.6718371395634)) ;
#108902 = CARTESIAN_POINT('Ctrl Pts',(60.4402651077865,253.521212580397,22.6703790162596)) ;
#108903 = CARTESIAN_POINT('Ctrl Pts',(60.440286369022,253.521173072598,22.6689209669186)) ;
#108904 = CARTESIAN_POINT('Ctrl Pts',(60.4403288850239,253.521133700923,22.667463456485)) ;
#108905 = CARTESIAN_POINT('Ctrl Pts',(60.4408750760621,253.52062790416,22.6487392325954)) ;
#108906 = CARTESIAN_POINT('Ctrl Pts',(60.4449239452532,253.520149690092,22.6302810697323)) ;
#108907 = CARTESIAN_POINT('Ctrl Pts',(60.452266539598,253.519716235534,22.6130460247761)) ;
#108908 = CARTESIAN_POINT('Ctrl Pts',(60.4599211853139,253.519264359681,22.5950785112735)) ;
#108909 = CARTESIAN_POINT('Ctrl Pts',(60.4710122117668,253.518869237177,22.5787765926025)) ;
#108910 = CARTESIAN_POINT('Ctrl Pts',(60.4849165768426,253.518542867634,22.5650584571031)) ;
#108911 = CARTESIAN_POINT('Ctrl Pts',(60.4988172216939,253.518216585413,22.5513439920009)) ;
#108912 = CARTESIAN_POINT('Ctrl Pts',(60.5152637963994,253.517965001224,22.5404743147172)) ;
#108913 = CARTESIAN_POINT('Ctrl Pts',(60.5333315664698,253.517794524335,22.5330618828598)) ;
#108914 = CARTESIAN_POINT('Ctrl Pts',(60.5513971100607,253.517624068453,22.5256503644316)) ;
#108915 = CARTESIAN_POINT('Ctrl Pts',(60.5707376338847,253.517537835059,22.5218371395634)) ;
#108916 = CARTESIAN_POINT('Ctrl Pts',(60.5902651077865,253.517537835059,22.5218371395634)) ;
#108917 = CARTESIAN_POINT('Origin',(60.5902651077865,253.540265107786,23.0213203435596)) ;
#108918 = CARTESIAN_POINT('Origin',(60.5902651077865,253.540265107786,23.0213203435596)) ;
#108919 = CARTESIAN_POINT('Origin',(60.5902651077865,242.809454268163,21.3217268744974)) ;
#108920 = CARTESIAN_POINT('Origin',(60.5902651077865,248.040265107786,23.0213203435596)) ;
#108921 = CARTESIAN_POINT('',(60.5902651077865,253.021684041655,24.1146937497175)) ;
#108922 = CARTESIAN_POINT('Origin',(60.5902651077865,248.040265107786,23.0213203435596)) ;
#108923 = CARTESIAN_POINT('Ctrl Pts',(60.4402651077865,252.844243057664,24.2147590127358)) ;
#108924 = CARTESIAN_POINT('Ctrl Pts',(60.4402651077865,252.844932736563,24.2143763349877)) ;
#108925 = CARTESIAN_POINT('Ctrl Pts',(60.440268437892,252.845622389192,24.213993598331)) ;
#108926 = CARTESIAN_POINT('Ctrl Pts',(60.4404467789386,252.864083054386,24.2037465132206)) ;
#108927 = CARTESIAN_POINT('Ctrl Pts',(60.4428319502744,252.881900097428,24.1938067967769)) ;
#108928 = CARTESIAN_POINT('Ctrl Pts',(60.4520052987548,252.915644153157,24.1748932926068)) ;
#108929 = CARTESIAN_POINT('Ctrl Pts',(60.4586423249845,252.931768908382,24.1658124618668)) ;
#108930 = CARTESIAN_POINT('Ctrl Pts',(60.4774783235665,252.963394691376,24.1479325933121)) ;
#108931 = CARTESIAN_POINT('Ctrl Pts',(60.4902886559452,252.978776583803,24.1391923192062)) ;
#108932 = CARTESIAN_POINT('Ctrl Pts',(60.5183067650572,253.001100194315,24.1264705301978)) ;
#108933 = CARTESIAN_POINT('Ctrl Pts',(60.5322233323113,253.009076434455,24.1219106066435)) ;
#108934 = CARTESIAN_POINT('Ctrl Pts',(60.5612197979217,253.019163431181,24.1161387285016)) ;
#108935 = CARTESIAN_POINT('Ctrl Pts',(60.5755858845327,253.021684041655,24.1146937497175)) ;
#108936 = CARTESIAN_POINT('Ctrl Pts',(60.5902651077866,253.021684041655,24.1146937497175)) ;
#108937 = CARTESIAN_POINT('Origin',(60.5902651077865,250.418405397417,23.426556577058)) ;
#108938 = CARTESIAN_POINT('',(60.5902651077865,253.403809825024,24.2388539431727)) ;
#108939 = CARTESIAN_POINT('',(60.5902651077865,250.464757946574,23.2838980996137)) ;
#108940 = CARTESIAN_POINT('Ctrl Pts',(60.4402651077865,253.360989860305,24.3826602268791)) ;
#108941 = CARTESIAN_POINT('Ctrl Pts',(60.4402651077865,253.361402751249,24.3812612217063)) ;
#108942 = CARTESIAN_POINT('Ctrl Pts',(60.440286369022,253.361815739121,24.3798623257983)) ;
#108943 = CARTESIAN_POINT('Ctrl Pts',(60.4403288850239,253.362228689928,24.378463984486)) ;
#108944 = CARTESIAN_POINT('Ctrl Pts',(60.4408750760622,253.367533752024,24.3604998895503)) ;
#108945 = CARTESIAN_POINT('Ctrl Pts',(60.4449239452534,253.372782829414,24.3427973572039)) ;
#108946 = CARTESIAN_POINT('Ctrl Pts',(60.4522665395982,253.377696511422,24.3262719105652)) ;
#108947 = CARTESIAN_POINT('Ctrl Pts',(60.459921185314,253.382819018967,24.3090441524494)) ;
#108948 = CARTESIAN_POINT('Ctrl Pts',(60.4710122117669,253.387480805045,24.2934180069006)) ;
#108949 = CARTESIAN_POINT('Ctrl Pts',(60.4849165768428,253.391409546165,24.2802704310071)) ;
#108950 = CARTESIAN_POINT('Ctrl Pts',(60.4988172216941,253.395337236118,24.2671263728531)) ;
#108951 = CARTESIAN_POINT('Ctrl Pts',(60.5152637963996,253.39845688034,24.2567109516526)) ;
#108952 = CARTESIAN_POINT('Ctrl Pts',(60.53333156647,253.400585314597,24.2496086297771)) ;
#108953 = CARTESIAN_POINT('Ctrl Pts',(60.5513971100607,253.402713486568,24.2425071831161)) ;
#108954 = CARTESIAN_POINT('Ctrl Pts',(60.5707376338847,253.403809825025,24.238853943173)) ;
#108955 = CARTESIAN_POINT('Ctrl Pts',(60.5902651077865,253.403809825025,24.238853943173)) ;
#108956 = CARTESIAN_POINT('Origin',(60.5902651077865,253.27107594741,24.7209138126218)) ;
#108957 = CARTESIAN_POINT('Origin',(60.5902651077865,253.27107594741,24.7209138126218)) ;
#108958 = CARTESIAN_POINT('Origin',(60.5902651077865,242.540265107786,23.0213203435596)) ;
#108959 = CARTESIAN_POINT('Origin',(60.5902651077865,248.040265107786,23.0213203435596)) ;
#108960 = CARTESIAN_POINT('',(60.5902651077865,252.440005081538,25.6005233528965)) ;
#108961 = CARTESIAN_POINT('Origin',(60.5902651077865,248.040265107786,23.0213203435596)) ;
#108962 = CARTESIAN_POINT('Ctrl Pts',(60.4402651077865,252.240326810636,25.6408587937931)) ;
#108963 = CARTESIAN_POINT('Ctrl Pts',(60.4402651077865,252.241100988174,25.6407079681274)) ;
#108964 = CARTESIAN_POINT('Ctrl Pts',(60.440268437892,252.241875158933,25.6405570783186)) ;
#108965 = CARTESIAN_POINT('Ctrl Pts',(60.4404467789386,252.262598818302,25.6365161805241)) ;
#108966 = CARTESIAN_POINT('Ctrl Pts',(60.4428319502744,252.282615374489,25.6325687175193)) ;
#108967 = CARTESIAN_POINT('Ctrl Pts',(60.4520052987548,252.320552472788,25.6250083928119)) ;
#108968 = CARTESIAN_POINT('Ctrl Pts',(60.4586423249844,252.338694157341,25.621354832958)) ;
#108969 = CARTESIAN_POINT('Ctrl Pts',(60.4774783235665,252.374297247581,25.6141229718641)) ;
#108970 = CARTESIAN_POINT('Ctrl Pts',(60.4902886559452,252.39162718984,25.6105637433868)) ;
#108971 = CARTESIAN_POINT('Ctrl Pts',(60.5183067650571,252.416789454087,25.6053629780756)) ;
#108972 = CARTESIAN_POINT('Ctrl Pts',(60.5322233323112,252.42578440312,25.6034910268201)) ;
#108973 = CARTESIAN_POINT('Ctrl Pts',(60.5612197979217,252.437161315521,25.6011186979124)) ;
#108974 = CARTESIAN_POINT('Ctrl Pts',(60.5755858845327,252.440005081538,25.6005233528966)) ;
#108975 = CARTESIAN_POINT('Ctrl Pts',(60.5902651077865,252.440005081538,25.6005233528966)) ;
#108976 = CARTESIAN_POINT('Origin',(60.5902651077865,250.176786044017,24.1416086685709)) ;
#108977 = CARTESIAN_POINT('',(60.5902651077865,252.765060688053,25.8366900749965)) ;
#108978 = CARTESIAN_POINT('',(60.5902651077865,250.26495383186,24.0202561194147)) ;
#108979 = CARTESIAN_POINT('Ctrl Pts',(60.4402651077865,252.679897896016,25.9602258814029)) ;
#108980 = CARTESIAN_POINT('Ctrl Pts',(60.4402651077865,252.680722895012,25.9590229387354)) ;
#108981 = CARTESIAN_POINT('Ctrl Pts',(60.440286369022,252.681547952429,25.9578201299378)) ;
#108982 = CARTESIAN_POINT('Ctrl Pts',(60.4403288850239,252.682372803214,25.9566178371377)) ;
#108983 = CARTESIAN_POINT('Ctrl Pts',(60.4408750760621,252.692969427709,25.9411723219306)) ;
#108984 = CARTESIAN_POINT('Ctrl Pts',(60.4449239452532,252.703431980308,25.9259582673091)) ;
#108985 = CARTESIAN_POINT('Ctrl Pts',(60.452266539598,252.713211813452,25.911760044844)) ;
#108986 = CARTESIAN_POINT('Ctrl Pts',(60.4599211853139,252.723407277665,25.8969584151117)) ;
#108987 = CARTESIAN_POINT('Ctrl Pts',(60.4710122117667,252.732669644223,25.8835376386852)) ;
#108988 = CARTESIAN_POINT('Ctrl Pts',(60.4849165768426,252.740468923451,25.8722475987305)) ;
#108989 = CARTESIAN_POINT('Ctrl Pts',(60.4988172216939,252.74826611592,25.8609605795167)) ;
#108990 = CARTESIAN_POINT('Ctrl Pts',(60.5152637963993,252.75445161604,25.8520189483948)) ;
#108991 = CARTESIAN_POINT('Ctrl Pts',(60.5333315664698,252.758670615469,25.8459219612514)) ;
#108992 = CARTESIAN_POINT('Ctrl Pts',(60.5513971100607,252.762889094994,25.8398257254357)) ;
#108993 = CARTESIAN_POINT('Ctrl Pts',(60.5707376338847,252.765060688054,25.8366900749968)) ;
#108994 = CARTESIAN_POINT('Ctrl Pts',(60.5902651077865,252.765060688054,25.8366900749968)) ;
#108995 = CARTESIAN_POINT('Origin',(60.5902651077865,252.489858576849,26.2541392311682)) ;
#108996 = CARTESIAN_POINT('Origin',(60.5902651077865,252.489858576849,26.2541392311682)) ;
#108997 = CARTESIAN_POINT('Origin',(60.5902651077865,242.809454268163,24.7209138126218)) ;
#108998 = CARTESIAN_POINT('Origin',(60.5902651077865,248.040265107786,23.0213203435596)) ;
#108999 = CARTESIAN_POINT('',(60.5902651077865,251.427648917999,26.8338825951576)) ;
#109000 = CARTESIAN_POINT('Origin',(60.5902651077865,248.040265107786,23.0213203435596)) ;
#109001 = CARTESIAN_POINT('Ctrl Pts',(60.4402651077865,251.225279260583,26.8105398999439)) ;
#109002 = CARTESIAN_POINT('Ctrl Pts',(60.4402651077865,251.22606215487,26.8106356902278)) ;
#109003 = CARTESIAN_POINT('Ctrl Pts',(60.440268437892,251.226845062531,26.810731417413)) ;
#109004 = CARTESIAN_POINT('Ctrl Pts',(60.4404467789389,251.247803139908,26.8132922581646)) ;
#109005 = CARTESIAN_POINT('Ctrl Pts',(60.4428319502749,251.268059849255,26.8157234537816)) ;
#109006 = CARTESIAN_POINT('Ctrl Pts',(60.4520052987553,251.306476442619,26.8202563657949)) ;
#109007 = CARTESIAN_POINT('Ctrl Pts',(60.4586423249848,251.324859222013,26.8223877127214)) ;
#109008 = CARTESIAN_POINT('Ctrl Pts',(60.4774783235664,251.360954540964,26.8265117640394)) ;
#109009 = CARTESIAN_POINT('Ctrl Pts',(60.4902886559451,251.378536157563,26.8284819832727)) ;
#109010 = CARTESIAN_POINT('Ctrl Pts',(60.5183067650572,251.404074017806,26.8313113288033)) ;
#109011 = CARTESIAN_POINT('Ctrl Pts',(60.5322233323113,251.413207187447,26.832310589478)) ;
#109012 = CARTESIAN_POINT('Ctrl Pts',(60.5612197979217,251.42476036407,26.8335700298871)) ;
#109013 = CARTESIAN_POINT('Ctrl Pts',(60.5755858845327,251.427648917999,26.8338825951576)) ;
#109014 = CARTESIAN_POINT('Ctrl Pts',(60.5902651077866,251.427648917999,26.8338825951576)) ;
#109015 = CARTESIAN_POINT('Origin',(60.5902651077865,249.726029135361,24.746999133324)) ;
#109016 = CARTESIAN_POINT('',(60.5902651077865,251.663815640099,27.1589382016729)) ;
#109017 = CARTESIAN_POINT('',(60.5902651077865,249.847381684517,24.6588313454802)) ;
#109018 = CARTESIAN_POINT('Ctrl Pts',(60.4402651077865,251.544646348192,27.2501109853232)) ;
#109019 = CARTESIAN_POINT('Ctrl Pts',(60.4402651077865,251.545802698591,27.2492218575707)) ;
#109020 = CARTESIAN_POINT('Ctrl Pts',(60.440286369022,251.546959063183,27.2483328751888)) ;
#109021 = CARTESIAN_POINT('Ctrl Pts',(60.4403288850239,251.548115071804,27.2474443196972)) ;
#109022 = CARTESIAN_POINT('Ctrl Pts',(60.4408750760621,251.562965987268,27.2360292988668)) ;
#109023 = CARTESIAN_POINT('Ctrl Pts',(60.4449239452532,251.577617867525,27.2247929796352)) ;
#109024 = CARTESIAN_POINT('Ctrl Pts',(60.452266539598,251.591306533596,27.2143118022833)) ;
#109025 = CARTESIAN_POINT('Ctrl Pts',(60.459921185314,251.605576951405,27.2033851875821)) ;
#109026 = CARTESIAN_POINT('Ctrl Pts',(60.4710122117669,251.61853323347,27.1934834993827)) ;
#109027 = CARTESIAN_POINT('Ctrl Pts',(60.4849165768426,251.629439603015,27.1851561431399)) ;
#109028 = CARTESIAN_POINT('Ctrl Pts',(60.4988172216938,251.640343054474,27.1768310149481)) ;
#109029 = CARTESIAN_POINT('Ctrl Pts',(60.5152637963993,251.648988930644,27.1702384430593)) ;
#109030 = CARTESIAN_POINT('Ctrl Pts',(60.5333315664697,251.654885510185,27.1657436062293)) ;
#109031 = CARTESIAN_POINT('Ctrl Pts',(60.5513971100606,251.660781363094,27.1612493232952)) ;
#109032 = CARTESIAN_POINT('Ctrl Pts',(60.5707376338847,251.663815640098,27.1589382016717)) ;
#109033 = CARTESIAN_POINT('Ctrl Pts',(60.5902651077865,251.663815640098,27.1589382016716)) ;
#109034 = CARTESIAN_POINT('Origin',(60.5902651077865,251.273083995395,27.4709138126218)) ;
#109035 = CARTESIAN_POINT('Origin',(60.5902651077865,251.273083995395,27.4709138126218)) ;
#109036 = CARTESIAN_POINT('Origin',(60.5902651077865,243.590671638724,26.2541392311682)) ;
#109037 = CARTESIAN_POINT('Origin',(60.5902651077865,248.040265107786,23.0213203435596)) ;
#109038 = CARTESIAN_POINT('',(60.5902651077865,250.083712025826,27.694041680549)) ;
#109039 = CARTESIAN_POINT('Origin',(60.5902651077865,248.040265107786,23.0213203435596)) ;
#109040 = CARTESIAN_POINT('Ctrl Pts',(60.4402651077865,249.898460333955,27.6093057948708)) ;
#109041 = CARTESIAN_POINT('Ctrl Pts',(60.4402651077865,249.89917530984,27.6096388244826)) ;
#109042 = CARTESIAN_POINT('Ctrl Pts',(60.4402684378921,249.899890317948,27.6099717982194)) ;
#109043 = CARTESIAN_POINT('Ctrl Pts',(60.4404467789386,249.91903129069,27.6188837045809)) ;
#109044 = CARTESIAN_POINT('Ctrl Pts',(60.4428319502743,249.937545285353,27.6274555764535)) ;
#109045 = CARTESIAN_POINT('Ctrl Pts',(60.4520052987548,249.97268088996,27.6436380121775)) ;
#109046 = CARTESIAN_POINT('Ctrl Pts',(60.4586423249844,249.989505329671,27.6513456347974)) ;
#109047 = CARTESIAN_POINT('Ctrl Pts',(60.4774783235665,250.022559616025,27.6664219076506)) ;
#109048 = CARTESIAN_POINT('Ctrl Pts',(60.4902886559452,250.038671895832,27.6737287158086)) ;
#109049 = CARTESIAN_POINT('Ctrl Pts',(60.5183067650571,250.062085528376,27.6843112161272)) ;
#109050 = CARTESIAN_POINT('Ctrl Pts',(60.5322233323112,250.070462900348,27.6880838741351)) ;
#109051 = CARTESIAN_POINT('Ctrl Pts',(60.5612197979218,250.08106143577,27.6928518010587)) ;
#109052 = CARTESIAN_POINT('Ctrl Pts',(60.5755858845328,250.083712025825,27.6940416805491)) ;
#109053 = CARTESIAN_POINT('Ctrl Pts',(60.5902651077866,250.083712025825,27.6940416805491)) ;
#109054 = CARTESIAN_POINT('Origin',(60.5902651077865,249.110257898277,25.1834681346239)) ;
#109055 = CARTESIAN_POINT('',(60.5902651077865,250.207872219281,28.0761674639184)) ;
#109056 = CARTESIAN_POINT('',(60.5902651077865,249.252916375722,25.1371155854676)) ;
#109057 = CARTESIAN_POINT('Ctrl Pts',(60.4402651077865,250.066361548098,28.1260525975113)) ;
#109058 = CARTESIAN_POINT('Ctrl Pts',(60.4402651077865,250.067736058265,28.1255643186932)) ;
#109059 = CARTESIAN_POINT('Ctrl Pts',(60.440286369022,250.069110537011,28.1250761825189)) ;
#109060 = CARTESIAN_POINT('Ctrl Pts',(60.4403288850239,250.07048454529,28.1245883423372)) ;
#109061 = CARTESIAN_POINT('Ctrl Pts',(60.4408750760621,250.088136040636,28.1183211976397)) ;
#109062 = CARTESIAN_POINT('Ctrl Pts',(60.4449239452533,250.105543020433,28.112162503026)) ;
#109063 = CARTESIAN_POINT('Ctrl Pts',(60.4522665395981,250.121800577422,28.1064243414531)) ;
#109064 = CARTESIAN_POINT('Ctrl Pts',(60.4599211853138,250.138749060902,28.1004423149599)) ;
#109065 = CARTESIAN_POINT('Ctrl Pts',(60.4710122117668,250.154131007314,28.095028961218)) ;
#109066 = CARTESIAN_POINT('Ctrl Pts',(60.4849165768428,250.167076875737,28.0904794283365)) ;
#109067 = CARTESIAN_POINT('Ctrl Pts',(60.4988172216942,250.180019280389,28.085931112719)) ;
#109068 = CARTESIAN_POINT('Ctrl Pts',(60.5152637963998,250.190279214009,28.0823329269325)) ;
#109069 = CARTESIAN_POINT('Ctrl Pts',(60.5333315664701,250.197276175373,28.0798802263628)) ;
#109070 = CARTESIAN_POINT('Ctrl Pts',(60.5513971100608,250.204272274506,28.0774278280377)) ;
#109071 = CARTESIAN_POINT('Ctrl Pts',(60.5707376338848,250.20787221928,28.0761674639187)) ;
#109072 = CARTESIAN_POINT('Ctrl Pts',(60.5902651077865,250.20787221928,28.0761674639188)) ;
#109073 = CARTESIAN_POINT('Origin',(60.5902651077865,249.739858576849,28.252131183183)) ;
#109074 = CARTESIAN_POINT('Origin',(60.5902651077865,249.739858576849,28.252131183183)) ;
#109075 = CARTESIAN_POINT('Origin',(60.5902651077865,244.807446220178,27.4709138126218)) ;
#109076 = CARTESIAN_POINT('Origin',(60.5902651077865,248.040265107786,23.0213203435596)) ;
#109077 = CARTESIAN_POINT('',(60.5902651077865,248.539748311783,28.096802244712)) ;
#109078 = CARTESIAN_POINT('Origin',(60.5902651077865,248.040265107786,23.0213203435596)) ;
#109079 = CARTESIAN_POINT('Ctrl Pts',(60.4402651077865,248.389748311783,27.9589677074491)) ;
#109080 = CARTESIAN_POINT('Ctrl Pts',(60.4402651077865,248.390325382447,27.9595053771305)) ;
#109081 = CARTESIAN_POINT('Ctrl Pts',(60.4402684378921,248.390902501024,27.9600430036291)) ;
#109082 = CARTESIAN_POINT('Ctrl Pts',(60.4404467789386,248.406352717361,27.974433616113)) ;
#109083 = CARTESIAN_POINT('Ctrl Pts',(60.4428319502743,248.421311718545,27.9883070896991)) ;
#109084 = CARTESIAN_POINT('Ctrl Pts',(60.4520052987548,248.449727016612,28.014554999575)) ;
#109085 = CARTESIAN_POINT('Ctrl Pts',(60.4586423249844,248.463346223256,28.027084422084)) ;
#109086 = CARTESIAN_POINT('Ctrl Pts',(60.4774783235664,248.490123893161,28.0516371458428)) ;
#109087 = CARTESIAN_POINT('Ctrl Pts',(60.4902886559451,248.503189653969,28.0635653016335)) ;
#109088 = CARTESIAN_POINT('Ctrl Pts',(60.5183067650572,248.522187169328,28.0808650678765)) ;
#109089 = CARTESIAN_POINT('Ctrl Pts',(60.5322233323113,248.528988708093,28.087041829166)) ;
#109090 = CARTESIAN_POINT('Ctrl Pts',(60.5612197979217,248.537595143822,28.0948515246968)) ;
#109091 = CARTESIAN_POINT('Ctrl Pts',(60.5755858845327,248.539748311783,28.096802244712)) ;
#109092 = CARTESIAN_POINT('Ctrl Pts',(60.5902651077865,248.539748311783,28.096802244712)) ;
#109093 = CARTESIAN_POINT('Origin',(60.5902651077865,248.389748311783,25.4082910455649)) ;
#109094 = CARTESIAN_POINT('',(60.5902651077865,248.539748311783,28.4985930708324)) ;
#109095 = CARTESIAN_POINT('',(60.5902651077865,248.539748311783,25.4082910455649)) ;
#109096 = CARTESIAN_POINT('Ctrl Pts',(60.4402651077865,248.389748311783,28.5023074499214)) ;
#109097 = CARTESIAN_POINT('Ctrl Pts',(60.4402651077865,248.391206435086,28.5022678161702)) ;
#109098 = CARTESIAN_POINT('Ctrl Pts',(60.440286369022,248.392664484427,28.5022283083715)) ;
#109099 = CARTESIAN_POINT('Ctrl Pts',(60.4403288850238,248.394121994861,28.5021889366964)) ;
#109100 = CARTESIAN_POINT('Ctrl Pts',(60.440875076062,248.412846218751,28.501683139933)) ;
#109101 = CARTESIAN_POINT('Ctrl Pts',(60.4449239452532,248.431304381614,28.5012049258673)) ;
#109102 = CARTESIAN_POINT('Ctrl Pts',(60.4522665395979,248.44853942657,28.5007714713081)) ;
#109103 = CARTESIAN_POINT('Ctrl Pts',(60.4599211853135,248.466506940072,28.5003195954549)) ;
#109104 = CARTESIAN_POINT('Ctrl Pts',(60.4710122117664,248.482808858743,28.4999244729506)) ;
#109105 = CARTESIAN_POINT('Ctrl Pts',(60.4849165768423,248.496526994243,28.499598103407)) ;
#109106 = CARTESIAN_POINT('Ctrl Pts',(60.4988172216937,248.510241459345,28.4992718211862)) ;
#109107 = CARTESIAN_POINT('Ctrl Pts',(60.5152637963994,248.521111136629,28.4990202369969)) ;
#109108 = CARTESIAN_POINT('Ctrl Pts',(60.5333315664697,248.528523568487,28.4988497601079)) ;
#109109 = CARTESIAN_POINT('Ctrl Pts',(60.5513971100605,248.535935086915,28.4986793042266)) ;
#109110 = CARTESIAN_POINT('Ctrl Pts',(60.5707376338847,248.539748311783,28.4985930708331)) ;
#109111 = CARTESIAN_POINT('Ctrl Pts',(60.5902651077865,248.539748311783,28.4985930708331)) ;
#109112 = CARTESIAN_POINT('Origin',(60.5902651077865,248.040265107786,28.5213203435596)) ;
#109113 = CARTESIAN_POINT('Origin',(60.5902651077865,248.040265107786,28.5213203435596)) ;
#109114 = CARTESIAN_POINT('Origin',(60.5902651077865,246.340671638724,28.252131183183)) ;
#109115 = CARTESIAN_POINT('Origin',(60.5902651077865,246.340671638724,28.252131183183)) ;
#109116 = CARTESIAN_POINT('Origin',(60.4402651077865,248.040265107786,23.0213203435596)) ;
#109117 = CARTESIAN_POINT('',(60.4402651077865,247.54078190379,28.096802244712)) ;
#109118 = CARTESIAN_POINT('',(60.4402651077865,246.946891701628,28.0027392774284)) ;
#109119 = CARTESIAN_POINT('Origin',(60.4402651077865,247.040072839737,27.7159572226947)) ;
#109120 = CARTESIAN_POINT('',(60.4402651077865,246.822731508173,28.3848650607978)) ;
#109121 = CARTESIAN_POINT('Origin',(60.4402651077865,246.340671638724,28.252131183183)) ;
#109122 = CARTESIAN_POINT('',(60.4402651077865,245.872657996292,28.0761674639184)) ;
#109123 = CARTESIAN_POINT('Origin',(60.4402651077865,245.872657996292,28.0761674639184)) ;
#109124 = CARTESIAN_POINT('Origin',(60.4402651077865,250.442227059934,18.8655317564881)) ;
#109125 = CARTESIAN_POINT('',(60.4402651077865,250.619468117123,18.6215803698081)) ;
#109126 = CARTESIAN_POINT('',(60.4402651077865,250.855634839223,18.2965247632928)) ;
#109127 = CARTESIAN_POINT('Origin',(60.4402651077865,251.663815640099,18.8837024854464)) ;
#109128 = CARTESIAN_POINT('',(60.4402651077865,251.663815640099,18.8837024854464)) ;
#109129 = CARTESIAN_POINT('',(60.4402651077865,251.427648917999,19.2087580919617)) ;
#109130 = CARTESIAN_POINT('Origin',(60.4402651077865,251.273083995395,18.5717268744974)) ;
#109131 = CARTESIAN_POINT('Origin',(60.4402651077865,251.608875972704,19.811177590536)) ;
#109132 = CARTESIAN_POINT('',(60.4402651077865,251.852827359384,19.6339365333471)) ;
#109133 = CARTESIAN_POINT('',(60.4402651077865,252.1778829659,19.3977698112471)) ;
#109134 = CARTESIAN_POINT('Origin',(60.4402651077865,252.765060688053,20.2059506121228)) ;
#109135 = CARTESIAN_POINT('',(60.4402651077865,252.765060688053,20.2059506121228)) ;
#109136 = CARTESIAN_POINT('',(60.4402651077865,252.440005081538,20.4421173342227)) ;
#109137 = CARTESIAN_POINT('Origin',(60.4402651077865,252.489858576849,19.788501455951)) ;
#109138 = CARTESIAN_POINT('Origin',(60.4402651077865,252.426204390042,21.0710545636296)) ;
#109139 = CARTESIAN_POINT('',(60.4402651077865,252.712986444776,20.9778734255204)) ;
#109140 = CARTESIAN_POINT('',(60.4402651077865,253.095112228145,20.8537132320653)) ;
#109141 = CARTESIAN_POINT('Origin',(60.4402651077865,253.403809825024,21.8037867439466)) ;
#109142 = CARTESIAN_POINT('',(60.4402651077865,253.403809825024,21.8037867439466)) ;
#109143 = CARTESIAN_POINT('',(60.4402651077865,253.021684041655,21.9279469374017)) ;
#109144 = CARTESIAN_POINT('Origin',(60.4402651077865,253.27107594741,21.3217268744974)) ;
#109145 = CARTESIAN_POINT('Origin',(60.4402651077865,252.814206511797,22.5218371395634)) ;
#109146 = CARTESIAN_POINT('',(60.4402651077865,253.115747008939,22.5218371395634)) ;
#109147 = CARTESIAN_POINT('',(60.4402651077865,253.517537835059,22.5218371395634)) ;
#109148 = CARTESIAN_POINT('Origin',(60.4402651077865,253.517537835059,23.5208035475559)) ;
#109149 = CARTESIAN_POINT('',(60.4402651077865,253.517537835059,23.5208035475559)) ;
#109150 = CARTESIAN_POINT('',(60.4402651077865,253.115747008939,23.5208035475559)) ;
#109151 = CARTESIAN_POINT('Origin',(60.4402651077865,253.540265107786,23.0213203435596)) ;
#109152 = CARTESIAN_POINT('Origin',(60.4402651077865,252.734901986921,24.0215126116084)) ;
#109153 = CARTESIAN_POINT('',(60.4402651077865,253.021684041655,24.1146937497175)) ;
#109154 = CARTESIAN_POINT('',(60.4402651077865,253.403809825024,24.2388539431727)) ;
#109155 = CARTESIAN_POINT('Origin',(60.4402651077865,253.095112228145,25.188927455054)) ;
#109156 = CARTESIAN_POINT('',(60.4402651077865,253.095112228145,25.188927455054)) ;
#109157 = CARTESIAN_POINT('',(60.4402651077865,252.712986444776,25.0647672615988)) ;
#109158 = CARTESIAN_POINT('Origin',(60.4402651077865,253.27107594741,24.7209138126218)) ;
#109159 = CARTESIAN_POINT('Origin',(60.4402651077865,252.196053694858,25.4232822957076)) ;
#109160 = CARTESIAN_POINT('',(60.4402651077865,252.440005081538,25.6005233528965)) ;
#109161 = CARTESIAN_POINT('',(60.4402651077865,252.765060688053,25.8366900749965)) ;
#109162 = CARTESIAN_POINT('Origin',(60.4402651077865,252.1778829659,26.6448708758722)) ;
#109163 = CARTESIAN_POINT('',(60.4402651077865,252.1778829659,26.6448708758722)) ;
#109164 = CARTESIAN_POINT('',(60.4402651077865,251.852827359384,26.4087041537722)) ;
#109165 = CARTESIAN_POINT('Origin',(60.4402651077865,252.489858576849,26.2541392311682)) ;
#109166 = CARTESIAN_POINT('Origin',(60.4402651077865,251.25040786081,26.5899312084775)) ;
#109167 = CARTESIAN_POINT('',(60.4402651077865,251.427648917999,26.8338825951576)) ;
#109168 = CARTESIAN_POINT('',(60.4402651077865,251.663815640099,27.1589382016729)) ;
#109169 = CARTESIAN_POINT('Origin',(60.4402651077865,250.855634839223,27.7461159238265)) ;
#109170 = CARTESIAN_POINT('',(60.4402651077865,250.855634839223,27.7461159238265)) ;
#109171 = CARTESIAN_POINT('',(60.4402651077865,250.619468117123,27.4210603173112)) ;
#109172 = CARTESIAN_POINT('Origin',(60.4402651077865,251.273083995395,27.4709138126218)) ;
#109173 = CARTESIAN_POINT('Origin',(60.4402651077865,249.990530887716,27.4072596258153)) ;
#109174 = CARTESIAN_POINT('',(60.4402651077865,250.083712025826,27.694041680549)) ;
#109175 = CARTESIAN_POINT('',(60.4402651077865,250.207872219281,28.0761674639184)) ;
#109176 = CARTESIAN_POINT('Origin',(60.4402651077865,249.257798707399,28.3848650607978)) ;
#109177 = CARTESIAN_POINT('',(60.4402651077865,249.257798707399,28.3848650607978)) ;
#109178 = CARTESIAN_POINT('',(60.4402651077865,249.133638513944,28.0027392774284)) ;
#109179 = CARTESIAN_POINT('Origin',(60.4402651077865,249.739858576849,28.252131183183)) ;
#109180 = CARTESIAN_POINT('Origin',(60.4402651077865,248.539748311783,27.7952617475701)) ;
#109181 = CARTESIAN_POINT('',(60.4402651077865,248.539748311783,28.096802244712)) ;
#109182 = CARTESIAN_POINT('',(60.4402651077865,248.539748311783,28.4985930708324)) ;
#109183 = CARTESIAN_POINT('Origin',(60.4402651077865,247.54078190379,28.4985930708324)) ;
#109184 = CARTESIAN_POINT('',(60.4402651077865,247.54078190379,28.4985930708324)) ;
#109185 = CARTESIAN_POINT('Origin',(60.4402651077865,248.040265107786,28.5213203435596)) ;
#109186 = CARTESIAN_POINT('Origin',(60.4402651077865,248.040265107786,23.0213203435596)) ;
#109187 = CARTESIAN_POINT('Origin',(60.4402651077865,248.040265107786,23.0213203435596)) ;
#109188 = CARTESIAN_POINT('Origin',(60.4402651077865,248.040265107786,23.0213203435596)) ;
#109189 = CARTESIAN_POINT('Origin',(60.4402651077865,248.040265107786,23.0213203435596)) ;
#109190 = CARTESIAN_POINT('Origin',(60.4402651077865,248.040265107786,23.0213203435596)) ;
#109191 = CARTESIAN_POINT('Origin',(60.4402651077865,248.040265107786,23.0213203435596)) ;
#109192 = CARTESIAN_POINT('Origin',(60.4402651077865,248.040265107786,23.0213203435596)) ;
#109193 = CARTESIAN_POINT('Origin',(60.4402651077865,248.040265107786,23.0213203435596)) ;
#109194 = CARTESIAN_POINT('Origin',(60.4402651077865,248.040265107786,23.0213203435596)) ;
#109195 = CARTESIAN_POINT('Origin',(59.9402651077865,248.040265107786,23.0213203435596)) ;
#109196 = CARTESIAN_POINT('',(59.9402651077865,250.040265107786,23.0213203435596)) ;
#109197 = CARTESIAN_POINT('',(0.,0.,0.)) ;
#109198 = CARTESIAN_POINT('Origin',(67.8645744874958,248.040265107786,23.0213203435596)) ;
#109199 = CARTESIAN_POINT('',(66.6775101468938,247.272170391243,24.5129220226009)) ;
#109200 = CARTESIAN_POINT('',(66.7760547678839,247.272170398758,24.5129220264705)) ;
#109201 = CARTESIAN_POINT('',(67.8645744874958,247.272170391302,24.5129220226314)) ;
#109202 = CARTESIAN_POINT('',(66.9402651077865,248.99748421711,21.6434318722943)) ;
#109203 = CARTESIAN_POINT('Ctrl Pts',(66.6775101468938,247.272170391243,24.5129220226009)) ;
#109204 = CARTESIAN_POINT('Ctrl Pts',(66.677589495217,247.27066246832,24.5121455233208)) ;
#109205 = CARTESIAN_POINT('Ctrl Pts',(66.6776689190512,247.269155710994,24.5113667312804)) ;
#109206 = CARTESIAN_POINT('Ctrl Pts',(66.6791016407658,247.242022407589,24.4972902623795)) ;
#109207 = CARTESIAN_POINT('Ctrl Pts',(66.6804764523606,247.216743161287,24.4833361073896)) ;
#109208 = CARTESIAN_POINT('Ctrl Pts',(66.6838763528271,247.156118525715,24.4477999566119)) ;
#109209 = CARTESIAN_POINT('Ctrl Pts',(66.6859237159345,247.121188973355,24.4255489497983)) ;
#109210 = CARTESIAN_POINT('Ctrl Pts',(66.6905785877253,247.045196098053,24.3730887816372)) ;
#109211 = CARTESIAN_POINT('Ctrl Pts',(66.6932043974035,247.004614632758,24.3422547967654)) ;
#109212 = CARTESIAN_POINT('Ctrl Pts',(66.7005043372691,246.897316724161,24.2527417542348)) ;
#109213 = CARTESIAN_POINT('Ctrl Pts',(66.7052453931358,246.833757851215,24.1905378350948)) ;
#109214 = CARTESIAN_POINT('Ctrl Pts',(66.7121603957986,246.746503512077,24.090414949827)) ;
#109215 = CARTESIAN_POINT('Ctrl Pts',(66.7144187371205,246.71890128238,24.0561055536296)) ;
#109216 = CARTESIAN_POINT('Ctrl Pts',(66.7175997681525,246.680795494484,24.0047253430734)) ;
#109217 = CARTESIAN_POINT('Ctrl Pts',(66.7185772458303,246.669198241514,23.9884908220179)) ;
#109218 = CARTESIAN_POINT('Ctrl Pts',(66.7203334479191,246.648502004517,23.9583983321257)) ;
#109219 = CARTESIAN_POINT('Ctrl Pts',(66.7211170566993,246.639314211992,23.9446059362019)) ;
#109220 = CARTESIAN_POINT('Ctrl Pts',(66.723139446091,246.615774834301,23.9081088486848)) ;
#109221 = CARTESIAN_POINT('Ctrl Pts',(66.7243591509514,246.601761119866,23.885191166995)) ;
#109222 = CARTESIAN_POINT('Ctrl Pts',(66.727136033152,246.570548443607,23.8312793875019)) ;
#109223 = CARTESIAN_POINT('Ctrl Pts',(66.728675983708,246.553769105835,23.8000568535244)) ;
#109224 = CARTESIAN_POINT('Ctrl Pts',(66.7350389622131,246.487679759062,23.6671469696579)) ;
#109225 = CARTESIAN_POINT('Ctrl Pts',(66.7396748067044,246.447718995985,23.5611454754844)) ;
#109226 = CARTESIAN_POINT('Ctrl Pts',(66.746836208827,246.40525673722,23.4012450590947)) ;
#109227 = CARTESIAN_POINT('Ctrl Pts',(66.7491533706109,246.394181727546,23.3499601749954)) ;
#109228 = CARTESIAN_POINT('Ctrl Pts',(66.7529194256483,246.380530714064,23.2683891944497)) ;
#109229 = CARTESIAN_POINT('Ctrl Pts',(66.754320259486,246.3763436531,23.2384068153772)) ;
#109230 = CARTESIAN_POINT('Ctrl Pts',(66.7571290346595,246.369695429576,23.179133758156)) ;
#109231 = CARTESIAN_POINT('Ctrl Pts',(66.7585350539675,246.36718836913,23.1498591431466)) ;
#109232 = CARTESIAN_POINT('Ctrl Pts',(66.7622064319954,246.362724258965,23.0745016512219)) ;
#109233 = CARTESIAN_POINT('Ctrl Pts',(66.7645038638689,246.361896476781,23.028378542832)) ;
#109234 = CARTESIAN_POINT('Ctrl Pts',(66.7727046558224,246.365650040328,22.8671042789749)) ;
#109235 = CARTESIAN_POINT('Ctrl Pts',(66.7788557938352,246.380187517667,22.7525145458225)) ;
#109236 = CARTESIAN_POINT('Ctrl Pts',(66.7879140723522,246.419358406331,22.5845248105605)) ;
#109237 = CARTESIAN_POINT('Ctrl Pts',(66.7908865423378,246.435222833392,22.5294168978723)) ;
#109238 = CARTESIAN_POINT('Ctrl Pts',(66.7947732274432,246.460589101807,22.4557286402266)) ;
#109239 = CARTESIAN_POINT('Ctrl Pts',(66.7957863875769,246.467660000436,22.4363558108457)) ;
#109240 = CARTESIAN_POINT('Ctrl Pts',(66.797576050284,246.481031886641,22.4017161359753)) ;
#109241 = CARTESIAN_POINT('Ctrl Pts',(66.798358657287,246.487203710612,22.3864046667242)) ;
#109242 = CARTESIAN_POINT('Ctrl Pts',(66.8003312840557,246.503576010695,22.3474551513525)) ;
#109243 = CARTESIAN_POINT('Ctrl Pts',(66.8015046235481,246.514096136701,22.3239566890586)) ;
#109244 = CARTESIAN_POINT('Ctrl Pts',(66.8041443689531,246.539424984486,22.2707018828668)) ;
#109245 = CARTESIAN_POINT('Ctrl Pts',(66.8055962555243,246.554585512081,22.2411245656152)) ;
#109246 = CARTESIAN_POINT('Ctrl Pts',(66.8111134378521,246.616348325701,22.1289668447959)) ;
#109247 = CARTESIAN_POINT('Ctrl Pts',(66.8150350209205,246.669039513265,22.0499424395502)) ;
#109248 = CARTESIAN_POINT('Ctrl Pts',(66.8218681372491,246.768756808877,21.9247972156988)) ;
#109249 = CARTESIAN_POINT('Ctrl Pts',(66.8247044336688,246.812324516317,21.8762188654033)) ;
#109250 = CARTESIAN_POINT('Ctrl Pts',(66.8291253105473,246.881868058254,21.8072218688268)) ;
#109251 = CARTESIAN_POINT('Ctrl Pts',(66.830629253651,246.9058002168,21.7848301163973)) ;
#109252 = CARTESIAN_POINT('Ctrl Pts',(66.8335062751651,246.951936980499,21.7441304954835)) ;
#109253 = CARTESIAN_POINT('Ctrl Pts',(66.8348723255865,246.97398682311,21.7256650951107)) ;
#109254 = CARTESIAN_POINT('Ctrl Pts',(66.8381689391688,247.0274643318,21.6831709195566)) ;
#109255 = CARTESIAN_POINT('Ctrl Pts',(66.840118057264,247.059287763348,21.6596697127395)) ;
#109256 = CARTESIAN_POINT('Ctrl Pts',(66.8444830759063,247.130995574921,21.6105337130148)) ;
#109257 = CARTESIAN_POINT('Ctrl Pts',(66.8469132559169,247.171195675123,21.5854206623276)) ;
#109258 = CARTESIAN_POINT('Ctrl Pts',(66.8542990423983,247.294686396303,21.5153631363168)) ;
#109259 = CARTESIAN_POINT('Ctrl Pts',(66.8593535462031,247.380767499731,21.4757276380051)) ;
#109260 = CARTESIAN_POINT('Ctrl Pts',(66.8667041686732,247.513376272754,21.4277747664925)) ;
#109261 = CARTESIAN_POINT('Ctrl Pts',(66.8690884760933,247.557663384699,21.4138081540797)) ;
#109262 = CARTESIAN_POINT('Ctrl Pts',(66.8723880681245,247.621744251482,21.3964868788731)) ;
#109263 = CARTESIAN_POINT('Ctrl Pts',(66.8733657184046,247.641105699513,21.3916224189345)) ;
#109264 = CARTESIAN_POINT('Ctrl Pts',(66.8751381584295,247.677023634178,21.3832767778421)) ;
#109265 = CARTESIAN_POINT('Ctrl Pts',(66.8759373524931,247.693553850535,21.3796984628091)) ;
#109266 = CARTESIAN_POINT('Ctrl Pts',(66.8780298931353,247.73763191715,21.3708523168368)) ;
#109267 = CARTESIAN_POINT('Ctrl Pts',(66.8793023530883,247.765263447124,21.3660240603119)) ;
#109268 = CARTESIAN_POINT('Ctrl Pts',(66.8822311821563,247.830297485916,21.356333759192)) ;
#109269 = CARTESIAN_POINT('Ctrl Pts',(66.8838681097253,247.86776892858,21.3520354644793)) ;
#109270 = CARTESIAN_POINT('Ctrl Pts',(66.8914009094704,248.042892544921,21.3379077512273)) ;
#109271 = CARTESIAN_POINT('Ctrl Pts',(66.8970665204552,248.18126848814,21.3438211107561)) ;
#109272 = CARTESIAN_POINT('Ctrl Pts',(66.9048506159575,248.353018815771,21.3725822466916)) ;
#109273 = CARTESIAN_POINT('Ctrl Pts',(66.9064955152177,248.388472650282,21.3797042202269)) ;
#109274 = CARTESIAN_POINT('Ctrl Pts',(66.9095037958456,248.451533646708,21.3945067215273)) ;
#109275 = CARTESIAN_POINT('Ctrl Pts',(66.9108538964968,248.47922678199,21.4017596296088)) ;
#109276 = CARTESIAN_POINT('Ctrl Pts',(66.9139175008519,248.540628767216,21.4195315302631)) ;
#109277 = CARTESIAN_POINT('Ctrl Pts',(66.9156416071258,248.574217745349,21.4304131944191)) ;
#109278 = CARTESIAN_POINT('Ctrl Pts',(66.9218759832484,248.692238902346,21.4728067195242)) ;
#109279 = CARTESIAN_POINT('Ctrl Pts',(66.9265555086629,248.774440746881,21.5100468643801)) ;
#109280 = CARTESIAN_POINT('Ctrl Pts',(66.9342921276663,248.902815547265,21.5811596995484)) ;
#109281 = CARTESIAN_POINT('Ctrl Pts',(66.9372988470437,248.950955657761,21.611108482509)) ;
#109282 = CARTESIAN_POINT('Ctrl Pts',(66.9402651077865,248.99748421711,21.6434318722943)) ;
#109283 = CARTESIAN_POINT('',(66.9402651077866,247.065925086493,21.6554848536836)) ;
#109284 = CARTESIAN_POINT('Origin',(66.9402651077866,248.040265107786,23.0213203435596)) ;
#109285 = CARTESIAN_POINT('Ctrl Pts',(66.9402651077869,247.065925086493,21.6554848536832)) ;
#109286 = CARTESIAN_POINT('Ctrl Pts',(66.9396667652069,247.055655376798,21.662810911057)) ;
#109287 = CARTESIAN_POINT('Ctrl Pts',(66.9390747274394,247.045468389277,21.6702527272938)) ;
#109288 = CARTESIAN_POINT('Ctrl Pts',(66.9377500820969,247.022652288243,21.6873183636409)) ;
#109289 = CARTESIAN_POINT('Ctrl Pts',(66.9370207683082,247.010073823175,21.6970080414531)) ;
#109290 = CARTESIAN_POINT('Ctrl Pts',(66.9305114561942,246.897933188338,21.7859590655746)) ;
#109291 = CARTESIAN_POINT('Ctrl Pts',(66.9251900559135,246.807547014657,21.8761346376893)) ;
#109292 = CARTESIAN_POINT('Ctrl Pts',(66.9176770011432,246.700047100627,22.0110211304123)) ;
#109293 = CARTESIAN_POINT('Ctrl Pts',(66.9156857672986,246.673312831565,22.0474979577537)) ;
#109294 = CARTESIAN_POINT('Ctrl Pts',(66.9119145015543,246.626500509914,22.1171021179088)) ;
#109295 = CARTESIAN_POINT('Ctrl Pts',(66.9101467604585,246.606033204961,22.1499309015644)) ;
#109296 = CARTESIAN_POINT('Ctrl Pts',(66.9069079117755,246.571355558215,22.2100890547301)) ;
#109297 = CARTESIAN_POINT('Ctrl Pts',(66.90545079394,246.556728440201,22.2371581847755)) ;
#109298 = CARTESIAN_POINT('Ctrl Pts',(66.9021015713666,246.525349759796,22.2992519276511)) ;
#109299 = CARTESIAN_POINT('Ctrl Pts',(66.9001962886567,246.509053389052,22.3344857903657)) ;
#109300 = CARTESIAN_POINT('Ctrl Pts',(66.8924653337291,246.449074523345,22.4769339858134)) ;
#109301 = CARTESIAN_POINT('Ctrl Pts',(66.8863507974608,246.415320799033,22.5879679183732)) ;
#109302 = CARTESIAN_POINT('Ctrl Pts',(66.8755249468204,246.376533100155,22.7877630291077)) ;
#109303 = CARTESIAN_POINT('Ctrl Pts',(66.8708568005199,246.366590976947,22.8751356895038)) ;
#109304 = CARTESIAN_POINT('Ctrl Pts',(66.8652862956974,246.362736369824,22.9857465047002)) ;
#109305 = CARTESIAN_POINT('Ctrl Pts',(66.8641530262041,246.362407267465,23.0086189873426)) ;
#109306 = CARTESIAN_POINT('Ctrl Pts',(66.8622491506825,246.362645058344,23.0478403303629)) ;
#109307 = CARTESIAN_POINT('Ctrl Pts',(66.8614679558607,246.362983098206,23.0641857098725)) ;
#109308 = CARTESIAN_POINT('Ctrl Pts',(66.8596284129968,246.364363324888,23.1032741773016)) ;
#109309 = CARTESIAN_POINT('Ctrl Pts',(66.8585808952561,246.365629514157,23.1260052564638)) ;
#109310 = CARTESIAN_POINT('Ctrl Pts',(66.8533778600519,246.374362107618,23.2406884841878)) ;
#109311 = CARTESIAN_POINT('Ctrl Pts',(66.8494973621617,246.388941443014,23.3319454566303)) ;
#109312 = CARTESIAN_POINT('Ctrl Pts',(66.841621769976,246.433320860933,23.5126133967525)) ;
#109313 = CARTESIAN_POINT('Ctrl Pts',(66.837636011074,246.463285368154,23.601641092563)) ;
#109314 = CARTESIAN_POINT('Ctrl Pts',(66.8319022845595,246.514031654486,23.7188964443653)) ;
#109315 = CARTESIAN_POINT('Ctrl Pts',(66.8303501366459,246.528480067574,23.7496793115379)) ;
#109316 = CARTESIAN_POINT('Ctrl Pts',(66.8274768431064,246.556383029008,23.8047147592589)) ;
#109317 = CARTESIAN_POINT('Ctrl Pts',(66.8261665734354,246.569522763633,23.829113438509)) ;
#109318 = CARTESIAN_POINT('Ctrl Pts',(66.8231597257058,246.60055188431,23.8834613867776)) ;
#109319 = CARTESIAN_POINT('Ctrl Pts',(66.8214515534895,246.618782828753,23.9131999631784)) ;
#109320 = CARTESIAN_POINT('Ctrl Pts',(66.8134162094592,246.707213717487,24.0478431595334)) ;
#109321 = CARTESIAN_POINT('Ctrl Pts',(66.8066933520668,246.788176496121,24.1451714051298)) ;
#109322 = CARTESIAN_POINT('Ctrl Pts',(66.7959645933761,246.933483548018,24.2844592372969)) ;
#109323 = CARTESIAN_POINT('Ctrl Pts',(66.7919836347308,246.991131322703,24.3327337132411)) ;
#109324 = CARTESIAN_POINT('Ctrl Pts',(66.7870684111828,247.069871480798,24.3901447279616)) ;
#109325 = CARTESIAN_POINT('Ctrl Pts',(66.7859595508096,247.088181865371,24.402943148782)) ;
#109326 = CARTESIAN_POINT('Ctrl Pts',(66.7841052750378,247.119875740253,24.4241668345064)) ;
#109327 = CARTESIAN_POINT('Ctrl Pts',(66.7833491088747,247.13313102736,24.4327744329739)) ;
#109328 = CARTESIAN_POINT('Ctrl Pts',(66.7816144860752,247.164292992633,24.4523897261082)) ;
#109329 = CARTESIAN_POINT('Ctrl Pts',(66.7806445405037,247.182288044758,24.4632503534813)) ;
#109330 = CARTESIAN_POINT('Ctrl Pts',(66.7784542596184,247.224061045493,24.4874027943518)) ;
#109331 = CARTESIAN_POINT('Ctrl Pts',(66.7772452853061,247.247964004995,24.5004570345183)) ;
#109332 = CARTESIAN_POINT('Ctrl Pts',(66.7760547678839,247.272170398758,24.5129220264705)) ;
#109333 = CARTESIAN_POINT('Origin',(67.8645744874958,248.040265107786,23.0213203435596)) ;
#109334 = CARTESIAN_POINT('',(66.1803112149446,247.2721703913,24.51292202263)) ;
#109335 = CARTESIAN_POINT('',(66.2786264835566,247.272170393047,24.5129220235297)) ;
#109336 = CARTESIAN_POINT('',(67.8645744874958,247.272170391302,24.5129220226314)) ;
#109337 = CARTESIAN_POINT('Ctrl Pts',(66.1803112149446,247.2721703913,24.51292202263)) ;
#109338 = CARTESIAN_POINT('Ctrl Pts',(66.1813433707766,247.252559808362,24.5028236261527)) ;
#109339 = CARTESIAN_POINT('Ctrl Pts',(66.1823542298636,247.233149391274,24.4923390118849)) ;
#109340 = CARTESIAN_POINT('Ctrl Pts',(66.1875253071974,247.133303961512,24.4358355602508)) ;
#109341 = CARTESIAN_POINT('Ctrl Pts',(66.1914076081278,247.056570630232,24.3835903719263)) ;
#109342 = CARTESIAN_POINT('Ctrl Pts',(66.1995787953728,246.905796268944,24.261518189032)) ;
#109343 = CARTESIAN_POINT('Ctrl Pts',(66.2038619131075,246.832992279066,24.1907650147767)) ;
#109344 = CARTESIAN_POINT('Ctrl Pts',(66.2099411111492,246.744806082918,24.0879948669146)) ;
#109345 = CARTESIAN_POINT('Ctrl Pts',(66.2114992468374,246.723388374238,24.0614376996361)) ;
#109346 = CARTESIAN_POINT('Ctrl Pts',(66.2144126350155,246.685628776196,24.0115798954605)) ;
#109347 = CARTESIAN_POINT('Ctrl Pts',(66.2157579827885,246.669041507144,23.9884807720735)) ;
#109348 = CARTESIAN_POINT('Ctrl Pts',(66.218866033917,246.632676359447,23.935022181925)) ;
#109349 = CARTESIAN_POINT('Ctrl Pts',(66.2206413827271,246.613279257904,23.9044218569684)) ;
#109350 = CARTESIAN_POINT('Ctrl Pts',(66.2274407600937,246.544086080448,23.7870250333236)) ;
#109351 = CARTESIAN_POINT('Ctrl Pts',(66.2326779323192,246.501100428625,23.6964675500411)) ;
#109352 = CARTESIAN_POINT('Ctrl Pts',(66.2426141220224,246.435905778428,23.5199613514512)) ;
#109353 = CARTESIAN_POINT('Ctrl Pts',(66.247282847654,246.411930371038,23.4350101637201)) ;
#109354 = CARTESIAN_POINT('Ctrl Pts',(66.2528474822375,246.390306964967,23.3262786015287)) ;
#109355 = CARTESIAN_POINT('Ctrl Pts',(66.2539707882866,246.386327819247,23.3039029805037)) ;
#109356 = CARTESIAN_POINT('Ctrl Pts',(66.2558609765731,246.380277271449,23.2653512480786)) ;
#109357 = CARTESIAN_POINT('Ctrl Pts',(66.2566381563459,246.377985074659,23.2492146791449)) ;
#109358 = CARTESIAN_POINT('Ctrl Pts',(66.2584759021051,246.373043953528,23.2103733257162)) ;
#109359 = CARTESIAN_POINT('Ctrl Pts',(66.2595253780448,246.370623215279,23.1876436573217)) ;
#109360 = CARTESIAN_POINT('Ctrl Pts',(66.2659164827693,246.358506598636,23.0465495853369)) ;
#109361 = CARTESIAN_POINT('Ctrl Pts',(66.2707929661402,246.360936047135,22.927473977817)) ;
#109362 = CARTESIAN_POINT('Ctrl Pts',(66.2781260976021,246.382782027693,22.7557049790287)) ;
#109363 = CARTESIAN_POINT('Ctrl Pts',(66.2804531518485,246.392260230318,22.7021319452076)) ;
#109364 = CARTESIAN_POINT('Ctrl Pts',(66.2847382334814,246.413891640272,22.6070559651377)) ;
#109365 = CARTESIAN_POINT('Ctrl Pts',(66.2866711898336,246.425078814962,22.5653833463018)) ;
#109366 = CARTESIAN_POINT('Ctrl Pts',(66.2899874852909,246.446471308085,22.4964287018514)) ;
#109367 = CARTESIAN_POINT('Ctrl Pts',(66.2913437830984,246.455803507772,22.4688972888353)) ;
#109368 = CARTESIAN_POINT('Ctrl Pts',(66.29420161315,246.476617878492,22.412366840157)) ;
#109369 = CARTESIAN_POINT('Ctrl Pts',(66.2957059918197,246.488202854992,22.3834178127161)) ;
#109370 = CARTESIAN_POINT('Ctrl Pts',(66.300114035265,246.523898489675,22.3009588805755)) ;
#109371 = CARTESIAN_POINT('Ctrl Pts',(66.3030796610631,246.55001708755,22.2483725592334)) ;
#109372 = CARTESIAN_POINT('Ctrl Pts',(66.3123282536655,246.638004823593,22.0923295861903)) ;
#109373 = CARTESIAN_POINT('Ctrl Pts',(66.3188137172501,246.708300127418,21.9940790822397)) ;
#109374 = CARTESIAN_POINT('Ctrl Pts',(66.3264318419567,246.806541128242,21.8839972401355)) ;
#109375 = CARTESIAN_POINT('Ctrl Pts',(66.3278142847729,246.825063353164,21.8642276482552)) ;
#109376 = CARTESIAN_POINT('Ctrl Pts',(66.3302898413743,246.859689241534,21.8290189006079)) ;
#109377 = CARTESIAN_POINT('Ctrl Pts',(66.3313906171093,246.875637679484,21.8134357692751)) ;
#109378 = CARTESIAN_POINT('Ctrl Pts',(66.3332585807155,246.903780084173,21.7870137658914)) ;
#109379 = CARTESIAN_POINT('Ctrl Pts',(66.3340352350746,246.915828982252,21.7760274591387)) ;
#109380 = CARTESIAN_POINT('Ctrl Pts',(66.3358929538339,246.945491779348,21.7497622702217)) ;
#109381 = CARTESIAN_POINT('Ctrl Pts',(66.3369620250232,246.963267069211,21.7346720269874)) ;
#109382 = CARTESIAN_POINT('Ctrl Pts',(66.3421462388854,247.052503339811,21.6620609139343)) ;
#109383 = CARTESIAN_POINT('Ctrl Pts',(66.3459917798339,247.128288778479,21.6100934858166)) ;
#109384 = CARTESIAN_POINT('Ctrl Pts',(66.3540036519011,247.293450909869,21.515727092631)) ;
#109385 = CARTESIAN_POINT('Ctrl Pts',(66.3581629994262,247.383086146486,21.4744988396476)) ;
#109386 = CARTESIAN_POINT('Ctrl Pts',(66.3641487966006,247.509119373181,21.4294723281427)) ;
#109387 = CARTESIAN_POINT('Ctrl Pts',(66.3657589138963,247.542791267655,21.418630267983)) ;
#109388 = CARTESIAN_POINT('Ctrl Pts',(66.3687211974726,247.604069326491,21.4010164909781)) ;
#109389 = CARTESIAN_POINT('Ctrl Pts',(66.3700611097827,247.631552937364,21.393866631955)) ;
#109390 = CARTESIAN_POINT('Ctrl Pts',(66.3731197439098,247.693679024002,21.3793774898711)) ;
#109391 = CARTESIAN_POINT('Ctrl Pts',(66.3748496628768,247.728398350681,21.3724306705407)) ;
#109392 = CARTESIAN_POINT('Ctrl Pts',(66.3823405135124,247.876925771365,21.3475714137341)) ;
#109393 = CARTESIAN_POINT('Ctrl Pts',(66.3884055174911,247.992186747832,21.3403093220466)) ;
#109394 = CARTESIAN_POINT('Ctrl Pts',(66.3985316136585,248.18381146681,21.347968023991)) ;
#109395 = CARTESIAN_POINT('Ctrl Pts',(66.4025633935918,248.260061519177,21.3562664659935)) ;
#109396 = CARTESIAN_POINT('Ctrl Pts',(66.4075384096676,248.357679684639,21.3737155420066)) ;
#109397 = CARTESIAN_POINT('Ctrl Pts',(66.4086526386034,248.379797239721,21.3781308796469)) ;
#109398 = CARTESIAN_POINT('Ctrl Pts',(66.4105339272271,248.417739280072,21.3865041217997)) ;
#109399 = CARTESIAN_POINT('Ctrl Pts',(66.4113109456865,248.43360583474,21.3902489357526)) ;
#109400 = CARTESIAN_POINT('Ctrl Pts',(66.4131569463465,248.471764108648,21.3998442741033)) ;
#109401 = CARTESIAN_POINT('Ctrl Pts',(66.4142144733173,248.493993974325,21.4059237248676)) ;
#109402 = CARTESIAN_POINT('Ctrl Pts',(66.4195273178358,248.606950080852,21.43933096478)) ;
#109403 = CARTESIAN_POINT('Ctrl Pts',(66.4234915730814,248.69537549886,21.4738529163656)) ;
#109404 = CARTESIAN_POINT('Ctrl Pts',(66.4316893608181,248.870019415013,21.5597043765571)) ;
#109405 = CARTESIAN_POINT('Ctrl Pts',(66.43591533074,248.955506052543,21.611658771381)) ;
#109406 = CARTESIAN_POINT('Ctrl Pts',(66.4419265758015,249.063261427622,21.691101416567)) ;
#109407 = CARTESIAN_POINT('Ctrl Pts',(66.4434818519492,249.090038813524,21.7121301917032)) ;
#109408 = CARTESIAN_POINT('Ctrl Pts',(66.4463928703559,249.13798156533,21.7521975657878)) ;
#109409 = CARTESIAN_POINT('Ctrl Pts',(66.44773884653,249.159337830941,21.7709883185167)) ;
#109410 = CARTESIAN_POINT('Ctrl Pts',(66.4508526923697,249.206857025458,21.8149921273443)) ;
#109411 = CARTESIAN_POINT('Ctrl Pts',(66.4526333823141,249.232698739022,21.8405298178118)) ;
#109412 = CARTESIAN_POINT('Ctrl Pts',(66.4590334921456,249.320937170429,21.9335828241501)) ;
#109413 = CARTESIAN_POINT('Ctrl Pts',(66.4638258052329,249.378590235261,22.0053593298391)) ;
#109414 = CARTESIAN_POINT('Ctrl Pts',(66.4721979422453,249.467482101721,22.1368109230564)) ;
#109415 = CARTESIAN_POINT('Ctrl Pts',(66.4757402991034,249.501557157053,22.1943190499528)) ;
#109416 = CARTESIAN_POINT('Ctrl Pts',(66.4812548747535,249.550300941525,22.289051986342)) ;
#109417 = CARTESIAN_POINT('Ctrl Pts',(66.483279816849,249.567227026516,22.3250353245085)) ;
#109418 = CARTESIAN_POINT('Ctrl Pts',(66.4861640374801,249.590167909187,22.3786759759734)) ;
#109419 = CARTESIAN_POINT('Ctrl Pts',(66.4870696114554,249.597191957824,22.3958850441892)) ;
#109420 = CARTESIAN_POINT('Ctrl Pts',(66.4887838818375,249.610176935599,22.429273835447)) ;
#109421 = CARTESIAN_POINT('Ctrl Pts',(66.4895943418289,249.616177078331,22.4454352076101)) ;
#109422 = CARTESIAN_POINT('Ctrl Pts',(66.491835433538,249.632321015476,22.4910619162574)) ;
#109423 = CARTESIAN_POINT('Ctrl Pts',(66.4932380895439,249.64189497613,22.5207227332288)) ;
#109424 = CARTESIAN_POINT('Ctrl Pts',(66.4965706464777,249.663072976935,22.5931796846697)) ;
#109425 = CARTESIAN_POINT('Ctrl Pts',(66.4984718910945,249.673817859092,22.6362028131126)) ;
#109426 = CARTESIAN_POINT('Ctrl Pts',(66.5059738419224,249.709820300481,22.8092605717972)) ;
#109427 = CARTESIAN_POINT('Ctrl Pts',(66.5114318524569,249.721346846575,22.9416488271284)) ;
#109428 = CARTESIAN_POINT('Ctrl Pts',(66.5189266491568,249.716089524742,23.1089522508896)) ;
#109429 = CARTESIAN_POINT('Ctrl Pts',(66.5205195603772,249.713900222963,23.1438443783018)) ;
#109430 = CARTESIAN_POINT('Ctrl Pts',(66.5234646076773,249.707961017773,23.2069039348667)) ;
#109431 = CARTESIAN_POINT('Ctrl Pts',(66.5248052370053,249.70458237105,23.2350932417736)) ;
#109432 = CARTESIAN_POINT('Ctrl Pts',(66.5278851467738,249.695329222162,23.2986100873906)) ;
#109433 = CARTESIAN_POINT('Ctrl Pts',(66.5296363786789,249.68903569244,23.3338617907631)) ;
#109434 = CARTESIAN_POINT('Ctrl Pts',(66.5355841613892,249.664291945331,23.4507131688029)) ;
#109435 = CARTESIAN_POINT('Ctrl Pts',(66.539919604221,249.640870750907,23.5311248654465)) ;
#109436 = CARTESIAN_POINT('Ctrl Pts',(66.5500777890073,249.573219509862,23.7118672785298)) ;
#109437 = CARTESIAN_POINT('Ctrl Pts',(66.5559297626788,249.524961690004,23.810295640799)) ;
#109438 = CARTESIAN_POINT('Ctrl Pts',(66.5624651069322,249.456263635375,23.9214577718262)) ;
#109439 = CARTESIAN_POINT('Ctrl Pts',(66.5635151307348,249.444715394716,23.9393719142512)) ;
#109440 = CARTESIAN_POINT('Ctrl Pts',(66.5653344144998,249.423717332963,23.9706210697346)) ;
#109441 = CARTESIAN_POINT('Ctrl Pts',(66.5661112394953,249.414409217415,23.9840455991035)) ;
#109442 = CARTESIAN_POINT('Ctrl Pts',(66.5680012349603,249.390925402805,24.0168801582264)) ;
#109443 = CARTESIAN_POINT('Ctrl Pts',(66.5691010007004,249.376526352373,24.0361250349577)) ;
#109444 = CARTESIAN_POINT('Ctrl Pts',(66.5715363590945,249.3431517713,24.0787887461828)) ;
#109445 = CARTESIAN_POINT('Ctrl Pts',(66.5728605366494,249.323948567457,24.1020191862595)) ;
#109446 = CARTESIAN_POINT('Ctrl Pts',(66.5774386753978,249.254434287927,24.1816427137725)) ;
#109447 = CARTESIAN_POINT('Ctrl Pts',(66.5805906138049,249.200948957556,24.2351442704249)) ;
#109448 = CARTESIAN_POINT('Ctrl Pts',(66.5871961043524,249.08309164241,24.3380992979809)) ;
#109449 = CARTESIAN_POINT('Ctrl Pts',(66.5906485378677,249.018376199185,24.3868574369339)) ;
#109450 = CARTESIAN_POINT('Ctrl Pts',(66.5958732170954,248.920036147092,24.4503599800255)) ;
#109451 = CARTESIAN_POINT('Ctrl Pts',(66.5975155661291,248.889049297604,24.468979335324)) ;
#109452 = CARTESIAN_POINT('Ctrl Pts',(66.6005105289135,248.83266991517,24.5004238283064)) ;
#109453 = CARTESIAN_POINT('Ctrl Pts',(66.6018494713179,248.807506669269,24.5136315614698)) ;
#109454 = CARTESIAN_POINT('Ctrl Pts',(66.6048715551597,248.750891062974,24.5415375405759)) ;
#109455 = CARTESIAN_POINT('Ctrl Pts',(66.6065645988116,248.719294019325,24.555911202305)) ;
#109456 = CARTESIAN_POINT('Ctrl Pts',(66.6102195017308,248.651369151631,24.5843019148011)) ;
#109457 = CARTESIAN_POINT('Ctrl Pts',(66.6121880085618,248.614953475018,24.5980551222346)) ;
#109458 = CARTESIAN_POINT('Ctrl Pts',(66.6182653362812,248.502830294328,24.636000476212)) ;
#109459 = CARTESIAN_POINT('Ctrl Pts',(66.622464789576,248.425855514463,24.656091673371)) ;
#109460 = CARTESIAN_POINT('Ctrl Pts',(66.6304919812157,248.276375435229,24.6839594030375)) ;
#109461 = CARTESIAN_POINT('Ctrl Pts',(66.6343105948735,248.204206445034,24.6926195689881)) ;
#109462 = CARTESIAN_POINT('Ctrl Pts',(66.6391644383837,248.107935743506,24.6978740064464)) ;
#109463 = CARTESIAN_POINT('Ctrl Pts',(66.6403442568994,248.084145184136,24.6986653106294)) ;
#109464 = CARTESIAN_POINT('Ctrl Pts',(66.6422929520108,248.044004342234,24.6991457608791)) ;
#109465 = CARTESIAN_POINT('Ctrl Pts',(66.6430741543972,248.027662126044,24.6991026082971)) ;
#109466 = CARTESIAN_POINT('Ctrl Pts',(66.6448756920634,247.989371233389,24.6984419333739)) ;
#109467 = CARTESIAN_POINT('Ctrl Pts',(66.6458867725033,247.967429763483,24.6976323981297)) ;
#109468 = CARTESIAN_POINT('Ctrl Pts',(66.6480805523382,247.919058359992,24.6948961249696)) ;
#109469 = CARTESIAN_POINT('Ctrl Pts',(66.6492552200846,247.892645265416,24.6927734398668)) ;
#109470 = CARTESIAN_POINT('Ctrl Pts',(66.6554023650222,247.752723802649,24.6781857982299)) ;
#109471 = CARTESIAN_POINT('Ctrl Pts',(66.6600807567697,247.640656613757,24.6547825211783)) ;
#109472 = CARTESIAN_POINT('Ctrl Pts',(66.6676940274392,247.471135374613,24.6008750044367)) ;
#109473 = CARTESIAN_POINT('Ctrl Pts',(66.670474229424,247.411591411855,24.5781344447023)) ;
#109474 = CARTESIAN_POINT('Ctrl Pts',(66.6747189934773,247.326034152191,24.539748667258)) ;
#109475 = CARTESIAN_POINT('Ctrl Pts',(66.6761026158922,247.298918886678,24.5266960604741)) ;
#109476 = CARTESIAN_POINT('Ctrl Pts',(66.6775101468938,247.272170391243,24.5129220226009)) ;
#109477 = CARTESIAN_POINT('Ctrl Pts',(66.7760547678839,247.272170398758,24.5129220264705)) ;
#109478 = CARTESIAN_POINT('Ctrl Pts',(66.7746260058025,247.30122094173,24.5278814949449)) ;
#109479 = CARTESIAN_POINT('Ctrl Pts',(66.7732237782137,247.330708514315,24.5419922776791)) ;
#109480 = CARTESIAN_POINT('Ctrl Pts',(66.7670524975973,247.463406236797,24.6007899101927)) ;
#109481 = CARTESIAN_POINT('Ctrl Pts',(66.7624140234548,247.57053297492,24.6358921340749)) ;
#109482 = CARTESIAN_POINT('Ctrl Pts',(66.7554925396234,247.72504518138,24.6698269201577)) ;
#109483 = CARTESIAN_POINT('Ctrl Pts',(66.7534508186818,247.770104091084,24.67780764622)) ;
#109484 = CARTESIAN_POINT('Ctrl Pts',(66.7500001725226,247.844744109367,24.6879011472955)) ;
#109485 = CARTESIAN_POINT('Ctrl Pts',(66.7486233362743,247.874155812901,24.6910890746417)) ;
#109486 = CARTESIAN_POINT('Ctrl Pts',(66.7457616483045,247.934415189029,24.6960127256743)) ;
#109487 = CARTESIAN_POINT('Ctrl Pts',(66.7442752550599,247.965257197395,24.6976772410028)) ;
#109488 = CARTESIAN_POINT('Ctrl Pts',(66.7400501988935,248.051591037136,24.6999493183941)) ;
#109489 = CARTESIAN_POINT('Ctrl Pts',(66.7372587974006,248.107089863153,24.6986566814682)) ;
#109490 = CARTESIAN_POINT('Ctrl Pts',(66.7281543674001,248.283881268916,24.6857505253967)) ;
#109491 = CARTESIAN_POINT('Ctrl Pts',(66.7216190595541,248.40400683852,24.663686267586)) ;
#109492 = CARTESIAN_POINT('Ctrl Pts',(66.7139415018536,248.546759586007,24.6210231980383)) ;
#109493 = CARTESIAN_POINT('Ctrl Pts',(66.7125546810463,248.572645306484,24.6125957164748)) ;
#109494 = CARTESIAN_POINT('Ctrl Pts',(66.7100703821569,248.619448747485,24.5960881203137)) ;
#109495 = CARTESIAN_POINT('Ctrl Pts',(66.7089653361317,248.640431553691,24.5882113930192)) ;
#109496 = CARTESIAN_POINT('Ctrl Pts',(66.7070853766348,248.676562264737,24.5738159593817)) ;
#109497 = CARTESIAN_POINT('Ctrl Pts',(66.7063011777376,248.691781978999,24.5674906154246)) ;
#109498 = CARTESIAN_POINT('Ctrl Pts',(66.7044104191885,248.72882797282,24.5514500199998)) ;
#109499 = CARTESIAN_POINT('Ctrl Pts',(66.7033166386824,248.75054399774,24.541491268422)) ;
#109500 = CARTESIAN_POINT('Ctrl Pts',(66.6991362639863,248.834155148673,24.5009649874613)) ;
#109501 = CARTESIAN_POINT('Ctrl Pts',(66.6961915715714,248.894356498031,24.4670515714953)) ;
#109502 = CARTESIAN_POINT('Ctrl Pts',(66.6898114863581,249.021057481715,24.3849925749504)) ;
#109503 = CARTESIAN_POINT('Ctrl Pts',(66.6863924717727,249.08646071182,24.3354855302863)) ;
#109504 = CARTESIAN_POINT('Ctrl Pts',(66.6811458698143,249.177639297353,24.2553317003306)) ;
#109505 = CARTESIAN_POINT('Ctrl Pts',(66.6794141458992,249.206363539487,24.2282247780209)) ;
#109506 = CARTESIAN_POINT('Ctrl Pts',(66.6760747774206,249.258751821425,24.175168608329)) ;
#109507 = CARTESIAN_POINT('Ctrl Pts',(66.6744757298295,249.282609669363,24.1494406778354)) ;
#109508 = CARTESIAN_POINT('Ctrl Pts',(66.6715180740521,249.324368770513,24.1014759530029)) ;
#109509 = CARTESIAN_POINT('Ctrl Pts',(66.6701709728188,249.342542641005,24.0794939918291)) ;
#109510 = CARTESIAN_POINT('Ctrl Pts',(66.6670727237618,249.382395269289,24.0287083108948)) ;
#109511 = CARTESIAN_POINT('Ctrl Pts',(66.6653094409075,249.40372325872,23.9996482675196)) ;
#109512 = CARTESIAN_POINT('Ctrl Pts',(66.658078213854,249.485809388289,23.8799003123941)) ;
#109513 = CARTESIAN_POINT('Ctrl Pts',(66.6523467487962,249.53858264882,23.7840769448208)) ;
#109514 = CARTESIAN_POINT('Ctrl Pts',(66.6422501659289,249.614112463005,23.6083454299327)) ;
#109515 = CARTESIAN_POINT('Ctrl Pts',(66.6379183902125,249.640966593167,23.5305847452125)) ;
#109516 = CARTESIAN_POINT('Ctrl Pts',(66.6327016987057,249.667660571226,23.4298718929731)) ;
#109517 = CARTESIAN_POINT('Ctrl Pts',(66.6316152393811,249.672884913724,23.4084676204684)) ;
#109518 = CARTESIAN_POINT('Ctrl Pts',(66.6297608359402,249.681244338317,23.3710327246674)) ;
#109519 = CARTESIAN_POINT('Ctrl Pts',(66.6289839721954,249.684569379557,23.355049392568)) ;
#109520 = CARTESIAN_POINT('Ctrl Pts',(66.6271101753576,249.692144048794,23.3157715865528)) ;
#109521 = CARTESIAN_POINT('Ctrl Pts',(66.6260259476179,249.696134776591,23.2924315848488)) ;
#109522 = CARTESIAN_POINT('Ctrl Pts',(66.6214111606782,249.711276519546,23.190993044962)) ;
#109523 = CARTESIAN_POINT('Ctrl Pts',(66.6180740139388,249.717406403861,23.1122421198656)) ;
#109524 = CARTESIAN_POINT('Ctrl Pts',(66.6115603529938,249.718514756525,22.9576382593858)) ;
#109525 = CARTESIAN_POINT('Ctrl Pts',(66.6083892208669,249.71393207545,22.8819797664537)) ;
#109526 = CARTESIAN_POINT('Ctrl Pts',(66.6034630176377,249.699392269194,22.7691492301083)) ;
#109527 = CARTESIAN_POINT('Ctrl Pts',(66.6017904699721,249.693246119073,22.7315846184465)) ;
#109528 = CARTESIAN_POINT('Ctrl Pts',(66.5985513916876,249.679171002658,22.6607668524994)) ;
#109529 = CARTESIAN_POINT('Ctrl Pts',(66.5969923996442,249.671492795986,22.6274835724027)) ;
#109530 = CARTESIAN_POINT('Ctrl Pts',(66.5940856369422,249.655608301905,22.5671051469266)) ;
#109531 = CARTESIAN_POINT('Ctrl Pts',(66.5927480954021,249.647721712694,22.5399387580991)) ;
#109532 = CARTESIAN_POINT('Ctrl Pts',(66.5896718865396,249.628322388765,22.4789212221474)) ;
#109533 = CARTESIAN_POINT('Ctrl Pts',(66.5879211814873,249.616406993283,22.4452133534045)) ;
#109534 = CARTESIAN_POINT('Ctrl Pts',(66.5807965439382,249.564502251018,22.3120751267256)) ;
#109535 = CARTESIAN_POINT('Ctrl Pts',(66.5751680679827,249.516108225971,22.2162053244757)) ;
#109536 = CARTESIAN_POINT('Ctrl Pts',(66.5650278432338,249.413677381476,22.0539720887832)) ;
#109537 = CARTESIAN_POINT('Ctrl Pts',(66.5605501432138,249.363078582201,21.9858542324839)) ;
#109538 = CARTESIAN_POINT('Ctrl Pts',(66.5552205830076,249.29331441755,21.9054421131403)) ;
#109539 = CARTESIAN_POINT('Ctrl Pts',(66.554149583085,249.278763246229,21.8893136128457)) ;
#109540 = CARTESIAN_POINT('Ctrl Pts',(66.5523123682857,249.252761508665,21.861595069506)) ;
#109541 = CARTESIAN_POINT('Ctrl Pts',(66.5515377065103,249.241449043364,21.8498821635411)) ;
#109542 = CARTESIAN_POINT('Ctrl Pts',(66.5496598646258,249.213180120709,21.8214527612052)) ;
#109543 = CARTESIAN_POINT('Ctrl Pts',(66.5485697281867,249.196035492092,21.8049294698952)) ;
#109544 = CARTESIAN_POINT('Ctrl Pts',(66.5443833462662,249.127675848237,21.7417979802871)) ;
#109545 = CARTESIAN_POINT('Ctrl Pts',(66.5414308997888,249.073944433215,21.6980109000327)) ;
#109546 = CARTESIAN_POINT('Ctrl Pts',(66.5350558600926,248.951295785619,21.6101029699729)) ;
#109547 = CARTESIAN_POINT('Ctrl Pts',(66.5316491198968,248.881550375901,21.5674461356559)) ;
#109548 = CARTESIAN_POINT('Ctrl Pts',(66.5257699369946,248.760598629428,21.5050989736082)) ;
#109549 = CARTESIAN_POINT('Ctrl Pts',(66.5233696573372,248.711036569657,21.482530982679)) ;
#109550 = CARTESIAN_POINT('Ctrl Pts',(66.5195002956231,248.632002613909,21.451087786692)) ;
#109551 = CARTESIAN_POINT('Ctrl Pts',(66.518083865029,248.603234035771,21.4405454038247)) ;
#109552 = CARTESIAN_POINT('Ctrl Pts',(66.515260050051,248.546341212787,21.4214468374385)) ;
#109553 = CARTESIAN_POINT('Ctrl Pts',(66.5138551748204,248.51824881191,21.4128304580471)) ;
#109554 = CARTESIAN_POINT('Ctrl Pts',(66.5102218867648,248.44620808186,21.3927883669801)) ;
#109555 = CARTESIAN_POINT('Ctrl Pts',(66.5079632221664,248.401997377095,21.3824013663251)) ;
#109556 = CARTESIAN_POINT('Ctrl Pts',(66.5000030746146,248.247989208181,21.3527535525927)) ;
#109557 = CARTESIAN_POINT('Ctrl Pts',(66.4940715821999,248.136735613736,21.3426440522411)) ;
#109558 = CARTESIAN_POINT('Ctrl Pts',(66.4850479824135,247.965100932978,21.3441735386682)) ;
#109559 = CARTESIAN_POINT('Ctrl Pts',(66.4819158122742,247.904955690021,21.3479514935566)) ;
#109560 = CARTESIAN_POINT('Ctrl Pts',(66.4778460981594,247.824085839844,21.3574210153989)) ;
#109561 = CARTESIAN_POINT('Ctrl Pts',(66.4768021572404,247.803078659241,21.3602853912995)) ;
#109562 = CARTESIAN_POINT('Ctrl Pts',(66.4749879001035,247.765964581455,21.3660644842077)) ;
#109563 = CARTESIAN_POINT('Ctrl Pts',(66.4742102736576,247.749837354732,21.3688178530435)) ;
#109564 = CARTESIAN_POINT('Ctrl Pts',(66.4723095312937,247.709904599137,21.3762381893585)) ;
#109565 = CARTESIAN_POINT('Ctrl Pts',(66.4712002280521,247.686155827551,21.3811861789226)) ;
#109566 = CARTESIAN_POINT('Ctrl Pts',(66.4687383944685,247.632770014284,21.3935226772839)) ;
#109567 = CARTESIAN_POINT('Ctrl Pts',(66.4673976724533,247.603210410797,21.4012089825697)) ;
#109568 = CARTESIAN_POINT('Ctrl Pts',(66.4627079699437,247.499121090916,21.4313314980471)) ;
#109569 = CARTESIAN_POINT('Ctrl Pts',(66.4594658248662,247.425959780457,21.4581405427182)) ;
#109570 = CARTESIAN_POINT('Ctrl Pts',(66.4528733965416,247.28353497792,21.5218799962939)) ;
#109571 = CARTESIAN_POINT('Ctrl Pts',(66.4495295860475,247.214472648948,21.5587788630213)) ;
#109572 = CARTESIAN_POINT('Ctrl Pts',(66.4444322179629,247.117795631709,21.6194690087539)) ;
#109573 = CARTESIAN_POINT('Ctrl Pts',(66.4427980899802,247.087975658428,21.6395527437328)) ;
#109574 = CARTESIAN_POINT('Ctrl Pts',(66.4398120180902,247.035791991214,21.6771904005733)) ;
#109575 = CARTESIAN_POINT('Ctrl Pts',(66.43847339613,247.0131856024,21.6943843531252)) ;
#109576 = CARTESIAN_POINT('Ctrl Pts',(66.4354443339418,246.963835150169,21.733936192661)) ;
#109577 = CARTESIAN_POINT('Ctrl Pts',(66.4337437102941,246.937329989998,21.7565700436083)) ;
#109578 = CARTESIAN_POINT('Ctrl Pts',(66.4273404585247,246.841945861539,21.8433023262077)) ;
#109579 = CARTESIAN_POINT('Ctrl Pts',(66.4224481469518,246.777795351718,21.9123287626435)) ;
#109580 = CARTESIAN_POINT('Ctrl Pts',(66.4122562516643,246.658570100657,22.0644466034939)) ;
#109581 = CARTESIAN_POINT('Ctrl Pts',(66.4069702007148,246.604412402534,22.1478118410557)) ;
#109582 = CARTESIAN_POINT('Ctrl Pts',(66.4008579163586,246.547354882143,22.2554387607092)) ;
#109583 = CARTESIAN_POINT('Ctrl Pts',(66.3997413969471,246.537176004263,22.2756134471926)) ;
#109584 = CARTESIAN_POINT('Ctrl Pts',(66.3978583437663,246.520364381107,22.3106782134209)) ;
#109585 = CARTESIAN_POINT('Ctrl Pts',(66.3970817493275,246.513536043084,22.3254691703481)) ;
#109586 = CARTESIAN_POINT('Ctrl Pts',(66.3952399503525,246.49760490167,22.361341806325)) ;
#109587 = CARTESIAN_POINT('Ctrl Pts',(66.3941860552735,246.488717625122,22.3825146784016)) ;
#109588 = CARTESIAN_POINT('Ctrl Pts',(66.3918760824001,246.469873282128,22.4301247473335)) ;
#109589 = CARTESIAN_POINT('Ctrl Pts',(66.3906296235424,246.460143549805,22.4566445995034)) ;
#109590 = CARTESIAN_POINT('Ctrl Pts',(66.3865342775035,246.429954626768,22.5458314235494)) ;
#109591 = CARTESIAN_POINT('Ctrl Pts',(66.3837671257855,246.41251838099,22.6094578036103)) ;
#109592 = CARTESIAN_POINT('Ctrl Pts',(66.3770678641161,246.379587455675,22.7650616052376)) ;
#109593 = CARTESIAN_POINT('Ctrl Pts',(66.3731309786512,246.367925485131,22.85762042588)) ;
#109594 = CARTESIAN_POINT('Ctrl Pts',(66.3673624905043,246.362473781355,22.9869567235963)) ;
#109595 = CARTESIAN_POINT('Ctrl Pts',(66.365714524909,246.36212312572,23.0232883115724)) ;
#109596 = CARTESIAN_POINT('Ctrl Pts',(66.3627155375746,246.36360030673,23.088012219576)) ;
#109597 = CARTESIAN_POINT('Ctrl Pts',(66.3613785083754,246.364970439127,23.1164009524269)) ;
#109598 = CARTESIAN_POINT('Ctrl Pts',(66.3583956892156,246.369560152878,23.1786237154051)) ;
#109599 = CARTESIAN_POINT('Ctrl Pts',(66.356741295661,246.373088024749,23.2124218230698)) ;
#109600 = CARTESIAN_POINT('Ctrl Pts',(66.3502387329908,246.390670619754,23.342481683184)) ;
#109601 = CARTESIAN_POINT('Ctrl Pts',(66.345181320729,246.412058631375,23.4375493679102)) ;
#109602 = CARTESIAN_POINT('Ctrl Pts',(66.3348658700508,246.471383231633,23.6239178409833)) ;
#109603 = CARTESIAN_POINT('Ctrl Pts',(66.3296285504755,246.50938998515,23.7148166169628)) ;
#109604 = CARTESIAN_POINT('Ctrl Pts',(66.3235545872295,246.565691239186,23.821939633711)) ;
#109605 = CARTESIAN_POINT('Ctrl Pts',(66.3224336160856,246.576648060666,23.8417986001987)) ;
#109606 = CARTESIAN_POINT('Ctrl Pts',(66.3205462347099,246.596160543956,23.8755289644073)) ;
#109607 = CARTESIAN_POINT('Ctrl Pts',(66.3197695962981,246.604521011534,23.889507700196)) ;
#109608 = CARTESIAN_POINT('Ctrl Pts',(66.3179319715617,246.62510505987,23.9228134787423)) ;
#109609 = CARTESIAN_POINT('Ctrl Pts',(66.3168821103347,246.637522289801,23.9420160084296)) ;
#109610 = CARTESIAN_POINT('Ctrl Pts',(66.312503861122,246.691857407885,24.0223898010052)) ;
#109611 = CARTESIAN_POINT('Ctrl Pts',(66.3093487905346,246.737416069323,24.0810039240524)) ;
#109612 = CARTESIAN_POINT('Ctrl Pts',(66.3012494422756,246.86493954656,24.2243623970562)) ;
#109613 = CARTESIAN_POINT('Ctrl Pts',(66.2963437600446,246.952205316677,24.3038275948203)) ;
#109614 = CARTESIAN_POINT('Ctrl Pts',(66.2895040320248,247.075373183139,24.3942959719754)) ;
#109615 = CARTESIAN_POINT('Ctrl Pts',(66.2879041695097,247.104323067194,24.414191768733)) ;
#109616 = CARTESIAN_POINT('Ctrl Pts',(66.2849523246596,247.157763036749,24.4484997266618)) ;
#109617 = CARTESIAN_POINT('Ctrl Pts',(66.2836121503365,247.182035619835,24.4632263496245)) ;
#109618 = CARTESIAN_POINT('Ctrl Pts',(66.2810583911226,247.228238561312,24.4896785004803)) ;
#109619 = CARTESIAN_POINT('Ctrl Pts',(66.2798502066838,247.250077654912,24.5015454505323)) ;
#109620 = CARTESIAN_POINT('Ctrl Pts',(66.2786264835566,247.272170393047,24.5129220235297)) ;
#109621 = CARTESIAN_POINT('Origin',(67.8645744874958,248.040265107786,23.0213203435596)) ;
#109622 = CARTESIAN_POINT('',(65.6787784786721,247.273150902455,24.5110052762898)) ;
#109623 = CARTESIAN_POINT('',(65.7773991381782,247.271019322241,24.5151747855319)) ;
#109624 = CARTESIAN_POINT('',(67.8645744874958,247.272170391302,24.5129220226314)) ;
#109625 = CARTESIAN_POINT('',(66.0159551384008,249.720171106522,23.0220506151371)) ;
#109626 = CARTESIAN_POINT('Ctrl Pts',(66.0159551384008,249.720171106522,23.0220506151371)) ;
#109627 = CARTESIAN_POINT('Ctrl Pts',(65.9924478890589,249.717352510068,22.5280345358421)) ;
#109628 = CARTESIAN_POINT('Ctrl Pts',(65.9431670940094,249.230820605579,21.4875383102286)) ;
#109629 = CARTESIAN_POINT('Ctrl Pts',(65.8681127532527,247.483588425899,21.135600117915)) ;
#109630 = CARTESIAN_POINT('Ctrl Pts',(65.7907921161305,246.169079052195,22.4175852103976)) ;
#109631 = CARTESIAN_POINT('Ctrl Pts',(65.7276806912704,246.428124491481,23.8937448247901)) ;
#109632 = CARTESIAN_POINT('Ctrl Pts',(65.6903428121175,247.05537004442,24.3995509628447)) ;
#109633 = CARTESIAN_POINT('Ctrl Pts',(65.6787784786721,247.273150902455,24.5110052762898)) ;
#109634 = CARTESIAN_POINT('Ctrl Pts',(66.017195723299,249.718014971169,23.0219974094422)) ;
#109635 = CARTESIAN_POINT('Ctrl Pts',(66.0183307318067,249.718006022754,23.0441713249733)) ;
#109636 = CARTESIAN_POINT('Ctrl Pts',(66.0194529908537,249.717557483142,23.0663438085581)) ;
#109637 = CARTESIAN_POINT('Ctrl Pts',(66.021465334691,249.715940060581,23.1067040054386)) ;
#109638 = CARTESIAN_POINT('Ctrl Pts',(66.0223609644086,249.714914173444,23.1248938511936)) ;
#109639 = CARTESIAN_POINT('Ctrl Pts',(66.0239984203668,249.712457011443,23.1586667450493)) ;
#109640 = CARTESIAN_POINT('Ctrl Pts',(66.0247434850627,249.711103734731,23.1742520498825)) ;
#109641 = CARTESIAN_POINT('Ctrl Pts',(66.0265597681603,249.70721549077,23.2127720293691)) ;
#109642 = CARTESIAN_POINT('Ctrl Pts',(66.0276184783189,249.704425149736,23.2356769875758)) ;
#109643 = CARTESIAN_POINT('Ctrl Pts',(66.0328458013089,249.688038012043,23.3504224814466)) ;
#109644 = CARTESIAN_POINT('Ctrl Pts',(66.0367357202072,249.667306265743,23.4410863473143)) ;
#109645 = CARTESIAN_POINT('Ctrl Pts',(66.0449183114521,249.608454766642,23.626226805628)) ;
#109646 = CARTESIAN_POINT('Ctrl Pts',(66.0492050618568,249.569032217515,23.7198903405972)) ;
#109647 = CARTESIAN_POINT('Ctrl Pts',(66.0552895113974,249.505360238047,23.8395543279455)) ;
#109648 = CARTESIAN_POINT('Ctrl Pts',(66.0568488359026,249.488408110045,23.8691954879158)) ;
#109649 = CARTESIAN_POINT('Ctrl Pts',(66.0597632646483,249.45570255263,23.9225363415388)) ;
#109650 = CARTESIAN_POINT('Ctrl Pts',(66.0611084086615,249.440227748398,23.9463921930167)) ;
#109651 = CARTESIAN_POINT('Ctrl Pts',(66.0642142910449,249.403697978,23.9996889655832)) ;
#109652 = CARTESIAN_POINT('Ctrl Pts',(66.0659876070543,249.382281997893,24.0288642802643)) ;
#109653 = CARTESIAN_POINT('Ctrl Pts',(66.0721834043994,249.305597893543,24.1265455949657)) ;
#109654 = CARTESIAN_POINT('Ctrl Pts',(66.0767615615587,249.245898013545,24.1913787261678)) ;
#109655 = CARTESIAN_POINT('Ctrl Pts',(66.0850758752835,249.130282496361,24.2986490598222)) ;
#109656 = CARTESIAN_POINT('Ctrl Pts',(66.0887786124962,249.076262594256,24.3428407015681)) ;
#109657 = CARTESIAN_POINT('Ctrl Pts',(66.0938953160846,248.996084900296,24.4004852683806)) ;
#109658 = CARTESIAN_POINT('Ctrl Pts',(66.0953822343774,248.972083987731,24.4168134712521)) ;
#109659 = CARTESIAN_POINT('Ctrl Pts',(66.0980191405281,248.927983240968,24.4451705569346)) ;
#109660 = CARTESIAN_POINT('Ctrl Pts',(66.0991783383882,248.908032119533,24.4574169362175)) ;
#109661 = CARTESIAN_POINT('Ctrl Pts',(66.1011048873075,248.873756109275,24.4774809717395)) ;
#109662 = CARTESIAN_POINT('Ctrl Pts',(66.1018838491254,248.859562755676,24.4855137853536)) ;
#109663 = CARTESIAN_POINT('Ctrl Pts',(66.1036754997755,248.826121581469,24.5038014164912)) ;
#109664 = CARTESIAN_POINT('Ctrl Pts',(66.1046791770869,248.806787291003,24.5138900564829)) ;
#109665 = CARTESIAN_POINT('Ctrl Pts',(66.1110360019845,248.681024783047,24.5764244379773)) ;
#109666 = CARTESIAN_POINT('Ctrl Pts',(66.1159123410292,248.569475347406,24.6178363717818)) ;
#109667 = CARTESIAN_POINT('Ctrl Pts',(66.1232769014826,248.400841243134,24.6608001380958)) ;
#109668 = CARTESIAN_POINT('Ctrl Pts',(66.125642992403,248.346558997878,24.6718029448756)) ;
#109669 = CARTESIAN_POINT('Ctrl Pts',(66.1299885237556,248.248709121012,24.6866427419714)) ;
#109670 = CARTESIAN_POINT('Ctrl Pts',(66.1319415846934,248.205347785647,24.6914984695287)) ;
#109671 = CARTESIAN_POINT('Ctrl Pts',(66.1352812621692,248.132794340044,24.696770130613)) ;
#109672 = CARTESIAN_POINT('Ctrl Pts',(66.1366398584891,248.103691522083,24.6981240347842)) ;
#109673 = CARTESIAN_POINT('Ctrl Pts',(66.1394930739171,248.043532547513,24.6993543303389)) ;
#109674 = CARTESIAN_POINT('Ctrl Pts',(66.140990222113,248.012485630232,24.6991275100511)) ;
#109675 = CARTESIAN_POINT('Ctrl Pts',(66.1453372502987,247.923879381478,24.6960201650657)) ;
#109676 = CARTESIAN_POINT('Ctrl Pts',(66.1482462447078,247.866441389921,24.6910357596945)) ;
#109677 = CARTESIAN_POINT('Ctrl Pts',(66.1574990457002,247.688730677397,24.6663447055157)) ;
#109678 = CARTESIAN_POINT('Ctrl Pts',(66.1640580625483,247.570277716357,24.636495508201)) ;
#109679 = CARTESIAN_POINT('Ctrl Pts',(66.1717533023906,247.430598429913,24.5846155480122)) ;
#109680 = CARTESIAN_POINT('Ctrl Pts',(66.1731423478088,247.405325839823,24.5745227103385)) ;
#109681 = CARTESIAN_POINT('Ctrl Pts',(66.1756281601356,247.35974615837,24.5550215057614)) ;
#109682 = CARTESIAN_POINT('Ctrl Pts',(66.1767326836644,247.339360362305,24.5458130193764)) ;
#109683 = CARTESIAN_POINT('Ctrl Pts',(66.1786043328474,247.304442562548,24.5291917141201)) ;
#109684 = CARTESIAN_POINT('Ctrl Pts',(66.1793810626801,247.289824813099,24.5219702977892)) ;
#109685 = CARTESIAN_POINT('Ctrl Pts',(66.1802009438783,247.274264917999,24.5139991966942)) ;
#109686 = CARTESIAN_POINT('Ctrl Pts',(66.1802561097733,247.273217369381,24.5134611600847)) ;
#109687 = CARTESIAN_POINT('Ctrl Pts',(66.1803112149446,247.2721703913,24.51292202263)) ;
#109688 = CARTESIAN_POINT('',(66.1145741302299,249.716961070455,23.0201358258391)) ;
#109689 = CARTESIAN_POINT('Ctrl Pts',(66.2786264835566,247.272170393047,24.5129220235297)) ;
#109690 = CARTESIAN_POINT('Ctrl Pts',(66.2780959412381,247.281748648333,24.5178543103196)) ;
#109691 = CARTESIAN_POINT('Ctrl Pts',(66.2775624890064,247.291374580145,24.5226944240961)) ;
#109692 = CARTESIAN_POINT('Ctrl Pts',(66.2729300042456,247.374926310296,24.5637023836631)) ;
#109693 = CARTESIAN_POINT('Ctrl Pts',(66.2686688738934,247.451366986508,24.5944747791049)) ;
#109694 = CARTESIAN_POINT('Ctrl Pts',(66.2587731205218,247.630559375766,24.6517146979187)) ;
#109695 = CARTESIAN_POINT('Ctrl Pts',(66.2531111661463,247.734191361197,24.6743069365427)) ;
#109696 = CARTESIAN_POINT('Ctrl Pts',(66.2465757706648,247.863019263849,24.6898531020637)) ;
#109697 = CARTESIAN_POINT('Ctrl Pts',(66.2453890978721,247.886835529114,24.6922114595139)) ;
#109698 = CARTESIAN_POINT('Ctrl Pts',(66.2434342945908,247.926972257001,24.6953204415881)) ;
#109699 = CARTESIAN_POINT('Ctrl Pts',(66.242653548385,247.943266761729,24.6963436184616)) ;
#109700 = CARTESIAN_POINT('Ctrl Pts',(66.2408608095576,247.981319477784,24.6981758461444)) ;
#109701 = CARTESIAN_POINT('Ctrl Pts',(66.2398577550726,248.003082770755,24.6987995578256)) ;
#109702 = CARTESIAN_POINT('Ctrl Pts',(66.2350509636585,248.109181875366,24.699774251177)) ;
#109703 = CARTESIAN_POINT('Ctrl Pts',(66.2314849324052,248.193456178054,24.6941896580212)) ;
#109704 = CARTESIAN_POINT('Ctrl Pts',(66.2234132367607,248.383057119953,24.6671709658645)) ;
#109705 = CARTESIAN_POINT('Ctrl Pts',(66.2189212295562,248.487460871254,24.6419205868222)) ;
#109706 = CARTESIAN_POINT('Ctrl Pts',(66.2125422512741,248.622542624032,24.5951937602889)) ;
#109707 = CARTESIAN_POINT('Ctrl Pts',(66.2109172226369,248.655964213954,24.5824222134172)) ;
#109708 = CARTESIAN_POINT('Ctrl Pts',(66.2079415574842,248.715144469431,24.5576112039242)) ;
#109709 = CARTESIAN_POINT('Ctrl Pts',(66.2066038915539,248.741053969619,24.5459667350772)) ;
#109710 = CARTESIAN_POINT('Ctrl Pts',(66.2035962932795,248.797705710801,24.5187566179239)) ;
#109711 = CARTESIAN_POINT('Ctrl Pts',(66.2019168993095,248.828288674192,24.5028905640462)) ;
#109712 = CARTESIAN_POINT('Ctrl Pts',(66.1954817284678,248.94153181943,24.4396428293417)) ;
#109713 = CARTESIAN_POINT('Ctrl Pts',(66.1905288118633,249.020587385653,24.3861958647092)) ;
#109714 = CARTESIAN_POINT('Ctrl Pts',(66.1802806195899,249.171752811789,24.2640593751003)) ;
#109715 = CARTESIAN_POINT('Ctrl Pts',(66.1750012444952,249.243165919496,24.1950733020853)) ;
#109716 = CARTESIAN_POINT('Ctrl Pts',(66.1688944934997,249.322877015503,24.1031070800742)) ;
#109717 = CARTESIAN_POINT('Ctrl Pts',(66.1677776148412,249.337333631833,24.0857305937707)) ;
#109718 = CARTESIAN_POINT('Ctrl Pts',(66.1658941588295,249.36159977872,24.0553344506698)) ;
#109719 = CARTESIAN_POINT('Ctrl Pts',(66.16511750987,249.371577815513,24.0424554945693)) ;
#109720 = CARTESIAN_POINT('Ctrl Pts',(66.1632757834583,249.395161333476,24.0110820600265)) ;
#109721 = CARTESIAN_POINT('Ctrl Pts',(66.1622220061168,249.408577416785,23.9924503814133)) ;
#109722 = CARTESIAN_POINT('Ctrl Pts',(66.1576468161301,249.466135375677,23.9089543776519)) ;
#109723 = CARTESIAN_POINT('Ctrl Pts',(66.1543207900658,249.506081012181,23.8413116154289)) ;
#109724 = CARTESIAN_POINT('Ctrl Pts',(66.1462641006527,249.59146658526,23.6703937581057)) ;
#109725 = CARTESIAN_POINT('Ctrl Pts',(66.1415556208221,249.631517182786,23.5648621199517)) ;
#109726 = CARTESIAN_POINT('Ctrl Pts',(66.1349394962132,249.669851065968,23.4219984157488)) ;
#109727 = CARTESIAN_POINT('Ctrl Pts',(66.1333309432536,249.677926693574,23.3875957153835)) ;
#109728 = CARTESIAN_POINT('Ctrl Pts',(66.1303708693538,249.690520215476,23.3251437116456)) ;
#109729 = CARTESIAN_POINT('Ctrl Pts',(66.1290315545452,249.695423342456,23.2971856461358)) ;
#109730 = CARTESIAN_POINT('Ctrl Pts',(66.1263670620569,249.703631006821,23.2422238340263)) ;
#109731 = CARTESIAN_POINT('Ctrl Pts',(66.1250440486545,249.70699260088,23.2152374125494)) ;
#109732 = CARTESIAN_POINT('Ctrl Pts',(66.1209327491675,249.71527946995,23.1323282828555)) ;
#109733 = CARTESIAN_POINT('Ctrl Pts',(66.118085034826,249.718055118912,23.0762344201526)) ;
#109734 = CARTESIAN_POINT('Ctrl Pts',(66.1151815854425,249.718014672093,23.0201112243472)) ;
#109735 = CARTESIAN_POINT('Ctrl Pts',(66.1145741302299,249.716961070455,23.0201358258391)) ;
#109736 = CARTESIAN_POINT('Ctrl Pts',(66.1062954533008,249.718173463304,22.8452907521841)) ;
#109737 = CARTESIAN_POINT('Ctrl Pts',(66.0722432306643,249.614025132092,22.1275182747943)) ;
#109738 = CARTESIAN_POINT('Ctrl Pts',(66.0124174623205,248.596941784018,21.1356001370716)) ;
#109739 = CARTESIAN_POINT('Ctrl Pts',(65.9350968251983,246.796951235849,21.4981652426359)) ;
#109740 = CARTESIAN_POINT('Ctrl Pts',(65.8577761880761,246.081263858291,23.1890860546867)) ;
#109741 = CARTESIAN_POINT('Ctrl Pts',(65.8052102924027,246.756193730657,24.2391790716563)) ;
#109742 = CARTESIAN_POINT('Ctrl Pts',(65.7784179424368,247.25196421432,24.5054393601585)) ;
#109743 = CARTESIAN_POINT('Ctrl Pts',(65.7773991381782,247.271019322241,24.5151747855319)) ;
#109744 = CARTESIAN_POINT('Origin',(67.8645744874958,248.040265107786,23.0213203435596)) ;
#109745 = CARTESIAN_POINT('',(65.1788202510297,247.272170391302,24.5129220226313)) ;
#109746 = CARTESIAN_POINT('',(65.2787248749179,247.272170391302,24.5129220226314)) ;
#109747 = CARTESIAN_POINT('',(67.8645744874958,247.272170391302,24.5129220226314)) ;
#109748 = CARTESIAN_POINT('',(65.5159557280774,249.717822745899,23.0208879934084)) ;
#109749 = CARTESIAN_POINT('Ctrl Pts',(65.5159557280774,249.718015052066,23.0208879438461)) ;
#109750 = CARTESIAN_POINT('Ctrl Pts',(65.5128383103028,249.717998033866,22.9548557931966)) ;
#109751 = CARTESIAN_POINT('Ctrl Pts',(65.5097208925282,249.714078457698,22.8889248391981)) ;
#109752 = CARTESIAN_POINT('Ctrl Pts',(65.5066034747536,249.706317429151,22.8235459140342)) ;
#109753 = CARTESIAN_POINT('Ctrl Pts',(65.5034791103217,249.698539106417,22.7580213025946)) ;
#109754 = CARTESIAN_POINT('Ctrl Pts',(65.5003547458898,249.686902320308,22.6930515529353)) ;
#109755 = CARTESIAN_POINT('Ctrl Pts',(65.4972303814579,249.671519178825,22.6290765185997)) ;
#109756 = CARTESIAN_POINT('Ctrl Pts',(65.4940947990912,249.656080804643,22.5648717838627)) ;
#109757 = CARTESIAN_POINT('Ctrl Pts',(65.4909592167245,249.636869280332,22.5016692784945)) ;
#109758 = CARTESIAN_POINT('Ctrl Pts',(65.4878236343579,249.614046703296,22.4398940351297)) ;
#109759 = CARTESIAN_POINT('Ctrl Pts',(65.4857189454525,249.59872756348,22.3984287970561)) ;
#109760 = CARTESIAN_POINT('Ctrl Pts',(65.4836142565472,249.581782486181,22.3576061933882)) ;
#109761 = CARTESIAN_POINT('Ctrl Pts',(65.4815095676419,249.563272157893,22.317548656274)) ;
#109762 = CARTESIAN_POINT('Ctrl Pts',(65.4785924797904,249.537616939375,22.2620291186446)) ;
#109763 = CARTESIAN_POINT('Ctrl Pts',(65.4756753919389,249.508873303146,22.2078089745261)) ;
#109764 = CARTESIAN_POINT('Ctrl Pts',(65.4727583040873,249.477195952274,22.1552517488974)) ;
#109765 = CARTESIAN_POINT('Ctrl Pts',(65.4698460395561,249.445570978984,22.1027814251191)) ;
#109766 = CARTESIAN_POINT('Ctrl Pts',(65.4669337750249,249.411022183956,22.0519689904515)) ;
#109767 = CARTESIAN_POINT('Ctrl Pts',(65.4640215104936,249.373750954022,22.0031550522693)) ;
#109768 = CARTESIAN_POINT('Ctrl Pts',(65.4611119374221,249.336514169453,21.9543862270041)) ;
#109769 = CARTESIAN_POINT('Ctrl Pts',(65.4582023643506,249.296560244532,21.907612637462)) ;
#109770 = CARTESIAN_POINT('Ctrl Pts',(65.455292791279,249.254133936172,21.8631461209263)) ;
#109771 = CARTESIAN_POINT('Ctrl Pts',(65.4523848522289,249.211731454502,21.8187045768651)) ;
#109772 = CARTESIAN_POINT('Ctrl Pts',(65.4494769131787,249.166859692877,21.7765679018234)) ;
#109773 = CARTESIAN_POINT('Ctrl Pts',(65.4465689741286,249.119802454161,21.7370134564484)) ;
#109774 = CARTESIAN_POINT('Ctrl Pts',(65.4436616139098,249.072754582287,21.697466884468)) ;
#109775 = CARTESIAN_POINT('Ctrl Pts',(65.440754253691,249.023522485433,21.6605018469641)) ;
#109776 = CARTESIAN_POINT('Ctrl Pts',(65.4378468934721,248.972423926319,21.6263561864822)) ;
#109777 = CARTESIAN_POINT('Ctrl Pts',(65.4349370717318,248.921282104523,21.5921816165183)) ;
#109778 = CARTESIAN_POINT('Ctrl Pts',(65.4320272499915,248.868271084647,21.5608314763569)) ;
#109779 = CARTESIAN_POINT('Ctrl Pts',(65.4291174282511,248.813737561792,21.5325001981444)) ;
#109780 = CARTESIAN_POINT('Ctrl Pts',(65.4262064361497,248.759182104976,21.5041575247916)) ;
#109781 = CARTESIAN_POINT('Ctrl Pts',(65.4232954440482,248.703103386298,21.4788363449978)) ;
#109782 = CARTESIAN_POINT('Ctrl Pts',(65.4203844519467,248.645869944603,21.4566836943262)) ;
#109783 = CARTESIAN_POINT('Ctrl Pts',(65.4174682764158,248.588534590742,21.4344915977549)) ;
#109784 = CARTESIAN_POINT('Ctrl Pts',(65.4145521008848,248.530040888254,21.4154794629481)) ;
#109785 = CARTESIAN_POINT('Ctrl Pts',(65.4116359253539,248.470773655906,21.3997447355487)) ;
#109786 = CARTESIAN_POINT('Ctrl Pts',(65.4091535937425,248.42032370088,21.3863508877483)) ;
#109787 = CARTESIAN_POINT('Ctrl Pts',(65.4066712621311,248.369313663447,21.3753309846636)) ;
#109788 = CARTESIAN_POINT('Ctrl Pts',(65.4041889305196,248.317984969375,21.3667156351839)) ;
#109789 = CARTESIAN_POINT('Ctrl Pts',(65.4012720962684,248.257671797575,21.3565922711929)) ;
#109790 = CARTESIAN_POINT('Ctrl Pts',(65.3983552620171,248.196690065062,21.3497517539178)) ;
#109791 = CARTESIAN_POINT('Ctrl Pts',(65.3954384277659,248.135427179136,21.3462713166125)) ;
#109792 = CARTESIAN_POINT('Ctrl Pts',(65.3925264077411,248.074265407425,21.3427966237589)) ;
#109793 = CARTESIAN_POINT('Ctrl Pts',(65.3896143877162,248.012823906315,21.3426710261847)) ;
#109794 = CARTESIAN_POINT('Ctrl Pts',(65.3867023676914,247.951497483721,21.3459202804649)) ;
#109795 = CARTESIAN_POINT('Ctrl Pts',(65.3837930334048,247.89022762211,21.3491665379778)) ;
#109796 = CARTESIAN_POINT('Ctrl Pts',(65.3808836991181,247.829073132597,21.3557814495652)) ;
#109797 = CARTESIAN_POINT('Ctrl Pts',(65.3779743648315,247.768429519284,21.3657387311576)) ;
#109798 = CARTESIAN_POINT('Ctrl Pts',(65.3750666584934,247.707819839741,21.3756904410486)) ;
#109799 = CARTESIAN_POINT('Ctrl Pts',(65.3721589521552,247.647720968723,21.3889807291357)) ;
#109800 = CARTESIAN_POINT('Ctrl Pts',(65.3692512458171,247.588521954332,21.4055316241388)) ;
#109801 = CARTESIAN_POINT('Ctrl Pts',(65.3663441118793,247.52933459364,21.4220792609939)) ;
#109802 = CARTESIAN_POINT('Ctrl Pts',(65.3634369779414,247.471047225645,21.4418860930771)) ;
#109803 = CARTESIAN_POINT('Ctrl Pts',(65.3605298440036,247.414035409919,21.46482381995)) ;
#109804 = CARTESIAN_POINT('Ctrl Pts',(65.3576202368912,247.356975092755,21.4877810605449)) ;
#109805 = CARTESIAN_POINT('Ctrl Pts',(65.3547106297788,247.301192967862,21.5138743293845)) ;
#109806 = CARTESIAN_POINT('Ctrl Pts',(65.3518010226664,247.24704505771,21.5429269538768)) ;
#109807 = CARTESIAN_POINT('Ctrl Pts',(65.3488902390681,247.192875253107,21.5719913256603)) ;
#109808 = CARTESIAN_POINT('Ctrl Pts',(65.3459794554698,247.140341415325,21.6040171760256)) ;
#109809 = CARTESIAN_POINT('Ctrl Pts',(65.3430686718716,247.089772737581,21.6387830685893)) ;
#109810 = CARTESIAN_POINT('Ctrl Pts',(65.3401526922266,247.039113789571,21.6736110218302)) ;
#109811 = CARTESIAN_POINT('Ctrl Pts',(65.3372367125816,246.99042741484,21.7111884815772)) ;
#109812 = CARTESIAN_POINT('Ctrl Pts',(65.3343207329366,246.944011029941,21.7512526054813)) ;
#109813 = CARTESIAN_POINT('Ctrl Pts',(65.3318365864236,246.904468538313,21.7853835548748)) ;
#109814 = CARTESIAN_POINT('Ctrl Pts',(65.3293524399105,246.866573031895,21.8213183879479)) ;
#109815 = CARTESIAN_POINT('Ctrl Pts',(65.3268682933975,246.830486267395,21.8588745513426)) ;
#109816 = CARTESIAN_POINT('Ctrl Pts',(65.3239534845639,246.78814334624,21.9029416127029)) ;
#109817 = CARTESIAN_POINT('Ctrl Pts',(65.3210386757303,246.748130245474,21.9494095769339)) ;
#109818 = CARTESIAN_POINT('Ctrl Pts',(65.3181238668967,246.710729112967,21.9980026504742)) ;
#109819 = CARTESIAN_POINT('Ctrl Pts',(65.3152138828244,246.673389888992,22.0465152899298)) ;
#109820 = CARTESIAN_POINT('Ctrl Pts',(65.3123038987521,246.63865435526,22.0971456540691)) ;
#109821 = CARTESIAN_POINT('Ctrl Pts',(65.3093939146798,246.606766356824,22.1495827721025)) ;
#109822 = CARTESIAN_POINT('Ctrl Pts',(65.3064866210556,246.574907840681,22.2019714089964)) ;
#109823 = CARTESIAN_POINT('Ctrl Pts',(65.3035793274314,246.545891903166,22.25616305621)) ;
#109824 = CARTESIAN_POINT('Ctrl Pts',(65.3006720338072,246.519919828641,22.3118167884718)) ;
#109825 = CARTESIAN_POINT('Ctrl Pts',(65.2977663690951,246.493962305872,22.3674393387992)) ;
#109826 = CARTESIAN_POINT('Ctrl Pts',(65.294860704383,246.471045477772,22.424521890027)) ;
#109827 = CARTESIAN_POINT('Ctrl Pts',(65.2919550396709,246.451324316602,22.482699674988)) ;
#109828 = CARTESIAN_POINT('Ctrl Pts',(65.2890499445796,246.43160702153,22.5408660548911)) ;
#109829 = CARTESIAN_POINT('Ctrl Pts',(65.2861448494882,246.415084311733,22.6001267612825)) ;
#109830 = CARTESIAN_POINT('Ctrl Pts',(65.2832397543969,246.401861995641,22.6600997674362)) ;
#109831 = CARTESIAN_POINT('Ctrl Pts',(65.2803321655009,246.38862832919,22.7201242558858)) ;
#109832 = CARTESIAN_POINT('Ctrl Pts',(65.2774245766048,246.378700827985,22.7808617691219)) ;
#109833 = CARTESIAN_POINT('Ctrl Pts',(65.2745169877088,246.372134338007,22.8419191244501)) ;
#109834 = CARTESIAN_POINT('Ctrl Pts',(65.2716082137543,246.365565171697,22.9030013651862)) ;
#109835 = CARTESIAN_POINT('Ctrl Pts',(65.2686994397998,246.362359775844,22.964403199947)) ;
#109836 = CARTESIAN_POINT('Ctrl Pts',(65.2657906658453,246.362520898481,23.0257283639149)) ;
#109837 = CARTESIAN_POINT('Ctrl Pts',(65.2628766566017,246.362682311111,23.0871639025526)) ;
#109838 = CARTESIAN_POINT('Ctrl Pts',(65.259962647358,246.366222321665,23.1485219860933)) ;
#109839 = CARTESIAN_POINT('Ctrl Pts',(65.2570486381144,246.373091563555,23.2094092478441)) ;
#109840 = CARTESIAN_POINT('Ctrl Pts',(65.2545483108347,246.378985626151,23.2616527614408)) ;
#109841 = CARTESIAN_POINT('Ctrl Pts',(65.252047983555,246.387329856001,23.3135495519082)) ;
#109842 = CARTESIAN_POINT('Ctrl Pts',(65.2495476562753,246.398063312116,23.3648582960463)) ;
#109843 = CARTESIAN_POINT('Ctrl Pts',(65.2466006810568,246.410714147644,23.4253326182277)) ;
#109844 = CARTESIAN_POINT('Ctrl Pts',(65.2436537058382,246.426733710662,23.4852213825265)) ;
#109845 = CARTESIAN_POINT('Ctrl Pts',(65.2407067306196,246.446050225804,23.5441242958844)) ;
#109846 = CARTESIAN_POINT('Ctrl Pts',(65.2377909266074,246.465162423286,23.6024041721524)) ;
#109847 = CARTESIAN_POINT('Ctrl Pts',(65.2348751225951,246.487502027005,23.6597184543634)) ;
#109848 = CARTESIAN_POINT('Ctrl Pts',(65.2319593185829,246.512948324416,23.7156894858295)) ;
#109849 = CARTESIAN_POINT('Ctrl Pts',(65.2290462723041,246.538370555016,23.7716075805463)) ;
#109850 = CARTESIAN_POINT('Ctrl Pts',(65.2261332260252,246.56689344367,23.8261844859753)) ;
#109851 = CARTESIAN_POINT('Ctrl Pts',(65.2232201797464,246.598347602175,23.8790609625773)) ;
#109852 = CARTESIAN_POINT('Ctrl Pts',(65.2203088400178,246.629783333888,23.9319064625492)) ;
#109853 = CARTESIAN_POINT('Ctrl Pts',(65.2173975002891,246.664146669705,23.9830530769868)) ;
#109854 = CARTESIAN_POINT('Ctrl Pts',(65.2144861605604,246.701222489793,24.0321664889742)) ;
#109855 = CARTESIAN_POINT('Ctrl Pts',(65.2115140014328,246.739072843018,24.0823059056439)) ;
#109856 = CARTESIAN_POINT('Ctrl Pts',(65.2085418423053,246.779750030088,24.1303257300894)) ;
#109857 = CARTESIAN_POINT('Ctrl Pts',(65.2055696831777,246.822979955493,24.1759033507563)) ;
#109858 = CARTESIAN_POINT('Ctrl Pts',(65.2026572829908,246.865340689703,24.2205645769067)) ;
#109859 = CARTESIAN_POINT('Ctrl Pts',(65.1997448828038,246.910152044671,24.2628805765233)) ;
#109860 = CARTESIAN_POINT('Ctrl Pts',(65.1968324826169,246.957118595572,24.3025848344348)) ;
#109861 = CARTESIAN_POINT('Ctrl Pts',(65.193830444019,247.005530691974,24.3435111176029)) ;
#109862 = CARTESIAN_POINT('Ctrl Pts',(65.1908284054212,247.056232409242,24.3816618563829)) ;
#109863 = CARTESIAN_POINT('Ctrl Pts',(65.1878263668233,247.10886539866,24.4167914626949)) ;
#109864 = CARTESIAN_POINT('Ctrl Pts',(65.1848243282255,247.161498388079,24.451921069007)) ;
#109865 = CARTESIAN_POINT('Ctrl Pts',(65.1818222896276,247.216062125856,24.4840292807919)) ;
#109866 = CARTESIAN_POINT('Ctrl Pts',(65.1788202510297,247.272170391302,24.5129220226314)) ;
#109867 = CARTESIAN_POINT('Ctrl Pts',(65.6787784786721,247.273150902455,24.5110052762898)) ;
#109868 = CARTESIAN_POINT('Ctrl Pts',(65.6645692664101,247.540740422681,24.6479503068636)) ;
#109869 = CARTESIAN_POINT('Ctrl Pts',(65.6245865084408,248.393573021656,24.8412580942799)) ;
#109870 = CARTESIAN_POINT('Ctrl Pts',(65.5703122582425,249.494912575159,24.1717753210047)) ;
#109871 = CARTESIAN_POINT('Ctrl Pts',(65.5302472203063,249.715145368677,23.3232200710915)) ;
#109872 = CARTESIAN_POINT('Ctrl Pts',(65.5159557280774,249.715873122799,23.0208884958769)) ;
#109873 = CARTESIAN_POINT('',(65.6145744874959,249.719484537996,23.0224181452927)) ;
#109874 = CARTESIAN_POINT('Ctrl Pts',(65.7773991381782,247.271019322241,24.5151747855319)) ;
#109875 = CARTESIAN_POINT('Ctrl Pts',(65.7526443967294,247.734017259182,24.7517245800444)) ;
#109876 = CARTESIAN_POINT('Ctrl Pts',(65.7021161095732,248.923660698597,24.7653398940284)) ;
#109877 = CARTESIAN_POINT('Ctrl Pts',(65.6478412260124,249.679932032969,23.7216704578517)) ;
#109878 = CARTESIAN_POINT('Ctrl Pts',(65.6183210839004,249.720089797457,23.1012396421188)) ;
#109879 = CARTESIAN_POINT('Ctrl Pts',(65.6145744874959,249.719484537996,23.0224181452927)) ;
#109880 = CARTESIAN_POINT('Ctrl Pts',(65.2787248749179,247.272170391302,24.5129220226314)) ;
#109881 = CARTESIAN_POINT('Ctrl Pts',(65.2787251604049,247.272165032388,24.5129192630787)) ;
#109882 = CARTESIAN_POINT('Ctrl Pts',(65.278725445891,247.272159673489,24.512916503497)) ;
#109883 = CARTESIAN_POINT('Ctrl Pts',(65.2801133552695,247.246107015076,24.49950042904)) ;
#109884 = CARTESIAN_POINT('Ctrl Pts',(65.2814781085148,247.220414718267,24.4854067141748)) ;
#109885 = CARTESIAN_POINT('Ctrl Pts',(65.2848794516747,247.156328053296,24.4480351672425)) ;
#109886 = CARTESIAN_POINT('Ctrl Pts',(65.2868854010309,247.118474008147,24.4238756659129)) ;
#109887 = CARTESIAN_POINT('Ctrl Pts',(65.2913925336548,247.034042371573,24.3650924671633)) ;
#109888 = CARTESIAN_POINT('Ctrl Pts',(65.2938636731129,246.988200616357,24.3295131520187)) ;
#109889 = CARTESIAN_POINT('Ctrl Pts',(65.3010003376567,246.860303295283,24.2191684344408)) ;
#109890 = CARTESIAN_POINT('Ctrl Pts',(65.3055809102225,246.783715368561,24.1385618226974)) ;
#109891 = CARTESIAN_POINT('Ctrl Pts',(65.3116269153918,246.701398169249,24.0326657289751)) ;
#109892 = CARTESIAN_POINT('Ctrl Pts',(65.3126918567843,246.687530974627,24.0140410709375)) ;
#109893 = CARTESIAN_POINT('Ctrl Pts',(65.3145449454229,246.664596390981,23.981865094348)) ;
#109894 = CARTESIAN_POINT('Ctrl Pts',(65.3153212784597,246.655332341131,23.9684591063175)) ;
#109895 = CARTESIAN_POINT('Ctrl Pts',(65.3171919504421,246.633824620252,23.9363449278579)) ;
#109896 = CARTESIAN_POINT('Ctrl Pts',(65.3182958844824,246.621757662664,23.9175242141664)) ;
#109897 = CARTESIAN_POINT('Ctrl Pts',(65.3207803355331,246.595853010081,23.8752865730941)) ;
#109898 = CARTESIAN_POINT('Ctrl Pts',(65.3221686027896,246.582201406051,23.8517628516253)) ;
#109899 = CARTESIAN_POINT('Ctrl Pts',(65.3298577335332,246.510623849625,23.7212141198065)) ;
#109900 = CARTESIAN_POINT('Ctrl Pts',(65.336411255635,246.463901164489,23.6084600415325)) ;
#109901 = CARTESIAN_POINT('Ctrl Pts',(65.345663437879,246.413614234233,23.4362656595576)) ;
#109902 = CARTESIAN_POINT('Ctrl Pts',(65.348576409491,246.400309053115,23.3800928278022)) ;
#109903 = CARTESIAN_POINT('Ctrl Pts',(65.3529269233677,246.384336808603,23.2928155010469)) ;
#109904 = CARTESIAN_POINT('Ctrl Pts',(65.3544238202099,246.379598112549,23.2621386009732)) ;
#109905 = CARTESIAN_POINT('Ctrl Pts',(65.3572752977917,246.37207064708,23.2024800752714)) ;
#109906 = CARTESIAN_POINT('Ctrl Pts',(65.3586324492277,246.369179785801,23.1735227491316)) ;
#109907 = CARTESIAN_POINT('Ctrl Pts',(65.3619655614132,246.363849652597,23.1011226534158)) ;
#109908 = CARTESIAN_POINT('Ctrl Pts',(65.3639137021724,246.362344080841,23.05763214007)) ;
#109909 = CARTESIAN_POINT('Ctrl Pts',(65.3682449836589,246.362766770456,22.9590030410233)) ;
#109910 = CARTESIAN_POINT('Ctrl Pts',(65.3706020249864,246.365719932988,22.9039195112528)) ;
#109911 = CARTESIAN_POINT('Ctrl Pts',(65.3779883922573,246.383636634124,22.7303198055549)) ;
#109912 = CARTESIAN_POINT('Ctrl Pts',(65.3828917689606,246.40853370839,22.613219200442)) ;
#109913 = CARTESIAN_POINT('Ctrl Pts',(65.3892784100183,246.452384887201,22.4791468955633)) ;
#109914 = CARTESIAN_POINT('Ctrl Pts',(65.3902771503213,246.459527437132,22.4586623801986)) ;
#109915 = CARTESIAN_POINT('Ctrl Pts',(65.3920635401806,246.472729948615,22.4230358147814)) ;
#109916 = CARTESIAN_POINT('Ctrl Pts',(65.3928423826101,246.478616937231,22.4078337534041)) ;
#109917 = CARTESIAN_POINT('Ctrl Pts',(65.3947737097523,246.493531245029,22.3709266885103)) ;
#109918 = CARTESIAN_POINT('Ctrl Pts',(65.3959380073934,246.502794473464,22.3493222034538)) ;
#109919 = CARTESIAN_POINT('Ctrl Pts',(65.3985892806452,246.524575729568,22.301331906094)) ;
#109920 = CARTESIAN_POINT('Ctrl Pts',(65.4000856119861,246.537335019653,22.2750639124343)) ;
#109921 = CARTESIAN_POINT('Ctrl Pts',(65.4052595685095,246.583278770671,22.1864406222688)) ;
#109922 = CARTESIAN_POINT('Ctrl Pts',(65.4090114474638,246.619711198304,22.1258541807603)) ;
#109923 = CARTESIAN_POINT('Ctrl Pts',(65.4173111465078,246.709218627299,21.9962816305537)) ;
#109924 = CARTESIAN_POINT('Ctrl Pts',(65.4218272120108,246.764063484794,21.9287540899728)) ;
#109925 = CARTESIAN_POINT('Ctrl Pts',(65.4279623017477,246.848770742242,21.8395882949436)) ;
#109926 = CARTESIAN_POINT('Ctrl Pts',(65.4297322298052,246.874485847982,21.8142128883417)) ;
#109927 = CARTESIAN_POINT('Ctrl Pts',(65.4328341767626,246.921863363349,21.7703886016868)) ;
#109928 = CARTESIAN_POINT('Ctrl Pts',(65.434178668651,246.943213088448,21.751623661276)) ;
#109929 = CARTESIAN_POINT('Ctrl Pts',(65.4370937445044,246.991258376166,21.7115122065079)) ;
#109930 = CARTESIAN_POINT('Ctrl Pts',(65.4386542991453,247.018150410036,21.6904205718303)) ;
#109931 = CARTESIAN_POINT('Ctrl Pts',(65.4445965678961,247.124773141631,21.6119347870737)) ;
#109932 = CARTESIAN_POINT('Ctrl Pts',(65.4487577439654,247.208841680642,21.5607622513343)) ;
#109933 = CARTESIAN_POINT('Ctrl Pts',(65.4569526253967,247.383225950798,21.4745767918507)) ;
#109934 = CARTESIAN_POINT('Ctrl Pts',(65.4609765818969,247.473050731389,21.4394287615949)) ;
#109935 = CARTESIAN_POINT('Ctrl Pts',(65.4663537933726,247.587337636108,21.4057010584497)) ;
#109936 = CARTESIAN_POINT('Ctrl Pts',(65.4674046480988,247.609420007946,21.3996726068345)) ;
#109937 = CARTESIAN_POINT('Ctrl Pts',(65.4692435415761,247.647421883392,21.390129127431)) ;
#109938 = CARTESIAN_POINT('Ctrl Pts',(65.4700204214036,247.663281139555,21.3863910994407)) ;
#109939 = CARTESIAN_POINT('Ctrl Pts',(65.4719079220205,247.701339515509,21.3780039424865)) ;
#109940 = CARTESIAN_POINT('Ctrl Pts',(65.4730287551434,247.723581797488,21.373573110626)) ;
#109941 = CARTESIAN_POINT('Ctrl Pts',(65.4755595190611,247.773225000526,21.3647260443167)) ;
#109942 = CARTESIAN_POINT('Ctrl Pts',(65.4769776308851,247.800659549744,21.3605361459666)) ;
#109943 = CARTESIAN_POINT('Ctrl Pts',(65.4816986909607,247.891247202965,21.3489925524759)) ;
#109944 = CARTESIAN_POINT('Ctrl Pts',(65.4850656301792,247.954714461548,21.3445474587606)) ;
#109945 = CARTESIAN_POINT('Ctrl Pts',(65.4935234272992,248.114909464125,21.3424480098814)) ;
#109946 = CARTESIAN_POINT('Ctrl Pts',(65.4985749878756,248.211477082246,21.3495327070713)) ;
#109947 = CARTESIAN_POINT('Ctrl Pts',(65.5052113220985,248.342756622173,21.3706651342026)) ;
#109948 = CARTESIAN_POINT('Ctrl Pts',(65.5069917015127,248.378413240225,21.3775990125917)) ;
#109949 = CARTESIAN_POINT('Ctrl Pts',(65.510104566423,248.441530932365,21.3920140983603)) ;
#109950 = CARTESIAN_POINT('Ctrl Pts',(65.5114498825721,248.469078979458,21.3990466676376)) ;
#109951 = CARTESIAN_POINT('Ctrl Pts',(65.514358806751,248.529161377567,21.416022259653)) ;
#109952 = CARTESIAN_POINT('Ctrl Pts',(65.5159126842182,248.561599106234,21.4262615548055)) ;
#109953 = CARTESIAN_POINT('Ctrl Pts',(65.5218657125502,248.686749484563,21.469992704685)) ;
#109954 = CARTESIAN_POINT('Ctrl Pts',(65.5260417031075,248.776752628797,21.5106425754533)) ;
#109955 = CARTESIAN_POINT('Ctrl Pts',(65.5342601391638,248.946792333908,21.6062696522357)) ;
#109956 = CARTESIAN_POINT('Ctrl Pts',(65.5382928781597,249.026670321995,21.6607462513169)) ;
#109957 = CARTESIAN_POINT('Ctrl Pts',(65.5436796871986,249.119128040101,21.736243404269)) ;
#109958 = CARTESIAN_POINT('Ctrl Pts',(65.5447295886078,249.136542013623,21.7510665005758)) ;
#109959 = CARTESIAN_POINT('Ctrl Pts',(65.5465674037911,249.165834684351,21.7770520327555)) ;
#109960 = CARTESIAN_POINT('Ctrl Pts',(65.5473441965105,249.177863027752,21.7880395822384)) ;
#109961 = CARTESIAN_POINT('Ctrl Pts',(65.5492322487321,249.206258311595,21.8147467780886)) ;
#109962 = CARTESIAN_POINT('Ctrl Pts',(65.5503537497323,249.222468918479,21.8306255961116)) ;
#109963 = CARTESIAN_POINT('Ctrl Pts',(65.5528863816545,249.257793171086,21.8666594628687)) ;
#109964 = CARTESIAN_POINT('Ctrl Pts',(65.5543057122949,249.27673841995,21.8869703245343)) ;
#109965 = CARTESIAN_POINT('Ctrl Pts',(65.5590336541357,249.337436027233,21.9553711461487)) ;
#109966 = CARTESIAN_POINT('Ctrl Pts',(65.5624064163098,249.376955019651,22.0053676825847)) ;
#109967 = CARTESIAN_POINT('Ctrl Pts',(65.5708611051912,249.468958568187,22.136454546869)) ;
#109968 = CARTESIAN_POINT('Ctrl Pts',(65.5759037432801,249.517471887109,22.2200613676321)) ;
#109969 = CARTESIAN_POINT('Ctrl Pts',(65.58253208066,249.573986140451,22.3402449527344)) ;
#109970 = CARTESIAN_POINT('Ctrl Pts',(65.5843125817513,249.588369220925,22.3736029778339)) ;
#109971 = CARTESIAN_POINT('Ctrl Pts',(65.5874255138225,249.61206008712,22.4338566617689)) ;
#109972 = CARTESIAN_POINT('Ctrl Pts',(65.5887707820689,249.621787599742,22.4605710632023)) ;
#109973 = CARTESIAN_POINT('Ctrl Pts',(65.5916794326902,249.641650009961,22.5197552421261)) ;
#109974 = CARTESIAN_POINT('Ctrl Pts',(65.5932330914424,249.651485988112,22.5523122334519)) ;
#109975 = CARTESIAN_POINT('Ctrl Pts',(65.5991772599446,249.685899499949,22.6801329498468)) ;
#109976 = CARTESIAN_POINT('Ctrl Pts',(65.6033456360179,249.703070745726,22.777188221211)) ;
#109977 = CARTESIAN_POINT('Ctrl Pts',(65.6095610206486,249.71592081736,22.9241629434479)) ;
#109978 = CARTESIAN_POINT('Ctrl Pts',(65.6116258859239,249.718047910538,22.9732975817688)) ;
#109979 = CARTESIAN_POINT('Ctrl Pts',(65.6137281789529,249.718014725454,23.0224530012129)) ;
#109980 = CARTESIAN_POINT('Origin',(61.8645744874958,248.040265107786,23.0213203435596)) ;
#109981 = CARTESIAN_POINT('',(60.6787800750062,247.272018954284,24.5128440309777)) ;
#109982 = CARTESIAN_POINT('',(60.7756980793888,247.272018954284,24.5128440309778)) ;
#109983 = CARTESIAN_POINT('',(61.8645744874958,247.272018954284,24.5128440309778)) ;
#109984 = CARTESIAN_POINT('',(60.940227675589,249.014561429937,21.655453681274)) ;
#109985 = CARTESIAN_POINT('Ctrl Pts',(60.940227675589,249.014561429937,21.655453681274)) ;
#109986 = CARTESIAN_POINT('Ctrl Pts',(60.9372127561583,248.963091283515,21.6187391353054)) ;
#109987 = CARTESIAN_POINT('Ctrl Pts',(60.9341978367275,248.909424109754,21.5848535129617)) ;
#109988 = CARTESIAN_POINT('Ctrl Pts',(60.9311829172968,248.853911725446,21.5540697705248)) ;
#109989 = CARTESIAN_POINT('Ctrl Pts',(60.9283156924155,248.801118775861,21.5247940587582)) ;
#109990 = CARTESIAN_POINT('Ctrl Pts',(60.9254484675342,248.746657684804,21.4983237503668)) ;
#109991 = CARTESIAN_POINT('Ctrl Pts',(60.9225812426529,248.690862876965,21.4748509435263)) ;
#109992 = CARTESIAN_POINT('Ctrl Pts',(60.9197165162814,248.635116688918,21.4513985909722)) ;
#109993 = CARTESIAN_POINT('Ctrl Pts',(60.91685178991,248.578039567083,21.430938769325)) ;
#109994 = CARTESIAN_POINT('Ctrl Pts',(60.9139870635385,248.519989426209,21.4136171244258)) ;
#109995 = CARTESIAN_POINT('Ctrl Pts',(60.911123712368,248.461967152084,21.396303794716)) ;
#109996 = CARTESIAN_POINT('Ctrl Pts',(60.9082603611976,248.402973286455,21.3821258056995)) ;
#109997 = CARTESIAN_POINT('Ctrl Pts',(60.9053970100271,248.343382425444,21.3711794543516)) ;
#109998 = CARTESIAN_POINT('Ctrl Pts',(60.9025339129334,248.283796852173,21.3602340743183)) ;
#109999 = CARTESIAN_POINT('Ctrl Pts',(60.8996708158398,248.223614904701,21.3525198551716)) ;
#110000 = CARTESIAN_POINT('Ctrl Pts',(60.8968077187462,248.163220700734,21.3480818714156)) ;
#110001 = CARTESIAN_POINT('Ctrl Pts',(60.8939419153504,248.102769409998,21.343639692718)) ;
#110002 = CARTESIAN_POINT('Ctrl Pts',(60.8910761119546,248.042105986334,21.3424799663762)) ;
#110003 = CARTESIAN_POINT('Ctrl Pts',(60.8882103085588,247.981617458099,21.3445957043638)) ;
#110004 = CARTESIAN_POINT('Ctrl Pts',(60.8853429246568,247.921095570111,21.3467126091925)) ;
#110005 = CARTESIAN_POINT('Ctrl Pts',(60.8824755407547,247.860749291517,21.35210852332)) ;
#110006 = CARTESIAN_POINT('Ctrl Pts',(60.8796081568527,247.800960246066,21.3607245933371)) ;
#110007 = CARTESIAN_POINT('Ctrl Pts',(60.876735943038,247.741070490045,21.3693551765366)) ;
#110008 = CARTESIAN_POINT('Ctrl Pts',(60.8738637292232,247.6817403521,21.3812166293377)) ;
#110009 = CARTESIAN_POINT('Ctrl Pts',(60.8709915154085,247.623339591769,21.396199370649)) ;
#110010 = CARTESIAN_POINT('Ctrl Pts',(60.8699508800227,247.602180339122,21.4016277864256)) ;
#110011 = CARTESIAN_POINT('Ctrl Pts',(60.8689102446368,247.581142917275,21.407465464781)) ;
#110012 = CARTESIAN_POINT('Ctrl Pts',(60.867869609251,247.560244271735,21.4137056324247)) ;
#110013 = CARTESIAN_POINT('Ctrl Pts',(60.8649570713242,247.501752989794,21.4311706592527)) ;
#110014 = CARTESIAN_POINT('Ctrl Pts',(60.8620445333974,247.444100412217,21.451866578102)) ;
#110015 = CARTESIAN_POINT('Ctrl Pts',(60.8591319954706,247.387667546907,21.4756937761009)) ;
#110016 = CARTESIAN_POINT('Ctrl Pts',(60.8561992107954,247.330842383862,21.4996866108386)) ;
#110017 = CARTESIAN_POINT('Ctrl Pts',(60.8532664261202,247.275254476981,21.5268543518343)) ;
#110018 = CARTESIAN_POINT('Ctrl Pts',(60.850333641445,247.221278510744,21.5570437247593)) ;
#110019 = CARTESIAN_POINT('Ctrl Pts',(60.8474288575414,247.167817880227,21.5869448645441)) ;
#110020 = CARTESIAN_POINT('Ctrl Pts',(60.8445240736378,247.115939000221,21.6198099425868)) ;
#110021 = CARTESIAN_POINT('Ctrl Pts',(60.8416192897342,247.065984729456,21.6554423084112)) ;
#110022 = CARTESIAN_POINT('Ctrl Pts',(60.8387162072254,247.016059717989,21.6910538035876)) ;
#110023 = CARTESIAN_POINT('Ctrl Pts',(60.8358131247166,246.968057493728,21.7294290772779)) ;
#110024 = CARTESIAN_POINT('Ctrl Pts',(60.8329100422078,246.922292452755,21.7703278555314)) ;
#110025 = CARTESIAN_POINT('Ctrl Pts',(60.8300075968063,246.876537455328,21.8112176581835)) ;
#110026 = CARTESIAN_POINT('Ctrl Pts',(60.8271051514049,246.833019045543,21.854629526766)) ;
#110027 = CARTESIAN_POINT('Ctrl Pts',(60.8242027060034,246.792017410026,21.9002838822717)) ;
#110028 = CARTESIAN_POINT('Ctrl Pts',(60.8212479107753,246.750276250343,21.9467616805193)) ;
#110029 = CARTESIAN_POINT('Ctrl Pts',(60.8182931155471,246.711143946213,21.9955632832225)) ;
#110030 = CARTESIAN_POINT('Ctrl Pts',(60.8153383203189,246.674874157318,22.0463574648406)) ;
#110031 = CARTESIAN_POINT('Ctrl Pts',(60.8124321301431,246.639200990136,22.0963161050191)) ;
#110032 = CARTESIAN_POINT('Ctrl Pts',(60.8095259399674,246.606297086554,22.1482017830271)) ;
#110033 = CARTESIAN_POINT('Ctrl Pts',(60.8066197497916,246.576359287954,22.2016711422781)) ;
#110034 = CARTESIAN_POINT('Ctrl Pts',(60.8036406520372,246.545670439949,22.2564818870804)) ;
#110035 = CARTESIAN_POINT('Ctrl Pts',(60.8006615542829,246.518098805243,22.3129563487326)) ;
#110036 = CARTESIAN_POINT('Ctrl Pts',(60.7976824565285,246.493804490034,22.3707016993125)) ;
#110037 = CARTESIAN_POINT('Ctrl Pts',(60.7947033587741,246.469510174825,22.4284470498924)) ;
#110038 = CARTESIAN_POINT('Ctrl Pts',(60.7917242610198,246.448493306057,22.4874627311267)) ;
#110039 = CARTESIAN_POINT('Ctrl Pts',(60.7887451632654,246.430858864895,22.5473407998624)) ;
#110040 = CARTESIAN_POINT('Ctrl Pts',(60.7858386217233,246.413653912243,22.6057605324766)) ;
#110041 = CARTESIAN_POINT('Ctrl Pts',(60.7829320801812,246.399598409989,22.6652389656913)) ;
#110042 = CARTESIAN_POINT('Ctrl Pts',(60.7800255386391,246.388817625871,22.7254043470751)) ;
#110043 = CARTESIAN_POINT('Ctrl Pts',(60.7770920044158,246.377936721983,22.7861284766945)) ;
#110044 = CARTESIAN_POINT('Ctrl Pts',(60.7741584701925,246.370391906018,22.847551900403)) ;
#110045 = CARTESIAN_POINT('Ctrl Pts',(60.7712249359692,246.366260596378,22.9092758957446)) ;
#110046 = CARTESIAN_POINT('Ctrl Pts',(60.7683263931628,246.362178565311,22.9702636426268)) ;
#110047 = CARTESIAN_POINT('Ctrl Pts',(60.7654278503564,246.361429090042,23.0315443067775)) ;
#110048 = CARTESIAN_POINT('Ctrl Pts',(60.7625293075499,246.364035269663,23.0927247711881)) ;
#110049 = CARTESIAN_POINT('Ctrl Pts',(60.759632539937,246.366639853146,23.1538677660251)) ;
#110050 = CARTESIAN_POINT('Ctrl Pts',(60.7567357723241,246.37259599498,23.2149101729716)) ;
#110051 = CARTESIAN_POINT('Ctrl Pts',(60.7538390047112,246.381874709416,23.2754587882954)) ;
#110052 = CARTESIAN_POINT('Ctrl Pts',(60.7509429373374,246.391151180896,23.3359927671289)) ;
#110053 = CARTESIAN_POINT('Ctrl Pts',(60.7480468699636,246.403748553129,23.3960326860824)) ;
#110054 = CARTESIAN_POINT('Ctrl Pts',(60.7451508025899,246.419586222929,23.4551924614458)) ;
#110055 = CARTESIAN_POINT('Ctrl Pts',(60.7421899621474,246.435778116006,23.5156753967019)) ;
#110056 = CARTESIAN_POINT('Ctrl Pts',(60.7392291217049,246.455356913336,23.5752377911731)) ;
#110057 = CARTESIAN_POINT('Ctrl Pts',(60.7362682812624,246.478182388077,23.6334826090456)) ;
#110058 = CARTESIAN_POINT('Ctrl Pts',(60.7333685507391,246.500536759107,23.6905252898268)) ;
#110059 = CARTESIAN_POINT('Ctrl Pts',(60.7304688202159,246.526004774298,23.7463038198903)) ;
#110060 = CARTESIAN_POINT('Ctrl Pts',(60.7275690896927,246.554406672558,23.8004671673109)) ;
#110061 = CARTESIAN_POINT('Ctrl Pts',(60.7245776942905,246.58370639789,23.8563427002747)) ;
#110062 = CARTESIAN_POINT('Ctrl Pts',(60.7215862988884,246.616128349212,23.9104986900731)) ;
#110063 = CARTESIAN_POINT('Ctrl Pts',(60.7185949034863,246.651426535596,23.9625814565875)) ;
#110064 = CARTESIAN_POINT('Ctrl Pts',(60.7156035080842,246.686724721981,24.0146642231019)) ;
#110065 = CARTESIAN_POINT('Ctrl Pts',(60.712612112682,246.724898729234,24.0646733408183)) ;
#110066 = CARTESIAN_POINT('Ctrl Pts',(60.7096207172799,246.765658802135,24.1122941416385)) ;
#110067 = CARTESIAN_POINT('Ctrl Pts',(60.7067130024914,246.80527866204,24.1585828090228)) ;
#110068 = CARTESIAN_POINT('Ctrl Pts',(60.703805287703,246.847504173481,24.2028048745381)) ;
#110069 = CARTESIAN_POINT('Ctrl Pts',(60.7008975729145,246.892091487186,24.244652841067)) ;
#110070 = CARTESIAN_POINT('Ctrl Pts',(60.6979937914438,246.936618486835,24.2864441991037)) ;
#110071 = CARTESIAN_POINT('Ctrl Pts',(60.6950900099731,246.983500589642,24.32586747502)) ;
#110072 = CARTESIAN_POINT('Ctrl Pts',(60.6921862285023,247.032454689335,24.3626492454181)) ;
#110073 = CARTESIAN_POINT('Ctrl Pts',(60.6892856669198,247.081354505766,24.3993902299686)) ;
#110074 = CARTESIAN_POINT('Ctrl Pts',(60.6863851053373,247.132321354308,24.4334952153625)) ;
#110075 = CARTESIAN_POINT('Ctrl Pts',(60.6834845437548,247.185038029898,24.4647300940279)) ;
#110076 = CARTESIAN_POINT('Ctrl Pts',(60.6819163875053,247.213538712241,24.4816168825995)) ;
#110077 = CARTESIAN_POINT('Ctrl Pts',(60.6803482312557,247.242550279933,24.4976654616331)) ;
#110078 = CARTESIAN_POINT('Ctrl Pts',(60.6787800750062,247.272018954284,24.5128440309778)) ;
#110079 = CARTESIAN_POINT('',(60.9402651077866,247.065925086493,21.6554848536836)) ;
#110080 = CARTESIAN_POINT('Origin',(60.9402651077866,248.040265107786,23.0213203435596)) ;
#110081 = CARTESIAN_POINT('Ctrl Pts',(60.9402651077869,247.065925086493,21.6554848536831)) ;
#110082 = CARTESIAN_POINT('Ctrl Pts',(60.9396867647248,247.055998640425,21.6625660386021)) ;
#110083 = CARTESIAN_POINT('Ctrl Pts',(60.9391145488013,247.046149459394,21.6697553872395)) ;
#110084 = CARTESIAN_POINT('Ctrl Pts',(60.9377470480283,247.022577449097,21.6873587177246)) ;
#110085 = CARTESIAN_POINT('Ctrl Pts',(60.9369572365182,247.008934778977,21.6978780237137)) ;
#110086 = CARTESIAN_POINT('Ctrl Pts',(60.9335105960238,246.949447707252,21.7452246655429)) ;
#110087 = CARTESIAN_POINT('Ctrl Pts',(60.9309500858802,246.905393691192,21.7842389538113)) ;
#110088 = CARTESIAN_POINT('Ctrl Pts',(60.92518819345,246.810011803345,21.8781017813637)) ;
#110089 = CARTESIAN_POINT('Ctrl Pts',(60.9220089750807,246.760135358974,21.9342418382204)) ;
#110090 = CARTESIAN_POINT('Ctrl Pts',(60.9170000430791,246.689467121177,22.0254199173532)) ;
#110091 = CARTESIAN_POINT('Ctrl Pts',(60.9152280878726,246.665910284633,22.0581892549186)) ;
#110092 = CARTESIAN_POINT('Ctrl Pts',(60.9119646114264,246.625515443228,22.1188853236253)) ;
#110093 = CARTESIAN_POINT('Ctrl Pts',(60.910485682088,246.608266535942,22.1465143478789)) ;
#110094 = CARTESIAN_POINT('Ctrl Pts',(60.9080063213577,246.581193941108,22.1928272329416)) ;
#110095 = CARTESIAN_POINT('Ctrl Pts',(60.9070213098529,246.570899078315,22.211225946749)) ;
#110096 = CARTESIAN_POINT('Ctrl Pts',(60.9050354726144,246.551079395075,22.2482685496161)) ;
#110097 = CARTESIAN_POINT('Ctrl Pts',(60.9040349879792,246.541551405675,22.26690642732)) ;
#110098 = CARTESIAN_POINT('Ctrl Pts',(60.9015011388585,246.518574142374,22.3140068144291)) ;
#110099 = CARTESIAN_POINT('Ctrl Pts',(60.8999537124246,246.505572902896,22.342677947094)) ;
#110100 = CARTESIAN_POINT('Ctrl Pts',(60.891820612325,246.442540613751,22.4927699565146)) ;
#110101 = CARTESIAN_POINT('Ctrl Pts',(60.8848046578023,246.406091410028,22.6193796112316)) ;
#110102 = CARTESIAN_POINT('Ctrl Pts',(60.873091660205,246.370638855896,22.8348390986218)) ;
#110103 = CARTESIAN_POINT('Ctrl Pts',(60.8684410143515,246.363210501457,22.9217354108926)) ;
#110104 = CARTESIAN_POINT('Ctrl Pts',(60.8631745389201,246.362429865603,23.0265114899575)) ;
#110105 = CARTESIAN_POINT('Ctrl Pts',(60.8622971625612,246.362577881107,23.0442040284292)) ;
#110106 = CARTESIAN_POINT('Ctrl Pts',(60.860896988545,246.363271947923,23.0728975400407)) ;
#110107 = CARTESIAN_POINT('Ctrl Pts',(60.8603654784424,246.363646504033,23.0839009961984)) ;
#110108 = CARTESIAN_POINT('Ctrl Pts',(60.8592973572389,246.364628201922,23.1062638624013)) ;
#110109 = CARTESIAN_POINT('Ctrl Pts',(60.8587611606733,246.36524260645,23.1176223426978)) ;
#110110 = CARTESIAN_POINT('Ctrl Pts',(60.8573069279922,246.367244052481,23.14875000601)) ;
#110111 = CARTESIAN_POINT('Ctrl Pts',(60.8564009465218,246.368865938047,23.168502693823)) ;
#110112 = CARTESIAN_POINT('Ctrl Pts',(60.852477944768,246.377539470122,23.2552590034297)) ;
#110113 = CARTESIAN_POINT('Ctrl Pts',(60.8496135629811,246.388273699,23.3218357141254)) ;
#110114 = CARTESIAN_POINT('Ctrl Pts',(60.8443246245783,246.415756471825,23.4446878375553)) ;
#110115 = CARTESIAN_POINT('Ctrl Pts',(60.841895438994,246.431507497226,23.5010778840882)) ;
#110116 = CARTESIAN_POINT('Ctrl Pts',(60.8363359680186,246.473521197085,23.6258994598745)) ;
#110117 = CARTESIAN_POINT('Ctrl Pts',(60.8331866541431,246.501383272451,23.6936624628327)) ;
#110118 = CARTESIAN_POINT('Ctrl Pts',(60.8287680082623,246.544564766011,23.7818130819286)) ;
#110119 = CARTESIAN_POINT('Ctrl Pts',(60.8276280218364,246.556049771089,23.8039910764275)) ;
#110120 = CARTESIAN_POINT('Ctrl Pts',(60.8256301604299,246.576719212668,23.8418123561527)) ;
#110121 = CARTESIAN_POINT('Ctrl Pts',(60.8247807287349,246.585670321803,23.8575785016638)) ;
#110122 = CARTESIAN_POINT('Ctrl Pts',(60.8230019298047,246.604733888494,23.8899239347454)) ;
#110123 = CARTESIAN_POINT('Ctrl Pts',(60.8220713071847,246.614882187956,23.9064788446261)) ;
#110124 = CARTESIAN_POINT('Ctrl Pts',(60.8195773404605,246.642520506606,23.9498569892743)) ;
#110125 = CARTESIAN_POINT('Ctrl Pts',(60.8179957968244,246.66049440445,23.9763611276772)) ;
#110126 = CARTESIAN_POINT('Ctrl Pts',(60.8096084557132,246.75807404293,24.1117423521865)) ;
#110127 = CARTESIAN_POINT('Ctrl Pts',(60.8023153144641,246.849829528678,24.2112309089791)) ;
#110128 = CARTESIAN_POINT('Ctrl Pts',(60.792432542256,246.990100397675,24.3306869456728)) ;
#110129 = CARTESIAN_POINT('Ctrl Pts',(60.7898016721395,247.029119870425,24.3610488833073)) ;
#110130 = CARTESIAN_POINT('Ctrl Pts',(60.7861158787418,247.087115783232,24.4021975944882)) ;
#110131 = CARTESIAN_POINT('Ctrl Pts',(60.7850053541749,247.105049846946,24.4144061643936)) ;
#110132 = CARTESIAN_POINT('Ctrl Pts',(60.7830396281911,247.137750903115,24.4357511248514)) ;
#110133 = CARTESIAN_POINT('Ctrl Pts',(60.7821778845666,247.152432438562,24.4450125580265)) ;
#110134 = CARTESIAN_POINT('Ctrl Pts',(60.7808134620318,247.176302589428,24.4595574822181)) ;
#110135 = CARTESIAN_POINT('Ctrl Pts',(60.7803018029719,247.18540183663,24.4649844698352)) ;
#110136 = CARTESIAN_POINT('Ctrl Pts',(60.779265837799,247.20414302895,24.4759227777364)) ;
#110137 = CARTESIAN_POINT('Ctrl Pts',(60.7787419818932,247.213789109344,24.4814250688233)) ;
#110138 = CARTESIAN_POINT('Ctrl Pts',(60.7773672882245,247.239521947716,24.4957667959593)) ;
#110139 = CARTESIAN_POINT('Ctrl Pts',(60.7765263339732,247.255700655054,24.5044388874851)) ;
#110140 = CARTESIAN_POINT('Ctrl Pts',(60.7756980793889,247.272018954284,24.5128440309776)) ;
#110141 = CARTESIAN_POINT('Origin',(61.8645744874958,248.040265107786,23.0213203435596)) ;
#110142 = CARTESIAN_POINT('',(60.178415027332,247.272018800728,24.5128439518851)) ;
#110143 = CARTESIAN_POINT('',(60.2784744057375,247.272018982637,24.5128440455817)) ;
#110144 = CARTESIAN_POINT('',(61.8645744874958,247.272018954284,24.5128440309778)) ;
#110145 = CARTESIAN_POINT('',(60.5159557281095,249.718015041886,23.0217905853416)) ;
#110146 = CARTESIAN_POINT('Ctrl Pts',(60.178415027332,247.272018800728,24.5128439518851)) ;
#110147 = CARTESIAN_POINT('Ctrl Pts',(60.1811705889247,247.213831808876,24.4828732954635)) ;
#110148 = CARTESIAN_POINT('Ctrl Pts',(60.1839757745729,247.157415788768,24.4495065124652)) ;
#110149 = CARTESIAN_POINT('Ctrl Pts',(60.1882301766301,247.078122707203,24.3961045007148)) ;
#110150 = CARTESIAN_POINT('Ctrl Pts',(60.1895902049024,247.053635880327,24.3786383312463)) ;
#110151 = CARTESIAN_POINT('Ctrl Pts',(60.191868695306,247.014142009741,24.3488342070395)) ;
#110152 = CARTESIAN_POINT('Ctrl Pts',(60.1927724821908,246.998855964066,24.3368767384678)) ;
#110153 = CARTESIAN_POINT('Ctrl Pts',(60.1945815551,246.969028882844,24.3126989245764)) ;
#110154 = CARTESIAN_POINT('Ctrl Pts',(60.1954862600071,246.954481119213,24.300491474847)) ;
#110155 = CARTESIAN_POINT('Ctrl Pts',(60.1977392628852,246.919169348636,24.2698238983159)) ;
#110156 = CARTESIAN_POINT('Ctrl Pts',(60.1990987197496,246.898651165582,24.2510903713293)) ;
#110157 = CARTESIAN_POINT('Ctrl Pts',(60.2059852468756,246.798617310351,24.1550957229905)) ;
#110158 = CARTESIAN_POINT('Ctrl Pts',(60.2118247025089,246.726441138572,24.0706042579183)) ;
#110159 = CARTESIAN_POINT('Ctrl Pts',(60.2224827440213,246.612126515002,23.9063284304355)) ;
#110160 = CARTESIAN_POINT('Ctrl Pts',(60.2272541985357,246.567051464706,23.8290718136566)) ;
#110161 = CARTESIAN_POINT('Ctrl Pts',(60.2327745233088,246.519648160462,23.7305248824824)) ;
#110162 = CARTESIAN_POINT('Ctrl Pts',(60.2337724854315,246.511281990191,23.7123034604854)) ;
#110163 = CARTESIAN_POINT('Ctrl Pts',(60.2353124276838,246.498653815277,23.6834463022867)) ;
#110164 = CARTESIAN_POINT('Ctrl Pts',(60.2358663507129,246.494170896116,23.6729098345444)) ;
#110165 = CARTESIAN_POINT('Ctrl Pts',(60.2369372579101,246.485611802032,23.6522071026085)) ;
#110166 = CARTESIAN_POINT('Ctrl Pts',(60.2374546879911,246.481526686834,23.6420453585046)) ;
#110167 = CARTESIAN_POINT('Ctrl Pts',(60.2387894501942,246.471135165012,23.6154467612984)) ;
#110168 = CARTESIAN_POINT('Ctrl Pts',(60.239597986921,246.464987280693,23.5989489330212)) ;
#110169 = CARTESIAN_POINT('Ctrl Pts',(60.2441819501055,246.431114055562,23.5034842683512)) ;
#110170 = CARTESIAN_POINT('Ctrl Pts',(60.2476991211754,246.409066403289,23.4226211171969)) ;
#110171 = CARTESIAN_POINT('Ctrl Pts',(60.2560977517516,246.370794914273,23.2250876269592)) ;
#110172 = CARTESIAN_POINT('Ctrl Pts',(60.260953232974,246.360625820245,23.1077034773157)) ;
#110173 = CARTESIAN_POINT('Ctrl Pts',(60.2675013718757,246.36334880304,22.9607937346077)) ;
#110174 = CARTESIAN_POINT('Ctrl Pts',(60.268834271811,246.364669003289,22.9313795871221)) ;
#110175 = CARTESIAN_POINT('Ctrl Pts',(60.2710798620106,246.368133877454,22.8827770579642)) ;
#110176 = CARTESIAN_POINT('Ctrl Pts',(60.2719787780596,246.36983708027,22.8635633732702)) ;
#110177 = CARTESIAN_POINT('Ctrl Pts',(60.2737879069914,246.373883861288,22.8254049236208)) ;
#110178 = CARTESIAN_POINT('Ctrl Pts',(60.2746977671713,246.376220246872,22.806462310032)) ;
#110179 = CARTESIAN_POINT('Ctrl Pts',(60.2769831638854,246.382825443789,22.7595169007374)) ;
#110180 = CARTESIAN_POINT('Ctrl Pts',(60.2783705875292,246.387481110738,22.7315752457179)) ;
#110181 = CARTESIAN_POINT('Ctrl Pts',(60.2842982973178,246.410041152097,22.6145372652656)) ;
#110182 = CARTESIAN_POINT('Ctrl Pts',(60.2890358102792,246.434459543021,22.5268631904767)) ;
#110183 = CARTESIAN_POINT('Ctrl Pts',(60.2996583956505,246.503619773932,22.3390349618594)) ;
#110184 = CARTESIAN_POINT('Ctrl Pts',(60.3055593102924,246.551321389504,22.2403974576678)) ;
#110185 = CARTESIAN_POINT('Ctrl Pts',(60.3120451237019,246.618380286035,22.130554177403)) ;
#110186 = CARTESIAN_POINT('Ctrl Pts',(60.31300866222,246.628767127593,22.1141851172961)) ;
#110187 = CARTESIAN_POINT('Ctrl Pts',(60.3145080453651,246.645662011748,22.0885528124602)) ;
#110188 = CARTESIAN_POINT('Ctrl Pts',(60.3150548807429,246.651983874632,22.0791694567574)) ;
#110189 = CARTESIAN_POINT('Ctrl Pts',(60.3161235023812,246.664671823486,22.0607421463588)) ;
#110190 = CARTESIAN_POINT('Ctrl Pts',(60.3166455009921,246.671033320294,22.051695840326)) ;
#110191 = CARTESIAN_POINT('Ctrl Pts',(60.3180089703817,246.688064867842,22.027978185396)) ;
#110192 = CARTESIAN_POINT('Ctrl Pts',(60.3188409069329,246.698884480097,22.0134154920811)) ;
#110193 = CARTESIAN_POINT('Ctrl Pts',(60.3206890541358,246.723812832313,21.9809757150205)) ;
#110194 = CARTESIAN_POINT('Ctrl Pts',(60.3216979336936,246.738053743316,21.963204484442)) ;
#110195 = CARTESIAN_POINT('Ctrl Pts',(60.3250061150887,246.78661993943,21.905064935095)) ;
#110196 = CARTESIAN_POINT('Ctrl Pts',(60.3272403118247,246.822496100017,21.8660318697313)) ;
#110197 = CARTESIAN_POINT('Ctrl Pts',(60.3347604134617,246.950303633682,21.7395591581177)) ;
#110198 = CARTESIAN_POINT('Ctrl Pts',(60.3399709896441,247.050262283888,21.6608716316085)) ;
#110199 = CARTESIAN_POINT('Ctrl Pts',(60.3469015939312,247.182198562016,21.5793191472611)) ;
#110200 = CARTESIAN_POINT('Ctrl Pts',(60.3481854385056,247.206638058707,21.5650540615996)) ;
#110201 = CARTESIAN_POINT('Ctrl Pts',(60.3502840909381,247.246474995144,21.5431331519946)) ;
#110202 = CARTESIAN_POINT('Ctrl Pts',(60.351084852309,247.26165011277,21.5350838953927)) ;
#110203 = CARTESIAN_POINT('Ctrl Pts',(60.3527858571736,247.293810892603,21.5186527685344)) ;
#110204 = CARTESIAN_POINT('Ctrl Pts',(60.3536877568611,247.310820195851,21.5103227191475)) ;
#110205 = CARTESIAN_POINT('Ctrl Pts',(60.3559229685263,247.352848697118,21.4906149504757)) ;
#110206 = CARTESIAN_POINT('Ctrl Pts',(60.3572670441465,247.378012866435,21.4795609001742)) ;
#110207 = CARTESIAN_POINT('Ctrl Pts',(60.3634639044702,247.493513829258,21.4321734444685)) ;
#110208 = CARTESIAN_POINT('Ctrl Pts',(60.3685504548122,247.586627091968,21.403132035691)) ;
#110209 = CARTESIAN_POINT('Ctrl Pts',(60.3793636933516,247.785424136848,21.35964350066)) ;
#110210 = CARTESIAN_POINT('Ctrl Pts',(60.3850818917271,247.891049231485,21.3468501489587)) ;
#110211 = CARTESIAN_POINT('Ctrl Pts',(60.3913544923533,248.015741089614,21.3436468202095)) ;
#110212 = CARTESIAN_POINT('Ctrl Pts',(60.3922758013978,248.034311530069,21.3434781326632)) ;
#110213 = CARTESIAN_POINT('Ctrl Pts',(60.393725341286,248.064027634494,21.3437016008822)) ;
#110214 = CARTESIAN_POINT('Ctrl Pts',(60.39426343295,248.075172867825,21.3438964955723)) ;
#110215 = CARTESIAN_POINT('Ctrl Pts',(60.395330569705,248.097531247299,21.3445104150266)) ;
#110216 = CARTESIAN_POINT('Ctrl Pts',(60.3958595175572,248.108743767186,21.3449308801168)) ;
#110217 = CARTESIAN_POINT('Ctrl Pts',(60.3972650958725,248.138851398337,21.3463624875682)) ;
#110218 = CARTESIAN_POINT('Ctrl Pts',(60.3981310897179,248.157735420768,21.3475808617472)) ;
#110219 = CARTESIAN_POINT('Ctrl Pts',(60.4024502929226,248.253264443539,21.3553690986169)) ;
#110220 = CARTESIAN_POINT('Ctrl Pts',(60.4056949701534,248.329419110123,21.3668856789759)) ;
#110221 = CARTESIAN_POINT('Ctrl Pts',(60.4140548037342,248.524691430933,21.4103169502864)) ;
#110222 = CARTESIAN_POINT('Ctrl Pts',(60.4191244793235,248.641547874058,21.4501875437323)) ;
#110223 = CARTESIAN_POINT('Ctrl Pts',(60.425903326889,248.779041935032,21.5147075856406)) ;
#110224 = CARTESIAN_POINT('Ctrl Pts',(60.4272078751849,248.804773819481,21.5276003158052)) ;
#110225 = CARTESIAN_POINT('Ctrl Pts',(60.429419345957,248.84707229154,21.5501729392805)) ;
#110226 = CARTESIAN_POINT('Ctrl Pts',(60.4303134226966,248.863827613651,21.559486810022)) ;
#110227 = CARTESIAN_POINT('Ctrl Pts',(60.4321238349279,248.897042112574,21.5787022282945)) ;
#110228 = CARTESIAN_POINT('Ctrl Pts',(60.433040071941,248.913498152863,21.5886033882758)) ;
#110229 = CARTESIAN_POINT('Ctrl Pts',(60.4353642952565,248.954343588767,21.6141441399071)) ;
#110230 = CARTESIAN_POINT('Ctrl Pts',(60.436785047033,248.97850398986,21.6301366714241)) ;
#110231 = CARTESIAN_POINT('Ctrl Pts',(60.4421684081947,249.067064902063,21.6921145110272)) ;
#110232 = CARTESIAN_POINT('Ctrl Pts',(60.4462721951324,249.128595431866,21.7420076747762)) ;
#110233 = CARTESIAN_POINT('Ctrl Pts',(60.4568123768335,249.274166564319,21.8781736391898)) ;
#110234 = CARTESIAN_POINT('Ctrl Pts',(60.4633375740573,249.352881552832,21.9694950356638)) ;
#110235 = CARTESIAN_POINT('Ctrl Pts',(60.4703539246244,249.432010599461,22.0841680348933)) ;
#110236 = CARTESIAN_POINT('Ctrl Pts',(60.4713028533939,249.442590869066,22.1000752741307)) ;
#110237 = CARTESIAN_POINT('Ctrl Pts',(60.4727850108929,249.458970246633,22.1256376491726)) ;
#110238 = CARTESIAN_POINT('Ctrl Pts',(60.4733288340088,249.464947581473,22.1351760989331)) ;
#110239 = CARTESIAN_POINT('Ctrl Pts',(60.4743964479814,249.476629760029,22.1542419506994)) ;
#110240 = CARTESIAN_POINT('Ctrl Pts',(60.474920351834,249.482336882512,22.1637672198921)) ;
#110241 = CARTESIAN_POINT('Ctrl Pts',(60.4762964678703,249.497238432476,22.1892076156252)) ;
#110242 = CARTESIAN_POINT('Ctrl Pts',(60.4771388026686,249.50626683707,22.2052187333813)) ;
#110243 = CARTESIAN_POINT('Ctrl Pts',(60.4814826501672,249.552151512365,22.2898109894164)) ;
#110244 = CARTESIAN_POINT('Ctrl Pts',(60.4847667762189,249.584466937395,22.3607531136743)) ;
#110245 = CARTESIAN_POINT('Ctrl Pts',(60.4908119799773,249.635139035958,22.4962628569805)) ;
#110246 = CARTESIAN_POINT('Ctrl Pts',(60.4935758249554,249.654779644228,22.5601794688302)) ;
#110247 = CARTESIAN_POINT('Ctrl Pts',(60.4991576355374,249.68587489522,22.6881228634387)) ;
#110248 = CARTESIAN_POINT('Ctrl Pts',(60.5019671094267,249.697524210488,22.7519813499238)) ;
#110249 = CARTESIAN_POINT('Ctrl Pts',(60.5059970770317,249.708452116705,22.8407600485552)) ;
#110250 = CARTESIAN_POINT('Ctrl Pts',(60.5071204011434,249.710919546307,22.8652319318812)) ;
#110251 = CARTESIAN_POINT('Ctrl Pts',(60.5091055429909,249.714277774323,22.9079227996584)) ;
#110252 = CARTESIAN_POINT('Ctrl Pts',(60.5099596821151,249.715411080149,22.9261187119359)) ;
#110253 = CARTESIAN_POINT('Ctrl Pts',(60.5114560893805,249.716860866305,22.9576783431437)) ;
#110254 = CARTESIAN_POINT('Ctrl Pts',(60.5120939908299,249.717314580784,22.9710342204351)) ;
#110255 = CARTESIAN_POINT('Ctrl Pts',(60.5133377228246,249.717883585693,22.9968806246684)) ;
#110256 = CARTESIAN_POINT('Ctrl Pts',(60.513942882745,249.718019031575,23.0093697979911)) ;
#110257 = CARTESIAN_POINT('Ctrl Pts',(60.5145522989917,249.718015021295,23.0218590659304)) ;
#110258 = CARTESIAN_POINT('Ctrl Pts',(60.6787800750062,247.272018954284,24.5128440309778)) ;
#110259 = CARTESIAN_POINT('Ctrl Pts',(60.6758817378808,247.326484287654,24.5408977475989)) ;
#110260 = CARTESIAN_POINT('Ctrl Pts',(60.6729834007554,247.382512350534,24.5659766848025)) ;
#110261 = CARTESIAN_POINT('Ctrl Pts',(60.67008506363,247.439744604203,24.5879154371548)) ;
#110262 = CARTESIAN_POINT('Ctrl Pts',(60.6671868492106,247.496974434847,24.6098532606924)) ;
#110263 = CARTESIAN_POINT('Ctrl Pts',(60.6642886347913,247.55540787763,24.6286509827448)) ;
#110264 = CARTESIAN_POINT('Ctrl Pts',(60.6613904203719,247.61466777786,24.6441918650485)) ;
#110265 = CARTESIAN_POINT('Ctrl Pts',(60.6584892760978,247.673987584943,24.6597484578976)) ;
#110266 = CARTESIAN_POINT('Ctrl Pts',(60.6555881318236,247.734135022389,24.6720415091348)) ;
#110267 = CARTESIAN_POINT('Ctrl Pts',(60.6526869875494,247.794720421271,24.6810049128149)) ;
#110268 = CARTESIAN_POINT('Ctrl Pts',(60.6497842408534,247.855339283972,24.6899732673532)) ;
#110269 = CARTESIAN_POINT('Ctrl Pts',(60.6468814941574,247.916396080965,24.6956082659881)) ;
#110270 = CARTESIAN_POINT('Ctrl Pts',(60.6439787474614,247.977496717446,24.6978957792839)) ;
#110271 = CARTESIAN_POINT('Ctrl Pts',(60.641070832045,248.038706151607,24.7001873657965)) ;
#110272 = CARTESIAN_POINT('Ctrl Pts',(60.6381629166285,248.099959070422,24.6991195769611)) ;
#110273 = CARTESIAN_POINT('Ctrl Pts',(60.6352550012121,248.160863169467,24.6947303859637)) ;
#110274 = CARTESIAN_POINT('Ctrl Pts',(60.6336687579062,248.194085841236,24.6923361193359)) ;
#110275 = CARTESIAN_POINT('Ctrl Pts',(60.6320825146003,248.227204831506,24.6889544394523)) ;
#110276 = CARTESIAN_POINT('Ctrl Pts',(60.6304962712944,248.260157771901,24.684597914733)) ;
#110277 = CARTESIAN_POINT('Ctrl Pts',(60.627587417587,248.320586889225,24.6766089176896)) ;
#110278 = CARTESIAN_POINT('Ctrl Pts',(60.6246785638795,248.38070298245,24.6653061876332)) ;
#110279 = CARTESIAN_POINT('Ctrl Pts',(60.6217697101721,248.440114926134,24.6507267340181)) ;
#110280 = CARTESIAN_POINT('Ctrl Pts',(60.6188364649694,248.500025054425,24.6360250278909)) ;
#110281 = CARTESIAN_POINT('Ctrl Pts',(60.6159032197668,248.559218639349,24.6179913754864)) ;
#110282 = CARTESIAN_POINT('Ctrl Pts',(60.6129699745642,248.617300469956,24.5967171993725)) ;
#110283 = CARTESIAN_POINT('Ctrl Pts',(60.6100690397587,248.674742515314,24.5756773633943)) ;
#110284 = CARTESIAN_POINT('Ctrl Pts',(60.6071681049532,248.731096683785,24.5514682099505)) ;
#110285 = CARTESIAN_POINT('Ctrl Pts',(60.6042671701477,248.78599392584,24.52422872148)) ;
#110286 = CARTESIAN_POINT('Ctrl Pts',(60.6013679874107,248.840858011781,24.497005684758)) ;
#110287 = CARTESIAN_POINT('Ctrl Pts',(60.5984688046737,248.894266459826,24.4667561685163)) ;
#110288 = CARTESIAN_POINT('Ctrl Pts',(60.5955696219366,248.94587133027,24.4336667714231)) ;
#110289 = CARTESIAN_POINT('Ctrl Pts',(60.5926711203359,248.997464076625,24.4005851483787)) ;
#110290 = CARTESIAN_POINT('Ctrl Pts',(60.5897726187351,249.047253657176,24.3646652444936)) ;
#110291 = CARTESIAN_POINT('Ctrl Pts',(60.5868741171344,249.094919624155,24.3261379222279)) ;
#110292 = CARTESIAN_POINT('Ctrl Pts',(60.5839155928156,249.143572666972,24.2868127689035)) ;
#110293 = CARTESIAN_POINT('Ctrl Pts',(60.5809570684968,249.190012693819,24.244771299182)) ;
#110294 = CARTESIAN_POINT('Ctrl Pts',(60.577998544178,249.233934908198,24.2003018828912)) ;
#110295 = CARTESIAN_POINT('Ctrl Pts',(60.5750963603741,249.27702069201,24.1566793177811)) ;
#110296 = CARTESIAN_POINT('Ctrl Pts',(60.5721941765702,249.317683431554,24.1107209130333)) ;
#110297 = CARTESIAN_POINT('Ctrl Pts',(60.5692919927664,249.355674923129,24.0627338446237)) ;
#110298 = CARTESIAN_POINT('Ctrl Pts',(60.5663052981901,249.394772716206,24.0133494063403)) ;
#110299 = CARTESIAN_POINT('Ctrl Pts',(60.5633186036139,249.431040904279,23.9618167711563)) ;
#110300 = CARTESIAN_POINT('Ctrl Pts',(60.5603319090376,249.464257260494,23.9085020676312)) ;
#110301 = CARTESIAN_POINT('Ctrl Pts',(60.5573452144614,249.497473616709,23.8551873641062)) ;
#110302 = CARTESIAN_POINT('Ctrl Pts',(60.5543585198851,249.527637922912,23.8000911356975)) ;
#110303 = CARTESIAN_POINT('Ctrl Pts',(60.5513718253088,249.554580836769,23.7436034843402)) ;
#110304 = CARTESIAN_POINT('Ctrl Pts',(60.5482383900215,249.582847495735,23.6843405113292)) ;
#110305 = CARTESIAN_POINT('Ctrl Pts',(60.5451049547341,249.60767069774,23.6233339249503)) ;
#110306 = CARTESIAN_POINT('Ctrl Pts',(60.5419715194467,249.628850532698,23.5609882138808)) ;
#110307 = CARTESIAN_POINT('Ctrl Pts',(60.5388459790484,249.649977003717,23.4987995867887)) ;
#110308 = CARTESIAN_POINT('Ctrl Pts',(60.5357204386502,249.667478246505,23.4352789068086)) ;
#110309 = CARTESIAN_POINT('Ctrl Pts',(60.5325948982519,249.681201746002,23.3708514750201)) ;
#110310 = CARTESIAN_POINT('Ctrl Pts',(60.5294814213625,249.694872277521,23.3066727109147)) ;
#110311 = CARTESIAN_POINT('Ctrl Pts',(60.526367944473,249.704794021286,23.2415945367422)) ;
#110312 = CARTESIAN_POINT('Ctrl Pts',(60.5232544675836,249.710864391968,23.1760559056965)) ;
#110313 = CARTESIAN_POINT('Ctrl Pts',(60.5208215544255,249.715607862124,23.124843128634)) ;
#110314 = CARTESIAN_POINT('Ctrl Pts',(60.5183886412675,249.718000590858,23.0733496192864)) ;
#110315 = CARTESIAN_POINT('Ctrl Pts',(60.5159557281095,249.718015041886,23.0217905853416)) ;
#110316 = CARTESIAN_POINT('Ctrl Pts',(60.7756980793889,247.272018954284,24.5128440309776)) ;
#110317 = CARTESIAN_POINT('Ctrl Pts',(60.7756882950196,247.27221172625,24.512943322945)) ;
#110318 = CARTESIAN_POINT('Ctrl Pts',(60.7756785124232,247.272404517696,24.5130425776592)) ;
#110319 = CARTESIAN_POINT('Ctrl Pts',(60.7708844068105,247.36691143135,24.5616743441787)) ;
#110320 = CARTESIAN_POINT('Ctrl Pts',(60.7665244328513,247.465624464848,24.601158305853)) ;
#110321 = CARTESIAN_POINT('Ctrl Pts',(60.758085179004,247.659911268451,24.6582291111127)) ;
#110322 = CARTESIAN_POINT('Ctrl Pts',(60.75403018082,247.754575228724,24.6773755531183)) ;
#110323 = CARTESIAN_POINT('Ctrl Pts',(60.7484518396211,247.878663337132,24.6915124855888)) ;
#110324 = CARTESIAN_POINT('Ctrl Pts',(60.7471593590571,247.907049901099,24.6940159297791)) ;
#110325 = CARTESIAN_POINT('Ctrl Pts',(60.7449585594767,247.954650642069,24.6969945255557)) ;
#110326 = CARTESIAN_POINT('Ctrl Pts',(60.7440625699028,247.973834394399,24.6978646242705)) ;
#110327 = CARTESIAN_POINT('Ctrl Pts',(60.7422396821312,248.012442664656,24.6989520631554)) ;
#110328 = CARTESIAN_POINT('Ctrl Pts',(60.7413126878787,248.031864424137,24.6991617141892)) ;
#110329 = CARTESIAN_POINT('Ctrl Pts',(60.7389405694075,248.081009530957,24.6988389103594)) ;
#110330 = CARTESIAN_POINT('Ctrl Pts',(60.737481838675,248.110722385268,24.697853756757)) ;
#110331 = CARTESIAN_POINT('Ctrl Pts',(60.732081154403,248.218891572664,24.6913867519337)) ;
#110332 = CARTESIAN_POINT('Ctrl Pts',(60.7280040725607,248.296956449574,24.6811807978971)) ;
#110333 = CARTESIAN_POINT('Ctrl Pts',(60.7195223545697,248.454473878442,24.6492076559596)) ;
#110334 = CARTESIAN_POINT('Ctrl Pts',(60.7151227743156,248.533628491368,24.6269911287199)) ;
#110335 = CARTESIAN_POINT('Ctrl Pts',(60.7093542847243,248.63776696951,24.5893307269102)) ;
#110336 = CARTESIAN_POINT('Ctrl Pts',(60.7078792233013,248.664442732654,24.5789041953016)) ;
#110337 = CARTESIAN_POINT('Ctrl Pts',(60.7053441390305,248.710645677828,24.5594674962714)) ;
#110338 = CARTESIAN_POINT('Ctrl Pts',(60.7042726836258,248.730290814842,24.5507553276267)) ;
#110339 = CARTESIAN_POINT('Ctrl Pts',(60.7026417578212,248.760491106601,24.5366617922452)) ;
#110340 = CARTESIAN_POINT('Ctrl Pts',(60.7020685170289,248.771165296168,24.5315422229156)) ;
#110341 = CARTESIAN_POINT('Ctrl Pts',(60.7009860921404,248.791459879833,24.5215429307525)) ;
#110342 = CARTESIAN_POINT('Ctrl Pts',(60.7004759211982,248.801088817705,24.5166827345866)) ;
#110343 = CARTESIAN_POINT('Ctrl Pts',(60.6991765729357,248.825751476529,24.5039343993476)) ;
#110344 = CARTESIAN_POINT('Ctrl Pts',(60.6983953249766,248.840713921812,24.4959101197923)) ;
#110345 = CARTESIAN_POINT('Ctrl Pts',(60.694546708812,248.91486447455,24.4546822810237)) ;
#110346 = CARTESIAN_POINT('Ctrl Pts',(60.6916476221793,248.972125779834,24.4181337118554)) ;
#110347 = CARTESIAN_POINT('Ctrl Pts',(60.6848564495383,249.102774253487,24.3231241485434)) ;
#110348 = CARTESIAN_POINT('Ctrl Pts',(60.6810107040293,249.173781445533,24.2617878033091)) ;
#110349 = CARTESIAN_POINT('Ctrl Pts',(60.6753721079551,249.265790247043,24.1677790671748)) ;
#110350 = CARTESIAN_POINT('Ctrl Pts',(60.6737241419899,249.291356368138,24.1398237805439)) ;
#110351 = CARTESIAN_POINT('Ctrl Pts',(60.6706628629479,249.336101441456,24.087442050423)) ;
#110352 = CARTESIAN_POINT('Ctrl Pts',(60.6692617156258,249.355590246044,24.0633025612448)) ;
#110353 = CARTESIAN_POINT('Ctrl Pts',(60.6669299425261,249.386315352493,24.0230089552003)) ;
#110354 = CARTESIAN_POINT('Ctrl Pts',(60.6660152281954,249.397956759727,24.0071726021503)) ;
#110355 = CARTESIAN_POINT('Ctrl Pts',(60.6642057547193,249.420168449357,23.9758171969229)) ;
#110356 = CARTESIAN_POINT('Ctrl Pts',(60.6633120699751,249.430761741512,23.960317975081)) ;
#110357 = CARTESIAN_POINT('Ctrl Pts',(60.6611005586341,249.456049589632,23.9219523538644)) ;
#110358 = CARTESIAN_POINT('Ctrl Pts',(60.6597722976602,249.470452514102,23.8989008779105)) ;
#110359 = CARTESIAN_POINT('Ctrl Pts',(60.6517310427637,249.553007381473,23.7593404150994)) ;
#110360 = CARTESIAN_POINT('Ctrl Pts',(60.6445299888298,249.607448218882,23.6353153559151)) ;
#110361 = CARTESIAN_POINT('Ctrl Pts',(60.6347425156901,249.660680397238,23.4589592042698)) ;
#110362 = CARTESIAN_POINT('Ctrl Pts',(60.6321398812924,249.672835583179,23.4111760884053)) ;
#110363 = CARTESIAN_POINT('Ctrl Pts',(60.628473696915,249.687321102699,23.3415226424904)) ;
#110364 = CARTESIAN_POINT('Ctrl Pts',(60.6273600044258,249.691353604983,23.3200339255529)) ;
#110365 = CARTESIAN_POINT('Ctrl Pts',(60.625380552339,249.697874976116,23.2810988537752)) ;
#110366 = CARTESIAN_POINT('Ctrl Pts',(60.624508782199,249.700511158593,23.2636804990575)) ;
#110367 = CARTESIAN_POINT('Ctrl Pts',(60.6231160373809,249.704345382404,23.2353357829859)) ;
#110368 = CARTESIAN_POINT('Ctrl Pts',(60.6225865440398,249.705711213931,23.2244337413542)) ;
#110369 = CARTESIAN_POINT('Ctrl Pts',(60.621518287902,249.708280171311,23.2021562694147)) ;
#110370 = CARTESIAN_POINT('Ctrl Pts',(60.6209800218559,249.709474253776,23.1907804409843)) ;
#110371 = CARTESIAN_POINT('Ctrl Pts',(60.6195120421287,249.712445946117,23.1593798266152)) ;
#110372 = CARTESIAN_POINT('Ctrl Pts',(60.6185947790194,249.713980179265,23.1393334662328)) ;
#110373 = CARTESIAN_POINT('Ctrl Pts',(60.613676389243,249.720375347754,23.0299722824248)) ;
#110374 = CARTESIAN_POINT('Ctrl Pts',(60.609953180776,249.718448519362,22.9403987509123)) ;
#110375 = CARTESIAN_POINT('Ctrl Pts',(60.6016168885664,249.698182982402,22.7413304997973)) ;
#110376 = CARTESIAN_POINT('Ctrl Pts',(60.5970090634153,249.676117704702,22.6326427516485)) ;
#110377 = CARTESIAN_POINT('Ctrl Pts',(60.5908208374004,249.635348857434,22.5004351797759)) ;
#110378 = CARTESIAN_POINT('Ctrl Pts',(60.589561966257,249.626525091478,22.4741524664437)) ;
#110379 = CARTESIAN_POINT('Ctrl Pts',(60.587408304133,249.610591504135,22.4303229589549)) ;
#110380 = CARTESIAN_POINT('Ctrl Pts',(60.5865250345099,249.603828431932,22.4126557428071)) ;
#110381 = CARTESIAN_POINT('Ctrl Pts',(60.5848272278056,249.59041021247,22.3793036862277)) ;
#110382 = CARTESIAN_POINT('Ctrl Pts',(60.5840146965054,249.583812027777,22.3635984316594)) ;
#110383 = CARTESIAN_POINT('Ctrl Pts',(60.5818568407713,249.565836837352,22.3225740722141)) ;
#110384 = CARTESIAN_POINT('Ctrl Pts',(60.5804983637245,249.554068978814,22.2974327967767)) ;
#110385 = CARTESIAN_POINT('Ctrl Pts',(60.5723757747726,249.481108827343,22.1511257064931)) ;
#110386 = CARTESIAN_POINT('Ctrl Pts',(60.5651155371879,249.406023608246,22.0374693238109)) ;
#110387 = CARTESIAN_POINT('Ctrl Pts',(60.5553237484603,249.286704425232,21.8972296846088)) ;
#110388 = CARTESIAN_POINT('Ctrl Pts',(60.552764878943,249.253735585327,21.8617167236432)) ;
#110389 = CARTESIAN_POINT('Ctrl Pts',(60.5491552082394,249.203911859243,21.8125037247045)) ;
#110390 = CARTESIAN_POINT('Ctrl Pts',(60.5480549537141,249.18825634191,21.7976261119993)) ;
#110391 = CARTESIAN_POINT('Ctrl Pts',(60.5460983017611,249.159458036674,21.7712980128618)) ;
#110392 = CARTESIAN_POINT('Ctrl Pts',(60.5452359778907,249.146415803772,21.7597422364009)) ;
#110393 = CARTESIAN_POINT('Ctrl Pts',(60.5438575751423,249.124938523242,21.7413019527496)) ;
#110394 = CARTESIAN_POINT('Ctrl Pts',(60.5433330862607,249.116612465502,21.7342928050292)) ;
#110395 = CARTESIAN_POINT('Ctrl Pts',(60.5422686903961,249.099380095688,21.7200702400599)) ;
#110396 = CARTESIAN_POINT('Ctrl Pts',(60.5417293674013,249.090467056009,21.7128661904103)) ;
#110397 = CARTESIAN_POINT('Ctrl Pts',(60.5402600063694,249.065712958405,21.6932743629481)) ;
#110398 = CARTESIAN_POINT('Ctrl Pts',(60.5393423679675,249.049721558261,21.6810788891601)) ;
#110399 = CARTESIAN_POINT('Ctrl Pts',(60.5344257611681,248.961479629719,21.6162588514937)) ;
#110400 = CARTESIAN_POINT('Ctrl Pts',(60.530703392912,248.88532566335,21.5691808088167)) ;
#110401 = CARTESIAN_POINT('Ctrl Pts',(60.52235692247,248.707133430032,21.4778110470787)) ;
#110402 = CARTESIAN_POINT('Ctrl Pts',(60.5177380727145,248.603721629302,21.4371331550186)) ;
#110403 = CARTESIAN_POINT('Ctrl Pts',(60.5115372780093,248.47037171682,21.39940088093)) ;
#110404 = CARTESIAN_POINT('Ctrl Pts',(60.5102772963219,248.443499761471,21.3925121436769)) ;
#110405 = CARTESIAN_POINT('Ctrl Pts',(60.5081189006906,248.397961592575,21.3820342206756)) ;
#110406 = CARTESIAN_POINT('Ctrl Pts',(60.5072319080356,248.37938247349,21.378090248574)) ;
#110407 = CARTESIAN_POINT('Ctrl Pts',(60.5055247244688,248.343906610515,21.3711867055994)) ;
#110408 = CARTESIAN_POINT('Ctrl Pts',(60.5047065016694,248.327023548782,21.3681691843591)) ;
#110409 = CARTESIAN_POINT('Ctrl Pts',(60.5025272218163,248.282388182096,21.3608957963608)) ;
#110410 = CARTESIAN_POINT('Ctrl Pts',(60.50115271224,248.25457095609,21.3570769278201)) ;
#110411 = CARTESIAN_POINT('Ctrl Pts',(60.4933914856086,248.099375177315,21.3397264348219)) ;
#110412 = CARTESIAN_POINT('Ctrl Pts',(60.4865739325228,247.970881768513,21.3401215126213)) ;
#110413 = CARTESIAN_POINT('Ctrl Pts',(60.4758300255216,247.770272905264,21.3637869690811)) ;
#110414 = CARTESIAN_POINT('Ctrl Pts',(60.4719222587402,247.697486713986,21.3772956834323)) ;
#110415 = CARTESIAN_POINT('Ctrl Pts',(60.467275531377,247.607914624016,21.4001294947751)) ;
#110416 = CARTESIAN_POINT('Ctrl Pts',(60.4663587592489,247.590079746232,21.4049912001505)) ;
#110417 = CARTESIAN_POINT('Ctrl Pts',(60.4649141409273,247.561632340025,21.4132532467426)) ;
#110418 = CARTESIAN_POINT('Ctrl Pts',(60.4643765755097,247.550967348624,21.4164661970968)) ;
#110419 = CARTESIAN_POINT('Ctrl Pts',(60.463308548036,247.529594499147,21.4231378798415)) ;
#110420 = CARTESIAN_POINT('Ctrl Pts',(60.4627782256082,247.518887881234,21.4265985940511)) ;
#110421 = CARTESIAN_POINT('Ctrl Pts',(60.4613649441349,247.490138613034,21.436211748705)) ;
#110422 = CARTESIAN_POINT('Ctrl Pts',(60.4604928148477,247.472164280201,21.4425645297025)) ;
#110423 = CARTESIAN_POINT('Ctrl Pts',(60.4550548068125,247.35904409104,21.4847274998758)) ;
#110424 = CARTESIAN_POINT('Ctrl Pts',(60.4508590982514,247.267202078817,21.5288201309582)) ;
#110425 = CARTESIAN_POINT('Ctrl Pts',(60.4424256144262,247.093567330351,21.6325353855568)) ;
#110426 = CARTESIAN_POINT('Ctrl Pts',(60.4382010448268,247.012039817882,21.6917673475751)) ;
#110427 = CARTESIAN_POINT('Ctrl Pts',(60.4324634142796,246.915504421682,21.7761207598601)) ;
#110428 = CARTESIAN_POINT('Ctrl Pts',(60.4312079239434,246.895149846064,21.7948132941593)) ;
#110429 = CARTESIAN_POINT('Ctrl Pts',(60.4290551255958,246.861616999917,21.8271706465075)) ;
#110430 = CARTESIAN_POINT('Ctrl Pts',(60.4281691054647,246.848191937335,21.8405721136499)) ;
#110431 = CARTESIAN_POINT('Ctrl Pts',(60.4263542050348,246.821467995756,21.8681694834337)) ;
#110432 = CARTESIAN_POINT('Ctrl Pts',(60.4254249473787,246.808183032421,21.8823747666608)) ;
#110433 = CARTESIAN_POINT('Ctrl Pts',(60.4230220527906,246.774854356027,21.9192779390892)) ;
#110434 = CARTESIAN_POINT('Ctrl Pts',(60.4215338158998,246.755173265535,21.9422927057729)) ;
#110435 = CARTESIAN_POINT('Ctrl Pts',(60.4147117881363,246.669233207805,22.0484778426541)) ;
#110436 = CARTESIAN_POINT('Ctrl Pts',(60.4091032168068,246.610355916954,22.1372921443611)) ;
#110437 = CARTESIAN_POINT('Ctrl Pts',(60.3984874373699,246.516465566557,22.3131295558868)) ;
#110438 = CARTESIAN_POINT('Ctrl Pts',(60.3935174048435,246.47954616916,22.398698708304)) ;
#110439 = CARTESIAN_POINT('Ctrl Pts',(60.3879624601977,246.444273578533,22.5036629687607)) ;
#110440 = CARTESIAN_POINT('Ctrl Pts',(60.3870864591605,246.438902991245,22.5205234427913)) ;
#110441 = CARTESIAN_POINT('Ctrl Pts',(60.3856903291533,246.430636301643,22.5479700439543)) ;
#110442 = CARTESIAN_POINT('Ctrl Pts',(60.3851615107751,246.427575638185,22.558504945522)) ;
#110443 = CARTESIAN_POINT('Ctrl Pts',(60.3840945940326,246.421539827396,22.5800676212644)) ;
#110444 = CARTESIAN_POINT('Ctrl Pts',(60.3835569672277,246.418573548026,22.5910971495276)) ;
#110445 = CARTESIAN_POINT('Ctrl Pts',(60.3820976712151,246.410742634974,22.6214472569034)) ;
#110446 = CARTESIAN_POINT('Ctrl Pts',(60.3811881224416,246.406109033969,22.6408259805346)) ;
#110447 = CARTESIAN_POINT('Ctrl Pts',(60.3761759654763,246.382102346082,22.7497721627554)) ;
#110448 = CARTESIAN_POINT('Ctrl Pts',(60.372366129365,246.369746197939,22.8407338175472)) ;
#110449 = CARTESIAN_POINT('Ctrl Pts',(60.3640447714708,246.35914671648,23.0401185575803)) ;
#110450 = CARTESIAN_POINT('Ctrl Pts',(60.3595378802725,246.363842773623,23.1482794770371)) ;
#110451 = CARTESIAN_POINT('Ctrl Pts',(60.3534536156352,246.382818964015,23.2830589160743)) ;
#110452 = CARTESIAN_POINT('Ctrl Pts',(60.352178063071,246.387435369662,23.3107828668696)) ;
#110453 = CARTESIAN_POINT('Ctrl Pts',(60.3500018828507,246.396343500692,23.3570721362936)) ;
#110454 = CARTESIAN_POINT('Ctrl Pts',(60.3491131952654,246.400259152053,23.3757042404542)) ;
#110455 = CARTESIAN_POINT('Ctrl Pts',(60.3473022120707,246.408785382454,23.4131011524053)) ;
#110456 = CARTESIAN_POINT('Ctrl Pts',(60.3463797517914,246.413404740268,23.4318609661218)) ;
#110457 = CARTESIAN_POINT('Ctrl Pts',(60.3440152204185,246.425931961412,23.4791987326212)) ;
#110458 = CARTESIAN_POINT('Ctrl Pts',(60.3425594201409,246.434275134729,23.5076537640707)) ;
#110459 = CARTESIAN_POINT('Ctrl Pts',(60.3353219573036,246.478778390795,23.6457685170047)) ;
#110460 = CARTESIAN_POINT('Ctrl Pts',(60.3292055530495,246.525435192964,23.7517040998283)) ;
#110461 = CARTESIAN_POINT('Ctrl Pts',(60.3185222353801,246.62474042496,23.9259656762753)) ;
#110462 = CARTESIAN_POINT('Ctrl Pts',(60.3139947988517,246.672464682292,23.9966239774957)) ;
#110463 = CARTESIAN_POINT('Ctrl Pts',(60.3088339231225,246.736353482213,24.0772433758745)) ;
#110464 = CARTESIAN_POINT('Ctrl Pts',(60.3079566381448,246.74757744604,24.0909546884778)) ;
#110465 = CARTESIAN_POINT('Ctrl Pts',(60.3065592499092,246.766098866837,24.1128631887207)) ;
#110466 = CARTESIAN_POINT('Ctrl Pts',(60.306030414377,246.77326309095,24.121170924443)) ;
#110467 = CARTESIAN_POINT('Ctrl Pts',(60.3049637958043,246.788046791023,24.1379781333443)) ;
#110468 = CARTESIAN_POINT('Ctrl Pts',(60.3044264739577,246.79567246014,24.1464712165966)) ;
#110469 = CARTESIAN_POINT('Ctrl Pts',(60.3029695896086,246.81681335625,24.1695389282979)) ;
#110470 = CARTESIAN_POINT('Ctrl Pts',(60.3020620702347,246.830502139319,24.1839525835433)) ;
#110471 = CARTESIAN_POINT('Ctrl Pts',(60.2959718241457,246.925568341256,24.2805553744733)) ;
#110472 = CARTESIAN_POINT('Ctrl Pts',(60.2912598309266,247.015006414797,24.3543887465359)) ;
#110473 = CARTESIAN_POINT('Ctrl Pts',(60.2838183154058,247.163121216806,24.4528687515382)) ;
#110474 = CARTESIAN_POINT('Ctrl Pts',(60.281189755399,247.216765758693,24.4843845077685)) ;
#110475 = CARTESIAN_POINT('Ctrl Pts',(60.2784744057375,247.272018982637,24.5128440455817)) ;
#110476 = CARTESIAN_POINT('Origin',(61.8645744874958,248.040265107786,23.0213203435596)) ;
#110477 = CARTESIAN_POINT('',(59.6804129742801,247.272018954245,24.5128440309576)) ;
#110478 = CARTESIAN_POINT('',(59.7780545670443,247.272019328904,24.5128442239351)) ;
#110479 = CARTESIAN_POINT('',(61.8645744874958,247.272018954284,24.5128440309778)) ;
#110480 = CARTESIAN_POINT('Ctrl Pts',(59.6804129742801,247.272018954245,24.5128440309576)) ;
#110481 = CARTESIAN_POINT('Ctrl Pts',(59.6806620543328,247.267515292292,24.5105243085142)) ;
#110482 = CARTESIAN_POINT('Ctrl Pts',(59.680910035148,247.263022056024,24.5081841461442)) ;
#110483 = CARTESIAN_POINT('Ctrl Pts',(59.6816927490163,247.248806677377,24.5006984589357)) ;
#110484 = CARTESIAN_POINT('Ctrl Pts',(59.6822231433743,247.239124257337,24.4954775302037)) ;
#110485 = CARTESIAN_POINT('Ctrl Pts',(59.6832900874761,247.219525017563,24.4846591336161)) ;
#110486 = CARTESIAN_POINT('Ctrl Pts',(59.6838262319107,247.209612530942,24.4790552371634)) ;
#110487 = CARTESIAN_POINT('Ctrl Pts',(59.6852756879414,247.182676206818,24.4634631512753)) ;
#110488 = CARTESIAN_POINT('Ctrl Pts',(59.6861771656862,247.165769965694,24.4532745694072)) ;
#110489 = CARTESIAN_POINT('Ctrl Pts',(59.6912317207679,247.070505234997,24.3935464652148)) ;
#110490 = CARTESIAN_POINT('Ctrl Pts',(59.6950835451313,246.996173230672,24.3378740844751)) ;
#110491 = CARTESIAN_POINT('Ctrl Pts',(59.7034050316022,246.846817675636,24.2053666354242)) ;
#110492 = CARTESIAN_POINT('Ctrl Pts',(59.7078698496296,246.773790947453,24.1269078185332)) ;
#110493 = CARTESIAN_POINT('Ctrl Pts',(59.7139114988955,246.691535368857,24.0196049521105)) ;
#110494 = CARTESIAN_POINT('Ctrl Pts',(59.7151941431971,246.674908651948,23.9967411301763)) ;
#110495 = CARTESIAN_POINT('Ctrl Pts',(59.7173792147044,246.648042166898,23.9577626691775)) ;
#110496 = CARTESIAN_POINT('Ctrl Pts',(59.7182694917991,246.637485331802,23.9418733354475)) ;
#110497 = CARTESIAN_POINT('Ctrl Pts',(59.7200810816836,246.616796745235,23.9095519603271)) ;
#110498 = CARTESIAN_POINT('Ctrl Pts',(59.7210024991347,246.606673098588,23.8931181970382)) ;
#110499 = CARTESIAN_POINT('Ctrl Pts',(59.7233587767216,246.58179563045,23.8511290155879)) ;
#110500 = CARTESIAN_POINT('Ctrl Pts',(59.7248071498076,246.56742869951,23.8253529472319)) ;
#110501 = CARTESIAN_POINT('Ctrl Pts',(59.7321061886695,246.499554335427,23.6956481816735)) ;
#110502 = CARTESIAN_POINT('Ctrl Pts',(59.7383015402635,246.456336543008,23.586715429275)) ;
#110503 = CARTESIAN_POINT('Ctrl Pts',(59.7488672525254,246.402785392522,23.3956896665759)) ;
#110504 = CARTESIAN_POINT('Ctrl Pts',(59.7531996129895,246.386528265154,23.3156811934708)) ;
#110505 = CARTESIAN_POINT('Ctrl Pts',(59.7582610935112,246.373735831642,23.2159636805495)) ;
#110506 = CARTESIAN_POINT('Ctrl Pts',(59.7592044377581,246.371638914121,23.1970830737012)) ;
#110507 = CARTESIAN_POINT('Ctrl Pts',(59.7606799968342,246.368812790461,23.1669857456145)) ;
#110508 = CARTESIAN_POINT('Ctrl Pts',(59.7612226563386,246.367874902904,23.1557906900765)) ;
#110509 = CARTESIAN_POINT('Ctrl Pts',(59.7622903191718,246.366231754429,23.1334866319748)) ;
#110510 = CARTESIAN_POINT('Ctrl Pts',(59.7628153918554,246.36552446292,23.1223783844853)) ;
#110511 = CARTESIAN_POINT('Ctrl Pts',(59.7641978007073,246.363936367739,23.0927975921678)) ;
#110512 = CARTESIAN_POINT('Ctrl Pts',(59.7650451074473,246.363250325296,23.0743157150745)) ;
#110513 = CARTESIAN_POINT('Ctrl Pts',(59.7706993737046,246.360673216758,22.9490355425851)) ;
#110514 = CARTESIAN_POINT('Ctrl Pts',(59.7750907626066,246.368679309752,22.8422695042726)) ;
#110515 = CARTESIAN_POINT('Ctrl Pts',(59.7834881657177,246.402793732002,22.6438876448596)) ;
#110516 = CARTESIAN_POINT('Ctrl Pts',(59.7874663023605,246.426635285591,22.5523160474912)) ;
#110517 = CARTESIAN_POINT('Ctrl Pts',(59.7929599491064,246.467559136449,22.4362924270615)) ;
#110518 = CARTESIAN_POINT('Ctrl Pts',(59.7942559158159,246.47775166217,22.4095905351453)) ;
#110519 = CARTESIAN_POINT('Ctrl Pts',(59.7964569872288,246.495897738814,22.3654693671202)) ;
#110520 = CARTESIAN_POINT('Ctrl Pts',(59.7973495177739,246.503476576124,22.347902162373)) ;
#110521 = CARTESIAN_POINT('Ctrl Pts',(59.799160178796,246.519276040873,22.3129366505932)) ;
#110522 = CARTESIAN_POINT('Ctrl Pts',(59.8000782882456,246.527498858853,22.2955425286946)) ;
#110523 = CARTESIAN_POINT('Ctrl Pts',(59.80241436431,246.548936896717,22.2521415193206)) ;
#110524 = CARTESIAN_POINT('Ctrl Pts',(59.8038453742908,246.562534298642,22.2263313991135)) ;
#110525 = CARTESIAN_POINT('Ctrl Pts',(59.8112745460522,246.63544887219,22.0962678079333)) ;
#110526 = CARTESIAN_POINT('Ctrl Pts',(59.8176397208265,246.705144028713,21.9982486888786)) ;
#110527 = CARTESIAN_POINT('Ctrl Pts',(59.8283536907305,246.838600459491,21.8476695345017)) ;
#110528 = CARTESIAN_POINT('Ctrl Pts',(59.8326672965295,246.89687679133,21.7908248963279)) ;
#110529 = CARTESIAN_POINT('Ctrl Pts',(59.8376454559327,246.972716823504,21.7269072492334)) ;
#110530 = CARTESIAN_POINT('Ctrl Pts',(59.8385308772057,246.986569126506,21.7156062005181)) ;
#110531 = CARTESIAN_POINT('Ctrl Pts',(59.8399380576791,247.00923746462,21.6977085506039)) ;
#110532 = CARTESIAN_POINT('Ctrl Pts',(59.8404687494576,247.017942251053,21.6909737068636)) ;
#110533 = CARTESIAN_POINT('Ctrl Pts',(59.8415356650139,247.035780964374,21.6774505018725)) ;
#110534 = CARTESIAN_POINT('Ctrl Pts',(59.8420714963053,247.044918856245,21.6706685014664)) ;
#110535 = CARTESIAN_POINT('Ctrl Pts',(59.843519053562,247.070064244445,21.6523997850894)) ;
#110536 = CARTESIAN_POINT('Ctrl Pts',(59.8444189982827,247.086206548856,21.6411009646054)) ;
#110537 = CARTESIAN_POINT('Ctrl Pts',(59.8494824127726,247.179598553874,21.5781527210778)) ;
#110538 = CARTESIAN_POINT('Ctrl Pts',(59.8533428632908,247.260840683327,21.5327034850549)) ;
#110539 = CARTESIAN_POINT('Ctrl Pts',(59.8602595992641,247.411897658155,21.4639728176958)) ;
#110540 = CARTESIAN_POINT('Ctrl Pts',(59.8633028648079,247.480262978178,21.4381039762889)) ;
#110541 = CARTESIAN_POINT('Ctrl Pts',(59.8679047265794,247.582156804546,21.4069765648762)) ;
#110542 = CARTESIAN_POINT('Ctrl Pts',(59.8693743103539,247.614505270356,21.3981452235329)) ;
#110543 = CARTESIAN_POINT('Ctrl Pts',(59.8721388166287,247.674660573343,21.3836444393334)) ;
#110544 = CARTESIAN_POINT('Ctrl Pts',(59.8734252273868,247.702388555088,21.3776998364978)) ;
#110545 = CARTESIAN_POINT('Ctrl Pts',(59.8756148182735,247.749015659346,21.3689331905283)) ;
#110546 = CARTESIAN_POINT('Ctrl Pts',(59.8765057288458,247.767836680698,21.3657261115105)) ;
#110547 = CARTESIAN_POINT('Ctrl Pts',(59.8783170323988,247.805769324692,21.3599267655374)) ;
#110548 = CARTESIAN_POINT('Ctrl Pts',(59.8792374941412,247.824879061656,21.3573414655143)) ;
#110549 = CARTESIAN_POINT('Ctrl Pts',(59.8815879433654,247.873235390856,21.3516464227134)) ;
#110550 = CARTESIAN_POINT('Ctrl Pts',(59.883031307828,247.902526281754,21.3489753402142)) ;
#110551 = CARTESIAN_POINT('Ctrl Pts',(59.8903697848691,248.049430745504,21.3394644534301)) ;
#110552 = CARTESIAN_POINT('Ctrl Pts',(59.8966161979755,248.167451889076,21.3442573763587)) ;
#110553 = CARTESIAN_POINT('Ctrl Pts',(59.9072597423143,248.36519220519,21.3732897104311)) ;
#110554 = CARTESIAN_POINT('Ctrl Pts',(59.9116194942626,248.445424895147,21.3911578188894)) ;
#110555 = CARTESIAN_POINT('Ctrl Pts',(59.9166655293252,248.541570827575,21.4201104334586)) ;
#110556 = CARTESIAN_POINT('Ctrl Pts',(59.917573824157,248.559023520705,21.4256792938913)) ;
#110557 = CARTESIAN_POINT('Ctrl Pts',(59.9190079718349,248.586894857967,21.4350782232109)) ;
#110558 = CARTESIAN_POINT('Ctrl Pts',(59.919543347158,248.597372494598,21.4387276849206)) ;
#110559 = CARTESIAN_POINT('Ctrl Pts',(59.9206101519694,248.618421714908,21.4462942877779)) ;
#110560 = CARTESIAN_POINT('Ctrl Pts',(59.9211413817521,248.628991512373,21.4502145634733)) ;
#110561 = CARTESIAN_POINT('Ctrl Pts',(59.9225610680006,248.657440004371,21.4610933589955)) ;
#110562 = CARTESIAN_POINT('Ctrl Pts',(59.9234385048945,248.675240560305,21.4682526295292)) ;
#110563 = CARTESIAN_POINT('Ctrl Pts',(59.9288204001479,248.785351529421,21.5147483001097)) ;
#110564 = CARTESIAN_POINT('Ctrl Pts',(59.9329652812003,248.874108544832,21.5619979734944)) ;
#110565 = CARTESIAN_POINT('Ctrl Pts',(59.9414086583789,249.043646344936,21.6727985130441)) ;
#110566 = CARTESIAN_POINT('Ctrl Pts',(59.9456967805549,249.123887365524,21.7363900494957)) ;
#110567 = CARTESIAN_POINT('Ctrl Pts',(59.9514991253078,249.217684543246,21.8257953187344)) ;
#110568 = CARTESIAN_POINT('Ctrl Pts',(59.9527452136855,249.237061175161,21.8451929321733)) ;
#110569 = CARTESIAN_POINT('Ctrl Pts',(59.9548866111785,249.268997066268,21.8787701020926)) ;
#110570 = CARTESIAN_POINT('Ctrl Pts',(59.9557709119488,249.281807506611,21.8927036162442)) ;
#110571 = CARTESIAN_POINT('Ctrl Pts',(59.9574774542275,249.305796584708,21.9196985519908)) ;
#110572 = CARTESIAN_POINT('Ctrl Pts',(59.9582978318402,249.317015595051,21.9327209419725)) ;
#110573 = CARTESIAN_POINT('Ctrl Pts',(59.9604938797889,249.346213569501,21.9676846215701)) ;
#110574 = CARTESIAN_POINT('Ctrl Pts',(59.9618834253937,249.363839048349,21.989912799075)) ;
#110575 = CARTESIAN_POINT('Ctrl Pts',(59.9695760071074,249.456831727206,22.1135006251323)) ;
#110576 = CARTESIAN_POINT('Ctrl Pts',(59.9762956255979,249.521123262515,22.2226661050005)) ;
#110577 = CARTESIAN_POINT('Ctrl Pts',(59.9858480768859,249.594229813972,22.3865987221059)) ;
#110578 = CARTESIAN_POINT('Ctrl Pts',(59.9886687109269,249.613582853527,22.4362139139115)) ;
#110579 = CARTESIAN_POINT('Ctrl Pts',(59.9925977756553,249.637820047479,22.5083053032928)) ;
#110580 = CARTESIAN_POINT('Ctrl Pts',(59.9937635155822,249.644652836141,22.5300909582373)) ;
#110581 = CARTESIAN_POINT('Ctrl Pts',(59.9958233867228,249.65612311291,22.5694594152369)) ;
#110582 = CARTESIAN_POINT('Ctrl Pts',(59.9967242944594,249.660923431469,22.586990932214)) ;
#110583 = CARTESIAN_POINT('Ctrl Pts',(59.9981497256906,249.66818654112,22.6153162635981)) ;
#110584 = CARTESIAN_POINT('Ctrl Pts',(59.998683580311,249.670828974291,22.6260622006264)) ;
#110585 = CARTESIAN_POINT('Ctrl Pts',(59.9997503535679,249.675955915187,22.6478387954203)) ;
#110586 = CARTESIAN_POINT('Ctrl Pts',(60.0002830116965,249.678435609763,22.65886992806)) ;
#110587 = CARTESIAN_POINT('Ctrl Pts',(60.0017113515012,249.684855324651,22.6888413174326)) ;
#110588 = CARTESIAN_POINT('Ctrl Pts',(60.002595779097,249.688579672782,22.7078264304126)) ;
#110589 = CARTESIAN_POINT('Ctrl Pts',(60.0078865104848,249.70921120396,22.8235592857794)) ;
#110590 = CARTESIAN_POINT('Ctrl Pts',(60.011950079609,249.717925993855,22.9215816218335)) ;
#110591 = CARTESIAN_POINT('Ctrl Pts',(60.0201232737497,249.718102523529,23.1176623295655)) ;
#110592 = CARTESIAN_POINT('Ctrl Pts',(60.0242214056265,249.709629801772,23.2153307942135)) ;
#110593 = CARTESIAN_POINT('Ctrl Pts',(60.0299224414467,249.6874451356,23.3415752665169)) ;
#110594 = CARTESIAN_POINT('Ctrl Pts',(60.031293642495,249.681385808762,23.3713031658761)) ;
#110595 = CARTESIAN_POINT('Ctrl Pts',(60.0335856870227,249.670123200892,23.4198001473)) ;
#110596 = CARTESIAN_POINT('Ctrl Pts',(60.0344914771101,249.665393061834,23.4386722970718)) ;
#110597 = CARTESIAN_POINT('Ctrl Pts',(60.0363006411081,249.655408946824,23.4757591950049)) ;
#110598 = CARTESIAN_POINT('Ctrl Pts',(60.0372033423329,249.650172324099,23.4939756189885)) ;
#110599 = CARTESIAN_POINT('Ctrl Pts',(60.0394437668875,249.636563545334,23.5384629348542)) ;
#110600 = CARTESIAN_POINT('Ctrl Pts',(60.0407923706905,249.627850453181,23.5646230417524)) ;
#110601 = CARTESIAN_POINT('Ctrl Pts',(60.0470888523167,249.584820661287,23.6839251770361)) ;
#110602 = CARTESIAN_POINT('Ctrl Pts',(60.0522806503703,249.542928947074,23.7741112937021)) ;
#110603 = CARTESIAN_POINT('Ctrl Pts',(60.0630593888772,249.441570125258,23.9497085752273)) ;
#110604 = CARTESIAN_POINT('Ctrl Pts',(60.0686286752913,249.381632988268,24.0343823419641)) ;
#110605 = CARTESIAN_POINT('Ctrl Pts',(60.074788335451,249.30199696185,24.127319291666)) ;
#110606 = CARTESIAN_POINT('Ctrl Pts',(60.0757249585487,249.289480826448,24.1414368940227)) ;
#110607 = CARTESIAN_POINT('Ctrl Pts',(60.077192575774,249.26915386275,24.1636001186608)) ;
#110608 = CARTESIAN_POINT('Ctrl Pts',(60.0777338352236,249.261496174889,24.1717834461276)) ;
#110609 = CARTESIAN_POINT('Ctrl Pts',(60.0788012445498,249.246053312973,24.1879583834992)) ;
#110610 = CARTESIAN_POINT('Ctrl Pts',(60.0793274150755,249.238269289188,24.1959502874408)) ;
#110611 = CARTESIAN_POINT('Ctrl Pts',(60.0807165071776,249.217284130595,24.2170702614548)) ;
#110612 = CARTESIAN_POINT('Ctrl Pts',(60.0815692233575,249.203942941329,24.2300575338184)) ;
#110613 = CARTESIAN_POINT('Ctrl Pts',(60.0834725975997,249.17322038371,24.2589848434578)) ;
#110614 = CARTESIAN_POINT('Ctrl Pts',(60.084515233874,249.155713414926,24.27478602767)) ;
#110615 = CARTESIAN_POINT('Ctrl Pts',(60.0879981563692,249.095260791897,24.3270785467251)) ;
#110616 = CARTESIAN_POINT('Ctrl Pts',(60.0903658832081,249.050810893612,24.3617747895713)) ;
#110617 = CARTESIAN_POINT('Ctrl Pts',(60.0977238833365,248.90663352903,24.4630600238041)) ;
#110618 = CARTESIAN_POINT('Ctrl Pts',(60.102669048862,248.801471193271,24.5212440829292)) ;
#110619 = CARTESIAN_POINT('Ctrl Pts',(60.1093138582763,248.66412148195,24.5790429401345)) ;
#110620 = CARTESIAN_POINT('Ctrl Pts',(60.1106355864062,248.636937357643,24.5896565875319)) ;
#110621 = CARTESIAN_POINT('Ctrl Pts',(60.1128677037412,248.591391687656,24.6060836574672)) ;
#110622 = CARTESIAN_POINT('Ctrl Pts',(60.1137646863813,248.573181731164,24.6122996345218)) ;
#110623 = CARTESIAN_POINT('Ctrl Pts',(60.1155741787527,248.536661596145,24.6240684642749)) ;
#110624 = CARTESIAN_POINT('Ctrl Pts',(60.1164864340269,248.518355336366,24.6296240177572)) ;
#110625 = CARTESIAN_POINT('Ctrl Pts',(60.1187865147663,248.472483387148,24.6426927794214)) ;
#110626 = CARTESIAN_POINT('Ctrl Pts',(60.1201865581757,248.444813936547,24.6498169935464)) ;
#110627 = CARTESIAN_POINT('Ctrl Pts',(60.12628226775,248.325437690679,24.6773233640216)) ;
#110628 = CARTESIAN_POINT('Ctrl Pts',(60.1311899878649,248.232298598277,24.6906881914895)) ;
#110629 = CARTESIAN_POINT('Ctrl Pts',(60.1418908589937,248.031209442134,24.7024874134421)) ;
#110630 = CARTESIAN_POINT('Ctrl Pts',(60.1476860631058,247.923517444686,24.6984538113917)) ;
#110631 = CARTESIAN_POINT('Ctrl Pts',(60.1540166341008,247.798699582628,24.681690849035)) ;
#110632 = CARTESIAN_POINT('Ctrl Pts',(60.1549298848446,247.780490848836,24.6789395709323)) ;
#110633 = CARTESIAN_POINT('Ctrl Pts',(60.1563698854962,247.751370037737,24.6740478533021)) ;
#110634 = CARTESIAN_POINT('Ctrl Pts',(60.1569062866519,247.740427855667,24.6720978028562)) ;
#110635 = CARTESIAN_POINT('Ctrl Pts',(60.1579731562519,247.718448733921,24.6679550571688)) ;
#110636 = CARTESIAN_POINT('Ctrl Pts',(60.1585034649354,247.707412897652,24.6657597853227)) ;
#110637 = CARTESIAN_POINT('Ctrl Pts',(60.1599175492146,247.677724596064,24.659543006165)) ;
#110638 = CARTESIAN_POINT('Ctrl Pts',(60.1607904564246,247.659116875322,24.6553139764596)) ;
#110639 = CARTESIAN_POINT('Ctrl Pts',(60.1655611620724,247.55624837165,24.6300817951632)) ;
#110640 = CARTESIAN_POINT('Ctrl Pts',(60.1691912131327,247.473638034325,24.6028771224125)) ;
#110641 = CARTESIAN_POINT('Ctrl Pts',(60.174677093633,247.352244883397,24.5521607359739)) ;
#110642 = CARTESIAN_POINT('Ctrl Pts',(60.1765349147425,247.311719635658,24.5332928537005)) ;
#110643 = CARTESIAN_POINT('Ctrl Pts',(60.178415027332,247.272018800728,24.5128439518851)) ;
#110644 = CARTESIAN_POINT('Ctrl Pts',(60.2784744057375,247.272018982637,24.5128440455817)) ;
#110645 = CARTESIAN_POINT('Ctrl Pts',(60.2776289566685,247.289222581645,24.5217051842002)) ;
#110646 = CARTESIAN_POINT('Ctrl Pts',(60.2767753101108,247.306582142027,24.530270043404)) ;
#110647 = CARTESIAN_POINT('Ctrl Pts',(60.2746056555497,247.350595837132,24.5510459570075)) ;
#110648 = CARTESIAN_POINT('Ctrl Pts',(60.2732782937851,247.377423864104,24.5628603281162)) ;
#110649 = CARTESIAN_POINT('Ctrl Pts',(60.2710394110508,247.422374309508,24.5812649347257)) ;
#110650 = CARTESIAN_POINT('Ctrl Pts',(60.2701414805683,247.440325821343,24.5882565203609)) ;
#110651 = CARTESIAN_POINT('Ctrl Pts',(60.2683322577767,247.476313648988,24.6015636353876)) ;
#110652 = CARTESIAN_POINT('Ctrl Pts',(60.2674212700478,247.494345378787,24.6078832077013)) ;
#110653 = CARTESIAN_POINT('Ctrl Pts',(60.2651288195875,247.539478463412,24.6228404752716)) ;
#110654 = CARTESIAN_POINT('Ctrl Pts',(60.2637353116982,247.566698296678,24.6310993189415)) ;
#110655 = CARTESIAN_POINT('Ctrl Pts',(60.2560685179331,247.715271468106,24.6720839146282)) ;
#110656 = CARTESIAN_POINT('Ctrl Pts',(60.2493837110393,247.83978716468,24.6917818949342)) ;
#110657 = CARTESIAN_POINT('Ctrl Pts',(60.2398496418138,248.018753539113,24.6997851073337)) ;
#110658 = CARTESIAN_POINT('Ctrl Pts',(60.2370142102413,248.072280280384,24.6996177426996)) ;
#110659 = CARTESIAN_POINT('Ctrl Pts',(60.2330673123463,248.148573954947,24.695727227887)) ;
#110660 = CARTESIAN_POINT('Ctrl Pts',(60.2318980800607,248.171413337977,24.6940933221516)) ;
#110661 = CARTESIAN_POINT('Ctrl Pts',(60.2298327726669,248.212349703012,24.6903211498672)) ;
#110662 = CARTESIAN_POINT('Ctrl Pts',(60.2289298729534,248.23045877387,24.688354601587)) ;
#110663 = CARTESIAN_POINT('Ctrl Pts',(60.2275020895802,248.259520507672,24.6847188976708)) ;
#110664 = CARTESIAN_POINT('Ctrl Pts',(60.2269678250872,248.270494625683,24.6832355234875)) ;
#110665 = CARTESIAN_POINT('Ctrl Pts',(60.225901099512,248.292632040687,24.6800197098943)) ;
#110666 = CARTESIAN_POINT('Ctrl Pts',(60.2253688816639,248.303794072806,24.678282972677)) ;
#110667 = CARTESIAN_POINT('Ctrl Pts',(60.2239430247819,248.333977014467,24.6732739887185)) ;
#110668 = CARTESIAN_POINT('Ctrl Pts',(60.2230605731415,248.352960799856,24.6697859902233)) ;
#110669 = CARTESIAN_POINT('Ctrl Pts',(60.2177403334771,248.468825812525,24.6464237890574)) ;
#110670 = CARTESIAN_POINT('Ctrl Pts',(60.2136505668861,248.563861354591,24.6183412808526)) ;
#110671 = CARTESIAN_POINT('Ctrl Pts',(60.2066222833348,248.720706019702,24.5564757553712)) ;
#110672 = CARTESIAN_POINT('Ctrl Pts',(60.2037090470471,248.783878514843,24.5268901868337)) ;
#110673 = CARTESIAN_POINT('Ctrl Pts',(60.1992785438693,248.87372764079,24.4777733020803)) ;
#110674 = CARTESIAN_POINT('Ctrl Pts',(60.1978423994883,248.901963167498,24.4612478878456)) ;
#110675 = CARTESIAN_POINT('Ctrl Pts',(60.1951337894306,248.953307455088,24.4291463667674)) ;
#110676 = CARTESIAN_POINT('Ctrl Pts',(60.193869202453,248.976546106726,24.4137995100251)) ;
#110677 = CARTESIAN_POINT('Ctrl Pts',(60.1917058411474,249.014980022186,24.3870204845665)) ;
#110678 = CARTESIAN_POINT('Ctrl Pts',(60.1908186505491,249.030382630649,24.3758952935882)) ;
#110679 = CARTESIAN_POINT('Ctrl Pts',(60.1890056858663,249.061114141341,24.3528939207677)) ;
#110680 = CARTESIAN_POINT('Ctrl Pts',(60.1880796326852,249.076432696064,24.3410088034847)) ;
#110681 = CARTESIAN_POINT('Ctrl Pts',(60.1856947277643,249.114909014026,24.3100734457593)) ;
#110682 = CARTESIAN_POINT('Ctrl Pts',(60.1842216857803,249.137767696647,24.2906634844707)) ;
#110683 = CARTESIAN_POINT('Ctrl Pts',(60.1771586567455,249.243146709639,24.1962078936101)) ;
#110684 = CARTESIAN_POINT('Ctrl Pts',(60.1712608176561,249.31856072352,24.1136754353094)) ;
#110685 = CARTESIAN_POINT('Ctrl Pts',(60.1606912426268,249.437187380823,23.9545993991115)) ;
#110686 = CARTESIAN_POINT('Ctrl Pts',(60.1560600002136,249.483662343065,23.8809760304521)) ;
#110687 = CARTESIAN_POINT('Ctrl Pts',(60.1507620607461,249.532830317509,23.7877630568401)) ;
#110688 = CARTESIAN_POINT('Ctrl Pts',(60.1498470939627,249.541167262585,23.7713057501868)) ;
#110689 = CARTESIAN_POINT('Ctrl Pts',(60.1484051218049,249.554092078485,23.7447127752868)) ;
#110690 = CARTESIAN_POINT('Ctrl Pts',(60.1478684196099,249.558853369701,23.734663467821)) ;
#110691 = CARTESIAN_POINT('Ctrl Pts',(60.1468017496556,249.56822610669,23.7143618984894)) ;
#110692 = CARTESIAN_POINT('Ctrl Pts',(60.1462719256948,249.572835118125,23.7041091742211)) ;
#110693 = CARTESIAN_POINT('Ctrl Pts',(60.1448603799075,249.58497045517,23.67637207197)) ;
#110694 = CARTESIAN_POINT('Ctrl Pts',(60.1439894627165,249.592303011124,23.6588042852826)) ;
#110695 = CARTESIAN_POINT('Ctrl Pts',(60.1385422714053,249.636973627156,23.546437012392)) ;
#110696 = CARTESIAN_POINT('Ctrl Pts',(60.1343383950824,249.665912945952,23.4485187011399)) ;
#110697 = CARTESIAN_POINT('Ctrl Pts',(60.1259017325359,249.705381695324,23.2500578618463)) ;
#110698 = CARTESIAN_POINT('Ctrl Pts',(60.1216825504788,249.716086396669,23.149987297837)) ;
#110699 = CARTESIAN_POINT('Ctrl Pts',(60.1159514715112,249.718242326937,23.0219504888093)) ;
#110700 = CARTESIAN_POINT('Ctrl Pts',(60.1146965564959,249.718025295756,22.9943277999102)) ;
#110701 = CARTESIAN_POINT('Ctrl Pts',(60.1125447908475,249.716509591761,22.9477748517733)) ;
#110702 = CARTESIAN_POINT('Ctrl Pts',(60.1116592250982,249.715571501506,22.9288381203865)) ;
#110703 = CARTESIAN_POINT('Ctrl Pts',(60.1098453366348,249.713022137616,22.8905274193764)) ;
#110704 = CARTESIAN_POINT('Ctrl Pts',(60.1089166384687,249.71139464885,22.8711574720957)) ;
#110705 = CARTESIAN_POINT('Ctrl Pts',(60.1065154503971,249.706374399746,22.8217200450597)) ;
#110706 = CARTESIAN_POINT('Ctrl Pts',(60.1050283793628,249.702504234628,22.791708951012)) ;
#110707 = CARTESIAN_POINT('Ctrl Pts',(60.0981901461491,249.681324375861,22.6564224785539)) ;
#110708 = CARTESIAN_POINT('Ctrl Pts',(60.0925619274017,249.654810566574,22.5528504564865)) ;
#110709 = CARTESIAN_POINT('Ctrl Pts',(60.0820908158341,249.588152766786,22.3678828921028)) ;
#110710 = CARTESIAN_POINT('Ctrl Pts',(60.0772865967868,249.550897350326,22.2858417433541)) ;
#110711 = CARTESIAN_POINT('Ctrl Pts',(60.0717923536121,249.497959749139,22.1904549648953)) ;
#110712 = CARTESIAN_POINT('Ctrl Pts',(60.0708420889847,249.48839201615,22.1738892502953)) ;
#110713 = CARTESIAN_POINT('Ctrl Pts',(60.0693584318031,249.472745405935,22.1478376371493)) ;
#110714 = CARTESIAN_POINT('Ctrl Pts',(60.0688144069575,249.466850910674,22.138243448215)) ;
#110715 = CARTESIAN_POINT('Ctrl Pts',(60.0678107402087,249.455667647009,22.1204452314797)) ;
#110716 = CARTESIAN_POINT('Ctrl Pts',(60.067349557359,249.45040307088,22.1122267030499)) ;
#110717 = CARTESIAN_POINT('Ctrl Pts',(60.0660992080836,249.43579650794,22.0898566062344)) ;
#110718 = CARTESIAN_POINT('Ctrl Pts',(60.0653189963652,249.426311010344,22.0757996525973)) ;
#110719 = CARTESIAN_POINT('Ctrl Pts',(60.0612969764142,249.375597332534,22.0030485779749)) ;
#110720 = CARTESIAN_POINT('Ctrl Pts',(60.0582456609486,249.330846479603,21.94689450141)) ;
#110721 = CARTESIAN_POINT('Ctrl Pts',(60.0514267454659,249.221551625529,21.826469589256)) ;
#110722 = CARTESIAN_POINT('Ctrl Pts',(60.0476909914728,249.155099031945,21.7642398631361)) ;
#110723 = CARTESIAN_POINT('Ctrl Pts',(60.0421934580009,249.054712872913,21.6844831048761)) ;
#110724 = CARTESIAN_POINT('Ctrl Pts',(60.0405688634349,249.024724734728,21.6622481865668)) ;
#110725 = CARTESIAN_POINT('Ctrl Pts',(60.0375473430975,248.968795796088,21.6236022207869)) ;
#110726 = CARTESIAN_POINT('Ctrl Pts',(60.0361621733384,248.943098454237,21.6068674436997)) ;
#110727 = CARTESIAN_POINT('Ctrl Pts',(60.0338532450256,248.900319818457,21.5806497499206)) ;
#110728 = CARTESIAN_POINT('Ctrl Pts',(60.0329450185226,248.883505578718,21.5707441356093)) ;
#110729 = CARTESIAN_POINT('Ctrl Pts',(60.0311460588964,248.850256867152,21.5519300925993)) ;
#110730 = CARTESIAN_POINT('Ctrl Pts',(60.0302563369079,248.833838716279,21.542998574357)) ;
#110731 = CARTESIAN_POINT('Ctrl Pts',(60.028050875092,248.793225056177,21.5217761721123)) ;
#110732 = CARTESIAN_POINT('Ctrl Pts',(60.0267246242141,248.768874532681,21.5097947545086)) ;
#110733 = CARTESIAN_POINT('Ctrl Pts',(60.0186859080469,248.621751214475,21.4417856139034)) ;
#110734 = CARTESIAN_POINT('Ctrl Pts',(60.011482968448,248.492887076939,21.4001543102271)) ;
#110735 = CARTESIAN_POINT('Ctrl Pts',(60.0016864712964,248.311981568598,21.364982871853)) ;
#110736 = CARTESIAN_POINT('Ctrl Pts',(59.9990770962117,248.263112652409,21.3577028974612)) ;
#110737 = CARTESIAN_POINT('Ctrl Pts',(59.9954044167687,248.192249671143,21.3503255455471)) ;
#110738 = CARTESIAN_POINT('Ctrl Pts',(59.9942904565498,248.170464216292,21.3484870637654)) ;
#110739 = CARTESIAN_POINT('Ctrl Pts',(59.9923115370205,248.131088056635,21.3459380260121)) ;
#110740 = CARTESIAN_POINT('Ctrl Pts',(59.9914405149514,248.113510342178,21.3450775514954)) ;
#110741 = CARTESIAN_POINT('Ctrl Pts',(59.9900503235385,248.08497855944,21.3441305347332)) ;
#110742 = CARTESIAN_POINT('Ctrl Pts',(59.9895225884216,248.074031676831,21.3438744322677)) ;
#110743 = CARTESIAN_POINT('Ctrl Pts',(59.9884554670857,248.051634479983,21.3435698007015)) ;
#110744 = CARTESIAN_POINT('Ctrl Pts',(59.987916599857,248.040184750347,21.3435312764594)) ;
#110745 = CARTESIAN_POINT('Ctrl Pts',(59.9864503158695,248.008685340553,21.343747752589)) ;
#110746 = CARTESIAN_POINT('Ctrl Pts',(59.9855352060764,247.98863877069,21.3442449543637)) ;
#110747 = CARTESIAN_POINT('Ctrl Pts',(59.9806245948603,247.879400427121,21.3489149940543)) ;
#110748 = CARTESIAN_POINT('Ctrl Pts',(59.9769054622383,247.790634846768,21.3598437692565)) ;
#110749 = CARTESIAN_POINT('Ctrl Pts',(59.9685631184884,247.594573335977,21.4000584915383)) ;
#110750 = CARTESIAN_POINT('Ctrl Pts',(59.9639454051421,247.488469314128,21.4330349305119)) ;
#110751 = CARTESIAN_POINT('Ctrl Pts',(59.9577439875736,247.36081060111,21.4870587354343)) ;
#110752 = CARTESIAN_POINT('Ctrl Pts',(59.9564819733251,247.335495780502,21.4985212093475)) ;
#110753 = CARTESIAN_POINT('Ctrl Pts',(59.9543217070367,247.293380042413,21.5188662431163)) ;
#110754 = CARTESIAN_POINT('Ctrl Pts',(59.9534349594196,247.276423950401,21.5274153010682)) ;
#110755 = CARTESIAN_POINT('Ctrl Pts',(59.951621788238,247.242444769981,21.5452769362036)) ;
#110756 = CARTESIAN_POINT('Ctrl Pts',(59.9506950603393,247.225430866707,21.5546006863894)) ;
#110757 = CARTESIAN_POINT('Ctrl Pts',(59.9483059547366,247.182481433473,21.5791152712235)) ;
#110758 = CARTESIAN_POINT('Ctrl Pts',(59.9468292857573,247.156786139901,21.5947114016268)) ;
#110759 = CARTESIAN_POINT('Ctrl Pts',(59.93981248876,247.038622908499,21.6708493221273)) ;
#110760 = CARTESIAN_POINT('Ctrl Pts',(59.9339711610932,246.95187351876,21.7397364030671)) ;
#110761 = CARTESIAN_POINT('Ctrl Pts',(59.9233954851838,246.8093054475,21.8779314600053)) ;
#110762 = CARTESIAN_POINT('Ctrl Pts',(59.9187014689674,246.750994377659,21.9441097336536)) ;
#110763 = CARTESIAN_POINT('Ctrl Pts',(59.9133556903777,246.687160626746,22.0292072201083)) ;
#110764 = CARTESIAN_POINT('Ctrl Pts',(59.9124479787295,246.67641562535,22.0440308138027)) ;
#110765 = CARTESIAN_POINT('Ctrl Pts',(59.9110145780852,246.659553728031,22.0681130442463)) ;
#110766 = CARTESIAN_POINT('Ctrl Pts',(59.9104793807375,246.65328248386,22.0772614015037)) ;
#110767 = CARTESIAN_POINT('Ctrl Pts',(59.9094127799267,246.640821253868,22.0958318092894)) ;
#110768 = CARTESIAN_POINT('Ctrl Pts',(59.9088815791073,246.634634615109,22.1052553577)) ;
#110769 = CARTESIAN_POINT('Ctrl Pts',(59.9074617601964,246.618175038949,22.1308861397013)) ;
#110770 = CARTESIAN_POINT('Ctrl Pts',(59.9065841681356,246.608084167493,22.1472087700735)) ;
#110771 = CARTESIAN_POINT('Ctrl Pts',(59.9012046744278,246.547012659867,22.2498936618512)) ;
#110772 = CARTESIAN_POINT('Ctrl Pts',(59.8970619082503,246.503576654935,22.3405162958788)) ;
#110773 = CARTESIAN_POINT('Ctrl Pts',(59.8886912264801,246.433344702514,22.5286238023864)) ;
#110774 = CARTESIAN_POINT('Ctrl Pts',(59.8844750014276,246.406726595847,22.6257282148712)) ;
#110775 = CARTESIAN_POINT('Ctrl Pts',(59.8787238383411,246.383969900176,22.7523840366644)) ;
#110776 = CARTESIAN_POINT('Ctrl Pts',(59.8774438687043,246.379683156247,22.7802642735121)) ;
#110777 = CARTESIAN_POINT('Ctrl Pts',(59.875262120269,246.373680316341,22.8271462900867)) ;
#110778 = CARTESIAN_POINT('Ctrl Pts',(59.8743724096161,246.371581807744,22.8460935225829)) ;
#110779 = CARTESIAN_POINT('Ctrl Pts',(59.8725609532958,246.368008390957,22.8842970803671)) ;
#110780 = CARTESIAN_POINT('Ctrl Pts',(59.871639079679,246.366542217407,22.9035512909055)) ;
#110781 = CARTESIAN_POINT('Ctrl Pts',(59.8692794575189,246.363673171748,22.9523382726886)) ;
#110782 = CARTESIAN_POINT('Ctrl Pts',(59.8678281126643,246.362718043102,22.9818899504526)) ;
#110783 = CARTESIAN_POINT('Ctrl Pts',(59.860554321418,246.361859930396,23.1277536837001)) ;
#110784 = CARTESIAN_POINT('Ctrl Pts',(59.8543913300841,246.373271260917,23.2437999833863)) ;
#110785 = CARTESIAN_POINT('Ctrl Pts',(59.843729332673,246.413410824383,23.4399273947475)) ;
#110786 = CARTESIAN_POINT('Ctrl Pts',(59.8392691218913,246.436381294541,23.5207652839083)) ;
#110787 = CARTESIAN_POINT('Ctrl Pts',(59.8341531008635,246.471500740201,23.6164224509797)) ;
#110788 = CARTESIAN_POINT('Ctrl Pts',(59.8332625394611,246.47796669936,23.6331960574591)) ;
#110789 = CARTESIAN_POINT('Ctrl Pts',(59.8318493654624,246.488831124832,23.6600841379111)) ;
#110790 = CARTESIAN_POINT('Ctrl Pts',(59.8313176873039,246.493061830395,23.6702645816247)) ;
#110791 = CARTESIAN_POINT('Ctrl Pts',(59.8302510504881,246.501851863298,23.6908415151552)) ;
#110792 = CARTESIAN_POINT('Ctrl Pts',(59.8297164379778,246.506416933716,23.7012348250137)) ;
#110793 = CARTESIAN_POINT('Ctrl Pts',(59.8282759728107,246.519139132218,23.7294191008815)) ;
#110794 = CARTESIAN_POINT('Ctrl Pts',(59.8273817084125,246.527502814997,23.7471153459206)) ;
#110795 = CARTESIAN_POINT('Ctrl Pts',(59.8212183621269,246.588219129601,23.8699698340151)) ;
#110796 = CARTESIAN_POINT('Ctrl Pts',(59.8164385838963,246.651184154417,23.9695306862723)) ;
#110797 = CARTESIAN_POINT('Ctrl Pts',(59.8081486912913,246.774001139679,24.1249108419736)) ;
#110798 = CARTESIAN_POINT('Ctrl Pts',(59.8047261055606,246.828447763627,24.1844342050131)) ;
#110799 = CARTESIAN_POINT('Ctrl Pts',(59.799832917847,246.908142733688,24.2598658499563)) ;
#110800 = CARTESIAN_POINT('Ctrl Pts',(59.7985115037745,246.929847619416,24.2793620469127)) ;
#110801 = CARTESIAN_POINT('Ctrl Pts',(59.7962798767943,246.966690635002,24.3107593601767)) ;
#110802 = CARTESIAN_POINT('Ctrl Pts',(59.7953830626951,246.981545374015,24.3229837467207)) ;
#110803 = CARTESIAN_POINT('Ctrl Pts',(59.793573888811,247.011582311392,24.3468476337114)) ;
#110804 = CARTESIAN_POINT('Ctrl Pts',(59.7926617827875,247.026759904857,24.3584882683831)) ;
#110805 = CARTESIAN_POINT('Ctrl Pts',(59.7903620554979,247.065092315258,24.3868601660425)) ;
#110806 = CARTESIAN_POINT('Ctrl Pts',(59.7889622193492,247.088481093266,24.4032639201617)) ;
#110807 = CARTESIAN_POINT('Ctrl Pts',(59.7844636919244,247.163799223822,24.4532691361644)) ;
#110808 = CARTESIAN_POINT('Ctrl Pts',(59.7812897935359,247.217131225822,24.4845727667639)) ;
#110809 = CARTESIAN_POINT('Ctrl Pts',(59.7780545670443,247.272019328904,24.5128442239351)) ;
#110810 = CARTESIAN_POINT('Origin',(61.8645744874958,248.040265107786,23.0213203435596)) ;
#110811 = CARTESIAN_POINT('',(59.1778464475999,247.272018857277,24.5128439810119)) ;
#110812 = CARTESIAN_POINT('',(59.2757724421406,247.272018954284,24.5128440309779)) ;
#110813 = CARTESIAN_POINT('',(61.8645744874958,247.272018954284,24.5128440309778)) ;
#110814 = CARTESIAN_POINT('',(59.5173146749147,249.718014940025,23.0220706242834)) ;
#110815 = CARTESIAN_POINT('Ctrl Pts',(59.1778464475999,247.272018857277,24.5128439810119)) ;
#110816 = CARTESIAN_POINT('Ctrl Pts',(59.1805262364689,247.225785172619,24.4890301747845)) ;
#110817 = CARTESIAN_POINT('Ctrl Pts',(59.1832623412498,247.180668289674,24.4630716048173)) ;
#110818 = CARTESIAN_POINT('Ctrl Pts',(59.19177069459,247.045554803543,24.3767267360753)) ;
#110819 = CARTESIAN_POINT('Ctrl Pts',(59.1976176759093,246.960152553852,24.3097044244426)) ;
#110820 = CARTESIAN_POINT('Ctrl Pts',(59.2041114285501,246.867150441261,24.2209275633693)) ;
#110821 = CARTESIAN_POINT('Ctrl Pts',(59.205120369381,246.852749898037,24.2066739592982)) ;
#110822 = CARTESIAN_POINT('Ctrl Pts',(59.2066732173524,246.830590024083,24.183930915194)) ;
#110823 = CARTESIAN_POINT('Ctrl Pts',(59.2072293773417,246.82265411331,24.1756169386283)) ;
#110824 = CARTESIAN_POINT('Ctrl Pts',(59.2083011882245,246.807344350987,24.1592442249343)) ;
#110825 = CARTESIAN_POINT('Ctrl Pts',(59.2088173564832,246.799962671476,24.1511938866593)) ;
#110826 = CARTESIAN_POINT('Ctrl Pts',(59.2101438889143,246.78099308439,24.1300960312892)) ;
#110827 = CARTESIAN_POINT('Ctrl Pts',(59.2109456690779,246.769528878101,24.1169384478775)) ;
#110828 = CARTESIAN_POINT('Ctrl Pts',(59.2157328882929,246.701322920596,24.0361466951019)) ;
#110829 = CARTESIAN_POINT('Ctrl Pts',(59.2194286999149,246.649782071289,23.9642934885275)) ;
#110830 = CARTESIAN_POINT('Ctrl Pts',(59.2277907217402,246.546128817064,23.7926758277306)) ;
#110831 = CARTESIAN_POINT('Ctrl Pts',(59.232442425993,246.497905741599,23.6910653928879)) ;
#110832 = CARTESIAN_POINT('Ctrl Pts',(59.2387690741854,246.450122333068,23.5572187109055)) ;
#110833 = CARTESIAN_POINT('Ctrl Pts',(59.2401231303217,246.440814660975,23.5287641811556)) ;
#110834 = CARTESIAN_POINT('Ctrl Pts',(59.2423943677765,246.426743149611,23.4815024217254)) ;
#110835 = CARTESIAN_POINT('Ctrl Pts',(59.2432970737672,246.421535287482,23.4628340877475)) ;
#110836 = CARTESIAN_POINT('Ctrl Pts',(59.2451060969882,246.411861946623,23.4256835330762)) ;
#110837 = CARTESIAN_POINT('Ctrl Pts',(59.2460118824369,246.407384934586,23.4072073062803)) ;
#110838 = CARTESIAN_POINT('Ctrl Pts',(59.2482717202955,246.397115329551,23.3614409377309)) ;
#110839 = CARTESIAN_POINT('Ctrl Pts',(59.2496370844581,246.39168773807,23.3340754454846)) ;
#110840 = CARTESIAN_POINT('Ctrl Pts',(59.2563315532777,246.368777798862,23.2012969168908)) ;
#110841 = CARTESIAN_POINT('Ctrl Pts',(59.2619476270299,246.36071230708,23.0945231180888)) ;
#110842 = CARTESIAN_POINT('Ctrl Pts',(59.2726342336333,246.364732404227,22.8938217066899)) ;
#110843 = CARTESIAN_POINT('Ctrl Pts',(59.2776634200091,246.374494562018,22.8002410163271)) ;
#110844 = CARTESIAN_POINT('Ctrl Pts',(59.2833860141549,246.39569261367,22.6887405256839)) ;
#110845 = CARTESIAN_POINT('Ctrl Pts',(59.2843591536899,246.399683834716,22.6695801420623)) ;
#110846 = CARTESIAN_POINT('Ctrl Pts',(59.2858698682483,246.406518612943,22.6394220313487)) ;
#110847 = CARTESIAN_POINT('Ctrl Pts',(59.2864186963647,246.409140070377,22.628376255911)) ;
#110848 = CARTESIAN_POINT('Ctrl Pts',(59.2874878933858,246.414528584567,22.6066549149141)) ;
#110849 = CARTESIAN_POINT('Ctrl Pts',(59.288008540993,246.417289154133,22.5959784552958)) ;
#110850 = CARTESIAN_POINT('Ctrl Pts',(59.2893636120749,246.424828210806,22.567963848282)) ;
#110851 = CARTESIAN_POINT('Ctrl Pts',(59.2901887187188,246.429780675887,22.5506735339747)) ;
#110852 = CARTESIAN_POINT('Ctrl Pts',(59.2948029032425,246.459466541709,22.4529940943306)) ;
#110853 = CARTESIAN_POINT('Ctrl Pts',(59.2983337978351,246.489941376754,22.3744683306017)) ;
#110854 = CARTESIAN_POINT('Ctrl Pts',(59.3066863236911,246.576165043054,22.1938427726764)) ;
#110855 = CARTESIAN_POINT('Ctrl Pts',(59.3114854116076,246.636877313754,22.0946007726532)) ;
#110856 = CARTESIAN_POINT('Ctrl Pts',(59.3179725400787,246.72530908657,21.978913810968)) ;
#110857 = CARTESIAN_POINT('Ctrl Pts',(59.3193119381519,246.743898108902,21.95588465756)) ;
#110858 = CARTESIAN_POINT('Ctrl Pts',(59.3215654172298,246.775611956246,21.9186551166341)) ;
#110859 = CARTESIAN_POINT('Ctrl Pts',(59.3224655108632,246.788390810563,21.9041682037294)) ;
#110860 = CARTESIAN_POINT('Ctrl Pts',(59.3242746181335,246.814271467177,21.8758300465532)) ;
#110861 = CARTESIAN_POINT('Ctrl Pts',(59.3251832237285,246.827364891083,21.8619750735617)) ;
#110862 = CARTESIAN_POINT('Ctrl Pts',(59.3274606787177,246.860400006349,21.828190805582)) ;
#110863 = CARTESIAN_POINT('Ctrl Pts',(59.3288412345459,246.880612848469,21.8085358320895)) ;
#110864 = CARTESIAN_POINT('Ctrl Pts',(59.3351422846897,246.973672327309,21.7224989984122)) ;
#110865 = CARTESIAN_POINT('Ctrl Pts',(59.3403006963104,247.051779716983,21.6621111580782)) ;
#110866 = CARTESIAN_POINT('Ctrl Pts',(59.3510002120209,247.221185028564,21.5534984433146)) ;
#110867 = CARTESIAN_POINT('Ctrl Pts',(59.3565238075376,247.312556380683,21.5061189539152)) ;
#110868 = CARTESIAN_POINT('Ctrl Pts',(59.3626484798939,247.42524334896,21.4602462000249)) ;
#110869 = CARTESIAN_POINT('Ctrl Pts',(59.363589624051,247.442917261678,21.4533981992962)) ;
#110870 = CARTESIAN_POINT('Ctrl Pts',(59.3650625843092,247.471237992364,21.4429733590442)) ;
#110871 = CARTESIAN_POINT('Ctrl Pts',(59.3656047862379,247.481810853277,21.4392015363143)) ;
#110872 = CARTESIAN_POINT('Ctrl Pts',(59.3666723629663,247.502948963701,21.4318989112463)) ;
#110873 = CARTESIAN_POINT('Ctrl Pts',(59.367197791234,247.513513080998,21.4283666588737)) ;
#110874 = CARTESIAN_POINT('Ctrl Pts',(59.3685823678694,247.54174593161,21.4192382098166)) ;
#110875 = CARTESIAN_POINT('Ctrl Pts',(59.3694314298216,247.559473929841,21.4138289986105)) ;
#110876 = CARTESIAN_POINT('Ctrl Pts',(59.3738892527358,247.65444180146,21.3865638739216)) ;
#110877 = CARTESIAN_POINT('Ctrl Pts',(59.3772673473169,247.733091853232,21.3699769526928)) ;
#110878 = CARTESIAN_POINT('Ctrl Pts',(59.3856151217524,247.931151469249,21.3428539355113)) ;
#110879 = CARTESIAN_POINT('Ctrl Pts',(59.3905519373948,248.051065239868,21.3393462045111)) ;
#110880 = CARTESIAN_POINT('Ctrl Pts',(59.3971877515056,248.199439791846,21.3508828710565)) ;
#110881 = CARTESIAN_POINT('Ctrl Pts',(59.3985105549316,248.228490623729,21.3539064870433)) ;
#110882 = CARTESIAN_POINT('Ctrl Pts',(59.400743969436,248.27653020596,21.3601778910361)) ;
#110883 = CARTESIAN_POINT('Ctrl Pts',(59.4016411387878,248.295568800932,21.3629972652574)) ;
#110884 = CARTESIAN_POINT('Ctrl Pts',(59.4034505947073,248.333422397931,21.3692702081686)) ;
#110885 = CARTESIAN_POINT('Ctrl Pts',(59.4043626173041,248.35223520456,21.3727192795222)) ;
#110886 = CARTESIAN_POINT('Ctrl Pts',(59.4066612670227,248.39896894871,21.3821158391385)) ;
#110887 = CARTESIAN_POINT('Ctrl Pts',(59.408060079665,248.426804104621,21.3884555805986)) ;
#110888 = CARTESIAN_POINT('Ctrl Pts',(59.4140854195912,248.544152186667,21.4183514978897)) ;
#110889 = CARTESIAN_POINT('Ctrl Pts',(59.4189169681766,248.631787100732,21.4485808066904)) ;
#110890 = CARTESIAN_POINT('Ctrl Pts',(59.4296378346349,248.816549827562,21.5299502541684)) ;
#110891 = CARTESIAN_POINT('Ctrl Pts',(59.4355369521123,248.912080608784,21.5837034246399)) ;
#110892 = CARTESIAN_POINT('Ctrl Pts',(59.4419455224123,249.016621536164,21.6568041053846)) ;
#110893 = CARTESIAN_POINT('Ctrl Pts',(59.4428479210382,249.031369659197,21.6674783083586)) ;
#110894 = CARTESIAN_POINT('Ctrl Pts',(59.4442751107914,249.054803469309,21.6850271316829)) ;
#110895 = CARTESIAN_POINT('Ctrl Pts',(59.4448092716059,249.063599668567,21.6917512299296)) ;
#110896 = CARTESIAN_POINT('Ctrl Pts',(59.4458760480371,249.08123729999,21.7055127484445)) ;
#110897 = CARTESIAN_POINT('Ctrl Pts',(59.4464084154968,249.090075435629,21.7125533586212)) ;
#110898 = CARTESIAN_POINT('Ctrl Pts',(59.4478349886522,249.113824689174,21.7318678081727)) ;
#110899 = CARTESIAN_POINT('Ctrl Pts',(59.4487179883856,249.128596437354,21.744310951591)) ;
#110900 = CARTESIAN_POINT('Ctrl Pts',(59.4524360961693,249.190846680087,21.7986130577541)) ;
#110901 = CARTESIAN_POINT('Ctrl Pts',(59.4551357772857,249.236153651935,21.8428880178773)) ;
#110902 = CARTESIAN_POINT('Ctrl Pts',(59.4634328941075,249.369376348737,21.9886933902383)) ;
#110903 = CARTESIAN_POINT('Ctrl Pts',(59.4689004280523,249.447681155356,22.0982631211536)) ;
#110904 = CARTESIAN_POINT('Ctrl Pts',(59.4761999283544,249.526346155825,22.2420326360001)) ;
#110905 = CARTESIAN_POINT('Ctrl Pts',(59.4775432949157,249.539900549804,22.2684460961854)) ;
#110906 = CARTESIAN_POINT('Ctrl Pts',(59.4798015786771,249.561114241396,22.3126336904868)) ;
#110907 = CARTESIAN_POINT('Ctrl Pts',(59.4807023769587,249.569179638151,22.3302058947182)) ;
#110908 = CARTESIAN_POINT('Ctrl Pts',(59.4825114413461,249.584584640663,22.3653591731933)) ;
#110909 = CARTESIAN_POINT('Ctrl Pts',(59.4834192655936,249.591932047347,22.3829336669998)) ;
#110910 = CARTESIAN_POINT('Ctrl Pts',(59.4856918521451,249.609377443325,22.4267434817076)) ;
#110911 = CARTESIAN_POINT('Ctrl Pts',(59.4870682115034,249.619118077597,22.4531140881108)) ;
#110912 = CARTESIAN_POINT('Ctrl Pts',(59.4938356197225,249.663067096999,22.5819679337792)) ;
#110913 = CARTESIAN_POINT('Ctrl Pts',(59.4995201046604,249.687980812302,22.6873375349047)) ;
#110914 = CARTESIAN_POINT('Ctrl Pts',(59.5093266138071,249.712896146806,22.869822058914)) ;
#110915 = CARTESIAN_POINT('Ctrl Pts',(59.5133969118513,249.718049001863,22.945902810493)) ;
#110916 = CARTESIAN_POINT('Ctrl Pts',(59.5173146749147,249.718014940025,23.0220706242834)) ;
#110917 = CARTESIAN_POINT('Ctrl Pts',(59.5173148011493,249.718014938926,23.0220730784946)) ;
#110918 = CARTESIAN_POINT('Ctrl Pts',(59.5187308942661,249.718002586838,23.0496043024628)) ;
#110919 = CARTESIAN_POINT('Ctrl Pts',(59.520125791784,249.717312569216,23.0771326893012)) ;
#110920 = CARTESIAN_POINT('Ctrl Pts',(59.5220396377411,249.715394524352,23.1157105614426)) ;
#110921 = CARTESIAN_POINT('Ctrl Pts',(59.5225841699245,249.71473392328,23.1267825312265)) ;
#110922 = CARTESIAN_POINT('Ctrl Pts',(59.5235968137477,249.713286273174,23.1475753839361)) ;
#110923 = CARTESIAN_POINT('Ctrl Pts',(59.5240661907489,249.712524163427,23.1572976206492)) ;
#110924 = CARTESIAN_POINT('Ctrl Pts',(59.5250769350779,249.710681659853,23.1784351450741)) ;
#110925 = CARTESIAN_POINT('Ctrl Pts',(59.5256165125746,249.709568940235,23.1898470380258)) ;
#110926 = CARTESIAN_POINT('Ctrl Pts',(59.5270868280488,249.706181119012,23.2212550563819)) ;
#110927 = CARTESIAN_POINT('Ctrl Pts',(59.528005147852,249.703663047617,23.2412235046442)) ;
#110928 = CARTESIAN_POINT('Ctrl Pts',(59.5328093928304,249.688369264406,23.3471171650295)) ;
#110929 = CARTESIAN_POINT('Ctrl Pts',(59.536434848772,249.669292901835,23.4320048008461)) ;
#110930 = CARTESIAN_POINT('Ctrl Pts',(59.5412198095171,249.635516970733,23.5416998057986)) ;
#110931 = CARTESIAN_POINT('Ctrl Pts',(59.5423811561681,249.626644012976,23.5681523582366)) ;
#110932 = CARTESIAN_POINT('Ctrl Pts',(59.5469722036763,249.589158223124,23.6713011119839)) ;
#110933 = CARTESIAN_POINT('Ctrl Pts',(59.5504450930294,249.555610087597,23.7460776470531)) ;
#110934 = CARTESIAN_POINT('Ctrl Pts',(59.5554015745482,249.502801234747,23.8439349139661)) ;
#110935 = CARTESIAN_POINT('Ctrl Pts',(59.5567307583138,249.488186245953,23.8693951717872)) ;
#110936 = CARTESIAN_POINT('Ctrl Pts',(59.558971881816,249.462881488672,23.9109152687918)) ;
#110937 = CARTESIAN_POINT('Ctrl Pts',(59.5598701708822,249.452569012188,23.9271978977621)) ;
#110938 = CARTESIAN_POINT('Ctrl Pts',(59.5616794590218,249.431482197501,23.9592568566776)) ;
#110939 = CARTESIAN_POINT('Ctrl Pts',(59.5625901382069,249.42071435872,23.9750339914206)) ;
#110940 = CARTESIAN_POINT('Ctrl Pts',(59.5648804736064,249.393268714089,24.0138087225754)) ;
#110941 = CARTESIAN_POINT('Ctrl Pts',(59.5662721268453,249.376272168342,24.0365725065368)) ;
#110942 = CARTESIAN_POINT('Ctrl Pts',(59.5739523041733,249.280784807041,24.1579080939915)) ;
#110943 = CARTESIAN_POINT('Ctrl Pts',(59.5806549468218,249.191965734632,24.2478187763718)) ;
#110944 = CARTESIAN_POINT('Ctrl Pts',(59.5901990676382,249.052410741105,24.3604447505936)) ;
#110945 = CARTESIAN_POINT('Ctrl Pts',(59.5930275059842,249.009305029107,24.3919607088536)) ;
#110946 = CARTESIAN_POINT('Ctrl Pts',(59.596965985669,248.945689939851,24.4339680981686)) ;
#110947 = CARTESIAN_POINT('Ctrl Pts',(59.5981335850957,248.926354496423,24.4461759417771)) ;
#110948 = CARTESIAN_POINT('Ctrl Pts',(59.6001963531454,248.891194019983,24.4673826262163)) ;
#110949 = CARTESIAN_POINT('Ctrl Pts',(59.6010983245476,248.875460697278,24.4765263478056)) ;
#110950 = CARTESIAN_POINT('Ctrl Pts',(59.6025250103263,248.849921290618,24.490818374756)) ;
#110951 = CARTESIAN_POINT('Ctrl Pts',(59.6030590833381,248.840207818122,24.4961285597051)) ;
#110952 = CARTESIAN_POINT('Ctrl Pts',(59.6041258592792,248.820472999704,24.5066648899307)) ;
#110953 = CARTESIAN_POINT('Ctrl Pts',(59.6046583105073,248.81045004299,24.5118866636684)) ;
#110954 = CARTESIAN_POINT('Ctrl Pts',(59.6060853906529,248.783150120489,24.5257605175601)) ;
#110955 = CARTESIAN_POINT('Ctrl Pts',(59.6069687998426,248.765774841195,24.534216262099)) ;
#110956 = CARTESIAN_POINT('Ctrl Pts',(59.6122757365485,248.658878232088,24.5839726213769)) ;
#110957 = CARTESIAN_POINT('Ctrl Pts',(59.6163536363015,248.565998675546,24.6176197964051)) ;
#110958 = CARTESIAN_POINT('Ctrl Pts',(59.6246698344004,248.373169096507,24.6688037265239)) ;
#110959 = CARTESIAN_POINT('Ctrl Pts',(59.6288983498874,248.273510653106,24.6858386676765)) ;
#110960 = CARTESIAN_POINT('Ctrl Pts',(59.6346832530808,248.144329734024,24.6960856601306)) ;
#110961 = CARTESIAN_POINT('Ctrl Pts',(59.6359841411847,248.11567482639,24.697620309563)) ;
#110962 = CARTESIAN_POINT('Ctrl Pts',(59.6381911332643,248.067850840389,24.6989528702247)) ;
#110963 = CARTESIAN_POINT('Ctrl Pts',(59.6390845053475,248.04869889806,24.6991584473113)) ;
#110964 = CARTESIAN_POINT('Ctrl Pts',(59.6408948820142,248.010331445425,24.6989133611145)) ;
#110965 = CARTESIAN_POINT('Ctrl Pts',(59.6418118200348,247.991118858991,24.6984604585725)) ;
#110966 = CARTESIAN_POINT('Ctrl Pts',(59.6441407199324,247.942893465726,24.6964942729807)) ;
#110967 = CARTESIAN_POINT('Ctrl Pts',(59.6455655594682,247.913905025383,24.6945573055447)) ;
#110968 = CARTESIAN_POINT('Ctrl Pts',(59.6530372784655,247.764548728882,24.6806741818089)) ;
#110969 = CARTESIAN_POINT('Ctrl Pts',(59.6594587820107,247.645692176022,24.6564899854684)) ;
#110970 = CARTESIAN_POINT('Ctrl Pts',(59.6701882789886,247.453705534772,24.5952605478754)) ;
#110971 = CARTESIAN_POINT('Ctrl Pts',(59.6744624274261,247.378784043383,24.5652712557968)) ;
#110972 = CARTESIAN_POINT('Ctrl Pts',(59.6791490969792,247.294811225893,24.5244194538945)) ;
#110973 = CARTESIAN_POINT('Ctrl Pts',(59.6797845335315,247.283381906269,24.5186968003499)) ;
#110974 = CARTESIAN_POINT('Ctrl Pts',(59.6804129742801,247.272018954245,24.5128440309576)) ;
#110975 = CARTESIAN_POINT('Ctrl Pts',(59.7780545670443,247.272019328904,24.5128442239351)) ;
#110976 = CARTESIAN_POINT('Ctrl Pts',(59.774761794154,247.327883750854,24.5416185579683)) ;
#110977 = CARTESIAN_POINT('Ctrl Pts',(59.7714055505668,247.385360102237,24.5672519396114)) ;
#110978 = CARTESIAN_POINT('Ctrl Pts',(59.7651852062337,247.494600491515,24.6087724922865)) ;
#110979 = CARTESIAN_POINT('Ctrl Pts',(59.762325360688,247.545914614006,24.6254937168973)) ;
#110980 = CARTESIAN_POINT('Ctrl Pts',(59.7583490811463,247.620134709861,24.6457785904628)) ;
#110981 = CARTESIAN_POINT('Ctrl Pts',(59.7571740831682,247.642445978209,24.6513860366435)) ;
#110982 = CARTESIAN_POINT('Ctrl Pts',(59.7550998233612,247.682679481403,24.6606225172389)) ;
#110983 = CARTESIAN_POINT('Ctrl Pts',(59.7541936532009,247.700559010831,24.6644207402717)) ;
#110984 = CARTESIAN_POINT('Ctrl Pts',(59.7527620710491,247.729376717799,24.6700520818001)) ;
#110985 = CARTESIAN_POINT('Ctrl Pts',(59.7522271907319,247.740276916286,24.6720701841887)) ;
#110986 = CARTESIAN_POINT('Ctrl Pts',(59.7511605958433,247.762307184996,24.6759235213669)) ;
#110987 = CARTESIAN_POINT('Ctrl Pts',(59.7506290965651,247.773437306327,24.6777548337123)) ;
#110988 = CARTESIAN_POINT('Ctrl Pts',(59.7492074792761,247.803581987803,24.6824030074996)) ;
#110989 = CARTESIAN_POINT('Ctrl Pts',(59.7483284357257,247.822628278194,24.685005644251)) ;
#110990 = CARTESIAN_POINT('Ctrl Pts',(59.7429653475135,247.940912304063,24.6991027499984)) ;
#110991 = CARTESIAN_POINT('Ctrl Pts',(59.7388373156994,248.040975550861,24.7020427459108)) ;
#110992 = CARTESIAN_POINT('Ctrl Pts',(59.7304696760117,248.241339005617,24.6900253734806)) ;
#110993 = CARTESIAN_POINT('Ctrl Pts',(59.7262411098734,248.34121223189,24.6749334012655)) ;
#110994 = CARTESIAN_POINT('Ctrl Pts',(59.7204756214179,248.466519057224,24.644264668261)) ;
#110995 = CARTESIAN_POINT('Ctrl Pts',(59.7191955308437,248.493743133007,24.6368692551899)) ;
#110996 = CARTESIAN_POINT('Ctrl Pts',(59.7170136347423,248.539031252983,24.6233318240841)) ;
#110997 = CARTESIAN_POINT('Ctrl Pts',(59.7161239010689,248.557200644494,24.6175615743021)) ;
#110998 = CARTESIAN_POINT('Ctrl Pts',(59.7143124464029,248.593567907158,24.6053259923635)) ;
#110999 = CARTESIAN_POINT('Ctrl Pts',(59.7133905985666,248.611760312604,24.5988535685712)) ;
#111000 = CARTESIAN_POINT('Ctrl Pts',(59.7110311466097,248.657511589341,24.5816810893695)) ;
#111001 = CARTESIAN_POINT('Ctrl Pts',(59.7095799503321,248.684906112866,24.5705642606709)) ;
#111002 = CARTESIAN_POINT('Ctrl Pts',(59.7023049196112,248.818594572278,24.5121529646731)) ;
#111003 = CARTESIAN_POINT('Ctrl Pts',(59.696140338342,248.920052083842,24.4546197581295)) ;
#111004 = CARTESIAN_POINT('Ctrl Pts',(59.6854779745309,249.083021796893,24.3383403192104)) ;
#111005 = CARTESIAN_POINT('Ctrl Pts',(59.6810189661873,249.14756740238,24.284556888648)) ;
#111006 = CARTESIAN_POINT('Ctrl Pts',(59.6759040712347,249.220729409296,24.2136592905779)) ;
#111007 = CARTESIAN_POINT('Ctrl Pts',(59.6750135496421,249.233435858065,24.200943901888)) ;
#111008 = CARTESIAN_POINT('Ctrl Pts',(59.6736004212274,249.253601868926,24.1801044001107)) ;
#111009 = CARTESIAN_POINT('Ctrl Pts',(59.6730687499222,249.261189781961,24.1721068323961)) ;
#111010 = CARTESIAN_POINT('Ctrl Pts',(59.6720021109092,249.276429952263,24.155723442942)) ;
#111011 = CARTESIAN_POINT('Ctrl Pts',(59.6714674896903,249.284076967901,24.1473336580495)) ;
#111012 = CARTESIAN_POINT('Ctrl Pts',(59.6700269700435,249.30467527621,24.1242686875443)) ;
#111013 = CARTESIAN_POINT('Ctrl Pts',(59.6691326614019,249.317456159265,24.109443129741)) ;
#111014 = CARTESIAN_POINT('Ctrl Pts',(59.6640307037729,249.390011486994,24.0222402705537)) ;
#111015 = CARTESIAN_POINT('Ctrl Pts',(59.6601335143789,249.443891693565,23.9451663070665)) ;
#111016 = CARTESIAN_POINT('Ctrl Pts',(59.6517667254847,249.544720537382,23.771573505906)) ;
#111017 = CARTESIAN_POINT('Ctrl Pts',(59.6473018333757,249.589441737181,23.6742489334558)) ;
#111018 = CARTESIAN_POINT('Ctrl Pts',(59.6412747623058,249.633780750475,23.546992653337)) ;
#111019 = CARTESIAN_POINT('Ctrl Pts',(59.6400078404709,249.642301593623,23.5204220132433)) ;
#111020 = CARTESIAN_POINT('Ctrl Pts',(59.6378417115146,249.655507120173,23.475412433816)) ;
#111021 = CARTESIAN_POINT('Ctrl Pts',(59.6369541621637,249.660548018405,23.4570836271768)) ;
#111022 = CARTESIAN_POINT('Ctrl Pts',(59.6351415088113,249.670095850163,23.4199080815493)) ;
#111023 = CARTESIAN_POINT('Ctrl Pts',(59.634216149424,249.674589859489,23.4010610460801)) ;
#111024 = CARTESIAN_POINT('Ctrl Pts',(59.6318353408483,249.685190146919,23.3529249872554)) ;
#111025 = CARTESIAN_POINT('Ctrl Pts',(59.6303657969879,249.690841079606,23.3235435136852)) ;
#111026 = CARTESIAN_POINT('Ctrl Pts',(59.623263615938,249.713974244059,23.1831163693322)) ;
#111027 = CARTESIAN_POINT('Ctrl Pts',(59.6173173192074,249.721050621605,23.0706617828455)) ;
#111028 = CARTESIAN_POINT('Ctrl Pts',(59.6066511748029,249.713535852349,22.8705510765495)) ;
#111029 = CARTESIAN_POINT('Ctrl Pts',(59.6019716717976,249.703344836954,22.783131050542)) ;
#111030 = CARTESIAN_POINT('Ctrl Pts',(59.5966832838548,249.682953897403,22.6796664194113)) ;
#111031 = CARTESIAN_POINT('Ctrl Pts',(59.5958135164287,249.679285212283,22.6624791466082)) ;
#111032 = CARTESIAN_POINT('Ctrl Pts',(59.5944248058086,249.672894524959,22.6346861150518)) ;
#111033 = CARTESIAN_POINT('Ctrl Pts',(59.5938973284434,249.670337607899,22.6240439865378)) ;
#111034 = CARTESIAN_POINT('Ctrl Pts',(59.5928301761248,249.664891550901,22.602315315598)) ;
#111035 = CARTESIAN_POINT('Ctrl Pts',(59.5922910315064,249.661992671096,22.5912319607847)) ;
#111036 = CARTESIAN_POINT('Ctrl Pts',(59.5908230508129,249.653700155936,22.5608035776308)) ;
#111037 = CARTESIAN_POINT('Ctrl Pts',(59.5899065697292,249.648072241925,22.5415239012834)) ;
#111038 = CARTESIAN_POINT('Ctrl Pts',(59.5849910277009,249.615518922208,22.4370188126257)) ;
#111039 = CARTESIAN_POINT('Ctrl Pts',(59.5812686711442,249.582160356368,22.3539415299896)) ;
#111040 = CARTESIAN_POINT('Ctrl Pts',(59.5729218036873,249.492950912579,22.1746562990521)) ;
#111041 = CARTESIAN_POINT('Ctrl Pts',(59.5683025964055,249.433847722074,22.0805432491439)) ;
#111042 = CARTESIAN_POINT('Ctrl Pts',(59.5621024417683,249.348914668885,21.9710588354632)) ;
#111043 = CARTESIAN_POINT('Ctrl Pts',(59.5608436740857,249.331390763142,21.9495893367198)) ;
#111044 = CARTESIAN_POINT('Ctrl Pts',(59.5586872849192,249.300984759523,21.914165845468)) ;
#111045 = CARTESIAN_POINT('Ctrl Pts',(59.5578010668375,249.28838269399,21.8999784782596)) ;
#111046 = CARTESIAN_POINT('Ctrl Pts',(59.5559875399162,249.262403415081,21.8717116882523)) ;
#111047 = CARTESIAN_POINT('Ctrl Pts',(59.5550598940995,249.249016987054,21.8576447194599)) ;
#111048 = CARTESIAN_POINT('Ctrl Pts',(59.5526652158698,249.214231694936,21.8223389683243)) ;
#111049 = CARTESIAN_POINT('Ctrl Pts',(59.5511837595219,249.192499602197,21.801439442893)) ;
#111050 = CARTESIAN_POINT('Ctrl Pts',(59.5453676721818,249.106389150695,21.722982725395)) ;
#111051 = CARTESIAN_POINT('Ctrl Pts',(59.5408631118082,249.038173399908,21.6698480468623)) ;
#111052 = CARTESIAN_POINT('Ctrl Pts',(59.5321061176216,248.900542143154,21.5787658566816)) ;
#111053 = CARTESIAN_POINT('Ctrl Pts',(59.527879502502,248.831929939601,21.5400009696296)) ;
#111054 = CARTESIAN_POINT('Ctrl Pts',(59.5223074232035,248.735466302676,21.4941234324246)) ;
#111055 = CARTESIAN_POINT('Ctrl Pts',(59.5208580733492,248.709782671801,21.4826906083421)) ;
#111056 = CARTESIAN_POINT('Ctrl Pts',(59.5183634155121,248.664267267667,21.4637855062765)) ;
#111057 = CARTESIAN_POINT('Ctrl Pts',(59.5173068652299,248.644558704881,21.4560335369966)) ;
#111058 = CARTESIAN_POINT('Ctrl Pts',(59.515698250874,248.613762793008,21.4445889754111)) ;
#111059 = CARTESIAN_POINT('Ctrl Pts',(59.5151325552097,248.602775230741,21.4406357519086)) ;
#111060 = CARTESIAN_POINT('Ctrl Pts',(59.5140626043835,248.581663938695,21.4332881171425)) ;
#111061 = CARTESIAN_POINT('Ctrl Pts',(59.5135573903211,248.571547621024,21.4298751074472)) ;
#111062 = CARTESIAN_POINT('Ctrl Pts',(59.5122748658985,248.545512104935,21.4213672535861)) ;
#111063 = CARTESIAN_POINT('Ctrl Pts',(59.511505263184,248.529547687484,21.4164131773161)) ;
#111064 = CARTESIAN_POINT('Ctrl Pts',(59.5079262555667,248.453902052813,21.3941725424164)) ;
#111065 = CARTESIAN_POINT('Ctrl Pts',(59.5052581977839,248.393360519861,21.3799702131822)) ;
#111066 = CARTESIAN_POINT('Ctrl Pts',(59.4996340259662,248.26199503237,21.3567607345253)) ;
#111067 = CARTESIAN_POINT('Ctrl Pts',(59.4966972215952,248.191104367986,21.3488459574273)) ;
#111068 = CARTESIAN_POINT('Ctrl Pts',(59.4915022641246,248.067678804981,21.3429790930685)) ;
#111069 = CARTESIAN_POINT('Ctrl Pts',(59.4892750213532,248.015347367843,21.3429402932568)) ;
#111070 = CARTESIAN_POINT('Ctrl Pts',(59.4852852154806,247.924292856095,21.3471325413208)) ;
#111071 = CARTESIAN_POINT('Ctrl Pts',(59.4835520019177,247.88555993595,21.3502666584703)) ;
#111072 = CARTESIAN_POINT('Ctrl Pts',(59.4808168830331,247.826069783601,21.3571664407301)) ;
#111073 = CARTESIAN_POINT('Ctrl Pts',(59.4798442104066,247.805215456688,21.3599836937173)) ;
#111074 = CARTESIAN_POINT('Ctrl Pts',(59.4779985574567,247.766250544468,21.3659958810795)) ;
#111075 = CARTESIAN_POINT('Ctrl Pts',(59.4771286314416,247.748128710412,21.3690977950707)) ;
#111076 = CARTESIAN_POINT('Ctrl Pts',(59.4751231416628,247.706926102166,21.3768494918451)) ;
#111077 = CARTESIAN_POINT('Ctrl Pts',(59.4739817338708,247.683885235584,21.3816884970079)) ;
#111078 = CARTESIAN_POINT('Ctrl Pts',(59.4703541573072,247.611954166381,21.3983831395589)) ;
#111079 = CARTESIAN_POINT('Ctrl Pts',(59.4678153528255,247.563493579279,21.4119528557484)) ;
#111080 = CARTESIAN_POINT('Ctrl Pts',(59.4590396175844,247.401795136794,21.4651758203841)) ;
#111081 = CARTESIAN_POINT('Ctrl Pts',(59.4525458340495,247.292224243684,21.5147810328645)) ;
#111082 = CARTESIAN_POINT('Ctrl Pts',(59.4436696934603,247.146681567672,21.6004920259415)) ;
#111083 = CARTESIAN_POINT('Ctrl Pts',(59.4411363442711,247.105577499193,21.6271882236737)) ;
#111084 = CARTESIAN_POINT('Ctrl Pts',(59.4379188436745,247.05302158639,21.6646929711772)) ;
#111085 = CARTESIAN_POINT('Ctrl Pts',(59.4371522566458,247.04047100183,21.6739156621638)) ;
#111086 = CARTESIAN_POINT('Ctrl Pts',(59.4358831307604,247.019601499764,21.689703621198)) ;
#111087 = CARTESIAN_POINT('Ctrl Pts',(59.4353746242082,247.011213237778,21.6961752323037)) ;
#111088 = CARTESIAN_POINT('Ctrl Pts',(59.434293753018,246.993314485507,21.7102567356795)) ;
#111089 = CARTESIAN_POINT('Ctrl Pts',(59.4337230629041,246.983824705338,21.7178913730078)) ;
#111090 = CARTESIAN_POINT('Ctrl Pts',(59.4320583899658,246.956071291668,21.7407215592049)) ;
#111091 = CARTESIAN_POINT('Ctrl Pts',(59.4309828465802,246.938045794223,21.7562028957448)) ;
#111092 = CARTESIAN_POINT('Ctrl Pts',(59.4252547384642,246.842143437684,21.8421755941424)) ;
#111093 = CARTESIAN_POINT('Ctrl Pts',(59.4209532032415,246.770683440108,21.9194838239143)) ;
#111094 = CARTESIAN_POINT('Ctrl Pts',(59.4130581662455,246.656002026043,22.0696388219923)) ;
#111095 = CARTESIAN_POINT('Ctrl Pts',(59.4095090047085,246.610159526125,22.1400265909284)) ;
#111096 = CARTESIAN_POINT('Ctrl Pts',(59.4044355855961,246.555262773169,22.2399614866442)) ;
#111097 = CARTESIAN_POINT('Ctrl Pts',(59.4030726362694,246.541465644329,22.2667650844466)) ;
#111098 = CARTESIAN_POINT('Ctrl Pts',(59.400790718495,246.519980244556,22.311421757387)) ;
#111099 = CARTESIAN_POINT('Ctrl Pts',(59.3998865266387,246.51186667889,22.3290629685585)) ;
#111100 = CARTESIAN_POINT('Ctrl Pts',(59.3980777747049,246.496432704842,22.3642155880455)) ;
#111101 = CARTESIAN_POINT('Ctrl Pts',(59.3971738218356,246.489099638532,22.3817182805544)) ;
#111102 = CARTESIAN_POINT('Ctrl Pts',(59.3949249176763,246.471791036399,22.4250802825795)) ;
#111103 = CARTESIAN_POINT('Ctrl Pts',(59.3935688931329,246.462156620707,22.4510689835856)) ;
#111104 = CARTESIAN_POINT('Ctrl Pts',(59.386686291932,246.417218527503,22.5821648795098)) ;
#111105 = CARTESIAN_POINT('Ctrl Pts',(59.3808470178179,246.391755600703,22.6903393598047)) ;
#111106 = CARTESIAN_POINT('Ctrl Pts',(59.3701828656917,246.365365456292,22.8888452760489)) ;
#111107 = CARTESIAN_POINT('Ctrl Pts',(59.3654052785317,246.360685573072,22.9782762457737)) ;
#111108 = CARTESIAN_POINT('Ctrl Pts',(59.3598786003915,246.363709196641,23.087711662349)) ;
#111109 = CARTESIAN_POINT('Ctrl Pts',(59.3588799218448,246.364622942463,23.1077548711933)) ;
#111110 = CARTESIAN_POINT('Ctrl Pts',(59.3573391963446,246.366622621998,23.1392060002222)) ;
#111111 = CARTESIAN_POINT('Ctrl Pts',(59.3567851852818,246.3674662508,23.1506269406852)) ;
#111112 = CARTESIAN_POINT('Ctrl Pts',(59.3557143794269,246.36934498136,23.1729476611568)) ;
#111113 = CARTESIAN_POINT('Ctrl Pts',(59.3551971330036,246.370369951855,23.1838475282997)) ;
#111114 = CARTESIAN_POINT('Ctrl Pts',(59.3538632957894,246.373319480054,23.2122304594866)) ;
#111115 = CARTESIAN_POINT('Ctrl Pts',(59.3530554784209,246.37541244506,23.2296951304503)) ;
#111116 = CARTESIAN_POINT('Ctrl Pts',(59.3484464973521,246.389119258351,23.330611797653)) ;
#111117 = CARTESIAN_POINT('Ctrl Pts',(59.3449073114498,246.406732676285,23.4131341028129)) ;
#111118 = CARTESIAN_POINT('Ctrl Pts',(59.3365146431292,246.463384127568,23.6060747644031)) ;
#111119 = CARTESIAN_POINT('Ctrl Pts',(59.3316853673595,246.507910793797,23.7144148222799)) ;
#111120 = CARTESIAN_POINT('Ctrl Pts',(59.3251656518772,246.57732484112,23.8432215865148)) ;
#111121 = CARTESIAN_POINT('Ctrl Pts',(59.3238297635604,246.592006557289,23.8688242837909)) ;
#111122 = CARTESIAN_POINT('Ctrl Pts',(59.3215806421183,246.61739407242,23.9105084778274)) ;
#111123 = CARTESIAN_POINT('Ctrl Pts',(59.320681282857,246.627716210268,23.9268163937017)) ;
#111124 = CARTESIAN_POINT('Ctrl Pts',(59.3188724490701,246.648793108471,23.9588780397437)) ;
#111125 = CARTESIAN_POINT('Ctrl Pts',(59.3179633544818,246.659539758871,23.9746336355874)) ;
#111126 = CARTESIAN_POINT('Ctrl Pts',(59.3156822821868,246.686867914198,24.013267572458)) ;
#111127 = CARTESIAN_POINT('Ctrl Pts',(59.3142985116661,246.703762781768,24.0359161656126)) ;
#111128 = CARTESIAN_POINT('Ctrl Pts',(59.3112348031537,246.741838498622,24.084356803264)) ;
#111129 = CARTESIAN_POINT('Ctrl Pts',(59.3095472147758,246.763233071231,24.1099649922655)) ;
#111130 = CARTESIAN_POINT('Ctrl Pts',(59.3041223612164,246.833398297222,24.1890327113843)) ;
#111131 = CARTESIAN_POINT('Ctrl Pts',(59.3002965380526,246.884867880334,24.2399817859792)) ;
#111132 = CARTESIAN_POINT('Ctrl Pts',(59.2914262774161,247.010615316636,24.3493099009446)) ;
#111133 = CARTESIAN_POINT('Ctrl Pts',(59.2863765328242,247.086860945118,24.4050679017676)) ;
#111134 = CARTESIAN_POINT('Ctrl Pts',(59.2806379440077,247.184068925345,24.4642876270644)) ;
#111135 = CARTESIAN_POINT('Ctrl Pts',(59.2796668443651,247.200924459311,24.4741568170896)) ;
#111136 = CARTESIAN_POINT('Ctrl Pts',(59.278158591979,247.227835958453,24.4892892113407)) ;
#111137 = CARTESIAN_POINT('Ctrl Pts',(59.2776102411725,247.237779201986,24.4947483546354)) ;
#111138 = CARTESIAN_POINT('Ctrl Pts',(59.276632254559,247.255822990797,24.5044180988372)) ;
#111139 = CARTESIAN_POINT('Ctrl Pts',(59.2762004036355,247.263903808271,24.5086641243746)) ;
#111140 = CARTESIAN_POINT('Ctrl Pts',(59.2757724421406,247.272018954284,24.5128440309779)) ;
#111141 = CARTESIAN_POINT('Origin',(61.8645744874958,248.040265107786,23.0213203435596)) ;
#111142 = CARTESIAN_POINT('',(58.6780583779715,247.272018809212,24.512843956255)) ;
#111143 = CARTESIAN_POINT('',(58.7781769759756,247.272019165218,24.5128441396244)) ;
#111144 = CARTESIAN_POINT('',(61.8645744874958,247.272018954284,24.5128440309778)) ;
#111145 = CARTESIAN_POINT('Ctrl Pts',(58.6780583779715,247.272018809212,24.512843956255)) ;
#111146 = CARTESIAN_POINT('Ctrl Pts',(58.6800068924602,247.231512300371,24.4919800723578)) ;
#111147 = CARTESIAN_POINT('Ctrl Pts',(58.6819912802419,247.191850795628,24.469463559986)) ;
#111148 = CARTESIAN_POINT('Ctrl Pts',(58.6852925950531,247.129145477612,24.4303998213336)) ;
#111149 = CARTESIAN_POINT('Ctrl Pts',(58.6865751585715,247.105537624819,24.4148512480985)) ;
#111150 = CARTESIAN_POINT('Ctrl Pts',(58.6887601557558,247.06667367633,24.3878226944819)) ;
#111151 = CARTESIAN_POINT('Ctrl Pts',(58.6896504429267,247.051200149417,24.3766651052517)) ;
#111152 = CARTESIAN_POINT('Ctrl Pts',(58.6914621087527,247.020459040762,24.3536916206181)) ;
#111153 = CARTESIAN_POINT('Ctrl Pts',(58.6923835933263,247.005198464231,24.341871228463)) ;
#111154 = CARTESIAN_POINT('Ctrl Pts',(58.6947401655318,246.96713070797,24.3113197523509)) ;
#111155 = CARTESIAN_POINT('Ctrl Pts',(58.6961887716055,246.944608137751,24.2922458266315)) ;
#111156 = CARTESIAN_POINT('Ctrl Pts',(58.7034865319802,246.835449869319,24.1947429378636)) ;
#111157 = CARTESIAN_POINT('Ctrl Pts',(58.7096801360837,246.756679787355,24.1080137953495)) ;
#111158 = CARTESIAN_POINT('Ctrl Pts',(58.7203497328208,246.638165635079,23.9464885838306)) ;
#111159 = CARTESIAN_POINT('Ctrl Pts',(58.7247873478086,246.593856025307,23.8755578817659)) ;
#111160 = CARTESIAN_POINT('Ctrl Pts',(58.7298822590129,246.546657306,23.7857177662923)) ;
#111161 = CARTESIAN_POINT('Ctrl Pts',(58.7307721363177,246.538559141151,23.7696831713953)) ;
#111162 = CARTESIAN_POINT('Ctrl Pts',(58.7321845691273,246.525909293868,23.7436035490382)) ;
#111163 = CARTESIAN_POINT('Ctrl Pts',(58.7327161714001,246.521196516751,23.7336385260547)) ;
#111164 = CARTESIAN_POINT('Ctrl Pts',(58.7337830046694,246.51182804092,23.7133132471223)) ;
#111165 = CARTESIAN_POINT('Ctrl Pts',(58.7343178820646,246.507178687058,23.7029508048126)) ;
#111166 = CARTESIAN_POINT('Ctrl Pts',(58.7357597144667,246.494795213463,23.674582808946)) ;
#111167 = CARTESIAN_POINT('Ctrl Pts',(58.7366550452951,246.487270567014,23.656487294631)) ;
#111168 = CARTESIAN_POINT('Ctrl Pts',(58.7417491617437,246.445617614282,23.551150247605)) ;
#111169 = CARTESIAN_POINT('Ctrl Pts',(58.7456389575049,246.418524230147,23.4612974253404)) ;
#111170 = CARTESIAN_POINT('Ctrl Pts',(58.7540021755883,246.376862887085,23.2650036127155)) ;
#111171 = CARTESIAN_POINT('Ctrl Pts',(58.7584709205864,246.36471336984,23.1584804108466)) ;
#111172 = CARTESIAN_POINT('Ctrl Pts',(58.7645033374796,246.362284364243,23.0236165178458)) ;
#111173 = CARTESIAN_POINT('Ctrl Pts',(58.7657711570691,246.362478537671,22.9956928014189)) ;
#111174 = CARTESIAN_POINT('Ctrl Pts',(58.7679384458552,246.36397605214,22.9487834829235)) ;
#111175 = CARTESIAN_POINT('Ctrl Pts',(58.7688262306036,246.364905742131,22.9297913596818)) ;
#111176 = CARTESIAN_POINT('Ctrl Pts',(58.7706390536231,246.367433967197,22.8914882791098)) ;
#111177 = CARTESIAN_POINT('Ctrl Pts',(58.771564340197,246.369044648063,22.8721810583319)) ;
#111178 = CARTESIAN_POINT('Ctrl Pts',(58.773944291295,246.373990673928,22.823157279201)) ;
#111179 = CARTESIAN_POINT('Ctrl Pts',(58.7754130269918,246.377786686637,22.793494867268)) ;
#111180 = CARTESIAN_POINT('Ctrl Pts',(58.7825252867883,246.399650464576,22.6526554152987)) ;
#111181 = CARTESIAN_POINT('Ctrl Pts',(58.7884839693428,246.428089011615,22.5433948972293)) ;
#111182 = CARTESIAN_POINT('Ctrl Pts',(58.7991001305919,246.497407177365,22.3565249039626)) ;
#111183 = CARTESIAN_POINT('Ctrl Pts',(58.8037172290047,246.533822426037,22.2776834042871)) ;
#111184 = CARTESIAN_POINT('Ctrl Pts',(58.8089802150941,246.584999227896,22.1862316864812)) ;
#111185 = CARTESIAN_POINT('Ctrl Pts',(58.8098760663716,246.59408175224,22.1705997100946)) ;
#111186 = CARTESIAN_POINT('Ctrl Pts',(58.8112955195643,246.609118067985,22.1456576155755)) ;
#111187 = CARTESIAN_POINT('Ctrl Pts',(58.8118283227689,246.614914135414,22.1362544222591)) ;
#111188 = CARTESIAN_POINT('Ctrl Pts',(58.8128950891015,246.626842337563,22.1173239494713)) ;
#111189 = CARTESIAN_POINT('Ctrl Pts',(58.8134287493444,246.632978910035,22.1078002405373)) ;
#111190 = CARTESIAN_POINT('Ctrl Pts',(58.8148631424279,246.649915568187,22.0820909794099)) ;
#111191 = CARTESIAN_POINT('Ctrl Pts',(58.8157524563631,246.660901737458,22.0660296083724)) ;
#111192 = CARTESIAN_POINT('Ctrl Pts',(58.8219431047456,246.740550424521,21.9538260651249)) ;
#111193 = CARTESIAN_POINT('Ctrl Pts',(58.8267480939625,246.818926087262,21.8649732255836)) ;
#111194 = CARTESIAN_POINT('Ctrl Pts',(58.8350524953649,246.965094437661,21.7308605477397)) ;
#111195 = CARTESIAN_POINT('Ctrl Pts',(58.8384609251298,247.028004390372,21.6809452436266)) ;
#111196 = CARTESIAN_POINT('Ctrl Pts',(58.8433364277247,247.118290947778,21.6193014914828)) ;
#111197 = CARTESIAN_POINT('Ctrl Pts',(58.8446557688708,247.142765264961,21.6035096613941)) ;
#111198 = CARTESIAN_POINT('Ctrl Pts',(58.8468850118474,247.184062219823,21.5783610591849)) ;
#111199 = CARTESIAN_POINT('Ctrl Pts',(58.8477815852708,247.200657365204,21.5686422360755)) ;
#111200 = CARTESIAN_POINT('Ctrl Pts',(58.84959117711,247.23409518255,21.5498240160585)) ;
#111201 = CARTESIAN_POINT('Ctrl Pts',(58.8505039623618,247.250933810155,21.5407233505481)) ;
#111202 = CARTESIAN_POINT('Ctrl Pts',(58.8528072779376,247.293333256262,21.5187368650762)) ;
#111203 = CARTESIAN_POINT('Ctrl Pts',(58.8542100993148,247.319074435748,21.5062136834201)) ;
#111204 = CARTESIAN_POINT('Ctrl Pts',(58.8618230108034,247.458302993651,21.4428306180321)) ;
#111205 = CARTESIAN_POINT('Ctrl Pts',(58.8684340781813,247.576848577834,21.4040550390575)) ;
#111206 = CARTESIAN_POINT('Ctrl Pts',(58.8791490750161,247.773930296575,21.3630573987211)) ;
#111207 = CARTESIAN_POINT('Ctrl Pts',(58.8832253930222,247.850286809356,21.3525842887454)) ;
#111208 = CARTESIAN_POINT('Ctrl Pts',(58.8880217651646,247.94548325457,21.3461483892609)) ;
#111209 = CARTESIAN_POINT('Ctrl Pts',(58.8889357985629,247.963889822747,21.3452083120157)) ;
#111210 = CARTESIAN_POINT('Ctrl Pts',(58.8903767283326,247.993419333748,21.344187633411)) ;
#111211 = CARTESIAN_POINT('Ctrl Pts',(58.8909132960796,248.004533747088,21.3439140306238)) ;
#111212 = CARTESIAN_POINT('Ctrl Pts',(58.8919801750569,248.026897197378,21.3435858951377)) ;
#111213 = CARTESIAN_POINT('Ctrl Pts',(58.8925103329082,248.038145668024,21.3435339741781)) ;
#111214 = CARTESIAN_POINT('Ctrl Pts',(58.8939235311602,248.068457642554,21.3436989103481)) ;
#111215 = CARTESIAN_POINT('Ctrl Pts',(58.8947957265094,248.087518735271,21.3441275581854)) ;
#111216 = CARTESIAN_POINT('Ctrl Pts',(58.9002313698804,248.208099244399,21.3488965723468)) ;
#111217 = CARTESIAN_POINT('Ctrl Pts',(58.9044247550774,248.309064077088,21.3621276568549)) ;
#111218 = CARTESIAN_POINT('Ctrl Pts',(58.9128581300875,248.506412010373,21.4064886287213)) ;
#111219 = CARTESIAN_POINT('Ctrl Pts',(58.9170850366825,248.602416382107,21.4373511458664)) ;
#111220 = CARTESIAN_POINT('Ctrl Pts',(58.922825496935,248.720511232688,21.4874123225659)) ;
#111221 = CARTESIAN_POINT('Ctrl Pts',(58.9240809350991,248.745680878951,21.4988233492552)) ;
#111222 = CARTESIAN_POINT('Ctrl Pts',(58.926233468294,248.787629872405,21.5191051086089)) ;
#111223 = CARTESIAN_POINT('Ctrl Pts',(58.9271192659513,248.804561618889,21.5276485216295)) ;
#111224 = CARTESIAN_POINT('Ctrl Pts',(58.9289335319453,248.838549624449,21.5455273973439)) ;
#111225 = CARTESIAN_POINT('Ctrl Pts',(58.9298623735548,248.855595657085,21.554875988622)) ;
#111226 = CARTESIAN_POINT('Ctrl Pts',(58.9322637473162,248.898746729296,21.5795263875509)) ;
#111227 = CARTESIAN_POINT('Ctrl Pts',(58.9337508581201,248.924606547087,21.5952416012535)) ;
#111228 = CARTESIAN_POINT('Ctrl Pts',(58.9405909841939,249.039693264303,21.6695151362722)) ;
#111229 = CARTESIAN_POINT('Ctrl Pts',(58.946221265251,249.123624540158,21.7358004508164)) ;
#111230 = CARTESIAN_POINT('Ctrl Pts',(58.9566921257936,249.265621064996,21.8717847574258)) ;
#111231 = CARTESIAN_POINT('Ctrl Pts',(58.9614940015473,249.325458123753,21.9390957679159)) ;
#111232 = CARTESIAN_POINT('Ctrl Pts',(58.9669862199653,249.391135525068,22.0261519612688)) ;
#111233 = CARTESIAN_POINT('Ctrl Pts',(58.967936545685,249.40239475477,22.0416194331383)) ;
#111234 = CARTESIAN_POINT('Ctrl Pts',(58.9694203489835,249.419858301762,22.0664933944996)) ;
#111235 = CARTESIAN_POINT('Ctrl Pts',(58.9699644587535,249.426236415168,22.0757752987595)) ;
#111236 = CARTESIAN_POINT('Ctrl Pts',(58.9710324195051,249.438717222206,22.0943359539026)) ;
#111237 = CARTESIAN_POINT('Ctrl Pts',(58.9715563898702,249.444822179253,22.1036124282152)) ;
#111238 = CARTESIAN_POINT('Ctrl Pts',(58.9729320575894,249.460779244435,22.1283914479827)) ;
#111239 = CARTESIAN_POINT('Ctrl Pts',(58.9737739021991,249.470469876354,22.1439966904043)) ;
#111240 = CARTESIAN_POINT('Ctrl Pts',(58.9794742523339,249.535316435537,22.2523528520838)) ;
#111241 = CARTESIAN_POINT('Ctrl Pts',(58.9839071642455,249.58167315091,22.3500863143635)) ;
#111242 = CARTESIAN_POINT('Ctrl Pts',(58.9924770014192,249.651419951054,22.5432776526206)) ;
#111243 = CARTESIAN_POINT('Ctrl Pts',(58.9965868135225,249.676463579344,22.6376572512019)) ;
#111244 = CARTESIAN_POINT('Ctrl Pts',(59.0021600130385,249.697771279016,22.7600966090702)) ;
#111245 = CARTESIAN_POINT('Ctrl Pts',(59.0033807261859,249.701735556985,22.786628200569)) ;
#111246 = CARTESIAN_POINT('Ctrl Pts',(59.0054920409605,249.70739697299,22.8319242948974)) ;
#111247 = CARTESIAN_POINT('Ctrl Pts',(59.0063724087197,249.709417253397,22.8506434567142)) ;
#111248 = CARTESIAN_POINT('Ctrl Pts',(59.008191851812,249.712901249862,22.8889593358785)) ;
#111249 = CARTESIAN_POINT('Ctrl Pts',(59.0091316703644,249.71433654715,22.908555651142)) ;
#111250 = CARTESIAN_POINT('Ctrl Pts',(59.0115994151221,249.717168420724,22.9594836213597)) ;
#111251 = CARTESIAN_POINT('Ctrl Pts',(59.0131435349899,249.718031200923,22.9908363139679)) ;
#111252 = CARTESIAN_POINT('Ctrl Pts',(59.0196052657794,249.717964004018,23.1199459778461)) ;
#111253 = CARTESIAN_POINT('Ctrl Pts',(59.024745600192,249.709370144375,23.2174968252151)) ;
#111254 = CARTESIAN_POINT('Ctrl Pts',(59.0350639591994,249.675580179381,23.408402413195)) ;
#111255 = CARTESIAN_POINT('Ctrl Pts',(59.040217835334,249.65071716102,23.5014598733502)) ;
#111256 = CARTESIAN_POINT('Ctrl Pts',(59.0460433831368,249.611411359966,23.610151451488)) ;
#111257 = CARTESIAN_POINT('Ctrl Pts',(59.04700933739,249.604486250839,23.6283087232919)) ;
#111258 = CARTESIAN_POINT('Ctrl Pts',(59.0485115797545,249.593028602881,23.6568506833149)) ;
#111259 = CARTESIAN_POINT('Ctrl Pts',(59.0490589241114,249.588703800771,23.6673164053325)) ;
#111260 = CARTESIAN_POINT('Ctrl Pts',(59.0501276907253,249.579949729371,23.6879075053629)) ;
#111261 = CARTESIAN_POINT('Ctrl Pts',(59.050649342149,249.57552575876,23.6980344042429)) ;
#111262 = CARTESIAN_POINT('Ctrl Pts',(59.0520106772798,249.563592389382,23.7246315747849)) ;
#111263 = CARTESIAN_POINT('Ctrl Pts',(59.0528408818623,249.555915767636,23.7410257122566)) ;
#111264 = CARTESIAN_POINT('Ctrl Pts',(59.0546844514362,249.538015911516,23.7776952715522)) ;
#111265 = CARTESIAN_POINT('Ctrl Pts',(59.055690540886,249.527643300369,23.7978940250859)) ;
#111266 = CARTESIAN_POINT('Ctrl Pts',(59.0589846081115,249.49183639373,23.8642702780622)) ;
#111267 = CARTESIAN_POINT('Ctrl Pts',(59.0612080670382,249.464635510417,23.9094606537765)) ;
#111268 = CARTESIAN_POINT('Ctrl Pts',(59.0687421837228,249.364582981845,24.0592303900436)) ;
#111269 = CARTESIAN_POINT('Ctrl Pts',(59.0739747414648,249.281985627891,24.1567514518126)) ;
#111270 = CARTESIAN_POINT('Ctrl Pts',(59.0809289571639,249.168587520957,24.2633065079118)) ;
#111271 = CARTESIAN_POINT('Ctrl Pts',(59.0822093487065,249.14754304456,24.2821044511304)) ;
#111272 = CARTESIAN_POINT('Ctrl Pts',(59.0843038949953,249.112950355457,24.3114699540109)) ;
#111273 = CARTESIAN_POINT('Ctrl Pts',(59.0851041141105,249.099696076997,24.3223759355834)) ;
#111274 = CARTESIAN_POINT('Ctrl Pts',(59.0868052296141,249.071460111801,24.3448916749606)) ;
#111275 = CARTESIAN_POINT('Ctrl Pts',(59.0877078081271,249.056444406092,24.3564547200788)) ;
#111276 = CARTESIAN_POINT('Ctrl Pts',(59.0899474364691,249.019121589641,24.3842012663169)) ;
#111277 = CARTESIAN_POINT('Ctrl Pts',(59.0912953489291,248.996605959164,24.4000938881119)) ;
#111278 = CARTESIAN_POINT('Ctrl Pts',(59.0975763310836,248.89147858849,24.4704836188712)) ;
#111279 = CARTESIAN_POINT('Ctrl Pts',(59.102751724479,248.804546483278,24.5181531354213)) ;
#111280 = CARTESIAN_POINT('Ctrl Pts',(59.113535694934,248.618754302963,24.5996090550592)) ;
#111281 = CARTESIAN_POINT('Ctrl Pts',(59.1191279591078,248.519902044397,24.6324054936291)) ;
#111282 = CARTESIAN_POINT('Ctrl Pts',(59.1253051408544,248.400312364848,24.6600897694251)) ;
#111283 = CARTESIAN_POINT('Ctrl Pts',(59.1262394457633,248.381906318736,24.6640256107041)) ;
#111284 = CARTESIAN_POINT('Ctrl Pts',(59.1277043253735,248.352449302477,24.6698079774404)) ;
#111285 = CARTESIAN_POINT('Ctrl Pts',(59.1282451036836,248.341439720121,24.6718548982652)) ;
#111286 = CARTESIAN_POINT('Ctrl Pts',(59.1293124388825,248.319413677259,24.675722286849)) ;
#111287 = CARTESIAN_POINT('Ctrl Pts',(59.1298389994593,248.308397897902,24.677543315478)) ;
#111288 = CARTESIAN_POINT('Ctrl Pts',(59.1312304569059,248.278924256982,24.6821138564977)) ;
#111289 = CARTESIAN_POINT('Ctrl Pts',(59.1320850859488,248.260436928664,24.6846656777916)) ;
#111290 = CARTESIAN_POINT('Ctrl Pts',(59.1339935648034,248.218426788412,24.6897516526688)) ;
#111291 = CARTESIAN_POINT('Ctrl Pts',(59.1350393274011,248.194885019713,24.6920978202689)) ;
#111292 = CARTESIAN_POINT('Ctrl Pts',(59.1385387753894,248.114803847398,24.6983714843983)) ;
#111293 = CARTESIAN_POINT('Ctrl Pts',(59.1409191793168,248.058116498361,24.6999323936584)) ;
#111294 = CARTESIAN_POINT('Ctrl Pts',(59.1482633569917,247.882275219614,24.6958639063609)) ;
#111295 = CARTESIAN_POINT('Ctrl Pts',(59.1531844219596,247.76372828289,24.680411270846)) ;
#111296 = CARTESIAN_POINT('Ctrl Pts',(59.1598032730574,247.6193888287,24.6456860174553)) ;
#111297 = CARTESIAN_POINT('Ctrl Pts',(59.1611280950841,247.591134131045,24.6381016937144)) ;
#111298 = CARTESIAN_POINT('Ctrl Pts',(59.1633639478416,247.544634214823,24.6243068672195)) ;
#111299 = CARTESIAN_POINT('Ctrl Pts',(59.164261470855,247.526271530763,24.6185136140823)) ;
#111300 = CARTESIAN_POINT('Ctrl Pts',(59.1660708691775,247.489883050916,24.6063408902297)) ;
#111301 = CARTESIAN_POINT('Ctrl Pts',(59.166982462753,247.471858531281,24.599966747521)) ;
#111302 = CARTESIAN_POINT('Ctrl Pts',(59.1692784594062,247.427244067947,24.5833262747688)) ;
#111303 = CARTESIAN_POINT('Ctrl Pts',(59.1706749877738,247.400800053489,24.5726880132938)) ;
#111304 = CARTESIAN_POINT('Ctrl Pts',(59.1739768072608,247.339880550374,24.5463582163533)) ;
#111305 = CARTESIAN_POINT('Ctrl Pts',(59.1758968835936,247.305654166584,24.5301686814799)) ;
#111306 = CARTESIAN_POINT('Ctrl Pts',(59.1778464475999,247.272018857277,24.5128439810119)) ;
#111307 = CARTESIAN_POINT('Ctrl Pts',(59.2757724421406,247.272018954284,24.5128440309779)) ;
#111308 = CARTESIAN_POINT('Ctrl Pts',(59.2756832338205,247.273710551664,24.5137153300333)) ;
#111309 = CARTESIAN_POINT('Ctrl Pts',(59.2755941944142,247.275403640655,24.5145837561406)) ;
#111310 = CARTESIAN_POINT('Ctrl Pts',(59.274664186804,247.293136301171,24.5236411934761)) ;
#111311 = CARTESIAN_POINT('Ctrl Pts',(59.2738379793636,247.309305809266,24.5315746064805)) ;
#111312 = CARTESIAN_POINT('Ctrl Pts',(59.2691900068813,247.40235556953,24.5753839694454)) ;
#111313 = CARTESIAN_POINT('Ctrl Pts',(59.2656309187946,247.481747968796,24.6056509131867)) ;
#111314 = CARTESIAN_POINT('Ctrl Pts',(59.2572898826209,247.673398463464,24.6625063832365)) ;
#111315 = CARTESIAN_POINT('Ctrl Pts',(59.2525282212603,247.786773605299,24.6837953462717)) ;
#111316 = CARTESIAN_POINT('Ctrl Pts',(59.2460817644186,247.93100929316,24.6957723084332)) ;
#111317 = CARTESIAN_POINT('Ctrl Pts',(59.2447383994796,247.960650548587,24.6974431363461)) ;
#111318 = CARTESIAN_POINT('Ctrl Pts',(59.2424802275104,248.009642506877,24.6989022418924)) ;
#111319 = CARTESIAN_POINT('Ctrl Pts',(59.2415795418324,248.028973428159,24.6991437044648)) ;
#111320 = CARTESIAN_POINT('Ctrl Pts',(59.239770799108,248.067346942264,24.6989598424482)) ;
#111321 = CARTESIAN_POINT('Ctrl Pts',(59.2388631858678,248.086386687892,24.6985443826624)) ;
#111322 = CARTESIAN_POINT('Ctrl Pts',(59.2365913380461,248.133491807594,24.6967138361549)) ;
#111323 = CARTESIAN_POINT('Ctrl Pts',(59.2352155180496,248.161535854383,24.6949176253331)) ;
#111324 = CARTESIAN_POINT('Ctrl Pts',(59.2286621040817,248.292853503695,24.6831888805836)) ;
#111325 = CARTESIAN_POINT('Ctrl Pts',(59.2232167922381,248.395095754938,24.6643962503533)) ;
#111326 = CARTESIAN_POINT('Ctrl Pts',(59.2125418273794,248.588182566326,24.6100354308629)) ;
#111327 = CARTESIAN_POINT('Ctrl Pts',(59.2073467257661,248.678984786095,24.5757553602442)) ;
#111328 = CARTESIAN_POINT('Ctrl Pts',(59.2014859311529,248.783818635691,24.5254313073959)) ;
#111329 = CARTESIAN_POINT('Ctrl Pts',(59.2005212819831,248.801166668533,24.5167301580052)) ;
#111330 = CARTESIAN_POINT('Ctrl Pts',(59.1990206350808,248.828386947691,24.5024810728117)) ;
#111331 = CARTESIAN_POINT('Ctrl Pts',(59.1984736158019,248.838360323534,24.4971310293533)) ;
#111332 = CARTESIAN_POINT('Ctrl Pts',(59.1974051062263,248.85796506062,24.4863575446352)) ;
#111333 = CARTESIAN_POINT('Ctrl Pts',(59.1968833943735,248.867598392539,24.4809390806193)) ;
#111334 = CARTESIAN_POINT('Ctrl Pts',(59.1955213675278,248.892877620234,24.4663895831641)) ;
#111335 = CARTESIAN_POINT('Ctrl Pts',(59.1946905523746,248.908430773549,24.4570994443033)) ;
#111336 = CARTESIAN_POINT('Ctrl Pts',(59.1928453212638,248.943151769816,24.4355895184086)) ;
#111337 = CARTESIAN_POINT('Ctrl Pts',(59.1918382021674,248.962228043646,24.4232283424403)) ;
#111338 = CARTESIAN_POINT('Ctrl Pts',(59.1885387492599,249.024780274094,24.3808660889052)) ;
#111339 = CARTESIAN_POINT('Ctrl Pts',(59.1863111621762,249.067091650836,24.3491992774067)) ;
#111340 = CARTESIAN_POINT('Ctrl Pts',(59.1787824063012,249.205946775922,24.2346648135798)) ;
#111341 = CARTESIAN_POINT('Ctrl Pts',(59.1735582698871,249.294527689775,24.1428561113039)) ;
#111342 = CARTESIAN_POINT('Ctrl Pts',(59.1666132026627,249.389067246547,24.0195064469067)) ;
#111343 = CARTESIAN_POINT('Ctrl Pts',(59.1653315961221,249.405678283071,23.9966610335597)) ;
#111344 = CARTESIAN_POINT('Ctrl Pts',(59.1632357144701,249.431445739271,23.9592735358202)) ;
#111345 = CARTESIAN_POINT('Ctrl Pts',(59.1624354163397,249.440969454907,23.944990764425)) ;
#111346 = CARTESIAN_POINT('Ctrl Pts',(59.1607346766371,249.460537674307,23.9146454260799)) ;
#111347 = CARTESIAN_POINT('Ctrl Pts',(59.1598325646368,249.470532608402,23.8985538968733)) ;
#111348 = CARTESIAN_POINT('Ctrl Pts',(59.1575952925211,249.494374606878,23.8586780385084)) ;
#111349 = CARTESIAN_POINT('Ctrl Pts',(59.1562493168796,249.507912701337,23.8347161732236)) ;
#111350 = CARTESIAN_POINT('Ctrl Pts',(59.150008424147,249.56704370909,23.7237703359854)) ;
#111351 = CARTESIAN_POINT('Ctrl Pts',(59.1448752581481,249.605529245702,23.6332296458638)) ;
#111352 = CARTESIAN_POINT('Ctrl Pts',(59.1340771840239,249.668321215754,23.4400090897544)) ;
#111353 = CARTESIAN_POINT('Ctrl Pts',(59.1284249762466,249.69132651387,23.3373348111415)) ;
#111354 = CARTESIAN_POINT('Ctrl Pts',(59.1222023406101,249.706946259922,23.2146301974013)) ;
#111355 = CARTESIAN_POINT('Ctrl Pts',(59.1212742391056,249.70899744145,23.1960407298871)) ;
#111356 = CARTESIAN_POINT('Ctrl Pts',(59.1198167510851,249.711776892762,23.1662969678575)) ;
#111357 = CARTESIAN_POINT('Ctrl Pts',(59.119277323937,249.712705220842,23.1551633495173)) ;
#111358 = CARTESIAN_POINT('Ctrl Pts',(59.1182103668189,249.714340401072,23.132864552665)) ;
#111359 = CARTESIAN_POINT('Ctrl Pts',(59.1176828777974,249.715046930052,23.1216999164919)) ;
#111360 = CARTESIAN_POINT('Ctrl Pts',(59.1162855029825,249.716639866945,23.0917838042115)) ;
#111361 = CARTESIAN_POINT('Ctrl Pts',(59.1154260441635,249.717323349405,23.0730227318097)) ;
#111362 = CARTESIAN_POINT('Ctrl Pts',(59.1106028756525,249.719423330873,22.9660616467604)) ;
#111363 = CARTESIAN_POINT('Ctrl Pts',(59.1069180968881,249.714197124594,22.877862799474)) ;
#111364 = CARTESIAN_POINT('Ctrl Pts',(59.0986812719752,249.687015575204,22.6821873776594)) ;
#111365 = CARTESIAN_POINT('Ctrl Pts',(59.0941397554922,249.661423920133,22.5756291101106)) ;
#111366 = CARTESIAN_POINT('Ctrl Pts',(59.0879345999278,249.615792645264,22.4438554301119)) ;
#111367 = CARTESIAN_POINT('Ctrl Pts',(59.0865722535898,249.60516951322,22.4156580422304)) ;
#111368 = CARTESIAN_POINT('Ctrl Pts',(59.0842910679346,249.586462163637,22.369786284481)) ;
#111369 = CARTESIAN_POINT('Ctrl Pts',(59.0833869848968,249.578819712629,22.3519387959534)) ;
#111370 = CARTESIAN_POINT('Ctrl Pts',(59.0815782390122,249.563097403902,22.3169149055017)) ;
#111371 = CARTESIAN_POINT('Ctrl Pts',(59.0806741784275,249.555032355823,22.2997350253682)) ;
#111372 = CARTESIAN_POINT('Ctrl Pts',(59.0784245944884,249.534471831554,22.2578021567064)) ;
#111373 = CARTESIAN_POINT('Ctrl Pts',(59.0770679827655,249.521651151157,22.2332156341506)) ;
#111374 = CARTESIAN_POINT('Ctrl Pts',(59.0701848029926,249.454545247717,22.1119531686992)) ;
#111375 = CARTESIAN_POINT('Ctrl Pts',(59.0643456032795,249.391385998898,22.0205188670627)) ;
#111376 = CARTESIAN_POINT('Ctrl Pts',(59.0536820571112,249.26185125817,21.8678194649851)) ;
#111377 = CARTESIAN_POINT('Ctrl Pts',(59.0489049680732,249.198660974826,21.8043742735574)) ;
#111378 = CARTESIAN_POINT('Ctrl Pts',(59.0433791905355,249.115472558587,21.733230219853)) ;
#111379 = CARTESIAN_POINT('Ctrl Pts',(59.0423809018738,249.099998770894,21.7204699080264)) ;
#111380 = CARTESIAN_POINT('Ctrl Pts',(59.0408406350502,249.075336421302,21.7008645362373)) ;
#111381 = CARTESIAN_POINT('Ctrl Pts',(59.0402867037317,249.066300565406,21.6938312036526)) ;
#111382 = CARTESIAN_POINT('Ctrl Pts',(59.0392159284342,249.048484937863,21.6802544575572)) ;
#111383 = CARTESIAN_POINT('Ctrl Pts',(59.0386986353898,249.039711863784,21.6737035124262)) ;
#111384 = CARTESIAN_POINT('Ctrl Pts',(59.0373644982815,249.016675734297,21.6568508919402)) ;
#111385 = CARTESIAN_POINT('Ctrl Pts',(59.0365564353191,249.002313280192,21.6466865915394)) ;
#111386 = CARTESIAN_POINT('Ctrl Pts',(59.0347711755006,248.969757747503,21.6244072801883)) ;
#111387 = CARTESIAN_POINT('Ctrl Pts',(59.0338005635506,248.951482329002,21.6124179650065)) ;
#111388 = CARTESIAN_POINT('Ctrl Pts',(59.0306825977539,248.891184782886,21.5745248579657)) ;
#111389 = CARTESIAN_POINT('Ctrl Pts',(59.0285926323636,248.848251720638,21.5501169208241)) ;
#111390 = CARTESIAN_POINT('Ctrl Pts',(59.0208652754726,248.684121063009,21.4661619896179)) ;
#111391 = CARTESIAN_POINT('Ctrl Pts',(59.0153460338213,248.556968156538,21.4194199658274)) ;
#111392 = CARTESIAN_POINT('Ctrl Pts',(59.0080817135993,248.39918600657,21.3821874172139)) ;
#111393 = CARTESIAN_POINT('Ctrl Pts',(59.0068479444681,248.372637394238,21.376598625297)) ;
#111394 = CARTESIAN_POINT('Ctrl Pts',(59.0047299598419,248.327590647772,21.3682509753661)) ;
#111395 = CARTESIAN_POINT('Ctrl Pts',(59.0038565676469,248.309160398292,21.3651532048937)) ;
#111396 = CARTESIAN_POINT('Ctrl Pts',(59.0020510631478,248.27138542847,21.359451116319)) ;
#111397 = CARTESIAN_POINT('Ctrl Pts',(59.0011182035658,248.252039363202,21.3568752238686)) ;
#111398 = CARTESIAN_POINT('Ctrl Pts',(58.9986919659079,248.202183982957,21.3511203296651)) ;
#111399 = CARTESIAN_POINT('Ctrl Pts',(58.9971834057496,248.171625359811,21.3484395524482)) ;
#111400 = CARTESIAN_POINT('Ctrl Pts',(58.9937842867575,248.103738671579,21.3443556846649)) ;
#111401 = CARTESIAN_POINT('Ctrl Pts',(58.9918828540747,248.066403104802,21.3433585082654)) ;
#111402 = CARTESIAN_POINT('Ctrl Pts',(58.9852501600673,247.938082526444,21.3442150068167)) ;
#111403 = CARTESIAN_POINT('Ctrl Pts',(58.9803795988204,247.847302454304,21.3522226315655)) ;
#111404 = CARTESIAN_POINT('Ctrl Pts',(58.9717395520393,247.687052260192,21.3796102814224)) ;
#111405 = CARTESIAN_POINT('Ctrl Pts',(58.9679687205315,247.617317290485,21.3961779373445)) ;
#111406 = CARTESIAN_POINT('Ctrl Pts',(58.9635355362364,247.532637767708,21.4221183368638)) ;
#111407 = CARTESIAN_POINT('Ctrl Pts',(58.9626976219862,247.516500882964,21.4273304905638)) ;
#111408 = CARTESIAN_POINT('Ctrl Pts',(58.9613981210444,247.491204560043,21.4359267556684)) ;
#111409 = CARTESIAN_POINT('Ctrl Pts',(58.9609277845549,247.481991193062,21.4391476095167)) ;
#111410 = CARTESIAN_POINT('Ctrl Pts',(58.9599251710927,247.462209461428,21.4462573199981)) ;
#111411 = CARTESIAN_POINT('Ctrl Pts',(58.9593944861244,247.451651061834,21.450172554115)) ;
#111412 = CARTESIAN_POINT('Ctrl Pts',(58.9579777970654,247.423264218973,21.4610252073203)) ;
#111413 = CARTESIAN_POINT('Ctrl Pts',(58.9571027345452,247.405513312165,21.4681618777725)) ;
#111414 = CARTESIAN_POINT('Ctrl Pts',(58.955139455352,247.365349113441,21.4851133457979)) ;
#111415 = CARTESIAN_POINT('Ctrl Pts',(58.9540600469222,247.343020455939,21.4951180248594)) ;
#111416 = CARTESIAN_POINT('Ctrl Pts',(58.9503786464123,247.266519163842,21.5314250365684)) ;
#111417 = CARTESIAN_POINT('Ctrl Pts',(58.9478580874344,247.21354743314,21.5601532427633)) ;
#111418 = CARTESIAN_POINT('Ctrl Pts',(58.9406477027788,247.066241987889,21.6506220243604)) ;
#111419 = CARTESIAN_POINT('Ctrl Pts',(58.9359784797362,246.976434506998,21.7190923748397)) ;
#111420 = CARTESIAN_POINT('Ctrl Pts',(58.9296327427801,246.872337684337,21.8164617003937)) ;
#111421 = CARTESIAN_POINT('Ctrl Pts',(58.9282803263903,246.851055079706,21.8374630033313)) ;
#111422 = CARTESIAN_POINT('Ctrl Pts',(58.9260111853406,246.816926029838,21.8729903431372)) ;
#111423 = CARTESIAN_POINT('Ctrl Pts',(58.9251088835541,246.803749775198,21.887190683996)) ;
#111424 = CARTESIAN_POINT('Ctrl Pts',(58.9233001766887,246.778134663553,21.9157737630462)) ;
#111425 = CARTESIAN_POINT('Ctrl Pts',(58.9223942915969,246.765688580717,21.9301461410217)) ;
#111426 = CARTESIAN_POINT('Ctrl Pts',(58.9201332532231,246.735575535026,21.9661381066379)) ;
#111427 = CARTESIAN_POINT('Ctrl Pts',(58.9187667565292,246.718199287022,21.9879925712087)) ;
#111428 = CARTESIAN_POINT('Ctrl Pts',(58.9120650556819,246.63691815688,22.0956294463276)) ;
#111429 = CARTESIAN_POINT('Ctrl Pts',(58.9064422590297,246.5807775837,22.1869479321452)) ;
#111430 = CARTESIAN_POINT('Ctrl Pts',(58.8957605556408,246.492477302808,22.3671194538856)) ;
#111431 = CARTESIAN_POINT('Ctrl Pts',(58.8907432286155,246.458358890063,22.4545748597694)) ;
#111432 = CARTESIAN_POINT('Ctrl Pts',(58.8850297653321,246.426151035413,22.5632103880907)) ;
#111433 = CARTESIAN_POINT('Ctrl Pts',(58.8840553706572,246.420910909986,22.5820925991769)) ;
#111434 = CARTESIAN_POINT('Ctrl Pts',(58.8825432344746,246.413158080223,22.6120566921717)) ;
#111435 = CARTESIAN_POINT('Ctrl Pts',(58.8819942043579,246.410425208202,22.6230792976749)) ;
#111436 = CARTESIAN_POINT('Ctrl Pts',(58.8809251145403,246.405261114147,22.6448519498689)) ;
#111437 = CARTESIAN_POINT('Ctrl Pts',(58.8804047660875,246.402823512767,22.6555997660341)) ;
#111438 = CARTESIAN_POINT('Ctrl Pts',(58.8790512412998,246.396693094635,22.6839206939715)) ;
#111439 = CARTESIAN_POINT('Ctrl Pts',(58.8782273446952,246.393176093099,22.7015308686017)) ;
#111440 = CARTESIAN_POINT('Ctrl Pts',(58.8736452966569,246.374921429963,22.8012446361361)) ;
#111441 = CARTESIAN_POINT('Ctrl Pts',(58.8701411218086,246.36603908736,22.8843078139307)) ;
#111442 = CARTESIAN_POINT('Ctrl Pts',(58.8617767426315,246.359633400343,23.0846081531142)) ;
#111443 = CARTESIAN_POINT('Ctrl Pts',(58.8569414150446,246.368132146755,23.201592323637)) ;
#111444 = CARTESIAN_POINT('Ctrl Pts',(58.8504151549209,246.393920590317,23.3457654695649)) ;
#111445 = CARTESIAN_POINT('Ctrl Pts',(58.8490799687286,246.399878087681,23.3746547676323)) ;
#111446 = CARTESIAN_POINT('Ctrl Pts',(58.8468316993007,246.410987738129,23.4221602807902)) ;
#111447 = CARTESIAN_POINT('Ctrl Pts',(58.8459324668906,246.415705477713,23.4408717399387)) ;
#111448 = CARTESIAN_POINT('Ctrl Pts',(58.8441236294452,246.42572615438,23.4779085854282)) ;
#111449 = CARTESIAN_POINT('Ctrl Pts',(58.8432143983577,246.431020989747,23.4962331635209)) ;
#111450 = CARTESIAN_POINT('Ctrl Pts',(58.8409324641281,246.444935497676,23.5414813961833)) ;
#111451 = CARTESIAN_POINT('Ctrl Pts',(58.8395479485843,246.453925187186,23.5682843485361)) ;
#111452 = CARTESIAN_POINT('Ctrl Pts',(58.8328216666303,246.500165118509,23.695402307595)) ;
#111453 = CARTESIAN_POINT('Ctrl Pts',(58.8271933792132,246.546274434922,23.7922167174662)) ;
#111454 = CARTESIAN_POINT('Ctrl Pts',(58.8165664935499,246.648902277645,23.963410117423)) ;
#111455 = CARTESIAN_POINT('Ctrl Pts',(58.8116095845956,246.703024063899,24.0387739582984)) ;
#111456 = CARTESIAN_POINT('Ctrl Pts',(58.8059404796308,246.775901722118,24.1243255587703)) ;
#111457 = CARTESIAN_POINT('Ctrl Pts',(58.8049577719186,246.788976536466,24.1391361816344)) ;
#111458 = CARTESIAN_POINT('Ctrl Pts',(58.8034358438087,246.809997031716,24.1621162160562)) ;
#111459 = CARTESIAN_POINT('Ctrl Pts',(58.8028851051076,246.817769270327,24.1704411825542)) ;
#111460 = CARTESIAN_POINT('Ctrl Pts',(58.8018154691542,246.833210207075,24.1866462238561)) ;
#111461 = CARTESIAN_POINT('Ctrl Pts',(58.8012962267056,246.840872689327,24.1945312255709)) ;
#111462 = CARTESIAN_POINT('Ctrl Pts',(58.7999496706984,246.861160494751,24.2150016827531)) ;
#111463 = CARTESIAN_POINT('Ctrl Pts',(58.7991314570207,246.873910179236,24.2274625625539)) ;
#111464 = CARTESIAN_POINT('Ctrl Pts',(58.7947027895651,246.945032188495,24.2947909260585)) ;
#111465 = CARTESIAN_POINT('Ctrl Pts',(58.7913266365165,247.007082701722,24.3456309901094)) ;
#111466 = CARTESIAN_POINT('Ctrl Pts',(58.7847244126569,247.136185351128,24.4367907842065)) ;
#111467 = CARTESIAN_POINT('Ctrl Pts',(58.7815055650463,247.202845155603,24.4772143680056)) ;
#111468 = CARTESIAN_POINT('Ctrl Pts',(58.7781769759756,247.272019165218,24.5128441396244)) ;
#111469 = CARTESIAN_POINT('Origin',(61.8645744874958,248.040265107786,23.0213203435596)) ;
#111470 = CARTESIAN_POINT('',(58.1788076829103,247.272018954284,24.5128440309778)) ;
#111471 = CARTESIAN_POINT('',(58.2783798877068,247.272019130299,24.5128441216388)) ;
#111472 = CARTESIAN_POINT('',(61.8645744874958,247.272018954284,24.5128440309778)) ;
#111473 = CARTESIAN_POINT('',(58.5159557280534,249.718014455466,23.019840864003)) ;
#111474 = CARTESIAN_POINT('Ctrl Pts',(58.5159557280534,249.718014455466,23.019840864003)) ;
#111475 = CARTESIAN_POINT('Ctrl Pts',(58.512319144992,249.717946765379,22.9430794117974)) ;
#111476 = CARTESIAN_POINT('Ctrl Pts',(58.5086825619307,249.712607036384,22.8665495704283)) ;
#111477 = CARTESIAN_POINT('Ctrl Pts',(58.5050459788693,249.702113747406,22.7908769416287)) ;
#111478 = CARTESIAN_POINT('Ctrl Pts',(58.501409395808,249.691620458428,22.7152043128292)) ;
#111479 = CARTESIAN_POINT('Ctrl Pts',(58.4977728127466,249.675973792176,22.6403886898807)) ;
#111480 = CARTESIAN_POINT('Ctrl Pts',(58.4941362296853,249.655340419636,22.5670332101811)) ;
#111481 = CARTESIAN_POINT('Ctrl Pts',(58.4912273357581,249.638835835232,22.5083563407627)) ;
#111482 = CARTESIAN_POINT('Ctrl Pts',(58.488318441831,249.619095809122,22.4504605153754)) ;
#111483 = CARTESIAN_POINT('Ctrl Pts',(58.4854095479039,249.596212549723,22.3937276249675)) ;
#111484 = CARTESIAN_POINT('Ctrl Pts',(58.4824763077287,249.573137766837,22.3365199035561)) ;
#111485 = CARTESIAN_POINT('Ctrl Pts',(58.4795430675535,249.54686695187,22.2804952007317)) ;
#111486 = CARTESIAN_POINT('Ctrl Pts',(58.4766098273783,249.517546749281,22.2260317077794)) ;
#111487 = CARTESIAN_POINT('Ctrl Pts',(58.4737088759363,249.488549299736,22.1721677419993)) ;
#111488 = CARTESIAN_POINT('Ctrl Pts',(58.4708079244942,249.456569502694,22.1198312496985)) ;
#111489 = CARTESIAN_POINT('Ctrl Pts',(58.4679069730521,249.421797367442,22.0693677827505)) ;
#111490 = CARTESIAN_POINT('Ctrl Pts',(58.4650077825223,249.387046339292,22.0189349477316)) ;
#111491 = CARTESIAN_POINT('Ctrl Pts',(58.4621085919926,249.349506622877,21.9703733030639)) ;
#111492 = CARTESIAN_POINT('Ctrl Pts',(58.4592094014628,249.309412361891,21.9240007411198)) ;
#111493 = CARTESIAN_POINT('Ctrl Pts',(58.4563109008991,249.269327642768,21.8776392151865)) ;
#111494 = CARTESIAN_POINT('Ctrl Pts',(58.4534124003355,249.226689919712,21.8334661235975)) ;
#111495 = CARTESIAN_POINT('Ctrl Pts',(58.4505138997719,249.18177324594,21.7917658579719)) ;
#111496 = CARTESIAN_POINT('Ctrl Pts',(58.4475553900992,249.135926639771,21.749202250859)) ;
#111497 = CARTESIAN_POINT('Ctrl Pts',(58.4445968804265,249.087706025917,21.7092154260372)) ;
#111498 = CARTESIAN_POINT('Ctrl Pts',(58.4416383707538,249.037440157736,21.6720661116754)) ;
#111499 = CARTESIAN_POINT('Ctrl Pts',(58.4387362096991,248.988131667599,21.6356243537374)) ;
#111500 = CARTESIAN_POINT('Ctrl Pts',(58.4358340486445,248.936855629865,21.6019131867214)) ;
#111501 = CARTESIAN_POINT('Ctrl Pts',(58.4329318875898,248.88395137375,21.5711346495455)) ;
#111502 = CARTESIAN_POINT('Ctrl Pts',(58.4299452036081,248.829506327,21.5394597141334)) ;
#111503 = CARTESIAN_POINT('Ctrl Pts',(58.4269585196264,248.773337245491,21.5108911838589)) ;
#111504 = CARTESIAN_POINT('Ctrl Pts',(58.4239718356447,248.715838132977,21.4855970123135)) ;
#111505 = CARTESIAN_POINT('Ctrl Pts',(58.4209851516631,248.658339020463,21.460302840768)) ;
#111506 = CARTESIAN_POINT('Ctrl Pts',(58.4179984676814,248.599510445876,21.4382831667924)) ;
#111507 = CARTESIAN_POINT('Ctrl Pts',(58.4150117836997,248.539762635379,21.4196501894927)) ;
#111508 = CARTESIAN_POINT('Ctrl Pts',(58.4121032756731,248.481578713856,21.401504927266)) ;
#111509 = CARTESIAN_POINT('Ctrl Pts',(58.4091947676465,248.422286197173,21.3864972799856)) ;
#111510 = CARTESIAN_POINT('Ctrl Pts',(58.4062862596199,248.36225544961,21.3747580816722)) ;
#111511 = CARTESIAN_POINT('Ctrl Pts',(58.4033529712071,248.301713242189,21.3629188658018)) ;
#111512 = CARTESIAN_POINT('Ctrl Pts',(58.4004196827944,248.240420639795,21.3544042929628)) ;
#111513 = CARTESIAN_POINT('Ctrl Pts',(58.3974863943817,248.178774750602,21.3492975741731)) ;
#111514 = CARTESIAN_POINT('Ctrl Pts',(58.3945858116232,248.117816202324,21.3442477944074)) ;
#111515 = CARTESIAN_POINT('Ctrl Pts',(58.3916852288648,248.056512725529,21.3425303093672)) ;
#111516 = CARTESIAN_POINT('Ctrl Pts',(58.3887846461064,247.99525752739,21.3441741423574)) ;
#111517 = CARTESIAN_POINT('Ctrl Pts',(58.3858858168575,247.934039360282,21.3458169815898)) ;
#111518 = CARTESIAN_POINT('Ctrl Pts',(58.3829869876085,247.872869923269,21.3508170959372)) ;
#111519 = CARTESIAN_POINT('Ctrl Pts',(58.3800881583596,247.812143285866,21.3591514301023)) ;
#111520 = CARTESIAN_POINT('Ctrl Pts',(58.3771900111413,247.7514309361,21.3674838033825)) ;
#111521 = CARTESIAN_POINT('Ctrl Pts',(58.3742918639229,247.69116168467,21.3791487696651)) ;
#111522 = CARTESIAN_POINT('Ctrl Pts',(58.3713937167045,247.63172326158,21.3940715542227)) ;
#111523 = CARTESIAN_POINT('Ctrl Pts',(58.3684348517887,247.57103957249,21.4093069789088)) ;
#111524 = CARTESIAN_POINT('Ctrl Pts',(58.3654759868728,247.511222467808,21.4279381960708)) ;
#111525 = CARTESIAN_POINT('Ctrl Pts',(58.3625171219569,247.452669923237,21.4498315712183)) ;
#111526 = CARTESIAN_POINT('Ctrl Pts',(58.3596152908466,247.395246012293,21.4713029390971)) ;
#111527 = CARTESIAN_POINT('Ctrl Pts',(58.3567134597363,247.339038791254,21.4959115382701)) ;
#111528 = CARTESIAN_POINT('Ctrl Pts',(58.3538116286261,247.284402505327,21.5234829729803)) ;
#111529 = CARTESIAN_POINT('Ctrl Pts',(58.3508242468074,247.228155452686,21.551867258501)) ;
#111530 = CARTESIAN_POINT('Ctrl Pts',(58.3478368649888,247.173573943315,21.58339157008)) ;
#111531 = CARTESIAN_POINT('Ctrl Pts',(58.3448494831701,247.121013786214,21.6178168450647)) ;
#111532 = CARTESIAN_POINT('Ctrl Pts',(58.3418621013515,247.068453629112,21.6522421200494)) ;
#111533 = CARTESIAN_POINT('Ctrl Pts',(58.3388747195328,247.017915251416,21.6895679561089)) ;
#111534 = CARTESIAN_POINT('Ctrl Pts',(58.3358873377142,246.969716489903,21.7295112557881)) ;
#111535 = CARTESIAN_POINT('Ctrl Pts',(58.3329808840848,246.922823433095,21.7683724912673)) ;
#111536 = CARTESIAN_POINT('Ctrl Pts',(58.3300744304555,246.877952616534,21.8098703856135)) ;
#111537 = CARTESIAN_POINT('Ctrl Pts',(58.3271679768261,246.835415446672,21.8537663376942)) ;
#111538 = CARTESIAN_POINT('Ctrl Pts',(58.3242344316138,246.79248178011,21.8980714519302)) ;
#111539 = CARTESIAN_POINT('Ctrl Pts',(58.3213008864014,246.751925950203,21.9448192926936)) ;
#111540 = CARTESIAN_POINT('Ctrl Pts',(58.318367341189,246.714034725236,21.9937221560853)) ;
#111541 = CARTESIAN_POINT('Ctrl Pts',(58.3154688347601,246.676596079769,22.0420409150172)) ;
#111542 = CARTESIAN_POINT('Ctrl Pts',(58.3125703283311,246.641759057408,22.0924630850673)) ;
#111543 = CARTESIAN_POINT('Ctrl Pts',(58.3096718219022,246.60976219787,22.1446753257664)) ;
#111544 = CARTESIAN_POINT('Ctrl Pts',(58.3067750713524,246.577784721631,22.1968559369408)) ;
#111545 = CARTESIAN_POINT('Ctrl Pts',(58.3038783208025,246.548644263484,22.25082403357)) ;
#111546 = CARTESIAN_POINT('Ctrl Pts',(58.3009815702527,246.522536186484,22.3062371428449)) ;
#111547 = CARTESIAN_POINT('Ctrl Pts',(58.298085500658,246.496434246855,22.3616372258537)) ;
#111548 = CARTESIAN_POINT('Ctrl Pts',(58.2951894310634,246.473363491077,22.4184811847766)) ;
#111549 = CARTESIAN_POINT('Ctrl Pts',(58.2922933614687,246.453472472819,22.4764036562443)) ;
#111550 = CARTESIAN_POINT('Ctrl Pts',(58.2893324889904,246.433136370181,22.5356222095421)) ;
#111551 = CARTESIAN_POINT('Ctrl Pts',(58.286371616512,246.41612425942,22.5959676176771)) ;
#111552 = CARTESIAN_POINT('Ctrl Pts',(58.2834107440337,246.402541327335,22.6570321589531)) ;
#111553 = CARTESIAN_POINT('Ctrl Pts',(58.2805109638258,246.389238654587,22.7168367434091)) ;
#111554 = CARTESIAN_POINT('Ctrl Pts',(58.277611183618,246.379225004203,22.777330536764)) ;
#111555 = CARTESIAN_POINT('Ctrl Pts',(58.2747114034101,246.372547084093,22.8381219375916)) ;
#111556 = CARTESIAN_POINT('Ctrl Pts',(58.2717199847966,246.365658129384,22.9008344588676)) ;
#111557 = CARTESIAN_POINT('Ctrl Pts',(58.268728566183,246.36231935317,22.9638631286378)) ;
#111558 = CARTESIAN_POINT('Ctrl Pts',(58.2657371475694,246.362523982039,23.0267772177427)) ;
#111559 = CARTESIAN_POINT('Ctrl Pts',(58.2627457289558,246.362728610907,23.0896913068475)) ;
#111560 = CARTESIAN_POINT('Ctrl Pts',(58.2597543103423,246.366476538335,23.1524902311482)) ;
#111561 = CARTESIAN_POINT('Ctrl Pts',(58.2567628917287,246.373702911042,23.2147512275519)) ;
#111562 = CARTESIAN_POINT('Ctrl Pts',(58.2538499587604,246.380739685902,23.2753786864564)) ;
#111563 = CARTESIAN_POINT('Ctrl Pts',(58.2509370257922,246.391103214285,23.3357435029581)) ;
#111564 = CARTESIAN_POINT('Ctrl Pts',(58.2480240928239,246.404762219472,23.3954531606417)) ;
#111565 = CARTESIAN_POINT('Ctrl Pts',(58.2451162792155,246.418397219521,23.4550578810588)) ;
#111566 = CARTESIAN_POINT('Ctrl Pts',(58.2422084656071,246.435316083139,23.5140092369757)) ;
#111567 = CARTESIAN_POINT('Ctrl Pts',(58.2393006519987,246.455436000457,23.5719216176783)) ;
#111568 = CARTESIAN_POINT('Ctrl Pts',(58.2363957088068,246.475536056617,23.6297768308042)) ;
#111569 = CARTESIAN_POINT('Ctrl Pts',(58.233490765615,246.49883073656,23.6865946235036)) ;
#111570 = CARTESIAN_POINT('Ctrl Pts',(58.2305858224232,246.525186974954,23.742002876936)) ;
#111571 = CARTESIAN_POINT('Ctrl Pts',(58.2276826827665,246.551526850066,23.7973767301316)) ;
#111572 = CARTESIAN_POINT('Ctrl Pts',(58.2247795431098,246.580924295902,23.8513423210356)) ;
#111573 = CARTESIAN_POINT('Ctrl Pts',(58.2218764034532,246.613198284203,23.9035478332288)) ;
#111574 = CARTESIAN_POINT('Ctrl Pts',(58.2189740028974,246.645464055975,23.9557400545912)) ;
#111575 = CARTESIAN_POINT('Ctrl Pts',(58.2160716023415,246.680604648608,24.0061726544247)) ;
#111576 = CARTESIAN_POINT('Ctrl Pts',(58.2131692017857,246.718394304614,24.0545205382078)) ;
#111577 = CARTESIAN_POINT('Ctrl Pts',(58.2102644853581,246.75621411359,24.1029069995403)) ;
#111578 = CARTESIAN_POINT('Ctrl Pts',(58.2073597689305,246.796686898043,24.1492050171797)) ;
#111579 = CARTESIAN_POINT('Ctrl Pts',(58.2044550525028,246.839545718577,24.1931215258754)) ;
#111580 = CARTESIAN_POINT('Ctrl Pts',(58.2015492914808,246.882419952002,24.2370538278295)) ;
#111581 = CARTESIAN_POINT('Ctrl Pts',(58.1986435304589,246.927681558917,24.2786025660187)) ;
#111582 = CARTESIAN_POINT('Ctrl Pts',(58.1957377694369,246.975027895082,24.3175127456246)) ;
#111583 = CARTESIAN_POINT('Ctrl Pts',(58.1928267896766,247.022459265128,24.3564928077992)) ;
#111584 = CARTESIAN_POINT('Ctrl Pts',(58.1899158099164,247.071982436888,24.3928245366809)) ;
#111585 = CARTESIAN_POINT('Ctrl Pts',(58.1870048301561,247.123263613894,24.426294835392)) ;
#111586 = CARTESIAN_POINT('Ctrl Pts',(58.1842724477408,247.17139853678,24.4577116308227)) ;
#111587 = CARTESIAN_POINT('Ctrl Pts',(58.1815400653256,247.221081789228,24.4866075846815)) ;
#111588 = CARTESIAN_POINT('Ctrl Pts',(58.1788076829103,247.272018954284,24.5128440309778)) ;
#111589 = CARTESIAN_POINT('Ctrl Pts',(58.515643070046,249.718014466972,23.01985397027)) ;
#111590 = CARTESIAN_POINT('Ctrl Pts',(58.5179320301945,249.718062191968,23.0744584714563)) ;
#111591 = CARTESIAN_POINT('Ctrl Pts',(58.5202465310105,249.715444140582,23.1290318143707)) ;
#111592 = CARTESIAN_POINT('Ctrl Pts',(58.5240382880717,249.707042313032,23.2156066858572)) ;
#111593 = CARTESIAN_POINT('Ctrl Pts',(58.5254717260617,249.702982624228,23.247735351128)) ;
#111594 = CARTESIAN_POINT('Ctrl Pts',(58.5278030221993,249.695024000041,23.2987918396245)) ;
#111595 = CARTESIAN_POINT('Ctrl Pts',(58.528683075632,249.691723312647,23.3178050577416)) ;
#111596 = CARTESIAN_POINT('Ctrl Pts',(58.5304557462619,249.684499348991,23.3555428350881)) ;
#111597 = CARTESIAN_POINT('Ctrl Pts',(58.5313480524487,249.680582307546,23.3742656114643)) ;
#111598 = CARTESIAN_POINT('Ctrl Pts',(58.5331578527914,249.672087840024,23.4116654128546)) ;
#111599 = CARTESIAN_POINT('Ctrl Pts',(58.5340753167885,249.667507723484,23.4303388451223)) ;
#111600 = CARTESIAN_POINT('Ctrl Pts',(58.5364088090204,249.6551834298,23.4770970861105)) ;
#111601 = CARTESIAN_POINT('Ctrl Pts',(58.5378378385315,249.647026999209,23.5050658550262)) ;
#111602 = CARTESIAN_POINT('Ctrl Pts',(58.5453499516503,249.60105925046,23.6486688460366)) ;
#111603 = CARTESIAN_POINT('Ctrl Pts',(58.5518124162021,249.551484034298,23.7601400907936)) ;
#111604 = CARTESIAN_POINT('Ctrl Pts',(58.5612304916895,249.462507892651,23.9130178303199)) ;
#111605 = CARTESIAN_POINT('Ctrl Pts',(58.5641635121313,249.432366386356,23.9593786641421)) ;
#111606 = CARTESIAN_POINT('Ctrl Pts',(58.5682276679555,249.386329564592,24.0230685030165)) ;
#111607 = CARTESIAN_POINT('Ctrl Pts',(58.5694197585455,249.372275163203,24.0416821363769)) ;
#111608 = CARTESIAN_POINT('Ctrl Pts',(58.5715205452099,249.346406410939,24.074496895347)) ;
#111609 = CARTESIAN_POINT('Ctrl Pts',(58.5724363990657,249.334737027622,24.0888073235102)) ;
#111610 = CARTESIAN_POINT('Ctrl Pts',(58.5738793039246,249.315664163357,24.111423999665)) ;
#111611 = CARTESIAN_POINT('Ctrl Pts',(58.5744160817446,249.308410384526,24.1198540498652)) ;
#111612 = CARTESIAN_POINT('Ctrl Pts',(58.5754826946989,249.293659286898,24.1366563344218)) ;
#111613 = CARTESIAN_POINT('Ctrl Pts',(58.5760123921181,249.286160623736,24.145026584935)) ;
#111614 = CARTESIAN_POINT('Ctrl Pts',(58.5774227989656,249.26575057283,24.1673534557708)) ;
#111615 = CARTESIAN_POINT('Ctrl Pts',(58.5782927381509,249.252684846015,24.1811672945508)) ;
#111616 = CARTESIAN_POINT('Ctrl Pts',(58.583750004731,249.167961298428,24.2677453579383)) ;
#111617 = CARTESIAN_POINT('Ctrl Pts',(58.5879629602787,249.09001440943,24.3340671440252)) ;
#111618 = CARTESIAN_POINT('Ctrl Pts',(58.5963099657129,248.92635643896,24.4493613893714)) ;
#111619 = CARTESIAN_POINT('Ctrl Pts',(58.6004280223336,248.841406858024,24.4986927361666)) ;
#111620 = CARTESIAN_POINT('Ctrl Pts',(58.6060840722861,248.726708687347,24.55248353038)) ;
#111621 = CARTESIAN_POINT('Ctrl Pts',(58.6073828591067,248.700469523681,24.5639789292531)) ;
#111622 = CARTESIAN_POINT('Ctrl Pts',(58.6095873956141,248.656223033881,24.5820276899201)) ;
#111623 = CARTESIAN_POINT('Ctrl Pts',(58.6104804836726,248.638374270672,24.5889545423018)) ;
#111624 = CARTESIAN_POINT('Ctrl Pts',(58.6122912009387,248.602368152751,24.6022235655979)) ;
#111625 = CARTESIAN_POINT('Ctrl Pts',(58.6132087845088,248.584212516365,24.6085619791354)) ;
#111626 = CARTESIAN_POINT('Ctrl Pts',(58.6155412829522,248.538309720398,24.6237072903177)) ;
#111627 = CARTESIAN_POINT('Ctrl Pts',(58.6169691536816,248.510435543522,24.6321064854137)) ;
#111628 = CARTESIAN_POINT('Ctrl Pts',(58.6244183518366,248.36618946995,24.6715083441976)) ;
#111629 = CARTESIAN_POINT('Ctrl Pts',(58.6308102685836,248.24695511078,24.6906373721208)) ;
#111630 = CARTESIAN_POINT('Ctrl Pts',(58.6415295244695,248.045900337825,24.7010115267353)) ;
#111631 = CARTESIAN_POINT('Ctrl Pts',(58.6458223555456,247.964879534078,24.6993289756702)) ;
#111632 = CARTESIAN_POINT('Ctrl Pts',(58.6507810093612,247.866507964071,24.6901440500868)) ;
#111633 = CARTESIAN_POINT('Ctrl Pts',(58.6516657097671,247.848750453958,24.6881995509372)) ;
#111634 = CARTESIAN_POINT('Ctrl Pts',(58.6530721019866,247.820108830985,24.684599442471)) ;
#111635 = CARTESIAN_POINT('Ctrl Pts',(58.6536027052168,247.809204271112,24.6831196860291)) ;
#111636 = CARTESIAN_POINT('Ctrl Pts',(58.6546697822737,247.78704903131,24.6798909000274)) ;
#111637 = CARTESIAN_POINT('Ctrl Pts',(58.6552058562418,247.775800125529,24.678134442542)) ;
#111638 = CARTESIAN_POINT('Ctrl Pts',(58.6566547762021,247.745111478052,24.6730220498855)) ;
#111639 = CARTESIAN_POINT('Ctrl Pts',(58.6575558051197,247.725711225189,24.6694374826725)) ;
#111640 = CARTESIAN_POINT('Ctrl Pts',(58.6626130507342,247.615465082727,24.6470497176586)) ;
#111641 = CARTESIAN_POINT('Ctrl Pts',(58.6664675055547,247.526232084007,24.6210778177386)) ;
#111642 = CARTESIAN_POINT('Ctrl Pts',(58.672888695377,247.382377997139,24.5659190495331)) ;
#111643 = CARTESIAN_POINT('Ctrl Pts',(58.6754407143328,247.326435861763,24.5408728113435)) ;
#111644 = CARTESIAN_POINT('Ctrl Pts',(58.6780583779715,247.272018809212,24.512843956255)) ;
#111645 = CARTESIAN_POINT('Ctrl Pts',(58.7781769759756,247.272019165218,24.5128441396244)) ;
#111646 = CARTESIAN_POINT('Ctrl Pts',(58.7763091666173,247.310835570535,24.5328374819825)) ;
#111647 = CARTESIAN_POINT('Ctrl Pts',(58.774407975385,247.350443695255,24.5513213682175)) ;
#111648 = CARTESIAN_POINT('Ctrl Pts',(58.7711652789816,247.417460655586,24.5794597720553)) ;
#111649 = CARTESIAN_POINT('Ctrl Pts',(58.7698528371765,247.444449249757,24.58997811835)) ;
#111650 = CARTESIAN_POINT('Ctrl Pts',(58.7676320365219,247.489758419209,24.6062985897986)) ;
#111651 = CARTESIAN_POINT('Ctrl Pts',(58.7667367847226,247.507931004924,24.6124941310397)) ;
#111652 = CARTESIAN_POINT('Ctrl Pts',(58.7649272881695,247.544447029362,24.6242478918723)) ;
#111653 = CARTESIAN_POINT('Ctrl Pts',(58.7640132172179,247.562787341133,24.6298063513237)) ;
#111654 = CARTESIAN_POINT('Ctrl Pts',(58.761701374617,247.608887281234,24.642920093752)) ;
#111655 = CARTESIAN_POINT('Ctrl Pts',(58.7602911119702,247.636752865747,24.6500776379853)) ;
#111656 = CARTESIAN_POINT('Ctrl Pts',(58.7536240153106,247.767284446877,24.6800506204373)) ;
#111657 = CARTESIAN_POINT('Ctrl Pts',(58.7480935357987,247.871755414129,24.6938944737568)) ;
#111658 = CARTESIAN_POINT('Ctrl Pts',(58.7375092745268,248.070428162307,24.7014126090336)) ;
#111659 = CARTESIAN_POINT('Ctrl Pts',(58.7324937558047,248.164171910562,24.6971093414747)) ;
#111660 = CARTESIAN_POINT('Ctrl Pts',(58.7267816618943,248.276503243161,24.6824707501298)) ;
#111661 = CARTESIAN_POINT('Ctrl Pts',(58.72580705598,248.295891470333,24.6795978692146)) ;
#111662 = CARTESIAN_POINT('Ctrl Pts',(58.7242946691828,248.326428696776,24.674524636937)) ;
#111663 = CARTESIAN_POINT('Ctrl Pts',(58.7237455939469,248.337612874061,24.6725496900193)) ;
#111664 = CARTESIAN_POINT('Ctrl Pts',(58.7226764739928,248.359608509145,24.6684348796372)) ;
#111665 = CARTESIAN_POINT('Ctrl Pts',(58.7221561392753,248.370420520988,24.6663017760783)) ;
#111666 = CARTESIAN_POINT('Ctrl Pts',(58.7208027443307,248.398789837314,24.6604138158854)) ;
#111667 = CARTESIAN_POINT('Ctrl Pts',(58.719978959852,248.416309692928,24.6564833040354)) ;
#111668 = CARTESIAN_POINT('Ctrl Pts',(58.7154002734769,248.514779735428,24.6327255086645)) ;
#111669 = CARTESIAN_POINT('Ctrl Pts',(58.7118988982531,248.5942339226,24.6071676261343)) ;
#111670 = CARTESIAN_POINT('Ctrl Pts',(58.7035334161776,248.779933585828,24.5317643156487)) ;
#111671 = CARTESIAN_POINT('Ctrl Pts',(58.6986944345953,248.883493050375,24.4764888669701)) ;
#111672 = CARTESIAN_POINT('Ctrl Pts',(58.6921642461824,249.004867232207,24.3943669735868)) ;
#111673 = CARTESIAN_POINT('Ctrl Pts',(58.6908294958231,249.028845313321,24.3772050602596)) ;
#111674 = CARTESIAN_POINT('Ctrl Pts',(58.6885817424774,249.067746451667,24.3477815857167)) ;
#111675 = CARTESIAN_POINT('Ctrl Pts',(58.687682575334,249.082932548257,24.3358780299583)) ;
#111676 = CARTESIAN_POINT('Ctrl Pts',(58.6858736959232,249.112717399393,24.3116904520405)) ;
#111677 = CARTESIAN_POINT('Ctrl Pts',(58.6849643536074,249.127318621607,24.299414063143)) ;
#111678 = CARTESIAN_POINT('Ctrl Pts',(58.6826817887202,249.163037362025,24.268327615606)) ;
#111679 = CARTESIAN_POINT('Ctrl Pts',(58.681296740239,249.183894114938,24.249228013608)) ;
#111680 = CARTESIAN_POINT('Ctrl Pts',(58.674558673086,249.281479774344,24.155220042489)) ;
#111681 = CARTESIAN_POINT('Ctrl Pts',(58.6689178165271,249.351383794338,24.0736059583046)) ;
#111682 = CARTESIAN_POINT('Ctrl Pts',(58.6582977029097,249.466061233093,23.9104003964724)) ;
#111683 = CARTESIAN_POINT('Ctrl Pts',(58.6533605397259,249.512791377416,23.8306571743344)) ;
#111684 = CARTESIAN_POINT('Ctrl Pts',(58.6477053890401,249.561305607179,23.7296094913164)) ;
#111685 = CARTESIAN_POINT('Ctrl Pts',(58.6467194803946,249.569565230345,23.7115948643374)) ;
#111686 = CARTESIAN_POINT('Ctrl Pts',(58.6451937806029,249.582071479195,23.6829910801999)) ;
#111687 = CARTESIAN_POINT('Ctrl Pts',(58.6446423824,249.586532403169,23.6724981345098)) ;
#111688 = CARTESIAN_POINT('Ctrl Pts',(58.6435725463192,249.595080412569,23.6518083168824)) ;
#111689 = CARTESIAN_POINT('Ctrl Pts',(58.6430537413628,249.599174943509,23.6416153111299)) ;
#111690 = CARTESIAN_POINT('Ctrl Pts',(58.6417098750084,249.609632840876,23.6148234755993)) ;
#111691 = CARTESIAN_POINT('Ctrl Pts',(58.6408938454047,249.615833190677,23.5981620107676)) ;
#111692 = CARTESIAN_POINT('Ctrl Pts',(58.6361593568661,249.65077928568,23.499485173232)) ;
#111693 = CARTESIAN_POINT('Ctrl Pts',(58.6325187981103,249.673384600467,23.4154279840847)) ;
#111694 = CARTESIAN_POINT('Ctrl Pts',(58.624176308611,249.710180687893,23.2188409489268)) ;
#111695 = CARTESIAN_POINT('Ctrl Pts',(58.6194905188775,249.719694018365,23.1058737582084)) ;
#111696 = CARTESIAN_POINT('Ctrl Pts',(58.613126656964,249.717265645328,22.9629602650058)) ;
#111697 = CARTESIAN_POINT('Ctrl Pts',(58.6117757601395,249.715961390043,22.9331242656587)) ;
#111698 = CARTESIAN_POINT('Ctrl Pts',(58.6095084885204,249.712500076772,22.8840242382705)) ;
#111699 = CARTESIAN_POINT('Ctrl Pts',(58.6086064872593,249.710804158887,22.864734093427)) ;
#111700 = CARTESIAN_POINT('Ctrl Pts',(58.6067978621239,249.706781787383,22.8265671273519)) ;
#111701 = CARTESIAN_POINT('Ctrl Pts',(58.6058917460839,249.704467476912,22.807691935192)) ;
#111702 = CARTESIAN_POINT('Ctrl Pts',(58.6036291117501,249.697961078725,22.7611857229054)) ;
#111703 = CARTESIAN_POINT('Ctrl Pts',(58.6022612126478,249.693398594909,22.7336130070024)) ;
#111704 = CARTESIAN_POINT('Ctrl Pts',(58.5955505633836,249.668030433951,22.6009666465405)) ;
#111705 = CARTESIAN_POINT('Ctrl Pts',(58.5899194324147,249.637885583593,22.4979458718017)) ;
#111706 = CARTESIAN_POINT('Ctrl Pts',(58.5792439998436,249.563448488295,22.3117512918139)) ;
#111707 = CARTESIAN_POINT('Ctrl Pts',(58.5742415628301,249.521573424786,22.2280339232889)) ;
#111708 = CARTESIAN_POINT('Ctrl Pts',(58.568539314449,249.462729399463,22.1314744743989)) ;
#111709 = CARTESIAN_POINT('Ctrl Pts',(58.5675631160725,249.452221275872,22.1148931975161)) ;
#111710 = CARTESIAN_POINT('Ctrl Pts',(58.5660488664004,249.435174366666,22.0890101317272)) ;
#111711 = CARTESIAN_POINT('Ctrl Pts',(58.565499476295,249.42882812751,22.0795842206011)) ;
#111712 = CARTESIAN_POINT('Ctrl Pts',(58.5644302806529,249.416142369524,22.0611494494127)) ;
#111713 = CARTESIAN_POINT('Ctrl Pts',(58.5639101741161,249.409808993762,22.0521372149261)) ;
#111714 = CARTESIAN_POINT('Ctrl Pts',(58.5625581970151,249.392935666634,22.0286226032031)) ;
#111715 = CARTESIAN_POINT('Ctrl Pts',(58.561735565789,249.382250961371,22.0142252846363)) ;
#111716 = CARTESIAN_POINT('Ctrl Pts',(58.5571890944492,249.321027141696,21.9344330456867)) ;
#111717 = CARTESIAN_POINT('Ctrl Pts',(58.5537145890524,249.26593654388,21.8726658335845)) ;
#111718 = CARTESIAN_POINT('Ctrl Pts',(58.5453362716452,249.121656529711,21.7331545956064)) ;
#111719 = CARTESIAN_POINT('Ctrl Pts',(58.540460143388,249.028378067632,21.6602878179039)) ;
#111720 = CARTESIAN_POINT('Ctrl Pts',(58.5338897740087,248.903303594657,21.582267572326)) ;
#111721 = CARTESIAN_POINT('Ctrl Pts',(58.5325593846841,248.877971752257,21.5673754449325)) ;
#111722 = CARTESIAN_POINT('Ctrl Pts',(58.5303168920002,248.835394780419,21.5438273895886)) ;
#111723 = CARTESIAN_POINT('Ctrl Pts',(58.5294184804517,248.818367709945,21.5347898429423)) ;
#111724 = CARTESIAN_POINT('Ctrl Pts',(58.5276094787576,248.784173224159,21.5173887300536)) ;
#111725 = CARTESIAN_POINT('Ctrl Pts',(58.5266992206044,248.767011231781,21.5090208962999)) ;
#111726 = CARTESIAN_POINT('Ctrl Pts',(58.524411039067,248.724000826396,21.4889511171973)) ;
#111727 = CARTESIAN_POINT('Ctrl Pts',(58.5230211639088,248.697991953697,21.4776088243472)) ;
#111728 = CARTESIAN_POINT('Ctrl Pts',(58.5167073842392,248.580383650691,21.4298324576466)) ;
#111729 = CARTESIAN_POINT('Ctrl Pts',(58.5115460560139,248.485976780048,21.4008578236516)) ;
#111730 = CARTESIAN_POINT('Ctrl Pts',(58.5008720152831,248.289637497897,21.359062711305)) ;
#111731 = CARTESIAN_POINT('Ctrl Pts',(58.4953776921804,248.187952045253,21.3469615037871)) ;
#111732 = CARTESIAN_POINT('Ctrl Pts',(58.4892756047735,248.066795757564,21.3436724668466)) ;
#111733 = CARTESIAN_POINT('Ctrl Pts',(58.4883316948739,248.047789072863,21.3434795530609)) ;
#111734 = CARTESIAN_POINT('Ctrl Pts',(58.4868555039266,248.017547584194,21.343686531784)) ;
#111735 = CARTESIAN_POINT('Ctrl Pts',(58.4863127629332,248.006313406644,21.343876279719)) ;
#111736 = CARTESIAN_POINT('Ctrl Pts',(58.4852451213693,247.983957828478,21.3444785552276)) ;
#111737 = CARTESIAN_POINT('Ctrl Pts',(58.4847201473515,247.972836973909,21.3448889103273)) ;
#111738 = CARTESIAN_POINT('Ctrl Pts',(58.4833383540921,247.943259950205,21.3462750865881)) ;
#111739 = CARTESIAN_POINT('Ctrl Pts',(58.482491545943,247.924814012191,21.3474452866173)) ;
#111740 = CARTESIAN_POINT('Ctrl Pts',(58.4783241605687,247.832757650797,21.3548143390947)) ;
#111741 = CARTESIAN_POINT('Ctrl Pts',(58.4751973989511,247.759588383597,21.3655655741958)) ;
#111742 = CARTESIAN_POINT('Ctrl Pts',(58.4667268005291,247.561682982708,21.408146299191)) ;
#111743 = CARTESIAN_POINT('Ctrl Pts',(58.4614501685449,247.439537945236,21.4495389279885)) ;
#111744 = CARTESIAN_POINT('Ctrl Pts',(58.4544488059768,247.297959053896,21.5164570714694)) ;
#111745 = CARTESIAN_POINT('Ctrl Pts',(58.4531755358376,247.272906528287,21.5290762441629)) ;
#111746 = CARTESIAN_POINT('Ctrl Pts',(58.4510894463472,247.233076424013,21.5504073115548)) ;
#111747 = CARTESIAN_POINT('Ctrl Pts',(58.4502903316322,247.218095189481,21.5587283571787)) ;
#111748 = CARTESIAN_POINT('Ctrl Pts',(58.4485889186806,247.186797123065,21.5767451072029)) ;
#111749 = CARTESIAN_POINT('Ctrl Pts',(58.447684884219,247.170512153954,21.5864910932166)) ;
#111750 = CARTESIAN_POINT('Ctrl Pts',(58.4454358629747,247.130860041733,21.6111446128651)) ;
#111751 = CARTESIAN_POINT('Ctrl Pts',(58.4440798047152,247.107690837377,21.626358593766)) ;
#111752 = CARTESIAN_POINT('Ctrl Pts',(58.437197109501,246.99376686969,21.7052734168937)) ;
#111753 = CARTESIAN_POINT('Ctrl Pts',(58.4313577839772,246.909117391874,21.7772796676543)) ;
#111754 = CARTESIAN_POINT('Ctrl Pts',(58.4206935283578,246.770156731069,21.9214734008873)) ;
#111755 = CARTESIAN_POINT('Ctrl Pts',(58.4159159000148,246.71335763094,21.9907104003349)) ;
#111756 = CARTESIAN_POINT('Ctrl Pts',(58.4103889491236,246.650897267652,22.0806266151527)) ;
#111757 = CARTESIAN_POINT('Ctrl Pts',(58.4093900699783,246.639745807282,22.0973109073648)) ;
#111758 = CARTESIAN_POINT('Ctrl Pts',(58.4078491050382,246.622703866114,22.1238258622081)) ;
#111759 = CARTESIAN_POINT('Ctrl Pts',(58.4072950496932,246.616610453297,22.1335232629072)) ;
#111760 = CARTESIAN_POINT('Ctrl Pts',(58.4062244929914,246.604890547417,22.1526059781332)) ;
#111761 = CARTESIAN_POINT('Ctrl Pts',(58.4057075349024,246.599255729897,22.1619852778634)) ;
#111762 = CARTESIAN_POINT('Ctrl Pts',(58.404374683682,246.584811067766,22.1865704374236)) ;
#111763 = CARTESIAN_POINT('Ctrl Pts',(58.403567550519,246.576147427895,22.201861174364)) ;
#111764 = CARTESIAN_POINT('Ctrl Pts',(58.4017846317166,246.557267414991,22.2364387520759)) ;
#111765 = CARTESIAN_POINT('Ctrl Pts',(58.4008154108517,246.547183818055,22.2557946456414)) ;
#111766 = CARTESIAN_POINT('Ctrl Pts',(58.397703865375,246.51558548612,22.3194499960749)) ;
#111767 = CARTESIAN_POINT('Ctrl Pts',(58.3956187279498,246.495642111868,22.3645021501016)) ;
#111768 = CARTESIAN_POINT('Ctrl Pts',(58.3878816574461,246.428423412721,22.5364189890206)) ;
#111769 = CARTESIAN_POINT('Ctrl Pts',(58.3823497885551,246.394574102488,22.6679607977833)) ;
#111770 = CARTESIAN_POINT('Ctrl Pts',(58.3750713163291,246.373355750385,22.8289883848575)) ;
#111771 = CARTESIAN_POINT('Ctrl Pts',(58.3738396310956,246.370468698972,22.8559170571086)) ;
#111772 = CARTESIAN_POINT('Ctrl Pts',(58.3717243950754,246.366694048073,22.9015134445233)) ;
#111773 = CARTESIAN_POINT('Ctrl Pts',(58.370851616067,246.365464260998,22.9201478419344)) ;
#111774 = CARTESIAN_POINT('Ctrl Pts',(58.3690466900847,246.363585878384,22.9582909590887)) ;
#111775 = CARTESIAN_POINT('Ctrl Pts',(58.3681137805869,246.362966170763,22.977798187214)) ;
#111776 = CARTESIAN_POINT('Ctrl Pts',(58.3656858914236,246.36224753231,23.0280114505093)) ;
#111777 = CARTESIAN_POINT('Ctrl Pts',(58.3641756709277,246.362650989571,23.0587165050758)) ;
#111778 = CARTESIAN_POINT('Ctrl Pts',(58.3607717902728,246.365413982445,23.1267593839296)) ;
#111779 = CARTESIAN_POINT('Ctrl Pts',(58.3588671967442,246.368180251952,23.1640637223062)) ;
#111780 = CARTESIAN_POINT('Ctrl Pts',(58.3522136656842,246.381983242826,23.292032202533)) ;
#111781 = CARTESIAN_POINT('Ctrl Pts',(58.3473243659794,246.399171449346,23.3818663382931)) ;
#111782 = CARTESIAN_POINT('Ctrl Pts',(58.3386915740641,246.442600760751,23.5384037208412)) ;
#111783 = CARTESIAN_POINT('Ctrl Pts',(58.3349455946988,246.465963221582,23.6056846059942)) ;
#111784 = CARTESIAN_POINT('Ctrl Pts',(58.3305352836636,246.50009545241,23.6869101854176)) ;
#111785 = CARTESIAN_POINT('Ctrl Pts',(58.3296976069603,246.5068990544,23.7024378013214)) ;
#111786 = CARTESIAN_POINT('Ctrl Pts',(58.3283984476285,246.517987934605,23.7267368703102)) ;
#111787 = CARTESIAN_POINT('Ctrl Pts',(58.3279282180068,246.522116296513,23.7355783262644)) ;
#111788 = CARTESIAN_POINT('Ctrl Pts',(58.3269255457853,246.531176009976,23.7545474762277)) ;
#111789 = CARTESIAN_POINT('Ctrl Pts',(58.3263946983799,246.536132699469,23.7646625557054)) ;
#111790 = CARTESIAN_POINT('Ctrl Pts',(58.3249775885554,246.549783758182,23.7918244381563)) ;
#111791 = CARTESIAN_POINT('Ctrl Pts',(58.3241022699391,246.558668692689,23.8087740431688)) ;
#111792 = CARTESIAN_POINT('Ctrl Pts',(58.3221384058258,246.579572301457,23.8470445146311)) ;
#111793 = CARTESIAN_POINT('Ctrl Pts',(58.3210586706229,246.591771508122,23.8682620509178)) ;
#111794 = CARTESIAN_POINT('Ctrl Pts',(58.3173760155993,246.635589618798,23.9407549596521)) ;
#111795 = CARTESIAN_POINT('Ctrl Pts',(58.3148545498496,246.669503147108,23.9905909396671)) ;
#111796 = CARTESIAN_POINT('Ctrl Pts',(58.3076432850708,246.7743178802,24.1280774838715)) ;
#111797 = CARTESIAN_POINT('Ctrl Pts',(58.3029740208238,246.85145768565,24.2105507553264)) ;
#111798 = CARTESIAN_POINT('Ctrl Pts',(58.2966279008363,246.958792838534,24.3043469209137)) ;
#111799 = CARTESIAN_POINT('Ctrl Pts',(58.2952749658863,246.981833823012,24.3234196328338)) ;
#111800 = CARTESIAN_POINT('Ctrl Pts',(58.2930048943598,247.020624717965,24.353819533697)) ;
#111801 = CARTESIAN_POINT('Ctrl Pts',(58.2921021837853,247.036083521804,24.3655078012965)) ;
#111802 = CARTESIAN_POINT('Ctrl Pts',(58.2902925822343,247.067110057282,24.3881327388936)) ;
#111803 = CARTESIAN_POINT('Ctrl Pts',(58.289386209874,247.082668229832,24.3990776006084)) ;
#111804 = CARTESIAN_POINT('Ctrl Pts',(58.2871237393485,247.121527625192,24.4254381932065)) ;
#111805 = CARTESIAN_POINT('Ctrl Pts',(58.2857562855252,247.145033661721,24.440540566286)) ;
#111806 = CARTESIAN_POINT('Ctrl Pts',(58.2824087606323,247.20260611765,24.4755307017307)) ;
#111807 = CARTESIAN_POINT('Ctrl Pts',(58.2804101508806,247.236999629262,24.4948064669926)) ;
#111808 = CARTESIAN_POINT('Ctrl Pts',(58.2783798877068,247.272019130299,24.5128441216388)) ;
#111809 = CARTESIAN_POINT('Origin',(59.9402651077866,248.040265107786,23.0213203435596)) ;
#111810 = CARTESIAN_POINT('',(67.9402651077866,250.003765107786,23.0213203435596)) ;
#111811 = CARTESIAN_POINT('Origin',(67.9402651077866,248.040265107786,23.0213203435596)) ;
#111812 = CARTESIAN_POINT('',(64.9402651077866,248.926035539849,24.773673901402)) ;
#111813 = CARTESIAN_POINT('',(64.9402651077866,247.188367839728,24.7903888257486)) ;
#111814 = CARTESIAN_POINT('Origin',(64.9402651077866,248.040265107786,23.0213203435596)) ;
#111815 = CARTESIAN_POINT('',(65.2795522049911,250.003149224854,23.0202913881658)) ;
#111816 = CARTESIAN_POINT('Ctrl Pts',(64.9402651077866,247.188367839728,24.7903888257487)) ;
#111817 = CARTESIAN_POINT('Ctrl Pts',(64.966038653494,246.615402068142,24.5144764004132)) ;
#111818 = CARTESIAN_POINT('Ctrl Pts',(65.0175857449088,245.767082084754,23.3666879407905)) ;
#111819 = CARTESIAN_POINT('Ctrl Pts',(65.094906382031,246.471954521124,21.3360833564102)) ;
#111820 = CARTESIAN_POINT('Ctrl Pts',(65.1722270191531,248.547505040093,20.777031256302)) ;
#111821 = CARTESIAN_POINT('Ctrl Pts',(65.2337755287617,249.846624333595,21.8890188139763)) ;
#111822 = CARTESIAN_POINT('Ctrl Pts',(65.2695504926629,250.002831124184,22.772803931472)) ;
#111823 = CARTESIAN_POINT('Ctrl Pts',(65.2795519108567,250.001664111351,23.0202848861717)) ;
#111824 = CARTESIAN_POINT('',(65.7795523268879,250.003764688188,23.0226039947667)) ;
#111825 = CARTESIAN_POINT('Ctrl Pts',(65.2795523269168,250.003764839589,23.0202940833964)) ;
#111826 = CARTESIAN_POINT('Ctrl Pts',(65.2823744169042,250.003801377307,23.0902001376797)) ;
#111827 = CARTESIAN_POINT('Ctrl Pts',(65.2851965068916,250.00010029984,23.1601117387701)) ;
#111828 = CARTESIAN_POINT('Ctrl Pts',(65.288018596879,249.992686234058,23.2296085949989)) ;
#111829 = CARTESIAN_POINT('Ctrl Pts',(65.2908413713362,249.985270370068,23.2991223069976)) ;
#111830 = CARTESIAN_POINT('Ctrl Pts',(65.2936641457934,249.974139780495,23.3682206035034)) ;
#111831 = CARTESIAN_POINT('Ctrl Pts',(65.2964869202507,249.959370802772,23.4364896842759)) ;
#111832 = CARTESIAN_POINT('Ctrl Pts',(65.2993133109198,249.944582904746,23.5048462234925)) ;
#111833 = CARTESIAN_POINT('Ctrl Pts',(65.3021397015889,249.926147414425,23.5723709624915)) ;
#111834 = CARTESIAN_POINT('Ctrl Pts',(65.304966092258,249.90419138201,23.6386623024912)) ;
#111835 = CARTESIAN_POINT('Ctrl Pts',(65.3077944426461,249.882220126061,23.7049996065549)) ;
#111836 = CARTESIAN_POINT('Ctrl Pts',(65.3106227930343,249.856723639135,23.7701013671339)) ;
#111837 = CARTESIAN_POINT('Ctrl Pts',(65.3134511434225,249.827877287848,23.8335856596324)) ;
#111838 = CARTESIAN_POINT('Ctrl Pts',(65.3162847933004,249.798976887053,23.8971889028677)) ;
#111839 = CARTESIAN_POINT('Ctrl Pts',(65.3191184431784,249.766714305099,23.9591682047407)) ;
#111840 = CARTESIAN_POINT('Ctrl Pts',(65.3219520930564,249.731310792157,24.0191663954992)) ;
#111841 = CARTESIAN_POINT('Ctrl Pts',(65.3235908265034,249.710836519294,24.0538640632389)) ;
#111842 = CARTESIAN_POINT('Ctrl Pts',(65.3252295599505,249.689312593963,24.0878996918042)) ;
#111843 = CARTESIAN_POINT('Ctrl Pts',(65.3268682933975,249.666788097151,24.1212090720539)) ;
#111844 = CARTESIAN_POINT('Ctrl Pts',(65.3296726910431,249.628241470824,24.17821208723)) ;
#111845 = CARTESIAN_POINT('Ctrl Pts',(65.3324770886888,249.586624367975,24.2332903131143)) ;
#111846 = CARTESIAN_POINT('Ctrl Pts',(65.3352814863345,249.542155517383,24.2860959946378)) ;
#111847 = CARTESIAN_POINT('Ctrl Pts',(65.3381526298422,249.496628289149,24.3401584739413)) ;
#111848 = CARTESIAN_POINT('Ctrl Pts',(65.3410237733499,249.448112038248,24.3918383687241)) ;
#111849 = CARTESIAN_POINT('Ctrl Pts',(65.3438949168576,249.396889058754,24.4407933815775)) ;
#111850 = CARTESIAN_POINT('Ctrl Pts',(65.346692200189,249.346983790579,24.4884890265612)) ;
#111851 = CARTESIAN_POINT('Ctrl Pts',(65.3494894835203,249.294509759058,24.5335979427487)) ;
#111852 = CARTESIAN_POINT('Ctrl Pts',(65.3522867668517,249.239767702999,24.5758382026002)) ;
#111853 = CARTESIAN_POINT('Ctrl Pts',(65.3550824698301,249.185056574007,24.6180545983987)) ;
#111854 = CARTESIAN_POINT('Ctrl Pts',(65.3578781728086,249.128080348433,24.6574052568979)) ;
#111855 = CARTESIAN_POINT('Ctrl Pts',(65.360673875787,249.069173262012,24.6936481404244)) ;
#111856 = CARTESIAN_POINT('Ctrl Pts',(65.3634689366283,249.010279705794,24.729882699425)) ;
#111857 = CARTESIAN_POINT('Ctrl Pts',(65.3662639974696,248.949456584652,24.7630106461511)) ;
#111858 = CARTESIAN_POINT('Ctrl Pts',(65.3690590583109,248.887066087755,24.7928339196646)) ;
#111859 = CARTESIAN_POINT('Ctrl Pts',(65.3719865476616,248.821719562,24.8240702041577)) ;
#111860 = CARTESIAN_POINT('Ctrl Pts',(65.3749140370124,248.754653949304,24.8516805938501)) ;
#111861 = CARTESIAN_POINT('Ctrl Pts',(65.3778415263631,248.686310907772,24.8754932250139)) ;
#111862 = CARTESIAN_POINT('Ctrl Pts',(65.3806398236742,248.620983889827,24.898254989028)) ;
#111863 = CARTESIAN_POINT('Ctrl Pts',(65.3834381209853,248.554490323935,24.9175470485588)) ;
#111864 = CARTESIAN_POINT('Ctrl Pts',(65.3862364182963,248.487231047264,24.933270577992)) ;
#111865 = CARTESIAN_POINT('Ctrl Pts',(65.3890365162122,248.419928491641,24.9490042249572)) ;
#111866 = CARTESIAN_POINT('Ctrl Pts',(65.3918366141281,248.351859724051,24.9611646863053)) ;
#111867 = CARTESIAN_POINT('Ctrl Pts',(65.3946367120439,248.283433860123,24.9697045992665)) ;
#111868 = CARTESIAN_POINT('Ctrl Pts',(65.3974411055399,248.214903025304,24.9782576131553)) ;
#111869 = CARTESIAN_POINT('Ctrl Pts',(65.4002454990358,248.146014486428,24.9831789665619)) ;
#111870 = CARTESIAN_POINT('Ctrl Pts',(65.4030498925317,248.077179448845,24.9844733130004)) ;
#111871 = CARTESIAN_POINT('Ctrl Pts',(65.403429571861,248.067860057347,24.9846485511003)) ;
#111872 = CARTESIAN_POINT('Ctrl Pts',(65.4038092511904,248.058541640326,24.9847573850822)) ;
#111873 = CARTESIAN_POINT('Ctrl Pts',(65.4041889305197,248.049225210902,24.9847998994889)) ;
#111874 = CARTESIAN_POINT('Ctrl Pts',(65.4069935126991,247.980407421991,24.9851139412027)) ;
#111875 = CARTESIAN_POINT('Ctrl Pts',(65.4097980948786,247.911447888344,24.9818062564764)) ;
#111876 = CARTESIAN_POINT('Ctrl Pts',(65.412602677058,247.842757201115,24.9748614556948)) ;
#111877 = CARTESIAN_POINT('Ctrl Pts',(65.415473797499,247.772436838369,24.9677518906306)) ;
#111878 = CARTESIAN_POINT('Ctrl Pts',(65.41834491794,247.702398755633,24.9568303285523)) ;
#111879 = CARTESIAN_POINT('Ctrl Pts',(65.421216038381,247.63308477106,24.942136946826)) ;
#111880 = CARTESIAN_POINT('Ctrl Pts',(65.4240135270963,247.565548388091,24.9278203863007)) ;
#111881 = CARTESIAN_POINT('Ctrl Pts',(65.4268110158116,247.498699915975,24.9099232606698)) ;
#111882 = CARTESIAN_POINT('Ctrl Pts',(65.4296085045269,247.432941807806,24.8885350230492)) ;
#111883 = CARTESIAN_POINT('Ctrl Pts',(65.4324044200699,247.367220678815,24.8671588131385)) ;
#111884 = CARTESIAN_POINT('Ctrl Pts',(65.4352003356129,247.302589159481,24.8422955377268)) ;
#111885 = CARTESIAN_POINT('Ctrl Pts',(65.437996251156,247.239435639966,24.8140848047957)) ;
#111886 = CARTESIAN_POINT('Ctrl Pts',(65.4407915314058,247.176296470313,24.7858804819607)) ;
#111887 = CARTESIAN_POINT('Ctrl Pts',(65.4435868116556,247.114635078082,24.7543304112435)) ;
#111888 = CARTESIAN_POINT('Ctrl Pts',(65.4463820919054,247.054819290828,24.7196220811314)) ;
#111889 = CARTESIAN_POINT('Ctrl Pts',(65.4493093815501,246.992178654122,24.6832746217562)) ;
#111890 = CARTESIAN_POINT('Ctrl Pts',(65.4522366711948,246.931562785623,24.6434634606412)) ;
#111891 = CARTESIAN_POINT('Ctrl Pts',(65.4551639608395,246.873362514501,24.6004563692978)) ;
#111892 = CARTESIAN_POINT('Ctrl Pts',(65.4579624923183,246.817722208763,24.559340964419)) ;
#111893 = CARTESIAN_POINT('Ctrl Pts',(65.4607610237972,246.764289811874,24.5153052505619)) ;
#111894 = CARTESIAN_POINT('Ctrl Pts',(65.4635595552761,246.71337298715,24.4686245790936)) ;
#111895 = CARTESIAN_POINT('Ctrl Pts',(65.4663598922761,246.662423312553,24.4219137907796)) ;
#111896 = CARTESIAN_POINT('Ctrl Pts',(65.4691602292762,246.613992781093,24.3725549962916)) ;
#111897 = CARTESIAN_POINT('Ctrl Pts',(65.4719605662762,246.568351221111,24.3208594003846)) ;
#111898 = CARTESIAN_POINT('Ctrl Pts',(65.4747652041905,246.522639562269,24.2690844074901)) ;
#111899 = CARTESIAN_POINT('Ctrl Pts',(65.4775698421047,246.479725719894,24.2149658360299)) ;
#111900 = CARTESIAN_POINT('Ctrl Pts',(65.480374480019,246.439837741792,24.1588459459873)) ;
#111901 = CARTESIAN_POINT('Ctrl Pts',(65.4807528425599,246.434456613387,24.1512750349309)) ;
#111902 = CARTESIAN_POINT('Ctrl Pts',(65.4811312051008,246.429130487227,24.1436677391668)) ;
#111903 = CARTESIAN_POINT('Ctrl Pts',(65.4815095676418,246.423859859516,24.1360249337381)) ;
#111904 = CARTESIAN_POINT('Ctrl Pts',(65.4843136713075,246.384798417421,24.0793829134542)) ;
#111905 = CARTESIAN_POINT('Ctrl Pts',(65.4871177749731,246.34864643985,24.0205817797099)) ;
#111906 = CARTESIAN_POINT('Ctrl Pts',(65.4899218786388,246.315648228617,23.959951724925)) ;
#111907 = CARTESIAN_POINT('Ctrl Pts',(65.492793058894,246.281860671577,23.8978713466918)) ;
#111908 = CARTESIAN_POINT('Ctrl Pts',(65.4956642391493,246.251380075197,23.8338737921426)) ;
#111909 = CARTESIAN_POINT('Ctrl Pts',(65.4985354194045,246.22442260256,23.7683466123185)) ;
#111910 = CARTESIAN_POINT('Ctrl Pts',(65.501332407077,246.198161723081,23.7045126841452)) ;
#111911 = CARTESIAN_POINT('Ctrl Pts',(65.5041293947495,246.175244283028,23.6392277106462)) ;
#111912 = CARTESIAN_POINT('Ctrl Pts',(65.5069263824221,246.155823425945,23.5728743279883)) ;
#111913 = CARTESIAN_POINT('Ctrl Pts',(65.5097217900188,246.136413540102,23.5065584297199)) ;
#111914 = CARTESIAN_POINT('Ctrl Pts',(65.5125171976155,246.120496453996,23.4391757870567)) ;
#111915 = CARTESIAN_POINT('Ctrl Pts',(65.5153126052122,246.10817596721,23.3711257221154)) ;
#111916 = CARTESIAN_POINT('Ctrl Pts',(65.5181073714904,246.095858306972,23.3030912691264)) ;
#111917 = CARTESIAN_POINT('Ctrl Pts',(65.5209021377685,246.087135693778,23.2343901775297)) ;
#111918 = CARTESIAN_POINT('Ctrl Pts',(65.5236969040467,246.082060793314,23.1654318031459)) ;
#111919 = CARTESIAN_POINT('Ctrl Pts',(65.5266246791064,246.076744367707,23.0931915552718)) ;
#111920 = CARTESIAN_POINT('Ctrl Pts',(65.5295524541662,246.075431614551,23.020669499252)) ;
#111921 = CARTESIAN_POINT('Ctrl Pts',(65.532480229226,246.078121870574,22.9483397525469)) ;
#111922 = CARTESIAN_POINT('Ctrl Pts',(65.5352782376675,246.080692887442,22.8792158486533)) ;
#111923 = CARTESIAN_POINT('Ctrl Pts',(65.538076246109,246.086919464182,22.8102680703954)) ;
#111924 = CARTESIAN_POINT('Ctrl Pts',(65.5408742545506,246.096747759992,22.74190565385)) ;
#111925 = CARTESIAN_POINT('Ctrl Pts',(65.5436740658715,246.106582388604,22.6734991884048)) ;
#111926 = CARTESIAN_POINT('Ctrl Pts',(65.5464738771925,246.120023260211,22.6056793131083)) ;
#111927 = CARTESIAN_POINT('Ctrl Pts',(65.5492736885134,246.136965588452,22.5388442408341)) ;
#111928 = CARTESIAN_POINT('Ctrl Pts',(65.5520778006902,246.1539339422,22.4719065016373)) ;
#111929 = CARTESIAN_POINT('Ctrl Pts',(65.554881912867,246.174414335663,22.4059570469023)) ;
#111930 = CARTESIAN_POINT('Ctrl Pts',(65.5576860250438,246.198252774597,22.3413771000614)) ;
#111931 = CARTESIAN_POINT('Ctrl Pts',(65.5580674182839,246.201495091198,22.332593444624)) ;
#111932 = CARTESIAN_POINT('Ctrl Pts',(65.5584488115239,246.20479945831,22.3238350896746)) ;
#111933 = CARTESIAN_POINT('Ctrl Pts',(65.558830204764,246.208165422206,22.3151029605269)) ;
#111934 = CARTESIAN_POINT('Ctrl Pts',(65.5616345176778,246.232914723003,22.2508972537607)) ;
#111935 = CARTESIAN_POINT('Ctrl Pts',(65.5644388305917,246.261088319541,22.1878769827904)) ;
#111936 = CARTESIAN_POINT('Ctrl Pts',(65.5672431435055,246.292551236391,22.126430141505)) ;
#111937 = CARTESIAN_POINT('Ctrl Pts',(65.5701142976047,246.324764076207,22.0635187062759)) ;
#111938 = CARTESIAN_POINT('Ctrl Pts',(65.5729854517039,246.36042495406,22.002257183029)) ;
#111939 = CARTESIAN_POINT('Ctrl Pts',(65.5758566058031,246.39933570864,21.9430425699689)) ;
#111940 = CARTESIAN_POINT('Ctrl Pts',(65.578653809421,246.437244263782,21.8853531098551)) ;
#111941 = CARTESIAN_POINT('Ctrl Pts',(65.5814510130389,246.478237012326,21.8296068198098)) ;
#111942 = CARTESIAN_POINT('Ctrl Pts',(65.5842482166568,246.522084271727,21.7761459786521)) ;
#111943 = CARTESIAN_POINT('Ctrl Pts',(65.5870438420561,246.565906791934,21.7227153007958)) ;
#111944 = CARTESIAN_POINT('Ctrl Pts',(65.5898394674554,246.612580318353,21.6715678890376)) ;
#111945 = CARTESIAN_POINT('Ctrl Pts',(65.5926350928547,246.661833564721,21.6230146791631)) ;
#111946 = CARTESIAN_POINT('Ctrl Pts',(65.595430078416,246.711075538442,21.5744725817173)) ;
#111947 = CARTESIAN_POINT('Ctrl Pts',(65.5982250639774,246.762895712278,21.5285238487395)) ;
#111948 = CARTESIAN_POINT('Ctrl Pts',(65.6010200495387,246.816985680048,21.4854428446451)) ;
#111949 = CARTESIAN_POINT('Ctrl Pts',(65.6039476155676,246.873641411777,21.4403182880727)) ;
#111950 = CARTESIAN_POINT('Ctrl Pts',(65.6068751815966,246.932787206431,21.3983406889682)) ;
#111951 = CARTESIAN_POINT('Ctrl Pts',(65.6098027476256,246.994031275681,21.3597767785098)) ;
#111952 = CARTESIAN_POINT('Ctrl Pts',(65.6126009764781,247.052569638242,21.3229165861707)) ;
#111953 = CARTESIAN_POINT('Ctrl Pts',(65.6153992053307,247.113024308223,21.2891750086416)) ;
#111954 = CARTESIAN_POINT('Ctrl Pts',(65.6181974341833,247.175026921842,21.2587383932423)) ;
#111955 = CARTESIAN_POINT('Ctrl Pts',(65.620997466096,247.237069487318,21.2282821657777)) ;
#111956 = CARTESIAN_POINT('Ctrl Pts',(65.6237974980087,247.300661533568,21.2011353298438)) ;
#111957 = CARTESIAN_POINT('Ctrl Pts',(65.6265975299214,247.365415068727,21.1774359451272)) ;
#111958 = CARTESIAN_POINT('Ctrl Pts',(65.6294018614015,247.430268035678,21.1537001690032)) ;
#111959 = CARTESIAN_POINT('Ctrl Pts',(65.6322061928816,247.496285583913,21.1334225446893)) ;
#111960 = CARTESIAN_POINT('Ctrl Pts',(65.6350105243617,247.563065999685,21.1166909147133)) ;
#111961 = CARTESIAN_POINT('Ctrl Pts',(65.6353906302032,247.572117578043,21.1144230692974)) ;
#111962 = CARTESIAN_POINT('Ctrl Pts',(65.6357707360447,247.581183160105,21.11222029248)) ;
#111963 = CARTESIAN_POINT('Ctrl Pts',(65.6361508418862,247.590261736264,21.1100827299649)) ;
#111964 = CARTESIAN_POINT('Ctrl Pts',(65.6389551462454,247.657240687697,21.0943124491003)) ;
#111965 = CARTESIAN_POINT('Ctrl Pts',(65.6417594506045,247.725171800938,21.0820385006581)) ;
#111966 = CARTESIAN_POINT('Ctrl Pts',(65.6445637549637,247.793658548226,21.0733682253641)) ;
#111967 = CARTESIAN_POINT('Ctrl Pts',(65.6474349101322,247.863777926606,21.0644912624762)) ;
#111968 = CARTESIAN_POINT('Ctrl Pts',(65.6503060653008,247.934479290863,21.0593922007207)) ;
#111969 = CARTESIAN_POINT('Ctrl Pts',(65.6531772204693,248.005323040076,21.0581312793317)) ;
#111970 = CARTESIAN_POINT('Ctrl Pts',(65.6559744166489,248.074341902875,21.0569028384132)) ;
#111971 = CARTESIAN_POINT('Ctrl Pts',(65.6587716128286,248.143495383548,21.0593171883109)) ;
#111972 = CARTESIAN_POINT('Ctrl Pts',(65.6615688090083,248.212371297335,21.0653776783675)) ;
#111973 = CARTESIAN_POINT('Ctrl Pts',(65.6643644274066,248.281208361103,21.0714347499553)) ;
#111974 = CARTESIAN_POINT('Ctrl Pts',(65.667160045805,248.349767684046,21.0811338376912)) ;
#111975 = CARTESIAN_POINT('Ctrl Pts',(65.6699556642034,248.417639503082,21.0944262583087)) ;
#111976 = CARTESIAN_POINT('Ctrl Pts',(65.6727506432144,248.485495799118,21.1077156388094)) ;
#111977 = CARTESIAN_POINT('Ctrl Pts',(65.6755456222253,248.552664425469,21.1245966259919)) ;
#111978 = CARTESIAN_POINT('Ctrl Pts',(65.6783406012363,248.618744887007,21.1449692583328)) ;
#111979 = CARTESIAN_POINT('Ctrl Pts',(65.681268174384,248.687960213501,21.166308370775)) ;
#111980 = CARTESIAN_POINT('Ctrl Pts',(65.6841957475316,248.755980993142,21.1914785334642)) ;
#111981 = CARTESIAN_POINT('Ctrl Pts',(65.6871233206793,248.822366006382,21.2203066194546)) ;
#111982 = CARTESIAN_POINT('Ctrl Pts',(65.6899215441968,248.885817915484,21.2478609875651)) ;
#111983 = CARTESIAN_POINT('Ctrl Pts',(65.6927197677142,248.947775128316,21.2787565729496)) ;
#111984 = CARTESIAN_POINT('Ctrl Pts',(65.6955179912317,249.007876023601,21.3127942636895)) ;
#111985 = CARTESIAN_POINT('Ctrl Pts',(65.6983180182362,249.0680156546,21.3468538921104)) ;
#111986 = CARTESIAN_POINT('Ctrl Pts',(65.7011180452407,249.126296176496,21.3840593941392)) ;
#111987 = CARTESIAN_POINT('Ctrl Pts',(65.7039180722452,249.182384775927,21.4241682175409)) ;
#111988 = CARTESIAN_POINT('Ctrl Pts',(65.7067223994572,249.238559514747,21.4643386390141)) ;
#111989 = CARTESIAN_POINT('Ctrl Pts',(65.7095267266692,249.292535237366,21.5074209713915)) ;
#111990 = CARTESIAN_POINT('Ctrl Pts',(65.7123310538812,249.344012862449,21.5531330114348)) ;
#111991 = CARTESIAN_POINT('Ctrl Pts',(65.7127111955903,249.35099093273,21.5593295255051)) ;
#111992 = CARTESIAN_POINT('Ctrl Pts',(65.7130913372993,249.357923157329,21.5655743079424)) ;
#111993 = CARTESIAN_POINT('Ctrl Pts',(65.7134714790084,249.364808846371,21.5718666069489)) ;
#111994 = CARTESIAN_POINT('Ctrl Pts',(65.7162356678715,249.414877924591,21.61762086759)) ;
#111995 = CARTESIAN_POINT('Ctrl Pts',(65.7189998567346,249.462677693738,21.6660680056072)) ;
#111996 = CARTESIAN_POINT('Ctrl Pts',(65.7217640455977,249.50790051215,21.7169513122429)) ;
#111997 = CARTESIAN_POINT('Ctrl Pts',(65.7245247450279,249.553066242569,21.7677703852476)) ;
#111998 = CARTESIAN_POINT('Ctrl Pts',(65.727285444458,249.595661137275,21.8210191605267)) ;
#111999 = CARTESIAN_POINT('Ctrl Pts',(65.7300461438882,249.635412551539,21.8764024938038)) ;
#112000 = CARTESIAN_POINT('Ctrl Pts',(65.7328043528181,249.675128104997,21.9317358643068)) ;
#112001 = CARTESIAN_POINT('Ctrl Pts',(65.7355625617481,249.7120049712,21.9891995688869)) ;
#112002 = CARTESIAN_POINT('Ctrl Pts',(65.738320770678,249.745810455506,22.0484651041374)) ;
#112003 = CARTESIAN_POINT('Ctrl Pts',(65.7410774846502,249.779597617135,22.1076985172849)) ;
#112004 = CARTESIAN_POINT('Ctrl Pts',(65.7438341986225,249.81031645043,22.1687313877624)) ;
#112005 = CARTESIAN_POINT('Ctrl Pts',(65.7465909125947,249.837778407826,22.2312075755451)) ;
#112006 = CARTESIAN_POINT('Ctrl Pts',(65.749348553021,249.865249594414,22.2937047598186)) ;
#112007 = CARTESIAN_POINT('Ctrl Pts',(65.7521061934473,249.889461502537,22.3576457753752)) ;
#112008 = CARTESIAN_POINT('Ctrl Pts',(65.7548638338736,249.910272881316,22.4226525083319)) ;
#112009 = CARTESIAN_POINT('Ctrl Pts',(65.7576217613921,249.931086426725,22.487666009006)) ;
#112010 = CARTESIAN_POINT('Ctrl Pts',(65.7603796889107,249.948498597497,22.5537449641857)) ;
#112011 = CARTESIAN_POINT('Ctrl Pts',(65.7631376164293,249.962418217271,22.6204965996326)) ;
#112012 = CARTESIAN_POINT('Ctrl Pts',(65.765899358522,249.976357089699,22.6873405613132)) ;
#112013 = CARTESIAN_POINT('Ctrl Pts',(65.7686611006147,249.986793672311,22.754858565243)) ;
#112014 = CARTESIAN_POINT('Ctrl Pts',(65.7714228427074,249.993688246243,22.8226490267054)) ;
#112015 = CARTESIAN_POINT('Ctrl Pts',(65.7741326707675,250.000453218959,22.8891651924147)) ;
#112016 = CARTESIAN_POINT('Ctrl Pts',(65.7768424988277,250.003808268137,22.9559431984112)) ;
#112017 = CARTESIAN_POINT('Ctrl Pts',(65.7795523268879,250.003764688188,23.0226039947667)) ;
#112018 = CARTESIAN_POINT('',(66.2795523268944,250.003764624032,23.019942046258)) ;
#112019 = CARTESIAN_POINT('Ctrl Pts',(65.7795523269168,250.003764688188,23.0226039954774)) ;
#112020 = CARTESIAN_POINT('Ctrl Pts',(65.7832989233214,250.003704434708,23.1147689204846)) ;
#112021 = CARTESIAN_POINT('Ctrl Pts',(65.787045519726,249.997153658522,23.2067142655956)) ;
#112022 = CARTESIAN_POINT('Ctrl Pts',(65.7907921161306,249.984212027855,23.2977305856885)) ;
#112023 = CARTESIAN_POINT('Ctrl Pts',(65.7935964027768,249.974525358105,23.3658553110284)) ;
#112024 = CARTESIAN_POINT('Ctrl Pts',(65.796400689423,249.961235643221,23.43359451641)) ;
#112025 = CARTESIAN_POINT('Ctrl Pts',(65.7992049760692,249.94438720405,23.5005398053073)) ;
#112026 = CARTESIAN_POINT('Ctrl Pts',(65.8020761334518,249.927136998699,23.5690814648099)) ;
#112027 = CARTESIAN_POINT('Ctrl Pts',(65.8049472908345,249.906156147452,23.6367903357438)) ;
#112028 = CARTESIAN_POINT('Ctrl Pts',(65.8078184482171,249.881548520379,23.7032350336118)) ;
#112029 = CARTESIAN_POINT('Ctrl Pts',(65.8106156254977,249.857574949375,23.7679676743284)) ;
#112030 = CARTESIAN_POINT('Ctrl Pts',(65.8134128027783,249.830159435462,23.8315000181063)) ;
#112031 = CARTESIAN_POINT('Ctrl Pts',(65.8162099800589,249.79944885858,23.8934469289492)) ;
#112032 = CARTESIAN_POINT('Ctrl Pts',(65.8190055791721,249.768755608605,23.9553588893453)) ;
#112033 = CARTESIAN_POINT('Ctrl Pts',(65.8218011782852,249.734771201065,24.0156867560399)) ;
#112034 = CARTESIAN_POINT('Ctrl Pts',(65.8245967773984,249.697690099425,24.0740665841562)) ;
#112035 = CARTESIAN_POINT('Ctrl Pts',(65.8273917367707,249.660617483372,24.1324330527153)) ;
#112036 = CARTESIAN_POINT('Ctrl Pts',(65.8301866961429,249.620449842153,24.188851956971)) ;
#112037 = CARTESIAN_POINT('Ctrl Pts',(65.8329816555152,249.577426028614,24.242986645575)) ;
#112038 = CARTESIAN_POINT('Ctrl Pts',(65.8359092469933,249.532360561428,24.2996902437033)) ;
#112039 = CARTESIAN_POINT('Ctrl Pts',(65.8388368384714,249.484161425465,24.353886957013)) ;
#112040 = CARTESIAN_POINT('Ctrl Pts',(65.8417644299495,249.43315045536,24.4052288154293)) ;
#112041 = CARTESIAN_POINT('Ctrl Pts',(65.8445626331684,249.384393973519,24.4543015615948)) ;
#112042 = CARTESIAN_POINT('Ctrl Pts',(65.8473608363873,249.333069380292,24.5007661813769)) ;
#112043 = CARTESIAN_POINT('Ctrl Pts',(65.8501590396061,249.279493733614,24.5443583151576)) ;
#112044 = CARTESIAN_POINT('Ctrl Pts',(65.8529590461022,249.225883560586,24.5879785415018)) ;
#112045 = CARTESIAN_POINT('Ctrl Pts',(65.8557590525983,249.170019840529,24.6287223107889)) ;
#112046 = CARTESIAN_POINT('Ctrl Pts',(65.8585590590943,249.112249609004,24.666367904923)) ;
#112047 = CARTESIAN_POINT('Ctrl Pts',(65.8613633656434,249.054390658023,24.7040713125116)) ;
#112048 = CARTESIAN_POINT('Ctrl Pts',(65.8641676721924,248.994619776891,24.7386668120721)) ;
#112049 = CARTESIAN_POINT('Ctrl Pts',(65.8669719787414,248.933308657236,24.7699785345121)) ;
#112050 = CARTESIAN_POINT('Ctrl Pts',(65.8673522369118,248.924994996166,24.7742243393411)) ;
#112051 = CARTESIAN_POINT('Ctrl Pts',(65.8677324950823,248.916653043686,24.7784098390137)) ;
#112052 = CARTESIAN_POINT('Ctrl Pts',(65.8681127532527,248.908283751993,24.7825346642227)) ;
#112053 = CARTESIAN_POINT('Ctrl Pts',(65.8709170369376,248.846562873984,24.8129539449544)) ;
#112054 = CARTESIAN_POINT('Ctrl Pts',(65.8737213206225,248.783128441438,24.8401803846571)) ;
#112055 = CARTESIAN_POINT('Ctrl Pts',(65.8765256043074,248.718342706596,24.8640202702952)) ;
#112056 = CARTESIAN_POINT('Ctrl Pts',(65.8793967620602,248.652012019061,24.888428668363)) ;
#112057 = CARTESIAN_POINT('Ctrl Pts',(65.882267919813,248.584265172412,24.9092866076984)) ;
#112058 = CARTESIAN_POINT('Ctrl Pts',(65.8851390775658,248.515516986662,24.9264365871587)) ;
#112059 = CARTESIAN_POINT('Ctrl Pts',(65.8879362518848,248.448540290772,24.9431446492884)) ;
#112060 = CARTESIAN_POINT('Ctrl Pts',(65.8907334262039,248.380613744292,24.9563334198147)) ;
#112061 = CARTESIAN_POINT('Ctrl Pts',(65.8935306005229,248.312138228577,24.9659069978878)) ;
#112062 = CARTESIAN_POINT('Ctrl Pts',(65.8963261966832,248.243701346575,24.9754751745723)) ;
#112063 = CARTESIAN_POINT('Ctrl Pts',(65.8991217928436,248.174716591821,24.9814321391608)) ;
#112064 = CARTESIAN_POINT('Ctrl Pts',(65.9019173890039,248.105594180368,24.9837332364737)) ;
#112065 = CARTESIAN_POINT('Ctrl Pts',(65.9047123454372,248.036487586461,24.9860338072178)) ;
#112066 = CARTESIAN_POINT('Ctrl Pts',(65.9075073018706,247.967243885384,24.9846801563403)) ;
#112067 = CARTESIAN_POINT('Ctrl Pts',(65.910302258304,247.898275787108,24.979679678006)) ;
#112068 = CARTESIAN_POINT('Ctrl Pts',(65.9132298526432,247.826034727573,24.9744418961608)) ;
#112069 = CARTESIAN_POINT('Ctrl Pts',(65.9161574469824,247.754096661642,24.9652025381079)) ;
#112070 = CARTESIAN_POINT('Ctrl Pts',(65.9190850413217,247.682930446395,24.9520311426614)) ;
#112071 = CARTESIAN_POINT('Ctrl Pts',(65.9218832416723,247.61490963976,24.9394418973338)) ;
#112072 = CARTESIAN_POINT('Ctrl Pts',(65.9246814420229,247.547594376103,24.9232610403567)) ;
#112073 = CARTESIAN_POINT('Ctrl Pts',(65.9274796423735,247.481381769452,24.9036013173074)) ;
#112074 = CARTESIAN_POINT('Ctrl Pts',(65.9302796460286,247.415126491985,24.8839289245192)) ;
#112075 = CARTESIAN_POINT('Ctrl Pts',(65.9330796496838,247.349975744644,24.8607733669104)) ;
#112076 = CARTESIAN_POINT('Ctrl Pts',(65.9358796533389,247.286308333306,24.8342961934308)) ;
#112077 = CARTESIAN_POINT('Ctrl Pts',(65.9386839571058,247.222543144603,24.8077783575741)) ;
#112078 = CARTESIAN_POINT('Ctrl Pts',(65.9414882608727,247.160266273636,24.7779289420924)) ;
#112079 = CARTESIAN_POINT('Ctrl Pts',(65.9442925646396,247.099832568283,24.7449557135392)) ;
#112080 = CARTESIAN_POINT('Ctrl Pts',(65.9446728398847,247.091637506683,24.7404844067148)) ;
#112081 = CARTESIAN_POINT('Ctrl Pts',(65.9450531151298,247.083476293981,24.7359557225224)) ;
#112082 = CARTESIAN_POINT('Ctrl Pts',(65.9454333903749,247.075349772257,24.7313702391066)) ;
#112083 = CARTESIAN_POINT('Ctrl Pts',(65.9482376714969,247.015421991652,24.6975552991565)) ;
#112084 = CARTESIAN_POINT('Ctrl Pts',(65.951041952619,246.957164536995,24.6605247010187)) ;
#112085 = CARTESIAN_POINT('Ctrl Pts',(65.953846233741,246.900941669287,24.6204683518713)) ;
#112086 = CARTESIAN_POINT('Ctrl Pts',(65.9567173918141,246.843377989508,24.5794567324105)) ;
#112087 = CARTESIAN_POINT('Ctrl Pts',(65.9595885498873,246.787947679348,24.5352733627102)) ;
#112088 = CARTESIAN_POINT('Ctrl Pts',(65.9624597079605,246.73501474225,24.4881719833885)) ;
#112089 = CARTESIAN_POINT('Ctrl Pts',(65.9652568795533,246.683445826781,24.4422843530792)) ;
#112090 = CARTESIAN_POINT('Ctrl Pts',(65.9680540511461,246.634247511617,24.3936276378542)) ;
#112091 = CARTESIAN_POINT('Ctrl Pts',(65.970851222739,246.587725068246,24.3424788062479)) ;
#112092 = CARTESIAN_POINT('Ctrl Pts',(65.9736468161203,246.541228873624,24.2913588336764)) ;
#112093 = CARTESIAN_POINT('Ctrl Pts',(65.9764424095017,246.497405882032,24.2377498950117)) ;
#112094 = CARTESIAN_POINT('Ctrl Pts',(65.979238002883,246.456524310034,24.1819655673617)) ;
#112095 = CARTESIAN_POINT('Ctrl Pts',(65.9820329564894,246.415652093834,24.1261940060242)) ;
#112096 = CARTESIAN_POINT('Ctrl Pts',(65.9848279100957,246.377720248034,24.0682484376437)) ;
#112097 = CARTESIAN_POINT('Ctrl Pts',(65.9876228637021,246.342955412737,24.0084738519319)) ;
#112098 = CARTESIAN_POINT('Ctrl Pts',(65.990550460685,246.306540702061,23.9458624739157)) ;
#112099 = CARTESIAN_POINT('Ctrl Pts',(65.9934780576679,246.2736014171,23.8812446314221)) ;
#112100 = CARTESIAN_POINT('Ctrl Pts',(65.9964056546508,246.244344543332,23.8150467297727)) ;
#112101 = CARTESIAN_POINT('Ctrl Pts',(65.9992038520868,246.21638082099,23.7517747699573)) ;
#112102 = CARTESIAN_POINT('Ctrl Pts',(66.0020020495227,246.191780974643,23.6870599811615)) ;
#112103 = CARTESIAN_POINT('Ctrl Pts',(66.0048002469586,246.170675848666,23.6212938864612)) ;
#112104 = CARTESIAN_POINT('Ctrl Pts',(66.0076002476715,246.149557121651,23.5554854093052)) ;
#112105 = CARTESIAN_POINT('Ctrl Pts',(66.0104002483843,246.131937721229,23.4886247488484)) ;
#112106 = CARTESIAN_POINT('Ctrl Pts',(66.0132002490971,246.11789786458,23.4211158315903)) ;
#112107 = CARTESIAN_POINT('Ctrl Pts',(66.016004549903,246.103836446261,23.3535032377054)) ;
#112108 = CARTESIAN_POINT('Ctrl Pts',(66.0188088507089,246.093365609272,23.2852408819788)) ;
#112109 = CARTESIAN_POINT('Ctrl Pts',(66.0216131515148,246.08651389274,23.2167389703751)) ;
#112110 = CARTESIAN_POINT('Ctrl Pts',(66.0219934435089,246.0855847296,23.2074494075337)) ;
#112111 = CARTESIAN_POINT('Ctrl Pts',(66.022373735503,246.084722044184,23.1981554393433)) ;
#112112 = CARTESIAN_POINT('Ctrl Pts',(66.0227540274971,246.083925833939,23.1888580873805)) ;
#112113 = CARTESIAN_POINT('Ctrl Pts',(66.0255583084631,246.078054563263,23.1202992232747)) ;
#112114 = CARTESIAN_POINT('Ctrl Pts',(66.0283625894291,246.075780794755,23.0513062766017)) ;
#112115 = CARTESIAN_POINT('Ctrl Pts',(66.0311668703951,246.077153124161,22.9822871557965)) ;
#112116 = CARTESIAN_POINT('Ctrl Pts',(66.0340380284878,246.078558181188,22.9116220513894)) ;
#112117 = CARTESIAN_POINT('Ctrl Pts',(66.0369091865804,246.083785612578,22.8409300130663)) ;
#112118 = CARTESIAN_POINT('Ctrl Pts',(66.0397803446731,246.092831154402,22.7706547352107)) ;
#112119 = CARTESIAN_POINT('Ctrl Pts',(66.042577516201,246.10164360263,22.7021903734493)) ;
#112120 = CARTESIAN_POINT('Ctrl Pts',(66.0453746877289,246.114079684301,22.6341220671762)) ;
#112121 = CARTESIAN_POINT('Ctrl Pts',(66.0481718592568,246.130082831969,22.566858108434)) ;
#112122 = CARTESIAN_POINT('Ctrl Pts',(66.050967452607,246.146076950585,22.4996321003405)) ;
#112123 = CARTESIAN_POINT('Ctrl Pts',(66.0537630459573,246.165634028701,22.4332100124937)) ;
#112124 = CARTESIAN_POINT('Ctrl Pts',(66.0565586393075,246.188646370115,22.3679901817676)) ;
#112125 = CARTESIAN_POINT('Ctrl Pts',(66.0593535929166,246.211653445405,22.302785275892)) ;
#112126 = CARTESIAN_POINT('Ctrl Pts',(66.0621485465256,246.238114051163,22.2387825400709)) ;
#112127 = CARTESIAN_POINT('Ctrl Pts',(66.0649435001347,246.267871103425,22.1763636918273)) ;
#112128 = CARTESIAN_POINT('Ctrl Pts',(66.0678710971751,246.299040371442,22.1109825582049)) ;
#112129 = CARTESIAN_POINT('Ctrl Pts',(66.0707986942155,246.33382655352,22.047339934533)) ;
#112130 = CARTESIAN_POINT('Ctrl Pts',(66.0737262912559,246.371994247573,21.9858472212796)) ;
#112131 = CARTESIAN_POINT('Ctrl Pts',(66.0765244887789,246.408474933093,21.9270724802423)) ;
#112132 = CARTESIAN_POINT('Ctrl Pts',(66.0793226863019,246.448044167759,21.8702619899651)) ;
#112133 = CARTESIAN_POINT('Ctrl Pts',(66.082120883825,246.490452416229,21.8157446009826)) ;
#112134 = CARTESIAN_POINT('Ctrl Pts',(66.0849208846539,246.53288799481,21.7611920781217)) ;
#112135 = CARTESIAN_POINT('Ctrl Pts',(66.0877208854829,246.578165909477,21.7089359656719)) ;
#112136 = CARTESIAN_POINT('Ctrl Pts',(66.0905208863119,246.625997831022,21.6592703004726)) ;
#112137 = CARTESIAN_POINT('Ctrl Pts',(66.0933251872741,246.673903210985,21.6095283606616)) ;
#112138 = CARTESIAN_POINT('Ctrl Pts',(66.0961294882363,246.724370065361,21.5623851343566)) ;
#112139 = CARTESIAN_POINT('Ctrl Pts',(66.0989337891985,246.777075735682,21.5180955233138)) ;
#112140 = CARTESIAN_POINT('Ctrl Pts',(66.0993140810054,246.784223162036,21.5120894004193)) ;
#112141 = CARTESIAN_POINT('Ctrl Pts',(66.0996943728124,246.791411716169,21.5061356911673)) ;
#112142 = CARTESIAN_POINT('Ctrl Pts',(66.1000746646193,246.798640553014,21.500234969563)) ;
#112143 = CARTESIAN_POINT('Ctrl Pts',(66.1028789485387,246.851946226575,21.4567228601616)) ;
#112144 = CARTESIAN_POINT('Ctrl Pts',(66.1056832324581,246.907639171652,21.4159368162257)) ;
#112145 = CARTESIAN_POINT('Ctrl Pts',(66.1084875163775,246.965409937471,21.3781470073448)) ;
#112146 = CARTESIAN_POINT('Ctrl Pts',(66.111358674101,247.024558363679,21.3394560242788)) ;
#112147 = CARTESIAN_POINT('Ctrl Pts',(66.1142298318245,247.085884643482,21.303906411777)) ;
#112148 = CARTESIAN_POINT('Ctrl Pts',(66.117100989548,247.14901996494,21.2717448678076)) ;
#112149 = CARTESIAN_POINT('Ctrl Pts',(66.1198981639646,247.210528430505,21.2404120548259)) ;
#112150 = CARTESIAN_POINT('Ctrl Pts',(66.1226953383813,247.273753365653,21.212295040097)) ;
#112151 = CARTESIAN_POINT('Ctrl Pts',(66.125492512798,247.338325696517,21.1875773645937)) ;
#112152 = CARTESIAN_POINT('Ctrl Pts',(66.128288109005,247.40286159466,21.1628736351897)) ;
#112153 = CARTESIAN_POINT('Ctrl Pts',(66.1310837052121,247.468742925502,21.1415656127726)) ;
#112154 = CARTESIAN_POINT('Ctrl Pts',(66.1338793014192,247.535580002394,21.1237890014218)) ;
#112155 = CARTESIAN_POINT('Ctrl Pts',(66.1366742578485,247.602401783486,21.1060164582841)) ;
#112156 = CARTESIAN_POINT('Ctrl Pts',(66.1394692142778,247.670178405283,21.0917738460281)) ;
#112157 = CARTESIAN_POINT('Ctrl Pts',(66.1422641707071,247.738506053524,21.0811467113372)) ;
#112158 = CARTESIAN_POINT('Ctrl Pts',(66.1451917649599,247.810076267716,21.0700152539309)) ;
#112159 = CARTESIAN_POINT('Ctrl Pts',(66.1481193592128,247.882250543566,21.0628511036595)) ;
#112160 = CARTESIAN_POINT('Ctrl Pts',(66.1510469534657,247.954556389716,21.0596918706711)) ;
#112161 = CARTESIAN_POINT('Ctrl Pts',(66.1538451536853,248.023666456584,21.0566722697024)) ;
#112162 = CARTESIAN_POINT('Ctrl Pts',(66.156643353905,248.092896198804,21.0573109666162)) ;
#112163 = CARTESIAN_POINT('Ctrl Pts',(66.1594415541247,248.161833322598,21.0615873466574)) ;
#112164 = CARTESIAN_POINT('Ctrl Pts',(66.1622415576052,248.230814871954,21.0658664825516)) ;
#112165 = CARTESIAN_POINT('Ctrl Pts',(66.1650415610857,248.299502943777,21.0737879112051)) ;
#112166 = CARTESIAN_POINT('Ctrl Pts',(66.1678415645663,248.367492116105,21.0852793483772)) ;
#112167 = CARTESIAN_POINT('Ctrl Pts',(66.1706458680983,248.435585701495,21.0967884333028)) ;
#112168 = CARTESIAN_POINT('Ctrl Pts',(66.1734501716303,248.50297777235,21.1118783550531)) ;
#112169 = CARTESIAN_POINT('Ctrl Pts',(66.1762544751623,248.569275864971,21.1304264097859)) ;
#112170 = CARTESIAN_POINT('Ctrl Pts',(66.1766347506886,248.578266169259,21.1329416051619)) ;
#112171 = CARTESIAN_POINT('Ctrl Pts',(66.177015026215,248.587236385339,21.1355203173889)) ;
#112172 = CARTESIAN_POINT('Ctrl Pts',(66.1773953017414,248.596185562741,21.1381621723581)) ;
#112173 = CARTESIAN_POINT('Ctrl Pts',(66.1801995884356,248.662179973029,21.1576441485155)) ;
#112174 = CARTESIAN_POINT('Ctrl Pts',(66.1830038751297,248.727269454682,21.1806349226248)) ;
#112175 = CARTESIAN_POINT('Ctrl Pts',(66.1858081618239,248.791056384375,21.2070313067749)) ;
#112176 = CARTESIAN_POINT('Ctrl Pts',(66.1886793192006,248.856364369505,21.2340571359195)) ;
#112177 = CARTESIAN_POINT('Ctrl Pts',(66.1915504765772,248.920306364013,21.2646530243737)) ;
#112178 = CARTESIAN_POINT('Ctrl Pts',(66.1944216339539,248.982470652671,21.2986535269093)) ;
#112179 = CARTESIAN_POINT('Ctrl Pts',(66.1972188112544,249.043033176535,21.3317779507649)) ;
#112180 = CARTESIAN_POINT('Ctrl Pts',(66.200015988555,249.101908047876,21.3681333979902)) ;
#112181 = CARTESIAN_POINT('Ctrl Pts',(66.2028131658556,249.158735558242,21.4075185894839)) ;
#112182 = CARTESIAN_POINT('Ctrl Pts',(66.2056087649783,249.215531006315,21.4468815597063)) ;
#112183 = CARTESIAN_POINT('Ctrl Pts',(66.2084043641011,249.270280985882,21.4892706047942)) ;
#112184 = CARTESIAN_POINT('Ctrl Pts',(66.2111999632238,249.322653668317,21.534440445982)) ;
#112185 = CARTESIAN_POINT('Ctrl Pts',(66.2139949225952,249.375014365666,21.5795999503994)) ;
#112186 = CARTESIAN_POINT('Ctrl Pts',(66.2167898819666,249.42499847763,21.6275386685791)) ;
#112187 = CARTESIAN_POINT('Ctrl Pts',(66.219584841338,249.472307628976,21.6779713689805)) ;
#112188 = CARTESIAN_POINT('Ctrl Pts',(66.2225124327985,249.521861790264,21.7307973043174)) ;
#112189 = CARTESIAN_POINT('Ctrl Pts',(66.225440024259,249.568480366161,21.786359421252)) ;
#112190 = CARTESIAN_POINT('Ctrl Pts',(66.2283676157194,249.611865839533,21.8442887424657)) ;
#112191 = CARTESIAN_POINT('Ctrl Pts',(66.2311658189115,249.653333842059,21.8996578107674)) ;
#112192 = CARTESIAN_POINT('Ctrl Pts',(66.2339640221036,249.691848263824,21.9571887949095)) ;
#112193 = CARTESIAN_POINT('Ctrl Pts',(66.2367622252956,249.727193616902,22.0165295916453)) ;
#112194 = CARTESIAN_POINT('Ctrl Pts',(66.239562231756,249.762561747866,22.0759086298412)) ;
#112195 = CARTESIAN_POINT('Ctrl Pts',(66.2423622382163,249.794756518943,22.1370993707667)) ;
#112196 = CARTESIAN_POINT('Ctrl Pts',(66.2451622446767,249.823608986797,22.199726247187)) ;
#112197 = CARTESIAN_POINT('Ctrl Pts',(66.2479665511776,249.852505764114,22.2624493012825)) ;
#112198 = CARTESIAN_POINT('Ctrl Pts',(66.2507708576786,249.87804982134,22.3266124379175)) ;
#112199 = CARTESIAN_POINT('Ctrl Pts',(66.2535751641795,249.900121159985,22.3918223569875)) ;
#112200 = CARTESIAN_POINT('Ctrl Pts',(66.2539554224075,249.90311398838,22.4006646886898)) ;
#112201 = CARTESIAN_POINT('Ctrl Pts',(66.2543356806356,249.906043040956,22.4095262496389)) ;
#112202 = CARTESIAN_POINT('Ctrl Pts',(66.2547159388636,249.908908090672,22.4184060440853)) ;
#112203 = CARTESIAN_POINT('Ctrl Pts',(66.2580138048557,249.933755810796,22.4954178480688)) ;
#112204 = CARTESIAN_POINT('Ctrl Pts',(66.2613116708477,249.953858330787,22.5740280426585)) ;
#112205 = CARTESIAN_POINT('Ctrl Pts',(66.2646095368398,249.969042667699,22.6536936655638)) ;
#112206 = CARTESIAN_POINT('Ctrl Pts',(66.2678762584172,249.984083606643,22.7326069415889)) ;
#112207 = CARTESIAN_POINT('Ctrl Pts',(66.2711429799946,249.994298745068,22.8125556966939)) ;
#112208 = CARTESIAN_POINT('Ctrl Pts',(66.2744097015721,249.999567098801,22.8929928016749)) ;
#112209 = CARTESIAN_POINT('Ctrl Pts',(66.2761239100128,250.002331661444,22.9352020812362)) ;
#112210 = CARTESIAN_POINT('Ctrl Pts',(66.2778381184536,250.003734863383,22.9775455190962)) ;
#112211 = CARTESIAN_POINT('Ctrl Pts',(66.2795523268944,250.003764624032,23.019942046258)) ;
#112212 = CARTESIAN_POINT('',(66.7795523268961,250.003764452858,23.0229240588049)) ;
#112213 = CARTESIAN_POINT('Ctrl Pts',(66.2795523269168,250.003764624032,23.0199420468122)) ;
#112214 = CARTESIAN_POINT('Ctrl Pts',(66.2823406185767,250.003813031993,23.0889032537952)) ;
#112215 = CARTESIAN_POINT('Ctrl Pts',(66.2851289102367,250.000224085711,23.1579109029645)) ;
#112216 = CARTESIAN_POINT('Ctrl Pts',(66.2879172018966,249.993009685332,23.2265540271134)) ;
#112217 = CARTESIAN_POINT('Ctrl Pts',(66.2907048552082,249.98579693661,23.2951814361853)) ;
#112218 = CARTESIAN_POINT('Ctrl Pts',(66.2934925085199,249.974960433389,23.3634439989452)) ;
#112219 = CARTESIAN_POINT('Ctrl Pts',(66.2962801618316,249.96056397712,23.4309354097307)) ;
#112220 = CARTESIAN_POINT('Ctrl Pts',(66.2990681239764,249.946165925925,23.4984342976234)) ;
#112221 = CARTESIAN_POINT('Ctrl Pts',(66.3018560861212,249.928207243678,23.565161385473)) ;
#112222 = CARTESIAN_POINT('Ctrl Pts',(66.304644048266,249.906802553114,23.6307218657)) ;
#112223 = CARTESIAN_POINT('Ctrl Pts',(66.3074350008797,249.885374903107,23.6963526684659)) ;
#112224 = CARTESIAN_POINT('Ctrl Pts',(66.3102259534934,249.860494023033,23.7608139008159)) ;
#112225 = CARTESIAN_POINT('Ctrl Pts',(66.3130169061071,249.83232367605,23.823728181203)) ;
#112226 = CARTESIAN_POINT('Ctrl Pts',(66.3158096453554,249.804135295755,23.8866827363103)) ;
#112227 = CARTESIAN_POINT('Ctrl Pts',(66.3186023846038,249.772653481735,23.9480879332316)) ;
#112228 = CARTESIAN_POINT('Ctrl Pts',(66.3213951238522,249.738087949321,24.0075910207892)) ;
#112229 = CARTESIAN_POINT('Ctrl Pts',(66.3241924149176,249.703466079395,24.0671910909663)) ;
#112230 = CARTESIAN_POINT('Ctrl Pts',(66.326989705983,249.665750732254,24.124882458082)) ;
#112231 = CARTESIAN_POINT('Ctrl Pts',(66.3297869970484,249.625194313814,24.1803421992117)) ;
#112232 = CARTESIAN_POINT('Ctrl Pts',(66.3305368566942,249.614322502174,24.1952090903813)) ;
#112233 = CARTESIAN_POINT('Ctrl Pts',(66.33128671634,249.603246748992,24.209915810732)) ;
#112234 = CARTESIAN_POINT('Ctrl Pts',(66.3320365759858,249.591972378206,24.224456577295)) ;
#112235 = CARTESIAN_POINT('Ctrl Pts',(66.3348408832902,249.549808753952,24.2788357909423)) ;
#112236 = CARTESIAN_POINT('Ctrl Pts',(66.3376451905946,249.504706239201,24.3310951425113)) ;
#112237 = CARTESIAN_POINT('Ctrl Pts',(66.340449497899,249.456905656582,24.3809018253054)) ;
#112238 = CARTESIAN_POINT('Ctrl Pts',(66.3433206526994,249.407965630633,24.4318957717145)) ;
#112239 = CARTESIAN_POINT('Ctrl Pts',(66.3461918074997,249.356197496886,24.4803181537219)) ;
#112240 = CARTESIAN_POINT('Ctrl Pts',(66.3490629623001,249.30190518708,24.525845704037)) ;
#112241 = CARTESIAN_POINT('Ctrl Pts',(66.3518601597058,249.249011379988,24.5702005209955)) ;
#112242 = CARTESIAN_POINT('Ctrl Pts',(66.3546573571116,249.193722271344,24.6118075141096)) ;
#112243 = CARTESIAN_POINT('Ctrl Pts',(66.3574545545173,249.136356249685,24.6504048897544)) ;
#112244 = CARTESIAN_POINT('Ctrl Pts',(66.3602501735027,249.079022598889,24.6889804854265)) ;
#112245 = CARTESIAN_POINT('Ctrl Pts',(66.363045792488,249.019614764495,24.7245495622709)) ;
#112246 = CARTESIAN_POINT('Ctrl Pts',(66.3658414114734,248.958481971273,24.7568923073823)) ;
#112247 = CARTESIAN_POINT('Ctrl Pts',(66.3686363904332,248.897363173718,24.7892276479856)) ;
#112248 = CARTESIAN_POINT('Ctrl Pts',(66.371431369393,248.834520632473,24.8183378962952)) ;
#112249 = CARTESIAN_POINT('Ctrl Pts',(66.3742263483528,248.77032861088,24.8440489386746)) ;
#112250 = CARTESIAN_POINT('Ctrl Pts',(66.3771539204158,248.70309133583,24.8709797064767)) ;
#112251 = CARTESIAN_POINT('Ctrl Pts',(66.3800814924787,248.634373877362,24.8941804696978)) ;
#112252 = CARTESIAN_POINT('Ctrl Pts',(66.3830090645416,248.564628171981,24.9135083962933)) ;
#112253 = CARTESIAN_POINT('Ctrl Pts',(66.3858072864145,248.497964071442,24.9319823486997)) ;
#112254 = CARTESIAN_POINT('Ctrl Pts',(66.3886055082874,248.430361183098,24.9469184298629)) ;
#112255 = CARTESIAN_POINT('Ctrl Pts',(66.3914037301603,248.362225891714,24.958244065241)) ;
#112256 = CARTESIAN_POINT('Ctrl Pts',(66.3942037549716,248.294046699689,24.9695769979045)) ;
#112257 = CARTESIAN_POINT('Ctrl Pts',(66.3970037797829,248.225334905901,24.9772948007852)) ;
#112258 = CARTESIAN_POINT('Ctrl Pts',(66.3998038045943,248.156501811782,24.9813767913805)) ;
#112259 = CARTESIAN_POINT('Ctrl Pts',(66.4026081288559,248.087563024148,24.98546504989)) ;
#112260 = CARTESIAN_POINT('Ctrl Pts',(66.4054124531175,248.018503050828,24.9859063585669)) ;
#112261 = CARTESIAN_POINT('Ctrl Pts',(66.4082167773791,247.949731898289,24.9827320769746)) ;
#112262 = CARTESIAN_POINT('Ctrl Pts',(66.4085969226221,247.940409500431,24.9823017814972)) ;
#112263 = CARTESIAN_POINT('Ctrl Pts',(66.408977067865,247.931092398573,24.9818051247597)) ;
#112264 = CARTESIAN_POINT('Ctrl Pts',(66.409357213108,247.921781601908,24.9812422575232)) ;
#112265 = CARTESIAN_POINT('Ctrl Pts',(66.4121615246675,247.853096342257,24.9770900153815)) ;
#112266 = CARTESIAN_POINT('Ctrl Pts',(66.414965836227,247.784504331069,24.9693152890603)) ;
#112267 = CARTESIAN_POINT('Ctrl Pts',(66.4177701477865,247.716416217242,24.9579292731304)) ;
#112268 = CARTESIAN_POINT('Ctrl Pts',(66.4206413020549,247.646705176046,24.9462718636219)) ;
#112269 = CARTESIAN_POINT('Ctrl Pts',(66.4235124563234,247.577522881246,24.930828737212)) ;
#112270 = CARTESIAN_POINT('Ctrl Pts',(66.4263836105919,247.509307690899,24.9116685843483)) ;
#112271 = CARTESIAN_POINT('Ctrl Pts',(66.4291808136461,247.442849492929,24.8930019321602)) ;
#112272 = CARTESIAN_POINT('Ctrl Pts',(66.4319780167002,247.377309680021,24.8708075687004)) ;
#112273 = CARTESIAN_POINT('Ctrl Pts',(66.4347752197543,247.313083999177,24.8452007906509)) ;
#112274 = CARTESIAN_POINT('Ctrl Pts',(66.4375708448837,247.248894548556,24.819608457591)) ;
#112275 = CARTESIAN_POINT('Ctrl Pts',(66.4403664700131,247.186018210787,24.7906077102002)) ;
#112276 = CARTESIAN_POINT('Ctrl Pts',(66.4431620951424,247.124833453977,24.7583629847186)) ;
#112277 = CARTESIAN_POINT('Ctrl Pts',(66.4459570807273,247.063662694172,24.7261256357403)) ;
#112278 = CARTESIAN_POINT('Ctrl Pts',(66.4487520663121,247.004183177623,24.6906460100167)) ;
#112279 = CARTESIAN_POINT('Ctrl Pts',(66.4515470518969,246.946749753233,24.6521349925484)) ;
#112280 = CARTESIAN_POINT('Ctrl Pts',(66.4544746184247,246.886591957883,24.6117971939199)) ;
#112281 = CARTESIAN_POINT('Ctrl Pts',(66.4574021849525,246.8286797056,24.5681335426055)) ;
#112282 = CARTESIAN_POINT('Ctrl Pts',(66.4603297514802,246.77338581049,24.5214367044075)) ;
#112283 = CARTESIAN_POINT('Ctrl Pts',(66.463127981089,246.720534743567,24.4768028851435)) ;
#112284 = CARTESIAN_POINT('Ctrl Pts',(66.4659262106978,246.670075887954,24.4293986300107)) ;
#112285 = CARTESIAN_POINT('Ctrl Pts',(66.4687244403066,246.622298354367,24.379518611928)) ;
#112286 = CARTESIAN_POINT('Ctrl Pts',(66.4715244732278,246.574490030663,24.3296064487869)) ;
#112287 = CARTESIAN_POINT('Ctrl Pts',(66.474324506149,246.529366785742,24.2772157164121)) ;
#112288 = CARTESIAN_POINT('Ctrl Pts',(66.4771245390702,246.487177649648,24.2226744118407)) ;
#112289 = CARTESIAN_POINT('Ctrl Pts',(66.479928871907,246.444923725129,24.1680493500373)) ;
#112290 = CARTESIAN_POINT('Ctrl Pts',(66.4827332047438,246.405613172611,24.111267529043)) ;
#112291 = CARTESIAN_POINT('Ctrl Pts',(66.4855375375806,246.369451314658,24.0526852250122)) ;
#112292 = CARTESIAN_POINT('Ctrl Pts',(66.4859176417971,246.364549872681,24.0447448762482)) ;
#112293 = CARTESIAN_POINT('Ctrl Pts',(66.4862977460136,246.35970620678,24.0367714842076)) ;
#112294 = CARTESIAN_POINT('Ctrl Pts',(66.4866778502301,246.354920761433,24.0287659670131)) ;
#112295 = CARTESIAN_POINT('Ctrl Pts',(66.4894819430555,246.319617725101,23.9697079183149)) ;
#112296 = CARTESIAN_POINT('Ctrl Pts',(66.4922860358808,246.287358211815,23.9086841781292)) ;
#112297 = CARTESIAN_POINT('Ctrl Pts',(66.4950901287062,246.258364562065,23.8460401112139)) ;
#112298 = CARTESIAN_POINT('Ctrl Pts',(66.4979613103164,246.228677230311,23.7818972656948)) ;
#112299 = CARTESIAN_POINT('Ctrl Pts',(66.5008324919267,246.202414393297,23.716055954698)) ;
#112300 = CARTESIAN_POINT('Ctrl Pts',(66.5037036735369,246.17976658824,23.6489169566531)) ;
#112301 = CARTESIAN_POINT('Ctrl Pts',(66.5065006566966,246.15770405861,23.5835129967578)) ;
#112302 = CARTESIAN_POINT('Ctrl Pts',(66.5092976398563,246.139072137996,23.5168781045418)) ;
#112303 = CARTESIAN_POINT('Ctrl Pts',(66.512094623016,246.123998794174,23.449404056535)) ;
#112304 = CARTESIAN_POINT('Ctrl Pts',(66.5148900284519,246.108933952931,23.3819680693253)) ;
#112305 = CARTESIAN_POINT('Ctrl Pts',(66.5176854338878,246.097423811082,23.3136943405699)) ;
#112306 = CARTESIAN_POINT('Ctrl Pts',(66.5204808393238,246.0895460126,23.2449880919614)) ;
#112307 = CARTESIAN_POINT('Ctrl Pts',(66.5232756057897,246.081670014814,23.1762975481341)) ;
#112308 = CARTESIAN_POINT('Ctrl Pts',(66.5260703722556,246.077424766582,23.1071751649751)) ;
#112309 = CARTESIAN_POINT('Ctrl Pts',(66.5288651387215,246.076836234115,23.0380328548493)) ;
#112310 = CARTESIAN_POINT('Ctrl Pts',(66.5317929177741,246.076219691355,22.9655998234315)) ;
#112311 = CARTESIAN_POINT('Ctrl Pts',(66.5347206968267,246.079616675261,22.8931455006518)) ;
#112312 = CARTESIAN_POINT('Ctrl Pts',(66.5376484758792,246.086995729267,22.8211429598744)) ;
#112313 = CARTESIAN_POINT('Ctrl Pts',(66.5404464903734,246.094047730012,22.7523317042792)) ;
#112314 = CARTESIAN_POINT('Ctrl Pts',(66.5432445048676,246.104736141785,22.6839335251056)) ;
#112315 = CARTESIAN_POINT('Ctrl Pts',(66.5460425193617,246.118980656983,22.6163532966271)) ;
#112316 = CARTESIAN_POINT('Ctrl Pts',(66.5488423387544,246.133234360804,22.5487294745744)) ;
#112317 = CARTESIAN_POINT('Ctrl Pts',(66.5516421581471,246.151048607749,22.4819251239235)) ;
#112318 = CARTESIAN_POINT('Ctrl Pts',(66.5544419775398,246.172292968435,22.4163308092623)) ;
#112319 = CARTESIAN_POINT('Ctrl Pts',(66.5572461005754,246.193569984136,22.350635668628)) ;
#112320 = CARTESIAN_POINT('Ctrl Pts',(66.5600502236111,246.218287455024,22.2861547275074)) ;
#112321 = CARTESIAN_POINT('Ctrl Pts',(66.5628543466468,246.246266951478,22.2232584003724)) ;
#112322 = CARTESIAN_POINT('Ctrl Pts',(66.563235726882,246.25007235759,22.2147040624463)) ;
#112323 = CARTESIAN_POINT('Ctrl Pts',(66.5636171071171,246.253938035722,22.2061789975571)) ;
#112324 = CARTESIAN_POINT('Ctrl Pts',(66.5639984873523,246.257863473067,22.1976840994865)) ;
#112325 = CARTESIAN_POINT('Ctrl Pts',(66.56680310456,246.286730593358,22.1352138005322)) ;
#112326 = CARTESIAN_POINT('Ctrl Pts',(66.5696077217676,246.318938468299,22.0741490763927)) ;
#112327 = CARTESIAN_POINT('Ctrl Pts',(66.5724123389752,246.354327170167,22.0148683971174)) ;
#112328 = CARTESIAN_POINT('Ctrl Pts',(66.5752834550377,246.39055495558,21.95418214375)) ;
#112329 = CARTESIAN_POINT('Ctrl Pts',(66.5781545711002,246.430116201379,21.8953661229176)) ;
#112330 = CARTESIAN_POINT('Ctrl Pts',(66.5810256871627,246.472787424797,21.838803551572)) ;
#112331 = CARTESIAN_POINT('Ctrl Pts',(66.5838231904591,246.51436459743,21.7836911923528)) ;
#112332 = CARTESIAN_POINT('Ctrl Pts',(66.5866206937555,246.558893868519,21.7307185269278)) ;
#112333 = CARTESIAN_POINT('Ctrl Pts',(66.589418197052,246.60612377853,21.6802122577885)) ;
#112334 = CARTESIAN_POINT('Ctrl Pts',(66.5922141195746,246.653327000528,21.6297345280219)) ;
#112335 = CARTESIAN_POINT('Ctrl Pts',(66.5950100420972,246.703227500808,21.581720784043)) ;
#112336 = CARTESIAN_POINT('Ctrl Pts',(66.5978059646198,246.755534338094,21.5364637513572)) ;
#112337 = CARTESIAN_POINT('Ctrl Pts',(66.6006012442589,246.807829148151,21.4912171248968)) ;
#112338 = CARTESIAN_POINT('Ctrl Pts',(66.603396523898,246.862528827727,21.4487262692637)) ;
#112339 = CARTESIAN_POINT('Ctrl Pts',(66.6061918035371,246.919307766271,21.409245007695)) ;
#112340 = CARTESIAN_POINT('Ctrl Pts',(66.6091190802819,246.978767887565,21.367899384442)) ;
#112341 = CARTESIAN_POINT('Ctrl Pts',(66.6120463570266,247.040508054616,21.3298549997475)) ;
#112342 = CARTESIAN_POINT('Ctrl Pts',(66.6149736337714,247.104120186999,21.2953525172994)) ;
#112343 = CARTESIAN_POINT('Ctrl Pts',(66.617772145689,247.164934153733,21.2623677274298)) ;
#112344 = CARTESIAN_POINT('Ctrl Pts',(66.6205706576066,247.227458366892,21.2326199408459)) ;
#112345 = CARTESIAN_POINT('Ctrl Pts',(66.6233691695242,247.291313095359,21.2062712717487)) ;
#112346 = CARTESIAN_POINT('Ctrl Pts',(66.6261694804375,247.355208872207,21.1799056646699)) ;
#112347 = CARTESIAN_POINT('Ctrl Pts',(66.6289697913508,247.420436407318,21.1569436854979)) ;
#112348 = CARTESIAN_POINT('Ctrl Pts',(66.6317701022641,247.48659950903,21.1374979913317)) ;
#112349 = CARTESIAN_POINT('Ctrl Pts',(66.6345747050863,247.552864015911,21.1180224936366)) ;
#112350 = CARTESIAN_POINT('Ctrl Pts',(66.6373793079084,247.620066476324,21.1020741416477)) ;
#112351 = CARTESIAN_POINT('Ctrl Pts',(66.6401839107306,247.687800256479,21.089714592224)) ;
#112352 = CARTESIAN_POINT('Ctrl Pts',(66.6405623153119,247.696939080884,21.0880470084621)) ;
#112353 = CARTESIAN_POINT('Ctrl Pts',(66.6409407198932,247.706087571098,21.0864446783601)) ;
#112354 = CARTESIAN_POINT('Ctrl Pts',(66.6413191244745,247.715244723888,21.084907680915)) ;
#112355 = CARTESIAN_POINT('Ctrl Pts',(66.6441234978784,247.78310879586,21.0735169235878)) ;
#112356 = CARTESIAN_POINT('Ctrl Pts',(66.6469278712823,247.8516960402,21.0656772442205)) ;
#112357 = CARTESIAN_POINT('Ctrl Pts',(66.6497322446863,247.920603762888,21.0614699889312)) ;
#112358 = CARTESIAN_POINT('Ctrl Pts',(66.6526033912242,247.991152203105,21.0571625573883)) ;
#112359 = CARTESIAN_POINT('Ctrl Pts',(66.6554745377622,248.062036086872,21.0566629239467)) ;
#112360 = CARTESIAN_POINT('Ctrl Pts',(66.6583456843001,248.132812836757,21.060002631443)) ;
#112361 = CARTESIAN_POINT('Ctrl Pts',(66.66114295754,248.201768532974,21.0632564097804)) ;
#112362 = CARTESIAN_POINT('Ctrl Pts',(66.66394023078,248.270622022945,21.0701543075325)) ;
#112363 = CARTESIAN_POINT('Ctrl Pts',(66.6667375040199,248.338961748443,21.0806728828239)) ;
#112364 = CARTESIAN_POINT('Ctrl Pts',(66.6695332021673,248.407262993113,21.0911855353011)) ;
#112365 = CARTESIAN_POINT('Ctrl Pts',(66.6723289003146,248.475050566595,21.1053147454544)) ;
#112366 = CARTESIAN_POINT('Ctrl Pts',(66.675124598462,248.541918708859,21.1229853060779)) ;
#112367 = CARTESIAN_POINT('Ctrl Pts',(66.6779196597248,248.608771617973,21.1406518411926)) ;
#112368 = CARTESIAN_POINT('Ctrl Pts',(66.6807147209876,248.674705040942,21.1618579997019)) ;
#112369 = CARTESIAN_POINT('Ctrl Pts',(66.6835097822504,248.739325798165,21.1864780066908)) ;
#112370 = CARTESIAN_POINT('Ctrl Pts',(66.6864372805292,248.807008449014,21.2122645713879)) ;
#112371 = CARTESIAN_POINT('Ctrl Pts',(66.6893647788081,248.873250389559,21.2417963754347)) ;
#112372 = CARTESIAN_POINT('Ctrl Pts',(66.692292277087,248.937622622676,21.2748720218303)) ;
#112373 = CARTESIAN_POINT('Ctrl Pts',(66.6950905879347,248.999154176604,21.3064880746122)) ;
#112374 = CARTESIAN_POINT('Ctrl Pts',(66.6978888987824,249.058977155078,21.3413414730132)) ;
#112375 = CARTESIAN_POINT('Ctrl Pts',(66.7006872096301,249.116743609473,21.379210028932)) ;
#112376 = CARTESIAN_POINT('Ctrl Pts',(66.7034873255982,249.174547327564,21.4171030129107)) ;
#112377 = CARTESIAN_POINT('Ctrl Pts',(66.7062874415664,249.230291488826,21.4580147371391)) ;
#112378 = CARTESIAN_POINT('Ctrl Pts',(66.7090875575346,249.283659712831,21.5016815357681)) ;
#112379 = CARTESIAN_POINT('Ctrl Pts',(66.7118919753153,249.337109926331,21.545415419612)) ;
#112380 = CARTESIAN_POINT('Ctrl Pts',(66.7146963930959,249.38817656324,21.5919124921997)) ;
#112381 = CARTESIAN_POINT('Ctrl Pts',(66.7175008108766,249.436579478484,21.6408717106214)) ;
#112382 = CARTESIAN_POINT('Ctrl Pts',(66.7178804611166,249.443132060812,21.6474996029249)) ;
#112383 = CARTESIAN_POINT('Ctrl Pts',(66.7182601113567,249.449635886879,21.6541725687552)) ;
#112384 = CARTESIAN_POINT('Ctrl Pts',(66.7186397615967,249.456090319567,21.6608898162314)) ;
#112385 = CARTESIAN_POINT('Ctrl Pts',(66.72140456754,249.503094777811,21.709808225302)) ;
#112386 = CARTESIAN_POINT('Ctrl Pts',(66.7241693734833,249.54765892548,21.7612677748274)) ;
#112387 = CARTESIAN_POINT('Ctrl Pts',(66.7269341794266,249.589492264482,21.8149922509759)) ;
#112388 = CARTESIAN_POINT('Ctrl Pts',(66.7296954263439,249.631271753071,21.8686475697182)) ;
#112389 = CARTESIAN_POINT('Ctrl Pts',(66.7324566732612,249.670327093644,21.9245616439305)) ;
#112390 = CARTESIAN_POINT('Ctrl Pts',(66.7352179201785,249.706405216602,21.9824221831053)) ;
#112391 = CARTESIAN_POINT('Ctrl Pts',(66.7379766065846,249.742449884226,22.0402290680572)) ;
#112392 = CARTESIAN_POINT('Ctrl Pts',(66.7407352929908,249.775522543469,22.0999784146441)) ;
#112393 = CARTESIAN_POINT('Ctrl Pts',(66.7434939793969,249.805412160736,22.1613272439004)) ;
#112394 = CARTESIAN_POINT('Ctrl Pts',(66.7462511002973,249.835284816175,22.2226412587823)) ;
#112395 = CARTESIAN_POINT('Ctrl Pts',(66.7490082211978,249.861977794241,22.285552504173)) ;
#112396 = CARTESIAN_POINT('Ctrl Pts',(66.7517653420982,249.885325908284,22.3496932949189)) ;
#112397 = CARTESIAN_POINT('Ctrl Pts',(66.7545228691849,249.908677462033,22.4138435350553)) ;
#112398 = CARTESIAN_POINT('Ctrl Pts',(66.7572803962717,249.928682984491,22.4792232138235)) ;
#112399 = CARTESIAN_POINT('Ctrl Pts',(66.7600379233585,249.94522595852,22.5454459828584)) ;
#112400 = CARTESIAN_POINT('Ctrl Pts',(66.7627957000588,249.961770430031,22.6116747464332)) ;
#112401 = CARTESIAN_POINT('Ctrl Pts',(66.7655534767592,249.974851620613,22.6787462610508)) ;
#112402 = CARTESIAN_POINT('Ctrl Pts',(66.7683112534596,249.984403886993,22.7462627910657)) ;
#112403 = CARTESIAN_POINT('Ctrl Pts',(66.7710716188912,249.993965120107,22.8138426989994)) ;
#112404 = CARTESIAN_POINT('Ctrl Pts',(66.7738319843228,249.999990765927,22.8818679558387)) ;
#112405 = CARTESIAN_POINT('Ctrl Pts',(66.7765923497544,250.002467061614,22.9499358747035)) ;
#112406 = CARTESIAN_POINT('Ctrl Pts',(66.7775790088016,250.003352183386,22.9742659243427)) ;
#112407 = CARTESIAN_POINT('Ctrl Pts',(66.7785656678489,250.003784318705,22.9986014255071)) ;
#112408 = CARTESIAN_POINT('Ctrl Pts',(66.7795523268961,250.003764452858,23.0229240588049)) ;
#112409 = CARTESIAN_POINT('',(66.9402651077866,247.187420265513,24.7899322074257)) ;
#112410 = CARTESIAN_POINT('Ctrl Pts',(66.7795523269168,250.003764452857,23.0229240593157)) ;
#112411 = CARTESIAN_POINT('Ctrl Pts',(66.7833403875917,250.003688182277,23.1163054669723)) ;
#112412 = CARTESIAN_POINT('Ctrl Pts',(66.7871284482667,249.996946522773,23.2094191785349)) ;
#112413 = CARTESIAN_POINT('Ctrl Pts',(66.7909165089416,249.983675392804,23.3014787167803)) ;
#112414 = CARTESIAN_POINT('Ctrl Pts',(66.7925978055341,249.977785121368,23.3423385131858)) ;
#112415 = CARTESIAN_POINT('Ctrl Pts',(66.7942791021265,249.970609197882,23.3829909913529)) ;
#112416 = CARTESIAN_POINT('Ctrl Pts',(66.7959603987189,249.962162427064,23.4233687786404)) ;
#112417 = CARTESIAN_POINT('Ctrl Pts',(66.7987684406399,249.948054930112,23.4908063264787)) ;
#112418 = CARTESIAN_POINT('Ctrl Pts',(66.8015764825609,249.930368358597,23.5576217364157)) ;
#112419 = CARTESIAN_POINT('Ctrl Pts',(66.8043845244819,249.909174104639,23.6234095491443)) ;
#112420 = CARTESIAN_POINT('Ctrl Pts',(66.8072552124552,249.887507017163,23.6906650560432)) ;
#112421 = CARTESIAN_POINT('Ctrl Pts',(66.8101259004285,249.862173867243,23.7568460432548)) ;
#112422 = CARTESIAN_POINT('Ctrl Pts',(66.8129965884018,249.833306360801,23.8215298879838)) ;
#112423 = CARTESIAN_POINT('Ctrl Pts',(66.8157975052758,249.80514046933,23.8846416137651)) ;
#112424 = CARTESIAN_POINT('Ctrl Pts',(66.8185984221498,249.773610291121,23.9463276776076)) ;
#112425 = CARTESIAN_POINT('Ctrl Pts',(66.8213993390237,249.738887943492,24.0062125772683)) ;
#112426 = CARTESIAN_POINT('Ctrl Pts',(66.8241986612997,249.704185363741,24.0660633836856)) ;
#112427 = CARTESIAN_POINT('Ctrl Pts',(66.8269979835757,249.666294464709,24.1241146414449)) ;
#112428 = CARTESIAN_POINT('Ctrl Pts',(66.8297973058516,249.625433461131,24.1800151012739)) ;
#112429 = CARTESIAN_POINT('Ctrl Pts',(66.8325959657634,249.584582125916,24.2359023341646)) ;
#112430 = CARTESIAN_POINT('Ctrl Pts',(66.8353946256752,249.540762368943,24.2896393879892)) ;
#112431 = CARTESIAN_POINT('Ctrl Pts',(66.838193285587,249.494234927956,24.3409051312997)) ;
#112432 = CARTESIAN_POINT('Ctrl Pts',(66.8411172647748,249.445624066544,24.3944664682303)) ;
#112433 = CARTESIAN_POINT('Ctrl Pts',(66.8440412439626,249.394057673407,24.4453295090004)) ;
#112434 = CARTESIAN_POINT('Ctrl Pts',(66.8469652231504,249.339877448202,24.4931695255883)) ;
#112435 = CARTESIAN_POINT('Ctrl Pts',(66.8497670277675,249.287961071449,24.5390106108855)) ;
#112436 = CARTESIAN_POINT('Ctrl Pts',(66.8525688323846,249.233645384136,24.582076004081)) ;
#112437 = CARTESIAN_POINT('Ctrl Pts',(66.8553706370016,249.177264424868,24.6221216438323)) ;
#112438 = CARTESIAN_POINT('Ctrl Pts',(66.8581742072453,249.120847935742,24.6621925193357)) ;
#112439 = CARTESIAN_POINT('Ctrl Pts',(66.860977777489,249.062363994278,24.6992395936262)) ;
#112440 = CARTESIAN_POINT('Ctrl Pts',(66.8637813477326,249.002173853502,24.7330632608564)) ;
#112441 = CARTESIAN_POINT('Ctrl Pts',(66.8665891405139,248.941893058629,24.7669378708818)) ;
#112442 = CARTESIAN_POINT('Ctrl Pts',(66.8693969332951,248.879901373507,24.7975791757488)) ;
#112443 = CARTESIAN_POINT('Ctrl Pts',(66.8722047260763,248.816581757081,24.8248348874507)) ;
#112444 = CARTESIAN_POINT('Ctrl Pts',(66.8725634959978,248.808490998401,24.8283175267732)) ;
#112445 = CARTESIAN_POINT('Ctrl Pts',(66.8729222659194,248.800378580186,24.8317449564989)) ;
#112446 = CARTESIAN_POINT('Ctrl Pts',(66.8732810358409,248.792245318936,24.8351169176106)) ;
#112447 = CARTESIAN_POINT('Ctrl Pts',(66.8760720388387,248.728973692283,24.8613486416366)) ;
#112448 = CARTESIAN_POINT('Ctrl Pts',(66.8788630418364,248.664195049807,24.8843205322089)) ;
#112449 = CARTESIAN_POINT('Ctrl Pts',(66.8816540448341,248.59828361459,24.9038578853005)) ;
#112450 = CARTESIAN_POINT('Ctrl Pts',(66.8844124564412,248.533141847243,24.9231670947795)) ;
#112451 = CARTESIAN_POINT('Ctrl Pts',(66.8871708680483,248.466894088193,24.9391213768116)) ;
#112452 = CARTESIAN_POINT('Ctrl Pts',(66.8899292796554,248.399922967563,24.9515997207226)) ;
#112453 = CARTESIAN_POINT('Ctrl Pts',(66.8926852815423,248.333010352218,24.9640671636802)) ;
#112454 = CARTESIAN_POINT('Ctrl Pts',(66.8954412834293,248.265376120888,24.9730645956052)) ;
#112455 = CARTESIAN_POINT('Ctrl Pts',(66.8981972853162,248.197416078765,24.9785213609108)) ;
#112456 = CARTESIAN_POINT('Ctrl Pts',(66.9009518753248,248.129490852044,24.9839753307578)) ;
#112457 = CARTESIAN_POINT('Ctrl Pts',(66.9037064653333,248.061240646926,24.9858921916273)) ;
#112458 = CARTESIAN_POINT('Ctrl Pts',(66.9064610553419,247.993067466502,24.9842530048237)) ;
#112459 = CARTESIAN_POINT('Ctrl Pts',(66.9092780597123,247.923349596837,24.9825766768128)) ;
#112460 = CARTESIAN_POINT('Ctrl Pts',(66.9120950640826,247.853712829984,24.9771811257619)) ;
#112461 = CARTESIAN_POINT('Ctrl Pts',(66.914912068453,247.784586283387,24.9681024548278)) ;
#112462 = CARTESIAN_POINT('Ctrl Pts',(66.9176681774467,247.71695405009,24.9592200381461)) ;
#112463 = CARTESIAN_POINT('Ctrl Pts',(66.9204242864404,247.649810699675,24.9468122973506)) ;
#112464 = CARTESIAN_POINT('Ctrl Pts',(66.923180395434,247.583549651707,24.930965138326)) ;
#112465 = CARTESIAN_POINT('Ctrl Pts',(66.9260278474928,247.515092577662,24.9145927721772)) ;
#112466 = CARTESIAN_POINT('Ctrl Pts',(66.9288752995515,247.447577886713,24.8945491173228)) ;
#112467 = CARTESIAN_POINT('Ctrl Pts',(66.9317227516103,247.381421698607,24.8709845325901)) ;
#112468 = CARTESIAN_POINT('Ctrl Pts',(66.9345702036691,247.315265510502,24.8474199478574)) ;
#112469 = CARTESIAN_POINT('Ctrl Pts',(66.9374176557278,247.250468345473,24.8203347117332)) ;
#112470 = CARTESIAN_POINT('Ctrl Pts',(66.9402651077866,247.187420265513,24.7899322074257)) ;
#112471 = CARTESIAN_POINT('',(66.9402651077866,247.154495177753,24.7736741551653)) ;
#112472 = CARTESIAN_POINT('Ctrl Pts',(66.9402651077866,247.187420265513,24.7899322074257)) ;
#112473 = CARTESIAN_POINT('Ctrl Pts',(66.9402651077866,247.176445236259,24.7845128566722)) ;
#112474 = CARTESIAN_POINT('Ctrl Pts',(66.9402651077866,247.165470207006,24.7790935059188)) ;
#112475 = CARTESIAN_POINT('Ctrl Pts',(66.9402651077866,247.154495177753,24.7736741551653)) ;
#112476 = CARTESIAN_POINT('',(66.9402651077866,248.892162375845,24.7903888257488)) ;
#112477 = CARTESIAN_POINT('Origin',(66.9402651077866,248.040265107786,23.0213203435596)) ;
#112478 = CARTESIAN_POINT('',(66.8509778886564,250.003764893262,23.0222381855048)) ;
#112479 = CARTESIAN_POINT('Ctrl Pts',(66.9402651077866,248.892162375845,24.7903888257488)) ;
#112480 = CARTESIAN_POINT('Ctrl Pts',(66.9144915620792,249.465128147431,24.5144764004134)) ;
#112481 = CARTESIAN_POINT('Ctrl Pts',(66.8847291557025,249.954933534302,23.8517629624628)) ;
#112482 = CARTESIAN_POINT('Ctrl Pts',(66.8549667493257,250.005277703762,23.1203925250327)) ;
#112483 = CARTESIAN_POINT('Ctrl Pts',(66.8509778886564,250.00450609953,23.0222385319832)) ;
#112484 = CARTESIAN_POINT('',(66.3509778886297,250.003764831718,23.0202791324881)) ;
#112485 = CARTESIAN_POINT('Ctrl Pts',(66.8509778886564,250.003764893262,23.0222381855048)) ;
#112486 = CARTESIAN_POINT('Ctrl Pts',(66.8482267036004,250.003796526989,22.9545655163395)) ;
#112487 = CARTESIAN_POINT('Ctrl Pts',(66.8454755185445,250.000325357658,22.8867680494306)) ;
#112488 = CARTESIAN_POINT('Ctrl Pts',(66.8427243334885,249.993338983009,22.8192443976375)) ;
#112489 = CARTESIAN_POINT('Ctrl Pts',(66.8399758974318,249.986359589185,22.7517882158492)) ;
#112490 = CARTESIAN_POINT('Ctrl Pts',(66.8372274613752,249.975872000238,22.6846058083517)) ;
#112491 = CARTESIAN_POINT('Ctrl Pts',(66.8344790253185,249.961915836364,22.6180949384146)) ;
#112492 = CARTESIAN_POINT('Ctrl Pts',(66.831732330507,249.947968514284,22.5516262057995)) ;
#112493 = CARTESIAN_POINT('Ctrl Pts',(66.8289856356955,249.930557076584,22.4858286624589)) ;
#112494 = CARTESIAN_POINT('Ctrl Pts',(66.8262389408841,249.90977260833,22.4210920908021)) ;
#112495 = CARTESIAN_POINT('Ctrl Pts',(66.8234929821263,249.888993709856,22.3563728671186)) ;
#112496 = CARTESIAN_POINT('Ctrl Pts',(66.8207470233684,249.864843729529,22.2927145333732)) ;
#112497 = CARTESIAN_POINT('Ctrl Pts',(66.8180010646106,249.837463659151,22.2304919064297)) ;
#112498 = CARTESIAN_POINT('Ctrl Pts',(66.815252997896,249.810062570247,22.1682215137992)) ;
#112499 = CARTESIAN_POINT('Ctrl Pts',(66.8125049311814,249.779426638707,22.1073894964761)) ;
#112500 = CARTESIAN_POINT('Ctrl Pts',(66.8097568644668,249.745744629783,22.0483497119119)) ;
#112501 = CARTESIAN_POINT('Ctrl Pts',(66.8070078405071,249.712050888268,21.9892893617802)) ;
#112502 = CARTESIAN_POINT('Ctrl Pts',(66.8042588165472,249.675309229075,21.9320229161002)) ;
#112503 = CARTESIAN_POINT('Ctrl Pts',(66.8015097925875,249.635752384316,21.8768761114409)) ;
#112504 = CARTESIAN_POINT('Ctrl Pts',(66.7987559331582,249.596125959985,21.8216323048304)) ;
#112505 = CARTESIAN_POINT('Ctrl Pts',(66.796002073729,249.553674774807,21.7685159848195)) ;
#112506 = CARTESIAN_POINT('Ctrl Pts',(66.7932482142998,249.508672063172,21.7178199548472)) ;
#112507 = CARTESIAN_POINT('Ctrl Pts',(66.7907067540473,249.467140312619,21.6710339991927)) ;
#112508 = CARTESIAN_POINT('Ctrl Pts',(66.7881652937948,249.423436103688,21.6263092066677)) ;
#112509 = CARTESIAN_POINT('Ctrl Pts',(66.7856238335423,249.377799747824,21.5838457049321)) ;
#112510 = CARTESIAN_POINT('Ctrl Pts',(66.7828201544163,249.327454794291,21.5370009693849)) ;
#112511 = CARTESIAN_POINT('Ctrl Pts',(66.7800164752903,249.274551903111,21.4927167710767)) ;
#112512 = CARTESIAN_POINT('Ctrl Pts',(66.7772127961643,249.219381460994,21.4512831224729)) ;
#112513 = CARTESIAN_POINT('Ctrl Pts',(66.7743415628416,249.162881695966,21.4088511367836)) ;
#112514 = CARTESIAN_POINT('Ctrl Pts',(66.771470329519,249.104004001477,21.369409270451)) ;
#112515 = CARTESIAN_POINT('Ctrl Pts',(66.7685990961963,249.043099853033,21.3332283070507)) ;
#112516 = CARTESIAN_POINT('Ctrl Pts',(66.7658027497716,248.983784193659,21.2979910078564)) ;
#112517 = CARTESIAN_POINT('Ctrl Pts',(66.7630064033468,248.922546947128,21.2658468506903)) ;
#112518 = CARTESIAN_POINT('Ctrl Pts',(66.7602100569221,248.85974380801,21.2370034126644)) ;
#112519 = CARTESIAN_POINT('Ctrl Pts',(66.7574153681327,248.79697789772,21.208177072628)) ;
#112520 = CARTESIAN_POINT('Ctrl Pts',(66.7546206793433,248.732648379345,21.1826477722248)) ;
#112521 = CARTESIAN_POINT('Ctrl Pts',(66.7518259905539,248.66713472333,21.160576746202)) ;
#112522 = CARTESIAN_POINT('Ctrl Pts',(66.7490320186323,248.601637872276,21.1385113816357)) ;
#112523 = CARTESIAN_POINT('Ctrl Pts',(66.7462380467108,248.534957949055,21.1199026851751)) ;
#112524 = CARTESIAN_POINT('Ctrl Pts',(66.7434440747892,248.467491879638,21.1048627950048)) ;
#112525 = CARTESIAN_POINT('Ctrl Pts',(66.7405156682585,248.396779616297,21.089099246253)) ;
#112526 = CARTESIAN_POINT('Ctrl Pts',(66.7375872617277,248.325204202411,21.0772567738979)) ;
#112527 = CARTESIAN_POINT('Ctrl Pts',(66.7346588551969,248.253235180171,21.0694043622048)) ;
#112528 = CARTESIAN_POINT('Ctrl Pts',(66.7318618178326,248.184494709143,21.0619042119778)) ;
#112529 = CARTESIAN_POINT('Ctrl Pts',(66.7290647804682,248.115395702809,21.0580437680177)) ;
#112530 = CARTESIAN_POINT('Ctrl Pts',(66.7262677431038,248.046350626325,21.0578297740727)) ;
#112531 = CARTESIAN_POINT('Ctrl Pts',(66.7234689624468,247.977262516533,21.0576156467529)) ;
#112532 = CARTESIAN_POINT('Ctrl Pts',(66.7206701817898,247.908228890469,21.0610524685653)) ;
#112533 = CARTESIAN_POINT('Ctrl Pts',(66.7178714011328,247.839658797962,21.0680949703733)) ;
#112534 = CARTESIAN_POINT('Ctrl Pts',(66.7150683953953,247.770985191034,21.0751481036457)) ;
#112535 = CARTESIAN_POINT('Ctrl Pts',(66.7122653896578,247.702776994151,21.0858176978745)) ;
#112536 = CARTESIAN_POINT('Ctrl Pts',(66.7094623839203,247.635433671554,21.1000073138222)) ;
#112537 = CARTESIAN_POINT('Ctrl Pts',(66.7090759880869,247.626150358677,21.1019633599361)) ;
#112538 = CARTESIAN_POINT('Ctrl Pts',(66.7086895922535,247.616883456562,21.1039862189317)) ;
#112539 = CARTESIAN_POINT('Ctrl Pts',(66.7083031964201,247.607633986837,21.1060755646381)) ;
#112540 = CARTESIAN_POINT('Ctrl Pts',(66.7054954325608,247.540422271368,21.121257895442)) ;
#112541 = CARTESIAN_POINT('Ctrl Pts',(66.7026876687015,247.473891429089,21.1400093724741)) ;
#112542 = CARTESIAN_POINT('Ctrl Pts',(66.6998799048422,247.408445683413,21.1622516345052)) ;
#112543 = CARTESIAN_POINT('Ctrl Pts',(66.6970091821112,247.341532438862,21.1849926378093)) ;
#112544 = CARTESIAN_POINT('Ctrl Pts',(66.6941384593802,247.275754062132,21.2113828453259)) ;
#112545 = CARTESIAN_POINT('Ctrl Pts',(66.6912677366492,247.211530999387,21.2412832575483)) ;
#112546 = CARTESIAN_POINT('Ctrl Pts',(66.688466935483,247.148872203716,21.2704553919782)) ;
#112547 = CARTESIAN_POINT('Ctrl Pts',(66.6856661343169,247.08769428332,21.3029684559092)) ;
#112548 = CARTESIAN_POINT('Ctrl Pts',(66.6828653331508,247.028369760528,21.3386438873749)) ;
#112549 = CARTESIAN_POINT('Ctrl Pts',(66.6800660661747,246.969077733829,21.3742997769703)) ;
#112550 = CARTESIAN_POINT('Ctrl Pts',(66.6772667991987,246.911637505547,21.4131143461349)) ;
#112551 = CARTESIAN_POINT('Ctrl Pts',(66.6744675322227,246.856396541157,21.4548633645944)) ;
#112552 = CARTESIAN_POINT('Ctrl Pts',(66.6716688672921,246.801167457582,21.4966034039868)) ;
#112553 = CARTESIAN_POINT('Ctrl Pts',(66.6688702023615,246.748137085706,21.541276345894)) ;
#112554 = CARTESIAN_POINT('Ctrl Pts',(66.6660715374309,246.697622033173,21.5886159692403)) ;
#112555 = CARTESIAN_POINT('Ctrl Pts',(66.6631474559198,246.64484324943,21.638077023279)) ;
#112556 = CARTESIAN_POINT('Ctrl Pts',(66.6602233744087,246.5948109811,21.6904490326929)) ;
#112557 = CARTESIAN_POINT('Ctrl Pts',(66.6572992928976,246.54784403798,21.7453847650921)) ;
#112558 = CARTESIAN_POINT('Ctrl Pts',(66.6544973328726,246.502838624615,21.7980261588232)) ;
#112559 = CARTESIAN_POINT('Ctrl Pts',(66.6516953728476,246.460647846571,21.8530209500657)) ;
#112560 = CARTESIAN_POINT('Ctrl Pts',(66.6488934128226,246.421509977807,21.9100309666791)) ;
#112561 = CARTESIAN_POINT('Ctrl Pts',(66.6460896353153,246.382346722391,21.9670779626554)) ;
#112562 = CARTESIAN_POINT('Ctrl Pts',(66.643285857808,246.346240570875,22.0261423714026)) ;
#112563 = CARTESIAN_POINT('Ctrl Pts',(66.6404820803007,246.313384870534,22.0868595920092)) ;
#112564 = CARTESIAN_POINT('Ctrl Pts',(66.6376740088167,246.280478851789,22.1476698008527)) ;
#112565 = CARTESIAN_POINT('Ctrl Pts',(66.6348659373327,246.250833420726,22.2101374322724)) ;
#112566 = CARTESIAN_POINT('Ctrl Pts',(66.6320578658488,246.224594237369,22.2738770077013)) ;
#112567 = CARTESIAN_POINT('Ctrl Pts',(66.6316994303318,246.221244943982,22.2820130283832)) ;
#112568 = CARTESIAN_POINT('Ctrl Pts',(66.6313409948149,246.217951082534,22.2901697529364)) ;
#112569 = CARTESIAN_POINT('Ctrl Pts',(66.6309825592979,246.214712897158,22.2983463632043)) ;
#112570 = CARTESIAN_POINT('Ctrl Pts',(66.6281800443638,246.189394360223,22.3622771716815)) ;
#112571 = CARTESIAN_POINT('Ctrl Pts',(66.6253775294297,246.167391336414,22.4276576817178)) ;
#112572 = CARTESIAN_POINT('Ctrl Pts',(66.6225750144956,246.148867895085,22.4941118138594)) ;
#112573 = CARTESIAN_POINT('Ctrl Pts',(66.619703635649,246.129889292348,22.5621988691624)) ;
#112574 = CARTESIAN_POINT('Ctrl Pts',(66.6168322568023,246.114563812163,22.6314125618807)) ;
#112575 = CARTESIAN_POINT('Ctrl Pts',(66.6139608779556,246.103015479204,22.7013263958668)) ;
#112576 = CARTESIAN_POINT('Ctrl Pts',(66.6111655312091,246.091772938011,22.7693889605107)) ;
#112577 = CARTESIAN_POINT('Ctrl Pts',(66.6083701844626,246.084110072188,22.8381145319354)) ;
#112578 = CARTESIAN_POINT('Ctrl Pts',(66.6055748377161,246.080090340551,22.9070963010212)) ;
#112579 = CARTESIAN_POINT('Ctrl Pts',(66.6027810857162,246.076072902172,22.9760387159777)) ;
#112580 = CARTESIAN_POINT('Ctrl Pts',(66.5999873337162,246.075694501959,23.0452365521402)) ;
#112581 = CARTESIAN_POINT('Ctrl Pts',(66.5971935817163,246.078966771708,23.1142777902697)) ;
#112582 = CARTESIAN_POINT('Ctrl Pts',(66.5944004829009,246.082238276395,23.1833028864261)) ;
#112583 = CARTESIAN_POINT('Ctrl Pts',(66.5916073840854,246.089158732519,23.2521709698612)) ;
#112584 = CARTESIAN_POINT('Ctrl Pts',(66.58881428527,246.099687690267,23.320471704272)) ;
#112585 = CARTESIAN_POINT('Ctrl Pts',(66.5858849216788,246.110730316225,23.3921045743768)) ;
#112586 = CARTESIAN_POINT('Ctrl Pts',(66.5829555580876,246.12574249303,23.4631127389016)) ;
#112587 = CARTESIAN_POINT('Ctrl Pts',(66.5800261944964,246.144616879569,23.5330331974709)) ;
#112588 = CARTESIAN_POINT('Ctrl Pts',(66.5772298638925,246.162634112004,23.5997783153261)) ;
#112589 = CARTESIAN_POINT('Ctrl Pts',(66.5744335332887,246.184170152109,23.6655319101723)) ;
#112590 = CARTESIAN_POINT('Ctrl Pts',(66.5716372026848,246.20908072843,23.729907683838)) ;
#112591 = CARTESIAN_POINT('Ctrl Pts',(66.5688390712557,246.234007347058,23.7943249152326)) ;
#112592 = CARTESIAN_POINT('Ctrl Pts',(66.5660409398266,246.262312626854,23.8573621146967)) ;
#112593 = CARTESIAN_POINT('Ctrl Pts',(66.5632428083975,246.293805132647,23.9186551780761)) ;
#112594 = CARTESIAN_POINT('Ctrl Pts',(66.5604403673259,246.325346142753,23.9800426441668)) ;
#112595 = CARTESIAN_POINT('Ctrl Pts',(66.5576379262542,246.360083924017,24.0396801960135)) ;
#112596 = CARTESIAN_POINT('Ctrl Pts',(66.5548354851826,246.39778291499,24.0972313511934)) ;
#112597 = CARTESIAN_POINT('Ctrl Pts',(66.5544442975136,246.4030452488,24.1052648126169)) ;
#112598 = CARTESIAN_POINT('Ctrl Pts',(66.5540531098447,246.408365216766,24.1132576730071)) ;
#112599 = CARTESIAN_POINT('Ctrl Pts',(66.5536619221757,246.413742116473,24.1212090691728)) ;
#112600 = CARTESIAN_POINT('Ctrl Pts',(66.5508575245513,246.452288742457,24.1782120840603)) ;
#112601 = CARTESIAN_POINT('Ctrl Pts',(66.5480531269269,246.493905844935,24.2332903096945)) ;
#112602 = CARTESIAN_POINT('Ctrl Pts',(66.5452487293026,246.538374695132,24.2860959910081)) ;
#112603 = CARTESIAN_POINT('Ctrl Pts',(66.5423775857922,246.583901923349,24.3401584705568)) ;
#112604 = CARTESIAN_POINT('Ctrl Pts',(66.5395064422818,246.63241817426,24.3918383655865)) ;
#112605 = CARTESIAN_POINT('Ctrl Pts',(66.5366352987714,246.683641153788,24.4407933786813)) ;
#112606 = CARTESIAN_POINT('Ctrl Pts',(66.5338380154614,246.733546421569,24.4884890234926)) ;
#112607 = CARTESIAN_POINT('Ctrl Pts',(66.5310407321513,246.786020452675,24.5335979395467)) ;
#112608 = CARTESIAN_POINT('Ctrl Pts',(66.5282434488413,246.840762508303,24.5758381993054)) ;
#112609 = CARTESIAN_POINT('Ctrl Pts',(66.5254477458841,246.895473636864,24.6180545950115)) ;
#112610 = CARTESIAN_POINT('Ctrl Pts',(66.5226520429269,246.952449861992,24.6574052534587)) ;
#112611 = CARTESIAN_POINT('Ctrl Pts',(66.5198563399697,247.011356947953,24.693648136975)) ;
#112612 = CARTESIAN_POINT('Ctrl Pts',(66.5170612791496,247.070250503714,24.7298826959663)) ;
#112613 = CARTESIAN_POINT('Ctrl Pts',(66.5142662183296,247.131073624387,24.7630106427246)) ;
#112614 = CARTESIAN_POINT('Ctrl Pts',(66.5114711575094,247.193464120806,24.7928339163131)) ;
#112615 = CARTESIAN_POINT('Ctrl Pts',(66.5085436681381,247.258810647016,24.8240702013415)) ;
#112616 = CARTESIAN_POINT('Ctrl Pts',(66.5056161787668,247.325876260209,24.85168059151)) ;
#112617 = CARTESIAN_POINT('Ctrl Pts',(66.5026886893955,247.394219302264,24.875493223085)) ;
#112618 = CARTESIAN_POINT('Ctrl Pts',(66.4998903921052,247.459546319764,24.8982549871627)) ;
#112619 = CARTESIAN_POINT('Ctrl Pts',(66.497092094815,247.526039885201,24.9175470467986)) ;
#112620 = CARTESIAN_POINT('Ctrl Pts',(66.4942937975247,247.593299161412,24.9332705763801)) ;
#112621 = CARTESIAN_POINT('Ctrl Pts',(66.4914936996295,247.66060171658,24.9490042234946)) ;
#112622 = CARTESIAN_POINT('Ctrl Pts',(66.4886936017343,247.728670483708,24.961164685035)) ;
#112623 = CARTESIAN_POINT('Ctrl Pts',(66.4858935038391,247.797096347173,24.9697045982337)) ;
#112624 = CARTESIAN_POINT('Ctrl Pts',(66.4830891103635,247.865627181538,24.9782576123614)) ;
#112625 = CARTESIAN_POINT('Ctrl Pts',(66.4802847168879,247.934515719959,24.9831789660512)) ;
#112626 = CARTESIAN_POINT('Ctrl Pts',(66.4774803234124,248.00335075709,24.9844733128192)) ;
#112627 = CARTESIAN_POINT('Ctrl Pts',(66.4771006439594,248.012670151629,24.984648551022)) ;
#112628 = CARTESIAN_POINT('Ctrl Pts',(66.4767209645065,248.021988571689,24.9847573850635)) ;
#112629 = CARTESIAN_POINT('Ctrl Pts',(66.4763412850535,248.031305004152,24.9847998994865)) ;
#112630 = CARTESIAN_POINT('Ctrl Pts',(66.4735367028759,248.100122793056,24.9851139412185)) ;
#112631 = CARTESIAN_POINT('Ctrl Pts',(66.4707321206983,248.169082326696,24.981806256511)) ;
#112632 = CARTESIAN_POINT('Ctrl Pts',(66.4679275385207,248.237773013919,24.9748614557492)) ;
#112633 = CARTESIAN_POINT('Ctrl Pts',(66.4650564180795,248.30809337671,24.9677518907)) ;
#112634 = CARTESIAN_POINT('Ctrl Pts',(66.4621852976383,248.378131459492,24.9568303286319)) ;
#112635 = CARTESIAN_POINT('Ctrl Pts',(66.4593141771971,248.447445444109,24.9421369469113)) ;
#112636 = CARTESIAN_POINT('Ctrl Pts',(66.4565166884835,248.514981827075,24.9278203864017)) ;
#112637 = CARTESIAN_POINT('Ctrl Pts',(66.45371919977,248.581830299186,24.9099232607873)) ;
#112638 = CARTESIAN_POINT('Ctrl Pts',(66.4509217110564,248.647588407351,24.8885350231841)) ;
#112639 = CARTESIAN_POINT('Ctrl Pts',(66.4481257955151,248.713309536339,24.8671588132905)) ;
#112640 = CARTESIAN_POINT('Ctrl Pts',(66.4453298799738,248.77794105567,24.8422955378968)) ;
#112641 = CARTESIAN_POINT('Ctrl Pts',(66.4425339644325,248.841094575183,24.8140848049847)) ;
#112642 = CARTESIAN_POINT('Ctrl Pts',(66.4397386841844,248.904233744834,24.7858804821683)) ;
#112643 = CARTESIAN_POINT('Ctrl Pts',(66.4369434039363,248.965895137064,24.7543304114707)) ;
#112644 = CARTESIAN_POINT('Ctrl Pts',(66.4341481236882,249.025710924317,24.7196220813791)) ;
#112645 = CARTESIAN_POINT('Ctrl Pts',(66.4312208340418,249.088351561096,24.6832746219824)) ;
#112646 = CARTESIAN_POINT('Ctrl Pts',(66.4282935443954,249.148967429664,24.6434634608389)) ;
#112647 = CARTESIAN_POINT('Ctrl Pts',(66.425366254749,249.20716770085,24.6004563694609)) ;
#112648 = CARTESIAN_POINT('Ctrl Pts',(66.4225677232717,249.262808006586,24.5593409645963)) ;
#112649 = CARTESIAN_POINT('Ctrl Pts',(66.4197691917944,249.316240403472,24.5153052507546)) ;
#112650 = CARTESIAN_POINT('Ctrl Pts',(66.4169706603171,249.367157228193,24.4686245793031)) ;
#112651 = CARTESIAN_POINT('Ctrl Pts',(66.4141703233186,249.418106902789,24.4219137910052)) ;
#112652 = CARTESIAN_POINT('Ctrl Pts',(66.4113699863201,249.466537434248,24.3725549965347)) ;
#112653 = CARTESIAN_POINT('Ctrl Pts',(66.4085696493216,249.51217899423,24.3208594006466)) ;
#112654 = CARTESIAN_POINT('Ctrl Pts',(66.4057650114089,249.557890653073,24.26908440777)) ;
#112655 = CARTESIAN_POINT('Ctrl Pts',(66.4029603734962,249.600804495448,24.214965836329)) ;
#112656 = CARTESIAN_POINT('Ctrl Pts',(66.4001557355835,249.640692473552,24.1588459463071)) ;
#112657 = CARTESIAN_POINT('Ctrl Pts',(66.3997773730328,249.6460736021,24.1512750350546)) ;
#112658 = CARTESIAN_POINT('Ctrl Pts',(66.3993990104821,249.651399728399,24.1436677390925)) ;
#112659 = CARTESIAN_POINT('Ctrl Pts',(66.3990206479314,249.656670356245,24.1360249334639)) ;
#112660 = CARTESIAN_POINT('Ctrl Pts',(66.3961923042638,249.696069463972,24.0788932726709)) ;
#112661 = CARTESIAN_POINT('Ctrl Pts',(66.3933639605962,249.73250654892,24.0195681046214)) ;
#112662 = CARTESIAN_POINT('Ctrl Pts',(66.3905356169286,249.765733822899,23.9583848894514)) ;
#112663 = CARTESIAN_POINT('Ctrl Pts',(66.3877114631021,249.798911874783,23.897292309643)) ;
#112664 = CARTESIAN_POINT('Ctrl Pts',(66.3848873092756,249.828889330847,23.8343475626674)) ;
#112665 = CARTESIAN_POINT('Ctrl Pts',(66.3820631554491,249.855461540977,23.7699151331032)) ;
#112666 = CARTESIAN_POINT('Ctrl Pts',(66.3792426862401,249.881999082872,23.7055667672503)) ;
#112667 = CARTESIAN_POINT('Ctrl Pts',(66.376422217031,249.905140028878,23.6397350147491)) ;
#112668 = CARTESIAN_POINT('Ctrl Pts',(66.3736017478219,249.924726369716,23.5728074261705)) ;
#112669 = CARTESIAN_POINT('Ctrl Pts',(66.3707834643677,249.944297531895,23.505931703891)) ;
#112670 = CARTESIAN_POINT('Ctrl Pts',(66.3679651809134,249.960319426279,23.437962287707)) ;
#112671 = CARTESIAN_POINT('Ctrl Pts',(66.3651468974592,249.972683213614,23.3693038406779)) ;
#112672 = CARTESIAN_POINT('Ctrl Pts',(66.3623295387996,249.985042943883,23.3006679233083)) ;
#112673 = CARTESIAN_POINT('Ctrl Pts',(66.35951218014,249.993746861307,23.2313438912878)) ;
#112674 = CARTESIAN_POINT('Ctrl Pts',(66.3566948214805,249.998737100951,23.1617471999234)) ;
#112675 = CARTESIAN_POINT('Ctrl Pts',(66.3547891772058,250.002112468718,23.1146724208622)) ;
#112676 = CARTESIAN_POINT('Ctrl Pts',(66.3528835329311,250.003789857887,23.067473125536)) ;
#112677 = CARTESIAN_POINT('Ctrl Pts',(66.3509778886564,250.003764831718,23.0202791331489)) ;
#112678 = CARTESIAN_POINT('',(65.8509778886254,250.003764915913,23.0221883796948)) ;
#112679 = CARTESIAN_POINT('Ctrl Pts',(66.3509778886297,250.003764831718,23.0202791324881)) ;
#112680 = CARTESIAN_POINT('Ctrl Pts',(66.3478598655463,250.00372388377,22.9430601259727)) ;
#112681 = CARTESIAN_POINT('Ctrl Pts',(66.3447418424628,249.999123582142,22.8659967115464)) ;
#112682 = CARTESIAN_POINT('Ctrl Pts',(66.3416238193793,249.99004343271,22.7895947867999)) ;
#112683 = CARTESIAN_POINT('Ctrl Pts',(66.3384932790686,249.980926831241,22.7128861483981)) ;
#112684 = CARTESIAN_POINT('Ctrl Pts',(66.3353627387578,249.967294471348,22.6368445763685)) ;
#112685 = CARTESIAN_POINT('Ctrl Pts',(66.332232198447,249.949276702868,22.5619653829443)) ;
#112686 = CARTESIAN_POINT('Ctrl Pts',(66.3290871137584,249.931175224483,22.4867383034769)) ;
#112687 = CARTESIAN_POINT('Ctrl Pts',(66.3259420290698,249.908647624235,22.4126846747573)) ;
#112688 = CARTESIAN_POINT('Ctrl Pts',(66.3227969443812,249.881874367055,22.3402861401784)) ;
#112689 = CARTESIAN_POINT('Ctrl Pts',(66.3224312998572,249.8787617339,22.3318691561106)) ;
#112690 = CARTESIAN_POINT('Ctrl Pts',(66.3220656553331,249.875591767863,22.3234745173636)) ;
#112691 = CARTESIAN_POINT('Ctrl Pts',(66.3217000108091,249.872364793347,22.3151029604768)) ;
#112692 = CARTESIAN_POINT('Ctrl Pts',(66.3188956978973,249.847615492569,22.2508972537666)) ;
#112693 = CARTESIAN_POINT('Ctrl Pts',(66.3160913849855,249.819441896056,22.1878769828483)) ;
#112694 = CARTESIAN_POINT('Ctrl Pts',(66.3132870720737,249.787978979235,22.1264301416105)) ;
#112695 = CARTESIAN_POINT('Ctrl Pts',(66.3104159179742,249.755766139423,22.0635187063797)) ;
#112696 = CARTESIAN_POINT('Ctrl Pts',(66.3075447638748,249.720105261573,22.0022571831292)) ;
#112697 = CARTESIAN_POINT('Ctrl Pts',(66.3046736097753,249.681194506994,21.9430425700643)) ;
#112698 = CARTESIAN_POINT('Ctrl Pts',(66.3018764061595,249.643285951886,21.885353109994)) ;
#112699 = CARTESIAN_POINT('Ctrl Pts',(66.2990792025437,249.602293203379,21.8296068199877)) ;
#112700 = CARTESIAN_POINT('Ctrl Pts',(66.2962819989278,249.558445944019,21.7761459788644)) ;
#112701 = CARTESIAN_POINT('Ctrl Pts',(66.2934863735306,249.514623423853,21.7227153010431)) ;
#112702 = CARTESIAN_POINT('Ctrl Pts',(66.2906907481334,249.467949897479,21.6715678893151)) ;
#112703 = CARTESIAN_POINT('Ctrl Pts',(66.2878951227363,249.418696651158,21.6230146794661)) ;
#112704 = CARTESIAN_POINT('Ctrl Pts',(66.2851001371771,249.369454677485,21.574472582046)) ;
#112705 = CARTESIAN_POINT('Ctrl Pts',(66.2823051516179,249.317634503699,21.528523849089)) ;
#112706 = CARTESIAN_POINT('Ctrl Pts',(66.2795101660587,249.263544535983,21.4854428450103)) ;
#112707 = CARTESIAN_POINT('Ctrl Pts',(66.2765826000278,249.206888804227,21.4403182883889)) ;
#112708 = CARTESIAN_POINT('Ctrl Pts',(66.2736550339968,249.147743009541,21.3983406892389)) ;
#112709 = CARTESIAN_POINT('Ctrl Pts',(66.2707274679658,249.086498940256,21.3597767787396)) ;
#112710 = CARTESIAN_POINT('Ctrl Pts',(66.2679292391154,249.027960577747,21.322916586415)) ;
#112711 = CARTESIAN_POINT('Ctrl Pts',(66.265131010265,248.967505907819,21.2891750088955)) ;
#112712 = CARTESIAN_POINT('Ctrl Pts',(66.2623327814145,248.905503294256,21.2587383935005)) ;
#112713 = CARTESIAN_POINT('Ctrl Pts',(66.259532749504,248.843460728835,21.2282821660402)) ;
#112714 = CARTESIAN_POINT('Ctrl Pts',(66.2567327175935,248.779868682643,21.2011353301055)) ;
#112715 = CARTESIAN_POINT('Ctrl Pts',(66.2539326856829,248.715115147543,21.1774359453826)) ;
#112716 = CARTESIAN_POINT('Ctrl Pts',(66.251128354205,248.65026218065,21.1537001692522)) ;
#112717 = CARTESIAN_POINT('Ctrl Pts',(66.248324022727,248.584244632475,21.1334225449265)) ;
#112718 = CARTESIAN_POINT('Ctrl Pts',(66.2455196912491,248.517464216764,21.116690914933)) ;
#112719 = CARTESIAN_POINT('Ctrl Pts',(66.2451395853951,248.50841263811,21.1144230694384)) ;
#112720 = CARTESIAN_POINT('Ctrl Pts',(66.2447594795411,248.49934705575,21.1122202925466)) ;
#112721 = CARTESIAN_POINT('Ctrl Pts',(66.2443793736871,248.490268479293,21.1100827299615)) ;
#112722 = CARTESIAN_POINT('Ctrl Pts',(66.2415750693281,248.42328952787,21.0943124490994)) ;
#112723 = CARTESIAN_POINT('Ctrl Pts',(66.2387707649692,248.355358414636,21.0820385006588)) ;
#112724 = CARTESIAN_POINT('Ctrl Pts',(66.2359664606102,248.286871667356,21.0733682253655)) ;
#112725 = CARTESIAN_POINT('Ctrl Pts',(66.2330953054417,248.216752288978,21.0644912624774)) ;
#112726 = CARTESIAN_POINT('Ctrl Pts',(66.2302241502731,248.146050924723,21.0593922007215)) ;
#112727 = CARTESIAN_POINT('Ctrl Pts',(66.2273529951046,248.075207175511,21.0581312793319)) ;
#112728 = CARTESIAN_POINT('Ctrl Pts',(66.2245557989252,248.00618831272,21.0569028384131)) ;
#112729 = CARTESIAN_POINT('Ctrl Pts',(66.2217586027458,247.937034832054,21.0593171883096)) ;
#112730 = CARTESIAN_POINT('Ctrl Pts',(66.2189614065664,247.868158918274,21.0653776783642)) ;
#112731 = CARTESIAN_POINT('Ctrl Pts',(66.2161657881682,247.799321854513,21.0714347499501)) ;
#112732 = CARTESIAN_POINT('Ctrl Pts',(66.2133701697701,247.730762531577,21.0811338376834)) ;
#112733 = CARTESIAN_POINT('Ctrl Pts',(66.210574551372,247.662890712547,21.0944262582976)) ;
#112734 = CARTESIAN_POINT('Ctrl Pts',(66.2077795723613,247.595034416518,21.1077156387949)) ;
#112735 = CARTESIAN_POINT('Ctrl Pts',(66.2049845933506,247.527865790172,21.1245966259734)) ;
#112736 = CARTESIAN_POINT('Ctrl Pts',(66.2021896143399,247.461785328639,21.1449692583098)) ;
#112737 = CARTESIAN_POINT('Ctrl Pts',(66.199262041192,247.392570002138,21.1663083707512)) ;
#112738 = CARTESIAN_POINT('Ctrl Pts',(66.1963344680441,247.32454922249,21.1914785334405)) ;
#112739 = CARTESIAN_POINT('Ctrl Pts',(66.1934068948962,247.258164209242,21.2203066194318)) ;
#112740 = CARTESIAN_POINT('Ctrl Pts',(66.190608671379,247.194712300146,21.2478609875378)) ;
#112741 = CARTESIAN_POINT('Ctrl Pts',(66.1878104478619,247.132755087318,21.2787565729174)) ;
#112742 = CARTESIAN_POINT('Ctrl Pts',(66.1850122243447,247.072654192038,21.312794263652)) ;
#112743 = CARTESIAN_POINT('Ctrl Pts',(66.1822121973405,247.012514561043,21.3468538920675)) ;
#112744 = CARTESIAN_POINT('Ctrl Pts',(66.1794121703363,246.954234039149,21.3840593940906)) ;
#112745 = CARTESIAN_POINT('Ctrl Pts',(66.1766121433321,246.898145439722,21.4241682174863)) ;
#112746 = CARTESIAN_POINT('Ctrl Pts',(66.1738078161204,246.841970700905,21.4643386389532)) ;
#112747 = CARTESIAN_POINT('Ctrl Pts',(66.1710034889088,246.787994978288,21.507420971324)) ;
#112748 = CARTESIAN_POINT('Ctrl Pts',(66.1681991616971,246.736517353207,21.5531330113605)) ;
#112749 = CARTESIAN_POINT('Ctrl Pts',(66.1678190199863,246.729539282894,21.559329525458)) ;
#112750 = CARTESIAN_POINT('Ctrl Pts',(66.1674388782756,246.722607058264,21.5655743079229)) ;
#112751 = CARTESIAN_POINT('Ctrl Pts',(66.1670587365648,246.715721369191,21.5718666069575)) ;
#112752 = CARTESIAN_POINT('Ctrl Pts',(66.164254472231,246.664926384755,21.6182842171846)) ;
#112753 = CARTESIAN_POINT('Ctrl Pts',(66.1614502078971,246.616481631369,21.6674598175612)) ;
#112754 = CARTESIAN_POINT('Ctrl Pts',(66.1586459435633,246.570699372434,21.719126502582)) ;
#112755 = CARTESIAN_POINT('Ctrl Pts',(66.1557747833916,246.523824975881,21.7720256984405)) ;
#112756 = CARTESIAN_POINT('Ctrl Pts',(66.1529036232199,246.479742176359,21.8275360775242)) ;
#112757 = CARTESIAN_POINT('Ctrl Pts',(66.1500324630482,246.438748647046,21.8853285847958)) ;
#112758 = CARTESIAN_POINT('Ctrl Pts',(66.1472353088917,246.398811752532,21.9416314527184)) ;
#112759 = CARTESIAN_POINT('Ctrl Pts',(66.1444381547351,246.361807088797,22.0000997932479)) ;
#112760 = CARTESIAN_POINT('Ctrl Pts',(66.1416410005786,246.32796987339,22.0603951226066)) ;
#112761 = CARTESIAN_POINT('Ctrl Pts',(66.1388454248234,246.294151751928,22.1206564280162)) ;
#112762 = CARTESIAN_POINT('Ctrl Pts',(66.1360498490683,246.26349776992,22.1827422520709)) ;
#112763 = CARTESIAN_POINT('Ctrl Pts',(66.1332542733131,246.236198810827,22.2462867661089)) ;
#112764 = CARTESIAN_POINT('Ctrl Pts',(66.1304593374925,246.208906100731,22.3098167341885)) ;
#112765 = CARTESIAN_POINT('Ctrl Pts',(66.1276644016719,246.184967080257,22.3748042812797)) ;
#112766 = CARTESIAN_POINT('Ctrl Pts',(66.1248694658512,246.16452506053,22.4408623131028)) ;
#112767 = CARTESIAN_POINT('Ctrl Pts',(66.1219418519838,246.143112640257,22.5100561774446)) ;
#112768 = CARTESIAN_POINT('Ctrl Pts',(66.1190142381165,246.125537714434,22.5804241505789)) ;
#112769 = CARTESIAN_POINT('Ctrl Pts',(66.1160866242491,246.111906148906,22.6515042058526)) ;
#112770 = CARTESIAN_POINT('Ctrl Pts',(66.1132884447899,246.098877256305,22.7194417002207)) ;
#112771 = CARTESIAN_POINT('Ctrl Pts',(66.1104902653307,246.089450404183,22.7880291263575)) ;
#112772 = CARTESIAN_POINT('Ctrl Pts',(66.1076920858715,246.083665100118,22.8568555753116)) ;
#112773 = CARTESIAN_POINT('Ctrl Pts',(66.1048921031845,246.077876067837,22.9257263780205)) ;
#112774 = CARTESIAN_POINT('Ctrl Pts',(66.1020921204975,246.075733269037,22.9948360232998)) ;
#112775 = CARTESIAN_POINT('Ctrl Pts',(66.0992921378105,246.077224091665,23.0637728938718)) ;
#112776 = CARTESIAN_POINT('Ctrl Pts',(66.0964878549738,246.078717203865,23.1328156361199)) ;
#112777 = CARTESIAN_POINT('Ctrl Pts',(66.0936835721371,246.083855031025,23.2016845896588)) ;
#112778 = CARTESIAN_POINT('Ctrl Pts',(66.0908792893005,246.092573193766,23.2699736324214)) ;
#112779 = CARTESIAN_POINT('Ctrl Pts',(66.0904988926812,246.093755799026,23.279236935202)) ;
#112780 = CARTESIAN_POINT('Ctrl Pts',(66.090118496062,246.095004207766,23.2884895848537)) ;
#112781 = CARTESIAN_POINT('Ctrl Pts',(66.0897380994427,246.096318187715,23.297730585677)) ;
#112782 = CARTESIAN_POINT('Ctrl Pts',(66.0869338127968,246.106004857464,23.3658553110087)) ;
#112783 = CARTESIAN_POINT('Ctrl Pts',(66.084129526151,246.119294572346,23.4335945163826)) ;
#112784 = CARTESIAN_POINT('Ctrl Pts',(66.0813252395051,246.136143011513,23.5005398052726)) ;
#112785 = CARTESIAN_POINT('Ctrl Pts',(66.0784540821224,246.153393216863,23.5690814647762)) ;
#112786 = CARTESIAN_POINT('Ctrl Pts',(66.0755829247397,246.174374068109,23.6367903357114)) ;
#112787 = CARTESIAN_POINT('Ctrl Pts',(66.072711767357,246.198981695181,23.7032350335809)) ;
#112788 = CARTESIAN_POINT('Ctrl Pts',(66.0699145900767,246.222955266182,23.7679676742907)) ;
#112789 = CARTESIAN_POINT('Ctrl Pts',(66.0671174127965,246.25037078009,23.8315000180623)) ;
#112790 = CARTESIAN_POINT('Ctrl Pts',(66.0643202355162,246.281081356968,23.8934469288994)) ;
#112791 = CARTESIAN_POINT('Ctrl Pts',(66.0615246364033,246.311774606937,23.9553588892896)) ;
#112792 = CARTESIAN_POINT('Ctrl Pts',(66.0587290372905,246.345759014471,24.0156867559789)) ;
#112793 = CARTESIAN_POINT('Ctrl Pts',(66.0559334381776,246.382840116105,24.0740665840905)) ;
#112794 = CARTESIAN_POINT('Ctrl Pts',(66.0531384788057,246.419912732153,24.132433052645)) ;
#112795 = CARTESIAN_POINT('Ctrl Pts',(66.0503435194338,246.460080373364,24.1888519568964)) ;
#112796 = CARTESIAN_POINT('Ctrl Pts',(66.0475485600618,246.503104186896,24.242986645497)) ;
#112797 = CARTESIAN_POINT('Ctrl Pts',(66.0446209685834,246.548169654084,24.2996902436343)) ;
#112798 = CARTESIAN_POINT('Ctrl Pts',(66.0416933771049,246.596368790051,24.3538869569526)) ;
#112799 = CARTESIAN_POINT('Ctrl Pts',(66.0387657856265,246.64737976016,24.4052288153768)) ;
#112800 = CARTESIAN_POINT('Ctrl Pts',(66.0359675824079,246.696136241994,24.4543015615391)) ;
#112801 = CARTESIAN_POINT('Ctrl Pts',(66.0331693791894,246.747460835214,24.5007661813184)) ;
#112802 = CARTESIAN_POINT('Ctrl Pts',(66.0303711759709,246.801036481884,24.5443583150971)) ;
#112803 = CARTESIAN_POINT('Ctrl Pts',(66.0275711694751,246.854646654904,24.5879785414393)) ;
#112804 = CARTESIAN_POINT('Ctrl Pts',(66.0247711629794,246.910510374953,24.6287223107252)) ;
#112805 = CARTESIAN_POINT('Ctrl Pts',(66.0219711564836,246.968280606469,24.6663679048587)) ;
#112806 = CARTESIAN_POINT('Ctrl Pts',(66.0191668499349,247.026139557442,24.7040713124466)) ;
#112807 = CARTESIAN_POINT('Ctrl Pts',(66.0163625433862,247.085910438564,24.7386668120072)) ;
#112808 = CARTESIAN_POINT('Ctrl Pts',(66.0135582368375,247.14722155821,24.7699785344481)) ;
#112809 = CARTESIAN_POINT('Ctrl Pts',(66.0131779786652,247.155535219323,24.7742243392991)) ;
#112810 = CARTESIAN_POINT('Ctrl Pts',(66.0127977204928,247.163877171844,24.7784098389931)) ;
#112811 = CARTESIAN_POINT('Ctrl Pts',(66.0124174623205,247.172246463579,24.7825346642229)) ;
#112812 = CARTESIAN_POINT('Ctrl Pts',(66.0096131786355,247.233967341589,24.8129539449549)) ;
#112813 = CARTESIAN_POINT('Ctrl Pts',(66.0068088949506,247.297401774136,24.8401803846579)) ;
#112814 = CARTESIAN_POINT('Ctrl Pts',(66.0040046112657,247.362187508978,24.8640202702962)) ;
#112815 = CARTESIAN_POINT('Ctrl Pts',(66.0011334535129,247.428518196513,24.8884286683639)) ;
#112816 = CARTESIAN_POINT('Ctrl Pts',(65.9982622957601,247.496265043163,24.9092866076992)) ;
#112817 = CARTESIAN_POINT('Ctrl Pts',(65.9953911380073,247.565013228913,24.9264365871594)) ;
#112818 = CARTESIAN_POINT('Ctrl Pts',(65.9925939636882,247.631989924803,24.9431446492891)) ;
#112819 = CARTESIAN_POINT('Ctrl Pts',(65.9897967893692,247.699916471284,24.9563334198154)) ;
#112820 = CARTESIAN_POINT('Ctrl Pts',(65.9869996150501,247.768391987,24.9659069978885)) ;
#112821 = CARTESIAN_POINT('Ctrl Pts',(65.9842040188898,247.836828869002,24.975475174573)) ;
#112822 = CARTESIAN_POINT('Ctrl Pts',(65.9814084227294,247.905813623758,24.9814321391612)) ;
#112823 = CARTESIAN_POINT('Ctrl Pts',(65.978612826569,247.974936035212,24.983733236474)) ;
#112824 = CARTESIAN_POINT('Ctrl Pts',(65.9758178701356,248.044042629119,24.9860338072178)) ;
#112825 = CARTESIAN_POINT('Ctrl Pts',(65.9730229137023,248.113286330197,24.98468015634)) ;
#112826 = CARTESIAN_POINT('Ctrl Pts',(65.9702279572689,248.182254428473,24.9796796780054)) ;
#112827 = CARTESIAN_POINT('Ctrl Pts',(65.9673003629297,248.254495488007,24.9744418961598)) ;
#112828 = CARTESIAN_POINT('Ctrl Pts',(65.9643727685905,248.326433553938,24.9652025381067)) ;
#112829 = CARTESIAN_POINT('Ctrl Pts',(65.9614451742512,248.397599769185,24.95203114266)) ;
#112830 = CARTESIAN_POINT('Ctrl Pts',(65.9586469739006,248.46562057582,24.9394418973321)) ;
#112831 = CARTESIAN_POINT('Ctrl Pts',(65.95584877355,248.532935839477,24.9232610403545)) ;
#112832 = CARTESIAN_POINT('Ctrl Pts',(65.9530505731994,248.599148446129,24.9036013173046)) ;
#112833 = CARTESIAN_POINT('Ctrl Pts',(65.9502505695442,248.665403723597,24.8839289245158)) ;
#112834 = CARTESIAN_POINT('Ctrl Pts',(65.9474505658891,248.730554470939,24.8607733669065)) ;
#112835 = CARTESIAN_POINT('Ctrl Pts',(65.9446505622339,248.794221882277,24.8342961934261)) ;
#112836 = CARTESIAN_POINT('Ctrl Pts',(65.941846258467,248.857987070981,24.8077783575687)) ;
#112837 = CARTESIAN_POINT('Ctrl Pts',(65.9390419547001,248.920263941948,24.7779289420863)) ;
#112838 = CARTESIAN_POINT('Ctrl Pts',(65.9362376509332,248.980697647301,24.7449557135322)) ;
#112839 = CARTESIAN_POINT('Ctrl Pts',(65.9358573756882,248.988892708899,24.7404844067096)) ;
#112840 = CARTESIAN_POINT('Ctrl Pts',(65.9354771004433,248.997053921597,24.7359557225192)) ;
#112841 = CARTESIAN_POINT('Ctrl Pts',(65.9350968251983,249.005180443317,24.7313702391054)) ;
#112842 = CARTESIAN_POINT('Ctrl Pts',(65.9322925440763,249.065108223923,24.6975552991548)) ;
#112843 = CARTESIAN_POINT('Ctrl Pts',(65.9294882629542,249.12336567858,24.6605247010165)) ;
#112844 = CARTESIAN_POINT('Ctrl Pts',(65.9266839818322,249.179588546289,24.6204683518684)) ;
#112845 = CARTESIAN_POINT('Ctrl Pts',(65.923812823759,249.237152226068,24.5794567324075)) ;
#112846 = CARTESIAN_POINT('Ctrl Pts',(65.9209416656859,249.292582536227,24.535273362707)) ;
#112847 = CARTESIAN_POINT('Ctrl Pts',(65.9180705076127,249.345515473325,24.4881719833853)) ;
#112848 = CARTESIAN_POINT('Ctrl Pts',(65.9152733360198,249.397084388795,24.4422843530754)) ;
#112849 = CARTESIAN_POINT('Ctrl Pts',(65.912476164427,249.44628270396,24.3936276378496)) ;
#112850 = CARTESIAN_POINT('Ctrl Pts',(65.9096789928341,249.492805147331,24.3424788062426)) ;
#112851 = CARTESIAN_POINT('Ctrl Pts',(65.9068833994527,249.539301341954,24.2913588336705)) ;
#112852 = CARTESIAN_POINT('Ctrl Pts',(65.9040878060713,249.583124333545,24.237749895005)) ;
#112853 = CARTESIAN_POINT('Ctrl Pts',(65.9012922126899,249.624005905544,24.1819655673543)) ;
#112854 = CARTESIAN_POINT('Ctrl Pts',(65.8984972590836,249.664878121744,24.1261940060159)) ;
#112855 = CARTESIAN_POINT('Ctrl Pts',(65.8957023054772,249.702809967544,24.0682484376347)) ;
#112856 = CARTESIAN_POINT('Ctrl Pts',(65.8929073518708,249.737574802841,24.0084738519221)) ;
#112857 = CARTESIAN_POINT('Ctrl Pts',(65.8899797548879,249.773989513516,23.9458624739065)) ;
#112858 = CARTESIAN_POINT('Ctrl Pts',(65.887052157905,249.806928798476,23.8812446314136)) ;
#112859 = CARTESIAN_POINT('Ctrl Pts',(65.8841245609221,249.836185672244,23.815046729765)) ;
#112860 = CARTESIAN_POINT('Ctrl Pts',(65.8813263634862,249.864149394586,23.7517747699488)) ;
#112861 = CARTESIAN_POINT('Ctrl Pts',(65.8785281660502,249.888749240932,23.6870599811523)) ;
#112862 = CARTESIAN_POINT('Ctrl Pts',(65.8757299686142,249.90985436691,23.6212938864512)) ;
#112863 = CARTESIAN_POINT('Ctrl Pts',(65.8729299679014,249.930973093924,23.5554854092946)) ;
#112864 = CARTESIAN_POINT('Ctrl Pts',(65.8701299671885,249.948592494345,23.488624748837)) ;
#112865 = CARTESIAN_POINT('Ctrl Pts',(65.8673299664757,249.962632350994,23.4211158315783)) ;
#112866 = CARTESIAN_POINT('Ctrl Pts',(65.8645256656697,249.976693769313,23.3535032376927)) ;
#112867 = CARTESIAN_POINT('Ctrl Pts',(65.8617213648638,249.987164606302,23.2852408819655)) ;
#112868 = CARTESIAN_POINT('Ctrl Pts',(65.8589170640578,249.994016322833,23.2167389703612)) ;
#112869 = CARTESIAN_POINT('Ctrl Pts',(65.8585367720639,249.994945485973,23.2074494075246)) ;
#112870 = CARTESIAN_POINT('Ctrl Pts',(65.85815648007,249.995808171389,23.1981554393389)) ;
#112871 = CARTESIAN_POINT('Ctrl Pts',(65.8577761880761,249.996604381633,23.1888580873809)) ;
#112872 = CARTESIAN_POINT('Ctrl Pts',(65.8555100882696,250.001348872468,23.1334566384633)) ;
#112873 = CARTESIAN_POINT('Ctrl Pts',(65.853243988463,250.003740308255,23.0778509121811)) ;
#112874 = CARTESIAN_POINT('Ctrl Pts',(65.8509778886564,250.003764915912,23.0221883804556)) ;
#112875 = CARTESIAN_POINT('',(65.3509778886241,250.003765042575,23.0208142978541)) ;
#112876 = CARTESIAN_POINT('Ctrl Pts',(65.8509778886254,250.003764915913,23.0221883796948)) ;
#112877 = CARTESIAN_POINT('Ctrl Pts',(65.8482056816273,250.00379501938,22.9540942650674)) ;
#112878 = CARTESIAN_POINT('Ctrl Pts',(65.8454334746292,250.000278609981,22.8858688531145)) ;
#112879 = CARTESIAN_POINT('Ctrl Pts',(65.842661267631,249.993201004529,22.8179152472297)) ;
#112880 = CARTESIAN_POINT('Ctrl Pts',(65.839893088671,249.986133682892,22.7500603784575)) ;
#112881 = CARTESIAN_POINT('Ctrl Pts',(65.837124909711,249.975515490756,22.6824770252418)) ;
#112882 = CARTESIAN_POINT('Ctrl Pts',(65.834356730751,249.961383762869,22.6155675085799)) ;
#112883 = CARTESIAN_POINT('Ctrl Pts',(65.8315907501217,249.947263257598,22.5487111276625)) ;
#112884 = CARTESIAN_POINT('Ctrl Pts',(65.8288247694925,249.929634851148,22.4825280095449)) ;
#112885 = CARTESIAN_POINT('Ctrl Pts',(65.8260587888633,249.908587403347,22.4174130245871)) ;
#112886 = CARTESIAN_POINT('Ctrl Pts',(65.8232940214172,249.887549187141,22.3523265996291)) ;
#112887 = CARTESIAN_POINT('Ctrl Pts',(65.8205292539712,249.863095057984,22.288307853408)) ;
#112888 = CARTESIAN_POINT('Ctrl Pts',(65.8177644865251,249.835363955398,22.2257373011925)) ;
#112889 = CARTESIAN_POINT('Ctrl Pts',(65.81499994881,249.807635157054,22.163171948108)) ;
#112890 = CARTESIAN_POINT('Ctrl Pts',(65.8122354110949,249.776630130297,22.1020550060658)) ;
#112891 = CARTESIAN_POINT('Ctrl Pts',(65.8094708733797,249.742535503141,22.0427459973307)) ;
#112892 = CARTESIAN_POINT('Ctrl Pts',(65.8067038695793,249.708410462128,21.9833840824373)) ;
#112893 = CARTESIAN_POINT('Ctrl Pts',(65.803936865779,249.671190568739,21.9258337541972)) ;
#112894 = CARTESIAN_POINT('Ctrl Pts',(65.8011698619786,249.631107292221,21.8704279097408)) ;
#112895 = CARTESIAN_POINT('Ctrl Pts',(65.7984014827221,249.591004090618,21.8149945234684)) ;
#112896 = CARTESIAN_POINT('Ctrl Pts',(65.7956331034655,249.548034986855,21.7617081317784)) ;
#112897 = CARTESIAN_POINT('Ctrl Pts',(65.792864724209,249.502471713444,21.7108684778389)) ;
#112898 = CARTESIAN_POINT('Ctrl Pts',(65.7900918625712,249.456834666917,21.6599465076085)) ;
#112899 = CARTESIAN_POINT('Ctrl Pts',(65.7873190009335,249.408595420747,21.6114795351642)) ;
#112900 = CARTESIAN_POINT('Ctrl Pts',(65.7845461392957,249.358061767697,21.5657296685664)) ;
#112901 = CARTESIAN_POINT('Ctrl Pts',(65.7831826098485,249.333212304215,21.5432325884877)) ;
#112902 = CARTESIAN_POINT('Ctrl Pts',(65.7818190804012,249.307808527302,21.5213919009542)) ;
#112903 = CARTESIAN_POINT('Ctrl Pts',(65.780455550954,249.28188966256,21.5002349695647)) ;
#112904 = CARTESIAN_POINT('Ctrl Pts',(65.7776512670346,249.228583988999,21.4567228601631)) ;
#112905 = CARTESIAN_POINT('Ctrl Pts',(65.7748469831152,249.172891043922,21.415936816227)) ;
#112906 = CARTESIAN_POINT('Ctrl Pts',(65.7720426991958,249.115120278103,21.3781470073459)) ;
#112907 = CARTESIAN_POINT('Ctrl Pts',(65.7691715414723,249.055971851894,21.3394560242798)) ;
#112908 = CARTESIAN_POINT('Ctrl Pts',(65.7663003837488,248.994645572091,21.3039064117778)) ;
#112909 = CARTESIAN_POINT('Ctrl Pts',(65.7634292260253,248.931510250634,21.2717448678083)) ;
#112910 = CARTESIAN_POINT('Ctrl Pts',(65.7606320516086,248.870001785068,21.2404120548264)) ;
#112911 = CARTESIAN_POINT('Ctrl Pts',(65.757834877192,248.80677684992,21.2122950400974)) ;
#112912 = CARTESIAN_POINT('Ctrl Pts',(65.7550377027753,248.742204519056,21.187577364594)) ;
#112913 = CARTESIAN_POINT('Ctrl Pts',(65.7522421065682,248.677668620912,21.1628736351899)) ;
#112914 = CARTESIAN_POINT('Ctrl Pts',(65.7494465103611,248.61178729007,21.1415656127727)) ;
#112915 = CARTESIAN_POINT('Ctrl Pts',(65.746650914154,248.544950213178,21.1237890014219)) ;
#112916 = CARTESIAN_POINT('Ctrl Pts',(65.7438559577247,248.478128432086,21.1060164582841)) ;
#112917 = CARTESIAN_POINT('Ctrl Pts',(65.7410610012954,248.410351810289,21.0917738460281)) ;
#112918 = CARTESIAN_POINT('Ctrl Pts',(65.7382660448661,248.342024162048,21.0811467113372)) ;
#112919 = CARTESIAN_POINT('Ctrl Pts',(65.7353384506133,248.270453947855,21.0700152539309)) ;
#112920 = CARTESIAN_POINT('Ctrl Pts',(65.7324108563604,248.198279672005,21.0628511036595)) ;
#112921 = CARTESIAN_POINT('Ctrl Pts',(65.7294832621075,248.125973825856,21.0596918706711)) ;
#112922 = CARTESIAN_POINT('Ctrl Pts',(65.7266850618879,248.056863758987,21.0566722697024)) ;
#112923 = CARTESIAN_POINT('Ctrl Pts',(65.7238868616682,247.987634016768,21.0573109666162)) ;
#112924 = CARTESIAN_POINT('Ctrl Pts',(65.7210886614485,247.918696892974,21.0615873466574)) ;
#112925 = CARTESIAN_POINT('Ctrl Pts',(65.718288657968,247.849715343617,21.0658664825517)) ;
#112926 = CARTESIAN_POINT('Ctrl Pts',(65.7154886544874,247.781027271794,21.0737879112052)) ;
#112927 = CARTESIAN_POINT('Ctrl Pts',(65.7126886510069,247.713038099466,21.0852793483774)) ;
#112928 = CARTESIAN_POINT('Ctrl Pts',(65.7098843474749,247.644944514076,21.096788433303)) ;
#112929 = CARTESIAN_POINT('Ctrl Pts',(65.7070800439429,247.577552443221,21.1118783550534)) ;
#112930 = CARTESIAN_POINT('Ctrl Pts',(65.7042757404108,247.511254350599,21.1304264097862)) ;
#112931 = CARTESIAN_POINT('Ctrl Pts',(65.7038954648845,247.502264046312,21.1329416051622)) ;
#112932 = CARTESIAN_POINT('Ctrl Pts',(65.7035151893581,247.493293830232,21.135520317389)) ;
#112933 = CARTESIAN_POINT('Ctrl Pts',(65.7031349138318,247.484344652831,21.1381621723581)) ;
#112934 = CARTESIAN_POINT('Ctrl Pts',(65.7003306271379,247.41835024255,21.1576441485133)) ;
#112935 = CARTESIAN_POINT('Ctrl Pts',(65.6975263404441,247.353260760904,21.1806349226197)) ;
#112936 = CARTESIAN_POINT('Ctrl Pts',(65.6947220537502,247.289473831217,21.2070313067662)) ;
#112937 = CARTESIAN_POINT('Ctrl Pts',(65.6918508963735,247.224165846086,21.2340571359106)) ;
#112938 = CARTESIAN_POINT('Ctrl Pts',(65.6889797389968,247.160223851577,21.2646530243647)) ;
#112939 = CARTESIAN_POINT('Ctrl Pts',(65.6861085816201,247.098059562917,21.2986535269004)) ;
#112940 = CARTESIAN_POINT('Ctrl Pts',(65.6833114043199,247.037497039059,21.3317779507521)) ;
#112941 = CARTESIAN_POINT('Ctrl Pts',(65.6805142270196,246.978622167724,21.3681333979727)) ;
#112942 = CARTESIAN_POINT('Ctrl Pts',(65.6777170497193,246.921794657363,21.4075185894613)) ;
#112943 = CARTESIAN_POINT('Ctrl Pts',(65.6749214505969,246.864999209295,21.4468815596785)) ;
#112944 = CARTESIAN_POINT('Ctrl Pts',(65.6721258514745,246.810249229733,21.4892706047607)) ;
#112945 = CARTESIAN_POINT('Ctrl Pts',(65.6693302523521,246.757876547301,21.5344404459424)) ;
#112946 = CARTESIAN_POINT('Ctrl Pts',(65.666535292981,246.705515849955,21.5795999503536)) ;
#112947 = CARTESIAN_POINT('Ctrl Pts',(65.6637403336099,246.655531737995,21.6275386685267)) ;
#112948 = CARTESIAN_POINT('Ctrl Pts',(65.6609453742388,246.608222586651,21.677971368921)) ;
#112949 = CARTESIAN_POINT('Ctrl Pts',(65.658017782778,246.558668425356,21.7307973042619)) ;
#112950 = CARTESIAN_POINT('Ctrl Pts',(65.6550901913172,246.512049849452,21.7863594212012)) ;
#112951 = CARTESIAN_POINT('Ctrl Pts',(65.6521625998565,246.468664376074,21.84428874242)) ;
#112952 = CARTESIAN_POINT('Ctrl Pts',(65.6493643966647,246.42719637355,21.8996578107149)) ;
#112953 = CARTESIAN_POINT('Ctrl Pts',(65.646566193473,246.388681951787,21.9571887948497)) ;
#112954 = CARTESIAN_POINT('Ctrl Pts',(65.6437679902812,246.353336598711,22.0165295915777)) ;
#112955 = CARTESIAN_POINT('Ctrl Pts',(65.6409679838212,246.317968467748,22.075908629766)) ;
#112956 = CARTESIAN_POINT('Ctrl Pts',(65.6381679773612,246.285773696671,22.1370993706835)) ;
#112957 = CARTESIAN_POINT('Ctrl Pts',(65.6353679709011,246.256921228817,22.1997262470955)) ;
#112958 = CARTESIAN_POINT('Ctrl Pts',(65.6325636644005,246.2280244515,22.2624493011828)) ;
#112959 = CARTESIAN_POINT('Ctrl Pts',(65.6297593578998,246.202480394273,22.3266124378093)) ;
#112960 = CARTESIAN_POINT('Ctrl Pts',(65.6269550513992,246.180409055626,22.3918223568706)) ;
#112961 = CARTESIAN_POINT('Ctrl Pts',(65.6265747931693,246.177416227217,22.400664688615)) ;
#112962 = CARTESIAN_POINT('Ctrl Pts',(65.6261945349395,246.174487174627,22.4095262496064)) ;
#112963 = CARTESIAN_POINT('Ctrl Pts',(65.6258142767096,246.171622124897,22.4184060440952)) ;
#112964 = CARTESIAN_POINT('Ctrl Pts',(65.6230100136664,246.150493448529,22.4838912264291)) ;
#112965 = CARTESIAN_POINT('Ctrl Pts',(65.6202057506231,246.13277264757,22.5506078742004)) ;
#112966 = CARTESIAN_POINT('Ctrl Pts',(65.6174014875799,246.118598747863,22.6181694398748)) ;
#112967 = CARTESIAN_POINT('Ctrl Pts',(65.6145303272469,246.104086721718,22.6873427251233)) ;
#112968 = CARTESIAN_POINT('Ctrl Pts',(65.6116591669139,246.093293244499,22.7574012971836)) ;
#112969 = CARTESIAN_POINT('Ctrl Pts',(65.6087880065809,246.086313879054,22.8279118490807)) ;
#112970 = CARTESIAN_POINT('Ctrl Pts',(65.6059908529616,246.079514412967,22.8966049287275)) ;
#112971 = CARTESIAN_POINT('Ctrl Pts',(65.6031936993423,246.076334850784,22.9657264507413)) ;
#112972 = CARTESIAN_POINT('Ctrl Pts',(65.6003965457231,246.076811831283,23.034865859025)) ;
#112973 = CARTESIAN_POINT('Ctrl Pts',(65.5976009702251,246.077288542675,23.1039662596639)) ;
#112974 = CARTESIAN_POINT('Ctrl Pts',(65.5948053947272,246.081417699443,23.1730840400311)) ;
#112975 = CARTESIAN_POINT('Ctrl Pts',(65.5920098192293,246.089183882217,23.2418068538744)) ;
#112976 = CARTESIAN_POINT('Ctrl Pts',(65.5892148833862,246.096948288012,23.310513943269)) ;
#112977 = CARTESIAN_POINT('Ctrl Pts',(65.5864199475432,246.108348011975,23.3788257615127)) ;
#112978 = CARTESIAN_POINT('Ctrl Pts',(65.5836250117002,246.123315775349,23.44633505727)) ;
#112979 = CARTESIAN_POINT('Ctrl Pts',(65.5806973973574,246.138994073956,23.5170490892284)) ;
#112980 = CARTESIAN_POINT('Ctrl Pts',(65.5777697830147,246.158587523414,23.5868819323492)) ;
#112981 = CARTESIAN_POINT('Ctrl Pts',(65.574842168672,246.181959195878,23.6553797948474)) ;
#112982 = CARTESIAN_POINT('Ctrl Pts',(65.5720439884921,246.204297572112,23.7208492654699)) ;
#112983 = CARTESIAN_POINT('Ctrl Pts',(65.5692458083123,246.230086890269,23.7850988572933)) ;
#112984 = CARTESIAN_POINT('Ctrl Pts',(65.5664476281324,246.25915790344,23.8477520567871)) ;
#112985 = CARTESIAN_POINT('Ctrl Pts',(65.5636476444843,246.288247653306,23.9104456371874)) ;
#112986 = CARTESIAN_POINT('Ctrl Pts',(65.5608476608363,246.320623079513,23.9715403472528)) ;
#112987 = CARTESIAN_POINT('Ctrl Pts',(65.5580476771882,246.356069309894,24.0306848784831)) ;
#112988 = CARTESIAN_POINT('Ctrl Pts',(65.5552433930587,246.39156998197,24.0899202495158)) ;
#112989 = CARTESIAN_POINT('Ctrl Pts',(65.5524391089292,246.430150593162,24.1471990646923)) ;
#112990 = CARTESIAN_POINT('Ctrl Pts',(65.5496348247996,246.471554025327,24.2022004347507)) ;
#112991 = CARTESIAN_POINT('Ctrl Pts',(65.5492544297289,246.47717031126,24.2096612515182)) ;
#112992 = CARTESIAN_POINT('Ctrl Pts',(65.5488740346582,246.48283848028,24.2170802156454)) ;
#112993 = CARTESIAN_POINT('Ctrl Pts',(65.5484936395874,246.488557837358,24.2244565772841)) ;
#112994 = CARTESIAN_POINT('Ctrl Pts',(65.5456893322833,246.530721461607,24.278835790927)) ;
#112995 = CARTESIAN_POINT('Ctrl Pts',(65.5428850249792,246.575823976354,24.3310951424919)) ;
#112996 = CARTESIAN_POINT('Ctrl Pts',(65.5400807176752,246.623624558968,24.3809018252824)) ;
#112997 = CARTESIAN_POINT('Ctrl Pts',(65.5372095628748,246.672564584918,24.4318957716942)) ;
#112998 = CARTESIAN_POINT('Ctrl Pts',(65.5343384080743,246.724332718666,24.4803181537042)) ;
#112999 = CARTESIAN_POINT('Ctrl Pts',(65.5314672532739,246.778625028474,24.5258457040215)) ;
#113000 = CARTESIAN_POINT('Ctrl Pts',(65.5286700558685,246.831518835561,24.5702005209769)) ;
#113001 = CARTESIAN_POINT('Ctrl Pts',(65.5258728584631,246.886807944199,24.6118075140883)) ;
#113002 = CARTESIAN_POINT('Ctrl Pts',(65.5230756610576,246.944173965852,24.6504048897309)) ;
#113003 = CARTESIAN_POINT('Ctrl Pts',(65.5202800420725,247.001507616642,24.6889804854009)) ;
#113004 = CARTESIAN_POINT('Ctrl Pts',(65.5174844230875,247.06091545103,24.7245495622436)) ;
#113005 = CARTESIAN_POINT('Ctrl Pts',(65.5146888041024,247.122048244245,24.7568923073538)) ;
#113006 = CARTESIAN_POINT('Ctrl Pts',(65.5118938251428,247.183167041794,24.7892276479561)) ;
#113007 = CARTESIAN_POINT('Ctrl Pts',(65.5090988461833,247.246009583031,24.8183378962652)) ;
#113008 = CARTESIAN_POINT('Ctrl Pts',(65.5063038672238,247.310201604617,24.8440489386447)) ;
#113009 = CARTESIAN_POINT('Ctrl Pts',(65.5033762951605,247.377438879672,24.8709797064522)) ;
#113010 = CARTESIAN_POINT('Ctrl Pts',(65.5004487230973,247.446156338146,24.8941804696778)) ;
#113011 = CARTESIAN_POINT('Ctrl Pts',(65.4975211510341,247.515902043533,24.9135083962772)) ;
#113012 = CARTESIAN_POINT('Ctrl Pts',(65.4947229291615,247.582566144064,24.9319823486838)) ;
#113013 = CARTESIAN_POINT('Ctrl Pts',(65.4919247072889,247.650169032401,24.9469184298479)) ;
#113014 = CARTESIAN_POINT('Ctrl Pts',(65.4891264854162,247.718304323777,24.9582440652276)) ;
#113015 = CARTESIAN_POINT('Ctrl Pts',(65.4863264606051,247.786483515794,24.9695769978927)) ;
#113016 = CARTESIAN_POINT('Ctrl Pts',(65.483526435794,247.855195309575,24.9772948007758)) ;
#113017 = CARTESIAN_POINT('Ctrl Pts',(65.480726410983,247.924028403685,24.9813767913742)) ;
#113018 = CARTESIAN_POINT('Ctrl Pts',(65.4779220867216,247.992967191311,24.9854650498871)) ;
#113019 = CARTESIAN_POINT('Ctrl Pts',(65.4751177624602,248.062027164623,24.9859063585679)) ;
#113020 = CARTESIAN_POINT('Ctrl Pts',(65.4723134381988,248.130798317154,24.9827320769806)) ;
#113021 = CARTESIAN_POINT('Ctrl Pts',(65.4719332929543,248.14012071505,24.982301781502)) ;
#113022 = CARTESIAN_POINT('Ctrl Pts',(65.4715531477098,248.149437816945,24.9818051247629)) ;
#113023 = CARTESIAN_POINT('Ctrl Pts',(65.4711730024652,248.158748613648,24.9812422575242)) ;
#113024 = CARTESIAN_POINT('Ctrl Pts',(65.4683686909079,248.227433873243,24.9770900153864)) ;
#113025 = CARTESIAN_POINT('Ctrl Pts',(65.4655643793505,248.296025884377,24.9693152890749)) ;
#113026 = CARTESIAN_POINT('Ctrl Pts',(65.4627600677932,248.364113998153,24.9579292731601)) ;
#113027 = CARTESIAN_POINT('Ctrl Pts',(65.4598889135244,248.433825039354,24.9462718636571)) ;
#113028 = CARTESIAN_POINT('Ctrl Pts',(65.4570177592556,248.503007334162,24.930828737252)) ;
#113029 = CARTESIAN_POINT('Ctrl Pts',(65.4541466049869,248.571222524517,24.9116685843919)) ;
#113030 = CARTESIAN_POINT('Ctrl Pts',(65.4513494019349,248.637680722439,24.8930019322235)) ;
#113031 = CARTESIAN_POINT('Ctrl Pts',(65.4485521988829,248.7032205353,24.8708075687884)) ;
#113032 = CARTESIAN_POINT('Ctrl Pts',(65.4457549958309,248.7674462161,24.8452007907684)) ;
#113033 = CARTESIAN_POINT('Ctrl Pts',(65.4429593707037,248.831635666677,24.819608457738)) ;
#113034 = CARTESIAN_POINT('Ctrl Pts',(65.4401637455764,248.894512004406,24.7906077103815)) ;
#113035 = CARTESIAN_POINT('Ctrl Pts',(65.4373681204492,248.955696761178,24.7583629849385)) ;
#113036 = CARTESIAN_POINT('Ctrl Pts',(65.4345731348665,249.016867520945,24.7261256359989)) ;
#113037 = CARTESIAN_POINT('Ctrl Pts',(65.4317781492838,249.07634703746,24.6906460103184)) ;
#113038 = CARTESIAN_POINT('Ctrl Pts',(65.4289831637011,249.133780461819,24.6521349928972)) ;
#113039 = CARTESIAN_POINT('Ctrl Pts',(65.4260555971713,249.193938257225,24.6117971942588)) ;
#113040 = CARTESIAN_POINT('Ctrl Pts',(65.4231280306415,249.251850509562,24.5681335429293)) ;
#113041 = CARTESIAN_POINT('Ctrl Pts',(65.4202004641116,249.307144404721,24.5214367047118)) ;
#113042 = CARTESIAN_POINT('Ctrl Pts',(65.4174022345049,249.359995471616,24.4768028854939)) ;
#113043 = CARTESIAN_POINT('Ctrl Pts',(65.4146040048982,249.410454327204,24.4293986304115)) ;
#113044 = CARTESIAN_POINT('Ctrl Pts',(65.4118057752914,249.458231860769,24.3795186123828)) ;
#113045 = CARTESIAN_POINT('Ctrl Pts',(65.4090057423723,249.506040184452,24.3296064492953)) ;
#113046 = CARTESIAN_POINT('Ctrl Pts',(65.4062057094532,249.551163429357,24.277215716978)) ;
#113047 = CARTESIAN_POINT('Ctrl Pts',(65.403405676534,249.593352565439,24.2226744124676)) ;
#113048 = CARTESIAN_POINT('Ctrl Pts',(65.4006013436993,249.635606489946,24.1680493507246)) ;
#113049 = CARTESIAN_POINT('Ctrl Pts',(65.3977970108645,249.674917042458,24.1112675297942)) ;
#113050 = CARTESIAN_POINT('Ctrl Pts',(65.3949926780297,249.711078900409,24.0526852258304)) ;
#113051 = CARTESIAN_POINT('Ctrl Pts',(65.3946125738008,249.715980342549,24.0447448768113)) ;
#113052 = CARTESIAN_POINT('Ctrl Pts',(65.394232469572,249.720824008609,24.0367714845135)) ;
#113053 = CARTESIAN_POINT('Ctrl Pts',(65.3938523653431,249.725609454111,24.0287659670596)) ;
#113054 = CARTESIAN_POINT('Ctrl Pts',(65.3909709021382,249.761886569934,23.9680783918435)) ;
#113055 = CARTESIAN_POINT('Ctrl Pts',(65.3880894389332,249.794939945734,23.9053322650928)) ;
#113056 = CARTESIAN_POINT('Ctrl Pts',(65.3852079757282,249.824539173868,23.8408923703566)) ;
#113057 = CARTESIAN_POINT('Ctrl Pts',(65.3823327770366,249.854074051099,23.776592572699)) ;
#113058 = CARTESIAN_POINT('Ctrl Pts',(65.3794575783449,249.880169538016,23.710606740984)) ;
#113059 = CARTESIAN_POINT('Ctrl Pts',(65.3765823796533,249.90264063787,23.6433248732417)) ;
#113060 = CARTESIAN_POINT('Ctrl Pts',(65.3737108851966,249.925082787295,23.5761296874564)) ;
#113061 = CARTESIAN_POINT('Ctrl Pts',(65.3708393907399,249.943909684919,23.5076422072702)) ;
#113062 = CARTESIAN_POINT('Ctrl Pts',(65.3679678962833,249.958984224268,23.4382726214603)) ;
#113063 = CARTESIAN_POINT('Ctrl Pts',(65.3650999636564,249.974040065011,23.3689890823635)) ;
#113064 = CARTESIAN_POINT('Ctrl Pts',(65.3622320310296,249.985352710673,23.2988260522388)) ;
#113065 = CARTESIAN_POINT('Ctrl Pts',(65.3593640984028,249.992835185236,23.2282076139426)) ;
#113066 = CARTESIAN_POINT('Ctrl Pts',(65.356568695154,250.000128429683,23.1593751002392)) ;
#113067 = CARTESIAN_POINT('Ctrl Pts',(65.3537732919052,250.00378290197,23.0901103612602)) ;
#113068 = CARTESIAN_POINT('Ctrl Pts',(65.3509778886564,250.003765042576,23.0208142986557)) ;
#113069 = CARTESIAN_POINT('',(64.9402651077866,248.893109917435,24.7899322231574)) ;
#113070 = CARTESIAN_POINT('Ctrl Pts',(65.3509778886241,250.003765042575,23.0208142978541)) ;
#113071 = CARTESIAN_POINT('Ctrl Pts',(65.3479806653745,250.003745893754,22.946515260666)) ;
#113072 = CARTESIAN_POINT('Ctrl Pts',(65.344983442125,249.999505258812,22.8723256198793)) ;
#113073 = CARTESIAN_POINT('Ctrl Pts',(65.3419862188755,249.99110566956,22.7987145203243)) ;
#113074 = CARTESIAN_POINT('Ctrl Pts',(65.338982572516,249.982688079818,22.7249456706965)) ;
#113075 = CARTESIAN_POINT('Ctrl Pts',(65.3359789261565,249.970093813032,22.6517582009852)) ;
#113076 = CARTESIAN_POINT('Ctrl Pts',(65.332975279797,249.953436469231,22.579610493379)) ;
#113077 = CARTESIAN_POINT('Ctrl Pts',(65.3299608740215,249.936719456857,22.5072043441616)) ;
#113078 = CARTESIAN_POINT('Ctrl Pts',(65.3269464682459,249.915910352595,22.4358457658401)) ;
#113079 = CARTESIAN_POINT('Ctrl Pts',(65.3239320624703,249.891172956104,22.3659789157249)) ;
#113080 = CARTESIAN_POINT('Ctrl Pts',(65.3214652843872,249.870929607317,22.3088047900646)) ;
#113081 = CARTESIAN_POINT('Ctrl Pts',(65.318998506304,249.84805658175,22.2526293393555)) ;
#113082 = CARTESIAN_POINT('Ctrl Pts',(65.3165317282209,249.822666742645,22.1976840997892)) ;
#113083 = CARTESIAN_POINT('Ctrl Pts',(65.3137271110147,249.793799622371,22.1352138008449)) ;
#113084 = CARTESIAN_POINT('Ctrl Pts',(65.3109224938086,249.761591747449,22.0741490767129)) ;
#113085 = CARTESIAN_POINT('Ctrl Pts',(65.3081178766025,249.726203045599,22.0148683974425)) ;
#113086 = CARTESIAN_POINT('Ctrl Pts',(65.3052467605398,249.689975260183,21.954182144044)) ;
#113087 = CARTESIAN_POINT('Ctrl Pts',(65.3023756444771,249.650414014378,21.8953661231801)) ;
#113088 = CARTESIAN_POINT('Ctrl Pts',(65.2995045284145,249.607742790949,21.8388035518035)) ;
#113089 = CARTESIAN_POINT('Ctrl Pts',(65.2967070251196,249.566165618334,21.7836911925892)) ;
#113090 = CARTESIAN_POINT('Ctrl Pts',(65.2939095218248,249.521636347261,21.7307185271669)) ;
#113091 = CARTESIAN_POINT('Ctrl Pts',(65.2911120185299,249.474406437266,21.6802122580281)) ;
#113092 = CARTESIAN_POINT('Ctrl Pts',(65.288316096009,249.427203215285,21.6297345282628)) ;
#113093 = CARTESIAN_POINT('Ctrl Pts',(65.285520173488,249.377302715022,21.581720784283)) ;
#113094 = CARTESIAN_POINT('Ctrl Pts',(65.2827242509671,249.324995877752,21.5364637515943)) ;
#113095 = CARTESIAN_POINT('Ctrl Pts',(65.2799289713297,249.272701067712,21.4912171251316)) ;
#113096 = CARTESIAN_POINT('Ctrl Pts',(65.2771336916922,249.218001388152,21.4487262694942)) ;
#113097 = CARTESIAN_POINT('Ctrl Pts',(65.2743384120548,249.161222449624,21.4092450079194)) ;
#113098 = CARTESIAN_POINT('Ctrl Pts',(65.2714111353085,249.101762328279,21.3678993846132)) ;
#113099 = CARTESIAN_POINT('Ctrl Pts',(65.2684838585621,249.040022161171,21.3298549998709)) ;
#113100 = CARTESIAN_POINT('Ctrl Pts',(65.2655565818158,248.976410028725,21.2953525173818)) ;
#113101 = CARTESIAN_POINT('Ctrl Pts',(65.2627580699,248.915596062002,21.2623677275113)) ;
#113102 = CARTESIAN_POINT('Ctrl Pts',(65.2599595579842,248.853071848854,21.2326199409251)) ;
#113103 = CARTESIAN_POINT('Ctrl Pts',(65.2571610460684,248.789217120396,21.2062712718244)) ;
#113104 = CARTESIAN_POINT('Ctrl Pts',(65.2543607351569,248.725321343559,21.1799056647423)) ;
#113105 = CARTESIAN_POINT('Ctrl Pts',(65.2515604242454,248.660093808458,21.1569436855658)) ;
#113106 = CARTESIAN_POINT('Ctrl Pts',(65.2487601133339,248.593930706755,21.137497991394)) ;
#113107 = CARTESIAN_POINT('Ctrl Pts',(65.2459555105135,248.527666199883,21.1180224936936)) ;
#113108 = CARTESIAN_POINT('Ctrl Pts',(65.2431509076932,248.460463739478,21.1020741416983)) ;
#113109 = CARTESIAN_POINT('Ctrl Pts',(65.2403463048729,248.392729959331,21.0897145922673)) ;
#113110 = CARTESIAN_POINT('Ctrl Pts',(65.2399679002815,248.383591134676,21.0880470084589)) ;
#113111 = CARTESIAN_POINT('Ctrl Pts',(65.2395894956901,248.374442644214,21.0864446783139)) ;
#113112 = CARTESIAN_POINT('Ctrl Pts',(65.2392110910987,248.365285491174,21.0849076808294)) ;
#113113 = CARTESIAN_POINT('Ctrl Pts',(65.2364067177151,248.297421419652,21.0735169235961)) ;
#113114 = CARTESIAN_POINT('Ctrl Pts',(65.2336023443314,248.228834175757,21.0656772442728)) ;
#113115 = CARTESIAN_POINT('Ctrl Pts',(65.2307979709478,248.159926453501,21.0614699889811)) ;
#113116 = CARTESIAN_POINT('Ctrl Pts',(65.2279268244073,248.089378013155,21.0571625574008)) ;
#113117 = CARTESIAN_POINT('Ctrl Pts',(65.2250556778669,248.018494129241,21.056662923935)) ;
#113118 = CARTESIAN_POINT('Ctrl Pts',(65.2221845313264,247.947717379197,21.060002631425)) ;
#113119 = CARTESIAN_POINT('Ctrl Pts',(65.2193872581074,247.878761683402,21.063256409729)) ;
#113120 = CARTESIAN_POINT('Ctrl Pts',(65.2165899848883,247.809908193841,21.0701543074036)) ;
#113121 = CARTESIAN_POINT('Ctrl Pts',(65.2137927116693,247.741568468735,21.0806728825766)) ;
#113122 = CARTESIAN_POINT('Ctrl Pts',(65.210997013543,247.673267224463,21.0911855349348)) ;
#113123 = CARTESIAN_POINT('Ctrl Pts',(65.2082013154167,247.60547965136,21.1053147449279)) ;
#113124 = CARTESIAN_POINT('Ctrl Pts',(65.2054056172904,247.538611509456,21.1229853053531)) ;
#113125 = CARTESIAN_POINT('Ctrl Pts',(65.2026105560488,247.471758600705,21.1406518402685)) ;
#113126 = CARTESIAN_POINT('Ctrl Pts',(65.1998154948073,247.405825178078,21.16185799854)) ;
#113127 = CARTESIAN_POINT('Ctrl Pts',(65.1970204335657,247.341204421173,21.1864780052558)) ;
#113128 = CARTESIAN_POINT('Ctrl Pts',(65.1940929352666,247.273521769676,21.2122645700411)) ;
#113129 = CARTESIAN_POINT('Ctrl Pts',(65.1911654369675,247.207279828497,21.241796374246)) ;
#113130 = CARTESIAN_POINT('Ctrl Pts',(65.1882379386684,247.142907594777,21.274872020864)) ;
#113131 = CARTESIAN_POINT('Ctrl Pts',(65.1854396278421,247.081376041167,21.3064880733985)) ;
#113132 = CARTESIAN_POINT('Ctrl Pts',(65.1826413170157,247.021553062989,21.3413414715165)) ;
#113133 = CARTESIAN_POINT('Ctrl Pts',(65.1798430061894,246.963786608865,21.3792100271189)) ;
#113134 = CARTESIAN_POINT('Ctrl Pts',(65.1770428902427,246.905982891044,21.4171030107807)) ;
#113135 = CARTESIAN_POINT('Ctrl Pts',(65.1742427742959,246.850238730028,21.4580147346589)) ;
#113136 = CARTESIAN_POINT('Ctrl Pts',(65.1714426583492,246.796870506239,21.5016815329066)) ;
#113137 = CARTESIAN_POINT('Ctrl Pts',(65.1686382405898,246.743420292952,21.5454154163703)) ;
#113138 = CARTESIAN_POINT('Ctrl Pts',(65.1658338228304,246.692353656227,21.5919124885469)) ;
#113139 = CARTESIAN_POINT('Ctrl Pts',(65.1630294050711,246.643950741133,21.640871706529)) ;
#113140 = CARTESIAN_POINT('Ctrl Pts',(65.1626497547062,246.637398156621,21.6474996010029)) ;
#113141 = CARTESIAN_POINT('Ctrl Pts',(65.1622701043414,246.630894328402,21.6541725690334)) ;
#113142 = CARTESIAN_POINT('Ctrl Pts',(65.1618904539765,246.624439893596,21.6608898187387)) ;
#113143 = CARTESIAN_POINT('Ctrl Pts',(65.159088027919,246.576795855917,21.7104738501322)) ;
#113144 = CARTESIAN_POINT('Ctrl Pts',(65.1562856018614,246.531672008957,21.7626549423151)) ;
#113145 = CARTESIAN_POINT('Ctrl Pts',(65.1534831758038,246.489362512684,21.8171470211069)) ;
#113146 = CARTESIAN_POINT('Ctrl Pts',(65.1506117858476,246.446011837179,21.8729800759395)) ;
#113147 = CARTESIAN_POINT('Ctrl Pts',(65.1477403958914,246.405616285875,21.9312390567331)) ;
#113148 = CARTESIAN_POINT('Ctrl Pts',(65.1448690059351,246.368452042583,21.9915760427659)) ;
#113149 = CARTESIAN_POINT('Ctrl Pts',(65.1420736961978,246.332272501406,22.0503143427368)) ;
#113150 = CARTESIAN_POINT('Ctrl Pts',(65.1392783864604,246.299155428829,22.1110214496346)) ;
#113151 = CARTESIAN_POINT('Ctrl Pts',(65.136483076723,246.269313470916,22.1733447838484)) ;
#113152 = CARTESIAN_POINT('Ctrl Pts',(65.1336893424598,246.239488332333,22.2356329917911)) ;
#113153 = CARTESIAN_POINT('Ctrl Pts',(65.1308956081967,246.212934855869,22.299535179937)) ;
#113154 = CARTESIAN_POINT('Ctrl Pts',(65.1281018739335,246.189819680115,22.3646743436401)) ;
#113155 = CARTESIAN_POINT('Ctrl Pts',(65.1253087736113,246.166709749546,22.4297987262746)) ;
#113156 = CARTESIAN_POINT('Ctrl Pts',(65.122515673289,246.147036733082,22.4961590670286)) ;
#113157 = CARTESIAN_POINT('Ctrl Pts',(65.1197225729667,246.130918419439,22.5633602211707)) ;
#113158 = CARTESIAN_POINT('Ctrl Pts',(65.116793176624,246.114013574075,22.6338406165929)) ;
#113159 = CARTESIAN_POINT('Ctrl Pts',(65.1138637802813,246.101019404348,22.7052454260632)) ;
#113160 = CARTESIAN_POINT('Ctrl Pts',(65.1109343839386,246.092011701315,22.7771054501234)) ;
#113161 = CARTESIAN_POINT('Ctrl Pts',(65.1081380037395,246.083413014264,22.8457025004649)) ;
#113162 = CARTESIAN_POINT('Ctrl Pts',(65.1053416235404,246.078446591114,22.9147138070442)) ;
#113163 = CARTESIAN_POINT('Ctrl Pts',(65.1025452433413,246.07712501953,22.9837272074345)) ;
#113164 = CARTESIAN_POINT('Ctrl Pts',(65.0997470457728,246.075802589056,23.0527854596817)) ;
#113165 = CARTESIAN_POINT('Ctrl Pts',(65.0969488482042,246.078129707593,23.1218453209855)) ;
#113166 = CARTESIAN_POINT('Ctrl Pts',(65.0941506506357,246.084066908575,23.1904973378721)) ;
#113167 = CARTESIAN_POINT('Ctrl Pts',(65.0913481205674,246.090013302233,23.2592556499141)) ;
#113168 = CARTESIAN_POINT('Ctrl Pts',(65.0885455904991,246.099580858384,23.3276043760247)) ;
#113169 = CARTESIAN_POINT('Ctrl Pts',(65.0857430604308,246.11267881539,23.3951429423531)) ;
#113170 = CARTESIAN_POINT('Ctrl Pts',(65.0853519792387,246.114506579773,23.4045676630132)) ;
#113171 = CARTESIAN_POINT('Ctrl Pts',(65.0849608980465,246.116403012254,23.4139766312272)) ;
#113172 = CARTESIAN_POINT('Ctrl Pts',(65.0845698168544,246.118367789474,23.4233687832602)) ;
#113173 = CARTESIAN_POINT('Ctrl Pts',(65.0817617749785,246.132475286387,23.4908063301007)) ;
#113174 = CARTESIAN_POINT('Ctrl Pts',(65.0789537331027,246.150161857754,23.5576217390252)) ;
#113175 = CARTESIAN_POINT('Ctrl Pts',(65.0761456912268,246.171356111447,23.6234095507392)) ;
#113176 = CARTESIAN_POINT('Ctrl Pts',(65.0732750032479,246.193023199043,23.6906650578138)) ;
#113177 = CARTESIAN_POINT('Ctrl Pts',(65.0704043152689,246.218356349094,23.7568460451602)) ;
#113178 = CARTESIAN_POINT('Ctrl Pts',(65.06753362729,246.247223855661,23.8215298899763)) ;
#113179 = CARTESIAN_POINT('Ctrl Pts',(65.0647327104559,246.275389746797,23.8846416148205)) ;
#113180 = CARTESIAN_POINT('Ctrl Pts',(65.0619317936218,246.306919924558,23.9463276777269)) ;
#113181 = CARTESIAN_POINT('Ctrl Pts',(65.0591308767876,246.341642271617,24.0062125764685)) ;
#113182 = CARTESIAN_POINT('Ctrl Pts',(65.0563315545494,246.376344850823,24.0660633820118)) ;
#113183 = CARTESIAN_POINT('Ctrl Pts',(65.0535322323112,246.414235749193,24.1241146389114)) ;
#113184 = CARTESIAN_POINT('Ctrl Pts',(65.050732910073,246.455096751985,24.1800150979131)) ;
#113185 = CARTESIAN_POINT('Ctrl Pts',(65.0479342501967,246.495948086445,24.2359023300204)) ;
#113186 = CARTESIAN_POINT('Ctrl Pts',(65.0451355903205,246.539767842544,24.2896393830908)) ;
#113187 = CARTESIAN_POINT('Ctrl Pts',(65.0423369304442,246.586295282531,24.3409051256965)) ;
#113188 = CARTESIAN_POINT('Ctrl Pts',(65.0394129512182,246.634906144149,24.3944664632699)) ;
#113189 = CARTESIAN_POINT('Ctrl Pts',(65.0364889719922,246.686472537509,24.4453295045976)) ;
#113190 = CARTESIAN_POINT('Ctrl Pts',(65.0335649927662,246.740652762921,24.4931695216599)) ;
#113191 = CARTESIAN_POINT('Ctrl Pts',(65.0307631881786,246.792569138649,24.539010606331)) ;
#113192 = CARTESIAN_POINT('Ctrl Pts',(65.027961383591,246.846884824809,24.582075998955)) ;
#113193 = CARTESIAN_POINT('Ctrl Pts',(65.0251595790034,246.903265782795,24.6221216382147)) ;
#113194 = CARTESIAN_POINT('Ctrl Pts',(65.0223560087871,246.959682270682,24.6621925132574)) ;
#113195 = CARTESIAN_POINT('Ctrl Pts',(65.0195524385707,247.01816621078,24.6992395871625)) ;
#113196 = CARTESIAN_POINT('Ctrl Pts',(65.0167488683544,247.078356350065,24.7330632541101)) ;
#113197 = CARTESIAN_POINT('Ctrl Pts',(65.0139410755972,247.138637143516,24.7669378638926)) ;
#113198 = CARTESIAN_POINT('Ctrl Pts',(65.01113328284,247.200628827093,24.7975791686121)) ;
#113199 = CARTESIAN_POINT('Ctrl Pts',(65.0083254900828,247.263948441857,24.8248348802908)) ;
#113200 = CARTESIAN_POINT('Ctrl Pts',(65.0079667199659,247.272039204799,24.828317521536)) ;
#113201 = CARTESIAN_POINT('Ctrl Pts',(65.0076079498491,247.280151627297,24.8317449531255)) ;
#113202 = CARTESIAN_POINT('Ctrl Pts',(65.0072491797322,247.288284892852,24.8351169160415)) ;
#113203 = CARTESIAN_POINT('Ctrl Pts',(65.0044581767345,247.351556518543,24.8613486398238)) ;
#113204 = CARTESIAN_POINT('Ctrl Pts',(65.0016671737367,247.416335160015,24.8843205302459)) ;
#113205 = CARTESIAN_POINT('Ctrl Pts',(64.998876170739,247.482246594188,24.9038578832867)) ;
#113206 = CARTESIAN_POINT('Ctrl Pts',(64.9961177591618,247.547388359798,24.9231670925065)) ;
#113207 = CARTESIAN_POINT('Ctrl Pts',(64.9933593475846,247.613636117047,24.9391213744491)) ;
#113208 = CARTESIAN_POINT('Ctrl Pts',(64.9906009360073,247.680607235827,24.9515997184528)) ;
#113209 = CARTESIAN_POINT('Ctrl Pts',(64.9878449341485,247.747519849367,24.964067161511)) ;
#113210 = CARTESIAN_POINT('Ctrl Pts',(64.9850889322896,247.815154078844,24.973064593714)) ;
#113211 = CARTESIAN_POINT('Ctrl Pts',(64.9823329304307,247.883114119084,24.9785213594877)) ;
#113212 = CARTESIAN_POINT('Ctrl Pts',(64.9795783404483,247.951039343968,24.9839753298063)) ;
#113213 = CARTESIAN_POINT('Ctrl Pts',(64.976823750466,248.019289547218,24.9858921913326)) ;
#113214 = CARTESIAN_POINT('Ctrl Pts',(64.9740691604836,248.087462725763,24.9842530053841)) ;
#113215 = CARTESIAN_POINT('Ctrl Pts',(64.9712521560922,248.15718059469,24.9825766782192)) ;
#113216 = CARTESIAN_POINT('Ctrl Pts',(64.9684351517008,248.22681736079,24.9771811280954)) ;
#113217 = CARTESIAN_POINT('Ctrl Pts',(64.9656181473094,248.295943906619,24.9681024581855)) ;
#113218 = CARTESIAN_POINT('Ctrl Pts',(64.9628620383367,248.363576138146,24.9592200426397)) ;
#113219 = CARTESIAN_POINT('Ctrl Pts',(64.960105929364,248.430719486793,24.9468123031796)) ;
#113220 = CARTESIAN_POINT('Ctrl Pts',(64.9573498203913,248.496980533019,24.9309651457034)) ;
#113221 = CARTESIAN_POINT('Ctrl Pts',(64.9545023682905,248.565437606793,24.9145927807882)) ;
#113222 = CARTESIAN_POINT('Ctrl Pts',(64.9516549161897,248.632952297457,24.8945491272306)) ;
#113223 = CARTESIAN_POINT('Ctrl Pts',(64.9488074640889,248.699108485264,24.8709845438818)) ;
#113224 = CARTESIAN_POINT('Ctrl Pts',(64.9459600119882,248.765264673071,24.847419960533)) ;
#113225 = CARTESIAN_POINT('Ctrl Pts',(64.9431125598874,248.830061837789,24.8203347258801)) ;
#113226 = CARTESIAN_POINT('Ctrl Pts',(64.9402651077866,248.893109917435,24.7899322231574)) ;
#113227 = CARTESIAN_POINT('Ctrl Pts',(64.9402651077866,248.893109917435,24.7899322231574)) ;
#113228 = CARTESIAN_POINT('Ctrl Pts',(64.9402651077866,248.904085124906,24.7845127825723)) ;
#113229 = CARTESIAN_POINT('Ctrl Pts',(64.9402651077866,248.915060332378,24.7790933419871)) ;
#113230 = CARTESIAN_POINT('Ctrl Pts',(64.9402651077866,248.926035539849,24.773673901402)) ;
#113231 = CARTESIAN_POINT('',(57.9402651077866,248.936544011728,24.7683224547054)) ;
#113232 = CARTESIAN_POINT('',(57.9402651077866,247.188367839728,24.7903888257488)) ;
#113233 = CARTESIAN_POINT('Origin',(57.9402651077866,248.040265107786,23.0213203435596)) ;
#113234 = CARTESIAN_POINT('',(58.2795523269168,250.003764327853,23.0195702593774)) ;
#113235 = CARTESIAN_POINT('Ctrl Pts',(57.9402651077866,247.188367839728,24.7903888257487)) ;
#113236 = CARTESIAN_POINT('Ctrl Pts',(57.9666399231151,246.602035381373,24.5080396547158)) ;
#113237 = CARTESIAN_POINT('Ctrl Pts',(58.0193895537721,245.742675425061,23.3177389351249)) ;
#113238 = CARTESIAN_POINT('Ctrl Pts',(58.0985139997576,246.538528075967,21.2534684972079)) ;
#113239 = CARTESIAN_POINT('Ctrl Pts',(58.1776384457431,248.70384260527,20.8001158056293)) ;
#113240 = CARTESIAN_POINT('Ctrl Pts',(58.2379844498895,249.893805686828,21.994549066635)) ;
#113241 = CARTESIAN_POINT('Ctrl Pts',(58.2719556387072,250.004418999133,22.8319096049426)) ;
#113242 = CARTESIAN_POINT('Ctrl Pts',(58.2795520121964,250.002860502623,23.019563290465)) ;
#113243 = CARTESIAN_POINT('',(58.7795523269483,250.003764821541,23.0223805714202)) ;
#113244 = CARTESIAN_POINT('Ctrl Pts',(58.2795523269168,250.003764327853,23.0195702593774)) ;
#113245 = CARTESIAN_POINT('Ctrl Pts',(58.2823182633917,250.003825255953,23.0879282718707)) ;
#113246 = CARTESIAN_POINT('Ctrl Pts',(58.2850841998665,250.000312138262,23.1563562695139)) ;
#113247 = CARTESIAN_POINT('Ctrl Pts',(58.2878501363414,249.993229751855,23.2244492410987)) ;
#113248 = CARTESIAN_POINT('Ctrl Pts',(58.2906148535111,249.98615048757,23.2925121953241)) ;
#113249 = CARTESIAN_POINT('Ctrl Pts',(58.2933795706809,249.975505126965,23.360239920402)) ;
#113250 = CARTESIAN_POINT('Ctrl Pts',(58.2961442878506,249.961350421642,23.4272310072374)) ;
#113251 = CARTESIAN_POINT('Ctrl Pts',(58.2989087672538,249.947196933628,23.4942163328193)) ;
#113252 = CARTESIAN_POINT('Ctrl Pts',(58.3016732466571,249.929534804802,23.5604646577782)) ;
#113253 = CARTESIAN_POINT('Ctrl Pts',(58.3044377260603,249.90847180973,23.6255851603507)) ;
#113254 = CARTESIAN_POINT('Ctrl Pts',(58.3072048962958,249.887388312792,23.6907690485835)) ;
#113255 = CARTESIAN_POINT('Ctrl Pts',(58.3099720665314,249.862897492722,23.7548224458987)) ;
#113256 = CARTESIAN_POINT('Ctrl Pts',(58.3127392367669,249.835156583672,23.8173711207049)) ;
#113257 = CARTESIAN_POINT('Ctrl Pts',(58.3155077613593,249.807402097179,23.8799504091782)) ;
#113258 = CARTESIAN_POINT('Ctrl Pts',(58.3182762859518,249.776394581466,23.9410230634081)) ;
#113259 = CARTESIAN_POINT('Ctrl Pts',(58.3210448105442,249.742337590698,24.0002388860917)) ;
#113260 = CARTESIAN_POINT('Ctrl Pts',(58.3238184206147,249.708218040949,24.0595634817899)) ;
#113261 = CARTESIAN_POINT('Ctrl Pts',(58.3265920306851,249.671038101262,24.1170240146228)) ;
#113262 = CARTESIAN_POINT('Ctrl Pts',(58.3293656407556,249.631044645718,24.1722993666953)) ;
#113263 = CARTESIAN_POINT('Ctrl Pts',(58.3315395397418,249.599698591206,24.2156230599248)) ;
#113264 = CARTESIAN_POINT('Ctrl Pts',(58.333713438728,249.566625063434,24.2576049393308)) ;
#113265 = CARTESIAN_POINT('Ctrl Pts',(58.3358873377142,249.531959030203,24.2981059527453)) ;
#113266 = CARTESIAN_POINT('Ctrl Pts',(58.3386837429993,249.48736621372,24.3502046236985)) ;
#113267 = CARTESIAN_POINT('Ctrl Pts',(58.3414801482845,249.439953245343,24.4000665465058)) ;
#113268 = CARTESIAN_POINT('Ctrl Pts',(58.3442765535696,249.389973128362,24.4473710120822)) ;
#113269 = CARTESIAN_POINT('Ctrl Pts',(58.3470687747069,249.340067794603,24.494604697904)) ;
#113270 = CARTESIAN_POINT('Ctrl Pts',(58.3498609958442,249.287603289537,24.5392881866717)) ;
#113271 = CARTESIAN_POINT('Ctrl Pts',(58.3526532169815,249.232871932943,24.581134823102)) ;
#113272 = CARTESIAN_POINT('Ctrl Pts',(58.3554421775713,249.178204487541,24.6229325941542)) ;
#113273 = CARTESIAN_POINT('Ctrl Pts',(58.3582311381612,249.121275836045,24.6618997954725)) ;
#113274 = CARTESIAN_POINT('Ctrl Pts',(58.3610200987511,249.062412750517,24.6977887883742)) ;
#113275 = CARTESIAN_POINT('Ctrl Pts',(58.3638073250054,249.00358626943,24.7336554634434)) ;
#113276 = CARTESIAN_POINT('Ctrl Pts',(58.3665945512598,248.942828158839,24.7664474725727)) ;
#113277 = CARTESIAN_POINT('Ctrl Pts',(58.3693817775141,248.880494381143,24.7959603121712)) ;
#113278 = CARTESIAN_POINT('Ctrl Pts',(58.3721682218784,248.818178089708,24.8254648726438)) ;
#113279 = CARTESIAN_POINT('Ctrl Pts',(58.3749546662426,248.754287452094,24.8516918799336)) ;
#113280 = CARTESIAN_POINT('Ctrl Pts',(58.3777411106069,248.689201645731,24.8744834825519)) ;
#113281 = CARTESIAN_POINT('Ctrl Pts',(58.3805277243677,248.624111882601,24.8972764707421)) ;
#113282 = CARTESIAN_POINT('Ctrl Pts',(58.3833143381285,248.557827270531,24.9166334798408)) ;
#113283 = CARTESIAN_POINT('Ctrl Pts',(58.3861009518893,248.490743802197,24.9324459793779)) ;
#113284 = CARTESIAN_POINT('Ctrl Pts',(58.388890510028,248.423589452464,24.9482751866391)) ;
#113285 = CARTESIAN_POINT('Ctrl Pts',(58.3916800681667,248.355635040572,24.9605522974399)) ;
#113286 = CARTESIAN_POINT('Ctrl Pts',(58.3944696263054,248.287287471066,24.9692197768054)) ;
#113287 = CARTESIAN_POINT('Ctrl Pts',(58.3972608512449,248.218899062914,24.9778924351134)) ;
#113288 = CARTESIAN_POINT('Ctrl Pts',(58.4000520761843,248.150117519127,24.9829511333549)) ;
#113289 = CARTESIAN_POINT('Ctrl Pts',(58.4028433011238,248.081352802459,24.9843904012362)) ;
#113290 = CARTESIAN_POINT('Ctrl Pts',(58.4056392855601,248.012470830658,24.9858321233056)) ;
#113291 = CARTESIAN_POINT('Ctrl Pts',(58.4084352699964,247.943606233485,24.9836421131475)) ;
#113292 = CARTESIAN_POINT('Ctrl Pts',(58.4112312544326,247.875166021403,24.977866929173)) ;
#113293 = CARTESIAN_POINT('Ctrl Pts',(58.412491430855,247.844319375589,24.9752639995625)) ;
#113294 = CARTESIAN_POINT('Ctrl Pts',(58.4137516072774,247.813558825869,24.9719334780948)) ;
#113295 = CARTESIAN_POINT('Ctrl Pts',(58.4150117836997,247.782920898768,24.9678830083831)) ;
#113296 = CARTESIAN_POINT('Ctrl Pts',(58.4178084842444,247.714926365708,24.958893829846)) ;
#113297 = CARTESIAN_POINT('Ctrl Pts',(58.4206051847891,247.647270448959,24.9463201700162)) ;
#113298 = CARTESIAN_POINT('Ctrl Pts',(58.4234018853337,247.580360008718,24.9301994779868)) ;
#113299 = CARTESIAN_POINT('Ctrl Pts',(58.4261944131009,247.513549401254,24.914102838608)) ;
#113300 = CARTESIAN_POINT('Ctrl Pts',(58.428986940868,247.447482535954,24.8944697850432)) ;
#113301 = CARTESIAN_POINT('Ctrl Pts',(58.4317794686352,247.382559132849,24.8713892883646)) ;
#113302 = CARTESIAN_POINT('Ctrl Pts',(58.4345687511967,247.317711177444,24.8483356136071)) ;
#113303 = CARTESIAN_POINT('Ctrl Pts',(58.4373580337581,247.254004505233,24.8218426162695)) ;
#113304 = CARTESIAN_POINT('Ctrl Pts',(58.4401473163196,247.191824888038,24.7920494147372)) ;
#113305 = CARTESIAN_POINT('Ctrl Pts',(58.4429348738925,247.129683724863,24.7622746383484)) ;
#113306 = CARTESIAN_POINT('Ctrl Pts',(58.4457224314654,247.06906818475,24.7292039182264)) ;
#113307 = CARTESIAN_POINT('Ctrl Pts',(58.4485099890383,247.010343770323,24.6930243510438)) ;
#113308 = CARTESIAN_POINT('Ctrl Pts',(58.4512967735691,246.95163564128,24.6568548171349)) ;
#113309 = CARTESIAN_POINT('Ctrl Pts',(58.4540835580999,246.894818014287,24.617578405069)) ;
#113310 = CARTESIAN_POINT('Ctrl Pts',(58.4568703426308,246.84022991973,24.575427095822)) ;
#113311 = CARTESIAN_POINT('Ctrl Pts',(58.4596573049167,246.785638343269,24.5332730979523)) ;
#113312 = CARTESIAN_POINT('Ctrl Pts',(58.4624442672027,246.733276968376,24.4882441407519)) ;
#113313 = CARTESIAN_POINT('Ctrl Pts',(58.4652312294887,246.683452629847,24.4406131779352)) ;
#113314 = CARTESIAN_POINT('Ctrl Pts',(58.4680211464405,246.633575468835,24.3929317179949)) ;
#113315 = CARTESIAN_POINT('Ctrl Pts',(58.4708110633923,246.586241067216,24.3426430869953)) ;
#113316 = CARTESIAN_POINT('Ctrl Pts',(58.4736009803441,246.541719445691,24.2900571754578)) ;
#113317 = CARTESIAN_POINT('Ctrl Pts',(58.476392570498,246.49717112313,24.237439726474)) ;
#113318 = CARTESIAN_POINT('Ctrl Pts',(58.4791841606519,246.455439234969,24.1825226455728)) ;
#113319 = CARTESIAN_POINT('Ctrl Pts',(58.4819757508057,246.416751811975,24.1256467574084)) ;
#113320 = CARTESIAN_POINT('Ctrl Pts',(58.4847721065347,246.377998344967,24.0686737753646)) ;
#113321 = CARTESIAN_POINT('Ctrl Pts',(58.4875684622637,246.342299969793,24.0097357317403)) ;
#113322 = CARTESIAN_POINT('Ctrl Pts',(58.4903648179927,246.309839483422,23.9491993273412)) ;
#113323 = CARTESIAN_POINT('Ctrl Pts',(58.4916219552236,246.295246459535,23.9219844179492)) ;
#113324 = CARTESIAN_POINT('Ctrl Pts',(58.4928790924545,246.281307191147,23.8944467528534)) ;
#113325 = CARTESIAN_POINT('Ctrl Pts',(58.4941362296853,246.268035077378,23.866620863683)) ;
#113326 = CARTESIAN_POINT('Ctrl Pts',(58.4969323681109,246.238515096276,23.8047302156097)) ;
#113327 = CARTESIAN_POINT('Ctrl Pts',(58.4997285065364,246.21218309461,23.7411698010235)) ;
#113328 = CARTESIAN_POINT('Ctrl Pts',(58.502524644962,246.189229532673,23.676300915536)) ;
#113329 = CARTESIAN_POINT('Ctrl Pts',(58.5053165998703,246.166310313322,23.6115290853648)) ;
#113330 = CARTESIAN_POINT('Ctrl Pts',(58.5081085547787,246.146759663823,23.5454531289407)) ;
#113331 = CARTESIAN_POINT('Ctrl Pts',(58.510900509687,246.130720968833,23.4784564626628)) ;
#113332 = CARTESIAN_POINT('Ctrl Pts',(58.5136892063705,246.114700991077,23.4115379818187)) ;
#113333 = CARTESIAN_POINT('Ctrl Pts',(58.516477903054,246.102184941641,23.3437014003189)) ;
#113334 = CARTESIAN_POINT('Ctrl Pts',(58.5192665997374,246.093266566467,23.2753457952426)) ;
#113335 = CARTESIAN_POINT('Ctrl Pts',(58.522053563702,246.084353732605,23.2070326619946)) ;
#113336 = CARTESIAN_POINT('Ctrl Pts',(58.5248405276666,246.07903420188,23.1382016306277)) ;
#113337 = CARTESIAN_POINT('Ctrl Pts',(58.5276274916312,246.077350451562,23.0692609566347)) ;
#113338 = CARTESIAN_POINT('Ctrl Pts',(58.5304136757485,246.07566717239,23.0003395735963)) ;
#113339 = CARTESIAN_POINT('Ctrl Pts',(58.5331998598658,246.077617665834,22.9313090993776)) ;
#113340 = CARTESIAN_POINT('Ctrl Pts',(58.5359860439832,246.083192350296,22.8625800780558)) ;
#113341 = CARTESIAN_POINT('Ctrl Pts',(58.5387723999681,246.088767378637,22.7938468171395)) ;
#113342 = CARTESIAN_POINT('Ctrl Pts',(58.541558755953,246.097966999588,22.725415535126)) ;
#113343 = CARTESIAN_POINT('Ctrl Pts',(58.5443451119379,246.110729730287,22.657692130987)) ;
#113344 = CARTESIAN_POINT('Ctrl Pts',(58.547134417857,246.123505972976,22.5898970276161)) ;
#113345 = CARTESIAN_POINT('Ctrl Pts',(58.549923723776,246.139852762486,22.5228117810505)) ;
#113346 = CARTESIAN_POINT('Ctrl Pts',(58.5527130296951,246.159657579804,22.4568315698038)) ;
#113347 = CARTESIAN_POINT('Ctrl Pts',(58.5555040052378,246.179474251896,22.3908118641018)) ;
#113348 = CARTESIAN_POINT('Ctrl Pts',(58.5582949807805,246.202752905681,22.3258989723056)) ;
#113349 = CARTESIAN_POINT('Ctrl Pts',(58.5610859563231,246.229332196717,22.262469737968)) ;
#113350 = CARTESIAN_POINT('Ctrl Pts',(58.5638816983426,246.25595688033,22.1989321780755)) ;
#113351 = CARTESIAN_POINT('Ctrl Pts',(58.5666774403621,246.285893238002,22.1368837744407)) ;
#113352 = CARTESIAN_POINT('Ctrl Pts',(58.5694731823816,246.318933572051,22.0766775570614)) ;
#113353 = CARTESIAN_POINT('Ctrl Pts',(58.5707356801446,246.333853885705,22.0494897070255)) ;
#113354 = CARTESIAN_POINT('Ctrl Pts',(58.5719981779077,246.349406580268,22.0226771347491)) ;
#113355 = CARTESIAN_POINT('Ctrl Pts',(58.5732606756708,246.365569721326,21.9962702898693)) ;
#113356 = CARTESIAN_POINT('Ctrl Pts',(58.5760570346494,246.401370136934,21.9377806672056)) ;
#113357 = CARTESIAN_POINT('Ctrl Pts',(58.578853393628,246.440308605341,21.8810541206144)) ;
#113358 = CARTESIAN_POINT('Ctrl Pts',(58.5816497526066,246.482185959513,21.8264472884962)) ;
#113359 = CARTESIAN_POINT('Ctrl Pts',(58.5844419309789,246.524000706297,21.7719220945611)) ;
#113360 = CARTESIAN_POINT('Ctrl Pts',(58.5872341093512,246.568745322163,21.7195107118026)) ;
#113361 = CARTESIAN_POINT('Ctrl Pts',(58.5900262877235,246.61617643857,21.669542361711)) ;
#113362 = CARTESIAN_POINT('Ctrl Pts',(58.5928152110515,246.663552261093,21.6196322633398)) ;
#113363 = CARTESIAN_POINT('Ctrl Pts',(58.5956041343795,246.713608027649,21.5721598954964)) ;
#113364 = CARTESIAN_POINT('Ctrl Pts',(58.5983930577075,246.766060187121,21.5274213944491)) ;
#113365 = CARTESIAN_POINT('Ctrl Pts',(58.6011802501525,246.818479793332,21.4827106593532)) ;
#113366 = CARTESIAN_POINT('Ctrl Pts',(58.6039674425975,246.873292469407,21.4407307429236)) ;
#113367 = CARTESIAN_POINT('Ctrl Pts',(58.6067546350425,246.930179027894,21.4017397974827)) ;
#113368 = CARTESIAN_POINT('Ctrl Pts',(58.6095410491183,246.987049699876,21.362759740903)) ;
#113369 = CARTESIAN_POINT('Ctrl Pts',(58.6123274631941,247.045992699782,21.3267672754933)) ;
#113370 = CARTESIAN_POINT('Ctrl Pts',(58.6151138772699,247.106658548957,21.2939781529931)) ;
#113371 = CARTESIAN_POINT('Ctrl Pts',(58.6179004643351,247.16732816446,21.2611869948399)) ;
#113372 = CARTESIAN_POINT('Ctrl Pts',(58.6206870514004,247.229720408583,21.2315998055393)) ;
#113373 = CARTESIAN_POINT('Ctrl Pts',(58.6234736384656,247.293461409716,21.2053862900903)) ;
#113374 = CARTESIAN_POINT('Ctrl Pts',(58.6262631755665,247.357269890609,21.1791450235597)) ;
#113375 = CARTESIAN_POINT('Ctrl Pts',(58.6290527126674,247.422429523254,21.1562847454821)) ;
#113376 = CARTESIAN_POINT('Ctrl Pts',(58.6318422497683,247.488547607392,21.1369265286263)) ;
#113377 = CARTESIAN_POINT('Ctrl Pts',(58.6346334568804,247.554705274421,21.1175567225933)) ;
#113378 = CARTESIAN_POINT('Ctrl Pts',(58.6374246639925,247.621822057238,21.1016932634121)) ;
#113379 = CARTESIAN_POINT('Ctrl Pts',(58.6402158711046,247.689494014506,21.0894062952337)) ;
#113380 = CARTESIAN_POINT('Ctrl Pts',(58.6430118428712,247.757281489355,21.0770983529192)) ;
#113381 = CARTESIAN_POINT('Ctrl Pts',(58.6458078146379,247.825625543487,21.0683791482484)) ;
#113382 = CARTESIAN_POINT('Ctrl Pts',(58.6486037864045,247.894116934739,21.0632669833278)) ;
#113383 = CARTESIAN_POINT('Ctrl Pts',(58.6498642314884,247.924993368625,21.0609623809639)) ;
#113384 = CARTESIAN_POINT('Ctrl Pts',(58.6511246765724,247.955899747104,21.0593901220406)) ;
#113385 = CARTESIAN_POINT('Ctrl Pts',(58.6523851216563,247.986798772013,21.0585484258527)) ;
#113386 = CARTESIAN_POINT('Ctrl Pts',(58.6551814899633,248.055349996556,21.0566810755222)) ;
#113387 = CARTESIAN_POINT('Ctrl Pts',(58.6579778582703,248.124133566806,21.0584056752107)) ;
#113388 = CARTESIAN_POINT('Ctrl Pts',(58.6607742265772,248.192741916983,21.0637496366228)) ;
#113389 = CARTESIAN_POINT('Ctrl Pts',(58.6635664151064,248.261247717128,21.0690856103277)) ;
#113390 = CARTESIAN_POINT('Ctrl Pts',(58.6663586036356,248.329578331552,21.0780301706077)) ;
#113391 = CARTESIAN_POINT('Ctrl Pts',(58.6691507921648,248.397325088048,21.0905587268665)) ;
#113392 = CARTESIAN_POINT('Ctrl Pts',(58.6719397268291,248.464992896152,21.1030726830261)) ;
#113393 = CARTESIAN_POINT('Ctrl Pts',(58.6747286614933,248.532077717279,21.1191622511777)) ;
#113394 = CARTESIAN_POINT('Ctrl Pts',(58.6775175961576,248.598176715433,21.1387511182579)) ;
#113395 = CARTESIAN_POINT('Ctrl Pts',(58.6803048006659,248.664234708116,21.1583278331008)) ;
#113396 = CARTESIAN_POINT('Ctrl Pts',(58.6830920051742,248.72930762151,21.1813994011998)) ;
#113397 = CARTESIAN_POINT('Ctrl Pts',(58.6858792096824,248.793005041016,21.2078389284572)) ;
#113398 = CARTESIAN_POINT('Ctrl Pts',(58.688665636531,248.856684688264,21.2342710788057)) ;
#113399 = CARTESIAN_POINT('Ctrl Pts',(58.6914520633797,248.918989150438,21.264069134643)) ;
#113400 = CARTESIAN_POINT('Ctrl Pts',(58.6942384902283,248.979547050605,21.2970576948037)) ;
#113401 = CARTESIAN_POINT('Ctrl Pts',(58.6970250907593,249.04010872544,21.3300483111932)) ;
#113402 = CARTESIAN_POINT('Ctrl Pts',(58.6998116912902,249.098923192355,21.3662295896848)) ;
#113403 = CARTESIAN_POINT('Ctrl Pts',(58.7025982918212,249.155644383876,21.4053805796855)) ;
#113404 = CARTESIAN_POINT('Ctrl Pts',(58.7053878433467,249.212425642824,21.4445730303674)) ;
#113405 = CARTESIAN_POINT('Ctrl Pts',(58.7081773948722,249.267108797801,21.4867411893515)) ;
#113406 = CARTESIAN_POINT('Ctrl Pts',(58.7109669463977,249.319378291217,21.5316218123213)) ;
#113407 = CARTESIAN_POINT('Ctrl Pts',(58.7137581685039,249.371679087302,21.5765293129827)) ;
#113408 = CARTESIAN_POINT('Ctrl Pts',(58.7165493906102,249.42156298993,21.6241521716751)) ;
#113409 = CARTESIAN_POINT('Ctrl Pts',(58.7193406127164,249.468751012494,21.6741899600959)) ;
#113410 = CARTESIAN_POINT('Ctrl Pts',(58.7221366001999,249.516019597879,21.7243131766656)) ;
#113411 = CARTESIAN_POINT('Ctrl Pts',(58.7249325876834,249.560582800146,21.7768591773811)) ;
#113412 = CARTESIAN_POINT('Ctrl Pts',(58.7277285751669,249.602202207231,21.831494832244)) ;
#113413 = CARTESIAN_POINT('Ctrl Pts',(58.7289889059919,249.620962742454,21.8561226248836)) ;
#113414 = CARTESIAN_POINT('Ctrl Pts',(58.7302492368168,249.639125725635,21.8811746274393)) ;
#113415 = CARTESIAN_POINT('Ctrl Pts',(58.7315095676418,249.65667232475,21.9066186081401)) ;
#113416 = CARTESIAN_POINT('Ctrl Pts',(58.734341194748,249.696094851511,21.9637844442945)) ;
#113417 = CARTESIAN_POINT('Ctrl Pts',(58.7371728218541,249.73255539459,22.0231515764158)) ;
#113418 = CARTESIAN_POINT('Ctrl Pts',(58.7400044489602,249.765804160563,22.0843853258864)) ;
#113419 = CARTESIAN_POINT('Ctrl Pts',(58.7428315631313,249.798999935969,22.1455214834324)) ;
#113420 = CARTESIAN_POINT('Ctrl Pts',(58.7456586773023,249.828993872798,22.2085179383267)) ;
#113421 = CARTESIAN_POINT('Ctrl Pts',(58.7484857914733,249.855579119968,22.273010723698)) ;
#113422 = CARTESIAN_POINT('Ctrl Pts',(58.7513087092328,249.882124905471,22.3374077795556)) ;
#113423 = CARTESIAN_POINT('Ctrl Pts',(58.7541316269924,249.905271880031,22.4032963141276)) ;
#113424 = CARTESIAN_POINT('Ctrl Pts',(58.7569545447519,249.924859700972,22.4702890655611)) ;
#113425 = CARTESIAN_POINT('Ctrl Pts',(58.7597749878247,249.944430350418,22.5372230883702)) ;
#113426 = CARTESIAN_POINT('Ctrl Pts',(58.7625954308975,249.96044790909,22.6052589520035)) ;
#113427 = CARTESIAN_POINT('Ctrl Pts',(58.7654158739702,249.972801063341,22.6739919247885)) ;
#113428 = CARTESIAN_POINT('Ctrl Pts',(58.7682349199379,249.985148098463,22.742690850728)) ;
#113429 = CARTESIAN_POINT('Ctrl Pts',(58.7710539659055,249.99383424755,22.8120857340777)) ;
#113430 = CARTESIAN_POINT('Ctrl Pts',(58.7738730118731,249.998799091685,22.8817607365289)) ;
#113431 = CARTESIAN_POINT('Ctrl Pts',(58.7757661168877,250.002133188196,22.9285503589917)) ;
#113432 = CARTESIAN_POINT('Ctrl Pts',(58.7776592219022,250.003790153872,22.9754660703664)) ;
#113433 = CARTESIAN_POINT('Ctrl Pts',(58.7795523269168,250.003764821542,23.0223805706392)) ;
#113434 = CARTESIAN_POINT('',(59.2795523268825,250.003764929479,23.0221571305627)) ;
#113435 = CARTESIAN_POINT('Ctrl Pts',(58.7795523269483,250.003764821541,23.0223805714202)) ;
#113436 = CARTESIAN_POINT('Ctrl Pts',(58.7826465261243,250.0037234169,23.0990603155281)) ;
#113437 = CARTESIAN_POINT('Ctrl Pts',(58.7857407253004,249.999186060935,23.1755820244515)) ;
#113438 = CARTESIAN_POINT('Ctrl Pts',(58.7888349244764,249.990232745583,23.2514473987812)) ;
#113439 = CARTESIAN_POINT('Ctrl Pts',(58.7919411809528,249.981244541458,23.3276084010112)) ;
#113440 = CARTESIAN_POINT('Ctrl Pts',(58.7950474374292,249.967806032364,23.4031076705707)) ;
#113441 = CARTESIAN_POINT('Ctrl Pts',(58.7981536939056,249.950047983388,23.4774580618604)) ;
#113442 = CARTESIAN_POINT('Ctrl Pts',(58.8012752838319,249.932202275149,23.5521754698508)) ;
#113443 = CARTESIAN_POINT('Ctrl Pts',(58.8043968737583,249.909994416863,23.6257323648907)) ;
#113444 = CARTESIAN_POINT('Ctrl Pts',(58.8075184636846,249.883605268359,23.6976555433071)) ;
#113445 = CARTESIAN_POINT('Ctrl Pts',(58.8085569803322,249.8748259057,23.721583547912)) ;
#113446 = CARTESIAN_POINT('Ctrl Pts',(58.8095954969798,249.865584135377,23.7453309205817)) ;
#113447 = CARTESIAN_POINT('Ctrl Pts',(58.8106340136274,249.855887747668,23.7688808291055)) ;
#113448 = CARTESIAN_POINT('Ctrl Pts',(58.8134303540687,249.829778969199,23.8322920047936)) ;
#113449 = CARTESIAN_POINT('Ctrl Pts',(58.8162266945101,249.800293020772,23.8944581076853)) ;
#113450 = CARTESIAN_POINT('Ctrl Pts',(58.8190230349514,249.767570213188,23.9549955134402)) ;
#113451 = CARTESIAN_POINT('Ctrl Pts',(58.8218151949193,249.734896325552,24.0154424169766)) ;
#113452 = CARTESIAN_POINT('Ctrl Pts',(58.8246073548873,249.698995414582,24.0742650276122)) ;
#113453 = CARTESIAN_POINT('Ctrl Pts',(58.8273995148552,249.660055769466,24.1310998091892)) ;
#113454 = CARTESIAN_POINT('Ctrl Pts',(58.8301884200708,249.621161515339,24.1878683398563)) ;
#113455 = CARTESIAN_POINT('Ctrl Pts',(58.8329773252864,249.579235838321,24.2426532405667)) ;
#113456 = CARTESIAN_POINT('Ctrl Pts',(58.835766230502,249.534511933172,24.29511729552)) ;
#113457 = CARTESIAN_POINT('Ctrl Pts',(58.8385534050279,249.489815781997,24.3475487932539)) ;
#113458 = CARTESIAN_POINT('Ctrl Pts',(58.8413405795538,249.442325165229,24.3976619296572)) ;
#113459 = CARTESIAN_POINT('Ctrl Pts',(58.8441277540797,249.39231446803,24.4451513649466)) ;
#113460 = CARTESIAN_POINT('Ctrl Pts',(58.8469141504586,249.342317733242,24.4926275417321)) ;
#113461 = CARTESIAN_POINT('Ctrl Pts',(58.8497005468374,249.289802670604,24.5374811338375)) ;
#113462 = CARTESIAN_POINT('Ctrl Pts',(58.8524869432162,249.235080275476,24.5794438832885)) ;
#113463 = CARTESIAN_POINT('Ctrl Pts',(58.8552735128358,249.180354478052,24.6214092417208)) ;
#113464 = CARTESIAN_POINT('Ctrl Pts',(58.8580600824553,249.123421466723,24.660483104034)) ;
#113465 = CARTESIAN_POINT('Ctrl Pts',(58.8608466520749,249.064623598917,24.6964388264282)) ;
#113466 = CARTESIAN_POINT('Ctrl Pts',(58.8636361722326,249.005763473434,24.7324326202669)) ;
#113467 = CARTESIAN_POINT('Ctrl Pts',(58.8664256923903,248.945034970413,24.7653014287764)) ;
#113468 = CARTESIAN_POINT('Ctrl Pts',(58.869215212548,248.88280672345,24.7948636545263)) ;
#113469 = CARTESIAN_POINT('Ctrl Pts',(58.8720064029805,248.820541216217,24.8244435811847)) ;
#113470 = CARTESIAN_POINT('Ctrl Pts',(58.874797593413,248.756774631668,24.8507127976591)) ;
#113471 = CARTESIAN_POINT('Ctrl Pts',(58.8775887838455,248.69189474994,24.8735382193687)) ;
#113472 = CARTESIAN_POINT('Ctrl Pts',(58.8803847395139,248.626904102592,24.8964026095829)) ;
#113473 = CARTESIAN_POINT('Ctrl Pts',(58.8831806951822,248.560796835394,24.9158113328648)) ;
#113474 = CARTESIAN_POINT('Ctrl Pts',(58.8859766508506,248.493974153722,24.9316816579805)) ;
#113475 = CARTESIAN_POINT('Ctrl Pts',(58.8872372537713,248.463846040947,24.9388370569093)) ;
#113476 = CARTESIAN_POINT('Ctrl Pts',(58.8884978566921,248.433572608176,24.9452738653903)) ;
#113477 = CARTESIAN_POINT('Ctrl Pts',(58.8897584596129,248.403190980567,24.9509879472846)) ;
#113478 = CARTESIAN_POINT('Ctrl Pts',(58.8925547989444,248.335796768767,24.9636632407346)) ;
#113479 = CARTESIAN_POINT('Ctrl Pts',(58.8953511382759,248.267605562946,24.9728285101274)) ;
#113480 = CARTESIAN_POINT('Ctrl Pts',(58.8981474776075,248.199015467649,24.9783922822586)) ;
#113481 = CARTESIAN_POINT('Ctrl Pts',(58.9009396365133,248.130527912052,24.9839477367528)) ;
#113482 = CARTESIAN_POINT('Ctrl Pts',(58.9037317954192,248.061643135884,24.9859123407114)) ;
#113483 = CARTESIAN_POINT('Ctrl Pts',(58.9065239543251,247.992768554336,24.9842457948721)) ;
#113484 = CARTESIAN_POINT('Ctrl Pts',(58.9093128585551,247.923974256343,24.9825811916395)) ;
#113485 = CARTESIAN_POINT('Ctrl Pts',(58.9121017627851,247.855190617769,24.9772938568925)) ;
#113486 = CARTESIAN_POINT('Ctrl Pts',(58.9148906670151,247.78682746458,24.9683954861789)) ;
#113487 = CARTESIAN_POINT('Ctrl Pts',(58.9176778406036,247.718506733826,24.9595026373076)) ;
#113488 = CARTESIAN_POINT('Ctrl Pts',(58.9204650141921,247.650606456473,24.9470032610063)) ;
#113489 = CARTESIAN_POINT('Ctrl Pts',(58.9232521877806,247.5835321864,24.9309609611948)) ;
#113490 = CARTESIAN_POINT('Ctrl Pts',(58.9260385832719,247.516476641499,24.9149231399236)) ;
#113491 = CARTESIAN_POINT('Ctrl Pts',(58.9288249787631,247.450247123213,24.895344472897)) ;
#113492 = CARTESIAN_POINT('Ctrl Pts',(58.9316113742544,247.385238052294,24.8723394700339)) ;
#113493 = CARTESIAN_POINT('Ctrl Pts',(58.9343979430379,247.320224938315,24.849333036438)) ;
#113494 = CARTESIAN_POINT('Ctrl Pts',(58.9371845118213,247.256432884241,24.822900010107)) ;
#113495 = CARTESIAN_POINT('Ctrl Pts',(58.9399710806048,247.194238517168,24.7932038775334)) ;
#113496 = CARTESIAN_POINT('Ctrl Pts',(58.9427606000104,247.131978294167,24.7634763005301)) ;
#113497 = CARTESIAN_POINT('Ctrl Pts',(58.945550119416,247.071319578055,24.7304789337767)) ;
#113498 = CARTESIAN_POINT('Ctrl Pts',(58.9483396388216,247.012615552558,24.6944218472468)) ;
#113499 = CARTESIAN_POINT('Ctrl Pts',(58.951130828549,246.953876375983,24.6583431702813)) ;
#113500 = CARTESIAN_POINT('Ctrl Pts',(58.9539220182765,246.897094623642,24.6192014057697)) ;
#113501 = CARTESIAN_POINT('Ctrl Pts',(58.9567132080039,246.842593243395,24.577249119322)) ;
#113502 = CARTESIAN_POINT('Ctrl Pts',(58.9595091630472,246.787998814549,24.535225208974)) ;
#113503 = CARTESIAN_POINT('Ctrl Pts',(58.9623051180904,246.735692900195,24.4903815195425)) ;
#113504 = CARTESIAN_POINT('Ctrl Pts',(58.9651010731337,246.685963550708,24.4430093188615)) ;
#113505 = CARTESIAN_POINT('Ctrl Pts',(58.9663616839553,246.663542104317,24.4216506389487)) ;
#113506 = CARTESIAN_POINT('Ctrl Pts',(58.9676222947768,246.641643905704,24.3997784272724)) ;
#113507 = CARTESIAN_POINT('Ctrl Pts',(58.9688829055984,246.620292659259,24.3774215549088)) ;
#113508 = CARTESIAN_POINT('Ctrl Pts',(58.9716792401988,246.572930516895,24.3278286951007)) ;
#113509 = CARTESIAN_POINT('Ctrl Pts',(58.9744755747991,246.528076671213,24.2756543986102)) ;
#113510 = CARTESIAN_POINT('Ctrl Pts',(58.9772719093995,246.486024812183,24.2211825662849)) ;
#113511 = CARTESIAN_POINT('Ctrl Pts',(58.9800640634739,246.444035820768,24.1667921694607)) ;
#113512 = CARTESIAN_POINT('Ctrl Pts',(58.9828562175483,246.404840799509,24.1101114395027)) ;
#113513 = CARTESIAN_POINT('Ctrl Pts',(58.9856483716227,246.368695610334,24.0514599773901)) ;
#113514 = CARTESIAN_POINT('Ctrl Pts',(58.9884372708968,246.332592555428,23.9928768849977)) ;
#113515 = CARTESIAN_POINT('Ctrl Pts',(58.991226170171,246.299532527978,23.9323280389777)) ;
#113516 = CARTESIAN_POINT('Ctrl Pts',(58.9940150694451,246.269729112615,23.8701634031445)) ;
#113517 = CARTESIAN_POINT('Ctrl Pts',(58.9968022380036,246.239944192449,23.8080373450087)) ;
#113518 = CARTESIAN_POINT('Ctrl Pts',(58.999589406562,246.213412086901,23.7442979278645)) ;
#113519 = CARTESIAN_POINT('Ctrl Pts',(59.0023765751204,246.190300533026,23.6793198284634)) ;
#113520 = CARTESIAN_POINT('Ctrl Pts',(59.0051629655152,246.167195431783,23.6143598706264)) ;
#113521 = CARTESIAN_POINT('Ctrl Pts',(59.0079493559099,246.147509150645,23.5481623793557)) ;
#113522 = CARTESIAN_POINT('Ctrl Pts',(59.0107357463047,246.131360679587,23.4811204457802)) ;
#113523 = CARTESIAN_POINT('Ctrl Pts',(59.0135223099329,246.115211204558,23.4140743441216)) ;
#113524 = CARTESIAN_POINT('Ctrl Pts',(59.0163088735611,246.102600088724,23.3461841737032)) ;
#113525 = CARTESIAN_POINT('Ctrl Pts',(59.0190954371893,246.093595562003,23.2778548042511)) ;
#113526 = CARTESIAN_POINT('Ctrl Pts',(59.0218849513863,246.084581500788,23.2094530838579)) ;
#113527 = CARTESIAN_POINT('Ctrl Pts',(59.0246744655832,246.079181714025,23.1406117238914)) ;
#113528 = CARTESIAN_POINT('Ctrl Pts',(59.0274639797802,246.077412598308,23.0717413315915)) ;
#113529 = CARTESIAN_POINT('Ctrl Pts',(59.030255164261,246.075642423292,23.0028297016082)) ;
#113530 = CARTESIAN_POINT('Ctrl Pts',(59.0330463487418,246.077507232746,22.9338894953879)) ;
#113531 = CARTESIAN_POINT('Ctrl Pts',(59.0358375332225,246.082971314618,22.8653291347449)) ;
#113532 = CARTESIAN_POINT('Ctrl Pts',(59.0386334830153,246.088444725166,22.796651722896)) ;
#113533 = CARTESIAN_POINT('Ctrl Pts',(59.0414294328081,246.097529607418,22.7283559371215)) ;
#113534 = CARTESIAN_POINT('Ctrl Pts',(59.0442253826009,246.110138780026,22.6608420378504)) ;
#113535 = CARTESIAN_POINT('Ctrl Pts',(59.0454860389286,246.115824087135,22.630400924587)) ;
#113536 = CARTESIAN_POINT('Ctrl Pts',(59.0467466952562,246.12222519591,22.6001185853171)) ;
#113537 = CARTESIAN_POINT('Ctrl Pts',(59.0480073515839,246.129330820986,22.5700306344666)) ;
#113538 = CARTESIAN_POINT('Ctrl Pts',(59.05080368882,246.145092233156,22.503290750269)) ;
#113539 = CARTESIAN_POINT('Ctrl Pts',(59.0536000260561,246.164385113101,22.4372466801164)) ;
#113540 = CARTESIAN_POINT('Ctrl Pts',(59.0563963632922,246.187131528414,22.3722993985944)) ;
#113541 = CARTESIAN_POINT('Ctrl Pts',(59.0591885200428,246.209843938151,22.3074492123594)) ;
#113542 = CARTESIAN_POINT('Ctrl Pts',(59.0619806767934,246.235999475072,22.2436930199692)) ;
#113543 = CARTESIAN_POINT('Ctrl Pts',(59.064772833544,246.265469657009,22.1814195411433)) ;
#113544 = CARTESIAN_POINT('Ctrl Pts',(59.0675617355409,246.294905486223,22.1192186530988)) ;
#113545 = CARTESIAN_POINT('Ctrl Pts',(59.0703506375377,246.32764807756,22.0584974874983)) ;
#113546 = CARTESIAN_POINT('Ctrl Pts',(59.0731395395346,246.363520448566,21.9996258697678)) ;
#113547 = CARTESIAN_POINT('Ctrl Pts',(59.0759267108429,246.399370558517,21.9407907855667)) ;
#113548 = CARTESIAN_POINT('Ctrl Pts',(59.0787138821512,246.438346340316,21.8838033905302)) ;
#113549 = CARTESIAN_POINT('Ctrl Pts',(59.0815010534596,246.480225101903,21.8290085428787)) ;
#113550 = CARTESIAN_POINT('Ctrl Pts',(59.0842874466271,246.522092171501,21.7742289932125)) ;
#113551 = CARTESIAN_POINT('Ctrl Pts',(59.0870738397947,246.566860313932,21.721641165454)) ;
#113552 = CARTESIAN_POINT('Ctrl Pts',(59.0898602329622,246.614264827651,21.671559086502)) ;
#113553 = CARTESIAN_POINT('Ctrl Pts',(59.0926467993818,246.661672288883,21.6214738935511)) ;
#113554 = CARTESIAN_POINT('Ctrl Pts',(59.0954333658015,246.711716107579,21.5738951134208)) ;
#113555 = CARTESIAN_POINT('Ctrl Pts',(59.0982199322211,246.76409403878,21.5291006370043)) ;
#113556 = CARTESIAN_POINT('Ctrl Pts',(59.1010094492184,246.816527430763,21.4842587296061)) ;
#113557 = CARTESIAN_POINT('Ctrl Pts',(59.1037989662157,246.871299493763,21.4422073290616)) ;
#113558 = CARTESIAN_POINT('Ctrl Pts',(59.106588483213,246.928074919113,21.4031839975677)) ;
#113559 = CARTESIAN_POINT('Ctrl Pts',(59.1093796705032,246.984884340167,21.3641372998798)) ;
#113560 = CARTESIAN_POINT('Ctrl Pts',(59.1121708577934,247.043699092379,21.3281225361713)) ;
#113561 = CARTESIAN_POINT('Ctrl Pts',(59.1149620450837,247.10415729574,21.2953323904655)) ;
#113562 = CARTESIAN_POINT('Ctrl Pts',(59.1177579976706,247.164718717282,21.262486263288)) ;
#113563 = CARTESIAN_POINT('Ctrl Pts',(59.1205539502575,247.226928746853,21.2328759522659)) ;
#113564 = CARTESIAN_POINT('Ctrl Pts',(59.1233499028444,247.290404291723,21.2066465418713)) ;
#113565 = CARTESIAN_POINT('Ctrl Pts',(59.1246105344194,247.319023974504,21.1948202959282)) ;
#113566 = CARTESIAN_POINT('Ctrl Pts',(59.1258711659944,247.347900705571,21.183680683096)) ;
#113567 = CARTESIAN_POINT('Ctrl Pts',(59.1271317975694,247.376998477152,21.1732376542062)) ;
#113568 = CARTESIAN_POINT('Ctrl Pts',(59.1299281344919,247.441543245541,21.1500728946957)) ;
#113569 = CARTESIAN_POINT('Ctrl Pts',(59.1327244714143,247.507429602488,21.1302481286355)) ;
#113570 = CARTESIAN_POINT('Ctrl Pts',(59.1355208083368,247.574278898709,21.1139165837462)) ;
#113571 = CARTESIAN_POINT('Ctrl Pts',(59.1383129647749,247.641028256174,21.0976094542866)) ;
#113572 = CARTESIAN_POINT('Ctrl Pts',(59.141105121213,247.708737222676,21.0847852965806)) ;
#113573 = CARTESIAN_POINT('Ctrl Pts',(59.1438972776511,247.777009869317,21.0755482784352)) ;
#113574 = CARTESIAN_POINT('Ctrl Pts',(59.1466861793387,247.845202932154,21.0663220276625)) ;
#113575 = CARTESIAN_POINT('Ctrl Pts',(59.1494750810264,247.913957885993,21.0606746771762)) ;
#113576 = CARTESIAN_POINT('Ctrl Pts',(59.152263982714,247.982868205832,21.0586594340681)) ;
#113577 = CARTESIAN_POINT('Ctrl Pts',(59.1550511537154,248.051735762549,21.0566454415432)) ;
#113578 = CARTESIAN_POINT('Ctrl Pts',(59.1578383247167,248.120758004461,21.0582590993305)) ;
#113579 = CARTESIAN_POINT('Ctrl Pts',(59.1606254957181,248.189524423037,21.0635016832106)) ;
#113580 = CARTESIAN_POINT('Ctrl Pts',(59.1634118885814,248.258271643017,21.0687428034366)) ;
#113581 = CARTESIAN_POINT('Ctrl Pts',(59.1661982814448,248.326762692275,21.0776108010526)) ;
#113582 = CARTESIAN_POINT('Ctrl Pts',(59.1689846743081,248.39459001199,21.0900549262074)) ;
#113583 = CARTESIAN_POINT('Ctrl Pts',(59.1717712404267,248.462421549146,21.1024998251265)) ;
#113584 = CARTESIAN_POINT('Ctrl Pts',(59.1745578065454,248.529588792526,21.1185212019465)) ;
#113585 = CARTESIAN_POINT('Ctrl Pts',(59.177344372664,248.595694014761,21.1380171339577)) ;
#113586 = CARTESIAN_POINT('Ctrl Pts',(59.1801338893674,248.6618692332,21.1575337094402)) ;
#113587 = CARTESIAN_POINT('Ctrl Pts',(59.1829234060707,248.726979714662,21.1805320431338)) ;
#113588 = CARTESIAN_POINT('Ctrl Pts',(59.185712922774,248.790643520116,21.2068605098048)) ;
#113589 = CARTESIAN_POINT('Ctrl Pts',(59.1885041097738,248.854345445948,21.2332047413381)) ;
#113590 = CARTESIAN_POINT('Ctrl Pts',(59.1912952967737,248.916598528649,21.2628828631803)) ;
#113591 = CARTESIAN_POINT('Ctrl Pts',(59.1940864837735,248.97704397061,21.2956965108062)) ;
#113592 = CARTESIAN_POINT('Ctrl Pts',(59.1968824360786,249.037592609161,21.3285661801345)) ;
#113593 = CARTESIAN_POINT('Ctrl Pts',(59.1996783883837,249.09632702957,21.3645818026303)) ;
#113594 = CARTESIAN_POINT('Ctrl Pts',(59.2024743406888,249.152916778104,21.4035012836708)) ;
#113595 = CARTESIAN_POINT('Ctrl Pts',(59.2037349749775,249.178431869066,21.4210492340455)) ;
#113596 = CARTESIAN_POINT('Ctrl Pts',(59.2049956092663,249.203511410583,21.4391869641449)) ;
#113597 = CARTESIAN_POINT('Ctrl Pts',(59.206256243555,249.228127432623,21.4578897095905)) ;
#113598 = CARTESIAN_POINT('Ctrl Pts',(59.2090240914643,249.282174356261,21.4989534465851)) ;
#113599 = CARTESIAN_POINT('Ctrl Pts',(59.2117919393736,249.334206058704,21.5429118444611)) ;
#113600 = CARTESIAN_POINT('Ctrl Pts',(59.2145597872828,249.38389135594,21.5895379734799)) ;
#113601 = CARTESIAN_POINT('Ctrl Pts',(59.2173229304128,249.433492198262,21.6360848475491)) ;
#113602 = CARTESIAN_POINT('Ctrl Pts',(59.2200860735428,249.480754191283,21.68529010922)) ;
#113603 = CARTESIAN_POINT('Ctrl Pts',(59.2228492166728,249.525377669804,21.7368854763372)) ;
#113604 = CARTESIAN_POINT('Ctrl Pts',(59.2256097351383,249.569958761213,21.7884318338591)) ;
#113605 = CARTESIAN_POINT('Ctrl Pts',(59.2283702536038,249.6119059787,21.8423634196678)) ;
#113606 = CARTESIAN_POINT('Ctrl Pts',(59.2311307720693,249.650956196326,21.8983749008513)) ;
#113607 = CARTESIAN_POINT('Ctrl Pts',(59.2338896588018,249.689983331501,21.9543532738406)) ;
#113608 = CARTESIAN_POINT('Ctrl Pts',(59.2366485455343,249.726116575792,22.0124086935422)) ;
#113609 = CARTESIAN_POINT('Ctrl Pts',(59.2394074322669,249.759134070949,22.072204050645)) ;
#113610 = CARTESIAN_POINT('Ctrl Pts',(59.2421656779635,249.792143894389,22.1319855141116)) ;
#113611 = CARTESIAN_POINT('Ctrl Pts',(59.2449239236602,249.822039163659,22.1935056729784)) ;
#113612 = CARTESIAN_POINT('Ctrl Pts',(59.2476821693568,249.848643235575,22.2564015263404)) ;
#113613 = CARTESIAN_POINT('Ctrl Pts',(59.2504425590596,249.875267987045,22.3193462691449)) ;
#113614 = CARTESIAN_POINT('Ctrl Pts',(59.2532029487623,249.898596232054,22.3836683803723)) ;
#113615 = CARTESIAN_POINT('Ctrl Pts',(59.2559633384651,249.918499395345,22.4489845932885)) ;
#113616 = CARTESIAN_POINT('Ctrl Pts',(59.2587247477834,249.938409910342,22.5143249322992)) ;
#113617 = CARTESIAN_POINT('Ctrl Pts',(59.2614861571016,249.95489270078,22.5806596168693)) ;
#113618 = CARTESIAN_POINT('Ctrl Pts',(59.2642475664199,249.967869816684,22.6475927205034)) ;
#113619 = CARTESIAN_POINT('Ctrl Pts',(59.2670136854443,249.980869065635,22.7146399815153)) ;
#113620 = CARTESIAN_POINT('Ctrl Pts',(59.2697798044686,249.990350625957,22.7822872022128)) ;
#113621 = CARTESIAN_POINT('Ctrl Pts',(59.272545923493,249.9962882853,22.8501316201319)) ;
#113622 = CARTESIAN_POINT('Ctrl Pts',(59.2748813912895,250.001301523002,22.907413483937)) ;
#113623 = CARTESIAN_POINT('Ctrl Pts',(59.277216859086,250.003789358227,22.9648356828553)) ;
#113624 = CARTESIAN_POINT('Ctrl Pts',(59.2795523268825,250.003764929479,23.0221571305627)) ;
#113625 = CARTESIAN_POINT('',(59.7795523268953,250.003764314891,23.0195557760669)) ;
#113626 = CARTESIAN_POINT('Ctrl Pts',(59.2795523269168,250.003764929478,23.0221571314038)) ;
#113627 = CARTESIAN_POINT('Ctrl Pts',(59.281495114458,250.003744608104,23.0698406809764)) ;
#113628 = CARTESIAN_POINT('Ctrl Pts',(59.2834379019993,250.001987440133,23.1174851609697)) ;
#113629 = CARTESIAN_POINT('Ctrl Pts',(59.2853806895405,249.998501062365,23.1650012267499)) ;
#113630 = CARTESIAN_POINT('Ctrl Pts',(59.2881770263262,249.993482970476,23.2333931223291)) ;
#113631 = CARTESIAN_POINT('Ctrl Pts',(59.2909733631119,249.984867830952,23.3016559393838)) ;
#113632 = CARTESIAN_POINT('Ctrl Pts',(59.2937696998977,249.972669240583,23.3693814266331)) ;
#113633 = CARTESIAN_POINT('Ctrl Pts',(59.2965618561942,249.960488886956,23.4370056651103)) ;
#113634 = CARTESIAN_POINT('Ctrl Pts',(59.2993540124907,249.944735801524,23.5040936889007)) ;
#113635 = CARTESIAN_POINT('Ctrl Pts',(59.3021461687872,249.925475432185,23.5702413604475)) ;
#113636 = CARTESIAN_POINT('Ctrl Pts',(59.3049350703268,249.906237514246,23.6363119250666)) ;
#113637 = CARTESIAN_POINT('Ctrl Pts',(59.3077239718664,249.883500568894,23.7014438454418)) ;
#113638 = CARTESIAN_POINT('Ctrl Pts',(59.310512873406,249.857380920474,23.7652439775968)) ;
#113639 = CARTESIAN_POINT('Ctrl Pts',(59.3133000442554,249.831277480952,23.8290045177253)) ;
#113640 = CARTESIAN_POINT('Ctrl Pts',(59.3160872151048,249.801795688275,23.8914344559288)) ;
#113641 = CARTESIAN_POINT('Ctrl Pts',(59.3188743859541,249.769100947178,23.9521580793838)) ;
#113642 = CARTESIAN_POINT('Ctrl Pts',(59.3216607786618,249.736415334026,24.0128647495953)) ;
#113643 = CARTESIAN_POINT('Ctrl Pts',(59.3244471713694,249.700518785888,24.0718656188556)) ;
#113644 = CARTESIAN_POINT('Ctrl Pts',(59.327233564077,249.661623060812,24.1288087805911)) ;
#113645 = CARTESIAN_POINT('Ctrl Pts',(59.3300201300365,249.622724917285,24.185755482929)) ;
#113646 = CARTESIAN_POINT('Ctrl Pts',(59.332806695996,249.580827505552,24.2406438198851)) ;
#113647 = CARTESIAN_POINT('Ctrl Pts',(59.3355932619555,249.536185365182,24.2931516348526)) ;
#113648 = CARTESIAN_POINT('Ctrl Pts',(59.3383827784955,249.491495955079,24.3457150481933)) ;
#113649 = CARTESIAN_POINT('Ctrl Pts',(59.3411722950355,249.444056334951,24.3958925345985)) ;
#113650 = CARTESIAN_POINT('Ctrl Pts',(59.3439618115755,249.394160064921,24.4433965352748)) ;
#113651 = CARTESIAN_POINT('Ctrl Pts',(59.3467529984094,249.344233918232,24.4909289801784)) ;
#113652 = CARTESIAN_POINT('Ctrl Pts',(59.3495441852432,249.291848566881,24.5357844340582)) ;
#113653 = CARTESIAN_POINT('Ctrl Pts',(59.3523353720771,249.237330899584,24.5777154540976)) ;
#113654 = CARTESIAN_POINT('Ctrl Pts',(59.3551313242139,249.182720156039,24.6197180616105)) ;
#113655 = CARTESIAN_POINT('Ctrl Pts',(59.3579272763508,249.125970235061,24.6587859926092)) ;
#113656 = CARTESIAN_POINT('Ctrl Pts',(59.3607232284876,249.067436492644,24.6947154541444)) ;
#113657 = CARTESIAN_POINT('Ctrl Pts',(59.3619838641671,249.041044866274,24.7109152883828)) ;
#113658 = CARTESIAN_POINT('Ctrl Pts',(59.3632444998465,249.014290925836,24.7264777260704)) ;
#113659 = CARTESIAN_POINT('Ctrl Pts',(59.364505135526,248.987208654823,24.7413872517713)) ;
#113660 = CARTESIAN_POINT('Ctrl Pts',(59.3673014722637,248.927134875691,24.7744594986845)) ;
#113661 = CARTESIAN_POINT('Ctrl Pts',(59.3700978090013,248.865208620798,24.8044456889588)) ;
#113662 = CARTESIAN_POINT('Ctrl Pts',(59.372894145739,248.801779571836,24.8311346906801)) ;
#113663 = CARTESIAN_POINT('Ctrl Pts',(59.3756863019872,248.738445348532,24.8577837926679)) ;
#113664 = CARTESIAN_POINT('Ctrl Pts',(59.3784784582354,248.673613239039,24.8811453005798)) ;
#113665 = CARTESIAN_POINT('Ctrl Pts',(59.3812706144836,248.607657739388,24.9010537958351)) ;
#113666 = CARTESIAN_POINT('Ctrl Pts',(59.3840595159747,248.541779122659,24.9209390841812)) ;
#113667 = CARTESIAN_POINT('Ctrl Pts',(59.3868484174658,248.474780184297,24.9373792129642)) ;
#113668 = CARTESIAN_POINT('Ctrl Pts',(59.3896373189569,248.40705393545,24.9502574098997)) ;
#113669 = CARTESIAN_POINT('Ctrl Pts',(59.3924244897578,248.339369715037,24.963127615097)) ;
#113670 = CARTESIAN_POINT('Ctrl Pts',(59.3952116605586,248.270959560639,24.9724401819621)) ;
#113671 = CARTESIAN_POINT('Ctrl Pts',(59.3979988313594,248.202228622381,24.9781289877402)) ;
#113672 = CARTESIAN_POINT('Ctrl Pts',(59.4007852240185,248.133516872904,24.983816205278)) ;
#113673 = CARTESIAN_POINT('Ctrl Pts',(59.4035716166776,248.064485006299,24.9858816298161)) ;
#113674 = CARTESIAN_POINT('Ctrl Pts',(59.4063580093366,247.995543480419,24.9843109767633)) ;
#113675 = CARTESIAN_POINT('Ctrl Pts',(59.4091445752477,247.926597667901,24.9827402260507)) ;
#113676 = CARTESIAN_POINT('Ctrl Pts',(59.4119311411587,247.857742697894,24.9775329626426)) ;
#113677 = CARTESIAN_POINT('Ctrl Pts',(59.4147177070697,247.789387405947,24.9687269854092)) ;
#113678 = CARTESIAN_POINT('Ctrl Pts',(59.4175072235617,247.72095973537,24.9599116838858)) ;
#113679 = CARTESIAN_POINT('Ctrl Pts',(59.4202967400537,247.653033286443,24.9474901268922)) ;
#113680 = CARTESIAN_POINT('Ctrl Pts',(59.4230862565456,247.586009158029,24.9315516861228)) ;
#113681 = CARTESIAN_POINT('Ctrl Pts',(59.4258774433317,247.51894489721,24.9156037018057)) ;
#113682 = CARTESIAN_POINT('Ctrl Pts',(59.4286686301177,247.452784503118,24.8961347811677)) ;
#113683 = CARTESIAN_POINT('Ctrl Pts',(59.4314598169038,247.387913609002,24.8732841045535)) ;
#113684 = CARTESIAN_POINT('Ctrl Pts',(59.4342557689936,247.322931962888,24.8503944157113)) ;
#113685 = CARTESIAN_POINT('Ctrl Pts',(59.4370517210834,247.259244663932,24.8241116352296)) ;
#113686 = CARTESIAN_POINT('Ctrl Pts',(59.4398476731733,247.197216267198,24.7946226027313)) ;
#113687 = CARTESIAN_POINT('Ctrl Pts',(59.441108309286,247.169248965032,24.7813266169264)) ;
#113688 = CARTESIAN_POINT('Ctrl Pts',(59.4423689453988,247.141618552985,24.7673794386527)) ;
#113689 = CARTESIAN_POINT('Ctrl Pts',(59.4436295815115,247.114356562801,24.7528011018482)) ;
#113690 = CARTESIAN_POINT('Ctrl Pts',(59.4464259182225,247.053884152725,24.7204635081688)) ;
#113691 = CARTESIAN_POINT('Ctrl Pts',(59.4492222549335,246.994989280571,24.6848906733036)) ;
#113692 = CARTESIAN_POINT('Ctrl Pts',(59.4520185916445,246.938039561295,24.6462606792835)) ;
#113693 = CARTESIAN_POINT('Ctrl Pts',(59.4548107478652,246.881174981174,24.6076884366464)) ;
#113694 = CARTESIAN_POINT('Ctrl Pts',(59.457602904086,246.826250185303,24.5660683793279)) ;
#113695 = CARTESIAN_POINT('Ctrl Pts',(59.4603950603067,246.773607989323,24.5216243108435)) ;
#113696 = CARTESIAN_POINT('Ctrl Pts',(59.4631839617694,246.721027157251,24.4772320498805)) ;
#113697 = CARTESIAN_POINT('Ctrl Pts',(59.465972863232,246.670724013783,24.4300226309442)) ;
#113698 = CARTESIAN_POINT('Ctrl Pts',(59.4687617646946,246.623010682701,24.3802618965991)) ;
#113699 = CARTESIAN_POINT('Ctrl Pts',(59.4715489354664,246.575326960779,24.3305320419574)) ;
#113700 = CARTESIAN_POINT('Ctrl Pts',(59.4743361062381,246.530230201944,24.2782543662651)) ;
#113701 = CARTESIAN_POINT('Ctrl Pts',(59.4771232770098,246.487996683113,24.2237324974251)) ;
#113702 = CARTESIAN_POINT('Ctrl Pts',(59.4799096696393,246.445774955338,24.1692258503911)) ;
#113703 = CARTESIAN_POINT('Ctrl Pts',(59.4826960622687,246.406415180982,24.1124766419585)) ;
#113704 = CARTESIAN_POINT('Ctrl Pts',(59.4854824548981,246.370153069959,24.0538212060807)) ;
#113705 = CARTESIAN_POINT('Ctrl Pts',(59.488269020779,246.333888704243,23.9951621231441)) ;
#113706 = CARTESIAN_POINT('Ctrl Pts',(59.4910555866598,246.30072264016,23.934596996283)) ;
#113707 = CARTESIAN_POINT('Ctrl Pts',(59.4938421525407,246.270846037523,23.8724891892)) ;
#113708 = CARTESIAN_POINT('Ctrl Pts',(59.4966316690019,246.240937799777,23.8103156187065)) ;
#113709 = CARTESIAN_POINT('Ctrl Pts',(59.4994211854631,246.214326187638,23.7465965512806)) ;
#113710 = CARTESIAN_POINT('Ctrl Pts',(59.5022107019243,246.191154906077,23.681716975847)) ;
#113711 = CARTESIAN_POINT('Ctrl Pts',(59.5050018886792,246.167969750124,23.6167985521223)) ;
#113712 = CARTESIAN_POINT('Ctrl Pts',(59.5077930754341,246.148229165143,23.5507187077312)) ;
#113713 = CARTESIAN_POINT('Ctrl Pts',(59.5105842621891,246.132026667399,23.4838766154112)) ;
#113714 = CARTESIAN_POINT('Ctrl Pts',(59.5133802142475,246.115796507651,23.4169204057341)) ;
#113715 = CARTESIAN_POINT('Ctrl Pts',(59.5161761663059,246.103116580869,23.3491998330277)) ;
#113716 = CARTESIAN_POINT('Ctrl Pts',(59.5189721183643,246.09402895728,23.2811223767758)) ;
#113717 = CARTESIAN_POINT('Ctrl Pts',(59.5202327547419,246.089931537638,23.2504276738445)) ;
#113718 = CARTESIAN_POINT('Ctrl Pts',(59.5214933911195,246.086563699403,23.2196604587693)) ;
#113719 = CARTESIAN_POINT('Ctrl Pts',(59.522754027497,246.083925833939,23.1888580873807)) ;
#113720 = CARTESIAN_POINT('Ctrl Pts',(59.525550364206,246.078074535212,23.1205324358522)) ;
#113721 = CARTESIAN_POINT('Ctrl Pts',(59.528346700915,246.075795493367,23.0517658849627)) ;
#113722 = CARTESIAN_POINT('Ctrl Pts',(59.531143037624,246.077139788722,22.9829637059369)) ;
#113723 = CARTESIAN_POINT('Ctrl Pts',(59.5339351938432,246.078482074372,22.9142643853419)) ;
#113724 = CARTESIAN_POINT('Ctrl Pts',(59.5367273500625,246.083436936639,22.8455300291764)) ;
#113725 = CARTESIAN_POINT('Ctrl Pts',(59.5395195062817,246.09200360609,22.7771700394243)) ;
#113726 = CARTESIAN_POINT('Ctrl Pts',(59.5423084077435,246.100560289555,22.7088897354664)) ;
#113727 = CARTESIAN_POINT('Ctrl Pts',(59.5450973092052,246.112720357553,22.6409834159562)) ;
#113728 = CARTESIAN_POINT('Ctrl Pts',(59.547886210667,246.128431066251,22.573857666201)) ;
#113729 = CARTESIAN_POINT('Ctrl Pts',(59.5506733814383,246.144132025457,22.5067735722365)) ;
#113730 = CARTESIAN_POINT('Ctrl Pts',(59.5534605522096,246.163379142651,22.4404695639475)) ;
#113731 = CARTESIAN_POINT('Ctrl Pts',(59.5562477229809,246.186068455924,22.3753427694719)) ;
#113732 = CARTESIAN_POINT('Ctrl Pts',(59.5590341156103,246.208751434635,22.3102341575516)) ;
#113733 = CARTESIAN_POINT('Ctrl Pts',(59.5618205082397,246.234874540101,22.2463025702368)) ;
#113734 = CARTESIAN_POINT('Ctrl Pts',(59.5646069008691,246.264284277843,22.1839289525864)) ;
#113735 = CARTESIAN_POINT('Ctrl Pts',(59.5673934667504,246.293695844219,22.12155145668)) ;
#113736 = CARTESIAN_POINT('Ctrl Pts',(59.5701800326316,246.326394236939,22.0607325656101)) ;
#113737 = CARTESIAN_POINT('Ctrl Pts',(59.5729665985129,246.36217901674,22.0018306079372)) ;
#113738 = CARTESIAN_POINT('Ctrl Pts',(59.5757561149751,246.398001687586,21.9428662813831)) ;
#113739 = CARTESIAN_POINT('Ctrl Pts',(59.5785456314373,246.436917012061,21.8858233591829)) ;
#113740 = CARTESIAN_POINT('Ctrl Pts',(59.5813351478996,246.478680553845,21.8310321721944)) ;
#113741 = CARTESIAN_POINT('Ctrl Pts',(59.5841263346559,246.520469102614,21.7762081775863)) ;
#113742 = CARTESIAN_POINT('Ctrl Pts',(59.5869175214122,246.565108945219,21.7236389757832)) ;
#113743 = CARTESIAN_POINT('Ctrl Pts',(59.5897087081685,246.612316396838,21.6736205517286)) ;
#113744 = CARTESIAN_POINT('Ctrl Pts',(59.5925046602289,246.659604444231,21.6235167328156)) ;
#113745 = CARTESIAN_POINT('Ctrl Pts',(59.5953006122892,246.709468494342,21.5759727215004)) ;
#113746 = CARTESIAN_POINT('Ctrl Pts',(59.5980965643495,246.761589855718,21.5312458991949)) ;
#113747 = CARTESIAN_POINT('Ctrl Pts',(59.5993572007272,246.785090288768,21.5110795093427)) ;
#113748 = CARTESIAN_POINT('Ctrl Pts',(59.6006178371049,246.80904919775,21.4914852618308)) ;
#113749 = CARTESIAN_POINT('Ctrl Pts',(59.6018784734826,246.833435477553,21.4724838468335)) ;
#113750 = CARTESIAN_POINT('Ctrl Pts',(59.604674810223,246.887528990464,21.4303350116772)) ;
#113751 = CARTESIAN_POINT('Ctrl Pts',(59.6074711469633,246.943939325071,21.3909407634578)) ;
#113752 = CARTESIAN_POINT('Ctrl Pts',(59.6102674837036,247.002354552538,21.3545648338025)) ;
#113753 = CARTESIAN_POINT('Ctrl Pts',(59.6130596399539,247.060682449938,21.318243285728)) ;
#113754 = CARTESIAN_POINT('Ctrl Pts',(59.6158517962042,247.121008877979,21.2849313577405)) ;
#113755 = CARTESIAN_POINT('Ctrl Pts',(59.6186439524545,247.182990182206,21.2548515632037)) ;
#113756 = CARTESIAN_POINT('Ctrl Pts',(59.6214328539467,247.244899236126,21.224806832053)) ;
#113757 = CARTESIAN_POINT('Ctrl Pts',(59.624221755439,247.308458895413,21.1979869647537)) ;
#113758 = CARTESIAN_POINT('Ctrl Pts',(59.6270106569312,247.373299536651,21.1745693649704)) ;
#113759 = CARTESIAN_POINT('Ctrl Pts',(59.6297978277326,247.438099940145,21.151166297298)) ;
#113760 = CARTESIAN_POINT('Ctrl Pts',(59.632584998534,247.504179287979,21.1311614750551)) ;
#113761 = CARTESIAN_POINT('Ctrl Pts',(59.6353721693355,247.571147967304,21.1146842066668)) ;
#113762 = CARTESIAN_POINT('Ctrl Pts',(59.6381585619946,247.638097949833,21.0982115385202)) ;
#113763 = CARTESIAN_POINT('Ctrl Pts',(59.6409449546537,247.705936294524,21.0852645862101)) ;
#113764 = CARTESIAN_POINT('Ctrl Pts',(59.6437313473128,247.774259956716,21.075922309839)) ;
#113765 = CARTESIAN_POINT('Ctrl Pts',(59.6465179132233,247.842587867113,21.0665794525869)) ;
#113766 = CARTESIAN_POINT('Ctrl Pts',(59.6493044791337,247.911400668276,21.0608417801967)) ;
#113767 = CARTESIAN_POINT('Ctrl Pts',(59.6520910450442,247.980288687947,21.0587365672425)) ;
#113768 = CARTESIAN_POINT('Ctrl Pts',(59.6548805615348,248.04924965031,21.0566291251647)) ;
#113769 = CARTESIAN_POINT('Ctrl Pts',(59.6576700780254,248.118285498609,21.0581618333255)) ;
#113770 = CARTESIAN_POINT('Ctrl Pts',(59.660459594516,248.186986051253,21.063309818882)) ;
#113771 = CARTESIAN_POINT('Ctrl Pts',(59.6632507813002,248.255727740091,21.0684608869251)) ;
#113772 = CARTESIAN_POINT('Ctrl Pts',(59.6660419680844,248.324133246809,21.0772314783119)) ;
#113773 = CARTESIAN_POINT('Ctrl Pts',(59.6688331548686,248.391799791067,21.0895450935756)) ;
#113774 = CARTESIAN_POINT('Ctrl Pts',(59.6716291069559,248.45958186023,21.1018797314769)) ;
#113775 = CARTESIAN_POINT('Ctrl Pts',(59.6744250590431,248.526621971747,21.1177693524047)) ;
#113776 = CARTESIAN_POINT('Ctrl Pts',(59.6772210111303,248.592530628211,21.1370870658179)) ;
#113777 = CARTESIAN_POINT('Ctrl Pts',(59.6784816472429,248.622247458071,21.1457970173412)) ;
#113778 = CARTESIAN_POINT('Ctrl Pts',(59.6797422833555,248.65173452234,21.1552032118979)) ;
#113779 = CARTESIAN_POINT('Ctrl Pts',(59.6810029194681,248.680957519887,21.1652908494308)) ;
#113780 = CARTESIAN_POINT('Ctrl Pts',(59.6837992562552,248.745779828445,21.1876671970908)) ;
#113781 = CARTESIAN_POINT('Ctrl Pts',(59.6865955930423,248.809555604496,21.2134874063395)) ;
#113782 = CARTESIAN_POINT('Ctrl Pts',(59.6893919298294,248.871893712924,21.2426337176708)) ;
#113783 = CARTESIAN_POINT('Ctrl Pts',(59.692184086127,248.934138626638,21.2717364556212)) ;
#113784 = CARTESIAN_POINT('Ctrl Pts',(59.6949762424246,248.994949697429,21.3041552202896)) ;
#113785 = CARTESIAN_POINT('Ctrl Pts',(59.6977683987222,249.053953053683,21.3397231865858)) ;
#113786 = CARTESIAN_POINT('Ctrl Pts',(59.7005573002624,249.112887630976,21.3752496920575)) ;
#113787 = CARTESIAN_POINT('Ctrl Pts',(59.7033462018026,249.170018260476,21.4139178560407)) ;
#113788 = CARTESIAN_POINT('Ctrl Pts',(59.7061351033428,249.224994734446,21.4555144929788)) ;
#113789 = CARTESIAN_POINT('Ctrl Pts',(59.7089222741924,249.279937092024,21.4970853165624)) ;
#113790 = CARTESIAN_POINT('Ctrl Pts',(59.7117094450421,249.332727555446,21.5415807124321)) ;
#113791 = CARTESIAN_POINT('Ctrl Pts',(59.7144966158918,249.383045343216,21.5887445203175)) ;
#113792 = CARTESIAN_POINT('Ctrl Pts',(59.7172830085995,249.433349082911,21.6358951606779)) ;
#113793 = CARTESIAN_POINT('Ctrl Pts',(59.7200694013071,249.48118115955,21.6857123985147)) ;
#113794 = CARTESIAN_POINT('Ctrl Pts',(59.7228557940148,249.526255681274,21.7379013685143)) ;
#113795 = CARTESIAN_POINT('Ctrl Pts',(59.725642359974,249.571333005628,21.7900935835056)) ;
#113796 = CARTESIAN_POINT('Ctrl Pts',(59.7284289259332,249.61365211579,21.8446574502999)) ;
#113797 = CARTESIAN_POINT('Ctrl Pts',(59.7312154918924,249.652966839496,21.9012643741811)) ;
#113798 = CARTESIAN_POINT('Ctrl Pts',(59.7340050084317,249.692323191944,21.957931236805)) ;
#113799 = CARTESIAN_POINT('Ctrl Pts',(59.7367945249709,249.72866852883,22.0166450698258)) ;
#113800 = CARTESIAN_POINT('Ctrl Pts',(59.7395840415102,249.761800119688,22.0770484267928)) ;
#113801 = CARTESIAN_POINT('Ctrl Pts',(59.7423752283431,249.794951548925,22.137487951799)) ;
#113802 = CARTESIAN_POINT('Ctrl Pts',(59.745166415176,249.824885189213,22.1996185719547)) ;
#113803 = CARTESIAN_POINT('Ctrl Pts',(59.7479576020089,249.851445627197,22.263060905038)) ;
#113804 = CARTESIAN_POINT('Ctrl Pts',(59.7507535541444,249.878051410953,22.3266115511548)) ;
#113805 = CARTESIAN_POINT('Ctrl Pts',(59.7535495062799,249.901272333448,22.3914779178315)) ;
#113806 = CARTESIAN_POINT('Ctrl Pts',(59.7563454584154,249.921002468584,22.4572642916478)) ;
#113807 = CARTESIAN_POINT('Ctrl Pts',(59.7576060940948,249.929898369196,22.4869259761237)) ;
#113808 = CARTESIAN_POINT('Ctrl Pts',(59.7588667297742,249.938085311495,22.5167745401338)) ;
#113809 = CARTESIAN_POINT('Ctrl Pts',(59.7601273654536,249.945557006586,22.5467731590084)) ;
#113810 = CARTESIAN_POINT('Ctrl Pts',(59.7637661613916,249.967123882878,22.633363483467)) ;
#113811 = CARTESIAN_POINT('Ctrl Pts',(59.7674049573295,249.982796529675,22.7214759039678)) ;
#113812 = CARTESIAN_POINT('Ctrl Pts',(59.7710437532675,249.992405426665,22.8104165137978)) ;
#113813 = CARTESIAN_POINT('Ctrl Pts',(59.7738799444767,249.999894901106,22.879739603097)) ;
#113814 = CARTESIAN_POINT('Ctrl Pts',(59.776716135686,250.003701415725,22.9495655586124)) ;
#113815 = CARTESIAN_POINT('Ctrl Pts',(59.7795523268953,250.003764314891,23.019555776067)) ;
#113816 = CARTESIAN_POINT('',(60.2795523269397,250.003764993893,23.0219891156808)) ;
#113817 = CARTESIAN_POINT('Ctrl Pts',(59.7795523269168,250.003764314891,23.0195557765974)) ;
#113818 = CARTESIAN_POINT('Ctrl Pts',(59.7823087837182,250.003825445742,23.0875783451414)) ;
#113819 = CARTESIAN_POINT('Ctrl Pts',(59.7850652405196,250.000347506381,23.1556930422578)) ;
#113820 = CARTESIAN_POINT('Ctrl Pts',(59.787821697321,249.993328455219,23.2234980152068)) ;
#113821 = CARTESIAN_POINT('Ctrl Pts',(59.7905763409642,249.98631402109,23.2912583870053)) ;
#113822 = CARTESIAN_POINT('Ctrl Pts',(59.7933309846074,249.97576314405,23.3587089388388)) ;
#113823 = CARTESIAN_POINT('Ctrl Pts',(59.7960856282505,249.961725799627,23.4254503470355)) ;
#113824 = CARTESIAN_POINT('Ctrl Pts',(59.7988394545505,249.947692620291,23.4921719520753)) ;
#113825 = CARTESIAN_POINT('Ctrl Pts',(59.8015932808504,249.930175129706,23.5581843383787)) ;
#113826 = CARTESIAN_POINT('Ctrl Pts',(59.8043471071503,249.909274517264,23.6230977752439)) ;
#113827 = CARTESIAN_POINT('Ctrl Pts',(59.8071011106438,249.888372559981,23.6880153889329)) ;
#113828 = CARTESIAN_POINT('Ctrl Pts',(59.8098551141374,249.864087206595,23.7518334345976)) ;
#113829 = CARTESIAN_POINT('Ctrl Pts',(59.8126091176309,249.836569075627,23.8141786569548)) ;
#113830 = CARTESIAN_POINT('Ctrl Pts',(59.8153659991076,249.809022187717,23.8765890311893)) ;
#113831 = CARTESIAN_POINT('Ctrl Pts',(59.8181228805843,249.778235988887,23.9375230514109)) ;
#113832 = CARTESIAN_POINT('Ctrl Pts',(59.8208797620609,249.744408177207,23.9966298579936)) ;
#113833 = CARTESIAN_POINT('Ctrl Pts',(59.8236383977984,249.71055884019,24.0557742754617)) ;
#113834 = CARTESIAN_POINT('Ctrl Pts',(59.8263970335359,249.673664315791,24.1130887454574)) ;
#113835 = CARTESIAN_POINT('Ctrl Pts',(59.8291556692733,249.633965373405,24.1682517771538)) ;
#113836 = CARTESIAN_POINT('Ctrl Pts',(59.8319188058152,249.594201660896,24.2235048091405)) ;
#113837 = CARTESIAN_POINT('Ctrl Pts',(59.8346819423571,249.551624723831,24.2765990144869)) ;
#113838 = CARTESIAN_POINT('Ctrl Pts',(59.837445078899,249.50651445534,24.3272472560621)) ;
#113839 = CARTESIAN_POINT('Ctrl Pts',(59.838047323079,249.496682369141,24.3382863807149)) ;
#113840 = CARTESIAN_POINT('Ctrl Pts',(59.8386495672591,249.486730067739,24.3492094562372)) ;
#113841 = CARTESIAN_POINT('Ctrl Pts',(59.8392518114391,249.476660661121,24.3600137604257)) ;
#113842 = CARTESIAN_POINT('Ctrl Pts',(59.8420481483943,249.429906446177,24.4101802478372)) ;
#113843 = CARTESIAN_POINT('Ctrl Pts',(59.8448444853495,249.380429270683,24.4579928233434)) ;
#113844 = CARTESIAN_POINT('Ctrl Pts',(59.8476408223046,249.328495473826,24.5031417815248)) ;
#113845 = CARTESIAN_POINT('Ctrl Pts',(59.850432978768,249.276639317402,24.5482232425296)) ;
#113846 = CARTESIAN_POINT('Ctrl Pts',(59.8532251352314,249.222334196329,24.5906486701504)) ;
#113847 = CARTESIAN_POINT('Ctrl Pts',(59.8560172916948,249.165884289625,24.6301440466038)) ;
#113848 = CARTESIAN_POINT('Ctrl Pts',(59.8588061933965,249.109500185461,24.6695933840776)) ;
#113849 = CARTESIAN_POINT('Ctrl Pts',(59.8615950950983,249.050976661485,24.7061191738545)) ;
#113850 = CARTESIAN_POINT('Ctrl Pts',(59.8643839968001,248.990650667072,24.7394878379269)) ;
#113851 = CARTESIAN_POINT('Ctrl Pts',(59.8671711678087,248.930362108825,24.7728357945933)) ;
#113852 = CARTESIAN_POINT('Ctrl Pts',(59.8699583388173,248.868273727674,24.8030302751666)) ;
#113853 = CARTESIAN_POINT('Ctrl Pts',(59.8727455098259,248.804749810678,24.8298820342529)) ;
#113854 = CARTESIAN_POINT('Ctrl Pts',(59.8755319026895,248.741243628803,24.8567262966479)) ;
#113855 = CARTESIAN_POINT('Ctrl Pts',(59.8783182955532,248.676303158655,24.8802294993315)) ;
#113856 = CARTESIAN_POINT('Ctrl Pts',(59.8811046884168,248.610313905732,24.9002499904492)) ;
#113857 = CARTESIAN_POINT('Ctrl Pts',(59.8838912545289,248.544320549821,24.920271726373)) ;
#113858 = CARTESIAN_POINT('Ctrl Pts',(59.886677820641,248.477278752097,24.9368101807817)) ;
#113859 = CARTESIAN_POINT('Ctrl Pts',(59.8894643867531,248.409588729042,24.9497736908776)) ;
#113860 = CARTESIAN_POINT('Ctrl Pts',(59.8922539034395,248.34182703195,24.9627509274737)) ;
#113861 = CARTESIAN_POINT('Ctrl Pts',(59.8950434201259,248.273416222728,24.9721455730314)) ;
#113862 = CARTESIAN_POINT('Ctrl Pts',(59.8978329368124,248.204765260421,24.9779173766206)) ;
#113863 = CARTESIAN_POINT('Ctrl Pts',(59.9006241237894,248.136073191688,24.9836926362169)) ;
#113864 = CARTESIAN_POINT('Ctrl Pts',(59.9034153107664,248.067141174311,24.9858407211747)) ;
#113865 = CARTESIAN_POINT('Ctrl Pts',(59.9062064977434,247.998379016395,24.9843735281035)) ;
#113866 = CARTESIAN_POINT('Ctrl Pts',(59.9090024500169,247.929499463239,24.9829038301446)) ;
#113867 = CARTESIAN_POINT('Ctrl Pts',(59.9117984022903,247.86079083748,24.9778065719949)) ;
#113868 = CARTESIAN_POINT('Ctrl Pts',(59.9145943545638,247.792657793264,24.969145507119)) ;
#113869 = CARTESIAN_POINT('Ctrl Pts',(59.9158549888508,247.761938080188,24.9652404206667)) ;
#113870 = CARTESIAN_POINT('Ctrl Pts',(59.9171156231378,247.731335235253,24.960611534983)) ;
#113871 = CARTESIAN_POINT('Ctrl Pts',(59.9183762574247,247.700885467052,24.9552680443662)) ;
#113872 = CARTESIAN_POINT('Ctrl Pts',(59.9211725946597,247.633341833265,24.943415120857)) ;
#113873 = CARTESIAN_POINT('Ctrl Pts',(59.9239689318947,247.566287434072,24.9279962372579)) ;
#113874 = CARTESIAN_POINT('Ctrl Pts',(59.9267652691297,247.500127098043,24.9090658720751)) ;
#113875 = CARTESIAN_POINT('Ctrl Pts',(59.9295574258795,247.434065670794,24.8901638075247)) ;
#113876 = CARTESIAN_POINT('Ctrl Pts',(59.9323495826293,247.368896122028,24.8677608145071)) ;
#113877 = CARTESIAN_POINT('Ctrl Pts',(59.9351417393791,247.305013986331,24.8419625484971)) ;
#113878 = CARTESIAN_POINT('Ctrl Pts',(59.9379306413755,247.241206316582,24.8161943549369)) ;
#113879 = CARTESIAN_POINT('Ctrl Pts',(59.9407195433719,247.17868353234,24.787038931905)) ;
#113880 = CARTESIAN_POINT('Ctrl Pts',(59.9435084453682,247.117825126815,24.7546514520054)) ;
#113881 = CARTESIAN_POINT('Ctrl Pts',(59.9462956166763,247.057004487741,24.7222840705649)) ;
#113882 = CARTESIAN_POINT('Ctrl Pts',(59.9490827879844,246.997846610751,24.6866888412325)) ;
#113883 = CARTESIAN_POINT('Ctrl Pts',(59.9518699592925,246.940708722735,24.6480680210107)) ;
#113884 = CARTESIAN_POINT('Ctrl Pts',(59.95465635246,246.883586786844,24.6094579831999)) ;
#113885 = CARTESIAN_POINT('Ctrl Pts',(59.9574427456276,246.828484126762,24.5678243062383)) ;
#113886 = CARTESIAN_POINT('Ctrl Pts',(59.9602291387951,246.775729633658,24.5234129787429)) ;
#113887 = CARTESIAN_POINT('Ctrl Pts',(59.9630157052149,246.722971860386,24.4789988898405)) ;
#113888 = CARTESIAN_POINT('Ctrl Pts',(59.9658022716348,246.672562917786,24.431807125583)) ;
#113889 = CARTESIAN_POINT('Ctrl Pts',(59.9685888380547,246.624797805843,24.3821232562294)) ;
#113890 = CARTESIAN_POINT('Ctrl Pts',(59.9713783550525,246.576982117431,24.3323867787157)) ;
#113891 = CARTESIAN_POINT('Ctrl Pts',(59.9741678720504,246.531816187178,24.280153284517)) ;
#113892 = CARTESIAN_POINT('Ctrl Pts',(59.9769573890482,246.489556677735,24.2257436972719)) ;
#113893 = CARTESIAN_POINT('Ctrl Pts',(59.9797485763392,246.447271864352,24.1713015309245)) ;
#113894 = CARTESIAN_POINT('Ctrl Pts',(59.9825397636302,246.407897215653,24.1146810812581)) ;
#113895 = CARTESIAN_POINT('Ctrl Pts',(59.9853309509212,246.371646137567,24.0562324085314)) ;
#113896 = CARTESIAN_POINT('Ctrl Pts',(59.9881269035092,246.335333169275,23.997683948419)) ;
#113897 = CARTESIAN_POINT('Ctrl Pts',(59.9909228560971,246.302154650851,23.9373014657754)) ;
#113898 = CARTESIAN_POINT('Ctrl Pts',(59.9937188086851,246.272277703052,23.8754589662088)) ;
#113899 = CARTESIAN_POINT('Ctrl Pts',(59.9949794402601,246.258806865269,23.847575586509)) ;
#113900 = CARTESIAN_POINT('Ctrl Pts',(59.9962400718352,246.246006547433,23.8193956568979)) ;
#113901 = CARTESIAN_POINT('Ctrl Pts',(59.9975007034102,246.233888777856,23.7909545454175)) ;
#113902 = CARTESIAN_POINT('Ctrl Pts',(60.0002970378614,246.207009127045,23.7278664382821)) ;
#113903 = CARTESIAN_POINT('Ctrl Pts',(60.0030933723127,246.183385777887,23.663244750275)) ;
#113904 = CARTESIAN_POINT('Ctrl Pts',(60.0058897067639,246.163193722276,23.59745857671)) ;
#113905 = CARTESIAN_POINT('Ctrl Pts',(60.0086818607232,246.143031853584,23.531770752814)) ;
#113906 = CARTESIAN_POINT('Ctrl Pts',(60.0114740146825,246.126291240063,23.4649223641062)) ;
#113907 = CARTESIAN_POINT('Ctrl Pts',(60.0142661686418,246.113098901805,23.3973026097979)) ;
#113908 = CARTESIAN_POINT('Ctrl Pts',(60.0170550678515,246.099921941553,23.3297616782809)) ;
#113909 = CARTESIAN_POINT('Ctrl Pts',(60.0198439670612,246.090285135311,23.2614516464973)) ;
#113910 = CARTESIAN_POINT('Ctrl Pts',(60.0226328662709,246.084265245048,23.1927752559079)) ;
#113911 = CARTESIAN_POINT('Ctrl Pts',(60.0254200347964,246.078249090498,23.1241414832611)) ;
#113912 = CARTESIAN_POINT('Ctrl Pts',(60.0282072033219,246.075845442013,23.0551422906988)) ;
#113913 = CARTESIAN_POINT('Ctrl Pts',(60.0309943718473,246.077079449864,22.9861874169946)) ;
#113914 = CARTESIAN_POINT('Ctrl Pts',(60.0337807622405,246.0783131132,22.9172517943728)) ;
#113915 = CARTESIAN_POINT('Ctrl Pts',(60.0365671526338,246.083182407858,22.8483609565684)) ;
#113916 = CARTESIAN_POINT('Ctrl Pts',(60.039353543027,246.091660374989,22.7799247236318)) ;
#113917 = CARTESIAN_POINT('Ctrl Pts',(60.0421401066851,246.100138869301,22.7114842351551)) ;
#113918 = CARTESIAN_POINT('Ctrl Pts',(60.0449266703432,246.112226418696,22.6434988944507)) ;
#113919 = CARTESIAN_POINT('Ctrl Pts',(60.0477132340013,246.127844406267,22.5763716831496)) ;
#113920 = CARTESIAN_POINT('Ctrl Pts',(60.0505027482751,246.143478931295,22.5091733926874)) ;
#113921 = CARTESIAN_POINT('Ctrl Pts',(60.053292262549,246.16265124336,22.442835523928)) ;
#113922 = CARTESIAN_POINT('Ctrl Pts',(60.0560817768228,246.185232188868,22.3777481877512)) ;
#113923 = CARTESIAN_POINT('Ctrl Pts',(60.0588729614075,246.20782665544,22.3126218784513)) ;
#113924 = CARTESIAN_POINT('Ctrl Pts',(60.0616641459922,246.233833632505,22.2487480466602)) ;
#113925 = CARTESIAN_POINT('Ctrl Pts',(60.0644553305769,246.263075960335,22.1864964195009)) ;
#113926 = CARTESIAN_POINT('Ctrl Pts',(60.0672512805139,246.2923682132,22.1241385109683)) ;
#113927 = CARTESIAN_POINT('Ctrl Pts',(60.0700472304508,246.324906609224,22.0634087668915)) ;
#113928 = CARTESIAN_POINT('Ctrl Pts',(60.0728431803877,246.36046868405,22.0046511619653)) ;
#113929 = CARTESIAN_POINT('Ctrl Pts',(60.0741038367237,246.376503146741,21.978158145778)) ;
#113930 = CARTESIAN_POINT('Ctrl Pts',(60.0753644930597,246.393151745223,21.9520656520359)) ;
#113931 = CARTESIAN_POINT('Ctrl Pts',(60.0766251493957,246.4103913826,21.9264030453364)) ;
#113932 = CARTESIAN_POINT('Ctrl Pts',(60.0794214890823,246.448631687118,21.8694792322975)) ;
#113933 = CARTESIAN_POINT('Ctrl Pts',(60.082217828769,246.489932684402,21.8144495207951)) ;
#113934 = CARTESIAN_POINT('Ctrl Pts',(60.0850141684556,246.534080315867,21.7616618094353)) ;
#113935 = CARTESIAN_POINT('Ctrl Pts',(60.0878063276356,246.578161946956,21.7089530153048)) ;
#113936 = CARTESIAN_POINT('Ctrl Pts',(60.0905984868155,246.62508145335,21.658479942422)) ;
#113937 = CARTESIAN_POINT('Ctrl Pts',(60.0933906459954,246.674581773116,21.6105612289672)) ;
#113938 = CARTESIAN_POINT('Ctrl Pts',(60.0961795503789,246.724024390776,21.5626983739544)) ;
#113939 = CARTESIAN_POINT('Ctrl Pts',(60.0989684547623,246.776041495738,21.5173843043578)) ;
#113940 = CARTESIAN_POINT('Ctrl Pts',(60.1017573591458,246.830337277652,21.4749029044874)) ;
#113941 = CARTESIAN_POINT('Ctrl Pts',(60.1045445328128,246.884599365114,21.4324478673915)) ;
#113942 = CARTESIAN_POINT('Ctrl Pts',(60.1073317064798,246.941136938552,21.3928223145322)) ;
#113943 = CARTESIAN_POINT('Ctrl Pts',(60.1101188801468,246.999620188514,21.356270674032)) ;
#113944 = CARTESIAN_POINT('Ctrl Pts',(60.1129052756417,247.058087110096,21.3197292386605)) ;
#113945 = CARTESIAN_POINT('Ctrl Pts',(60.1156916711366,247.118498213693,21.28626027181)) ;
#113946 = CARTESIAN_POINT('Ctrl Pts',(60.1184780666315,247.180495217874,21.2560645585811)) ;
#113947 = CARTESIAN_POINT('Ctrl Pts',(60.1212646353438,247.242496076122,21.2258669682236)) ;
#113948 = CARTESIAN_POINT('Ctrl Pts',(60.1240512040562,247.306082588296,21.1989432480789)) ;
#113949 = CARTESIAN_POINT('Ctrl Pts',(60.1268377727685,247.370874048168,21.1754471465864)) ;
#113950 = CARTESIAN_POINT('Ctrl Pts',(60.129627291991,247.435734111359,21.1519261666527)) ;
#113951 = CARTESIAN_POINT('Ctrl Pts',(60.1324168112134,247.501801206085,21.1318402157681)) ;
#113952 = CARTESIAN_POINT('Ctrl Pts',(60.1352063304359,247.568677869959,21.1152936577236)) ;
#113953 = CARTESIAN_POINT('Ctrl Pts',(60.1379975199159,247.635594577025,21.0987371922322)) ;
#113954 = CARTESIAN_POINT('Ctrl Pts',(60.1407887093959,247.703321335937,21.085724430048)) ;
#113955 = CARTESIAN_POINT('Ctrl Pts',(60.143579898876,247.771451606222,21.0763083766615)) ;
#113956 = CARTESIAN_POINT('Ctrl Pts',(60.146375853576,247.839698190977,21.0668762478468)) ;
#113957 = CARTESIAN_POINT('Ctrl Pts',(60.1491718082761,247.90834917322,21.0610531242606)) ;
#113958 = CARTESIAN_POINT('Ctrl Pts',(60.1519677629761,247.976994907934,21.0588399916043)) ;
#113959 = CARTESIAN_POINT('Ctrl Pts',(60.1532283737778,248.007945178576,21.0578421575077)) ;
#113960 = CARTESIAN_POINT('Ctrl Pts',(60.1544889845795,248.03889441398,21.0575774690528)) ;
#113961 = CARTESIAN_POINT('Ctrl Pts',(60.1557495953812,248.069805409754,21.0580425688778)) ;
#113962 = CARTESIAN_POINT('Ctrl Pts',(60.1585459356804,248.138373490443,21.0590742730182)) ;
#113963 = CARTESIAN_POINT('Ctrl Pts',(60.1613422759796,248.207021923866,21.063704453176)) ;
#113964 = CARTESIAN_POINT('Ctrl Pts',(60.1641386162787,248.275342358042,21.0719432798769)) ;
#113965 = CARTESIAN_POINT('Ctrl Pts',(60.166930776137,248.343560655314,21.0801697897905)) ;
#113966 = CARTESIAN_POINT('Ctrl Pts',(60.1697229359952,248.411451443118,21.0919941806046)) ;
#113967 = CARTESIAN_POINT('Ctrl Pts',(60.1725150958534,248.478607460541,21.1073746202483)) ;
#113968 = CARTESIAN_POINT('Ctrl Pts',(60.1753040010076,248.545685197001,21.1227371315563)) ;
#113969 = CARTESIAN_POINT('Ctrl Pts',(60.1780929061617,248.612029387947,21.1416473499608)) ;
#113970 = CARTESIAN_POINT('Ctrl Pts',(60.1808818113159,248.677240788408,21.164012013665)) ;
#113971 = CARTESIAN_POINT('Ctrl Pts',(60.1836689858104,248.742411721828,21.1863627989404)) ;
#113972 = CARTESIAN_POINT('Ctrl Pts',(60.1864561603049,248.806450796026,21.2121636180408)) ;
#113973 = CARTESIAN_POINT('Ctrl Pts',(60.1892433347993,248.868973313096,21.2412711980438)) ;
#113974 = CARTESIAN_POINT('Ctrl Pts',(60.1920297311767,248.93147837527,21.2703706518581)) ;
#113975 = CARTESIAN_POINT('Ctrl Pts',(60.1948161275541,248.992467276113,21.3027748267235)) ;
#113976 = CARTESIAN_POINT('Ctrl Pts',(60.1976025239315,249.051576387676,21.3382927902592)) ;
#113977 = CARTESIAN_POINT('Ctrl Pts',(60.2003890935795,249.110689174908,21.3738129624615)) ;
#113978 = CARTESIAN_POINT('Ctrl Pts',(60.2031756632276,249.167921521403,21.4124470527529)) ;
#113979 = CARTESIAN_POINT('Ctrl Pts',(60.2059622328756,249.222937010551,21.4539596893355)) ;
#113980 = CARTESIAN_POINT('Ctrl Pts',(60.2087517531066,249.278010753319,21.4955162819267)) ;
#113981 = CARTESIAN_POINT('Ctrl Pts',(60.2115412733376,249.330862561746,21.539957207296)) ;
#113982 = CARTESIAN_POINT('Ctrl Pts',(60.2143307935686,249.381188288939,21.5870061268527)) ;
#113983 = CARTESIAN_POINT('Ctrl Pts',(60.2171219841002,249.431544150019,21.6340832182205)) ;
#113984 = CARTESIAN_POINT('Ctrl Pts',(60.2199131746318,249.479370579081,21.6837710581063)) ;
#113985 = CARTESIAN_POINT('Ctrl Pts',(60.2227043651634,249.524401538805,21.7357577024867)) ;
#113986 = CARTESIAN_POINT('Ctrl Pts',(60.2255003209692,249.569509377863,21.7878331013293)) ;
#113987 = CARTESIAN_POINT('Ctrl Pts',(60.2282962767749,249.611811921378,21.8422147502424)) ;
#113988 = CARTESIAN_POINT('Ctrl Pts',(60.2310922325807,249.651085052258,21.8985597473098)) ;
#113989 = CARTESIAN_POINT('Ctrl Pts',(60.2323528355094,249.668791993013,21.9239638213565)) ;
#113990 = CARTESIAN_POINT('Ctrl Pts',(60.2336134384381,249.685883721363,21.9497666479969)) ;
#113991 = CARTESIAN_POINT('Ctrl Pts',(60.2348740413668,249.702342772904,21.975935206342)) ;
#113992 = CARTESIAN_POINT('Ctrl Pts',(60.2377412276648,249.739778166702,22.0354544492515)) ;
#113993 = CARTESIAN_POINT('Ctrl Pts',(60.2406084139629,249.774078324787,22.0970909793996)) ;
#113994 = CARTESIAN_POINT('Ctrl Pts',(60.2434756002609,249.805004331575,22.1604906728236)) ;
#113995 = CARTESIAN_POINT('Ctrl Pts',(60.2464819941489,249.837431857423,22.2269685472966)) ;
#113996 = CARTESIAN_POINT('Ctrl Pts',(60.2494883880369,249.866148909367,22.2953847829146)) ;
#113997 = CARTESIAN_POINT('Ctrl Pts',(60.2524947819249,249.890931274391,22.3652967237239)) ;
#113998 = CARTESIAN_POINT('Ctrl Pts',(60.2553516150131,249.9144807769,22.4317307151471)) ;
#113999 = CARTESIAN_POINT('Ctrl Pts',(60.2582084481014,249.934477515015,22.4995146613668)) ;
#114000 = CARTESIAN_POINT('Ctrl Pts',(60.2610652811897,249.950776875416,22.5682452551403)) ;
#114001 = CARTESIAN_POINT('Ctrl Pts',(60.2639190906064,249.967058984577,22.6369031044661)) ;
#114002 = CARTESIAN_POINT('Ctrl Pts',(60.266772900023,249.979651385476,22.7065051674995)) ;
#114003 = CARTESIAN_POINT('Ctrl Pts',(60.2696267094397,249.988459223616,22.7766329163271)) ;
#114004 = CARTESIAN_POINT('Ctrl Pts',(60.2724778878943,249.997258941702,22.846696013518)) ;
#114005 = CARTESIAN_POINT('Ctrl Pts',(60.2753290663488,250.002280980204,22.917283379616)) ;
#114006 = CARTESIAN_POINT('Ctrl Pts',(60.2781802448034,250.003481818976,22.9879677588878)) ;
#114007 = CARTESIAN_POINT('Ctrl Pts',(60.2786376055079,250.003674446858,22.9993063187197)) ;
#114008 = CARTESIAN_POINT('Ctrl Pts',(60.2790949662123,250.003768856915,23.0106473625013)) ;
#114009 = CARTESIAN_POINT('Ctrl Pts',(60.2795523269168,250.003764993894,23.0219891151141)) ;
#114010 = CARTESIAN_POINT('',(60.7795523268794,250.003764678819,23.02261824718)) ;
#114011 = CARTESIAN_POINT('Ctrl Pts',(60.2795523269397,250.003764993893,23.0219891156808)) ;
#114012 = CARTESIAN_POINT('Ctrl Pts',(60.2825667509946,250.00373953304,23.0967416065853)) ;
#114013 = CARTESIAN_POINT('Ctrl Pts',(60.2855811750496,249.999440984289,23.1713682677577)) ;
#114014 = CARTESIAN_POINT('Ctrl Pts',(60.2885955991045,249.99093752082,23.2453948557862)) ;
#114015 = CARTESIAN_POINT('Ctrl Pts',(60.2916177917231,249.982412142817,23.3196122199815)) ;
#114016 = CARTESIAN_POINT('Ctrl Pts',(60.2946399843418,249.969660279399,23.3932260736516)) ;
#114017 = CARTESIAN_POINT('Ctrl Pts',(60.2976621769605,249.952801046831,23.4657734140421)) ;
#114018 = CARTESIAN_POINT('Ctrl Pts',(60.3006968067865,249.935872433585,23.5386193079761)) ;
#114019 = CARTESIAN_POINT('Ctrl Pts',(60.3037314366125,249.914802725252,23.6103895617087)) ;
#114020 = CARTESIAN_POINT('Ctrl Pts',(60.3067660664385,249.889761187779,23.6806355186404)) ;
#114021 = CARTESIAN_POINT('Ctrl Pts',(60.3091768734098,249.869867389664,23.7364411530614)) ;
#114022 = CARTESIAN_POINT('Ctrl Pts',(60.311587680381,249.847467869694,23.7912851094937)) ;
#114023 = CARTESIAN_POINT('Ctrl Pts',(60.3139984873523,249.822668197138,23.8449534397057)) ;
#114024 = CARTESIAN_POINT('Ctrl Pts',(60.3167948593909,249.793902264516,23.9072050507863)) ;
#114025 = CARTESIAN_POINT('Ctrl Pts',(60.3195912314296,249.761814742582,23.9680699192819)) ;
#114026 = CARTESIAN_POINT('Ctrl Pts',(60.3223876034682,249.726562036934,24.0271706886639)) ;
#114027 = CARTESIAN_POINT('Ctrl Pts',(60.3251797948775,249.691362034751,24.0861831012709)) ;
#114028 = CARTESIAN_POINT('Ctrl Pts',(60.3279719862867,249.653006490149,24.1434362310788)) ;
#114029 = CARTESIAN_POINT('Ctrl Pts',(60.3307641776959,249.611698894999,24.1985748200451)) ;
#114030 = CARTESIAN_POINT('Ctrl Pts',(60.3335531139729,249.570439456177,24.2536491285323)) ;
#114031 = CARTESIAN_POINT('Ctrl Pts',(60.3363420502498,249.526235094886,24.3066134011991)) ;
#114032 = CARTESIAN_POINT('Ctrl Pts',(60.3391309865267,249.479333055782,24.357140575122)) ;
#114033 = CARTESIAN_POINT('Ctrl Pts',(60.3419181918599,249.432460126269,24.4076363895265)) ;
#114034 = CARTESIAN_POINT('Ctrl Pts',(60.344705397193,249.382893173611,24.4556977469108)) ;
#114035 = CARTESIAN_POINT('Ctrl Pts',(60.3474926025261,249.330919248694,24.5010311729304)) ;
#114036 = CARTESIAN_POINT('Ctrl Pts',(60.3502790294131,249.278959839716,24.5463519376537)) ;
#114037 = CARTESIAN_POINT('Ctrl Pts',(60.3530654563001,249.224595162818,24.588945961132)) ;
#114038 = CARTESIAN_POINT('Ctrl Pts',(60.355851883187,249.168147279082,24.6285583650342)) ;
#114039 = CARTESIAN_POINT('Ctrl Pts',(60.3586384829702,249.111695892784,24.6681732268647)) ;
#114040 = CARTESIAN_POINT('Ctrl Pts',(60.3614250827535,249.05316144625,24.704805821987)) ;
#114041 = CARTESIAN_POINT('Ctrl Pts',(60.3642116825367,248.992895575888,24.7382441744978)) ;
#114042 = CARTESIAN_POINT('Ctrl Pts',(60.3670012321378,248.932565909735,24.7717179239281)) ;
#114043 = CARTESIAN_POINT('Ctrl Pts',(60.3697907817388,248.870501592039,24.8019904442138)) ;
#114044 = CARTESIAN_POINT('Ctrl Pts',(60.3725803313399,248.807078608147,24.8288958760517)) ;
#114045 = CARTESIAN_POINT('Ctrl Pts',(60.375371550846,248.743617657424,24.8558174142589)) ;
#114046 = CARTESIAN_POINT('Ctrl Pts',(60.3781627703521,248.678796883113,24.8793676847712)) ;
#114047 = CARTESIAN_POINT('Ctrl Pts',(60.3809539898581,248.613009350054,24.8994301068453)) ;
#114048 = CARTESIAN_POINT('Ctrl Pts',(60.3837499737347,248.547109523362,24.9195267737398)) ;
#114049 = CARTESIAN_POINT('Ctrl Pts',(60.3865459576112,248.480240120589,24.9361235922249)) ;
#114050 = CARTESIAN_POINT('Ctrl Pts',(60.3893419414877,248.412805492076,24.9491548572234)) ;
#114051 = CARTESIAN_POINT('Ctrl Pts',(60.3906022721044,248.382408347209,24.9550288904715)) ;
#114052 = CARTESIAN_POINT('Ctrl Pts',(60.3918626027211,248.35189643516,24.9601791446228)) ;
#114053 = CARTESIAN_POINT('Ctrl Pts',(60.3931229333378,248.321306998146,24.9646030573876)) ;
#114054 = CARTESIAN_POINT('Ctrl Pts',(60.3959192896097,248.253436740206,24.9744186058175)) ;
#114055 = CARTESIAN_POINT('Ctrl Pts',(60.3987156458815,248.184918568129,24.9806935219423)) ;
#114056 = CARTESIAN_POINT('Ctrl Pts',(60.4015120021534,248.116154103306,24.9833532460255)) ;
#114057 = CARTESIAN_POINT('Ctrl Pts',(60.4043041784366,248.047492427488,24.9860089943578)) ;
#114058 = CARTESIAN_POINT('Ctrl Pts',(60.4070963547199,247.978585676197,24.9850602573779)) ;
#114059 = CARTESIAN_POINT('Ctrl Pts',(60.4098885310032,247.909842609292,24.980483997236)) ;
#114060 = CARTESIAN_POINT('Ctrl Pts',(60.4126774531614,247.84117965858,24.9759130704688)) ;
#114061 = CARTESIAN_POINT('Ctrl Pts',(60.4154663753196,247.772680500832,24.9677230495881)) ;
#114062 = CARTESIAN_POINT('Ctrl Pts',(60.4182552974779,247.70475410613,24.9559429470064)) ;
#114063 = CARTESIAN_POINT('Ctrl Pts',(60.4210424893246,247.636869854527,24.9441701530717)) ;
#114064 = CARTESIAN_POINT('Ctrl Pts',(60.4238296811713,247.569558143552,24.9288117797785)) ;
#114065 = CARTESIAN_POINT('Ctrl Pts',(60.426616873018,247.503221480302,24.9099485208826)) ;
#114066 = CARTESIAN_POINT('Ctrl Pts',(60.4294032870659,247.436903329079,24.8910905260014)) ;
#114067 = CARTESIAN_POINT('Ctrl Pts',(60.4321897011139,247.371560157267,24.8687297214978)) ;
#114068 = CARTESIAN_POINT('Ctrl Pts',(60.4349761151619,247.307581196557,24.8429971909249)) ;
#114069 = CARTESIAN_POINT('Ctrl Pts',(60.4377627027695,247.243598250739,24.8172630575292)) ;
#114070 = CARTESIAN_POINT('Ctrl Pts',(60.4405492903771,247.180980139128,24.7881569666392)) ;
#114071 = CARTESIAN_POINT('Ctrl Pts',(60.4433358779846,247.120096245115,24.7558581823426)) ;
#114072 = CARTESIAN_POINT('Ctrl Pts',(60.4461254164814,247.059147877398,24.723525194875)) ;
#114073 = CARTESIAN_POINT('Ctrl Pts',(60.4489149549781,246.999937826622,24.6879929972857)) ;
#114074 = CARTESIAN_POINT('Ctrl Pts',(60.4517044934749,246.942810084486,24.6494864044494)) ;
#114075 = CARTESIAN_POINT('Ctrl Pts',(60.454495702473,246.885648131683,24.6109567521297)) ;
#114076 = CARTESIAN_POINT('Ctrl Pts',(60.4572869114711,246.830571361334,24.5694494549501)) ;
#114077 = CARTESIAN_POINT('Ctrl Pts',(60.4600781204692,246.777891759898,24.5252305072802)) ;
#114078 = CARTESIAN_POINT('Ctrl Pts',(60.4628740948521,246.725122219454,24.4809360653353)) ;
#114079 = CARTESIAN_POINT('Ctrl Pts',(60.465670069235,246.674758374516,24.4339210680221)) ;
#114080 = CARTESIAN_POINT('Ctrl Pts',(60.4684660436179,246.62707570927,24.3844887021715)) ;
#114081 = CARTESIAN_POINT('Ctrl Pts',(60.4697264888531,246.60558002298,24.362204238344)) ;
#114082 = CARTESIAN_POINT('Ctrl Pts',(60.4709869340882,246.584628680812,24.3394289493908)) ;
#114083 = CARTESIAN_POINT('Ctrl Pts',(60.4722473793233,246.564244136686,24.316192670422)) ;
#114084 = CARTESIAN_POINT('Ctrl Pts',(60.4750435067742,246.519023779772,24.2646461250667)) ;
#114085 = CARTESIAN_POINT('Ctrl Pts',(60.4778396342251,246.476418112565,24.2106267345541)) ;
#114086 = CARTESIAN_POINT('Ctrl Pts',(60.480635761676,246.436708552273,24.1544304985185)) ;
#114087 = CARTESIAN_POINT('Ctrl Pts',(60.483427708114,246.397058369168,24.0983182919802)) ;
#114088 = CARTESIAN_POINT('Ctrl Pts',(60.486219654552,246.360295979102,24.0400360979995)) ;
#114089 = CARTESIAN_POINT('Ctrl Pts',(60.4890116009901,246.326663499278,23.9799139891246)) ;
#114090 = CARTESIAN_POINT('Ctrl Pts',(60.4918002929304,246.293070223941,23.9198619629935)) ;
#114091 = CARTESIAN_POINT('Ctrl Pts',(60.4945889848707,246.262599851231,23.8579747080533)) ;
#114092 = CARTESIAN_POINT('Ctrl Pts',(60.497377676811,246.235450977629,23.7946108488587)) ;
#114093 = CARTESIAN_POINT('Ctrl Pts',(60.5001646383492,246.208318950086,23.7312863073662)) ;
#114094 = CARTESIAN_POINT('Ctrl Pts',(60.5029515998873,246.184504525948,23.6664874294933)) ;
#114095 = CARTESIAN_POINT('Ctrl Pts',(60.5057385614254,246.164159451687,23.6005955951925)) ;
#114096 = CARTESIAN_POINT('Ctrl Pts',(60.5085247454293,246.143820053498,23.5347221440525)) ;
#114097 = CARTESIAN_POINT('Ctrl Pts',(60.5113109294331,246.126948228345,23.4677568106951)) ;
#114098 = CARTESIAN_POINT('Ctrl Pts',(60.5140971134369,246.113646241324,23.4000973140725)) ;
#114099 = CARTESIAN_POINT('Ctrl Pts',(60.5168834716199,246.100343422724,23.3324335876949)) ;
#114100 = CARTESIAN_POINT('Ctrl Pts',(60.5196698298029,246.090610977498,23.2640760940751)) ;
#114101 = CARTESIAN_POINT('Ctrl Pts',(60.522456187986,246.084499958264,23.1954321751935)) ;
#114102 = CARTESIAN_POINT('Ctrl Pts',(60.5252454995637,246.078382461667,23.1267154973289)) ;
#114103 = CARTESIAN_POINT('Ctrl Pts',(60.5280348111414,246.075894094999,23.0577122782262)) ;
#114104 = CARTESIAN_POINT('Ctrl Pts',(60.5308241227191,246.077033881316,22.9888334013953)) ;
#114105 = CARTESIAN_POINT('Ctrl Pts',(60.5336151059076,246.078174350696,22.9199132460377)) ;
#114106 = CARTESIAN_POINT('Ctrl Pts',(60.5364060890962,246.082947266486,22.8511180710345)) ;
#114107 = CARTESIAN_POINT('Ctrl Pts',(60.5391970722847,246.091299682121,22.7828543720631)) ;
#114108 = CARTESIAN_POINT('Ctrl Pts',(60.5419928249112,246.09966637098,22.7144740190451)) ;
#114109 = CARTESIAN_POINT('Ctrl Pts',(60.5447885775378,246.111624682532,22.6466274378222)) ;
#114110 = CARTESIAN_POINT('Ctrl Pts',(60.5475843301643,246.127070592193,22.579710792595)) ;
#114111 = CARTESIAN_POINT('Ctrl Pts',(60.5488468285458,246.134045614146,22.5494927556)) ;
#114112 = CARTESIAN_POINT('Ctrl Pts',(60.5501093269274,246.141731158904,22.5194641413635)) ;
#114113 = CARTESIAN_POINT('Ctrl Pts',(60.5513718253089,246.150114385329,22.4896602111498)) ;
#114114 = CARTESIAN_POINT('Ctrl Pts',(60.5541685645237,246.168685259107,22.4236372984863)) ;
#114115 = CARTESIAN_POINT('Ctrl Pts',(60.5569653037384,246.190755923697,22.3584592614936)) ;
#114116 = CARTESIAN_POINT('Ctrl Pts',(60.5597620429532,246.216231499799,22.2945235033544)) ;
#114117 = CARTESIAN_POINT('Ctrl Pts',(60.5625546005643,246.241668985555,22.2306833401114)) ;
#114118 = CARTESIAN_POINT('Ctrl Pts',(60.5653471581755,246.270501098344,22.1680822214019)) ;
#114119 = CARTESIAN_POINT('Ctrl Pts',(60.5681397157866,246.302582973991,22.1071031637326)) ;
#114120 = CARTESIAN_POINT('Ctrl Pts',(60.5709290150576,246.33462741669,22.0461952560776)) ;
#114121 = CARTESIAN_POINT('Ctrl Pts',(60.5737183143286,246.36991386385,21.9869060827224)) ;
#114122 = CARTESIAN_POINT('Ctrl Pts',(60.5765076135996,246.408249795115,21.929597728054)) ;
#114123 = CARTESIAN_POINT('Ctrl Pts',(60.5792951797171,246.446561906041,21.8723249823906)) ;
#114124 = CARTESIAN_POINT('Ctrl Pts',(60.5820827458347,246.487919469867,21.817031020669)) ;
#114125 = CARTESIAN_POINT('Ctrl Pts',(60.5848703119522,246.532085354106,21.7640510483844)) ;
#114126 = CARTESIAN_POINT('Ctrl Pts',(60.5876570968761,246.5762388612,21.7110859233243)) ;
#114127 = CARTESIAN_POINT('Ctrl Pts',(60.5904438817999,246.623198812189,21.6604338769742)) ;
#114128 = CARTESIAN_POINT('Ctrl Pts',(60.5932306667238,246.672687406079,21.6123975352432)) ;
#114129 = CARTESIAN_POINT('Ctrl Pts',(60.5960176212559,246.722179011925,21.564358269943)) ;
#114130 = CARTESIAN_POINT('Ctrl Pts',(60.5988045757879,246.774199212344,21.5189353652299)) ;
#114131 = CARTESIAN_POINT('Ctrl Pts',(60.60159153032,246.82843422262,21.4763937576798)) ;
#114132 = CARTESIAN_POINT('Ctrl Pts',(60.6043814273241,246.882726494326,21.4338072346176)) ;
#114133 = CARTESIAN_POINT('Ctrl Pts',(60.6071713243282,246.939237855736,21.3941083830617)) ;
#114134 = CARTESIAN_POINT('Ctrl Pts',(60.6099612213323,246.997623190867,21.3575204508188)) ;
#114135 = CARTESIAN_POINT('Ctrl Pts',(60.612752784535,247.056043395231,21.3209106673166)) ;
#114136 = CARTESIAN_POINT('Ctrl Pts',(60.6155443477377,247.116339371843,21.2874157392378)) ;
#114137 = CARTESIAN_POINT('Ctrl Pts',(60.6183359109405,247.178141348584,21.2572129562899)) ;
#114138 = CARTESIAN_POINT('Ctrl Pts',(60.6211322292867,247.240048598697,21.2269587259782)) ;
#114139 = CARTESIAN_POINT('Ctrl Pts',(60.6239285476329,247.303466517481,21.2000080246737)) ;
#114140 = CARTESIAN_POINT('Ctrl Pts',(60.6267248659792,247.3680061454,21.1764896907646)) ;
#114141 = CARTESIAN_POINT('Ctrl Pts',(60.6279820010843,247.397021093585,21.1659166016136)) ;
#114142 = CARTESIAN_POINT('Ctrl Pts',(60.6292391361893,247.426262562519,21.1560365558167)) ;
#114143 = CARTESIAN_POINT('Ctrl Pts',(60.6304962712944,247.455694464905,21.1468579103587)) ;
#114144 = CARTESIAN_POINT('Ctrl Pts',(60.6332926395102,247.521162715715,21.1264409541228)) ;
#114145 = CARTESIAN_POINT('Ctrl Pts',(60.636089007726,247.587830124222,21.1094179783846)) ;
#114146 = CARTESIAN_POINT('Ctrl Pts',(60.6388853759418,247.655311867762,21.095926032517)) ;
#114147 = CARTESIAN_POINT('Ctrl Pts',(60.6416775684694,247.722692843916,21.0824542335521)) ;
#114148 = CARTESIAN_POINT('Ctrl Pts',(60.6444697609971,247.79088526415,21.0725030948673)) ;
#114149 = CARTESIAN_POINT('Ctrl Pts',(60.6472619535248,247.85948912198,21.0661599171608)) ;
#114150 = CARTESIAN_POINT('Ctrl Pts',(60.650050898095,247.928013177859,21.0598241180184)) ;
#114151 = CARTESIAN_POINT('Ctrl Pts',(60.6528398426652,247.996947234345,21.0570879894057)) ;
#114152 = CARTESIAN_POINT('Ctrl Pts',(60.6556287872354,248.065882857958,21.0579874678413)) ;
#114153 = CARTESIAN_POINT('Ctrl Pts',(60.658416005296,248.13477580664,21.0588863894505)) ;
#114154 = CARTESIAN_POINT('Ctrl Pts',(60.6612032233566,248.203669830839,21.0634164468891)) ;
#114155 = CARTESIAN_POINT('Ctrl Pts',(60.6639904414172,248.27215471858,21.0715615229857)) ;
#114156 = CARTESIAN_POINT('Ctrl Pts',(60.6667768854009,248.340620586436,21.0797043370005)) ;
#114157 = CARTESIAN_POINT('Ctrl Pts',(60.6695633293846,248.408677056274,21.0914601185186)) ;
#114158 = CARTESIAN_POINT('Ctrl Pts',(60.6723497733684,248.475919068293,21.1067608964036)) ;
#114159 = CARTESIAN_POINT('Ctrl Pts',(60.6751363945573,248.543165356601,21.1220626473492)) ;
#114160 = CARTESIAN_POINT('Ctrl Pts',(60.6779230157463,248.609596606267,21.1409097308469)) ;
#114161 = CARTESIAN_POINT('Ctrl Pts',(60.6807096369353,248.674819748712,21.16318346548)) ;
#114162 = CARTESIAN_POINT('Ctrl Pts',(60.6834992141911,248.740112080312,21.1854808282428)) ;
#114163 = CARTESIAN_POINT('Ctrl Pts',(60.6862887914468,248.804193281804,21.2112119374179)) ;
#114164 = CARTESIAN_POINT('Ctrl Pts',(60.6890783687026,248.86668816404,21.2402091224139)) ;
#114165 = CARTESIAN_POINT('Ctrl Pts',(60.6918696194718,248.929220537989,21.2692237033)) ;
#114166 = CARTESIAN_POINT('Ctrl Pts',(60.694660870241,248.990164264906,21.3015080298612)) ;
#114167 = CARTESIAN_POINT('Ctrl Pts',(60.6974521210102,249.049169256588,21.3368487146709)) ;
#114168 = CARTESIAN_POINT('Ctrl Pts',(60.7002481412775,249.108275071955,21.3722497872205)) ;
#114169 = CARTESIAN_POINT('Ctrl Pts',(60.7030441615447,249.165435133589,21.4107173671274)) ;
#114170 = CARTESIAN_POINT('Ctrl Pts',(60.7058401818119,249.220329523796,21.45199557664)) ;
#114171 = CARTESIAN_POINT('Ctrl Pts',(60.7071003603012,249.2450706641,21.4705998451125)) ;
#114172 = CARTESIAN_POINT('Ctrl Pts',(60.7083605387906,249.269352034815,21.4897745194347)) ;
#114173 = CARTESIAN_POINT('Ctrl Pts',(60.7096207172799,249.293146769467,21.509493702763)) ;
#114174 = CARTESIAN_POINT('Ctrl Pts',(60.7123779967535,249.345209817673,21.5526394157617)) ;
#114175 = CARTESIAN_POINT('Ctrl Pts',(60.7151352762271,249.395157754924,21.5985742313354)) ;
#114176 = CARTESIAN_POINT('Ctrl Pts',(60.7178925557008,249.442670499818,21.6470600456544)) ;
#114177 = CARTESIAN_POINT('Ctrl Pts',(60.7206451164748,249.490101933272,21.6954628832595)) ;
#114178 = CARTESIAN_POINT('Ctrl Pts',(60.7233976772489,249.535106096424,21.7464076952068)) ;
#114179 = CARTESIAN_POINT('Ctrl Pts',(60.726150238023,249.577396023049,21.7996162880111)) ;
#114180 = CARTESIAN_POINT('Ctrl Pts',(60.7289001789681,249.619645699019,21.8527742380057)) ;
#114181 = CARTESIAN_POINT('Ctrl Pts',(60.7316501199133,249.659185944413,21.9081913054828)) ;
#114182 = CARTESIAN_POINT('Ctrl Pts',(60.7344000608584,249.695767790971,21.9655537424747)) ;
#114183 = CARTESIAN_POINT('Ctrl Pts',(60.7371483861221,249.732328144482,22.0228824771329)) ;
#114184 = CARTESIAN_POINT('Ctrl Pts',(60.7398967113857,249.765933273921,22.0821538895004)) ;
#114185 = CARTESIAN_POINT('Ctrl Pts',(60.7426450366494,249.796376751589,22.1430241836579)) ;
#114186 = CARTESIAN_POINT('Ctrl Pts',(60.7453927480107,249.826813428999,22.2038808810211)) ;
#114187 = CARTESIAN_POINT('Ctrl Pts',(60.7481404593721,249.854089631235,22.2663352984914)) ;
#114188 = CARTESIAN_POINT('Ctrl Pts',(60.7508881707335,249.878045195176,22.3300196850955)) ;
#114189 = CARTESIAN_POINT('Ctrl Pts',(60.7536378075823,249.902017546229,22.3937486991993)) ;
#114190 = CARTESIAN_POINT('Ctrl Pts',(60.7563874444311,249.922664433148,22.4587089295423)) ;
#114191 = CARTESIAN_POINT('Ctrl Pts',(60.7591370812799,249.939874614559,22.5245145748941)) ;
#114192 = CARTESIAN_POINT('Ctrl Pts',(60.7618877928552,249.957091522762,22.5903459411223)) ;
#114193 = CARTESIAN_POINT('Ctrl Pts',(60.7646385044305,249.970868947996,22.6570228845858)) ;
#114194 = CARTESIAN_POINT('Ctrl Pts',(60.7673892160059,249.981146754236,22.724149206885)) ;
#114195 = CARTESIAN_POINT('Ctrl Pts',(60.7701439626157,249.99143963705,22.7913739971708)) ;
#114196 = CARTESIAN_POINT('Ctrl Pts',(60.7728987092256,249.998222606019,22.8590489785077)) ;
#114197 = CARTESIAN_POINT('Ctrl Pts',(60.7756534558355,250.001487481974,22.9267737995547)) ;
#114198 = CARTESIAN_POINT('Ctrl Pts',(60.7769530795168,250.003027772502,22.9587247532035)) ;
#114199 = CARTESIAN_POINT('Ctrl Pts',(60.7782527031981,250.003785785992,22.9906868126438)) ;
#114200 = CARTESIAN_POINT('Ctrl Pts',(60.7795523268794,250.003764678819,23.02261824718)) ;
#114201 = CARTESIAN_POINT('',(60.9402651077866,247.187596811119,24.7900173288734)) ;
#114202 = CARTESIAN_POINT('Ctrl Pts',(60.7795523269168,250.003764678818,23.0226182480982)) ;
#114203 = CARTESIAN_POINT('Ctrl Pts',(60.7826166056997,250.003714911868,23.0979068249079)) ;
#114204 = CARTESIAN_POINT('Ctrl Pts',(60.7856808844825,249.999334962485,23.1730560108799)) ;
#114205 = CARTESIAN_POINT('Ctrl Pts',(60.7887451632653,249.990671827291,23.247695868984)) ;
#114206 = CARTESIAN_POINT('Ctrl Pts',(60.7915457584845,249.982754161592,23.3159129094631)) ;
#114207 = CARTESIAN_POINT('Ctrl Pts',(60.7943463537037,249.971237999381,23.3838458374833)) ;
#114208 = CARTESIAN_POINT('Ctrl Pts',(60.7971469489229,249.956154825269,23.4510863734446)) ;
#114209 = CARTESIAN_POINT('Ctrl Pts',(60.7999433589634,249.941094191287,23.518226425889)) ;
#114210 = CARTESIAN_POINT('Ctrl Pts',(60.802739769004,249.922477232334,23.5846756664621)) ;
#114211 = CARTESIAN_POINT('Ctrl Pts',(60.8055361790446,249.900387055117,23.6500321941365)) ;
#114212 = CARTESIAN_POINT('Ctrl Pts',(60.8083293066438,249.878322807471,23.7153120059637)) ;
#114213 = CARTESIAN_POINT('Ctrl Pts',(60.8111224342431,249.852793595527,23.7795011913223)) ;
#114214 = CARTESIAN_POINT('Ctrl Pts',(60.8139155618424,249.823932876028,23.8422110442841)) ;
#114215 = CARTESIAN_POINT('Ctrl Pts',(60.8167069388807,249.795090244656,23.9048815945579)) ;
#114216 = CARTESIAN_POINT('Ctrl Pts',(60.819498315919,249.762920452405,23.9660742085282)) ;
#114217 = CARTESIAN_POINT('Ctrl Pts',(60.8222896929573,249.727605241829,24.0254197022134)) ;
#114218 = CARTESIAN_POINT('Ctrl Pts',(60.825080265588,249.692300208244,24.0847480939579)) ;
#114219 = CARTESIAN_POINT('Ctrl Pts',(60.8278708382187,249.653851806104,24.1422300021104)) ;
#114220 = CARTESIAN_POINT('Ctrl Pts',(60.8306614108495,249.612487076523,24.1975219976233)) ;
#114221 = CARTESIAN_POINT('Ctrl Pts',(60.8334521240458,249.571120263334,24.2528167782825)) ;
#114222 = CARTESIAN_POINT('Ctrl Pts',(60.8362428372421,249.526837126104,24.3059210371075)) ;
#114223 = CARTESIAN_POINT('Ctrl Pts',(60.8390335504385,249.479906196998,24.3565228691157)) ;
#114224 = CARTESIAN_POINT('Ctrl Pts',(60.8418271369309,249.432926948183,24.407176800366)) ;
#114225 = CARTESIAN_POINT('Ctrl Pts',(60.8446207234232,249.38329480011,24.4553228035038)) ;
#114226 = CARTESIAN_POINT('Ctrl Pts',(60.8474143099156,249.331315818112,24.5006851779959)) ;
#114227 = CARTESIAN_POINT('Ctrl Pts',(60.8502095281215,249.27930647557,24.5460740483204)) ;
#114228 = CARTESIAN_POINT('Ctrl Pts',(60.8530047463274,249.224947955461,24.5886757515398)) ;
#114229 = CARTESIAN_POINT('Ctrl Pts',(60.8557999645333,249.16857797034,24.6282560405289)) ;
#114230 = CARTESIAN_POINT('Ctrl Pts',(60.8585998475443,249.112113912064,24.6679023831583)) ;
#114231 = CARTESIAN_POINT('Ctrl Pts',(60.8613997305554,249.053632103304,24.704516988195)) ;
#114232 = CARTESIAN_POINT('Ctrl Pts',(60.8641996135665,248.993496900582,24.7379103933977)) ;
#114233 = CARTESIAN_POINT('Ctrl Pts',(60.8654229454614,248.967222477255,24.7525007236018)) ;
#114234 = CARTESIAN_POINT('Ctrl Pts',(60.8666462773563,248.940632700595,24.7664767340529)) ;
#114235 = CARTESIAN_POINT('Ctrl Pts',(60.8678696092512,248.913759119968,24.7798255214544)) ;
#114236 = CARTESIAN_POINT('Ctrl Pts',(60.8706315295515,248.853086551723,24.8099631211221)) ;
#114237 = CARTESIAN_POINT('Ctrl Pts',(60.8733934498519,248.790720386366,24.8370223887974)) ;
#114238 = CARTESIAN_POINT('Ctrl Pts',(60.8761553701522,248.727009736357,24.8608077898689)) ;
#114239 = CARTESIAN_POINT('Ctrl Pts',(60.878912687101,248.663405274249,24.8845535473044)) ;
#114240 = CARTESIAN_POINT('Ctrl Pts',(60.8816700040498,248.598461244098,24.905036095618)) ;
#114241 = CARTESIAN_POINT('Ctrl Pts',(60.8844273209986,248.532549844046,24.9221064936684)) ;
#114242 = CARTESIAN_POINT('Ctrl Pts',(60.8871820798996,248.466699592027,24.9391610549855)) ;
#114243 = CARTESIAN_POINT('Ctrl Pts',(60.8899368388007,248.39988423402,24.9528096133014)) ;
#114244 = CARTESIAN_POINT('Ctrl Pts',(60.8926915977017,248.332492926079,24.9629524282286)) ;
#114245 = CARTESIAN_POINT('Ctrl Pts',(60.8954447975409,248.265139758393,24.9730895028078)) ;
#114246 = CARTESIAN_POINT('Ctrl Pts',(60.8981979973802,248.197211784568,24.9797246929004)) ;
#114247 = CARTESIAN_POINT('Ctrl Pts',(60.9009511972195,248.129108262437,24.9828093554767)) ;
#114248 = CARTESIAN_POINT('Ctrl Pts',(60.9037038347724,248.061018649097,24.9858933880721)) ;
#114249 = CARTESIAN_POINT('Ctrl Pts',(60.9064564723254,247.992754062083,24.9854283104596)) ;
#114250 = CARTESIAN_POINT('Ctrl Pts',(60.9092091098783,247.924716804232,24.9814174940973)) ;
#114251 = CARTESIAN_POINT('Ctrl Pts',(60.911963958828,247.856624887036,24.9774034555504)) ;
#114252 = CARTESIAN_POINT('Ctrl Pts',(60.9147188077776,247.7887611682,24.9698380167252)) ;
#114253 = CARTESIAN_POINT('Ctrl Pts',(60.9174736567273,247.721524649355,24.9587766063328)) ;
#114254 = CARTESIAN_POINT('Ctrl Pts',(60.920229606145,247.654261271819,24.947710777285)) ;
#114255 = CARTESIAN_POINT('Ctrl Pts',(60.9229855555627,247.587626086452,24.9331463029519)) ;
#114256 = CARTESIAN_POINT('Ctrl Pts',(60.9257415049803,247.522006821555,24.9151895572998)) ;
#114257 = CARTESIAN_POINT('Ctrl Pts',(60.9285021102181,247.456276701397,24.8972024760485)) ;
#114258 = CARTESIAN_POINT('Ctrl Pts',(60.9312627154558,247.391566408411,24.8758118376269)) ;
#114259 = CARTESIAN_POINT('Ctrl Pts',(60.9340233206936,247.328246605691,24.8511733165261)) ;
#114260 = CARTESIAN_POINT('Ctrl Pts',(60.9361039163912,247.28052413262,24.8326039099705)) ;
#114261 = CARTESIAN_POINT('Ctrl Pts',(60.9381845120889,247.233591139334,24.8121906608919)) ;
#114262 = CARTESIAN_POINT('Ctrl Pts',(60.9402651077866,247.187596811119,24.7900173288734)) ;
#114263 = CARTESIAN_POINT('',(60.9402651077866,247.14398687089,24.7683227969256)) ;
#114264 = CARTESIAN_POINT('Ctrl Pts',(60.9402651077866,247.187596811119,24.7900173288734)) ;
#114265 = CARTESIAN_POINT('Ctrl Pts',(60.9402651077866,247.173060164376,24.7827858182242)) ;
#114266 = CARTESIAN_POINT('Ctrl Pts',(60.9402651077866,247.158523517633,24.7755543075749)) ;
#114267 = CARTESIAN_POINT('Ctrl Pts',(60.9402651077866,247.14398687089,24.7683227969256)) ;
#114268 = CARTESIAN_POINT('',(60.9402651077866,248.892162375845,24.7903888257488)) ;
#114269 = CARTESIAN_POINT('Origin',(60.9402651077866,248.040265107786,23.0213203435596)) ;
#114270 = CARTESIAN_POINT('',(60.8509778886564,250.003885734109,23.0224059228657)) ;
#114271 = CARTESIAN_POINT('Ctrl Pts',(60.9402651077866,248.892162375845,24.7903888257488)) ;
#114272 = CARTESIAN_POINT('Ctrl Pts',(60.9138902924581,249.4784948342,24.5080396547159)) ;
#114273 = CARTESIAN_POINT('Ctrl Pts',(60.8841278860814,249.963363030827,23.8364478392611)) ;
#114274 = CARTESIAN_POINT('Ctrl Pts',(60.8543654797046,250.005755321297,23.1056824073686)) ;
#114275 = CARTESIAN_POINT('Ctrl Pts',(60.8509778886564,250.005100724118,23.0224065945677)) ;
#114276 = CARTESIAN_POINT('',(60.3509778886947,250.003765030662,23.0218706758452)) ;
#114277 = CARTESIAN_POINT('Ctrl Pts',(60.8509778886564,250.003764807726,23.022405856012)) ;
#114278 = CARTESIAN_POINT('Ctrl Pts',(60.8481044856214,250.003803831657,22.9518184785068)) ;
#114279 = CARTESIAN_POINT('Ctrl Pts',(60.8452310825863,250.000031341811,22.8810740559555)) ;
#114280 = CARTESIAN_POINT('Ctrl Pts',(60.8423576795513,249.992428256182,22.8106279325778)) ;
#114281 = CARTESIAN_POINT('Ctrl Pts',(60.8396190931482,249.985181898232,22.7434870570089)) ;
#114282 = CARTESIAN_POINT('Ctrl Pts',(60.8368805067451,249.97445637034,22.6766177015196)) ;
#114283 = CARTESIAN_POINT('Ctrl Pts',(60.8341419203419,249.960288344394,22.6104152196129)) ;
#114284 = CARTESIAN_POINT('Ctrl Pts',(60.8314053936341,249.946130974243,22.5442625286998)) ;
#114285 = CARTESIAN_POINT('Ctrl Pts',(60.8286688669262,249.928536341561,22.478776215336)) ;
#114286 = CARTESIAN_POINT('Ctrl Pts',(60.8259323402184,249.907592640746,22.414344121084)) ;
#114287 = CARTESIAN_POINT('Ctrl Pts',(60.8231968585997,249.886656938403,22.3499366336765)) ;
#114288 = CARTESIAN_POINT('Ctrl Pts',(60.8204613769811,249.862374861438,22.2865830523612)) ;
#114289 = CARTESIAN_POINT('Ctrl Pts',(60.8177258953625,249.834884627419,22.2246566568309)) ;
#114290 = CARTESIAN_POINT('Ctrl Pts',(60.8149904459441,249.807394716997,22.1627309902567)) ;
#114291 = CARTESIAN_POINT('Ctrl Pts',(60.8122549965257,249.776696934551,22.1022329415506)) ;
#114292 = CARTESIAN_POINT('Ctrl Pts',(60.8095195471073,249.742977034958,22.0435144614604)) ;
#114293 = CARTESIAN_POINT('Ctrl Pts',(60.8067813717529,249.709223532737,21.9847374671022)) ;
#114294 = CARTESIAN_POINT('Ctrl Pts',(60.8040431963985,249.672442161198,21.9277440220705)) ;
#114295 = CARTESIAN_POINT('Ctrl Pts',(60.8013050210441,249.632863245043,21.8728590149956)) ;
#114296 = CARTESIAN_POINT('Ctrl Pts',(60.7985652476696,249.593261230329,21.8179419766104)) ;
#114297 = CARTESIAN_POINT('Ctrl Pts',(60.7958254742951,249.550858746639,21.765136218727)) ;
#114298 = CARTESIAN_POINT('Ctrl Pts',(60.7930857009206,249.50592592897,21.7147329537355)) ;
#114299 = CARTESIAN_POINT('Ctrl Pts',(60.7903413487892,249.460918018793,21.6642454539302)) ;
#114300 = CARTESIAN_POINT('Ctrl Pts',(60.7875969966577,249.413371702513,21.6161688131355)) ;
#114301 = CARTESIAN_POINT('Ctrl Pts',(60.7848526445263,249.36359248379,21.570756003064)) ;
#114302 = CARTESIAN_POINT('Ctrl Pts',(60.7839071682894,249.346442691731,21.5551105134491)) ;
#114303 = CARTESIAN_POINT('Ctrl Pts',(60.7829616920525,249.329028140442,21.5397808315764)) ;
#114304 = CARTESIAN_POINT('Ctrl Pts',(60.7820162158156,249.311362119412,21.5247761119928)) ;
#114305 = CARTESIAN_POINT('Ctrl Pts',(60.7792207997854,249.259130369472,21.4804128249879)) ;
#114306 = CARTESIAN_POINT('Ctrl Pts',(60.7764253837552,249.204468501124,21.4386982606199)) ;
#114307 = CARTESIAN_POINT('Ctrl Pts',(60.773629967725,249.14767608081,21.3999094805068)) ;
#114308 = CARTESIAN_POINT('Ctrl Pts',(60.7708388225159,249.090970427642,21.3611799616775)) ;
#114309 = CARTESIAN_POINT('Ctrl Pts',(60.7680476773068,249.032141085041,21.3253676305957)) ;
#114310 = CARTESIAN_POINT('Ctrl Pts',(60.7652565320977,248.971521162682,21.2927098003142)) ;
#114311 = CARTESIAN_POINT('Ctrl Pts',(60.7624687690074,248.910974695395,21.2600915425557)) ;
#114312 = CARTESIAN_POINT('Ctrl Pts',(60.759681005917,248.848642388168,21.2306204256485)) ;
#114313 = CARTESIAN_POINT('Ctrl Pts',(60.7568932428266,248.784885296644,21.2044898549489)) ;
#114314 = CARTESIAN_POINT('Ctrl Pts',(60.7541072886962,248.721169576652,21.1783762401944)) ;
#114315 = CARTESIAN_POINT('Ctrl Pts',(60.7513213345658,248.656031359958,21.1555990575248)) ;
#114316 = CARTESIAN_POINT('Ctrl Pts',(60.7485353804355,248.589853819179,21.1363045615809)) ;
#114317 = CARTESIAN_POINT('Ctrl Pts',(60.7457502803917,248.523696566371,21.1170159807276)) ;
#114318 = CARTESIAN_POINT('Ctrl Pts',(60.742965180348,248.456501093471,21.1012081045428)) ;
#114319 = CARTESIAN_POINT('Ctrl Pts',(60.7401800803043,248.388666233287,21.0889774894704)) ;
#114320 = CARTESIAN_POINT('Ctrl Pts',(60.73739488071,248.320828948416,21.0767464372273)) ;
#114321 = CARTESIAN_POINT('Ctrl Pts',(60.7346096811158,248.252352714911,21.0680929846255)) ;
#114322 = CARTESIAN_POINT('Ctrl Pts',(60.7318244815215,248.183645280938,21.0630623483131)) ;
#114323 = CARTESIAN_POINT('Ctrl Pts',(60.7290364322837,248.114867549779,21.0580265649656)) ;
#114324 = CARTESIAN_POINT('Ctrl Pts',(60.7262483830459,248.045858637042,21.0566210313713)) ;
#114325 = CARTESIAN_POINT('Ctrl Pts',(60.7234603338081,247.97702909406,21.0588388897445)) ;
#114326 = CARTESIAN_POINT('Ctrl Pts',(60.7206706740539,247.9081597917,21.0610580292635)) ;
#114327 = CARTESIAN_POINT('Ctrl Pts',(60.7178810142997,247.839470555038,21.0669046851393)) ;
#114328 = CARTESIAN_POINT('Ctrl Pts',(60.7150913545455,247.77136682293,21.0763200961557)) ;
#114329 = CARTESIAN_POINT('Ctrl Pts',(60.7122970046519,247.703148590836,21.0857513369128)) ;
#114330 = CARTESIAN_POINT('Ctrl Pts',(60.7095026547583,247.635518310246,21.098763215029)) ;
#114331 = CARTESIAN_POINT('Ctrl Pts',(60.7067083048646,247.56887036202,21.1152460418431)) ;
#114332 = CARTESIAN_POINT('Ctrl Pts',(60.7054361265197,247.538527677785,21.12275014696)) ;
#114333 = CARTESIAN_POINT('Ctrl Pts',(60.7041639481749,247.508388377401,21.1309729915753)) ;
#114334 = CARTESIAN_POINT('Ctrl Pts',(60.70289176983,247.4784883761,21.1399008917264)) ;
#114335 = CARTESIAN_POINT('Ctrl Pts',(60.7000915271226,247.4126742857,21.1595524503236)) ;
#114336 = CARTESIAN_POINT('Ctrl Pts',(60.6972912844152,247.347767441634,21.1826988792258)) ;
#114337 = CARTESIAN_POINT('Ctrl Pts',(60.6944910417078,247.284164349133,21.2092375935824)) ;
#114338 = CARTESIAN_POINT('Ctrl Pts',(60.6916949036419,247.220654487084,21.2357374070584)) ;
#114339 = CARTESIAN_POINT('Ctrl Pts',(60.688898765576,247.15844503129,21.2656194488466)) ;
#114340 = CARTESIAN_POINT('Ctrl Pts',(60.68610262751,247.09791714036,21.2987314319828)) ;
#114341 = CARTESIAN_POINT('Ctrl Pts',(60.6833096520937,247.037457711181,21.331805962891)) ;
#114342 = CARTESIAN_POINT('Ctrl Pts',(60.6805166766774,246.9786764964,21.3681029451052)) ;
#114343 = CARTESIAN_POINT('Ctrl Pts',(60.6777237012611,246.921932836441,21.4074228310548)) ;
#114344 = CARTESIAN_POINT('Ctrl Pts',(60.6749324018922,246.865223228005,21.4467191213821)) ;
#114345 = CARTESIAN_POINT('Ctrl Pts',(60.6721411025233,246.810549149747,21.4890344383072)) ;
#114346 = CARTESIAN_POINT('Ctrl Pts',(60.6693498031544,246.758242239952,21.5341251255906)) ;
#114347 = CARTESIAN_POINT('Ctrl Pts',(60.6665592337996,246.705949010089,21.5792040202154)) ;
#114348 = CARTESIAN_POINT('Ctrl Pts',(60.6637686644449,246.656022089808,21.6270565246742)) ;
#114349 = CARTESIAN_POINT('Ctrl Pts',(60.6609780950902,246.608759804541,21.6773989110412)) ;
#114350 = CARTESIAN_POINT('Ctrl Pts',(60.6581873108187,246.561493879352,21.7277451745457)) ;
#114351 = CARTESIAN_POINT('Ctrl Pts',(60.6553965265472,246.516893329597,21.7805813422929)) ;
#114352 = CARTESIAN_POINT('Ctrl Pts',(60.6526057422757,246.475218158088,21.8355883775404)) ;
#114353 = CARTESIAN_POINT('Ctrl Pts',(60.6498119735595,246.433498419448,21.8906542369183)) ;
#114354 = CARTESIAN_POINT('Ctrl Pts',(60.6470182048433,246.394710598093,21.9478952060108)) ;
#114355 = CARTESIAN_POINT('Ctrl Pts',(60.6442244361271,246.359072471378,22.0069616450271)) ;
#114356 = CARTESIAN_POINT('Ctrl Pts',(60.6414289717839,246.323412714753,22.0660639333415)) ;
#114357 = CARTESIAN_POINT('Ctrl Pts',(60.6386335074407,246.290906688001,22.1269934651638)) ;
#114358 = CARTESIAN_POINT('Ctrl Pts',(60.6358380430975,246.261725797918,22.189376731736)) ;
#114359 = CARTESIAN_POINT('Ctrl Pts',(60.6330378190237,246.232495222646,22.2518662159187)) ;
#114360 = CARTESIAN_POINT('Ctrl Pts',(60.6302375949499,246.206601267018,22.3158139217921)) ;
#114361 = CARTESIAN_POINT('Ctrl Pts',(60.6274373708761,246.184166573019,22.3808279710544)) ;
#114362 = CARTESIAN_POINT('Ctrl Pts',(60.6262140218656,246.17436540712,22.4092310097893)) ;
#114363 = CARTESIAN_POINT('Ctrl Pts',(60.624990672855,246.165223824895,22.4378374014921)) ;
#114364 = CARTESIAN_POINT('Ctrl Pts',(60.6237673238445,246.156748995185,22.4666138413696)) ;
#114365 = CARTESIAN_POINT('Ctrl Pts',(60.6209728463264,246.137390070716,22.5323474248334)) ;
#114366 = CARTESIAN_POINT('Ctrl Pts',(60.6181783688083,246.121437928544,22.5992261940902)) ;
#114367 = CARTESIAN_POINT('Ctrl Pts',(60.6153838912903,246.109023833977,22.6668638690292)) ;
#114368 = CARTESIAN_POINT('Ctrl Pts',(60.6125936203238,246.096628426456,22.7343997283795)) ;
#114369 = CARTESIAN_POINT('Ctrl Pts',(60.6098033493574,246.087760584623,22.8026917465618)) ;
#114370 = CARTESIAN_POINT('Ctrl Pts',(60.607013078391,246.082501613517,22.871339176387)) ;
#114371 = CARTESIAN_POINT('Ctrl Pts',(60.6042260913646,246.077248831826,22.9399058133263)) ;
#114372 = CARTESIAN_POINT('Ctrl Pts',(60.6014391043382,246.075596522822,23.0088265433377)) ;
#114373 = CARTESIAN_POINT('Ctrl Pts',(60.5986521173118,246.077574510736,23.0776929455325)) ;
#114374 = CARTESIAN_POINT('Ctrl Pts',(60.5958668779608,246.079551258286,23.1465161627001)) ;
#114375 = CARTESIAN_POINT('Ctrl Pts',(60.5930816386097,246.085153772792,23.2152846293504)) ;
#114376 = CARTESIAN_POINT('Ctrl Pts',(60.5902963992586,246.094359805167,23.2835889143811)) ;
#114377 = CARTESIAN_POINT('Ctrl Pts',(60.5875119520576,246.103563219255,23.3518737729869)) ;
#114378 = CARTESIAN_POINT('Ctrl Pts',(60.5847275048566,246.116368051003,23.4196942250991)) ;
#114379 = CARTESIAN_POINT('Ctrl Pts',(60.5819430576555,246.132700280669,23.4866467669927)) ;
#114380 = CARTESIAN_POINT('Ctrl Pts',(60.5791584482503,246.149033461747,23.553603209116)) ;
#114381 = CARTESIAN_POINT('Ctrl Pts',(60.5763738388451,246.168894329681,23.6196911636752)) ;
#114382 = CARTESIAN_POINT('Ctrl Pts',(60.5735892294399,246.192158342209,23.6845198859525)) ;
#114383 = CARTESIAN_POINT('Ctrl Pts',(60.5708016727571,246.215446977761,23.7494172240416)) ;
#114384 = CARTESIAN_POINT('Ctrl Pts',(60.5680141160744,246.242145779759,23.8130522064917)) ;
#114385 = CARTESIAN_POINT('Ctrl Pts',(60.5652265593917,246.272081496719,23.8750527182253)) ;
#114386 = CARTESIAN_POINT('Ctrl Pts',(60.56243733713,246.302035100417,23.9370902755716)) ;
#114387 = CARTESIAN_POINT('Ctrl Pts',(60.5596481148684,246.335229231385,23.9974909877557)) ;
#114388 = CARTESIAN_POINT('Ctrl Pts',(60.5568588926067,246.371445317106,24.0559085496765)) ;
#114389 = CARTESIAN_POINT('Ctrl Pts',(60.5540648918213,246.407723448592,24.1144261931551)) ;
#114390 = CARTESIAN_POINT('Ctrl Pts',(60.5512708910359,246.447033586875,24.170953502343)) ;
#114391 = CARTESIAN_POINT('Ctrl Pts',(60.5484768902505,246.489115146096,24.225175005198)) ;
#114392 = CARTESIAN_POINT('Ctrl Pts',(60.54719888612,246.508363675582,24.2499764673062)) ;
#114393 = CARTESIAN_POINT('Ctrl Pts',(60.5459208819895,246.528191518457,24.2742959840743)) ;
#114394 = CARTESIAN_POINT('Ctrl Pts',(60.544642877859,246.548571183694,24.2981059507884)) ;
#114395 = CARTESIAN_POINT('Ctrl Pts',(60.541846472607,246.593163999588,24.350204621192)) ;
#114396 = CARTESIAN_POINT('Ctrl Pts',(60.539050067355,246.640576967329,24.4000665435235)) ;
#114397 = CARTESIAN_POINT('Ctrl Pts',(60.5362536621031,246.690557083637,24.4473710087)) ;
#114398 = CARTESIAN_POINT('Ctrl Pts',(60.5334614409992,246.740462416718,24.4946046941182)) ;
#114399 = CARTESIAN_POINT('Ctrl Pts',(60.5306692198953,246.792926921071,24.5392881825583)) ;
#114400 = CARTESIAN_POINT('Ctrl Pts',(60.5278769987914,246.847658276922,24.5811348187384)) ;
#114401 = CARTESIAN_POINT('Ctrl Pts',(60.525088038235,246.902325721579,24.622932589538)) ;
#114402 = CARTESIAN_POINT('Ctrl Pts',(60.5222990776787,246.959254372302,24.6618997906813)) ;
#114403 = CARTESIAN_POINT('Ctrl Pts',(60.5195101171224,247.018117457038,24.6977887834864)) ;
#114404 = CARTESIAN_POINT('Ctrl Pts',(60.5167228909016,247.076943937332,24.7336554584578)) ;
#114405 = CARTESIAN_POINT('Ctrl Pts',(60.5139356646809,247.137702047111,24.7664474675678)) ;
#114406 = CARTESIAN_POINT('Ctrl Pts',(60.5111484384601,247.200035823984,24.7959603072259)) ;
#114407 = CARTESIAN_POINT('Ctrl Pts',(60.5083619941295,247.262352114596,24.8254648677579)) ;
#114408 = CARTESIAN_POINT('Ctrl Pts',(60.5055755497989,247.326242751377,24.8516918751861)) ;
#114409 = CARTESIAN_POINT('Ctrl Pts',(60.5027891054682,247.391328556904,24.8744834780218)) ;
#114410 = CARTESIAN_POINT('Ctrl Pts',(60.500002491741,247.4564183192,24.8972764664297)) ;
#114411 = CARTESIAN_POINT('Ctrl Pts',(60.4972158780138,247.522702930432,24.9166334758251)) ;
#114412 = CARTESIAN_POINT('Ctrl Pts',(60.4944292642866,247.589786397934,24.9324459757382)) ;
#114413 = CARTESIAN_POINT('Ctrl Pts',(60.4916397061812,247.656940746841,24.9482751833776)) ;
#114414 = CARTESIAN_POINT('Ctrl Pts',(60.4888501480758,247.724895157914,24.9605522946353)) ;
#114415 = CARTESIAN_POINT('Ctrl Pts',(60.4860605899705,247.793242726614,24.9692197745365)) ;
#114416 = CARTESIAN_POINT('Ctrl Pts',(60.4832693650643,247.861631133963,24.9778924333808)) ;
#114417 = CARTESIAN_POINT('Ctrl Pts',(60.4804781401581,247.93041267696,24.9829511322373)) ;
#114418 = CARTESIAN_POINT('Ctrl Pts',(60.4776869152519,247.999177392859,24.9843904008123)) ;
#114419 = CARTESIAN_POINT('Ctrl Pts',(60.4748909308483,248.068059363904,24.9858321235768)) ;
#114420 = CARTESIAN_POINT('Ctrl Pts',(60.4720949464448,248.136923960343,24.9836421141915)) ;
#114421 = CARTESIAN_POINT('Ctrl Pts',(60.4692989620412,248.205364171719,24.9778669310674)) ;
#114422 = CARTESIAN_POINT('Ctrl Pts',(60.4680387853186,248.236210824925,24.9752640011897)) ;
#114423 = CARTESIAN_POINT('Ctrl Pts',(60.4667786085961,248.266971381999,24.9719334791067)) ;
#114424 = CARTESIAN_POINT('Ctrl Pts',(60.4655184318735,248.297609316392,24.9678830084377)) ;
#114425 = CARTESIAN_POINT('Ctrl Pts',(60.4627217313374,248.365603849224,24.9588938299453)) ;
#114426 = CARTESIAN_POINT('Ctrl Pts',(60.4599250308014,248.433259765759,24.9463201701829)) ;
#114427 = CARTESIAN_POINT('Ctrl Pts',(60.4571283302653,248.500170205801,24.9301994782405)) ;
#114428 = CARTESIAN_POINT('Ctrl Pts',(60.454335802507,248.566980813061,24.9141028389498)) ;
#114429 = CARTESIAN_POINT('Ctrl Pts',(60.4515432747487,248.633047678172,24.8944697854931)) ;
#114430 = CARTESIAN_POINT('Ctrl Pts',(60.4487507469903,248.697971081105,24.8713892889397)) ;
#114431 = CARTESIAN_POINT('Ctrl Pts',(60.4459614644379,248.762819036333,24.8483356143094)) ;
#114432 = CARTESIAN_POINT('Ctrl Pts',(60.4431721818855,248.826525708382,24.8218426171166)) ;
#114433 = CARTESIAN_POINT('Ctrl Pts',(60.4403828993332,248.888705325434,24.7920494157437)) ;
#114434 = CARTESIAN_POINT('Ctrl Pts',(60.4375953417695,248.950846488462,24.7622746395159)) ;
#114435 = CARTESIAN_POINT('Ctrl Pts',(60.4348077842058,249.011462028446,24.7292039195699)) ;
#114436 = CARTESIAN_POINT('Ctrl Pts',(60.4320202266421,249.070186442763,24.6930243525755)) ;
#114437 = CARTESIAN_POINT('Ctrl Pts',(60.4292334421206,249.128894571694,24.6568548188564)) ;
#114438 = CARTESIAN_POINT('Ctrl Pts',(60.4264466575992,249.185712198593,24.6175784069928)) ;
#114439 = CARTESIAN_POINT('Ctrl Pts',(60.4236598730777,249.240300293076,24.5754270979577)) ;
#114440 = CARTESIAN_POINT('Ctrl Pts',(60.4208729108012,249.294891869461,24.5332731003019)) ;
#114441 = CARTESIAN_POINT('Ctrl Pts',(60.4180859485247,249.347253244298,24.4882441433253)) ;
#114442 = CARTESIAN_POINT('Ctrl Pts',(60.4152989862482,249.397077582791,24.4406131807398)) ;
#114443 = CARTESIAN_POINT('Ctrl Pts',(60.412509069306,249.446954743765,24.3929317210332)) ;
#114444 = CARTESIAN_POINT('Ctrl Pts',(60.4097191523638,249.494289145367,24.3426430902747)) ;
#114445 = CARTESIAN_POINT('Ctrl Pts',(60.4069292354216,249.538810766896,24.2900571789836)) ;
#114446 = CARTESIAN_POINT('Ctrl Pts',(60.4041376452774,249.583359089459,24.237439730248)) ;
#114447 = CARTESIAN_POINT('Ctrl Pts',(60.4013460551333,249.625090977645,24.1825226496002)) ;
#114448 = CARTESIAN_POINT('Ctrl Pts',(60.3985544649891,249.663778400683,24.1256467616923)) ;
#114449 = CARTESIAN_POINT('Ctrl Pts',(60.3957581092698,249.702531867736,24.068673779906)) ;
#114450 = CARTESIAN_POINT('Ctrl Pts',(60.3929617535506,249.738230242976,24.0097357365423)) ;
#114451 = CARTESIAN_POINT('Ctrl Pts',(60.3901653978313,249.770690729435,23.9491993324047)) ;
#114452 = CARTESIAN_POINT('Ctrl Pts',(60.3889082605168,249.785283754383,23.9219844212257)) ;
#114453 = CARTESIAN_POINT('Ctrl Pts',(60.3876511232024,249.799223023744,23.8944467542978)) ;
#114454 = CARTESIAN_POINT('Ctrl Pts',(60.3863939858879,249.812495138397,23.8666208632575)) ;
#114455 = CARTESIAN_POINT('Ctrl Pts',(60.3833813626935,249.844300638067,23.7999384700241)) ;
#114456 = CARTESIAN_POINT('Ctrl Pts',(60.3803687394992,249.872381270698,23.7313699924473)) ;
#114457 = CARTESIAN_POINT('Ctrl Pts',(60.3773561163049,249.896528208531,23.6613356174494)) ;
#114458 = CARTESIAN_POINT('Ctrl Pts',(60.3743507893122,249.92061666546,23.5914708570667)) ;
#114459 = CARTESIAN_POINT('Ctrl Pts',(60.3713454623195,249.940790267254,23.520147609701)) ;
#114460 = CARTESIAN_POINT('Ctrl Pts',(60.3683401353268,249.956887480057,23.4478070750172)) ;
#114461 = CARTESIAN_POINT('Ctrl Pts',(60.3653462472982,249.972923423175,23.3757418850056)) ;
#114462 = CARTESIAN_POINT('Ctrl Pts',(60.3623523592696,249.984913803617,23.3026674779063)) ;
#114463 = CARTESIAN_POINT('Ctrl Pts',(60.359358471241,249.992746915436,23.2290390013499)) ;
#114464 = CARTESIAN_POINT('Ctrl Pts',(60.3565649437256,250.000055810489,23.1603379767246)) ;
#114465 = CARTESIAN_POINT('Ctrl Pts',(60.3537714162101,250.003745611572,23.0911549666261)) ;
#114466 = CARTESIAN_POINT('Ctrl Pts',(60.3509778886947,250.003765030662,23.0218706758452)) ;
#114467 = CARTESIAN_POINT('',(59.8509778886854,250.003764316488,23.0195575538546)) ;
#114468 = CARTESIAN_POINT('Ctrl Pts',(60.3509778886564,250.003765030662,23.0218706748954)) ;
#114469 = CARTESIAN_POINT('Ctrl Pts',(60.3481156163826,250.003784927595,22.9508813957776)) ;
#114470 = CARTESIAN_POINT('Ctrl Pts',(60.3452533441087,249.999950618947,22.8799290676602)) ;
#114471 = CARTESIAN_POINT('Ctrl Pts',(60.3423910718349,249.992300212387,22.8094449075012)) ;
#114472 = CARTESIAN_POINT('Ctrl Pts',(60.3394642775072,249.984477348459,22.7373718758636)) ;
#114473 = CARTESIAN_POINT('Ctrl Pts',(60.3365374831795,249.972664300783,22.665788871538)) ;
#114474 = CARTESIAN_POINT('Ctrl Pts',(60.3336106888518,249.956957141299,22.5951467889264)) ;
#114475 = CARTESIAN_POINT('Ctrl Pts',(60.3307403892547,249.941553170779,22.5258682819477)) ;
#114476 = CARTESIAN_POINT('Ctrl Pts',(60.3278700896576,249.922404298269,22.4574951094046)) ;
#114477 = CARTESIAN_POINT('Ctrl Pts',(60.3249997900605,249.899651448691,22.3904362929958)) ;
#114478 = CARTESIAN_POINT('Ctrl Pts',(60.3220447483675,249.876226848971,22.3213976467955)) ;
#114479 = CARTESIAN_POINT('Ctrl Pts',(60.3190897066745,249.848982314889,22.253752671223)) ;
#114480 = CARTESIAN_POINT('Ctrl Pts',(60.3161346649815,249.818123636963,22.1879228992188)) ;
#114481 = CARTESIAN_POINT('Ctrl Pts',(60.3131796232885,249.787264959037,22.1220931272147)) ;
#114482 = CARTESIAN_POINT('Ctrl Pts',(60.3102245815955,249.75279244704,22.0580789757814)) ;
#114483 = CARTESIAN_POINT('Ctrl Pts',(60.3072695399025,249.7149604943,21.9962702899579)) ;
#114484 = CARTESIAN_POINT('Ctrl Pts',(60.3044731809281,249.679160078756,21.9377806673909)) ;
#114485 = CARTESIAN_POINT('Ctrl Pts',(60.3016768219538,249.640221610421,21.8810541208869)) ;
#114486 = CARTESIAN_POINT('Ctrl Pts',(60.2988804629795,249.598344256327,21.8264472888461)) ;
#114487 = CARTESIAN_POINT('Ctrl Pts',(60.2960882846115,249.556529509622,21.7719220949892)) ;
#114488 = CARTESIAN_POINT('Ctrl Pts',(60.2932961062435,249.511784893843,21.7195107122991)) ;
#114489 = CARTESIAN_POINT('Ctrl Pts',(60.2905039278755,249.464353777528,21.6695423622655)) ;
#114490 = CARTESIAN_POINT('Ctrl Pts',(60.2877150045518,249.416977955098,21.6196322639534)) ;
#114491 = CARTESIAN_POINT('Ctrl Pts',(60.2849260812282,249.366922188642,21.5721598961588)) ;
#114492 = CARTESIAN_POINT('Ctrl Pts',(60.2821371579046,249.314470029272,21.5274213951497)) ;
#114493 = CARTESIAN_POINT('Ctrl Pts',(60.279349965464,249.262050423165,21.4827106600924)) ;
#114494 = CARTESIAN_POINT('Ctrl Pts',(60.2765627730233,249.207237747198,21.4407307436908)) ;
#114495 = CARTESIAN_POINT('Ctrl Pts',(60.2737755805827,249.150351188822,21.4017397982671)) ;
#114496 = CARTESIAN_POINT('Ctrl Pts',(60.2709891665113,249.093480516952,21.362759741705)) ;
#114497 = CARTESIAN_POINT('Ctrl Pts',(60.2682027524399,249.034537517161,21.326767276302)) ;
#114498 = CARTESIAN_POINT('Ctrl Pts',(60.2654163383685,248.973871668104,21.2939781537975)) ;
#114499 = CARTESIAN_POINT('Ctrl Pts',(60.2626297513077,248.913202052718,21.2611869956402)) ;
#114500 = CARTESIAN_POINT('Ctrl Pts',(60.2598431642469,248.850809808714,21.2315998063246)) ;
#114501 = CARTESIAN_POINT('Ctrl Pts',(60.2570565771861,248.787068807701,21.2053862908493)) ;
#114502 = CARTESIAN_POINT('Ctrl Pts',(60.2542670400896,248.723260326928,21.1791450242923)) ;
#114503 = CARTESIAN_POINT('Ctrl Pts',(60.2514775029931,248.658100694404,21.1562847461771)) ;
#114504 = CARTESIAN_POINT('Ctrl Pts',(60.2486879658967,248.591982610388,21.1369265292726)) ;
#114505 = CARTESIAN_POINT('Ctrl Pts',(60.2458967587889,248.52582494348,21.1175567231909)) ;
#114506 = CARTESIAN_POINT('Ctrl Pts',(60.2431055516812,248.458708160783,21.1016932639497)) ;
#114507 = CARTESIAN_POINT('Ctrl Pts',(60.2403143445735,248.391036203635,21.0894062957001)) ;
#114508 = CARTESIAN_POINT('Ctrl Pts',(60.2375183728113,248.323248728905,21.0770983533139)) ;
#114509 = CARTESIAN_POINT('Ctrl Pts',(60.234722401049,248.254904674889,21.0683791485604)) ;
#114510 = CARTESIAN_POINT('Ctrl Pts',(60.2319264292868,248.186413283751,21.0632669835456)) ;
#114511 = CARTESIAN_POINT('Ctrl Pts',(60.2306659841635,248.155536848906,21.0609623810638)) ;
#114512 = CARTESIAN_POINT('Ctrl Pts',(60.2294055390402,248.124630469464,21.0593901220682)) ;
#114513 = CARTESIAN_POINT('Ctrl Pts',(60.2281450939169,248.093731443593,21.0585484258536)) ;
#114514 = CARTESIAN_POINT('Ctrl Pts',(60.2253487256112,248.025180219086,21.056681075523)) ;
#114515 = CARTESIAN_POINT('Ctrl Pts',(60.2225523573054,247.956396648871,21.0584056752074)) ;
#114516 = CARTESIAN_POINT('Ctrl Pts',(60.2197559889997,247.887788298727,21.063749636612)) ;
#114517 = CARTESIAN_POINT('Ctrl Pts',(60.2169638004718,247.819282498616,21.0690856103094)) ;
#114518 = CARTESIAN_POINT('Ctrl Pts',(60.2141716119439,247.750951884224,21.0780301705784)) ;
#114519 = CARTESIAN_POINT('Ctrl Pts',(60.2113794234159,247.683205127758,21.0905587268232)) ;
#114520 = CARTESIAN_POINT('Ctrl Pts',(60.208590488753,247.615537319686,21.1030726829685)) ;
#114521 = CARTESIAN_POINT('Ctrl Pts',(60.20580155409,247.548452498587,21.1191622511027)) ;
#114522 = CARTESIAN_POINT('Ctrl Pts',(60.2030126194271,247.48235350046,21.1387511181628)) ;
#114523 = CARTESIAN_POINT('Ctrl Pts',(60.2002254149202,247.416295507804,21.1583278329855)) ;
#114524 = CARTESIAN_POINT('Ctrl Pts',(60.1974382104132,247.351222594435,21.1813994010614)) ;
#114525 = CARTESIAN_POINT('Ctrl Pts',(60.1946510059063,247.287525174951,21.2078389282935)) ;
#114526 = CARTESIAN_POINT('Ctrl Pts',(60.1918645790591,247.223845527724,21.2342710786165)) ;
#114527 = CARTESIAN_POINT('Ctrl Pts',(60.1890781522118,247.16154106557,21.264069134426)) ;
#114528 = CARTESIAN_POINT('Ctrl Pts',(60.1862917253646,247.10098316542,21.2970576945569)) ;
#114529 = CARTESIAN_POINT('Ctrl Pts',(60.183505124835,247.040421490602,21.3300483109162)) ;
#114530 = CARTESIAN_POINT('Ctrl Pts',(60.1807185243054,246.981607023702,21.3662295893756)) ;
#114531 = CARTESIAN_POINT('Ctrl Pts',(60.1779319237758,246.924885832193,21.4053805793426)) ;
#114532 = CARTESIAN_POINT('Ctrl Pts',(60.1751423722518,246.868104573257,21.4445730299903)) ;
#114533 = CARTESIAN_POINT('Ctrl Pts',(60.1723528207277,246.813421418289,21.4867411889387)) ;
#114534 = CARTESIAN_POINT('Ctrl Pts',(60.1695632692037,246.761151924879,21.5316218118715)) ;
#114535 = CARTESIAN_POINT('Ctrl Pts',(60.1667720470989,246.7088511288,21.5765293124957)) ;
#114536 = CARTESIAN_POINT('Ctrl Pts',(60.1639808249941,246.658967226175,21.6241521711496)) ;
#114537 = CARTESIAN_POINT('Ctrl Pts',(60.1611896028893,246.611779203611,21.6741899595309)) ;
#114538 = CARTESIAN_POINT('Ctrl Pts',(60.1583936154072,246.564510618226,21.7243131760609)) ;
#114539 = CARTESIAN_POINT('Ctrl Pts',(60.1555976279252,246.519947415956,21.7768591767358)) ;
#114540 = CARTESIAN_POINT('Ctrl Pts',(60.1528016404432,246.478328008864,21.8314948315574)) ;
#114541 = CARTESIAN_POINT('Ctrl Pts',(60.1515413096059,246.459567473446,21.8561226244312)) ;
#114542 = CARTESIAN_POINT('Ctrl Pts',(60.1502809787687,246.441404490081,21.8811746272296)) ;
#114543 = CARTESIAN_POINT('Ctrl Pts',(60.1490206479314,246.423857890794,21.9066186081808)) ;
#114544 = CARTESIAN_POINT('Ctrl Pts',(60.1462243320115,246.384926974025,21.9630715702901)) ;
#114545 = CARTESIAN_POINT('Ctrl Pts',(60.1434280160915,246.348880673387,22.0216771985092)) ;
#114546 = CARTESIAN_POINT('Ctrl Pts',(60.1406317001716,246.315964132663,22.0821087608005)) ;
#114547 = CARTESIAN_POINT('Ctrl Pts',(60.1378395650777,246.283096806096,22.1424499706933)) ;
#114548 = CARTESIAN_POINT('Ctrl Pts',(60.1350474299839,246.253350185016,22.2046112686915)) ;
#114549 = CARTESIAN_POINT('Ctrl Pts',(60.13225529489,246.226926419963,22.2682366475178)) ;
#114550 = CARTESIAN_POINT('Ctrl Pts',(60.129466414945,246.200533460472,22.3317878501041)) ;
#114551 = CARTESIAN_POINT('Ctrl Pts',(60.126677535,246.177455850471,22.3967992923198)) ;
#114552 = CARTESIAN_POINT('Ctrl Pts',(60.1238886550551,246.157849197065,22.4628916649776)) ;
#114553 = CARTESIAN_POINT('Ctrl Pts',(60.1211015060306,246.138254712543,22.528943017354)) ;
#114554 = CARTESIAN_POINT('Ctrl Pts',(60.118314357006,246.122127050301,22.5960734997507)) ;
#114555 = CARTESIAN_POINT('Ctrl Pts',(60.1155272079815,246.109572641203,22.6638866441411)) ;
#114556 = CARTESIAN_POINT('Ctrl Pts',(60.1127408372949,246.097021738043,22.7316808510648)) ;
#114557 = CARTESIAN_POINT('Ctrl Pts',(60.1099544666084,246.088042196262,22.80015685909)) ;
#114558 = CARTESIAN_POINT('Ctrl Pts',(60.1071680959218,246.082689402512,22.8689077190084)) ;
#114559 = CARTESIAN_POINT('Ctrl Pts',(60.1043815521456,246.077336276246,22.9376628497352)) ;
#114560 = CARTESIAN_POINT('Ctrl Pts',(60.1015950083695,246.075610380834,23.0066923767052)) ;
#114561 = CARTESIAN_POINT('Ctrl Pts',(60.0988084645933,246.077515119444,23.0755857401096)) ;
#114562 = CARTESIAN_POINT('Ctrl Pts',(60.0960189703294,246.079421874856,23.1445520501628)) ;
#114563 = CARTESIAN_POINT('Ctrl Pts',(60.0932294760654,246.084966922447,23.2133814173607)) ;
#114564 = CARTESIAN_POINT('Ctrl Pts',(60.0904399818014,246.094101576605,23.2816658061659)) ;
#114565 = CARTESIAN_POINT('Ctrl Pts',(60.0876488173283,246.103241700135,23.3499910802353)) ;
#114566 = CARTESIAN_POINT('Ctrl Pts',(60.0848576528552,246.115975617192,23.4177702440408)) ;
#114567 = CARTESIAN_POINT('Ctrl Pts',(60.0820664883821,246.132203533377,23.4846056533459)) ;
#114568 = CARTESIAN_POINT('Ctrl Pts',(60.0792705585032,246.148459155778,23.5515551719592)) ;
#114569 = CARTESIAN_POINT('Ctrl Pts',(60.0764746286243,246.168220542193,23.6175572503759)) ;
#114570 = CARTESIAN_POINT('Ctrl Pts',(60.0736786987453,246.19133836498,23.6822304355829)) ;
#114571 = CARTESIAN_POINT('Ctrl Pts',(60.0724178664789,246.20176341073,23.7113949862754)) ;
#114572 = CARTESIAN_POINT('Ctrl Pts',(60.0711570342124,246.212870371109,23.7402895834809)) ;
#114573 = CARTESIAN_POINT('Ctrl Pts',(60.0698962019459,246.224642467898,23.7688808290893)) ;
#114574 = CARTESIAN_POINT('Ctrl Pts',(60.0670998615051,246.250751246359,23.8322920047631)) ;
#114575 = CARTESIAN_POINT('Ctrl Pts',(60.0643035210644,246.280237194779,23.8944581076416)) ;
#114576 = CARTESIAN_POINT('Ctrl Pts',(60.0615071806236,246.312960002354,23.9549955133845)) ;
#114577 = CARTESIAN_POINT('Ctrl Pts',(60.0587150206563,246.345633889981,24.0154424169087)) ;
#114578 = CARTESIAN_POINT('Ctrl Pts',(60.0559228606889,246.38153480094,24.0742650275334)) ;
#114579 = CARTESIAN_POINT('Ctrl Pts',(60.0531307007216,246.420474446045,24.1310998091008)) ;
#114580 = CARTESIAN_POINT('Ctrl Pts',(60.0503417955066,246.459368700161,24.187868339758)) ;
#114581 = CARTESIAN_POINT('Ctrl Pts',(60.0475528902916,246.501294377167,24.2426532404599)) ;
#114582 = CARTESIAN_POINT('Ctrl Pts',(60.0447639850766,246.546018282303,24.2951172954059)) ;
#114583 = CARTESIAN_POINT('Ctrl Pts',(60.0419768105513,246.590714433464,24.3475487931324)) ;
#114584 = CARTESIAN_POINT('Ctrl Pts',(60.039189636026,246.638205050219,24.3976619295297)) ;
#114585 = CARTESIAN_POINT('Ctrl Pts',(60.0364024615007,246.688215747403,24.4451513648145)) ;
#114586 = CARTESIAN_POINT('Ctrl Pts',(60.0336160651225,246.738212482176,24.4926275415953)) ;
#114587 = CARTESIAN_POINT('Ctrl Pts',(60.0308296687442,246.790727544799,24.5374811336974)) ;
#114588 = CARTESIAN_POINT('Ctrl Pts',(60.028043272366,246.845449939911,24.5794438831465)) ;
#114589 = CARTESIAN_POINT('Ctrl Pts',(60.025256702747,246.900175737319,24.6214092415769)) ;
#114590 = CARTESIAN_POINT('Ctrl Pts',(60.0224701331281,246.957108748631,24.6604831038896)) ;
#114591 = CARTESIAN_POINT('Ctrl Pts',(60.0196835635092,247.015906616421,24.6964388262848)) ;
#114592 = CARTESIAN_POINT('Ctrl Pts',(60.0168940433521,247.074766741887,24.7324326201246)) ;
#114593 = CARTESIAN_POINT('Ctrl Pts',(60.014104523195,247.135495244891,24.7653014286367)) ;
#114594 = CARTESIAN_POINT('Ctrl Pts',(60.0113150030379,247.197723491837,24.7948636543907)) ;
#114595 = CARTESIAN_POINT('Ctrl Pts',(60.0085238126059,247.259988999052,24.8244435810532)) ;
#114596 = CARTESIAN_POINT('Ctrl Pts',(60.005732622174,247.323755583584,24.8507127975332)) ;
#114597 = CARTESIAN_POINT('Ctrl Pts',(60.0029414317421,247.388635465295,24.8735382192499)) ;
#114598 = CARTESIAN_POINT('Ctrl Pts',(60.0001454760743,247.453626112625,24.8964026094713)) ;
#114599 = CARTESIAN_POINT('Ctrl Pts',(59.9973495204066,247.519733379805,24.9158113327619)) ;
#114600 = CARTESIAN_POINT('Ctrl Pts',(59.9945535647388,247.58655606146,24.9316816578878)) ;
#114601 = CARTESIAN_POINT('Ctrl Pts',(59.9932929618127,247.616684174362,24.9388370568535)) ;
#114602 = CARTESIAN_POINT('Ctrl Pts',(59.9920323588865,247.646957607263,24.9452738653652)) ;
#114603 = CARTESIAN_POINT('Ctrl Pts',(59.9907717559603,247.677339235002,24.950987947284)) ;
#114604 = CARTESIAN_POINT('Ctrl Pts',(59.9879754166289,247.744733446798,24.9636632407334)) ;
#114605 = CARTESIAN_POINT('Ctrl Pts',(59.9851790772975,247.812924652615,24.972828510126)) ;
#114606 = CARTESIAN_POINT('Ctrl Pts',(59.9823827379661,247.881514747908,24.9783922822575)) ;
#114607 = CARTESIAN_POINT('Ctrl Pts',(59.9795905790604,247.950002303501,24.9839477367518)) ;
#114608 = CARTESIAN_POINT('Ctrl Pts',(59.9767984201546,248.018887079666,24.9859123407111)) ;
#114609 = CARTESIAN_POINT('Ctrl Pts',(59.9740062612489,248.087761661209,24.9842457948727)) ;
#114610 = CARTESIAN_POINT('Ctrl Pts',(59.9712173570191,248.156555959199,24.9825811916411)) ;
#114611 = CARTESIAN_POINT('Ctrl Pts',(59.9684284527892,248.22533959777,24.9772938568956)) ;
#114612 = CARTESIAN_POINT('Ctrl Pts',(59.9656395485594,248.293702750956,24.9683954861837)) ;
#114613 = CARTESIAN_POINT('Ctrl Pts',(59.962852374971,248.362023481706,24.9595026373141)) ;
#114614 = CARTESIAN_POINT('Ctrl Pts',(59.9600652013827,248.429923759056,24.9470032610149)) ;
#114615 = CARTESIAN_POINT('Ctrl Pts',(59.9572780277943,248.496998029126,24.9309609612058)) ;
#114616 = CARTESIAN_POINT('Ctrl Pts',(59.9544916323032,248.564053574025,24.914923139937)) ;
#114617 = CARTESIAN_POINT('Ctrl Pts',(59.9517052368121,248.630283092308,24.895344472913)) ;
#114618 = CARTESIAN_POINT('Ctrl Pts',(59.948918841321,248.695292163224,24.8723394700529)) ;
#114619 = CARTESIAN_POINT('Ctrl Pts',(59.9461322725377,248.760305277201,24.84933303646)) ;
#114620 = CARTESIAN_POINT('Ctrl Pts',(59.9433457037544,248.824097331273,24.8229000101322)) ;
#114621 = CARTESIAN_POINT('Ctrl Pts',(59.9405591349711,248.886291698344,24.793203877562)) ;
#114622 = CARTESIAN_POINT('Ctrl Pts',(59.9377696155656,248.948551921344,24.7634763005621)) ;
#114623 = CARTESIAN_POINT('Ctrl Pts',(59.9349800961602,249.009210637454,24.7304789338125)) ;
#114624 = CARTESIAN_POINT('Ctrl Pts',(59.9321905767547,249.067914662949,24.6944218472864)) ;
#114625 = CARTESIAN_POINT('Ctrl Pts',(59.9293993870275,249.126653839523,24.6583431703248)) ;
#114626 = CARTESIAN_POINT('Ctrl Pts',(59.9266081973002,249.183435591863,24.6192014058172)) ;
#114627 = CARTESIAN_POINT('Ctrl Pts',(59.9238170075729,249.23793697211,24.5772491193738)) ;
#114628 = CARTESIAN_POINT('Ctrl Pts',(59.9210210525298,249.292531400955,24.53522520903)) ;
#114629 = CARTESIAN_POINT('Ctrl Pts',(59.9182250974867,249.344837315308,24.4903815196029)) ;
#114630 = CARTESIAN_POINT('Ctrl Pts',(59.9154291424436,249.394566664796,24.4430093189264)) ;
#114631 = CARTESIAN_POINT('Ctrl Pts',(59.9141685316206,249.416988111212,24.4216506389915)) ;
#114632 = CARTESIAN_POINT('Ctrl Pts',(59.9129079207977,249.43888630985,24.399778427292)) ;
#114633 = CARTESIAN_POINT('Ctrl Pts',(59.9116473099748,249.460237556318,24.3774215549041)) ;
#114634 = CARTESIAN_POINT('Ctrl Pts',(59.9088873770359,249.506983155628,24.3284742768134)) ;
#114635 = CARTESIAN_POINT('Ctrl Pts',(59.9061274440971,249.551298080798,24.2769988443449)) ;
#114636 = CARTESIAN_POINT('Ctrl Pts',(59.9033675111582,249.592892025422,24.2232695540639)) ;
#114637 = CARTESIAN_POINT('Ctrl Pts',(59.900611316268,249.634429635276,24.1696130346455)) ;
#114638 = CARTESIAN_POINT('Ctrl Pts',(59.8978551213778,249.673253261259,24.1137091011783)) ;
#114639 = CARTESIAN_POINT('Ctrl Pts',(59.8950989264875,249.709109865646,24.0558682758293)) ;
#114640 = CARTESIAN_POINT('Ctrl Pts',(59.8923454648814,249.744930911485,23.9980848105057)) ;
#114641 = CARTESIAN_POINT('Ctrl Pts',(59.8895920032753,249.77779050426,23.9383686876626)) ;
#114642 = CARTESIAN_POINT('Ctrl Pts',(59.8868385416692,249.807477523031,23.8770612677907)) ;
#114643 = CARTESIAN_POINT('Ctrl Pts',(59.8840868124706,249.83714586349,23.8157924209773)) ;
#114644 = CARTESIAN_POINT('Ctrl Pts',(59.881335083272,249.863645370605,23.7529347165331)) ;
#114645 = CARTESIAN_POINT('Ctrl Pts',(59.8785833540734,249.886810688586,23.6888543636881)) ;
#114646 = CARTESIAN_POINT('Ctrl Pts',(59.8758314591609,249.909977401622,23.6247701518134)) ;
#114647 = CARTESIAN_POINT('Ctrl Pts',(59.8730795642484,249.929809339602,23.5594636142436)) ;
#114648 = CARTESIAN_POINT('Ctrl Pts',(59.870327669336,249.94618977602,23.4933197175161)) ;
#114649 = CARTESIAN_POINT('Ctrl Pts',(59.8675756586827,249.962570901377,23.427173038871)) ;
#114650 = CARTESIAN_POINT('Ctrl Pts',(59.8648236480295,249.975500126689,23.360189423837)) ;
#114651 = CARTESIAN_POINT('Ctrl Pts',(59.8620716373762,249.984911569834,23.292765342855)) ;
#114652 = CARTESIAN_POINT('Ctrl Pts',(59.8593172440457,249.994331161361,23.2252828864359)) ;
#114653 = CARTESIAN_POINT('Ctrl Pts',(59.8565628507152,250.000226840174,23.1573597050943)) ;
#114654 = CARTESIAN_POINT('Ctrl Pts',(59.8538084573847,250.002584597775,23.0893972795253)) ;
#114655 = CARTESIAN_POINT('Ctrl Pts',(59.8528649344849,250.003392252319,23.0661166158163)) ;
#114656 = CARTESIAN_POINT('Ctrl Pts',(59.8519214115852,250.003785211226,23.0428313468794)) ;
#114657 = CARTESIAN_POINT('Ctrl Pts',(59.8509778886854,250.003764316488,23.0195575538546)) ;
#114658 = CARTESIAN_POINT('',(59.3509778886203,250.003764873166,23.0222802139838)) ;
#114659 = CARTESIAN_POINT('Ctrl Pts',(59.8509778886564,250.003764316487,23.0195575531404)) ;
#114660 = CARTESIAN_POINT('Ctrl Pts',(59.8472606717211,250.003681997014,22.927865303171)) ;
#114661 = CARTESIAN_POINT('Ctrl Pts',(59.8435434547858,249.997173150939,22.8364543306825)) ;
#114662 = CARTESIAN_POINT('Ctrl Pts',(59.8398262378505,249.984377212935,22.7460743215828)) ;
#114663 = CARTESIAN_POINT('Ctrl Pts',(59.8373917798968,249.975996972128,22.6868831751301)) ;
#114664 = CARTESIAN_POINT('Ctrl Pts',(59.834957321943,249.964921092644,22.6281335842206)) ;
#114665 = CARTESIAN_POINT('Ctrl Pts',(59.8325228639892,249.951199394586,22.570030634469)) ;
#114666 = CARTESIAN_POINT('Ctrl Pts',(59.8297265267532,249.935437982417,22.5032907502732)) ;
#114667 = CARTESIAN_POINT('Ctrl Pts',(59.8269301895171,249.916145102473,22.4372466801222)) ;
#114668 = CARTESIAN_POINT('Ctrl Pts',(59.8241338522811,249.893398687161,22.3722993986017)) ;
#114669 = CARTESIAN_POINT('Ctrl Pts',(59.8213416955306,249.870686277425,22.3074492123683)) ;
#114670 = CARTESIAN_POINT('Ctrl Pts',(59.81854953878,249.844530740505,22.2436930199796)) ;
#114671 = CARTESIAN_POINT('Ctrl Pts',(59.8157573820295,249.815060558569,22.1814195411551)) ;
#114672 = CARTESIAN_POINT('Ctrl Pts',(59.8129684800327,249.785624729356,22.1192186531119)) ;
#114673 = CARTESIAN_POINT('Ctrl Pts',(59.8101795780359,249.752882138021,22.0584974875127)) ;
#114674 = CARTESIAN_POINT('Ctrl Pts',(59.8073906760391,249.717009767016,21.9996258697832)) ;
#114675 = CARTESIAN_POINT('Ctrl Pts',(59.8046035047309,249.681159657066,21.9407907855831)) ;
#114676 = CARTESIAN_POINT('Ctrl Pts',(59.8018163334226,249.642183875268,21.8838033905476)) ;
#114677 = CARTESIAN_POINT('Ctrl Pts',(59.7990291621144,249.600305113683,21.8290085428969)) ;
#114678 = CARTESIAN_POINT('Ctrl Pts',(59.7962427689469,249.558438044086,21.7742289932315)) ;
#114679 = CARTESIAN_POINT('Ctrl Pts',(59.7934563757794,249.513669901657,21.7216411654736)) ;
#114680 = CARTESIAN_POINT('Ctrl Pts',(59.790669982612,249.46626538794,21.6715590865221)) ;
#114681 = CARTESIAN_POINT('Ctrl Pts',(59.7878834161924,249.41885792671,21.6214738935717)) ;
#114682 = CARTESIAN_POINT('Ctrl Pts',(59.7850968497728,249.368814108016,21.5738951134417)) ;
#114683 = CARTESIAN_POINT('Ctrl Pts',(59.7823102833533,249.316436176817,21.5291006370254)) ;
#114684 = CARTESIAN_POINT('Ctrl Pts',(59.7795207663561,249.264002784835,21.4842587296273)) ;
#114685 = CARTESIAN_POINT('Ctrl Pts',(59.7767312493589,249.209230721837,21.4422073290829)) ;
#114686 = CARTESIAN_POINT('Ctrl Pts',(59.7739417323616,249.152455296489,21.4031839975887)) ;
#114687 = CARTESIAN_POINT('Ctrl Pts',(59.7711505450715,249.095645875438,21.3641372999007)) ;
#114688 = CARTESIAN_POINT('Ctrl Pts',(59.7683593577814,249.036831123228,21.3281225361919)) ;
#114689 = CARTESIAN_POINT('Ctrl Pts',(59.7655681704912,248.976372919869,21.2953323904856)) ;
#114690 = CARTESIAN_POINT('Ctrl Pts',(59.7627722179044,248.915811498329,21.2624862633075)) ;
#114691 = CARTESIAN_POINT('Ctrl Pts',(59.7599762653176,248.853601468761,21.2328759522848)) ;
#114692 = CARTESIAN_POINT('Ctrl Pts',(59.7571803127307,248.790125923892,21.2066465418893)) ;
#114693 = CARTESIAN_POINT('Ctrl Pts',(59.7559196811551,248.761506241098,21.1948202959398)) ;
#114694 = CARTESIAN_POINT('Ctrl Pts',(59.7546590495795,248.732629510017,21.1836806831018)) ;
#114695 = CARTESIAN_POINT('Ctrl Pts',(59.7533984180038,248.703531738422,21.1732376542069)) ;
#114696 = CARTESIAN_POINT('Ctrl Pts',(59.7506020810814,248.638986970034,21.1500728946966)) ;
#114697 = CARTESIAN_POINT('Ctrl Pts',(59.747805744159,248.573100613088,21.1302481286367)) ;
#114698 = CARTESIAN_POINT('Ctrl Pts',(59.7450094072366,248.506251316868,21.1139165837474)) ;
#114699 = CARTESIAN_POINT('Ctrl Pts',(59.7422172507985,248.439501959404,21.0976094542878)) ;
#114700 = CARTESIAN_POINT('Ctrl Pts',(59.7394250943605,248.371792992903,21.0847852965818)) ;
#114701 = CARTESIAN_POINT('Ctrl Pts',(59.7366329379224,248.303520346263,21.0755482784363)) ;
#114702 = CARTESIAN_POINT('Ctrl Pts',(59.7338440362348,248.235327283426,21.0663220276634)) ;
#114703 = CARTESIAN_POINT('Ctrl Pts',(59.7310551345472,248.166572329588,21.0606746771768)) ;
#114704 = CARTESIAN_POINT('Ctrl Pts',(59.7282662328596,248.09766200975,21.0586594340684)) ;
#114705 = CARTESIAN_POINT('Ctrl Pts',(59.7254790618583,248.028794453035,21.0566454415431)) ;
#114706 = CARTESIAN_POINT('Ctrl Pts',(59.7226918908569,247.959772211123,21.05825909933)) ;
#114707 = CARTESIAN_POINT('Ctrl Pts',(59.7199047198556,247.891005792548,21.0635016832096)) ;
#114708 = CARTESIAN_POINT('Ctrl Pts',(59.7171183269923,247.822258572568,21.0687428034351)) ;
#114709 = CARTESIAN_POINT('Ctrl Pts',(59.714331934129,247.753767523312,21.0776108010505)) ;
#114710 = CARTESIAN_POINT('Ctrl Pts',(59.7115455412657,247.685940203597,21.0900549262046)) ;
#114711 = CARTESIAN_POINT('Ctrl Pts',(59.7087589751471,247.618108666442,21.102499825123)) ;
#114712 = CARTESIAN_POINT('Ctrl Pts',(59.7059724090285,247.550941423062,21.1185212019422)) ;
#114713 = CARTESIAN_POINT('Ctrl Pts',(59.7031858429099,247.484836200829,21.1380171339526)) ;
#114714 = CARTESIAN_POINT('Ctrl Pts',(59.7003963262066,247.41866098239,21.1575337094343)) ;
#114715 = CARTESIAN_POINT('Ctrl Pts',(59.6976068095033,247.353550500928,21.1805320431269)) ;
#114716 = CARTESIAN_POINT('Ctrl Pts',(59.6948172928,247.289886695475,21.206860509797)) ;
#114717 = CARTESIAN_POINT('Ctrl Pts',(59.6920261058002,247.226184769644,21.2332047413293)) ;
#114718 = CARTESIAN_POINT('Ctrl Pts',(59.6892349188004,247.163931686943,21.2628828631704)) ;
#114719 = CARTESIAN_POINT('Ctrl Pts',(59.6864437318006,247.103486244982,21.2956965107952)) ;
#114720 = CARTESIAN_POINT('Ctrl Pts',(59.6836477794956,247.042937606431,21.3285661801224)) ;
#114721 = CARTESIAN_POINT('Ctrl Pts',(59.6808518271905,246.984203186022,21.3645818026171)) ;
#114722 = CARTESIAN_POINT('Ctrl Pts',(59.6780558748854,246.927613437489,21.4035012836564)) ;
#114723 = CARTESIAN_POINT('Ctrl Pts',(59.6767952405964,246.902098346519,21.4210492340356)) ;
#114724 = CARTESIAN_POINT('Ctrl Pts',(59.6755346063073,246.877018804996,21.4391869641399)) ;
#114725 = CARTESIAN_POINT('Ctrl Pts',(59.6742739720182,246.852402782949,21.4578897095906)) ;
#114726 = CARTESIAN_POINT('Ctrl Pts',(59.6714776355049,246.797799571012,21.4993761029525)) ;
#114727 = CARTESIAN_POINT('Ctrl Pts',(59.6686812989916,246.745265268268,21.5438078353552)) ;
#114728 = CARTESIAN_POINT('Ctrl Pts',(59.6658849624783,246.695134733625,21.5909509763994)) ;
#114729 = CARTESIAN_POINT('Ctrl Pts',(59.6630928064587,246.645079143604,21.6380236389441)) ;
#114730 = CARTESIAN_POINT('Ctrl Pts',(59.6603006504391,246.597420544006,21.6877993313116)) ;
#114731 = CARTESIAN_POINT('Ctrl Pts',(59.6575084944194,246.552462081674,21.740002894411)) ;
#114732 = CARTESIAN_POINT('Ctrl Pts',(59.654719593162,246.507556026551,21.7921456048284)) ;
#114733 = CARTESIAN_POINT('Ctrl Pts',(59.6519306919045,246.465344176247,21.8467101948815)) ;
#114734 = CARTESIAN_POINT('Ctrl Pts',(59.6491417906471,246.426092728863,21.9033848440245)) ;
#114735 = CARTESIAN_POINT('Ctrl Pts',(59.6463546200829,246.386865639535,21.9600243228888)) ;
#114736 = CARTESIAN_POINT('Ctrl Pts',(59.6435674495187,246.350595587487,22.0187708605839)) ;
#114737 = CARTESIAN_POINT('Ctrl Pts',(59.6407802789545,246.317507403936,22.0792809899092)) ;
#114738 = CARTESIAN_POINT('Ctrl Pts',(59.6379938865347,246.284428458207,22.1397742255368)) ;
#114739 = CARTESIAN_POINT('Ctrl Pts',(59.6352074941149,246.254529852721,22.202029644829)) ;
#114740 = CARTESIAN_POINT('Ctrl Pts',(59.6324211016952,246.227991193536,22.2656778952236)) ;
#114741 = CARTESIAN_POINT('Ctrl Pts',(59.6296345360257,246.201450884255,22.3293301030789)) ;
#114742 = CARTESIAN_POINT('Ctrl Pts',(59.6268479703562,246.178271122553,22.3943748599644)) ;
#114743 = CARTESIAN_POINT('Ctrl Pts',(59.6240614046867,246.158583253151,22.4604231623084)) ;
#114744 = CARTESIAN_POINT('Ctrl Pts',(59.6212718884381,246.138874537077,22.5265414004688)) ;
#114745 = CARTESIAN_POINT('Ctrl Pts',(59.6184823721895,246.122665232523,22.5936648334317)) ;
#114746 = CARTESIAN_POINT('Ctrl Pts',(59.6156928559408,246.110036408564,22.6613906022208)) ;
#114747 = CARTESIAN_POINT('Ctrl Pts',(59.6129016693994,246.097400022781,22.7291569235108)) ;
#114748 = CARTESIAN_POINT('Ctrl Pts',(59.6101104828581,246.088348448924,22.7975258118115)) ;
#114749 = CARTESIAN_POINT('Ctrl Pts',(59.6073192963167,246.082910956697,22.8660883326423)) ;
#114750 = CARTESIAN_POINT('Ctrl Pts',(59.6045233444711,246.077464181212,22.9347679080891)) ;
#114751 = CARTESIAN_POINT('Ctrl Pts',(59.6017273926255,246.075643814714,23.0036412854946)) ;
#114752 = CARTESIAN_POINT('Ctrl Pts',(59.5989314407799,246.077427014612,23.0722994567796)) ;
#114753 = CARTESIAN_POINT('Ctrl Pts',(59.5976708025309,246.078231023451,23.1032560403021)) ;
#114754 = CARTESIAN_POINT('Ctrl Pts',(59.5964101642818,246.079766908328,23.1341689464842)) ;
#114755 = CARTESIAN_POINT('Ctrl Pts',(59.5951495260327,246.082029153207,23.1650012267496)) ;
#114756 = CARTESIAN_POINT('Ctrl Pts',(59.592353189247,246.087047245096,23.2333931223285)) ;
#114757 = CARTESIAN_POINT('Ctrl Pts',(59.5895568524614,246.09566238462,23.3016559393828)) ;
#114758 = CARTESIAN_POINT('Ctrl Pts',(59.5867605156757,246.107860974989,23.3693814266318)) ;
#114759 = CARTESIAN_POINT('Ctrl Pts',(59.5839683593791,246.120041328615,23.4370056651086)) ;
#114760 = CARTESIAN_POINT('Ctrl Pts',(59.5811762030826,246.135794414048,23.5040936888987)) ;
#114761 = CARTESIAN_POINT('Ctrl Pts',(59.5783840467861,246.155054783387,23.5702413604452)) ;
#114762 = CARTESIAN_POINT('Ctrl Pts',(59.5755951452465,246.174292701325,23.636311925064)) ;
#114763 = CARTESIAN_POINT('Ctrl Pts',(59.572806243707,246.197029646677,23.7014438454389)) ;
#114764 = CARTESIAN_POINT('Ctrl Pts',(59.5700173421674,246.223149295097,23.7652439775936)) ;
#114765 = CARTESIAN_POINT('Ctrl Pts',(59.567230171318,246.249252734618,23.8290045177218)) ;
#114766 = CARTESIAN_POINT('Ctrl Pts',(59.5644430004686,246.278734527295,23.8914344559251)) ;
#114767 = CARTESIAN_POINT('Ctrl Pts',(59.5616558296193,246.311429268392,23.9521580793799)) ;
#114768 = CARTESIAN_POINT('Ctrl Pts',(59.5588694369117,246.344114881543,24.0128647495911)) ;
#114769 = CARTESIAN_POINT('Ctrl Pts',(59.556083044204,246.380011429681,24.0718656188513)) ;
#114770 = CARTESIAN_POINT('Ctrl Pts',(59.5532966514964,246.418907154757,24.1288087805866)) ;
#114771 = CARTESIAN_POINT('Ctrl Pts',(59.5505100855369,246.457805298284,24.1857554829242)) ;
#114772 = CARTESIAN_POINT('Ctrl Pts',(59.5477235195775,246.499702710016,24.2406438198802)) ;
#114773 = CARTESIAN_POINT('Ctrl Pts',(59.544936953618,246.544344850386,24.2931516348476)) ;
#114774 = CARTESIAN_POINT('Ctrl Pts',(59.542147437078,246.589034260488,24.3457150481881)) ;
#114775 = CARTESIAN_POINT('Ctrl Pts',(59.539357920538,246.636473880616,24.3958925345933)) ;
#114776 = CARTESIAN_POINT('Ctrl Pts',(59.5365684039981,246.686370150645,24.4433965352695)) ;
#114777 = CARTESIAN_POINT('Ctrl Pts',(59.5337772171642,246.736296297334,24.4909289801731)) ;
#114778 = CARTESIAN_POINT('Ctrl Pts',(59.5309860303303,246.788681648685,24.5357844340528)) ;
#114779 = CARTESIAN_POINT('Ctrl Pts',(59.5281948434965,246.843199315981,24.5777154540923)) ;
#114780 = CARTESIAN_POINT('Ctrl Pts',(59.5253988913597,246.897810059526,24.6197180616052)) ;
#114781 = CARTESIAN_POINT('Ctrl Pts',(59.5226029392228,246.954559980504,24.6587859926039)) ;
#114782 = CARTESIAN_POINT('Ctrl Pts',(59.519806987086,247.01309372292,24.6947154541392)) ;
#114783 = CARTESIAN_POINT('Ctrl Pts',(59.5185463514064,247.039485349293,24.7109152883797)) ;
#114784 = CARTESIAN_POINT('Ctrl Pts',(59.5172857157268,247.066239289734,24.7264777260693)) ;
#114785 = CARTESIAN_POINT('Ctrl Pts',(59.5160250800472,247.09332156075,24.741387251772)) ;
#114786 = CARTESIAN_POINT('Ctrl Pts',(59.5132287433095,247.153395339883,24.774459498685)) ;
#114787 = CARTESIAN_POINT('Ctrl Pts',(59.5104324065719,247.215321594776,24.8044456889594)) ;
#114788 = CARTESIAN_POINT('Ctrl Pts',(59.5076360698342,247.278750643737,24.8311346906806)) ;
#114789 = CARTESIAN_POINT('Ctrl Pts',(59.504843913586,247.342084867042,24.8577837926684)) ;
#114790 = CARTESIAN_POINT('Ctrl Pts',(59.5020517573378,247.406916976534,24.8811453005803)) ;
#114791 = CARTESIAN_POINT('Ctrl Pts',(59.4992596010895,247.472872476185,24.9010537958356)) ;
#114792 = CARTESIAN_POINT('Ctrl Pts',(59.4964706995984,247.538751092915,24.9209390841816)) ;
#114793 = CARTESIAN_POINT('Ctrl Pts',(59.4936817981073,247.605750031277,24.9373792129646)) ;
#114794 = CARTESIAN_POINT('Ctrl Pts',(59.4908928966162,247.673476280123,24.9502574099)) ;
#114795 = CARTESIAN_POINT('Ctrl Pts',(59.4881057258154,247.741160500536,24.9631276150973)) ;
#114796 = CARTESIAN_POINT('Ctrl Pts',(59.4853185550146,247.809570654934,24.9724401819623)) ;
#114797 = CARTESIAN_POINT('Ctrl Pts',(59.4825313842138,247.878301593193,24.9781289877404)) ;
#114798 = CARTESIAN_POINT('Ctrl Pts',(59.4797449915547,247.947013342669,24.9838162052781)) ;
#114799 = CARTESIAN_POINT('Ctrl Pts',(59.4769585988956,248.016045209274,24.9858816298161)) ;
#114800 = CARTESIAN_POINT('Ctrl Pts',(59.4741722062365,248.084986735155,24.9843109767633)) ;
#114801 = CARTESIAN_POINT('Ctrl Pts',(59.4713856403255,248.153932547673,24.9827402260506)) ;
#114802 = CARTESIAN_POINT('Ctrl Pts',(59.4685990744145,248.22278751768,24.9775329626424)) ;
#114803 = CARTESIAN_POINT('Ctrl Pts',(59.4658125085035,248.291142809627,24.968726985409)) ;
#114804 = CARTESIAN_POINT('Ctrl Pts',(59.4630229920115,248.359570480204,24.9599116838855)) ;
#114805 = CARTESIAN_POINT('Ctrl Pts',(59.4602334755195,248.42749692913,24.9474901268919)) ;
#114806 = CARTESIAN_POINT('Ctrl Pts',(59.4574439590276,248.494521057544,24.9315516861224)) ;
#114807 = CARTESIAN_POINT('Ctrl Pts',(59.4546527722415,248.561585318363,24.9156037018053)) ;
#114808 = CARTESIAN_POINT('Ctrl Pts',(59.4518615854554,248.627745712456,24.8961347811673)) ;
#114809 = CARTESIAN_POINT('Ctrl Pts',(59.4490703986694,248.692616606571,24.873284104553)) ;
#114810 = CARTESIAN_POINT('Ctrl Pts',(59.4462744465796,248.757598252685,24.8503944157108)) ;
#114811 = CARTESIAN_POINT('Ctrl Pts',(59.4434784944897,248.821285551641,24.8241116352291)) ;
#114812 = CARTESIAN_POINT('Ctrl Pts',(59.4406825423999,248.883313948375,24.7946226027307)) ;
#114813 = CARTESIAN_POINT('Ctrl Pts',(59.4394219062872,248.911281250542,24.7813266169258)) ;
#114814 = CARTESIAN_POINT('Ctrl Pts',(59.4381612701744,248.938911662588,24.7673794386522)) ;
#114815 = CARTESIAN_POINT('Ctrl Pts',(59.4369006340617,248.966173652772,24.7528011018477)) ;
#114816 = CARTESIAN_POINT('Ctrl Pts',(59.4341042973507,249.026646062848,24.7204635081682)) ;
#114817 = CARTESIAN_POINT('Ctrl Pts',(59.4313079606397,249.085540935002,24.6848906733029)) ;
#114818 = CARTESIAN_POINT('Ctrl Pts',(59.4285116239287,249.142490654278,24.6462606792827)) ;
#114819 = CARTESIAN_POINT('Ctrl Pts',(59.4257194677079,249.1993552344,24.6076884366455)) ;
#114820 = CARTESIAN_POINT('Ctrl Pts',(59.4229273114872,249.25428003027,24.5660683793269)) ;
#114821 = CARTESIAN_POINT('Ctrl Pts',(59.4201351552664,249.30692222625,24.5216243108424)) ;
#114822 = CARTESIAN_POINT('Ctrl Pts',(59.4173462538038,249.359503058323,24.4772320498793)) ;
#114823 = CARTESIAN_POINT('Ctrl Pts',(59.4145573523411,249.40980620179,24.4300226309428)) ;
#114824 = CARTESIAN_POINT('Ctrl Pts',(59.4117684508785,249.457519532872,24.3802618965976)) ;
#114825 = CARTESIAN_POINT('Ctrl Pts',(59.4089812801067,249.505203254795,24.3305320419557)) ;
#114826 = CARTESIAN_POINT('Ctrl Pts',(59.406194109335,249.550300013629,24.2782543662633)) ;
#114827 = CARTESIAN_POINT('Ctrl Pts',(59.4034069385633,249.59253353246,24.2237324974231)) ;
#114828 = CARTESIAN_POINT('Ctrl Pts',(59.4006205459338,249.634755260235,24.169225850389)) ;
#114829 = CARTESIAN_POINT('Ctrl Pts',(59.3978341533044,249.674115034592,24.1124766419563)) ;
#114830 = CARTESIAN_POINT('Ctrl Pts',(59.3950477606749,249.710377145614,24.0538212060783)) ;
#114831 = CARTESIAN_POINT('Ctrl Pts',(59.3922611947941,249.74664151133,23.9951621231416)) ;
#114832 = CARTESIAN_POINT('Ctrl Pts',(59.3894746289132,249.779807575414,23.9345969962803)) ;
#114833 = CARTESIAN_POINT('Ctrl Pts',(59.3866880630324,249.809684178051,23.8724891891972)) ;
#114834 = CARTESIAN_POINT('Ctrl Pts',(59.3838985465712,249.839592415797,23.8103156187036)) ;
#114835 = CARTESIAN_POINT('Ctrl Pts',(59.3811090301099,249.866204027935,23.7465965512774)) ;
#114836 = CARTESIAN_POINT('Ctrl Pts',(59.3783195136487,249.889375309496,23.6817169758437)) ;
#114837 = CARTESIAN_POINT('Ctrl Pts',(59.3755283268938,249.912560465449,23.6167985521189)) ;
#114838 = CARTESIAN_POINT('Ctrl Pts',(59.3727371401388,249.93230105043,23.5507187077277)) ;
#114839 = CARTESIAN_POINT('Ctrl Pts',(59.3699459533839,249.948503548174,23.4838766154075)) ;
#114840 = CARTESIAN_POINT('Ctrl Pts',(59.3671500013255,249.964733707922,23.4169204057302)) ;
#114841 = CARTESIAN_POINT('Ctrl Pts',(59.3643540492671,249.977413634704,23.3491998330237)) ;
#114842 = CARTESIAN_POINT('Ctrl Pts',(59.3615580972086,249.986501258293,23.2811223767716)) ;
#114843 = CARTESIAN_POINT('Ctrl Pts',(59.3602974608311,249.990598677934,23.2504276738417)) ;
#114844 = CARTESIAN_POINT('Ctrl Pts',(59.3590368244536,249.993966516169,23.2196604587679)) ;
#114845 = CARTESIAN_POINT('Ctrl Pts',(59.3577761880761,249.996604381633,23.1888580873807)) ;
#114846 = CARTESIAN_POINT('Ctrl Pts',(59.3555100882696,250.001346166437,23.1334882368135)) ;
#114847 = CARTESIAN_POINT('Ctrl Pts',(59.353243988463,250.003737676047,23.0779142731246)) ;
#114848 = CARTESIAN_POINT('Ctrl Pts',(59.3509778886564,250.003764873166,23.0222802148703)) ;
#114849 = CARTESIAN_POINT('',(58.8509778886861,250.003764876387,23.0222736029538)) ;
#114850 = CARTESIAN_POINT('Ctrl Pts',(59.3509778886203,250.003764873166,23.0222802139838)) ;
#114851 = CARTESIAN_POINT('Ctrl Pts',(59.3482144163914,250.003798039584,22.9544353756742)) ;
#114852 = CARTESIAN_POINT('Ctrl Pts',(59.3454509441625,250.000310596167,22.8864497538944)) ;
#114853 = CARTESIAN_POINT('Ctrl Pts',(59.3426874719336,249.993285064595,22.8187239509328)) ;
#114854 = CARTESIAN_POINT('Ctrl Pts',(59.3399282395187,249.986270311835,22.751102055225)) ;
#114855 = CARTESIAN_POINT('Ctrl Pts',(59.3371690071039,249.975728298068,22.6837396835978)) ;
#114856 = CARTESIAN_POINT('Ctrl Pts',(59.334409774689,249.961693556368,22.6170370678999)) ;
#114857 = CARTESIAN_POINT('Ctrl Pts',(59.3316528777829,249.947670694155,22.5503909115782)) ;
#114858 = CARTESIAN_POINT('Ctrl Pts',(59.3288959808767,249.930161066131,22.4844038946956)) ;
#114859 = CARTESIAN_POINT('Ctrl Pts',(59.3261390839706,249.909250777936,22.4194691868974)) ;
#114860 = CARTESIAN_POINT('Ctrl Pts',(59.3233835269175,249.888350652149,22.354566037394)) ;
#114861 = CARTESIAN_POINT('Ctrl Pts',(59.3206279698644,249.864053297393,22.2907146611191)) ;
#114862 = CARTESIAN_POINT('Ctrl Pts',(59.3178724128113,249.836494990548,22.2282942038426)) ;
#114863 = CARTESIAN_POINT('Ctrl Pts',(59.315117201858,249.808940145045,22.1658815866184)) ;
#114864 = CARTESIAN_POINT('Ctrl Pts',(59.3123619909048,249.77812536494,22.1048999913118)) ;
#114865 = CARTESIAN_POINT('Ctrl Pts',(59.3096067799515,249.744234736134,22.0457078407358)) ;
#114866 = CARTESIAN_POINT('Ctrl Pts',(59.306849047208,249.710313087904,21.9864615127514)) ;
#114867 = CARTESIAN_POINT('Ctrl Pts',(59.3040913144645,249.673310219145,21.9290083380907)) ;
#114868 = CARTESIAN_POINT('Ctrl Pts',(59.301333581721,249.633455230042,21.8736803807023)) ;
#114869 = CARTESIAN_POINT('Ctrl Pts',(59.2985745664988,249.593581706447,21.8183266931472)) ;
#114870 = CARTESIAN_POINT('Ctrl Pts',(59.2958155512767,249.550853737858,21.7651005827768)) ;
#114871 = CARTESIAN_POINT('Ctrl Pts',(59.2930565360545,249.5055408328,21.7143011012815)) ;
#114872 = CARTESIAN_POINT('Ctrl Pts',(59.2902926206499,249.460147449205,21.6634113967496)) ;
#114873 = CARTESIAN_POINT('Ctrl Pts',(59.2875287052452,249.412160316883,21.6149572842967)) ;
#114874 = CARTESIAN_POINT('Ctrl Pts',(59.2847647898405,249.361885300937,21.5692004053125)) ;
#114875 = CARTESIAN_POINT('Ctrl Pts',(59.2827271072572,249.324820300975,21.5354663788601)) ;
#114876 = CARTESIAN_POINT('Ctrl Pts',(59.2806894246739,249.286512526135,21.5031975824389)) ;
#114877 = CARTESIAN_POINT('Ctrl Pts',(59.2786517420906,249.24709473802,21.472483846834)) ;
#114878 = CARTESIAN_POINT('Ctrl Pts',(59.2758554053502,249.193001225109,21.4303350116775)) ;
#114879 = CARTESIAN_POINT('Ctrl Pts',(59.2730590686099,249.136590890501,21.390940763458)) ;
#114880 = CARTESIAN_POINT('Ctrl Pts',(59.2702627318695,249.078175663034,21.3545648338026)) ;
#114881 = CARTESIAN_POINT('Ctrl Pts',(59.2674705756192,249.019847765634,21.318243285728)) ;
#114882 = CARTESIAN_POINT('Ctrl Pts',(59.264678419369,248.959521337593,21.2849313577405)) ;
#114883 = CARTESIAN_POINT('Ctrl Pts',(59.2618862631187,248.897540033366,21.2548515632037)) ;
#114884 = CARTESIAN_POINT('Ctrl Pts',(59.2590973616264,248.835630979446,21.224806832053)) ;
#114885 = CARTESIAN_POINT('Ctrl Pts',(59.2563084601342,248.772071320159,21.1979869647537)) ;
#114886 = CARTESIAN_POINT('Ctrl Pts',(59.2535195586419,248.707230678921,21.1745693649704)) ;
#114887 = CARTESIAN_POINT('Ctrl Pts',(59.2507323878405,248.642430275427,21.1511662972978)) ;
#114888 = CARTESIAN_POINT('Ctrl Pts',(59.2479452170391,248.576350927592,21.131161475055)) ;
#114889 = CARTESIAN_POINT('Ctrl Pts',(59.2451580462377,248.509382248268,21.1146842066666)) ;
#114890 = CARTESIAN_POINT('Ctrl Pts',(59.2423716535786,248.442432265739,21.09821153852)) ;
#114891 = CARTESIAN_POINT('Ctrl Pts',(59.2395852609194,248.374593921047,21.08526458621)) ;
#114892 = CARTESIAN_POINT('Ctrl Pts',(59.2367988682603,248.306270258855,21.0759223098388)) ;
#114893 = CARTESIAN_POINT('Ctrl Pts',(59.2340123023499,248.237942348458,21.0665794525868)) ;
#114894 = CARTESIAN_POINT('Ctrl Pts',(59.2312257364394,248.169129547296,21.0608417801966)) ;
#114895 = CARTESIAN_POINT('Ctrl Pts',(59.2284391705289,248.100241527624,21.0587365672424)) ;
#114896 = CARTESIAN_POINT('Ctrl Pts',(59.2256496540383,248.031280565261,21.0566291251648)) ;
#114897 = CARTESIAN_POINT('Ctrl Pts',(59.2228601375477,247.962244716962,21.0581618333256)) ;
#114898 = CARTESIAN_POINT('Ctrl Pts',(59.2200706210571,247.893544164318,21.0633098188821)) ;
#114899 = CARTESIAN_POINT('Ctrl Pts',(59.2172794342729,247.82480247548,21.0684608869253)) ;
#114900 = CARTESIAN_POINT('Ctrl Pts',(59.2144882474887,247.756396968761,21.0772314783121)) ;
#114901 = CARTESIAN_POINT('Ctrl Pts',(59.2116970607045,247.688730424504,21.0895450935759)) ;
#114902 = CARTESIAN_POINT('Ctrl Pts',(59.2089011086172,247.620948355341,21.1018797314773)) ;
#114903 = CARTESIAN_POINT('Ctrl Pts',(59.20610515653,247.553908243824,21.1177693524051)) ;
#114904 = CARTESIAN_POINT('Ctrl Pts',(59.2033092044427,247.487999587359,21.1370870658184)) ;
#114905 = CARTESIAN_POINT('Ctrl Pts',(59.2020485683302,247.458282757501,21.1457970173414)) ;
#114906 = CARTESIAN_POINT('Ctrl Pts',(59.2007879322176,247.428795693232,21.1552032118979)) ;
#114907 = CARTESIAN_POINT('Ctrl Pts',(59.1995272961051,247.399572695686,21.1652908494305)) ;
#114908 = CARTESIAN_POINT('Ctrl Pts',(59.196730959318,247.334750387128,21.1876671970903)) ;
#114909 = CARTESIAN_POINT('Ctrl Pts',(59.1939346225309,247.270974611077,21.2134874063389)) ;
#114910 = CARTESIAN_POINT('Ctrl Pts',(59.1911382857438,247.208636502649,21.2426337176701)) ;
#114911 = CARTESIAN_POINT('Ctrl Pts',(59.1883461294462,247.146391588935,21.2717364556203)) ;
#114912 = CARTESIAN_POINT('Ctrl Pts',(59.1855539731486,247.085580518145,21.3041552202885)) ;
#114913 = CARTESIAN_POINT('Ctrl Pts',(59.182761816851,247.026577161891,21.3397231865845)) ;
#114914 = CARTESIAN_POINT('Ctrl Pts',(59.1799729153109,246.967642584598,21.375249692056)) ;
#114915 = CARTESIAN_POINT('Ctrl Pts',(59.1771840137707,246.910511955099,21.4139178560389)) ;
#114916 = CARTESIAN_POINT('Ctrl Pts',(59.1743951122305,246.855535481128,21.4555144929768)) ;
#114917 = CARTESIAN_POINT('Ctrl Pts',(59.1716079413808,246.800593123551,21.49708531656)) ;
#114918 = CARTESIAN_POINT('Ctrl Pts',(59.1688207705312,246.747802660129,21.5415807124295)) ;
#114919 = CARTESIAN_POINT('Ctrl Pts',(59.1660335996815,246.697484872359,21.5887445203145)) ;
#114920 = CARTESIAN_POINT('Ctrl Pts',(59.1632472069738,246.647181132664,21.6358951606747)) ;
#114921 = CARTESIAN_POINT('Ctrl Pts',(59.1604608142662,246.599349056025,21.6857123985113)) ;
#114922 = CARTESIAN_POINT('Ctrl Pts',(59.1576744215586,246.554274534302,21.7379013685107)) ;
#114923 = CARTESIAN_POINT('Ctrl Pts',(59.1548878555993,246.509197209947,21.7900935835016)) ;
#114924 = CARTESIAN_POINT('Ctrl Pts',(59.1521012896402,246.466878099785,21.8446574502955)) ;
#114925 = CARTESIAN_POINT('Ctrl Pts',(59.1493147236809,246.42756337608,21.9012643741764)) ;
#114926 = CARTESIAN_POINT('Ctrl Pts',(59.1465252071417,246.388207023631,21.9579312367999)) ;
#114927 = CARTESIAN_POINT('Ctrl Pts',(59.1437356906024,246.351861686745,22.0166450698203)) ;
#114928 = CARTESIAN_POINT('Ctrl Pts',(59.1409461740632,246.318730095887,22.0770484267869)) ;
#114929 = CARTESIAN_POINT('Ctrl Pts',(59.1381549872303,246.28557866665,22.1374879517928)) ;
#114930 = CARTESIAN_POINT('Ctrl Pts',(59.1353638003974,246.255645026362,22.1996185719482)) ;
#114931 = CARTESIAN_POINT('Ctrl Pts',(59.1325726135645,246.229084588378,22.2630609050312)) ;
#114932 = CARTESIAN_POINT('Ctrl Pts',(59.129776661429,246.202478804622,22.3266115511476)) ;
#114933 = CARTESIAN_POINT('Ctrl Pts',(59.1269807092936,246.179257882127,22.3914779178238)) ;
#114934 = CARTESIAN_POINT('Ctrl Pts',(59.1241847571581,246.15952774699,22.4572642916397)) ;
#114935 = CARTESIAN_POINT('Ctrl Pts',(59.1229241214786,246.150631846378,22.4869259761183)) ;
#114936 = CARTESIAN_POINT('Ctrl Pts',(59.121663485799,246.142444904077,22.5167745401311)) ;
#114937 = CARTESIAN_POINT('Ctrl Pts',(59.1204028501195,246.134973208986,22.5467731590085)) ;
#114938 = CARTESIAN_POINT('Ctrl Pts',(59.1176065136226,246.118399527931,22.6133159629168)) ;
#114939 = CARTESIAN_POINT('Ctrl Pts',(59.1148101771257,246.105283563965,22.6808585669027)) ;
#114940 = CARTESIAN_POINT('Ctrl Pts',(59.1120138406289,246.095739791186,22.7490088617933)) ;
#114941 = CARTESIAN_POINT('Ctrl Pts',(59.1092216846219,246.086210286234,22.8170572728011)) ;
#114942 = CARTESIAN_POINT('Ctrl Pts',(59.1064295286149,246.080242440688,22.8857110893508)) ;
#114943 = CARTESIAN_POINT('Ctrl Pts',(59.1036373726079,246.077900182911,22.9545659308058)) ;
#114944 = CARTESIAN_POINT('Ctrl Pts',(59.1008484713576,246.075560655454,23.0233405096432)) ;
#114945 = CARTESIAN_POINT('Ctrl Pts',(59.0980595701072,246.076838338569,23.0923151597208)) ;
#114946 = CARTESIAN_POINT('Ctrl Pts',(59.0952706688569,246.081745394066,23.1610800694073)) ;
#114947 = CARTESIAN_POINT('Ctrl Pts',(59.0924834982963,246.086649404423,23.229802306113)) ;
#114948 = CARTESIAN_POINT('Ctrl Pts',(59.0896963277358,246.095178284277,23.2983145721291)) ;
#114949 = CARTESIAN_POINT('Ctrl Pts',(59.0869091571752,246.107292126462,23.3662083014096)) ;
#114950 = CARTESIAN_POINT('Ctrl Pts',(59.0841227647556,246.119402586622,23.4340830756645)) ;
#114951 = CARTESIAN_POINT('Ctrl Pts',(59.081336372336,246.135095935891,23.5013391730481)) ;
#114952 = CARTESIAN_POINT('Ctrl Pts',(59.0785499799164,246.15428079973,23.5675761808417)) ;
#114953 = CARTESIAN_POINT('Ctrl Pts',(59.0757634142437,246.17346685645,23.6338173071393)) ;
#114954 = CARTESIAN_POINT('Ctrl Pts',(59.0729768485709,246.196144719733,23.6990387473166)) ;
#114955 = CARTESIAN_POINT('Ctrl Pts',(59.0701902828982,246.222173086422,23.7628550034729)) ;
#114956 = CARTESIAN_POINT('Ctrl Pts',(59.0674007666411,246.24822901352,23.8267388321427)) ;
#114957 = CARTESIAN_POINT('Ctrl Pts',(59.064611250384,246.2776423383,23.8892140521497)) ;
#114958 = CARTESIAN_POINT('Ctrl Pts',(59.0618217341269,246.310223889416,23.9499158597772)) ;
#114959 = CARTESIAN_POINT('Ctrl Pts',(59.0590305475741,246.342824949586,24.0106540141971)) ;
#114960 = CARTESIAN_POINT('Ctrl Pts',(59.0562393610214,246.378597757097,24.0696162231625)) ;
#114961 = CARTESIAN_POINT('Ctrl Pts',(59.0534481744686,246.417308958266,24.1264653959102)) ;
#114962 = CARTESIAN_POINT('Ctrl Pts',(59.0506522226072,246.456086249901,24.1834116255363)) ;
#114963 = CARTESIAN_POINT('Ctrl Pts',(59.0478562707458,246.497811650241,24.2382372287799)) ;
#114964 = CARTESIAN_POINT('Ctrl Pts',(59.0450603188843,246.54221113912,24.2906377022076)) ;
#114965 = CARTESIAN_POINT('Ctrl Pts',(59.0437996806343,246.562229972326,24.3142640178237)) ;
#114966 = CARTESIAN_POINT('Ctrl Pts',(59.0425390423842,246.582791925877,24.3373978189575)) ;
#114967 = CARTESIAN_POINT('Ctrl Pts',(59.0412784041341,246.603869554451,24.3600137604256)) ;
#114968 = CARTESIAN_POINT('Ctrl Pts',(59.0384820671789,246.650623769395,24.4101802478371)) ;
#114969 = CARTESIAN_POINT('Ctrl Pts',(59.0356857302238,246.700100944889,24.4579928233431)) ;
#114970 = CARTESIAN_POINT('Ctrl Pts',(59.0328893932686,246.752034741746,24.5031417815244)) ;
#114971 = CARTESIAN_POINT('Ctrl Pts',(59.0300972368053,246.80389089817,24.548223242529)) ;
#114972 = CARTESIAN_POINT('Ctrl Pts',(59.0273050803419,246.858196019243,24.5906486701497)) ;
#114973 = CARTESIAN_POINT('Ctrl Pts',(59.0245129238785,246.914645925946,24.630144046603)) ;
#114974 = CARTESIAN_POINT('Ctrl Pts',(59.0217240221768,246.971030030109,24.6695933840767)) ;
#114975 = CARTESIAN_POINT('Ctrl Pts',(59.018935120475,247.029553554085,24.7061191738536)) ;
#114976 = CARTESIAN_POINT('Ctrl Pts',(59.0161462187732,247.089879548498,24.739487837926)) ;
#114977 = CARTESIAN_POINT('Ctrl Pts',(59.0133590477647,247.150168106745,24.7728357945925)) ;
#114978 = CARTESIAN_POINT('Ctrl Pts',(59.0105718767561,247.212256487896,24.8030302751658)) ;
#114979 = CARTESIAN_POINT('Ctrl Pts',(59.0077847057475,247.275780404892,24.8298820342521)) ;
#114980 = CARTESIAN_POINT('Ctrl Pts',(59.0049983128838,247.339286586767,24.8567262966472)) ;
#114981 = CARTESIAN_POINT('Ctrl Pts',(59.0022119200202,247.404227056915,24.8802294993308)) ;
#114982 = CARTESIAN_POINT('Ctrl Pts',(58.9994255271565,247.470216309838,24.9002499904485)) ;
#114983 = CARTESIAN_POINT('Ctrl Pts',(58.9966389610445,247.536209665749,24.9202717263723)) ;
#114984 = CARTESIAN_POINT('Ctrl Pts',(58.9938523949324,247.603251463472,24.936810180781)) ;
#114985 = CARTESIAN_POINT('Ctrl Pts',(58.9910658288203,247.670941486527,24.949773690877)) ;
#114986 = CARTESIAN_POINT('Ctrl Pts',(58.9882763121339,247.738703183619,24.9627509274732)) ;
#114987 = CARTESIAN_POINT('Ctrl Pts',(58.9854867954475,247.80711399284,24.972145573031)) ;
#114988 = CARTESIAN_POINT('Ctrl Pts',(58.982697278761,247.875764955148,24.9779173766203)) ;
#114989 = CARTESIAN_POINT('Ctrl Pts',(58.979906091784,247.94445702388,24.9836926362167)) ;
#114990 = CARTESIAN_POINT('Ctrl Pts',(58.977114904807,248.013389041257,24.9858407211746)) ;
#114991 = CARTESIAN_POINT('Ctrl Pts',(58.97432371783,248.082151199172,24.9843735281036)) ;
#114992 = CARTESIAN_POINT('Ctrl Pts',(58.9715277655566,248.151030752329,24.9829038301449)) ;
#114993 = CARTESIAN_POINT('Ctrl Pts',(58.9687318132831,248.219739378087,24.9778065719954)) ;
#114994 = CARTESIAN_POINT('Ctrl Pts',(58.9659358610097,248.287872422303,24.9691455071197)) ;
#114995 = CARTESIAN_POINT('Ctrl Pts',(58.9646752267226,248.318592135381,24.9652404206671)) ;
#114996 = CARTESIAN_POINT('Ctrl Pts',(58.9634145924355,248.349194980317,24.9606115349833)) ;
#114997 = CARTESIAN_POINT('Ctrl Pts',(58.9621539581485,248.379644748521,24.9552680443661)) ;
#114998 = CARTESIAN_POINT('Ctrl Pts',(58.9593576209136,248.447188382306,24.9434151208572)) ;
#114999 = CARTESIAN_POINT('Ctrl Pts',(58.9565612836786,248.514242781497,24.9279962372586)) ;
#115000 = CARTESIAN_POINT('Ctrl Pts',(58.9537649464437,248.580403117524,24.9090658720766)) ;
#115001 = CARTESIAN_POINT('Ctrl Pts',(58.950972789694,248.646464544771,24.8901638075269)) ;
#115002 = CARTESIAN_POINT('Ctrl Pts',(58.9481806329443,248.711634093535,24.8677608145103)) ;
#115003 = CARTESIAN_POINT('Ctrl Pts',(58.9453884761946,248.77551622923,24.8419625485013)) ;
#115004 = CARTESIAN_POINT('Ctrl Pts',(58.9425995741983,248.839323898978,24.8161943549422)) ;
#115005 = CARTESIAN_POINT('Ctrl Pts',(58.939810672202,248.901846683219,24.7870389319116)) ;
#115006 = CARTESIAN_POINT('Ctrl Pts',(58.9370217702057,248.962705088742,24.7546514520135)) ;
#115007 = CARTESIAN_POINT('Ctrl Pts',(58.9342345988977,249.023525727814,24.7222840705744)) ;
#115008 = CARTESIAN_POINT('Ctrl Pts',(58.9314474275897,249.082683604803,24.6866888412435)) ;
#115009 = CARTESIAN_POINT('Ctrl Pts',(58.9286602562817,249.139821492819,24.6480680210235)) ;
#115010 = CARTESIAN_POINT('Ctrl Pts',(58.9258738631143,249.196943428708,24.6094579832144)) ;
#115011 = CARTESIAN_POINT('Ctrl Pts',(58.9230874699468,249.252046088789,24.5678243062547)) ;
#115012 = CARTESIAN_POINT('Ctrl Pts',(58.9203010767794,249.304800581892,24.5234129787613)) ;
#115013 = CARTESIAN_POINT('Ctrl Pts',(58.9175145103596,249.357558355164,24.4789988898608)) ;
#115014 = CARTESIAN_POINT('Ctrl Pts',(58.9147279439398,249.407967297763,24.4318071256052)) ;
#115015 = CARTESIAN_POINT('Ctrl Pts',(58.91194137752,249.455732409706,24.3821232562536)) ;
#115016 = CARTESIAN_POINT('Ctrl Pts',(58.9091518605222,249.503548098117,24.3323867787421)) ;
#115017 = CARTESIAN_POINT('Ctrl Pts',(58.9063623435245,249.54871402837,24.2801532845457)) ;
#115018 = CARTESIAN_POINT('Ctrl Pts',(58.9035728265267,249.590973537813,24.2257436973031)) ;
#115019 = CARTESIAN_POINT('Ctrl Pts',(58.9007816392358,249.633258351196,24.171301530958)) ;
#115020 = CARTESIAN_POINT('Ctrl Pts',(58.8979904519449,249.672632999894,24.1146810812941)) ;
#115021 = CARTESIAN_POINT('Ctrl Pts',(58.895199264654,249.708884077981,24.05623240857)) ;
#115022 = CARTESIAN_POINT('Ctrl Pts',(58.8924033120661,249.745197046273,23.9976839484601)) ;
#115023 = CARTESIAN_POINT('Ctrl Pts',(58.8896073594782,249.778375564698,23.9373014658192)) ;
#115024 = CARTESIAN_POINT('Ctrl Pts',(58.8868114068903,249.808252512498,23.8754589662552)) ;
#115025 = CARTESIAN_POINT('Ctrl Pts',(58.8855507753145,249.821723350289,23.8475755865395)) ;
#115026 = CARTESIAN_POINT('Ctrl Pts',(58.8842901437388,249.834523668133,23.8193956569121)) ;
#115027 = CARTESIAN_POINT('Ctrl Pts',(58.883029512163,249.846641437717,23.7909545454152)) ;
#115028 = CARTESIAN_POINT('Ctrl Pts',(58.8799366091877,249.876371841364,23.7211755552172)) ;
#115029 = CARTESIAN_POINT('Ctrl Pts',(58.8768437062124,249.902089895002,23.6495903556867)) ;
#115030 = CARTESIAN_POINT('Ctrl Pts',(58.8737508032372,249.923596879455,23.5766523954176)) ;
#115031 = CARTESIAN_POINT('Ctrl Pts',(58.8706676326043,249.945036188545,23.5039439467784)) ;
#115032 = CARTESIAN_POINT('Ctrl Pts',(58.8675844619714,249.962290726759,23.4298915073856)) ;
#115033 = CARTESIAN_POINT('Ctrl Pts',(58.8645012913385,249.975210146838,23.3549667819474)) ;
#115034 = CARTESIAN_POINT('Ctrl Pts',(58.8614340620078,249.988062768026,23.2804294491742)) ;
#115035 = CARTESIAN_POINT('Ctrl Pts',(58.8583668326771,249.996624855943,23.2050291159775)) ;
#115036 = CARTESIAN_POINT('Ctrl Pts',(58.8552996033464,250.000796615895,23.1292483552738)) ;
#115037 = CARTESIAN_POINT('Ctrl Pts',(58.8538590317929,250.002755947287,23.0936567524309)) ;
#115038 = CARTESIAN_POINT('Ctrl Pts',(58.8524184602395,250.003747540578,23.0579814668026)) ;
#115039 = CARTESIAN_POINT('Ctrl Pts',(58.8509778886861,250.003764876387,23.0222736029538)) ;
#115040 = CARTESIAN_POINT('',(58.3509778886279,250.003764344364,23.019588882796)) ;
#115041 = CARTESIAN_POINT('Ctrl Pts',(58.8509778886564,250.003764876387,23.0222736022181)) ;
#115042 = CARTESIAN_POINT('Ctrl Pts',(58.8481505255564,250.003798900791,22.9521909351076)) ;
#115043 = CARTESIAN_POINT('Ctrl Pts',(58.8453231624564,250.000076419562,22.8821143861072)) ;
#115044 = CARTESIAN_POINT('Ctrl Pts',(58.8424957993564,249.992625746799,22.812465884105)) ;
#115045 = CARTESIAN_POINT('Ctrl Pts',(58.8396672877594,249.985172047514,22.7427890903375)) ;
#115046 = CARTESIAN_POINT('Ctrl Pts',(58.8368387761624,249.973987198681,22.6735411566306)) ;
#115047 = CARTESIAN_POINT('Ctrl Pts',(58.8340102645655,249.9591511568,22.6051369934624)) ;
#115048 = CARTESIAN_POINT('Ctrl Pts',(58.8311775185464,249.944292904629,22.5366304258706)) ;
#115049 = CARTESIAN_POINT('Ctrl Pts',(58.8283447725273,249.925772649025,22.4689706108314)) ;
#115050 = CARTESIAN_POINT('Ctrl Pts',(58.8255120265083,249.903720959079,22.4025598565522)) ;
#115051 = CARTESIAN_POINT('Ctrl Pts',(58.8226769540086,249.881651158498,22.3360945603783)) ;
#115052 = CARTESIAN_POINT('Ctrl Pts',(58.8198418815089,249.856044320734,22.2708808052718)) ;
#115053 = CARTESIAN_POINT('Ctrl Pts',(58.8170068090091,249.827079144851,22.2073007817881)) ;
#115054 = CARTESIAN_POINT('Ctrl Pts',(58.8141660072348,249.798055434505,22.1435922722015)) ;
#115055 = CARTESIAN_POINT('Ctrl Pts',(58.8113252054604,249.765660051054,22.081524504325)) ;
#115056 = CARTESIAN_POINT('Ctrl Pts',(58.8084844036861,249.730117371809,22.021454564679)) ;
#115057 = CARTESIAN_POINT('Ctrl Pts',(58.8069579578499,249.711019251261,21.989177230132)) ;
#115058 = CARTESIAN_POINT('Ctrl Pts',(58.8054315120137,249.69101317592,21.9574762078088)) ;
#115059 = CARTESIAN_POINT('Ctrl Pts',(58.8039050661775,249.670138832976,21.9264030453423)) ;
#115060 = CARTESIAN_POINT('Ctrl Pts',(58.801108726491,249.63189852846,21.8694792323062)) ;
#115061 = CARTESIAN_POINT('Ctrl Pts',(58.7983123868046,249.590597531178,21.8144495208064)) ;
#115062 = CARTESIAN_POINT('Ctrl Pts',(58.7955160471181,249.546449899716,21.7616618094488)) ;
#115063 = CARTESIAN_POINT('Ctrl Pts',(58.7927238879383,249.502368268629,21.7089530153205)) ;
#115064 = CARTESIAN_POINT('Ctrl Pts',(58.7899317287585,249.455448762239,21.6584799424396)) ;
#115065 = CARTESIAN_POINT('Ctrl Pts',(58.7871395695787,249.405948442476,21.6105612289866)) ;
#115066 = CARTESIAN_POINT('Ctrl Pts',(58.7843506651955,249.356505824819,21.5626983739753)) ;
#115067 = CARTESIAN_POINT('Ctrl Pts',(58.7815617608122,249.30448871986,21.51738430438)) ;
#115068 = CARTESIAN_POINT('Ctrl Pts',(58.7787728564289,249.25019293795,21.4749029045106)) ;
#115069 = CARTESIAN_POINT('Ctrl Pts',(58.7759856827621,249.195930850491,21.4324478674157)) ;
#115070 = CARTESIAN_POINT('Ctrl Pts',(58.7731985090952,249.139393277057,21.3928223145572)) ;
#115071 = CARTESIAN_POINT('Ctrl Pts',(58.7704113354284,249.080910027098,21.3562706740573)) ;
#115072 = CARTESIAN_POINT('Ctrl Pts',(58.7676249399336,249.02244310552,21.3197292386862)) ;
#115073 = CARTESIAN_POINT('Ctrl Pts',(58.7648385444389,248.962032001927,21.2862602718357)) ;
#115074 = CARTESIAN_POINT('Ctrl Pts',(58.7620521489441,248.900034997751,21.2560645586065)) ;
#115075 = CARTESIAN_POINT('Ctrl Pts',(58.7592655802319,248.838034139506,21.2258669682488)) ;
#115076 = CARTESIAN_POINT('Ctrl Pts',(58.7564790115198,248.774447627337,21.1989432481034)) ;
#115077 = CARTESIAN_POINT('Ctrl Pts',(58.7536924428076,248.709656167469,21.17544714661)) ;
#115078 = CARTESIAN_POINT('Ctrl Pts',(58.7509029235853,248.644796104282,21.1519261666751)) ;
#115079 = CARTESIAN_POINT('Ctrl Pts',(58.748113404363,248.57872900956,21.1318402157891)) ;
#115080 = CARTESIAN_POINT('Ctrl Pts',(58.7453238851406,248.51185234569,21.1152936577427)) ;
#115081 = CARTESIAN_POINT('Ctrl Pts',(58.7425326956608,248.444935638628,21.0987371922495)) ;
#115082 = CARTESIAN_POINT('Ctrl Pts',(58.7397415061809,248.37720887972,21.0857244300631)) ;
#115083 = CARTESIAN_POINT('Ctrl Pts',(58.736950316701,248.30907860944,21.076308376674)) ;
#115084 = CARTESIAN_POINT('Ctrl Pts',(58.7341543620011,248.240832024689,21.0668762478566)) ;
#115085 = CARTESIAN_POINT('Ctrl Pts',(58.7313584073012,248.17218104245,21.0610531242674)) ;
#115086 = CARTESIAN_POINT('Ctrl Pts',(58.7285624526013,248.103535307741,21.0588399916076)) ;
#115087 = CARTESIAN_POINT('Ctrl Pts',(58.7273018417982,248.072585037063,21.0578421575083)) ;
#115088 = CARTESIAN_POINT('Ctrl Pts',(58.726041230995,248.041635801624,21.0575774690523)) ;
#115089 = CARTESIAN_POINT('Ctrl Pts',(58.7247806201919,248.010724805815,21.0580425688778)) ;
#115090 = CARTESIAN_POINT('Ctrl Pts',(58.7219842798933,247.942156725141,21.0590742730181)) ;
#115091 = CARTESIAN_POINT('Ctrl Pts',(58.7191879395947,247.873508291733,21.0637044531742)) ;
#115092 = CARTESIAN_POINT('Ctrl Pts',(58.7163915992962,247.805187857571,21.0719432798719)) ;
#115093 = CARTESIAN_POINT('Ctrl Pts',(58.7135994394385,247.736969560314,21.0801697897824)) ;
#115094 = CARTESIAN_POINT('Ctrl Pts',(58.7108072795809,247.669078772524,21.0919941805918)) ;
#115095 = CARTESIAN_POINT('Ctrl Pts',(58.7080151197233,247.601922755114,21.1073746202295)) ;
#115096 = CARTESIAN_POINT('Ctrl Pts',(58.7052262145697,247.534845018667,21.1227371315315)) ;
#115097 = CARTESIAN_POINT('Ctrl Pts',(58.7024373094162,247.468500827733,21.1416473499285)) ;
#115098 = CARTESIAN_POINT('Ctrl Pts',(58.6996484042626,247.403289427283,21.1640120136241)) ;
#115099 = CARTESIAN_POINT('Ctrl Pts',(58.6968612297687,247.338118493875,21.1863627988909)) ;
#115100 = CARTESIAN_POINT('Ctrl Pts',(58.6940740552748,247.274079419687,21.2121636179814)) ;
#115101 = CARTESIAN_POINT('Ctrl Pts',(58.691286880781,247.211556902627,21.2412711979733)) ;
#115102 = CARTESIAN_POINT('Ctrl Pts',(58.6885004844042,247.149051840463,21.2703706517766)) ;
#115103 = CARTESIAN_POINT('Ctrl Pts',(58.6857140880274,247.088062939629,21.3027748266298)) ;
#115104 = CARTESIAN_POINT('Ctrl Pts',(58.6829276916506,247.028953828074,21.3382927901524)) ;
#115105 = CARTESIAN_POINT('Ctrl Pts',(58.6801411220031,246.969841040849,21.3738129623415)) ;
#115106 = CARTESIAN_POINT('Ctrl Pts',(58.6773545523557,246.912608694361,21.4124470526189)) ;
#115107 = CARTESIAN_POINT('Ctrl Pts',(58.6745679827083,246.857593205218,21.4539596891866)) ;
#115108 = CARTESIAN_POINT('Ctrl Pts',(58.6717784624778,246.802519462457,21.4955162817626)) ;
#115109 = CARTESIAN_POINT('Ctrl Pts',(58.6689889422474,246.749667654034,21.5399572071158)) ;
#115110 = CARTESIAN_POINT('Ctrl Pts',(58.666199422017,246.699341926844,21.5870061266556)) ;
#115111 = CARTESIAN_POINT('Ctrl Pts',(58.663408231486,246.648986065767,21.6340832180065)) ;
#115112 = CARTESIAN_POINT('Ctrl Pts',(58.660617040955,246.601159636707,21.6837710578745)) ;
#115113 = CARTESIAN_POINT('Ctrl Pts',(58.6578258504241,246.556128676984,21.7357577022364)) ;
#115114 = CARTESIAN_POINT('Ctrl Pts',(58.6550298946189,246.511020837926,21.7878331010608)) ;
#115115 = CARTESIAN_POINT('Ctrl Pts',(58.6522339388137,246.46871829441,21.842214749955)) ;
#115116 = CARTESIAN_POINT('Ctrl Pts',(58.6494379830085,246.429445163528,21.898559747003)) ;
#115117 = CARTESIAN_POINT('Ctrl Pts',(58.6481773800745,246.411738222693,21.9239638211535)) ;
#115118 = CARTESIAN_POINT('Ctrl Pts',(58.6469167771404,246.394646494269,21.9497666479011)) ;
#115119 = CARTESIAN_POINT('Ctrl Pts',(58.6456561742064,246.378187442659,21.9759352063564)) ;
#115120 = CARTESIAN_POINT('Ctrl Pts',(58.6428598595974,246.341677384473,22.0339832406195)) ;
#115121 = CARTESIAN_POINT('Ctrl Pts',(58.6400635449883,246.308140358677,22.0940600892534)) ;
#115122 = CARTESIAN_POINT('Ctrl Pts',(58.6372672303792,246.27780747817,22.1558289491428)) ;
#115123 = CARTESIAN_POINT('Ctrl Pts',(58.6344750962971,246.247519945717,22.2175054637788)) ;
#115124 = CARTESIAN_POINT('Ctrl Pts',(58.6316829622149,246.220427265785,22.2808685320038)) ;
#115125 = CARTESIAN_POINT('Ctrl Pts',(58.6288908281328,246.196716358875,22.345553919129)) ;
#115126 = CARTESIAN_POINT('Ctrl Pts',(58.6261019487543,246.17303309103,22.4101639045139)) ;
#115127 = CARTESIAN_POINT('Ctrl Pts',(58.6233130693759,246.152723935081,22.4760926887444)) ;
#115128 = CARTESIAN_POINT('Ctrl Pts',(58.6205241899974,246.135928324648,22.5429547235698)) ;
#115129 = CARTESIAN_POINT('Ctrl Pts',(58.6177370412627,246.119143136759,22.6097752670487)) ;
#115130 = CARTESIAN_POINT('Ctrl Pts',(58.6149498925279,246.105867288354,22.6775274372463)) ;
#115131 = CARTESIAN_POINT('Ctrl Pts',(58.6121627437932,246.096190355381,22.7458106212959)) ;
#115132 = CARTESIAN_POINT('Ctrl Pts',(58.6093763731201,246.086516123825,22.8140747433828)) ;
#115133 = CARTESIAN_POINT('Ctrl Pts',(58.606590002447,246.080438881949,22.8828690992664)) ;
#115134 = CARTESIAN_POINT('Ctrl Pts',(58.6038036317739,246.077996764028,22.9517847621219)) ;
#115135 = CARTESIAN_POINT('Ctrl Pts',(58.6010170877351,246.075554494161,23.0207047128525)) ;
#115136 = CARTESIAN_POINT('Ctrl Pts',(58.5982305436963,246.076747812098,23.0897454949275)) ;
#115137 = CARTESIAN_POINT('Ctrl Pts',(58.5954439996576,246.081562762467,23.1584967717109)) ;
#115138 = CARTESIAN_POINT('Ctrl Pts',(58.5926545047176,246.086382811783,23.2273208548889)) ;
#115139 = CARTESIAN_POINT('Ctrl Pts',(58.5898650097776,246.094832112971,23.2958543303937)) ;
#115140 = CARTESIAN_POINT('Ctrl Pts',(58.5870755148377,246.106844775149,23.3636915855581)) ;
#115141 = CARTESIAN_POINT('Ctrl Pts',(58.5842843494512,246.118864630927,23.4315694640283)) ;
#115142 = CARTESIAN_POINT('Ctrl Pts',(58.5814931840647,246.134451983669,23.4987498142027)) ;
#115143 = CARTESIAN_POINT('Ctrl Pts',(58.5787020186782,246.15349031868,23.5648395660296)) ;
#115144 = CARTESIAN_POINT('Ctrl Pts',(58.5759060875323,246.172561160589,23.6310421624277)) ;
#115145 = CARTESIAN_POINT('Ctrl Pts',(58.5731101563863,246.195094584209,23.6961499805135)) ;
#115146 = CARTESIAN_POINT('Ctrl Pts',(58.5703142252404,246.220925270349,23.7597882209357)) ;
#115147 = CARTESIAN_POINT('Ctrl Pts',(58.5690533929005,246.232573684687,23.7884860490959)) ;
#115148 = CARTESIAN_POINT('Ctrl Pts',(58.5677925605607,246.244891992381,23.8168853416463)) ;
#115149 = CARTESIAN_POINT('Ctrl Pts',(58.5665317282209,246.257862018413,23.8449534396603)) ;
#115150 = CARTESIAN_POINT('Ctrl Pts',(58.5637353561837,246.286627951021,23.907205050714)) ;
#115151 = CARTESIAN_POINT('Ctrl Pts',(58.5609389841465,246.318715472937,23.9680699191845)) ;
#115152 = CARTESIAN_POINT('Ctrl Pts',(58.5581426121093,246.353968178566,24.0271706885432)) ;
#115153 = CARTESIAN_POINT('Ctrl Pts',(58.5553504207015,246.389168180729,24.0861831011273)) ;
#115154 = CARTESIAN_POINT('Ctrl Pts',(58.5525582292937,246.427523725309,24.1434362309142)) ;
#115155 = CARTESIAN_POINT('Ctrl Pts',(58.5497660378859,246.468831320435,24.1985748198616)) ;
#115156 = CARTESIAN_POINT('Ctrl Pts',(58.5469771016104,246.510090759233,24.2536491283305)) ;
#115157 = CARTESIAN_POINT('Ctrl Pts',(58.5441881653349,246.554295120499,24.3066134009809)) ;
#115158 = CARTESIAN_POINT('Ctrl Pts',(58.5413992290594,246.601197159575,24.3571405748899)) ;
#115159 = CARTESIAN_POINT('Ctrl Pts',(58.5386120237277,246.64807008906,24.4076363892807)) ;
#115160 = CARTESIAN_POINT('Ctrl Pts',(58.5358248183959,246.697637041688,24.4556977466538)) ;
#115161 = CARTESIAN_POINT('Ctrl Pts',(58.5330376130642,246.749610966573,24.5010311726646)) ;
#115162 = CARTESIAN_POINT('Ctrl Pts',(58.5302511861787,246.80157037552,24.5463519373794)) ;
#115163 = CARTESIAN_POINT('Ctrl Pts',(58.5274647592931,246.855935052385,24.5889459608517)) ;
#115164 = CARTESIAN_POINT('Ctrl Pts',(58.5246783324075,246.912382936087,24.6285583647508)) ;
#115165 = CARTESIAN_POINT('Ctrl Pts',(58.5218917326256,246.96883432235,24.6681732265785)) ;
#115166 = CARTESIAN_POINT('Ctrl Pts',(58.5191051328438,247.027368768849,24.7048058217007)) ;
#115167 = CARTESIAN_POINT('Ctrl Pts',(58.5163185330619,247.087634639173,24.7382441742145)) ;
#115168 = CARTESIAN_POINT('Ctrl Pts',(58.5135289834622,247.14796430529,24.7717179236481)) ;
#115169 = CARTESIAN_POINT('Ctrl Pts',(58.5107394338625,247.210028622949,24.8019904439401)) ;
#115170 = CARTESIAN_POINT('Ctrl Pts',(58.5079498842627,247.273451606802,24.8288958757875)) ;
#115171 = CARTESIAN_POINT('Ctrl Pts',(58.505158664758,247.336912557487,24.8558174140043)) ;
#115172 = CARTESIAN_POINT('Ctrl Pts',(58.5023674452532,247.401733331759,24.8793676845295)) ;
#115173 = CARTESIAN_POINT('Ctrl Pts',(58.4995762257484,247.467520864779,24.8994301066198)) ;
#115174 = CARTESIAN_POINT('Ctrl Pts',(58.4967802418732,247.533420691432,24.9195267735309)) ;
#115175 = CARTESIAN_POINT('Ctrl Pts',(58.4939842579979,247.600290094166,24.9361235920358)) ;
#115176 = CARTESIAN_POINT('Ctrl Pts',(58.4911882741226,247.667724722639,24.9491548570577)) ;
#115177 = CARTESIAN_POINT('Ctrl Pts',(58.4899279434935,247.698121867801,24.9550288903769)) ;
#115178 = CARTESIAN_POINT('Ctrl Pts',(58.4886676128644,247.728633780147,24.960179144585)) ;
#115179 = CARTESIAN_POINT('Ctrl Pts',(58.4874072822353,247.759223217459,24.9646030573924)) ;
#115180 = CARTESIAN_POINT('Ctrl Pts',(58.4846109259678,247.827093475288,24.9744186058051)) ;
#115181 = CARTESIAN_POINT('Ctrl Pts',(58.4818145697003,247.895611647255,24.9806935219246)) ;
#115182 = CARTESIAN_POINT('Ctrl Pts',(58.4790182134328,247.964376111971,24.9833532460141)) ;
#115183 = CARTESIAN_POINT('Ctrl Pts',(58.4762260371539,248.033037787681,24.9860089943526)) ;
#115184 = CARTESIAN_POINT('Ctrl Pts',(58.473433860875,248.101944538866,24.9850602573903)) ;
#115185 = CARTESIAN_POINT('Ctrl Pts',(58.4706416845961,248.170687605668,24.9804839972767)) ;
#115186 = CARTESIAN_POINT('Ctrl Pts',(58.4678527624422,248.239350556276,24.975913070538)) ;
#115187 = CARTESIAN_POINT('Ctrl Pts',(58.4650638402884,248.307849713925,24.9677230496966)) ;
#115188 = CARTESIAN_POINT('Ctrl Pts',(58.4622749181345,248.375776108533,24.9559429471642)) ;
#115189 = CARTESIAN_POINT('Ctrl Pts',(58.4594877262922,248.44366036004,24.9441701532789)) ;
#115190 = CARTESIAN_POINT('Ctrl Pts',(58.4567005344499,248.510972070924,24.9288117800453)) ;
#115191 = CARTESIAN_POINT('Ctrl Pts',(58.4539133426076,248.577308734089,24.9099485212185)) ;
#115192 = CARTESIAN_POINT('Ctrl Pts',(58.451126928564,248.643626885226,24.8910905264064)) ;
#115193 = CARTESIAN_POINT('Ctrl Pts',(58.4483405145204,248.708970056959,24.8687297219814)) ;
#115194 = CARTESIAN_POINT('Ctrl Pts',(58.4455541004769,248.772949017595,24.842997191496)) ;
#115195 = CARTESIAN_POINT('Ctrl Pts',(58.4427675128737,248.836931963339,24.8172630581879)) ;
#115196 = CARTESIAN_POINT('Ctrl Pts',(58.4399809252705,248.899550074883,24.7881569673943)) ;
#115197 = CARTESIAN_POINT('Ctrl Pts',(58.4371943376673,248.960433968837,24.7558581832023)) ;
#115198 = CARTESIAN_POINT('Ctrl Pts',(58.4344047991749,249.021382336495,24.7235251958388)) ;
#115199 = CARTESIAN_POINT('Ctrl Pts',(58.4316152606825,249.080592387219,24.687992998362)) ;
#115200 = CARTESIAN_POINT('Ctrl Pts',(58.4288257221901,249.137720129312,24.6494864056455)) ;
#115201 = CARTESIAN_POINT('Ctrl Pts',(58.4260345131964,249.194882082071,24.6109567534454)) ;
#115202 = CARTESIAN_POINT('Ctrl Pts',(58.4232433042026,249.249958852386,24.5694494563931)) ;
#115203 = CARTESIAN_POINT('Ctrl Pts',(58.4204520952088,249.302638453795,24.5252305088572)) ;
#115204 = CARTESIAN_POINT('Ctrl Pts',(58.4176561208302,249.355407994215,24.4809360670453)) ;
#115205 = CARTESIAN_POINT('Ctrl Pts',(58.4148601464515,249.405771839137,24.4339210698719)) ;
#115206 = CARTESIAN_POINT('Ctrl Pts',(58.4120641720729,249.453454504378,24.3844887041671)) ;
#115207 = CARTESIAN_POINT('Ctrl Pts',(58.4108037267986,249.474950191366,24.3622042396784)) ;
#115208 = CARTESIAN_POINT('Ctrl Pts',(58.4095432815242,249.495901534199,24.3394289500331)) ;
#115209 = CARTESIAN_POINT('Ctrl Pts',(58.4082828362499,249.516286078954,24.3161926703443)) ;
#115210 = CARTESIAN_POINT('Ctrl Pts',(58.4055122728199,249.56109300186,24.2651173971337)) ;
#115211 = CARTESIAN_POINT('Ctrl Pts',(58.40274170939,249.603342138574,24.2116035703064)) ;
#115212 = CARTESIAN_POINT('Ctrl Pts',(58.3999711459601,249.642753907238,24.1559400585432)) ;
#115213 = CARTESIAN_POINT('Ctrl Pts',(58.3972044286694,249.682110963872,24.1003538197341)) ;
#115214 = CARTESIAN_POINT('Ctrl Pts',(58.3944377113788,249.718638173866,24.0426242158972)) ;
#115215 = CARTESIAN_POINT('Ctrl Pts',(58.3916709940882,249.752094809022,23.9830746385671)) ;
#115216 = CARTESIAN_POINT('Ctrl Pts',(58.3889071300701,249.785516940869,23.9235864737921)) ;
#115217 = CARTESIAN_POINT('Ctrl Pts',(58.3861432660521,249.815874533976,23.8622824917599)) ;
#115218 = CARTESIAN_POINT('Ctrl Pts',(58.3833794020341,249.842970083777,23.7995150618265)) ;
#115219 = CARTESIAN_POINT('Ctrl Pts',(58.3806168005465,249.870053256357,23.7367763039944)) ;
#115220 = CARTESIAN_POINT('Ctrl Pts',(58.3778541990589,249.893877133095,23.6725758783721)) ;
#115221 = CARTESIAN_POINT('Ctrl Pts',(58.3750915975712,249.914290896923,23.6072892775912)) ;
#115222 = CARTESIAN_POINT('Ctrl Pts',(58.3723298784158,249.93469814091,23.5420235283397)) ;
#115223 = CARTESIAN_POINT('Ctrl Pts',(58.3695681592603,249.951697288545,23.4756727715741)) ;
#115224 = CARTESIAN_POINT('Ctrl Pts',(58.3668064401048,249.965187020979,23.4086288486433)) ;
#115225 = CARTESIAN_POINT('Ctrl Pts',(58.3640429993408,249.978685162682,23.341543131676)) ;
#115226 = CARTESIAN_POINT('Ctrl Pts',(58.3612795585768,249.988669418579,23.2737638768196)) ;
#115227 = CARTESIAN_POINT('Ctrl Pts',(58.3585161178127,249.995089633367,23.2056931294797)) ;
#115228 = CARTESIAN_POINT('Ctrl Pts',(58.3560033747606,250.000927410066,23.1437977200838)) ;
#115229 = CARTESIAN_POINT('Ctrl Pts',(58.3534906317085,250.003819081637,23.0816616940208)) ;
#115230 = CARTESIAN_POINT('Ctrl Pts',(58.3509778886564,250.003764344365,23.0195888835014)) ;
#115231 = CARTESIAN_POINT('',(57.9402651077866,248.892933365216,24.7900173477895)) ;
#115232 = CARTESIAN_POINT('Ctrl Pts',(58.3509778886279,250.003764344364,23.019588882796)) ;
#115233 = CARTESIAN_POINT('Ctrl Pts',(58.347531931365,250.003689278043,22.9344626889131)) ;
#115234 = CARTESIAN_POINT('Ctrl Pts',(58.3440859741021,249.998074586572,22.8495796685279)) ;
#115235 = CARTESIAN_POINT('Ctrl Pts',(58.3406400168393,249.987036956171,22.7655633879631)) ;
#115236 = CARTESIAN_POINT('Ctrl Pts',(58.3371336303593,249.975805766967,22.6800737757032)) ;
#115237 = CARTESIAN_POINT('Ctrl Pts',(58.3336272438794,249.95895981642,22.5954814373205)) ;
#115238 = CARTESIAN_POINT('Ctrl Pts',(58.3301208573995,249.936670483819,22.5124206483804)) ;
#115239 = CARTESIAN_POINT('Ctrl Pts',(58.3298000350211,249.934631086069,22.5048208700867)) ;
#115240 = CARTESIAN_POINT('Ctrl Pts',(58.3294792126427,249.932546151232,22.4972338987649)) ;
#115241 = CARTESIAN_POINT('Ctrl Pts',(58.3291583902643,249.930415830371,22.4896602116041)) ;
#115242 = CARTESIAN_POINT('Ctrl Pts',(58.3263616510593,249.911844956662,22.423637299127)) ;
#115243 = CARTESIAN_POINT('Ctrl Pts',(58.3235649118542,249.889774292161,22.3584592623116)) ;
#115244 = CARTESIAN_POINT('Ctrl Pts',(58.3207681726492,249.864298716166,22.2945235043388)) ;
#115245 = CARTESIAN_POINT('Ctrl Pts',(58.3179756150477,249.838861230515,22.2306833412612)) ;
#115246 = CARTESIAN_POINT('Ctrl Pts',(58.3151830574462,249.810029117849,22.1680822227063)) ;
#115247 = CARTESIAN_POINT('Ctrl Pts',(58.3123904998447,249.777947242342,22.1071031651792)) ;
#115248 = CARTESIAN_POINT('Ctrl Pts',(58.3096012005832,249.745902799781,22.0461952576638)) ;
#115249 = CARTESIAN_POINT('Ctrl Pts',(58.3068119013218,249.710616352775,21.986906084436)) ;
#115250 = CARTESIAN_POINT('Ctrl Pts',(58.3040226020603,249.67228042168,21.9295977298812)) ;
#115251 = CARTESIAN_POINT('Ctrl Pts',(58.3012350359522,249.633968310921,21.8723249843298)) ;
#115252 = CARTESIAN_POINT('Ctrl Pts',(58.2984474698442,249.592610747277,21.8170310227065)) ;
#115253 = CARTESIAN_POINT('Ctrl Pts',(58.2956599037361,249.548444863234,21.7640510505049)) ;
#115254 = CARTESIAN_POINT('Ctrl Pts',(58.2928731188216,249.504291356334,21.7110859255261)) ;
#115255 = CARTESIAN_POINT('Ctrl Pts',(58.2900863339071,249.457331405552,21.6604338792422)) ;
#115256 = CARTESIAN_POINT('Ctrl Pts',(58.2872995489926,249.40784281188,21.6123975375607)) ;
#115257 = CARTESIAN_POINT('Ctrl Pts',(58.2845125944698,249.358351206252,21.5643582723083)) ;
#115258 = CARTESIAN_POINT('Ctrl Pts',(58.281725639947,249.306331006061,21.5189353676264)) ;
#115259 = CARTESIAN_POINT('Ctrl Pts',(58.2789386854242,249.252095996024,21.4763937600894)) ;
#115260 = CARTESIAN_POINT('Ctrl Pts',(58.2761487884291,249.197803724553,21.433807237037)) ;
#115261 = CARTESIAN_POINT('Ctrl Pts',(58.2733588914341,249.141292363387,21.3941083854731)) ;
#115262 = CARTESIAN_POINT('Ctrl Pts',(58.270568994439,249.082907028509,21.3575204532029)) ;
#115263 = CARTESIAN_POINT('Ctrl Pts',(58.2677774312452,249.024486824397,21.320910669672)) ;
#115264 = CARTESIAN_POINT('Ctrl Pts',(58.2649858680514,248.964190848044,21.2874157415453)) ;
#115265 = CARTESIAN_POINT('Ctrl Pts',(58.2621943048577,248.902388871569,21.2572129585288)) ;
#115266 = CARTESIAN_POINT('Ctrl Pts',(58.2593979865201,248.840481621717,21.2269587281453)) ;
#115267 = CARTESIAN_POINT('Ctrl Pts',(58.2566016681825,248.777063703201,21.2000080267488)) ;
#115268 = CARTESIAN_POINT('Ctrl Pts',(58.2538053498449,248.712524075554,21.1764896927257)) ;
#115269 = CARTESIAN_POINT('Ctrl Pts',(58.2525482146562,248.68350912547,21.1659166027871)) ;
#115270 = CARTESIAN_POINT('Ctrl Pts',(58.2512910794675,248.654267654608,21.1560365562948)) ;
#115271 = CARTESIAN_POINT('Ctrl Pts',(58.2500339442788,248.62483575027,21.1468579102349)) ;
#115272 = CARTESIAN_POINT('Ctrl Pts',(58.2472375760956,248.559367500237,21.1264409542565)) ;
#115273 = CARTESIAN_POINT('Ctrl Pts',(58.2444412079124,248.49270009251,21.109417978687)) ;
#115274 = CARTESIAN_POINT('Ctrl Pts',(58.2416448397292,248.425218349744,21.0959260329037)) ;
#115275 = CARTESIAN_POINT('Ctrl Pts',(58.2388526472344,248.357837374371,21.0824542340247)) ;
#115276 = CARTESIAN_POINT('Ctrl Pts',(58.2360604547397,248.289644954913,21.0725030953405)) ;
#115277 = CARTESIAN_POINT('Ctrl Pts',(58.2332682622449,248.221041097842,21.0661599175538)) ;
#115278 = CARTESIAN_POINT('Ctrl Pts',(58.230479317708,248.152517042732,21.0598241183322)) ;
#115279 = CARTESIAN_POINT('Ctrl Pts',(58.227690373171,248.083582986998,21.0570879895587)) ;
#115280 = CARTESIAN_POINT('Ctrl Pts',(58.2249014286341,248.014647364114,21.0579874677565)) ;
#115281 = CARTESIAN_POINT('Ctrl Pts',(58.2221142106069,247.945754416166,21.058886389128)) ;
#115282 = CARTESIAN_POINT('Ctrl Pts',(58.2193269925798,247.876860392677,21.0634164462515)) ;
#115283 = CARTESIAN_POINT('Ctrl Pts',(58.2165397745527,247.808375505614,21.0715615219602)) ;
#115284 = CARTESIAN_POINT('Ctrl Pts',(58.2137533306026,247.739909638441,21.0797043355868)) ;
#115285 = CARTESIAN_POINT('Ctrl Pts',(58.2109668866525,247.671853169254,21.0914601166436)) ;
#115286 = CARTESIAN_POINT('Ctrl Pts',(58.2081804427024,247.604611157847,21.1067608939988)) ;
#115287 = CARTESIAN_POINT('Ctrl Pts',(58.2053938215471,247.537364870154,21.122062644414)) ;
#115288 = CARTESIAN_POINT('Ctrl Pts',(58.2026072003918,247.470933621065,21.1409097273127)) ;
#115289 = CARTESIAN_POINT('Ctrl Pts',(58.1998205792366,247.405710479151,21.1631834612825)) ;
#115290 = CARTESIAN_POINT('Ctrl Pts',(58.1970310020144,247.340418148081,21.1854808233821)) ;
#115291 = CARTESIAN_POINT('Ctrl Pts',(58.1942414247923,247.276336947073,21.2112119318301)) ;
#115292 = CARTESIAN_POINT('Ctrl Pts',(58.1914518475702,247.21384206527,21.2402091160393)) ;
#115293 = CARTESIAN_POINT('Ctrl Pts',(58.1886605968347,247.151309691755,21.2692236961382)) ;
#115294 = CARTESIAN_POINT('Ctrl Pts',(58.1858693460991,247.090365965219,21.3015080218526)) ;
#115295 = CARTESIAN_POINT('Ctrl Pts',(58.1830780953635,247.031360973862,21.3368487057601)) ;
#115296 = CARTESIAN_POINT('Ctrl Pts',(58.1802820751297,246.972255158811,21.372249777411)) ;
#115297 = CARTESIAN_POINT('Ctrl Pts',(58.1774860548958,246.915095097436,21.4107173563645)) ;
#115298 = CARTESIAN_POINT('Ctrl Pts',(58.1746900346619,246.860200707424,21.4519955648736)) ;
#115299 = CARTESIAN_POINT('Ctrl Pts',(58.1734298558723,246.835459561019,21.4705998375473)) ;
#115300 = CARTESIAN_POINT('Ctrl Pts',(58.1721696770828,246.811178184421,21.4897745163459)) ;
#115301 = CARTESIAN_POINT('Ctrl Pts',(58.1709094982933,246.787383444121,21.5094937044066)) ;
#115302 = CARTESIAN_POINT('Ctrl Pts',(58.1681151052984,246.734619617146,21.5532201672229)) ;
#115303 = CARTESIAN_POINT('Ctrl Pts',(58.1653207123035,246.684043271349,21.5997987073911)) ;
#115304 = CARTESIAN_POINT('Ctrl Pts',(58.1625263193086,246.63597889751,21.6489820144193)) ;
#115305 = CARTESIAN_POINT('Ctrl Pts',(58.1597361135886,246.587986546018,21.6980916224268)) ;
#115306 = CARTESIAN_POINT('Ctrl Pts',(58.1569459078686,246.542499036916,21.7497979021576)) ;
#115307 = CARTESIAN_POINT('Ctrl Pts',(58.1541557021486,246.499807471406,21.80381366164)) ;
#115308 = CARTESIAN_POINT('Ctrl Pts',(58.1513687516734,246.457165712795,21.8577664026454)) ;
#115309 = CARTESIAN_POINT('Ctrl Pts',(58.1485818011981,246.417313722939,21.9140228884521)) ;
#115310 = CARTESIAN_POINT('Ctrl Pts',(58.1457948507228,246.380504163978,21.9722608317058)) ;
#115311 = CARTESIAN_POINT('Ctrl Pts',(58.1430096300917,246.3437174525,22.0304626270022)) ;
#115312 = CARTESIAN_POINT('Ctrl Pts',(58.1402244094606,246.30996968794,22.090643025414)) ;
#115313 = CARTESIAN_POINT('Ctrl Pts',(58.1374391888295,246.27947088064,22.152449847082)) ;
#115314 = CARTESIAN_POINT('Ctrl Pts',(58.1346547425464,246.24898055263,22.2142394851943)) ;
#115315 = CARTESIAN_POINT('Ctrl Pts',(58.1318702962634,246.221737606122,22.2776542082484)) ;
#115316 = CARTESIAN_POINT('Ctrl Pts',(58.1290858499804,246.197905780348,22.3423178703659)) ;
#115317 = CARTESIAN_POINT('Ctrl Pts',(58.1263012237015,246.174072414006,22.4069857125577)) ;
#115318 = CARTESIAN_POINT('Ctrl Pts',(58.1235165974226,246.153650773739,22.4729021919415)) ;
#115319 = CARTESIAN_POINT('Ctrl Pts',(58.1207319711437,246.136755552144,22.5396735626319)) ;
#115320 = CARTESIAN_POINT('Ctrl Pts',(58.1179443709375,246.119842286777,22.6065162438617)) ;
#115321 = CARTESIAN_POINT('Ctrl Pts',(58.1151567707312,246.106463076697,22.67421516094)) ;
#115322 = CARTESIAN_POINT('Ctrl Pts',(58.112369170525,246.096681798163,22.7423648479079)) ;
#115323 = CARTESIAN_POINT('Ctrl Pts',(58.109579889445,246.08689462169,22.8105556279367)) ;
#115324 = CARTESIAN_POINT('Ctrl Pts',(58.106790608365,246.080709738345,22.879197229136)) ;
#115325 = CARTESIAN_POINT('Ctrl Pts',(58.104001327285,246.078139012731,22.9478803197007)) ;
#115326 = CARTESIAN_POINT('Ctrl Pts',(58.1012072448587,246.075563861983,23.0166816383284)) ;
#115327 = CARTESIAN_POINT('Ctrl Pts',(58.0984131624324,246.076615277465,23.0855240976552)) ;
#115328 = CARTESIAN_POINT('Ctrl Pts',(58.0956190800061,246.081253054944,23.1540005109516)) ;
#115329 = CARTESIAN_POINT('Ctrl Pts',(58.0943410707733,246.083374367609,23.1853215226719)) ;
#115330 = CARTESIAN_POINT('Ctrl Pts',(58.0930630615406,246.086245281554,23.2165660568276)) ;
#115331 = CARTESIAN_POINT('Ctrl Pts',(58.0917850523078,246.089858388485,23.2476958707352)) ;
#115332 = CARTESIAN_POINT('Ctrl Pts',(58.0889844571912,246.097776053995,23.3159129090573)) ;
#115333 = CARTESIAN_POINT('Ctrl Pts',(58.0861838620747,246.109292215792,23.3838458349369)) ;
#115334 = CARTESIAN_POINT('Ctrl Pts',(58.0833832669581,246.124375389261,23.4510863687974)) ;
#115335 = CARTESIAN_POINT('Ctrl Pts',(58.0805868570181,246.139436022612,23.5182264191906)) ;
#115336 = CARTESIAN_POINT('Ctrl Pts',(58.0777904470782,246.158052980711,23.584675657751)) ;
#115337 = CARTESIAN_POINT('Ctrl Pts',(58.0749940371382,246.180143156851,23.6500321834753)) ;
#115338 = CARTESIAN_POINT('Ctrl Pts',(58.0722009096359,246.20220740345,23.7153119934366)) ;
#115339 = CARTESIAN_POINT('Ctrl Pts',(58.0694077821336,246.227736614132,23.7795011769888)) ;
#115340 = CARTESIAN_POINT('Ctrl Pts',(58.0666146546313,246.256597332155,23.8422110282283)) ;
#115341 = CARTESIAN_POINT('Ctrl Pts',(58.0638232776877,246.285439962074,23.9048815768318)) ;
#115342 = CARTESIAN_POINT('Ctrl Pts',(58.0610319007441,246.317609752663,23.9660741892134)) ;
#115343 = CARTESIAN_POINT('Ctrl Pts',(58.0582405238005,246.352924961368,24.0254196814177)) ;
#115344 = CARTESIAN_POINT('Ctrl Pts',(58.0554499512619,246.388229993113,24.0847480717338)) ;
#115345 = CARTESIAN_POINT('Ctrl Pts',(58.0526593787234,246.426678393208,24.1422299785625)) ;
#115346 = CARTESIAN_POINT('Ctrl Pts',(58.0498688061849,246.468043120542,24.1975219728842)) ;
#115347 = CARTESIAN_POINT('Ctrl Pts',(58.0470780930781,246.509409931522,24.2528167524048)) ;
#115348 = CARTESIAN_POINT('Ctrl Pts',(58.0442873799713,246.553693066345,24.3059210102196)) ;
#115349 = CARTESIAN_POINT('Ctrl Pts',(58.0414966668645,246.600623992847,24.3565228413767)) ;
#115350 = CARTESIAN_POINT('Ctrl Pts',(58.0387030804571,246.647603239136,24.4071767718607)) ;
#115351 = CARTESIAN_POINT('Ctrl Pts',(58.0359094940496,246.697235384496,24.4553227743831)) ;
#115352 = CARTESIAN_POINT('Ctrl Pts',(58.0331159076422,246.749214363596,24.500685148443)) ;
#115353 = CARTESIAN_POINT('Ctrl Pts',(58.0303206895187,246.801223703288,24.5460740183772)) ;
#115354 = CARTESIAN_POINT('Ctrl Pts',(58.0275254713952,246.855582220368,24.5886757213844)) ;
#115355 = CARTESIAN_POINT('Ctrl Pts',(58.0247302532716,246.911952202286,24.6282560103748)) ;
#115356 = CARTESIAN_POINT('Ctrl Pts',(58.0219303703382,246.968416257455,24.6679023530748)) ;
#115357 = CARTESIAN_POINT('Ctrl Pts',(58.0191304874047,247.026898062941,24.7045169583855)) ;
#115358 = CARTESIAN_POINT('Ctrl Pts',(58.0163306044712,247.087033262235,24.7379103641024)) ;
#115359 = CARTESIAN_POINT('Ctrl Pts',(58.0151072717549,247.113307702434,24.7525007047326)) ;
#115360 = CARTESIAN_POINT('Ctrl Pts',(58.0138839390385,247.139897496379,24.7664767247963)) ;
#115361 = CARTESIAN_POINT('Ctrl Pts',(58.0126606063222,247.166771094637,24.7798255209739)) ;
#115362 = CARTESIAN_POINT('Ctrl Pts',(58.0098986862272,247.227443657434,24.8099631179776)) ;
#115363 = CARTESIAN_POINT('Ctrl Pts',(58.0071367661322,247.2898098171,24.8370223835677)) ;
#115364 = CARTESIAN_POINT('Ctrl Pts',(58.0043748460373,247.353520461229,24.8608077831538)) ;
#115365 = CARTESIAN_POINT('Ctrl Pts',(58.0016175292885,247.417124917582,24.8845535391494)) ;
#115366 = CARTESIAN_POINT('Ctrl Pts',(57.9988602125398,247.482068941796,24.9050360866091)) ;
#115367 = CARTESIAN_POINT('Ctrl Pts',(57.996102895791,247.547980335786,24.922106484412)) ;
#115368 = CARTESIAN_POINT('Ctrl Pts',(57.9933481370867,247.613830581823,24.9391610455012)) ;
#115369 = CARTESIAN_POINT('Ctrl Pts',(57.9905933783824,247.680645933727,24.9528096041868)) ;
#115370 = CARTESIAN_POINT('Ctrl Pts',(57.9878386196781,247.748037235499,24.9629524201021)) ;
#115371 = CARTESIAN_POINT('Ctrl Pts',(57.9850854200319,247.815390397105,24.9730894956817)) ;
#115372 = CARTESIAN_POINT('Ctrl Pts',(57.9823322203858,247.883318364787,24.9797246873835)) ;
#115373 = CARTESIAN_POINT('Ctrl Pts',(57.9795790207396,247.951421880769,24.982809352199)) ;
#115374 = CARTESIAN_POINT('Ctrl Pts',(57.9768263833758,248.019511488059,24.9858933870375)) ;
#115375 = CARTESIAN_POINT('Ctrl Pts',(57.9740737460121,248.087776069018,24.985428312288)) ;
#115376 = CARTESIAN_POINT('Ctrl Pts',(57.9713211086483,248.155813320873,24.9814174994303)) ;
#115377 = CARTESIAN_POINT('Ctrl Pts',(57.9685662598804,248.223905232256,24.9774034643798)) ;
#115378 = CARTESIAN_POINT('Ctrl Pts',(57.9658114111125,248.291768945337,24.969838029674)) ;
#115379 = CARTESIAN_POINT('Ctrl Pts',(57.9630565623445,248.35900545855,24.9587766240456)) ;
#115380 = CARTESIAN_POINT('Ctrl Pts',(57.9603006131048,248.426268830547,24.9477107997481)) ;
#115381 = CARTESIAN_POINT('Ctrl Pts',(57.9575446638651,248.492904010497,24.9331463308006)) ;
#115382 = CARTESIAN_POINT('Ctrl Pts',(57.9547887146254,248.558523270173,24.9151895911899)) ;
#115383 = CARTESIAN_POINT('Ctrl Pts',(57.9520281095573,248.624253385304,24.8972025159342)) ;
#115384 = CARTESIAN_POINT('Ctrl Pts',(57.9492675044892,248.688963673453,24.875811884145)) ;
#115385 = CARTESIAN_POINT('Ctrl Pts',(57.9465068994212,248.752283471603,24.8511733703317)) ;
#115386 = CARTESIAN_POINT('Ctrl Pts',(57.9444263022096,248.800005978886,24.8326039546159)) ;
#115387 = CARTESIAN_POINT('Ctrl Pts',(57.9423457049981,248.84693900529,24.8121906938376)) ;
#115388 = CARTESIAN_POINT('Ctrl Pts',(57.9402651077866,248.892933365216,24.7900173477895)) ;
#115389 = CARTESIAN_POINT('Ctrl Pts',(57.9402651077866,248.892933365216,24.7900173477895)) ;
#115390 = CARTESIAN_POINT('Ctrl Pts',(57.9402651077866,248.907470247387,24.7827857167614)) ;
#115391 = CARTESIAN_POINT('Ctrl Pts',(57.9402651077866,248.922007129558,24.7755540857334)) ;
#115392 = CARTESIAN_POINT('Ctrl Pts',(57.9402651077866,248.936544011728,24.7683224547054)) ;
#115393 = CARTESIAN_POINT('',(55.9402651077866,250.003765107786,23.0213203435596)) ;
#115394 = CARTESIAN_POINT('Origin',(55.9402651077866,248.040265107786,23.0213203435596)) ;
#115395 = CARTESIAN_POINT('Origin',(61.8645744874958,248.040265107786,23.0213203435596)) ;
#115396 = CARTESIAN_POINT('',(57.9402651077867,247.09020061484,21.6384890010805)) ;
#115397 = CARTESIAN_POINT('Ctrl Pts',(58.2783798877068,247.272019130299,24.5128441216388)) ;
#115398 = CARTESIAN_POINT('Ctrl Pts',(58.2748979901455,247.332077509349,24.5437786657587)) ;
#115399 = CARTESIAN_POINT('Ctrl Pts',(58.271320587604,247.393976935328,24.5710716276367)) ;
#115400 = CARTESIAN_POINT('Ctrl Pts',(58.2627451136209,247.545035169529,24.627038133204)) ;
#115401 = CARTESIAN_POINT('Ctrl Pts',(58.2577412103424,247.635251058642,24.6521323366216)) ;
#115402 = CARTESIAN_POINT('Ctrl Pts',(58.2520375966099,247.746374322123,24.6732460496859)) ;
#115403 = CARTESIAN_POINT('Ctrl Pts',(58.2510614554046,247.765721207416,24.6765713936764)) ;
#115404 = CARTESIAN_POINT('Ctrl Pts',(58.2495470185004,247.796358451649,24.6812853540765)) ;
#115405 = CARTESIAN_POINT('Ctrl Pts',(58.2489973964822,247.807611769283,24.6828999325575)) ;
#115406 = CARTESIAN_POINT('Ctrl Pts',(58.2479269228372,247.82982153336,24.6858564298797)) ;
#115407 = CARTESIAN_POINT('Ctrl Pts',(58.2474057836264,247.840776417959,24.6872048386251)) ;
#115408 = CARTESIAN_POINT('Ctrl Pts',(58.2460500620374,247.869616457428,24.6904661162285)) ;
#115409 = CARTESIAN_POINT('Ctrl Pts',(58.2452247764834,247.887520895965,24.6921996997116)) ;
#115410 = CARTESIAN_POINT('Ctrl Pts',(58.2406147555242,247.989179322784,24.7003949117824)) ;
#115411 = CARTESIAN_POINT('Ctrl Pts',(58.2370870272144,248.073304410782,24.7008476342292)) ;
#115412 = CARTESIAN_POINT('Ctrl Pts',(58.2287463145611,248.272606508734,24.6869330955302)) ;
#115413 = CARTESIAN_POINT('Ctrl Pts',(58.2239556977729,248.386951254969,24.666937377997)) ;
#115414 = CARTESIAN_POINT('Ctrl Pts',(58.2174797274263,248.526774465455,24.6272557885101)) ;
#115415 = CARTESIAN_POINT('Ctrl Pts',(58.2161407395415,248.555010573944,24.618429292159)) ;
#115416 = CARTESIAN_POINT('Ctrl Pts',(58.2138873395185,248.601282287633,24.6026103821848)) ;
#115417 = CARTESIAN_POINT('Ctrl Pts',(58.2129868720803,248.619457016907,24.5960441790141)) ;
#115418 = CARTESIAN_POINT('Ctrl Pts',(58.211176412634,248.655345786747,24.5823728542874)) ;
#115419 = CARTESIAN_POINT('Ctrl Pts',(58.2102668150887,248.673060055623,24.5752764884306)) ;
#115420 = CARTESIAN_POINT('Ctrl Pts',(58.2079855305723,248.716687486869,24.5569295826173)) ;
#115421 = CARTESIAN_POINT('Ctrl Pts',(58.2066020787698,248.742444209569,24.5453240706538)) ;
#115422 = CARTESIAN_POINT('Ctrl Pts',(58.2035397571162,248.797939511295,24.5186133560451)) ;
#115423 = CARTESIAN_POINT('Ctrl Pts',(58.2018532644446,248.827545110282,24.5032605867735)) ;
#115424 = CARTESIAN_POINT('Ctrl Pts',(58.1964360981523,248.919771472909,24.4518902846567)) ;
#115425 = CARTESIAN_POINT('Ctrl Pts',(58.1926171847178,248.980531233698,24.4127082157092)) ;
#115426 = CARTESIAN_POINT('Ctrl Pts',(58.1837372591114,249.114597859774,24.3134510911288)) ;
#115427 = CARTESIAN_POINT('Ctrl Pts',(58.1786702794447,249.185729624582,24.2508347284892)) ;
#115428 = CARTESIAN_POINT('Ctrl Pts',(58.1729178114678,249.264707236925,24.1684763816803)) ;
#115429 = CARTESIAN_POINT('Ctrl Pts',(58.1719480002254,249.277961319081,24.1541635148172)) ;
#115430 = CARTESIAN_POINT('Ctrl Pts',(58.1704413246273,249.298519479715,24.1311714641225)) ;
#115431 = CARTESIAN_POINT('Ctrl Pts',(58.1698932954084,249.305990030728,24.1226440957261)) ;
#115432 = CARTESIAN_POINT('Ctrl Pts',(58.168827411681,249.32052174376,24.1057134721195)) ;
#115433 = CARTESIAN_POINT('Ctrl Pts',(58.168309261345,249.327587902867,24.0973154820613)) ;
#115434 = CARTESIAN_POINT('Ctrl Pts',(58.1669608589769,249.345957850368,24.0750431585538)) ;
#115435 = CARTESIAN_POINT('Ctrl Pts',(58.1661398787163,249.357123244922,24.0610558868507)) ;
#115436 = CARTESIAN_POINT('Ctrl Pts',(58.1615902604397,249.418663666299,23.9813800957598)) ;
#115437 = CARTESIAN_POINT('Ctrl Pts',(58.1581133955458,249.464350905108,23.9122071198179)) ;
#115438 = CARTESIAN_POINT('Ctrl Pts',(58.1497133261122,249.562639591519,23.7363718607849)) ;
#115439 = CARTESIAN_POINT('Ctrl Pts',(58.1448185566736,249.609381217752,23.6269569637157)) ;
#115440 = CARTESIAN_POINT('Ctrl Pts',(58.1382251156756,249.652798275206,23.4854788705331)) ;
#115441 = CARTESIAN_POINT('Ctrl Pts',(58.1368966544137,249.660670299946,23.4572024944238)) ;
#115442 = CARTESIAN_POINT('Ctrl Pts',(58.1346592433347,249.672461531608,23.4100991480262)) ;
#115443 = CARTESIAN_POINT('Ctrl Pts',(58.133764063552,249.676806062136,23.3913849231925)) ;
#115444 = CARTESIAN_POINT('Ctrl Pts',(58.1319634604706,249.684803683137,23.354034121129)) ;
#115445 = CARTESIAN_POINT('Ctrl Pts',(58.1310584101892,249.688463610433,23.3354019303104)) ;
#115446 = CARTESIAN_POINT('Ctrl Pts',(58.1287878578837,249.696757591018,23.2890301136861)) ;
#115447 = CARTESIAN_POINT('Ctrl Pts',(58.1274106257705,249.701011779221,23.261229166923)) ;
#115448 = CARTESIAN_POINT('Ctrl Pts',(58.1211474422744,249.716930184925,23.136271055147)) ;
#115449 = CARTESIAN_POINT('Ctrl Pts',(58.116026325459,249.720778833748,23.0383220310557)) ;
#115450 = CARTESIAN_POINT('Ctrl Pts',(58.1053096317472,249.711084330988,22.8370403410001)) ;
#115451 = CARTESIAN_POINT('Ctrl Pts',(58.0997283898167,249.696506013282,22.7341548738862)) ;
#115452 = CARTESIAN_POINT('Ctrl Pts',(58.0935609702691,249.668167456351,22.6149541822122)) ;
#115453 = CARTESIAN_POINT('Ctrl Pts',(58.0926260918652,249.663504790088,22.5967116992631)) ;
#115454 = CARTESIAN_POINT('Ctrl Pts',(58.0911615920557,249.655586213827,22.5677702245165)) ;
#115455 = CARTESIAN_POINT('Ctrl Pts',(58.0906217053732,249.652528797081,22.5570189341692)) ;
#115456 = CARTESIAN_POINT('Ctrl Pts',(58.0895529908071,249.646190233062,22.5355475427917)) ;
#115457 = CARTESIAN_POINT('Ctrl Pts',(58.089024191361,249.64290865212,22.5248282444628)) ;
#115458 = CARTESIAN_POINT('Ctrl Pts',(58.0876284254771,249.633866577783,22.496316399195)) ;
#115459 = CARTESIAN_POINT('Ctrl Pts',(58.08677169367,249.627915504649,22.4785855522774)) ;
#115460 = CARTESIAN_POINT('Ctrl Pts',(58.0815853579806,249.589520970401,22.3702321063645)) ;
#115461 = CARTESIAN_POINT('Ctrl Pts',(58.0775885480795,249.549622248674,22.2824334260245)) ;
#115462 = CARTESIAN_POINT('Ctrl Pts',(58.0693654513875,249.452957056141,22.1106526920531)) ;
#115463 = CARTESIAN_POINT('Ctrl Pts',(58.0651478651584,249.395682564177,22.0274109048578)) ;
#115464 = CARTESIAN_POINT('Ctrl Pts',(58.0593077990619,249.311859657264,21.9264150970558)) ;
#115465 = CARTESIAN_POINT('Ctrl Pts',(58.057932431993,249.291802257686,21.9035436080008)) ;
#115466 = CARTESIAN_POINT('Ctrl Pts',(58.0556320097518,249.25785639115,21.8668947867048)) ;
#115467 = CARTESIAN_POINT('Ctrl Pts',(58.0547219724047,249.244328748527,21.8527923760427)) ;
#115468 = CARTESIAN_POINT('Ctrl Pts',(58.0529028381644,249.217119371765,21.8254011447104)) ;
#115469 = CARTESIAN_POINT('Ctrl Pts',(58.05199438389,249.203451236086,21.8121029589124)) ;
#115470 = CARTESIAN_POINT('Ctrl Pts',(58.0497360855303,249.169297481163,21.7799885935626)) ;
#115471 = CARTESIAN_POINT('Ctrl Pts',(58.048375181623,249.1485654137,21.7614437890237)) ;
#115472 = CARTESIAN_POINT('Ctrl Pts',(58.0414723744861,249.042698798655,21.6713821694049)) ;
#115473 = CARTESIAN_POINT('Ctrl Pts',(58.0356180024846,248.951073489103,21.6079453898174)) ;
#115474 = CARTESIAN_POINT('Ctrl Pts',(58.0249619385237,248.775979976737,21.5108570780169)) ;
#115475 = CARTESIAN_POINT('Ctrl Pts',(58.0202073655345,248.694778896838,21.4739389864986)) ;
#115476 = CARTESIAN_POINT('Ctrl Pts',(58.0146997007208,248.59213829509,21.4368063633293)) ;
#115477 = CARTESIAN_POINT('Ctrl Pts',(58.0137001563191,248.573126993811,21.4303122222319)) ;
#115478 = CARTESIAN_POINT('Ctrl Pts',(58.0121563064781,248.543054449113,21.4206391722487)) ;
#115479 = CARTESIAN_POINT('Ctrl Pts',(58.0116001012966,248.532069751408,21.4172300904024)) ;
#115480 = CARTESIAN_POINT('Ctrl Pts',(58.0105177425053,248.510370249532,21.4107395497992)) ;
#115481 = CARTESIAN_POINT('Ctrl Pts',(58.0099912505437,248.49965813027,21.4076514189601)) ;
#115482 = CARTESIAN_POINT('Ctrl Pts',(58.0086248640635,248.471479036562,21.3998311922984)) ;
#115483 = CARTESIAN_POINT('Ctrl Pts',(58.0077942134424,248.453964504307,21.3952744111645)) ;
#115484 = CARTESIAN_POINT('Ctrl Pts',(58.005951466049,248.414373542241,21.3856551050401)) ;
#115485 = CARTESIAN_POINT('Ctrl Pts',(58.0049464301702,248.392261256857,21.3807543828688)) ;
#115486 = CARTESIAN_POINT('Ctrl Pts',(58.0016621161521,248.318671226203,21.3660011609283)) ;
#115487 = CARTESIAN_POINT('Ctrl Pts',(57.9994450969059,248.266829949253,21.3581124851648)) ;
#115488 = CARTESIAN_POINT('Ctrl Pts',(57.9920522315695,248.091675339794,21.3398022241462)) ;
#115489 = CARTESIAN_POINT('Ctrl Pts',(57.9869451430184,247.967612030511,21.34058648171)) ;
#115490 = CARTESIAN_POINT('Ctrl Pts',(57.9801496161107,247.816730852348,21.3582887454584)) ;
#115491 = CARTESIAN_POINT('Ctrl Pts',(57.97886791646,247.788787547477,21.3622843005214)) ;
#115492 = CARTESIAN_POINT('Ctrl Pts',(57.9767682610458,247.743958274348,21.3698529378715)) ;
#115493 = CARTESIAN_POINT('Ctrl Pts',(57.9759640560679,247.727003030229,21.3729850693059)) ;
#115494 = CARTESIAN_POINT('Ctrl Pts',(57.9742510932236,247.691363668561,21.3801384466992)) ;
#115495 = CARTESIAN_POINT('Ctrl Pts',(57.9733405748524,247.672694031667,21.3842187278339)) ;
#115496 = CARTESIAN_POINT('Ctrl Pts',(57.971072575685,247.626884688805,21.3950535390632)) ;
#115497 = CARTESIAN_POINT('Ctrl Pts',(57.9697038275137,247.599837049454,21.402169300435)) ;
#115498 = CARTESIAN_POINT('Ctrl Pts',(57.9666844118785,247.541471207537,21.4190949980413)) ;
#115499 = CARTESIAN_POINT('Ctrl Pts',(57.9650265886409,247.510237800917,21.4291544307489)) ;
#115500 = CARTESIAN_POINT('Ctrl Pts',(57.9597702061772,247.41360619379,21.4634353894848)) ;
#115501 = CARTESIAN_POINT('Ctrl Pts',(57.956089153945,247.349413117597,21.4908206473135)) ;
#115502 = CARTESIAN_POINT('Ctrl Pts',(57.9483128361232,247.218895015048,21.556388768177)) ;
#115503 = CARTESIAN_POINT('Ctrl Pts',(57.9442208456806,247.153105283643,21.5952707933102)) ;
#115504 = CARTESIAN_POINT('Ctrl Pts',(57.9402651077867,247.09020061484,21.6384890010805)) ;
#115505 = CARTESIAN_POINT('',(57.9402651077866,249.01460512908,21.6554848536836)) ;
#115506 = CARTESIAN_POINT('Origin',(57.9402651077866,248.040265107786,23.0213203435596)) ;
#115507 = CARTESIAN_POINT('',(58.0159557280338,249.718014855353,23.0222406915478)) ;
#115508 = CARTESIAN_POINT('Ctrl Pts',(58.0159557280338,249.718014855353,23.0222406915478)) ;
#115509 = CARTESIAN_POINT('Ctrl Pts',(58.0130009107869,249.718048781581,22.9603948218142)) ;
#115510 = CARTESIAN_POINT('Ctrl Pts',(58.0100460935399,249.71465877968,22.8984282829972)) ;
#115511 = CARTESIAN_POINT('Ctrl Pts',(58.007091276293,249.707831191182,22.8367440178679)) ;
#115512 = CARTESIAN_POINT('Ctrl Pts',(58.0041427654337,249.701018174625,22.7751914038217)) ;
#115513 = CARTESIAN_POINT('Ctrl Pts',(58.0011942545745,249.690782209106,22.7139203500751)) ;
#115514 = CARTESIAN_POINT('Ctrl Pts',(57.9982457437152,249.67716158959,22.6533326122993)) ;
#115515 = CARTESIAN_POINT('Ctrl Pts',(57.9953008849976,249.663557841109,22.5928199208812)) ;
#115516 = CARTESIAN_POINT('Ctrl Pts',(57.99235602628,249.64657786523,22.5329893419975)) ;
#115517 = CARTESIAN_POINT('Ctrl Pts',(57.9894111675624,249.626311417612,22.4742351896888)) ;
#115518 = CARTESIAN_POINT('Ctrl Pts',(57.9864689847879,249.606063385772,22.4155344262787)) ;
#115519 = CARTESIAN_POINT('Ctrl Pts',(57.9835268020133,249.582534970385,22.3579086103247)) ;
#115520 = CARTESIAN_POINT('Ctrl Pts',(57.9805846192387,249.555865987917,22.3017378016325)) ;
#115521 = CARTESIAN_POINT('Ctrl Pts',(57.9776441397485,249.52921244462,22.2455995112676)) ;
#115522 = CARTESIAN_POINT('Ctrl Pts',(57.9747036602584,249.499422156201,22.1909149978639)) ;
#115523 = CARTESIAN_POINT('Ctrl Pts',(57.9717631807682,249.466682681607,22.1380435083633)) ;
#115524 = CARTESIAN_POINT('Ctrl Pts',(57.9688224013677,249.433939867794,22.0851666263053)) ;
#115525 = CARTESIAN_POINT('Ctrl Pts',(57.9658816219672,249.39824751513,22.0341035617204)) ;
#115526 = CARTESIAN_POINT('Ctrl Pts',(57.9629408425668,249.359837984726,21.9851869134728)) ;
#115527 = CARTESIAN_POINT('Ctrl Pts',(57.9599999943149,249.321427555054,21.9362691199573)) ;
#115528 = CARTESIAN_POINT('Ctrl Pts',(57.957059146063,249.280300131595,21.8894982238037)) ;
#115529 = CARTESIAN_POINT('Ctrl Pts',(57.9541182978111,249.236728627424,21.8451740479502)) ;
#115530 = CARTESIAN_POINT('Ctrl Pts',(57.9511747935572,249.19311777202,21.8008098410945)) ;
#115531 = CARTESIAN_POINT('Ctrl Pts',(57.9482312893032,249.147058780088,21.758897110781)) ;
#115532 = CARTESIAN_POINT('Ctrl Pts',(57.9452877850493,249.098860870152,21.7196982500162)) ;
#115533 = CARTESIAN_POINT('Ctrl Pts',(57.9436135592951,249.0714465452,21.6974024635769)) ;
#115534 = CARTESIAN_POINT('Ctrl Pts',(57.9419393335408,249.043340861804,21.6759839362171)) ;
#115535 = CARTESIAN_POINT('Ctrl Pts',(57.9402651077866,249.01460512908,21.6554848536836)) ;
#115536 = CARTESIAN_POINT('Ctrl Pts',(58.1788076829103,247.272018954284,24.5128440309778)) ;
#115537 = CARTESIAN_POINT('Ctrl Pts',(58.1784179371879,247.279284607174,24.5165863851439)) ;
#115538 = CARTESIAN_POINT('Ctrl Pts',(58.1780281914655,247.286575747914,24.520274691396)) ;
#115539 = CARTESIAN_POINT('Ctrl Pts',(58.1776384457431,247.293891499148,24.5239086101279)) ;
#115540 = CARTESIAN_POINT('Ctrl Pts',(58.1747316426243,247.348453864506,24.551011117471)) ;
#115541 = CARTESIAN_POINT('Ctrl Pts',(58.1718248395055,247.404604858308,24.5751927161058)) ;
#115542 = CARTESIAN_POINT('Ctrl Pts',(58.1689180363866,247.46199958075,24.596266070479)) ;
#115543 = CARTESIAN_POINT('Ctrl Pts',(58.1659845348604,247.51992146228,24.6175329794126)) ;
#115544 = CARTESIAN_POINT('Ctrl Pts',(58.1630510333342,247.579109603263,24.635633945886)) ;
#115545 = CARTESIAN_POINT('Ctrl Pts',(58.160117531808,247.639184487202,24.6504242071275)) ;
#115546 = CARTESIAN_POINT('Ctrl Pts',(58.1572184824335,247.698553828976,24.6650407659455)) ;
#115547 = CARTESIAN_POINT('Ctrl Pts',(58.1543194330591,247.758788688729,24.6764238394425)) ;
#115548 = CARTESIAN_POINT('Ctrl Pts',(58.1514203836846,247.819505594553,24.6844830835875)) ;
#115549 = CARTESIAN_POINT('Ctrl Pts',(58.1485230192334,247.8801872118,24.6925376437116)) ;
#115550 = CARTESIAN_POINT('Ctrl Pts',(58.1456256547822,247.941349813877,24.697272137706)) ;
#115551 = CARTESIAN_POINT('Ctrl Pts',(58.142728290331,248.002600915774,24.6986475242671)) ;
#115552 = CARTESIAN_POINT('Ctrl Pts',(58.1398315368371,248.063839101863,24.7000226208051)) ;
#115553 = CARTESIAN_POINT('Ctrl Pts',(58.1369347833431,248.125165239899,24.698040004807)) ;
#115554 = CARTESIAN_POINT('Ctrl Pts',(58.1340380298492,248.186185009511,24.6927127106537)) ;
#115555 = CARTESIAN_POINT('Ctrl Pts',(58.1310776940082,248.248544133741,24.687268484954)) ;
#115556 = CARTESIAN_POINT('Ctrl Pts',(58.1281173581673,248.310582723376,24.6783310047208)) ;
#115557 = CARTESIAN_POINT('Ctrl Pts',(58.1251570223263,248.371885976444,24.6659700515431)) ;
#115558 = CARTESIAN_POINT('Ctrl Pts',(58.1222563924866,248.431952825165,24.653858402203)) ;
#115559 = CARTESIAN_POINT('Ctrl Pts',(58.1193557626468,248.491313236416,24.6384603002759)) ;
#115560 = CARTESIAN_POINT('Ctrl Pts',(58.1164551328071,248.549590391702,24.6198924619402)) ;
#115561 = CARTESIAN_POINT('Ctrl Pts',(58.1134649439655,248.609666895456,24.6007513284376)) ;
#115562 = CARTESIAN_POINT('Ctrl Pts',(58.110474755124,248.668591588852,24.5782416766697)) ;
#115563 = CARTESIAN_POINT('Ctrl Pts',(58.1074845662824,248.725974522,24.5525445798354)) ;
#115564 = CARTESIAN_POINT('Ctrl Pts',(58.1044943774408,248.783357455147,24.5268474830012)) ;
#115565 = CARTESIAN_POINT('Ctrl Pts',(58.1015041885992,248.839198140224,24.4979632754152)) ;
#115566 = CARTESIAN_POINT('Ctrl Pts',(58.0985139997577,248.893137479031,24.4661226763606)) ;
#115567 = CARTESIAN_POINT('Ctrl Pts',(58.0956224023982,248.945298348437,24.4353319146303)) ;
#115568 = CARTESIAN_POINT('Ctrl Pts',(58.0927308050388,248.995903687477,24.4016453930233)) ;
#115569 = CARTESIAN_POINT('Ctrl Pts',(58.0898392076793,249.044610396575,24.3652457891802)) ;
#115570 = CARTESIAN_POINT('Ctrl Pts',(58.0869038054332,249.094054964928,24.328294766753)) ;
#115571 = CARTESIAN_POINT('Ctrl Pts',(58.083968403187,249.14154238529,24.2885479614825)) ;
#115572 = CARTESIAN_POINT('Ctrl Pts',(58.0810330009409,249.186740289614,24.246244716716)) ;
#115573 = CARTESIAN_POINT('Ctrl Pts',(58.0781493250111,249.231141737132,24.2046869203877)) ;
#115574 = CARTESIAN_POINT('Ctrl Pts',(58.0752656490813,249.273333311625,24.1606624209357)) ;
#115575 = CARTESIAN_POINT('Ctrl Pts',(58.0723819731514,249.313031776829,24.1144397646084)) ;
#115576 = CARTESIAN_POINT('Ctrl Pts',(58.0695000032287,249.352706756084,24.0682444539963)) ;
#115577 = CARTESIAN_POINT('Ctrl Pts',(58.066618033306,249.389891212695,24.0198539555883)) ;
#115578 = CARTESIAN_POINT('Ctrl Pts',(58.0637360633833,249.424339861513,23.9695724928302)) ;
#115579 = CARTESIAN_POINT('Ctrl Pts',(58.0608547006152,249.458781252914,23.9193016230424)) ;
#115580 = CARTESIAN_POINT('Ctrl Pts',(58.0579733378471,249.490487688015,23.8671410062943)) ;
#115581 = CARTESIAN_POINT('Ctrl Pts',(58.055091975079,249.51925646722,23.8134248955086)) ;
#115582 = CARTESIAN_POINT('Ctrl Pts',(58.0521167733035,249.548962175894,23.7579593810805)) ;
#115583 = CARTESIAN_POINT('Ctrl Pts',(58.0491415715279,249.57553523724,23.7008357853397)) ;
#115584 = CARTESIAN_POINT('Ctrl Pts',(58.0461663697523,249.598804484298,23.6424484095493)) ;
#115585 = CARTESIAN_POINT('Ctrl Pts',(58.0432809417461,249.621371604854,23.5858228150443)) ;
#115586 = CARTESIAN_POINT('Ctrl Pts',(58.0403955137399,249.640831383414,23.5280091627858)) ;
#115587 = CARTESIAN_POINT('Ctrl Pts',(58.0375100857337,249.657078109145,23.4693837108818)) ;
#115588 = CARTESIAN_POINT('Ctrl Pts',(58.0344899970734,249.674083056779,23.4080222552788)) ;
#115589 = CARTESIAN_POINT('Ctrl Pts',(58.0314699084132,249.687567524432,23.345771987281)) ;
#115590 = CARTESIAN_POINT('Ctrl Pts',(58.0284498197529,249.697470551021,23.2830743911185)) ;
#115591 = CARTESIAN_POINT('Ctrl Pts',(58.0254297310927,249.70737357761,23.2203767949559)) ;
#115592 = CARTESIAN_POINT('Ctrl Pts',(58.0224096424324,249.713695185353,23.157232515933)) ;
#115593 = CARTESIAN_POINT('Ctrl Pts',(58.0193895537721,249.716436503615,23.094083756793)) ;
#115594 = CARTESIAN_POINT('Ctrl Pts',(58.0182449452072,249.717475458664,23.0701504824072)) ;
#115595 = CARTESIAN_POINT('Ctrl Pts',(58.0171003366423,249.718001713324,23.0461979481158)) ;
#115596 = CARTESIAN_POINT('Ctrl Pts',(58.0159557280774,249.718014855352,23.0222406924601)) ;
#115597 = CARTESIAN_POINT('Origin',(67.8645744874958,248.040265107786,23.0213203435596)) ;
#115598 = CARTESIAN_POINT('',(64.9402651077865,247.083045674831,21.643432097121)) ;
#115599 = CARTESIAN_POINT('Ctrl Pts',(64.9402651077865,247.083045674831,21.643432097121)) ;
#115600 = CARTESIAN_POINT('Ctrl Pts',(64.9429442584677,247.12507063848,21.6142373405957)) ;
#115601 = CARTESIAN_POINT('Ctrl Pts',(64.9456568014745,247.168412522621,21.5869781986287)) ;
#115602 = CARTESIAN_POINT('Ctrl Pts',(64.9534903335802,247.297537671544,21.5137865668355)) ;
#115603 = CARTESIAN_POINT('Ctrl Pts',(64.9585541047601,247.386156155901,21.4732740839693)) ;
#115604 = CARTESIAN_POINT('Ctrl Pts',(64.9651045226291,247.510493389731,21.4290290087006)) ;
#115605 = CARTESIAN_POINT('Ctrl Pts',(64.9667974157123,247.54354804353,21.4184098240117)) ;
#115606 = CARTESIAN_POINT('Ctrl Pts',(64.9698295496712,247.604424180614,21.4009169071032)) ;
#115607 = CARTESIAN_POINT('Ctrl Pts',(64.9711783206033,247.632137220411,21.3937158607698)) ;
#115608 = CARTESIAN_POINT('Ctrl Pts',(64.9741845354924,247.69525834054,21.3790279756566)) ;
#115609 = CARTESIAN_POINT('Ctrl Pts',(64.9758286860229,247.730751853986,21.3719702773205)) ;
#115610 = CARTESIAN_POINT('Ctrl Pts',(64.9814973341675,247.856004905134,21.3512504991235)) ;
#115611 = CARTESIAN_POINT('Ctrl Pts',(64.9853512460892,247.946620612448,21.3437277039494)) ;
#115612 = CARTESIAN_POINT('Ctrl Pts',(64.9919640501974,248.103010786515,21.3434608258745)) ;
#115613 = CARTESIAN_POINT('Ctrl Pts',(64.9947278190027,248.168567408158,21.3471974311091)) ;
#115614 = CARTESIAN_POINT('Ctrl Pts',(64.9988173788173,248.261737060338,21.3580134073213)) ;
#115615 = CARTESIAN_POINT('Ctrl Pts',(65.0000640303766,248.289652569886,21.3619693947758)) ;
#115616 = CARTESIAN_POINT('Ctrl Pts',(65.0023757763416,248.340108117153,21.3704215465206)) ;
#115617 = CARTESIAN_POINT('Ctrl Pts',(65.0034315115626,248.362680892829,21.3746811471485)) ;
#115618 = CARTESIAN_POINT('Ctrl Pts',(65.0052841444264,248.4012774587,21.3827885489868)) ;
#115619 = CARTESIAN_POINT('Ctrl Pts',(65.0060701180475,248.417344242686,21.386411279269)) ;
#115620 = CARTESIAN_POINT('Ctrl Pts',(65.0079962241007,248.455971264325,21.3957205707178)) ;
#115621 = CARTESIAN_POINT('Ctrl Pts',(65.0091473486686,248.478469988853,21.4016405548478)) ;
#115622 = CARTESIAN_POINT('Ctrl Pts',(65.0150051661908,248.590558436948,21.4336401892062)) ;
#115623 = CARTESIAN_POINT('Ctrl Pts',(65.0199617587939,248.677982187339,21.4666929349023)) ;
#115624 = CARTESIAN_POINT('Ctrl Pts',(65.0301831850078,248.852853334251,21.5500519205486)) ;
#115625 = CARTESIAN_POINT('Ctrl Pts',(65.0354170419856,248.939451890663,21.6013212356338)) ;
#115626 = CARTESIAN_POINT('Ctrl Pts',(65.0421053422461,249.048876189929,21.6801517141006)) ;
#115627 = CARTESIAN_POINT('Ctrl Pts',(65.0437828749084,249.076176909543,21.7011246956489)) ;
#115628 = CARTESIAN_POINT('Ctrl Pts',(65.0467952350284,249.124902498778,21.7409995180681)) ;
#115629 = CARTESIAN_POINT('Ctrl Pts',(65.0481392160044,249.14652645241,21.7596366918629)) ;
#115630 = CARTESIAN_POINT('Ctrl Pts',(65.051140548017,249.194471114417,21.8031398531834)) ;
#115631 = CARTESIAN_POINT('Ctrl Pts',(65.0527843895861,249.220483820073,21.8283244466984)) ;
#115632 = CARTESIAN_POINT('Ctrl Pts',(65.0589312649896,249.316325785309,21.927320851295)) ;
#115633 = CARTESIAN_POINT('Ctrl Pts',(65.0632071273875,249.380216364349,22.00658009368)) ;
#115634 = CARTESIAN_POINT('Ctrl Pts',(65.0711704638523,249.484919915245,22.1637478284439)) ;
#115635 = CARTESIAN_POINT('Ctrl Pts',(65.0748495832706,249.527553272571,22.2400203241101)) ;
#115636 = CARTESIAN_POINT('Ctrl Pts',(65.0798106033813,249.573462309034,22.3396632888364)) ;
#115637 = CARTESIAN_POINT('Ctrl Pts',(65.0808441557246,249.58245401302,22.3602580953042)) ;
#115638 = CARTESIAN_POINT('Ctrl Pts',(65.0826668577343,249.597254712333,22.3961047410567)) ;
#115639 = CARTESIAN_POINT('Ctrl Pts',(65.0834457249163,249.603259483455,22.4112713940417)) ;
#115640 = CARTESIAN_POINT('Ctrl Pts',(65.0853603700128,249.617255362344,22.4481855550469)) ;
#115641 = CARTESIAN_POINT('Ctrl Pts',(65.0865072770545,249.62501846455,22.4700142096568)) ;
#115642 = CARTESIAN_POINT('Ctrl Pts',(65.0923552155905,249.661714190565,22.5803847497001)) ;
#115643 = CARTESIAN_POINT('Ctrl Pts',(65.0973069440346,249.683688334885,22.6710634921928)) ;
#115644 = CARTESIAN_POINT('Ctrl Pts',(65.1074780770495,249.713338807993,22.8614116087466)) ;
#115645 = CARTESIAN_POINT('Ctrl Pts',(65.1126679093436,249.719878348329,22.9609082642936)) ;
#115646 = CARTESIAN_POINT('Ctrl Pts',(65.119323468634,249.716755152683,23.0949345744186)) ;
#115647 = CARTESIAN_POINT('Ctrl Pts',(65.1210084104323,249.714884513712,23.129431290351)) ;
#115648 = CARTESIAN_POINT('Ctrl Pts',(65.1240154692681,249.709548965202,23.192011448943)) ;
#115649 = CARTESIAN_POINT('Ctrl Pts',(65.1253474629761,249.706436258269,23.2201113362441)) ;
#115650 = CARTESIAN_POINT('Ctrl Pts',(65.1283238725396,249.697763541368,23.2836787901742)) ;
#115651 = CARTESIAN_POINT('Ctrl Pts',(65.1299548226282,249.691772330958,23.3190737776624)) ;
#115652 = CARTESIAN_POINT('Ctrl Pts',(65.1350504674581,249.669116953594,23.4309714885259)) ;
#115653 = CARTESIAN_POINT('Ctrl Pts',(65.1383947776014,249.648232939902,23.5065140499877)) ;
#115654 = CARTESIAN_POINT('Ctrl Pts',(65.1460082802719,249.588134284354,23.6765825893051)) ;
#115655 = CARTESIAN_POINT('Ctrl Pts',(65.1502305999692,249.545406572774,23.7695274956142)) ;
#115656 = CARTESIAN_POINT('Ctrl Pts',(65.1560023665131,249.480698169872,23.8819966810041)) ;
#115657 = CARTESIAN_POINT('Ctrl Pts',(65.1572568431672,249.466304071478,23.9056414940144)) ;
#115658 = CARTESIAN_POINT('Ctrl Pts',(65.1593194550077,249.442312338524,23.9429420954991)) ;
#115659 = CARTESIAN_POINT('Ctrl Pts',(65.1601068460634,249.43308394525,23.9568302435055)) ;
#115660 = CARTESIAN_POINT('Ctrl Pts',(65.1618486804703,249.412565424976,23.9867325407185)) ;
#115661 = CARTESIAN_POINT('Ctrl Pts',(65.1628072591128,249.40119930379,24.0026902658671)) ;
#115662 = CARTESIAN_POINT('Ctrl Pts',(65.1658433818841,249.364861971646,24.0518613283244)) ;
#115663 = CARTESIAN_POINT('Ctrl Pts',(65.1679693571847,249.338935540798,24.0843472902241)) ;
#115664 = CARTESIAN_POINT('Ctrl Pts',(65.1749563133598,249.251189000192,24.1862879323962)) ;
#115665 = CARTESIAN_POINT('Ctrl Pts',(65.179925186363,249.184796137221,24.2515785716899)) ;
#115666 = CARTESIAN_POINT('Ctrl Pts',(65.1874216699593,249.074449164494,24.3433897312442)) ;
#115667 = CARTESIAN_POINT('Ctrl Pts',(65.1900282577352,249.034116798202,24.3739708699628)) ;
#115668 = CARTESIAN_POINT('Ctrl Pts',(65.1946544678301,248.95853025337,24.4260739293042)) ;
#115669 = CARTESIAN_POINT('Ctrl Pts',(65.1966919981801,248.923746636596,24.4482065491329)) ;
#115670 = CARTESIAN_POINT('Ctrl Pts',(65.2000806067675,248.863298028551,24.4836108252965)) ;
#115671 = CARTESIAN_POINT('Ctrl Pts',(65.2014536159437,248.838042315875,24.4975412914879)) ;
#115672 = CARTESIAN_POINT('Ctrl Pts',(65.2042967037316,248.784180894151,24.5254637868292)) ;
#115673 = CARTESIAN_POINT('Ctrl Pts',(65.2057614599285,248.755510610096,24.5393065804216)) ;
#115674 = CARTESIAN_POINT('Ctrl Pts',(65.2101065780863,248.667896007713,24.578575499168)) ;
#115675 = CARTESIAN_POINT('Ctrl Pts',(65.2129069953708,248.607868827205,24.6014440780068)) ;
#115676 = CARTESIAN_POINT('Ctrl Pts',(65.2205135385875,248.438355378822,24.6551130669273)) ;
#115677 = CARTESIAN_POINT('Ctrl Pts',(65.225169771777,248.326838347832,24.6783139549291)) ;
#115678 = CARTESIAN_POINT('Ctrl Pts',(65.231290067591,248.187545396196,24.6928024449318)) ;
#115679 = CARTESIAN_POINT('Ctrl Pts',(65.2324622510384,248.161191675343,24.6949154454761)) ;
#115680 = CARTESIAN_POINT('Ctrl Pts',(65.2346518915165,248.11291675029,24.6976398848391)) ;
#115681 = CARTESIAN_POINT('Ctrl Pts',(65.2356613661984,248.091012246291,24.6984458951228)) ;
#115682 = CARTESIAN_POINT('Ctrl Pts',(65.2374610128899,248.052764168063,24.6991033291543)) ;
#115683 = CARTESIAN_POINT('Ctrl Pts',(65.238241992344,248.036427754098,24.6991454827031)) ;
#115684 = CARTESIAN_POINT('Ctrl Pts',(65.2401914157994,247.996274145899,24.6986626703289)) ;
#115685 = CARTESIAN_POINT('Ctrl Pts',(65.2413722310537,247.972465038682,24.6978690413795)) ;
#115686 = CARTESIAN_POINT('Ctrl Pts',(65.2458790470289,247.883083345827,24.6929826902272)) ;
#115687 = CARTESIAN_POINT('Ctrl Pts',(65.2493207892809,247.817755356926,24.6855467624979)) ;
#115688 = CARTESIAN_POINT('Ctrl Pts',(65.257209788155,247.670373880065,24.6599370900106)) ;
#115689 = CARTESIAN_POINT('Ctrl Pts',(65.2616564299217,247.588901450293,24.6393921991111)) ;
#115690 = CARTESIAN_POINT('Ctrl Pts',(65.2688086709557,247.456985146216,24.5953825016102)) ;
#115691 = CARTESIAN_POINT('Ctrl Pts',(65.2715864294882,247.405554245718,24.5753570504909)) ;
#115692 = CARTESIAN_POINT('Ctrl Pts',(65.275790800191,247.32716430926,24.5402922240756)) ;
#115693 = CARTESIAN_POINT('Ctrl Pts',(65.2772701387459,247.299477434678,24.5269836826802)) ;
#115694 = CARTESIAN_POINT('Ctrl Pts',(65.2787248749179,247.272170391302,24.5129220226314)) ;
#115695 = CARTESIAN_POINT('',(64.9402651077866,249.014605129081,21.6554848536838)) ;
#115696 = CARTESIAN_POINT('Origin',(64.9402651077866,248.040265107786,23.0213203435596)) ;
#115697 = CARTESIAN_POINT('',(65.0159557280376,249.718014941427,23.0220674823532)) ;
#115698 = CARTESIAN_POINT('Ctrl Pts',(65.0159557280376,249.718014941427,23.0220674823532)) ;
#115699 = CARTESIAN_POINT('Ctrl Pts',(65.0129864470475,249.71804263635,22.9598766929778)) ;
#115700 = CARTESIAN_POINT('Ctrl Pts',(65.0100171660575,249.714608129592,22.8975767959568)) ;
#115701 = CARTESIAN_POINT('Ctrl Pts',(65.0070478850675,249.707701354092,22.8355747460244)) ;
#115702 = CARTESIAN_POINT('Ctrl Pts',(65.0040845793459,249.700808477526,22.7736974666644)) ;
#115703 = CARTESIAN_POINT('Ctrl Pts',(65.0011212736242,249.690457279382,22.7121173204969)) ;
#115704 = CARTESIAN_POINT('Ctrl Pts',(64.9981579679026,249.676689646731,22.6512395539492)) ;
#115705 = CARTESIAN_POINT('Ctrl Pts',(64.9951981429141,249.6629381857,22.5904332951301)) ;
#115706 = CARTESIAN_POINT('Ctrl Pts',(64.9922383179257,249.645778363244,22.5303282478015)) ;
#115707 = CARTESIAN_POINT('Ctrl Pts',(64.9892784929372,249.625303467312,22.4713217423501)) ;
#115708 = CARTESIAN_POINT('Ctrl Pts',(64.9863212174516,249.604846207829,22.4123660633003)) ;
#115709 = CARTESIAN_POINT('Ctrl Pts',(64.983363941966,249.581079704203,22.3545075029837)) ;
#115710 = CARTESIAN_POINT('Ctrl Pts',(64.9804066664804,249.554147202028,22.2981287595155)) ;
#115711 = CARTESIAN_POINT('Ctrl Pts',(64.9774510127355,249.527229469373,22.2417809335958)) ;
#115712 = CARTESIAN_POINT('Ctrl Pts',(64.9744953589907,249.497149396823,22.1869117481951)) ;
#115713 = CARTESIAN_POINT('Ctrl Pts',(64.9715397052459,249.464097851673,22.1338828077664)) ;
#115714 = CARTESIAN_POINT('Ctrl Pts',(64.9685837648145,249.431043100656,22.0808487237425)) ;
#115715 = CARTESIAN_POINT('Ctrl Pts',(64.965627824383,249.395016548061,22.0296556582547)) ;
#115716 = CARTESIAN_POINT('Ctrl Pts',(64.9626718839516,249.356253739544,21.9806383635174)) ;
#115717 = CARTESIAN_POINT('Ctrl Pts',(64.9597158841829,249.317490152905,21.9316200848114)) ;
#115718 = CARTESIAN_POINT('Ctrl Pts',(64.9567598844142,249.275990508209,21.8847780386099)) ;
#115719 = CARTESIAN_POINT('Ctrl Pts',(64.9538038846455,249.232030816093,21.8404140987611)) ;
#115720 = CARTESIAN_POINT('Ctrl Pts',(64.950845407407,249.18803428067,21.7960129767989)) ;
#115721 = CARTESIAN_POINT('Ctrl Pts',(64.9478869301686,249.141573928527,21.7540944464987)) ;
#115722 = CARTESIAN_POINT('Ctrl Pts',(64.9449284529302,249.09296200236,21.7149228884741)) ;
#115723 = CARTESIAN_POINT('Ctrl Pts',(64.943374004549,249.067420237511,21.6943412986722)) ;
#115724 = CARTESIAN_POINT('Ctrl Pts',(64.9418195561678,249.041285051488,21.6745173919063)) ;
#115725 = CARTESIAN_POINT('Ctrl Pts',(64.9402651077866,249.014605129081,21.6554848536842)) ;
#115726 = CARTESIAN_POINT('Ctrl Pts',(65.1788202510297,247.272170391302,24.5129220226314)) ;
#115727 = CARTESIAN_POINT('Ctrl Pts',(65.1766225070709,247.313246345993,24.5340739321629)) ;
#115728 = CARTESIAN_POINT('Ctrl Pts',(65.174424763112,247.355149468955,24.5535035893657)) ;
#115729 = CARTESIAN_POINT('Ctrl Pts',(65.1722270191532,247.397721280128,24.5711533965168)) ;
#115730 = CARTESIAN_POINT('Ctrl Pts',(65.1693116248914,247.454194470969,24.594566563589)) ;
#115731 = CARTESIAN_POINT('Ctrl Pts',(65.1663962306296,247.512055207638,24.6149330907892)) ;
#115732 = CARTESIAN_POINT('Ctrl Pts',(65.1634808363678,247.570943480191,24.6320910511313)) ;
#115733 = CARTESIAN_POINT('Ctrl Pts',(65.1605701441249,247.629736776302,24.6492213386967)) ;
#115734 = CARTESIAN_POINT('Ctrl Pts',(65.1576594518821,247.689553833606,24.6631531944018)) ;
#115735 = CARTESIAN_POINT('Ctrl Pts',(65.1547487596392,247.750015894706,24.6737732042507)) ;
#115736 = CARTESIAN_POINT('Ctrl Pts',(65.1518406833758,247.810423615637,24.684383669385)) ;
#115737 = CARTESIAN_POINT('Ctrl Pts',(65.1489326071123,247.871474693329,24.6916881022789)) ;
#115738 = CARTESIAN_POINT('Ctrl Pts',(65.1460245308489,247.932778055922,24.6956236602205)) ;
#115739 = CARTESIAN_POINT('Ctrl Pts',(65.1431180102194,247.994048625153,24.6995571128913)) ;
#115740 = CARTESIAN_POINT('Ctrl Pts',(65.14021148959,248.055570705937,24.7001252327289)) ;
#115741 = CARTESIAN_POINT('Ctrl Pts',(65.1373049689605,248.11694797027,24.697317002596)) ;
#115742 = CARTESIAN_POINT('Ctrl Pts',(65.13439894578,248.178314729927,24.6945092530898)) ;
#115743 = CARTESIAN_POINT('Ctrl Pts',(65.1314929225996,248.239536215573,24.6883263250917)) ;
#115744 = CARTESIAN_POINT('Ctrl Pts',(65.1285868994191,248.30021800925,24.6788092730914)) ;
#115745 = CARTESIAN_POINT('Ctrl Pts',(65.1256782756473,248.36095410688,24.6692837043102)) ;
#115746 = CARTESIAN_POINT('Ctrl Pts',(65.1227696518755,248.421149044928,24.6564181282543)) ;
#115747 = CARTESIAN_POINT('Ctrl Pts',(65.1198610281037,248.48041663666,24.6403051162274)) ;
#115748 = CARTESIAN_POINT('Ctrl Pts',(65.1169511589534,248.539709604855,24.6241852051305)) ;
#115749 = CARTESIAN_POINT('Ctrl Pts',(65.1140412898031,248.598073952237,24.6048152453039)) ;
#115750 = CARTESIAN_POINT('Ctrl Pts',(65.1111314206528,248.655139668826,24.5823374276062)) ;
#115751 = CARTESIAN_POINT('Ctrl Pts',(65.1082162276858,248.712309791282,24.5598184851111)) ;
#115752 = CARTESIAN_POINT('Ctrl Pts',(65.1053010347189,248.768176072337,24.5341805344946)) ;
#115753 = CARTESIAN_POINT('Ctrl Pts',(65.102385841752,248.822390237397,24.5056132203633)) ;
#115754 = CARTESIAN_POINT('Ctrl Pts',(65.0998926885117,248.868755683124,24.4811816672545)) ;
#115755 = CARTESIAN_POINT('Ctrl Pts',(65.0973995352714,248.913913001855,24.4546084166935)) ;
#115756 = CARTESIAN_POINT('Ctrl Pts',(65.094906382031,248.957661698003,24.4260368839186)) ;
#115757 = CARTESIAN_POINT('Ctrl Pts',(65.0920042795803,249.008586445128,24.3927787937431)) ;
#115758 = CARTESIAN_POINT('Ctrl Pts',(65.0891021771295,249.057803619847,24.3566803705642)) ;
#115759 = CARTESIAN_POINT('Ctrl Pts',(65.0862000746787,249.104977954238,24.3179435028086)) ;
#115760 = CARTESIAN_POINT('Ctrl Pts',(65.0833028142183,249.152073580976,24.2792712652799)) ;
#115761 = CARTESIAN_POINT('Ctrl Pts',(65.0804055537579,249.197132739833,24.2379696450035)) ;
#115762 = CARTESIAN_POINT('Ctrl Pts',(65.0775082932975,249.239849324372,24.194283586725)) ;
#115763 = CARTESIAN_POINT('Ctrl Pts',(65.0746137241619,249.282526228598,24.1506381093242)) ;
#115764 = CARTESIAN_POINT('Ctrl Pts',(65.0717191550263,249.322864513685,24.1046129485847)) ;
#115765 = CARTESIAN_POINT('Ctrl Pts',(65.0688245858907,249.360592641566,24.0564919554392)) ;
#115766 = CARTESIAN_POINT('Ctrl Pts',(65.0659316230768,249.398299832476,24.0083976667157)) ;
#115767 = CARTESIAN_POINT('Ctrl Pts',(65.0630386602628,249.43339942201,23.9582102548082)) ;
#115768 = CARTESIAN_POINT('Ctrl Pts',(65.0601456974489,249.465659540964,23.906247330584)) ;
#115769 = CARTESIAN_POINT('Ctrl Pts',(65.0572532582051,249.497913821463,23.8542938106398)) ;
#115770 = CARTESIAN_POINT('Ctrl Pts',(65.0543608189613,249.52732938148,23.8005658525202)) ;
#115771 = CARTESIAN_POINT('Ctrl Pts',(65.0514683797175,249.553718335989,23.7454090042501)) ;
#115772 = CARTESIAN_POINT('Ctrl Pts',(65.0485732702767,249.580131651843,23.6902012371412)) ;
#115773 = CARTESIAN_POINT('Ctrl Pts',(65.045678160836,249.603512557016,23.6335624081256)) ;
#115774 = CARTESIAN_POINT('Ctrl Pts',(65.0427830513952,249.623720301239,23.5758604348308)) ;
#115775 = CARTESIAN_POINT('Ctrl Pts',(65.0398866790995,249.643936860137,23.5181332917711)) ;
#115776 = CARTESIAN_POINT('Ctrl Pts',(65.0369903068037,249.660977356128,23.4593425740367)) ;
#115777 = CARTESIAN_POINT('Ctrl Pts',(65.034093934508,249.674751137605,23.3998708432641)) ;
#115778 = CARTESIAN_POINT('Ctrl Pts',(65.0311920366838,249.688551195891,23.3402856558261)) ;
#115779 = CARTESIAN_POINT('Ctrl Pts',(65.0282901388595,249.699071998874,23.2800173665856)) ;
#115780 = CARTESIAN_POINT('Ctrl Pts',(65.0253882410353,249.706274347918,23.2194573524548)) ;
#115781 = CARTESIAN_POINT('Ctrl Pts',(65.0227874089931,249.712729468432,23.1651803121289)) ;
#115782 = CARTESIAN_POINT('Ctrl Pts',(65.0201865769509,249.716519689942,23.1106692791193)) ;
#115783 = CARTESIAN_POINT('Ctrl Pts',(65.0175857449087,249.717652389637,23.0562054289579)) ;
#115784 = CARTESIAN_POINT('Ctrl Pts',(65.0170424059649,249.717889021548,23.0448274044094)) ;
#115785 = CARTESIAN_POINT('Ctrl Pts',(65.0164990670211,249.718009873619,23.0334475707981)) ;
#115786 = CARTESIAN_POINT('Ctrl Pts',(65.0159557280773,249.718014941427,23.0220674831853)) ;
#115787 = CARTESIAN_POINT('Origin',(64.9402651077866,248.040265107786,23.0213203435596)) ;
#115788 = CARTESIAN_POINT('Ctrl Pts',(64.9402651077867,248.926035539849,24.7736739014023)) ;
#115789 = CARTESIAN_POINT('Ctrl Pts',(64.9402651077866,248.976878141234,24.7437902125892)) ;
#115790 = CARTESIAN_POINT('Ctrl Pts',(64.9402651077866,249.026203795482,24.711570348078)) ;
#115791 = CARTESIAN_POINT('Ctrl Pts',(64.9402651077867,249.073820527419,24.6770177952892)) ;
#115792 = CARTESIAN_POINT('Ctrl Pts',(64.9402651077868,249.08462711755,24.6691761131584)) ;
#115793 = CARTESIAN_POINT('Ctrl Pts',(64.9402651077867,249.09534559418,24.6612141692458)) ;
#115794 = CARTESIAN_POINT('Ctrl Pts',(64.9402651077867,249.10597357269,24.6531318456028)) ;
#115795 = CARTESIAN_POINT('Ctrl Pts',(64.9402651077866,249.166471971025,24.6071242596107)) ;
#115796 = CARTESIAN_POINT('Ctrl Pts',(64.9402651077868,249.224042137625,24.5572188157012)) ;
#115797 = CARTESIAN_POINT('Ctrl Pts',(64.9402651077867,249.278496460635,24.5038024082393)) ;
#115798 = CARTESIAN_POINT('Ctrl Pts',(64.9402651077867,249.292324750794,24.4902376893917)) ;
#115799 = CARTESIAN_POINT('Ctrl Pts',(64.9402651077866,249.305954881182,24.4764429964786)) ;
#115800 = CARTESIAN_POINT('Ctrl Pts',(64.9402651077866,249.319363494654,24.4624456517121)) ;
#115801 = CARTESIAN_POINT('Ctrl Pts',(64.9402651077865,249.369335690605,24.410279329152)) ;
#115802 = CARTESIAN_POINT('Ctrl Pts',(64.9402651077867,249.416286779042,24.3552521689592)) ;
#115803 = CARTESIAN_POINT('Ctrl Pts',(64.9402651077868,249.460076530841,24.2977130577074)) ;
#115804 = CARTESIAN_POINT('Ctrl Pts',(64.9402651077868,249.493619627768,24.2536379052686)) ;
#115805 = CARTESIAN_POINT('Ctrl Pts',(64.9402651077866,249.525306996186,24.2080879408986)) ;
#115806 = CARTESIAN_POINT('Ctrl Pts',(64.9402651077865,249.555057167624,24.1612106694906)) ;
#115807 = CARTESIAN_POINT('Ctrl Pts',(64.9402651077865,249.566305768275,24.1434862773203)) ;
#115808 = CARTESIAN_POINT('Ctrl Pts',(64.9402651077866,249.577277252061,24.1255720746347)) ;
#115809 = CARTESIAN_POINT('Ctrl Pts',(64.9402651077866,249.587966566315,24.1074758724398)) ;
#115810 = CARTESIAN_POINT('Ctrl Pts',(64.9402651077865,249.597031260778,24.0921300289246)) ;
#115811 = CARTESIAN_POINT('Ctrl Pts',(64.9402651077867,249.605895515243,24.0766485406753)) ;
#115812 = CARTESIAN_POINT('Ctrl Pts',(64.9402651077867,249.61454108935,24.0610639553866)) ;
#115813 = CARTESIAN_POINT('Ctrl Pts',(64.9402651077866,249.649154760442,23.9986690579923)) ;
#115814 = CARTESIAN_POINT('Ctrl Pts',(64.9402651077868,249.680311264252,23.9345528731401)) ;
#115815 = CARTESIAN_POINT('Ctrl Pts',(64.9402651077867,249.707874303453,23.8690437513651)) ;
#115816 = CARTESIAN_POINT('Ctrl Pts',(64.9402651077867,249.734984622184,23.8046106110963)) ;
#115817 = CARTESIAN_POINT('Ctrl Pts',(64.9402651077868,249.758618760034,23.7388289129817)) ;
#115818 = CARTESIAN_POINT('Ctrl Pts',(64.9402651077867,249.778599553308,23.6719980103639)) ;
#115819 = CARTESIAN_POINT('Ctrl Pts',(64.9402651077866,249.793454839143,23.6223106857726)) ;
#115820 = CARTESIAN_POINT('Ctrl Pts',(64.9402651077868,249.806289760678,23.5720430656005)) ;
#115821 = CARTESIAN_POINT('Ctrl Pts',(64.9402651077867,249.817012969291,23.52131816757)) ;
#115822 = CARTESIAN_POINT('Ctrl Pts',(64.9402651077867,249.823067203089,23.492679314856)) ;
#115823 = CARTESIAN_POINT('Ctrl Pts',(64.9402651077865,249.828448004765,23.4638947217814)) ;
#115824 = CARTESIAN_POINT('Ctrl Pts',(64.9402651077865,249.833136547529,23.4349869551096)) ;
#115825 = CARTESIAN_POINT('Ctrl Pts',(64.9402651077865,249.83508243226,23.4229893719325)) ;
#115826 = CARTESIAN_POINT('Ctrl Pts',(64.9402651077869,249.836909364897,23.4109683655323)) ;
#115827 = CARTESIAN_POINT('Ctrl Pts',(64.9402651077869,249.838614913707,23.3989326615467)) ;
#115828 = CARTESIAN_POINT('Ctrl Pts',(64.9402651077868,249.848169345995,23.3315090158141)) ;
#115829 = CARTESIAN_POINT('Ctrl Pts',(64.9402651077869,249.853889383611,23.2638409901629)) ;
#115830 = CARTESIAN_POINT('Ctrl Pts',(64.9402651077868,249.855620926811,23.1962106757776)) ;
#115831 = CARTESIAN_POINT('Ctrl Pts',(64.9402651077867,249.856792844341,23.1504381238818)) ;
#115832 = CARTESIAN_POINT('Ctrl Pts',(64.9402651077866,249.856136765347,23.1046826723625)) ;
#115833 = CARTESIAN_POINT('Ctrl Pts',(64.9402651077866,249.853591307226,23.0590325880763)) ;
#115834 = CARTESIAN_POINT('Ctrl Pts',(64.9402651077865,249.849670880286,22.9887239003222)) ;
#115835 = CARTESIAN_POINT('Ctrl Pts',(64.9402651077867,249.841270878845,22.9186637285971)) ;
#115836 = CARTESIAN_POINT('Ctrl Pts',(64.9402651077868,249.82857851078,22.8491862645525)) ;
#115837 = CARTESIAN_POINT('Ctrl Pts',(64.9402651077869,249.823025599751,22.818789874033)) ;
#115838 = CARTESIAN_POINT('Ctrl Pts',(64.9402651077869,249.816650415106,22.7885053138842)) ;
#115839 = CARTESIAN_POINT('Ctrl Pts',(64.9402651077867,249.809465657346,22.7583623017282)) ;
#115840 = CARTESIAN_POINT('Ctrl Pts',(64.9402651077866,249.806390130223,22.7454592012243)) ;
#115841 = CARTESIAN_POINT('Ctrl Pts',(64.9402651077867,249.803166237982,22.7325820535054)) ;
#115842 = CARTESIAN_POINT('Ctrl Pts',(64.9402651077868,249.799794886782,22.7197332657928)) ;
#115843 = CARTESIAN_POINT('Ctrl Pts',(64.9402651077868,249.796887514073,22.7086527783227)) ;
#115844 = CARTESIAN_POINT('Ctrl Pts',(64.9402651077868,249.793870437363,22.6975935970397)) ;
#115845 = CARTESIAN_POINT('Ctrl Pts',(64.9402651077868,249.790748373431,22.6865709478748)) ;
#115846 = CARTESIAN_POINT('Ctrl Pts',(64.9402651077867,249.772317375906,22.6214991159499)) ;
#115847 = CARTESIAN_POINT('Ctrl Pts',(64.9402651077867,249.750200212747,22.5575763668043)) ;
#115848 = CARTESIAN_POINT('Ctrl Pts',(64.9402651077867,249.724600278997,22.4950834172018)) ;
#115849 = CARTESIAN_POINT('Ctrl Pts',(64.9402651077867,249.698928372785,22.4324147729458)) ;
#115850 = CARTESIAN_POINT('Ctrl Pts',(64.9402651077868,249.66975345666,22.3711830743851)) ;
#115851 = CARTESIAN_POINT('Ctrl Pts',(64.9402651077868,249.637235007895,22.3116966832185)) ;
#115852 = CARTESIAN_POINT('Ctrl Pts',(64.9402651077868,249.605225152613,22.2531406682546)) ;
#115853 = CARTESIAN_POINT('Ctrl Pts',(64.9402651077865,249.569974852449,22.1962750527875)) ;
#115854 = CARTESIAN_POINT('Ctrl Pts',(64.9402651077866,249.531601964295,22.1414304652508)) ;
#115855 = CARTESIAN_POINT('Ctrl Pts',(64.9402651077866,249.523894275526,22.1304142235314)) ;
#115856 = CARTESIAN_POINT('Ctrl Pts',(64.9402651077868,249.516060509705,22.1194796620047)) ;
#115857 = CARTESIAN_POINT('Ctrl Pts',(64.9402651077867,249.508101488473,22.1086296820219)) ;
#115858 = CARTESIAN_POINT('Ctrl Pts',(64.9402651077866,249.501173892893,22.0991857728804)) ;
#115859 = CARTESIAN_POINT('Ctrl Pts',(64.9402651077867,249.49415087098,22.0898054003738)) ;
#115860 = CARTESIAN_POINT('Ctrl Pts',(64.9402651077867,249.487043011387,22.0805032570583)) ;
#115861 = CARTESIAN_POINT('Ctrl Pts',(64.9402651077868,249.446920840516,22.0279948783107)) ;
#115862 = CARTESIAN_POINT('Ctrl Pts',(64.9402651077866,249.404026484517,21.9778764926067)) ;
#115863 = CARTESIAN_POINT('Ctrl Pts',(64.9402651077866,249.358515301884,21.9304287169379)) ;
#115864 = CARTESIAN_POINT('Ctrl Pts',(64.9402651077866,249.313732515653,21.8837403324135)) ;
#115865 = CARTESIAN_POINT('Ctrl Pts',(64.9402651077866,249.26641533439,21.8396371047943)) ;
#115866 = CARTESIAN_POINT('Ctrl Pts',(64.9402651077867,249.216681222564,21.7984258204361)) ;
#115867 = CARTESIAN_POINT('Ctrl Pts',(64.9402651077868,249.168600536501,21.758584617834)) ;
#115868 = CARTESIAN_POINT('Ctrl Pts',(64.9402651077867,249.118260356068,21.7214458696138)) ;
#115869 = CARTESIAN_POINT('Ctrl Pts',(64.9402651077866,249.065747227906,21.6873312956639)) ;
#115870 = CARTESIAN_POINT('Ctrl Pts',(64.9402651077866,249.048922193034,21.6764010975127)) ;
#115871 = CARTESIAN_POINT('Ctrl Pts',(64.9402651077868,249.03187397738,21.6657817184762)) ;
#115872 = CARTESIAN_POINT('Ctrl Pts',(64.9402651077866,249.014605129081,21.6554848536838)) ;
#115873 = CARTESIAN_POINT('',(64.9396944788746,247.064665290212,21.6551748675434)) ;
#115874 = CARTESIAN_POINT('Ctrl Pts',(64.9402651077865,247.083045674831,21.643432097121)) ;
#115875 = CARTESIAN_POINT('Ctrl Pts',(64.9400748981492,247.077082473966,21.6475747347883)) ;
#115876 = CARTESIAN_POINT('Ctrl Pts',(64.9398846885119,247.071146166134,21.6517560841535)) ;
#115877 = CARTESIAN_POINT('Ctrl Pts',(64.9396944788746,247.065237251657,21.655975792806)) ;
#115878 = CARTESIAN_POINT('Ctrl Pts',(64.9402651077866,247.06404364217,21.6543968943227)) ;
#115879 = CARTESIAN_POINT('Ctrl Pts',(64.9402651077866,247.007203713347,21.6877084303973)) ;
#115880 = CARTESIAN_POINT('Ctrl Pts',(64.9402651077865,246.952576865232,21.724365095361)) ;
#115881 = CARTESIAN_POINT('Ctrl Pts',(64.9402651077866,246.900517061953,21.7642811845472)) ;
#115882 = CARTESIAN_POINT('Ctrl Pts',(64.9402651077866,246.894704358926,21.7687379891796)) ;
#115883 = CARTESIAN_POINT('Ctrl Pts',(64.9402651077864,246.888923672635,21.7732354797134)) ;
#115884 = CARTESIAN_POINT('Ctrl Pts',(64.9402651077864,246.883175508364,21.7777735755836)) ;
#115885 = CARTESIAN_POINT('Ctrl Pts',(64.9402651077864,246.848492482056,21.8051553432266)) ;
#115886 = CARTESIAN_POINT('Ctrl Pts',(64.9402651077864,246.814992948051,21.8340145353038)) ;
#115887 = CARTESIAN_POINT('Ctrl Pts',(64.9402651077864,246.782700575228,21.8642422611924)) ;
#115888 = CARTESIAN_POINT('Ctrl Pts',(64.9402651077864,246.76387471842,21.8818644669791)) ;
#115889 = CARTESIAN_POINT('Ctrl Pts',(64.9402651077867,246.745459251001,21.8999519959579)) ;
#115890 = CARTESIAN_POINT('Ctrl Pts',(64.9402651077865,246.727459923415,21.9184848035206)) ;
#115891 = CARTESIAN_POINT('Ctrl Pts',(64.9402651077864,246.717725176082,21.9285080778969)) ;
#115892 = CARTESIAN_POINT('Ctrl Pts',(64.9402651077866,246.708111935049,21.9386620458343)) ;
#115893 = CARTESIAN_POINT('Ctrl Pts',(64.9402651077866,246.698631593824,21.9489318831291)) ;
#115894 = CARTESIAN_POINT('Ctrl Pts',(64.9402651077866,246.654113902873,21.9971568817832)) ;
#115895 = CARTESIAN_POINT('Ctrl Pts',(64.9402651077864,246.612466101452,22.0479919890593)) ;
#115896 = CARTESIAN_POINT('Ctrl Pts',(64.9402651077865,246.573755852033,22.1010784736613)) ;
#115897 = CARTESIAN_POINT('Ctrl Pts',(64.9402651077866,246.542635674679,22.1437560807737)) ;
#115898 = CARTESIAN_POINT('Ctrl Pts',(64.9402651077864,246.513414425502,22.1878899252643)) ;
#115899 = CARTESIAN_POINT('Ctrl Pts',(64.9402651077866,246.486142358642,22.2333127807452)) ;
#115900 = CARTESIAN_POINT('Ctrl Pts',(64.9402651077866,246.476976048295,22.2485796834088)) ;
#115901 = CARTESIAN_POINT('Ctrl Pts',(64.9402651077866,246.468030056022,22.26399232338)) ;
#115902 = CARTESIAN_POINT('Ctrl Pts',(64.9402651077866,246.45930668306,22.2795446899308)) ;
#115903 = CARTESIAN_POINT('Ctrl Pts',(64.9402651077867,246.451879243981,22.2927866154568)) ;
#115904 = CARTESIAN_POINT('Ctrl Pts',(64.9402651077865,246.444612289006,22.3061318511815)) ;
#115905 = CARTESIAN_POINT('Ctrl Pts',(64.9402651077866,246.437517831176,22.3195560702723)) ;
#115906 = CARTESIAN_POINT('Ctrl Pts',(64.9402651077867,246.405909948836,22.3793648883246)) ;
#115907 = CARTESIAN_POINT('Ctrl Pts',(64.9402651077867,246.377673843717,22.4408238708802)) ;
#115908 = CARTESIAN_POINT('Ctrl Pts',(64.9402651077867,246.352882265298,22.5035718480605)) ;
#115909 = CARTESIAN_POINT('Ctrl Pts',(64.9402651077867,246.327697168515,22.5673158280324)) ;
#115910 = CARTESIAN_POINT('Ctrl Pts',(64.9402651077866,246.30606621932,22.6323909223172)) ;
#115911 = CARTESIAN_POINT('Ctrl Pts',(64.9402651077865,246.288105482506,22.6984537994672)) ;
#115912 = CARTESIAN_POINT('Ctrl Pts',(64.9402651077864,246.274905996492,22.7470039247776)) ;
#115913 = CARTESIAN_POINT('Ctrl Pts',(64.9402651077866,246.26368954438,22.7960883480033)) ;
#115914 = CARTESIAN_POINT('Ctrl Pts',(64.9402651077865,246.25451844377,22.8455783499823)) ;
#115915 = CARTESIAN_POINT('Ctrl Pts',(64.9402651077865,246.249295136931,22.8737648759862)) ;
#115916 = CARTESIAN_POINT('Ctrl Pts',(64.9402651077866,246.244735556015,22.9020830550201)) ;
#115917 = CARTESIAN_POINT('Ctrl Pts',(64.9402651077864,246.240853456109,22.9305095743852)) ;
#115918 = CARTESIAN_POINT('Ctrl Pts',(64.9402651077864,246.238895922423,22.9448435355323)) ;
#115919 = CARTESIAN_POINT('Ctrl Pts',(64.9402651077865,246.23711043215,22.9592083501525)) ;
#115920 = CARTESIAN_POINT('Ctrl Pts',(64.9402651077865,246.23550138577,22.9735755832766)) ;
#115921 = CARTESIAN_POINT('Ctrl Pts',(64.9402651077866,246.227718516974,23.0430690992986)) ;
#115922 = CARTESIAN_POINT('Ctrl Pts',(64.9402651077865,246.224042287029,23.1127331202832)) ;
#115923 = CARTESIAN_POINT('Ctrl Pts',(64.9402651077865,246.224580256665,23.1822119780025)) ;
#115924 = CARTESIAN_POINT('Ctrl Pts',(64.9402651077864,246.224872323712,23.2199324800773)) ;
#115925 = CARTESIAN_POINT('Ctrl Pts',(64.9402651077866,246.226407295656,23.2575988579456)) ;
#115926 = CARTESIAN_POINT('Ctrl Pts',(64.9402651077866,246.229208441131,23.2951564187047)) ;
#115927 = CARTESIAN_POINT('Ctrl Pts',(64.9402651077865,246.234233948422,23.3625380656402)) ;
#115928 = CARTESIAN_POINT('Ctrl Pts',(64.9402651077864,246.24333176806,23.4295696364802)) ;
#115929 = CARTESIAN_POINT('Ctrl Pts',(64.9402651077864,246.256283967996,23.4960087497214)) ;
#115930 = CARTESIAN_POINT('Ctrl Pts',(64.9402651077863,246.262795924935,23.5294122369009)) ;
#115931 = CARTESIAN_POINT('Ctrl Pts',(64.9402651077864,246.270283012217,23.5626659794887)) ;
#115932 = CARTESIAN_POINT('Ctrl Pts',(64.9402651077865,246.27872235646,23.5957387507467)) ;
#115933 = CARTESIAN_POINT('Ctrl Pts',(64.9402651077865,246.282866147924,23.611977769237)) ;
#115934 = CARTESIAN_POINT('Ctrl Pts',(64.9402651077863,246.287239565845,23.6281731490293)) ;
#115935 = CARTESIAN_POINT('Ctrl Pts',(64.9402651077864,246.291840169129,23.6443211300255)) ;
#115936 = CARTESIAN_POINT('Ctrl Pts',(64.9402651077864,246.29470680334,23.6543829310353)) ;
#115937 = CARTESIAN_POINT('Ctrl Pts',(64.9402651077863,246.297660952432,23.6644237151454)) ;
#115938 = CARTESIAN_POINT('Ctrl Pts',(64.9402651077864,246.300699298176,23.6744344455488)) ;
#115939 = CARTESIAN_POINT('Ctrl Pts',(64.9402651077866,246.320915032361,23.7410411723224)) ;
#115940 = CARTESIAN_POINT('Ctrl Pts',(64.9402651077867,246.344883302498,23.8064223337815)) ;
#115941 = CARTESIAN_POINT('Ctrl Pts',(64.9402651077867,246.372338922461,23.8703257415957)) ;
#115942 = CARTESIAN_POINT('Ctrl Pts',(64.9402651077867,246.400335511009,23.9354882627066)) ;
#115943 = CARTESIAN_POINT('Ctrl Pts',(64.9402651077864,246.43195851161,23.9991150988841)) ;
#115944 = CARTESIAN_POINT('Ctrl Pts',(64.9402651077865,246.466981592319,24.0609347791762)) ;
#115945 = CARTESIAN_POINT('Ctrl Pts',(64.9402651077866,246.502167767235,24.1230423391028)) ;
#115946 = CARTESIAN_POINT('Ctrl Pts',(64.9402651077864,246.540786197948,24.1833268110854)) ;
#115947 = CARTESIAN_POINT('Ctrl Pts',(64.9402651077867,246.582656540073,24.2414951008919)) ;
#115948 = CARTESIAN_POINT('Ctrl Pts',(64.9402651077868,246.592936185813,24.2557760783621)) ;
#115949 = CARTESIAN_POINT('Ctrl Pts',(64.9402651077867,246.603412056763,24.2699293792961)) ;
#115950 = CARTESIAN_POINT('Ctrl Pts',(64.9402651077867,246.614081887465,24.2839504011325)) ;
#115951 = CARTESIAN_POINT('Ctrl Pts',(64.9402651077867,246.622719436239,24.2953008398928)) ;
#115952 = CARTESIAN_POINT('Ctrl Pts',(64.9402651077867,246.631485589334,24.3065662771629)) ;
#115953 = CARTESIAN_POINT('Ctrl Pts',(64.9402651077867,246.640364653424,24.3177264676288)) ;
#115954 = CARTESIAN_POINT('Ctrl Pts',(64.9402651077865,246.685954500382,24.3750288330827)) ;
#115955 = CARTESIAN_POINT('Ctrl Pts',(64.9402651077868,246.734594144709,24.4296616563077)) ;
#115956 = CARTESIAN_POINT('Ctrl Pts',(64.9402651077866,246.786040477115,24.4813467612197)) ;
#115957 = CARTESIAN_POINT('Ctrl Pts',(64.9402651077865,246.837430222288,24.5329750162671)) ;
#115958 = CARTESIAN_POINT('Ctrl Pts',(64.9402651077866,246.891621013889,24.5816629683342)) ;
#115959 = CARTESIAN_POINT('Ctrl Pts',(64.9402651077867,246.948416932819,24.6271104818581)) ;
#115960 = CARTESIAN_POINT('Ctrl Pts',(64.9402651077868,247.003811560799,24.6714366966933)) ;
#115961 = CARTESIAN_POINT('Ctrl Pts',(64.9402651077867,247.061684973714,24.7126811411786)) ;
#115962 = CARTESIAN_POINT('Ctrl Pts',(64.9402651077867,247.121890830459,24.7505314348811)) ;
#115963 = CARTESIAN_POINT('Ctrl Pts',(64.9402651077867,247.143744240579,24.7642702642267)) ;
#115964 = CARTESIAN_POINT('Ctrl Pts',(64.9402651077866,247.165905256939,24.777561520028)) ;
#115965 = CARTESIAN_POINT('Ctrl Pts',(64.9402651077866,247.188367839728,24.7903888257487)) ;
#115966 = CARTESIAN_POINT('Ctrl Pts',(67.1068977162686,248.766941441459,24.5303522971223)) ;
#115967 = CARTESIAN_POINT('Ctrl Pts',(67.0811241705612,249.255686601031,24.2949964189254)) ;
#115968 = CARTESIAN_POINT('Ctrl Pts',(67.0295770791465,249.979311447899,23.3159220295678)) ;
#115969 = CARTESIAN_POINT('Ctrl Pts',(66.9522564420243,249.378048699798,21.5837974034299)) ;
#115970 = CARTESIAN_POINT('Ctrl Pts',(66.8749358049021,247.607584691196,21.1069207281648)) ;
#115971 = CARTESIAN_POINT('Ctrl Pts',(66.7976151677799,246.21545175278,22.298523800085)) ;
#115972 = CARTESIAN_POINT('Ctrl Pts',(66.7202945306578,246.414252996263,24.1208760392277)) ;
#115973 = CARTESIAN_POINT('Ctrl Pts',(66.6429738935356,248.031328286107,24.9840872012945)) ;
#115974 = CARTESIAN_POINT('Ctrl Pts',(66.5656532564134,249.656094335495,24.1356422797888)) ;
#115975 = CARTESIAN_POINT('Ctrl Pts',(66.4883326192912,249.871729536703,22.315345749206)) ;
#115976 = CARTESIAN_POINT('Ctrl Pts',(66.4110119821691,248.490108895369,21.1107541100679)) ;
#115977 = CARTESIAN_POINT('Ctrl Pts',(66.3336913450469,246.71618583806,21.5723731211514)) ;
#115978 = CARTESIAN_POINT('Ctrl Pts',(66.2563707079247,246.096997993504,23.2976342270491)) ;
#115979 = CARTESIAN_POINT('Ctrl Pts',(66.1790500708025,247.172550498697,24.7819180094862)) ;
#115980 = CARTESIAN_POINT('Ctrl Pts',(66.1017294336803,249.004842624028,24.7307717823553)) ;
#115981 = CARTESIAN_POINT('Ctrl Pts',(66.0244087965582,249.995919764197,23.1887994578465)) ;
#115982 = CARTESIAN_POINT('Ctrl Pts',(65.947088159436,249.281455006808,21.5007672727967)) ;
#115983 = CARTESIAN_POINT('Ctrl Pts',(65.8697675223138,247.484539411195,21.1388215429649)) ;
#115984 = CARTESIAN_POINT('Ctrl Pts',(65.7924468851916,246.172275648143,22.4186165868738)) ;
#115985 = CARTESIAN_POINT('Ctrl Pts',(65.7151262480695,246.489101665562,24.2240364120271)) ;
#115986 = CARTESIAN_POINT('Ctrl Pts',(65.6378056109473,248.158705508057,24.9805535194141)) ;
#115987 = CARTESIAN_POINT('Ctrl Pts',(65.5604849738251,249.725024728806,24.0284187010416)) ;
#115988 = CARTESIAN_POINT('Ctrl Pts',(65.483164336703,249.822034046853,22.1979632409268)) ;
#115989 = CARTESIAN_POINT('Ctrl Pts',(65.4058436995807,248.365187254194,21.0856139599938)) ;
#115990 = CARTESIAN_POINT('Ctrl Pts',(65.3285230624586,246.624886709414,21.6613048641929)) ;
#115991 = CARTESIAN_POINT('Ctrl Pts',(65.2512024253364,246.119126056118,23.4233195575188)) ;
#115992 = CARTESIAN_POINT('Ctrl Pts',(65.1738817882143,247.288380017986,24.8342756772788)) ;
#115993 = CARTESIAN_POINT('Ctrl Pts',(65.0965611510921,249.114147404527,24.6653744652968)) ;
#115994 = CARTESIAN_POINT('Ctrl Pts',(65.0192317351474,250.001268617604,23.0605218282742)) ;
#115995 = CARTESIAN_POINT('Ctrl Pts',(64.96767586491,249.454365413351,21.9724776872887)) ;
#115996 = CARTESIAN_POINT('Ctrl Pts',(64.9418935403801,249.012489323783,21.6574963150814)) ;
#115997 = CARTESIAN_POINT('Ctrl Pts',(67.0508752479159,248.8090411595,24.6177774915559)) ;
#115998 = CARTESIAN_POINT('Ctrl Pts',(67.0251017022085,249.326101584699,24.3687863597358)) ;
#115999 = CARTESIAN_POINT('Ctrl Pts',(66.9735546107937,250.091649362878,23.3329896666175)) ;
#116000 = CARTESIAN_POINT('Ctrl Pts',(66.8962339736716,249.455552685294,21.5005150565937)) ;
#116001 = CARTESIAN_POINT('Ctrl Pts',(66.8189133365494,247.58251751521,20.9960107118432)) ;
#116002 = CARTESIAN_POINT('Ctrl Pts',(66.7415926994272,246.109731882509,22.2566488562179)) ;
#116003 = CARTESIAN_POINT('Ctrl Pts',(66.664272062305,246.320050600704,24.1845783818171)) ;
#116004 = CARTESIAN_POINT('Ctrl Pts',(66.5869514251829,248.03081053473,25.097799355474)) ;
#116005 = CARTESIAN_POINT('Ctrl Pts',(66.5096307880607,249.749706789539,24.2002000989301)) ;
#116006 = CARTESIAN_POINT('Ctrl Pts',(66.4323101509385,249.977834734421,22.2744453785871)) ;
#116007 = CARTESIAN_POINT('Ctrl Pts',(66.3549895138164,248.516170424749,21.0000661792743)) ;
#116008 = CARTESIAN_POINT('Ctrl Pts',(66.2776688766941,246.639475807283,21.4884289128503)) ;
#116009 = CARTESIAN_POINT('Ctrl Pts',(66.200348239572,245.984415549573,23.3136423671894)) ;
#116010 = CARTESIAN_POINT('Ctrl Pts',(66.1230276024498,247.122279781611,24.8839175681433)) ;
#116011 = CARTESIAN_POINT('Ctrl Pts',(66.0457069653276,249.060725056939,24.8298082037237)) ;
#116012 = CARTESIAN_POINT('Ctrl Pts',(65.9683863282055,250.109219875687,23.1985022968723)) ;
#116013 = CARTESIAN_POINT('Ctrl Pts',(65.8910656910833,249.353362873302,21.4126746068038)) ;
#116014 = CARTESIAN_POINT('Ctrl Pts',(65.8137450539611,247.452343653537,21.029759688261)) ;
#116015 = CARTESIAN_POINT('Ctrl Pts',(65.7364244168389,246.06405438661,22.3836991731043)) ;
#116016 = CARTESIAN_POINT('Ctrl Pts',(65.6591037797168,246.399235599297,24.2937153117255)) ;
#116017 = CARTESIAN_POINT('Ctrl Pts',(65.5817831425946,248.165567307768,25.0940609510727)) ;
#116018 = CARTESIAN_POINT('Ctrl Pts',(65.5044625054724,249.822630639067,24.0867645627768)) ;
#116019 = CARTESIAN_POINT('Ctrl Pts',(65.4271418683502,249.925260155198,22.1502623591688)) ;
#116020 = CARTESIAN_POINT('Ctrl Pts',(65.3498212312281,248.384011495629,20.9734695441316)) ;
#116021 = CARTESIAN_POINT('Ctrl Pts',(65.2725005941059,246.542887298214,21.5825128827272)) ;
#116022 = CARTESIAN_POINT('Ctrl Pts',(65.1951799569837,246.00782559311,23.4466092296557)) ;
#116023 = CARTESIAN_POINT('Ctrl Pts',(65.1178593198615,247.244819840209,24.9393085575803)) ;
#116024 = CARTESIAN_POINT('Ctrl Pts',(65.0405386827393,249.176362368478,24.7606221178815)) ;
#116025 = CARTESIAN_POINT('Ctrl Pts',(64.9632092667947,250.11487861289,23.0627929514371)) ;
#116026 = CARTESIAN_POINT('Ctrl Pts',(64.9116533965574,249.536290778729,21.9117133854207)) ;
#116027 = CARTESIAN_POINT('Ctrl Pts',(64.8858710720275,249.068814765345,21.578483686766)) ;
#116028 = CARTESIAN_POINT('Ctrl Pts',(66.9948527795633,248.851140877543,24.7052026859895)) ;
#116029 = CARTESIAN_POINT('Ctrl Pts',(66.9690792338559,249.396516568368,24.4425763005461)) ;
#116030 = CARTESIAN_POINT('Ctrl Pts',(66.9175321424411,250.203987277857,23.3500573036672)) ;
#116031 = CARTESIAN_POINT('Ctrl Pts',(66.840211505319,249.53305667079,21.4172327097574)) ;
#116032 = CARTESIAN_POINT('Ctrl Pts',(66.7628908681968,247.557450339225,20.8851006955216)) ;
#116033 = CARTESIAN_POINT('Ctrl Pts',(66.6855702310746,246.004012012238,22.2147739123507)) ;
#116034 = CARTESIAN_POINT('Ctrl Pts',(66.6082495939524,246.225848205145,24.2482807244066)) ;
#116035 = CARTESIAN_POINT('Ctrl Pts',(66.5309289568302,248.030292783352,25.2115115096535)) ;
#116036 = CARTESIAN_POINT('Ctrl Pts',(66.4536083197081,249.843319243583,24.2647579180714)) ;
#116037 = CARTESIAN_POINT('Ctrl Pts',(66.3762876825859,250.08393993214,22.2335450079682)) ;
#116038 = CARTESIAN_POINT('Ctrl Pts',(66.2989670454638,248.54223195413,20.8893782484808)) ;
#116039 = CARTESIAN_POINT('Ctrl Pts',(66.2216464083415,246.562765776506,21.4044847045491)) ;
#116040 = CARTESIAN_POINT('Ctrl Pts',(66.1443257712194,245.871833105641,23.3296505073297)) ;
#116041 = CARTESIAN_POINT('Ctrl Pts',(66.0670051340972,247.072009064524,24.9859171268005)) ;
#116042 = CARTESIAN_POINT('Ctrl Pts',(65.989684496975,249.116607489848,24.9288446250921)) ;
#116043 = CARTESIAN_POINT('Ctrl Pts',(65.9123638598528,250.222519987177,23.208205135898)) ;
#116044 = CARTESIAN_POINT('Ctrl Pts',(65.8350432227307,249.425270739795,21.3245819408107)) ;
#116045 = CARTESIAN_POINT('Ctrl Pts',(65.7577225856085,247.420147895879,20.9206978335572)) ;
#116046 = CARTESIAN_POINT('Ctrl Pts',(65.6804019484863,245.955833125076,22.3487817593347)) ;
#116047 = CARTESIAN_POINT('Ctrl Pts',(65.6030813113641,246.309369533032,24.3633942114241)) ;
#116048 = CARTESIAN_POINT('Ctrl Pts',(65.525760674242,248.172429107479,25.2075683827315)) ;
#116049 = CARTESIAN_POINT('Ctrl Pts',(65.4484400371198,249.920236549329,24.1451104245121)) ;
#116050 = CARTESIAN_POINT('Ctrl Pts',(65.3711193999976,250.028486263541,22.1025614774108)) ;
#116051 = CARTESIAN_POINT('Ctrl Pts',(65.2937987628754,248.402835737063,20.8613251282695)) ;
#116052 = CARTESIAN_POINT('Ctrl Pts',(65.2164781257533,246.460887887013,21.5037209012614)) ;
#116053 = CARTESIAN_POINT('Ctrl Pts',(65.1391574886311,245.896525130101,23.4698989017926)) ;
#116054 = CARTESIAN_POINT('Ctrl Pts',(65.0618368515089,247.201259662433,25.044341437882)) ;
#116055 = CARTESIAN_POINT('Ctrl Pts',(64.9845162143867,249.238577332429,24.8558697704663)) ;
#116056 = CARTESIAN_POINT('Ctrl Pts',(64.907186798442,250.228488608176,23.0650640745999)) ;
#116057 = CARTESIAN_POINT('Ctrl Pts',(64.8556309282047,249.618216144106,21.8509490835528)) ;
#116058 = CARTESIAN_POINT('Ctrl Pts',(64.8298486036748,249.125140206909,21.4994710584505)) ;
#116059 = CARTESIAN_POINT('Ctrl Pts',(66.9388303112106,248.893240595586,24.7926278804231)) ;
#116060 = CARTESIAN_POINT('Ctrl Pts',(66.9130567655032,249.466931552037,24.5163662413563)) ;
#116061 = CARTESIAN_POINT('Ctrl Pts',(66.8615096740885,250.316325192836,23.3671249407168)) ;
#116062 = CARTESIAN_POINT('Ctrl Pts',(66.7841890369662,249.610560656286,21.3339503629212)) ;
#116063 = CARTESIAN_POINT('Ctrl Pts',(66.7068683998441,247.532383163238,20.7741906792)) ;
#116064 = CARTESIAN_POINT('Ctrl Pts',(66.6295477627219,245.898292141966,22.1728989684836)) ;
#116065 = CARTESIAN_POINT('Ctrl Pts',(66.5522271255997,246.131645809585,24.3119830669961)) ;
#116066 = CARTESIAN_POINT('Ctrl Pts',(66.4749064884777,248.029775031975,25.3252236638329)) ;
#116067 = CARTESIAN_POINT('Ctrl Pts',(66.3975858513554,249.936931697627,24.3293157372126)) ;
#116068 = CARTESIAN_POINT('Ctrl Pts',(66.3202652142332,250.190045129858,22.1926446373492)) ;
#116069 = CARTESIAN_POINT('Ctrl Pts',(66.2429445771111,248.568293483511,20.7786903176872)) ;
#116070 = CARTESIAN_POINT('Ctrl Pts',(66.1656239399888,246.486055745729,21.3205404962479)) ;
#116071 = CARTESIAN_POINT('Ctrl Pts',(66.0883033028667,245.75925066171,23.3456586474699)) ;
#116072 = CARTESIAN_POINT('Ctrl Pts',(66.0109826657445,247.021738347437,25.0879166854576)) ;
#116073 = CARTESIAN_POINT('Ctrl Pts',(65.9336620286223,249.172489922758,25.0278810464605)) ;
#116074 = CARTESIAN_POINT('Ctrl Pts',(65.8563413915001,250.335820098668,23.2179079749237)) ;
#116075 = CARTESIAN_POINT('Ctrl Pts',(65.7790207543779,249.497178606289,21.2364892748176)) ;
#116076 = CARTESIAN_POINT('Ctrl Pts',(65.7017001172558,247.387952138219,20.8116359788532)) ;
#116077 = CARTESIAN_POINT('Ctrl Pts',(65.6243794801336,245.847611863543,22.313864345565)) ;
#116078 = CARTESIAN_POINT('Ctrl Pts',(65.5470588430114,246.219503466767,24.4330731111226)) ;
#116079 = CARTESIAN_POINT('Ctrl Pts',(65.4697382058892,248.17929090719,25.3210758143902)) ;
#116080 = CARTESIAN_POINT('Ctrl Pts',(65.3924175687671,250.01784245959,24.2034562862473)) ;
#116081 = CARTESIAN_POINT('Ctrl Pts',(65.3150969316449,250.131712371886,22.0548605956528)) ;
#116082 = CARTESIAN_POINT('Ctrl Pts',(65.2377762945227,248.421659978497,20.7491807124074)) ;
#116083 = CARTESIAN_POINT('Ctrl Pts',(65.1604556574006,246.378888475813,21.4249289197957)) ;
#116084 = CARTESIAN_POINT('Ctrl Pts',(65.0831350202784,245.785224667093,23.4931885739294)) ;
#116085 = CARTESIAN_POINT('Ctrl Pts',(65.0058143831562,247.157699484657,25.1493743181835)) ;
#116086 = CARTESIAN_POINT('Ctrl Pts',(64.9284937460341,249.30079229638,24.951117423051)) ;
#116087 = CARTESIAN_POINT('Ctrl Pts',(64.8511643300893,250.342098603462,23.0673351977628)) ;
#116088 = CARTESIAN_POINT('Ctrl Pts',(64.7996084598521,249.700141509485,21.7901847816847)) ;
#116089 = CARTESIAN_POINT('Ctrl Pts',(64.7738261353222,249.181465648471,21.4204584301351)) ;
#116090 = CARTESIAN_POINT('',(66.940838214598,249.015862219827,21.6551782011097)) ;
#116091 = CARTESIAN_POINT('Ctrl Pts',(66.9402651077866,249.016486567286,21.6543968495755)) ;
#116092 = CARTESIAN_POINT('Ctrl Pts',(66.9402651077865,249.073326496225,21.6877083848151)) ;
#116093 = CARTESIAN_POINT('Ctrl Pts',(66.9402651077866,249.127953344347,21.724365048829)) ;
#116094 = CARTESIAN_POINT('Ctrl Pts',(66.9402651077866,249.180013147505,21.764281136914)) ;
#116095 = CARTESIAN_POINT('Ctrl Pts',(66.9402651077866,249.185825850241,21.7687379412113)) ;
#116096 = CARTESIAN_POINT('Ctrl Pts',(66.9402651077866,249.191606536244,21.7732354314043)) ;
#116097 = CARTESIAN_POINT('Ctrl Pts',(66.9402651077866,249.197354700228,21.7777735269277)) ;
#116098 = CARTESIAN_POINT('Ctrl Pts',(66.9402651077867,249.232037725852,21.805155293308)) ;
#116099 = CARTESIAN_POINT('Ctrl Pts',(66.9402651077866,249.265537259157,21.8340144840013)) ;
#116100 = CARTESIAN_POINT('Ctrl Pts',(66.9402651077867,249.297829631273,21.8642422084135)) ;
#116101 = CARTESIAN_POINT('Ctrl Pts',(66.9402651077867,249.316655489125,21.8818644147024)) ;
#116102 = CARTESIAN_POINT('Ctrl Pts',(66.9402651077866,249.335070957522,21.8999519442239)) ;
#116103 = CARTESIAN_POINT('Ctrl Pts',(66.9402651077866,249.353070286022,21.9184847523711)) ;
#116104 = CARTESIAN_POINT('Ctrl Pts',(66.9402651077866,249.362805032771,21.9285080259532)) ;
#116105 = CARTESIAN_POINT('Ctrl Pts',(66.9402651077867,249.372418273226,21.9386619930784)) ;
#116106 = CARTESIAN_POINT('Ctrl Pts',(66.9402651077867,249.381898613883,21.9489318295471)) ;
#116107 = CARTESIAN_POINT('Ctrl Pts',(66.9402651077867,249.426416304368,21.9971568267049)) ;
#116108 = CARTESIAN_POINT('Ctrl Pts',(66.9402651077866,249.468064105244,22.0479919324255)) ;
#116109 = CARTESIAN_POINT('Ctrl Pts',(66.9402651077865,249.506774354067,22.1010784154893)) ;
#116110 = CARTESIAN_POINT('Ctrl Pts',(66.9402651077865,249.537894530784,22.1437560211474)) ;
#116111 = CARTESIAN_POINT('Ctrl Pts',(66.9402651077868,249.567115779311,22.1878898641801)) ;
#116112 = CARTESIAN_POINT('Ctrl Pts',(66.9402651077867,249.594387845524,22.2333127182412)) ;
#116113 = CARTESIAN_POINT('Ctrl Pts',(66.9402651077867,249.60355415791,22.2485796241852)) ;
#116114 = CARTESIAN_POINT('Ctrl Pts',(66.9402651077866,249.612500152114,22.2639922675129)) ;
#116115 = CARTESIAN_POINT('Ctrl Pts',(66.9402651077866,249.621223526897,22.2795446374933)) ;
#116116 = CARTESIAN_POINT('Ctrl Pts',(66.9402651077866,249.628650964169,22.2927865599521)) ;
#116117 = CARTESIAN_POINT('Ctrl Pts',(66.9402651077864,249.635917917401,22.306131792565)) ;
#116118 = CARTESIAN_POINT('Ctrl Pts',(66.9402651077865,249.643012373558,22.3195560085153)) ;
#116119 = CARTESIAN_POINT('Ctrl Pts',(66.9402651077868,249.67462025506,22.379364825088)) ;
#116120 = CARTESIAN_POINT('Ctrl Pts',(66.9402651077865,249.702856359346,22.4408238062802)) ;
#116121 = CARTESIAN_POINT('Ctrl Pts',(66.9402651077866,249.727647936966,22.5035717822936)) ;
#116122 = CARTESIAN_POINT('Ctrl Pts',(66.9402651077866,249.752833032827,22.5673157608029)) ;
#116123 = CARTESIAN_POINT('Ctrl Pts',(66.9402651077865,249.774463981167,22.6323908538163)) ;
#116124 = CARTESIAN_POINT('Ctrl Pts',(66.9402651077865,249.792424717225,22.6984537299751)) ;
#116125 = CARTESIAN_POINT('Ctrl Pts',(66.9402651077865,249.805624202608,22.747003854278)) ;
#116126 = CARTESIAN_POINT('Ctrl Pts',(66.9402651077867,249.816840654164,22.7960882766413)) ;
#116127 = CARTESIAN_POINT('Ctrl Pts',(66.9402651077866,249.82601175431,22.8455782779415)) ;
#116128 = CARTESIAN_POINT('Ctrl Pts',(66.9402651077866,249.831235060844,22.8737648033397)) ;
#116129 = CARTESIAN_POINT('Ctrl Pts',(66.9402651077864,249.835794641495,22.9020829818254)) ;
#116130 = CARTESIAN_POINT('Ctrl Pts',(66.9402651077865,249.839676741179,22.9305095007077)) ;
#116131 = CARTESIAN_POINT('Ctrl Pts',(66.9402651077865,249.841634274688,22.9448434611364)) ;
#116132 = CARTESIAN_POINT('Ctrl Pts',(66.9402651077866,249.843419764806,22.9592082750519)) ;
#116133 = CARTESIAN_POINT('Ctrl Pts',(66.9402651077866,249.845028811054,22.9735755074892)) ;
#116134 = CARTESIAN_POINT('Ctrl Pts',(66.9402651077866,249.852811679582,23.0430690234714)) ;
#116135 = CARTESIAN_POINT('Ctrl Pts',(66.9402651077867,249.856487909412,23.1127330448471)) ;
#116136 = CARTESIAN_POINT('Ctrl Pts',(66.9402651077867,249.855949939848,23.1822119034766)) ;
#116137 = CARTESIAN_POINT('Ctrl Pts',(66.9402651077867,249.85565787284,23.2199324061758)) ;
#116138 = CARTESIAN_POINT('Ctrl Pts',(66.9402651077866,249.854122900981,23.2575987848212)) ;
#116139 = CARTESIAN_POINT('Ctrl Pts',(66.9402651077866,249.851321755643,23.295156346524)) ;
#116140 = CARTESIAN_POINT('Ctrl Pts',(66.9402651077866,249.846296248548,23.3625379958313)) ;
#116141 = CARTESIAN_POINT('Ctrl Pts',(66.9402651077866,249.837198429191,23.429569569572)) ;
#116142 = CARTESIAN_POINT('Ctrl Pts',(66.9402651077864,249.824246229587,23.496008686096)) ;
#116143 = CARTESIAN_POINT('Ctrl Pts',(66.9402651077863,249.817734272897,23.5294121745024)) ;
#116144 = CARTESIAN_POINT('Ctrl Pts',(66.9402651077864,249.810247185901,23.5626659184175)) ;
#116145 = CARTESIAN_POINT('Ctrl Pts',(66.9402651077865,249.801807841976,23.5957386910865)) ;
#116146 = CARTESIAN_POINT('Ctrl Pts',(66.9402651077865,249.797664050485,23.6119777109885)) ;
#116147 = CARTESIAN_POINT('Ctrl Pts',(66.9402651077864,249.793290632525,23.6281730922088)) ;
#116148 = CARTESIAN_POINT('Ctrl Pts',(66.9402651077864,249.788690029188,23.6443210746468)) ;
#116149 = CARTESIAN_POINT('Ctrl Pts',(66.9402651077864,249.785823394845,23.6543828769038)) ;
#116150 = CARTESIAN_POINT('Ctrl Pts',(66.9402651077864,249.782869245611,23.6644236622611)) ;
#116151 = CARTESIAN_POINT('Ctrl Pts',(66.9402651077864,249.779830899714,23.6744343939138)) ;
#116152 = CARTESIAN_POINT('Ctrl Pts',(66.9402651077865,249.759680252296,23.7408266779849)) ;
#116153 = CARTESIAN_POINT('Ctrl Pts',(66.9402651077866,249.735801164671,23.8060012765027)) ;
#116154 = CARTESIAN_POINT('Ctrl Pts',(66.9402651077866,249.708456355635,23.8697084272248)) ;
#116155 = CARTESIAN_POINT('Ctrl Pts',(66.9402651077865,249.680373402716,23.9351352843627)) ;
#116156 = CARTESIAN_POINT('Ctrl Pts',(66.9402651077866,249.648634875389,23.9990152885733)) ;
#116157 = CARTESIAN_POINT('Ctrl Pts',(66.9402651077865,249.613469833398,24.0610737847212)) ;
#116158 = CARTESIAN_POINT('Ctrl Pts',(66.9402651077864,249.578304791407,24.123132280869)) ;
#116159 = CARTESIAN_POINT('Ctrl Pts',(66.9402651077865,249.539712760019,24.1833701962856)) ;
#116160 = CARTESIAN_POINT('Ctrl Pts',(66.9402651077866,249.497873662861,24.2414950835056)) ;
#116161 = CARTESIAN_POINT('Ctrl Pts',(66.9402651077866,249.487594016516,24.255776062901)) ;
#116162 = CARTESIAN_POINT('Ctrl Pts',(66.9402651077866,249.477118144931,24.2699293657298)) ;
#116163 = CARTESIAN_POINT('Ctrl Pts',(66.9402651077867,249.466448313562,24.2839503894272)) ;
#116164 = CARTESIAN_POINT('Ctrl Pts',(66.9402651077867,249.457810767089,24.2953008259602)) ;
#116165 = CARTESIAN_POINT('Ctrl Pts',(66.9402651077867,249.449044616362,24.3065662610333)) ;
#116166 = CARTESIAN_POINT('Ctrl Pts',(66.9402651077867,249.440165554696,24.3177264493437)) ;
#116167 = CARTESIAN_POINT('Ctrl Pts',(66.9402651077865,249.394575708576,24.3750288183199)) ;
#116168 = CARTESIAN_POINT('Ctrl Pts',(66.9402651077866,249.345936065014,24.429661644788)) ;
#116169 = CARTESIAN_POINT('Ctrl Pts',(66.9402651077866,249.294489733256,24.4813467525077)) ;
#116170 = CARTESIAN_POINT('Ctrl Pts',(66.9402651077867,249.243099989585,24.5329750095)) ;
#116171 = CARTESIAN_POINT('Ctrl Pts',(66.9402651077866,249.188909199461,24.5816629631761)) ;
#116172 = CARTESIAN_POINT('Ctrl Pts',(66.9402651077867,249.132113281926,24.6271104778317)) ;
#116173 = CARTESIAN_POINT('Ctrl Pts',(66.9402651077867,249.076718656809,24.6714366925687)) ;
#116174 = CARTESIAN_POINT('Ctrl Pts',(66.9402651077867,249.018845246814,24.7126811366689)) ;
#116175 = CARTESIAN_POINT('Ctrl Pts',(66.9402651077867,248.958639392982,24.7505314295909)) ;
#116176 = CARTESIAN_POINT('Ctrl Pts',(66.9402651077867,248.936785980341,24.764270260903)) ;
#116177 = CARTESIAN_POINT('Ctrl Pts',(66.9402651077868,248.914624961358,24.7775615184723)) ;
#116178 = CARTESIAN_POINT('Ctrl Pts',(66.9402651077866,248.892162375845,24.7903888257488)) ;
#116179 = CARTESIAN_POINT('Ctrl Pts',(66.940838214598,249.015292748841,21.6559756392158)) ;
#116180 = CARTESIAN_POINT('Ctrl Pts',(66.9406471789942,249.009383798495,21.6517559063544)) ;
#116181 = CARTESIAN_POINT('Ctrl Pts',(66.9404561433903,249.003447454475,21.6475745332417)) ;
#116182 = CARTESIAN_POINT('Ctrl Pts',(66.9402651077865,248.99748421711,21.6434318722943)) ;
#116183 = CARTESIAN_POINT('Origin',(66.9402651077866,248.040265107786,23.0213203435596)) ;
#116184 = CARTESIAN_POINT('Ctrl Pts',(66.9402651077866,247.154495177753,24.7736741551652)) ;
#116185 = CARTESIAN_POINT('Ctrl Pts',(66.9402651077866,247.103652956155,24.7437896484996)) ;
#116186 = CARTESIAN_POINT('Ctrl Pts',(66.9402651077865,247.054326565403,24.7115704134065)) ;
#116187 = CARTESIAN_POINT('Ctrl Pts',(66.9402651077866,247.006709671402,24.6770177424811)) ;
#116188 = CARTESIAN_POINT('Ctrl Pts',(66.9402651077866,246.995903081062,24.6691760600765)) ;
#116189 = CARTESIAN_POINT('Ctrl Pts',(66.9402651077867,246.98518460422,24.6612141158822)) ;
#116190 = CARTESIAN_POINT('Ctrl Pts',(66.9402651077867,246.974556625495,24.6531317919492)) ;
#116191 = CARTESIAN_POINT('Ctrl Pts',(66.9402651077867,246.914058226574,24.6071242047902)) ;
#116192 = CARTESIAN_POINT('Ctrl Pts',(66.9402651077865,246.856488059237,24.5572187595307)) ;
#116193 = CARTESIAN_POINT('Ctrl Pts',(66.9402651077866,246.802033735395,24.5038023506277)) ;
#116194 = CARTESIAN_POINT('Ctrl Pts',(66.9402651077866,246.788205445077,24.4902376314661)) ;
#116195 = CARTESIAN_POINT('Ctrl Pts',(66.9402651077866,246.774575314523,24.4764429382347)) ;
#116196 = CARTESIAN_POINT('Ctrl Pts',(66.9402651077866,246.761166700878,24.4624455931476)) ;
#116197 = CARTESIAN_POINT('Ctrl Pts',(66.9402651077867,246.71119450402,24.4102792691181)) ;
#116198 = CARTESIAN_POINT('Ctrl Pts',(66.9402651077868,246.664243414614,24.355252107392)) ;
#116199 = CARTESIAN_POINT('Ctrl Pts',(66.9402651077866,246.620453661835,24.2977129946242)) ;
#116200 = CARTESIAN_POINT('Ctrl Pts',(66.9402651077865,246.586910564207,24.25363784109)) ;
#116201 = CARTESIAN_POINT('Ctrl Pts',(66.9402651077868,246.555223195075,24.208087875639)) ;
#116202 = CARTESIAN_POINT('Ctrl Pts',(66.9402651077866,246.525473022933,24.1612106032007)) ;
#116203 = CARTESIAN_POINT('Ctrl Pts',(66.9402651077865,246.514224422105,24.1434862107816)) ;
#116204 = CARTESIAN_POINT('Ctrl Pts',(66.9402651077867,246.503252938138,24.1255720078574)) ;
#116205 = CARTESIAN_POINT('Ctrl Pts',(66.9402651077867,246.492563623701,24.1074758054361)) ;
#116206 = CARTESIAN_POINT('Ctrl Pts',(66.9402651077868,246.483498928947,24.0921299614971)) ;
#116207 = CARTESIAN_POINT('Ctrl Pts',(66.9402651077866,246.474634674195,24.0766484728284)) ;
#116208 = CARTESIAN_POINT('Ctrl Pts',(66.9402651077865,246.465989099807,24.061063887127)) ;
#116209 = CARTESIAN_POINT('Ctrl Pts',(66.9402651077865,246.43137542783,23.9986689885137)) ;
#116210 = CARTESIAN_POINT('Ctrl Pts',(66.9402651077865,246.40021892318,23.9345528025734)) ;
#116211 = CARTESIAN_POINT('Ctrl Pts',(66.9402651077865,246.372655883232,23.8690436799177)) ;
#116212 = CARTESIAN_POINT('Ctrl Pts',(66.9402651077865,246.345545564146,23.8046105396851)) ;
#116213 = CARTESIAN_POINT('Ctrl Pts',(66.9402651077867,246.321911425932,23.7388288418451)) ;
#116214 = CARTESIAN_POINT('Ctrl Pts',(66.9402651077866,246.301930632325,23.6719979398038)) ;
#116215 = CARTESIAN_POINT('Ctrl Pts',(66.9402651077865,246.287075345967,23.6223106147206)) ;
#116216 = CARTESIAN_POINT('Ctrl Pts',(66.9402651077867,246.274240423999,23.572042994202)) ;
#116217 = CARTESIAN_POINT('Ctrl Pts',(66.9402651077865,246.263517215067,23.5213180960051)) ;
#116218 = CARTESIAN_POINT('Ctrl Pts',(66.9402651077864,246.257462981285,23.4926792441283)) ;
#116219 = CARTESIAN_POINT('Ctrl Pts',(66.9402651077865,246.252082179617,23.4638946519576)) ;
#116220 = CARTESIAN_POINT('Ctrl Pts',(66.9402651077865,246.247393636855,23.4349868862611)) ;
#116221 = CARTESIAN_POINT('Ctrl Pts',(66.9402651077865,246.245447752022,23.4229893028557)) ;
#116222 = CARTESIAN_POINT('Ctrl Pts',(66.9402651077865,246.243620819294,23.4109682962387)) ;
#116223 = CARTESIAN_POINT('Ctrl Pts',(66.9402651077865,246.241915270405,23.398932592043)) ;
#116224 = CARTESIAN_POINT('Ctrl Pts',(66.9402651077866,246.232360838049,23.3315089477653)) ;
#116225 = CARTESIAN_POINT('Ctrl Pts',(66.9402651077867,246.226640800444,23.2638409239364)) ;
#116226 = CARTESIAN_POINT('Ctrl Pts',(66.9402651077867,246.22490925737,23.1962106118006)) ;
#116227 = CARTESIAN_POINT('Ctrl Pts',(66.9402651077867,246.223737339853,23.1504380585975)) ;
#116228 = CARTESIAN_POINT('Ctrl Pts',(66.9402651077867,246.224393419138,23.1046826059687)) ;
#116229 = CARTESIAN_POINT('Ctrl Pts',(66.9402651077866,246.226938877851,23.059032520807)) ;
#116230 = CARTESIAN_POINT('Ctrl Pts',(66.9402651077863,246.230859305516,22.98872383506)) ;
#116231 = CARTESIAN_POINT('Ctrl Pts',(66.9402651077865,246.239259307967,22.9186636658731)) ;
#116232 = CARTESIAN_POINT('Ctrl Pts',(66.9402651077866,246.251951677252,22.8491862047465)) ;
#116233 = CARTESIAN_POINT('Ctrl Pts',(66.9402651077867,246.257504588814,22.8187898155036)) ;
#116234 = CARTESIAN_POINT('Ctrl Pts',(66.9402651077866,246.263879774033,22.7885052567041)) ;
#116235 = CARTESIAN_POINT('Ctrl Pts',(66.9402651077865,246.271064532401,22.7583622459574)) ;
#116236 = CARTESIAN_POINT('Ctrl Pts',(66.9402651077865,246.274140059972,22.7454591452704)) ;
#116237 = CARTESIAN_POINT('Ctrl Pts',(66.9402651077867,246.277363952684,22.7325819973825)) ;
#116238 = CARTESIAN_POINT('Ctrl Pts',(66.9402651077866,246.28073530438,22.7197332095146)) ;
#116239 = CARTESIAN_POINT('Ctrl Pts',(66.9402651077864,246.283642677311,22.7086527226913)) ;
#116240 = CARTESIAN_POINT('Ctrl Pts',(66.9402651077864,246.286659754245,22.6975935420638)) ;
#116241 = CARTESIAN_POINT('Ctrl Pts',(66.9402651077865,246.289781818403,22.6865708935598)) ;
#116242 = CARTESIAN_POINT('Ctrl Pts',(66.9402651077866,246.308212817329,22.6214990652872)) ;
#116243 = CARTESIAN_POINT('Ctrl Pts',(66.9402651077864,246.330329981973,22.5575763200012)) ;
#116244 = CARTESIAN_POINT('Ctrl Pts',(66.9402651077865,246.355929917223,22.4950833743233)) ;
#116245 = CARTESIAN_POINT('Ctrl Pts',(66.9402651077867,246.381601825482,22.4324147326794)) ;
#116246 = CARTESIAN_POINT('Ctrl Pts',(66.9402651077865,246.410776743819,22.3711830368571)) ;
#116247 = CARTESIAN_POINT('Ctrl Pts',(66.9402651077865,246.443295194883,22.3116966484315)) ;
#116248 = CARTESIAN_POINT('Ctrl Pts',(66.9402651077865,246.475305053119,22.2531406349017)) ;
#116249 = CARTESIAN_POINT('Ctrl Pts',(66.9402651077865,246.510555356463,22.196275020944)) ;
#116250 = CARTESIAN_POINT('Ctrl Pts',(66.9402651077864,246.54892824794,22.141430434894)) ;
#116251 = CARTESIAN_POINT('Ctrl Pts',(66.9402651077864,246.556635945235,22.1304141822409)) ;
#116252 = CARTESIAN_POINT('Ctrl Pts',(66.9402651077867,246.564469719844,22.1194796099464)) ;
#116253 = CARTESIAN_POINT('Ctrl Pts',(66.9402651077867,246.572428750125,22.1086296193694)) ;
#116254 = CARTESIAN_POINT('Ctrl Pts',(66.9402651077867,246.579356337263,22.0991857232521)) ;
#116255 = CARTESIAN_POINT('Ctrl Pts',(66.9402651077867,246.586379350469,22.0898053636188)) ;
#116256 = CARTESIAN_POINT('Ctrl Pts',(66.9402651077866,246.593487201128,22.0805032329674)) ;
#116257 = CARTESIAN_POINT('Ctrl Pts',(66.9402651077865,246.633609374762,22.0279948560982)) ;
#116258 = CARTESIAN_POINT('Ctrl Pts',(66.9402651077865,246.676503733551,21.977876472155)) ;
#116259 = CARTESIAN_POINT('Ctrl Pts',(66.9402651077865,246.722014918924,21.930428698024)) ;
#116260 = CARTESIAN_POINT('Ctrl Pts',(66.9402651077866,246.766261027012,21.884299832657)) ;
#116261 = CARTESIAN_POINT('Ctrl Pts',(66.9402651077865,246.812981198213,21.8406946224787)) ;
#116262 = CARTESIAN_POINT('Ctrl Pts',(66.9402651077866,246.862061994689,21.7999086912144)) ;
#116263 = CARTESIAN_POINT('Ctrl Pts',(66.9402651077866,246.910681941446,21.7595057240879)) ;
#116264 = CARTESIAN_POINT('Ctrl Pts',(66.9402651077866,246.961618918586,21.7218687438548)) ;
#116265 = CARTESIAN_POINT('Ctrl Pts',(66.9402651077866,247.014783014899,21.6873312777196)) ;
#116266 = CARTESIAN_POINT('Ctrl Pts',(66.9402651077866,247.031608040966,21.6764010859492)) ;
#116267 = CARTESIAN_POINT('Ctrl Pts',(66.9402651077867,247.048656247541,21.665781712902)) ;
#116268 = CARTESIAN_POINT('Ctrl Pts',(66.9402651077866,247.065925086493,21.6554848536835)) ;
#116269 = CARTESIAN_POINT('Ctrl Pts',(67.1066093021096,246.899167654978,21.4205873299757)) ;
#116270 = CARTESIAN_POINT('Ctrl Pts',(67.0808268545257,246.380530910519,21.7902818863321)) ;
#116271 = CARTESIAN_POINT('Ctrl Pts',(67.0292708612343,245.73862285314,23.0673282297465)) ;
#116272 = CARTESIAN_POINT('Ctrl Pts',(66.9519413222356,246.779843576752,24.950955615441)) ;
#116273 = CARTESIAN_POINT('Ctrl Pts',(66.8746206851134,248.922756726385,25.1491958853405)) ;
#116274 = CARTESIAN_POINT('Ctrl Pts',(66.7973000479912,250.295116492069,23.4931490133159)) ;
#116275 = CARTESIAN_POINT('Ctrl Pts',(66.7199794108692,249.701502455305,21.4250627499166)) ;
#116276 = CARTESIAN_POINT('Ctrl Pts',(66.642658773747,247.658902211124,20.7493711995695)) ;
#116277 = CARTESIAN_POINT('Ctrl Pts',(66.5653381366247,245.948993181706,22.0549416187025)) ;
#116278 = CARTESIAN_POINT('Ctrl Pts',(66.4880174995025,246.062853547653,24.2033571811817)) ;
#116279 = CARTESIAN_POINT('Ctrl Pts',(66.4106968623804,247.901250963731,25.3208830123917)) ;
#116280 = CARTESIAN_POINT('Ctrl Pts',(66.3333762252582,249.860874103791,24.4329547557814)) ;
#116281 = CARTESIAN_POINT('Ctrl Pts',(66.256055588136,250.23273452922,22.3139236556595)) ;
#116282 = CARTESIAN_POINT('Ctrl Pts',(66.1787349510139,248.692523390174,20.8118212295067)) ;
#116283 = CARTESIAN_POINT('Ctrl Pts',(66.1014143138918,246.583473750784,21.2366389075348)) ;
#116284 = CARTESIAN_POINT('Ctrl Pts',(66.0240936767696,245.74490256657,23.2178914938439)) ;
#116285 = CARTESIAN_POINT('Ctrl Pts',(65.9467730396473,246.908135213782,25.0277128248629)) ;
#116286 = CARTESIAN_POINT('Ctrl Pts',(65.8694524025251,249.058706479129,25.0877434307034)) ;
#116287 = CARTESIAN_POINT('Ctrl Pts',(65.792131765403,250.321088323227,23.3456314563494)) ;
#116288 = CARTESIAN_POINT('Ctrl Pts',(65.7148111282808,249.59434417144,21.3206830824085)) ;
#116289 = CARTESIAN_POINT('Ctrl Pts',(65.6374904911586,247.51228099978,20.7788783305243)) ;
#116290 = CARTESIAN_POINT('Ctrl Pts',(65.5601698540364,245.890665314093,22.1927141098144)) ;
#116291 = CARTESIAN_POINT('Ctrl Pts',(65.4828492169142,246.143757526522,24.3292060812583)) ;
#116292 = CARTESIAN_POINT('Ctrl Pts',(65.4055285797921,248.050754303577,25.3250305138284)) ;
#116293 = CARTESIAN_POINT('Ctrl Pts',(65.3282079426699,249.948724394557,24.3118748680936)) ;
#116294 = CARTESIAN_POINT('Ctrl Pts',(65.2508873055477,250.182058496545,22.1729700982747)) ;
#116295 = CARTESIAN_POINT('Ctrl Pts',(65.1735666684256,248.548104464289,20.7743790968438)) ;
#116296 = CARTESIAN_POINT('Ctrl Pts',(65.0962460313034,246.470101190474,21.3340918495046)) ;
#116297 = CARTESIAN_POINT('Ctrl Pts',(65.0189253941812,245.764395780262,23.3670960744596)) ;
#116298 = CARTESIAN_POINT('Ctrl Pts',(64.9673783027664,246.613718254765,24.5162409181759)) ;
#116299 = CARTESIAN_POINT('Ctrl Pts',(64.941604757059,247.187361121204,24.7924793994338)) ;
#116300 = CARTESIAN_POINT('Ctrl Pts',(67.0506108178113,246.955468616385,21.4995663929808)) ;
#116301 = CARTESIAN_POINT('Ctrl Pts',(67.0248283702273,246.46242105124,21.8510204748725)) ;
#116302 = CARTESIAN_POINT('Ctrl Pts',(66.973272376936,245.852184294744,23.0650582323697)) ;
#116303 = CARTESIAN_POINT('Ctrl Pts',(66.8959428379373,246.842031905892,24.8557487418266)) ;
#116304 = CARTESIAN_POINT('Ctrl Pts',(66.8186222008151,248.879215198501,25.0442079735181)) ;
#116305 = CARTESIAN_POINT('Ctrl Pts',(66.7413015636929,250.183863679742,23.469869312129)) ;
#116306 = CARTESIAN_POINT('Ctrl Pts',(66.6639809265707,249.619538150188,21.503820998788)) ;
#116307 = CARTESIAN_POINT('Ctrl Pts',(66.5866602894486,247.677718393453,20.86146760357)) ;
#116308 = CARTESIAN_POINT('Ctrl Pts',(66.5093396523264,246.052175096372,22.1026220785603)) ;
#116309 = CARTESIAN_POINT('Ctrl Pts',(66.4320190152043,246.160417670383,24.1450362987605)) ;
#116310 = CARTESIAN_POINT('Ctrl Pts',(66.354698378082,247.908109825732,25.2074241761182)) ;
#116311 = CARTESIAN_POINT('Ctrl Pts',(66.2773777409599,249.771046511443,24.3633056873628)) ;
#116312 = CARTESIAN_POINT('Ctrl Pts',(66.2000571038377,250.12455959992,22.348826120411)) ;
#116313 = CARTESIAN_POINT('Ctrl Pts',(66.1227364667155,248.660341416326,20.9208363920962)) ;
#116314 = CARTESIAN_POINT('Ctrl Pts',(66.0454158295933,246.655350831718,21.3246938588499)) ;
#116315 = CARTESIAN_POINT('Ctrl Pts',(65.9680951924712,245.858154171443,23.2081928088468)) ;
#116316 = CARTESIAN_POINT('Ctrl Pts',(65.890774555349,246.963993722022,24.9287188034683)) ;
#116317 = CARTESIAN_POINT('Ctrl Pts',(65.8134539182268,249.008457284197,24.9857875406145)) ;
#116318 = CARTESIAN_POINT('Ctrl Pts',(65.7361332811046,250.208554078661,23.3296301696934)) ;
#116319 = CARTESIAN_POINT('Ctrl Pts',(65.6588126439825,249.517666982151,21.4045913520933)) ;
#116320 = CARTESIAN_POINT('Ctrl Pts',(65.5814920068603,247.538331371565,20.8895188730319)) ;
#116321 = CARTESIAN_POINT('Ctrl Pts',(65.5041713697381,245.996725085524,22.2335969699703)) ;
#116322 = CARTESIAN_POINT('Ctrl Pts',(65.4268507326159,246.237329902726,24.2646759008943)) ;
#116323 = CARTESIAN_POINT('Ctrl Pts',(65.3495300954938,248.05023677389,25.2113670426942)) ;
#116324 = CARTESIAN_POINT('Ctrl Pts',(65.2722094583716,249.854562329444,24.2481997978353)) ;
#116325 = CARTESIAN_POINT('Ctrl Pts',(65.1948888212494,250.07638388775,22.2148271143443)) ;
#116326 = CARTESIAN_POINT('Ctrl Pts',(65.1175681841272,248.523048020651,20.8852416284384)) ;
#116327 = CARTESIAN_POINT('Ctrl Pts',(65.040247547005,246.547571995349,21.4173385398677)) ;
#116328 = CARTESIAN_POINT('Ctrl Pts',(64.9629269098829,245.876685603414,23.3500357383482)) ;
#116329 = CARTESIAN_POINT('Ctrl Pts',(64.9113798184681,246.684103092728,24.44248256794)) ;
#116330 = CARTESIAN_POINT('Ctrl Pts',(64.8856062727607,247.22944281573,24.7050916330301)) ;
#116331 = CARTESIAN_POINT('Ctrl Pts',(66.994612333513,247.011769577792,21.5785454559859)) ;
#116332 = CARTESIAN_POINT('Ctrl Pts',(66.9688298859291,246.544311191959,21.9117590634128)) ;
#116333 = CARTESIAN_POINT('Ctrl Pts',(66.9172738926377,245.965745736347,23.0627882349928)) ;
#116334 = CARTESIAN_POINT('Ctrl Pts',(66.839944353639,246.904220235031,24.7605418682122)) ;
#116335 = CARTESIAN_POINT('Ctrl Pts',(66.7626237165168,248.835673670616,24.9392200616958)) ;
#116336 = CARTESIAN_POINT('Ctrl Pts',(66.6853030793946,250.072610867414,23.4465896109422)) ;
#116337 = CARTESIAN_POINT('Ctrl Pts',(66.6079824422724,249.537573845071,21.5825792476595)) ;
#116338 = CARTESIAN_POINT('Ctrl Pts',(66.5306618051503,247.696534575781,20.9735640075703)) ;
#116339 = CARTESIAN_POINT('Ctrl Pts',(66.4533411680281,246.155357011037,22.1503025384181)) ;
#116340 = CARTESIAN_POINT('Ctrl Pts',(66.3760205309059,246.257981793112,24.0867154163394)) ;
#116341 = CARTESIAN_POINT('Ctrl Pts',(66.2986998937837,247.914968687735,25.0939653398447)) ;
#116342 = CARTESIAN_POINT('Ctrl Pts',(66.2213792566616,249.681218919094,24.2936566189442)) ;
#116343 = CARTESIAN_POINT('Ctrl Pts',(66.1440586195394,250.01638467062,22.3837285851626)) ;
#116344 = CARTESIAN_POINT('Ctrl Pts',(66.0667379824172,248.628159442479,21.0298515546859)) ;
#116345 = CARTESIAN_POINT('Ctrl Pts',(65.989417345295,246.72722791265,21.4127488101651)) ;
#116346 = CARTESIAN_POINT('Ctrl Pts',(65.9120967081729,245.971405776317,23.1984941238496)) ;
#116347 = CARTESIAN_POINT('Ctrl Pts',(65.8347760710507,247.019852230261,24.8297247820737)) ;
#116348 = CARTESIAN_POINT('Ctrl Pts',(65.7574554339285,248.958208089265,24.8838316505256)) ;
#116349 = CARTESIAN_POINT('Ctrl Pts',(65.6801347968063,250.096019834095,23.3136288830372)) ;
#116350 = CARTESIAN_POINT('Ctrl Pts',(65.6028141596841,249.440989792863,21.4884996217781)) ;
#116351 = CARTESIAN_POINT('Ctrl Pts',(65.525493522562,247.564381743349,21.0001594155395)) ;
#116352 = CARTESIAN_POINT('Ctrl Pts',(65.4481728854398,246.102784856954,22.2744798301262)) ;
#116353 = CARTESIAN_POINT('Ctrl Pts',(65.3708522483176,246.330902278931,24.2001457205304)) ;
#116354 = CARTESIAN_POINT('Ctrl Pts',(65.2935316111954,248.049719244203,25.09770357156)) ;
#116355 = CARTESIAN_POINT('Ctrl Pts',(65.2162109740733,249.760400264332,24.1845247275771)) ;
#116356 = CARTESIAN_POINT('Ctrl Pts',(65.1388903369511,249.970709278956,22.2566841304139)) ;
#116357 = CARTESIAN_POINT('Ctrl Pts',(65.0615696998289,248.497991577014,20.9961041600331)) ;
#116358 = CARTESIAN_POINT('Ctrl Pts',(64.9842490627067,246.625042800225,21.500585230231)) ;
#116359 = CARTESIAN_POINT('Ctrl Pts',(64.9069284255846,245.988975426567,23.3329754022367)) ;
#116360 = CARTESIAN_POINT('Ctrl Pts',(64.8553813341698,246.754487930692,24.3687242177039)) ;
#116361 = CARTESIAN_POINT('Ctrl Pts',(64.8296077884624,247.271524510254,24.6177038666263)) ;
#116362 = CARTESIAN_POINT('Ctrl Pts',(66.9386138492147,247.068070539199,21.6575245189909)) ;
#116363 = CARTESIAN_POINT('Ctrl Pts',(66.9128314016307,246.62620133268,21.9724976519531)) ;
#116364 = CARTESIAN_POINT('Ctrl Pts',(66.8612754083394,246.079307177951,23.0605182376159)) ;
#116365 = CARTESIAN_POINT('Ctrl Pts',(66.7839458693407,246.966408564169,24.6653349945978)) ;
#116366 = CARTESIAN_POINT('Ctrl Pts',(66.7066252322185,248.792132142731,24.8342321498734)) ;
#116367 = CARTESIAN_POINT('Ctrl Pts',(66.6293045950963,249.961358055087,23.4233099097552)) ;
#116368 = CARTESIAN_POINT('Ctrl Pts',(66.5519839579741,249.455609539954,21.661337496531)) ;
#116369 = CARTESIAN_POINT('Ctrl Pts',(66.4746633208519,247.71535075811,21.0856604115707)) ;
#116370 = CARTESIAN_POINT('Ctrl Pts',(66.3973426837298,246.258538925704,22.1979829982759)) ;
#116371 = CARTESIAN_POINT('Ctrl Pts',(66.3200220466076,246.355545915842,24.0283945339182)) ;
#116372 = CARTESIAN_POINT('Ctrl Pts',(66.2427014094854,247.921827549737,24.9805065035713)) ;
#116373 = CARTESIAN_POINT('Ctrl Pts',(66.1653807723632,249.591391326746,24.2240075505256)) ;
#116374 = CARTESIAN_POINT('Ctrl Pts',(66.0880601352411,249.908209741321,22.418631049914)) ;
#116375 = CARTESIAN_POINT('Ctrl Pts',(66.0107394981189,248.595977468631,21.1388667172755)) ;
#116376 = CARTESIAN_POINT('Ctrl Pts',(65.9334188609967,246.799104993584,21.5008037614803)) ;
#116377 = CARTESIAN_POINT('Ctrl Pts',(65.8560982238745,246.08465738119,23.1887954388525)) ;
#116378 = CARTESIAN_POINT('Ctrl Pts',(65.7787775867523,247.075710738501,24.7307307606792)) ;
#116379 = CARTESIAN_POINT('Ctrl Pts',(65.7014569496302,248.907958894332,24.7818757604367)) ;
#116380 = CARTESIAN_POINT('Ctrl Pts',(65.624136312508,249.983485589529,23.2976275963811)) ;
#116381 = CARTESIAN_POINT('Ctrl Pts',(65.5468156753858,249.364312603574,21.5724078914629)) ;
#116382 = CARTESIAN_POINT('Ctrl Pts',(65.4694950382637,247.590432115134,21.110799958047)) ;
#116383 = CARTESIAN_POINT('Ctrl Pts',(65.3921744011415,246.208844628384,22.3153626902822)) ;
#116384 = CARTESIAN_POINT('Ctrl Pts',(65.3148537640193,246.424474655136,24.1356155401664)) ;
#116385 = CARTESIAN_POINT('Ctrl Pts',(65.2375331268972,248.049201714516,24.9840401004258)) ;
#116386 = CARTESIAN_POINT('Ctrl Pts',(65.1602124897749,249.66623819922,24.1208496573188)) ;
#116387 = CARTESIAN_POINT('Ctrl Pts',(65.0828918526528,249.865034670162,22.2985411464835)) ;
#116388 = CARTESIAN_POINT('Ctrl Pts',(65.0055712155306,248.472935133376,21.1069666916277)) ;
#116389 = CARTESIAN_POINT('Ctrl Pts',(64.9282505784084,246.702513605101,21.5838319205941)) ;
#116390 = CARTESIAN_POINT('Ctrl Pts',(64.8509299412862,246.10126524972,23.3159150661253)) ;
#116391 = CARTESIAN_POINT('Ctrl Pts',(64.7993828498715,246.824872768656,24.294965867468)) ;
#116392 = CARTESIAN_POINT('Ctrl Pts',(64.7736093041641,247.313606204779,24.5303161002225)) ;
#116393 = CARTESIAN_POINT('Origin',(57.9402651077866,248.040265107786,23.0213203435596)) ;
#116394 = CARTESIAN_POINT('Ctrl Pts',(57.9402651077866,248.936544011729,24.7683224547055)) ;
#116395 = CARTESIAN_POINT('Ctrl Pts',(57.9402651077867,248.969834251372,24.748365352915)) ;
#116396 = CARTESIAN_POINT('Ctrl Pts',(57.9402651077867,249.002451928547,24.7273685302422)) ;
#116397 = CARTESIAN_POINT('Ctrl Pts',(57.9402651077867,249.034342381865,24.7053298307907)) ;
#116398 = CARTESIAN_POINT('Ctrl Pts',(57.9402651077867,249.093869423035,24.664192172554)) ;
#116399 = CARTESIAN_POINT('Ctrl Pts',(57.9402651077867,249.150864283323,24.6194251339319)) ;
#116400 = CARTESIAN_POINT('Ctrl Pts',(57.9402651077866,249.205168560284,24.571368724925)) ;
#116401 = CARTESIAN_POINT('Ctrl Pts',(57.9402651077866,249.222893676953,24.5556829354442)) ;
#116402 = CARTESIAN_POINT('Ctrl Pts',(57.9402651077868,249.240331820689,24.5396464364662)) ;
#116403 = CARTESIAN_POINT('Ctrl Pts',(57.9402651077867,249.257476513462,24.5232703805546)) ;
#116404 = CARTESIAN_POINT('Ctrl Pts',(57.9402651077866,249.270127083224,24.51118696556)) ;
#116405 = CARTESIAN_POINT('Ctrl Pts',(57.9402651077866,249.282617872539,24.4989186712449)) ;
#116406 = CARTESIAN_POINT('Ctrl Pts',(57.9402651077866,249.294946099205,24.4864698925067)) ;
#116407 = CARTESIAN_POINT('Ctrl Pts',(57.9402651077866,249.305879409717,24.4754296701666)) ;
#116408 = CARTESIAN_POINT('Ctrl Pts',(57.9402651077865,249.31667896791,24.4642533778532)) ;
#116409 = CARTESIAN_POINT('Ctrl Pts',(57.9402651077865,249.327339178069,24.4529489071045)) ;
#116410 = CARTESIAN_POINT('Ctrl Pts',(57.9402651077867,249.377034801787,24.400249878074)) ;
#116411 = CARTESIAN_POINT('Ctrl Pts',(57.9402651077866,249.423735093708,24.3447378984001)) ;
#116412 = CARTESIAN_POINT('Ctrl Pts',(57.9402651077866,249.467281735283,24.2867546595153)) ;
#116413 = CARTESIAN_POINT('Ctrl Pts',(57.9402651077866,249.499219736011,24.2442285620089)) ;
#116414 = CARTESIAN_POINT('Ctrl Pts',(57.9402651077867,249.529460550065,24.2003723299463)) ;
#116415 = CARTESIAN_POINT('Ctrl Pts',(57.9402651077867,249.557925674325,24.155313058082)) ;
#116416 = CARTESIAN_POINT('Ctrl Pts',(57.9402651077868,249.569913244849,24.1363371634292)) ;
#116417 = CARTESIAN_POINT('Ctrl Pts',(57.9402651077868,249.581585718254,24.1171478514142)) ;
#116418 = CARTESIAN_POINT('Ctrl Pts',(57.9402651077866,249.592936441842,24.0977544311853)) ;
#116419 = CARTESIAN_POINT('Ctrl Pts',(57.9402651077866,249.599573895685,24.0864139267119)) ;
#116420 = CARTESIAN_POINT('Ctrl Pts',(57.9402651077867,249.606102094572,24.0750020847712)) ;
#116421 = CARTESIAN_POINT('Ctrl Pts',(57.9402651077867,249.612511676398,24.0635354567494)) ;
#116422 = CARTESIAN_POINT('Ctrl Pts',(57.9402651077865,249.647369793866,24.0011749038419)) ;
#116423 = CARTESIAN_POINT('Ctrl Pts',(57.9402651077865,249.678777831925,23.9371051763225)) ;
#116424 = CARTESIAN_POINT('Ctrl Pts',(57.9402651077865,249.706585851766,23.8716486500327)) ;
#116425 = CARTESIAN_POINT('Ctrl Pts',(57.9402651077865,249.733893355817,23.8073702739726)) ;
#116426 = CARTESIAN_POINT('Ctrl Pts',(57.9402651077864,249.757729494085,23.7417535820802)) ;
#116427 = CARTESIAN_POINT('Ctrl Pts',(57.9402651077865,249.777904928993,23.6750907110336)) ;
#116428 = CARTESIAN_POINT('Ctrl Pts',(57.9402651077865,249.792011167119,23.6284814390459)) ;
#116429 = CARTESIAN_POINT('Ctrl Pts',(57.9402651077868,249.804326895486,23.5813604604367)) ;
#116430 = CARTESIAN_POINT('Ctrl Pts',(57.9402651077866,249.81477232718,23.5338274809802)) ;
#116431 = CARTESIAN_POINT('Ctrl Pts',(57.9402651077865,249.823437278949,23.4943967531299)) ;
#116432 = CARTESIAN_POINT('Ctrl Pts',(57.9402651077867,249.830814990046,23.4546824717317)) ;
#116433 = CARTESIAN_POINT('Ctrl Pts',(57.9402651077865,249.836852913976,23.414742758069)) ;
#116434 = CARTESIAN_POINT('Ctrl Pts',(57.9402651077864,249.838603276049,23.4031644472442)) ;
#116435 = CARTESIAN_POINT('Ctrl Pts',(57.9402651077868,249.840240928434,23.3915670359813)) ;
#116436 = CARTESIAN_POINT('Ctrl Pts',(57.9402651077868,249.841762838499,23.379966701035)) ;
#116437 = CARTESIAN_POINT('Ctrl Pts',(57.9402651077867,249.850592372617,23.3126660401371)) ;
#116438 = CARTESIAN_POINT('Ctrl Pts',(57.9402651077866,249.855549682227,23.2451444439586)) ;
#116439 = CARTESIAN_POINT('Ctrl Pts',(57.9402651077867,249.85646379212,23.1776764759888)) ;
#116440 = CARTESIAN_POINT('Ctrl Pts',(57.9402651077867,249.856814189209,23.1518146187315)) ;
#116441 = CARTESIAN_POINT('Ctrl Pts',(57.9402651077864,249.856569965134,23.1259606312009)) ;
#116442 = CARTESIAN_POINT('Ctrl Pts',(57.9402651077865,249.855719437616,23.10013009651)) ;
#116443 = CARTESIAN_POINT('Ctrl Pts',(57.9402651077868,249.853467922705,23.0317515516244)) ;
#116444 = CARTESIAN_POINT('Ctrl Pts',(57.9402651077864,249.846971114348,22.9635360782984)) ;
#116445 = CARTESIAN_POINT('Ctrl Pts',(57.9402651077865,249.836406722431,22.8957887401495)) ;
#116446 = CARTESIAN_POINT('Ctrl Pts',(57.9402651077865,249.831283115032,22.8629320678713)) ;
#116447 = CARTESIAN_POINT('Ctrl Pts',(57.9402651077866,249.825202010033,22.8301857600486)) ;
#116448 = CARTESIAN_POINT('Ctrl Pts',(57.9402651077866,249.81817979325,22.797586544371)) ;
#116449 = CARTESIAN_POINT('Ctrl Pts',(57.9402651077866,249.814099592292,22.7786450398378)) ;
#116450 = CARTESIAN_POINT('Ctrl Pts',(57.9402651077866,249.809701618464,22.7597532225742)) ;
#116451 = CARTESIAN_POINT('Ctrl Pts',(57.9402651077866,249.804988737036,22.7409185608578)) ;
#116452 = CARTESIAN_POINT('Ctrl Pts',(57.9402651077867,249.802096108424,22.7293583970392)) ;
#116453 = CARTESIAN_POINT('Ctrl Pts',(57.9402651077864,249.799084386936,22.7178180905904)) ;
#116454 = CARTESIAN_POINT('Ctrl Pts',(57.9402651077865,249.795955629747,22.7063046865931)) ;
#116455 = CARTESIAN_POINT('Ctrl Pts',(57.9402651077866,249.778217509192,22.6410307980329)) ;
#116456 = CARTESIAN_POINT('Ctrl Pts',(57.9402651077866,249.75679097115,22.5768702168924)) ;
#116457 = CARTESIAN_POINT('Ctrl Pts',(57.9402651077866,249.731879665945,22.5141040056564)) ;
#116458 = CARTESIAN_POINT('Ctrl Pts',(57.9402651077866,249.706868342887,22.4510857906947)) ;
#116459 = CARTESIAN_POINT('Ctrl Pts',(57.9402651077866,249.678343600578,22.3894722456789)) ;
#116460 = CARTESIAN_POINT('Ctrl Pts',(57.9402651077867,249.646464982076,22.3295717693722)) ;
#116461 = CARTESIAN_POINT('Ctrl Pts',(57.9402651077868,249.615056130998,22.2705539941925)) ;
#116462 = CARTESIAN_POINT('Ctrl Pts',(57.9402651077867,249.580390846709,22.2131984103696)) ;
#116463 = CARTESIAN_POINT('Ctrl Pts',(57.9402651077866,249.54258637471,22.1578355096128)) ;
#116464 = CARTESIAN_POINT('Ctrl Pts',(57.9402651077866,249.533519373627,22.1445573058834)) ;
#116465 = CARTESIAN_POINT('Ctrl Pts',(57.9402651077865,249.524271660954,22.1313939187497)) ;
#116466 = CARTESIAN_POINT('Ctrl Pts',(57.9402651077865,249.514844610744,22.1183502921032)) ;
#116467 = CARTESIAN_POINT('Ctrl Pts',(57.9402651077866,249.505448906097,22.1053500363732)) ;
#116468 = CARTESIAN_POINT('Ctrl Pts',(57.9402651077865,249.495871453199,22.0924642624107)) ;
#116469 = CARTESIAN_POINT('Ctrl Pts',(57.9402651077865,249.486133728681,22.0797237707493)) ;
#116470 = CARTESIAN_POINT('Ctrl Pts',(57.9402651077865,249.446013857083,22.027232360806)) ;
#116471 = CARTESIAN_POINT('Ctrl Pts',(57.9402651077865,249.403126873497,21.9771313880535)) ;
#116472 = CARTESIAN_POINT('Ctrl Pts',(57.9402651077866,249.357623594114,21.929703658124)) ;
#116473 = CARTESIAN_POINT('Ctrl Pts',(57.9402651077867,249.312871487116,21.8830588695883)) ;
#116474 = CARTESIAN_POINT('Ctrl Pts',(57.9402651077866,249.265588098698,21.8389991407756)) ;
#116475 = CARTESIAN_POINT('Ctrl Pts',(57.9402651077866,249.215886432752,21.7978329278902)) ;
#116476 = CARTESIAN_POINT('Ctrl Pts',(57.9402651077865,249.167850788198,21.7580466243097)) ;
#116477 = CARTESIAN_POINT('Ctrl Pts',(57.9402651077866,249.117555685649,21.7209627068944)) ;
#116478 = CARTESIAN_POINT('Ctrl Pts',(57.9402651077865,249.065083510332,21.6869041375018)) ;
#116479 = CARTESIAN_POINT('Ctrl Pts',(57.9402651077864,249.048474840792,21.6761238044844)) ;
#116480 = CARTESIAN_POINT('Ctrl Pts',(57.9402651077865,249.031647939631,21.6656469393582)) ;
#116481 = CARTESIAN_POINT('Ctrl Pts',(57.9402651077866,249.01460512908,21.6554848536836)) ;
#116482 = CARTESIAN_POINT('',(57.9394803992446,247.064599950825,21.6547731742408)) ;
#116483 = CARTESIAN_POINT('Ctrl Pts',(57.9402651077867,247.09020061484,21.6384890010805)) ;
#116484 = CARTESIAN_POINT('Ctrl Pts',(57.9400035382726,247.081876264352,21.6442081872039)) ;
#116485 = CARTESIAN_POINT('Ctrl Pts',(57.9397419687586,247.073603557709,21.6500025415884)) ;
#116486 = CARTESIAN_POINT('Ctrl Pts',(57.9394803992446,247.065383843876,21.6558711193933)) ;
#116487 = CARTESIAN_POINT('Ctrl Pts',(57.9402651077866,247.063751382118,21.653699040999)) ;
#116488 = CARTESIAN_POINT('Ctrl Pts',(57.9402651077865,247.022795562072,21.6777771701807)) ;
#116489 = CARTESIAN_POINT('Ctrl Pts',(57.9402651077866,246.983015097768,21.7036389402643)) ;
#116490 = CARTESIAN_POINT('Ctrl Pts',(57.9402651077865,246.944545251137,21.731258981544)) ;
#116491 = CARTESIAN_POINT('Ctrl Pts',(57.9402651077865,246.893065219322,21.7682198932282)) ;
#116492 = CARTESIAN_POINT('Ctrl Pts',(57.9402651077865,246.843930666271,21.8083275360126)) ;
#116493 = CARTESIAN_POINT('Ctrl Pts',(57.9402651077865,246.79721860728,21.8512529472481)) ;
#116494 = CARTESIAN_POINT('Ctrl Pts',(57.9402651077865,246.778270710595,21.8686648591795)) ;
#116495 = CARTESIAN_POINT('Ctrl Pts',(57.9402651077864,246.759721683068,21.8865409338896)) ;
#116496 = CARTESIAN_POINT('Ctrl Pts',(57.9402651077865,246.741577912132,21.9048612357463)) ;
#116497 = CARTESIAN_POINT('Ctrl Pts',(57.9402651077866,246.732151157705,21.9143797083529)) ;
#116498 = CARTESIAN_POINT('Ctrl Pts',(57.9402651077865,246.722832136955,21.9240198964915)) ;
#116499 = CARTESIAN_POINT('Ctrl Pts',(57.9402651077865,246.713627348976,21.933773241702)) ;
#116500 = CARTESIAN_POINT('Ctrl Pts',(57.9402651077864,246.668538281455,21.9815493818791)) ;
#116501 = CARTESIAN_POINT('Ctrl Pts',(57.9402651077864,246.626266996622,22.0319509032703)) ;
#116502 = CARTESIAN_POINT('Ctrl Pts',(57.9402651077864,246.586892797857,22.084618239577)) ;
#116503 = CARTESIAN_POINT('Ctrl Pts',(57.9402651077864,246.55575619811,22.1262668780695)) ;
#116504 = CARTESIAN_POINT('Ctrl Pts',(57.9402651077867,246.52643165571,22.1693336238241)) ;
#116505 = CARTESIAN_POINT('Ctrl Pts',(57.9402651077865,246.498971999877,22.2136592363338)) ;
#116506 = CARTESIAN_POINT('Ctrl Pts',(57.9402651077864,246.484061222999,22.2377283405538)) ;
#116507 = CARTESIAN_POINT('Ctrl Pts',(57.9402651077866,246.469700544209,22.2621688855007)) ;
#116508 = CARTESIAN_POINT('Ctrl Pts',(57.9402651077866,246.455900172974,22.2869569486825)) ;
#116509 = CARTESIAN_POINT('Ctrl Pts',(57.9402651077867,246.449901218829,22.2977321989879)) ;
#116510 = CARTESIAN_POINT('Ctrl Pts',(57.9402651077867,246.444008646131,22.3085724311742)) ;
#116511 = CARTESIAN_POINT('Ctrl Pts',(57.9402651077866,246.438229248595,22.3194639887581)) ;
#116512 = CARTESIAN_POINT('Ctrl Pts',(57.9402651077865,246.406422480815,22.3794053997209)) ;
#116513 = CARTESIAN_POINT('Ctrl Pts',(57.9402651077865,246.377989861048,22.4409885827609)) ;
#116514 = CARTESIAN_POINT('Ctrl Pts',(57.9402651077866,246.353019437315,22.5038540656447)) ;
#116515 = CARTESIAN_POINT('Ctrl Pts',(57.9402651077866,246.327688728189,22.5676266022309)) ;
#116516 = CARTESIAN_POINT('Ctrl Pts',(57.9402651077867,246.305920219198,22.6327195891187)) ;
#116517 = CARTESIAN_POINT('Ctrl Pts',(57.9402651077866,246.287845359425,22.6987929595691)) ;
#116518 = CARTESIAN_POINT('Ctrl Pts',(57.9402651077865,246.275494931828,22.7439404399967)) ;
#116519 = CARTESIAN_POINT('Ctrl Pts',(57.9402651077865,246.264869853737,22.7895463862758)) ;
#116520 = CARTESIAN_POINT('Ctrl Pts',(57.9402651077865,246.256024758883,22.8355082400426)) ;
#116521 = CARTESIAN_POINT('Ctrl Pts',(57.9402651077865,246.251600756467,22.8584967275025)) ;
#116522 = CARTESIAN_POINT('Ctrl Pts',(57.9402651077866,246.247622214495,22.881574306955)) ;
#116523 = CARTESIAN_POINT('Ctrl Pts',(57.9402651077866,246.2440970561,22.9047283899068)) ;
#116524 = CARTESIAN_POINT('Ctrl Pts',(57.9402651077865,246.241835333762,22.9195839228383)) ;
#116525 = CARTESIAN_POINT('Ctrl Pts',(57.9402651077866,246.239760258836,22.9344709506001)) ;
#116526 = CARTESIAN_POINT('Ctrl Pts',(57.9402651077865,246.237874091866,22.9493861652913)) ;
#116527 = CARTESIAN_POINT('Ctrl Pts',(57.9402651077864,246.236484466093,22.9603748884925)) ;
#116528 = CARTESIAN_POINT('Ctrl Pts',(57.9402651077865,246.235198549517,22.9713697420018)) ;
#116529 = CARTESIAN_POINT('Ctrl Pts',(57.9402651077865,246.23401688886,22.9823680560691)) ;
#116530 = CARTESIAN_POINT('Ctrl Pts',(57.9402651077867,246.226554706152,23.0518223690129)) ;
#116531 = CARTESIAN_POINT('Ctrl Pts',(57.9402651077868,246.223244400811,23.1214287161277)) ;
#116532 = CARTESIAN_POINT('Ctrl Pts',(57.9402651077866,246.224210769353,23.1908364633901)) ;
#116533 = CARTESIAN_POINT('Ctrl Pts',(57.9402651077865,246.224503387308,23.2118532413484)) ;
#116534 = CARTESIAN_POINT('Ctrl Pts',(57.9402651077866,246.225188455189,23.2328519633107)) ;
#116535 = CARTESIAN_POINT('Ctrl Pts',(57.9402651077867,246.226270324961,23.2538232262009)) ;
#116536 = CARTESIAN_POINT('Ctrl Pts',(57.9402651077868,246.229736559053,23.3210136665446)) ;
#116537 = CARTESIAN_POINT('Ctrl Pts',(57.9402651077866,246.237271980017,23.3879220396537)) ;
#116538 = CARTESIAN_POINT('Ctrl Pts',(57.9402651077866,246.248654075727,23.4543056841415)) ;
#116539 = CARTESIAN_POINT('Ctrl Pts',(57.9402651077867,246.254586354754,23.4889044357236)) ;
#116540 = CARTESIAN_POINT('Ctrl Pts',(57.9402651077866,246.261564434129,23.523360710123)) ;
#116541 = CARTESIAN_POINT('Ctrl Pts',(57.9402651077867,246.26956226066,23.55763995277)) ;
#116542 = CARTESIAN_POINT('Ctrl Pts',(57.9402651077867,246.273897374718,23.5762205541502)) ;
#116543 = CARTESIAN_POINT('Ctrl Pts',(57.9402651077867,246.278532156485,23.5947491358563)) ;
#116544 = CARTESIAN_POINT('Ctrl Pts',(57.9402651077867,246.283462886363,23.6132201155199)) ;
#116545 = CARTESIAN_POINT('Ctrl Pts',(57.9402651077867,246.28644344509,23.624385569922)) ;
#116546 = CARTESIAN_POINT('Ctrl Pts',(57.9402651077865,246.289532150096,23.635529975047)) ;
#116547 = CARTESIAN_POINT('Ctrl Pts',(57.9402651077865,246.292728231333,23.646652083647)) ;
#116548 = CARTESIAN_POINT('Ctrl Pts',(57.9402651077865,246.296265107811,23.6589601325905)) ;
#116549 = CARTESIAN_POINT('Ctrl Pts',(57.9402651077868,246.299931179453,23.6712327041133)) ;
#116550 = CARTESIAN_POINT('Ctrl Pts',(57.9402651077867,246.303722785304,23.6834617388722)) ;
#116551 = CARTESIAN_POINT('Ctrl Pts',(57.9402651077865,246.324579729698,23.7507314678489)) ;
#116552 = CARTESIAN_POINT('Ctrl Pts',(57.9402651077866,246.349248273941,23.8167452634601)) ;
#116553 = CARTESIAN_POINT('Ctrl Pts',(57.9402651077866,246.377460807139,23.8812387823142)) ;
#116554 = CARTESIAN_POINT('Ctrl Pts',(57.9402651077866,246.405673340336,23.9457323011682)) ;
#116555 = CARTESIAN_POINT('Ctrl Pts',(57.9402651077867,246.437430309462,24.0087064048567)) ;
#116556 = CARTESIAN_POINT('Ctrl Pts',(57.9402651077866,246.47251718865,24.0698922633336)) ;
#116557 = CARTESIAN_POINT('Ctrl Pts',(57.9402651077865,246.508042580594,24.1318428173341)) ;
#116558 = CARTESIAN_POINT('Ctrl Pts',(57.9402651077865,246.546981996077,24.1919611082941)) ;
#116559 = CARTESIAN_POINT('Ctrl Pts',(57.9402651077866,246.589161244989,24.2499497148609)) ;
#116560 = CARTESIAN_POINT('Ctrl Pts',(57.9402651077866,246.598810156939,24.2632151705834)) ;
#116561 = CARTESIAN_POINT('Ctrl Pts',(57.9402651077865,246.608628797714,24.2763690679559)) ;
#116562 = CARTESIAN_POINT('Ctrl Pts',(57.9402651077864,246.618615401402,24.289407630059)) ;
#116563 = CARTESIAN_POINT('Ctrl Pts',(57.9402651077864,246.625695864494,24.2986519197716)) ;
#116564 = CARTESIAN_POINT('Ctrl Pts',(57.9402651077866,246.632860426978,24.3078376671516)) ;
#116565 = CARTESIAN_POINT('Ctrl Pts',(57.9402651077866,246.64009999969,24.3169532337087)) ;
#116566 = CARTESIAN_POINT('Ctrl Pts',(57.9402651077866,246.685677256768,24.3743409466196)) ;
#116567 = CARTESIAN_POINT('Ctrl Pts',(57.9402651077865,246.73430598704,24.4290572965446)) ;
#116568 = CARTESIAN_POINT('Ctrl Pts',(57.9402651077865,246.78574661108,24.4808204424783)) ;
#116569 = CARTESIAN_POINT('Ctrl Pts',(57.9402651077865,246.837101404366,24.5324972195167)) ;
#116570 = CARTESIAN_POINT('Ctrl Pts',(57.9402651077867,246.891259241171,24.5812315797706)) ;
#116571 = CARTESIAN_POINT('Ctrl Pts',(57.9402651077866,246.948028081008,24.6267202960962)) ;
#116572 = CARTESIAN_POINT('Ctrl Pts',(57.9402651077866,247.003352437633,24.6710515519693)) ;
#116573 = CARTESIAN_POINT('Ctrl Pts',(57.9402651077867,247.061157230315,24.7123009754626)) ;
#116574 = CARTESIAN_POINT('Ctrl Pts',(57.9402651077866,247.121300105744,24.7501540607501)) ;
#116575 = CARTESIAN_POINT('Ctrl Pts',(57.9402651077866,247.143343628465,24.7640279458888)) ;
#116576 = CARTESIAN_POINT('Ctrl Pts',(57.9402651077865,247.16570154556,24.7774451902113)) ;
#116577 = CARTESIAN_POINT('Ctrl Pts',(57.9402651077866,247.188367839728,24.7903888257488)) ;
#116578 = CARTESIAN_POINT('Ctrl Pts',(61.1070133762705,248.766854525377,24.5301718052866)) ;
#116579 = CARTESIAN_POINT('Ctrl Pts',(61.080638560942,249.266941772283,24.2893541299283)) ;
#116580 = CARTESIAN_POINT('Ctrl Pts',(61.027888930285,249.999896115323,23.2741377447068)) ;
#116581 = CARTESIAN_POINT('Ctrl Pts',(60.9487644842995,249.321107628342,21.5135065273509)) ;
#116582 = CARTESIAN_POINT('Ctrl Pts',(60.869640038314,247.474294984015,21.1268386661821)) ;
#116583 = CARTESIAN_POINT('Ctrl Pts',(60.7905155923284,246.143541845113,22.4625909175899)) ;
#116584 = CARTESIAN_POINT('Ctrl Pts',(60.7113911463429,246.537942674782,24.3072111397376)) ;
#116585 = CARTESIAN_POINT('Ctrl Pts',(60.6322667003574,248.299453084171,24.9816336600195)) ;
#116586 = CARTESIAN_POINT('Ctrl Pts',(60.5531422543719,249.825029443136,23.8726149962676)) ;
#116587 = CARTESIAN_POINT('Ctrl Pts',(60.4740178083863,249.726823714205,21.9890071491867)) ;
#116588 = CARTESIAN_POINT('Ctrl Pts',(60.3948933624008,248.094107651175,21.0446559799089)) ;
#116589 = CARTESIAN_POINT('Ctrl Pts',(60.3157689164153,246.412415556467,21.8987259886766)) ;
#116590 = CARTESIAN_POINT('Ctrl Pts',(60.2366444704298,246.211787909224,23.7741738257661)) ;
#116591 = CARTESIAN_POINT('Ctrl Pts',(60.1575200244442,247.674770120869,24.9646488533224)) ;
#116592 = CARTESIAN_POINT('Ctrl Pts',(60.0783955784587,249.470290254645,24.3870222847478)) ;
#116593 = CARTESIAN_POINT('Ctrl Pts',(59.9992711324732,249.964728074474,22.5668356392193)) ;
#116594 = CARTESIAN_POINT('Ctrl Pts',(59.9201466864877,248.708227359668,21.1601540415291)) ;
#116595 = CARTESIAN_POINT('Ctrl Pts',(59.8410222405021,246.843993229004,21.4468212689482)) ;
#116596 = CARTESIAN_POINT('Ctrl Pts',(59.7618977945166,246.068165661642,23.1660184318367)) ;
#116597 = CARTESIAN_POINT('Ctrl Pts',(59.6827733485311,247.086617602811,24.7535645967704)) ;
#116598 = CARTESIAN_POINT('Ctrl Pts',(59.6036489025456,248.972728693476,24.765059256107)) ;
#116599 = CARTESIAN_POINT('Ctrl Pts',(59.5245244565601,250.01045443974,23.1900441840451)) ;
#116600 = CARTESIAN_POINT('Ctrl Pts',(59.4454000105745,249.255638581674,21.4615187367073)) ;
#116601 = CARTESIAN_POINT('Ctrl Pts',(59.366275564589,247.395036866021,21.1521509471284)) ;
#116602 = CARTESIAN_POINT('Ctrl Pts',(59.2871511186035,246.121484539962,22.5434135589518)) ;
#116603 = CARTESIAN_POINT('Ctrl Pts',(59.2080266726179,246.593700488024,24.3694911579488)) ;
#116604 = CARTESIAN_POINT('Ctrl Pts',(59.1289022266325,248.382047392536,24.9689595410457)) ;
#116605 = CARTESIAN_POINT('Ctrl Pts',(59.0497777806469,249.859429881076,23.7964032967042)) ;
#116606 = CARTESIAN_POINT('Ctrl Pts',(58.9706533346614,249.681677563272,21.9186513706623)) ;
#116607 = CARTESIAN_POINT('Ctrl Pts',(58.8915288886758,248.010515861749,21.0441437544105)) ;
#116608 = CARTESIAN_POINT('Ctrl Pts',(58.8124044426904,246.366420027326,21.9685336234909)) ;
#116609 = CARTESIAN_POINT('Ctrl Pts',(58.7332799967048,246.245244316357,23.8507855964087)) ;
#116610 = CARTESIAN_POINT('Ctrl Pts',(58.6541555507193,247.757231817376,24.9783571808533)) ;
#116611 = CARTESIAN_POINT('Ctrl Pts',(58.5750311047338,249.52674160729,24.3253671527601)) ;
#116612 = CARTESIAN_POINT('Ctrl Pts',(58.4959066587482,249.943786803312,22.4858845648418)) ;
#116613 = CARTESIAN_POINT('Ctrl Pts',(58.4167822127627,248.628990691216,21.1336209784045)) ;
#116614 = CARTESIAN_POINT('Ctrl Pts',(58.3376577667772,246.778457851123,21.4987139336705)) ;
#116615 = CARTESIAN_POINT('Ctrl Pts',(58.2585333207917,246.076159531858,23.2494146074457)) ;
#116616 = CARTESIAN_POINT('Ctrl Pts',(58.1794088748061,247.160417795382,24.7919845448622)) ;
#116617 = CARTESIAN_POINT('Ctrl Pts',(58.1002844288207,249.04608391346,24.7249601520188)) ;
#116618 = CARTESIAN_POINT('Ctrl Pts',(58.0211505904172,250.014463203649,23.1051876352719)) ;
#116619 = CARTESIAN_POINT('Ctrl Pts',(57.9683915673424,249.46448777725,21.9799214227029)) ;
#116620 = CARTESIAN_POINT('Ctrl Pts',(57.9420073595959,249.012341492745,21.6576369534145)) ;
#116621 = CARTESIAN_POINT('Ctrl Pts',(61.0509160513592,248.809010496563,24.6177138162294)) ;
#116622 = CARTESIAN_POINT('Ctrl Pts',(61.0245412360307,249.338112291522,24.3629241468703)) ;
#116623 = CARTESIAN_POINT('Ctrl Pts',(60.9717916053737,250.113591892182,23.2888059504641)) ;
#116624 = CARTESIAN_POINT('Ctrl Pts',(60.8926671593882,249.395420794876,21.4260247195345)) ;
#116625 = CARTESIAN_POINT('Ctrl Pts',(60.8135427134026,247.441457979165,21.0169227864956)) ;
#116626 = CARTESIAN_POINT('Ctrl Pts',(60.7344182674171,246.033495910951,22.4301740105829)) ;
#116627 = CARTESIAN_POINT('Ctrl Pts',(60.6552938214316,246.450779471375,24.3818172020345)) ;
#116628 = CARTESIAN_POINT('Ctrl Pts',(60.5761693754461,248.314490904155,25.0953690237408)) ;
#116629 = CARTESIAN_POINT('Ctrl Pts',(60.4970449294606,249.928579635412,23.9220062370182)) ;
#116630 = CARTESIAN_POINT('Ctrl Pts',(60.417920483475,249.824676111027,21.9291133987079)) ;
#116631 = CARTESIAN_POINT('Ctrl Pts',(60.3387960374895,248.097231540201,20.929971945236)) ;
#116632 = CARTESIAN_POINT('Ctrl Pts',(60.259671591504,246.317969398677,21.8335942180601)) ;
#116633 = CARTESIAN_POINT('Ctrl Pts',(60.1805471455185,246.105701541555,23.8178536109865)) ;
#116634 = CARTESIAN_POINT('Ctrl Pts',(60.1014226995329,247.6535644774,25.0773987760169)) ;
#116635 = CARTESIAN_POINT('Ctrl Pts',(60.0222982535474,249.55325884382,24.4662589076446)) ;
#116636 = CARTESIAN_POINT('Ctrl Pts',(59.9431738075619,250.076383437751,22.5404669038136)) ;
#116637 = CARTESIAN_POINT('Ctrl Pts',(59.8640493615764,248.74698184296,21.0521710856772)) ;
#116638 = CARTESIAN_POINT('Ctrl Pts',(59.7849249155908,246.77458676418,21.3554704509814)) ;
#116639 = CARTESIAN_POINT('Ctrl Pts',(59.7058004696053,245.95374647879,23.1744136661912)) ;
#116640 = CARTESIAN_POINT('Ctrl Pts',(59.6266760236198,247.031287954775,24.8540676278617)) ;
#116641 = CARTESIAN_POINT('Ctrl Pts',(59.5475515776343,249.026829272288,24.8662291955183)) ;
#116642 = CARTESIAN_POINT('Ctrl Pts',(59.4684271316487,250.124762799729,23.1998333678479)) ;
#116643 = CARTESIAN_POINT('Ctrl Pts',(59.3893026856632,249.326153301412,21.3710206507133)) ;
#116644 = CARTESIAN_POINT('Ctrl Pts',(59.3101782396777,247.357601386628,21.0437036599653)) ;
#116645 = CARTESIAN_POINT('Ctrl Pts',(59.2310537936922,246.010158863627,22.5156858985233)) ;
#116646 = CARTESIAN_POINT('Ctrl Pts',(59.1519293477067,246.509772295631,24.447710642888)) ;
#116647 = CARTESIAN_POINT('Ctrl Pts',(59.0728049017211,248.401877249398,25.0819595654112)) ;
#116648 = CARTESIAN_POINT('Ctrl Pts',(58.9936804557356,249.964975951402,23.8413728129799)) ;
#116649 = CARTESIAN_POINT('Ctrl Pts',(58.9145560097501,249.77691062682,21.8546756502285)) ;
#116650 = CARTESIAN_POINT('Ctrl Pts',(58.8354315637646,248.008789841071,20.9294300009407)) ;
#116651 = CARTESIAN_POINT('Ctrl Pts',(58.756307117779,246.269305256213,21.9074520200949)) ;
#116652 = CARTESIAN_POINT('Ctrl Pts',(58.6771826717935,246.141099055042,23.8989103178167)) ;
#116653 = CARTESIAN_POINT('Ctrl Pts',(58.598058225808,247.74081051678,25.0919024466211)) ;
#116654 = CARTESIAN_POINT('Ctrl Pts',(58.5189337798225,249.612985445922,24.401026608271)) ;
#116655 = CARTESIAN_POINT('Ctrl Pts',(58.4398093338369,250.054227175559,22.4548191313059)) ;
#116656 = CARTESIAN_POINT('Ctrl Pts',(58.3606848878514,248.663147944448,21.0240986015019)) ;
#116657 = CARTESIAN_POINT('Ctrl Pts',(58.2815604418659,246.705249091034,21.4103738747732)) ;
#116658 = CARTESIAN_POINT('Ctrl Pts',(58.2024359958804,245.96220414514,23.2626484021906)) ;
#116659 = CARTESIAN_POINT('Ctrl Pts',(58.1233115498949,247.109369958663,24.8947166618521)) ;
#116660 = CARTESIAN_POINT('Ctrl Pts',(58.0441871039093,249.104440486738,24.8238035826266)) ;
#116661 = CARTESIAN_POINT('Ctrl Pts',(57.9650532655059,250.129004148,23.1100535293344)) ;
#116662 = CARTESIAN_POINT('Ctrl Pts',(57.912294242431,249.54711971265,21.9195005277123)) ;
#116663 = CARTESIAN_POINT('Ctrl Pts',(57.8859100346846,249.068740365456,21.5785174447743)) ;
#116664 = CARTESIAN_POINT('Ctrl Pts',(60.9948187264479,248.85116646775,24.7052558271723)) ;
#116665 = CARTESIAN_POINT('Ctrl Pts',(60.9684439111194,249.409282810763,24.4364941638122)) ;
#116666 = CARTESIAN_POINT('Ctrl Pts',(60.9156942804624,250.227287669041,23.3034741562214)) ;
#116667 = CARTESIAN_POINT('Ctrl Pts',(60.8365698344769,249.46973396141,21.338542911718)) ;
#116668 = CARTESIAN_POINT('Ctrl Pts',(60.7574453884913,247.408620974313,20.9070069068091)) ;
#116669 = CARTESIAN_POINT('Ctrl Pts',(60.6783209425058,245.92344997679,22.3977571035757)) ;
#116670 = CARTESIAN_POINT('Ctrl Pts',(60.5991964965203,246.363616267967,24.4564232643313)) ;
#116671 = CARTESIAN_POINT('Ctrl Pts',(60.5200720505348,248.32952872414,25.209104387462)) ;
#116672 = CARTESIAN_POINT('Ctrl Pts',(60.4409476045492,250.032129827686,23.9713974777687)) ;
#116673 = CARTESIAN_POINT('Ctrl Pts',(60.3618231585637,249.92252850785,21.869219648229)) ;
#116674 = CARTESIAN_POINT('Ctrl Pts',(60.2826987125782,248.100355429226,20.815287910563)) ;
#116675 = CARTESIAN_POINT('Ctrl Pts',(60.2035742665927,246.223523240888,21.7684624474437)) ;
#116676 = CARTESIAN_POINT('Ctrl Pts',(60.1244498206071,245.999615173888,23.8615333962069)) ;
#116677 = CARTESIAN_POINT('Ctrl Pts',(60.0453253746216,247.632358833932,25.1901486987114)) ;
#116678 = CARTESIAN_POINT('Ctrl Pts',(59.966200928636,249.636227432995,24.5454955305414)) ;
#116679 = CARTESIAN_POINT('Ctrl Pts',(59.8870764826506,250.188038801027,22.514098168408)) ;
#116680 = CARTESIAN_POINT('Ctrl Pts',(59.807952036665,248.785736326251,20.9441881298252)) ;
#116681 = CARTESIAN_POINT('Ctrl Pts',(59.7288275906795,246.705180299356,21.2641196330146)) ;
#116682 = CARTESIAN_POINT('Ctrl Pts',(59.649703144694,245.839327295939,23.1828089005457)) ;
#116683 = CARTESIAN_POINT('Ctrl Pts',(59.5705786987085,246.975958306739,24.9545706589532)) ;
#116684 = CARTESIAN_POINT('Ctrl Pts',(59.4914542527229,249.0809298511,24.9673991349296)) ;
#116685 = CARTESIAN_POINT('Ctrl Pts',(59.4123298067374,250.239071159718,23.2096225516508)) ;
#116686 = CARTESIAN_POINT('Ctrl Pts',(59.3332053607519,249.39666802115,21.2805225647191)) ;
#116687 = CARTESIAN_POINT('Ctrl Pts',(59.2540809147664,247.320165907236,20.9352563728022)) ;
#116688 = CARTESIAN_POINT('Ctrl Pts',(59.1749564687808,245.898833187292,22.4879582380948)) ;
#116689 = CARTESIAN_POINT('Ctrl Pts',(59.0958320227954,246.425844103238,24.5259301278273)) ;
#116690 = CARTESIAN_POINT('Ctrl Pts',(59.0167075768098,248.421707106259,25.1949595897767)) ;
#116691 = CARTESIAN_POINT('Ctrl Pts',(58.9375831308243,250.070522021727,23.8863423292556)) ;
#116692 = CARTESIAN_POINT('Ctrl Pts',(58.8584586848388,249.872143690368,21.7906999297945)) ;
#116693 = CARTESIAN_POINT('Ctrl Pts',(58.7793342388532,248.007063820394,20.8147162474708)) ;
#116694 = CARTESIAN_POINT('Ctrl Pts',(58.7002097928677,246.172190485098,21.8463704166988)) ;
#116695 = CARTESIAN_POINT('Ctrl Pts',(58.6210853468822,246.036953793729,23.9470350392246)) ;
#116696 = CARTESIAN_POINT('Ctrl Pts',(58.5419609008967,247.724389216186,25.2054477123889)) ;
#116697 = CARTESIAN_POINT('Ctrl Pts',(58.4628364549111,249.699229284554,24.4766860637818)) ;
#116698 = CARTESIAN_POINT('Ctrl Pts',(58.3837120089257,250.164667547808,22.4237536977701)) ;
#116699 = CARTESIAN_POINT('Ctrl Pts',(58.3045875629401,248.697305197679,20.9145762245993)) ;
#116700 = CARTESIAN_POINT('Ctrl Pts',(58.2254631169546,246.632040330946,21.322033815876)) ;
#116701 = CARTESIAN_POINT('Ctrl Pts',(58.1463386709691,245.848248758422,23.2758821969355)) ;
#116702 = CARTESIAN_POINT('Ctrl Pts',(58.0672142249835,247.058322121945,24.997448778842)) ;
#116703 = CARTESIAN_POINT('Ctrl Pts',(57.988089778998,249.162797060017,24.9226470132344)) ;
#116704 = CARTESIAN_POINT('Ctrl Pts',(57.9089559405946,250.243545092351,23.1149194233968)) ;
#116705 = CARTESIAN_POINT('Ctrl Pts',(57.8561969175197,249.629751648052,21.8590796327216)) ;
#116706 = CARTESIAN_POINT('Ctrl Pts',(57.8298127097733,249.125139238166,21.4993979361343)) ;
#116707 = CARTESIAN_POINT('Ctrl Pts',(60.9387214015366,248.893322438937,24.7927978381151)) ;
#116708 = CARTESIAN_POINT('Ctrl Pts',(60.9123465862081,249.480453330002,24.5100641807542)) ;
#116709 = CARTESIAN_POINT('Ctrl Pts',(60.8595969555511,250.340983445901,23.3181423619787)) ;
#116710 = CARTESIAN_POINT('Ctrl Pts',(60.7804725095656,249.544047127944,21.2510611039017)) ;
#116711 = CARTESIAN_POINT('Ctrl Pts',(60.70134806358,247.375783969461,20.7970910271226)) ;
#116712 = CARTESIAN_POINT('Ctrl Pts',(60.6222236175945,245.813404042628,22.3653401965687)) ;
#116713 = CARTESIAN_POINT('Ctrl Pts',(60.543099171609,246.27645306456,24.5310293266281)) ;
#116714 = CARTESIAN_POINT('Ctrl Pts',(60.4639747256235,248.344566544123,25.3228397511833)) ;
#116715 = CARTESIAN_POINT('Ctrl Pts',(60.3848502796379,250.13568001996,24.0207887185192)) ;
#116716 = CARTESIAN_POINT('Ctrl Pts',(60.3057258336524,250.020380904671,21.8093258977503)) ;
#116717 = CARTESIAN_POINT('Ctrl Pts',(60.2266013876669,248.103479318252,20.7006038758901)) ;
#116718 = CARTESIAN_POINT('Ctrl Pts',(60.1474769416814,246.129077083099,21.7033306768272)) ;
#116719 = CARTESIAN_POINT('Ctrl Pts',(60.0683524956958,245.893528806219,23.9052131814272)) ;
#116720 = CARTESIAN_POINT('Ctrl Pts',(59.9892280497103,247.611153190463,25.3028986214059)) ;
#116721 = CARTESIAN_POINT('Ctrl Pts',(59.9101036037248,249.71919602217,24.6247321534382)) ;
#116722 = CARTESIAN_POINT('Ctrl Pts',(59.8309791577393,250.299694164303,22.4877294330023)) ;
#116723 = CARTESIAN_POINT('Ctrl Pts',(59.7518547117538,248.824490809544,20.8362051739732)) ;
#116724 = CARTESIAN_POINT('Ctrl Pts',(59.6727302657682,246.635773834532,21.1727688150478)) ;
#116725 = CARTESIAN_POINT('Ctrl Pts',(59.5936058197827,245.724908113088,23.1912041349002)) ;
#116726 = CARTESIAN_POINT('Ctrl Pts',(59.5144813737972,246.920628658703,25.0550736900445)) ;
#116727 = CARTESIAN_POINT('Ctrl Pts',(59.4353569278117,249.135030429914,25.068569074341)) ;
#116728 = CARTESIAN_POINT('Ctrl Pts',(59.3562324818261,250.353379519707,23.2194117354537)) ;
#116729 = CARTESIAN_POINT('Ctrl Pts',(59.2771080358406,249.467182740888,21.190024478725)) ;
#116730 = CARTESIAN_POINT('Ctrl Pts',(59.1979835898551,247.282730427844,20.8268090856391)) ;
#116731 = CARTESIAN_POINT('Ctrl Pts',(59.1188591438696,245.787507510957,22.4602305776664)) ;
#116732 = CARTESIAN_POINT('Ctrl Pts',(59.0397346978841,246.341915910844,24.6041496127664)) ;
#116733 = CARTESIAN_POINT('Ctrl Pts',(58.9606102518985,248.441536963121,25.3079596141421)) ;
#116734 = CARTESIAN_POINT('Ctrl Pts',(58.881485805913,250.176068092052,23.9313118455313)) ;
#116735 = CARTESIAN_POINT('Ctrl Pts',(58.8023613599274,249.967376753917,21.7267242093606)) ;
#116736 = CARTESIAN_POINT('Ctrl Pts',(58.7232369139419,248.005337799717,20.7000024940009)) ;
#116737 = CARTESIAN_POINT('Ctrl Pts',(58.6441124679564,246.075075713985,21.7852888133028)) ;
#116738 = CARTESIAN_POINT('Ctrl Pts',(58.5649880219709,245.932808532414,23.9951597606326)) ;
#116739 = CARTESIAN_POINT('Ctrl Pts',(58.4858635759853,247.70796791559,25.3189929781567)) ;
#116740 = CARTESIAN_POINT('Ctrl Pts',(58.4067391299999,249.785473123187,24.5523455192925)) ;
#116741 = CARTESIAN_POINT('Ctrl Pts',(58.3276146840143,250.275107920055,22.3926882642343)) ;
#116742 = CARTESIAN_POINT('Ctrl Pts',(58.2484902380288,248.731462450911,20.8050538476968)) ;
#116743 = CARTESIAN_POINT('Ctrl Pts',(58.1693657920433,246.558831570858,21.2336937569787)) ;
#116744 = CARTESIAN_POINT('Ctrl Pts',(58.0902413460577,245.734293371704,23.2891159916804)) ;
#116745 = CARTESIAN_POINT('Ctrl Pts',(58.0111169000722,247.007274285226,25.1001808958319)) ;
#116746 = CARTESIAN_POINT('Ctrl Pts',(57.9319924540867,249.221153633296,25.0214904438423)) ;
#116747 = CARTESIAN_POINT('Ctrl Pts',(57.8528586156833,250.358086036701,23.1197853174594)) ;
#116748 = CARTESIAN_POINT('Ctrl Pts',(57.8000995926084,249.712383583452,21.7986587377309)) ;
#116749 = CARTESIAN_POINT('Ctrl Pts',(57.773715384862,249.181538110878,21.4202784274943)) ;
#116750 = CARTESIAN_POINT('Ctrl Pts',(60.9402651077866,249.016778829374,21.653698982557)) ;
#116751 = CARTESIAN_POINT('Ctrl Pts',(60.9402651077866,249.057734649078,21.6777771102707)) ;
#116752 = CARTESIAN_POINT('Ctrl Pts',(60.9402651077866,249.097515112934,21.7036388786869)) ;
#116753 = CARTESIAN_POINT('Ctrl Pts',(60.9402651077866,249.135984959003,21.7312589180718)) ;
#116754 = CARTESIAN_POINT('Ctrl Pts',(60.9402651077866,249.187464991094,21.7682198279585)) ;
#116755 = CARTESIAN_POINT('Ctrl Pts',(60.9402651077866,249.236599544122,21.8083274686639)) ;
#116756 = CARTESIAN_POINT('Ctrl Pts',(60.9402651077866,249.283311602843,21.8512528776645)) ;
#116757 = CARTESIAN_POINT('Ctrl Pts',(60.9402651077866,249.302259501122,21.8686647902544)) ;
#116758 = CARTESIAN_POINT('Ctrl Pts',(60.9402651077865,249.320808530131,21.8865408656809)) ;
#116759 = CARTESIAN_POINT('Ctrl Pts',(60.9402651077866,249.338952302437,21.9048611683146)) ;
#116760 = CARTESIAN_POINT('Ctrl Pts',(60.9402651077866,249.348379057922,21.9143796416741)) ;
#116761 = CARTESIAN_POINT('Ctrl Pts',(60.9402651077866,249.357698079696,21.9240198305948)) ;
#116762 = CARTESIAN_POINT('Ctrl Pts',(60.9402651077866,249.36690286865,21.9337731766018)) ;
#116763 = CARTESIAN_POINT('Ctrl Pts',(60.9402651077866,249.411991934883,21.9815493142511)) ;
#116764 = CARTESIAN_POINT('Ctrl Pts',(60.9402651077867,249.454263218238,22.0319508329691)) ;
#116765 = CARTESIAN_POINT('Ctrl Pts',(60.9402651077866,249.493637415392,22.0846181666045)) ;
#116766 = CARTESIAN_POINT('Ctrl Pts',(60.9402651077865,249.524774012978,22.1262668017985)) ;
#116767 = CARTESIAN_POINT('Ctrl Pts',(60.9402651077866,249.554098553236,22.1693335441747)) ;
#116768 = CARTESIAN_POINT('Ctrl Pts',(60.9402651077865,249.581558206979,22.2136591533113)) ;
#116769 = CARTESIAN_POINT('Ctrl Pts',(60.9402651077865,249.59646898522,22.2377282597327)) ;
#116770 = CARTESIAN_POINT('Ctrl Pts',(60.9402651077866,249.610829665203,22.2621688070069)) ;
#116771 = CARTESIAN_POINT('Ctrl Pts',(60.9402651077866,249.624630037462,22.2869568726434)) ;
#116772 = CARTESIAN_POINT('Ctrl Pts',(60.9402651077866,249.630628989966,22.2977321202693)) ;
#116773 = CARTESIAN_POINT('Ctrl Pts',(60.9402651077866,249.636521561056,22.3085723497387)) ;
#116774 = CARTESIAN_POINT('Ctrl Pts',(60.9402651077866,249.642300957031,22.3194639045933)) ;
#116775 = CARTESIAN_POINT('Ctrl Pts',(60.9402651077865,249.674107722661,22.3794053126736)) ;
#116776 = CARTESIAN_POINT('Ctrl Pts',(60.9402651077867,249.702540340268,22.44098849303)) ;
#116777 = CARTESIAN_POINT('Ctrl Pts',(60.9402651077866,249.727510761889,22.503853973586)) ;
#116778 = CARTESIAN_POINT('Ctrl Pts',(60.9402651077866,249.752826501334,22.5675888255631)) ;
#116779 = CARTESIAN_POINT('Ctrl Pts',(60.9402651077866,249.774584244754,22.6326425708184)) ;
#116780 = CARTESIAN_POINT('Ctrl Pts',(60.9402651077865,249.792652789188,22.6986757373846)) ;
#116781 = CARTESIAN_POINT('Ctrl Pts',(60.9402651077865,249.805016882959,22.7438614614688)) ;
#116782 = CARTESIAN_POINT('Ctrl Pts',(60.9402651077865,249.815652686325,22.7895065347492)) ;
#116783 = CARTESIAN_POINT('Ctrl Pts',(60.9402651077866,249.824505428491,22.8355081310719)) ;
#116784 = CARTESIAN_POINT('Ctrl Pts',(60.9402651077867,249.828929431581,22.8584966244073)) ;
#116785 = CARTESIAN_POINT('Ctrl Pts',(60.9402651077868,249.832907974007,22.8815742098594)) ;
#116786 = CARTESIAN_POINT('Ctrl Pts',(60.9402651077866,249.836433132633,22.9047282989318)) ;
#116787 = CARTESIAN_POINT('Ctrl Pts',(60.9402651077865,249.838694859355,22.9195838636081)) ;
#116788 = CARTESIAN_POINT('Ctrl Pts',(60.9402651077866,249.840769937873,22.9344709232824)) ;
#116789 = CARTESIAN_POINT('Ctrl Pts',(60.9402651077865,249.842656107631,22.9493861700344)) ;
#116790 = CARTESIAN_POINT('Ctrl Pts',(60.9402651077865,249.844045727851,22.9603748567076)) ;
#116791 = CARTESIAN_POINT('Ctrl Pts',(60.9402651077865,249.84533163955,22.9713696735096)) ;
#116792 = CARTESIAN_POINT('Ctrl Pts',(60.9402651077865,249.84651329604,22.9823679509404)) ;
#116793 = CARTESIAN_POINT('Ctrl Pts',(60.9402651077866,249.853975477243,23.0518222634181)) ;
#116794 = CARTESIAN_POINT('Ctrl Pts',(60.9402651077866,249.857285781381,23.1214286108591)) ;
#116795 = CARTESIAN_POINT('Ctrl Pts',(60.9402651077865,249.856319412001,23.1908363594129)) ;
#116796 = CARTESIAN_POINT('Ctrl Pts',(60.9402651077864,249.856026793893,23.2118531305353)) ;
#116797 = CARTESIAN_POINT('Ctrl Pts',(60.9402651077868,249.855341726161,23.2328518457626)) ;
#116798 = CARTESIAN_POINT('Ctrl Pts',(60.9402651077867,249.854259856848,23.2538231020334)) ;
#116799 = CARTESIAN_POINT('Ctrl Pts',(60.9402651077866,249.850793622953,23.3210135458965)) ;
#116800 = CARTESIAN_POINT('Ctrl Pts',(60.9402651077866,249.843258202366,23.3879219235019)) ;
#116801 = CARTESIAN_POINT('Ctrl Pts',(60.9402651077865,249.831876107148,23.4543055732081)) ;
#116802 = CARTESIAN_POINT('Ctrl Pts',(60.9402651077864,249.825943828568,23.4889043263943)) ;
#116803 = CARTESIAN_POINT('Ctrl Pts',(60.9402651077865,249.818965749739,23.5233606026032)) ;
#116804 = CARTESIAN_POINT('Ctrl Pts',(60.9402651077864,249.810967923841,23.5576398472338)) ;
#116805 = CARTESIAN_POINT('Ctrl Pts',(60.9402651077864,249.806632810109,23.5762204497635)) ;
#116806 = CARTESIAN_POINT('Ctrl Pts',(60.9402651077864,249.801998028691,23.5947490326698)) ;
#116807 = CARTESIAN_POINT('Ctrl Pts',(60.9402651077866,249.797067299182,23.6132200135793)) ;
#116808 = CARTESIAN_POINT('Ctrl Pts',(60.9402651077867,249.794086739133,23.6243854745273)) ;
#116809 = CARTESIAN_POINT('Ctrl Pts',(60.9402651077865,249.790998032701,23.6355298861929)) ;
#116810 = CARTESIAN_POINT('Ctrl Pts',(60.9402651077866,249.787801949933,23.6466520013255)) ;
#116811 = CARTESIAN_POINT('Ctrl Pts',(60.9402651077867,249.784265075083,23.6589600459386)) ;
#116812 = CARTESIAN_POINT('Ctrl Pts',(60.9402651077866,249.780599005193,23.671232613158)) ;
#116813 = CARTESIAN_POINT('Ctrl Pts',(60.9402651077866,249.776807401206,23.6834616436752)) ;
#116814 = CARTESIAN_POINT('Ctrl Pts',(60.9402651077866,249.755950457756,23.7507313793397)) ;
#116815 = CARTESIAN_POINT('Ctrl Pts',(60.9402651077866,249.731281914511,23.816745182075)) ;
#116816 = CARTESIAN_POINT('Ctrl Pts',(60.9402651077866,249.703069382292,23.8812387082105)) ;
#116817 = CARTESIAN_POINT('Ctrl Pts',(60.9402651077866,249.674856850073,23.9457322343459)) ;
#116818 = CARTESIAN_POINT('Ctrl Pts',(60.9402651077867,249.643099881907,24.0087063454738)) ;
#116819 = CARTESIAN_POINT('Ctrl Pts',(60.9402651077868,249.608013003586,24.0698922112783)) ;
#116820 = CARTESIAN_POINT('Ctrl Pts',(60.9402651077869,249.572487613619,24.1318427707814)) ;
#116821 = CARTESIAN_POINT('Ctrl Pts',(60.9402651077866,249.53354820023,24.1919610672433)) ;
#116822 = CARTESIAN_POINT('Ctrl Pts',(60.9402651077867,249.491368953434,24.2499496790592)) ;
#116823 = CARTESIAN_POINT('Ctrl Pts',(60.9402651077867,249.481720037426,24.2632151422266)) ;
#116824 = CARTESIAN_POINT('Ctrl Pts',(60.9402651077867,249.471901392435,24.2763690469256)) ;
#116825 = CARTESIAN_POINT('Ctrl Pts',(60.9402651077868,249.461914784373,24.2894076162287)) ;
#116826 = CARTESIAN_POINT('Ctrl Pts',(60.9402651077868,249.454834323785,24.2986519037288)) ;
#116827 = CARTESIAN_POINT('Ctrl Pts',(60.9402651077866,249.44766976387,24.3078376489109)) ;
#116828 = CARTESIAN_POINT('Ctrl Pts',(60.9402651077866,249.440430193774,24.3169532133058)) ;
#116829 = CARTESIAN_POINT('Ctrl Pts',(60.9402651077866,249.394852937774,24.3743409319824)) ;
#116830 = CARTESIAN_POINT('Ctrl Pts',(60.9402651077865,249.346224208465,24.4290572871775)) ;
#116831 = CARTESIAN_POINT('Ctrl Pts',(60.9402651077866,249.294783585182,24.4808204376118)) ;
#116832 = CARTESIAN_POINT('Ctrl Pts',(60.9402651077867,249.243428794205,24.5324972175814)) ;
#116833 = CARTESIAN_POINT('Ctrl Pts',(60.9402651077866,249.189270959674,24.5812315801778)) ;
#116834 = CARTESIAN_POINT('Ctrl Pts',(60.9402651077867,249.132502121971,24.6267202980104)) ;
#116835 = CARTESIAN_POINT('Ctrl Pts',(60.9402651077868,249.077177770065,24.6710515532367)) ;
#116836 = CARTESIAN_POINT('Ctrl Pts',(60.9402651077868,249.019372982206,24.7123009755837)) ;
#116837 = CARTESIAN_POINT('Ctrl Pts',(60.9402651077867,248.959230111589,24.7501540590356)) ;
#116838 = CARTESIAN_POINT('Ctrl Pts',(60.9402651077867,248.937186588349,24.7640279449378)) ;
#116839 = CARTESIAN_POINT('Ctrl Pts',(60.9402651077866,248.914828670669,24.7774451898368)) ;
#116840 = CARTESIAN_POINT('Ctrl Pts',(60.9402651077866,248.892162375845,24.7903888257488)) ;
#116841 = CARTESIAN_POINT('Origin',(60.9402651077866,248.040265107786,23.0213203435596)) ;
#116842 = CARTESIAN_POINT('Ctrl Pts',(60.9402651077865,247.14398687089,24.7683227969254)) ;
#116843 = CARTESIAN_POINT('Ctrl Pts',(60.9402651077865,247.110696623296,24.7483652569324)) ;
#116844 = CARTESIAN_POINT('Ctrl Pts',(60.9402651077865,247.078078487436,24.7273686112138)) ;
#116845 = CARTESIAN_POINT('Ctrl Pts',(60.9402651077865,247.046187815054,24.7053297595934)) ;
#116846 = CARTESIAN_POINT('Ctrl Pts',(60.9402651077865,246.986660772535,24.6641920989713)) ;
#116847 = CARTESIAN_POINT('Ctrl Pts',(60.9402651077865,246.929665910612,24.6194250575563)) ;
#116848 = CARTESIAN_POINT('Ctrl Pts',(60.9402651077866,246.875361631822,24.5713686455035)) ;
#116849 = CARTESIAN_POINT('Ctrl Pts',(60.9402651077866,246.857636515018,24.5556828554362)) ;
#116850 = CARTESIAN_POINT('Ctrl Pts',(60.9402651077866,246.84019837111,24.5396463558629)) ;
#116851 = CARTESIAN_POINT('Ctrl Pts',(60.9402651077867,246.823053678133,24.5232702993519)) ;
#116852 = CARTESIAN_POINT('Ctrl Pts',(60.9402651077867,246.810403115074,24.5111868904612)) ;
#116853 = CARTESIAN_POINT('Ctrl Pts',(60.9402651077867,246.797912332271,24.4989186024479)) ;
#116854 = CARTESIAN_POINT('Ctrl Pts',(60.9402651077866,246.785584111923,24.4864698302042)) ;
#116855 = CARTESIAN_POINT('Ctrl Pts',(60.9402651077866,246.774650795282,24.4754296017774)) ;
#116856 = CARTESIAN_POINT('Ctrl Pts',(60.9402651077867,246.763851231069,24.4642533032112)) ;
#116857 = CARTESIAN_POINT('Ctrl Pts',(60.9402651077867,246.753191015033,24.4529488260821)) ;
#116858 = CARTESIAN_POINT('Ctrl Pts',(60.9402651077866,246.703495389042,24.4002497939465)) ;
#116859 = CARTESIAN_POINT('Ctrl Pts',(60.9402651077865,246.656795094732,24.3447378110376)) ;
#116860 = CARTESIAN_POINT('Ctrl Pts',(60.9402651077865,246.613248450744,24.2867545689444)) ;
#116861 = CARTESIAN_POINT('Ctrl Pts',(60.9402651077865,246.581310448125,24.2442284689238)) ;
#116862 = CARTESIAN_POINT('Ctrl Pts',(60.9402651077867,246.55106963218,24.2003722343513)) ;
#116863 = CARTESIAN_POINT('Ctrl Pts',(60.9402651077866,246.522604506068,24.1553129600453)) ;
#116864 = CARTESIAN_POINT('Ctrl Pts',(60.9402651077866,246.510616937053,24.136337067987)) ;
#116865 = CARTESIAN_POINT('Ctrl Pts',(60.9402651077867,246.498944465043,24.11714775866)) ;
#116866 = CARTESIAN_POINT('Ctrl Pts',(60.9402651077866,246.487593742736,24.0977543412124)) ;
#116867 = CARTESIAN_POINT('Ctrl Pts',(60.9402651077865,246.480956285133,24.08641383066)) ;
#116868 = CARTESIAN_POINT('Ctrl Pts',(60.9402651077866,246.474428082592,24.0750019825718)) ;
#116869 = CARTESIAN_POINT('Ctrl Pts',(60.9402651077866,246.468018497233,24.0635353483554)) ;
#116870 = CARTESIAN_POINT('Ctrl Pts',(60.9402651077868,246.433160377772,24.0011747925748)) ;
#116871 = CARTESIAN_POINT('Ctrl Pts',(60.9402651077867,246.401752337816,23.937105062428)) ;
#116872 = CARTESIAN_POINT('Ctrl Pts',(60.9402651077866,246.373944316263,23.8716485339039)) ;
#116873 = CARTESIAN_POINT('Ctrl Pts',(60.9402651077865,246.346636811236,23.8073701573079)) ;
#116874 = CARTESIAN_POINT('Ctrl Pts',(60.9402651077868,246.32280067199,23.7417534653275)) ;
#116875 = CARTESIAN_POINT('Ctrl Pts',(60.9402651077867,246.302625236177,23.6750905947637)) ;
#116876 = CARTESIAN_POINT('Ctrl Pts',(60.9402651077866,246.288518996942,23.6284813215364)) ;
#116877 = CARTESIAN_POINT('Ctrl Pts',(60.9402651077865,246.276203267621,23.5813603419321)) ;
#116878 = CARTESIAN_POINT('Ctrl Pts',(60.9402651077867,246.265757835163,23.53382736178)) ;
#116879 = CARTESIAN_POINT('Ctrl Pts',(60.9402651077868,246.257092882906,23.4943966340122)) ;
#116880 = CARTESIAN_POINT('Ctrl Pts',(60.9402651077865,246.249715171408,23.454682352912)) ;
#116881 = CARTESIAN_POINT('Ctrl Pts',(60.9402651077866,246.243677247182,23.414742639793)) ;
#116882 = CARTESIAN_POINT('Ctrl Pts',(60.9402651077867,246.241926884875,23.4031643281448)) ;
#116883 = CARTESIAN_POINT('Ctrl Pts',(60.9402651077865,246.240289232283,23.3915669160736)) ;
#116884 = CARTESIAN_POINT('Ctrl Pts',(60.9402651077865,246.23876732204,23.3799665803396)) ;
#116885 = CARTESIAN_POINT('Ctrl Pts',(60.9402651077868,246.229937787811,23.312665921877)) ;
#116886 = CARTESIAN_POINT('Ctrl Pts',(60.9402651077865,246.224980478258,23.2451443288552)) ;
#116887 = CARTESIAN_POINT('Ctrl Pts',(60.9402651077866,246.224066368655,23.177676364878)) ;
#116888 = CARTESIAN_POINT('Ctrl Pts',(60.9402651077867,246.223715971633,23.1518145059036)) ;
#116889 = CARTESIAN_POINT('Ctrl Pts',(60.9402651077866,246.22396019596,23.1259605167808)) ;
#116890 = CARTESIAN_POINT('Ctrl Pts',(60.9402651077866,246.22481072392,23.1001299806353)) ;
#116891 = CARTESIAN_POINT('Ctrl Pts',(60.9402651077866,246.227062239739,23.0317514399507)) ;
#116892 = CARTESIAN_POINT('Ctrl Pts',(60.9402651077865,246.23355904935,22.9635359717512)) ;
#116893 = CARTESIAN_POINT('Ctrl Pts',(60.9402651077865,246.244123442748,22.895788639393)) ;
#116894 = CARTESIAN_POINT('Ctrl Pts',(60.9402651077865,246.249247050823,22.8629319701989)) ;
#116895 = CARTESIAN_POINT('Ctrl Pts',(60.9402651077865,246.255328156535,22.8301856656148)) ;
#116896 = CARTESIAN_POINT('Ctrl Pts',(60.9402651077864,246.262350374056,22.7975864532994)) ;
#116897 = CARTESIAN_POINT('Ctrl Pts',(60.9402651077864,246.266430574556,22.7786449548353)) ;
#116898 = CARTESIAN_POINT('Ctrl Pts',(60.9402651077865,246.270828547796,22.759753143661)) ;
#116899 = CARTESIAN_POINT('Ctrl Pts',(60.9402651077865,246.275541428506,22.7409184880431)) ;
#116900 = CARTESIAN_POINT('Ctrl Pts',(60.9402651077866,246.278434058103,22.7293583222674)) ;
#116901 = CARTESIAN_POINT('Ctrl Pts',(60.9402651077867,246.281445780643,22.7178180138917)) ;
#116902 = CARTESIAN_POINT('Ctrl Pts',(60.9402651077867,246.284574538954,22.7063046079789)) ;
#116903 = CARTESIAN_POINT('Ctrl Pts',(60.9402651077867,246.302289420104,22.6411162498198)) ;
#116904 = CARTESIAN_POINT('Ctrl Pts',(60.9402651077866,246.323683070667,22.5770382879317)) ;
#116905 = CARTESIAN_POINT('Ctrl Pts',(60.9402651077866,246.348552607161,22.5143506693262)) ;
#116906 = CARTESIAN_POINT('Ctrl Pts',(60.9402651077866,246.373476863233,22.4515251213285)) ;
#116907 = CARTESIAN_POINT('Ctrl Pts',(60.9402651077865,246.401892937332,22.3900951413175)) ;
#116908 = CARTESIAN_POINT('Ctrl Pts',(60.9402651077866,246.433642655425,22.3303661652523)) ;
#116909 = CARTESIAN_POINT('Ctrl Pts',(60.9402651077867,246.465163048057,22.2710686064036)) ;
#116910 = CARTESIAN_POINT('Ctrl Pts',(60.9402651077867,246.499969738244,22.2134467522368)) ;
#116911 = CARTESIAN_POINT('Ctrl Pts',(60.9402651077868,246.537943823293,22.1578354708785)) ;
#116912 = CARTESIAN_POINT('Ctrl Pts',(60.9402651077868,246.547010825524,22.1445572678233)) ;
#116913 = CARTESIAN_POINT('Ctrl Pts',(60.9402651077867,246.556258539357,22.1313938813587)) ;
#116914 = CARTESIAN_POINT('Ctrl Pts',(60.9402651077867,246.565685590736,22.1183502553737)) ;
#116915 = CARTESIAN_POINT('Ctrl Pts',(60.9402651077867,246.575081295221,22.10535000214)) ;
#116916 = CARTESIAN_POINT('Ctrl Pts',(60.9402651077867,246.584658747915,22.0924642306346)) ;
#116917 = CARTESIAN_POINT('Ctrl Pts',(60.9402651077866,246.594396472188,22.0797237413789)) ;
#116918 = CARTESIAN_POINT('Ctrl Pts',(60.9402651077865,246.634516348228,22.0272323342157)) ;
#116919 = CARTESIAN_POINT('Ctrl Pts',(60.9402651077865,246.677403336317,21.9771313640338)) ;
#116920 = CARTESIAN_POINT('Ctrl Pts',(60.9402651077865,246.722906620125,21.9297036362799)) ;
#116921 = CARTESIAN_POINT('Ctrl Pts',(60.9402651077866,246.767658732713,21.8830588485941)) ;
#116922 = CARTESIAN_POINT('Ctrl Pts',(60.9402651077868,246.814942126786,21.8389991203923)) ;
#116923 = CARTESIAN_POINT('Ctrl Pts',(60.9402651077867,246.864643798312,21.7978329077263)) ;
#116924 = CARTESIAN_POINT('Ctrl Pts',(60.9402651077866,246.912679449409,21.7580466034055)) ;
#116925 = CARTESIAN_POINT('Ctrl Pts',(60.9402651077866,246.962974558538,21.7209626850137)) ;
#116926 = CARTESIAN_POINT('Ctrl Pts',(60.9402651077867,247.015446740337,21.686904114294)) ;
#116927 = CARTESIAN_POINT('Ctrl Pts',(60.9402651077867,247.03205539854,21.6761237895472)) ;
#116928 = CARTESIAN_POINT('Ctrl Pts',(60.9402651077866,247.048882288002,21.6656469321673)) ;
#116929 = CARTESIAN_POINT('Ctrl Pts',(60.9402651077866,247.065925086493,21.6554848536835)) ;
#116930 = CARTESIAN_POINT('Ctrl Pts',(61.1067325548923,246.899092893641,21.4203834081426)) ;
#116931 = CARTESIAN_POINT('Ctrl Pts',(61.080348061988,246.368276064864,21.7987339961471)) ;
#116932 = CARTESIAN_POINT('Ctrl Pts',(61.0275887537553,245.722609719904,23.1197710503415)) ;
#116933 = CARTESIAN_POINT('Ctrl Pts',(60.948454630194,246.859463067054,25.0213439274063)) ;
#116934 = CARTESIAN_POINT('Ctrl Pts',(60.8693301842085,249.073180249221,25.1000285863252)) ;
#116935 = CARTESIAN_POINT('Ctrl Pts',(60.7902057382229,250.346067934117,23.2890963835466)) ;
#116936 = CARTESIAN_POINT('Ctrl Pts',(60.7110812922374,249.521590130723,21.2338246910011)) ;
#116937 = CARTESIAN_POINT('Ctrl Pts',(60.6319568462519,247.349118393682,20.8052161888267)) ;
#116938 = CARTESIAN_POINT('Ctrl Pts',(60.5528324002664,245.805585994569,22.3927343089783)) ;
#116939 = CARTESIAN_POINT('Ctrl Pts',(60.4737079542808,246.295184926232,24.5522333747062)) ;
#116940 = CARTESIAN_POINT('Ctrl Pts',(60.3945835082953,248.372537959759,25.3188246765677)) ;
#116941 = CARTESIAN_POINT('Ctrl Pts',(60.3154590623098,250.147567314984,23.9950884285102)) ;
#116942 = CARTESIAN_POINT('Ctrl Pts',(60.2363346163243,250.005310554343,21.7853793507168)) ;
#116943 = CARTESIAN_POINT('Ctrl Pts',(60.1572101703387,248.075189857469,20.7001725272112)) ;
#116944 = CARTESIAN_POINT('Ctrl Pts',(60.0780857243532,246.113294619792,21.7268190366224)) ;
#116945 = CARTESIAN_POINT('Ctrl Pts',(59.9989612783677,245.904618567983,23.9312451899875)) ;
#116946 = CARTESIAN_POINT('Ctrl Pts',(59.9198368323822,247.639022645035,25.307792121131)) ;
#116947 = CARTESIAN_POINT('Ctrl Pts',(59.8407123863967,249.738489903116,24.6040336728245)) ;
#116948 = CARTESIAN_POINT('Ctrl Pts',(59.7615879404111,250.292857693394,22.4602716766755)) ;
#116949 = CARTESIAN_POINT('Ctrl Pts',(59.6824634944256,248.797744299413,20.8269698304018)) ;
#116950 = CARTESIAN_POINT('Ctrl Pts',(59.6033390484401,246.613451994329,21.1901586184867)) ;
#116951 = CARTESIAN_POINT('Ctrl Pts',(59.5242146024546,245.727320128136,23.2193972255469)) ;
#116952 = CARTESIAN_POINT('Ctrl Pts',(59.4450901564691,246.945579975629,25.0684191163454)) ;
#116953 = CARTESIAN_POINT('Ctrl Pts',(59.3659657104835,249.159819545126,25.0549247205655)) ;
#116954 = CARTESIAN_POINT('Ctrl Pts',(59.286841264498,250.355452505948,23.1911916911607)) ;
#116955 = CARTESIAN_POINT('Ctrl Pts',(59.2077168185125,249.444653504094,21.1729042187596)) ;
#116956 = CARTESIAN_POINT('Ctrl Pts',(59.1285923725269,247.256096849426,20.8363652304909)) ;
#116957 = CARTESIAN_POINT('Ctrl Pts',(59.0494679265414,245.78100155116,22.4877685177501)) ;
#116958 = CARTESIAN_POINT('Ctrl Pts',(58.9703434805559,246.361457172664,24.624614705875)) ;
#116959 = CARTESIAN_POINT('Ctrl Pts',(58.8912190345704,248.469345593264,25.3027314990645)) ;
#116960 = CARTESIAN_POINT('Ctrl Pts',(58.8120945885848,250.186844164077,23.9051484376557)) ;
#116961 = CARTESIAN_POINT('Ctrl Pts',(58.7329701425994,249.951313140653,21.7034272174656)) ;
#116962 = CARTESIAN_POINT('Ctrl Pts',(58.6538456966138,247.977055527801,20.7007738653896)) ;
#116963 = CARTESIAN_POINT('Ctrl Pts',(58.5747212506283,246.060294351269,21.8094146738284)) ;
#116964 = CARTESIAN_POINT('Ctrl Pts',(58.4955968046428,245.945003682052,24.0207155105206)) ;
#116965 = CARTESIAN_POINT('Ctrl Pts',(58.4164723586572,247.735985960427,25.3226711654736)) ;
#116966 = CARTESIAN_POINT('Ctrl Pts',(58.3373479126717,249.803947954416,24.5309187497578)) ;
#116967 = CARTESIAN_POINT('Ctrl Pts',(58.2582234666862,250.266963056667,22.365388238877)) ;
#116968 = CARTESIAN_POINT('Ctrl Pts',(58.1790990207007,248.704697564139,20.7972539868847)) ;
#116969 = CARTESIAN_POINT('Ctrl Pts',(58.0999745747151,246.536593225254,21.2511907819118)) ;
#116970 = CARTESIAN_POINT('Ctrl Pts',(58.0208501287296,245.739715191048,23.3181208433496)) ;
#116971 = CARTESIAN_POINT('Ctrl Pts',(57.9681004980726,246.600182354009,24.5099551564717)) ;
#116972 = CARTESIAN_POINT('Ctrl Pts',(57.9417256827441,247.187270248071,24.7926681085687)) ;
#116973 = CARTESIAN_POINT('Ctrl Pts',(61.0506450234148,246.955481069846,21.4994897103189)) ;
#116974 = CARTESIAN_POINT('Ctrl Pts',(61.0242605305105,246.450893229562,21.8591450485099)) ;
#116975 = CARTESIAN_POINT('Ctrl Pts',(60.9715012222777,245.837130875234,23.1149063544326)) ;
#116976 = CARTESIAN_POINT('Ctrl Pts',(60.8923670987165,246.91780945221,24.9225177547551)) ;
#116977 = CARTESIAN_POINT('Ctrl Pts',(60.813242652731,249.022141326017,24.9973144076774)) ;
#116978 = CARTESIAN_POINT('Ctrl Pts',(60.7341182067454,250.232132443528,23.2758648989914)) ;
#116979 = CARTESIAN_POINT('Ctrl Pts',(60.6549937607599,249.448394152609,21.3221493264703)) ;
#116980 = CARTESIAN_POINT('Ctrl Pts',(60.5758693147743,247.38326968322,20.9147194434772)) ;
#116981 = CARTESIAN_POINT('Ctrl Pts',(60.4967448687889,245.916007084424,22.4237943187109)) ;
#116982 = CARTESIAN_POINT('Ctrl Pts',(60.4176204228033,246.381413707085,24.4765871289558)) ;
#116983 = CARTESIAN_POINT('Ctrl Pts',(60.3384959768178,248.356119526246,25.2052992353106)) ;
#116984 = CARTESIAN_POINT('Ctrl Pts',(60.2593715308323,250.043440236965,23.9469721094513)) ;
#116985 = CARTESIAN_POINT('Ctrl Pts',(60.1802470848468,249.908212739029,21.8464502895457)) ;
#116986 = CARTESIAN_POINT('Ctrl Pts',(60.1011226388612,248.073464138147,20.8148662521754)) ;
#116987 = CARTESIAN_POINT('Ctrl Pts',(60.0219981928757,246.208511056077,21.7907835871857)) ;
#116988 = CARTESIAN_POINT('Ctrl Pts',(59.9428737468902,246.010146210441,23.8862835251857)) ;
#116989 = CARTESIAN_POINT('Ctrl Pts',(59.8637493009047,247.658849039693,25.1948118260597)) ;
#116990 = CARTESIAN_POINT('Ctrl Pts',(59.7846248549191,249.654576364206,24.5258278446539)) ;
#116991 = CARTESIAN_POINT('Ctrl Pts',(59.7055004089336,250.18155145402,22.4879944959797)) ;
#116992 = CARTESIAN_POINT('Ctrl Pts',(59.6263759629481,248.760315356087,20.9353981831583)) ;
#116993 = CARTESIAN_POINT('Ctrl Pts',(59.5472515169626,246.683954402516,21.2806409039238)) ;
#116994 = CARTESIAN_POINT('Ctrl Pts',(59.468127070977,245.841608530402,23.2096097508913)) ;
#116995 = CARTESIAN_POINT('Ctrl Pts',(59.3890026249916,246.999671108725,24.9672668407485)) ;
#116996 = CARTESIAN_POINT('Ctrl Pts',(59.309878179006,249.104499557396,24.9544392368494)) ;
#116997 = CARTESIAN_POINT('Ctrl Pts',(59.2307537330205,250.24105330017,23.1827979225761)) ;
#116998 = CARTESIAN_POINT('Ctrl Pts',(59.151629287035,249.375259157325,21.2642390872863)) ;
#116999 = CARTESIAN_POINT('Ctrl Pts',(59.0725048410494,247.29484456636,20.9443293330062)) ;
#117000 = CARTESIAN_POINT('Ctrl Pts',(58.9933803950639,245.892637419915,22.5141326492943)) ;
#117001 = CARTESIAN_POINT('Ctrl Pts',(58.9142559490784,246.444411275898,24.5453919173336)) ;
#117002 = CARTESIAN_POINT('Ctrl Pts',(58.8351315030929,248.448143652206,25.1900012619997)) ;
#117003 = CARTESIAN_POINT('Ctrl Pts',(58.7560070571073,250.080776318608,23.8614762787238)) ;
#117004 = CARTESIAN_POINT('Ctrl Pts',(58.6768826111218,249.85688347274,21.7685476163785)) ;
#117005 = CARTESIAN_POINT('Ctrl Pts',(58.5977581651363,247.980178871404,20.8154378767288)) ;
#117006 = CARTESIAN_POINT('Ctrl Pts',(58.5186337191508,246.158129663517,21.8692979671662)) ;
#117007 = CARTESIAN_POINT('Ctrl Pts',(58.4395092731652,246.048535794914,23.9713328931781)) ;
#117008 = CARTESIAN_POINT('Ctrl Pts',(58.3603848271797,247.751021154908,25.2089556595693)) ;
#117009 = CARTESIAN_POINT('Ctrl Pts',(58.2812603811942,249.716799969307,24.4563257129906)) ;
#117010 = CARTESIAN_POINT('Ctrl Pts',(58.2021359352087,250.156936336125,22.3977994863984)) ;
#117011 = CARTESIAN_POINT('Ctrl Pts',(58.1230114892231,248.671866292958,20.9071506738677)) ;
#117012 = CARTESIAN_POINT('Ctrl Pts',(58.0438870432376,246.610893417648,21.3386573153505)) ;
#117013 = CARTESIAN_POINT('Ctrl Pts',(57.9647625972521,245.853391122223,23.3034551875683)) ;
#117014 = CARTESIAN_POINT('Ctrl Pts',(57.9120129665951,246.671340448346,24.4363979833345)) ;
#117015 = CARTESIAN_POINT('Ctrl Pts',(57.8856381512666,247.229418859696,24.7051413806521)) ;
#117016 = CARTESIAN_POINT('Ctrl Pts',(60.9945574919372,247.011869246051,21.5785960124951)) ;
#117017 = CARTESIAN_POINT('Ctrl Pts',(60.9681729990329,246.533510394261,21.9195561008726)) ;
#117018 = CARTESIAN_POINT('Ctrl Pts',(60.9154136908002,245.951652030563,23.1100416585237)) ;
#117019 = CARTESIAN_POINT('Ctrl Pts',(60.836279567239,246.976155837366,24.8236915821038)) ;
#117020 = CARTESIAN_POINT('Ctrl Pts',(60.7571551212534,248.971102402814,24.8946002290295)) ;
#117021 = CARTESIAN_POINT('Ctrl Pts',(60.6780306752679,250.118196952939,23.2626334144363)) ;
#117022 = CARTESIAN_POINT('Ctrl Pts',(60.5989062292824,249.375198174497,21.4104739619396)) ;
#117023 = CARTESIAN_POINT('Ctrl Pts',(60.5197817832969,247.417420972759,21.0242226981276)) ;
#117024 = CARTESIAN_POINT('Ctrl Pts',(60.4406573373113,246.026428174279,22.4548543284435)) ;
#117025 = CARTESIAN_POINT('Ctrl Pts',(60.3615328913258,246.467642487938,24.4009408832055)) ;
#117026 = CARTESIAN_POINT('Ctrl Pts',(60.2824084453403,248.339701092733,25.0917737940535)) ;
#117027 = CARTESIAN_POINT('Ctrl Pts',(60.2032839993548,249.939313158944,23.8988557903925)) ;
#117028 = CARTESIAN_POINT('Ctrl Pts',(60.1241595533693,249.811114923714,21.9075212283746)) ;
#117029 = CARTESIAN_POINT('Ctrl Pts',(60.0450351073837,248.071738418825,20.9295599771395)) ;
#117030 = CARTESIAN_POINT('Ctrl Pts',(59.9659106613982,246.303727492363,21.854748137749)) ;
#117031 = CARTESIAN_POINT('Ctrl Pts',(59.8867862154127,246.1156738529,23.8413218603838)) ;
#117032 = CARTESIAN_POINT('Ctrl Pts',(59.8076617694271,247.67867543435,25.0818315309884)) ;
#117033 = CARTESIAN_POINT('Ctrl Pts',(59.7285373234416,249.570662825296,24.4476220164834)) ;
#117034 = CARTESIAN_POINT('Ctrl Pts',(59.6494128774561,250.070245214644,22.515717315284)) ;
#117035 = CARTESIAN_POINT('Ctrl Pts',(59.5702884314706,248.722886412761,21.0438265359149)) ;
#117036 = CARTESIAN_POINT('Ctrl Pts',(59.4911639854851,246.754456810702,21.3711231893609)) ;
#117037 = CARTESIAN_POINT('Ctrl Pts',(59.4120395394995,245.955896932668,23.1998222762357)) ;
#117038 = CARTESIAN_POINT('Ctrl Pts',(59.332915093514,247.053762241821,24.8661145651516)) ;
#117039 = CARTESIAN_POINT('Ctrl Pts',(59.2537906475285,249.049179569667,24.8539537531333)) ;
#117040 = CARTESIAN_POINT('Ctrl Pts',(59.174666201543,250.126654094392,23.1744041539915)) ;
#117041 = CARTESIAN_POINT('Ctrl Pts',(59.0955417555573,249.305864810557,21.355573955813)) ;
#117042 = CARTESIAN_POINT('Ctrl Pts',(59.0164173095719,247.333592283294,21.0522934355215)) ;
#117043 = CARTESIAN_POINT('Ctrl Pts',(58.9372928635864,246.004273288669,22.5404967808384)) ;
#117044 = CARTESIAN_POINT('Ctrl Pts',(58.8581684176009,246.527365379132,24.4661691287921)) ;
#117045 = CARTESIAN_POINT('Ctrl Pts',(58.7790439716154,248.426941711148,25.0772710249347)) ;
#117046 = CARTESIAN_POINT('Ctrl Pts',(58.6999195256298,249.974708473138,23.817804119792)) ;
#117047 = CARTESIAN_POINT('Ctrl Pts',(58.6207950796443,249.762453804827,21.8336680152914)) ;
#117048 = CARTESIAN_POINT('Ctrl Pts',(58.5416706336588,247.983302215006,20.9301018880681)) ;
#117049 = CARTESIAN_POINT('Ctrl Pts',(58.4625461876733,246.255964975764,21.9291812605039)) ;
#117050 = CARTESIAN_POINT('Ctrl Pts',(58.3834217416877,246.152067907775,23.9219502758357)) ;
#117051 = CARTESIAN_POINT('Ctrl Pts',(58.3042972957023,247.76605634939,25.095240153665)) ;
#117052 = CARTESIAN_POINT('Ctrl Pts',(58.2251728497167,249.629651984198,24.3817326762235)) ;
#117053 = CARTESIAN_POINT('Ctrl Pts',(58.1460484037312,250.046909615583,22.4302107339199)) ;
#117054 = CARTESIAN_POINT('Ctrl Pts',(58.0669239577456,248.639035021779,21.0170473608507)) ;
#117055 = CARTESIAN_POINT('Ctrl Pts',(57.9877995117601,246.685193610043,21.426123848789)) ;
#117056 = CARTESIAN_POINT('Ctrl Pts',(57.9086750657746,245.967067053397,23.288789531787)) ;
#117057 = CARTESIAN_POINT('Ctrl Pts',(57.8559254351176,246.742498542684,24.3628408101973)) ;
#117058 = CARTESIAN_POINT('Ctrl Pts',(57.8295506197891,247.271567471321,24.6176146527354)) ;
#117059 = CARTESIAN_POINT('Ctrl Pts',(60.9384699604597,247.068257422256,21.6577023146713)) ;
#117060 = CARTESIAN_POINT('Ctrl Pts',(60.9120854675554,246.616127558959,21.9799671532354)) ;
#117061 = CARTESIAN_POINT('Ctrl Pts',(60.8593261593227,246.066173185893,23.1051769626147)) ;
#117062 = CARTESIAN_POINT('Ctrl Pts',(60.7801920357613,247.034502222522,24.7248654094525)) ;
#117063 = CARTESIAN_POINT('Ctrl Pts',(60.7010675897758,248.92006347961,24.7918860503816)) ;
#117064 = CARTESIAN_POINT('Ctrl Pts',(60.6219431437903,250.004261462351,23.2494019298812)) ;
#117065 = CARTESIAN_POINT('Ctrl Pts',(60.5428186978048,249.302002196383,21.4987985974089)) ;
#117066 = CARTESIAN_POINT('Ctrl Pts',(60.4636942518192,247.451572262297,21.133725952778)) ;
#117067 = CARTESIAN_POINT('Ctrl Pts',(60.3845698058337,246.136849264134,22.4859143381761)) ;
#117068 = CARTESIAN_POINT('Ctrl Pts',(60.3054453598482,246.553871268792,24.3252946374551)) ;
#117069 = CARTESIAN_POINT('Ctrl Pts',(60.2263209138627,248.32328265922,24.9782483527963)) ;
#117070 = CARTESIAN_POINT('Ctrl Pts',(60.1471964678772,249.835186080924,23.8507394713336)) ;
#117071 = CARTESIAN_POINT('Ctrl Pts',(60.0680720218916,249.714017108399,21.9685921672034)) ;
#117072 = CARTESIAN_POINT('Ctrl Pts',(59.9889475759061,248.070012699505,21.0442537021036)) ;
#117073 = CARTESIAN_POINT('Ctrl Pts',(59.9098231299206,246.398943928648,21.9187126883123)) ;
#117074 = CARTESIAN_POINT('Ctrl Pts',(59.8306986839351,246.221201495357,23.7963601955819)) ;
#117075 = CARTESIAN_POINT('Ctrl Pts',(59.7515742379496,247.698501829009,24.9688512359172)) ;
#117076 = CARTESIAN_POINT('Ctrl Pts',(59.672449791964,249.486749286386,24.3694161883128)) ;
#117077 = CARTESIAN_POINT('Ctrl Pts',(59.5933253459785,249.95893897527,22.5434401345883)) ;
#117078 = CARTESIAN_POINT('Ctrl Pts',(59.5142008999929,248.685457469433,21.1522548886714)) ;
#117079 = CARTESIAN_POINT('Ctrl Pts',(59.4350764540075,246.82495921889,21.4616054747979)) ;
#117080 = CARTESIAN_POINT('Ctrl Pts',(59.3559520080219,246.070185334933,23.1900348015801)) ;
#117081 = CARTESIAN_POINT('Ctrl Pts',(59.2768275620364,247.107853374917,24.7649622895547)) ;
#117082 = CARTESIAN_POINT('Ctrl Pts',(59.1977031160509,248.993859581938,24.7534682694172)) ;
#117083 = CARTESIAN_POINT('Ctrl Pts',(59.1185786700654,250.012254888613,23.166010385407)) ;
#117084 = CARTESIAN_POINT('Ctrl Pts',(59.0394542240798,249.236470463788,21.4469088243396)) ;
#117085 = CARTESIAN_POINT('Ctrl Pts',(58.9603297780943,247.372340000228,21.1602575380368)) ;
#117086 = CARTESIAN_POINT('Ctrl Pts',(58.8812053321088,246.115909157423,22.5668609123824)) ;
#117087 = CARTESIAN_POINT('Ctrl Pts',(58.8020808861232,246.610319482365,24.3869463402507)) ;
#117088 = CARTESIAN_POINT('Ctrl Pts',(58.7229564401378,248.40573977009,24.9645407878698)) ;
#117089 = CARTESIAN_POINT('Ctrl Pts',(58.6438319941522,249.86864062767,23.7741319608601)) ;
#117090 = CARTESIAN_POINT('Ctrl Pts',(58.5647075481667,249.668024136914,21.8987884142042)) ;
#117091 = CARTESIAN_POINT('Ctrl Pts',(58.4855831021812,247.986425558609,21.0447658994073)) ;
#117092 = CARTESIAN_POINT('Ctrl Pts',(58.4064586561957,246.353800288012,21.9890645538417)) ;
#117093 = CARTESIAN_POINT('Ctrl Pts',(58.3273342102101,246.255600020638,23.8725676584932)) ;
#117094 = CARTESIAN_POINT('Ctrl Pts',(58.2482097642246,247.781091543872,24.9815246477607)) ;
#117095 = CARTESIAN_POINT('Ctrl Pts',(58.1690853182391,249.542503999089,24.3071396394564)) ;
#117096 = CARTESIAN_POINT('Ctrl Pts',(58.0899608722536,249.93688289504,22.4626219814414)) ;
#117097 = CARTESIAN_POINT('Ctrl Pts',(58.010836426268,248.6062037506,21.1269440478337)) ;
#117098 = CARTESIAN_POINT('Ctrl Pts',(57.9317119802825,246.759493802438,21.5135903822277)) ;
#117099 = CARTESIAN_POINT('Ctrl Pts',(57.8525875342969,246.080742984571,23.2741238760057)) ;
#117100 = CARTESIAN_POINT('Ctrl Pts',(57.79983790364,246.813656637022,24.2892836370601)) ;
#117101 = CARTESIAN_POINT('Ctrl Pts',(57.7734630883115,247.313716082947,24.5300879248187)) ;
#117102 = CARTESIAN_POINT('Origin',(67.9402651077866,248.040265107786,23.0213203435596)) ;
#117103 = CARTESIAN_POINT('Origin',(55.9402651077866,248.040265107786,23.0213203435596)) ;
#117104 = CARTESIAN_POINT('',(0.,0.,0.)) ;
#117105 = CARTESIAN_POINT('',(0.,0.,0.)) ;
#117106 = CARTESIAN_POINT('',(0.,0.,0.)) ;
#117107 = CARTESIAN_POINT('',(0.,0.,0.)) ;
#117108 = CARTESIAN_POINT('',(0.,0.,0.)) ;
#117109 = CARTESIAN_POINT('',(0.,0.,0.)) ;
#117110 = CARTESIAN_POINT('',(0.,0.,0.)) ;
#117111 = CARTESIAN_POINT('',(0.,0.,0.)) ;
#117112 = CARTESIAN_POINT('',(0.,0.,0.)) ;
#117113 = CARTESIAN_POINT('',(0.,0.,0.)) ;
#117114 = CARTESIAN_POINT('',(0.,0.,0.)) ;
#117115 = CARTESIAN_POINT('',(0.,0.,0.)) ;
#117116 = CARTESIAN_POINT('',(0.,0.,0.)) ;
#117117 = CARTESIAN_POINT('',(0.,0.,0.)) ;
#117118 = CARTESIAN_POINT('',(0.,0.,0.)) ;
#117119 = CARTESIAN_POINT('',(0.,0.,0.)) ;
#117120 = CARTESIAN_POINT('',(0.,0.,0.)) ;
#117121 = CARTESIAN_POINT('',(0.,0.,0.)) ;
#117122 = CARTESIAN_POINT('',(0.,0.,0.)) ;
#117123 = CARTESIAN_POINT('',(0.,0.,0.)) ;
#117124 = CARTESIAN_POINT('',(0.,0.,0.)) ;
#117125 = UNCERTAINTY_MEASURE_WITH_UNIT(LENGTH_MEASURE(0.01),#117171,
'DISTANCE_ACCURACY_VALUE',
'Maximum model space distance between geometric entities at asserted c
onnectivities') ;
#117126 = UNCERTAINTY_MEASURE_WITH_UNIT(LENGTH_MEASURE(0.01),#117171,
'DISTANCE_ACCURACY_VALUE',
'Maximum model space distance between geometric entities at asserted c
onnectivities') ;
#117127 = UNCERTAINTY_MEASURE_WITH_UNIT(LENGTH_MEASURE(0.01),#117171,
'DISTANCE_ACCURACY_VALUE',
'Maximum model space distance between geometric entities at asserted c
onnectivities') ;
#117128 = UNCERTAINTY_MEASURE_WITH_UNIT(LENGTH_MEASURE(0.01),#117171,
'DISTANCE_ACCURACY_VALUE',
'Maximum model space distance between geometric entities at asserted c
onnectivities') ;
#117129 = UNCERTAINTY_MEASURE_WITH_UNIT(LENGTH_MEASURE(0.01),#117171,
'DISTANCE_ACCURACY_VALUE',
'Maximum model space distance between geometric entities at asserted c
onnectivities') ;
#117130 = UNCERTAINTY_MEASURE_WITH_UNIT(LENGTH_MEASURE(0.01),#117171,
'DISTANCE_ACCURACY_VALUE',
'Maximum model space distance between geometric entities at asserted c
onnectivities') ;
#117131 = UNCERTAINTY_MEASURE_WITH_UNIT(LENGTH_MEASURE(0.01),#117171,
'DISTANCE_ACCURACY_VALUE',
'Maximum model space distance between geometric entities at asserted c
onnectivities') ;
#117132 = UNCERTAINTY_MEASURE_WITH_UNIT(LENGTH_MEASURE(0.01),#117171,
'DISTANCE_ACCURACY_VALUE',
'Maximum model space distance between geometric entities at asserted c
onnectivities') ;
#117133 = UNCERTAINTY_MEASURE_WITH_UNIT(LENGTH_MEASURE(0.01),#117171,
'DISTANCE_ACCURACY_VALUE',
'Maximum model space distance between geometric entities at asserted c
onnectivities') ;
#117134 = UNCERTAINTY_MEASURE_WITH_UNIT(LENGTH_MEASURE(0.01),#117171,
'DISTANCE_ACCURACY_VALUE',
'Maximum model space distance between geometric entities at asserted c
onnectivities') ;
#117135 = UNCERTAINTY_MEASURE_WITH_UNIT(LENGTH_MEASURE(0.01),#117171,
'DISTANCE_ACCURACY_VALUE',
'Maximum model space distance between geometric entities at asserted c
onnectivities') ;
#117136 = UNCERTAINTY_MEASURE_WITH_UNIT(LENGTH_MEASURE(0.01),#117171,
'DISTANCE_ACCURACY_VALUE',
'Maximum model space distance between geometric entities at asserted c
onnectivities') ;
#117137 = UNCERTAINTY_MEASURE_WITH_UNIT(LENGTH_MEASURE(0.01),#117171,
'DISTANCE_ACCURACY_VALUE',
'Maximum model space distance between geometric entities at asserted c
onnectivities') ;
#117138 = UNCERTAINTY_MEASURE_WITH_UNIT(LENGTH_MEASURE(0.01),#117171,
'DISTANCE_ACCURACY_VALUE',
'Maximum model space distance between geometric entities at asserted c
onnectivities') ;
#117139 = UNCERTAINTY_MEASURE_WITH_UNIT(LENGTH_MEASURE(0.01),#117171,
'DISTANCE_ACCURACY_VALUE',
'Maximum model space distance between geometric entities at asserted c
onnectivities') ;
#117140 = UNCERTAINTY_MEASURE_WITH_UNIT(LENGTH_MEASURE(0.01),#117171,
'DISTANCE_ACCURACY_VALUE',
'Maximum model space distance between geometric entities at asserted c
onnectivities') ;
#117141 = UNCERTAINTY_MEASURE_WITH_UNIT(LENGTH_MEASURE(0.01),#117171,
'DISTANCE_ACCURACY_VALUE',
'Maximum model space distance between geometric entities at asserted c
onnectivities') ;
#117142 = UNCERTAINTY_MEASURE_WITH_UNIT(LENGTH_MEASURE(0.01),#117171,
'DISTANCE_ACCURACY_VALUE',
'Maximum model space distance between geometric entities at asserted c
onnectivities') ;
#117143 = UNCERTAINTY_MEASURE_WITH_UNIT(LENGTH_MEASURE(0.01),#117171,
'DISTANCE_ACCURACY_VALUE',
'Maximum model space distance between geometric entities at asserted c
onnectivities') ;
#117144 = UNCERTAINTY_MEASURE_WITH_UNIT(LENGTH_MEASURE(0.01),#117171,
'DISTANCE_ACCURACY_VALUE',
'Maximum model space distance between geometric entities at asserted c
onnectivities') ;
#117145 = UNCERTAINTY_MEASURE_WITH_UNIT(LENGTH_MEASURE(0.01),#117171,
'DISTANCE_ACCURACY_VALUE',
'Maximum model space distance between geometric entities at asserted c
onnectivities') ;
#117146 = UNCERTAINTY_MEASURE_WITH_UNIT(LENGTH_MEASURE(0.01),#117171,
'DISTANCE_ACCURACY_VALUE',
'Maximum model space distance between geometric entities at asserted c
onnectivities') ;
#117147 = UNCERTAINTY_MEASURE_WITH_UNIT(LENGTH_MEASURE(0.01),#117171,
'DISTANCE_ACCURACY_VALUE',
'Maximum model space distance between geometric entities at asserted c
onnectivities') ;
#117148 = (
GEOMETRIC_REPRESENTATION_CONTEXT(3)
GLOBAL_UNCERTAINTY_ASSIGNED_CONTEXT((#117125))
GLOBAL_UNIT_ASSIGNED_CONTEXT((#117171,#117173,#117174))
REPRESENTATION_CONTEXT('','3D')
) ;
#117149 = (
GEOMETRIC_REPRESENTATION_CONTEXT(3)
GLOBAL_UNCERTAINTY_ASSIGNED_CONTEXT((#117126))
GLOBAL_UNIT_ASSIGNED_CONTEXT((#117171,#117173,#117174))
REPRESENTATION_CONTEXT('','3D')
) ;
#117150 = (
GEOMETRIC_REPRESENTATION_CONTEXT(3)
GLOBAL_UNCERTAINTY_ASSIGNED_CONTEXT((#117127))
GLOBAL_UNIT_ASSIGNED_CONTEXT((#117171,#117173,#117174))
REPRESENTATION_CONTEXT('','3D')
) ;
#117151 = (
GEOMETRIC_REPRESENTATION_CONTEXT(3)
GLOBAL_UNCERTAINTY_ASSIGNED_CONTEXT((#117128))
GLOBAL_UNIT_ASSIGNED_CONTEXT((#117171,#117173,#117174))
REPRESENTATION_CONTEXT('','3D')
) ;
#117152 = (
GEOMETRIC_REPRESENTATION_CONTEXT(3)
GLOBAL_UNCERTAINTY_ASSIGNED_CONTEXT((#117129))
GLOBAL_UNIT_ASSIGNED_CONTEXT((#117171,#117173,#117174))
REPRESENTATION_CONTEXT('','3D')
) ;
#117153 = (
GEOMETRIC_REPRESENTATION_CONTEXT(3)
GLOBAL_UNCERTAINTY_ASSIGNED_CONTEXT((#117130))
GLOBAL_UNIT_ASSIGNED_CONTEXT((#117171,#117173,#117174))
REPRESENTATION_CONTEXT('','3D')
) ;
#117154 = (
GEOMETRIC_REPRESENTATION_CONTEXT(3)
GLOBAL_UNCERTAINTY_ASSIGNED_CONTEXT((#117131))
GLOBAL_UNIT_ASSIGNED_CONTEXT((#117171,#117173,#117174))
REPRESENTATION_CONTEXT('','3D')
) ;
#117155 = (
GEOMETRIC_REPRESENTATION_CONTEXT(3)
GLOBAL_UNCERTAINTY_ASSIGNED_CONTEXT((#117132))
GLOBAL_UNIT_ASSIGNED_CONTEXT((#117171,#117173,#117174))
REPRESENTATION_CONTEXT('','3D')
) ;
#117156 = (
GEOMETRIC_REPRESENTATION_CONTEXT(3)
GLOBAL_UNCERTAINTY_ASSIGNED_CONTEXT((#117133))
GLOBAL_UNIT_ASSIGNED_CONTEXT((#117171,#117173,#117174))
REPRESENTATION_CONTEXT('','3D')
) ;
#117157 = (
GEOMETRIC_REPRESENTATION_CONTEXT(3)
GLOBAL_UNCERTAINTY_ASSIGNED_CONTEXT((#117134))
GLOBAL_UNIT_ASSIGNED_CONTEXT((#117171,#117173,#117174))
REPRESENTATION_CONTEXT('','3D')
) ;
#117158 = (
GEOMETRIC_REPRESENTATION_CONTEXT(3)
GLOBAL_UNCERTAINTY_ASSIGNED_CONTEXT((#117135))
GLOBAL_UNIT_ASSIGNED_CONTEXT((#117171,#117173,#117174))
REPRESENTATION_CONTEXT('','3D')
) ;
#117159 = (
GEOMETRIC_REPRESENTATION_CONTEXT(3)
GLOBAL_UNCERTAINTY_ASSIGNED_CONTEXT((#117136))
GLOBAL_UNIT_ASSIGNED_CONTEXT((#117171,#117173,#117174))
REPRESENTATION_CONTEXT('','3D')
) ;
#117160 = (
GEOMETRIC_REPRESENTATION_CONTEXT(3)
GLOBAL_UNCERTAINTY_ASSIGNED_CONTEXT((#117137))
GLOBAL_UNIT_ASSIGNED_CONTEXT((#117171,#117173,#117174))
REPRESENTATION_CONTEXT('','3D')
) ;
#117161 = (
GEOMETRIC_REPRESENTATION_CONTEXT(3)
GLOBAL_UNCERTAINTY_ASSIGNED_CONTEXT((#117138))
GLOBAL_UNIT_ASSIGNED_CONTEXT((#117171,#117173,#117174))
REPRESENTATION_CONTEXT('','3D')
) ;
#117162 = (
GEOMETRIC_REPRESENTATION_CONTEXT(3)
GLOBAL_UNCERTAINTY_ASSIGNED_CONTEXT((#117139))
GLOBAL_UNIT_ASSIGNED_CONTEXT((#117171,#117173,#117174))
REPRESENTATION_CONTEXT('','3D')
) ;
#117163 = (
GEOMETRIC_REPRESENTATION_CONTEXT(3)
GLOBAL_UNCERTAINTY_ASSIGNED_CONTEXT((#117140))
GLOBAL_UNIT_ASSIGNED_CONTEXT((#117171,#117173,#117174))
REPRESENTATION_CONTEXT('','3D')
) ;
#117164 = (
GEOMETRIC_REPRESENTATION_CONTEXT(3)
GLOBAL_UNCERTAINTY_ASSIGNED_CONTEXT((#117141))
GLOBAL_UNIT_ASSIGNED_CONTEXT((#117171,#117173,#117174))
REPRESENTATION_CONTEXT('','3D')
) ;
#117165 = (
GEOMETRIC_REPRESENTATION_CONTEXT(3)
GLOBAL_UNCERTAINTY_ASSIGNED_CONTEXT((#117142))
GLOBAL_UNIT_ASSIGNED_CONTEXT((#117171,#117173,#117174))
REPRESENTATION_CONTEXT('','3D')
) ;
#117166 = (
GEOMETRIC_REPRESENTATION_CONTEXT(3)
GLOBAL_UNCERTAINTY_ASSIGNED_CONTEXT((#117143))
GLOBAL_UNIT_ASSIGNED_CONTEXT((#117171,#117173,#117174))
REPRESENTATION_CONTEXT('','3D')
) ;
#117167 = (
GEOMETRIC_REPRESENTATION_CONTEXT(3)
GLOBAL_UNCERTAINTY_ASSIGNED_CONTEXT((#117144))
GLOBAL_UNIT_ASSIGNED_CONTEXT((#117171,#117173,#117174))
REPRESENTATION_CONTEXT('','3D')
) ;
#117168 = (
GEOMETRIC_REPRESENTATION_CONTEXT(3)
GLOBAL_UNCERTAINTY_ASSIGNED_CONTEXT((#117145))
GLOBAL_UNIT_ASSIGNED_CONTEXT((#117171,#117173,#117174))
REPRESENTATION_CONTEXT('','3D')
) ;
#117169 = (
GEOMETRIC_REPRESENTATION_CONTEXT(3)
GLOBAL_UNCERTAINTY_ASSIGNED_CONTEXT((#117146))
GLOBAL_UNIT_ASSIGNED_CONTEXT((#117171,#117173,#117174))
REPRESENTATION_CONTEXT('','3D')
) ;
#117170 = (
GEOMETRIC_REPRESENTATION_CONTEXT(3)
GLOBAL_UNCERTAINTY_ASSIGNED_CONTEXT((#117147))
GLOBAL_UNIT_ASSIGNED_CONTEXT((#117171,#117173,#117174))
REPRESENTATION_CONTEXT('','3D')
) ;
#117171 = (
LENGTH_UNIT()
NAMED_UNIT(*)
SI_UNIT(.MILLI.,.METRE.)
) ;
#117172 = (
LENGTH_UNIT()
NAMED_UNIT(*)
SI_UNIT($,.METRE.)
) ;
#117173 = (
NAMED_UNIT(*)
PLANE_ANGLE_UNIT()
SI_UNIT($,.RADIAN.)
) ;
#117174 = (
NAMED_UNIT(*)
SI_UNIT($,.STERADIAN.)
SOLID_ANGLE_UNIT()
) ;
#117175 = SHAPE_DEFINITION_REPRESENTATION(#117197,#117240) ;
#117176 = SHAPE_DEFINITION_REPRESENTATION(#117198,#117241) ;
#117177 = SHAPE_DEFINITION_REPRESENTATION(#117199,#117242) ;
#117178 = SHAPE_DEFINITION_REPRESENTATION(#117200,#117243) ;
#117179 = SHAPE_DEFINITION_REPRESENTATION(#117201,#117244) ;
#117180 = SHAPE_DEFINITION_REPRESENTATION(#117202,#117245) ;
#117181 = SHAPE_DEFINITION_REPRESENTATION(#117203,#117246) ;
#117182 = SHAPE_DEFINITION_REPRESENTATION(#117204,#117247) ;
#117183 = SHAPE_DEFINITION_REPRESENTATION(#117205,#117248) ;
#117184 = SHAPE_DEFINITION_REPRESENTATION(#117206,#117249) ;
#117185 = SHAPE_DEFINITION_REPRESENTATION(#117207,#117250) ;
#117186 = SHAPE_DEFINITION_REPRESENTATION(#117208,#117251) ;
#117187 = SHAPE_DEFINITION_REPRESENTATION(#117209,#117252) ;
#117188 = SHAPE_DEFINITION_REPRESENTATION(#117210,#117253) ;
#117189 = SHAPE_DEFINITION_REPRESENTATION(#117211,#117254) ;
#117190 = SHAPE_DEFINITION_REPRESENTATION(#117212,#117255) ;
#117191 = SHAPE_DEFINITION_REPRESENTATION(#117213,#117256) ;
#117192 = SHAPE_DEFINITION_REPRESENTATION(#117214,#117257) ;
#117193 = SHAPE_DEFINITION_REPRESENTATION(#117215,#117258) ;
#117194 = SHAPE_DEFINITION_REPRESENTATION(#117216,#117259) ;
#117195 = SHAPE_DEFINITION_REPRESENTATION(#117217,#117260) ;
#117196 = SHAPE_DEFINITION_REPRESENTATION(#117218,#117261) ;
#117197 = PRODUCT_DEFINITION_SHAPE('',$,#117263) ;
#117198 = PRODUCT_DEFINITION_SHAPE('',$,#117264) ;
#117199 = PRODUCT_DEFINITION_SHAPE('',$,#117265) ;
#117200 = PRODUCT_DEFINITION_SHAPE('',$,#117266) ;
#117201 = PRODUCT_DEFINITION_SHAPE('',$,#117267) ;
#117202 = PRODUCT_DEFINITION_SHAPE('',$,#117268) ;
#117203 = PRODUCT_DEFINITION_SHAPE('',$,#117269) ;
#117204 = PRODUCT_DEFINITION_SHAPE('',$,#117270) ;
#117205 = PRODUCT_DEFINITION_SHAPE('',$,#117271) ;
#117206 = PRODUCT_DEFINITION_SHAPE('',$,#117272) ;
#117207 = PRODUCT_DEFINITION_SHAPE('',$,#117273) ;
#117208 = PRODUCT_DEFINITION_SHAPE('',$,#117274) ;
#117209 = PRODUCT_DEFINITION_SHAPE('',$,#117275) ;
#117210 = PRODUCT_DEFINITION_SHAPE('',$,#117276) ;
#117211 = PRODUCT_DEFINITION_SHAPE('',$,#117277) ;
#117212 = PRODUCT_DEFINITION_SHAPE('',$,#117278) ;
#117213 = PRODUCT_DEFINITION_SHAPE('',$,#117279) ;
#117214 = PRODUCT_DEFINITION_SHAPE('',$,#117280) ;
#117215 = PRODUCT_DEFINITION_SHAPE('',$,#117281) ;
#117216 = PRODUCT_DEFINITION_SHAPE('',$,#117282) ;
#117217 = PRODUCT_DEFINITION_SHAPE('',$,#117283) ;
#117218 = PRODUCT_DEFINITION_SHAPE('',$,#117284) ;
#117219 = PRODUCT_DEFINITION_SHAPE($,$,#74) ;
#117220 = PRODUCT_DEFINITION_SHAPE($,$,#75) ;
#117221 = PRODUCT_DEFINITION_SHAPE($,$,#76) ;
#117222 = PRODUCT_DEFINITION_SHAPE($,$,#77) ;
#117223 = PRODUCT_DEFINITION_SHAPE($,$,#78) ;
#117224 = PRODUCT_DEFINITION_SHAPE($,$,#79) ;
#117225 = PRODUCT_DEFINITION_SHAPE($,$,#80) ;
#117226 = PRODUCT_DEFINITION_SHAPE($,$,#81) ;
#117227 = PRODUCT_DEFINITION_SHAPE($,$,#82) ;
#117228 = PRODUCT_DEFINITION_SHAPE($,$,#83) ;
#117229 = PRODUCT_DEFINITION_SHAPE($,$,#84) ;
#117230 = PRODUCT_DEFINITION_SHAPE($,$,#85) ;
#117231 = PRODUCT_DEFINITION_SHAPE($,$,#86) ;
#117232 = PRODUCT_DEFINITION_SHAPE($,$,#87) ;
#117233 = PRODUCT_DEFINITION_SHAPE($,$,#88) ;
#117234 = PRODUCT_DEFINITION_SHAPE($,$,#89) ;
#117235 = PRODUCT_DEFINITION_SHAPE($,$,#90) ;
#117236 = PRODUCT_DEFINITION_SHAPE($,$,#91) ;
#117237 = PRODUCT_DEFINITION_SHAPE($,$,#92) ;
#117238 = PRODUCT_DEFINITION_SHAPE($,$,#93) ;
#117239 = PRODUCT_DEFINITION_SHAPE($,$,#94) ;
#117240 = SHAPE_REPRESENTATION('',(#49310,#55076,#55077,#55078,#55079,#55080,
#55081,#55082,#55083,#55084,#55085,#55086,#55087,#55088,#55089,#55090,#55091,
#55092,#55093,#55094,#55095,#55096),#117148) ;
#117241 = SHAPE_REPRESENTATION('',(#49311),#117149) ;
#117242 = SHAPE_REPRESENTATION('',(#49866),#117150) ;
#117243 = SHAPE_REPRESENTATION('',(#50164),#117151) ;
#117244 = SHAPE_REPRESENTATION('',(#51709),#117152) ;
#117245 = SHAPE_REPRESENTATION('',(#51734),#117153) ;
#117246 = SHAPE_REPRESENTATION('',(#51974),#117154) ;
#117247 = SHAPE_REPRESENTATION('',(#51981),#117155) ;
#117248 = SHAPE_REPRESENTATION('',(#51993),#117156) ;
#117249 = SHAPE_REPRESENTATION('',(#52005),#117157) ;
#117250 = SHAPE_REPRESENTATION('',(#52017),#117158) ;
#117251 = SHAPE_REPRESENTATION('',(#52179),#117159) ;
#117252 = SHAPE_REPRESENTATION('',(#52219),#117160) ;
#117253 = SHAPE_REPRESENTATION('',(#52294),#117161) ;
#117254 = SHAPE_REPRESENTATION('',(#52369),#117162) ;
#117255 = SHAPE_REPRESENTATION('',(#52444),#117163) ;
#117256 = SHAPE_REPRESENTATION('',(#52526),#117164) ;
#117257 = SHAPE_REPRESENTATION('',(#54011),#117165) ;
#117258 = SHAPE_REPRESENTATION('',(#54027),#117166) ;
#117259 = SHAPE_REPRESENTATION('',(#54042),#117167) ;
#117260 = SHAPE_REPRESENTATION('',(#54544),#117168) ;
#117261 = SHAPE_REPRESENTATION('',(#55046),#117169) ;
#117262 = PRODUCT_DEFINITION_CONTEXT('part definition',#117330,'design') ;
#117263 = PRODUCT_DEFINITION('MAS-655','MAS-655',#117285,
#117262) ;
#117264 = PRODUCT_DEFINITION('Vertical_Knob','Vertical_Knob',#117286,#117262) ;
#117265 = PRODUCT_DEFINITION('Clamp_Handle','Clamp_Handle',#117287,#117262) ;
#117266 = PRODUCT_DEFINITION('Base_Plate','Base_Plate',#117288,#117262) ;
#117267 = PRODUCT_DEFINITION('Pin_1','Pin_1',#117289,#117262) ;
#117268 = PRODUCT_DEFINITION('Cover_Plate','Cover_Plate',#117290,#117262) ;
#117269 = PRODUCT_DEFINITION('Pin_2','Pin_2',#117291,#117262) ;
#117270 = PRODUCT_DEFINITION('Spring_Washer_1','Spring_Washer_1',#117292,
#117262) ;
#117271 = PRODUCT_DEFINITION('Spring_Washer_2','Spring_Washer_2',#117293,
#117262) ;
#117272 = PRODUCT_DEFINITION('Spring_Washer_3','Spring_Washer_3',#117294,
#117262) ;
#117273 = PRODUCT_DEFINITION('Washer_1','Washer_1',#117295,#117262) ;
#117274 = PRODUCT_DEFINITION('Washer_2','Washer_2',#117296,#117262) ;
#117275 = PRODUCT_DEFINITION('Spacer_1','Spacer_1',#117297,#117262) ;
#117276 = PRODUCT_DEFINITION('Spacer_2','Spacer_2',#117298,#117262) ;
#117277 = PRODUCT_DEFINITION('Spacer_3','Spacer_3',#117299,#117262) ;
#117278 = PRODUCT_DEFINITION('Latch','Latch',#117300,#117262) ;
#117279 = PRODUCT_DEFINITION('Housing','Housing',#117301,#117262) ;
#117280 = PRODUCT_DEFINITION('Lever_Pin','Lever_Pin',#117302,#117262) ;
#117281 = PRODUCT_DEFINITION('Knob_Shaft','Knob_Shaft',#117303,#117262) ;
#117282 = PRODUCT_DEFINITION('Knob_Grip_1','Knob_Grip_1',#117304,#117262) ;
#117283 = PRODUCT_DEFINITION('Knob_Grip_2','Knob_Grip_2',#117305,#117262) ;
#117284 = PRODUCT_DEFINITION('Knob_Pin','Knob_Pin',#117306,#117262) ;
#117285 = PRODUCT_DEFINITION_FORMATION('',$,#117332) ;
#117286 = PRODUCT_DEFINITION_FORMATION('',$,#117333) ;
#117287 = PRODUCT_DEFINITION_FORMATION('',$,#117334) ;
#117288 = PRODUCT_DEFINITION_FORMATION('',$,#117335) ;
#117289 = PRODUCT_DEFINITION_FORMATION('',$,#117336) ;
#117290 = PRODUCT_DEFINITION_FORMATION('',$,#117337) ;
#117291 = PRODUCT_DEFINITION_FORMATION('',$,#117338) ;
#117292 = PRODUCT_DEFINITION_FORMATION('',$,#117339) ;
#117293 = PRODUCT_DEFINITION_FORMATION('',$,#117340) ;
#117294 = PRODUCT_DEFINITION_FORMATION('',$,#117341) ;
#117295 = PRODUCT_DEFINITION_FORMATION('',$,#117342) ;
#117296 = PRODUCT_DEFINITION_FORMATION('',$,#117343) ;
#117297 = PRODUCT_DEFINITION_FORMATION('',$,#117344) ;
#117298 = PRODUCT_DEFINITION_FORMATION('',$,#117345) ;
#117299 = PRODUCT_DEFINITION_FORMATION('',$,#117346) ;
#117300 = PRODUCT_DEFINITION_FORMATION('',$,#117347) ;
#117301 = PRODUCT_DEFINITION_FORMATION('',$,#117348) ;
#117302 = PRODUCT_DEFINITION_FORMATION('',$,#117349) ;
#117303 = PRODUCT_DEFINITION_FORMATION('',$,#117350) ;
#117304 = PRODUCT_DEFINITION_FORMATION('',$,#117351) ;
#117305 = PRODUCT_DEFINITION_FORMATION('',$,#117352) ;
#117306 = PRODUCT_DEFINITION_FORMATION('',$,#117353) ;
#117307 = PRODUCT_RELATED_PRODUCT_CATEGORY('MAS-655','MAS-655',(#117332)) ;
#117308 = PRODUCT_RELATED_PRODUCT_CATEGORY('Vertical_Knob',
'Vertical_Knob',(#117333)) ;
#117309 = PRODUCT_RELATED_PRODUCT_CATEGORY('Clamp_Handle','Clamp_Handle',
(#117334)) ;
#117310 = PRODUCT_RELATED_PRODUCT_CATEGORY('Base_Plate','Base_Plate',(#117335)) ;
#117311 = PRODUCT_RELATED_PRODUCT_CATEGORY('Pin_1','Pin_1',(#117336)) ;
#117312 = PRODUCT_RELATED_PRODUCT_CATEGORY('Cover_Plate','Cover_Plate',(#117337)) ;
#117313 = PRODUCT_RELATED_PRODUCT_CATEGORY('Pin_2','Pin_2',(#117338)) ;
#117314 = PRODUCT_RELATED_PRODUCT_CATEGORY('Spring_Washer_1',
'Spring_Washer_1',(#117339)) ;
#117315 = PRODUCT_RELATED_PRODUCT_CATEGORY('Spring_Washer_2',
'Spring_Washer_2',(#117340)) ;
#117316 = PRODUCT_RELATED_PRODUCT_CATEGORY('Spring_Washer_3',
'Spring_Washer_3',(#117341)) ;
#117317 = PRODUCT_RELATED_PRODUCT_CATEGORY('Washer_1','Washer_1',(#117342)) ;
#117318 = PRODUCT_RELATED_PRODUCT_CATEGORY('Washer_2','Washer_2',(#117343)) ;
#117319 = PRODUCT_RELATED_PRODUCT_CATEGORY('Spacer_1','Spacer_1',(#117344)) ;
#117320 = PRODUCT_RELATED_PRODUCT_CATEGORY('Spacer_2','Spacer_2',(#117345)) ;
#117321 = PRODUCT_RELATED_PRODUCT_CATEGORY('Spacer_3','Spacer_3',(#117346)) ;
#117322 = PRODUCT_RELATED_PRODUCT_CATEGORY('Latch','Latch',(#117347)) ;
#117323 = PRODUCT_RELATED_PRODUCT_CATEGORY('Housing','Housing',(#117348)) ;
#117324 = PRODUCT_RELATED_PRODUCT_CATEGORY('Lever_Pin','Lever_Pin',(#117349)) ;
#117325 = PRODUCT_RELATED_PRODUCT_CATEGORY('Knob_Shaft','Knob_Shaft',(#117350)) ;
#117326 = PRODUCT_RELATED_PRODUCT_CATEGORY('Knob_Grip_1','Knob_Grip_1',(#117351)) ;
#117327 = PRODUCT_RELATED_PRODUCT_CATEGORY('Knob_Grip_2','Knob_Grip_2',(#117352)) ;
#117328 = PRODUCT_RELATED_PRODUCT_CATEGORY('Knob_Pin','Knob_Pin',(#117353)) ;
#117329 = APPLICATION_PROTOCOL_DEFINITION('international standard',
'automotive_design',2009,#117330) ;
#117330 = APPLICATION_CONTEXT(
'Core Data for Automotive Mechanical Design Process') ;
#117331 = PRODUCT_CONTEXT('part definition',#117330,'mechanical') ;
#117332 = PRODUCT('MAS-655','MAS-655',$,(#117331)) ;
#117333 = PRODUCT('Vertical_Knob','Vertical_Knob',$,(#117331)) ;
#117334 = PRODUCT('Clamp_Handle','Clamp_Handle',$,(#117331)) ;
#117335 = PRODUCT('Base_Plate','Base_Plate',$,(#117331)) ;
#117336 = PRODUCT('Pin_1','Pin_1',$,(#117331)) ;
#117337 = PRODUCT('Cover_Plate','Cover_Plate',$,(#117331)) ;
#117338 = PRODUCT('Pin_2','Pin_2',$,(#117331)) ;
#117339 = PRODUCT('Spring_Washer_1','Spring_Washer_1',$,(#117331)) ;
#117340 = PRODUCT('Spring_Washer_2','Spring_Washer_2',$,(#117331)) ;
#117341 = PRODUCT('Spring_Washer_3','Spring_Washer_3',$,(#117331)) ;
#117342 = PRODUCT('Washer_1','Washer_1',$,(#117331)) ;
#117343 = PRODUCT('Washer_2','Washer_2',$,(#117331)) ;
#117344 = PRODUCT('Spacer_1','Spacer_1',$,(#117331)) ;
#117345 = PRODUCT('Spacer_2','Spacer_2',$,(#117331)) ;
#117346 = PRODUCT('Spacer_3','Spacer_3',$,(#117331)) ;
#117347 = PRODUCT('Latch','Latch',$,(#117331)) ;
#117348 = PRODUCT('Housing','Housing',$,(#117331)) ;
#117349 = PRODUCT('Lever_Pin','Lever_Pin',$,(#117331)) ;
#117350 = PRODUCT('Knob_Shaft','Knob_Shaft',$,(#117331)) ;
#117351 = PRODUCT('Knob_Grip_1','Knob_Grip_1',$,(#117331)) ;
#117352 = PRODUCT('Knob_Grip_2','Knob_Grip_2',$,(#117331)) ;
#117353 = PRODUCT('Knob_Pin','Knob_Pin',$,(#117331)) ;
#117354 = PRESENTATION_STYLE_ASSIGNMENT((#117356)) ;
#117355 = PRESENTATION_STYLE_ASSIGNMENT((#117357)) ;
#117356 = SURFACE_STYLE_USAGE(.BOTH.,#117358) ;
#117357 = SURFACE_STYLE_USAGE(.BOTH.,#117359) ;
#117358 = SURFACE_SIDE_STYLE('',(#117360)) ;
#117359 = SURFACE_SIDE_STYLE('',(#117361)) ;
#117360 = SURFACE_STYLE_FILL_AREA(#117362) ;
#117361 = SURFACE_STYLE_FILL_AREA(#117363) ;
#117362 = FILL_AREA_STYLE('Steel - Satin',(#117364)) ;
#117363 = FILL_AREA_STYLE('Opaque(160,160,160)',(#117365)) ;
#117364 = FILL_AREA_STYLE_COLOUR('Steel - Satin',#117366) ;
#117365 = FILL_AREA_STYLE_COLOUR('Opaque(160,160,160)',#117367) ;
#117366 = COLOUR_RGB('Steel - Satin', 0.09019608, 0.27058824, 0.51372549) ;
#117367 = COLOUR_RGB('Opaque(160,160,160)', 0.09019608, 0.27058824, 0.51372549) ;
ENDSEC;
END-ISO-10303-21;
